#216585=CARTESIAN_POINT('Ctrl Pts',(-17.7068495304908,-61.3772749311671,
-235.350049999996));
#216586=CARTESIAN_POINT('Ctrl Pts',(-17.7124533012131,-61.3775341254997,
-235.350049999996));
#216587=CARTESIAN_POINT('Ctrl Pts',(-17.7180571389861,-61.3777967664626,
-235.350049999996));
#216588=CARTESIAN_POINT('Ctrl Pts',(-17.7236610495722,-61.3780628532939,
-235.350049999996));
#216589=CARTESIAN_POINT('Ctrl Pts',(-17.9268662020405,-61.387711511008,
-235.350049999998));
#216590=CARTESIAN_POINT('Ctrl Pts',(-18.1305704995353,-61.4020849580281,
-235.350049999999));
#216591=CARTESIAN_POINT('Ctrl Pts',(-18.3343978331705,-61.421036350068,
-235.350049999999));
#216592=CARTESIAN_POINT('Ctrl Pts',(-18.5413055198001,-61.4402741461744,
-235.35005));
#216593=CARTESIAN_POINT('Ctrl Pts',(-18.7483412532968,-61.4642294656438,
-235.35005));
#216594=CARTESIAN_POINT('Ctrl Pts',(-18.95511001473,-61.4928010494512,-235.35005));
#216595=CARTESIAN_POINT('Ctrl Pts',(-19.1581684655807,-61.5208599375833,
-235.35005));
#216596=CARTESIAN_POINT('Ctrl Pts',(-19.3609706050519,-61.5533713065191,
-235.35005));
#216597=CARTESIAN_POINT('Ctrl Pts',(-19.5631227327773,-61.5902847141104,
-235.35005));
#216598=CARTESIAN_POINT('Ctrl Pts',(-19.7559941247032,-61.6255034396464,
-235.35005));
#216599=CARTESIAN_POINT('Ctrl Pts',(-19.9482746078014,-61.6647297766438,
-235.35005));
#216600=CARTESIAN_POINT('Ctrl Pts',(-20.1395905386961,-61.7079550103905,
-235.35005));
#216601=CARTESIAN_POINT('Ctrl Pts',(-20.1991813366268,-61.7214187410775,
-235.35005));
#216602=CARTESIAN_POINT('Ctrl Pts',(-20.2586782689426,-61.7352706787151,
-235.35005));
#216603=CARTESIAN_POINT('Ctrl Pts',(-20.3180691938068,-61.7495111937247,
-235.35005));
#216604=CARTESIAN_POINT('',(14.2619189241969,-62.8884528813233,-234.757545437753));
#216605=CARTESIAN_POINT('Ctrl Pts',(14.2619189241969,-62.8884528813233,
-234.757545437753));
#216606=CARTESIAN_POINT('Ctrl Pts',(14.2676221315376,-62.8870512825747,
-234.757599285427));
#216607=CARTESIAN_POINT('Ctrl Pts',(14.27309559464,-62.8857530533057,-234.757590335366));
#216608=CARTESIAN_POINT('Ctrl Pts',(14.2782562309469,-62.8845979535437,
-234.75749584595));
#216609=CARTESIAN_POINT('Ctrl Pts',(14.4728210423908,-62.8410487177465,
-234.753933433427));
#216610=CARTESIAN_POINT('Ctrl Pts',(14.6676054707436,-62.8029521711093,
-234.749855174901));
#216611=CARTESIAN_POINT('Ctrl Pts',(14.862267472532,-62.7701957889222,-234.74525442655));
#216612=CARTESIAN_POINT('Ctrl Pts',(15.0540973159843,-62.7379159828518,
-234.74072061498));
#216613=CARTESIAN_POINT('Ctrl Pts',(15.2458081247477,-62.7108217116278,
-234.735679369408));
#216614=CARTESIAN_POINT('Ctrl Pts',(15.4370736548847,-62.6887561762043,
-234.730130586681));
#216615=CARTESIAN_POINT('Ctrl Pts',(15.5314733326893,-62.6778656648139,
-234.727391968273));
#216616=CARTESIAN_POINT('Ctrl Pts',(15.6257144198455,-62.6682049982271,
-234.72453379674));
#216617=CARTESIAN_POINT('Ctrl Pts',(15.7197562183719,-62.6597512994103,
-234.721556787451));
#216618=CARTESIAN_POINT('Ctrl Pts',(15.9194398772557,-62.6418011374898,
-234.715235554589));
#216619=CARTESIAN_POINT('Ctrl Pts',(16.1183147406937,-62.6293052674362,
-234.708351013767));
#216620=CARTESIAN_POINT('Ctrl Pts',(16.3159941005111,-62.6220209771202,
-234.700911847004));
#216621=CARTESIAN_POINT('Ctrl Pts',(16.3574225292628,-62.6204943801976,
-234.699352792025));
#216622=CARTESIAN_POINT('Ctrl Pts',(16.3987984837776,-62.6191965047478,
-234.69776940586));
#216623=CARTESIAN_POINT('Ctrl Pts',(16.4401184612598,-62.6181248397371,
-234.696161814787));
#216624=CARTESIAN_POINT('Ctrl Pts',(16.5593593875656,-62.615032235715,-234.691522638766));
#216625=CARTESIAN_POINT('Ctrl Pts',(16.6781351876571,-62.6138244557668,
-234.68668086609));
#216626=CARTESIAN_POINT('Ctrl Pts',(16.7963700013562,-62.6144400515916,
-234.681635659345));
#216627=CARTESIAN_POINT('Ctrl Pts',(16.8554874082058,-62.6147478495039,
-234.679113055972));
#216628=CARTESIAN_POINT('Ctrl Pts',(16.9144695680729,-62.6155114373711,
-234.676539558438));
#216629=CARTESIAN_POINT('Ctrl Pts',(16.9733077389818,-62.6167227855682,
-234.673914918543));
#216630=CARTESIAN_POINT('Ctrl Pts',(17.0027268244363,-62.6173284596667,
-234.672602598595));
#216631=CARTESIAN_POINT('Ctrl Pts',(17.0321099129192,-62.6180460709255,
-234.671277491313));
#216632=CARTESIAN_POINT('Ctrl Pts',(17.0614559345793,-62.6188745972855,
-234.669939556944));
#216633=CARTESIAN_POINT('Ctrl Pts',(17.0847044612134,-62.6195309730414,
-234.668879617605));
#216634=CARTESIAN_POINT('Ctrl Pts',(17.1070374630585,-62.6202275257495,
-234.667852866661));
#216635=CARTESIAN_POINT('Ctrl Pts',(17.1305750905829,-62.621033000521,-234.666761357511));
#216636=CARTESIAN_POINT('Ctrl Pts',(17.136748409392,-62.6212442559907,-234.666475082526));
#216637=CARTESIAN_POINT('Ctrl Pts',(17.1430045641319,-62.6214632738738,
-234.666184319474));
#216638=CARTESIAN_POINT('Ctrl Pts',(17.1493817430919,-62.6216918876598,
-234.665887227365));
#216639=CARTESIAN_POINT('Ctrl Pts',(17.3478766374233,-62.6288076781356,
-234.656639993278));
#216640=CARTESIAN_POINT('Ctrl Pts',(17.5455520004757,-62.6410046705095,
-234.646771670025));
#216641=CARTESIAN_POINT('Ctrl Pts',(17.742009985154,-62.6580565731071,-234.636283597108));
#216642=CARTESIAN_POINT('Ctrl Pts',(17.9389575403572,-62.6751509688054,
-234.625769388061));
#216643=CARTESIAN_POINT('Ctrl Pts',(18.1347846733241,-62.6971222883386,
-234.614612391247));
#216644=CARTESIAN_POINT('Ctrl Pts',(18.3292291451991,-62.7237598595182,
-234.602804984691));
#216645=CARTESIAN_POINT('Ctrl Pts',(18.5259098814926,-62.7507037837252,
-234.590861783669));
#216646=CARTESIAN_POINT('Ctrl Pts',(18.7211759890429,-62.7824217829876,
-234.57825304333));
#216647=CARTESIAN_POINT('Ctrl Pts',(18.9147618610651,-62.8186429668106,
-234.56498137667));
#216648=CARTESIAN_POINT('Ctrl Pts',(19.1126402616024,-62.8556673108167,
-234.551415427131));
#216649=CARTESIAN_POINT('Ctrl Pts',(19.3087631000518,-62.8973966834212,
-234.537156722191));
#216650=CARTESIAN_POINT('Ctrl Pts',(19.5028524817591,-62.943488244167,-234.522220426416));
#216651=CARTESIAN_POINT('Ctrl Pts',(19.6704349995014,-62.9832850621511,
-234.509323986488));
#216652=CARTESIAN_POINT('Ctrl Pts',(19.8365016601851,-63.0263329686421,
-234.49592257589));
#216653=CARTESIAN_POINT('Ctrl Pts',(20.0008767707152,-63.0723812833681,
-234.482033933862));
#216654=CARTESIAN_POINT('Ctrl Pts',(8.7858832621216,-63.0089393155471,-234.571897587772));
#216655=CARTESIAN_POINT('Ctrl Pts',(8.79681567493446,-63.0115709797409,
-234.57181396807));
#216656=CARTESIAN_POINT('Ctrl Pts',(8.80985252396294,-63.0142665213595,
-234.572494303784));
#216657=CARTESIAN_POINT('Ctrl Pts',(8.82210928715347,-63.0169068663223,
-234.572891922504));
#216658=CARTESIAN_POINT('Ctrl Pts',(8.85244345145974,-63.0234414347627,
-234.573875985863));
#216659=CARTESIAN_POINT('Ctrl Pts',(8.88278396117814,-63.0298509579082,
-234.574862091849));
#216660=CARTESIAN_POINT('Ctrl Pts',(8.91316422636502,-63.0361424884105,
-234.575851272007));
#216661=CARTESIAN_POINT('Ctrl Pts',(8.99242293231775,-63.0525563861501,
-234.578431932142));
#216662=CARTESIAN_POINT('Ctrl Pts',(9.0719524711103,-63.0681709773559,-234.581033503827));
#216663=CARTESIAN_POINT('Ctrl Pts',(9.15234381497248,-63.0830750262618,
-234.583674547358));
#216664=CARTESIAN_POINT('Ctrl Pts',(9.19361826977972,-63.0907270502666,
-234.585030509663));
#216665=CARTESIAN_POINT('Ctrl Pts',(9.23511984058779,-63.0981909396172,
-234.586396884075));
#216666=CARTESIAN_POINT('Ctrl Pts',(9.27692812757237,-63.1054733788026,
-234.587776220271));
#216667=CARTESIAN_POINT('Ctrl Pts',(9.35723190012809,-63.1194612118898,
-234.590425596942));
#216668=CARTESIAN_POINT('Ctrl Pts',(9.4386674796978,-63.1327830283328,-234.593122828895));
#216669=CARTESIAN_POINT('Ctrl Pts',(9.52179594456459,-63.1454466317045,
-234.595885927164));
#216670=CARTESIAN_POINT('Ctrl Pts',(9.60320028398561,-63.1578475856835,
-234.598591717408));
#216671=CARTESIAN_POINT('Ctrl Pts',(9.68622805619257,-63.1696173756771,
-234.60136068521));
#216672=CARTESIAN_POINT('Ctrl Pts',(9.77140172737696,-63.1807142389001,
-234.604209720771));
#216673=CARTESIAN_POINT('Ctrl Pts',(9.84650123949516,-63.1904985889522,
-234.606721778519));
#216674=CARTESIAN_POINT('Ctrl Pts',(9.92326901592422,-63.1997592047957,
-234.60929609172));
#216675=CARTESIAN_POINT('Ctrl Pts',(10.0020597851061,-63.2084339698903,
-234.611944069746));
#216676=CARTESIAN_POINT('Ctrl Pts',(10.0079176914778,-63.2090789180518,
-234.612140940617));
#216677=CARTESIAN_POINT('Ctrl Pts',(10.0137868348703,-63.2097206627102,
-234.61233823974));
#216678=CARTESIAN_POINT('Ctrl Pts',(10.0196673616597,-63.2103591682456,
-234.61253597217));
#216679=CARTESIAN_POINT('Ctrl Pts',(10.1775217355446,-63.2274989407736,
-234.617843817891));
#216680=CARTESIAN_POINT('Ctrl Pts',(10.3408423339544,-63.2420090474358,
-234.623376571456));
#216681=CARTESIAN_POINT('Ctrl Pts',(10.5096382176533,-63.2531987375938,
-234.629123175597));
#216682=CARTESIAN_POINT('Ctrl Pts',(10.5851067962263,-63.2582016440177,
-234.631692480231));
#216683=CARTESIAN_POINT('Ctrl Pts',(10.6616697717933,-63.2625401196258,
-234.634304495196));
#216684=CARTESIAN_POINT('Ctrl Pts',(10.7393274396082,-63.2661491027286,
-234.636958032241));
#216685=CARTESIAN_POINT('Ctrl Pts',(10.8650023153563,-63.2719895884886,
-234.641252301536));
#216686=CARTESIAN_POINT('Ctrl Pts',(10.9935433905513,-63.2759200262142,
-234.645655597734));
#216687=CARTESIAN_POINT('Ctrl Pts',(11.124943865751,-63.2776525377261,-234.650163351666));
#216688=CARTESIAN_POINT('Ctrl Pts',(11.1906441033508,-63.278518793482,-234.652417228633));
#216689=CARTESIAN_POINT('Ctrl Pts',(11.2570590826227,-63.2788353452046,
-234.654697219748));
#216690=CARTESIAN_POINT('Ctrl Pts',(11.3241872747982,-63.2785648884929,
-234.657002776486));
#216691=CARTESIAN_POINT('Ctrl Pts',(11.3577513708859,-63.278429660137,-234.658155554855));
#216692=CARTESIAN_POINT('Ctrl Pts',(11.3914937693878,-63.2781476704804,
-234.659314718289));
#216693=CARTESIAN_POINT('Ctrl Pts',(11.4254142273421,-63.2777141703294,
-234.660480209155));
#216694=CARTESIAN_POINT('Ctrl Pts',(11.4423744563193,-63.2774974202539,
-234.661062954589));
#216695=CARTESIAN_POINT('Ctrl Pts',(11.4593792001185,-63.2772427919946,
-234.661647281495));
#216696=CARTESIAN_POINT('Ctrl Pts',(11.4764284266816,-63.2769496876593,
-234.662233181745));
#216697=CARTESIAN_POINT('Ctrl Pts',(11.4849530399631,-63.2768031354916,
-234.662526131871));
#216698=CARTESIAN_POINT('Ctrl Pts',(11.4934887739323,-63.2766469642703,
-234.662819475307));
#216699=CARTESIAN_POINT('Ctrl Pts',(11.5020356243932,-63.2764810989383,
-234.663113211071));
#216700=CARTESIAN_POINT('Ctrl Pts',(11.510582474854,-63.2763152336063,-234.663406946834));
#216701=CARTESIAN_POINT('Ctrl Pts',(11.5206164958058,-63.2761077505405,
-234.663751807062));
#216702=CARTESIAN_POINT('Ctrl Pts',(11.5277095211746,-63.2759543445152,
-234.663995595652));
#216703=CARTESIAN_POINT('Ctrl Pts',(11.7959382858705,-63.2701531656785,
-234.673214667765));
#216704=CARTESIAN_POINT('Ctrl Pts',(12.0647257367003,-63.2549839288532,
-234.682485491612));
#216705=CARTESIAN_POINT('Ctrl Pts',(12.3338331099587,-63.2303282374309,
-234.691756583846));
#216706=CARTESIAN_POINT('Ctrl Pts',(12.5122102573677,-63.2139852742112,
-234.697901904081));
#216707=CARTESIAN_POINT('Ctrl Pts',(12.6907279881409,-63.1934753535059,
-234.704047292337));
#216708=CARTESIAN_POINT('Ctrl Pts',(12.8693171326838,-63.1687765962808,
-234.710177274085));
#216709=CARTESIAN_POINT('Ctrl Pts',(13.1051691938716,-63.1361584166303,
-234.718272776385));
#216710=CARTESIAN_POINT('Ctrl Pts',(13.3412824605714,-63.0961134334835,
-234.726378967533));
#216711=CARTESIAN_POINT('Ctrl Pts',(13.5774175745815,-63.0484087566338,
-234.734431297969));
#216712=CARTESIAN_POINT('Ctrl Pts',(13.6949932812573,-63.0246557831895,
-234.738440690835));
#216713=CARTESIAN_POINT('Ctrl Pts',(13.8125727957745,-62.9990048475027,
-234.742436205742));
#216714=CARTESIAN_POINT('Ctrl Pts',(13.9301247417777,-62.9714309612777,
-234.746409185644));
#216715=CARTESIAN_POINT('Ctrl Pts',(13.9887912132901,-62.9576697036745,
-234.748391974702));
#216716=CARTESIAN_POINT('Ctrl Pts',(14.0474508288688,-62.9434295279964,
-234.750369153456));
#216717=CARTESIAN_POINT('Ctrl Pts',(14.1060997648205,-62.9287075009776,
-234.75233966774));
#216718=CARTESIAN_POINT('Ctrl Pts',(14.1112871883718,-62.9274053564725,
-234.752513957214));
#216719=CARTESIAN_POINT('Ctrl Pts',(14.1164745284042,-62.9260994424293,
-234.752688194559));
#216720=CARTESIAN_POINT('Ctrl Pts',(14.1216617823046,-62.9247897568609,
-234.752862379056));
#216721=CARTESIAN_POINT('Ctrl Pts',(14.1456979383595,-62.9187210724837,
-234.753669497011));
#216722=CARTESIAN_POINT('Ctrl Pts',(14.1698178995471,-62.9125255294095,
-234.754509575307));
#216723=CARTESIAN_POINT('Ctrl Pts',(14.1939742871885,-62.9062259828314,
-234.755364712355));
#216724=CARTESIAN_POINT('Ctrl Pts',(14.216952479753,-62.9002336881023,-234.756178141251));
#216725=CARTESIAN_POINT('Ctrl Pts',(14.2409845451924,-62.8936465131962,
-234.757285208748));
#216726=CARTESIAN_POINT('Ctrl Pts',(14.2619189241969,-62.8884528813233,
-234.757545437753));
#216727=CARTESIAN_POINT('Ctrl Pts',(55.6596124147223,-63.9410622767582,
-216.790642532039));
#216728=CARTESIAN_POINT('Ctrl Pts',(56.7746082597229,-64.9675904302956,
-215.348143273993));
#216729=CARTESIAN_POINT('Ctrl Pts',(56.7978769236249,-64.9962486583172,
-213.25615446688));
#216730=CARTESIAN_POINT('Ctrl Pts',(56.5646546671649,-62.9482476744138,
-216.79031846553));
#216731=CARTESIAN_POINT('Ctrl Pts',(57.7003423851772,-63.9568776617924,
-215.347378844935));
#216732=CARTESIAN_POINT('Ctrl Pts',(57.7238224635575,-63.9855135774693,
-213.252837709798));
#216733=CARTESIAN_POINT('Ctrl Pts',(57.4569850684519,-61.9095456344264,
-216.789947870949));
#216734=CARTESIAN_POINT('Ctrl Pts',(58.611700878634,-62.9065844937097,-215.346095403267));
#216735=CARTESIAN_POINT('Ctrl Pts',(58.6299194066537,-62.9418272935278,
-213.246154460278));
#216736=CARTESIAN_POINT('Ctrl Pts',(58.3016167962822,-60.8701016111416,
-216.790073419041));
#216737=CARTESIAN_POINT('Ctrl Pts',(59.4805126951739,-61.8494200250926,
-215.345222444811));
#216738=CARTESIAN_POINT('Ctrl Pts',(59.5017489787801,-61.8814728748856,
-213.239284157696));
#216739=CARTESIAN_POINT('',(59.5017489787801,-61.8814728748856,-213.239284157696));
#216740=CARTESIAN_POINT('Ctrl Pts',(56.8144552684302,-64.9781463796361,
-213.256094898505));
#216741=CARTESIAN_POINT('Ctrl Pts',(56.9294188925119,-64.8525744128834,
-213.255680555424));
#216742=CARTESIAN_POINT('Ctrl Pts',(57.0524106752843,-64.7173956850926,
-213.255183250552));
#216743=CARTESIAN_POINT('Ctrl Pts',(57.1833118747465,-64.5723463396209,
-213.254587821642));
#216744=CARTESIAN_POINT('Ctrl Pts',(57.3081863588042,-64.4339750928097,
-213.254019806389));
#216745=CARTESIAN_POINT('Ctrl Pts',(57.4402589750224,-64.2866205890543,
-213.253362393774));
#216746=CARTESIAN_POINT('Ctrl Pts',(57.5793799148568,-64.1300563307852,
-213.252605702994));
#216747=CARTESIAN_POINT('Ctrl Pts',(57.7142502997413,-63.9782755722807,
-213.251872131349));
#216748=CARTESIAN_POINT('Ctrl Pts',(57.8557452334703,-63.8178386808859,
-213.251045156913));
#216749=CARTESIAN_POINT('Ctrl Pts',(58.0036788274559,-63.6485500668985,
-213.250120374855));
#216750=CARTESIAN_POINT('Ctrl Pts',(58.1403782530185,-63.4921173347321,
-213.249265821317));
#216751=CARTESIAN_POINT('Ctrl Pts',(58.2825754484112,-63.3281259468563,
-213.248327716734));
#216752=CARTESIAN_POINT('Ctrl Pts',(58.4300800100018,-63.1564365856218,
-213.247307421374));
#216753=CARTESIAN_POINT('Ctrl Pts',(58.5727477993223,-62.9903770322558,
-213.246320582175));
#216754=CARTESIAN_POINT('Ctrl Pts',(58.7203807787913,-62.817115737271,-213.245256795861));
#216755=CARTESIAN_POINT('Ctrl Pts',(58.8727631035814,-62.6365458514646,
-213.244122705959));
#216756=CARTESIAN_POINT('Ctrl Pts',(59.0185109355358,-62.4638377016922,
-213.243037992593));
#216757=CARTESIAN_POINT('Ctrl Pts',(59.1686036195926,-62.2844432836784,
-213.241888927712));
#216758=CARTESIAN_POINT('Ctrl Pts',(59.3228101732188,-62.0982909448199,
-213.240687014781));
#216759=CARTESIAN_POINT('Ctrl Pts',(59.381858614956,-62.0270098917333,-213.240226780867));
#216760=CARTESIAN_POINT('Ctrl Pts',(59.4415097985946,-61.9547382044033,
-213.239758862166));
#216761=CARTESIAN_POINT('Ctrl Pts',(59.5017489787801,-61.8814728748856,
-213.239284157696));
#216762=CARTESIAN_POINT('',(58.3016167962821,-60.8701016111416,-216.790073419041));
#216763=CARTESIAN_POINT('Origin',(1.94104476119577,-15.0690951428036,-217.435380395218));
#216764=CARTESIAN_POINT('Origin',(55.6399013441494,-58.7068046741696,-213.15202212551));
#216765=CARTESIAN_POINT('Ctrl Pts',(60.0946517248888,-61.0923008758321,
-213.257460793579));
#216766=CARTESIAN_POINT('Ctrl Pts',(59.9794428890559,-61.1951119486122,
-215.368374394716));
#216767=CARTESIAN_POINT('Ctrl Pts',(58.6463245735781,-60.4071924582901,
-216.811211134516));
#216768=CARTESIAN_POINT('Ctrl Pts',(59.9074639858676,-61.3655831923349,
-213.24427462457));
#216769=CARTESIAN_POINT('Ctrl Pts',(59.8200433378112,-61.4202510270675,
-215.35259069506));
#216770=CARTESIAN_POINT('Ctrl Pts',(58.537453097357,-60.5671124334832,-216.797054630904));
#216771=CARTESIAN_POINT('Ctrl Pts',(59.7097127443643,-61.6285208837114,
-213.238301674021));
#216772=CARTESIAN_POINT('Ctrl Pts',(59.653667582921,-61.6382804704428,-215.344967772288));
#216773=CARTESIAN_POINT('Ctrl Pts',(58.4224878547945,-60.7213519315114,
-216.790091385297));
#216774=CARTESIAN_POINT('Ctrl Pts',(59.5017489787801,-61.8814728748855,
-213.239284157696));
#216775=CARTESIAN_POINT('Ctrl Pts',(59.4805126951738,-61.8494200250926,
-215.345222444811));
#216776=CARTESIAN_POINT('Ctrl Pts',(58.3016167962821,-60.8701016111416,
-216.790073419041));
#216777=CARTESIAN_POINT('',(58.6463245735781,-60.4071924582901,-216.811211134516));
#216778=CARTESIAN_POINT('',(60.094651724889,-61.0923008758319,-213.257460793579));
#216779=CARTESIAN_POINT('Origin',(55.9721510687884,-58.2643380616866,-213.170198761392));
#216780=CARTESIAN_POINT('Origin',(52.480669683245,-56.0916407951787,-217.694018753789));
#216781=CARTESIAN_POINT('Origin',(54.9927878736021,-61.8053486253609,-218.50906240554));
#216782=CARTESIAN_POINT('Ctrl Pts',(58.6074055114448,-60.4543100647495,
-216.811910699149));
#216783=CARTESIAN_POINT('Ctrl Pts',(59.9363259578221,-61.2556965846773,
-215.36842105937));
#216784=CARTESIAN_POINT('Ctrl Pts',(60.0500816328534,-61.1568904110335,
-213.254375849603));
#216785=CARTESIAN_POINT('Ctrl Pts',(58.6843926594325,-60.3569715803453,
-216.813280762464));
#216786=CARTESIAN_POINT('Ctrl Pts',(60.0245567355929,-61.1325327891189,
-215.370731335637));
#216787=CARTESIAN_POINT('Ctrl Pts',(60.1415615520333,-61.0252958819011,
-213.260597914992));
#216788=CARTESIAN_POINT('Ctrl Pts',(58.7617161401563,-60.257380322437,-216.813794119462));
#216789=CARTESIAN_POINT('Ctrl Pts',(60.1108245046652,-61.0067372913192,
-215.372344710318));
#216790=CARTESIAN_POINT('Ctrl Pts',(60.2301284165771,-60.8919475940444,
-213.267282154519));
#216791=CARTESIAN_POINT('Ctrl Pts',(58.8637629875194,-60.118929962275,-216.816300847937));
#216792=CARTESIAN_POINT('Ctrl Pts',(60.2274193821809,-60.8294290656787,
-215.376497710853));
#216793=CARTESIAN_POINT('Ctrl Pts',(60.351618647282,-60.7003634878413,-213.277642216535));
#216794=CARTESIAN_POINT('Ctrl Pts',(58.8929787543517,-60.0784113786681,
-216.817245287021));
#216795=CARTESIAN_POINT('Ctrl Pts',(60.2611173232929,-60.7772510392266,
-215.377939075409));
#216796=CARTESIAN_POINT('Ctrl Pts',(60.3869441313173,-60.6435508076928,
-213.280811345684));
#216797=CARTESIAN_POINT('Ctrl Pts',(58.9495124986678,-59.9981405703258,
-216.819674866848));
#216798=CARTESIAN_POINT('Ctrl Pts',(60.3271235407812,-60.6732372865155,
-215.381384415719));
#216799=CARTESIAN_POINT('Ctrl Pts',(60.4565718022466,-60.5293282073925,
-213.287428511102));
#216800=CARTESIAN_POINT('Ctrl Pts',(58.9761430287399,-59.9590023263254,
-216.821371021085));
#216801=CARTESIAN_POINT('Ctrl Pts',(60.359173711659,-60.6218554219661,-215.383594060466));
#216802=CARTESIAN_POINT('Ctrl Pts',(60.4908728037641,-60.4719198229408,
-213.290891213227));
#216803=CARTESIAN_POINT('Ctrl Pts',(59.0642485460056,-59.8329939373022,
-216.824171668603));
#216804=CARTESIAN_POINT('Ctrl Pts',(60.4575238287991,-60.4610669137915,
-215.388063886973));
#216805=CARTESIAN_POINT('Ctrl Pts',(60.5922460955355,-60.2987937845113,
-213.30164664474));
#216806=CARTESIAN_POINT('Ctrl Pts',(59.1308552045038,-59.7401265656055,
-216.823603457484));
#216807=CARTESIAN_POINT('Ctrl Pts',(60.5247139239745,-60.3469167156672,
-215.388758628301));
#216808=CARTESIAN_POINT('Ctrl Pts',(60.6577989462605,-60.182163619438,-213.309190814847));
#216809=CARTESIAN_POINT('Ctrl Pts',(59.2607825507709,-59.5528560555646,
-216.821806470031));
#216810=CARTESIAN_POINT('Ctrl Pts',(60.6547502248839,-60.1166039110421,
-215.389715911556));
#216811=CARTESIAN_POINT('Ctrl Pts',(60.7848819389693,-59.9464002293942,
-213.324386876106));
#216812=CARTESIAN_POINT('Ctrl Pts',(59.3235037477498,-59.4590534661329,
-216.82085617928));
#216813=CARTESIAN_POINT('Ctrl Pts',(60.7174143058776,-60.0009016819405,
-215.390241225136));
#216814=CARTESIAN_POINT('Ctrl Pts',(60.846408364718,-59.8272707789861,-213.332077521816));
#216815=CARTESIAN_POINT('Ctrl Pts',(59.497535989523,-59.1844462404644,-216.821411068371));
#216816=CARTESIAN_POINT('Ctrl Pts',(60.8959799414287,-59.6576852666735,
-215.395296546354));
#216817=CARTESIAN_POINT('Ctrl Pts',(61.0248485990128,-59.4661777527895,
-213.356063148757));
#216818=CARTESIAN_POINT('Ctrl Pts',(59.6013476331263,-59.0045621852585,
-216.824786693514));
#216819=CARTESIAN_POINT('Ctrl Pts',(61.0052029790378,-59.4294490925104,
-215.401835242901));
#216820=CARTESIAN_POINT('Ctrl Pts',(61.1355702178776,-59.2205125002805,
-213.373562975867));
#216821=CARTESIAN_POINT('Ctrl Pts',(59.7620679015636,-58.7165983993849,
-216.825507837644));
#216822=CARTESIAN_POINT('Ctrl Pts',(61.160929555377,-59.0728872758639,-215.408140407826));
#216823=CARTESIAN_POINT('Ctrl Pts',(61.2879458897801,-58.8475849978508,
-213.401799673797));
#216824=CARTESIAN_POINT('Ctrl Pts',(59.8184700980811,-58.6152752114856,
-216.824157923918));
#216825=CARTESIAN_POINT('Ctrl Pts',(61.2120467193731,-58.9500553531654,
-215.408866560461));
#216826=CARTESIAN_POINT('Ctrl Pts',(61.3365745411598,-58.7222537891958,
-213.411505588844));
#216827=CARTESIAN_POINT('Ctrl Pts',(59.9269424397347,-58.4123215093298,
-216.821223970727));
#216828=CARTESIAN_POINT('Ctrl Pts',(61.3093200563378,-58.7041349241579,
-215.410324805557));
#216829=CARTESIAN_POINT('Ctrl Pts',(61.429120358173,-58.4706258869242,-213.431043252633));
#216830=CARTESIAN_POINT('Ctrl Pts',(59.9776849531454,-58.3122310671642,
-216.820297737876));
#216831=CARTESIAN_POINT('Ctrl Pts',(61.3551328190027,-58.5821325532565,
-215.411652153446));
#216832=CARTESIAN_POINT('Ctrl Pts',(61.4730253186173,-58.3443774821519,
-213.440939227853));
#216833=CARTESIAN_POINT('Ctrl Pts',(60.1230288656398,-58.0127552603068,
-216.818391671956));
#216834=CARTESIAN_POINT('Ctrl Pts',(61.4853151645514,-58.2168872743818,
-215.416733820586));
#216835=CARTESIAN_POINT('Ctrl Pts',(61.5977142939005,-57.9644548465746,
-213.471381381577));
#216836=CARTESIAN_POINT('Ctrl Pts',(60.2105402005316,-57.8145726066615,
-216.818537217051));
#216837=CARTESIAN_POINT('Ctrl Pts',(61.5626251138468,-57.9742502615569,
-215.421806822622));
#216838=CARTESIAN_POINT('Ctrl Pts',(61.6714754954738,-57.7096224301994,
-213.49274435759));
#216839=CARTESIAN_POINT('Ctrl Pts',(60.3806025831265,-57.4045491967827,
-216.81529811369));
#216840=CARTESIAN_POINT('Ctrl Pts',(61.7018225456774,-57.4799411928046,
-215.429818040078));
#216841=CARTESIAN_POINT('Ctrl Pts',(61.8007144046227,-57.1969944641333,
-213.537796166961));
#216842=CARTESIAN_POINT('Ctrl Pts',(60.4634339941568,-57.1919229894312,
-216.811338644603));
#216843=CARTESIAN_POINT('Ctrl Pts',(61.7636221410114,-57.2279080669269,
-215.432277259244));
#216844=CARTESIAN_POINT('Ctrl Pts',(61.8562081200067,-56.9391516851297,
-213.561315895501));
#216845=CARTESIAN_POINT('Ctrl Pts',(60.6152405963767,-56.762184327613,-216.802302824218));
#216846=CARTESIAN_POINT('Ctrl Pts',(61.8694772718262,-56.7213693952703,
-215.43746654745));
#216847=CARTESIAN_POINT('Ctrl Pts',(61.9491342563802,-56.4203496749288,
-213.610036002497));
#216848=CARTESIAN_POINT('Ctrl Pts',(60.6824463640865,-56.5477747378356,
-216.798434344268));
#216849=CARTESIAN_POINT('Ctrl Pts',(61.9133532267272,-56.4685867807556,
-215.441201542271));
#216850=CARTESIAN_POINT('Ctrl Pts',(61.9865582056432,-56.1594017179448,
-213.635279158434));
#216851=CARTESIAN_POINT('Ctrl Pts',(60.8073533359841,-56.0969490021232,
-216.792401635896));
#216852=CARTESIAN_POINT('Ctrl Pts',(61.9872021354889,-55.9382448925313,
-215.452237086731));
#216853=CARTESIAN_POINT('Ctrl Pts',(62.0459484757164,-55.6091885457502,
-213.691499099128));
#216854=CARTESIAN_POINT('Ctrl Pts',(60.8666693908396,-55.8585138307279,
-216.788165726564));
#216855=CARTESIAN_POINT('Ctrl Pts',(62.0158520694785,-55.6592576800417,
-215.457808501477));
#216856=CARTESIAN_POINT('Ctrl Pts',(62.0660566009803,-55.3196727763676,
-213.722940188816));
#216857=CARTESIAN_POINT('Ctrl Pts',(60.9269250208923,-55.5935705192412,
-216.775920823856));
#216858=CARTESIAN_POINT('Ctrl Pts',(62.0343090115749,-55.3647134586715,
-215.458374400723));
#216859=CARTESIAN_POINT('Ctrl Pts',(62.0750191951853,-55.0282471371092,
-213.755373099554));
#216860=CARTESIAN_POINT('',(60.9119170756758,-55.6633990141858,-216.777770284882));
#216861=CARTESIAN_POINT('',(62.0723653519316,-55.1059089910534,-213.746749287634));
#216862=CARTESIAN_POINT('Origin',(57.0770276271036,-54.9084593705222,-213.659487255448));
#216863=CARTESIAN_POINT('Ctrl Pts',(60.0946517248888,-61.0923008758318,
-213.257460793579));
#216864=CARTESIAN_POINT('Ctrl Pts',(60.1688733048961,-60.9839420408379,
-213.262689226369));
#216865=CARTESIAN_POINT('Ctrl Pts',(60.2426760592975,-60.8721561614362,
-213.268476733384));
#216866=CARTESIAN_POINT('Ctrl Pts',(60.3157714398376,-60.7568862808627,
-213.274784382698));
#216867=CARTESIAN_POINT('Ctrl Pts',(60.3512737868304,-60.7008998249785,
-213.277848001124));
#216868=CARTESIAN_POINT('Ctrl Pts',(60.3866089369293,-60.6440917231958,
-213.281039224211));
#216869=CARTESIAN_POINT('Ctrl Pts',(60.4217426652322,-60.5864561384688,
-213.284371063984));
#216870=CARTESIAN_POINT('Ctrl Pts',(60.4435624323821,-60.5506616156829,
-213.286440299775));
#216871=CARTESIAN_POINT('Ctrl Pts',(60.4653040350053,-60.514548553946,-213.288569677611));
#216872=CARTESIAN_POINT('Ctrl Pts',(60.4869604790493,-60.4781138482913,
-213.290748336221));
#216873=CARTESIAN_POINT('Ctrl Pts',(60.4995551781952,-60.4569245821652,
-213.292015374783));
#216874=CARTESIAN_POINT('Ctrl Pts',(60.5121204198581,-60.4356273698192,
-213.293306640679));
#216875=CARTESIAN_POINT('Ctrl Pts',(60.5246547397792,-60.4142217745433,
-213.294620659626));
#216876=CARTESIAN_POINT('Ctrl Pts',(60.591150130146,-60.3006636858019,-213.301591616443));
#216877=CARTESIAN_POINT('Ctrl Pts',(60.6567843084902,-60.1840449613726,
-213.309095887413));
#216878=CARTESIAN_POINT('Ctrl Pts',(60.7213395261845,-60.0642830904757,
-213.316803279816));
#216879=CARTESIAN_POINT('Ctrl Pts',(60.7685965359593,-59.9766125952661,
-213.322445400331));
#216880=CARTESIAN_POINT('Ctrl Pts',(60.8152737419114,-59.8872593538088,
-213.328214013836));
#216881=CARTESIAN_POINT('Ctrl Pts',(60.8612668418636,-59.7962116928738,
-213.334193694335));
#216882=CARTESIAN_POINT('Ctrl Pts',(60.8762151842007,-59.7666200452991,
-213.336137166535));
#216883=CARTESIAN_POINT('Ctrl Pts',(60.8910888831917,-59.7368539552651,
-213.338107798564));
#216884=CARTESIAN_POINT('Ctrl Pts',(60.9058862461468,-59.7069094955419,
-213.340107694982));
#216885=CARTESIAN_POINT('Ctrl Pts',(60.9637435733099,-59.5898273905627,
-213.347927241053));
#216886=CARTESIAN_POINT('Ctrl Pts',(61.0204246813107,-59.4700172291252,
-213.356262962161));
#216887=CARTESIAN_POINT('Ctrl Pts',(61.0757281447404,-59.3474693357667,
-213.365036420254));
#216888=CARTESIAN_POINT('Ctrl Pts',(61.1204542243354,-59.2483600487051,
-213.372131859865));
#216889=CARTESIAN_POINT('Ctrl Pts',(61.1642786072501,-59.1474602983931,
-213.37951365019));
#216890=CARTESIAN_POINT('Ctrl Pts',(61.2070729743782,-59.0447771657053,
-213.387142007677));
#216891=CARTESIAN_POINT('Ctrl Pts',(61.2171558757692,-59.0205837035538,
-213.388939346473));
#216892=CARTESIAN_POINT('Ctrl Pts',(61.2271793702854,-58.996296378915,-213.390750959789));
#216893=CARTESIAN_POINT('Ctrl Pts',(61.2371418312946,-58.9719150325815,
-213.392578681107));
#216894=CARTESIAN_POINT('Ctrl Pts',(61.2783750144538,-58.8710041714885,
-213.400143354916));
#216895=CARTESIAN_POINT('Ctrl Pts',(61.3186449470215,-58.7682927383909,
-213.407960918625));
#216896=CARTESIAN_POINT('Ctrl Pts',(61.3577808239653,-58.6639330018756,
-213.416038726705));
#216897=CARTESIAN_POINT('Ctrl Pts',(61.3604129670204,-58.6569141287302,
-213.416582012));
#216898=CARTESIAN_POINT('Ctrl Pts',(61.3630399688414,-58.649887813559,-213.417126466415));
#216899=CARTESIAN_POINT('Ctrl Pts',(61.3656617724452,-58.642854108928,-213.417672088598));
#216900=CARTESIAN_POINT('Ctrl Pts',(61.3714146872104,-58.6274203429637,
-213.418869324694));
#216901=CARTESIAN_POINT('Ctrl Pts',(61.3771434762636,-58.6119486844701,
-213.420070235415));
#216902=CARTESIAN_POINT('Ctrl Pts',(61.3828474496664,-58.59643983806,-213.421274420738));
#216903=CARTESIAN_POINT('Ctrl Pts',(61.4066350315578,-58.5317624758125,
-213.426296298467));
#216904=CARTESIAN_POINT('Ctrl Pts',(61.4299886141107,-58.4664490159562,
-213.431392104351));
#216905=CARTESIAN_POINT('Ctrl Pts',(61.4528841092791,-58.4004915334073,
-213.436581849268));
#216906=CARTESIAN_POINT('Ctrl Pts',(61.4671034320988,-58.3595284212386,
-213.439804957473));
#216907=CARTESIAN_POINT('Ctrl Pts',(61.48114539916,-58.318318751907,-213.443064189012));
#216908=CARTESIAN_POINT('Ctrl Pts',(61.4950031156842,-58.2768639431237,
-213.446364418246));
#216909=CARTESIAN_POINT('Ctrl Pts',(61.4998241791749,-58.2624419231042,
-213.447512559402));
#216910=CARTESIAN_POINT('Ctrl Pts',(61.5050437465624,-58.2467173872201,
-213.448767386496));
#216911=CARTESIAN_POINT('Ctrl Pts',(61.5096349176404,-58.2327939136108,
-213.449881149215));
#216912=CARTESIAN_POINT('Ctrl Pts',(61.5106925269236,-58.2295865413098,
-213.450137712469));
#216913=CARTESIAN_POINT('Ctrl Pts',(61.5117170122721,-58.2264747787118,
-213.450386767174));
#216914=CARTESIAN_POINT('Ctrl Pts',(61.5126961916284,-58.2234966253952,
-213.450625245251));
#216915=CARTESIAN_POINT('Ctrl Pts',(61.5133274243917,-58.221576744287,-213.450778981311));
#216916=CARTESIAN_POINT('Ctrl Pts',(61.5139581302282,-58.2196567378002,
-213.450932777525));
#216917=CARTESIAN_POINT('Ctrl Pts',(61.5145883090845,-58.2177366063309,
-213.451086634312));
#216918=CARTESIAN_POINT('Ctrl Pts',(61.5754675922918,-58.0322397011969,
-213.465950177932));
#216919=CARTESIAN_POINT('Ctrl Pts',(61.6314260330506,-57.8455859554956,
-213.481413045566));
#216920=CARTESIAN_POINT('Ctrl Pts',(61.6824475740234,-57.6580324650191,
-213.49749706447));
#216921=CARTESIAN_POINT('Ctrl Pts',(61.7009806262513,-57.5899055804081,
-213.503339419615));
#216922=CARTESIAN_POINT('Ctrl Pts',(61.7188627796439,-57.5216600629364,
-213.509263678944));
#216923=CARTESIAN_POINT('Ctrl Pts',(61.736094926277,-57.4533085098064,-213.51527069985));
#216924=CARTESIAN_POINT('Ctrl Pts',(61.7840826055166,-57.2629647019827,
-213.531998911289));
#216925=CARTESIAN_POINT('Ctrl Pts',(61.8270345946187,-57.0717719007629,
-213.549276027728));
#216926=CARTESIAN_POINT('Ctrl Pts',(61.8649529491542,-56.8799677222285,
-213.567015134291));
#216927=CARTESIAN_POINT('Ctrl Pts',(61.8781328721527,-56.8132991039609,
-213.573181015206));
#216928=CARTESIAN_POINT('Ctrl Pts',(61.8907051028513,-56.7465566994706,
-213.579402669573));
#216929=CARTESIAN_POINT('Ctrl Pts',(61.9026711707414,-56.6797507397666,
-213.585676324044));
#216930=CARTESIAN_POINT('Ctrl Pts',(61.9367372826433,-56.4895613375432,
-213.60353674546));
#216931=CARTESIAN_POINT('Ctrl Pts',(61.9658823716952,-56.2988624688379,
-213.621842648317));
#216932=CARTESIAN_POINT('Ctrl Pts',(61.9901097322645,-56.1079785002405,
-213.640827105813));
#216933=CARTESIAN_POINT('Ctrl Pts',(61.9990293863389,-56.0377017995089,
-213.647816509102));
#216934=CARTESIAN_POINT('Ctrl Pts',(62.0072829516351,-55.9674000675249,
-213.654897754168));
#216935=CARTESIAN_POINT('Ctrl Pts',(62.0148722891561,-55.8970896752966,
-213.662081941508));
#216936=CARTESIAN_POINT('Ctrl Pts',(62.0354032478553,-55.7068833819308,
-213.68151687284));
#216937=CARTESIAN_POINT('Ctrl Pts',(62.0510721347403,-55.5166252894532,
-213.701767805664));
#216938=CARTESIAN_POINT('Ctrl Pts',(62.0619255431476,-55.3264908015158,
-213.722497227011));
#216939=CARTESIAN_POINT('Ctrl Pts',(62.0661239505739,-55.2529413674403,
-213.730515957465));
#216940=CARTESIAN_POINT('Ctrl Pts',(62.0696023181198,-55.1794105511713,
-213.738606363368));
#216941=CARTESIAN_POINT('Ctrl Pts',(62.0723653519315,-55.1059089910535,
-213.746749287634));
#216942=CARTESIAN_POINT('Ctrl Pts',(60.9119170756758,-55.6633990141858,
-216.777770284882));
#216943=CARTESIAN_POINT('Ctrl Pts',(60.9073907830727,-55.6830113627593,
-216.778588585298));
#216944=CARTESIAN_POINT('Ctrl Pts',(60.9027344732998,-55.7030660698564,
-216.779382142226));
#216945=CARTESIAN_POINT('Ctrl Pts',(60.8979388924468,-55.7235631928626,
-216.780150955665));
#216946=CARTESIAN_POINT('Ctrl Pts',(60.8855667250161,-55.7764439273244,
-216.782134425215));
#216947=CARTESIAN_POINT('Ctrl Pts',(60.8722672911103,-55.8322729157864,
-216.783953203688));
#216948=CARTESIAN_POINT('Ctrl Pts',(60.8579173895963,-55.8910134972092,
-216.785607291083));
#216949=CARTESIAN_POINT('Ctrl Pts',(60.8525552968731,-55.9129629470987,
-216.786225369888));
#216950=CARTESIAN_POINT('Ctrl Pts',(60.8470465325387,-55.9353184362973,
-216.786820453299));
#216951=CARTESIAN_POINT('Ctrl Pts',(60.8413847105074,-55.9580761274448,
-216.787392541314));
#216952=CARTESIAN_POINT('Ctrl Pts',(60.8280412423979,-56.0117101916013,
-216.788740806617));
#216953=CARTESIAN_POINT('Ctrl Pts',(60.8138474727369,-56.0675809540217,
-216.789961349869));
#216954=CARTESIAN_POINT('Ctrl Pts',(60.7987212695568,-56.1256111309988,
-216.791054171069));
#216955=CARTESIAN_POINT('Ctrl Pts',(60.7911581679667,-56.1546262194874,
-216.791600581669));
#216956=CARTESIAN_POINT('Ctrl Pts',(60.7833619960081,-56.1841805428932,
-216.792115061728));
#216957=CARTESIAN_POINT('Ctrl Pts',(60.7753227949662,-56.2142603888131,
-216.792597612924));
#216958=CARTESIAN_POINT('Ctrl Pts',(60.7713031944453,-56.2293003117731,
-216.792838888522));
#216959=CARTESIAN_POINT('Ctrl Pts',(60.7672228324461,-56.2444716142868,
-216.793072178277));
#216960=CARTESIAN_POINT('Ctrl Pts',(60.7630805012708,-56.2597722389012,
-216.793297487807));
#216961=CARTESIAN_POINT('Ctrl Pts',(60.7595341573754,-56.2728714514941,
-216.793490380419));
#216962=CARTESIAN_POINT('Ctrl Pts',(60.7555793881087,-56.2873946780629,
-216.793695306117));
#216963=CARTESIAN_POINT('Ctrl Pts',(60.7521474474415,-56.2999266198356,
-216.793866332403));
#216964=CARTESIAN_POINT('Ctrl Pts',(60.7515706864043,-56.3020326981266,
-216.793895074536));
#216965=CARTESIAN_POINT('Ctrl Pts',(60.7510088127115,-56.3040825498413,
-216.793922859246));
#216966=CARTESIAN_POINT('Ctrl Pts',(60.7504663829785,-56.3060599824529,
-216.793949468515));
#216967=CARTESIAN_POINT('Ctrl Pts',(60.726744928692,-56.3925367635904,-216.795113141008));
#216968=CARTESIAN_POINT('Ctrl Pts',(60.7021402838857,-56.4777392222418,
-216.796372991844));
#216969=CARTESIAN_POINT('Ctrl Pts',(60.6768135902453,-56.5613350649519,
-216.797729021024));
#216970=CARTESIAN_POINT('Ctrl Pts',(60.6619983636042,-56.610235698157,-216.798522250488));
#216971=CARTESIAN_POINT('Ctrl Pts',(60.6469357952424,-56.6585875450376,
-216.799348390635));
#216972=CARTESIAN_POINT('Ctrl Pts',(60.6316559403284,-56.7063320203518,
-216.800207441465));
#216973=CARTESIAN_POINT('Ctrl Pts',(60.6232394165903,-56.7326308636398,
-216.800680628007));
#216974=CARTESIAN_POINT('Ctrl Pts',(60.6147569210123,-56.7587455902481,
-216.801163799913));
#216975=CARTESIAN_POINT('Ctrl Pts',(60.6062090667045,-56.7846826419487,
-216.801656957185));
#216976=CARTESIAN_POINT('Ctrl Pts',(60.5977766165011,-56.8102695189606,
-216.802143456368));
#216977=CARTESIAN_POINT('Ctrl Pts',(60.5892805607033,-56.8356834853934,
-216.802639673109));
#216978=CARTESIAN_POINT('Ctrl Pts',(60.5807215482445,-56.8609304861147,
-216.803145607486));
#216979=CARTESIAN_POINT('Ctrl Pts',(60.5764420420152,-56.8735539864754,
-216.803398574674));
#216980=CARTESIAN_POINT('Ctrl Pts',(60.5721467964869,-56.8861357453652,
-216.803653971149));
#216981=CARTESIAN_POINT('Ctrl Pts',(60.5678358994622,-56.8986764798207,
-216.803911797061));
#216982=CARTESIAN_POINT('Ctrl Pts',(60.5656804509498,-56.9049468470485,
-216.804040710018));
#216983=CARTESIAN_POINT('Ctrl Pts',(60.5635210895554,-56.9112069581651,
-216.804170230326));
#216984=CARTESIAN_POINT('Ctrl Pts',(60.5613578264237,-56.9174569020256,
-216.804300357988));
#216985=CARTESIAN_POINT('Ctrl Pts',(60.5591945632921,-56.923706845886,-216.80443048565));
#216986=CARTESIAN_POINT('Ctrl Pts',(60.5576872782576,-56.9280531415995,
-216.8045212999));
#216987=CARTESIAN_POINT('Ctrl Pts',(60.5548563430524,-56.9361763202472,
-216.804692563016));
#216988=CARTESIAN_POINT('Ctrl Pts',(60.531775183356,-57.002406159512,-216.806088904177));
#216989=CARTESIAN_POINT('Ctrl Pts',(60.5092923413343,-57.0649063224503,
-216.80735534074));
#216990=CARTESIAN_POINT('Ctrl Pts',(60.4875747703621,-57.1238418980249,
-216.808491872706));
#216991=CARTESIAN_POINT('Ctrl Pts',(60.4666733138366,-57.1805627611569,
-216.809585695468));
#216992=CARTESIAN_POINT('Ctrl Pts',(60.4464808877171,-57.2339808981995,
-216.810559193437));
#216993=CARTESIAN_POINT('Ctrl Pts',(60.4271400166051,-57.2841984344429,
-216.811412366612));
#216994=CARTESIAN_POINT('Ctrl Pts',(60.4074215554359,-57.3353963630518,
-216.812282196209));
#216995=CARTESIAN_POINT('Ctrl Pts',(60.3885884660559,-57.3832669787684,
-216.813026956971));
#216996=CARTESIAN_POINT('Ctrl Pts',(60.3707817467398,-57.4278816294471,
-216.813646648899));
#216997=CARTESIAN_POINT('Ctrl Pts',(60.3618783870818,-57.4501889547864,
-216.813956494863));
#216998=CARTESIAN_POINT('Ctrl Pts',(60.353231441283,-57.4716817687946,-216.814235073607));
#216999=CARTESIAN_POINT('Ctrl Pts',(60.344857338237,-57.4923662297235,-216.814482391391));
#217000=CARTESIAN_POINT('Ctrl Pts',(60.340670286714,-57.502708460188,-216.814606050283));
#217001=CARTESIAN_POINT('Ctrl Pts',(60.3365514347898,-57.5128485980101,
-216.814721883031));
#217002=CARTESIAN_POINT('Ctrl Pts',(60.3325027491553,-57.5227872445278,
-216.814829903421));
#217003=CARTESIAN_POINT('Ctrl Pts',(60.330478406338,-57.5277565677866,-216.814883913616));
#217004=CARTESIAN_POINT('Ctrl Pts',(60.3284716044061,-57.5326755179509,
-216.814935970048));
#217005=CARTESIAN_POINT('Ctrl Pts',(60.3264825839235,-57.5375441656945,
-216.814986072732));
#217006=CARTESIAN_POINT('Ctrl Pts',(60.3244935634409,-57.5424128134381,
-216.815036175415));
#217007=CARTESIAN_POINT('Ctrl Pts',(60.3231512484711,-57.5456958600444,
-216.815069449648));
#217008=CARTESIAN_POINT('Ctrl Pts',(60.3205691041673,-57.5519992691854,
-216.815130518181));
#217009=CARTESIAN_POINT('Ctrl Pts',(60.3057977046936,-57.5880585143369,
-216.815479866468));
#217010=CARTESIAN_POINT('Ctrl Pts',(60.2908264545178,-57.6241214719244,
-216.815797788964));
#217011=CARTESIAN_POINT('Ctrl Pts',(60.2756504796204,-57.6602025647167,
-216.816084285669));
#217012=CARTESIAN_POINT('Ctrl Pts',(60.2483805836785,-57.7250371241154,
-216.816599095121));
#217013=CARTESIAN_POINT('Ctrl Pts',(60.2204496607956,-57.7899302381468,
-216.81701243403));
#217014=CARTESIAN_POINT('Ctrl Pts',(60.1919174451317,-57.854738387928,-216.817324302395));
#217015=CARTESIAN_POINT('Ctrl Pts',(60.1697121029587,-57.9051756606042,
-216.817567015538));
#217016=CARTESIAN_POINT('Ctrl Pts',(60.1471425664518,-57.9555614731162,
-216.817748269903));
#217017=CARTESIAN_POINT('Ctrl Pts',(60.124236944089,-58.0058281702384,-216.817868065669));
#217018=CARTESIAN_POINT('Ctrl Pts',(60.1127841329077,-58.0309615187996,
-216.817927963552));
#217019=CARTESIAN_POINT('Ctrl Pts',(60.1012472999562,-58.0560650883737,
-216.817972496468));
#217020=CARTESIAN_POINT('Ctrl Pts',(60.0896299548045,-58.0811304205851,
-216.818001664822));
#217021=CARTESIAN_POINT('Ctrl Pts',(60.0794647777968,-58.1030625862702,
-216.818027187132));
#217022=CARTESIAN_POINT('Ctrl Pts',(60.0692379586165,-58.1249654764669,
-216.81804094593));
#217023=CARTESIAN_POINT('Ctrl Pts',(60.0589518474159,-58.146833423864,-216.818042941059));
#217024=CARTESIAN_POINT('Ctrl Pts',(60.0574824029587,-58.1499574163493,
-216.818043226077));
#217025=CARTESIAN_POINT('Ctrl Pts',(60.0554334228072,-58.1543076149849,
-216.818043194359));
#217026=CARTESIAN_POINT('Ctrl Pts',(60.0545398907524,-58.156203245427,-216.818043075904));
#217027=CARTESIAN_POINT('Ctrl Pts',(60.0450523572134,-58.1763310710596,
-216.818041818146));
#217028=CARTESIAN_POINT('Ctrl Pts',(60.0333692392358,-58.2007570838859,
-216.818133804124));
#217029=CARTESIAN_POINT('Ctrl Pts',(60.019406065471,-58.2294040937821,-216.818319033837));
#217030=CARTESIAN_POINT('Ctrl Pts',(60.0123285027026,-58.2439245039755,
-216.81841292187));
#217031=CARTESIAN_POINT('Ctrl Pts',(60.0046647473224,-58.2595287307156,
-216.818530766153));
#217032=CARTESIAN_POINT('Ctrl Pts',(59.9964016741368,-58.2762019403733,
-216.818672566686));
#217033=CARTESIAN_POINT('Ctrl Pts',(59.9841191164583,-58.3009856563962,
-216.818883344587));
#217034=CARTESIAN_POINT('Ctrl Pts',(59.9705125067986,-58.32813243013,-216.819147053873));
#217035=CARTESIAN_POINT('Ctrl Pts',(59.955534532171,-58.35757651355,-216.819463694545));
#217036=CARTESIAN_POINT('Ctrl Pts',(59.9480455448571,-58.37229855526,-216.819622014881));
#217037=CARTESIAN_POINT('Ctrl Pts',(59.9402136478829,-58.3875945819531,
-216.819793568053));
#217038=CARTESIAN_POINT('Ctrl Pts',(59.9320326268601,-58.4034540498328,
-216.819978358033));
#217039=CARTESIAN_POINT('Ctrl Pts',(59.9279421163487,-58.4113837837727,
-216.820070753024));
#217040=CARTESIAN_POINT('Ctrl Pts',(59.9237643184495,-58.4194543747942,
-216.82016645031));
#217041=CARTESIAN_POINT('Ctrl Pts',(59.9194984513664,-58.4276643114252,
-216.820265458625));
#217042=CARTESIAN_POINT('Ctrl Pts',(59.9173655178249,-58.4317692797407,
-216.820314962783));
#217043=CARTESIAN_POINT('Ctrl Pts',(59.9152105665835,-58.4359090842562,
-216.820365294261));
#217044=CARTESIAN_POINT('Ctrl Pts',(59.9130334990711,-58.4400835282948,
-216.820416453085));
#217045=CARTESIAN_POINT('Ctrl Pts',(59.9108564315587,-58.4442579723333,
-216.82046761191));
#217046=CARTESIAN_POINT('Ctrl Pts',(59.9093877396424,-58.447071603812,-216.820502230613));
#217047=CARTESIAN_POINT('Ctrl Pts',(59.9064358482483,-58.4527105781537,
-216.820572410718));
#217048=CARTESIAN_POINT('Ctrl Pts',(59.8836567049482,-58.4962253920307,
-216.821113976256));
#217049=CARTESIAN_POINT('Ctrl Pts',(59.863123350219,-58.5347073198221,-216.821591266887));
#217050=CARTESIAN_POINT('Ctrl Pts',(59.8449810090749,-58.5683168623629,
-216.82200428261));
#217051=CARTESIAN_POINT('Ctrl Pts',(59.8406893207328,-58.5762674174075,
-216.822101984155));
#217052=CARTESIAN_POINT('Ctrl Pts',(59.8365311992246,-58.5839453291258,
-216.822196088943));
#217053=CARTESIAN_POINT('Ctrl Pts',(59.8325081565776,-58.5913526920526,
-216.822286596973));
#217054=CARTESIAN_POINT('Ctrl Pts',(59.8182762284612,-58.6175570020629,
-216.822606778461));
#217055=CARTESIAN_POINT('Ctrl Pts',(59.8057378540362,-58.6403753963495,
-216.822881947839));
#217056=CARTESIAN_POINT('Ctrl Pts',(59.7949528527874,-58.6598895003186,
-216.823112105107));
#217057=CARTESIAN_POINT('Ctrl Pts',(59.7823725663588,-58.6826519471338,
-216.82338057465));
#217058=CARTESIAN_POINT('Ctrl Pts',(59.7721774792337,-58.7009207038603,
-216.82358779928));
#217059=CARTESIAN_POINT('Ctrl Pts',(59.764413184972,-58.7148074027386,-216.823733778996));
#217060=CARTESIAN_POINT('Ctrl Pts',(59.7639315295643,-58.715668859477,-216.823742834799));
#217061=CARTESIAN_POINT('Ctrl Pts',(59.7634592167051,-58.7165134410566,
-216.823751654913));
#217062=CARTESIAN_POINT('Ctrl Pts',(59.7629962529251,-58.7173411691037,
-216.823760239338));
#217063=CARTESIAN_POINT('Ctrl Pts',(59.7590332786009,-58.7244265289962,
-216.823833722101));
#217064=CARTESIAN_POINT('Ctrl Pts',(59.7557554978705,-58.7302773052047,
-216.823889935053));
#217065=CARTESIAN_POINT('Ctrl Pts',(59.7531659200656,-58.7349047974698,
-216.82392889424));
#217066=CARTESIAN_POINT('Ctrl Pts',(59.7518711311631,-58.7372185436024,
-216.823948373834));
#217067=CARTESIAN_POINT('Ctrl Pts',(59.7507483680804,-58.739226455036,-216.823963511933));
#217068=CARTESIAN_POINT('Ctrl Pts',(59.7497978555437,-58.7409294698187,
-216.823974344221));
#217069=CARTESIAN_POINT('Ctrl Pts',(59.7493225992753,-58.7417809772101,
-216.823979760365));
#217070=CARTESIAN_POINT('Ctrl Pts',(59.7488904041548,-58.7425562596209,
-216.823984098381));
#217071=CARTESIAN_POINT('Ctrl Pts',(59.7485012918142,-58.7432554149837,
-216.823987357719));
#217072=CARTESIAN_POINT('Ctrl Pts',(59.7483067356439,-58.743604992665,-216.823988987388));
#217073=CARTESIAN_POINT('Ctrl Pts',(59.7481229499662,-58.7439355379926,
-216.823990347285));
#217074=CARTESIAN_POINT('Ctrl Pts',(59.7479553264888,-58.74423756571,-216.823991302489));
#217075=CARTESIAN_POINT('Ctrl Pts',(59.7477877030115,-58.7445395934275,
-216.823992257693));
#217076=CARTESIAN_POINT('Ctrl Pts',(59.7476255091587,-58.7448323222523,
-216.823993077977));
#217077=CARTESIAN_POINT('Ctrl Pts',(59.7467469666766,-58.7464181291695,
-216.823996273977));
#217078=CARTESIAN_POINT('Ctrl Pts',(59.7093801477012,-58.8138668424792,
-216.824132208612));
#217079=CARTESIAN_POINT('Ctrl Pts',(59.671557263908,-58.8808174952574,-216.824072812657));
#217080=CARTESIAN_POINT('Ctrl Pts',(59.6338697911996,-58.9464350884605,
-216.823817390672));
#217081=CARTESIAN_POINT('Ctrl Pts',(59.6148480499456,-58.9795538090835,
-216.823688473274));
#217082=CARTESIAN_POINT('Ctrl Pts',(59.5958613342072,-59.012333442612,-216.823509619128));
#217083=CARTESIAN_POINT('Ctrl Pts',(59.576987047306,-59.0446718084732,-216.823280738817));
#217084=CARTESIAN_POINT('Ctrl Pts',(59.5488522419803,-59.0928767357806,
-216.822939560206));
#217085=CARTESIAN_POINT('Ctrl Pts',(59.520967162405,-59.1401021366816,-216.822487212211));
#217086=CARTESIAN_POINT('Ctrl Pts',(59.4934981529907,-59.1861679523762,
-216.821923708002));
#217087=CARTESIAN_POINT('Ctrl Pts',(59.4797636482836,-59.2092008602235,
-216.821641955898));
#217088=CARTESIAN_POINT('Ctrl Pts',(59.4661331607649,-59.2319438715733,
-216.821332414342));
#217089=CARTESIAN_POINT('Ctrl Pts',(59.4526274993308,-59.2543744490891,
-216.82099508287));
#217090=CARTESIAN_POINT('Ctrl Pts',(59.4458746686138,-59.2655897378471,
-216.820826417134));
#217091=CARTESIAN_POINT('Ctrl Pts',(59.4391530444012,-59.2767269181358,
-216.820650803898));
#217092=CARTESIAN_POINT('Ctrl Pts',(59.4324652288841,-59.2877831705383,
-216.820468243147));
#217093=CARTESIAN_POINT('Ctrl Pts',(59.4266133903066,-59.2974573913905,
-216.820308502491));
#217094=CARTESIAN_POINT('Ctrl Pts',(59.4207874365105,-59.307069651829,-216.820143442642));
#217095=CARTESIAN_POINT('Ctrl Pts',(59.4149891112262,-59.3166180621561,
-216.81997306359));
#217096=CARTESIAN_POINT('Ctrl Pts',(59.4141607790427,-59.3179821207743,
-216.819948723726));
#217097=CARTESIAN_POINT('Ctrl Pts',(59.4127237069262,-59.3203476995733,
-216.819906186974));
#217098=CARTESIAN_POINT('Ctrl Pts',(59.412505811316,-59.3207063232844,-216.819899718332));
#217099=CARTESIAN_POINT('Ctrl Pts',(59.4101950050686,-59.3245095660916,
-216.81983111769));
#217100=CARTESIAN_POINT('Ctrl Pts',(59.4065064701905,-59.3304507048173,
-216.819787891195));
#217101=CARTESIAN_POINT('Ctrl Pts',(59.4014629664427,-59.3384677889279,
-216.819770038848));
#217102=CARTESIAN_POINT('Ctrl Pts',(59.3965571326525,-59.3462660347695,
-216.819752673807));
#217103=CARTESIAN_POINT('Ctrl Pts',(59.390369086223,-59.3560285473249,-216.819759316569));
#217104=CARTESIAN_POINT('Ctrl Pts',(59.3829384292983,-59.3676532194846,
-216.819789967134));
#217105=CARTESIAN_POINT('Ctrl Pts',(59.3755077723737,-59.3792778916444,
-216.819820617699));
#217106=CARTESIAN_POINT('Ctrl Pts',(59.3668340747563,-59.3927651891293,
-216.819875276067));
#217107=CARTESIAN_POINT('Ctrl Pts',(59.3569807137444,-59.4079627143511,
-216.819953942239));
#217108=CARTESIAN_POINT('Ctrl Pts',(59.345244910556,-59.4260636613008,-216.820047637243));
#217109=CARTESIAN_POINT('Ctrl Pts',(59.3318368966217,-59.446588707006,-216.820175389473));
#217110=CARTESIAN_POINT('Ctrl Pts',(59.3168812995138,-59.4692357632739,
-216.820337198929));
#217111=CARTESIAN_POINT('Ctrl Pts',(59.3114313506556,-59.4774885463329,
-216.820396163693));
#217112=CARTESIAN_POINT('Ctrl Pts',(59.3057761218172,-59.486022628311,-216.820459651041));
#217113=CARTESIAN_POINT('Ctrl Pts',(59.299922358357,-59.4948219380608,-216.820527660973));
#217114=CARTESIAN_POINT('Ctrl Pts',(59.2894628196999,-59.5105445959898,
-216.820649181515));
#217115=CARTESIAN_POINT('Ctrl Pts',(59.2783692893878,-59.5271142151468,
-216.820785141153));
#217116=CARTESIAN_POINT('Ctrl Pts',(59.2666825624745,-59.5444352646829,
-216.820935540058));
#217117=CARTESIAN_POINT('Ctrl Pts',(59.2608391990179,-59.553095789451,-216.821010739511));
#217118=CARTESIAN_POINT('Ctrl Pts',(59.2548475363252,-59.561944171757,-216.821089548675));
#217119=CARTESIAN_POINT('Ctrl Pts',(59.248712924834,-59.5709681710487,-216.821171967444));
#217120=CARTESIAN_POINT('Ctrl Pts',(59.2456456190885,-59.5754801706945,
-216.821213176829));
#217121=CARTESIAN_POINT('Ctrl Pts',(59.2425425764809,-59.5800360748127,
-216.821255289034));
#217122=CARTESIAN_POINT('Ctrl Pts',(59.2394044660912,-59.5846343656262,
-216.821298303416));
#217123=CARTESIAN_POINT('Ctrl Pts',(59.2368833700425,-59.5883285418536,
-216.821332860324));
#217124=CARTESIAN_POINT('Ctrl Pts',(59.2338763518166,-59.5927271064996,
-216.821374460242));
#217125=CARTESIAN_POINT('Ctrl Pts',(59.231500599681,-59.5961969430932,-216.821407532326));
#217126=CARTESIAN_POINT('Ctrl Pts',(59.2309191568838,-59.5970461526822,
-216.821415626405));
#217127=CARTESIAN_POINT('Ctrl Pts',(59.2303754231141,-59.5978399769206,
-216.821423209684));
#217128=CARTESIAN_POINT('Ctrl Pts',(59.2298856041354,-59.5985548823212,
-216.821430053904));
#217129=CARTESIAN_POINT('Ctrl Pts',(59.209665444883,-59.6280668074965,-216.821712589333));
#217130=CARTESIAN_POINT('Ctrl Pts',(59.190618034438,-59.6556168075343,-216.821931387029));
#217131=CARTESIAN_POINT('Ctrl Pts',(59.1726374240291,-59.6814738124503,
-216.822086446994));
#217132=CARTESIAN_POINT('Ctrl Pts',(59.1551735707798,-59.7065876950744,
-216.822237050583));
#217133=CARTESIAN_POINT('Ctrl Pts',(59.1387162929886,-59.7301038456633,
-216.822327527399));
#217134=CARTESIAN_POINT('Ctrl Pts',(59.1231840355727,-59.752224284079,-216.822357877443));
#217135=CARTESIAN_POINT('Ctrl Pts',(59.1074219776338,-59.7746719954842,
-216.822388676518));
#217136=CARTESIAN_POINT('Ctrl Pts',(59.0926126061971,-59.7956820867913,
-216.822357556502));
#217137=CARTESIAN_POINT('Ctrl Pts',(59.0786847843651,-59.8154259777699,
-216.822264517394));
#217138=CARTESIAN_POINT('Ctrl Pts',(59.0717208734491,-59.8252979232592,
-216.82221799784));
#217139=CARTESIAN_POINT('Ctrl Pts',(59.0649775596332,-59.8348527320287,
-216.822155998507));
#217140=CARTESIAN_POINT('Ctrl Pts',(59.0584471400814,-59.8441085381158,
-216.82207852147));
#217141=CARTESIAN_POINT('Ctrl Pts',(59.0551819303055,-59.8487364411594,
-216.822039782951));
#217142=CARTESIAN_POINT('Ctrl Pts',(59.0519699404847,-59.8532895909422,
-216.821997170372));
#217143=CARTESIAN_POINT('Ctrl Pts',(59.0488102987358,-59.8577700233926,
-216.821950690937));
#217144=CARTESIAN_POINT('Ctrl Pts',(59.0465865056734,-59.8609234045008,
-216.821917978162));
#217145=CARTESIAN_POINT('Ctrl Pts',(59.0449907155021,-59.8631849981604,
-216.821893998581));
#217146=CARTESIAN_POINT('Ctrl Pts',(59.0427507400838,-59.8663637683885,
-216.82185626504));
#217147=CARTESIAN_POINT('Ctrl Pts',(59.0418080813048,-59.8677015043465,
-216.821840385467));
#217148=CARTESIAN_POINT('Ctrl Pts',(59.0407515417077,-59.8692012370604,
-216.821822070046));
#217149=CARTESIAN_POINT('Ctrl Pts',(59.0394875349051,-59.8709951915532,
-216.821799642799));
#217150=CARTESIAN_POINT('Ctrl Pts',(59.0135515911386,-59.9078050431719,
-216.821339461873));
#217151=CARTESIAN_POINT('Ctrl Pts',(58.9883333235131,-59.9434790847653,
-216.820707237385));
#217152=CARTESIAN_POINT('Ctrl Pts',(58.9637410153438,-59.9783059369304,
-216.819902969334));
#217153=CARTESIAN_POINT('Ctrl Pts',(58.9559613748387,-59.989323218753,-216.81964854359));
#217154=CARTESIAN_POINT('Ctrl Pts',(58.9482443777768,-60.0002557171563,
-216.819376900789));
#217155=CARTESIAN_POINT('Ctrl Pts',(58.9405878012406,-60.0111070272961,
-216.819088040933));
#217156=CARTESIAN_POINT('Ctrl Pts',(58.9246578683285,-60.033683780982,-216.81848705195));
#217157=CARTESIAN_POINT('Ctrl Pts',(58.9089894699818,-60.055909105829,-216.817811535297));
#217158=CARTESIAN_POINT('Ctrl Pts',(58.8935626743483,-60.0778152568291,
-216.817061490999));
#217159=CARTESIAN_POINT('Ctrl Pts',(58.8858492765315,-60.0887683323292,
-216.81668646885));
#217160=CARTESIAN_POINT('Ctrl Pts',(58.8781962793657,-60.099641614347,-216.816292814753));
#217161=CARTESIAN_POINT('Ctrl Pts',(58.8706012070292,-60.110439113199,-216.815880528753));
#217162=CARTESIAN_POINT('Ctrl Pts',(58.866803670861,-60.115837862625,-216.815674385752));
#217163=CARTESIAN_POINT('Ctrl Pts',(58.863020615899,-60.1212176662587,-216.815463584775));
#217164=CARTESIAN_POINT('Ctrl Pts',(58.8592517332946,-60.1265790245349,
-216.815248125819));
#217165=CARTESIAN_POINT('Ctrl Pts',(58.8564250713412,-60.1306000432421,
-216.815086531601));
#217166=CARTESIAN_POINT('Ctrl Pts',(58.8536063813388,-60.1346106864355,
-216.814922317271));
#217167=CARTESIAN_POINT('Ctrl Pts',(58.8507955332033,-60.1386111649472,
-216.814755482828));
#217168=CARTESIAN_POINT('Ctrl Pts',(58.8498585838248,-60.1399446577845,
-216.814699871346));
#217169=CARTESIAN_POINT('Ctrl Pts',(58.8480958402674,-60.1424537514167,
-216.814594297181));
#217170=CARTESIAN_POINT('Ctrl Pts',(58.847987294226,-60.1426082630128,-216.814587775013));
#217171=CARTESIAN_POINT('Ctrl Pts',(58.8468665099384,-60.1442036613052,
-216.81452043084));
#217172=CARTESIAN_POINT('Ctrl Pts',(58.8440935586267,-60.1480106610434,
-216.814434654858));
#217173=CARTESIAN_POINT('Ctrl Pts',(58.8396892604093,-60.1539873399552,
-216.814330447067));
#217174=CARTESIAN_POINT('Ctrl Pts',(58.8351105470343,-60.1602007020666,
-216.814222112531));
#217175=CARTESIAN_POINT('Ctrl Pts',(58.8287688656326,-60.1687588230416,
-216.81409385744));
#217176=CARTESIAN_POINT('Ctrl Pts',(58.8207128959423,-60.1795626343486,
-216.813945681793));
#217177=CARTESIAN_POINT('Ctrl Pts',(58.811869777269,-60.191422086306,-216.813783027901));
#217178=CARTESIAN_POINT('Ctrl Pts',(58.8009614040296,-60.2059870821187,
-216.813596370391));
#217179=CARTESIAN_POINT('Ctrl Pts',(58.7880784139399,-60.2230686165378,
-216.813385709263));
#217180=CARTESIAN_POINT('Ctrl Pts',(58.7710458173898,-60.2456521070313,
-216.813107194263));
#217181=CARTESIAN_POINT('Ctrl Pts',(58.7505644746547,-60.2726315580116,
-216.8127867222));
#217182=CARTESIAN_POINT('Ctrl Pts',(58.7268679369996,-60.3034884132764,
-216.812424293076));
#217183=CARTESIAN_POINT('Ctrl Pts',(58.7099212444828,-60.3255558412619,
-216.812165100149));
#217184=CARTESIAN_POINT('Ctrl Pts',(58.6913314136815,-60.3496032862428,
-216.811884448436));
#217185=CARTESIAN_POINT('Ctrl Pts',(58.6711668129565,-60.3754537841668,
-216.811582337935));
#217186=CARTESIAN_POINT('Ctrl Pts',(58.6631352792496,-60.3857500031817,
-216.811462007723));
#217187=CARTESIAN_POINT('Ctrl Pts',(58.6548536162727,-60.3963326193122,
-216.81133827325));
#217188=CARTESIAN_POINT('Ctrl Pts',(58.6463245735781,-60.4071924582901,
-216.811211134516));
#217189=CARTESIAN_POINT('Ctrl Pts',(62.1098409646983,-54.1012044962367,
-213.84767448904));
#217190=CARTESIAN_POINT('Ctrl Pts',(62.0847752059267,-54.0775469760354,
-215.334866061346));
#217191=CARTESIAN_POINT('Ctrl Pts',(61.2512793605065,-54.0263658558187,
-216.565923216592));
#217192=CARTESIAN_POINT('Ctrl Pts',(62.1058460411768,-54.2039809660857,
-213.849362952052));
#217193=CARTESIAN_POINT('Ctrl Pts',(62.0790252058314,-54.2159363746381,
-215.358533969393));
#217194=CARTESIAN_POINT('Ctrl Pts',(61.2229035024388,-54.1935258578861,
-216.601366064467));
#217195=CARTESIAN_POINT('Ctrl Pts',(62.1019433372586,-54.3058734208768,
-213.846873799599));
#217196=CARTESIAN_POINT('Ctrl Pts',(62.0728759814261,-54.3629917147794,
-215.384322257423));
#217197=CARTESIAN_POINT('Ctrl Pts',(61.1851466716199,-54.3765718104657,
-216.640959213404));
#217198=CARTESIAN_POINT('Ctrl Pts',(62.0951493333585,-54.4857552569347,
-213.835536336055));
#217199=CARTESIAN_POINT('Ctrl Pts',(62.062450771888,-54.6155445114012,-215.41819658183));
#217200=CARTESIAN_POINT('Ctrl Pts',(61.1204223943136,-54.6858014957792,
-216.694930502363));
#217201=CARTESIAN_POINT('Ctrl Pts',(62.0922232746455,-54.5640610712165,
-213.828298048138));
#217202=CARTESIAN_POINT('Ctrl Pts',(62.058075754172,-54.7227158315903,-215.428854453095));
#217203=CARTESIAN_POINT('Ctrl Pts',(61.0933565049856,-54.8149488052244,
-216.712883469383));
#217204=CARTESIAN_POINT('Ctrl Pts',(62.0827290302579,-54.8200529665633,
-213.798945603707));
#217205=CARTESIAN_POINT('Ctrl Pts',(62.0441877755472,-55.0659530526541,
-215.453222968095));
#217206=CARTESIAN_POINT('Ctrl Pts',(61.0091373101189,-55.2224505676427,
-216.757651828807));
#217207=CARTESIAN_POINT('Ctrl Pts',(62.076302448301,-54.9963150897595,-213.769847381886));
#217208=CARTESIAN_POINT('Ctrl Pts',(62.0350662400492,-55.2949984649606,
-215.456884065042));
#217209=CARTESIAN_POINT('Ctrl Pts',(60.9535367563429,-55.4889120684891,
-216.77161448955));
#217210=CARTESIAN_POINT('Ctrl Pts',(62.0700163106713,-55.1711147821028,
-213.733564105162));
#217211=CARTESIAN_POINT('Ctrl Pts',(62.0256791069586,-55.5302233529213,
-215.457837347772));
#217212=CARTESIAN_POINT('Ctrl Pts',(60.8876885241678,-55.7663600659722,
-216.781995879541));
#217213=CARTESIAN_POINT('',(61.2313176176752,-54.1392424392486,-216.589725631893));
#217214=CARTESIAN_POINT('',(62.1072060041622,-54.1692103455281,-213.848185004792));
#217215=CARTESIAN_POINT('Origin',(57.1116967348753,-53.976149530741,-213.760922972606));
#217216=CARTESIAN_POINT('Ctrl Pts',(62.072365351932,-55.1059089910533,-213.746749287634));
#217217=CARTESIAN_POINT('Ctrl Pts',(62.0768793934982,-54.9808272265131,
-213.771366922161));
#217218=CARTESIAN_POINT('Ctrl Pts',(62.0814562559799,-54.8552883750893,
-213.792161075658));
#217219=CARTESIAN_POINT('Ctrl Pts',(62.0861030190974,-54.7293175780445,
-213.808641588953));
#217220=CARTESIAN_POINT('Ctrl Pts',(62.0871755724076,-54.7002413389646,
-213.812445576512));
#217221=CARTESIAN_POINT('Ctrl Pts',(62.088251845208,-54.6711421307964,-213.816019960792));
#217222=CARTESIAN_POINT('Ctrl Pts',(62.0893319159673,-54.6420203440083,
-213.819359111929));
#217223=CARTESIAN_POINT('Ctrl Pts',(62.0922302587967,-54.5638727585909,
-213.828319640368));
#217224=CARTESIAN_POINT('Ctrl Pts',(62.0951568916034,-54.4855551406274,
-213.835548948843));
#217225=CARTESIAN_POINT('Ctrl Pts',(62.0981243813907,-54.4069862261454,
-213.840500934119));
#217226=CARTESIAN_POINT('Ctrl Pts',(62.1011078230656,-54.3279949605924,
-213.845479539036));
#217227=CARTESIAN_POINT('Ctrl Pts',(62.1041343851103,-54.2487398377214,
-213.848073534587));
#217228=CARTESIAN_POINT('Ctrl Pts',(62.1072060041623,-54.1692103455281,
-213.848185004792));
#217229=CARTESIAN_POINT('Ctrl Pts',(61.2313176176752,-54.1392424392486,
-216.589725631893));
#217230=CARTESIAN_POINT('Ctrl Pts',(61.2129639729121,-54.2384590041938,
-216.610734004428));
#217231=CARTESIAN_POINT('Ctrl Pts',(61.1963872015487,-54.3223059115667,
-216.627485554306));
#217232=CARTESIAN_POINT('Ctrl Pts',(61.1768147446742,-54.4186192835125,
-216.64622764514));
#217233=CARTESIAN_POINT('Ctrl Pts',(61.1711748801229,-54.4458286746357,
-216.651410803087));
#217234=CARTESIAN_POINT('Ctrl Pts',(61.1643153908603,-54.4787172038371,
-216.657589231512));
#217235=CARTESIAN_POINT('Ctrl Pts',(61.1612845711754,-54.4931830366251,
-216.660279368601));
#217236=CARTESIAN_POINT('Ctrl Pts',(61.158491861122,-54.5065045129988,-216.662719476904));
#217237=CARTESIAN_POINT('Ctrl Pts',(61.157285649663,-54.51226760884,-216.663764934813));
#217238=CARTESIAN_POINT('Ctrl Pts',(61.1568098734461,-54.5145442864167,
-216.664175574723));
#217239=CARTESIAN_POINT('Ctrl Pts',(61.1565018821742,-54.5160190449251,
-216.664441020556));
#217240=CARTESIAN_POINT('Ctrl Pts',(61.1566637740706,-54.5152420950941,
-216.664302098725));
#217241=CARTESIAN_POINT('Ctrl Pts',(61.1416133774214,-54.5874172342758,
-216.677234683339));
#217242=CARTESIAN_POINT('Ctrl Pts',(61.1274208796436,-54.6546260509771,
-216.68825404635));
#217243=CARTESIAN_POINT('Ctrl Pts',(61.1005609955658,-54.7818940695041,
-216.707250122171));
#217244=CARTESIAN_POINT('Ctrl Pts',(61.0876513362582,-54.8431501608505,
-216.71536360823));
#217245=CARTESIAN_POINT('Ctrl Pts',(61.031332251096,-55.115600279193,-216.746956680543));
#217246=CARTESIAN_POINT('Ctrl Pts',(60.9789434732668,-55.3729747777418,
-216.765652701273));
#217247=CARTESIAN_POINT('Ctrl Pts',(60.9119170756758,-55.6633990141858,
-216.777770284882));
#217248=CARTESIAN_POINT('Ctrl Pts',(61.2313176176758,-54.1392424392492,
-216.589725631893));
#217249=CARTESIAN_POINT('Ctrl Pts',(62.080918261728,-54.1703109655354,-215.35065029375));
#217250=CARTESIAN_POINT('Ctrl Pts',(62.1072060041624,-54.1692103455281,
-213.848185004792));
#217251=CARTESIAN_POINT('Ctrl Pts',(61.3352033242247,-51.5493321211752,
-216.587755286045));
#217252=CARTESIAN_POINT('Ctrl Pts',(62.1810780798069,-51.5788094394057,
-215.35057926127));
#217253=CARTESIAN_POINT('Ctrl Pts',(62.2073146990362,-51.5772242306454,
-213.851818178003));
#217254=CARTESIAN_POINT('Ctrl Pts',(61.4293178843645,-48.9588621990231,
-216.585940879273));
#217255=CARTESIAN_POINT('Ctrl Pts',(62.2718155001796,-48.9862078816508,
-215.350513478332));
#217256=CARTESIAN_POINT('Ctrl Pts',(62.2979780119688,-48.9848138223875,
-213.855140923936));
#217257=CARTESIAN_POINT('Ctrl Pts',(61.5136373793521,-46.3682170785133,
-216.584262774589));
#217258=CARTESIAN_POINT('Ctrl Pts',(62.3531001006731,-46.3930946875274,
-215.350420378609));
#217259=CARTESIAN_POINT('Ctrl Pts',(62.3791894693652,-46.3921971636372,
-213.85810601718));
#217260=CARTESIAN_POINT('',(61.7446212189112,-46.4961938534599,-216.203488006702));
#217261=CARTESIAN_POINT('',(62.3685680449238,-46.7295402395978,-213.85775323375));
#217262=CARTESIAN_POINT('Ctrl Pts',(61.744621222757,-46.4961938535833,-216.203488008845));
#217263=CARTESIAN_POINT('Ctrl Pts',(61.823821619514,-46.5121026275102,-216.060434887725));
#217264=CARTESIAN_POINT('Ctrl Pts',(61.9058788067412,-46.5300994083013,
-215.895819447354));
#217265=CARTESIAN_POINT('Ctrl Pts',(62.0235044292652,-46.5599185298986,
-215.613803489315));
#217266=CARTESIAN_POINT('Ctrl Pts',(62.0617695753442,-46.5703278495255,
-215.513967395468));
#217267=CARTESIAN_POINT('Ctrl Pts',(62.1162526519497,-46.586598946888,-215.355377457539));
#217268=CARTESIAN_POINT('Ctrl Pts',(62.1427627631244,-46.5948986888364,
-215.273876942239));
#217269=CARTESIAN_POINT('Ctrl Pts',(62.1720569338811,-46.6048578961246,
-215.174955056835));
#217270=CARTESIAN_POINT('Ctrl Pts',(62.1862495019753,-46.6099050968833,
-215.124540908492));
#217271=CARTESIAN_POINT('Ctrl Pts',(62.1922296880582,-46.6120825122955,
-215.10273136339));
#217272=CARTESIAN_POINT('Ctrl Pts',(62.1961931824135,-46.6135372894546,
-215.088146545192));
#217273=CARTESIAN_POINT('Ctrl Pts',(62.1984567548069,-46.614375749181,-215.07973190005));
#217274=CARTESIAN_POINT('Ctrl Pts',(62.3066601348565,-46.6547437913238,
-214.674282540586));
#217275=CARTESIAN_POINT('Ctrl Pts',(62.3626521870614,-46.692922721645,-214.26279861847));
#217276=CARTESIAN_POINT('Ctrl Pts',(62.3685682383788,-46.7295544375158,
-213.857742675887));
#217277=CARTESIAN_POINT('Origin',(-1003.27568749664,-12.9672887026865,-175.207747633911));
#217278=CARTESIAN_POINT('',(61.5121276274299,-46.4145707938174,-216.584292818064));
#217279=CARTESIAN_POINT('Origin',(-967.127514096642,-12.8777453687604,-231.930774818293));
#217280=CARTESIAN_POINT('Origin',(59.4886098259839,-41.5000831614117,-215.164704043177));
#217281=CARTESIAN_POINT('Ctrl Pts',(61.6670578759491,-45.7769853366197,
-216.220244871724));
#217282=CARTESIAN_POINT('Ctrl Pts',(61.620109783049,-46.0863015287385,-216.444037055829));
#217283=CARTESIAN_POINT('Ctrl Pts',(61.4891978237332,-46.4033111269098,
-216.618195686949));
#217284=CARTESIAN_POINT('Ctrl Pts',(61.7028325176855,-45.8210961670719,
-216.166526245294));
#217285=CARTESIAN_POINT('Ctrl Pts',(61.6781627682026,-46.1318587895498,
-216.346038562299));
#217286=CARTESIAN_POINT('Ctrl Pts',(61.5806679860909,-46.4492865503325,
-216.484073286616));
#217287=CARTESIAN_POINT('Ctrl Pts',(61.7397430092403,-45.8565257688032,
-216.106843396371));
#217288=CARTESIAN_POINT('Ctrl Pts',(61.7393332826304,-46.1679717108974,
-216.237169913932));
#217289=CARTESIAN_POINT('Ctrl Pts',(61.674934118594,-46.4851009680931,-216.332569263343));
#217290=CARTESIAN_POINT('Ctrl Pts',(61.7761254129207,-45.8740236618143,
-216.040906882924));
#217291=CARTESIAN_POINT('Ctrl Pts',(61.8021587798992,-46.1846331282861,
-216.116674563313));
#217292=CARTESIAN_POINT('Ctrl Pts',(61.7678808137169,-46.5004734283573,
-216.161019659926));
#217293=CARTESIAN_POINT('',(61.7670326019138,-45.86927832895,-216.057267272101));
#217294=CARTESIAN_POINT('',(61.6760242364037,-45.7878268313144,-216.206690793879));
#217295=CARTESIAN_POINT('Ctrl Pts',(61.7670197730419,-45.8692809645528,
-216.057260894207));
#217296=CARTESIAN_POINT('Ctrl Pts',(61.7550845763212,-45.8625955283723,
-216.078505375557));
#217297=CARTESIAN_POINT('Ctrl Pts',(61.7431797213835,-45.854115763207,-216.09895572692));
#217298=CARTESIAN_POINT('Ctrl Pts',(61.7313327680375,-45.8441875378893,
-216.118692871638));
#217299=CARTESIAN_POINT('Ctrl Pts',(61.7181196261084,-45.8331143913684,
-216.140706100425));
#217300=CARTESIAN_POINT('Ctrl Pts',(61.7049782714986,-45.8202388908385,
-216.161832418214));
#217301=CARTESIAN_POINT('Ctrl Pts',(61.691944051632,-45.8059771378073,-216.182163997265));
#217302=CARTESIAN_POINT('Ctrl Pts',(61.6866187535004,-45.8001503152166,
-216.190470725327));
#217303=CARTESIAN_POINT('Ctrl Pts',(61.6813113300833,-45.7940914684588,
-216.198644553705));
#217304=CARTESIAN_POINT('Ctrl Pts',(61.6760242364037,-45.7878268313144,
-216.206690793879));
#217305=CARTESIAN_POINT('Origin',(59.1250215884199,-46.412156871143,-214.743818340268));
#217306=CARTESIAN_POINT('Origin',(59.0334256450291,-46.3348777618666,-214.896191665971));
#217307=CARTESIAN_POINT('Ctrl Pts',(61.7670197730426,-45.8692809645531,
-216.057260894206));
#217308=CARTESIAN_POINT('Ctrl Pts',(61.7864942538559,-46.1800624966811,
-216.146540979352));
#217309=CARTESIAN_POINT('Ctrl Pts',(61.744621222757,-46.4961938535834,-216.203488008845));
#217310=CARTESIAN_POINT('Ctrl Pts',(61.9631621369174,-46.0106807568515,
-215.721163036308));
#217311=CARTESIAN_POINT('Ctrl Pts',(61.9754348687076,-46.2721634433876,
-215.791058678043));
#217312=CARTESIAN_POINT('Ctrl Pts',(61.9444015484922,-46.5363231985591,
-215.842641422359));
#217313=CARTESIAN_POINT('Ctrl Pts',(62.1106980495454,-46.1537572969976,
-215.368567684276));
#217314=CARTESIAN_POINT('Ctrl Pts',(62.1171497321372,-46.3642951884269,
-215.421651993854));
#217315=CARTESIAN_POINT('Ctrl Pts',(62.0956418404433,-46.5759866556878,
-215.465343832486));
#217316=CARTESIAN_POINT('Ctrl Pts',(62.3127271221,-46.4421422876624,-214.631724106531));
#217317=CARTESIAN_POINT('Ctrl Pts',(62.3119048875977,-46.5481874588022,
-214.656051542736));
#217318=CARTESIAN_POINT('Ctrl Pts',(62.3051790602976,-46.6542226656792,
-214.679477777819));
#217319=CARTESIAN_POINT('Ctrl Pts',(62.3662837353377,-46.5885519083916,
-214.24418481767));
#217320=CARTESIAN_POINT('Ctrl Pts',(62.3644265280729,-46.6408054190759,
-214.25579858017));
#217321=CARTESIAN_POINT('Ctrl Pts',(62.3625689806341,-46.6930535773299,
-214.267441525086));
#217322=CARTESIAN_POINT('Ctrl Pts',(62.3685685933127,-46.7295566356152,
-213.857718370431));
#217323=CARTESIAN_POINT('Ctrl Pts',(62.3685685933127,-46.7295566356152,
-213.857718370431));
#217324=CARTESIAN_POINT('Ctrl Pts',(62.3685685933127,-46.7295566356152,
-213.857718370431));
#217325=CARTESIAN_POINT('Ctrl Pts',(61.7670326019138,-45.86927832895,-216.057267272101));
#217326=CARTESIAN_POINT('Ctrl Pts',(61.8196450544845,-45.9072070747506,
-215.96711325074));
#217327=CARTESIAN_POINT('Ctrl Pts',(61.8687216511235,-45.9452722675006,
-215.875738558968));
#217328=CARTESIAN_POINT('Ctrl Pts',(61.9143495212748,-45.9834416652426,
-215.783201258363));
#217329=CARTESIAN_POINT('Ctrl Pts',(61.9604188031332,-46.0219803201725,
-215.689768736313));
#217330=CARTESIAN_POINT('Ctrl Pts',(62.0029730973334,-46.0606255964866,
-215.595150355294));
#217331=CARTESIAN_POINT('Ctrl Pts',(62.0420704302675,-46.099363287737,-215.499366831777));
#217332=CARTESIAN_POINT('Ctrl Pts',(62.081415222604,-46.1383461621038,-215.402977064004));
#217333=CARTESIAN_POINT('Ctrl Pts',(62.1172597709746,-46.177423080767,-215.305406534752));
#217334=CARTESIAN_POINT('Ctrl Pts',(62.1496206711299,-46.2165922631161,
-215.206648172333));
#217335=CARTESIAN_POINT('Ctrl Pts',(62.1719889253612,-46.2436664861635,
-215.138385171383));
#217336=CARTESIAN_POINT('Ctrl Pts',(62.1926918700032,-46.2707850609034,
-215.069554047601));
#217337=CARTESIAN_POINT('Ctrl Pts',(62.2117212103626,-46.2979491248436,
-215.000147998789));
#217338=CARTESIAN_POINT('Ctrl Pts',(62.2374034026224,-46.3346100231978,
-214.906476885869));
#217339=CARTESIAN_POINT('Ctrl Pts',(62.2600776278325,-46.3714179102784,
-214.811587750487));
#217340=CARTESIAN_POINT('Ctrl Pts',(62.2796089098324,-46.4082437749361,
-214.71578939826));
#217341=CARTESIAN_POINT('Ctrl Pts',(62.2991036321638,-46.4450007070266,
-214.620170366368));
#217342=CARTESIAN_POINT('Ctrl Pts',(62.3154669417998,-46.4817752829743,
-214.523646019044));
#217343=CARTESIAN_POINT('Ctrl Pts',(62.3286125540718,-46.5184396641695,
-214.426543203837));
#217344=CARTESIAN_POINT('Ctrl Pts',(62.3417577176969,-46.555102794045,-214.329443702654));
#217345=CARTESIAN_POINT('Ctrl Pts',(62.3516852860051,-46.5916554724708,
-214.231766313919));
#217346=CARTESIAN_POINT('Ctrl Pts',(62.3583595568947,-46.6279743143229,
-214.133849819246));
#217347=CARTESIAN_POINT('Ctrl Pts',(62.3646248451903,-46.6620676285631,
-214.041933401983));
#217348=CARTESIAN_POINT('Ctrl Pts',(62.3680237825966,-46.6959547578441,
-213.949806767614));
#217349=CARTESIAN_POINT('Ctrl Pts',(62.3685680449238,-46.7295402395978,
-213.85775323375));
#217350=CARTESIAN_POINT('Ctrl Pts',(62.3422326083537,21.4655488148376,-214.137178092368));
#217351=CARTESIAN_POINT('Ctrl Pts',(62.3412085237329,20.8691191735829,-215.298600946727));
#217352=CARTESIAN_POINT('Ctrl Pts',(61.7024165239503,20.3282348619418,-216.300609606759));
#217353=CARTESIAN_POINT('Ctrl Pts',(62.3680533687935,20.8390832881022,-213.816997587882));
#217354=CARTESIAN_POINT('Ctrl Pts',(62.3638965167735,20.3074474023936,-215.017927985833));
#217355=CARTESIAN_POINT('Ctrl Pts',(61.7172757020854,19.824196871917,-216.053279622787));
#217356=CARTESIAN_POINT('Ctrl Pts',(62.3936763768326,20.1737977939208,-213.547199312721));
#217357=CARTESIAN_POINT('Ctrl Pts',(62.3866033956745,19.7050928579686,-214.784132304911));
#217358=CARTESIAN_POINT('Ctrl Pts',(61.7283519101567,19.2781211138106,-215.848545883872));
#217359=CARTESIAN_POINT('Ctrl Pts',(62.4421294023084,18.8292102512288,-213.116884807332));
#217360=CARTESIAN_POINT('Ctrl Pts',(62.4297715597234,18.480223357531,-214.418244849069));
#217361=CARTESIAN_POINT('Ctrl Pts',(61.7440121152497,18.1590865773314,-215.532301635935));
#217362=CARTESIAN_POINT('Ctrl Pts',(62.465140608479,18.1462075363528,-212.953486548188));
#217363=CARTESIAN_POINT('Ctrl Pts',(62.4504011796583,17.8540628328224,-214.283557758829));
#217364=CARTESIAN_POINT('Ctrl Pts',(61.7487288909466,17.58324508504,-215.418454515118));
#217365=CARTESIAN_POINT('Ctrl Pts',(62.5088056235126,16.7621631730818,-212.713827714098));
#217366=CARTESIAN_POINT('Ctrl Pts',(62.4897025499552,16.5802648276791,-214.096157268913));
#217367=CARTESIAN_POINT('Ctrl Pts',(61.7533580267159,16.4056510722738,-215.266990172273));
#217368=CARTESIAN_POINT('Ctrl Pts',(62.5294585302,16.0610980086273,-212.637681074457));
#217369=CARTESIAN_POINT('Ctrl Pts',(62.5083765259719,15.9323648740618,-214.043664436094));
#217370=CARTESIAN_POINT('Ctrl Pts',(61.7532369224541,15.8039519787059,-215.229498767323));
#217371=CARTESIAN_POINT('Ctrl Pts',(62.568416048291,14.6428357290655,-212.563275779244));
#217372=CARTESIAN_POINT('Ctrl Pts',(62.5437053983983,14.6184979888445,-214.012589278034));
#217373=CARTESIAN_POINT('Ctrl Pts',(61.7487163900049,14.5792839170071,-215.224013067664));
#217374=CARTESIAN_POINT('Ctrl Pts',(62.5864410346862,13.9358240577698,-212.565541839207));
#217375=CARTESIAN_POINT('Ctrl Pts',(62.5601079803605,13.9617491203001,-214.034345816612));
#217376=CARTESIAN_POINT('Ctrl Pts',(61.7443571097689,13.9650597457188,-215.256029021813));
#217377=CARTESIAN_POINT('Ctrl Pts',(62.6364325628104,11.8237195743705,-212.673714044577));
#217378=CARTESIAN_POINT('Ctrl Pts',(62.6057492551312,11.9950165428146,-214.195845570981));
#217379=CARTESIAN_POINT('Ctrl Pts',(61.7256266748608,12.1232209481819,-215.442654533669));
#217380=CARTESIAN_POINT('Ctrl Pts',(62.6643973443486,10.4250272317226,-212.879944055009));
#217381=CARTESIAN_POINT('Ctrl Pts',(62.6313772356455,10.6897808013045,-214.431496688937));
#217382=CARTESIAN_POINT('Ctrl Pts',(61.7057160584319,10.8942002544619,-215.687059023784));
#217383=CARTESIAN_POINT('Ctrl Pts',(62.6882099634729,8.99324453840434,-213.207737243319));
#217384=CARTESIAN_POINT('Ctrl Pts',(62.6531941668671,9.35784434440792,-214.783414534773));
#217385=CARTESIAN_POINT('Ctrl Pts',(61.6775843047233,9.63385243594079,-216.04393851968));
#217386=CARTESIAN_POINT('Ctrl Pts',(62.6889267575668,8.94986797085776,-213.217780919801));
#217387=CARTESIAN_POINT('Ctrl Pts',(62.6538525956858,9.31739109066463,-214.794211638116));
#217388=CARTESIAN_POINT('Ctrl Pts',(61.676724484433,9.59566774192812,-216.054853410616));
#217389=CARTESIAN_POINT('Ctrl Pts',(62.6899947648924,8.88481924519104,-213.233011700935));
#217390=CARTESIAN_POINT('Ctrl Pts',(62.6548336726685,9.25672938439221,-214.810565067534));
#217391=CARTESIAN_POINT('Ctrl Pts',(61.6754236852739,9.53840185263947,-216.071375999175));
#217392=CARTESIAN_POINT('Ctrl Pts',(62.6903499578519,8.86313707307649,-213.238096257503));
#217393=CARTESIAN_POINT('Ctrl Pts',(62.6552786040791,9.23183909531466,-214.814707920553));
#217394=CARTESIAN_POINT('Ctrl Pts',(61.6776818994437,9.51109461514074,-216.07534089488));
#217395=CARTESIAN_POINT('Ctrl Pts',(62.6910610727136,8.81976237959028,-213.248159965146));
#217396=CARTESIAN_POINT('Ctrl Pts',(62.6561013689098,9.18470089827482,-214.823639829792));
#217397=CARTESIAN_POINT('Ctrl Pts',(61.6806556143609,9.46114018087874,-216.084046497709));
#217398=CARTESIAN_POINT('Ctrl Pts',(62.6914166532021,8.79807157636304,-213.253156652719));
#217399=CARTESIAN_POINT('Ctrl Pts',(62.6565126981162,9.16112631942749,-214.82807085154));
#217400=CARTESIAN_POINT('Ctrl Pts',(61.6821392223453,9.43615432575777,-216.088363130015));
#217401=CARTESIAN_POINT('Ctrl Pts',(62.693194685499,8.68960018849763,-213.277963347887));
#217402=CARTESIAN_POINT('Ctrl Pts',(62.658568741826,9.04324596366052,-214.850046563724));
#217403=CARTESIAN_POINT('Ctrl Pts',(61.6895409461648,9.31118142695972,-216.109764509573));
#217404=CARTESIAN_POINT('Ctrl Pts',(62.6946175261465,8.60276749258736,-213.297243169367));
#217405=CARTESIAN_POINT('Ctrl Pts',(62.6602130641221,8.94883672773494,-214.867068548325));
#217406=CARTESIAN_POINT('Ctrl Pts',(61.6954101007806,9.21106386992964,-216.126303896624));
#217407=CARTESIAN_POINT('Ctrl Pts',(62.6988878681185,8.34209912341666,-213.353350073391));
#217408=CARTESIAN_POINT('Ctrl Pts',(62.665143127837,8.66539857132349,-214.916400103904));
#217409=CARTESIAN_POINT('Ctrl Pts',(61.7128578780018,8.91027943593482,-216.174139388407));
#217410=CARTESIAN_POINT('Ctrl Pts',(62.7017371797686,8.16809322423106,-213.388445162621));
#217411=CARTESIAN_POINT('Ctrl Pts',(62.6684282615003,8.47602746148447,-214.947001892893));
#217412=CARTESIAN_POINT('Ctrl Pts',(61.724276890348,8.70918150967842,-216.203653357584));
#217413=CARTESIAN_POINT('Ctrl Pts',(62.7102973061953,7.64536444866494,-213.486494648388));
#217414=CARTESIAN_POINT('Ctrl Pts',(62.6782774788102,7.90698464843204,-215.031562829203));
#217415=CARTESIAN_POINT('Ctrl Pts',(61.7578672711065,8.10404764104899,-216.284743705441));
#217416=CARTESIAN_POINT('Ctrl Pts',(62.7160201318226,7.29593153216955,-213.542223849032));
#217417=CARTESIAN_POINT('Ctrl Pts',(62.684844443005,7.52585577339385,-215.078390952383));
#217418=CARTESIAN_POINT('Ctrl Pts',(61.7793738539193,7.69817704538221,-216.328880163446));
#217419=CARTESIAN_POINT('Ctrl Pts',(62.7332823333847,6.24451635056923,-213.677692349319));
#217420=CARTESIAN_POINT('Ctrl Pts',(62.7045693598837,6.37797772727193,-215.187097629475));
#217421=CARTESIAN_POINT('Ctrl Pts',(61.8409395976697,6.47220794885748,-216.42854185076));
#217422=CARTESIAN_POINT('Ctrl Pts',(62.7449139403618,5.53942734608012,-213.725811404425));
#217423=CARTESIAN_POINT('Ctrl Pts',(62.7177658905222,5.6055034086315,-215.217916782497));
#217424=CARTESIAN_POINT('Ctrl Pts',(61.8776376267353,5.64552562952192,-216.451762661138));
#217425=CARTESIAN_POINT('Ctrl Pts',(62.7627331655823,4.47441539748971,-213.722866226851));
#217426=CARTESIAN_POINT('Ctrl Pts',(62.7377858408184,4.43512030427846,-215.189372776564));
#217427=CARTESIAN_POINT('Ctrl Pts',(61.9246048946113,4.38883323215275,-216.409638751896));
#217428=CARTESIAN_POINT('Ctrl Pts',(62.7687354860423,4.11817803008359,-213.709326696013));
#217429=CARTESIAN_POINT('Ctrl Pts',(62.7444894112431,4.04343699957454,-215.167470850043));
#217430=CARTESIAN_POINT('Ctrl Pts',(61.9388297011265,3.96768865050412,-216.38283829128));
#217431=CARTESIAN_POINT('Ctrl Pts',(62.7808960763514,3.40303826436503,-213.655109821484));
#217432=CARTESIAN_POINT('Ctrl Pts',(62.7579914493339,3.25632764876865,-215.096816607535));
#217433=CARTESIAN_POINT('Ctrl Pts',(61.9642060846595,3.12029037299094,-216.301632685202));
#217434=CARTESIAN_POINT('Ctrl Pts',(62.7870578417518,3.04396622992889,-213.614329768932));
#217435=CARTESIAN_POINT('Ctrl Pts',(62.764798254127,2.86044742865292,-215.047932027892));
#217436=CARTESIAN_POINT('Ctrl Pts',(61.9753669262453,2.69358808816948,-216.247065417161));
#217437=CARTESIAN_POINT('Ctrl Pts',(62.7994785535875,2.32831168170424,-213.504372226852));
#217438=CARTESIAN_POINT('Ctrl Pts',(62.7784280077131,2.07098012791206,-214.922299288837));
#217439=CARTESIAN_POINT('Ctrl Pts',(61.9941529245256,1.84204963832674,-216.109426235826));
#217440=CARTESIAN_POINT('Ctrl Pts',(62.8057475169848,1.97109323824117,-213.43520790963));
#217441=CARTESIAN_POINT('Ctrl Pts',(62.7852637475919,1.67660733927831,-214.845546681094));
#217442=CARTESIAN_POINT('Ctrl Pts',(62.0018065488482,1.41657236335453,-216.026373118398));
#217443=CARTESIAN_POINT('Ctrl Pts',(62.8136699413683,1.52535840970665,-213.330389729488));
#217444=CARTESIAN_POINT('Ctrl Pts',(62.7938456712648,1.18416909955933,-214.731582640628));
#217445=CARTESIAN_POINT('Ctrl Pts',(62.0091417138508,0.88496462984438,-215.904115945249));
#217446=CARTESIAN_POINT('Ctrl Pts',(62.8152587437295,1.43625087081009,-213.308507593617));
#217447=CARTESIAN_POINT('Ctrl Pts',(62.7955641544421,1.08569455170218,-214.70788534455));
#217448=CARTESIAN_POINT('Ctrl Pts',(62.0104970411636,0.778654812026788,
-215.878741948443));
#217449=CARTESIAN_POINT('Ctrl Pts',(62.81764868783,1.3026492637952,-213.274293620792));
#217450=CARTESIAN_POINT('Ctrl Pts',(62.7981450769487,0.938013811545139,
-214.670972759063));
#217451=CARTESIAN_POINT('Ctrl Pts',(62.0123610115366,0.619204373827452,
-215.839283178847));
#217452=CARTESIAN_POINT('Ctrl Pts',(62.8184464593903,1.25812534522924,-213.262657162745));
#217453=CARTESIAN_POINT('Ctrl Pts',(62.7990059459185,0.888790452628964,
-214.658440360413));
#217454=CARTESIAN_POINT('Ctrl Pts',(62.0129541628601,0.566056612067846,
-215.825897286883));
#217455=CARTESIAN_POINT('Ctrl Pts',(62.8194451065877,1.20248294550228,-213.247820438255));
#217456=CARTESIAN_POINT('Ctrl Pts',(62.8000827277237,0.827267573996727,
-214.642488734758));
#217457=CARTESIAN_POINT('Ctrl Pts',(62.0136602192421,0.499624509372178,
-215.808872193624));
#217458=CARTESIAN_POINT('Ctrl Pts',(62.8196449076661,1.19135509048132,-213.24483853566));
#217459=CARTESIAN_POINT('Ctrl Pts',(62.8002981228947,0.814963083819151,
-214.639284042805));
#217460=CARTESIAN_POINT('Ctrl Pts',(62.0137996613151,0.486338219736283,
-215.805452538661));
#217461=CARTESIAN_POINT('Ctrl Pts',(62.8200446538203,1.16910063183232,-213.238845579474));
#217462=CARTESIAN_POINT('Ctrl Pts',(62.8007289854141,0.790354624727844,
-214.632845981801));
#217463=CARTESIAN_POINT('Ctrl Pts',(62.0140750027388,0.45976589102507,-215.798583917059));
#217464=CARTESIAN_POINT('Ctrl Pts',(62.8202446769491,1.15797422719196,-213.235829903834));
#217465=CARTESIAN_POINT('Ctrl Pts',(62.8009680223541,0.776644373992607,
-214.629327854389));
#217466=CARTESIAN_POINT('Ctrl Pts',(62.0141560873609,0.443889927808329,
-215.794583971007));
#217467=CARTESIAN_POINT('Ctrl Pts',(62.8208444503325,1.12459558460624,-213.226769479739));
#217468=CARTESIAN_POINT('Ctrl Pts',(62.8015104527899,0.745946623824953,
-214.620839027899));
#217469=CARTESIAN_POINT('Ctrl Pts',(62.0148004761842,0.41547430450863,-215.786623443142));
#217470=CARTESIAN_POINT('Ctrl Pts',(62.8212428505405,1.102341230911,-213.22077375003));
#217471=CARTESIAN_POINT('Ctrl Pts',(62.8018707964773,0.725477633258065,
-214.615222311207));
#217472=CARTESIAN_POINT('Ctrl Pts',(62.0152269887982,0.396525463221588,
-215.781356665904));
#217473=CARTESIAN_POINT('Ctrl Pts',(62.8248154365303,0.902034785229426,
-213.167211635172));
#217474=CARTESIAN_POINT('Ctrl Pts',(62.805102284956,0.541229956352993,-214.565055000306));
#217475=CARTESIAN_POINT('Ctrl Pts',(62.0190380353134,0.225940477598872,
-215.734316604759));
#217476=CARTESIAN_POINT('Ctrl Pts',(62.8278985261067,0.72386189685476,-213.122440498364));
#217477=CARTESIAN_POINT('Ctrl Pts',(62.8078932046147,0.377207549051993,
-214.523169982245));
#217478=CARTESIAN_POINT('Ctrl Pts',(62.0222296924439,0.0739868204750567,
-215.695069192559));
#217479=CARTESIAN_POINT('Ctrl Pts',(62.8548240427874,-0.880767445010574,
-212.744334484548));
#217480=CARTESIAN_POINT('Ctrl Pts',(62.8322777445444,-1.10067369440056,
-214.170022992711));
#217481=CARTESIAN_POINT('Ctrl Pts',(62.0492626355665,-1.29628340734911,
-215.364351700278));
#217482=CARTESIAN_POINT('Ctrl Pts',(62.8729565843244,-2.31461725004268,
-212.582049783317));
#217483=CARTESIAN_POINT('Ctrl Pts',(62.8488210432101,-2.42949334313602,
-214.022238296534));
#217484=CARTESIAN_POINT('Ctrl Pts',(62.0615715076119,-2.53314160129442,
-215.228142992244));
#217485=CARTESIAN_POINT('Ctrl Pts',(62.8981414605001,-5.19559191584348,
-212.564399664962));
#217486=CARTESIAN_POINT('Ctrl Pts',(62.8718519000548,-5.1001878562054,-214.022587242802));
#217487=CARTESIAN_POINT('Ctrl Pts',(62.0663646755723,-5.02417617024219,
-215.238634491797));
#217488=CARTESIAN_POINT('Ctrl Pts',(62.9051900334741,-6.64273030664321,
-212.709348944425));
#217489=CARTESIAN_POINT('Ctrl Pts',(62.8783440818401,-6.44396797060244,
-214.171257323535));
#217490=CARTESIAN_POINT('Ctrl Pts',(62.0588087843662,-6.27849882636757,
-215.385574614432));
#217491=CARTESIAN_POINT('Ctrl Pts',(62.9066422728629,-8.27861416050181,
-213.053996708501));
#217492=CARTESIAN_POINT('Ctrl Pts',(62.8797610895578,-7.95625364053062,
-214.512708735063));
#217493=CARTESIAN_POINT('Ctrl Pts',(62.0376955265922,-7.69029576577868,
-215.717956609814));
#217494=CARTESIAN_POINT('Ctrl Pts',(62.9067130375752,-8.46050513615589,
-213.09485254092));
#217495=CARTESIAN_POINT('Ctrl Pts',(62.8798363892243,-8.12450410435317,
-214.553151196536));
#217496=CARTESIAN_POINT('Ctrl Pts',(62.0351702942178,-7.84718504561344,
-215.757241843704));
#217497=CARTESIAN_POINT('Ctrl Pts',(62.9066818269245,-8.7334636680148,-213.160032454394));
#217498=CARTESIAN_POINT('Ctrl Pts',(62.8798247003438,-8.37686367832318,
-214.617556180156));
#217499=CARTESIAN_POINT('Ctrl Pts',(62.0311058209299,-8.08247086921434,
-215.819744443959));
#217500=CARTESIAN_POINT('Ctrl Pts',(62.9066485485958,-8.82432470155739,
-213.182373733743));
#217501=CARTESIAN_POINT('Ctrl Pts',(62.8798000295548,-8.46085638262443,
-214.639616572718));
#217502=CARTESIAN_POINT('Ctrl Pts',(62.0297070531108,-8.16076599954354,
-215.841141115965));
#217503=CARTESIAN_POINT('Ctrl Pts',(62.9065784769814,-8.9377445621295,-213.211068643959));
#217504=CARTESIAN_POINT('Ctrl Pts',(62.879743353183,-8.56567236571989,-214.66792785609));
#217505=CARTESIAN_POINT('Ctrl Pts',(62.0279032485469,-8.25846566363754,
-215.868589453836));
#217506=CARTESIAN_POINT('Ctrl Pts',(62.9065630389366,-8.96042071227823,
-213.21684604351));
#217507=CARTESIAN_POINT('Ctrl Pts',(62.8797307248969,-8.58662834582749,
-214.673627324421));
#217508=CARTESIAN_POINT('Ctrl Pts',(62.0275397202892,-8.27799712775361,
-215.8741142462));
#217509=CARTESIAN_POINT('Ctrl Pts',(62.9065377484219,-8.99442320332278,
-213.225569775073));
#217510=CARTESIAN_POINT('Ctrl Pts',(62.8797098464659,-8.61804933049181,
-214.682231763241));
#217511=CARTESIAN_POINT('Ctrl Pts',(62.0269902683634,-8.3072815813721,-215.882454117388));
#217512=CARTESIAN_POINT('Ctrl Pts',(62.9065289038154,-9.00575475318705,
-213.228490523492));
#217513=CARTESIAN_POINT('Ctrl Pts',(62.8796976742588,-8.62706334820223,
-214.685080386211));
#217514=CARTESIAN_POINT('Ctrl Pts',(62.0264604156775,-8.31439581090885,
-215.885082867452));
#217515=CARTESIAN_POINT('Ctrl Pts',(62.9065107565238,-9.02841676696405,
-213.234337353352));
#217516=CARTESIAN_POINT('Ctrl Pts',(62.879695591268,-8.65191985769815,-214.690932006268));
#217517=CARTESIAN_POINT('Ctrl Pts',(62.0270215450733,-8.3410207670247,-215.89110921259));
#217518=CARTESIAN_POINT('Ctrl Pts',(62.9065017229464,-9.03975023999172,
-213.237248654769));
#217519=CARTESIAN_POINT('Ctrl Pts',(62.8796945523615,-8.66435102539255,
-214.693845992121));
#217520=CARTESIAN_POINT('Ctrl Pts',(62.0273007300244,-8.35433682400823,
-215.894110381235));
#217521=CARTESIAN_POINT('Ctrl Pts',(62.9064567562113,-9.0964299581106,-213.251744484892));
#217522=CARTESIAN_POINT('Ctrl Pts',(62.8796893713575,-8.72651863071803,
-214.708356037324));
#217523=CARTESIAN_POINT('Ctrl Pts',(62.0286897292193,-8.42093498218168,
-215.909056095157));
#217524=CARTESIAN_POINT('Ctrl Pts',(62.906421426558,-9.14181326257087,-213.263146980914));
#217525=CARTESIAN_POINT('Ctrl Pts',(62.8796852689654,-8.77630162451325,
-214.719775098578));
#217526=CARTESIAN_POINT('Ctrl Pts',(62.0297787648922,-8.47427065578853,
-215.920820239223));
#217527=CARTESIAN_POINT('Ctrl Pts',(62.9061093426684,-9.55062130297945,
-213.364009501424));
#217528=CARTESIAN_POINT('Ctrl Pts',(62.8796487835579,-9.22458700993411,
-214.82078775372));
#217529=CARTESIAN_POINT('Ctrl Pts',(62.0393775573417,-8.95480295651162,
-216.024953117001));
#217530=CARTESIAN_POINT('Ctrl Pts',(62.9058739446102,-9.91655549914845,
-213.44114324688));
#217531=CARTESIAN_POINT('Ctrl Pts',(62.8796194018479,-9.62623601331707,
-214.898410179928));
#217532=CARTESIAN_POINT('Ctrl Pts',(62.0464615113934,-9.38552114236539,
-216.105099157688));
#217533=CARTESIAN_POINT('Ctrl Pts',(62.9054945382152,-10.6537874440521,
-213.569065352509));
#217534=CARTESIAN_POINT('Ctrl Pts',(62.8795693127297,-10.435460010221,-215.027900806566));
#217535=CARTESIAN_POINT('Ctrl Pts',(62.0574632007413,-10.2539989076757,
-216.239254263903));
#217536=CARTESIAN_POINT('Ctrl Pts',(62.905350423994,-11.0264379343114,-213.619939162974));
#217537=CARTESIAN_POINT('Ctrl Pts',(62.87954862193,-10.8446388729512,-215.079895997074));
#217538=CARTESIAN_POINT('Ctrl Pts',(62.0613821604612,-10.6933250732436,
-216.293358240871));
#217539=CARTESIAN_POINT('Ctrl Pts',(62.9051593336146,-11.7684901551169,
-213.693446645343));
#217540=CARTESIAN_POINT('Ctrl Pts',(62.8795160056152,-11.6592885823963,
-215.156242176727));
#217541=CARTESIAN_POINT('Ctrl Pts',(62.0658080661948,-11.5683522558103,
-216.37343912484));
#217542=CARTESIAN_POINT('Ctrl Pts',(62.9051117861205,-12.1381923296176,
-213.716251957739));
#217543=CARTESIAN_POINT('Ctrl Pts',(62.8795039952751,-12.0652013454517,
-215.180780877871));
#217544=CARTESIAN_POINT('Ctrl Pts',(62.0663326131717,-12.0043471050542,
-216.399586213771));
#217545=CARTESIAN_POINT('Ctrl Pts',(62.9051036527997,-13.243445563085,-213.744071341037));
#217546=CARTESIAN_POINT('Ctrl Pts',(62.8794748263331,-13.2783114028496,
-215.214676585691));
#217547=CARTESIAN_POINT('Ctrl Pts',(62.0629721988681,-13.3072813139657,
-216.437555879606));
#217548=CARTESIAN_POINT('Ctrl Pts',(62.9052789204624,-13.9751373806058,
-213.708426173576));
#217549=CARTESIAN_POINT('Ctrl Pts',(62.8794655689834,-14.081457450616,-215.184200160213));
#217550=CARTESIAN_POINT('Ctrl Pts',(62.0541257046421,-14.1689833911665,
-216.408834050813));
#217551=CARTESIAN_POINT('Ctrl Pts',(62.9057445940404,-15.0655774299771,
-213.580180828239));
#217552=CARTESIAN_POINT('Ctrl Pts',(62.8794187494639,-15.2755977889231,
-215.065402979219));
#217553=CARTESIAN_POINT('Ctrl Pts',(62.0320573263821,-15.4490848449937,
-216.291038336921));
#217554=CARTESIAN_POINT('Ctrl Pts',(62.9059331942183,-15.4278764578799,
-213.524990067775));
#217555=CARTESIAN_POINT('Ctrl Pts',(62.8793972253274,-15.6723243016018,
-215.013586287052));
#217556=CARTESIAN_POINT('Ctrl Pts',(62.0232381588368,-15.8737432145396,
-216.239343311923));
#217557=CARTESIAN_POINT('Ctrl Pts',(62.9062547760745,-15.9696430762788,
-213.424484058149));
#217558=CARTESIAN_POINT('Ctrl Pts',(62.8793480927401,-16.2648134030746,
-214.918541783998));
#217559=CARTESIAN_POINT('Ctrl Pts',(62.0080259576815,-16.5073872973098,
-216.144071868544));
#217560=CARTESIAN_POINT('Ctrl Pts',(62.9063683773708,-16.1499518187337,
-213.38803074649));
#217561=CARTESIAN_POINT('Ctrl Pts',(62.8793288120533,-16.4619892047426,
-214.883956414301));
#217562=CARTESIAN_POINT('Ctrl Pts',(62.0026218050749,-16.7180652996643,
-216.109363202134));
#217563=CARTESIAN_POINT('Ctrl Pts',(62.9065468872613,-16.4200061599841,
-213.329044171076));
#217564=CARTESIAN_POINT('Ctrl Pts',(62.8792944775105,-16.7571264425052,
-214.827867382111));
#217565=CARTESIAN_POINT('Ctrl Pts',(61.994042677577,-17.0332563013891,-216.052989402922));
#217566=CARTESIAN_POINT('Ctrl Pts',(62.9066077402092,-16.5099561526457,
-213.308664291015));
#217567=CARTESIAN_POINT('Ctrl Pts',(62.8792821285777,-16.8554254196337,
-214.808463837074));
#217568=CARTESIAN_POINT('Ctrl Pts',(61.9911043964934,-17.1381808858366,
-216.033479730101));
#217569=CARTESIAN_POINT('Ctrl Pts',(62.9067008407091,-16.644780457911,-213.277033722408));
#217570=CARTESIAN_POINT('Ctrl Pts',(62.8792621149752,-17.0027153104515,
-214.778320560607));
#217571=CARTESIAN_POINT('Ctrl Pts',(61.9865832503263,-17.2953539198766,
-216.003152916317));
#217572=CARTESIAN_POINT('Ctrl Pts',(62.9067321776173,-16.6897051128861,
-213.266313413053));
#217573=CARTESIAN_POINT('Ctrl Pts',(62.8792551943321,-17.0517917499927,
-214.768098452986));
#217574=CARTESIAN_POINT('Ctrl Pts',(61.985057249836,-17.3477092677032,-215.992866939259));
#217575=CARTESIAN_POINT('Ctrl Pts',(62.9067796117351,-16.7570671165656,
-213.249969786042));
#217576=CARTESIAN_POINT('Ctrl Pts',(62.879244422478,-17.1253666622028,-214.75250769517));
#217577=CARTESIAN_POINT('Ctrl Pts',(61.9827403503223,-17.4261881952898,
-215.977174377362));
#217578=CARTESIAN_POINT('Ctrl Pts',(62.9067954945617,-16.7795169546794,
-213.244478050128));
#217579=CARTESIAN_POINT('Ctrl Pts',(62.8792407664544,-17.1498865664599,
-214.747267502411));
#217580=CARTESIAN_POINT('Ctrl Pts',(61.9819634009862,-17.4523388156653,
-215.971899592409));
#217581=CARTESIAN_POINT('Ctrl Pts',(62.9068194226298,-16.8131854913724,
-213.236174910655));
#217582=CARTESIAN_POINT('Ctrl Pts',(62.8792351823635,-17.1866564730818,
-214.739343052782));
#217583=CARTESIAN_POINT('Ctrl Pts',(61.9807910694282,-17.4915511452329,
-215.963921765975));
#217584=CARTESIAN_POINT('Ctrl Pts',(62.9068274159574,-16.8244073001866,
-213.233396274889));
#217585=CARTESIAN_POINT('Ctrl Pts',(62.8792333042642,-17.1989118397669,
-214.736690790842));
#217586=CARTESIAN_POINT('Ctrl Pts',(61.9803991410476,-17.5046196532664,
-215.961251549351));
#217587=CARTESIAN_POINT('Ctrl Pts',(62.9068434366578,-16.8468488483916,
-213.227817200875));
#217588=CARTESIAN_POINT('Ctrl Pts',(62.8792295142709,-17.223419512581,-214.731364863971));
#217589=CARTESIAN_POINT('Ctrl Pts',(61.9796129930294,-17.5307521218042,
-215.955889275238));
#217590=CARTESIAN_POINT('Ctrl Pts',(62.9068512246001,-16.8580698646293,
-213.225030214802));
#217591=CARTESIAN_POINT('Ctrl Pts',(62.8792447756866,-17.2324410430089,
-214.728381164571));
#217592=CARTESIAN_POINT('Ctrl Pts',(61.980377068186,-17.5380100722587,-215.952980774701));
#217593=CARTESIAN_POINT('Ctrl Pts',(62.9078064251384,-18.3057228153494,
-212.867003491606));
#217594=CARTESIAN_POINT('Ctrl Pts',(62.8802082957154,-18.5725016104741,
-214.363427060571));
#217595=CARTESIAN_POINT('Ctrl Pts',(62.0149243105808,-18.7952395296689,
-215.59183941935));
#217596=CARTESIAN_POINT('Ctrl Pts',(62.9033129898347,-19.7553919607571,
-212.653495577744));
#217597=CARTESIAN_POINT('Ctrl Pts',(62.8762357607657,-19.9205453051955,
-214.136541643927));
#217598=CARTESIAN_POINT('Ctrl Pts',(62.0392411361479,-20.0571576067025,
-215.363703521968));
#217599=CARTESIAN_POINT('Ctrl Pts',(62.8830851680151,-22.6547081034196,
-212.52986856343));
#217600=CARTESIAN_POINT('Ctrl Pts',(62.8581004822445,-22.6112951161231,
-213.975521928866));
#217601=CARTESIAN_POINT('Ctrl Pts',(62.0686653400334,-22.5711272294273,
-215.185493388832));
#217602=CARTESIAN_POINT('Ctrl Pts',(62.8673563795338,-24.1094370634719,
-212.617838162876));
#217603=CARTESIAN_POINT('Ctrl Pts',(62.8439525084138,-23.9605649484755,
-214.038745368151));
#217604=CARTESIAN_POINT('Ctrl Pts',(62.0739679487614,-23.8279590992824,
-215.233708940831));
#217605=CARTESIAN_POINT('Ctrl Pts',(62.8399085993617,-25.9282456355318,
-212.959941102886));
#217606=CARTESIAN_POINT('Ctrl Pts',(62.8193618641866,-25.6370453624972,
-214.33907548895));
#217607=CARTESIAN_POINT('Ctrl Pts',(62.0659506819248,-25.3798830245726,
-215.502362302155));
#217608=CARTESIAN_POINT('Ctrl Pts',(62.8340297350381,-26.2918276350351,
-213.040124650367));
#217609=CARTESIAN_POINT('Ctrl Pts',(62.8141018085935,-25.9715146998356,
-214.410299819559));
#217610=CARTESIAN_POINT('Ctrl Pts',(62.0635946113577,-25.6891136834931,
-215.566638111475));
#217611=CARTESIAN_POINT('Ctrl Pts',(62.8261731592033,-26.7460613321157,
-213.156334850829));
#217612=CARTESIAN_POINT('Ctrl Pts',(62.8070813385858,-26.3885631025506,
-214.514477388603));
#217613=CARTESIAN_POINT('Ctrl Pts',(62.0595992131559,-26.0739174525129,
-215.661200292517));
#217614=CARTESIAN_POINT('Ctrl Pts',(62.8245764208424,-26.8368958608164,
-213.180377302499));
#217615=CARTESIAN_POINT('Ctrl Pts',(62.8056550731544,-26.4719143407304,
-214.536069637883));
#217616=CARTESIAN_POINT('Ctrl Pts',(62.0587474792527,-26.1507912740874,
-215.680824692928));
#217617=CARTESIAN_POINT('Ctrl Pts',(62.8225483225521,-26.950423403808,-213.211454506225));
#217618=CARTESIAN_POINT('Ctrl Pts',(62.8038440965971,-26.5760357433315,
-214.564029548489));
#217619=CARTESIAN_POINT('Ctrl Pts',(62.0576149086873,-26.2467696827909,
-215.706264227521));
#217620=CARTESIAN_POINT('Ctrl Pts',(62.8221410940189,-26.9731281314207,
-213.217721160271));
#217621=CARTESIAN_POINT('Ctrl Pts',(62.8034805008598,-26.5968562497989,
-214.56966990827));
#217622=CARTESIAN_POINT('Ctrl Pts',(62.0573849987646,-26.2659596714963,
-215.71139759155));
#217623=CARTESIAN_POINT('Ctrl Pts',(62.8215278301372,-27.0071840444279,
-213.227198424036));
#217624=CARTESIAN_POINT('Ctrl Pts',(62.8029329912778,-26.6280818473612,
-214.57820358626));
#217625=CARTESIAN_POINT('Ctrl Pts',(62.0570349989822,-26.2947360125198,
-215.719166196104));
#217626=CARTESIAN_POINT('Ctrl Pts',(62.8213230053295,-27.0185358190149,
-213.230370392442));
#217627=CARTESIAN_POINT('Ctrl Pts',(62.8027501360862,-26.6384894816988,
-214.581060324812));
#217628=CARTESIAN_POINT('Ctrl Pts',(62.0569174765794,-26.3043266859831,
-215.721767157448));
#217629=CARTESIAN_POINT('Ctrl Pts',(62.8210151618606,-27.0355631854271,
-213.235147724465));
#217630=CARTESIAN_POINT('Ctrl Pts',(62.8024753235955,-26.6540996350435,
-214.585363770433));
#217631=CARTESIAN_POINT('Ctrl Pts',(62.0567399040033,-26.3187105229747,
-215.725685786475));
#217632=CARTESIAN_POINT('Ctrl Pts',(62.8209124463284,-27.0412389249793,
-213.236743398352));
#217633=CARTESIAN_POINT('Ctrl Pts',(62.8023836313177,-26.659302793678,-214.586801305957));
#217634=CARTESIAN_POINT('Ctrl Pts',(62.0566804983261,-26.3235047731397,
-215.726994860647));
#217635=CARTESIAN_POINT('Ctrl Pts',(62.8207068130133,-27.0525903054424,
-213.239941215787));
#217636=CARTESIAN_POINT('Ctrl Pts',(62.8022000701859,-26.669708670566,-214.589682496766));
#217637=CARTESIAN_POINT('Ctrl Pts',(62.0565612564283,-26.3330925469615,
-215.729618745949));
#217638=CARTESIAN_POINT('Ctrl Pts',(62.8206039569716,-27.0582660000666,
-213.241539781896));
#217639=CARTESIAN_POINT('Ctrl Pts',(62.8020756172633,-26.6766427063805,
-214.591683103012));
#217640=CARTESIAN_POINT('Ctrl Pts',(62.0563759404316,-26.3410999882819,
-215.731950428965));
#217641=CARTESIAN_POINT('Ctrl Pts',(62.8196787974583,-27.1093480735134,
-213.255871682944));
#217642=CARTESIAN_POINT('Ctrl Pts',(62.8010604891949,-26.7335035083587,
-214.607839142305));
#217643=CARTESIAN_POINT('Ctrl Pts',(62.0551041668616,-26.4028713900106,
-215.749611986012));
#217644=CARTESIAN_POINT('Ctrl Pts',(62.8188583609006,-27.1547585116387,
-213.268331481197));
#217645=CARTESIAN_POINT('Ctrl Pts',(62.8001595869042,-26.7840369239728,
-214.621921517333));
#217646=CARTESIAN_POINT('Ctrl Pts',(62.0539403091928,-26.4577601301325,
-215.765023583509));
#217647=CARTESIAN_POINT('Ctrl Pts',(62.8147655328413,-27.3818312159601,
-213.329248041548));
#217648=CARTESIAN_POINT('Ctrl Pts',(62.7956617726082,-27.0366682767733,
-214.690959778013));
#217649=CARTESIAN_POINT('Ctrl Pts',(62.0479560084918,-26.7321109243143,
-215.840660860072));
#217650=CARTESIAN_POINT('Ctrl Pts',(62.811521179222,-27.5635550010564,-213.373559009004));
#217651=CARTESIAN_POINT('Ctrl Pts',(62.792085332894,-27.238636566617,-214.741789248302));
#217652=CARTESIAN_POINT('Ctrl Pts',(62.0426408175475,-26.9512950299888,
-215.89662634158));
#217653=CARTESIAN_POINT('Ctrl Pts',(62.7954319749737,-28.4724876729194,
-213.573958234288));
#217654=CARTESIAN_POINT('Ctrl Pts',(62.7742896842574,-28.2481778367032,
-214.974978243553));
#217655=CARTESIAN_POINT('Ctrl Pts',(62.0135384026934,-28.0458953208882,
-216.15474774953));
#217656=CARTESIAN_POINT('Ctrl Pts',(62.7829855880237,-29.2006385623099,
-213.666528824371));
#217657=CARTESIAN_POINT('Ctrl Pts',(62.7603316101004,-29.0547579215752,
-215.09426369493));
#217658=CARTESIAN_POINT('Ctrl Pts',(61.9820535417445,-28.9180045033719,
-216.291912296996));
#217659=CARTESIAN_POINT('Ctrl Pts',(62.7463293349581,-31.3876040979605,
-213.774365476532));
#217660=CARTESIAN_POINT('Ctrl Pts',(62.7188256094512,-31.4679377673016,
-215.282340428597));
#217661=CARTESIAN_POINT('Ctrl Pts',(61.8687456407067,-31.514819604097,-216.526229178884));
#217662=CARTESIAN_POINT('Ctrl Pts',(62.7227759583408,-32.8489094531929,
-213.621230861582));
#217663=CARTESIAN_POINT('Ctrl Pts',(62.6915950430413,-33.0690705517719,
-215.181307910843));
#217664=CARTESIAN_POINT('Ctrl Pts',(61.7680050000962,-33.2220331134748,
-216.448292898274));
#217665=CARTESIAN_POINT('Ctrl Pts',(62.6973153894392,-34.4039131251247,
-213.297292874274));
#217666=CARTESIAN_POINT('Ctrl Pts',(62.6621683869121,-34.7487344411069,
-214.913581096992));
#217667=CARTESIAN_POINT('Ctrl Pts',(61.6490045697264,-35.0057699870247,
-216.194181682595));
#217668=CARTESIAN_POINT('Ctrl Pts',(62.6958162562235,-34.4953927542909,
-213.277636702595));
#217669=CARTESIAN_POINT('Ctrl Pts',(62.6604275289915,-34.8479236941524,
-214.897160427577));
#217670=CARTESIAN_POINT('Ctrl Pts',(61.6419554736938,-35.1105969222302,
-216.178600343238));
#217671=CARTESIAN_POINT('Ctrl Pts',(62.6939402205335,-34.609753063567,-213.252332432689));
#217672=CARTESIAN_POINT('Ctrl Pts',(62.6582484377325,-34.9718435394741,
-214.875901505568));
#217673=CARTESIAN_POINT('Ctrl Pts',(61.6330839192102,-35.241514474014,-216.158350002109));
#217674=CARTESIAN_POINT('Ctrl Pts',(62.6935649074929,-34.632625664123,-213.247234872736));
#217675=CARTESIAN_POINT('Ctrl Pts',(62.657812349987,-34.9966309075331,-214.871611881384));
#217676=CARTESIAN_POINT('Ctrl Pts',(61.6313066004446,-35.267692149343,-216.15426125142));
#217677=CARTESIAN_POINT('Ctrl Pts',(62.6930017735534,-34.6669353682869,
-213.23953378686));
#217678=CARTESIAN_POINT('Ctrl Pts',(62.6571579734683,-35.0338077059872,
-214.865122644271));
#217679=CARTESIAN_POINT('Ctrl Pts',(61.6286361305327,-35.306950041299,-216.148070435334));
#217680=CARTESIAN_POINT('Ctrl Pts',(62.6928140348451,-34.6783720702322,
-213.23695763384));
#217681=CARTESIAN_POINT('Ctrl Pts',(62.6569397952362,-35.0461999389248,
-214.86295031173));
#217682=CARTESIAN_POINT('Ctrl Pts',(61.6277452254698,-35.3200345655743,
-216.145997215361));
#217683=CARTESIAN_POINT('Ctrl Pts',(62.6924385017241,-34.7012457411244,
-213.231787130787));
#217684=CARTESIAN_POINT('Ctrl Pts',(62.6565033481798,-35.0709834459169,
-214.858587353424));
#217685=CARTESIAN_POINT('Ctrl Pts',(61.6259619219035,-35.3462007537114,
-216.141831601746));
#217686=CARTESIAN_POINT('Ctrl Pts',(62.6922505031027,-34.7126825313609,
-213.229204685838));
#217687=CARTESIAN_POINT('Ctrl Pts',(62.6563676105427,-35.0803506782823,
-214.855199499274));
#217688=CARTESIAN_POINT('Ctrl Pts',(61.6272019533633,-35.3540299418295,
-216.138259961343));
#217689=CARTESIAN_POINT('Ctrl Pts',(62.6913088110138,-34.7698657850159,
-213.216337901175));
#217690=CARTESIAN_POINT('Ctrl Pts',(62.6555047555815,-35.1338645553915,
-214.840975106258));
#217691=CARTESIAN_POINT('Ctrl Pts',(61.6286902735705,-35.4047784879965,
-216.12373712742));
#217692=CARTESIAN_POINT('Ctrl Pts',(62.6905505732427,-34.8156106395255,
-213.206157663252));
#217693=CARTESIAN_POINT('Ctrl Pts',(62.6548100127451,-35.176676489797,-214.829703015251));
#217694=CARTESIAN_POINT('Ctrl Pts',(61.6298739292442,-35.4453709799185,
-216.112221039658));
#217695=CARTESIAN_POINT('Ctrl Pts',(62.6867349314903,-35.0443261388968,
-213.15582449853));
#217696=CARTESIAN_POINT('Ctrl Pts',(62.6513153166306,-35.3906577352144,
-214.773903124995));
#217697=CARTESIAN_POINT('Ctrl Pts',(61.635757391351,-35.6483009438719,-216.05515295758));
#217698=CARTESIAN_POINT('Ctrl Pts',(62.6836041752042,-35.227270469835,-213.117375270577));
#217699=CARTESIAN_POINT('Ctrl Pts',(62.6484482028618,-35.561854520356,-214.730986421537));
#217700=CARTESIAN_POINT('Ctrl Pts',(61.6403527485721,-35.810539975685,-216.011138030016));
#217701=CARTESIAN_POINT('Ctrl Pts',(62.6739757829552,-35.7760179301671,
-213.007568080911));
#217702=CARTESIAN_POINT('Ctrl Pts',(62.6396380425831,-36.0750857329258,
-214.607582586062));
#217703=CARTESIAN_POINT('Ctrl Pts',(61.6538107373805,-36.2969010033139,
-215.884077811248));
#217704=CARTESIAN_POINT('Ctrl Pts',(62.6672458339371,-36.1415480006374,
-212.941772621246));
#217705=CARTESIAN_POINT('Ctrl Pts',(62.6334830510151,-36.4170090776854,
-214.532350962691));
#217706=CARTESIAN_POINT('Ctrl Pts',(61.6623415978292,-36.6205004660809,
-215.806047787868));
#217707=CARTESIAN_POINT('Ctrl Pts',(62.6460655421939,-37.2394079985843,
-212.767180740501));
#217708=CARTESIAN_POINT('Ctrl Pts',(62.6141474585686,-37.4426606009465,
-214.328492936668));
#217709=CARTESIAN_POINT('Ctrl Pts',(61.6866935200193,-37.5909455865243,
-215.592253113864));
#217710=CARTESIAN_POINT('Ctrl Pts',(62.6306238454731,-37.9731020337408,
-212.681065126087));
#217711=CARTESIAN_POINT('Ctrl Pts',(62.6000692240083,-38.1280246284507,
-214.221120830614));
#217712=CARTESIAN_POINT('Ctrl Pts',(61.7012950170652,-38.2375005898279,
-215.476682421731));
#217713=CARTESIAN_POINT('Ctrl Pts',(62.5969132094228,-39.4445711917938,
-212.577895377786));
#217714=CARTESIAN_POINT('Ctrl Pts',(62.5694213181663,-39.4999857528758,
-214.071635186044));
#217715=CARTESIAN_POINT('Ctrl Pts',(61.7271079946506,-39.52809238237,-215.306122006413));
#217716=CARTESIAN_POINT('Ctrl Pts',(62.5786465561153,-40.1823394734562,
-212.56072643116));
#217717=CARTESIAN_POINT('Ctrl Pts',(62.5528572913972,-40.186716811975,-214.029227841839));
#217718=CARTESIAN_POINT('Ctrl Pts',(61.7383115771298,-40.1721899106378,
-215.251065883709));
#217719=CARTESIAN_POINT('Ctrl Pts',(62.5489095967688,-41.2926666211419,
-212.597076537344));
#217720=CARTESIAN_POINT('Ctrl Pts',(62.5259796592712,-41.2177253956526,
-214.023715172298));
#217721=CARTESIAN_POINT('Ctrl Pts',(61.7522529494064,-41.1345693196256,
-215.221901979336));
#217722=CARTESIAN_POINT('Ctrl Pts',(62.5385733023658,-41.6645079426499,
-212.619734584269));
#217723=CARTESIAN_POINT('Ctrl Pts',(62.5166614548086,-41.5622368317271,
-214.031654331973));
#217724=CARTESIAN_POINT('Ctrl Pts',(61.7564322562654,-41.4556717679246,
-215.221175362458));
#217725=CARTESIAN_POINT('Ctrl Pts',(62.5172963966415,-42.4017436060864,
-212.687617475152));
#217726=CARTESIAN_POINT('Ctrl Pts',(62.4975235652628,-42.243965739272,-214.068785079329));
#217727=CARTESIAN_POINT('Ctrl Pts',(61.763623688336,-42.0895206278039,-215.239343116333));
#217728=CARTESIAN_POINT('Ctrl Pts',(62.5063477838447,-42.7675314704579,
-212.732780967694));
#217729=CARTESIAN_POINT('Ctrl Pts',(62.4876965212927,-42.5815841800676,
-214.097879730704));
#217730=CARTESIAN_POINT('Ctrl Pts',(61.7666445972041,-42.4026166823129,
-215.258164485443));
#217731=CARTESIAN_POINT('Ctrl Pts',(62.4725701813139,-43.8557232524475,
-212.904651540613));
#217732=CARTESIAN_POINT('Ctrl Pts',(62.4574785572312,-43.5829084833784,
-214.219091484158));
#217733=CARTESIAN_POINT('Ctrl Pts',(61.773814934178,-43.3290662887116,-215.345785453686));
#217734=CARTESIAN_POINT('Ctrl Pts',(62.4488123543698,-44.5690597591882,
-213.067323574869));
#217735=CARTESIAN_POINT('Ctrl Pts',(62.4363119561656,-44.236699042062,-214.344774294021));
#217736=CARTESIAN_POINT('Ctrl Pts',(61.7761368886402,-43.9296800867984,
-215.445400831427));
#217737=CARTESIAN_POINT('Ctrl Pts',(62.411269138031,-45.6166733720249,-213.400195879719));
#217738=CARTESIAN_POINT('Ctrl Pts',(62.4031003559944,-45.1899483809382,
-214.615484592056));
#217739=CARTESIAN_POINT('Ctrl Pts',(61.7744895314065,-44.7976174234393,
-215.668902106843));
#217740=CARTESIAN_POINT('Ctrl Pts',(62.3984364151383,-45.962125223904,-213.526046844514));
#217741=CARTESIAN_POINT('Ctrl Pts',(62.39179260267,-45.5029471693551,-214.719404394484));
#217742=CARTESIAN_POINT('Ctrl Pts',(61.7730731774584,-45.0814095354759,
-215.755816696107));
#217743=CARTESIAN_POINT('Ctrl Pts',(62.3721154800596,-46.6444314431214,
-213.811880088235));
#217744=CARTESIAN_POINT('Ctrl Pts',(62.3687040669745,-46.1180536806806,
-214.958482420413));
#217745=CARTESIAN_POINT('Ctrl Pts',(61.7680734151979,-45.6360416008198,
-215.957640236994));
#217746=CARTESIAN_POINT('Ctrl Pts',(62.3585615338657,-46.9827912699497,
-213.972791370421));
#217747=CARTESIAN_POINT('Ctrl Pts',(62.3568641610027,-46.4215724898018,
-215.094442901992));
#217748=CARTESIAN_POINT('Ctrl Pts',(61.7644619516127,-45.9080672741359,
-216.073240699382));
#217749=CARTESIAN_POINT('Ctrl Pts',(62.3449264240553,-47.3099624311764,
-214.150201433913));
#217750=CARTESIAN_POINT('Ctrl Pts',(62.3450159671272,-46.7131851982871,
-215.245597852421));
#217751=CARTESIAN_POINT('Ctrl Pts',(61.7595433353131,-46.167485490306,-216.202399824357));
#217752=CARTESIAN_POINT('',(61.7131038227433,20.038950662233,-216.160137831863));
#217753=CARTESIAN_POINT('',(62.3650463286435,20.9007637244406,-213.866522994717));
#217754=CARTESIAN_POINT('Ctrl Pts',(61.7131038227445,20.0389506617929,-216.160137831687));
#217755=CARTESIAN_POINT('Ctrl Pts',(61.7368124258176,20.0546467655865,-216.121235415936));
#217756=CARTESIAN_POINT('Ctrl Pts',(61.761719571167,20.0715966718075,-216.079068639254));
#217757=CARTESIAN_POINT('Ctrl Pts',(61.7875162077924,20.0898264294659,-216.033490938998));
#217758=CARTESIAN_POINT('Ctrl Pts',(61.8136580552382,20.1083001379032,-215.987303317552));
#217759=CARTESIAN_POINT('Ctrl Pts',(61.8407134872745,20.1280882012577,-215.937612918845));
#217760=CARTESIAN_POINT('Ctrl Pts',(61.8683094332131,20.1492190576661,-215.884248757928));
#217761=CARTESIAN_POINT('Ctrl Pts',(61.8959053791516,20.1703499140744,-215.83088459701));
#217762=CARTESIAN_POINT('Ctrl Pts',(61.924041838205,20.1928235921681,-215.773846675231));
#217763=CARTESIAN_POINT('Ctrl Pts',(61.9522938471338,20.2166694774165,-215.712945365588));
#217764=CARTESIAN_POINT('Ctrl Pts',(61.9839298364388,20.2433715846044,-215.644749394626));
#217765=CARTESIAN_POINT('Ctrl Pts',(62.0157021939934,20.2717882751306,-215.571724442015));
#217766=CARTESIAN_POINT('Ctrl Pts',(62.0468955895493,20.3019109118738,-215.493710167469));
#217767=CARTESIAN_POINT('Ctrl Pts',(62.0660815959063,20.3204383305708,-215.445726216356));
#217768=CARTESIAN_POINT('Ctrl Pts',(62.085048844248,20.3396125459156,-215.395850629491));
#217769=CARTESIAN_POINT('Ctrl Pts',(62.1036166227799,20.3594252104984,-215.344058873871));
#217770=CARTESIAN_POINT('Ctrl Pts',(62.1253168115682,20.3825802993589,-215.283529776506));
#217771=CARTESIAN_POINT('Ctrl Pts',(62.1464708764804,20.4066073064949,-215.220383743453));
#217772=CARTESIAN_POINT('Ctrl Pts',(62.1667783859581,20.4314829485095,-215.154604313644));
#217773=CARTESIAN_POINT('Ctrl Pts',(62.1721575938579,20.4380721981753,-215.137180156887));
#217774=CARTESIAN_POINT('Ctrl Pts',(62.1773035625962,20.4445030896074,-215.120148444136));
#217775=CARTESIAN_POINT('Ctrl Pts',(62.1825121872622,20.4511480694473,-215.10252207976));
#217776=CARTESIAN_POINT('Ctrl Pts',(62.1864240742462,20.4561387170388,-215.089283969933));
#217777=CARTESIAN_POINT('Ctrl Pts',(62.1903704548995,20.4612501557837,-215.075710136272));
#217778=CARTESIAN_POINT('Ctrl Pts',(62.1944585031203,20.4666408209093,-215.061375901005));
#217779=CARTESIAN_POINT('Ctrl Pts',(62.1945458745928,20.4667560324539,-215.061069543747));
#217780=CARTESIAN_POINT('Ctrl Pts',(62.1946331997095,20.466871226232,-215.060763226167));
#217781=CARTESIAN_POINT('Ctrl Pts',(62.1947204784964,20.4669864022318,-215.0604569483));
#217782=CARTESIAN_POINT('Ctrl Pts',(62.2137408953005,20.4920863789936,-214.993710687232));
#217783=CARTESIAN_POINT('Ctrl Pts',(62.2305183466783,20.5163680122445,-214.928763782419));
#217784=CARTESIAN_POINT('Ctrl Pts',(62.2453129380165,20.5396752117267,-214.866095687917));
#217785=CARTESIAN_POINT('Ctrl Pts',(62.2602442721621,20.5631978339817,-214.802848367469));
#217786=CARTESIAN_POINT('Ctrl Pts',(62.2731565800729,20.5857280016135,-214.74192226384));
#217787=CARTESIAN_POINT('Ctrl Pts',(62.2843394053267,20.6071284880971,-214.683764654696));
#217788=CARTESIAN_POINT('Ctrl Pts',(62.2959819233376,20.6294086850662,-214.623216358844));
#217789=CARTESIAN_POINT('Ctrl Pts',(62.305750679233,20.6504644959011,-214.565668984582));
#217790=CARTESIAN_POINT('Ctrl Pts',(62.3139850117542,20.6701651459376,-214.511575895126));
#217791=CARTESIAN_POINT('Ctrl Pts',(62.3213517958911,20.6877901854663,-214.463181916342));
#217792=CARTESIAN_POINT('Ctrl Pts',(62.3274911569473,20.7043310817668,-214.417551780352));
#217793=CARTESIAN_POINT('Ctrl Pts',(62.332644851844,20.7197079144591,-214.374977598554));
#217794=CARTESIAN_POINT('Ctrl Pts',(62.3385799996162,20.7374163306779,-214.325947909116));
#217795=CARTESIAN_POINT('Ctrl Pts',(62.343548092569,20.7545910669149,-214.278189339776));
#217796=CARTESIAN_POINT('Ctrl Pts',(62.3476965833135,20.7713604195755,-214.231380372206));
#217797=CARTESIAN_POINT('Ctrl Pts',(62.3519241262657,20.7884493232321,-214.183679429109));
#217798=CARTESIAN_POINT('Ctrl Pts',(62.3553004212001,20.8051173944794,-214.136964144099));
#217799=CARTESIAN_POINT('Ctrl Pts',(62.3579284930835,20.8215000454921,-214.090879110919));
#217800=CARTESIAN_POINT('Ctrl Pts',(62.3605956251293,20.8381261864238,-214.044109131146));
#217801=CARTESIAN_POINT('Ctrl Pts',(62.3624920885415,20.8544585042312,-213.997987834824));
#217802=CARTESIAN_POINT('Ctrl Pts',(62.3636727291745,20.8706359516702,-213.95213530026));
#217803=CARTESIAN_POINT('Ctrl Pts',(62.364409404324,20.8807300676777,-213.923525051031));
#217804=CARTESIAN_POINT('Ctrl Pts',(62.364866354255,20.8907638289918,-213.895019299259));
#217805=CARTESIAN_POINT('Ctrl Pts',(62.3650466932196,20.9007701135701,-213.866525240701));
#217806=CARTESIAN_POINT('Ctrl Pts',(62.3685680730117,-46.7295395343351,
-213.857752904022));
#217807=CARTESIAN_POINT('Ctrl Pts',(62.3741929789703,-46.5883029740106,
-213.791721229881));
#217808=CARTESIAN_POINT('Ctrl Pts',(62.379769730669,-46.4460136161633,-213.728758447291));
#217809=CARTESIAN_POINT('Ctrl Pts',(62.3852759446209,-46.3032780419763,
-213.66896415876));
#217810=CARTESIAN_POINT('Ctrl Pts',(62.3975426120195,-45.9852937010517,
-213.535755268559));
#217811=CARTESIAN_POINT('Ctrl Pts',(62.4095164075117,-45.6637866135429,
-213.417460796858));
#217812=CARTESIAN_POINT('Ctrl Pts',(62.4212099409829,-45.3390922762075,
-213.312250040624));
#217813=CARTESIAN_POINT('Ctrl Pts',(62.4220692467669,-45.3152319329839,
-213.304518569927));
#217814=CARTESIAN_POINT('Ctrl Pts',(62.4229270386808,-45.2913543736635,
-213.296857775458));
#217815=CARTESIAN_POINT('Ctrl Pts',(62.423783321531,-45.2674597292971,-213.289266941104));
#217816=CARTESIAN_POINT('Ctrl Pts',(62.4306555056666,-45.0756908577114,
-213.228345936535));
#217817=CARTESIAN_POINT('Ctrl Pts',(62.4374306715992,-44.882827891531,-213.171905711604));
#217818=CARTESIAN_POINT('Ctrl Pts',(62.4441103360269,-44.688905615938,-213.119707758193));
#217819=CARTESIAN_POINT('Ctrl Pts',(62.4591991199772,-44.2508519754838,
-213.001797098131));
#217820=CARTESIAN_POINT('Ctrl Pts',(62.4737962270731,-43.807586665038,-212.90545317022));
#217821=CARTESIAN_POINT('Ctrl Pts',(62.487910617321,-43.3597345734855,-212.828052812568));
#217822=CARTESIAN_POINT('Ctrl Pts',(62.4903171662194,-43.2833743525594,
-212.814855802838));
#217823=CARTESIAN_POINT('Ctrl Pts',(62.4927096777594,-43.2068808554448,
-212.802209610105));
#217824=CARTESIAN_POINT('Ctrl Pts',(62.4950881915083,-43.1302572609202,
-212.790101352926));
#217825=CARTESIAN_POINT('Ctrl Pts',(62.5008761037459,-42.9438002178856,
-212.760636932155));
#217826=CARTESIAN_POINT('Ctrl Pts',(62.5065809373473,-42.7565658493193,
-212.734385263862));
#217827=CARTESIAN_POINT('Ctrl Pts',(62.5122027551557,-42.5685838171507,
-212.711227872825));
#217828=CARTESIAN_POINT('Ctrl Pts',(62.5175209296256,-42.3907549941012,
-212.68932124938));
#217829=CARTESIAN_POINT('Ctrl Pts',(62.5227648065833,-42.21226341704,-212.670174115219));
#217830=CARTESIAN_POINT('Ctrl Pts',(62.527934793664,-42.0331254267331,-212.653679770052));
#217831=CARTESIAN_POINT('Ctrl Pts',(62.5385750526626,-41.6644446962851,
-212.619733049905));
#217832=CARTESIAN_POINT('Ctrl Pts',(62.5489103696869,-41.2926330468725,
-212.597082683292));
#217833=CARTESIAN_POINT('Ctrl Pts',(62.5588215912844,-40.9225569182794,
-212.584979442347));
#217834=CARTESIAN_POINT('Ctrl Pts',(62.563546913138,-40.7461176367326,-212.579209042767));
#217835=CARTESIAN_POINT('Ctrl Pts',(62.5681836632464,-40.569818240452,-212.575793047685));
#217836=CARTESIAN_POINT('Ctrl Pts',(62.5727340550042,-40.3936434675018,
-212.574637782399));
#217837=CARTESIAN_POINT('Ctrl Pts',(62.5872728250113,-39.830754678735,-212.570946641683));
#217838=CARTESIAN_POINT('Ctrl Pts',(62.6009299850148,-39.2692127837649,
-212.590224636208));
#217839=CARTESIAN_POINT('Ctrl Pts',(62.6137680988129,-38.7088381795347,
-212.62950263278));
#217840=CARTESIAN_POINT('Ctrl Pts',(62.6174709897939,-38.5472096022638,
-212.640831566418));
#217841=CARTESIAN_POINT('Ctrl Pts',(62.621105625632,-38.3856786969335,-212.653829961871));
#217842=CARTESIAN_POINT('Ctrl Pts',(62.624672913913,-38.2242434316524,-212.668455765851));
#217843=CARTESIAN_POINT('Ctrl Pts',(62.6373436782581,-37.6508363946395,
-212.720405622716));
#217844=CARTESIAN_POINT('Ctrl Pts',(62.6491674651189,-37.0786070163394,
-212.792770228162));
#217845=CARTESIAN_POINT('Ctrl Pts',(62.6601855978898,-36.5075023878112,
-212.883581944354));
#217846=CARTESIAN_POINT('Ctrl Pts',(62.6630243100176,-36.3603629705465,
-212.906978678217));
#217847=CARTESIAN_POINT('Ctrl Pts',(62.6658095819956,-36.2132944881765,
-212.93160444825));
#217848=CARTESIAN_POINT('Ctrl Pts',(62.6685426178707,-36.0662511671652,
-212.957447775204));
#217849=CARTESIAN_POINT('Ctrl Pts',(62.6726066835548,-35.8475955247613,
-212.995877193271));
#217850=CARTESIAN_POINT('Ctrl Pts',(62.67655631062,-35.6289441133066,-213.037001059776));
#217851=CARTESIAN_POINT('Ctrl Pts',(62.6803946782102,-35.4101865945502,
-213.080774391982));
#217852=CARTESIAN_POINT('Ctrl Pts',(62.6828563633534,-35.2698894184096,
-213.108847826594));
#217853=CARTESIAN_POINT('Ctrl Pts',(62.6852717293958,-35.1295761809506,
-213.138007694812));
#217854=CARTESIAN_POINT('Ctrl Pts',(62.6876407845124,-34.9892589138444,
-213.16823854491));
#217855=CARTESIAN_POINT('Ctrl Pts',(62.6883605905984,-34.9466253667735,
-213.177423789158));
#217856=CARTESIAN_POINT('Ctrl Pts',(62.6890761418335,-34.9039903123139,
-213.186708083956));
#217857=CARTESIAN_POINT('Ctrl Pts',(62.6897874443054,-34.8613537452904,
-213.196091056993));
#217858=CARTESIAN_POINT('Ctrl Pts',(62.6905505729892,-34.8156106352106,
-213.206157682861));
#217859=CARTESIAN_POINT('Ctrl Pts',(62.6913088108168,-34.7698657837733,
-213.216337913904));
#217860=CARTESIAN_POINT('Ctrl Pts',(62.6920621645108,-34.7241191838738,
-213.2266313368));
#217861=CARTESIAN_POINT('Ctrl Pts',(62.6922505029487,-34.7126825330211,
-213.229204692721));
#217862=CARTESIAN_POINT('Ctrl Pts',(62.6924385015879,-34.701245742664,-213.231787136791));
#217863=CARTESIAN_POINT('Ctrl Pts',(62.692626268168,-34.6898089068763,-213.234372387596));
#217864=CARTESIAN_POINT('Ctrl Pts',(62.6928140347403,-34.678372071559,-213.236957638295));
#217865=CARTESIAN_POINT('Ctrl Pts',(62.6930017734619,-34.6669353695333,
-213.239533790651));
#217866=CARTESIAN_POINT('Ctrl Pts',(62.6931894847934,-34.6554988009795,
-213.242100818803));
#217867=CARTESIAN_POINT('Ctrl Pts',(62.6935649074065,-34.6326256669264,
-213.247234874423));
#217868=CARTESIAN_POINT('Ctrl Pts',(62.6939402204544,-34.6097530667514,
-213.252332433524));
#217869=CARTESIAN_POINT('Ctrl Pts',(62.6943154276501,-34.5868810019283,
-213.257393287646));
#217870=CARTESIAN_POINT('Ctrl Pts',(62.6950609186324,-34.5414369958777,
-213.267448588167));
#217871=CARTESIAN_POINT('Ctrl Pts',(62.6958059915227,-34.4959951029891,
-213.277359001683));
#217872=CARTESIAN_POINT('Ctrl Pts',(62.6965506762906,-34.450555335488,-213.287122844289));
#217873=CARTESIAN_POINT('Ctrl Pts',(62.6973051981913,-34.4045153179871,
-213.297015665251));
#217874=CARTESIAN_POINT('Ctrl Pts',(62.6980593192824,-34.3584776267158,
-213.306757986268));
#217875=CARTESIAN_POINT('Ctrl Pts',(62.6988130699628,-34.3124423208934,
-213.316348049998));
#217876=CARTESIAN_POINT('Ctrl Pts',(62.7009988974642,-34.1789429555056,
-213.344158605375));
#217877=CARTESIAN_POINT('Ctrl Pts',(62.7031812969115,-34.0454633873906,
-213.370706259287));
#217878=CARTESIAN_POINT('Ctrl Pts',(62.7053612372102,-33.9120052530642,
-213.395935334584));
#217879=CARTESIAN_POINT('Ctrl Pts',(62.7241253003464,-32.7632504637629,
-213.613097227511));
#217880=CARTESIAN_POINT('Ctrl Pts',(62.7427109763742,-31.6158487719858,
-213.732605809556));
#217881=CARTESIAN_POINT('Ctrl Pts',(62.7617431549812,-30.470412971391,-213.718959456451));
#217882=CARTESIAN_POINT('Ctrl Pts',(62.7647391511292,-30.2901014412562,
-213.716811282971));
#217883=CARTESIAN_POINT('Ctrl Pts',(62.767746212059,-30.1098386199596,-213.711363604099));
#217884=CARTESIAN_POINT('Ctrl Pts',(62.770766775426,-29.9296268901167,-213.702478069901));
#217885=CARTESIAN_POINT('Ctrl Pts',(62.7725414402335,-29.8237474974408,
-213.697257571961));
#217886=CARTESIAN_POINT('Ctrl Pts',(62.7743209052535,-29.7178858577718,
-213.690842589647));
#217887=CARTESIAN_POINT('Ctrl Pts',(62.7761057740119,-29.6120425444016,
-213.683199054815));
#217888=CARTESIAN_POINT('Ctrl Pts',(62.7866097971823,-28.989150462946,-213.638216550309));
#217889=CARTESIAN_POINT('Ctrl Pts',(62.7973012895257,-28.3668822616731,
-213.550676253015));
#217890=CARTESIAN_POINT('Ctrl Pts',(62.8083033340944,-27.7453414694754,
-213.413639151457));
#217891=CARTESIAN_POINT('Ctrl Pts',(62.8099338015368,-27.6532311331184,
-213.39333069596));
#217892=CARTESIAN_POINT('Ctrl Pts',(62.811571077252,-27.5611367494674,-213.371935988233));
#217893=CARTESIAN_POINT('Ctrl Pts',(62.8132156027367,-27.4690586781095,
-213.349430181196));
#217894=CARTESIAN_POINT('Ctrl Pts',(62.8148166574626,-27.3794145633349,
-213.32751928407));
#217895=CARTESIAN_POINT('Ctrl Pts',(62.8164245864001,-27.2897858690399,
-213.3045551313));
#217896=CARTESIAN_POINT('Ctrl Pts',(62.8180397952865,-27.2001730524583,
-213.280514793433));
#217897=CARTESIAN_POINT('Ctrl Pts',(62.818858360563,-27.1547585301625,-213.268331486382));
#217898=CARTESIAN_POINT('Ctrl Pts',(62.8196787972069,-27.1093480871571,
-213.25587168702));
#217899=CARTESIAN_POINT('Ctrl Pts',(62.8205011614668,-27.063941785938,-213.243132215583));
#217900=CARTESIAN_POINT('Ctrl Pts',(62.820603956966,-27.0582660001277,-213.24153978217));
#217901=CARTESIAN_POINT('Ctrl Pts',(62.8207068130079,-27.0525903054936,
-213.239941216059));
#217902=CARTESIAN_POINT('Ctrl Pts',(62.8208096296676,-27.046914615143,-213.238342307309));
#217903=CARTESIAN_POINT('Ctrl Pts',(62.8209124463233,-27.0412389250115,
-213.23674339862));
#217904=CARTESIAN_POINT('Ctrl Pts',(62.8210151618557,-27.03556318545,-213.23514772473));
#217905=CARTESIAN_POINT('Ctrl Pts',(62.821117776347,-27.0298873965556,-213.233555280696));
#217906=CARTESIAN_POINT('Ctrl Pts',(62.8213230053217,-27.0185358191961,
-213.230370392749));
#217907=CARTESIAN_POINT('Ctrl Pts',(62.8215278301309,-27.0071840445339,
-213.22719842432));
#217908=CARTESIAN_POINT('Ctrl Pts',(62.8217322514279,-26.9958320733607,
-213.224039336346));
#217909=CARTESIAN_POINT('Ctrl Pts',(62.8221023145259,-26.9752816430423,
-213.218320451379));
#217910=CARTESIAN_POINT('Ctrl Pts',(62.8224710552458,-26.9547305687673,
-213.212643777775));
#217911=CARTESIAN_POINT('Ctrl Pts',(62.8228384774045,-26.9341788553177,
-213.207009087125));
#217912=CARTESIAN_POINT('Ctrl Pts',(62.8228769801512,-26.9320252088913,
-213.206418619015));
#217913=CARTESIAN_POINT('Ctrl Pts',(62.8229154684173,-26.9298715555002,
-213.205828611962));
#217914=CARTESIAN_POINT('Ctrl Pts',(62.8229539422071,-26.9277178951481,
-213.205239065704));
#217915=CARTESIAN_POINT('Ctrl Pts',(62.8245764233091,-26.8368957212833,
-213.180377265789));
#217916=CARTESIAN_POINT('Ctrl Pts',(62.8261731614529,-26.7460611681055,
-213.156334842928));
#217917=CARTESIAN_POINT('Ctrl Pts',(62.8277444695764,-26.6552145055668,
-213.133093149396));
#217918=CARTESIAN_POINT('Ctrl Pts',(62.8292202126583,-26.5698930261205,
-213.111264987287));
#217919=CARTESIAN_POINT('Ctrl Pts',(62.8306735455578,-26.4845608838062,
-213.090141906316));
#217920=CARTESIAN_POINT('Ctrl Pts',(62.8321046858337,-26.3992182785356,
-213.069710892685));
#217921=CARTESIAN_POINT('Ctrl Pts',(62.8367688988909,-26.1210791607011,
-213.003124407662));
#217922=CARTESIAN_POINT('Ctrl Pts',(62.8411971255009,-25.8428597458081,
-212.943883039828));
#217923=CARTESIAN_POINT('Ctrl Pts',(62.8453976824702,-25.5644780440299,
-212.891551576529));
#217924=CARTESIAN_POINT('Ctrl Pts',(62.8465846366303,-25.4858155424996,
-212.876764240344));
#217925=CARTESIAN_POINT('Ctrl Pts',(62.8477534065636,-25.407149458358,-212.862521456414));
#217926=CARTESIAN_POINT('Ctrl Pts',(62.8489040944972,-25.3284786414785,
-212.848818315902));
#217927=CARTESIAN_POINT('Ctrl Pts',(62.8589719385763,-24.640155165815,-212.728923878815));
#217928=CARTESIAN_POINT('Ctrl Pts',(62.867653735289,-23.9520875862966,-212.650037662992));
#217929=CARTESIAN_POINT('Ctrl Pts',(62.8750146865603,-23.2647003090921,
-212.608425061389));
#217930=CARTESIAN_POINT('Ctrl Pts',(62.8823756378316,-22.5773130318876,
-212.566812459786));
#217931=CARTESIAN_POINT('Ctrl Pts',(62.8884156923502,-21.8906064258735,
-212.562474309897));
#217932=CARTESIAN_POINT('Ctrl Pts',(62.8931986251439,-21.2050511218171,
-212.591707581156));
#217933=CARTESIAN_POINT('Ctrl Pts',(62.8935577382081,-21.1535781288824,
-212.593902479154));
#217934=CARTESIAN_POINT('Ctrl Pts',(62.8939097569274,-21.1021052395343,
-212.596289051621));
#217935=CARTESIAN_POINT('Ctrl Pts',(62.8942546885952,-21.0506330432678,
-212.598866899388));
#217936=CARTESIAN_POINT('Ctrl Pts',(62.8968212608728,-20.6676380203924,
-212.618048184355));
#217937=CARTESIAN_POINT('Ctrl Pts',(62.898993894224,-20.2848774438081,-212.647828821471));
#217938=CARTESIAN_POINT('Ctrl Pts',(62.900778786722,-19.9023518511915,-212.687972680865));
#217939=CARTESIAN_POINT('Ctrl Pts',(62.9023087147126,-19.5744684565815,
-212.722382156061));
#217940=CARTESIAN_POINT('Ctrl Pts',(62.9035537360166,-19.2467573919566,
-212.764406500889));
#217941=CARTESIAN_POINT('Ctrl Pts',(62.9045166573415,-18.9192122497013,
-212.81392668013));
#217942=CARTESIAN_POINT('Ctrl Pts',(62.9053466520591,-18.6368831218555,
-212.856610839387));
#217943=CARTESIAN_POINT('Ctrl Pts',(62.9059670124065,-18.3545500700666,
-212.904900139622));
#217944=CARTESIAN_POINT('Ctrl Pts',(62.9063776080623,-18.0726457860283,
-212.958691242021));
#217945=CARTESIAN_POINT('Ctrl Pts',(62.9064830589281,-18.0002459678496,
-212.972506094273));
#217946=CARTESIAN_POINT('Ctrl Pts',(62.9065746841136,-17.9278744301198,
-212.986683569855));
#217947=CARTESIAN_POINT('Ctrl Pts',(62.9066525023395,-17.8555384962728,
-213.00122136616));
#217948=CARTESIAN_POINT('Ctrl Pts',(62.9070069220114,-17.5260876814359,
-213.06743311714));
#217949=CARTESIAN_POINT('Ctrl Pts',(62.9070749640207,-17.197340288906,-213.141130341411));
#217950=CARTESIAN_POINT('Ctrl Pts',(62.9068586171446,-16.8692921444043,
-213.222255473336));
#217951=CARTESIAN_POINT('Ctrl Pts',(62.9068512161578,-16.8580699810933,
-213.225030674155));
#217952=CARTESIAN_POINT('Ctrl Pts',(62.9068434310689,-16.8468489287218,
-213.227817504345));
#217953=CARTESIAN_POINT('Ctrl Pts',(62.9068354227292,-16.8356281229708,
-213.230606932774));
#217954=CARTESIAN_POINT('Ctrl Pts',(62.9068274143987,-16.8244073300739,
-213.233396358007));
#217955=CARTESIAN_POINT('Ctrl Pts',(62.9068194222443,-16.81318550769,-213.236174929377));
#217956=CARTESIAN_POINT('Ctrl Pts',(62.9068114465212,-16.8019626469682,
-213.238942628495));
#217957=CARTESIAN_POINT('Ctrl Pts',(62.9068100308831,-16.7999706633578,
-213.239433876798));
#217958=CARTESIAN_POINT('Ctrl Pts',(62.9068086157626,-16.7979786470357,
-213.239924782582));
#217959=CARTESIAN_POINT('Ctrl Pts',(62.9068072011611,-16.7959865979526,
-213.240415345746));
#217960=CARTESIAN_POINT('Ctrl Pts',(62.9067926759976,-16.7755321875305,
-213.245452460734));
#217961=CARTESIAN_POINT('Ctrl Pts',(62.9067782084953,-16.755074364096,-213.250453275771));
#217962=CARTESIAN_POINT('Ctrl Pts',(62.9067638003454,-16.7346131155667,
-213.255417662646));
#217963=CARTESIAN_POINT('Ctrl Pts',(62.9067321774736,-16.6897049597551,
-213.266313452264));
#217964=CARTESIAN_POINT('Ctrl Pts',(62.9067008405294,-16.6447803048274,
-213.277033762557));
#217965=CARTESIAN_POINT('Ctrl Pts',(62.9066698070808,-16.5998390244792,
-213.287577252305));
#217966=CARTESIAN_POINT('Ctrl Pts',(62.9066077395427,-16.5099555355157,
-213.308664449577));
#217967=CARTESIAN_POINT('Ctrl Pts',(62.9065468864317,-16.4200055414544,
-213.329044330242));
#217968=CARTESIAN_POINT('Ctrl Pts',(62.9064873833149,-16.3299880540902,
-213.348706398678));
#217969=CARTESIAN_POINT('Ctrl Pts',(62.9063683745862,-16.14994930492,-213.388031359981));
#217970=CARTESIAN_POINT('Ctrl Pts',(62.9062547727652,-15.9696405404371,
-213.424484631683));
#217971=CARTESIAN_POINT('Ctrl Pts',(62.9061475795573,-15.7890542301196,
-213.457986204279));
#217972=CARTESIAN_POINT('Ctrl Pts',(62.9059331838863,-15.4278660176251,
-213.524992242004));
#217973=CARTESIAN_POINT('Ctrl Pts',(62.9057445834295,-15.0655667619647,
-213.58018242881));
#217974=CARTESIAN_POINT('Ctrl Pts',(62.905589362047,-14.7020974635233,-213.622929699831));
#217975=CARTESIAN_POINT('Ctrl Pts',(62.9052798509934,-13.9773405794218,
-213.708167652755));
#217976=CARTESIAN_POINT('Ctrl Pts',(62.9051047269462,-13.2479237446018,
-213.743849925036));
#217977=CARTESIAN_POINT('Ctrl Pts',(62.9051090261727,-12.5134449350678,
-213.725695782834));
#217978=CARTESIAN_POINT('Ctrl Pts',(62.9051090395082,-12.5111666950214,
-213.725639471484));
#217979=CARTESIAN_POINT('Ctrl Pts',(62.9051090545696,-12.5088884062743,
-213.725582642177));
#217980=CARTESIAN_POINT('Ctrl Pts',(62.9051090713583,-12.5066100688143,
-213.725525294786));
#217981=CARTESIAN_POINT('Ctrl Pts',(62.9051117186635,-12.1473516978959,
-213.716482503419));
#217982=CARTESIAN_POINT('Ctrl Pts',(62.9051569926989,-11.7868835043618,
-213.694572753784));
#217983=CARTESIAN_POINT('Ctrl Pts',(62.9052478305722,-11.4251692471516,
-213.659411822611));
#217984=CARTESIAN_POINT('Ctrl Pts',(62.9052501495695,-11.4159350548302,
-213.658514200263));
#217985=CARTESIAN_POINT('Ctrl Pts',(62.905252498141,-11.4066999814362,-213.657607942971));
#217986=CARTESIAN_POINT('Ctrl Pts',(62.9052548763439,-11.3974640308012,
-213.656693043944));
#217987=CARTESIAN_POINT('Ctrl Pts',(62.9053396597116,-11.0682006948942,
-213.624076725649));
#217988=CARTESIAN_POINT('Ctrl Pts',(62.9054625664031,-10.7375855896784,
-213.580337710379));
#217989=CARTESIAN_POINT('Ctrl Pts',(62.9056218033686,-10.409778663214,-213.526208718247));
#217990=CARTESIAN_POINT('Ctrl Pts',(62.9056341733888,-10.3843136067658,
-213.522003810635));
#217991=CARTESIAN_POINT('Ctrl Pts',(62.905646762572,-10.358865493353,-213.517736228733));
#217992=CARTESIAN_POINT('Ctrl Pts',(62.9056595700396,-10.3334362698611,
-213.513406328741));
#217993=CARTESIAN_POINT('Ctrl Pts',(62.9056676765601,-10.317340775653,-213.510665707099));
#217994=CARTESIAN_POINT('Ctrl Pts',(62.9056758700813,-10.3012520481916,
-213.507900031565));
#217995=CARTESIAN_POINT('Ctrl Pts',(62.9056841503679,-10.2851705845394,
-213.505109387712));
#217996=CARTESIAN_POINT('Ctrl Pts',(62.9058495001971,-9.96403831223543,
-213.449382756036));
#217997=CARTESIAN_POINT('Ctrl Pts',(62.9060495440864,-9.64477667567345,
-213.383630454476));
#217998=CARTESIAN_POINT('Ctrl Pts',(62.9062818494613,-9.32750692224311,
-213.308308849075));
#217999=CARTESIAN_POINT('Ctrl Pts',(62.9062995203884,-9.30337295346862,
-213.302579310558));
#218000=CARTESIAN_POINT('Ctrl Pts',(62.9063173779087,-9.27925050600009,
-213.296794425732));
#218001=CARTESIAN_POINT('Ctrl Pts',(62.9063354209129,-9.25513963110861,
-213.290954407383));
#218002=CARTESIAN_POINT('Ctrl Pts',(62.9063523663721,-9.23249540595939,
-213.28546963377));
#218003=CARTESIAN_POINT('Ctrl Pts',(62.9063694755794,-9.20986097578642,
-213.279936139709));
#218004=CARTESIAN_POINT('Ctrl Pts',(62.9063867476374,-9.18723633851541,
-213.274354087607));
#218005=CARTESIAN_POINT('Ctrl Pts',(62.9064214242477,-9.14181351020547,
-213.263147163439));
#218006=CARTESIAN_POINT('Ctrl Pts',(62.9064567545313,-9.09643013343645,
-213.251744618045));
#218007=CARTESIAN_POINT('Ctrl Pts',(62.9064927284741,-9.05108616789961,
-213.240147881952));
#218008=CARTESIAN_POINT('Ctrl Pts',(62.9065017219161,-9.03975023169194,
-213.23724871204));
#218009=CARTESIAN_POINT('Ctrl Pts',(62.9065107555831,-9.02841675862816,
-213.234337405481));
#218010=CARTESIAN_POINT('Ctrl Pts',(62.9065198293118,-9.01708574800015,
-213.231413985003));
#218011=CARTESIAN_POINT('Ctrl Pts',(62.9065289030347,-9.00575474452809,
-213.228490566372));
#218012=CARTESIAN_POINT('Ctrl Pts',(62.9065377477119,-8.99442319446877,
-213.225569813864));
#218013=CARTESIAN_POINT('Ctrl Pts',(62.9065461779452,-8.98308903056771,
-213.222661899751));
#218014=CARTESIAN_POINT('Ctrl Pts',(62.9065630384181,-8.96042069442155,
-213.216846069384));
#218015=CARTESIAN_POINT('Ctrl Pts',(62.9065784765558,-8.93774453557201,
-213.211068662567));
#218016=CARTESIAN_POINT('Ctrl Pts',(62.9065924909309,-8.91506058486269,
-213.205329682185));
#218017=CARTESIAN_POINT('Ctrl Pts',(62.906632507978,-8.85028818379569,-213.188942433607));
#218018=CARTESIAN_POINT('Ctrl Pts',(62.9066609166417,-8.7854522548987,-213.172868479925));
#218019=CARTESIAN_POINT('Ctrl Pts',(62.9066776826504,-8.72055350098855,
-213.157107960246));
#218020=CARTESIAN_POINT('Ctrl Pts',(62.9066844034019,-8.69453846021989,
-213.1507902648));
#218021=CARTESIAN_POINT('Ctrl Pts',(62.9066892533842,-8.66851311367876,
-213.144522883906));
#218022=CARTESIAN_POINT('Ctrl Pts',(62.9066922303343,-8.64247748890024,
-213.13830582419));
#218023=CARTESIAN_POINT('Ctrl Pts',(62.9067096741274,-8.48991865034706,
-213.101876223688));
#218024=CARTESIAN_POINT('Ctrl Pts',(62.9066627545095,-8.33741593724109,
-213.067272060264));
#218025=CARTESIAN_POINT('Ctrl Pts',(62.906552054195,-8.18500124845787,-213.034473300197));
#218026=CARTESIAN_POINT('Ctrl Pts',(62.9065307100423,-8.15561413774858,
-213.02814936383));
#218027=CARTESIAN_POINT('Ctrl Pts',(62.906506993431,-8.12623007030402,-213.021892565579));
#218028=CARTESIAN_POINT('Ctrl Pts',(62.9064809085264,-8.09684923724608,
-213.015702751583));
#218029=CARTESIAN_POINT('Ctrl Pts',(62.9056899601275,-7.20596145140312,
-212.828014755284));
#218030=CARTESIAN_POINT('Ctrl Pts',(62.9027366747181,-6.31764267914539,
-212.700961335132));
#218031=CARTESIAN_POINT('Ctrl Pts',(62.8976715771841,-5.43185195165195,
-212.632707606633));
#218032=CARTESIAN_POINT('Ctrl Pts',(62.8947900085006,-4.92791953904146,
-212.593877592946));
#218033=CARTESIAN_POINT('Ctrl Pts',(62.8912249487153,-4.42480439538323,
-212.574078170132));
#218034=CARTESIAN_POINT('Ctrl Pts',(62.8869856905768,-3.92249156539548,
-212.572970530223));
#218035=CARTESIAN_POINT('Ctrl Pts',(62.8865147226824,-3.8666862314995,-212.572847475005));
#218036=CARTESIAN_POINT('Ctrl Pts',(62.8860354164368,-3.81089071961118,
-212.572956060008));
#218037=CARTESIAN_POINT('Ctrl Pts',(62.885547785291,-3.75510503118202,-212.573295788909));
#218038=CARTESIAN_POINT('Ctrl Pts',(62.8793243758262,-3.04313824163497,
-212.577631590838));
#218039=CARTESIAN_POINT('Ctrl Pts',(62.8717459291031,-2.332772344863,-212.619539913621));
#218040=CARTESIAN_POINT('Ctrl Pts',(62.862782948286,-1.62412895620658,-212.701365863942));
#218041=CARTESIAN_POINT('Ctrl Pts',(62.8546488502804,-0.981019828565715,
-212.775624675034));
#218042=CARTESIAN_POINT('Ctrl Pts',(62.8453744839341,-0.339328956701179,
-212.882759122652));
#218043=CARTESIAN_POINT('Ctrl Pts',(62.8349373318117,0.300889820690812,
-213.0245235881));
#218044=CARTESIAN_POINT('Ctrl Pts',(62.833607314137,0.382473597531864,-213.0425887885));
#218045=CARTESIAN_POINT('Ctrl Pts',(62.8322582595392,0.464033344884034,
-213.0612252722));
#218046=CARTESIAN_POINT('Ctrl Pts',(62.8308901810048,0.545568613619925,
-213.080433504715));
#218047=CARTESIAN_POINT('Ctrl Pts',(62.8293216865052,0.639048349845703,
-213.102455637427));
#218048=CARTESIAN_POINT('Ctrl Pts',(62.8277279878957,0.732495388150152,
-213.125241286057));
#218049=CARTESIAN_POINT('Ctrl Pts',(62.8261090055383,0.825909081274457,
-213.148796974995));
#218050=CARTESIAN_POINT('Ctrl Pts',(62.8246401331402,0.910661577070946,
-213.170168610789));
#218051=CARTESIAN_POINT('Ctrl Pts',(62.8231504392874,0.995387120789026,
-213.19217425345));
#218052=CARTESIAN_POINT('Ctrl Pts',(62.8216398034464,1.08008493804852,-213.214822482474));
#218053=CARTESIAN_POINT('Ctrl Pts',(62.8212428495944,1.10234121180029,-213.220773818665));
#218054=CARTESIAN_POINT('Ctrl Pts',(62.8208444494793,1.12459557041626,-213.226769539353));
#218055=CARTESIAN_POINT('Ctrl Pts',(62.8204446007168,1.1468479993255,-213.232809812552));
#218056=CARTESIAN_POINT('Ctrl Pts',(62.8202446762942,1.15797421608229,-213.235829949777));
#218057=CARTESIAN_POINT('Ctrl Pts',(62.8200446532189,1.16910062229262,-213.238845621166));
#218058=CARTESIAN_POINT('Ctrl Pts',(62.8198447802284,1.18022785110113,-213.241842094699));
#218059=CARTESIAN_POINT('Ctrl Pts',(62.8196449071674,1.19135508383185,-213.244838569288));
#218060=CARTESIAN_POINT('Ctrl Pts',(62.8194451061373,1.20248294022609,-213.247820468069));
#218061=CARTESIAN_POINT('Ctrl Pts',(62.8192453767934,1.21361141859933,-213.250787808692));
#218062=CARTESIAN_POINT('Ctrl Pts',(62.8184464580711,1.25812540713238,-213.262657191193));
#218063=CARTESIAN_POINT('Ctrl Pts',(62.8176486863074,1.30264934735082,-213.27429364379));
#218064=CARTESIAN_POINT('Ctrl Pts',(62.8168520397832,1.34718313255599,-213.285698279349));
#218065=CARTESIAN_POINT('Ctrl Pts',(62.8168331493297,1.34823913841709,-213.28596871138));
#218066=CARTESIAN_POINT('Ctrl Pts',(62.8168142595089,1.3492951498137,-213.286239013068));
#218067=CARTESIAN_POINT('Ctrl Pts',(62.8167953703204,1.35035116674446,-213.286509184428));
#218068=CARTESIAN_POINT('Ctrl Pts',(62.8152210633643,1.43836420129823,-213.309026438185));
#218069=CARTESIAN_POINT('Ctrl Pts',(62.8136511488776,1.52641572030258,-213.330638365248));
#218070=CARTESIAN_POINT('Ctrl Pts',(62.8120854563785,1.61450537353353,-213.351353373465));
#218071=CARTESIAN_POINT('Ctrl Pts',(62.8074297466584,1.87644688185748,-213.412951078738));
#218072=CARTESIAN_POINT('Ctrl Pts',(62.8028113125304,2.13872544174159,-213.466621196677));
#218073=CARTESIAN_POINT('Ctrl Pts',(62.7982260322374,2.40133274732117,-213.512564584869));
#218074=CARTESIAN_POINT('Ctrl Pts',(62.7965691479007,2.4962255136348,-213.529166161088));
#218075=CARTESIAN_POINT('Ctrl Pts',(62.7949165988104,2.59116092814633,-213.544758707681));
#218076=CARTESIAN_POINT('Ctrl Pts',(62.7932681861794,2.6861388388309,-213.559351754428));
#218077=CARTESIAN_POINT('Ctrl Pts',(62.7870578081227,3.04396716487127,-213.614330911704));
#218078=CARTESIAN_POINT('Ctrl Pts',(62.7808961247407,3.40303459047103,-213.655110348135));
#218079=CARTESIAN_POINT('Ctrl Pts',(62.7748157638915,3.76060806585576,-213.682219323134));
#218080=CARTESIAN_POINT('Ctrl Pts',(62.7705733532611,4.0100954812797,-213.701133891952));
#218081=CARTESIAN_POINT('Ctrl Pts',(62.7663688307482,4.25893819616771,-213.71344333557));
#218082=CARTESIAN_POINT('Ctrl Pts',(62.7621968858992,4.50717455612251,-213.719490676919));
#218083=CARTESIAN_POINT('Ctrl Pts',(62.760389727327,4.61470293486154,-213.722110199743));
#218084=CARTESIAN_POINT('Ctrl Pts',(62.758588694089,4.72211697151828,-213.723554528345));
#218085=CARTESIAN_POINT('Ctrl Pts',(62.756793361705,4.8294193693953,-213.723851522448));
#218086=CARTESIAN_POINT('Ctrl Pts',(62.744914568547,5.53938427675417,-213.725816580036));
#218087=CARTESIAN_POINT('Ctrl Pts',(62.7332829196987,6.24447623948652,-213.677701667471));
#218088=CARTESIAN_POINT('Ctrl Pts',(62.7217741472389,6.94546014142257,-213.587382621443));
#218089=CARTESIAN_POINT('Ctrl Pts',(62.7160202469305,7.29592249555947,-213.542226911865));
#218090=CARTESIAN_POINT('Ctrl Pts',(62.7102974318193,7.64535562408464,-213.486497387274));
#218091=CARTESIAN_POINT('Ctrl Pts',(62.7045905440092,7.99385039894293,-213.421128855621));
#218092=CARTESIAN_POINT('Ctrl Pts',(62.7017372091522,8.16809112729064,-213.388445838864));
#218093=CARTESIAN_POINT('Ctrl Pts',(62.6988879008502,8.34209702777281,-213.353350616144));
#218094=CARTESIAN_POINT('Ctrl Pts',(62.6960409729441,8.51587804140931,-213.31594549485));
#218095=CARTESIAN_POINT('Ctrl Pts',(62.6953306860554,8.55923508435001,-213.306613201199));
#218096=CARTESIAN_POINT('Ctrl Pts',(62.6946205479401,8.6025781254609,-213.297137089371));
#218097=CARTESIAN_POINT('Ctrl Pts',(62.693910534767,8.64590730924635,-213.287518647044));
#218098=CARTESIAN_POINT('Ctrl Pts',(62.6931976571302,8.68941129946275,-213.277861400257));
#218099=CARTESIAN_POINT('Ctrl Pts',(62.6924849069969,8.73290123523708,-213.268060682277));
#218100=CARTESIAN_POINT('Ctrl Pts',(62.6917722569378,8.77637732701844,-213.258118114802));
#218101=CARTESIAN_POINT('Ctrl Pts',(62.6914166494633,8.79807159758174,-213.253156842064));
#218102=CARTESIAN_POINT('Ctrl Pts',(62.6910610669504,8.81976242088063,-213.248160247012));
#218103=CARTESIAN_POINT('Ctrl Pts',(62.6907055060663,8.84144982288392,-213.243128526156));
#218104=CARTESIAN_POINT('Ctrl Pts',(62.69034994597,8.86313717683587,-213.238096816449));
#218105=CARTESIAN_POINT('Ctrl Pts',(62.6899947488889,8.88481939248927,-213.233012444835));
#218106=CARTESIAN_POINT('Ctrl Pts',(62.6896387405559,8.90650238461306,-213.227935756798));
#218107=CARTESIAN_POINT('Ctrl Pts',(62.6889267268058,8.94986819125055,-213.217782422308));
#218108=CARTESIAN_POINT('Ctrl Pts',(62.6882099166076,8.99324491620445,-213.20773948302));
#218109=CARTESIAN_POINT('Ctrl Pts',(62.6874882954834,9.03663265289044,-213.197807426414));
#218110=CARTESIAN_POINT('Ctrl Pts',(62.6868204901171,9.0767846972564,-213.1886160648));
#218111=CARTESIAN_POINT('Ctrl Pts',(62.6861485996542,9.11694554599575,-213.179518348821));
#218112=CARTESIAN_POINT('Ctrl Pts',(62.6854726096978,9.15711522005327,-213.170514913905));
#218113=CARTESIAN_POINT('Ctrl Pts',(62.6826037415343,9.3275933432039,-213.132304778465));
#218114=CARTESIAN_POINT('Ctrl Pts',(62.6796606062759,9.49823764842399,-213.0958088569));
#218115=CARTESIAN_POINT('Ctrl Pts',(62.6766425417446,9.66904980342632,-213.061049681902));
#218116=CARTESIAN_POINT('Ctrl Pts',(62.6706064126818,10.010674113431,-212.991531331906));
#218117=CARTESIAN_POINT('Ctrl Pts',(62.664270812359,10.3529550669585,-212.928960848345));
#218118=CARTESIAN_POINT('Ctrl Pts',(62.6576327768096,10.6957266313347,-212.873621170708));
#218119=CARTESIAN_POINT('Ctrl Pts',(62.6473143570134,11.2285440393083,-212.787599030422));
#218120=CARTESIAN_POINT('Ctrl Pts',(62.6362643202696,11.7626593744765,-212.718966127623));
#218121=CARTESIAN_POINT('Ctrl Pts',(62.6244492722701,12.298183791666,-212.669131165341));
#218122=CARTESIAN_POINT('Ctrl Pts',(62.6210626304398,12.4516854441756,-212.654846570993));
#218123=CARTESIAN_POINT('Ctrl Pts',(62.6176131332116,12.6053025653798,-212.642106558566));
#218124=CARTESIAN_POINT('Ctrl Pts',(62.6140999935327,12.7590370278545,-212.630944584506));
#218125=CARTESIAN_POINT('Ctrl Pts',(62.6105014211192,12.9165100139116,-212.619511172914));
#218126=CARTESIAN_POINT('Ctrl Pts',(62.6068362958068,13.0740938080762,-212.609737755954));
#218127=CARTESIAN_POINT('Ctrl Pts',(62.6031038882692,13.2317919256033,-212.60165208257));
#218128=CARTESIAN_POINT('Ctrl Pts',(62.5920978381641,13.696809040022,-212.577809207562));
#218129=CARTESIAN_POINT('Ctrl Pts',(62.5804979949266,14.1630945001764,-212.568752968163));
#218130=CARTESIAN_POINT('Ctrl Pts',(62.5682752553844,14.6305393352631,-212.5760493123));
#218131=CARTESIAN_POINT('Ctrl Pts',(62.5664789095161,14.699238549155,-212.577121637993));
#218132=CARTESIAN_POINT('Ctrl Pts',(62.564669105666,14.7679628448817,-212.578547253472));
#218133=CARTESIAN_POINT('Ctrl Pts',(62.5628457474452,14.8367119180636,-212.580331218975));
#218134=CARTESIAN_POINT('Ctrl Pts',(62.5582940634694,15.0083315434169,-212.584784566155));
#218135=CARTESIAN_POINT('Ctrl Pts',(62.5536582189233,15.1800866651588,-212.591481763735));
#218136=CARTESIAN_POINT('Ctrl Pts',(62.5489369347187,15.3519656949738,-212.600500512767));
#218137=CARTESIAN_POINT('Ctrl Pts',(62.5345339878629,15.8763070446592,-212.628013485379));
#218138=CARTESIAN_POINT('Ctrl Pts',(62.5194888785073,16.3962308632545,-212.676843393471));
#218139=CARTESIAN_POINT('Ctrl Pts',(62.5037997387388,16.9113773860641,-212.748829194443));
#218140=CARTESIAN_POINT('Ctrl Pts',(62.4982710429057,17.0929098649717,-212.774196270252));
#218141=CARTESIAN_POINT('Ctrl Pts',(62.4926620464245,17.2738497478371,-212.802456316523));
#218142=CARTESIAN_POINT('Ctrl Pts',(62.4869727360513,17.4541800510743,-212.833687547545));
#218143=CARTESIAN_POINT('Ctrl Pts',(62.471224815544,17.953331458564,-212.920135097635));
#218144=CARTESIAN_POINT('Ctrl Pts',(62.4548621630433,18.4478214139081,-213.029285839066));
#218145=CARTESIAN_POINT('Ctrl Pts',(62.4378715929549,18.937051788145,-213.164110067595));
#218146=CARTESIAN_POINT('Ctrl Pts',(62.4313084944047,19.126031153945,-213.216189820905));
#218147=CARTESIAN_POINT('Ctrl Pts',(62.4246524255105,19.3141920754888,-213.27211651907));
#218148=CARTESIAN_POINT('Ctrl Pts',(62.4179027766836,19.5014992838758,-213.332056784808));
#218149=CARTESIAN_POINT('Ctrl Pts',(62.4127593088452,19.6442339100702,-213.377733358058));
#218150=CARTESIAN_POINT('Ctrl Pts',(62.407553332654,19.7866395914419,-213.425870497296));
#218151=CARTESIAN_POINT('Ctrl Pts',(62.4022963811677,19.9284129896787,-213.476422874377));
#218152=CARTESIAN_POINT('Ctrl Pts',(62.3923400029788,20.1969240409302,-213.572166307785));
#218153=CARTESIAN_POINT('Ctrl Pts',(62.3821761384627,20.4638252083206,-213.676819485766));
#218154=CARTESIAN_POINT('Ctrl Pts',(62.3718829557378,20.7269505827977,-213.790195793082));
#218155=CARTESIAN_POINT('Ctrl Pts',(62.3696094190776,20.7850691648823,-213.815238114585));
#218156=CARTESIAN_POINT('Ctrl Pts',(62.3673295818174,20.8430033464101,-213.840705944543));
#218157=CARTESIAN_POINT('Ctrl Pts',(62.3650443003753,20.9007294710424,-213.866597158579));
#218158=CARTESIAN_POINT('',(61.6307906445947,-35.3347454921122,-216.138336328427));
#218159=CARTESIAN_POINT('Ctrl Pts',(61.6307906445947,-35.3347454921122,
-216.138336328427));
#218160=CARTESIAN_POINT('Ctrl Pts',(61.6308040666128,-35.3417600414872,
-216.136573459783));
#218161=CARTESIAN_POINT('Ctrl Pts',(61.6308188619637,-35.3487748507191,
-216.134811634988));
#218162=CARTESIAN_POINT('Ctrl Pts',(61.6310464376898,-35.3557090446008,
-216.132792415564));
#218163=CARTESIAN_POINT('Ctrl Pts',(61.6312601624137,-35.3622212007881,
-216.130896092432));
#218164=CARTESIAN_POINT('Ctrl Pts',(61.6316614890751,-35.3686622440919,
-216.128772703321));
#218165=CARTESIAN_POINT('Ctrl Pts',(61.6319689130928,-35.375140928003,-216.1267658518));
#218166=CARTESIAN_POINT('Ctrl Pts',(61.6326034322233,-35.3885128464071,
-216.122623736647));
#218167=CARTESIAN_POINT('Ctrl Pts',(61.632838216593,-35.4020451702368,-216.118978299824));
#218168=CARTESIAN_POINT('Ctrl Pts',(61.6331431613905,-35.4155525532659,
-216.115257033341));
#218169=CARTESIAN_POINT('Ctrl Pts',(61.633753020954,-35.4425659890872,-216.107814866852));
#218170=CARTESIAN_POINT('Ctrl Pts',(61.6346427632318,-35.4694795358603,
-216.100068857125));
#218171=CARTESIAN_POINT('Ctrl Pts',(61.6354796087042,-35.4964244671033,
-216.092424963586));
#218172=CARTESIAN_POINT('Ctrl Pts',(61.6371531603808,-35.5503098454024,
-216.077138448608));
#218173=CARTESIAN_POINT('Ctrl Pts',(61.6386161988779,-35.6043209298415,
-216.062261116095));
#218174=CARTESIAN_POINT('Ctrl Pts',(61.6401043809673,-35.658364025579,-216.047507238149));
#218175=CARTESIAN_POINT('Ctrl Pts',(61.6430804365425,-35.766439010163,-216.018002541761));
#218176=CARTESIAN_POINT('Ctrl Pts',(61.646155530417,-35.8746417481196,-215.98899042091));
#218177=CARTESIAN_POINT('Ctrl Pts',(61.649162113972,-35.9830350128333,-215.960691861929));
#218178=CARTESIAN_POINT('Ctrl Pts',(61.6551756296919,-36.1998341103363,
-215.904091462781));
#218179=CARTESIAN_POINT('Ctrl Pts',(61.6609168613943,-36.4173956880617,
-215.850346973261));
#218180=CARTESIAN_POINT('Ctrl Pts',(61.6665143671927,-36.6356225549127,
-215.799441647033));
#218181=CARTESIAN_POINT('Ctrl Pts',(61.6721571209959,-36.855613480733,-215.748124822448));
#218182=CARTESIAN_POINT('Ctrl Pts',(61.6776529206739,-37.0762803739165,
-215.699692593711));
#218183=CARTESIAN_POINT('Ctrl Pts',(61.682966870277,-37.2975828727595,-215.654351989951));
#218184=CARTESIAN_POINT('Ctrl Pts',(61.6881722529671,-37.5143640398369,
-215.609937719663));
#218185=CARTESIAN_POINT('Ctrl Pts',(61.6932031661431,-37.7317551162009,
-215.568490060376));
#218186=CARTESIAN_POINT('Ctrl Pts',(61.6980595479273,-37.9497193529901,
-215.530178847675));
#218187=CARTESIAN_POINT('Ctrl Pts',(61.7021486633458,-38.1332471234445,
-215.497920475596));
#218188=CARTESIAN_POINT('Ctrl Pts',(61.7061154994121,-38.3171775092552,
-215.467884589685));
#218189=CARTESIAN_POINT('Ctrl Pts',(61.7099526889049,-38.5014704241579,
-215.440197130652));
#218190=CARTESIAN_POINT('Ctrl Pts',(61.7155196281875,-38.7688399323387,
-215.400028563628));
#218191=CARTESIAN_POINT('Ctrl Pts',(61.7208119697472,-39.0369744580731,
-215.364802915884));
#218192=CARTESIAN_POINT('Ctrl Pts',(61.7258355244156,-39.305719263793,-215.334904757817));
#218193=CARTESIAN_POINT('Ctrl Pts',(61.7303410289492,-39.5467499722198,
-215.30808982385));
#218194=CARTESIAN_POINT('Ctrl Pts',(61.7346309998384,-39.7882688950653,
-215.285559347836));
#218195=CARTESIAN_POINT('Ctrl Pts',(61.7386614013115,-40.0301288296822,
-215.267705907674));
#218196=CARTESIAN_POINT('Ctrl Pts',(61.7418669752936,-40.2224917788592,
-215.253506199865));
#218197=CARTESIAN_POINT('Ctrl Pts',(61.7449089826414,-40.4150698378095,
-215.242265088223));
#218198=CARTESIAN_POINT('Ctrl Pts',(61.7477803186499,-40.6077707354279,
-215.234180086954));
#218199=CARTESIAN_POINT('Ctrl Pts',(61.7510847334047,-40.8295363830086,
-215.224875638639));
#218200=CARTESIAN_POINT('Ctrl Pts',(61.7541605291425,-41.0514720876124,
-215.21975341874));
#218201=CARTESIAN_POINT('Ctrl Pts',(61.7569816337569,-41.2734309002291,
-215.219176498584));
#218202=CARTESIAN_POINT('Ctrl Pts',(61.7577170450897,-41.3312915784105,
-215.219026105855));
#218203=CARTESIAN_POINT('Ctrl Pts',(61.7584352929738,-41.3891536203518,
-215.219184613554));
#218204=CARTESIAN_POINT('Ctrl Pts',(61.7591360681483,-41.4470135072824,
-215.21965872786));
#218205=CARTESIAN_POINT('Ctrl Pts',(61.7610546287376,-41.6054205154189,
-215.220956743338));
#218206=CARTESIAN_POINT('Ctrl Pts',(61.7628416990792,-41.7638121989732,
-215.224620350087));
#218207=CARTESIAN_POINT('Ctrl Pts',(61.7644946995693,-41.9221090036954,
-215.230787163063));
#218208=CARTESIAN_POINT('Ctrl Pts',(61.7666911381223,-42.1324472382017,
-215.238981368601));
#218209=CARTESIAN_POINT('Ctrl Pts',(61.7686498260413,-42.3426193701357,
-215.251595075326));
#218210=CARTESIAN_POINT('Ctrl Pts',(61.7703482765748,-42.5524019980439,
-215.269012080392));
#218211=CARTESIAN_POINT('Ctrl Pts',(61.7719995865043,-42.7563620955974,
-215.28594567536));
#218212=CARTESIAN_POINT('Ctrl Pts',(61.773404874694,-42.959953962892,-215.307419583956));
#218213=CARTESIAN_POINT('Ctrl Pts',(61.7745274697019,-43.1629057175116,
-215.33385125057));
#218214=CARTESIAN_POINT('Ctrl Pts',(61.7756179114226,-43.3600445422469,
-215.359525863247));
#218215=CARTESIAN_POINT('Ctrl Pts',(61.7764416279693,-43.5565795724041,
-215.389878433321));
#218216=CARTESIAN_POINT('Ctrl Pts',(61.776979990947,-43.7522133493642,-215.425304673598));
#218217=CARTESIAN_POINT('Ctrl Pts',(61.7772599446031,-43.8539446967897,
-215.443726641489));
#218218=CARTESIAN_POINT('Ctrl Pts',(61.7774630868531,-43.9554311411284,
-215.463520493776));
#218219=CARTESIAN_POINT('Ctrl Pts',(61.7775694692765,-44.0566083899622,
-215.484773367159));
#218220=CARTESIAN_POINT('Ctrl Pts',(61.7776616631061,-44.1442912770964,
-215.503191670874));
#218221=CARTESIAN_POINT('Ctrl Pts',(61.7776812199491,-44.2317418789998,
-215.522705760019));
#218222=CARTESIAN_POINT('Ctrl Pts',(61.7776158976463,-44.3189153994202,
-215.543372349475));
#218223=CARTESIAN_POINT('Ctrl Pts',(61.7774793872847,-44.5010903732092,
-215.586561329047));
#218224=CARTESIAN_POINT('Ctrl Pts',(61.776971632175,-44.6820611556678,-215.634785515999));
#218225=CARTESIAN_POINT('Ctrl Pts',(61.7762981534219,-44.861601675134,-215.688054278203));
#218226=CARTESIAN_POINT('Ctrl Pts',(61.7758058406997,-44.9928457291807,
-215.726993723886));
#218227=CARTESIAN_POINT('Ctrl Pts',(61.7752246785357,-45.1233178082053,
-215.76862450638));
#218228=CARTESIAN_POINT('Ctrl Pts',(61.7741149286305,-45.2524961979307,
-215.813816197241));
#218229=CARTESIAN_POINT('Ctrl Pts',(61.7737518188742,-45.2947633190072,
-215.828602901684));
#218230=CARTESIAN_POINT('Ctrl Pts',(61.7733322304229,-45.3368915425888,
-215.84377083554));
#218231=CARTESIAN_POINT('Ctrl Pts',(61.7728410789541,-45.3788614114542,
-215.85935045978));
#218232=CARTESIAN_POINT('Ctrl Pts',(61.7716501647156,-45.4806273993207,
-215.897126985992));
#218233=CARTESIAN_POINT('Ctrl Pts',(61.770039058637,-45.5814837181052,-215.937335255004));
#218234=CARTESIAN_POINT('Ctrl Pts',(61.7687805957718,-45.6818729518896,
-215.97872923867));
#218235=CARTESIAN_POINT('Ctrl Pts',(61.7679957127754,-45.7444840982349,
-216.004545998808));
#218236=CARTESIAN_POINT('Ctrl Pts',(61.7673475935058,-45.8069144706641,
-216.030823980101));
#218237=CARTESIAN_POINT('Ctrl Pts',(61.7670197730423,-45.8692809645529,
-216.057260894206));
#218238=CARTESIAN_POINT('',(62.0596235416337,-26.3318125162586,-215.724256795808));
#218239=CARTESIAN_POINT('Ctrl Pts',(62.0596235416336,-26.3318125162586,
-215.724256795808));
#218240=CARTESIAN_POINT('Ctrl Pts',(62.0577555696928,-26.4339470287308,
-215.753206765195));
#218241=CARTESIAN_POINT('Ctrl Pts',(62.0556509594839,-26.5309758697194,
-215.78008917588));
#218242=CARTESIAN_POINT('Ctrl Pts',(62.0535185542792,-26.6228963243231,
-215.804904027864));
#218243=CARTESIAN_POINT('Ctrl Pts',(62.0524523516769,-26.6688565516249,
-215.817311453857));
#218244=CARTESIAN_POINT('Ctrl Pts',(62.0513788550085,-26.7135398071411,
-215.829201990171));
#218245=CARTESIAN_POINT('Ctrl Pts',(62.0503220815731,-26.7569463787902,
-215.840575642485));
#218246=CARTESIAN_POINT('Ctrl Pts',(62.0497936948554,-26.7786496646148,
-215.846262468642));
#218247=CARTESIAN_POINT('Ctrl Pts',(62.0492694727596,-26.8000337816635,
-215.851820063874));
#218248=CARTESIAN_POINT('Ctrl Pts',(62.0487522794443,-26.8210987994165,
-215.857248440741));
#218249=CARTESIAN_POINT('Ctrl Pts',(62.0484936827866,-26.831631308293,-215.859962629175));
#218250=CARTESIAN_POINT('Ctrl Pts',(62.0482368423131,-26.8420840424851,
-215.862644512399));
#218251=CARTESIAN_POINT('Ctrl Pts',(62.0479821086777,-26.8524570116361,
-215.865294090431));
#218252=CARTESIAN_POINT('Ctrl Pts',(62.0477273750424,-26.8628299807872,
-215.867943668463));
#218253=CARTESIAN_POINT('Ctrl Pts',(62.0475055092753,-26.8718673652825,
-215.87024310001));
#218254=CARTESIAN_POINT('Ctrl Pts',(62.0472245741916,-26.8833366343711,
-215.873145907713));
#218255=CARTESIAN_POINT('Ctrl Pts',(62.044686460433,-26.9869559804883,-215.899371383265));
#218256=CARTESIAN_POINT('Ctrl Pts',(62.0420179406569,-27.0914557462519,
-215.92482563192));
#218257=CARTESIAN_POINT('Ctrl Pts',(62.0392255024341,-27.1958803121717,
-215.949297947245));
#218258=CARTESIAN_POINT('Ctrl Pts',(62.037072574512,-27.276390083844,-215.968165734741));
#218259=CARTESIAN_POINT('Ctrl Pts',(62.0348470483848,-27.3568551308637,
-215.986449843552));
#218260=CARTESIAN_POINT('Ctrl Pts',(62.0325730614187,-27.4368380736824,
-216.004053709611));
#218261=CARTESIAN_POINT('Ctrl Pts',(62.0273496175495,-27.6205622632014,
-216.044490531642));
#218262=CARTESIAN_POINT('Ctrl Pts',(62.0217447926267,-27.8051449629816,
-216.082146693372));
#218263=CARTESIAN_POINT('Ctrl Pts',(62.0157615800826,-27.9906023336393,
-216.117022203835));
#218264=CARTESIAN_POINT('Ctrl Pts',(62.0127699738106,-28.0833310189681,
-216.134459959066));
#218265=CARTESIAN_POINT('Ctrl Pts',(62.0096837379248,-28.1762783746767,
-216.151202530794));
#218266=CARTESIAN_POINT('Ctrl Pts',(62.0065029781599,-28.2694468745861,
-216.167249951255));
#218267=CARTESIAN_POINT('Ctrl Pts',(62.0045649202469,-28.326215056352,-216.17702775043));
#218268=CARTESIAN_POINT('Ctrl Pts',(62.0025715818842,-28.3837721485962,
-216.186658104095));
#218269=CARTESIAN_POINT('Ctrl Pts',(62.0005575197782,-28.440826636372,-216.195938775444));
#218270=CARTESIAN_POINT('Ctrl Pts',(61.999266083288,-28.4774105367535,-216.201889633464));
#218271=CARTESIAN_POINT('Ctrl Pts',(61.9979668951508,-28.5137878102374,
-216.207696719568));
#218272=CARTESIAN_POINT('Ctrl Pts',(61.9966772047599,-28.5496182363568,
-216.213306717361));
#218273=CARTESIAN_POINT('Ctrl Pts',(61.9834730873014,-28.916457563364,-216.270743037214));
#218274=CARTESIAN_POINT('Ctrl Pts',(61.9688293280833,-29.2870958911852,
-216.317548125342));
#218275=CARTESIAN_POINT('Ctrl Pts',(61.952786772668,-29.6616689192713,-216.353721981745));
#218276=CARTESIAN_POINT('Ctrl Pts',(61.9447654949604,-29.8489554333143,
-216.371808909947));
#218277=CARTESIAN_POINT('Ctrl Pts',(61.9363936787991,-30.0372261754395,
-216.387238030228));
#218278=CARTESIAN_POINT('Ctrl Pts',(61.927671271276,-30.2265006299287,-216.400009356926));
#218279=CARTESIAN_POINT('Ctrl Pts',(61.9233100675144,-30.3211378571733,
-216.406395020275));
#218280=CARTESIAN_POINT('Ctrl Pts',(61.918861178249,-30.416026012326,-216.412116210088));
#218281=CARTESIAN_POINT('Ctrl Pts',(61.9143242456229,-30.511167646582,-216.417172959074));
#218282=CARTESIAN_POINT('Ctrl Pts',(61.9122918465998,-30.5537880204005,
-216.419438219007));
#218283=CARTESIAN_POINT('Ctrl Pts',(61.9102417779571,-30.5964592611722,
-216.421570140067));
#218284=CARTESIAN_POINT('Ctrl Pts',(61.9081739949697,-30.6391815979838,
-216.423568722218));
#218285=CARTESIAN_POINT('Ctrl Pts',(61.9079338177601,-30.6441438845029,
-216.42380086161));
#218286=CARTESIAN_POINT('Ctrl Pts',(61.907693401551,-30.6491068603752,-216.424031202087));
#218287=CARTESIAN_POINT('Ctrl Pts',(61.9074527465505,-30.6540705259621,
-216.424259743649));
#218288=CARTESIAN_POINT('Ctrl Pts',(61.9062964708086,-30.6779194636387,
-216.425357817919));
#218289=CARTESIAN_POINT('Ctrl Pts',(61.9051346810113,-30.7017843234952,
-216.426414366295));
#218290=CARTESIAN_POINT('Ctrl Pts',(61.9039674023205,-30.7256651457048,
-216.427429384853));
#218291=CARTESIAN_POINT('Ctrl Pts',(61.9028001236297,-30.7495459679144,
-216.42844440341));
#218292=CARTESIAN_POINT('Ctrl Pts',(61.9015664443406,-30.774678958245,-216.429466072831));
#218293=CARTESIAN_POINT('Ctrl Pts',(61.9004491180021,-30.7973555397603,
-216.430349855778));
#218294=CARTESIAN_POINT('Ctrl Pts',(61.8821128244839,-31.1694978945224,
-216.444853499847));
#218295=CARTESIAN_POINT('Ctrl Pts',(61.8624992424722,-31.5454595353348,
-216.449238051427));
#218296=CARTESIAN_POINT('Ctrl Pts',(61.8416722272066,-31.9253979377884,
-216.443503510518));
#218297=CARTESIAN_POINT('Ctrl Pts',(61.8234061296913,-32.2586186043355,
-216.438474096456));
#218298=CARTESIAN_POINT('Ctrl Pts',(61.80420578693,-32.5948987249562,-216.425661108758));
#218299=CARTESIAN_POINT('Ctrl Pts',(61.7840819782534,-32.9343377021117,
-216.405064547423));
#218300=CARTESIAN_POINT('Ctrl Pts',(61.7608750372752,-33.3257815105432,
-216.381312424209));
#218301=CARTESIAN_POINT('Ctrl Pts',(61.736440544479,-33.7214276748005,-216.347209011029));
#218302=CARTESIAN_POINT('Ctrl Pts',(61.710868892887,-34.1214456828077,-216.302754307884));
#218303=CARTESIAN_POINT('Ctrl Pts',(61.6852972412951,-34.5214636908148,
-216.258299604738));
#218304=CARTESIAN_POINT('Ctrl Pts',(61.6585878780578,-34.9258545898999,
-216.203493611628));
#218305=CARTESIAN_POINT('Ctrl Pts',(61.6307906445938,-35.3347454916144,
-216.138336328552));
#218306=CARTESIAN_POINT('',(61.9835319875972,-17.519732572983,-215.952954107728));
#218307=CARTESIAN_POINT('Ctrl Pts',(61.9835319875972,-17.519732572983,-215.952954107728));
#218308=CARTESIAN_POINT('Ctrl Pts',(61.9836423128332,-17.5314237398636,
-215.949884435609));
#218309=CARTESIAN_POINT('Ctrl Pts',(61.9839561888802,-17.5486136892257,
-215.94516693725));
#218310=CARTESIAN_POINT('Ctrl Pts',(61.9846242057265,-17.5694505236489,
-215.939058207716));
#218311=CARTESIAN_POINT('Ctrl Pts',(61.9850106576282,-17.5789972212952,
-215.936149795196));
#218312=CARTESIAN_POINT('Ctrl Pts',(61.9852497232006,-17.5844090820673,
-215.934473721412));
#218313=CARTESIAN_POINT('Ctrl Pts',(61.985366427141,-17.5869458954142,-215.933681710066));
#218314=CARTESIAN_POINT('Ctrl Pts',(61.985432903138,-17.5883703075193,-215.933235701669));
#218315=CARTESIAN_POINT('Ctrl Pts',(61.9856070518024,-17.594619343813,-215.931447708497));
#218316=CARTESIAN_POINT('Ctrl Pts',(61.9860546172725,-17.6114739051512,
-215.92667840684));
#218317=CARTESIAN_POINT('Ctrl Pts',(61.9863253289469,-17.6217716024391,
-215.923771928037));
#218318=CARTESIAN_POINT('Ctrl Pts',(61.9867299233137,-17.6370620065691,
-215.919467837146));
#218319=CARTESIAN_POINT('Ctrl Pts',(61.9869232851332,-17.6443175804049,
-215.917427541273));
#218320=CARTESIAN_POINT('Ctrl Pts',(61.9870567406185,-17.6493108036505,
-215.91602385836));
#218321=CARTESIAN_POINT('Ctrl Pts',(61.9871592737459,-17.6531325304696,
-215.914949912397));
#218322=CARTESIAN_POINT('Ctrl Pts',(61.9884067096461,-17.6995234326739,
-215.901916052651));
#218323=CARTESIAN_POINT('Ctrl Pts',(61.9896013562167,-17.7444613163572,
-215.889465407473));
#218324=CARTESIAN_POINT('Ctrl Pts',(61.9931612274189,-17.8798611362945,
-215.852478094865));
#218325=CARTESIAN_POINT('Ctrl Pts',(61.9954673813378,-17.9696252699092,
-215.828653542303));
#218326=CARTESIAN_POINT('Ctrl Pts',(62.0023087939979,-18.2421350443946,
-215.758452964092));
#218327=CARTESIAN_POINT('Ctrl Pts',(62.0066123618738,-18.4220229695549,
-215.714899340256));
#218328=CARTESIAN_POINT('Ctrl Pts',(62.0149533931261,-18.7884597836193,
-215.631916484355));
#218329=CARTESIAN_POINT('Ctrl Pts',(62.0208820386822,-19.0631041231828,
-215.574032320922));
#218330=CARTESIAN_POINT('Ctrl Pts',(62.0263304049722,-19.337211649177,-215.522677625229));
#218331=CARTESIAN_POINT('Ctrl Pts',(62.0298564228196,-19.5198018772034,
-215.489892154265));
#218332=CARTESIAN_POINT('Ctrl Pts',(62.0315368963012,-19.6094031181495,
-215.474490491189));
#218333=CARTESIAN_POINT('Ctrl Pts',(62.0399691054701,-20.0731650506289,
-215.398453897984));
#218334=CARTESIAN_POINT('Ctrl Pts',(62.0458406539154,-20.4430189247693,
-215.349605146099));
#218335=CARTESIAN_POINT('Ctrl Pts',(62.053384096181,-20.9946381408474,-215.294302802292));
#218336=CARTESIAN_POINT('Ctrl Pts',(62.0568388647613,-21.2696575934642,
-215.271144326393));
#218337=CARTESIAN_POINT('Ctrl Pts',(62.0603145156397,-21.5888204107672,
-215.25198832252));
#218338=CARTESIAN_POINT('Ctrl Pts',(62.0619127847657,-21.7479398050394,
-215.244375875086));
#218339=CARTESIAN_POINT('Ctrl Pts',(62.0625677447133,-21.8160306805066,
-215.241534587864));
#218340=CARTESIAN_POINT('Ctrl Pts',(62.0629977011145,-21.8614012144509,
-215.239733994217));
#218341=CARTESIAN_POINT('Ctrl Pts',(62.0631962788612,-21.8826539937182,
-215.23893107315));
#218342=CARTESIAN_POINT('Ctrl Pts',(62.0775837642522,-23.4480132314265,
-215.183208144136));
#218343=CARTESIAN_POINT('Ctrl Pts',(62.0768822737846,-24.9479678284623,
-215.345269143632));
#218344=CARTESIAN_POINT('Ctrl Pts',(62.0596235416337,-26.3318125162586,
-215.724256795808));
#218345=CARTESIAN_POINT('',(62.0301313496079,-8.32556739006806,-215.882447372551));
#218346=CARTESIAN_POINT('Ctrl Pts',(62.030115892062,-8.32556237289759,-215.882468962491));
#218347=CARTESIAN_POINT('Ctrl Pts',(62.0303011812704,-8.34626436240946,
-215.88753471463));
#218348=CARTESIAN_POINT('Ctrl Pts',(62.030989541129,-8.38035489028408,-215.895278718971));
#218349=CARTESIAN_POINT('Ctrl Pts',(62.0325396354948,-8.45153820976076,
-215.910912103787));
#218350=CARTESIAN_POINT('Ctrl Pts',(62.0334411715356,-8.49214135874183,
-215.919733140771));
#218351=CARTESIAN_POINT('Ctrl Pts',(62.0346319766011,-8.54826989225757,
-215.931781953593));
#218352=CARTESIAN_POINT('Ctrl Pts',(62.035249580053,-8.57852190021065,-215.938245760757));
#218353=CARTESIAN_POINT('Ctrl Pts',(62.035517626716,-8.59195564672906,-215.941110121131));
#218354=CARTESIAN_POINT('Ctrl Pts',(62.035696909637,-8.60101558787812,-215.943040618559));
#218355=CARTESIAN_POINT('Ctrl Pts',(62.0358192267169,-8.60726231337101,
-215.944370592652));
#218356=CARTESIAN_POINT('Ctrl Pts',(62.0377253709339,-8.70525149376917,
-215.965223593057));
#218357=CARTESIAN_POINT('Ctrl Pts',(62.0394990136822,-8.80024742224131,
-215.984787334564));
#218358=CARTESIAN_POINT('Ctrl Pts',(62.0446069194413,-9.08616302923329,
-216.041699399449));
#218359=CARTESIAN_POINT('Ctrl Pts',(62.0477024749532,-9.27634345079324,
-216.076945388547));
#218360=CARTESIAN_POINT('Ctrl Pts',(62.0561197654603,-9.85181203919491,
-216.175621086794));
#218361=CARTESIAN_POINT('Ctrl Pts',(62.0604994716209,-10.2371764573657,
-216.231000261074));
#218362=CARTESIAN_POINT('Ctrl Pts',(62.0666464852748,-11.0056304231739,
-216.320132465571));
#218363=CARTESIAN_POINT('Ctrl Pts',(62.0684180957827,-11.3899288480629,
-216.354110109381));
#218364=CARTESIAN_POINT('Ctrl Pts',(62.0691637284138,-11.9674718683663,
-216.38919388744));
#218365=CARTESIAN_POINT('Ctrl Pts',(62.0690573031364,-12.2565170460506,
-216.402765104555));
#218366=CARTESIAN_POINT('Ctrl Pts',(62.0682218034411,-12.546158239528,-216.410380313799));
#218367=CARTESIAN_POINT('Ctrl Pts',(62.0675010132409,-12.7394054961317,
-216.414133562656));
#218368=CARTESIAN_POINT('Ctrl Pts',(62.0670521567137,-12.8373278964512,
-216.415355334398));
#218369=CARTESIAN_POINT('Ctrl Pts',(62.064459531591,-13.3151375449165,-216.418086040195));
#218370=CARTESIAN_POINT('Ctrl Pts',(62.0611113064883,-13.6974629887201,
-216.409927510236));
#218371=CARTESIAN_POINT('Ctrl Pts',(62.0542476848807,-14.2720292606053,
-216.382175073402));
#218372=CARTESIAN_POINT('Ctrl Pts',(62.0516520094611,-14.4637308422343,
-216.370338487474));
#218373=CARTESIAN_POINT('Ctrl Pts',(62.0458415981264,-14.8476509075169,
-216.341493768322));
#218374=CARTESIAN_POINT('Ctrl Pts',(62.0425860803387,-15.0420961048042,
-216.32425904904));
#218375=CARTESIAN_POINT('Ctrl Pts',(62.0251468210422,-15.9937435603833,
-216.227422444945));
#218376=CARTESIAN_POINT('Ctrl Pts',(62.0064818380416,-16.7545321493873,
-216.110109904781));
#218377=CARTESIAN_POINT('Ctrl Pts',(61.9835319875972,-17.519732572983,-215.952954107728));
#218378=CARTESIAN_POINT('',(62.0174953884411,0.438808195154074,-215.788045995909));
#218379=CARTESIAN_POINT('Ctrl Pts',(62.0174993799523,0.438809887676684,
-215.78803981657));
#218380=CARTESIAN_POINT('Ctrl Pts',(62.0175199857004,0.437737880397535,
-215.787745494507));
#218381=CARTESIAN_POINT('Ctrl Pts',(62.0175417397146,0.436720607586659,
-215.787462636701));
#218382=CARTESIAN_POINT('Ctrl Pts',(62.0175648395666,0.435767459872816,
-215.787193239101));
#218383=CARTESIAN_POINT('Ctrl Pts',(62.0180184663837,0.417049878348607,
-215.781902903222));
#218384=CARTESIAN_POINT('Ctrl Pts',(62.0184685135507,0.398079840556354,
-215.776592465129));
#218385=CARTESIAN_POINT('Ctrl Pts',(62.0189140804213,0.3789318657975,-215.771283693546));
#218386=CARTESIAN_POINT('Ctrl Pts',(62.0200362972047,0.330705258177559,
-215.757912877713));
#218387=CARTESIAN_POINT('Ctrl Pts',(62.0211298298166,0.281349530773877,
-215.744556209106));
#218388=CARTESIAN_POINT('Ctrl Pts',(62.0221829382759,0.232059213442546,
-215.731526094723));
#218389=CARTESIAN_POINT('Ctrl Pts',(62.0232455199048,0.182325508223198,
-215.718378768783));
#218390=CARTESIAN_POINT('Ctrl Pts',(62.0242669515709,0.132658426088991,
-215.705563865472));
#218391=CARTESIAN_POINT('Ctrl Pts',(62.0252391344941,0.0842905961880013,
-215.693349192722));
#218392=CARTESIAN_POINT('Ctrl Pts',(62.0262580962381,0.0335954367315529,
-215.680546782854));
#218393=CARTESIAN_POINT('Ctrl Pts',(62.0272229739792,-0.01567238529281,
-215.668403547226));
#218394=CARTESIAN_POINT('Ctrl Pts',(62.0281286510849,-0.0620880344041088,
-215.657170900034));
#218395=CARTESIAN_POINT('Ctrl Pts',(62.028226837897,-0.0671200757225747,
-215.655953139518));
#218396=CARTESIAN_POINT('Ctrl Pts',(62.0283243325486,-0.0721185899463497,
-215.654746031811));
#218397=CARTESIAN_POINT('Ctrl Pts',(62.0284211310589,-0.0770817583052276,
-215.653549862627));
#218398=CARTESIAN_POINT('Ctrl Pts',(62.0286398303158,-0.088295166749099,
-215.650847328145));
#218399=CARTESIAN_POINT('Ctrl Pts',(62.0288550016787,-0.0993281296954822,
-215.648200444206));
#218400=CARTESIAN_POINT('Ctrl Pts',(62.0290666028553,-0.110159665422851,
-215.64561242937));
#218401=CARTESIAN_POINT('Ctrl Pts',(62.0293620204162,-0.125281631738813,
-215.641999287692));
#218402=CARTESIAN_POINT('Ctrl Pts',(62.0296517907571,-0.140209428581813,
-215.638457495469));
#218403=CARTESIAN_POINT('Ctrl Pts',(62.0299360452298,-0.154942260830281,
-215.634985279954));
#218404=CARTESIAN_POINT('Ctrl Pts',(62.0300059984789,-0.158567918766427,
-215.634130789417));
#218405=CARTESIAN_POINT('Ctrl Pts',(62.0300756176579,-0.162181769268651,
-215.633280512819));
#218406=CARTESIAN_POINT('Ctrl Pts',(62.0301449046902,-0.165783800560488,
-215.632434424177));
#218407=CARTESIAN_POINT('Ctrl Pts',(62.0301647249564,-0.166814198551956,
-215.632192391844));
#218408=CARTESIAN_POINT('Ctrl Pts',(62.0301845180428,-0.167843629372059,
-215.631950702214));
#218409=CARTESIAN_POINT('Ctrl Pts',(62.0302042839942,-0.168872092745587,
-215.631709354683));
#218410=CARTESIAN_POINT('Ctrl Pts',(62.0302210196731,-0.169742884768136,
-215.631505007586));
#218411=CARTESIAN_POINT('Ctrl Pts',(62.0302377586917,-0.170614166281166,
-215.631300627362));
#218412=CARTESIAN_POINT('Ctrl Pts',(62.0302547273007,-0.171497727936975,
-215.631093451879));
#218413=CARTESIAN_POINT('Ctrl Pts',(62.0305332898224,-0.186002579968649,
-215.627692387902));
#218414=CARTESIAN_POINT('Ctrl Pts',(62.030856381188,-0.202924818300808,
-215.623750049934));
#218415=CARTESIAN_POINT('Ctrl Pts',(62.0311751486078,-0.219750316957847,
-215.619863638711));
#218416=CARTESIAN_POINT('Ctrl Pts',(62.0312538679905,-0.223905361629116,
-215.618903892283));
#218417=CARTESIAN_POINT('Ctrl Pts',(62.0313323354895,-0.228054487912501,
-215.617947396967));
#218418=CARTESIAN_POINT('Ctrl Pts',(62.0314098394012,-0.232159795046044,
-215.617002821984));
#218419=CARTESIAN_POINT('Ctrl Pts',(62.031458562176,-0.234740593235482,
-215.616409015643));
#218420=CARTESIAN_POINT('Ctrl Pts',(62.0315067944369,-0.237298224911199,
-215.615821256297));
#218421=CARTESIAN_POINT('Ctrl Pts',(62.0315550744332,-0.239861171708681,
-215.615232983426));
#218422=CARTESIAN_POINT('Ctrl Pts',(62.0323343763903,-0.281230467590438,
-215.605737493905));
#218423=CARTESIAN_POINT('Ctrl Pts',(62.0331009888089,-0.322656164563466,
-215.596414500743));
#218424=CARTESIAN_POINT('Ctrl Pts',(62.0338548909205,-0.364136660223962,
-215.587264567044));
#218425=CARTESIAN_POINT('Ctrl Pts',(62.0340165521309,-0.373031431884385,
-215.585302522723));
#218426=CARTESIAN_POINT('Ctrl Pts',(62.0341776604944,-0.381930442620933,
-215.583348052048));
#218427=CARTESIAN_POINT('Ctrl Pts',(62.0343383387091,-0.390840585373911,
-215.581399672612));
#218428=CARTESIAN_POINT('Ctrl Pts',(62.0354513689017,-0.45256182073756,
-215.567903100327));
#218429=CARTESIAN_POINT('Ctrl Pts',(62.0365412856687,-0.514694904346594,
-215.554729173333));
#218430=CARTESIAN_POINT('Ctrl Pts',(62.0375948581298,-0.576467803200393,
-215.542038436149));
#218431=CARTESIAN_POINT('Ctrl Pts',(62.0378614395503,-0.592097964134217,
-215.538827347335));
#218432=CARTESIAN_POINT('Ctrl Pts',(62.0381257087559,-0.607705042805249,
-215.535646994792));
#218433=CARTESIAN_POINT('Ctrl Pts',(62.0383874809175,-0.623276488100884,
-215.532499578114));
#218434=CARTESIAN_POINT('Ctrl Pts',(62.0385111622365,-0.630633637468982,
-215.531012496203));
#218435=CARTESIAN_POINT('Ctrl Pts',(62.0386342476484,-0.637980515719275,
-215.529533228673));
#218436=CARTESIAN_POINT('Ctrl Pts',(62.038756844207,-0.645323326956518,
-215.528060485936));
#218437=CARTESIAN_POINT('Ctrl Pts',(62.0411798407565,-0.790446538305592,
-215.498953220549));
#218438=CARTESIAN_POINT('Ctrl Pts',(62.0434488356458,-0.936202892943907,
-215.471950926648));
#218439=CARTESIAN_POINT('Ctrl Pts',(62.0455635795042,-1.08252171004957,
-215.4470693343));
#218440=CARTESIAN_POINT('Ctrl Pts',(62.0460443920013,-1.11578905613439,
-215.441412204478));
#218441=CARTESIAN_POINT('Ctrl Pts',(62.0465172330842,-1.14908547288418,
-215.435864670581));
#218442=CARTESIAN_POINT('Ctrl Pts',(62.0469821039688,-1.18241012093648,
-215.430426863699));
#218443=CARTESIAN_POINT('Ctrl Pts',(62.0471750188093,-1.19623937843347,
-215.428170250771));
#218444=CARTESIAN_POINT('Ctrl Pts',(62.0473666820277,-1.2100821617595,-215.425931119288));
#218445=CARTESIAN_POINT('Ctrl Pts',(62.0475571027041,-1.22393946910655,
-215.423709384899));
#218446=CARTESIAN_POINT('Ctrl Pts',(62.0487854491708,-1.31332878778413,
-215.409377645093));
#218447=CARTESIAN_POINT('Ctrl Pts',(62.0499611329979,-1.40327519821237,
-215.395781629928));
#218448=CARTESIAN_POINT('Ctrl Pts',(62.0510753972293,-1.49309213594665,
-215.383025488572));
#218449=CARTESIAN_POINT('Ctrl Pts',(62.0520503784318,-1.57168195646414,
-215.371863864886));
#218450=CARTESIAN_POINT('Ctrl Pts',(62.0529783941484,-1.65017255152723,
-215.361344478395));
#218451=CARTESIAN_POINT('Ctrl Pts',(62.0538558009956,-1.728101006012,-215.351506437208));
#218452=CARTESIAN_POINT('Ctrl Pts',(62.053961526629,-1.73749121676863,-215.350320974456));
#218453=CARTESIAN_POINT('Ctrl Pts',(62.0540665752971,-1.74687815347842,
-215.34914474847));
#218454=CARTESIAN_POINT('Ctrl Pts',(62.0541710336924,-1.75626947748911,
-215.347976789977));
#218455=CARTESIAN_POINT('Ctrl Pts',(62.0568806618616,-1.99987839011803,
-215.317680199397));
#218456=CARTESIAN_POINT('Ctrl Pts',(62.0591750307562,-2.24486471169071,
-215.29315003336));
#218457=CARTESIAN_POINT('Ctrl Pts',(62.0610585920148,-2.49090725646128,
-215.274384720384));
#218458=CARTESIAN_POINT('Ctrl Pts',(62.0629666027971,-2.74014355084581,
-215.255375824693));
#218459=CARTESIAN_POINT('Ctrl Pts',(62.064453075031,-2.99046152215792,-215.242282398062));
#218460=CARTESIAN_POINT('Ctrl Pts',(62.0655265978205,-3.24153013486207,
-215.235049704537));
#218461=CARTESIAN_POINT('Ctrl Pts',(62.06572580812,-3.28812015981675,-215.233707555998));
#218462=CARTESIAN_POINT('Ctrl Pts',(62.0659108088742,-3.33473606268537,
-215.232567081462));
#218463=CARTESIAN_POINT('Ctrl Pts',(62.0660816687505,-3.38137573845494,
-215.231627742877));
#218464=CARTESIAN_POINT('Ctrl Pts',(62.0664200834408,-3.47375290608351,
-215.229767235991));
#218465=CARTESIAN_POINT('Ctrl Pts',(62.0667030200249,-3.56622340514867,
-215.228695834708));
#218466=CARTESIAN_POINT('Ctrl Pts',(62.0669311442066,-3.65877138252441,
-215.228408582734));
#218467=CARTESIAN_POINT('Ctrl Pts',(62.0670291451991,-3.69852952464318,
-215.228285180741));
#218468=CARTESIAN_POINT('Ctrl Pts',(62.0671176862561,-3.73860300807162,
-215.228306525401));
#218469=CARTESIAN_POINT('Ctrl Pts',(62.0671957931192,-3.77860267586971,
-215.228474317159));
#218470=CARTESIAN_POINT('Ctrl Pts',(62.0672995013967,-3.83171320269179,
-215.228697106725));
#218471=CARTESIAN_POINT('Ctrl Pts',(62.0673846537059,-3.8846939386638,-215.229179757501));
#218472=CARTESIAN_POINT('Ctrl Pts',(62.0674508958752,-3.93663220814274,
-215.229897227125));
#218473=CARTESIAN_POINT('Ctrl Pts',(62.0677838568108,-4.19769574163658,
-215.233503530476));
#218474=CARTESIAN_POINT('Ctrl Pts',(62.0676791696996,-4.45960993311365,
-215.243348814244));
#218475=CARTESIAN_POINT('Ctrl Pts',(62.0671218812092,-4.72202625183822,
-215.259534787271));
#218476=CARTESIAN_POINT('Ctrl Pts',(62.0665693752761,-4.98219055725087,
-215.275581854964));
#218477=CARTESIAN_POINT('Ctrl Pts',(62.0655719913671,-5.24284830173915,
-215.297861274943));
#218478=CARTESIAN_POINT('Ctrl Pts',(62.0641187349921,-5.50365673697162,
-215.326421191673));
#218479=CARTESIAN_POINT('Ctrl Pts',(62.06267127947,-5.76342412301369,-215.354867107956));
#218480=CARTESIAN_POINT('Ctrl Pts',(62.0607715710024,-6.02334089753718,
-215.389543527112));
#218481=CARTESIAN_POINT('Ctrl Pts',(62.0584124940865,-6.28306684796035,
-215.430446656303));
#218482=CARTESIAN_POINT('Ctrl Pts',(62.056064416915,-6.54158176576643,-215.471159065147));
#218483=CARTESIAN_POINT('Ctrl Pts',(62.0532612348401,-6.79990753681709,
-215.518040271634));
#218484=CARTESIAN_POINT('Ctrl Pts',(62.0499998217298,-7.0577086353118,-215.571035080249));
#218485=CARTESIAN_POINT('Ctrl Pts',(62.0479865133785,-7.21685226019025,
-215.603749393695));
#218486=CARTESIAN_POINT('Ctrl Pts',(62.0457986624207,-7.37579595113682,
-215.638792426276));
#218487=CARTESIAN_POINT('Ctrl Pts',(62.0434363036247,-7.53446101372002,
-215.676141298899));
#218488=CARTESIAN_POINT('Ctrl Pts',(62.0410955413965,-7.69167556812021,
-215.713148729969));
#218489=CARTESIAN_POINT('Ctrl Pts',(62.0385792907942,-7.8486307341177,-215.752453819732));
#218490=CARTESIAN_POINT('Ctrl Pts',(62.0358856150351,-8.00521067750114,
-215.794042233454));
#218491=CARTESIAN_POINT('Ctrl Pts',(62.0356705839639,-8.01771015998553,
-215.797362158328));
#218492=CARTESIAN_POINT('Ctrl Pts',(62.0354544772225,-8.03020406724771,
-215.800695783931));
#218493=CARTESIAN_POINT('Ctrl Pts',(62.0352372951836,-8.04269236432169,
-215.804043085035));
#218494=CARTESIAN_POINT('Ctrl Pts',(62.0340910376763,-8.10860391184118,
-215.821709688772));
#218495=CARTESIAN_POINT('Ctrl Pts',(62.0329135938924,-8.17442996315404,
-215.839776233286));
#218496=CARTESIAN_POINT('Ctrl Pts',(62.0317048636879,-8.24016300281515,
-215.858240914477));
#218497=CARTESIAN_POINT('Ctrl Pts',(62.0313454521133,-8.25970848550308,
-215.863731320951));
#218498=CARTESIAN_POINT('Ctrl Pts',(62.0309832742987,-8.27924574457128,
-215.869256928137));
#218499=CARTESIAN_POINT('Ctrl Pts',(62.0306183276176,-8.2987745826764,-215.87481768646));
#218500=CARTESIAN_POINT('Ctrl Pts',(62.0304520445045,-8.30767263864652,
-215.877351372209));
#218501=CARTESIAN_POINT('Ctrl Pts',(62.0299989413369,-8.31437631353327,
-215.87976001137));
#218502=CARTESIAN_POINT('Ctrl Pts',(62.0301313496079,-8.32556739006806,
-215.882447372551));
#218503=CARTESIAN_POINT('',(61.6795265634691,9.54487894167559,-216.064116268519));
#218504=CARTESIAN_POINT('Ctrl Pts',(61.6795265634691,9.54487894167559,-216.064116268519));
#218505=CARTESIAN_POINT('Ctrl Pts',(61.6802430723727,9.521532518164,-216.069164370748));
#218506=CARTESIAN_POINT('Ctrl Pts',(61.6858191140444,9.43596373115034,-216.083872747801));
#218507=CARTESIAN_POINT('Ctrl Pts',(61.6957728249672,9.26950019496731,-216.11128748116));
#218508=CARTESIAN_POINT('Ctrl Pts',(61.6969269211031,9.25002898428,-216.114484504439));
#218509=CARTESIAN_POINT('Ctrl Pts',(61.6987217468774,9.21935845937455,-216.119506452048));
#218510=CARTESIAN_POINT('Ctrl Pts',(61.6990332190503,9.21399578439662,-216.120382944374));
#218511=CARTESIAN_POINT('Ctrl Pts',(61.6997227074585,9.20216114842476,-216.122313163012));
#218512=CARTESIAN_POINT('Ctrl Pts',(61.7014452264265,9.17257711291344,-216.127127572639));
#218513=CARTESIAN_POINT('Ctrl Pts',(61.7031617251547,9.1430058402448,-216.131886297433));
#218514=CARTESIAN_POINT('Ctrl Pts',(61.707269685065,9.07205921748622,-216.143200322058));
#218515=CARTESIAN_POINT('Ctrl Pts',(61.7099772069086,9.02506624388822,-216.150558627133));
#218516=CARTESIAN_POINT('Ctrl Pts',(61.7181461990841,8.88255125425903,-216.172456831843));
#218517=CARTESIAN_POINT('Ctrl Pts',(61.7235262896899,8.78772837399376,-216.186468897908));
#218518=CARTESIAN_POINT('Ctrl Pts',(61.7341541864233,8.59845357840604,-216.21331955589));
#218519=CARTESIAN_POINT('Ctrl Pts',(61.7393293185008,8.50532389398001,-216.225986299975));
#218520=CARTESIAN_POINT('Ctrl Pts',(61.7550912725796,8.21855250979642,-216.263257408001));
#218521=CARTESIAN_POINT('Ctrl Pts',(61.7704389797822,7.9330281740466,-216.296891034172));
#218522=CARTESIAN_POINT('Ctrl Pts',(61.7876193646635,7.6020550716402,-216.329764671456));
#218523=CARTESIAN_POINT('Ctrl Pts',(61.7948263815603,7.46066243116414,-216.342489317454));
#218524=CARTESIAN_POINT('Ctrl Pts',(61.7995963088469,7.36650073122957,-216.350669291297));
#218525=CARTESIAN_POINT('Ctrl Pts',(61.8019009783335,7.32072772463824,-216.354506331839));
#218526=CARTESIAN_POINT('Ctrl Pts',(61.8236187514576,6.88657756038332,-216.389500564472));
#218527=CARTESIAN_POINT('Ctrl Pts',(61.841685773179,6.50361036801132,-216.410524462369));
#218528=CARTESIAN_POINT('Ctrl Pts',(61.8669476828372,5.93336384123643,-216.426937179217));
#218529=CARTESIAN_POINT('Ctrl Pts',(61.8791181718381,5.6492911840457,-216.431362755141));
#218530=CARTESIAN_POINT('Ctrl Pts',(61.8925037732819,5.31966138595964,-216.429909557678));
#218531=CARTESIAN_POINT('Ctrl Pts',(61.89806457218,5.17876916430307,-216.427868965328));
#218532=CARTESIAN_POINT('Ctrl Pts',(61.9017324838976,5.08492433768665,-216.42619350522));
#218533=CARTESIAN_POINT('Ctrl Pts',(61.9034768601047,5.03986902103991,-216.425243169568));
#218534=CARTESIAN_POINT('Ctrl Pts',(61.965005265824,3.43392956880248,-216.385718336118));
#218535=CARTESIAN_POINT('Ctrl Pts',(62.0024632855742,1.91945558740173,-216.173720582219));
#218536=CARTESIAN_POINT('Ctrl Pts',(62.0174913965262,0.438806542391791,
-215.788052185604));
#218537=CARTESIAN_POINT('Ctrl Pts',(61.7131038227345,20.0389506617863,-216.160137831703));
#218538=CARTESIAN_POINT('Ctrl Pts',(61.7323346392832,19.2987667715537,-215.83025492416));
#218539=CARTESIAN_POINT('Ctrl Pts',(61.7438969106769,18.4794569854656,-215.58734776891));
#218540=CARTESIAN_POINT('Ctrl Pts',(61.7532854409784,17.1629064376784,-215.353450664475));
#218541=CARTESIAN_POINT('Ctrl Pts',(61.7550394001384,16.7094538020103,-215.29722890107));
#218542=CARTESIAN_POINT('Ctrl Pts',(61.7556514218488,16.011209030212,-215.245512163072));
#218543=CARTESIAN_POINT('Ctrl Pts',(61.7554491649581,15.657569560302,-215.227807770851));
#218544=CARTESIAN_POINT('Ctrl Pts',(61.7542962920732,15.2379182467459,-215.221422105953));
#218545=CARTESIAN_POINT('Ctrl Pts',(61.7534832401325,15.0264285229173,-215.221796638344));
#218546=CARTESIAN_POINT('Ctrl Pts',(61.7529831735412,14.91269863981,-215.22295282485));
#218547=CARTESIAN_POINT('Ctrl Pts',(61.7527320896283,14.8595090355654,-215.223752498906));
#218548=CARTESIAN_POINT('Ctrl Pts',(61.7525842430511,14.8290869986268,-215.224273158453));
#218549=CARTESIAN_POINT('Ctrl Pts',(61.7525410952316,14.8203036414675,-215.224430378052));
#218550=CARTESIAN_POINT('Ctrl Pts',(61.7443507875376,13.1665996145072,-215.255022606964));
#218551=CARTESIAN_POINT('Ctrl Pts',(61.720909381464,11.3762073620345,-215.53487822515));
#218552=CARTESIAN_POINT('Ctrl Pts',(61.6795265634691,9.54487894167559,-216.064116268519));
#218553=CARTESIAN_POINT('Ctrl Pts',(61.6907486315906,20.6657286340102,-216.300532529068));
#218554=CARTESIAN_POINT('Ctrl Pts',(61.7321110912357,20.3496658649069,-216.247078381677));
#218555=CARTESIAN_POINT('Ctrl Pts',(61.713103822739,20.0389506617614,-216.160137831685));
#218556=CARTESIAN_POINT('Ctrl Pts',(61.9064790936528,20.7060595729952,-215.92903923894));
#218557=CARTESIAN_POINT('Ctrl Pts',(61.9373844794568,20.4413798330517,-215.880084558757));
#218558=CARTESIAN_POINT('Ctrl Pts',(61.9252463833055,20.1793980393595,-215.812042320923));
#218559=CARTESIAN_POINT('Ctrl Pts',(62.0699842872639,20.7460043187545,-215.538658319552));
#218560=CARTESIAN_POINT('Ctrl Pts',(62.0914940184093,20.5335632238432,-215.496856996578));
#218561=CARTESIAN_POINT('Ctrl Pts',(62.0850713031281,20.3222903717942,-215.445236972404));
#218562=CARTESIAN_POINT('Ctrl Pts',(62.2967890390184,20.824939865421,-214.721940813782));
#218563=CARTESIAN_POINT('Ctrl Pts',(62.3035607512221,20.7183157084577,-214.699282243487));
#218564=CARTESIAN_POINT('Ctrl Pts',(62.3043696537349,20.611682425576,-214.675676922536));
#218565=CARTESIAN_POINT('Ctrl Pts',(62.3587717320579,20.8641365401031,-214.2924597236));
#218566=CARTESIAN_POINT('Ctrl Pts',(62.36063660277,20.8116268449194,-214.281171503343));
#218567=CARTESIAN_POINT('Ctrl Pts',(62.3625010497726,20.7591101230298,-214.269920324208));
#218568=CARTESIAN_POINT('Ctrl Pts',(62.3650472056256,20.9007985863674,-213.86644416092));
#218569=CARTESIAN_POINT('Ctrl Pts',(62.3650472056256,20.9007985863674,-213.86644416092));
#218570=CARTESIAN_POINT('Ctrl Pts',(62.3650472056256,20.9007985863674,-213.86644416092));
#218571=CARTESIAN_POINT('',(61.6907486315871,20.6657286340098,-216.300532529074));
#218572=CARTESIAN_POINT('Origin',(59.1013738165116,20.5826972454933,-214.78783829177));
#218573=CARTESIAN_POINT('Ctrl Pts',(61.6907486315871,20.66572863401,-216.300532529074));
#218574=CARTESIAN_POINT('Ctrl Pts',(61.9064790936528,20.7060595729952,-215.92903923894));
#218575=CARTESIAN_POINT('Ctrl Pts',(62.0699842872639,20.7460043187545,-215.538658319552));
#218576=CARTESIAN_POINT('Ctrl Pts',(62.296781831605,20.8249373570031,-214.721966767474));
#218577=CARTESIAN_POINT('Ctrl Pts',(62.358763853093,20.864131557726,-214.292514315806));
#218578=CARTESIAN_POINT('Ctrl Pts',(62.3650460084164,20.9007915960462,-213.866525388642));
#218579=CARTESIAN_POINT('Ctrl Pts',(61.4993881814496,20.607119072182,-216.605481304304));
#218580=CARTESIAN_POINT('Ctrl Pts',(61.6055583132372,20.2909606839731,-216.465410556121));
#218581=CARTESIAN_POINT('Ctrl Pts',(61.6377935655235,19.9815886122025,-216.280755810352));
#218582=CARTESIAN_POINT('Ctrl Pts',(61.5691908701343,20.635935030248,-216.502281627828));
#218583=CARTESIAN_POINT('Ctrl Pts',(61.6507949119074,20.3194192931332,-216.390568004056));
#218584=CARTESIAN_POINT('Ctrl Pts',(61.6652027952701,20.0090334790708,-216.239468240025));
#218585=CARTESIAN_POINT('Ctrl Pts',(61.6387815649058,20.6575029215218,-216.391600777272));
#218586=CARTESIAN_POINT('Ctrl Pts',(61.6967727624802,20.3410293418688,-216.311297779665));
#218587=CARTESIAN_POINT('Ctrl Pts',(61.6926044944813,20.0301302514676,-216.195652941674));
#218588=CARTESIAN_POINT('Ctrl Pts',(61.7080768938388,20.6687713493157,-216.270467388273));
#218589=CARTESIAN_POINT('Ctrl Pts',(61.7438559996883,20.3528222220489,-216.225852774312));
#218590=CARTESIAN_POINT('Ctrl Pts',(61.7199387591126,20.0421410735254,-216.14839440092));
#218591=CARTESIAN_POINT('',(61.5168384358791,20.6141575017552,-216.579518431174));
#218592=CARTESIAN_POINT('',(61.6446456814072,19.9883159925442,-216.270380726959));
#218593=CARTESIAN_POINT('Origin',(59.0326817073425,20.5344053061246,-214.899457439615));
#218594=CARTESIAN_POINT('Ctrl Pts',(61.516838435851,20.614157501844,-216.579518431211));
#218595=CARTESIAN_POINT('Ctrl Pts',(61.5771479675576,20.6380049970577,-216.489212055522));
#218596=CARTESIAN_POINT('Ctrl Pts',(61.6351552038294,20.6553354111624,-216.396265812028));
#218597=CARTESIAN_POINT('Ctrl Pts',(61.6907486315871,20.66572863401,-216.300532529074));
#218598=CARTESIAN_POINT('Ctrl Pts',(61.6446456814073,19.9883159925441,-216.270380726959));
#218599=CARTESIAN_POINT('Ctrl Pts',(61.6589899518011,20.0021161053552,-216.248548270214));
#218600=CARTESIAN_POINT('Ctrl Pts',(61.6733754048797,20.0141614257302,-216.225936038732));
#218601=CARTESIAN_POINT('Ctrl Pts',(61.6878163906252,20.0240270541524,-216.202356324519));
#218602=CARTESIAN_POINT('Ctrl Pts',(61.6962258005136,20.0297720991703,-216.188625164793));
#218603=CARTESIAN_POINT('Ctrl Pts',(61.7046540333319,20.034777214613,-216.174565637229));
#218604=CARTESIAN_POINT('Ctrl Pts',(61.7131038227239,20.038950661781,-216.160137831721));
#218605=CARTESIAN_POINT('Ctrl Pts',(62.0998335778874,28.4197995297673,-213.858707258037));
#218606=CARTESIAN_POINT('Ctrl Pts',(62.0737483304577,28.4205138141115,-215.350417820742));
#218607=CARTESIAN_POINT('Ctrl Pts',(61.235107328202,28.3894013135675,-216.583947161644));
#218608=CARTESIAN_POINT('Ctrl Pts',(62.2010617731482,25.8108994796242,-213.861712475947));
#218609=CARTESIAN_POINT('Ctrl Pts',(62.1750190192639,25.812006950141,-215.350359724743));
#218610=CARTESIAN_POINT('Ctrl Pts',(61.3394317178725,25.7825379828778,-216.58230034997));
#218611=CARTESIAN_POINT('Ctrl Pts',(62.2927210668524,23.2015642400677,-213.864398964149));
#218612=CARTESIAN_POINT('Ctrl Pts',(62.2667395005803,23.2024779691081,-215.350312870121));
#218613=CARTESIAN_POINT('Ctrl Pts',(61.4338508567495,23.1751069333097,-216.580828347939));
#218614=CARTESIAN_POINT('Ctrl Pts',(62.3748047396227,20.5920154834281,-213.866720382044));
#218615=CARTESIAN_POINT('Ctrl Pts',(62.3488810204336,20.5925259779214,-215.350234406272));
#218616=CARTESIAN_POINT('Ctrl Pts',(61.5183514407949,20.5675003107738,-216.579494546858));
#218617=CARTESIAN_POINT('',(61.2351073280272,28.3894013125172,-216.583947161963));
#218618=CARTESIAN_POINT('Origin',(-967.060476622167,-12.7722155952905,-232.807288933329));
#218619=CARTESIAN_POINT('',(62.099833577893,28.4197995297552,-213.858707258032));
#218620=CARTESIAN_POINT('Origin',(57.1043579940171,28.2258690560256,-213.771445225846));
#218621=CARTESIAN_POINT('Origin',(-1003.25098428815,-12.9621320438613,-174.780968069139));
#218622=CARTESIAN_POINT('Ctrl Pts',(62.0688011703024,29.2457316556486,-213.781328275569));
#218623=CARTESIAN_POINT('Ctrl Pts',(62.0289469563781,29.5310768106848,-215.415988103393));
#218624=CARTESIAN_POINT('Ctrl Pts',(61.0052807181397,29.7205356651696,-216.708851684624));
#218625=CARTESIAN_POINT('Ctrl Pts',(62.0742729941045,29.0960629819322,-213.807353032748));
#218626=CARTESIAN_POINT('Ctrl Pts',(62.0368058273153,29.3327506759839,-215.417932437979));
#218627=CARTESIAN_POINT('Ctrl Pts',(61.0493770342224,29.4859232929652,-216.703260974786));
#218628=CARTESIAN_POINT('Ctrl Pts',(62.0798211066684,28.9461456833678,-213.82776792667));
#218629=CARTESIAN_POINT('Ctrl Pts',(62.0445308741403,29.1383495067355,-215.415821866988));
#218630=CARTESIAN_POINT('Ctrl Pts',(61.0888241268935,29.2581335927935,-216.69312078545));
#218631=CARTESIAN_POINT('Ctrl Pts',(62.0911177663954,28.645756714799,-213.854728078229));
#218632=CARTESIAN_POINT('Ctrl Pts',(62.0608777530688,28.7334658375517,-215.390288011995));
#218633=CARTESIAN_POINT('Ctrl Pts',(61.1729733940828,28.7720316195816,-216.645653415601));
#218634=CARTESIAN_POINT('Ctrl Pts',(62.0968756241727,28.4952634919339,-213.860788934278));
#218635=CARTESIAN_POINT('Ctrl Pts',(62.0695770660397,28.5216890337278,-215.365176615215));
#218636=CARTESIAN_POINT('Ctrl Pts',(61.2182542009739,28.5113092167426,-216.605776792465));
#218637=CARTESIAN_POINT('Ctrl Pts',(62.1027691607293,28.3443970744867,-213.858075427907));
#218638=CARTESIAN_POINT('Ctrl Pts',(62.0779510070526,28.3183576151588,-215.336592494545));
#218639=CARTESIAN_POINT('Ctrl Pts',(61.2532962738455,28.2653275536711,-216.563073912214));
#218640=CARTESIAN_POINT('',(61.0271214515743,29.6036708476852,-216.705447812142));
#218641=CARTESIAN_POINT('',(62.0715435503803,29.170876467827,-213.793867031503));
#218642=CARTESIAN_POINT('Origin',(57.0762058255522,28.9734268472959,-213.706604999317));
#218643=CARTESIAN_POINT('Ctrl Pts',(62.0998335778932,28.4197995297553,-213.858707258032));
#218644=CARTESIAN_POINT('Ctrl Pts',(62.0949496006365,28.5456716573274,-213.858562269111));
#218645=CARTESIAN_POINT('Ctrl Pts',(62.0901675429832,28.6710240626335,-213.852460313436));
#218646=CARTESIAN_POINT('Ctrl Pts',(62.0854694365319,28.7959511990833,-213.84124800245));
#218647=CARTESIAN_POINT('Ctrl Pts',(62.0807548271212,28.9213171649822,-213.829996306167));
#218648=CARTESIAN_POINT('Ctrl Pts',(62.0761182844882,29.0462698189248,-213.813935251642));
#218649=CARTESIAN_POINT('Ctrl Pts',(62.0715435503805,29.1708764678268,-213.793867031503));
#218650=CARTESIAN_POINT('Ctrl Pts',(61.0271214515743,29.6036708476852,-216.705447812142));
#218651=CARTESIAN_POINT('Ctrl Pts',(61.0473497691228,29.4934302108373,-216.701965843739));
#218652=CARTESIAN_POINT('Ctrl Pts',(61.0662258246735,29.3872447406964,-216.697037564987));
#218653=CARTESIAN_POINT('Ctrl Pts',(61.092939107741,29.234817073613,-216.687475681334));
#218654=CARTESIAN_POINT('Ctrl Pts',(61.1015764034094,29.1851490360971,-216.683926809195));
#218655=CARTESIAN_POINT('Ctrl Pts',(61.1141822136387,29.1124498685452,-216.678061134607));
#218656=CARTESIAN_POINT('Ctrl Pts',(61.1203973405399,29.0765540137621,-216.674992705717));
#218657=CARTESIAN_POINT('Ctrl Pts',(61.1264920221608,29.0413270583538,-216.671720889435));
#218658=CARTESIAN_POINT('Ctrl Pts',(61.1305296762386,29.01798876909,-216.669494481381));
#218659=CARTESIAN_POINT('Ctrl Pts',(61.1328731847041,29.0044428970592,-216.668162653334));
#218660=CARTESIAN_POINT('Ctrl Pts',(61.1610345826342,28.8416940907171,-216.651802264667));
#218661=CARTESIAN_POINT('Ctrl Pts',(61.1982120890333,28.6316301319716,-216.62405122618));
#218662=CARTESIAN_POINT('Ctrl Pts',(61.2351073279234,28.3894013132814,-216.583947162069));
#218663=CARTESIAN_POINT('Ctrl Pts',(61.0265937502316,29.6037608952923,-216.706123999504));
#218664=CARTESIAN_POINT('Ctrl Pts',(62.0328659203364,29.432086372265,-215.416932921719));
#218665=CARTESIAN_POINT('Ctrl Pts',(62.0715435503799,29.1708764678276,-213.793867031504));
#218666=CARTESIAN_POINT('Ctrl Pts',(60.9825645796766,29.8436221509486,-216.713705040631));
#218667=CARTESIAN_POINT('Ctrl Pts',(62.0158262438435,29.7028146280762,-215.414349655834));
#218668=CARTESIAN_POINT('Ctrl Pts',(62.0610597588847,29.4471784511516,-213.768820140554));
#218669=CARTESIAN_POINT('Ctrl Pts',(60.9251255281948,30.093369550312,-216.724290200207));
#218670=CARTESIAN_POINT('Ctrl Pts',(61.9883890041931,29.9794001400379,-215.414675965098));
#218671=CARTESIAN_POINT('Ctrl Pts',(62.0405226886033,29.7223719581141,-213.744683753048));
#218672=CARTESIAN_POINT('Ctrl Pts',(60.8090550311091,30.5582447334237,-216.734083503021));
#218673=CARTESIAN_POINT('Ctrl Pts',(61.9158847636691,30.513005122286,-215.407737544432));
#218674=CARTESIAN_POINT('Ctrl Pts',(61.9794688757528,30.270714507063,-213.698186104728));
#218675=CARTESIAN_POINT('Ctrl Pts',(60.7468471946344,30.7826875211125,-216.737055032757));
#218676=CARTESIAN_POINT('Ctrl Pts',(61.8707136570867,30.7753294640716,-215.403383061571));
#218677=CARTESIAN_POINT('Ctrl Pts',(61.9389263175003,30.5439708219921,-213.676343773128));
#218678=CARTESIAN_POINT('Ctrl Pts',(60.5974728457365,31.2445885019563,-216.748323533354));
#218679=CARTESIAN_POINT('Ctrl Pts',(61.7592263865063,31.3084059968012,-215.399922850299));
#218680=CARTESIAN_POINT('Ctrl Pts',(61.8376360324932,31.0884065479068,-213.634598566576));
#218681=CARTESIAN_POINT('Ctrl Pts',(60.5132484754513,31.4761990764113,-216.754202271862));
#218682=CARTESIAN_POINT('Ctrl Pts',(61.6932218885361,31.5756441252082,-215.398886644252));
#218683=CARTESIAN_POINT('Ctrl Pts',(61.7769096374107,31.3595164244255,-213.614424841559));
#218684=CARTESIAN_POINT('Ctrl Pts',(60.3353787972406,31.9258725276716,-216.761796156373));
#218685=CARTESIAN_POINT('Ctrl Pts',(61.5426514848983,32.1020838962177,-215.394244475031));
#218686=CARTESIAN_POINT('Ctrl Pts',(61.6347983988382,31.8994507060226,-213.575433990375));
#218687=CARTESIAN_POINT('Ctrl Pts',(60.2431411074621,32.1425438899593,-216.763259486997));
#218688=CARTESIAN_POINT('Ctrl Pts',(61.4584458415044,32.3604872290325,-215.390415183932));
#218689=CARTESIAN_POINT('Ctrl Pts',(61.553185886347,32.168827114668,-213.55678698258));
#218690=CARTESIAN_POINT('Ctrl Pts',(60.0922775089899,32.4653895464032,-216.76679570928));
#218691=CARTESIAN_POINT('Ctrl Pts',(61.3177123000692,32.7449914243882,-215.386464661929));
#218692=CARTESIAN_POINT('Ctrl Pts',(61.4159587545684,32.5674954665497,-213.530743809026));
#218693=CARTESIAN_POINT('Ctrl Pts',(60.0397836500009,32.5728382848651,-216.768161995858));
#218694=CARTESIAN_POINT('Ctrl Pts',(61.2682557637607,32.8729588341924,-215.3854110548));
#218695=CARTESIAN_POINT('Ctrl Pts',(61.367676762258,32.699721268844,-213.52234238551));
#218696=CARTESIAN_POINT('Ctrl Pts',(59.9288125178118,32.7888250337031,-216.771641849425));
#218697=CARTESIAN_POINT('Ctrl Pts',(61.1639802174555,33.1287940399443,-215.384139008864));
#218698=CARTESIAN_POINT('Ctrl Pts',(61.2664764446162,32.9616854374291,-213.505934868453));
#218699=CARTESIAN_POINT('Ctrl Pts',(59.8686110761104,32.8993820177949,-216.774231175379));
#218700=CARTESIAN_POINT('Ctrl Pts',(61.1085304672864,33.2580306163176,-215.384328545335));
#218701=CARTESIAN_POINT('Ctrl Pts',(61.2135447672982,33.0914831455605,-213.497857516741));
#218702=CARTESIAN_POINT('Ctrl Pts',(59.6957162986054,33.2125071669439,-216.777043804247));
#218703=CARTESIAN_POINT('Ctrl Pts',(60.9396247822756,33.6325165068372,-215.38088449035));
#218704=CARTESIAN_POINT('Ctrl Pts',(61.0478125873327,33.4773667644598,-213.474082387732));
#218705=CARTESIAN_POINT('Ctrl Pts',(59.5851327557243,33.4043691267079,-216.775410250767));
#218706=CARTESIAN_POINT('Ctrl Pts',(60.8222645138006,33.8692180996893,-215.375922515872));
#218707=CARTESIAN_POINT('Ctrl Pts',(60.928044089869,33.730020614473,-213.459385328775));
#218708=CARTESIAN_POINT('Ctrl Pts',(59.401265962428,33.6968854804001,-216.776684954411));
#218709=CARTESIAN_POINT('Ctrl Pts',(60.6302585737573,34.2248518898603,-215.372298465673));
#218710=CARTESIAN_POINT('Ctrl Pts',(60.7344672841328,34.1022007074189,-213.439632708163));
#218711=CARTESIAN_POINT('Ctrl Pts',(59.3355992902892,33.7965187512738,-216.777959065008));
#218712=CARTESIAN_POINT('Ctrl Pts',(60.5629578125134,34.3444556219022,-215.371922956317));
#218713=CARTESIAN_POINT('Ctrl Pts',(60.6676250274774,34.2251152633889,-213.433348725254));
#218714=CARTESIAN_POINT('Ctrl Pts',(59.1992609912169,33.9957058462152,-216.780349347581));
#218715=CARTESIAN_POINT('Ctrl Pts',(60.4230592905929,34.5826912965888,-215.371180244526));
#218716=CARTESIAN_POINT('Ctrl Pts',(60.5293279501712,34.4685916589618,-213.420959244596));
#218717=CARTESIAN_POINT('Ctrl Pts',(59.1288052942883,34.0949722689346,-216.781320682795));
#218718=CARTESIAN_POINT('Ctrl Pts',(60.3505196458902,34.7011122420226,-215.370684459066));
#218719=CARTESIAN_POINT('Ctrl Pts',(60.45787721928,34.5891494282615,-213.414818675447));
#218720=CARTESIAN_POINT('Ctrl Pts',(59.03102591712,34.2324713614236,-216.780298741043));
#218721=CARTESIAN_POINT('Ctrl Pts',(60.2427003997968,34.8702746739671,-215.367852804425));
#218722=CARTESIAN_POINT('Ctrl Pts',(60.3471832550309,34.7682519438017,-213.406087731129));
#218723=CARTESIAN_POINT('Ctrl Pts',(59.0007435323251,34.2754518704397,-216.779359734745));
#218724=CARTESIAN_POINT('Ctrl Pts',(60.2073665276868,34.9246098826991,-215.366397395166));
#218725=CARTESIAN_POINT('Ctrl Pts',(60.3096963328381,34.8276667087864,-213.40328205755));
#218726=CARTESIAN_POINT('Ctrl Pts',(58.9378339843495,34.3626721170424,-216.778074064536));
#218727=CARTESIAN_POINT('Ctrl Pts',(60.1349754818777,35.0339069140606,-215.36407541824));
#218728=CARTESIAN_POINT('Ctrl Pts',(60.2335269589271,34.945932810391,-213.397980978203));
#218729=CARTESIAN_POINT('Ctrl Pts',(58.9053639383789,34.4067399736955,-216.777661739873));
#218730=CARTESIAN_POINT('Ctrl Pts',(60.0979756928914,35.088748275143,-215.363147491525));
#218731=CARTESIAN_POINT('Ctrl Pts',(60.1948462339725,35.0047819102636,-213.395467604646));
#218732=CARTESIAN_POINT('Ctrl Pts',(58.8053491301352,34.5398396001192,-216.776857332426));
#218733=CARTESIAN_POINT('Ctrl Pts',(59.9846859375433,35.2535081898727,-215.360820730381));
#218734=CARTESIAN_POINT('Ctrl Pts',(60.0770110939915,35.1804605606286,-213.388255279851));
#218735=CARTESIAN_POINT('Ctrl Pts',(58.7349881372357,34.6298757701064,-216.776911998089));
#218736=CARTESIAN_POINT('Ctrl Pts',(59.9060137786903,35.3637066384188,-215.359888334169));
#218737=CARTESIAN_POINT('Ctrl Pts',(59.9960526306669,35.2964118100118,-213.383856689816));
#218738=CARTESIAN_POINT('Ctrl Pts',(58.6659957159662,34.7166003426006,-216.776374027644));
#218739=CARTESIAN_POINT('Ctrl Pts',(59.8268160252816,35.4705884119597,-215.358542412566));
#218740=CARTESIAN_POINT('Ctrl Pts',(59.9134443065885,35.4101621769243,-213.379883144536));
#218741=CARTESIAN_POINT('',(58.6665914736623,34.7169872964315,-216.775646223556));
#218742=CARTESIAN_POINT('',(59.9134443065973,35.4101621769153,-213.379883144535));
#218743=CARTESIAN_POINT('Origin',(55.8698139418538,32.470529749032,-213.292621112349));
#218744=CARTESIAN_POINT('Ctrl Pts',(62.0715435503799,29.1708764678276,-213.793867031504));
#218745=CARTESIAN_POINT('Ctrl Pts',(62.0643014392995,29.3617434510075,-213.776564859235));
#218746=CARTESIAN_POINT('Ctrl Pts',(62.0522600475002,29.5519971941426,-213.759753107678));
#218747=CARTESIAN_POINT('Ctrl Pts',(62.0354890800171,29.7414131526144,-213.743402541702));
#218748=CARTESIAN_POINT('Ctrl Pts',(62.0279429432301,29.8266413145379,-213.736045565575));
#218749=CARTESIAN_POINT('Ctrl Pts',(62.0194399620359,29.9116999236011,-213.728781830163));
#218750=CARTESIAN_POINT('Ctrl Pts',(62.0099898554776,29.9965687797107,-213.721608053805));
#218751=CARTESIAN_POINT('Ctrl Pts',(61.9889706914869,30.1853362177545,-213.705651960531));
#218752=CARTESIAN_POINT('Ctrl Pts',(61.9632502648204,30.373215364858,-213.690387208237));
#218753=CARTESIAN_POINT('Ctrl Pts',(61.9329235309347,30.5599217016399,-213.675635343783));
#218754=CARTESIAN_POINT('Ctrl Pts',(61.9190056872795,30.6456068141406,-213.668865272733));
#218755=CARTESIAN_POINT('Ctrl Pts',(61.904118389167,30.73104504063,-213.66220316716));
#218756=CARTESIAN_POINT('Ctrl Pts',(61.8882744453593,30.8162093827887,-213.655631541451));
#218757=CARTESIAN_POINT('Ctrl Pts',(61.8865583969754,30.8254334833975,-213.654919772474));
#218758=CARTESIAN_POINT('Ctrl Pts',(61.884831153,30.8346542910449,-213.654208753614));
#218759=CARTESIAN_POINT('Ctrl Pts',(61.8830927250357,30.8438717751564,-213.653498479181));
#218760=CARTESIAN_POINT('Ctrl Pts',(61.8486303829777,31.0265978339227,-213.639418102558));
#218761=CARTESIAN_POINT('Ctrl Pts',(61.8097530423276,31.20808602447,-213.625773220073));
#218762=CARTESIAN_POINT('Ctrl Pts',(61.7665678010779,31.3880986014977,-213.612525374102));
#218763=CARTESIAN_POINT('Ctrl Pts',(61.747192030664,31.4688642117661,-213.606581509611));
#218764=CARTESIAN_POINT('Ctrl Pts',(61.7269497583691,31.54933287442,-213.600717484172));
#218765=CARTESIAN_POINT('Ctrl Pts',(61.7058540178194,31.6294835659502,-213.594929422224));
#218766=CARTESIAN_POINT('Ctrl Pts',(61.7034089471228,31.6387733136466,-213.59425856544));
#218767=CARTESIAN_POINT('Ctrl Pts',(61.7009521439872,31.6480594437296,-213.593588930303));
#218768=CARTESIAN_POINT('Ctrl Pts',(61.6984836689592,31.6573418016004,-213.592920528782));
#218769=CARTESIAN_POINT('Ctrl Pts',(61.6606248428338,31.7997046647723,-213.582669302148));
#218770=CARTESIAN_POINT('Ctrl Pts',(61.6200524091205,31.941077973338,-213.572715378021));
#218771=CARTESIAN_POINT('Ctrl Pts',(61.5768449470309,32.0813729523784,-213.563091155333));
#218772=CARTESIAN_POINT('Ctrl Pts',(61.5412940675433,32.1968069457527,-213.555172393981));
#218773=CARTESIAN_POINT('Ctrl Pts',(61.5039582038038,32.3115108548697,-213.547476866768));
#218774=CARTESIAN_POINT('Ctrl Pts',(61.4648558996718,32.4254280494983,-213.540024838124));
#218775=CARTESIAN_POINT('Ctrl Pts',(61.4637643495236,32.4286080751626,-213.539816812967));
#218776=CARTESIAN_POINT('Ctrl Pts',(61.4627391435221,32.4315904138355,-213.539621864181));
#218777=CARTESIAN_POINT('Ctrl Pts',(61.4617011316131,32.4346060163256,-213.539424870969));
#218778=CARTESIAN_POINT('Ctrl Pts',(61.4600818133902,32.4393104132821,-213.539117557831));
#218779=CARTESIAN_POINT('Ctrl Pts',(61.4584315246665,32.4440961213275,-213.538805189393));
#218780=CARTESIAN_POINT('Ctrl Pts',(61.4564456905764,32.4498387425552,-213.538430823349));
#218781=CARTESIAN_POINT('Ctrl Pts',(61.4168161144555,32.5644392755033,-213.530959923492));
#218782=CARTESIAN_POINT('Ctrl Pts',(61.3757353289488,32.6772777468317,-213.52379011113));
#218783=CARTESIAN_POINT('Ctrl Pts',(61.3334684629503,32.7880141235003,-213.516853234189));
#218784=CARTESIAN_POINT('Ctrl Pts',(61.3280232273835,32.8022802783837,-213.515959557117));
#218785=CARTESIAN_POINT('Ctrl Pts',(61.3225582818976,32.8165116104594,-213.515069754931));
#218786=CARTESIAN_POINT('Ctrl Pts',(61.317074171808,32.8307074509615,-213.514183689717));
#218787=CARTESIAN_POINT('Ctrl Pts',(61.2657604929994,32.963534981416,-213.505892961587));
#218788=CARTESIAN_POINT('Ctrl Pts',(61.2127553614539,33.0933166559663,-213.497856596317));
#218789=CARTESIAN_POINT('Ctrl Pts',(61.1582925442941,33.2201235367584,-213.490078204233));
#218790=CARTESIAN_POINT('Ctrl Pts',(61.0707863518123,33.423865977882,-213.477580549678));
#218791=CARTESIAN_POINT('Ctrl Pts',(60.9794973350864,33.6199773638123,-213.466093247516));
#218792=CARTESIAN_POINT('Ctrl Pts',(60.8853140442522,33.8087163473985,-213.455630952108));
#218793=CARTESIAN_POINT('Ctrl Pts',(60.8567940840068,33.8658690361711,-213.452462829116));
#218794=CARTESIAN_POINT('Ctrl Pts',(60.8280087145055,33.9223456729049,-213.449388335299));
#218795=CARTESIAN_POINT('Ctrl Pts',(60.7989825602443,33.9781533043984,-213.446406949198));
#218796=CARTESIAN_POINT('Ctrl Pts',(60.7789255400534,34.0167162770057,-213.444346816784));
#218797=CARTESIAN_POINT('Ctrl Pts',(60.758753934641,34.0549586516216,-213.44232317516));
#218798=CARTESIAN_POINT('Ctrl Pts',(60.7384761670337,34.0928815999144,-213.440328492273));
#218799=CARTESIAN_POINT('Ctrl Pts',(60.6923105839104,34.179219260726,-213.43578727746));
#218800=CARTESIAN_POINT('Ctrl Pts',(60.645609474611,34.2638723253871,-213.431435301927));
#218801=CARTESIAN_POINT('Ctrl Pts',(60.5984740490749,34.3468561605459,-213.427198972163));
#218802=CARTESIAN_POINT('Ctrl Pts',(60.5325838024229,34.4628586216366,-213.421277039564));
#218803=CARTESIAN_POINT('Ctrl Pts',(60.465847821872,34.5755963690338,-213.415555332432));
#218804=CARTESIAN_POINT('Ctrl Pts',(60.3984978653644,34.6851586013184,-213.410238215137));
#218805=CARTESIAN_POINT('Ctrl Pts',(60.3936934720552,34.6929741973935,-213.409858919825));
#218806=CARTESIAN_POINT('Ctrl Pts',(60.3888859574889,34.7007736311751,-213.409481661815));
#218807=CARTESIAN_POINT('Ctrl Pts',(60.3840754072371,34.7085569334586,-213.409106505425));
#218808=CARTESIAN_POINT('Ctrl Pts',(60.366977631822,34.7362205368859,-213.407773115403));
#218809=CARTESIAN_POINT('Ctrl Pts',(60.3498409473359,34.7636809861284,-213.406471589833));
#218810=CARTESIAN_POINT('Ctrl Pts',(60.3326688897114,34.7909397659281,-213.405206193258));
#218811=CARTESIAN_POINT('Ctrl Pts',(60.3123511070016,34.8231920432625,-213.403708990464));
#218812=CARTESIAN_POINT('Ctrl Pts',(60.2919954872675,34.8551439920857,-213.402249242024));
#218813=CARTESIAN_POINT('Ctrl Pts',(60.2716012226596,34.8868093488113,-213.400835331901));
#218814=CARTESIAN_POINT('Ctrl Pts',(60.233057341349,34.9466548874837,-213.398163130427));
#218815=CARTESIAN_POINT('Ctrl Pts',(60.1943775602019,35.0054745948108,-213.395635650738));
#218816=CARTESIAN_POINT('Ctrl Pts',(60.1555597569617,35.0633482773578,-213.393230682939));
#218817=CARTESIAN_POINT('Ctrl Pts',(60.1054112893713,35.1381149115123,-213.390123720679));
#218818=CARTESIAN_POINT('Ctrl Pts',(60.0550310847817,35.2112955200002,-213.387210565911));
#218819=CARTESIAN_POINT('Ctrl Pts',(60.0045837464213,35.2828198922257,-213.384513350095));
#218820=CARTESIAN_POINT('Ctrl Pts',(59.9742196990514,35.3258701203834,-213.382889906887));
#218821=CARTESIAN_POINT('Ctrl Pts',(59.9438303909373,35.3683210152462,-213.381344746419));
#218822=CARTESIAN_POINT('Ctrl Pts',(59.9134443065957,35.4101621769143,-213.379883144536));
#218823=CARTESIAN_POINT('Ctrl Pts',(58.6665914736623,34.7169872964315,-216.775646223557));
#218824=CARTESIAN_POINT('Ctrl Pts',(58.6670681057105,34.7163534317084,-216.775672326265));
#218825=CARTESIAN_POINT('Ctrl Pts',(58.6694802109214,34.7133058321613,-216.775702228632));
#218826=CARTESIAN_POINT('Ctrl Pts',(58.6738398478374,34.7078154007888,-216.77573593066));
#218827=CARTESIAN_POINT('Ctrl Pts',(58.6779611895904,34.7026250731325,-216.775767790554));
#218828=CARTESIAN_POINT('Ctrl Pts',(58.6838228717898,34.6952517669432,-216.775803046086));
#218829=CARTESIAN_POINT('Ctrl Pts',(58.6914531347878,34.6856286956792,-216.775841697255));
#218830=CARTESIAN_POINT('Ctrl Pts',(58.6946762133137,34.6815638404636,-216.77585802379));
#218831=CARTESIAN_POINT('Ctrl Pts',(58.6982150950876,34.6770970184521,-216.775874956201));
#218832=CARTESIAN_POINT('Ctrl Pts',(58.7020730820553,34.6722205751115,-216.775892494489));
#218833=CARTESIAN_POINT('Ctrl Pts',(58.7104004168453,34.6616949365798,-216.775930350291));
#218834=CARTESIAN_POINT('Ctrl Pts',(58.7202130485412,34.6492638479551,-216.775971028858));
#218835=CARTESIAN_POINT('Ctrl Pts',(58.7315582160844,34.6348202407144,-216.776014530189));
#218836=CARTESIAN_POINT('Ctrl Pts',(58.7356441068596,34.6296184663589,-216.776030196919));
#218837=CARTESIAN_POINT('Ctrl Pts',(58.7399289731632,34.624155238461,-216.776046229773));
#218838=CARTESIAN_POINT('Ctrl Pts',(58.7444157618656,34.6184240118923,-216.776062628748));
#218839=CARTESIAN_POINT('Ctrl Pts',(58.752888320475,34.6076015381303,-216.776093595502));
#218840=CARTESIAN_POINT('Ctrl Pts',(58.7599936864881,34.5984905903666,-216.77611896689));
#218841=CARTESIAN_POINT('Ctrl Pts',(58.766363196952,34.5903053720178,-216.776141810194));
#218842=CARTESIAN_POINT('Ctrl Pts',(58.7727327074159,34.582120153669,-216.776164653498));
#218843=CARTESIAN_POINT('Ctrl Pts',(58.7783668410405,34.5748594774657,-216.776184968719));
#218844=CARTESIAN_POINT('Ctrl Pts',(58.7839180023781,34.5676893598984,-216.776205823138));
#218845=CARTESIAN_POINT('Ctrl Pts',(58.7981566088431,34.5492981663918,-216.776259314263));
#218846=CARTESIAN_POINT('Ctrl Pts',(58.8103680803945,34.5334124046094,-216.776308259613));
#218847=CARTESIAN_POINT('Ctrl Pts',(58.8204666936249,34.5202243498463,-216.776352659188));
#218848=CARTESIAN_POINT('Ctrl Pts',(58.8261165404609,34.5128460605926,-216.776377499311));
#218849=CARTESIAN_POINT('Ctrl Pts',(58.831105290415,34.5063115020565,-216.776400916589));
#218850=CARTESIAN_POINT('Ctrl Pts',(58.8354207734538,34.5006474105254,-216.776422911022));
#218851=CARTESIAN_POINT('Ctrl Pts',(58.8430653672725,34.4906138456338,-216.776461872709));
#218852=CARTESIAN_POINT('Ctrl Pts',(58.8509803426121,34.4801753925234,-216.776514330255));
#218853=CARTESIAN_POINT('Ctrl Pts',(58.859576729319,34.4687645990523,-216.77659066946));
#218854=CARTESIAN_POINT('Ctrl Pts',(58.8645070583051,34.4622201091727,-216.776634452669));
#218855=CARTESIAN_POINT('Ctrl Pts',(58.8696618519958,34.4553550877796,-216.776686091569));
#218856=CARTESIAN_POINT('Ctrl Pts',(58.8751220460667,34.4480552757866,-216.776747545545));
#218857=CARTESIAN_POINT('Ctrl Pts',(58.8887140285765,34.4298839588616,-216.776900522043));
#218858=CARTESIAN_POINT('Ctrl Pts',(58.9035417976025,34.4099025757787,-216.777103008302));
#218859=CARTESIAN_POINT('Ctrl Pts',(58.9196893653339,34.3879363985254,-216.777355004323));
#218860=CARTESIAN_POINT('Ctrl Pts',(58.9350478981359,34.3670435768017,-216.777594686807));
#218861=CARTESIAN_POINT('Ctrl Pts',(58.9516002919803,34.344355360868,-216.777879158776));
#218862=CARTESIAN_POINT('Ctrl Pts',(58.9694406023619,34.3196790386863,-216.778208420229));
#218863=CARTESIAN_POINT('Ctrl Pts',(58.9741892585224,34.3131108026612,-216.778296061609));
#218864=CARTESIAN_POINT('Ctrl Pts',(58.9790292925856,34.3064014597548,-216.778386876301));
#218865=CARTESIAN_POINT('Ctrl Pts',(58.9839627723711,34.2995468089717,-216.778480864304));
#218866=CARTESIAN_POINT('Ctrl Pts',(58.9886303649067,34.2930615859201,-216.778569786874));
#218867=CARTESIAN_POINT('Ctrl Pts',(58.9937888639037,34.2858763757545,-216.778670966967));
#218868=CARTESIAN_POINT('Ctrl Pts',(58.9986503973408,34.2790909006063,-216.778766669489));
#218869=CARTESIAN_POINT('Ctrl Pts',(59.0011878457208,34.275549262326,-216.77881662085));
#218870=CARTESIAN_POINT('Ctrl Pts',(59.0036439919825,34.2721173577295,-216.77886507998));
#218871=CARTESIAN_POINT('Ctrl Pts',(59.0059043510499,34.2689566585687,-216.778909525111));
#218872=CARTESIAN_POINT('Ctrl Pts',(59.0092769019573,34.2642407623304,-216.778975839117));
#218873=CARTESIAN_POINT('Ctrl Pts',(59.0122136252413,34.2601285170381,-216.779033217198));
#218874=CARTESIAN_POINT('Ctrl Pts',(59.0143297408352,34.2571655299183,-216.779073283126));
#218875=CARTESIAN_POINT('Ctrl Pts',(59.0205814042945,34.2484119446414,-216.779191650335));
#218876=CARTESIAN_POINT('Ctrl Pts',(59.0269902590843,34.2394421233898,-216.779297323683));
#218877=CARTESIAN_POINT('Ctrl Pts',(59.0335603692097,34.230245789034,-216.779390226452));
#218878=CARTESIAN_POINT('Ctrl Pts',(59.0467005894606,34.2118531203223,-216.779576031989));
#218879=CARTESIAN_POINT('Ctrl Pts',(59.0604859975106,34.1925545204065,-216.779710952715));
#218880=CARTESIAN_POINT('Ctrl Pts',(59.0749542980427,34.1722521293946,-216.779794966433));
#218881=CARTESIAN_POINT('Ctrl Pts',(59.0928834858082,34.1470933085825,-216.779899076638));
#218882=CARTESIAN_POINT('Ctrl Pts',(59.1118608905283,34.1203946818412,-216.779925012753));
#218883=CARTESIAN_POINT('Ctrl Pts',(59.1319699799244,34.0919293325671,-216.779872774776));
#218884=CARTESIAN_POINT('Ctrl Pts',(59.1515521564952,34.0642098528504,-216.779821905577));
#218885=CARTESIAN_POINT('Ctrl Pts',(59.1722074420135,34.034815269011,-216.779696905362));
#218886=CARTESIAN_POINT('Ctrl Pts',(59.1940260470494,34.00348904357,-216.77949777413));
#218887=CARTESIAN_POINT('Ctrl Pts',(59.2150912904043,33.9732444627997,-216.779305518583));
#218888=CARTESIAN_POINT('Ctrl Pts',(59.2372408851721,33.9411994683062,-216.779044162892));
#218889=CARTESIAN_POINT('Ctrl Pts',(59.2605688679621,33.9070761502832,-216.778713707057));
#218890=CARTESIAN_POINT('Ctrl Pts',(59.2683576234456,33.8956830442971,-216.778603374341));
#218891=CARTESIAN_POINT('Ctrl Pts',(59.2762778514711,33.8840578464883,-216.77848533861));
#218892=CARTESIAN_POINT('Ctrl Pts',(59.2843333938043,33.8721889432235,-216.778359599865));
#218893=CARTESIAN_POINT('Ctrl Pts',(59.2946877417116,33.8569330177253,-216.778197979125));
#218894=CARTESIAN_POINT('Ctrl Pts',(59.3052656351694,33.8412745138219,-216.778023631672));
#218895=CARTESIAN_POINT('Ctrl Pts',(59.3160756783319,33.825187105161,-216.777836559618));
#218896=CARTESIAN_POINT('Ctrl Pts',(59.3214806999131,33.8171434008306,-216.777743023591));
#218897=CARTESIAN_POINT('Ctrl Pts',(59.3269437546586,33.8089924675107,-216.777646301599));
#218898=CARTESIAN_POINT('Ctrl Pts',(59.3324659843164,33.8007307931777,-216.777546401141));
#218899=CARTESIAN_POINT('Ctrl Pts',(59.336148956312,33.7952207877831,-216.777479773962));
#218900=CARTESIAN_POINT('Ctrl Pts',(59.3386313887352,33.7914980545715,-216.77743462791));
#218901=CARTESIAN_POINT('Ctrl Pts',(59.3409419466165,33.788029764492,-216.777393081159));
#218902=CARTESIAN_POINT('Ctrl Pts',(59.3420958275834,33.7862977178972,-216.777372332921));
#218903=CARTESIAN_POINT('Ctrl Pts',(59.3432071719571,33.7846282449242,-216.777352482332));
#218904=CARTESIAN_POINT('Ctrl Pts',(59.3444056335457,33.7828262864623,-216.777331302268));
#218905=CARTESIAN_POINT('Ctrl Pts',(59.3587987884887,33.7611853197513,-216.777076936214));
#218906=CARTESIAN_POINT('Ctrl Pts',(59.3733313547227,33.7391229883341,-216.776840546535));
#218907=CARTESIAN_POINT('Ctrl Pts',(59.3880081141125,33.7166181250504,-216.776622133232));
#218908=CARTESIAN_POINT('Ctrl Pts',(59.3968408863624,33.7030742406942,-216.776490687664));
#218909=CARTESIAN_POINT('Ctrl Pts',(59.4057258834763,33.689370076979,-216.776365752919));
#218910=CARTESIAN_POINT('Ctrl Pts',(59.414664146579,33.6755010224523,-216.776247328996));
#218911=CARTESIAN_POINT('Ctrl Pts',(59.4354299748332,33.6432797283332,-216.775972200504));
#218912=CARTESIAN_POINT('Ctrl Pts',(59.4564833090992,33.6101684309622,-216.775732214143));
#218913=CARTESIAN_POINT('Ctrl Pts',(59.4777543001217,33.5762439212329,-216.775527369912));
#218914=CARTESIAN_POINT('Ctrl Pts',(59.5386076841382,33.4791905579952,-216.7749413387));
#218915=CARTESIAN_POINT('Ctrl Pts',(59.6012426021026,33.3754811362627,-216.774642929323));
#218916=CARTESIAN_POINT('Ctrl Pts',(59.6640221266443,33.2669168310396,-216.774632140179));
#218917=CARTESIAN_POINT('Ctrl Pts',(59.6954118889152,33.2126346784281,-216.774626745607));
#218918=CARTESIAN_POINT('Ctrl Pts',(59.7268378070652,33.1571388073496,-216.774693260578));
#218919=CARTESIAN_POINT('Ctrl Pts',(59.7580951362872,33.1006547607048,-216.774831677976));
#218920=CARTESIAN_POINT('Ctrl Pts',(59.7624935951323,33.0927064567148,-216.774851155751));
#218921=CARTESIAN_POINT('Ctrl Pts',(59.7675147142201,33.0835960625502,-216.774877767774));
#218922=CARTESIAN_POINT('Ctrl Pts',(59.771546136366,33.0762626462417,-216.77489833135));
#218923=CARTESIAN_POINT('Ctrl Pts',(59.7746769665955,33.0705674645828,-216.774914301164));
#218924=CARTESIAN_POINT('Ctrl Pts',(59.7772112214269,33.0659462300852,-216.774926623049));
#218925=CARTESIAN_POINT('Ctrl Pts',(59.7783965726506,33.0637901480713,-216.774929122416));
#218926=CARTESIAN_POINT('Ctrl Pts',(59.7811082446338,33.0588577811293,-216.774934840101));
#218927=CARTESIAN_POINT('Ctrl Pts',(59.7843039578434,33.0530748594205,-216.774921261397));
#218928=CARTESIAN_POINT('Ctrl Pts',(59.787982068665,33.0464338395745,-216.774888013666));
#218929=CARTESIAN_POINT('Ctrl Pts',(59.7953382903084,33.0331517998827,-216.774821518205));
#218930=CARTESIAN_POINT('Ctrl Pts',(59.8046250197526,33.016437872032,-216.77467730494));
#218931=CARTESIAN_POINT('Ctrl Pts',(59.8158139222979,32.9962087252168,-216.774455267294));
#218932=CARTESIAN_POINT('Ctrl Pts',(59.8273746215905,32.9753073828081,-216.774225851545));
#218933=CARTESIAN_POINT('Ctrl Pts',(59.8409673874441,32.9506520965263,-216.773913353466));
#218934=CARTESIAN_POINT('Ctrl Pts',(59.8565272281041,32.9221349455562,-216.773517773058));
#218935=CARTESIAN_POINT('Ctrl Pts',(59.8668775326413,32.9031655226989,-216.77325463555));
#218936=CARTESIAN_POINT('Ctrl Pts',(59.8780975533821,32.8824869344996,-216.772954735577));
#218937=CARTESIAN_POINT('Ctrl Pts',(59.890155046688,32.86006864128,-216.772618073137));
#218938=CARTESIAN_POINT('Ctrl Pts',(59.8950579505909,32.8509527550394,-216.772481177056));
#218939=CARTESIAN_POINT('Ctrl Pts',(59.9000991622126,32.8415492682111,-216.772338202461));
#218940=CARTESIAN_POINT('Ctrl Pts',(59.905276601872,32.8318558217261,-216.772189149354));
#218941=CARTESIAN_POINT('Ctrl Pts',(59.923802279304,32.7971711755308,-216.771655814354));
#218942=CARTESIAN_POINT('Ctrl Pts',(59.9440745976445,32.7587734499515,-216.771044655015));
#218943=CARTESIAN_POINT('Ctrl Pts',(59.9659784543963,32.7165579454281,-216.770355671337));
#218944=CARTESIAN_POINT('Ctrl Pts',(59.9785736797882,32.6922830517175,-216.769959489751));
#218945=CARTESIAN_POINT('Ctrl Pts',(59.9897140153398,32.6705908525983,-216.769604001407));
#218946=CARTESIAN_POINT('Ctrl Pts',(60.0001226521558,32.6501730512935,-216.769272192519));
#218947=CARTESIAN_POINT('Ctrl Pts',(60.0078152626543,32.6350830644442,-216.769026965734));
#218948=CARTESIAN_POINT('Ctrl Pts',(60.0151073907883,32.6206878929927,-216.768794672909));
#218949=CARTESIAN_POINT('Ctrl Pts',(60.0222799414978,32.6064454485188,-216.768568445878));
#218950=CARTESIAN_POINT('Ctrl Pts',(60.0440128353844,32.5632907122228,-216.767882975919));
#218951=CARTESIAN_POINT('Ctrl Pts',(60.0636456592396,32.5235387638354,-216.767272561604));
#218952=CARTESIAN_POINT('Ctrl Pts',(60.0812847352957,32.4873272570907,-216.766737202934));
#218953=CARTESIAN_POINT('Ctrl Pts',(60.0910422583728,32.4672959010496,-216.766441055077));
#218954=CARTESIAN_POINT('Ctrl Pts',(60.1001895698892,32.4483469042561,-216.766167874568));
#218955=CARTESIAN_POINT('Ctrl Pts',(60.1087433600541,32.4304970192806,-216.765917661409));
#218956=CARTESIAN_POINT('Ctrl Pts',(60.120751774401,32.4054380909345,-216.765566394517));
#218957=CARTESIAN_POINT('Ctrl Pts',(60.1315907220463,32.3825457742647,-216.765260392976));
#218958=CARTESIAN_POINT('Ctrl Pts',(60.1413019208989,32.3618542151778,-216.764999703275));
#218959=CARTESIAN_POINT('Ctrl Pts',(60.1461575203253,32.3515084356343,-216.764869358425));
#218960=CARTESIAN_POINT('Ctrl Pts',(60.1507310984236,32.34171280714,-216.764750259777));
#218961=CARTESIAN_POINT('Ctrl Pts',(60.1550272753044,32.3324703279183,-216.764642510907));
#218962=CARTESIAN_POINT('Ctrl Pts',(60.1571753637447,32.3278490883075,-216.764588636472));
#218963=CARTESIAN_POINT('Ctrl Pts',(60.1592540966846,32.3233661336264,-216.764537594417));
#218964=CARTESIAN_POINT('Ctrl Pts',(60.1612640098706,32.3190218110534,-216.764489384796));
#218965=CARTESIAN_POINT('Ctrl Pts',(60.1632739230566,32.3146774884804,-216.764441175175));
#218966=CARTESIAN_POINT('Ctrl Pts',(60.1643981239921,32.3122456819017,-216.764414355239));
#218967=CARTESIAN_POINT('Ctrl Pts',(60.1670878018744,32.3064050638589,-216.764353243169));
#218968=CARTESIAN_POINT('Ctrl Pts',(60.2018664146461,32.2308835322313,-216.763563039623));
#218969=CARTESIAN_POINT('Ctrl Pts',(60.2364926227202,32.1536653398071,-216.762652288959));
#218970=CARTESIAN_POINT('Ctrl Pts',(60.2707822025251,32.0749362568614,-216.761620991176));
#218971=CARTESIAN_POINT('Ctrl Pts',(60.2901586062156,32.030447916613,-216.761038223984));
#218972=CARTESIAN_POINT('Ctrl Pts',(60.3094271217391,31.9854779357794,-216.760416964048));
#218973=CARTESIAN_POINT('Ctrl Pts',(60.3285512744986,31.9400665097129,-216.75975721137));
#218974=CARTESIAN_POINT('Ctrl Pts',(60.3668652508642,31.8490877182901,-216.758435440475));
#218975=CARTESIAN_POINT('Ctrl Pts',(60.4045983421644,31.7563428873234,-216.756959169431));
#218976=CARTESIAN_POINT('Ctrl Pts',(60.4416544436433,31.6615857304821,-216.755328398239));
#218977=CARTESIAN_POINT('Ctrl Pts',(60.478078104031,31.5684458058176,-216.753725459621));
#218978=CARTESIAN_POINT('Ctrl Pts',(60.513847627481,31.4733618155951,-216.751973249597));
#218979=CARTESIAN_POINT('Ctrl Pts',(60.5488797035791,31.3760505696478,-216.750071768167));
#218980=CARTESIAN_POINT('Ctrl Pts',(60.5831095211231,31.2809678179308,-216.748213831966));
#218981=CARTESIAN_POINT('Ctrl Pts',(60.6166352373989,31.183758742476,-216.746213382909));
#218982=CARTESIAN_POINT('Ctrl Pts',(60.649387527739,31.0841099747386,-216.744070420997));
#218983=CARTESIAN_POINT('Ctrl Pts',(60.6594381189747,31.0535310741102,-216.743412817086));
#218984=CARTESIAN_POINT('Ctrl Pts',(60.6694159421373,31.0227220726697,-216.742741793132));
#218985=CARTESIAN_POINT('Ctrl Pts',(60.6793191674292,30.9916729347315,-216.742057349136));
#218986=CARTESIAN_POINT('Ctrl Pts',(60.704438687947,30.9129168290677,-216.740321257659));
#218987=CARTESIAN_POINT('Ctrl Pts',(60.7290793248211,30.8326114173318,-216.738498823948));
#218988=CARTESIAN_POINT('Ctrl Pts',(60.7531045634047,30.7510497143758,-216.736590048002));
#218989=CARTESIAN_POINT('Ctrl Pts',(60.7768402186365,30.6704710989022,-216.734704279101));
#218990=CARTESIAN_POINT('Ctrl Pts',(60.7999752420945,30.5886661793071,-216.732734236839));
#218991=CARTESIAN_POINT('Ctrl Pts',(60.8223658568759,30.505966038184,-216.730679921216));
#218992=CARTESIAN_POINT('Ctrl Pts',(60.8443315930004,30.424835194073,-216.728664587767));
#218993=CARTESIAN_POINT('Ctrl Pts',(60.8655809084215,30.3428427332773,-216.726568148913));
#218994=CARTESIAN_POINT('Ctrl Pts',(60.8859661387063,30.2603493499802,-216.724390604653));
#218995=CARTESIAN_POINT('Ctrl Pts',(60.905775148304,30.1801877722767,-216.722274612115));
#218996=CARTESIAN_POINT('Ctrl Pts',(60.924768216205,30.0995532287051,-216.720082034513));
#218997=CARTESIAN_POINT('Ctrl Pts',(60.9427985975151,30.018822490257,-216.717812871847));
#218998=CARTESIAN_POINT('Ctrl Pts',(60.9628078301142,29.929231477415,-216.715294666445));
#218999=CARTESIAN_POINT('Ctrl Pts',(60.981629326843,29.8395226647074,-216.712682142926));
#219000=CARTESIAN_POINT('Ctrl Pts',(60.9992577262092,29.7501026756727,-216.709975301288));
#219001=CARTESIAN_POINT('Ctrl Pts',(61.0089023416902,29.7011804001644,-216.70849437008));
#219002=CARTESIAN_POINT('Ctrl Pts',(61.0181900345037,29.6523454397984,-216.706985207031));
#219003=CARTESIAN_POINT('Ctrl Pts',(61.0271214515743,29.6036708476852,-216.705447812141));
#219004=CARTESIAN_POINT('Ctrl Pts',(59.4999643211654,35.9450057402374,-213.371639708519));
#219005=CARTESIAN_POINT('Ctrl Pts',(59.4820528027665,35.9125166648153,-215.346308247144));
#219006=CARTESIAN_POINT('Ctrl Pts',(58.4265182736836,35.031835198701,-216.764384131257));
#219007=CARTESIAN_POINT('Ctrl Pts',(59.6440986517757,35.7696968033851,-213.370755972398));
#219008=CARTESIAN_POINT('Ctrl Pts',(59.6013542567595,35.7669646494558,-215.346152352702));
#219009=CARTESIAN_POINT('Ctrl Pts',(58.510163538665,34.9284713760201,-216.764533686556));
#219010=CARTESIAN_POINT('Ctrl Pts',(59.7818407313688,35.5913782362947,-213.373552880528));
#219011=CARTESIAN_POINT('Ctrl Pts',(59.7162237024563,35.619624715777,-215.350089533734));
#219012=CARTESIAN_POINT('Ctrl Pts',(58.5901397589686,34.8235003567024,-216.76833687912));
#219013=CARTESIAN_POINT('Ctrl Pts',(59.9134443065991,35.4101621769129,-213.379883144535));
#219014=CARTESIAN_POINT('Ctrl Pts',(59.8268417476681,35.4705704696998,-215.357954892849));
#219015=CARTESIAN_POINT('Ctrl Pts',(58.6665914736623,34.7169872964315,-216.775646223556));
#219016=CARTESIAN_POINT('',(58.4265182736835,35.0318351987012,-216.764384131257));
#219017=CARTESIAN_POINT('',(59.4999643211654,35.9450057402376,-213.371639708519));
#219018=CARTESIAN_POINT('Origin',(55.6381166865346,32.7703375395218,-213.284377676332));
#219019=CARTESIAN_POINT('Origin',(52.7506200812507,30.3721960348575,-218.064222059651));
#219020=CARTESIAN_POINT('Origin',(55.6093041609777,32.7570348813246,-220.18888881869));
#219021=CARTESIAN_POINT('Ctrl Pts',(58.4265182736835,35.0318351987011,-216.764384131257));
#219022=CARTESIAN_POINT('Ctrl Pts',(59.4820528027664,35.9125166648155,-215.346308247144));
#219023=CARTESIAN_POINT('Ctrl Pts',(59.4999643211654,35.9450057402375,-213.371639708519));
#219024=CARTESIAN_POINT('Ctrl Pts',(57.5486529224426,36.1166487545749,-216.76281454263));
#219025=CARTESIAN_POINT('Ctrl Pts',(58.5785030826818,37.0120312881232,-215.346864153326));
#219026=CARTESIAN_POINT('Ctrl Pts',(58.5926451028776,37.0484655333588,-213.380920503252));
#219027=CARTESIAN_POINT('Ctrl Pts',(56.6223825642191,37.1990499756784,-216.761500614409));
#219028=CARTESIAN_POINT('Ctrl Pts',(57.6304520413514,38.1023651317007,-215.347861259707));
#219029=CARTESIAN_POINT('Ctrl Pts',(57.6483853099758,38.1336349814895,-213.391180664313));
#219030=CARTESIAN_POINT('Ctrl Pts',(55.6813080372829,38.2352492592495,-216.760202274403));
#219031=CARTESIAN_POINT('Ctrl Pts',(56.6650296771562,39.1519706625638,-215.348455523392));
#219032=CARTESIAN_POINT('Ctrl Pts',(56.682191157046,39.1835711849515,-213.399142265953));
#219033=CARTESIAN_POINT('Ctrl Pts',(59.4999643211654,35.9450057402376,-213.371639708519));
#219034=CARTESIAN_POINT('Ctrl Pts',(59.3530691590842,36.1236561004343,-213.373142271034));
#219035=CARTESIAN_POINT('Ctrl Pts',(59.2112226056842,36.2945126600292,-213.374608432805));
#219036=CARTESIAN_POINT('Ctrl Pts',(59.0746685317258,36.4576720204601,-213.376021791858));
#219037=CARTESIAN_POINT('Ctrl Pts',(58.9328872802121,36.6270769869141,-213.377489253132));
#219038=CARTESIAN_POINT('Ctrl Pts',(58.796811282469,36.7881845701405,-213.378899850635));
#219039=CARTESIAN_POINT('Ctrl Pts',(58.6666613429046,36.9411232025734,-213.380242059925));
#219040=CARTESIAN_POINT('Ctrl Pts',(58.5286621778041,37.1032854260672,-213.381665216648));
#219041=CARTESIAN_POINT('Ctrl Pts',(58.3973253842116,37.2562640920389,-213.383011540957));
#219042=CARTESIAN_POINT('Ctrl Pts',(58.2728579280455,37.4002283770448,-213.384273976912));
#219043=CARTESIAN_POINT('Ctrl Pts',(58.1439265508173,37.5493558205486,-213.385581689076));
#219044=CARTESIAN_POINT('Ctrl Pts',(58.0223657791532,37.6888112780918,-213.386799480846));
#219045=CARTESIAN_POINT('Ctrl Pts',(57.9083499192908,37.8187915053139,-213.387925278214));
#219046=CARTESIAN_POINT('Ctrl Pts',(57.7890456668349,37.9548005996757,-213.389103293391));
#219047=CARTESIAN_POINT('Ctrl Pts',(57.6780022225769,38.080435763234,-213.390180681546));
#219048=CARTESIAN_POINT('Ctrl Pts',(57.5753634650057,38.1959220404739,-213.391159767909));
#219049=CARTESIAN_POINT('Ctrl Pts',(57.5666424872746,38.205734642223,-213.391242958612));
#219050=CARTESIAN_POINT('Ctrl Pts',(57.5579821567034,38.2154739702272,-213.391325441773));
#219051=CARTESIAN_POINT('Ctrl Pts',(57.54938254494,38.2251401600279,-213.391407219936));
#219052=CARTESIAN_POINT('Ctrl Pts',(57.4434126431882,38.3442531167146,-213.392414942629));
#219053=CARTESIAN_POINT('Ctrl Pts',(57.3467222359999,38.4521993238965,-213.393315003254));
#219054=CARTESIAN_POINT('Ctrl Pts',(57.2595019988215,38.5491319021046,-213.394112818152));
#219055=CARTESIAN_POINT('Ctrl Pts',(57.1707868735558,38.6477258304891,-213.394924306987));
#219056=CARTESIAN_POINT('Ctrl Pts',(57.0918688820637,38.7349261105185,-213.395630140928));
#219057=CARTESIAN_POINT('Ctrl Pts',(57.0229004219518,38.8108710912233,-213.396237430413));
#219058=CARTESIAN_POINT('Ctrl Pts',(56.9539806056297,38.8867625075645,-213.396844291575));
#219059=CARTESIAN_POINT('Ctrl Pts',(56.8949958287087,38.9514150403455,-213.39735285088));
#219060=CARTESIAN_POINT('Ctrl Pts',(56.846057438065,39.0049345300186,-213.397769859768));
#219061=CARTESIAN_POINT('Ctrl Pts',(56.7974487746849,39.0580934268187,-213.398184059017));
#219062=CARTESIAN_POINT('Ctrl Pts',(56.758751223571,39.1002691381783,-213.398508007919));
#219063=CARTESIAN_POINT('Ctrl Pts',(56.7300398301481,39.1315270272855,-213.398746686664));
#219064=CARTESIAN_POINT('Ctrl Pts',(56.718140259053,39.1444820054098,-213.398845608184));
#219065=CARTESIAN_POINT('Ctrl Pts',(56.7079556605156,39.1555611147679,-213.398929857286));
#219066=CARTESIAN_POINT('Ctrl Pts',(56.6994898314762,39.1647668800231,-213.398999668388));
#219067=CARTESIAN_POINT('Origin',(55.9211377566494,34.484843995799,-216.774150960848));
#219068=CARTESIAN_POINT('Ctrl Pts',(-33.195117167568,-74.788972786398,-216.360364163614));
#219069=CARTESIAN_POINT('Ctrl Pts',(-33.5111161912263,-75.4317844535893,
-215.275130706023));
#219070=CARTESIAN_POINT('Ctrl Pts',(-33.8499480590156,-75.4429517542805,
-214.019797229742));
#219071=CARTESIAN_POINT('Ctrl Pts',(-32.6155847805473,-74.7878402293263,
-216.243940775302));
#219072=CARTESIAN_POINT('Ctrl Pts',(-32.8892442190157,-75.4538060704667,
-215.132352055413));
#219073=CARTESIAN_POINT('Ctrl Pts',(-33.1824288617165,-75.4672690607831,
-213.840684379537));
#219074=CARTESIAN_POINT('Ctrl Pts',(-32.0212270237052,-74.7863264493868,
-216.159798603417));
#219075=CARTESIAN_POINT('Ctrl Pts',(-32.2560519535044,-75.4749926756692,
-215.02671038484));
#219076=CARTESIAN_POINT('Ctrl Pts',(-32.5054567082896,-75.490529408973,
-213.70327768978));
#219077=CARTESIAN_POINT('Ctrl Pts',(-30.8096077807694,-74.7834423664695,
-216.044618097811));
#219078=CARTESIAN_POINT('Ctrl Pts',(-30.9708520272369,-75.5157273627552,
-214.874910704589));
#219079=CARTESIAN_POINT('Ctrl Pts',(-31.1363635597063,-75.5350116089517,
-213.495389670921));
#219080=CARTESIAN_POINT('Ctrl Pts',(-30.1906743701442,-74.7820017193782,
-216.013777891697));
#219081=CARTESIAN_POINT('Ctrl Pts',(-30.3169577787275,-75.5353200743763,
-214.829020724472));
#219082=CARTESIAN_POINT('Ctrl Pts',(-30.4420278504982,-75.5562948594353,
-213.424911104697));
#219083=CARTESIAN_POINT('Ctrl Pts',(-28.3231908545672,-74.7775797475947,
-215.993570943196));
#219084=CARTESIAN_POINT('Ctrl Pts',(-28.3468574989069,-75.5911225591905,
-214.770729972352));
#219085=CARTESIAN_POINT('Ctrl Pts',(-28.3564670829161,-75.6166161717328,
-213.301750622476));
#219086=CARTESIAN_POINT('Ctrl Pts',(-27.0679344027315,-74.7746484451523,
-216.074360875667));
#219087=CARTESIAN_POINT('Ctrl Pts',(-27.0307252020175,-75.6241519763574,
-214.8360616272));
#219088=CARTESIAN_POINT('Ctrl Pts',(-26.9668397448124,-75.6520766916683,
-213.334864912836));
#219089=CARTESIAN_POINT('Ctrl Pts',(-25.4972121053677,-74.7680761663345,
-216.277655442628));
#219090=CARTESIAN_POINT('Ctrl Pts',(-25.3875902558758,-75.660467613276,
-215.025917676458));
#219091=CARTESIAN_POINT('Ctrl Pts',(-25.2304946712801,-75.69095341109,-213.493045368148));
#219092=CARTESIAN_POINT('Ctrl Pts',(-25.1829211564315,-74.7666138888157,
-216.323526964491));
#219093=CARTESIAN_POINT('Ctrl Pts',(-25.0584884038483,-75.667492051274,
-215.069507359353));
#219094=CARTESIAN_POINT('Ctrl Pts',(-24.8832331864634,-75.6984545252065,
-213.530658916364));
#219095=CARTESIAN_POINT('Ctrl Pts',(-24.7112938709068,-74.7641811379905,
-216.400031379012));
#219096=CARTESIAN_POINT('Ctrl Pts',(-24.5649041979751,-75.677656913773,
-215.143052185656));
#219097=CARTESIAN_POINT('Ctrl Pts',(-24.3623518852465,-75.7092984574834,
-213.595842802549));
#219098=CARTESIAN_POINT('Ctrl Pts',(-24.5540530570477,-74.7633303755955,
-216.426816063351));
#219099=CARTESIAN_POINT('Ctrl Pts',(-24.4003337914636,-75.6809842523408,
-215.168937491766));
#219100=CARTESIAN_POINT('Ctrl Pts',(-24.1887266067715,-75.7128451348644,
-213.619031941073));
#219101=CARTESIAN_POINT('Ctrl Pts',(-24.3771247109268,-74.7623270196362,
-216.458383475085));
#219102=CARTESIAN_POINT('Ctrl Pts',(-24.2152221662776,-75.6846576265878,
-215.199574868406));
#219103=CARTESIAN_POINT('Ctrl Pts',(-23.993400190719,-75.7167589553957,
-213.646748365346));
#219104=CARTESIAN_POINT('Ctrl Pts',(-24.3524265920656,-74.7640480279028,
-216.460210032117));
#219105=CARTESIAN_POINT('Ctrl Pts',(-24.1918224422937,-75.685150167527,
-215.201759610203));
#219106=CARTESIAN_POINT('Ctrl Pts',(-23.971697273502,-75.7171928640745,
-213.64984499144));
#219107=CARTESIAN_POINT('Ctrl Pts',(-24.3044381111283,-74.7669661611978,
-216.464262972695));
#219108=CARTESIAN_POINT('Ctrl Pts',(-24.145811351019,-75.686111198423,-215.206400261357));
#219109=CARTESIAN_POINT('Ctrl Pts',(-23.9282912658856,-75.7180607732476,
-213.655957300462));
#219110=CARTESIAN_POINT('Ctrl Pts',(-24.2804399390943,-74.768422067462,
-216.466265094574));
#219111=CARTESIAN_POINT('Ctrl Pts',(-24.122804155314,-75.6865914263234,
-215.208696671395));
#219112=CARTESIAN_POINT('Ctrl Pts',(-23.9065882035168,-75.7184945038463,
-213.65898840561));
#219113=CARTESIAN_POINT('Ctrl Pts',(-24.2084335919611,-74.7727802747408,
-216.472197988386));
#219114=CARTESIAN_POINT('Ctrl Pts',(-24.0537812020154,-75.6880311791424,
-215.215513350447));
#219115=CARTESIAN_POINT('Ctrl Pts',(-23.8414788399347,-75.7197950312437,
-213.668006138953));
#219116=CARTESIAN_POINT('Ctrl Pts',(-24.1604135896905,-74.7756730640264,
-216.476055288949));
#219117=CARTESIAN_POINT('Ctrl Pts',(-24.007756858606,-75.6889899241308,
-215.21996181218));
#219118=CARTESIAN_POINT('Ctrl Pts',(-23.7980723622357,-75.7206611636291,
-213.673917185906));
#219119=CARTESIAN_POINT('Ctrl Pts',(-24.0163059872845,-74.7843131366596,
-216.487329869079));
#219120=CARTESIAN_POINT('Ctrl Pts',(-23.8696780681879,-75.6918624958728,
-215.233013550851));
#219121=CARTESIAN_POINT('Ctrl Pts',(-23.6678522169305,-75.7232569640359,
-213.691344507444));
#219122=CARTESIAN_POINT('Ctrl Pts',(-23.9201708060206,-74.790022125549,
-216.494449836486));
#219123=CARTESIAN_POINT('Ctrl Pts',(-23.7775889862671,-75.693773263006,
-215.24132615917));
#219124=CARTESIAN_POINT('Ctrl Pts',(-23.5810378370742,-75.7249840351277,
-213.702554973155));
#219125=CARTESIAN_POINT('Ctrl Pts',(-23.0543761384816,-74.8409373246843,
-216.55487821878));
#219126=CARTESIAN_POINT('Ctrl Pts',(-22.9496972317124,-75.7109072613411,
-215.31244750849));
#219127=CARTESIAN_POINT('Ctrl Pts',(-22.7996997171921,-75.7404979925406,
-213.799694500261));
#219128=CARTESIAN_POINT('Ctrl Pts',(-22.2802129953757,-74.8830149514975,
-216.582469365009));
#219129=CARTESIAN_POINT('Ctrl Pts',(-22.2105077358072,-75.7258946484434,
-215.350200325304));
#219130=CARTESIAN_POINT('Ctrl Pts',(-22.1051150671109,-75.7540771354417,
-213.859339381341));
#219131=CARTESIAN_POINT('Ctrl Pts',(-19.9480374324794,-74.9971174078387,
-216.573710635787));
#219132=CARTESIAN_POINT('Ctrl Pts',(-19.9923615170938,-75.7701462160935,
-215.372355885965));
#219133=CARTESIAN_POINT('Ctrl Pts',(-20.0211481644292,-75.7944435076961,
-213.943127994586));
#219134=CARTESIAN_POINT('Ctrl Pts',(-18.3784534462325,-75.0569932128216,
-216.444004457652));
#219135=CARTESIAN_POINT('Ctrl Pts',(-18.5026050448183,-75.7989293347893,
-215.264664590274));
#219136=CARTESIAN_POINT('Ctrl Pts',(-18.6315506331755,-75.820882116255,
-213.870845873572));
#219137=CARTESIAN_POINT('Ctrl Pts',(-16.4159929405093,-75.1060693071363,
-216.099784138263));
#219138=CARTESIAN_POINT('Ctrl Pts',(-16.6428565698784,-75.8341980922607,
-214.945032036074));
#219139=CARTESIAN_POINT('Ctrl Pts',(-16.8941304191336,-75.8539663905531,
-213.584247821028));
#219140=CARTESIAN_POINT('Ctrl Pts',(-16.0234311669877,-75.1146217816123,
-216.021999801869));
#219141=CARTESIAN_POINT('Ctrl Pts',(-16.2709049660166,-75.8412164523101,
-214.872036381481));
#219142=CARTESIAN_POINT('Ctrl Pts',(-16.5465119853673,-75.8605843548391,
-213.517253116689));
#219143=CARTESIAN_POINT('Ctrl Pts',(-15.5821111183439,-75.1228293554344,
-215.924370829589));
#219144=CARTESIAN_POINT('Ctrl Pts',(-15.8527737534803,-75.8490693606545,
-214.779617569726));
#219145=CARTESIAN_POINT('Ctrl Pts',(-16.1557115150513,-75.8680259655566,
-213.430908966255));
#219146=CARTESIAN_POINT('Ctrl Pts',(-15.5330836643943,-75.1237216024415,
-215.913383521458));
#219147=CARTESIAN_POINT('Ctrl Pts',(-15.80632185682,-75.8499412604403,-214.76920653716));
#219148=CARTESIAN_POINT('Ctrl Pts',(-16.1122963714596,-75.8688526965665,
-213.421163614009));
#219149=CARTESIAN_POINT('Ctrl Pts',(-15.4595543784234,-75.1250304693475,
-215.89669284964));
#219150=CARTESIAN_POINT('Ctrl Pts',(-15.7366548093111,-75.8512481475662,
-214.753376392039));
#219151=CARTESIAN_POINT('Ctrl Pts',(-16.0471843630155,-75.8700926288146,
-213.406318025322));
#219152=CARTESIAN_POINT('Ctrl Pts',(-15.4428346873128,-75.1249802811429,
-215.893460636911));
#219153=CARTESIAN_POINT('Ctrl Pts',(-15.717616990686,-75.8515973969198,
-214.749400339868));
#219154=CARTESIAN_POINT('Ctrl Pts',(-16.0254808327191,-75.8705054473464,
-213.40135933222));
#219155=CARTESIAN_POINT('Ctrl Pts',(-15.4044488780932,-75.1251858633582,
-215.885607154577));
#219156=CARTESIAN_POINT('Ctrl Pts',(-15.6768826779187,-75.8523475797937,
-214.740718555761));
#219157=CARTESIAN_POINT('Ctrl Pts',(-15.9820686541031,-75.8713279510056,
-213.391549918843));
#219158=CARTESIAN_POINT('Ctrl Pts',(-15.3852505461376,-75.125287706196,
-215.881710069587));
#219159=CARTESIAN_POINT('Ctrl Pts',(-15.6565119316422,-75.8527215830931,
-214.736409774352));
#219160=CARTESIAN_POINT('Ctrl Pts',(-15.9603609089925,-75.8717379561663,
-213.386680086228));
#219161=CARTESIAN_POINT('Ctrl Pts',(-15.2892320910633,-75.1257922165004,
-215.862372207289));
#219162=CARTESIAN_POINT('Ctrl Pts',(-15.554636473512,-75.8545862406554,
-214.71502472581));
#219163=CARTESIAN_POINT('Ctrl Pts',(-15.8518139508743,-75.8737817636487,
-213.362504307539));
#219164=CARTESIAN_POINT('Ctrl Pts',(-15.2123315921028,-75.1261807769495,
-215.84737406594));
#219165=CARTESIAN_POINT('Ctrl Pts',(-15.4730825113387,-75.8560605251818,
-214.698428383582));
#219166=CARTESIAN_POINT('Ctrl Pts',(-15.7649500436515,-75.8753969121213,
-213.343718445522));
#219167=CARTESIAN_POINT('Ctrl Pts',(-14.9813854912302,-75.1273026315548,
-215.803769736317));
#219168=CARTESIAN_POINT('Ctrl Pts',(-15.228245061749,-75.8604317832489,
-214.650138423064));
#219169=CARTESIAN_POINT('Ctrl Pts',(-15.5042810069002,-75.8801832140909,
-213.288988999601));
#219170=CARTESIAN_POINT('Ctrl Pts',(-14.8270954714867,-75.1279921494453,
-215.776553069533));
#219171=CARTESIAN_POINT('Ctrl Pts',(-15.0648116368335,-75.8632766913161,
-214.619948856185));
#219172=CARTESIAN_POINT('Ctrl Pts',(-15.3303985992444,-75.8832952367866,
-213.254672773818));
#219173=CARTESIAN_POINT('Ctrl Pts',(-14.0541706789573,-75.1311620007791,
-215.649419407507));
#219174=CARTESIAN_POINT('Ctrl Pts',(-14.246396511414,-75.8771638537659,
-214.478590791259));
#219175=CARTESIAN_POINT('Ctrl Pts',(-14.4604916971159,-75.8984676315696,
-213.093510431314));
#219176=CARTESIAN_POINT('Ctrl Pts',(-13.431184632244,-75.132817249281,-215.576219198929));
#219177=CARTESIAN_POINT('Ctrl Pts',(-13.5887407903827,-75.8871770758808,
-214.396239991641));
#219178=CARTESIAN_POINT('Ctrl Pts',(-13.7629914808672,-75.909367896352,
-212.997732926983));
#219179=CARTESIAN_POINT('Ctrl Pts',(-11.5527066094476,-75.1354056675812,
-215.433716025809));
#219180=CARTESIAN_POINT('Ctrl Pts',(-11.6081515883783,-75.914047646435,
-214.231144849336));
#219181=CARTESIAN_POINT('Ctrl Pts',(-11.6663094461884,-75.9385232689356,
-212.798366319057));
#219182=CARTESIAN_POINT('Ctrl Pts',(-10.2877799376859,-75.1340135603591,
-215.440539106394));
#219183=CARTESIAN_POINT('Ctrl Pts',(-10.2793458601892,-75.927717636071,
-214.229655494057));
#219184=CARTESIAN_POINT('Ctrl Pts',(-10.2630041028497,-75.9532535042689,
-212.78151870618));
#219185=CARTESIAN_POINT('Ctrl Pts',(-8.38347923240153,-75.126649730628,
-215.593193327535));
#219186=CARTESIAN_POINT('Ctrl Pts',(-8.28003450179184,-75.941922781162,
-214.376965965048));
#219187=CARTESIAN_POINT('Ctrl Pts',(-8.15049526818619,-75.9684568916159,
-212.91497169383));
#219188=CARTESIAN_POINT('Ctrl Pts',(-7.74635347447534,-75.1232850699231,
-215.668279738107));
#219189=CARTESIAN_POINT('Ctrl Pts',(-7.61095052122154,-75.9456083422809,
-214.451585639128));
#219190=CARTESIAN_POINT('Ctrl Pts',(-7.44371915288171,-75.9723750977203,
-212.986447448666));
#219191=CARTESIAN_POINT('Ctrl Pts',(-6.7941630494427,-75.1167245643831,
-215.8171218942));
#219192=CARTESIAN_POINT('Ctrl Pts',(-6.61073165231177,-75.949511555175,
-214.601581194446));
#219193=CARTESIAN_POINT('Ctrl Pts',(-6.38618665189478,-75.9764782937961,
-213.134044386266));
#219194=CARTESIAN_POINT('Ctrl Pts',(-6.47794571480321,-75.1142884671426,
-215.872668348987));
#219195=CARTESIAN_POINT('Ctrl Pts',(-6.27842297660572,-75.9505402725157,
-214.657841670266));
#219196=CARTESIAN_POINT('Ctrl Pts',(-6.03476907566787,-75.97754871877,-213.189871250874));
#219197=CARTESIAN_POINT('Ctrl Pts',(-6.00556655574115,-75.1102319614325,
-215.964906904596));
#219198=CARTESIAN_POINT('Ctrl Pts',(-5.78184694432798,-75.9516786620228,
-214.751620845591));
#219199=CARTESIAN_POINT('Ctrl Pts',(-5.50928664215075,-75.978712818264,
-213.283577816478));
#219200=CARTESIAN_POINT('Ctrl Pts',(-5.84843151319126,-75.1088126744791,
-215.997140440631));
#219201=CARTESIAN_POINT('Ctrl Pts',(-5.61661283811424,-75.9519906782163,
-214.784451666501));
#219202=CARTESIAN_POINT('Ctrl Pts',(-5.33440000717681,-75.9790272405617,
-213.316475520459));
#219203=CARTESIAN_POINT('Ctrl Pts',(-5.65243869966684,-75.1069512163146,
-216.039300200532));
#219204=CARTESIAN_POINT('Ctrl Pts',(-5.4104807172672,-75.9522966621249,
-214.827456690397));
#219205=CARTESIAN_POINT('Ctrl Pts',(-5.1161362621178,-75.9793285596488,
-213.359686451246));
#219206=CARTESIAN_POINT('Ctrl Pts',(-5.61326165750729,-75.1065745592821,
-216.04782548518));
#219207=CARTESIAN_POINT('Ctrl Pts',(-5.36927136766082,-75.9523536622172,
-214.836156753581));
#219208=CARTESIAN_POINT('Ctrl Pts',(-5.07250098499984,-75.9793842386791,
-213.368433019225));
#219209=CARTESIAN_POINT('Ctrl Pts',(-5.55450205387992,-75.1060026905412,
-216.060759634097));
#219210=CARTESIAN_POINT('Ctrl Pts',(-5.30746024813262,-75.9524328958794,
-214.849360730742));
#219211=CARTESIAN_POINT('Ctrl Pts',(-5.00704455769206,-75.979460913428,
-213.381715900943));
#219212=CARTESIAN_POINT('Ctrl Pts',(-5.53491761156424,-75.1058109307596,
-216.065095153168));
#219213=CARTESIAN_POINT('Ctrl Pts',(-5.28685781194929,-75.9524582612829,
-214.85378754548));
#219214=CARTESIAN_POINT('Ctrl Pts',(-4.9852263867816,-75.9794853292611,
-213.386170460015));
#219215=CARTESIAN_POINT('Ctrl Pts',(-5.50554413451951,-75.1055215751752,
-216.071634702396));
#219216=CARTESIAN_POINT('Ctrl Pts',(-5.2559566454412,-75.952494739044,-214.860465953734));
#219217=CARTESIAN_POINT('Ctrl Pts',(-4.95250008958594,-75.9795202381749,
-213.392892775367));
#219218=CARTESIAN_POINT('Ctrl Pts',(-5.49575350661914,-75.1054248373341,
-216.073820597239));
#219219=CARTESIAN_POINT('Ctrl Pts',(-5.24565657882127,-75.9525066366783,
-214.862698474386));
#219220=CARTESIAN_POINT('Ctrl Pts',(-4.94159148370997,-75.9795315886736,
-213.395140293282));
#219221=CARTESIAN_POINT('Ctrl Pts',(-5.47617332109849,-75.1052307878912,
-216.078204488416));
#219222=CARTESIAN_POINT('Ctrl Pts',(-5.22505721795924,-75.9525299083859,
-214.867176270342));
#219223=CARTESIAN_POINT('Ctrl Pts',(-4.91977459201134,-75.9795537178522,
-213.399648834811));
#219224=CARTESIAN_POINT('Ctrl Pts',(-5.46775998763707,-75.1049040600624,
-216.080458414741));
#219225=CARTESIAN_POINT('Ctrl Pts',(-5.21551613357834,-75.9525365950561,
-214.869490968336));
#219226=CARTESIAN_POINT('Ctrl Pts',(-4.90886637668479,-75.979564444277,
-213.401912833547));
#219227=CARTESIAN_POINT('Ctrl Pts',(-5.35883349107929,-75.1074979249758,
-216.099458947456));
#219228=CARTESIAN_POINT('Ctrl Pts',(-5.11136656618359,-75.9527073582981,
-214.888713509689));
#219229=CARTESIAN_POINT('Ctrl Pts',(-4.81069244996574,-75.9796594680882,
-213.422289301941));
#219230=CARTESIAN_POINT('Ctrl Pts',(-5.26196254924258,-75.109746081089,
-216.115929091618));
#219231=CARTESIAN_POINT('Ctrl Pts',(-5.01875445567398,-75.9528546760428,
-214.905377832462));
#219232=CARTESIAN_POINT('Ctrl Pts',(-4.72341604058447,-75.9797411532712,
-213.43995044954));
#219233=CARTESIAN_POINT('Ctrl Pts',(-4.38966212112596,-75.129464412617,
-216.260333501036));
#219234=CARTESIAN_POINT('Ctrl Pts',(-4.1856409578542,-75.9541400040838,
-215.05137059809));
#219235=CARTESIAN_POINT('Ctrl Pts',(-3.93783085851934,-75.9804521342285,
-213.594787559664));
#219236=CARTESIAN_POINT('Ctrl Pts',(-3.61066071653182,-75.143382837027,
-216.361345807815));
#219237=CARTESIAN_POINT('Ctrl Pts',(-3.44231755118432,-75.9550058719466,
-215.153647449945));
#219238=CARTESIAN_POINT('Ctrl Pts',(-3.2388370683562,-75.9809140489,-213.703064133886));
#219239=CARTESIAN_POINT('Ctrl Pts',(-2.43793380877736,-75.158324347106,
-216.467698922128));
#219240=CARTESIAN_POINT('Ctrl Pts',(-2.32497867688892,-75.9559405053742,
-215.261362555356));
#219241=CARTESIAN_POINT('Ctrl Pts',(-2.18920489796754,-75.9814176712845,
-213.817320721562));
#219242=CARTESIAN_POINT('Ctrl Pts',(-2.04653708635396,-75.1623004098586,
-216.495634771282));
#219243=CARTESIAN_POINT('Ctrl Pts',(-1.95228850104495,-75.956191020554,
-215.289675834488));
#219244=CARTESIAN_POINT('Ctrl Pts',(-1.83913744423942,-75.9815538586382,
-213.847387631165));
#219245=CARTESIAN_POINT('Ctrl Pts',(-1.26261892289813,-75.1682023804309,
-216.536118946838));
#219246=CARTESIAN_POINT('Ctrl Pts',(-1.20625878776482,-75.956574549768,
-215.330747400307));
#219247=CARTESIAN_POINT('Ctrl Pts',(-1.13861344723909,-75.9817683431745,
-213.891105902662));
#219248=CARTESIAN_POINT('Ctrl Pts',(-0.870690610263053,-75.1700713359302,
-216.548458769496));
#219249=CARTESIAN_POINT('Ctrl Pts',(-0.8331611987563,-75.9567099274067,
-215.34331728403));
#219250=CARTESIAN_POINT('Ctrl Pts',(-0.788152053854913,-75.9818502107287,
-213.904552602819));
#219251=CARTESIAN_POINT('Ctrl Pts',(-0.0946346290956796,-75.1716828999797,
-216.55940101613));
#219252=CARTESIAN_POINT('Ctrl Pts',(-0.0911222846775505,-75.9568355718726,
-215.354479378076));
#219253=CARTESIAN_POINT('Ctrl Pts',(-0.0868749634279395,-75.9819292803481,
-213.916498075924));
#219254=CARTESIAN_POINT('Ctrl Pts',(0.289821995872756,-75.1715354727665,
-216.558387830722));
#219255=CARTESIAN_POINT('Ctrl Pts',(0.278068638204925,-75.956821763788,
-215.353439573327));
#219256=CARTESIAN_POINT('Ctrl Pts',(0.263931643533207,-75.9819197939239,
-213.91538037431));
#219257=CARTESIAN_POINT('Ctrl Pts',(1.06864077654397,-75.1692292709605,
-216.542760365914));
#219258=CARTESIAN_POINT('Ctrl Pts',(1.0219251337563,-75.9566479467771,-215.337513737709));
#219259=CARTESIAN_POINT('Ctrl Pts',(0.965895527519129,-75.9818124764925,
-213.898350217505));
#219260=CARTESIAN_POINT('Ctrl Pts',(1.46241230485478,-75.1669596440325,
-216.527770436365));
#219261=CARTESIAN_POINT('Ctrl Pts',(1.39635237112926,-75.9564918800891,
-215.322268188682));
#219262=CARTESIAN_POINT('Ctrl Pts',(1.31706165436456,-75.9817211615821,
-213.882064332672));
#219263=CARTESIAN_POINT('Ctrl Pts',(2.64158476672795,-75.157028128614,-216.458935843592));
#219264=CARTESIAN_POINT('Ctrl Pts',(2.518920939202,-75.9558541077429,-215.25245869547));
#219265=CARTESIAN_POINT('Ctrl Pts',(2.37116135636138,-75.9813684091457,
-213.807836336228));
#219266=CARTESIAN_POINT('Ctrl Pts',(3.42746352318773,-75.1462601427746,
-216.381942172347));
#219267=CARTESIAN_POINT('Ctrl Pts',(3.26785428161275,-75.9551914419494,
-215.174452709293));
#219268=CARTESIAN_POINT('Ctrl Pts',(3.07468059463055,-75.9810166072727,
-213.725184571819));
#219269=CARTESIAN_POINT('Ctrl Pts',(4.60404126994595,-75.1242840669289,
-216.222415136132));
#219270=CARTESIAN_POINT('Ctrl Pts',(4.39015023062561,-75.9537982622651,
-215.013097647576));
#219271=CARTESIAN_POINT('Ctrl Pts',(4.13107556051587,-75.9802608955334,
-213.554116576666));
#219272=CARTESIAN_POINT('Ctrl Pts',(4.99546403484811,-75.1160271457934,
-216.161939532443));
#219273=CARTESIAN_POINT('Ctrl Pts',(4.76410117541733,-75.9532672027339,
-214.951901043922));
#219274=CARTESIAN_POINT('Ctrl Pts',(4.48326091718761,-75.9799705283094,
-213.489291039963));
#219275=CARTESIAN_POINT('Ctrl Pts',(5.41027241482983,-75.1062699534614,
-216.09046397724));
#219276=CARTESIAN_POINT('Ctrl Pts',(5.16054567878141,-75.9526264884405,
-214.879614360294));
#219277=CARTESIAN_POINT('Ctrl Pts',(4.85705526974492,-75.9796144475554,
-213.412642866388));
#219278=CARTESIAN_POINT('Ctrl Pts',(5.4346695038882,-75.1056923633818,-216.086232887577));
#219279=CARTESIAN_POINT('Ctrl Pts',(5.18387402798683,-75.952588500194,-214.875333406559));
#219280=CARTESIAN_POINT('Ctrl Pts',(4.87904219608802,-75.9795933268261,
-213.408105477469));
#219281=CARTESIAN_POINT('Ctrl Pts',(5.4712601362539,-75.1048205145248,-216.079846427648));
#219282=CARTESIAN_POINT('Ctrl Pts',(5.21886319527768,-75.9525310919893,
-214.868871767276));
#219283=CARTESIAN_POINT('Ctrl Pts',(4.91202112514165,-75.9795613813585,
-213.40125652354));
#219284=CARTESIAN_POINT('Ctrl Pts',(5.4790807817468,-75.1052596530533,-216.077552452273));
#219285=CARTESIAN_POINT('Ctrl Pts',(5.22811604565769,-75.9525264981582,
-214.866510233269));
#219286=CARTESIAN_POINT('Ctrl Pts',(4.92301425681121,-75.9795504814768,
-213.398978166736));
#219287=CARTESIAN_POINT('Ctrl Pts',(5.49881361376608,-75.1054550956631,
-216.073136911307));
#219288=CARTESIAN_POINT('Ctrl Pts',(5.24887592608961,-75.9525029380811,
-214.862000190262));
#219289=CARTESIAN_POINT('Ctrl Pts',(4.94500105373396,-75.9795280629415,
-213.394437292551));
#219290=CARTESIAN_POINT('Ctrl Pts',(5.5086806337521,-75.1055525263003,-216.070935271933));
#219291=CARTESIAN_POINT('Ctrl Pts',(5.25925632234409,-75.9524908921101,
-214.859751631201));
#219292=CARTESIAN_POINT('Ctrl Pts',(4.95599468254889,-75.9795165632374,
-213.392173699146));
#219293=CARTESIAN_POINT('Ctrl Pts',(5.55801873311596,-75.1060382306792,
-216.05995770291));
#219294=CARTESIAN_POINT('Ctrl Pts',(5.31115963401093,-75.9524293340583,
-214.848541320831));
#219295=CARTESIAN_POINT('Ctrl Pts',(5.01096397729203,-75.9794576130073,
-213.380889917595));
#219296=CARTESIAN_POINT('Ctrl Pts',(5.59749880870147,-75.1064221580628,
-216.051273655991));
#219297=CARTESIAN_POINT('Ctrl Pts',(5.35269029216777,-75.9523758332619,
-214.839676206352));
#219298=CARTESIAN_POINT('Ctrl Pts',(5.05494309510992,-75.9794058073811,
-213.371972284299));
#219299=CARTESIAN_POINT('Ctrl Pts',(5.7159670297233,-75.1075602019096,-216.025514511917));
#219300=CARTESIAN_POINT('Ctrl Pts',(5.47730056979923,-75.9522025875599,
-214.813390278519));
#219301=CARTESIAN_POINT('Ctrl Pts',(5.18689145327219,-75.9792364716388,
-213.345546335821));
#219302=CARTESIAN_POINT('Ctrl Pts',(5.79498316352783,-75.1083005814153,
-216.008732396227));
#219303=CARTESIAN_POINT('Ctrl Pts',(5.56040450116008,-75.9520700938053,
-214.796277534812));
#219304=CARTESIAN_POINT('Ctrl Pts',(5.27487169751627,-75.9791050230153,
-213.328364951587));
#219305=CARTESIAN_POINT('Ctrl Pts',(6.03213727287012,-75.1104680783436,
-215.959550347728));
#219306=CARTESIAN_POINT('Ctrl Pts',(5.80978587963131,-75.9516217475982,
-214.746168419211));
#219307=CARTESIAN_POINT('Ctrl Pts',(5.53885614015153,-75.9786551294951,
-213.278119496813));
#219308=CARTESIAN_POINT('Ctrl Pts',(6.1903809047475,-75.1118415742934,-215.928314470138));
#219309=CARTESIAN_POINT('Ctrl Pts',(5.97615687411766,-75.9512550103054,
-214.71439558984));
#219310=CARTESIAN_POINT('Ctrl Pts',(5.71490403776887,-75.9782811424582,
-213.246353807529));
#219311=CARTESIAN_POINT('Ctrl Pts',(6.98222284448457,-75.1183676778219,
-215.779809027149));
#219312=CARTESIAN_POINT('Ctrl Pts',(6.80827192600329,-75.9490838436669,
-214.563656651227));
#219313=CARTESIAN_POINT('Ctrl Pts',(6.59543144166356,-75.9760422697398,
-213.096080563456));
#219314=CARTESIAN_POINT('Ctrl Pts',(7.61766362532376,-75.1225044545407,
-215.685484989009));
#219315=CARTESIAN_POINT('Ctrl Pts',(7.47572460167024,-75.9462668204644,
-214.468784151763));
#219316=CARTESIAN_POINT('Ctrl Pts',(7.30077147419061,-75.9730722423746,
-213.003143500855));
#219317=CARTESIAN_POINT('Ctrl Pts',(9.52720981831856,-75.1321158303546,
-215.474464687372));
#219318=CARTESIAN_POINT('Ctrl Pts',(9.48054159649718,-75.9345906696201,
-214.260062974152));
#219319=CARTESIAN_POINT('Ctrl Pts',(9.4194934943534,-75.960636334928,-212.804632346833));
#219320=CARTESIAN_POINT('Ctrl Pts',(10.8047815872151,-75.1348247966243,
-215.428648443105));
#219321=CARTESIAN_POINT('Ctrl Pts',(10.8218971913187,-75.9225254849928,
-214.220488336749));
#219322=CARTESIAN_POINT('Ctrl Pts',(10.8355301758809,-75.9476698821379,
-212.777963649677));
#219323=CARTESIAN_POINT('Ctrl Pts',(12.7172077249894,-75.1340707842268,
-215.513470836751));
#219324=CARTESIAN_POINT('Ctrl Pts',(12.8359348263178,-75.8977553183569,
-214.324390406467));
#219325=CARTESIAN_POINT('Ctrl Pts',(12.9654496957873,-75.9208595381148,
-212.912174558945));
#219326=CARTESIAN_POINT('Ctrl Pts',(13.3539693845637,-75.1330093149386,
-215.567557023935));
#219327=CARTESIAN_POINT('Ctrl Pts',(13.5071520281508,-75.8883911745511,
-214.386405940268));
#219328=CARTESIAN_POINT('Ctrl Pts',(13.6764103124011,-75.9106906578871,
-212.986243267424));
#219329=CARTESIAN_POINT('Ctrl Pts',(14.3064153442316,-75.1300979705268,
-215.691855458681));
#219330=CARTESIAN_POINT('Ctrl Pts',(14.5136752922168,-75.8725932457468,
-214.525772201742));
#219331=CARTESIAN_POINT('Ctrl Pts',(14.7445314576483,-75.8934744325803,
-213.147223427492));
#219332=CARTESIAN_POINT('Ctrl Pts',(14.623689531781,-75.1289051437049,-215.740556702165));
#219333=CARTESIAN_POINT('Ctrl Pts',(14.8492851726867,-75.8670321534769,
-214.580010009994));
#219334=CARTESIAN_POINT('Ctrl Pts',(15.1011378555104,-75.8874026004125,
-213.209291022116));
#219335=CARTESIAN_POINT('Ctrl Pts',(15.0973358826677,-75.1267587770309,
-215.825039956629));
#219336=CARTESIAN_POINT('Ctrl Pts',(15.3511219071714,-75.8582618484975,
-214.673710136175));
#219337=CARTESIAN_POINT('Ctrl Pts',(15.6350705546162,-75.8778081087278,
-213.315738009231));
#219338=CARTESIAN_POINT('Ctrl Pts',(15.2548567752318,-75.125983673237,-215.855107341301));
#219339=CARTESIAN_POINT('Ctrl Pts',(15.5181282247503,-75.8552673104085,
-214.706995901577));
#219340=CARTESIAN_POINT('Ctrl Pts',(15.8129038281666,-75.8745286185941,
-213.353446581077));
#219341=CARTESIAN_POINT('Ctrl Pts',(15.4218002487273,-75.1250930170855,
-215.889154542325));
#219342=CARTESIAN_POINT('Ctrl Pts',(15.6952956461322,-75.8520085747563,
-214.744640182935));
#219343=CARTESIAN_POINT('Ctrl Pts',(16.0016916963461,-75.8709562729166,
-213.395980975865));
#219344=CARTESIAN_POINT('Ctrl Pts',(15.4316188990632,-75.1250403784937,
-215.891165045285));
#219345=CARTESIAN_POINT('Ctrl Pts',(15.7057151340514,-75.8518166215729,
-214.746862695126));
#219346=CARTESIAN_POINT('Ctrl Pts',(16.0127962765676,-75.8707458117443,
-213.398492081262));
#219347=CARTESIAN_POINT('Ctrl Pts',(15.4512530718343,-75.1249346051803,
-215.895201541308));
#219348=CARTESIAN_POINT('Ctrl Pts',(15.7265519313712,-75.8514321507501,
-214.75132449253));
#219349=CARTESIAN_POINT('Ctrl Pts',(16.0350042567052,-75.8703242422743,
-213.403532508095));
#219350=CARTESIAN_POINT('Ctrl Pts',(15.459740253059,-75.1249637297094,-215.896828454245));
#219351=CARTESIAN_POINT('Ctrl Pts',(15.7362557047496,-75.8512542699721,
-214.753340594192));
#219352=CARTESIAN_POINT('Ctrl Pts',(16.0461076394828,-75.8701131295941,
-213.406062095362));
#219353=CARTESIAN_POINT('Ctrl Pts',(15.4820248334799,-75.1246924436737,
-215.901694128387));
#219354=CARTESIAN_POINT('Ctrl Pts',(15.7585152623914,-75.8508393951058,
-214.758282360298));
#219355=CARTESIAN_POINT('Ctrl Pts',(16.0683132899191,-75.8696902738925,
-213.411138474507));
#219356=CARTESIAN_POINT('Ctrl Pts',(15.4959535248115,-75.1243825850165,
-215.904955531531));
#219357=CARTESIAN_POINT('Ctrl Pts',(15.7711420877953,-75.8506012003567,
-214.761213105418));
#219358=CARTESIAN_POINT('Ctrl Pts',(16.0794167111148,-75.86947882605,-213.413667362903));
#219359=CARTESIAN_POINT('Ctrl Pts',(15.521032584694,-75.123932842705,-215.910624249774));
#219360=CARTESIAN_POINT('Ctrl Pts',(15.7949037776395,-75.8501553676149,
-214.766587894379));
#219361=CARTESIAN_POINT('Ctrl Pts',(16.101624858776,-75.8690559192528,-213.418704779072));
#219362=CARTESIAN_POINT('Ctrl Pts',(15.5335728237211,-75.1237066808223,
-215.913449505672));
#219363=CARTESIAN_POINT('Ctrl Pts',(15.8067852660439,-75.8499324059612,
-214.769266012297));
#219364=CARTESIAN_POINT('Ctrl Pts',(16.1127295663156,-75.8688444554581,
-213.421213600409));
#219365=CARTESIAN_POINT('Ctrl Pts',(15.596277579428,-75.1225694141948,-215.927530278499));
#219366=CARTESIAN_POINT('Ctrl Pts',(15.866195871248,-75.8488173718676,-214.78261021411));
#219367=CARTESIAN_POINT('Ctrl Pts',(16.1682562721183,-75.8677870840726,
-213.433708281287));
#219368=CARTESIAN_POINT('Ctrl Pts',(15.6464527782837,-75.1216389380232,
-215.93864927566));
#219369=CARTESIAN_POINT('Ctrl Pts',(15.9137348084119,-75.8479246157398,
-214.793137208678));
#219370=CARTESIAN_POINT('Ctrl Pts',(16.2126877745262,-75.8669410192569,
-213.443545863115));
#219371=CARTESIAN_POINT('Ctrl Pts',(15.7970131172075,-75.1187853774811,
-215.971569760114));
#219372=CARTESIAN_POINT('Ctrl Pts',(16.0563828683782,-75.8452441451922,
-214.824273352458));
#219373=CARTESIAN_POINT('Ctrl Pts',(16.3460126749685,-75.8644023051579,
-213.472584430655));
#219374=CARTESIAN_POINT('Ctrl Pts',(15.8974330079295,-75.1168001636331,
-215.992934742601));
#219375=CARTESIAN_POINT('Ctrl Pts',(16.1515241770282,-75.8434542111259,
-214.844437852363));
#219376=CARTESIAN_POINT('Ctrl Pts',(16.4349364663841,-75.8627091362929,
-213.491311234129));
#219377=CARTESIAN_POINT('Ctrl Pts',(17.6053820959646,-75.0816362045942,
-216.346260837099));
#219378=CARTESIAN_POINT('Ctrl Pts',(17.7698966769832,-75.8129696618018,
-215.177219033293));
#219379=CARTESIAN_POINT('Ctrl Pts',(17.9473288709126,-75.8339127266394,
-213.798933624518));
#219380=CARTESIAN_POINT('Ctrl Pts',(19.2277908337019,-75.0263499924907,
-216.527622591312));
#219381=CARTESIAN_POINT('Ctrl Pts',(19.3086934863095,-75.7834585100956,
-215.336116175665));
#219382=CARTESIAN_POINT('Ctrl Pts',(19.3813247221325,-75.8066729690042,
-213.923601542428));
#219383=CARTESIAN_POINT('Ctrl Pts',(21.6558359806902,-74.9150494601847,
-216.590897359445));
#219384=CARTESIAN_POINT('Ctrl Pts',(21.6153500443125,-75.7378479315545,
-215.366882072238));
#219385=CARTESIAN_POINT('Ctrl Pts',(21.5462509158658,-75.7649417071187,
-213.893044878855));
#219386=CARTESIAN_POINT('Ctrl Pts',(22.4648784248499,-74.8731903210939,
-216.578042999207));
#219387=CARTESIAN_POINT('Ctrl Pts',(22.3867384863216,-75.7223537446655,
-215.343224536461));
#219388=CARTESIAN_POINT('Ctrl Pts',(22.2701738627727,-75.7508758505917,
-213.84723891686));
#219389=CARTESIAN_POINT('Ctrl Pts',(23.4728708240175,-74.816161830225,-216.524453677946));
#219390=CARTESIAN_POINT('Ctrl Pts',(23.3494355632829,-75.7026196357405,
-215.276919328278));
#219391=CARTESIAN_POINT('Ctrl Pts',(23.177540032039,-75.732985743614,-213.751482920168));
#219392=CARTESIAN_POINT('Ctrl Pts',(23.6743655621636,-74.8045134968797,
-216.511872971906));
#219393=CARTESIAN_POINT('Ctrl Pts',(23.5422576362207,-75.6986468679756,
-215.261803887036));
#219394=CARTESIAN_POINT('Ctrl Pts',(23.3591731636709,-75.7293914716431,
-213.730409932309));
#219395=CARTESIAN_POINT('Ctrl Pts',(23.9762017683036,-74.7867010048439,
-216.490346610853));
#219396=CARTESIAN_POINT('Ctrl Pts',(23.8312594277273,-75.6926601948462,
-215.236527096512));
#219397=CARTESIAN_POINT('Ctrl Pts',(23.6316298755007,-75.7239779322202,
-213.696069266785));
#219398=CARTESIAN_POINT('Ctrl Pts',(24.0767465863703,-74.7807068465897,
-216.48272879554));
#219399=CARTESIAN_POINT('Ctrl Pts',(23.9275870343842,-75.690659379697,-215.227664419223));
#219400=CARTESIAN_POINT('Ctrl Pts',(23.7224502835782,-75.7221697265246,
-213.684167363404));
#219401=CARTESIAN_POINT('Ctrl Pts',(24.2274640600537,-74.7716317815129,
-216.470654320984));
#219402=CARTESIAN_POINT('Ctrl Pts',(24.0720224749929,-75.687650992375,-215.213735619942));
#219403=CARTESIAN_POINT('Ctrl Pts',(23.858683087999,-75.7194515985814,-213.665648035631));
#219404=CARTESIAN_POINT('Ctrl Pts',(24.2776865884637,-74.7685927882663,
-216.466521534823));
#219405=CARTESIAN_POINT('Ctrl Pts',(24.1201662478945,-75.6866468359805,
-215.208986051363));
#219406=CARTESIAN_POINT('Ctrl Pts',(23.9040943881952,-75.7185445860867,
-213.659363844575));
#219407=CARTESIAN_POINT('Ctrl Pts',(24.3529955852829,-74.7640134807405,
-216.460162360007));
#219408=CARTESIAN_POINT('Ctrl Pts',(24.1923680699484,-75.6851387760389,
-215.201704952376));
#219409=CARTESIAN_POINT('Ctrl Pts',(23.9722118786887,-75.7171825779668,
-213.649772915152));
#219410=CARTESIAN_POINT('Ctrl Pts',(24.3784994717427,-74.7623348648064,
-216.458136672852));
#219411=CARTESIAN_POINT('Ctrl Pts',(24.2166607054916,-75.6846291537297,
-215.199335161605));
#219412=CARTESIAN_POINT('Ctrl Pts',(23.9949178673861,-75.7167286261278,
-213.64653127887));
#219413=CARTESIAN_POINT('Ctrl Pts',(24.4196337599662,-74.7625680326348,
-216.450800742114));
#219414=CARTESIAN_POINT('Ctrl Pts',(24.259705887401,-75.6837748047058,-215.192214283183));
#219415=CARTESIAN_POINT('Ctrl Pts',(24.0403296350762,-75.7158185240332,
-213.640091106598));
#219416=CARTESIAN_POINT('Ctrl Pts',(24.4402002771278,-74.762683912951,-216.447154613061));
#219417=CARTESIAN_POINT('Ctrl Pts',(24.2812282571141,-75.6833465808423,
-215.188677021339));
#219418=CARTESIAN_POINT('Ctrl Pts',(24.0630354011898,-75.715362317608,-213.636895804635));
#219419=CARTESIAN_POINT('Ctrl Pts',(24.7898203708446,-74.764641964529,-216.385541888145));
#219420=CARTESIAN_POINT('Ctrl Pts',(24.6469467821791,-75.6760520799882,
-215.128963778829));
#219421=CARTESIAN_POINT('Ctrl Pts',(24.4490314221452,-75.7075871592492,
-213.582997463384));
#219422=CARTESIAN_POINT('Ctrl Pts',(25.1187116623081,-74.7663052298968,
-216.333145267762));
#219423=CARTESIAN_POINT('Ctrl Pts',(24.9912410172876,-75.6689153385714,
-215.078669907208));
#219424=CARTESIAN_POINT('Ctrl Pts',(24.812291644422,-75.6999735317664,-213.538617767255));
#219425=CARTESIAN_POINT('Ctrl Pts',(26.7622290318585,-74.7737857064687,
-216.099514369437));
#219426=CARTESIAN_POINT('Ctrl Pts',(26.7099624617689,-75.6319318195073,
-214.857743429527));
#219427=CARTESIAN_POINT('Ctrl Pts',(26.6284393652984,-75.6604150064864,
-213.3491278222));
#219428=CARTESIAN_POINT('Ctrl Pts',(28.075080877613,-74.7769924622541,-216.001871476478));
#219429=CARTESIAN_POINT('Ctrl Pts',(28.0859463587902,-75.5980221249252,
-214.775154563847));
#219430=CARTESIAN_POINT('Ctrl Pts',(28.0808759169087,-75.6240391544431,
-213.29892337729));
#219431=CARTESIAN_POINT('Ctrl Pts',(30.0270254090569,-74.7816141294705,
-216.00764859601));
#219432=CARTESIAN_POINT('Ctrl Pts',(30.1441281348009,-75.5404095409703,
-214.819104347431));
#219433=CARTESIAN_POINT('Ctrl Pts',(30.2586772078354,-75.5618154664653,
-213.408748577776));
#219434=CARTESIAN_POINT('Ctrl Pts',(30.6746003481513,-74.783131073334,-216.03519912743));
#219435=CARTESIAN_POINT('Ctrl Pts',(30.8278988046784,-75.5201201036592,
-214.861853605089));
#219436=CARTESIAN_POINT('Ctrl Pts',(30.9844671541994,-75.5397907755024,
-213.476605004965));
#219437=CARTESIAN_POINT('Ctrl Pts',(31.9599958800107,-74.7861720113306,
-216.151048029206));
#219438=CARTESIAN_POINT('Ctrl Pts',(32.1907307647438,-75.477181336842,-215.015719242188));
#219439=CARTESIAN_POINT('Ctrl Pts',(32.435703007658,-75.4929295570714,-213.689014761762));
#219440=CARTESIAN_POINT('Ctrl Pts',(32.6006286165977,-74.7878210783825,
-216.24000664944));
#219441=CARTESIAN_POINT('Ctrl Pts',(32.872988366941,-75.4544140916729,-215.127572191219));
#219442=CARTESIAN_POINT('Ctrl Pts',(33.1649378192402,-75.46794300932,-213.834823319187));
#219443=CARTESIAN_POINT('Ctrl Pts',(33.2168085208362,-74.7890149970872,
-216.36473842254));
#219444=CARTESIAN_POINT('Ctrl Pts',(33.5343686210915,-75.4309604638016,
-215.280488076331));
#219445=CARTESIAN_POINT('Ctrl Pts',(33.8749380667978,-75.4420407256794,
-214.026523605855));
#219446=CARTESIAN_POINT('',(24.3802580872756,-74.7628322230906,-216.457148834596));
#219447=CARTESIAN_POINT('',(15.4710515403103,-75.1252154310809,-215.898655568186));
#219448=CARTESIAN_POINT('Ctrl Pts',(24.3802580872756,-74.7628322230906,
-216.457148834596));
#219449=CARTESIAN_POINT('Ctrl Pts',(23.6057867097546,-74.8100705737294,
-216.52370992462));
#219450=CARTESIAN_POINT('Ctrl Pts',(22.8447074397333,-74.8532777187265,
-216.562969013006));
#219451=CARTESIAN_POINT('Ctrl Pts',(21.7246656382609,-74.9110314666933,
-216.58090464313));
#219452=CARTESIAN_POINT('Ctrl Pts',(21.3548976004719,-74.9291197144322,
-216.580057686095));
#219453=CARTESIAN_POINT('Ctrl Pts',(20.805828082717,-74.9545797369581,-216.568548999929));
#219454=CARTESIAN_POINT('Ctrl Pts',(20.5326875016302,-74.9668922756974,
-216.560235094192));
#219455=CARTESIAN_POINT('Ctrl Pts',(20.2164959770152,-74.9805477557225,
-216.546056302856));
#219456=CARTESIAN_POINT('Ctrl Pts',(20.0815178427006,-74.9862507373229,
-216.539019842002));
#219457=CARTESIAN_POINT('Ctrl Pts',(19.9916510399144,-74.9900198259762,
-216.534115571212));
#219458=CARTESIAN_POINT('Ctrl Pts',(19.9487412234712,-74.9918067539723,
-216.531673616063));
#219459=CARTESIAN_POINT('Ctrl Pts',(18.4050368468729,-75.0555944587559,
-216.439859003958));
#219460=CARTESIAN_POINT('Ctrl Pts',(16.9264817129947,-75.0994115785442,
-216.229780408324));
#219461=CARTESIAN_POINT('Ctrl Pts',(15.4710515403103,-75.1252154310809,
-215.898655568186));
#219462=CARTESIAN_POINT('',(32.8638454863375,-74.7886392304488,-216.296979356602));
#219463=CARTESIAN_POINT('Ctrl Pts',(32.863845486296,-74.788639230448,-216.296979356596));
#219464=CARTESIAN_POINT('Ctrl Pts',(32.2178333387358,-74.7872541619425,
-216.181772728121));
#219465=CARTESIAN_POINT('Ctrl Pts',(31.5389214686617,-74.7860747654139,
-216.100629599085));
#219466=CARTESIAN_POINT('Ctrl Pts',(30.4747208094706,-74.7835574505676,
-216.030010154687));
#219467=CARTESIAN_POINT('Ctrl Pts',(30.1123332242519,-74.7826192987842,
-216.014986214748));
#219468=CARTESIAN_POINT('Ctrl Pts',(29.5576378729449,-74.7811432549687,
-216.005224117128));
#219469=CARTESIAN_POINT('Ctrl Pts',(29.2775116904412,-74.7803894360587,
-216.00353652139));
#219470=CARTESIAN_POINT('Ctrl Pts',(28.9459188512441,-74.7795141404412,
-216.007156202572));
#219471=CARTESIAN_POINT('Ctrl Pts',(28.7789380649846,-74.7790835460274,
-216.010363178883));
#219472=CARTESIAN_POINT('Ctrl Pts',(28.6951526914092,-74.7788711619761,
-216.012315950968));
#219473=CARTESIAN_POINT('Ctrl Pts',(28.6591815979652,-74.7787808680542,
-216.013227699846));
#219474=CARTESIAN_POINT('Ctrl Pts',(28.6351868666064,-74.7787208463327,
-216.013852165));
#219475=CARTESIAN_POINT('Ctrl Pts',(28.6219205756486,-74.7786877885733,
-216.014207264721));
#219476=CARTESIAN_POINT('Ctrl Pts',(27.2352432404576,-74.7752439591572,
-216.052173807495));
#219477=CARTESIAN_POINT('Ctrl Pts',(25.8185917312215,-74.7709950882897,
-216.199722892692));
#219478=CARTESIAN_POINT('Ctrl Pts',(24.3802580872756,-74.7628322230906,
-216.457148834596));
#219479=CARTESIAN_POINT('',(33.3513892243221,-75.4608554610386,-213.894117162909));
#219480=CARTESIAN_POINT('Ctrl Pts',(32.863845486296,-74.788639230448,-216.296979356596));
#219481=CARTESIAN_POINT('Ctrl Pts',(32.9410850039213,-74.999970347199,-215.939487466059));
#219482=CARTESIAN_POINT('Ctrl Pts',(33.0236138935975,-75.1681413467096,
-215.548509757113));
#219483=CARTESIAN_POINT('Ctrl Pts',(33.1895226861483,-75.3962354831127,
-214.734437839155));
#219484=CARTESIAN_POINT('Ctrl Pts',(33.2727909348202,-75.4560174753842,
-214.311772816012));
#219485=CARTESIAN_POINT('Ctrl Pts',(33.3513899426336,-75.4608558287546,
-213.894117302352));
#219486=CARTESIAN_POINT('Ctrl Pts',(-33.3513928247577,-75.4608558931301,
-213.894101966659));
#219487=CARTESIAN_POINT('Ctrl Pts',(-32.8873496662889,-75.4772841921233,
-213.784425468418));
#219488=CARTESIAN_POINT('Ctrl Pts',(-32.4201892950423,-75.4931733089948,
-213.693836888586));
#219489=CARTESIAN_POINT('Ctrl Pts',(-31.9507721192534,-75.5085355661565,
-213.619497087055));
#219490=CARTESIAN_POINT('Ctrl Pts',(-31.9075027906416,-75.5099516084055,
-213.612644689088));
#219491=CARTESIAN_POINT('Ctrl Pts',(-31.8642143022296,-75.5113631741533,
-213.605930383152));
#219492=CARTESIAN_POINT('Ctrl Pts',(-31.8209073365556,-75.5127702730643,
-213.599351966943));
#219493=CARTESIAN_POINT('Ctrl Pts',(-31.657104814835,-75.51809242728,-213.574470030579));
#219494=CARTESIAN_POINT('Ctrl Pts',(-31.4929112225694,-75.5233541895962,
-213.551532319841));
#219495=CARTESIAN_POINT('Ctrl Pts',(-31.3284605632087,-75.5285525767555,
-213.530477412274));
#219496=CARTESIAN_POINT('Ctrl Pts',(-30.9340514163604,-75.5410200940794,
-213.479980514525));
#219497=CARTESIAN_POINT('Ctrl Pts',(-30.5375718139143,-75.5531426206814,
-213.440194218096));
#219498=CARTESIAN_POINT('Ctrl Pts',(-30.1405091673275,-75.5648865535421,
-213.410317899452));
#219499=CARTESIAN_POINT('Ctrl Pts',(-30.0093310829785,-75.5687664113645,
-213.400447622606));
#219500=CARTESIAN_POINT('Ctrl Pts',(-29.8780892162955,-75.5726049379618,
-213.391659383122));
#219501=CARTESIAN_POINT('Ctrl Pts',(-29.7468368704954,-75.5764008912256,
-213.383925473857));
#219502=CARTESIAN_POINT('Ctrl Pts',(-29.5908035364721,-75.5809135362373,
-213.37473137039));
#219503=CARTESIAN_POINT('Ctrl Pts',(-29.4348076545751,-75.5853653973002,
-213.366996066073));
#219504=CARTESIAN_POINT('Ctrl Pts',(-29.2788373795595,-75.5897573793404,
-213.360688865401));
#219505=CARTESIAN_POINT('Ctrl Pts',(-28.587495913932,-75.6092249304514,
-213.332732068141));
#219506=CARTESIAN_POINT('Ctrl Pts',(-27.8963404060334,-75.6275309381467,
-213.332477866803));
#219507=CARTESIAN_POINT('Ctrl Pts',(-27.2053257342637,-75.6447219136339,
-213.35739210847));
#219508=CARTESIAN_POINT('Ctrl Pts',(-26.6627179145517,-75.6582208422514,
-213.376955603868));
#219509=CARTESIAN_POINT('Ctrl Pts',(-26.120198033493,-75.6710321930194,
-213.412038537932));
#219510=CARTESIAN_POINT('Ctrl Pts',(-25.5777648626619,-75.683177813424,
-213.461422194978));
#219511=CARTESIAN_POINT('Ctrl Pts',(-25.4434846238148,-75.6861844820729,
-213.473647201891));
#219512=CARTESIAN_POINT('Ctrl Pts',(-25.3092057560598,-75.689150084866,
-213.48676925098));
#219513=CARTESIAN_POINT('Ctrl Pts',(-25.1749285663624,-75.692074732042,
-213.50078176889));
#219514=CARTESIAN_POINT('Ctrl Pts',(-24.9619426474422,-75.6967137080862,
-213.523007949004));
#219515=CARTESIAN_POINT('Ctrl Pts',(-24.7489594890241,-75.7012498838473,
-213.547462664372));
#219516=CARTESIAN_POINT('Ctrl Pts',(-24.5359790241656,-75.7056838071389,
-213.574115147839));
#219517=CARTESIAN_POINT('Ctrl Pts',(-24.4070995903422,-75.7083668772684,
-213.590243185599));
#219518=CARTESIAN_POINT('Ctrl Pts',(-24.2782211440055,-75.7110124995285,
-213.607176310471));
#219519=CARTESIAN_POINT('Ctrl Pts',(-24.1493436789706,-75.713620770764,
-213.62490909452));
#219520=CARTESIAN_POINT('Ctrl Pts',(-24.1045967081316,-75.714526377007,
-213.631066015519));
#219521=CARTESIAN_POINT('Ctrl Pts',(-24.0598498586817,-75.7154274806628,
-213.637319324643));
#219522=CARTESIAN_POINT('Ctrl Pts',(-24.0151031302881,-75.7163240858007,
-213.643668793969));
#219523=CARTESIAN_POINT('Ctrl Pts',(-23.9934001948624,-75.7167589547645,
-213.646748396159));
#219524=CARTESIAN_POINT('Ctrl Pts',(-23.9716972776745,-75.7171928634372,
-213.649845022571));
#219525=CARTESIAN_POINT('Ctrl Pts',(-23.9499942742991,-75.7176268179877,
-213.652901178597));
#219526=CARTESIAN_POINT('Ctrl Pts',(-23.9282912704726,-75.7180607725472,
-213.655957334687));
#219527=CARTESIAN_POINT('Ctrl Pts',(-23.9065882084806,-75.7184945030891,
-213.658988442607));
#219528=CARTESIAN_POINT('Ctrl Pts',(-23.8848850880541,-75.7189280121292,
-213.661994358033));
#219529=CARTESIAN_POINT('Ctrl Pts',(-23.8414788461836,-75.7197950302298,
-213.668006189026));
#219530=CARTESIAN_POINT('Ctrl Pts',(-23.7980723705685,-75.7206611623083,
-213.673917250899));
#219531=CARTESIAN_POINT('Ctrl Pts',(-23.7546656590397,-75.7215264286156,
-213.679726381899));
#219532=CARTESIAN_POINT('Ctrl Pts',(-23.6678522342647,-75.7232569612644,
-213.691344644129));
#219533=CARTESIAN_POINT('Ctrl Pts',(-23.581037865851,-75.7249840306461,
-213.702555193327));
#219534=CARTESIAN_POINT('Ctrl Pts',(-23.4942225353474,-75.7267078008841,
-213.713348614776));
#219535=CARTESIAN_POINT('Ctrl Pts',(-23.3707348340602,-75.7291597229468,
-213.72870137328));
#219536=CARTESIAN_POINT('Ctrl Pts',(-23.2472451863123,-75.7316049709933,
-213.743210120025));
#219537=CARTESIAN_POINT('Ctrl Pts',(-23.1237535338497,-75.7340440351597,
-213.75684673174));
#219538=CARTESIAN_POINT('Ctrl Pts',(-22.5526996859888,-75.7453228297144,
-213.819905565566));
#219539=CARTESIAN_POINT('Ctrl Pts',(-21.9816053178851,-75.7564694844777,
-213.864306970363));
#219540=CARTESIAN_POINT('Ctrl Pts',(-21.4104614756218,-75.7675316609456,
-213.88731993422));
#219541=CARTESIAN_POINT('Ctrl Pts',(-21.2977418163553,-75.7697148671187,
-213.891861720812));
#219542=CARTESIAN_POINT('Ctrl Pts',(-21.1850201592615,-75.7718949319907,
-213.895561976977));
#219543=CARTESIAN_POINT('Ctrl Pts',(-21.0722963627658,-75.7740721183519,
-213.898405686423));
#219544=CARTESIAN_POINT('Ctrl Pts',(-20.3101280724893,-75.7887929001041,
-213.917633083245));
#219545=CARTESIAN_POINT('Ctrl Pts',(-19.5478296370527,-75.8033869760415,
-213.897455950411));
#219546=CARTESIAN_POINT('Ctrl Pts',(-18.7854746599048,-75.8179333033253,
-213.833237968256));
#219547=CARTESIAN_POINT('Ctrl Pts',(-18.2708779812001,-75.8277522091264,
-213.789890234823));
#219548=CARTESIAN_POINT('Ctrl Pts',(-17.7562545676338,-75.8375493971014,
-213.72647578556));
#219549=CARTESIAN_POINT('Ctrl Pts',(-17.241613757919,-75.8473494730384,
-213.641571672275));
#219550=CARTESIAN_POINT('Ctrl Pts',(-17.1504453664671,-75.8490855521491,
-213.626530946219));
#219551=CARTESIAN_POINT('Ctrl Pts',(-17.059268607012,-75.8508216747552,
-213.610825285784));
#219552=CARTESIAN_POINT('Ctrl Pts',(-16.96809027621,-75.8525577589421,-213.594453482362));
#219553=CARTESIAN_POINT('Ctrl Pts',(-16.7970429357528,-75.8558145917923,
-213.563740555186));
#219554=CARTESIAN_POINT('Ctrl Pts',(-16.6259904766021,-75.8590713549408,
-213.530679591711));
#219555=CARTESIAN_POINT('Ctrl Pts',(-16.4549329472469,-75.8623283920597,
-213.495250367538));
#219556=CARTESIAN_POINT('Ctrl Pts',(-16.3696536621392,-75.8639521603797,
-213.477587427353));
#219557=CARTESIAN_POINT('Ctrl Pts',(-16.2843852368415,-75.865575760016,
-213.459338620813));
#219558=CARTESIAN_POINT('Ctrl Pts',(-16.1991337604474,-75.8671991180785,
-213.440502891606));
#219559=CARTESIAN_POINT('Ctrl Pts',(-16.1557108260507,-75.8680259773147,
-213.430908891968));
#219560=CARTESIAN_POINT('Ctrl Pts',(-16.1122956661453,-75.868852709237,
-213.421163496792));
#219561=CARTESIAN_POINT('Ctrl Pts',(-16.0688883605895,-75.8696793177453,
-213.411266577736));
#219562=CARTESIAN_POINT('Ctrl Pts',(-16.0471841769452,-75.8700926321087,
-213.40631799717));
#219563=CARTESIAN_POINT('Ctrl Pts',(-16.0254806449976,-75.8705054507595,
-213.401359298027));
#219564=CARTESIAN_POINT('Ctrl Pts',(-16.0037747424049,-75.8709166991138,
-213.396454629959));
#219565=CARTESIAN_POINT('Ctrl Pts',(-15.9831651900046,-75.871307175597,
-213.391797693296));
#219566=CARTESIAN_POINT('Ctrl Pts',(-15.9625543147019,-75.8716965249299,
-213.387172236819));
#219567=CARTESIAN_POINT('Ctrl Pts',(-15.9419421324393,-75.8720847496106,
-213.382578090849));
#219568=CARTESIAN_POINT('Ctrl Pts',(-15.9408452649187,-75.8721054088032,
-213.382333615547));
#219569=CARTESIAN_POINT('Ctrl Pts',(-15.9397483932213,-75.87212606482,-213.382089228799));
#219570=CARTESIAN_POINT('Ctrl Pts',(-15.9386515173484,-75.8721467176615,
-213.381844930582));
#219571=CARTESIAN_POINT('Ctrl Pts',(-15.851813756867,-75.8737817672998,
-213.362504264434));
#219572=CARTESIAN_POINT('Ctrl Pts',(-15.7649498283845,-75.8753969160326,
-213.343718402895));
#219573=CARTESIAN_POINT('Ctrl Pts',(-15.6780603215635,-75.8769923431775,
-213.325475501279));
#219574=CARTESIAN_POINT('Ctrl Pts',(-15.5042797865617,-75.8801832254017,
-213.288989378631));
#219575=CARTESIAN_POINT('Ctrl Pts',(-15.3303969644586,-75.883295232643,
-213.25467435116));
#219576=CARTESIAN_POINT('Ctrl Pts',(-15.1564162069293,-75.8863296353476,
-213.222445734065));
#219577=CARTESIAN_POINT('Ctrl Pts',(-15.0759336740236,-75.8877333331991,
-213.207536954653));
#219578=CARTESIAN_POINT('Ctrl Pts',(-14.9954303042051,-75.8891204649254,
-213.193072142904));
#219579=CARTESIAN_POINT('Ctrl Pts',(-14.9149064146963,-75.8904911137141,
-213.179045535909));
#219580=CARTESIAN_POINT('Ctrl Pts',(-14.2991321754372,-75.9009726021306,
-213.071782668898));
#219581=CARTESIAN_POINT('Ctrl Pts',(-13.6821528490865,-75.9104918796616,
-212.990053078907));
#219582=CARTESIAN_POINT('Ctrl Pts',(-13.0640933699476,-75.9190856566173,
-212.931320199254));
#219583=CARTESIAN_POINT('Ctrl Pts',(-12.9941535614473,-75.9200581311684,
-212.924673967792));
#219584=CARTESIAN_POINT('Ctrl Pts',(-12.9242001019972,-75.9210188053301,
-212.918319156356));
#219585=CARTESIAN_POINT('Ctrl Pts',(-12.8542330789119,-75.9219676899831,
-212.912254648701));
#219586=CARTESIAN_POINT('Ctrl Pts',(-12.103744918449,-75.932145723381,-212.847204843899));
#219587=CARTESIAN_POINT('Ctrl Pts',(-11.3516069380129,-75.9409718595207,
-212.815352430239));
#219588=CARTESIAN_POINT('Ctrl Pts',(-10.5980291929577,-75.9484605685429,
-212.815191307246));
#219589=CARTESIAN_POINT('Ctrl Pts',(-10.0177252773204,-75.9542273619457,
-212.815067232053));
#219590=CARTESIAN_POINT('Ctrl Pts',(-9.43656819308798,-75.9592010864688,
-212.833735208245));
#219591=CARTESIAN_POINT('Ctrl Pts',(-8.85466502499123,-75.9633890545989,
-212.870489657771));
#219592=CARTESIAN_POINT('Ctrl Pts',(-8.80621265809307,-75.9637377672018,
-212.873550029619));
#219593=CARTESIAN_POINT('Ctrl Pts',(-8.7577487416815,-75.9640810280511,
-212.876738332401));
#219594=CARTESIAN_POINT('Ctrl Pts',(-8.70927474202254,-75.9644188262203,
-212.880054548429));
#219595=CARTESIAN_POINT('Ctrl Pts',(-8.16802284443195,-75.9681906193745,
-212.917082815758));
#219596=CARTESIAN_POINT('Ctrl Pts',(-7.62521966310781,-75.9712836556175,
-212.970057781598));
#219597=CARTESIAN_POINT('Ctrl Pts',(-7.08306476118715,-75.9736810365594,
-213.038940050712));
#219598=CARTESIAN_POINT('Ctrl Pts',(-6.96823963948708,-75.9741887873101,
-213.053528897748));
#219599=CARTESIAN_POINT('Ctrl Pts',(-6.85344360943193,-75.9746653412367,
-213.06883110778));
#219600=CARTESIAN_POINT('Ctrl Pts',(-6.73869756970069,-75.9751105507597,
-213.084846007434));
#219601=CARTESIAN_POINT('Ctrl Pts',(-6.70123227716741,-75.9752559144258,
-213.090074971343));
#219602=CARTESIAN_POINT('Ctrl Pts',(-6.66377970851828,-75.9753979183016,
-213.095378751942));
#219603=CARTESIAN_POINT('Ctrl Pts',(-6.62633993925021,-75.9755365658722,
-213.10075735341));
#219604=CARTESIAN_POINT('Ctrl Pts',(-6.31150977816634,-75.9767024501139,
-213.145985889793));
#219605=CARTESIAN_POINT('Ctrl Pts',(-5.99754483591358,-75.9776311781919,
-213.196509446686));
#219606=CARTESIAN_POINT('Ctrl Pts',(-5.68444746635923,-75.9783247837595,
-213.252342367387));
#219607=CARTESIAN_POINT('Ctrl Pts',(-5.65269333611006,-75.9783951287822,
-213.258004905653));
#219608=CARTESIAN_POINT('Ctrl Pts',(-5.62094813600815,-75.9784630546653,
-213.263722092798));
#219609=CARTESIAN_POINT('Ctrl Pts',(-5.5892118753693,-75.9785285627877,
-213.269493984429));
#219610=CARTESIAN_POINT('Ctrl Pts',(-5.4458894272464,-75.9788244005545,
-213.295560118943));
#219611=CARTESIAN_POINT('Ctrl Pts',(-5.30273879712366,-75.9790709489129,
-213.322743719392));
#219612=CARTESIAN_POINT('Ctrl Pts',(-5.15978901555836,-75.9792682954213,
-213.351044287356));
#219613=CARTESIAN_POINT('Ctrl Pts',(-5.13085816823248,-75.9793082353333,
-213.35677188905));
#219614=CARTESIAN_POINT('Ctrl Pts',(-5.1019356538566,-75.9793461604998,
-213.362545209928));
#219615=CARTESIAN_POINT('Ctrl Pts',(-5.07301593827139,-75.9793820774016,
-213.368365449668));
#219616=CARTESIAN_POINT('Ctrl Pts',(-5.05829718990994,-75.9794003573822,
-213.37132767258));
#219617=CARTESIAN_POINT('Ctrl Pts',(-5.04358000194555,-75.9794181161351,
-213.374301880288));
#219618=CARTESIAN_POINT('Ctrl Pts',(-5.02886336884999,-75.9794353549927,
-213.377288283786));
#219619=CARTESIAN_POINT('Ctrl Pts',(-5.00704302178793,-75.9794609150413,
-213.381716223271));
#219620=CARTESIAN_POINT('Ctrl Pts',(-4.98522511827338,-75.9794853303841,
-213.386170733756));
#219621=CARTESIAN_POINT('Ctrl Pts',(-4.96340885953034,-75.9795086014944,
-213.390652023996));
#219622=CARTESIAN_POINT('Ctrl Pts',(-4.9524998768548,-75.9795202379597,
-213.392892844394));
#219623=CARTESIAN_POINT('Ctrl Pts',(-4.94159130543411,-75.979531588317,
-213.39514036091));
#219624=CARTESIAN_POINT('Ctrl Pts',(-4.93068304543216,-75.9795426525913,
-213.397394600517));
#219625=CARTESIAN_POINT('Ctrl Pts',(-4.91977448336048,-75.9795537171721,
-213.399648902548));
#219626=CARTESIAN_POINT('Ctrl Pts',(-4.9088663032563,-75.9795644433992,
-213.401912903139));
#219627=CARTESIAN_POINT('Ctrl Pts',(-4.89795817571377,-75.9795750013207,
-213.404176948458));
#219628=CARTESIAN_POINT('Ctrl Pts',(-4.8107062930038,-75.9796594519766,
-213.422286584224));
#219629=CARTESIAN_POINT('Ctrl Pts',(-4.72344700942351,-75.9797411185036,
-213.439944730912));
#219630=CARTESIAN_POINT('Ctrl Pts',(-4.63612898071532,-75.9798201342666,
-213.457155494977));
#219631=CARTESIAN_POINT('Ctrl Pts',(-4.60996385918782,-75.9798438115881,
-213.462312754481));
#219632=CARTESIAN_POINT('Ctrl Pts',(-4.5837934588528,-75.9798672535015,
-213.467429677896));
#219633=CARTESIAN_POINT('Ctrl Pts',(-4.5576163974065,-75.9798904631868,
-213.472506347965));
#219634=CARTESIAN_POINT('Ctrl Pts',(-4.07663947765109,-75.9803169175844,
-213.565785004833));
#219635=CARTESIAN_POINT('Ctrl Pts',(-3.59417252100192,-75.9806646032663,
-213.645311443452));
#219636=CARTESIAN_POINT('Ctrl Pts',(-3.11009598855904,-75.9809468066053,
-213.709986409894));
#219637=CARTESIAN_POINT('Ctrl Pts',(-2.92000878015336,-75.9810576222332,
-213.735382980479));
#219638=CARTESIAN_POINT('Ctrl Pts',(-2.72967334665686,-75.9811583442642,
-213.758488932177));
#219639=CARTESIAN_POINT('Ctrl Pts',(-2.53908232066754,-75.9812497918801,
-213.77923549017));
#219640=CARTESIAN_POINT('Ctrl Pts',(-2.52097369221552,-75.981258480594,
-213.781206683244));
#219641=CARTESIAN_POINT('Ctrl Pts',(-2.50286275684531,-75.9812670852011,
-213.783156596776));
#219642=CARTESIAN_POINT('Ctrl Pts',(-2.4847495087102,-75.9812756060268,
-213.785085192613));
#219643=CARTESIAN_POINT('Ctrl Pts',(-2.15358059177547,-75.9814313943545,
-213.820346178928));
#219644=CARTESIAN_POINT('Ctrl Pts',(-1.82162137854988,-75.9815590179761,
-213.848492418773));
#219645=CARTESIAN_POINT('Ctrl Pts',(-1.48887673016169,-75.9816607414808,
-213.86926725327));
#219646=CARTESIAN_POINT('Ctrl Pts',(-1.13928261377975,-75.9817676160432,
-213.891094080371));
#219647=CARTESIAN_POINT('Ctrl Pts',(-0.788816617423684,-75.9818494936408,
-213.90457805642));
#219648=CARTESIAN_POINT('Ctrl Pts',(-0.437513953977255,-75.9818892910274,
-213.91055136394));
#219649=CARTESIAN_POINT('Ctrl Pts',(-0.422238919642044,-75.9818910214625,
-213.910811090059));
#219650=CARTESIAN_POINT('Ctrl Pts',(-0.406962321199802,-75.9818926595883,
-213.911057348003));
#219651=CARTESIAN_POINT('Ctrl Pts',(-0.391684159219294,-75.9818942057822,
-213.911290104531));
#219652=CARTESIAN_POINT('Ctrl Pts',(-0.106400275277922,-75.9819230773301,
-213.915636287441));
#219653=CARTESIAN_POINT('Ctrl Pts',(0.179082832830468,-75.9819195513841,
-213.915281542));
#219654=CARTESIAN_POINT('Ctrl Pts',(0.464388804013359,-75.98188633428,-213.910069992462));
#219655=CARTESIAN_POINT('Ctrl Pts',(0.514569929607294,-75.9818804918797,
-213.909153357522));
#219656=CARTESIAN_POINT('Ctrl Pts',(0.564745571523509,-75.9818737317438,
-213.908086604403));
#219657=CARTESIAN_POINT('Ctrl Pts',(0.614913677116972,-75.9818660695581,
-213.906869053894));
#219658=CARTESIAN_POINT('Ctrl Pts',(0.883836747769246,-75.981824996879,
-213.90034244864));
#219659=CARTESIAN_POINT('Ctrl Pts',(1.15254856945707,-75.9817618231612,
-213.889259482589));
#219660=CARTESIAN_POINT('Ctrl Pts',(1.42073621839167,-75.9816819480231,
-213.873375461236));
#219661=CARTESIAN_POINT('Ctrl Pts',(1.50335308767494,-75.9816573419912,
-213.868482289903));
#219662=CARTESIAN_POINT('Ctrl Pts',(1.58592020389488,-75.9816311515161,
-213.86313387284));
#219663=CARTESIAN_POINT('Ctrl Pts',(1.66842839174222,-75.9816035352139,
-213.857324070858));
#219664=CARTESIAN_POINT('Ctrl Pts',(1.68217044445011,-75.9815989356136,
-213.856356426227));
#219665=CARTESIAN_POINT('Ctrl Pts',(1.69591085645726,-75.9815942920412,
-213.855376236483));
#219666=CARTESIAN_POINT('Ctrl Pts',(1.70964958405473,-75.9815896042878,
-213.854383528651));
#219667=CARTESIAN_POINT('Ctrl Pts',(2.19610545981022,-75.98142362202,-213.819234090393));
#219668=CARTESIAN_POINT('Ctrl Pts',(2.68121874436983,-75.9812020443835,
-213.76833459995));
#219669=CARTESIAN_POINT('Ctrl Pts',(3.16507275796152,-75.9809144082949,
-213.702579531751));
#219670=CARTESIAN_POINT('Ctrl Pts',(3.36992000515139,-75.9807926330087,
-213.674741083932));
#219671=CARTESIAN_POINT('Ctrl Pts',(3.57454157170993,-75.980659021922,-213.644239294627));
#219672=CARTESIAN_POINT('Ctrl Pts',(3.77894390642551,-75.980512799313,-213.611139249122));
#219673=CARTESIAN_POINT('Ctrl Pts',(3.78445653335865,-75.9805088557636,
-213.610246557742));
#219674=CARTESIAN_POINT('Ctrl Pts',(3.78996896840898,-75.9805049029287,
-213.609351987569));
#219675=CARTESIAN_POINT('Ctrl Pts',(3.79548121007169,-75.9805009407858,
-213.608455540887));
#219676=CARTESIAN_POINT('Ctrl Pts',(4.06858712343268,-75.9803046350508,
-213.56404078103));
#219677=CARTESIAN_POINT('Ctrl Pts',(4.34137765120749,-75.9800854014844,
-213.514997391923));
#219678=CARTESIAN_POINT('Ctrl Pts',(4.61403589949818,-75.9798400767937,
-213.461499221038));
#219679=CARTESIAN_POINT('Ctrl Pts',(4.68714478617817,-75.9797742969571,
-213.447154554271));
#219680=CARTESIAN_POINT('Ctrl Pts',(4.76024416353237,-75.979706639818,-213.432489315292));
#219681=CARTESIAN_POINT('Ctrl Pts',(4.83333754839952,-75.9796370409594,
-213.417506229945));
#219682=CARTESIAN_POINT('Ctrl Pts',(4.83391415551471,-75.9796364919194,
-213.417388033837));
#219683=CARTESIAN_POINT('Ctrl Pts',(4.8344907616134,-75.9796359427591,-213.41726981808));
#219684=CARTESIAN_POINT('Ctrl Pts',(4.83506736669369,-75.9796353934785,
-213.417151582676));
#219685=CARTESIAN_POINT('Ctrl Pts',(4.85705527089062,-75.9796144475508,
-213.412642866356));
#219686=CARTESIAN_POINT('Ctrl Pts',(4.87904219752034,-75.979593326817,-213.408105477613));
#219687=CARTESIAN_POINT('Ctrl Pts',(4.90102814896698,-75.9795720298321,
-213.40353950903));
#219688=CARTESIAN_POINT('Ctrl Pts',(4.91202112578867,-75.9795613813386,
-213.40125652451));
#219689=CARTESIAN_POINT('Ctrl Pts',(4.92301425754122,-75.9795504814521,
-213.398978167959));
#219690=CARTESIAN_POINT('Ctrl Pts',(4.93400765560909,-75.9795392721793,
-213.396707731265));
#219691=CARTESIAN_POINT('Ctrl Pts',(4.94500105464879,-75.9795280629055,
-213.39443729437));
#219692=CARTESIAN_POINT('Ctrl Pts',(4.95599468356498,-75.9795165631949,
-213.392173701309));
#219693=CARTESIAN_POINT('Ctrl Pts',(4.96698854204686,-75.9795047731424,
-213.3899169455));
#219694=CARTESIAN_POINT('Ctrl Pts',(5.01096398928681,-75.9794576129176,
-213.38088991953));
#219695=CARTESIAN_POINT('Ctrl Pts',(5.05494310946406,-75.9794058072462,
-213.371972288104));
#219696=CARTESIAN_POINT('Ctrl Pts',(5.09892588297217,-75.9793493619682,
-213.363163643794));
#219697=CARTESIAN_POINT('Ctrl Pts',(5.18689153127894,-75.9792364712821,
-213.345546334888));
#219698=CARTESIAN_POINT('Ctrl Pts',(5.27487179213221,-75.9791050224788,
-213.328364955098));
#219699=CARTESIAN_POINT('Ctrl Pts',(5.36286651682885,-75.9789550580173,
-213.31161649334));
#219700=CARTESIAN_POINT('Ctrl Pts',(5.53216176684228,-75.9786665376417,
-213.279393709186));
#219701=CARTESIAN_POINT('Ctrl Pts',(5.70151054468751,-75.9783094868255,
-213.248773074071));
#219702=CARTESIAN_POINT('Ctrl Pts',(5.8709119085587,-75.9778841486961,-213.219736583428));
#219703=CARTESIAN_POINT('Ctrl Pts',(5.87761103143291,-75.9778673283334,
-213.218588310391));
#219704=CARTESIAN_POINT('Ctrl Pts',(5.88431023694467,-75.9778504011683,
-213.217442515181));
#219705=CARTESIAN_POINT('Ctrl Pts',(5.89100952505437,-75.977833367216,-213.216299196671));
#219706=CARTESIAN_POINT('Ctrl Pts',(6.57648381222072,-75.9760904452671,
-213.099314313008));
#219707=CARTESIAN_POINT('Ctrl Pts',(7.26281953055674,-75.9732311015326,
-213.008169089905));
#219708=CARTESIAN_POINT('Ctrl Pts',(7.95000030915388,-75.9692589748972,
-212.942376327843));
#219709=CARTESIAN_POINT('Ctrl Pts',(7.96900370297949,-75.969149129149,-212.940556885554));
#219710=CARTESIAN_POINT('Ctrl Pts',(7.98800774705063,-75.96903843191,-212.938756857887));
#219711=CARTESIAN_POINT('Ctrl Pts',(8.00701244074232,-75.9689268832679,
-212.936976234005));
#219712=CARTESIAN_POINT('Ctrl Pts',(9.01669616134442,-75.9630005131925,
-212.842375027793));
#219713=CARTESIAN_POINT('Ctrl Pts',(10.0281851201039,-75.954683893227,-212.80183031115));
#219714=CARTESIAN_POINT('Ctrl Pts',(11.0415920643372,-75.9438949943452,
-212.819044947185));
#219715=CARTESIAN_POINT('Ctrl Pts',(11.4021166221425,-75.9400567899391,
-212.825169139525));
#219716=CARTESIAN_POINT('Ctrl Pts',(11.7628843913312,-75.9359056873238,
-212.838603457441));
#219717=CARTESIAN_POINT('Ctrl Pts',(12.1239020500588,-75.9314379745397,
-212.859514796659));
#219718=CARTESIAN_POINT('Ctrl Pts',(12.1677558321591,-75.9308952694997,
-212.862054953051));
#219719=CARTESIAN_POINT('Ctrl Pts',(12.2116133487246,-75.9303478845685,
-212.864705871123));
#219720=CARTESIAN_POINT('Ctrl Pts',(12.2554746014879,-75.9297958135096,
-212.86746783182));
#219721=CARTESIAN_POINT('Ctrl Pts',(12.9091879304763,-75.9215676807724,
-212.90863242261));
#219722=CARTESIAN_POINT('Ctrl Pts',(13.5637374768946,-75.9122941099966,
-212.974714278678));
#219723=CARTESIAN_POINT('Ctrl Pts',(14.2192120561195,-75.9019172187269,
-213.068681012528));
#219724=CARTESIAN_POINT('Ctrl Pts',(14.2756314127241,-75.9010240375913,
-213.076769110578));
#219725=CARTESIAN_POINT('Ctrl Pts',(14.3320574272743,-75.9001226764094,
-213.085064287729));
#219726=CARTESIAN_POINT('Ctrl Pts',(14.3884903026081,-75.8992130957741,
-213.093568472595));
#219727=CARTESIAN_POINT('Ctrl Pts',(14.6818682279193,-75.894484453505,-213.137779229139));
#219728=CARTESIAN_POINT('Ctrl Pts',(14.9756256940205,-75.8895296456064,
-213.187702769479));
#219729=CARTESIAN_POINT('Ctrl Pts',(15.2691013315942,-75.8843532160818,
-213.243611744504));
#219730=CARTESIAN_POINT('Ctrl Pts',(15.3317819141186,-75.8832476332788,
-213.25555279403));
#219731=CARTESIAN_POINT('Ctrl Pts',(15.3944477533609,-75.882131973196,-213.267766562248));
#219732=CARTESIAN_POINT('Ctrl Pts',(15.4570929624156,-75.8810062707486,
-213.280255808989));
#219733=CARTESIAN_POINT('Ctrl Pts',(15.56931266771,-75.8789897398949,-213.302628463016));
#219734=CARTESIAN_POINT('Ctrl Pts',(15.6814735367602,-75.87694090377,-213.325885882819));
#219735=CARTESIAN_POINT('Ctrl Pts',(15.7935782943546,-75.8748593371064,
-213.350053261412));
#219736=CARTESIAN_POINT('Ctrl Pts',(15.8592678329298,-75.8736396105169,
-213.364214515426));
#219737=CARTESIAN_POINT('Ctrl Pts',(15.9249374177143,-75.8724086568486,
-213.378688144354));
#219738=CARTESIAN_POINT('Ctrl Pts',(15.9905865115854,-75.8711664099023,
-213.393479023437));
#219739=CARTESIAN_POINT('Ctrl Pts',(16.0016916798719,-75.8709562720226,
-213.395981041236));
#219740=CARTESIAN_POINT('Ctrl Pts',(16.0127962614987,-75.8707458109113,
-213.39849214194));
#219741=CARTESIAN_POINT('Ctrl Pts',(16.0239002537432,-75.8705350262171,
-213.401012351154));
#219742=CARTESIAN_POINT('Ctrl Pts',(16.0350042443252,-75.8703242415545,
-213.403532559989));
#219743=CARTESIAN_POINT('Ctrl Pts',(16.0461076283636,-75.870113128927,-213.406062143155));
#219744=CARTESIAN_POINT('Ctrl Pts',(16.0572104545953,-75.8699017011283,
-213.408600328877));
#219745=CARTESIAN_POINT('Ctrl Pts',(16.068313281294,-75.8696902733207,-213.411138514705));
#219746=CARTESIAN_POINT('Ctrl Pts',(16.0794167037132,-75.8694788255209,
-213.413667399603));
#219747=CARTESIAN_POINT('Ctrl Pts',(16.0905207773752,-75.8692673721864,
-213.416186104166));
#219748=CARTESIAN_POINT('Ctrl Pts',(16.1016248536337,-75.8690559188024,
-213.418704809319));
#219749=CARTESIAN_POINT('Ctrl Pts',(16.1127295622337,-75.8688444550433,
-213.421213627703));
#219750=CARTESIAN_POINT('Ctrl Pts',(16.1238349020251,-75.868632980843,-213.423712560667));
#219751=CARTESIAN_POINT('Ctrl Pts',(16.1682563297534,-75.8677870827362,
-213.43370830795));
#219752=CARTESIAN_POINT('Ctrl Pts',(16.2126878564162,-75.8669410175819,
-213.44354588758));
#219753=CARTESIAN_POINT('Ctrl Pts',(16.2571294072557,-75.8660947811755,
-213.453225389057));
#219754=CARTESIAN_POINT('Ctrl Pts',(16.2772265474938,-75.8657121002966,
-213.45760260576));
#219755=CARTESIAN_POINT('Ctrl Pts',(16.2973257376673,-75.8653293844006,
-213.461947495525));
#219756=CARTESIAN_POINT('Ctrl Pts',(16.3174269708162,-75.8649466330907,
-213.466260067273));
#219757=CARTESIAN_POINT('Ctrl Pts',(16.3862275772071,-75.8636365879792,
-213.481020731416));
#219758=CARTESIAN_POINT('Ctrl Pts',(16.4550519918267,-75.8623261155969,
-213.495403612882));
#219759=CARTESIAN_POINT('Ctrl Pts',(16.5239002432807,-75.8610151961749,
-213.509409025261));
#219760=CARTESIAN_POINT('Ctrl Pts',(17.2221321564218,-75.8477203665076,
-213.651446414345));
#219761=CARTESIAN_POINT('Ctrl Pts',(17.9228698040644,-75.8343918984152,
-213.753884770493));
#219762=CARTESIAN_POINT('Ctrl Pts',(18.6259929002108,-75.8209788271971,
-213.818960489682));
#219763=CARTESIAN_POINT('Ctrl Pts',(19.2618685562882,-75.8088485963633,
-213.877812297936));
#219764=CARTESIAN_POINT('Ctrl Pts',(19.8996944331453,-75.7966491630361,
-213.906106594897));
#219765=CARTESIAN_POINT('Ctrl Pts',(20.5393478070102,-75.7843436373544,
-213.905482499602));
#219766=CARTESIAN_POINT('Ctrl Pts',(20.6343955077762,-75.7825151283986,
-213.905389763715));
#219767=CARTESIAN_POINT('Ctrl Pts',(20.7294829484021,-75.780684194172,-213.904663931103));
#219768=CARTESIAN_POINT('Ctrl Pts',(20.8246099557498,-75.7788507122291,
-213.903310241351));
#219769=CARTESIAN_POINT('Ctrl Pts',(21.4384220517384,-75.7670200720597,
-213.894575485918));
#219770=CARTESIAN_POINT('Ctrl Pts',(22.0538553854744,-75.7550759076376,
-213.860164387392));
#219771=CARTESIAN_POINT('Ctrl Pts',(22.6707441337976,-75.742964226742,-213.802911549687));
#219772=CARTESIAN_POINT('Ctrl Pts',(22.7791427338394,-75.7408359835915,
-213.792851182282));
#219773=CARTESIAN_POINT('Ctrl Pts',(22.8875828374366,-75.738702595359,-213.782088145393));
#219774=CARTESIAN_POINT('Ctrl Pts',(22.9960671998898,-75.7365636899579,
-213.770637922095));
#219775=CARTESIAN_POINT('Ctrl Pts',(23.1775336789479,-75.7329858505033,
-213.751484638991));
#219776=CARTESIAN_POINT('Ctrl Pts',(23.3591607784853,-75.729391712817,-213.730411774765));
#219777=CARTESIAN_POINT('Ctrl Pts',(23.5408109811078,-75.7257824438295,
-213.707516230951));
#219778=CARTESIAN_POINT('Ctrl Pts',(23.6074556822628,-75.7244582578413,
-213.699116203572));
#219779=CARTESIAN_POINT('Ctrl Pts',(23.6741036716134,-75.7231320329098,
-213.690470919469));
#219780=CARTESIAN_POINT('Ctrl Pts',(23.7407558015218,-75.7218036786003,
-213.681584355796));
#219781=CARTESIAN_POINT('Ctrl Pts',(23.7649272860614,-75.7213219491238,
-213.67836163153));
#219782=CARTESIAN_POINT('Ctrl Pts',(23.7890994558372,-75.7208399367944,
-213.675107155865));
#219783=CARTESIAN_POINT('Ctrl Pts',(23.8132721536629,-75.7203576411583,
-213.671821148346));
#219784=CARTESIAN_POINT('Ctrl Pts',(23.8586819366496,-75.719451621469,-213.665648196968));
#219785=CARTESIAN_POINT('Ctrl Pts',(23.9040935831152,-75.7185446020397,
-213.659363966219));
#219786=CARTESIAN_POINT('Ctrl Pts',(23.9495060511029,-75.7176365802963,
-213.652969909908));
#219787=CARTESIAN_POINT('Ctrl Pts',(23.9722118101336,-75.7171825789216,
-213.649772948628));
#219788=CARTESIAN_POINT('Ctrl Pts',(23.9949178430555,-75.7167286260788,
-213.646531313061));
#219789=CARTESIAN_POINT('Ctrl Pts',(24.0176237567913,-75.716273574272,-213.64331123187));
#219790=CARTESIAN_POINT('Ctrl Pts',(24.040329699698,-75.7158185218806,-213.640091146543));
#219791=CARTESIAN_POINT('Ctrl Pts',(24.0630355105879,-75.715362314347,-213.636895849934));
#219792=CARTESIAN_POINT('Ctrl Pts',(24.0857410597618,-75.7149049538362,
-213.63372538747));
#219793=CARTESIAN_POINT('Ctrl Pts',(24.149226200756,-75.7136261652772,-213.624860715005));
#219794=CARTESIAN_POINT('Ctrl Pts',(24.2127092960951,-75.7123383647039,
-213.616190085964));
#219795=CARTESIAN_POINT('Ctrl Pts',(24.2761875099214,-75.7110415995584,
-213.60771456582));
#219796=CARTESIAN_POINT('Ctrl Pts',(24.4546501076116,-75.707395875104,-213.583886495517));
#219797=CARTESIAN_POINT('Ctrl Pts',(24.6330855092358,-75.7036790698468,
-213.561598684543));
#219798=CARTESIAN_POINT('Ctrl Pts',(24.811493481113,-75.6998909745234,-213.540865649074));
#219799=CARTESIAN_POINT('Ctrl Pts',(24.9328485812406,-75.6973142696687,
-213.526762806198));
#219800=CARTESIAN_POINT('Ctrl Pts',(25.0541916184914,-75.694704503639,-213.51338286188));
#219801=CARTESIAN_POINT('Ctrl Pts',(25.1755222227724,-75.6920616293237,
-213.500729684749));
#219802=CARTESIAN_POINT('Ctrl Pts',(25.9054256855671,-75.6761625647317,
-213.42461040835));
#219803=CARTESIAN_POINT('Ctrl Pts',(26.6348775042369,-75.6590755014285,
-213.374208344441));
#219804=CARTESIAN_POINT('Ctrl Pts',(27.3638191453224,-75.6407602143513,
-213.352071040965));
#219805=CARTESIAN_POINT('Ctrl Pts',(27.9388020795704,-75.6263132724952,
-213.334609325251));
#219806=CARTESIAN_POINT('Ctrl Pts',(28.5134684250624,-75.6111021500901,
-213.334733221256));
#219807=CARTESIAN_POINT('Ctrl Pts',(29.0878122600391,-75.5951066404747,
-213.353691247444));
#219808=CARTESIAN_POINT('Ctrl Pts',(29.2361430259429,-75.5909756199121,
-213.358587371287));
#219809=CARTESIAN_POINT('Ctrl Pts',(29.3844524585103,-75.5867919458944,
-213.364758607598));
#219810=CARTESIAN_POINT('Ctrl Pts',(29.5327391727653,-75.5825553544812,
-213.372223725378));
#219811=CARTESIAN_POINT('Ctrl Pts',(30.095996724499,-75.5664629343402,-213.400579495384));
#219812=CARTESIAN_POINT('Ctrl Pts',(30.6589214000291,-75.5496030053619,
-213.447840466442));
#219813=CARTESIAN_POINT('Ctrl Pts',(31.2214620547992,-75.5319252870199,
-213.517061341304));
#219814=CARTESIAN_POINT('Ctrl Pts',(31.3845113472357,-75.5268014982891,
-213.537124628415));
#219815=CARTESIAN_POINT('Ctrl Pts',(31.5473250535973,-75.5216152683976,
-213.559016745048));
#219816=CARTESIAN_POINT('Ctrl Pts',(31.7100818423904,-75.5163598790567,
-213.582831843075));
#219817=CARTESIAN_POINT('Ctrl Pts',(31.9201729023719,-75.5095760740589,
-213.613573044256));
#219818=CARTESIAN_POINT('Ctrl Pts',(32.1304868253325,-75.5026645193156,
-213.647621648096));
#219819=CARTESIAN_POINT('Ctrl Pts',(32.3408536996831,-75.4956277389932,
-213.685202481806));
#219820=CARTESIAN_POINT('Ctrl Pts',(32.5391806661271,-75.4889936940697,
-213.720632455128));
#219821=CARTESIAN_POINT('Ctrl Pts',(32.7375557017912,-75.4822483051993,
-213.759202024971));
#219822=CARTESIAN_POINT('Ctrl Pts',(32.9358259199764,-75.4753925207355,
-213.801143310705));
#219823=CARTESIAN_POINT('Ctrl Pts',(33.0744170048196,-75.470600320399,-213.830460312233));
#219824=CARTESIAN_POINT('Ctrl Pts',(33.2129566775175,-75.4657541566474,
-213.861425618706));
#219825=CARTESIAN_POINT('Ctrl Pts',(33.3513856130173,-75.4608541370173,
-213.894132075576));
#219826=CARTESIAN_POINT('',(-24.3802580872756,-74.7628322230906,-216.457148834596));
#219827=CARTESIAN_POINT('Ctrl Pts',(-32.863845486296,-74.788639230448,-216.296979356596));
#219828=CARTESIAN_POINT('Ctrl Pts',(-32.3897890127524,-74.7876292350666,
-216.21237071581));
#219829=CARTESIAN_POINT('Ctrl Pts',(-31.9064151032494,-74.7864231071773,
-216.148265135018));
#219830=CARTESIAN_POINT('Ctrl Pts',(-30.8096937949103,-74.783832940506,
-216.043994115321));
#219831=CARTESIAN_POINT('Ctrl Pts',(-30.1907416630467,-74.7824030861366,
-216.013146550001));
#219832=CARTESIAN_POINT('Ctrl Pts',(-28.3232034263091,-74.7780118788819,
-215.992921294503));
#219833=CARTESIAN_POINT('Ctrl Pts',(-27.0679146701128,-74.7750988404896,
-216.073704234167));
#219834=CARTESIAN_POINT('Ctrl Pts',(-25.4971541039145,-74.7685482393304,
-216.276993162089));
#219835=CARTESIAN_POINT('Ctrl Pts',(-25.1828553480248,-74.7670902389161,
-216.322863772022));
#219836=CARTESIAN_POINT('Ctrl Pts',(-24.7112165018673,-74.7646638286032,
-216.399367062212));
#219837=CARTESIAN_POINT('Ctrl Pts',(-24.5539718322166,-74.7638151669929,
-216.426151417743));
#219838=CARTESIAN_POINT('Ctrl Pts',(-24.3915131858716,-74.7628960486129,
-216.455136152234));
#219839=CARTESIAN_POINT('Ctrl Pts',(-24.3859775141005,-74.7629941311872,
-216.455944332801));
#219840=CARTESIAN_POINT('Ctrl Pts',(-24.3802580872756,-74.7628322230906,
-216.457148834596));
#219841=CARTESIAN_POINT('',(-15.4710514507746,-75.1252161784242,-215.898656021024));
#219842=CARTESIAN_POINT('Ctrl Pts',(-24.3802580872756,-74.7628322230906,
-216.457148834596));
#219843=CARTESIAN_POINT('Ctrl Pts',(-24.3593193041524,-74.7638570105243,
-216.459291035607));
#219844=CARTESIAN_POINT('Ctrl Pts',(-24.3356346771204,-74.7655513238598,
-216.460962733904));
#219845=CARTESIAN_POINT('Ctrl Pts',(-24.2899211502609,-74.7683276680052,
-216.464803183085));
#219846=CARTESIAN_POINT('Ctrl Pts',(-24.2213401559703,-74.7724835783518,
-216.470497497242));
#219847=CARTESIAN_POINT('Ctrl Pts',(-24.0612427007151,-74.7821202755749,
-216.483317127563));
#219848=CARTESIAN_POINT('Ctrl Pts',(-23.9238868015989,-74.7902760704183,
-216.493495745774));
#219849=CARTESIAN_POINT('Ctrl Pts',(-23.6490005011524,-74.8064468993936,
-216.512749384951));
#219850=CARTESIAN_POINT('Ctrl Pts',(-23.0984533463628,-74.8382473041046,
-216.546816326886));
#219851=CARTESIAN_POINT('Ctrl Pts',(-22.5457350571009,-74.8683220564567,
-216.56702542312));
#219852=CARTESIAN_POINT('Ctrl Pts',(-21.4378390571114,-74.9258908205721,
-216.587544672568));
#219853=CARTESIAN_POINT('Ctrl Pts',(-20.6958771255011,-74.9607892729635,
-216.574455021372));
#219854=CARTESIAN_POINT('Ctrl Pts',(-19.207074977151,-75.0225411715837,
-216.488342549631));
#219855=CARTESIAN_POINT('Ctrl Pts',(-18.4604021561735,-75.0494131998981,
-216.415548765925));
#219856=CARTESIAN_POINT('Ctrl Pts',(-17.3393212995558,-75.0829993251798,
-216.258218186126));
#219857=CARTESIAN_POINT('Ctrl Pts',(-16.965457286696,-75.0930660264359,
-216.197703030854));
#219858=CARTESIAN_POINT('Ctrl Pts',(-16.3111878076399,-75.1086524189823,
-216.077446851186));
#219859=CARTESIAN_POINT('Ctrl Pts',(-16.0307837607371,-75.1146887137984,
-216.021340208994));
#219860=CARTESIAN_POINT('Ctrl Pts',(-15.7037899646612,-75.1209827194714,
-215.950528672311));
#219861=CARTESIAN_POINT('Ctrl Pts',(-15.6570792202537,-75.1218640593031,
-215.940285071964));
#219862=CARTESIAN_POINT('Ctrl Pts',(-15.5870218132984,-75.123159310396,
-215.924728992095));
#219863=CARTESIAN_POINT('Ctrl Pts',(-15.5636711778655,-75.1235865944026,
-215.91951195042));
#219864=CARTESIAN_POINT('Ctrl Pts',(-15.5169735358771,-75.124432237608,
-215.90901446866));
#219865=CARTESIAN_POINT('Ctrl Pts',(-15.4919351428462,-75.1249550271076,
-215.903217577102));
#219866=CARTESIAN_POINT('Ctrl Pts',(-15.4710515403103,-75.1252154310809,
-215.898655568186));
#219867=CARTESIAN_POINT('',(-5.46041973257396,-75.1055542085046,-216.081029782323));
#219868=CARTESIAN_POINT('Ctrl Pts',(-15.4710513612508,-75.1252169257673,
-215.898656473865));
#219869=CARTESIAN_POINT('Ctrl Pts',(-15.4532848117673,-75.1254395973537,
-215.894776408977));
#219870=CARTESIAN_POINT('Ctrl Pts',(-15.4393547346688,-75.1254225509925,
-215.892050193159));
#219871=CARTESIAN_POINT('Ctrl Pts',(-15.4238009726903,-75.1255059168102,
-215.888868014377));
#219872=CARTESIAN_POINT('Ctrl Pts',(-15.4139021823397,-75.125558972833,
-215.886842798828));
#219873=CARTESIAN_POINT('Ctrl Pts',(-15.4040019487999,-75.1256117765925,
-215.884825471668));
#219874=CARTESIAN_POINT('Ctrl Pts',(-15.3941002813744,-75.1256643291047,
-215.882816013199));
#219875=CARTESIAN_POINT('Ctrl Pts',(-15.3848027542714,-75.125713675178,
-215.880929159826));
#219876=CARTESIAN_POINT('Ctrl Pts',(-15.3755039630117,-75.1257627998731,
-215.879049244014));
#219877=CARTESIAN_POINT('Ctrl Pts',(-15.3662039151108,-75.1258117037368,
-215.877176249902));
#219878=CARTESIAN_POINT('Ctrl Pts',(-15.3500371100749,-75.1258967161193,
-215.87392031714));
#219879=CARTESIAN_POINT('Ctrl Pts',(-15.3338665084111,-75.1259810613781,
-215.870685298734));
#219880=CARTESIAN_POINT('Ctrl Pts',(-15.3176921482388,-75.1260647420003,
-215.867471115233));
#219881=CARTESIAN_POINT('Ctrl Pts',(-15.2667346398205,-75.1263283787665,
-215.857344793014));
#219882=CARTESIAN_POINT('Ctrl Pts',(-15.2157398292535,-75.126585424701,
-215.84742526286));
#219883=CARTESIAN_POINT('Ctrl Pts',(-15.1647089702132,-75.1268360572174,
-215.837709888246));
#219884=CARTESIAN_POINT('Ctrl Pts',(-15.1549733482384,-75.1268838726663,
-215.835856397704));
#219885=CARTESIAN_POINT('Ctrl Pts',(-15.1452364133038,-75.1269314532125,
-215.834010339996));
#219886=CARTESIAN_POINT('Ctrl Pts',(-15.1354981739144,-75.1269787997638,
-215.832171697309));
#219887=CARTESIAN_POINT('Ctrl Pts',(-15.0431472560069,-75.1274278026377,
-215.814735245702));
#219888=CARTESIAN_POINT('Ctrl Pts',(-14.9506790955974,-75.1278557796285,
-215.797965447865));
#219889=CARTESIAN_POINT('Ctrl Pts',(-14.8581003871648,-75.1282633600128,
-215.781848690665));
#219890=CARTESIAN_POINT('Ctrl Pts',(-14.7963296830584,-75.1285353072859,
-215.771095209039));
#219891=CARTESIAN_POINT('Ctrl Pts',(-14.7345097643979,-75.1287981742431,
-215.760632452894));
#219892=CARTESIAN_POINT('Ctrl Pts',(-14.6726426166134,-75.1290521427022,
-215.750456386401));
#219893=CARTESIAN_POINT('Ctrl Pts',(-14.0542810189402,-75.1315905552163,
-215.648746691346));
#219894=CARTESIAN_POINT('Ctrl Pts',(-13.4312745436638,-75.133248132206,
-215.575545102645));
#219895=CARTESIAN_POINT('Ctrl Pts',(-12.8050954815233,-75.1341130418415,
-215.528043650926));
#219896=CARTESIAN_POINT('Ctrl Pts',(-11.5527373572422,-75.1358428611124,
-215.433040747489));
#219897=CARTESIAN_POINT('Ctrl Pts',(-10.2877748918477,-75.1344540393816,
-215.439867099146));
#219898=CARTESIAN_POINT('Ctrl Pts',(-9.0182067883447,-75.1295474748707,
-215.541642492796));
#219899=CARTESIAN_POINT('Ctrl Pts',(-8.38342273659319,-75.1270941926152,
-215.592530189621));
#219900=CARTESIAN_POINT('Ctrl Pts',(-7.74627999058338,-75.123730716052,
-215.66762028791));
#219901=CARTESIAN_POINT('Ctrl Pts',(-7.11146965938098,-75.119358125502,
-215.766852735003));
#219902=CARTESIAN_POINT('Ctrl Pts',(-6.79406449377977,-75.117171830227,
-215.81646895855));
#219903=CARTESIAN_POINT('Ctrl Pts',(-6.47783883753869,-75.1147362439731,
-215.87201775923));
#219904=CARTESIAN_POINT('Ctrl Pts',(-6.1629111324363,-75.1120324006556,
-215.933512637504));
#219905=CARTESIAN_POINT('Ctrl Pts',(-6.03250386903793,-75.1109127760498,
-215.95897682709));
#219906=CARTESIAN_POINT('Ctrl Pts',(-5.90231929343371,-75.1097471139405,
-215.985461175739));
#219907=CARTESIAN_POINT('Ctrl Pts',(-5.77236656503421,-75.108533846862,
-216.012969613053));
#219908=CARTESIAN_POINT('Ctrl Pts',(-5.74540428172294,-75.1082821210914,
-216.018676998265));
#219909=CARTESIAN_POINT('Ctrl Pts',(-5.71845197873014,-75.1080283460713,
-216.024428467385));
#219910=CARTESIAN_POINT('Ctrl Pts',(-5.69150973786122,-75.1077725078021,
-216.03022405551));
#219911=CARTESIAN_POINT('Ctrl Pts',(-5.66646960728471,-75.1075347316017,
-216.035610477676));
#219912=CARTESIAN_POINT('Ctrl Pts',(-5.64143825767027,-75.1072951740359,
-216.041034985145));
#219913=CARTESIAN_POINT('Ctrl Pts',(-5.61641111550247,-75.1070537769128,
-216.046498659192));
#219914=CARTESIAN_POINT('Ctrl Pts',(-5.60225899656066,-75.1069172738804,
-216.049588207509));
#219915=CARTESIAN_POINT('Ctrl Pts',(-5.5881082229804,-75.1067801826414,
-216.052690279619));
#219916=CARTESIAN_POINT('Ctrl Pts',(-5.57395797348773,-75.1066424926987,
-216.055805069817));
#219917=CARTESIAN_POINT('Ctrl Pts',(-5.56213395055293,-75.106527438258,
-216.058407804897));
#219918=CARTESIAN_POINT('Ctrl Pts',(-5.5503106939716,-75.1064119695425,
-216.061019334865));
#219919=CARTESIAN_POINT('Ctrl Pts',(-5.5384882141471,-75.1062960850126,
-216.06363966873));
#219920=CARTESIAN_POINT('Ctrl Pts',(-5.53072620436407,-75.1062200014103,
-216.065360040209));
#219921=CARTESIAN_POINT('Ctrl Pts',(-5.52296450117121,-75.1061437384122,
-216.067084212726));
#219922=CARTESIAN_POINT('Ctrl Pts',(-5.51520313283029,-75.1060672957268,
-216.068812183402));
#219923=CARTESIAN_POINT('Ctrl Pts',(-5.50998013296097,-75.1060158537493,
-216.069975018384));
#219924=CARTESIAN_POINT('Ctrl Pts',(-5.50475728473136,-75.1059643304001,
-216.071139573398));
#219925=CARTESIAN_POINT('Ctrl Pts',(-5.49953459675603,-75.1059127255892,
-216.072305847558));
#219926=CARTESIAN_POINT('Ctrl Pts',(-5.4949664419899,-75.1058675881496,
-216.073325958444));
#219927=CARTESIAN_POINT('Ctrl Pts',(-5.49039840272466,-75.1058223886675,
-216.074347385634));
#219928=CARTESIAN_POINT('Ctrl Pts',(-5.48583047998682,-75.1057771267157,
-216.075370130076));
#219929=CARTESIAN_POINT('Ctrl Pts',(-5.47741546935228,-75.1056937453129,
-216.077254226161));
#219930=CARTESIAN_POINT('Ctrl Pts',(-5.47001733418767,-75.1054407487899,
-216.079184123322));
#219931=CARTESIAN_POINT('Ctrl Pts',(-5.46041973163172,-75.1055542085157,
-216.081029782504));
#219932=CARTESIAN_POINT('',(-2.08228321273563E-9,-75.1718294574641,-216.556685219365));
#219933=CARTESIAN_POINT('Ctrl Pts',(-5.46041973163172,-75.1055542085157,
-216.081029782504));
#219934=CARTESIAN_POINT('Ctrl Pts',(-5.45885110379661,-75.1055727671836,
-216.081331414038));
#219935=CARTESIAN_POINT('Ctrl Pts',(-5.45722372289247,-75.1056011148421,
-216.08163079528));
#219936=CARTESIAN_POINT('Ctrl Pts',(-5.45552354686627,-75.1056415918994,
-216.081927358492));
#219937=CARTESIAN_POINT('Ctrl Pts',(-5.42896346001207,-75.1062739229874,
-216.086560258006));
#219938=CARTESIAN_POINT('Ctrl Pts',(-5.4023997922979,-75.1069019363042,
-216.091161602676));
#219939=CARTESIAN_POINT('Ctrl Pts',(-5.37583248801623,-75.1075256256449,
-216.095731281078));
#219940=CARTESIAN_POINT('Ctrl Pts',(-5.34756454570321,-75.1081892388635,
-216.100593475754));
#219941=CARTESIAN_POINT('Ctrl Pts',(-5.31929239183766,-75.1088479905342,
-216.105419789335));
#219942=CARTESIAN_POINT('Ctrl Pts',(-5.29101614121995,-75.109501813166,
-216.110210140245));
#219943=CARTESIAN_POINT('Ctrl Pts',(-5.24899125576366,-75.1104735410511,
-216.117329682048));
#219944=CARTESIAN_POINT('Ctrl Pts',(-5.2069570409512,-75.1114344776116,
-216.124369701056));
#219945=CARTESIAN_POINT('Ctrl Pts',(-5.16491312624508,-75.1123846717332,
-216.131329677671));
#219946=CARTESIAN_POINT('Ctrl Pts',(-5.15037893222956,-75.1127131450881,
-216.133735677474));
#219947=CARTESIAN_POINT('Ctrl Pts',(-5.13584345917987,-75.1130403536024,
-216.136132065221));
#219948=CARTESIAN_POINT('Ctrl Pts',(-5.12130671024801,-75.1133662960798,
-216.138518821461));
#219949=CARTESIAN_POINT('Ctrl Pts',(-5.00813060145967,-75.1159039268427,
-216.157100953211));
#219950=CARTESIAN_POINT('Ctrl Pts',(-4.89487775170335,-75.1183645441208,
-216.17509957011));
#219951=CARTESIAN_POINT('Ctrl Pts',(-4.7815505844652,-75.1207471055566,
-216.192506042143));
#219952=CARTESIAN_POINT('Ctrl Pts',(-4.13290185680472,-75.1343841308309,
-216.292135162081));
#219953=CARTESIAN_POINT('Ctrl Pts',(-3.48181844620929,-75.1454639977537,
-216.372365290844));
#219954=CARTESIAN_POINT('Ctrl Pts',(-2.82877069498839,-75.1537838320299,
-216.431585941174));
#219955=CARTESIAN_POINT('Ctrl Pts',(-2.4378715048134,-75.1587638912597,
-216.467034044643));
#219956=CARTESIAN_POINT('Ctrl Pts',(-2.04648484597347,-75.1627399695325,
-216.49496695171));
#219957=CARTESIAN_POINT('Ctrl Pts',(-1.6545361090901,-75.1656914643869,
-216.51520608631));
#219958=CARTESIAN_POINT('Ctrl Pts',(-1.55726525698595,-75.1664239438987,
-216.520228880576));
#219959=CARTESIAN_POINT('Ctrl Pts',(-1.45999630524016,-75.1670898141191,
-216.524764978152));
#219960=CARTESIAN_POINT('Ctrl Pts',(-1.36278838454174,-75.1676893633231,
-216.528830176404));
#219961=CARTESIAN_POINT('Ctrl Pts',(-1.0683010862481,-75.1695056723644,
-216.541145523156));
#219962=CARTESIAN_POINT('Ctrl Pts',(-0.774374080750881,-75.1707133120289,
-216.549139133372));
#219963=CARTESIAN_POINT('Ctrl Pts',(-0.482651045412875,-75.1713202986035,
-216.553250233342));
#219964=CARTESIAN_POINT('Ctrl Pts',(-0.32135449366988,-75.1716559074844,
-216.55552330118));
#219965=CARTESIAN_POINT('Ctrl Pts',(-0.160674879972797,-75.1718268822641,
-216.556675869296));
#219966=CARTESIAN_POINT('Ctrl Pts',(-2.08390146224025E-9,-75.1718294574641,
-216.556685219365));
#219967=CARTESIAN_POINT('',(5.46042745654276,-75.1055279660516,-216.081066924971));
#219968=CARTESIAN_POINT('Ctrl Pts',(5.46042745578382,-75.1055279660664,
-216.081066925108));
#219969=CARTESIAN_POINT('Ctrl Pts',(5.45993480282964,-75.1055396823069,
-216.08115292583));
#219970=CARTESIAN_POINT('Ctrl Pts',(5.45943508011546,-75.105552577858,-216.081238659116));
#219971=CARTESIAN_POINT('Ctrl Pts',(5.45892782922234,-75.1055667291498,
-216.081324107006));
#219972=CARTESIAN_POINT('Ctrl Pts',(5.43445808519729,-75.106249386377,-216.08544610666));
#219973=CARTESIAN_POINT('Ctrl Pts',(5.41003401191501,-75.1069218819067,
-216.089540658102));
#219974=CARTESIAN_POINT('Ctrl Pts',(5.38565413548417,-75.1075845285616,
-216.093607913568));
#219975=CARTESIAN_POINT('Ctrl Pts',(5.18349069268347,-75.1130793443166,
-216.127334514682));
#219976=CARTESIAN_POINT('Ctrl Pts',(4.98432744151869,-75.1178998244099,
-216.159195131404));
#219977=CARTESIAN_POINT('Ctrl Pts',(4.7873988108972,-75.1222097067706,-216.189233242711));
#219978=CARTESIAN_POINT('Ctrl Pts',(4.59346686514457,-75.1264540051721,
-216.218814260739));
#219979=CARTESIAN_POINT('Ctrl Pts',(4.40170187503902,-75.1302028561389,
-216.246627797542));
#219980=CARTESIAN_POINT('Ctrl Pts',(4.2113748109516,-75.133596771578,-216.272668667851));
#219981=CARTESIAN_POINT('Ctrl Pts',(4.02263252030788,-75.1369624273102,
-216.29849270678));
#219982=CARTESIAN_POINT('Ctrl Pts',(3.83539560876742,-75.1399698220657,
-216.322564617354));
#219983=CARTESIAN_POINT('Ctrl Pts',(3.64894511433005,-75.1427408218472,
-216.344863570406));
#219984=CARTESIAN_POINT('Ctrl Pts',(3.46350264848808,-75.1454968404561,
-216.367041966081));
#219985=CARTESIAN_POINT('Ctrl Pts',(3.27883802569263,-75.1480189080841,
-216.387466521769));
#219986=CARTESIAN_POINT('Ctrl Pts',(3.0942537415948,-75.1504164842619,-216.406067479382));
#219987=CARTESIAN_POINT('Ctrl Pts',(2.97606961646031,-75.1519515848497,
-216.417977149335));
#219988=CARTESIAN_POINT('Ctrl Pts',(2.8579186272538,-75.1534354475146,-216.429138253026));
#219989=CARTESIAN_POINT('Ctrl Pts',(2.73962012210223,-75.1548947920788,
-216.439521688862));
#219990=CARTESIAN_POINT('Ctrl Pts',(2.47563199262865,-75.1581513813423,
-216.462692766133));
#219991=CARTESIAN_POINT('Ctrl Pts',(2.20960587740754,-75.1609796487111,
-216.482597308869));
#219992=CARTESIAN_POINT('Ctrl Pts',(1.94119260980385,-75.1633477206973,
-216.499030144061));
#219993=CARTESIAN_POINT('Ctrl Pts',(1.91262982784451,-75.1635997154083,
-216.500778818755));
#219994=CARTESIAN_POINT('Ctrl Pts',(1.88404001758171,-75.16384649255,-216.502488132198));
#219995=CARTESIAN_POINT('Ctrl Pts',(1.85542276083298,-75.1640880090813,
-216.504157802307));
#219996=CARTESIAN_POINT('Ctrl Pts',(1.6615865500581,-75.1657238978628,-216.515467150717));
#219997=CARTESIAN_POINT('Ctrl Pts',(1.46632769852334,-75.167117630478,-216.524914581302));
#219998=CARTESIAN_POINT('Ctrl Pts',(1.27012448174892,-75.1682493321424,
-216.532526663344));
#219999=CARTESIAN_POINT('Ctrl Pts',(1.0739212649745,-75.1693810338068,-216.540138745386));
#220000=CARTESIAN_POINT('Ctrl Pts',(0.876772908783234,-75.1702507211618,
-216.545915388321));
#220001=CARTESIAN_POINT('Ctrl Pts',(0.679214520499131,-75.1708359333832,
-216.549878882062));
#220002=CARTESIAN_POINT('Ctrl Pts',(0.514175265018196,-75.1713248166453,
-216.553189964228));
#220003=CARTESIAN_POINT('Ctrl Pts',(0.348963760683292,-75.1716349551876,
-216.555303266427));
#220004=CARTESIAN_POINT('Ctrl Pts',(0.182855563317092,-75.1717627023986,
-216.556196336037));
#220005=CARTESIAN_POINT('Ctrl Pts',(0.122036851785086,-75.1718094756518,
-216.556523323771));
#220006=CARTESIAN_POINT('Ctrl Pts',(0.0610974427796169,-75.17183179282,
-216.556686693538));
#220007=CARTESIAN_POINT('Ctrl Pts',(-2.08228314334659E-9,-75.1718294574641,
-216.556685219365));
#220008=CARTESIAN_POINT('Ctrl Pts',(15.4710515403117,-75.1252154310692,
-215.898655568178));
#220009=CARTESIAN_POINT('Ctrl Pts',(15.4710444072622,-75.1252155180421,
-215.898654010539));
#220010=CARTESIAN_POINT('Ctrl Pts',(15.4710372753328,-75.1252156049439,
-215.898652453234));
#220011=CARTESIAN_POINT('Ctrl Pts',(15.4710301445247,-75.1252156917747,
-215.898650896265));
#220012=CARTESIAN_POINT('Ctrl Pts',(15.4632205313114,-75.1253107882393,
-215.89694571343));
#220013=CARTESIAN_POINT('Ctrl Pts',(15.4566954720675,-75.1253250136118,
-215.895632435197));
#220014=CARTESIAN_POINT('Ctrl Pts',(15.4500821771012,-75.1253433777805,
-215.894298660203));
#220015=CARTESIAN_POINT('Ctrl Pts',(15.4473001599164,-75.1253511030419,
-215.893737580594));
#220016=CARTESIAN_POINT('Ctrl Pts',(15.4445019222413,-75.1253595982398,
-215.89317269173));
#220017=CARTESIAN_POINT('Ctrl Pts',(15.4415826360871,-75.1253753548161,
-215.892572501974));
#220018=CARTESIAN_POINT('Ctrl Pts',(15.431805521493,-75.1254281258855,-215.890562379049));
#220019=CARTESIAN_POINT('Ctrl Pts',(15.4219863172516,-75.125480885207,-215.888551578341));
#220020=CARTESIAN_POINT('Ctrl Pts',(15.4121257804215,-75.1255336230737,
-215.886540432606));
#220021=CARTESIAN_POINT('Ctrl Pts',(15.3125359516136,-75.1260662670059,
-215.866228185619));
#220022=CARTESIAN_POINT('Ctrl Pts',(15.2087290430498,-75.1265966180202,
-215.845884352904));
#220023=CARTESIAN_POINT('Ctrl Pts',(15.1014911451759,-75.1271154275382,
-215.825827329062));
#220024=CARTESIAN_POINT('Ctrl Pts',(15.0483340175637,-75.1273725980377,
-215.815885192961));
#220025=CARTESIAN_POINT('Ctrl Pts',(14.994334045534,-75.1276269586628,-215.806012782418));
#220026=CARTESIAN_POINT('Ctrl Pts',(14.9395881264798,-75.1278775432677,
-215.796244204861));
#220027=CARTESIAN_POINT('Ctrl Pts',(14.8328496966638,-75.1283661094974,
-215.777198353628));
#220028=CARTESIAN_POINT('Ctrl Pts',(14.7232666795004,-75.1288402890429,
-215.758549615031));
#220029=CARTESIAN_POINT('Ctrl Pts',(14.6116090761272,-75.1292936107873,
-215.740523436667));
#220030=CARTESIAN_POINT('Ctrl Pts',(14.4998196734473,-75.1297474676273,
-215.722475980418));
#220031=CARTESIAN_POINT('Ctrl Pts',(14.3859511729408,-75.1301804134914,
-215.705052733827));
#220032=CARTESIAN_POINT('Ctrl Pts',(14.2707946954948,-75.1305875112326,
-215.688430822599));
#220033=CARTESIAN_POINT('Ctrl Pts',(14.1775809961871,-75.1309170375196,
-215.674976174892));
#220034=CARTESIAN_POINT('Ctrl Pts',(14.08352386201,-75.1312296577405,-215.662045641129));
#220035=CARTESIAN_POINT('Ctrl Pts',(13.9890487123067,-75.131523511689,-215.649708842601));
#220036=CARTESIAN_POINT('Ctrl Pts',(13.8706173590175,-75.1318918786183,
-215.634243783804));
#220037=CARTESIAN_POINT('Ctrl Pts',(13.7514956746712,-75.1322310618388,
-215.619703035971));
#220038=CARTESIAN_POINT('Ctrl Pts',(13.6324649705354,-75.1325385051961,
-215.606174570825));
#220039=CARTESIAN_POINT('Ctrl Pts',(13.5110600892106,-75.1328520807948,
-215.592376267964));
#220040=CARTESIAN_POINT('Ctrl Pts',(13.3897499113001,-75.1331326371434,
-215.579631007093));
#220041=CARTESIAN_POINT('Ctrl Pts',(13.269366485729,-75.1333791353553,-215.567977329651));
#220042=CARTESIAN_POINT('Ctrl Pts',(13.1857541228561,-75.1335503408002,
-215.559883262694));
#220043=CARTESIAN_POINT('Ctrl Pts',(13.1025888908574,-75.1337051523037,
-215.552314606038));
#220044=CARTESIAN_POINT('Ctrl Pts',(13.0201501679703,-75.1338436762563,
-215.545269564757));
#220045=CARTESIAN_POINT('Ctrl Pts',(12.74793949394,-75.1343010790058,-215.522007008418));
#220046=CARTESIAN_POINT('Ctrl Pts',(12.4736131226656,-75.1346118390224,
-215.503567904302));
#220047=CARTESIAN_POINT('Ctrl Pts',(12.1974965686788,-75.1347541683181,
-215.489955494028));
#220048=CARTESIAN_POINT('Ctrl Pts',(12.158295281145,-75.1347743753341,-215.488022889838));
#220049=CARTESIAN_POINT('Ctrl Pts',(12.1190579304802,-75.1347911879743,
-215.486187491866));
#220050=CARTESIAN_POINT('Ctrl Pts',(12.079785468434,-75.134804544487,-215.484449227347));
#220051=CARTESIAN_POINT('Ctrl Pts',(11.9686573435008,-75.1348423390162,
-215.479530511623));
#220052=CARTESIAN_POINT('Ctrl Pts',(11.8572498437104,-75.1348526804321,
-215.475382902043));
#220053=CARTESIAN_POINT('Ctrl Pts',(11.745583751326,-75.1348334804312,-215.472014693408));
#220054=CARTESIAN_POINT('Ctrl Pts',(11.531040929044,-75.1347965916827,-215.465543391591));
#220055=CARTESIAN_POINT('Ctrl Pts',(11.3155447321185,-75.134682579359,-215.461900568881));
#220056=CARTESIAN_POINT('Ctrl Pts',(11.0992457878686,-75.1344846717163,
-215.461123426466));
#220057=CARTESIAN_POINT('Ctrl Pts',(10.9910963157436,-75.134385717895,-215.460734855258));
#220058=CARTESIAN_POINT('Ctrl Pts',(10.8827460955464,-75.1342626066487,
-215.46106738632));
#220059=CARTESIAN_POINT('Ctrl Pts',(10.7742145999442,-75.1341148057718,
-215.462123878904));
#220060=CARTESIAN_POINT('Ctrl Pts',(10.719948852143,-75.1340409053334,-215.462652125196));
#220061=CARTESIAN_POINT('Ctrl Pts',(10.665637788193,-75.1339608327989,-215.463361348184));
#220062=CARTESIAN_POINT('Ctrl Pts',(10.6112838593016,-75.1338745235653,
-215.464251823122));
#220063=CARTESIAN_POINT('Ctrl Pts',(10.5841068948558,-75.1338313689484,
-215.464697060592));
#220064=CARTESIAN_POINT('Ctrl Pts',(10.5569192142964,-75.1337866551771,
-215.465187610195));
#220065=CARTESIAN_POINT('Ctrl Pts',(10.5297211268796,-75.1337403743035,
-215.465723501161));
#220066=CARTESIAN_POINT('Ctrl Pts',(10.5025230394628,-75.1336940934299,
-215.466259392128));
#220067=CARTESIAN_POINT('Ctrl Pts',(10.4739383472588,-75.1336437465829,
-215.466872305924));
#220068=CARTESIAN_POINT('Ctrl Pts',(10.448095954022,-75.1335968225131,-215.467467223928));
#220069=CARTESIAN_POINT('Ctrl Pts',(10.1462333405878,-75.1330487067788,
-215.474416406298));
#220070=CARTESIAN_POINT('Ctrl Pts',(9.84329653499747,-75.1323073858502,
-215.486945485866));
#220071=CARTESIAN_POINT('Ctrl Pts',(9.53971836891024,-75.1313633897806,
-215.505042608647));
#220072=CARTESIAN_POINT('Ctrl Pts',(9.2333624588946,-75.1304107561355,-215.523305320322));
#220073=CARTESIAN_POINT('Ctrl Pts',(8.9263535402191,-75.1292517076195,-215.54723840805));
#220074=CARTESIAN_POINT('Ctrl Pts',(8.61913837793364,-75.1278781119617,
-215.576776604102));
#220075=CARTESIAN_POINT('Ctrl Pts',(8.49748869591185,-75.1273342017141,
-215.588473006488));
#220076=CARTESIAN_POINT('Ctrl Pts',(8.37580668504316,-75.1267566698495,
-215.601047692491));
#220077=CARTESIAN_POINT('Ctrl Pts',(8.25412008964395,-75.1261450871463,
-215.614494361863));
#220078=CARTESIAN_POINT('Ctrl Pts',(7.93597421378264,-75.1245461229043,
-215.649650267003));
#220079=CARTESIAN_POINT('Ctrl Pts',(7.6177819932054,-75.1227121680132,-215.690837597706));
#220080=CARTESIAN_POINT('Ctrl Pts',(7.30003766104192,-75.1206257462514,
-215.738083374911));
#220081=CARTESIAN_POINT('Ctrl Pts',(6.98229332887844,-75.1185393244897,
-215.785329152116));
#220082=CARTESIAN_POINT('Ctrl Pts',(6.66499706338629,-75.1162004058076,
-215.838633471389));
#220083=CARTESIAN_POINT('Ctrl Pts',(6.34863921534703,-75.1135939732195,
-215.897965001334));
#220084=CARTESIAN_POINT('Ctrl Pts',(6.19013846044381,-75.1122881054013,
-215.92769112428));
#220085=CARTESIAN_POINT('Ctrl Pts',(6.03187496724258,-75.110914607648,-215.95893405755));
#220086=CARTESIAN_POINT('Ctrl Pts',(5.87391202237455,-75.1094709993413,
-215.99169380274));
#220087=CARTESIAN_POINT('Ctrl Pts',(5.85986277650748,-75.1093426046216,
-215.994607458946));
#220088=CARTESIAN_POINT('Ctrl Pts',(5.84581590807222,-75.1092136552757,
-215.997533113053));
#220089=CARTESIAN_POINT('Ctrl Pts',(5.83177146177245,-75.1090841494548,
-216.000470765675));
#220090=CARTESIAN_POINT('Ctrl Pts',(5.76675282097511,-75.1084846033941,
-216.014070602686));
#220091=CARTESIAN_POINT('Ctrl Pts',(5.70178675789727,-75.1078733517838,
-216.027927095996));
#220092=CARTESIAN_POINT('Ctrl Pts',(5.63685944095259,-75.1072499409931,
-216.042044479373));
#220093=CARTESIAN_POINT('Ctrl Pts',(5.59736507119977,-75.1068707290152,
-216.050631884263));
#220094=CARTESIAN_POINT('Ctrl Pts',(5.55788503954139,-75.1064870172208,
-216.059315834801));
#220095=CARTESIAN_POINT('Ctrl Pts',(5.51841624616035,-75.1060986971487,
-216.068097395342));
#220096=CARTESIAN_POINT('Ctrl Pts',(5.50854826989078,-75.106001609477,-216.07029295856));
#220097=CARTESIAN_POINT('Ctrl Pts',(5.49868099617033,-75.1059042337217,
-216.072494623766));
#220098=CARTESIAN_POINT('Ctrl Pts',(5.48881437665547,-75.1058065681362,
-216.074702408412));
#220099=CARTESIAN_POINT('Ctrl Pts',(5.47935752456062,-75.1057129586689,
-216.07681850226));
#220100=CARTESIAN_POINT('Ctrl Pts',(5.47177960667182,-75.105305864689,-216.079013797392));
#220101=CARTESIAN_POINT('Ctrl Pts',(5.46042745654277,-75.1055279660516,
-216.081066924971));
#220102=CARTESIAN_POINT('Ctrl Pts',(33.2001189077142,-74.6413232806246,
-216.55743652807));
#220103=CARTESIAN_POINT('Ctrl Pts',(33.006978144415,-74.6583015829289,-216.5409993187));
#220104=CARTESIAN_POINT('Ctrl Pts',(32.8147762212939,-74.654089681431,-216.510956849065));
#220105=CARTESIAN_POINT('Ctrl Pts',(33.2543277379907,-75.1597676010536,
-215.769699247187));
#220106=CARTESIAN_POINT('Ctrl Pts',(33.1208674957723,-75.1687053141157,
-215.755692348251));
#220107=CARTESIAN_POINT('Ctrl Pts',(32.9875388545361,-75.1686237089069,
-215.738022261266));
#220108=CARTESIAN_POINT('Ctrl Pts',(33.3072722515331,-75.4457401389311,
-214.838681123811));
#220109=CARTESIAN_POINT('Ctrl Pts',(33.2414347818499,-75.4479382330087,
-214.830721324794));
#220110=CARTESIAN_POINT('Ctrl Pts',(33.1755313708028,-75.45012854121,-214.823325453787));
#220111=CARTESIAN_POINT('Ctrl Pts',(33.3513928282978,-75.4608560063641,
-213.894101968638));
#220112=CARTESIAN_POINT('Ctrl Pts',(33.3513928282978,-75.4608560063641,
-213.894101968638));
#220113=CARTESIAN_POINT('Ctrl Pts',(33.3513928282978,-75.4608560063641,
-213.894101968638));
#220114=CARTESIAN_POINT('',(33.2148661077881,-74.776924583375,-216.339144130369));
#220115=CARTESIAN_POINT('Origin',(33.132841491033,-72.1913959359691,-214.819830610287));
#220116=CARTESIAN_POINT('Origin',(33.2007176148554,-71.2835629216187,-214.037774394011));
#220117=CARTESIAN_POINT('Ctrl Pts',(33.1752262860966,-74.6372704537069,
-216.564961398279));
#220118=CARTESIAN_POINT('Ctrl Pts',(32.9990492150883,-74.6974990623407,
-216.482388336084));
#220119=CARTESIAN_POINT('Ctrl Pts',(32.8237598256931,-74.7342241033955,
-216.385388039321));
#220120=CARTESIAN_POINT('Ctrl Pts',(33.1949631872882,-74.6820694401112,
-216.496303691397));
#220121=CARTESIAN_POINT('Ctrl Pts',(33.0186275335319,-74.7272821064536,
-216.433478854616));
#220122=CARTESIAN_POINT('Ctrl Pts',(32.8430811295252,-74.7517232841479,
-216.358132577342));
#220123=CARTESIAN_POINT('Ctrl Pts',(33.2094670740371,-74.7292736488378,
-216.420526748278));
#220124=CARTESIAN_POINT('Ctrl Pts',(33.0332084422046,-74.7590740423288,
-216.380020841619));
#220125=CARTESIAN_POINT('Ctrl Pts',(32.8576392292869,-74.7701076430367,
-216.328432913941));
#220126=CARTESIAN_POINT('Ctrl Pts',(33.214866107803,-74.776924583857,-216.339144130663));
#220127=CARTESIAN_POINT('Ctrl Pts',(33.039029721468,-74.791820591591,-216.32328753345));
#220128=CARTESIAN_POINT('Ctrl Pts',(32.8638454862961,-74.788639230448,-216.296979356596));
#220129=CARTESIAN_POINT('',(33.1752262860962,-74.6372704537073,-216.564961398278));
#220130=CARTESIAN_POINT('',(32.8237598256931,-74.7342241033955,-216.385388039321));
#220131=CARTESIAN_POINT('Origin',(33.095784450501,-72.1361943004091,-214.910178309726));
#220132=CARTESIAN_POINT('Origin',(32.1378319467103,-74.4550490573172,-216.331724193165));
#220133=CARTESIAN_POINT('Origin',(31.688241471423,-74.6383695133239,-216.347659411481));
#220134=CARTESIAN_POINT('Ctrl Pts',(40.9503927122327,-75.196232348644,-213.885776709122));
#220135=CARTESIAN_POINT('Ctrl Pts',(40.9511754288092,-75.170618016806,-215.350418326104));
#220136=CARTESIAN_POINT('Ctrl Pts',(40.9214983009156,-74.3592730501824,
-216.569709261874));
#220137=CARTESIAN_POINT('Ctrl Pts',(38.3512480421664,-75.2960131239162,
-213.888896036206));
#220138=CARTESIAN_POINT('Ctrl Pts',(38.3524464105013,-75.2704427058848,
-215.35035620914));
#220139=CARTESIAN_POINT('Ctrl Pts',(38.3243446255555,-74.4622360886798,
-216.567950322327));
#220140=CARTESIAN_POINT('Ctrl Pts',(35.7515873189136,-75.386298205372,-213.891764703899));
#220141=CARTESIAN_POINT('Ctrl Pts',(35.7526446696784,-75.3607900951698,
-215.350336416166));
#220142=CARTESIAN_POINT('Ctrl Pts',(35.7265937516153,-74.5554064323997,
-216.566381833318));
#220143=CARTESIAN_POINT('Ctrl Pts',(33.1518661790638,-75.4670741746135,
-213.89429696046));
#220144=CARTESIAN_POINT('Ctrl Pts',(33.1525004164731,-75.4416278685769,
-215.350281850594));
#220145=CARTESIAN_POINT('Ctrl Pts',(33.1287433582894,-74.6387629869627,
-216.564935505388));
#220146=CARTESIAN_POINT('',(40.9214982998565,-74.3592730496089,-216.569709262804));
#220147=CARTESIAN_POINT('Origin',(-0.00331736233953883,957.648657693644,
-233.042565174374));
#220148=CARTESIAN_POINT('',(40.9503927122327,-75.1962323486441,-213.885776709122));
#220149=CARTESIAN_POINT('Origin',(40.758509388043,-70.2006777120066,-213.798514676938));
#220150=CARTESIAN_POINT('Origin',(-0.00137743448293204,990.512730862347,
-181.064274177303));
#220151=CARTESIAN_POINT('Ctrl Pts',(41.9926628230245,-75.1580153204876,
-213.752528187964));
#220152=CARTESIAN_POINT('Ctrl Pts',(42.3889675192146,-75.111938779609,-215.496580546143));
#220153=CARTESIAN_POINT('Ctrl Pts',(42.6506409244545,-73.9423397713714,
-216.824911934325));
#220154=CARTESIAN_POINT('Ctrl Pts',(41.9066793323699,-75.1610610934851,
-213.772054913982));
#220155=CARTESIAN_POINT('Ctrl Pts',(42.2773680112949,-75.116350496584,-215.497499167852));
#220156=CARTESIAN_POINT('Ctrl Pts',(42.5223146433776,-73.9743057102176,
-216.821387777151));
#220157=CARTESIAN_POINT('Ctrl Pts',(41.8205323433655,-75.1641318505835,
-213.789924116914));
#220158=CARTESIAN_POINT('Ctrl Pts',(42.1584887885637,-75.1211304958163,
-215.492781710638));
#220159=CARTESIAN_POINT('Ctrl Pts',(42.3813794284652,-74.0123061097281,
-216.810485774879));
#220160=CARTESIAN_POINT('Ctrl Pts',(41.6477999581399,-75.1703415381605,
-213.821539718001));
#220161=CARTESIAN_POINT('Ctrl Pts',(41.9257553840235,-75.1304773990168,
-215.482136500692));
#220162=CARTESIAN_POINT('Ctrl Pts',(42.1071714177053,-74.0810920561211,
-216.786773384908));
#220163=CARTESIAN_POINT('Ctrl Pts',(41.5612314342482,-75.1734777382289,
-213.835404439881));
#220164=CARTESIAN_POINT('Ctrl Pts',(41.8102296619885,-75.1351214208437,
-215.47561143684));
#220165=CARTESIAN_POINT('Ctrl Pts',(41.9710574680702,-74.1134796538391,
-216.773245626094));
#220166=CARTESIAN_POINT('Ctrl Pts',(41.3876518834424,-75.1798203744341,
-213.858883738274));
#220167=CARTESIAN_POINT('Ctrl Pts',(41.5763451014607,-75.1445888151757,
-215.456563678652));
#220168=CARTESIAN_POINT('Ctrl Pts',(41.6930958560081,-74.1786675398504,
-216.738185296849));
#220169=CARTESIAN_POINT('Ctrl Pts',(41.3006463902351,-75.1830256709096,
-213.868551556963));
#220170=CARTESIAN_POINT('Ctrl Pts',(41.457783462217,-75.1494218955781,-215.443955718151));
#220171=CARTESIAN_POINT('Ctrl Pts',(41.5508831144746,-74.211785746889,-216.716530930378));
#220172=CARTESIAN_POINT('Ctrl Pts',(41.1260290982083,-75.1895400074134,
-213.882061105842));
#220173=CARTESIAN_POINT('Ctrl Pts',(41.2077086857337,-75.1598056161679,
-215.404074252971));
#220174=CARTESIAN_POINT('Ctrl Pts',(41.2425985226721,-74.2859889767733,
-216.652644382816));
#220175=CARTESIAN_POINT('Ctrl Pts',(41.0384011165223,-75.1928537189715,
-213.885671097949));
#220176=CARTESIAN_POINT('Ctrl Pts',(41.0764186050639,-75.1653524051027,
-215.376453037444));
#220177=CARTESIAN_POINT('Ctrl Pts',(41.0767448130875,-74.3265280313286,
-216.609717214812));
#220178=CARTESIAN_POINT('Ctrl Pts',(40.9503927097337,-75.1962323487394,
-213.885776709126));
#220179=CARTESIAN_POINT('Ctrl Pts',(40.9511754272533,-75.1706180168537,
-215.350418326773));
#220180=CARTESIAN_POINT('Ctrl Pts',(40.9214983001298,-74.3592730495305,
-216.569709262898));
#220181=CARTESIAN_POINT('',(42.6506409244548,-73.9423397713703,-216.824911934326));
#220182=CARTESIAN_POINT('',(41.992662823025,-75.1580153204871,-213.752528187964));
#220183=CARTESIAN_POINT('Origin',(41.7958961124187,-70.1626506491805,-213.665266155779));
#220184=CARTESIAN_POINT('Ctrl Pts',(40.9503927122327,-75.1962323486435,
-213.885776709123));
#220185=CARTESIAN_POINT('Ctrl Pts',(41.0384742514642,-75.1928509113328,
-213.885671010119));
#220186=CARTESIAN_POINT('Ctrl Pts',(41.1260976159393,-75.1895374500536,
-213.882055874302));
#220187=CARTESIAN_POINT('Ctrl Pts',(41.2133377538246,-75.1862828366109,
-213.875306456167));
#220188=CARTESIAN_POINT('Ctrl Pts',(41.3007070197978,-75.183023405867,-213.868547047912));
#220189=CARTESIAN_POINT('Ctrl Pts',(41.3877081322076,-75.1798183151621,
-213.858876354802));
#220190=CARTESIAN_POINT('Ctrl Pts',(41.474441679009,-75.1766490529394,-213.847144238358));
#220191=CARTESIAN_POINT('Ctrl Pts',(41.5612776272786,-75.1734760489453,
-213.835398270459));
#220192=CARTESIAN_POINT('Ctrl Pts',(41.6478454293564,-75.1703399027889,
-213.821531434952));
#220193=CARTESIAN_POINT('Ctrl Pts',(41.7341661542895,-75.167236693896,-213.805731936783));
#220194=CARTESIAN_POINT('Ctrl Pts',(41.8205769752921,-75.1641302460715,
-213.789915948105));
#220195=CARTESIAN_POINT('Ctrl Pts',(41.9067233040927,-75.1610595358851,
-213.772044928068));
#220196=CARTESIAN_POINT('Ctrl Pts',(41.9926628230246,-75.1580153204876,
-213.752528187964));
#220197=CARTESIAN_POINT('Ctrl Pts',(42.6506409244545,-73.9423397713714,
-216.824911934325));
#220198=CARTESIAN_POINT('Ctrl Pts',(42.6307622877728,-73.9472915225057,
-216.824366012901));
#220199=CARTESIAN_POINT('Ctrl Pts',(42.6093064459885,-73.9527355471689,
-216.823572622786));
#220200=CARTESIAN_POINT('Ctrl Pts',(42.5862580487576,-73.9586516704412,
-216.822521533163));
#220201=CARTESIAN_POINT('Ctrl Pts',(42.5651297238504,-73.9640749444952,
-216.821558005729));
#220202=CARTESIAN_POINT('Ctrl Pts',(42.5426629131741,-73.9698950400132,
-216.820377807274));
#220203=CARTESIAN_POINT('Ctrl Pts',(42.5188810740907,-73.9760752302692,
-216.818985181213));
#220204=CARTESIAN_POINT('Ctrl Pts',(42.5012061616511,-73.9806684125396,
-216.817950166907));
#220205=CARTESIAN_POINT('Ctrl Pts',(42.4828055171911,-73.9854601121619,
-216.816798032545));
#220206=CARTESIAN_POINT('Ctrl Pts',(42.4637042950621,-73.9904260452816,
-216.815536054635));
#220207=CARTESIAN_POINT('Ctrl Pts',(42.4404178110658,-73.9964800622099,
-216.813997565203));
#220208=CARTESIAN_POINT('Ctrl Pts',(42.4160776169921,-74.0027995026238,
-216.812291477255));
#220209=CARTESIAN_POINT('Ctrl Pts',(42.3906990643268,-74.0093570496853,
-216.810412585741));
#220210=CARTESIAN_POINT('Ctrl Pts',(42.3763863042646,-74.0130553140792,
-216.809352945983));
#220211=CARTESIAN_POINT('Ctrl Pts',(42.3617439418181,-74.0168288938945,
-216.808238554472));
#220212=CARTESIAN_POINT('Ctrl Pts',(42.3467808471404,-74.0206690551345,
-216.807070477435));
#220213=CARTESIAN_POINT('Ctrl Pts',(42.3260334557344,-74.0259937108977,
-216.805450855826));
#220214=CARTESIAN_POINT('Ctrl Pts',(42.3046653349005,-74.0314489113354,
-216.803726144206));
#220215=CARTESIAN_POINT('Ctrl Pts',(42.282693951358,-74.0370140073013,-216.801893254208));
#220216=CARTESIAN_POINT('Ctrl Pts',(42.2717082595868,-74.0397965552843,
-216.80097680921));
#220217=CARTESIAN_POINT('Ctrl Pts',(42.2605717445896,-74.0426065375714,
-216.80003328781));
#220218=CARTESIAN_POINT('Ctrl Pts',(42.2492868609298,-74.0454417000548,
-216.799061210825));
#220219=CARTESIAN_POINT('Ctrl Pts',(42.2476466472937,-74.0458537798162,
-216.798919923243));
#220220=CARTESIAN_POINT('Ctrl Pts',(42.2459714240578,-74.0462743143251,
-216.79877538963));
#220221=CARTESIAN_POINT('Ctrl Pts',(42.2442753061012,-74.0466997068187,
-216.798628821829));
#220222=CARTESIAN_POINT('Ctrl Pts',(42.2343019113844,-74.0492010701416,
-216.797766984048));
#220223=CARTESIAN_POINT('Ctrl Pts',(42.2235917525255,-74.0518770861086,
-216.796829303334));
#220224=CARTESIAN_POINT('Ctrl Pts',(42.2149915568324,-74.0540196533554,
-216.796068609183));
#220225=CARTESIAN_POINT('Ctrl Pts',(42.1706803715226,-74.0650589014953,
-216.79214924959));
#220226=CARTESIAN_POINT('Ctrl Pts',(42.1275668081456,-74.0756321880183,
-216.788126946768));
#220227=CARTESIAN_POINT('Ctrl Pts',(42.0856601792248,-74.0857924220622,
-216.783988160757));
#220228=CARTESIAN_POINT('Ctrl Pts',(42.0514330282735,-74.0940907718287,
-216.780607815995));
#220229=CARTESIAN_POINT('Ctrl Pts',(42.0180116994635,-74.1021132445813,
-216.777150281193));
#220230=CARTESIAN_POINT('Ctrl Pts',(41.9854208969419,-74.1098785765232,
-216.773621645226));
#220231=CARTESIAN_POINT('Ctrl Pts',(41.9491739275612,-74.1185150545277,
-216.769697152734));
#220232=CARTESIAN_POINT('Ctrl Pts',(41.9139454439493,-74.1268379755528,
-216.765680926037));
#220233=CARTESIAN_POINT('Ctrl Pts',(41.8797446980124,-74.1348830668482,
-216.76157559263));
#220234=CARTESIAN_POINT('Ctrl Pts',(41.8636268779551,-74.1386744851431,
-216.759640868012));
#220235=CARTESIAN_POINT('Ctrl Pts',(41.8477367980506,-74.1424044857841,
-216.757686077121));
#220236=CARTESIAN_POINT('Ctrl Pts',(41.8320763341616,-74.1460759416482,
-216.755712418611));
#220237=CARTESIAN_POINT('Ctrl Pts',(41.8311216619832,-74.1462997560124,
-216.75559210309));
#220238=CARTESIAN_POINT('Ctrl Pts',(41.8301678262242,-74.1465233676039,
-216.755471711903));
#220239=CARTESIAN_POINT('Ctrl Pts',(41.8292148259921,-74.146746777301,-216.755351244198));
#220240=CARTESIAN_POINT('Ctrl Pts',(41.8209218072531,-74.1486908909979,
-216.754302932876));
#220241=CARTESIAN_POINT('Ctrl Pts',(41.8126931811236,-74.150619097667,-216.753249433925));
#220242=CARTESIAN_POINT('Ctrl Pts',(41.8045289047161,-74.1525319178485,
-216.752190218595));
#220243=CARTESIAN_POINT('Ctrl Pts',(41.7971876354883,-74.154251914482,-216.751237778412));
#220244=CARTESIAN_POINT('Ctrl Pts',(41.7908759595339,-74.155730666367,-216.750410022281));
#220245=CARTESIAN_POINT('Ctrl Pts',(41.7829568743593,-74.1575858560275,
-216.749357771845));
#220246=CARTESIAN_POINT('Ctrl Pts',(41.7820690900058,-74.157793835651,-216.749239807276));
#220247=CARTESIAN_POINT('Ctrl Pts',(41.7811610687575,-74.1580065539296,
-216.749118981173));
#220248=CARTESIAN_POINT('Ctrl Pts',(41.780229065532,-74.158224887783,-216.748994768089));
#220249=CARTESIAN_POINT('Ctrl Pts',(41.7432469728695,-74.166888423037,-216.74406596565));
#220250=CARTESIAN_POINT('Ctrl Pts',(41.7064247994052,-74.1755267166944,
-216.738833576768));
#220251=CARTESIAN_POINT('Ctrl Pts',(41.6698363362772,-74.1841324671723,
-216.733270467841));
#220252=CARTESIAN_POINT('Ctrl Pts',(41.6357861761109,-74.1921411988071,
-216.728093296301));
#220253=CARTESIAN_POINT('Ctrl Pts',(41.6019383182243,-74.2001218266649,
-216.722629698114));
#220254=CARTESIAN_POINT('Ctrl Pts',(41.5683888997643,-74.2080560005233,
-216.716887710817));
#220255=CARTESIAN_POINT('Ctrl Pts',(41.5658879250897,-74.208647461383,-216.716459668678));
#220256=CARTESIAN_POINT('Ctrl Pts',(41.5633886271414,-74.2092386577173,
-216.716030094091));
#220257=CARTESIAN_POINT('Ctrl Pts',(41.5608910547313,-74.209829578775,-216.715598997537));
#220258=CARTESIAN_POINT('Ctrl Pts',(41.5248897036665,-74.218347432497,-216.709384940102));
#220259=CARTESIAN_POINT('Ctrl Pts',(41.4892213917955,-74.2268154997241,
-216.702847269723));
#220260=CARTESIAN_POINT('Ctrl Pts',(41.4539047110238,-74.2352388213443,
-216.695991911182));
#220261=CARTESIAN_POINT('Ctrl Pts',(41.436246370638,-74.2394504821544,-216.692564231912));
#220262=CARTESIAN_POINT('Ctrl Pts',(41.4186759422659,-74.2436510576244,
-216.689057198583));
#220263=CARTESIAN_POINT('Ctrl Pts',(41.4011954472694,-74.2478417983752,
-216.685471738462));
#220264=CARTESIAN_POINT('Ctrl Pts',(41.3997093795187,-74.2481980654421,
-216.685166928062));
#220265=CARTESIAN_POINT('Ctrl Pts',(41.3982239689329,-74.248554247276,-216.684861570055));
#220266=CARTESIAN_POINT('Ctrl Pts',(41.3967391882741,-74.2489103603681,
-216.684555646867));
#220267=CARTESIAN_POINT('Ctrl Pts',(41.3894912914141,-74.2506487120545,
-216.683062295171));
#220268=CARTESIAN_POINT('Ctrl Pts',(41.3822589060392,-74.2523842115382,
-216.681553953867));
#220269=CARTESIAN_POINT('Ctrl Pts',(41.3750419560604,-74.2541173315647,
-216.680030625044));
#220270=CARTESIAN_POINT('Ctrl Pts',(41.3706942605806,-74.2551614122536,
-216.679112928531));
#220271=CARTESIAN_POINT('Ctrl Pts',(41.3663519670483,-74.2562081204571,
-216.678184906664));
#220272=CARTESIAN_POINT('Ctrl Pts',(41.3620153797659,-74.2572535870782,
-216.677252080092));
#220273=CARTESIAN_POINT('Ctrl Pts',(41.3597115677721,-74.2578089912207,
-216.676756515976));
#220274=CARTESIAN_POINT('Ctrl Pts',(41.357083273891,-74.2584426661523,-216.67618918604));
#220275=CARTESIAN_POINT('Ctrl Pts',(41.3546498070752,-74.2590293918546,
-216.675661945151));
#220276=CARTESIAN_POINT('Ctrl Pts',(41.3534710965864,-74.2593135871167,
-216.675406562845));
#220277=CARTESIAN_POINT('Ctrl Pts',(41.3523381619096,-74.2595867503155,
-216.675160651369));
#220278=CARTESIAN_POINT('Ctrl Pts',(41.3513103446013,-74.2598345701721,
-216.674937249552));
#220279=CARTESIAN_POINT('Ctrl Pts',(41.3507823355832,-74.2599618798779,
-216.674822483851));
#220280=CARTESIAN_POINT('Ctrl Pts',(41.3502820707845,-74.2600825005792,
-216.67471366168));
#220281=CARTESIAN_POINT('Ctrl Pts',(41.3498176099809,-74.260194488636,-216.674612565794));
#220282=CARTESIAN_POINT('Ctrl Pts',(41.3495507065253,-74.2602588428271,
-216.674554470813));
#220283=CARTESIAN_POINT('Ctrl Pts',(41.349295626601,-74.2603203462675,-216.6744989274));
#220284=CARTESIAN_POINT('Ctrl Pts',(41.3490539004976,-74.2603786299418,
-216.674446274729));
#220285=CARTESIAN_POINT('Ctrl Pts',(41.3488409954975,-74.2604299644295,
-216.674399899858));
#220286=CARTESIAN_POINT('Ctrl Pts',(41.3486297325562,-74.26048090302,-216.674353868862));
#220287=CARTESIAN_POINT('Ctrl Pts',(41.3484171089924,-74.260532169689,-216.674307527587));
#220288=CARTESIAN_POINT('Ctrl Pts',(41.332256670365,-74.2644286891677,-216.670785362304));
#220289=CARTESIAN_POINT('Ctrl Pts',(41.313866979032,-74.2688638131955,-216.666696381376));
#220290=CARTESIAN_POINT('Ctrl Pts',(41.2933719087617,-74.2737953734653,
-216.662018990123));
#220291=CARTESIAN_POINT('Ctrl Pts',(41.2715055234229,-74.2790569020066,
-216.657028636922));
#220292=CARTESIAN_POINT('Ctrl Pts',(41.2472462603474,-74.2848832608977,
-216.651368281838));
#220293=CARTESIAN_POINT('Ctrl Pts',(41.2207831869297,-74.2911945272362,
-216.645041682585));
#220294=CARTESIAN_POINT('Ctrl Pts',(41.2075516502209,-74.2943501604055,
-216.641878382958));
#220295=CARTESIAN_POINT('Ctrl Pts',(41.193769728485,-74.2976265312604,-216.638549076509));
#220296=CARTESIAN_POINT('Ctrl Pts',(41.1794634363018,-74.3010106466872,
-216.635057733616));
#220297=CARTESIAN_POINT('Ctrl Pts',(41.175886863256,-74.3018566755439,-216.634184897892));
#220298=CARTESIAN_POINT('Ctrl Pts',(41.1722775197716,-74.3027094288298,
-216.633301946298));
#220299=CARTESIAN_POINT('Ctrl Pts',(41.1686358540257,-74.303568675218,-216.632408973159));
#220300=CARTESIAN_POINT('Ctrl Pts',(41.1678188235789,-74.3037614525099,
-216.63220862906));
#220301=CARTESIAN_POINT('Ctrl Pts',(41.1670023237384,-74.3039540472148,
-216.632008309053));
#220302=CARTESIAN_POINT('Ctrl Pts',(41.166193024558,-74.3041448868624,-216.631809653647));
#220303=CARTESIAN_POINT('Ctrl Pts',(41.1561807058362,-74.3065058769922,
-216.629351970152));
#220304=CARTESIAN_POINT('Ctrl Pts',(41.146902295185,-74.3086873866522,-216.627062103609));
#220305=CARTESIAN_POINT('Ctrl Pts',(41.1349991103359,-74.3114709450446,
-216.624104235142));
#220306=CARTESIAN_POINT('Ctrl Pts',(41.1124558837132,-74.316742675968,-216.618502381518));
#220307=CARTESIAN_POINT('Ctrl Pts',(41.0914762557644,-74.3215964004882,
-216.61322223478));
#220308=CARTESIAN_POINT('Ctrl Pts',(41.0720298933579,-74.3260478784422,
-216.608296677193));
#220309=CARTESIAN_POINT('Ctrl Pts',(41.0490622752251,-74.3313054090608,
-216.602479222835));
#220310=CARTESIAN_POINT('Ctrl Pts',(41.0282329838513,-74.3360021895108,
-216.597156269549));
#220311=CARTESIAN_POINT('Ctrl Pts',(41.009435971611,-74.3401861457994,-216.59233766627));
#220312=CARTESIAN_POINT('Ctrl Pts',(40.9866694566912,-74.3452536587665,
-216.586501483263));
#220313=CARTESIAN_POINT('Ctrl Pts',(40.9668825400494,-74.3495699488692,
-216.581404474632));
#220314=CARTESIAN_POINT('Ctrl Pts',(40.9498286058995,-74.3532377994501,
-216.577010383348));
#220315=CARTESIAN_POINT('Ctrl Pts',(40.9393802972515,-74.355484954541,-216.574318287696));
#220316=CARTESIAN_POINT('Ctrl Pts',(40.9299569023606,-74.357488938127,-216.571889095025));
#220317=CARTESIAN_POINT('Ctrl Pts',(40.9214983001327,-74.359273049609,-216.56970926278));
#220318=CARTESIAN_POINT('Ctrl Pts',(42.378985830374,-74.0076928996301,-216.816073769133));
#220319=CARTESIAN_POINT('Ctrl Pts',(42.0789070994075,-75.1309710808869,
-215.501557062395));
#220320=CARTESIAN_POINT('Ctrl Pts',(41.6783348544084,-75.1653401212506,
-213.793428390226));
#220321=CARTESIAN_POINT('Ctrl Pts',(42.695627452923,-73.9307974382047,-216.831927633052));
#220322=CARTESIAN_POINT('Ctrl Pts',(42.436365014004,-75.113727280111,-215.499981515909));
#220323=CARTESIAN_POINT('Ctrl Pts',(42.0353813628522,-75.1619567754401,
-213.74615836671));
#220324=CARTESIAN_POINT('Ctrl Pts',(42.9815174465389,-73.8601470375395,
-216.832053666316));
#220325=CARTESIAN_POINT('Ctrl Pts',(42.7754409185831,-75.0814850954717,
-215.487452688235));
#220326=CARTESIAN_POINT('Ctrl Pts',(42.390949946975,-75.141795992121,-213.701832784708));
#220327=CARTESIAN_POINT('Ctrl Pts',(43.472508493266,-73.7123523458651,-216.83864882647));
#220328=CARTESIAN_POINT('Ctrl Pts',(43.3576044403188,-74.9997256985912,
-215.473802374509));
#220329=CARTESIAN_POINT('Ctrl Pts',(42.9950456425551,-75.0789259129395,
-213.631395393593));
#220330=CARTESIAN_POINT('Ctrl Pts',(43.6784848417686,-73.6416002218129,
-216.843674394851));
#220331=CARTESIAN_POINT('Ctrl Pts',(43.6010750190848,-74.9575939227159,
-215.470830714392));
#220332=CARTESIAN_POINT('Ctrl Pts',(43.2442829554274,-75.0445859118627,
-213.603599246343));
#220333=CARTESIAN_POINT('Ctrl Pts',(44.0840990697417,-73.4894561004303,
-216.851382274181));
#220334=CARTESIAN_POINT('Ctrl Pts',(44.0850213450697,-74.8573500503074,
-215.464209987895));
#220335=CARTESIAN_POINT('Ctrl Pts',(43.7407999450918,-74.95923489871,-213.549700262593));
#220336=CARTESIAN_POINT('Ctrl Pts',(44.2823423460514,-73.4093259654149,
-216.853445535287));
#220337=CARTESIAN_POINT('Ctrl Pts',(44.3244805372772,-74.7994341803878,
-215.459998179187));
#220338=CARTESIAN_POINT('Ctrl Pts',(43.9880896419911,-74.9082283395985,
-213.523624316504));
#220339=CARTESIAN_POINT('Ctrl Pts',(44.6663395277273,-73.2455758099323,
-216.853514051937));
#220340=CARTESIAN_POINT('Ctrl Pts',(44.7957647856255,-74.6691872475075,
-215.448954698364));
#220341=CARTESIAN_POINT('Ctrl Pts',(44.4808857844433,-74.7891870797359,
-213.473791302964));
#220342=CARTESIAN_POINT('Ctrl Pts',(44.8545941767413,-73.160040525945,-216.852689496172));
#220343=CARTESIAN_POINT('Ctrl Pts',(45.0293409228867,-74.5964823667737,
-215.443148236746));
#220344=CARTESIAN_POINT('Ctrl Pts',(44.7267891898549,-74.721020944827,-213.450088190065));
#220345=CARTESIAN_POINT('Ctrl Pts',(45.1403300017806,-73.0164913703724,
-216.854408324069));
#220346=CARTESIAN_POINT('Ctrl Pts',(45.3818326897387,-74.4739715465294,
-215.437873869065));
#220347=CARTESIAN_POINT('Ctrl Pts',(45.0928291473828,-74.6060271525094,
-213.416036405783));
#220348=CARTESIAN_POINT('Ctrl Pts',(45.2374002351368,-72.9646875296883,
-216.856056355454));
#220349=CARTESIAN_POINT('Ctrl Pts',(45.5006825021446,-74.4305046217021,
-215.437245699608));
#220350=CARTESIAN_POINT('Ctrl Pts',(45.214226071449,-74.5656241151966,-213.404928397068));
#220351=CARTESIAN_POINT('Ctrl Pts',(45.4284787286636,-72.8598153097967,
-216.858166103866));
#220352=CARTESIAN_POINT('Ctrl Pts',(45.7360618860342,-74.3398903326153,
-215.435132674419));
#220353=CARTESIAN_POINT('Ctrl Pts',(45.4557176198574,-74.4806914809447,
-213.382939645023));
#220354=CARTESIAN_POINT('Ctrl Pts',(45.5194683717665,-72.8099576191881,
-216.85739628503));
#220355=CARTESIAN_POINT('Ctrl Pts',(45.8503038319864,-74.2936199432179,
-215.432466908975));
#220356=CARTESIAN_POINT('Ctrl Pts',(45.5757446359314,-74.4361813329111,
-213.372122623236));
#220357=CARTESIAN_POINT('Ctrl Pts',(45.7858192096191,-72.661331939478,-216.853747605829));
#220358=CARTESIAN_POINT('Ctrl Pts',(46.1875371987659,-74.1507296656985,
-215.423451267174));
#220359=CARTESIAN_POINT('Ctrl Pts',(45.9328087573252,-74.2968675255568,
-213.340776903284));
#220360=CARTESIAN_POINT('Ctrl Pts',(45.9533357768491,-72.5652157418087,
-216.849067911601));
#220361=CARTESIAN_POINT('Ctrl Pts',(46.4038103241023,-74.0507287717429,
-215.415634323609));
#220362=CARTESIAN_POINT('Ctrl Pts',(46.1672258662471,-74.1961452862636,
-213.321432015392));
#220363=CARTESIAN_POINT('Ctrl Pts',(46.2126944376478,-72.3997852941367,
-216.847762456798));
#220364=CARTESIAN_POINT('Ctrl Pts',(46.7326853185615,-73.8858310589856,
-215.40996726368));
#220365=CARTESIAN_POINT('Ctrl Pts',(46.5133864112302,-74.0333951638931,
-213.294382252724));
#220366=CARTESIAN_POINT('Ctrl Pts',(46.3017762942777,-72.3394642981084,
-216.848685723507));
#220367=CARTESIAN_POINT('Ctrl Pts',(46.8441430626577,-73.827734396332,-215.409501019432));
#220368=CARTESIAN_POINT('Ctrl Pts',(46.6278478339237,-73.9772067981799,
-213.285618874283));
#220369=CARTESIAN_POINT('Ctrl Pts',(46.4779428408734,-72.2168840934957,
-216.849684972937));
#220370=CARTESIAN_POINT('Ctrl Pts',(47.0649879674724,-73.7078522436265,
-215.407953880452));
#220371=CARTESIAN_POINT('Ctrl Pts',(46.854860842577,-73.860987309113,-213.268274976754));
#220372=CARTESIAN_POINT('Ctrl Pts',(46.563987673213,-72.1558719051303,-216.84929201614));
#220373=CARTESIAN_POINT('Ctrl Pts',(47.1735256569728,-73.6464646449198,
-215.406402005381));
#220374=CARTESIAN_POINT('Ctrl Pts',(46.9674078998239,-73.8009605735783,
-213.259666405972));
#220375=CARTESIAN_POINT('Ctrl Pts',(46.6792210572178,-72.0788709964896,
-216.844067134084));
#220376=CARTESIAN_POINT('Ctrl Pts',(47.3251236075319,-73.5574882456331,
-215.399499935695));
#220377=CARTESIAN_POINT('Ctrl Pts',(47.1348908421815,-73.7079618268763,
-213.247450860241));
#220378=CARTESIAN_POINT('Ctrl Pts',(46.7161187190905,-72.054648443314,-216.841899297837));
#220379=CARTESIAN_POINT('Ctrl Pts',(47.3744063047614,-73.5280295183312,
-215.39678689924));
#220380=CARTESIAN_POINT('Ctrl Pts',(47.1904997834325,-73.6764658823414,
-213.243519901449));
#220381=CARTESIAN_POINT('Ctrl Pts',(46.7914227504076,-72.0034439643619,
-216.838436648525));
#220382=CARTESIAN_POINT('Ctrl Pts',(47.4739959337873,-73.4674961130268,
-215.392271721982));
#220383=CARTESIAN_POINT('Ctrl Pts',(47.3012779793222,-73.6124762223558,
-213.23594003108));
#220384=CARTESIAN_POINT('Ctrl Pts',(46.8291605334885,-71.9772975723057,
-216.836877529182));
#220385=CARTESIAN_POINT('Ctrl Pts',(47.5237795851717,-73.4367153932032,
-215.390203908609));
#220386=CARTESIAN_POINT('Ctrl Pts',(47.3564465383167,-73.5799829806061,
-213.232287185903));
#220387=CARTESIAN_POINT('Ctrl Pts',(47.0047959981998,-71.8539654157978,
-216.829930772006));
#220388=CARTESIAN_POINT('Ctrl Pts',(47.7552986345005,-73.2910829611759,
-215.380974273969));
#220389=CARTESIAN_POINT('Ctrl Pts',(47.6127233872645,-73.4260937179139,
-213.215858918559));
#220390=CARTESIAN_POINT('Ctrl Pts',(47.1416754793996,-71.7530639275421,
-216.825332946412));
#220391=CARTESIAN_POINT('Ctrl Pts',(47.9349954979552,-73.1707886047709,
-215.374842476235));
#220392=CARTESIAN_POINT('Ctrl Pts',(47.8110561400091,-73.2984848189965,
-213.204657242929));
#220393=CARTESIAN_POINT('Ctrl Pts',(47.2645314954405,-71.6680428481242,
-216.815412755198));
#220394=CARTESIAN_POINT('Ctrl Pts',(48.1016743030229,-73.0519933533766,
-215.363909661586));
#220395=CARTESIAN_POINT('Ctrl Pts',(48.0063773132287,-73.1639317249219,
-213.195676583529));
#220396=CARTESIAN_POINT('',(47.0905557676078,-71.7934728593479,-216.824560386716));
#220397=CARTESIAN_POINT('',(47.738383176916,-73.3429891884109,-213.20923907124));
#220398=CARTESIAN_POINT('Origin',(45.0170666017296,-69.1493247484068,-213.121977039054));
#220399=CARTESIAN_POINT('Ctrl Pts',(41.9926628230251,-75.158015320487,-213.752528187964));
#220400=CARTESIAN_POINT('Ctrl Pts',(42.2254656098299,-75.1493651193979,
-213.722768055243));
#220401=CARTESIAN_POINT('Ctrl Pts',(42.4681215167616,-75.1331685973929,
-213.693142558933));
#220402=CARTESIAN_POINT('Ctrl Pts',(42.7199965340293,-75.1075199128603,
-213.663651669654));
#220403=CARTESIAN_POINT('Ctrl Pts',(42.7283364387217,-75.1066706520372,
-213.662675188507));
#220404=CARTESIAN_POINT('Ctrl Pts',(42.7366864637874,-75.105811021856,-213.661698964705));
#220405=CARTESIAN_POINT('Ctrl Pts',(42.7450465875749,-75.1049409518136,
-213.660723025752));
#220406=CARTESIAN_POINT('Ctrl Pts',(42.8629292927521,-75.092672448034,-213.646961707528));
#220407=CARTESIAN_POINT('Ctrl Pts',(42.9828102619913,-75.0783292984929,
-213.633222439322));
#220408=CARTESIAN_POINT('Ctrl Pts',(43.1046068311246,-75.061707483384,-213.619516336771));
#220409=CARTESIAN_POINT('Ctrl Pts',(43.1698239612476,-75.0528071745612,
-213.61217727394));
#220410=CARTESIAN_POINT('Ctrl Pts',(43.2355897416449,-75.0432535660333,
-213.60484662163));
#220411=CARTESIAN_POINT('Ctrl Pts',(43.3018892782285,-75.0330153825397,
-213.597524382064));
#220412=CARTESIAN_POINT('Ctrl Pts',(43.3350390465203,-75.0278962907928,
-213.593863262281));
#220413=CARTESIAN_POINT('Ctrl Pts',(43.3683222534951,-75.0226060529535,
-213.590204245643));
#220414=CARTESIAN_POINT('Ctrl Pts',(43.4017369013796,-75.0171407709502,
-213.586547333187));
#220415=CARTESIAN_POINT('Ctrl Pts',(43.4257091389091,-75.0132198845532,
-213.583923801904));
#220416=CARTESIAN_POINT('Ctrl Pts',(43.4506713130679,-75.0090536411257,
-213.581201064996));
#220417=CARTESIAN_POINT('Ctrl Pts',(43.4746375299073,-75.0049733307183,
-213.578595150767));
#220418=CARTESIAN_POINT('Ctrl Pts',(43.4806793653705,-75.003944692603,-213.577938204988));
#220419=CARTESIAN_POINT('Ctrl Pts',(43.4866579344334,-75.0029217746917,
-213.577288656496));
#220420=CARTESIAN_POINT('Ctrl Pts',(43.492541479833,-75.0019103973164,-213.576649914173));
#220421=CARTESIAN_POINT('Ctrl Pts',(43.4958506536986,-75.001341552623,-213.576290656402));
#220422=CARTESIAN_POINT('Ctrl Pts',(43.4991297695187,-75.0007763630848,
-213.575934821562));
#220423=CARTESIAN_POINT('Ctrl Pts',(43.5023731804519,-75.0002158902631,
-213.575583015162));
#220424=CARTESIAN_POINT('Ctrl Pts',(43.6789624549774,-74.9697006422707,
-213.556428724122));
#220425=CARTESIAN_POINT('Ctrl Pts',(43.8536594409741,-74.9352051779825,
-213.537945346085));
#220426=CARTESIAN_POINT('Ctrl Pts',(44.0262846068755,-74.8969298990303,
-213.5201354507));
#220427=CARTESIAN_POINT('Ctrl Pts',(44.0960369712285,-74.8814640705733,
-213.512939035824));
#220428=CARTESIAN_POINT('Ctrl Pts',(44.1654511141014,-74.8653816412826,
-213.505852312176));
#220429=CARTESIAN_POINT('Ctrl Pts',(44.2345154218962,-74.8486979706476,
-213.498874379054));
#220430=CARTESIAN_POINT('Ctrl Pts',(44.2414195724209,-74.8470301544189,
-213.498176816127));
#220431=CARTESIAN_POINT('Ctrl Pts',(44.2483205387897,-74.8453562275326,
-213.497480382308));
#220432=CARTESIAN_POINT('Ctrl Pts',(44.2552182767284,-74.8436762135253,
-213.496785065357));
#220433=CARTESIAN_POINT('Ctrl Pts',(44.3785490214338,-74.8136377602704,
-213.484352879892));
#220434=CARTESIAN_POINT('Ctrl Pts',(44.5007688078792,-74.7816740241074,
-213.472271040558));
#220435=CARTESIAN_POINT('Ctrl Pts',(44.6218268047523,-74.7478698888918,
-213.460539666428));
#220436=CARTESIAN_POINT('Ctrl Pts',(44.6823558031889,-74.730967821284,-213.454673979364));
#220437=CARTESIAN_POINT('Ctrl Pts',(44.7425943156762,-74.7136054349217,
-213.448895904716));
#220438=CARTESIAN_POINT('Ctrl Pts',(44.8025361239107,-74.6957920070001,
-213.443205432122));
#220439=CARTESIAN_POINT('Ctrl Pts',(44.832507028028,-74.6868852930393,-213.440360195825));
#220440=CARTESIAN_POINT('Ctrl Pts',(44.862403752144,-74.6778658069359,-213.437536859826));
#220441=CARTESIAN_POINT('Ctrl Pts',(44.8922255056854,-74.6687346377144,
-213.434735421505));
#220442=CARTESIAN_POINT('Ctrl Pts',(44.9071363824561,-74.6641690531036,
-213.433334702345));
#220443=CARTESIAN_POINT('Ctrl Pts',(44.9220285163037,-74.659575547045,-213.431939457592));
#220444=CARTESIAN_POINT('Ctrl Pts',(44.9369018081516,-74.6549542512991,
-213.430549686832));
#220445=CARTESIAN_POINT('Ctrl Pts',(44.9443384540756,-74.6526436034261,
-213.429854801452));
#220446=CARTESIAN_POINT('Ctrl Pts',(44.951770389481,-74.6503260080913,-213.42916128457));
#220447=CARTESIAN_POINT('Ctrl Pts',(44.9591976019665,-74.648001481498,-213.428469136128));
#220448=CARTESIAN_POINT('Ctrl Pts',(44.9632239542959,-74.6467413367153,
-213.428093916826));
#220449=CARTESIAN_POINT('Ctrl Pts',(44.9669164143748,-74.6455834371407,
-213.42775004086));
#220450=CARTESIAN_POINT('Ctrl Pts',(44.9708158520873,-74.6443584060741,
-213.427387164341));
#220451=CARTESIAN_POINT('Ctrl Pts',(44.9741095137599,-74.6433236830783,
-213.427080660539));
#220452=CARTESIAN_POINT('Ctrl Pts',(44.9775507366128,-74.6422410785831,
-213.426760598811));
#220453=CARTESIAN_POINT('Ctrl Pts',(44.9814650631701,-74.6410071371356,
-213.426396801056));
#220454=CARTESIAN_POINT('Ctrl Pts',(45.1029661757967,-74.6027054633773,
-213.415104480054));
#220455=CARTESIAN_POINT('Ctrl Pts',(45.2207505984801,-74.5633287619067,
-213.404380114071));
#220456=CARTESIAN_POINT('Ctrl Pts',(45.3349856468011,-74.5231510781069,
-213.394033506047));
#220457=CARTESIAN_POINT('Ctrl Pts',(45.4338636380008,-74.4883746349437,
-213.385077832353));
#220458=CARTESIAN_POINT('Ctrl Pts',(45.5300341549536,-74.4530118326486,
-213.376452280864));
#220459=CARTESIAN_POINT('Ctrl Pts',(45.6234911871441,-74.4172713854539,
-213.368201767278));
#220460=CARTESIAN_POINT('Ctrl Pts',(45.647438567939,-74.4081132720548,-213.366087660015));
#220461=CARTESIAN_POINT('Ctrl Pts',(45.6712079590872,-74.3989302024541,
-213.363998049609));
#220462=CARTESIAN_POINT('Ctrl Pts',(45.6947996061161,-74.3897253635627,
-213.361933438076));
#220463=CARTESIAN_POINT('Ctrl Pts',(45.7122545962654,-74.3829148864485,
-213.36040587309));
#220464=CARTESIAN_POINT('Ctrl Pts',(45.7296144252457,-74.3760917616531,
-213.358892409563));
#220465=CARTESIAN_POINT('Ctrl Pts',(45.7468800576082,-74.3692569240176,
-213.35739252679));
#220466=CARTESIAN_POINT('Ctrl Pts',(45.8653228670678,-74.3223697116205,
-213.347103281331));
#220467=CARTESIAN_POINT('Ctrl Pts',(45.9792491168717,-74.2749665555787,
-213.337419776965));
#220468=CARTESIAN_POINT('Ctrl Pts',(46.0887466065047,-74.227432345403,-213.328341976054));
#220469=CARTESIAN_POINT('Ctrl Pts',(46.1434953513212,-74.2036652403152,
-213.323803075599));
#220470=CARTESIAN_POINT('Ctrl Pts',(46.1971371799208,-74.1798649863958,
-213.319415602941));
#220471=CARTESIAN_POINT('Ctrl Pts',(46.2496845193491,-74.1560772358378,
-213.315179562423));
#220472=CARTESIAN_POINT('Ctrl Pts',(46.2759581890632,-74.1441833605588,
-213.313061542164));
#220473=CARTESIAN_POINT('Ctrl Pts',(46.3019582288627,-74.1322925940271,
-213.310981379613));
#220474=CARTESIAN_POINT('Ctrl Pts',(46.3276862909874,-74.1204104680073,
-213.308939076144));
#220475=CARTESIAN_POINT('Ctrl Pts',(46.3405503220498,-74.1144694049973,
-213.307917924409));
#220476=CARTESIAN_POINT('Ctrl Pts',(46.3533463581902,-74.1085305009325,
-213.306906237422));
#220477=CARTESIAN_POINT('Ctrl Pts',(46.3660746062855,-74.1025944385409,
-213.305904015303));
#220478=CARTESIAN_POINT('Ctrl Pts',(46.3724387303331,-74.0996264073452,
-213.305402904244));
#220479=CARTESIAN_POINT('Ctrl Pts',(46.3787859073362,-74.0966590864933,
-213.3049041594));
#220480=CARTESIAN_POINT('Ctrl Pts',(46.3851161634271,-74.0936925606538,
-213.304407780787));
#220481=CARTESIAN_POINT('Ctrl Pts',(46.3882812914726,-74.0922092977341,
-213.304159591481));
#220482=CARTESIAN_POINT('Ctrl Pts',(46.3914421892879,-74.0907262335627,
-213.303911993733));
#220483=CARTESIAN_POINT('Ctrl Pts',(46.3945988601571,-74.0892433786806,
-213.303664987544));
#220484=CARTESIAN_POINT('Ctrl Pts',(46.3958585478266,-74.0886516369096,
-213.303566418304));
#220485=CARTESIAN_POINT('Ctrl Pts',(46.3969087996539,-74.0881580320819,
-213.303484260743));
#220486=CARTESIAN_POINT('Ctrl Pts',(46.3979995769197,-74.0876451955363,
-213.303398971659));
#220487=CARTESIAN_POINT('Ctrl Pts',(46.3996421953226,-74.0868729070281,
-213.303270533503));
#220488=CARTESIAN_POINT('Ctrl Pts',(46.401376773792,-74.0860571311396,-213.303134964987));
#220489=CARTESIAN_POINT('Ctrl Pts',(46.4040561947953,-74.0847954504982,
-213.30292574716));
#220490=CARTESIAN_POINT('Ctrl Pts',(46.5066049547341,-74.0365074864015,
-213.294918409471));
#220491=CARTESIAN_POINT('Ctrl Pts',(46.6048557467194,-73.9883693144774,
-213.28738335352));
#220492=CARTESIAN_POINT('Ctrl Pts',(46.6989248687914,-73.9407068034154,
-213.280190704557));
#220493=CARTESIAN_POINT('Ctrl Pts',(46.7131637398907,-73.9334923175529,
-213.27910198172));
#220494=CARTESIAN_POINT('Ctrl Pts',(46.7273067980788,-73.9262886830176,
-213.278021188919));
#220495=CARTESIAN_POINT('Ctrl Pts',(46.7413544421108,-73.9190969799375,
-213.276947964261));
#220496=CARTESIAN_POINT('Ctrl Pts',(46.8219064532499,-73.877858310642,-213.270793878609));
#220497=CARTESIAN_POINT('Ctrl Pts',(46.8993200983177,-73.8370145004555,
-213.264878976843));
#220498=CARTESIAN_POINT('Ctrl Pts',(46.9736981082125,-73.7967395376575,
-213.259314339676));
#220499=CARTESIAN_POINT('Ctrl Pts',(47.0095207926616,-73.7773419054064,
-213.256634243213));
#220500=CARTESIAN_POINT('Ctrl Pts',(47.0446390884701,-73.7580761615461,
-213.254034615544));
#220501=CARTESIAN_POINT('Ctrl Pts',(47.0790632952255,-73.7389613310804,
-213.25152381406));
#220502=CARTESIAN_POINT('Ctrl Pts',(47.1365946196497,-73.7070157434696,
-213.247327646642));
#220503=CARTESIAN_POINT('Ctrl Pts',(47.1921917917575,-73.6754884956987,
-213.243405092136));
#220504=CARTESIAN_POINT('Ctrl Pts',(47.2458889523972,-73.6444709939159,
-213.239730824515));
#220505=CARTESIAN_POINT('Ctrl Pts',(47.3032098578872,-73.6113602806669,
-213.235808599493));
#220506=CARTESIAN_POINT('Ctrl Pts',(47.3583648958864,-73.5788310316487,
-213.232164844058));
#220507=CARTESIAN_POINT('Ctrl Pts',(47.4113921142577,-73.546989220601,-213.228765490142));
#220508=CARTESIAN_POINT('Ctrl Pts',(47.5006757254644,-73.4933761523499,
-213.223041890023));
#220509=CARTESIAN_POINT('Ctrl Pts',(47.5839277861292,-73.4417153369978,
-213.218003707915));
#220510=CARTESIAN_POINT('Ctrl Pts',(47.6613227244206,-73.3924652818581,
-213.213567309774));
#220511=CARTESIAN_POINT('Ctrl Pts',(47.6876873451025,-73.3756882283325,
-213.212056048744));
#220512=CARTESIAN_POINT('Ctrl Pts',(47.7133720810526,-73.3591905530428,
-213.210614503331));
#220513=CARTESIAN_POINT('Ctrl Pts',(47.7383831769159,-73.3429891884108,
-213.20923907124));
#220514=CARTESIAN_POINT('Ctrl Pts',(47.0905557676078,-71.7934728593479,
-216.824560386716));
#220515=CARTESIAN_POINT('Ctrl Pts',(47.0153154861726,-71.8474340839192,
-216.828160153995));
#220516=CARTESIAN_POINT('Ctrl Pts',(46.9368040133168,-71.9030117484293,
-216.831773097603));
#220517=CARTESIAN_POINT('Ctrl Pts',(46.8105116370282,-71.9908582593833,
-216.837212277512));
#220518=CARTESIAN_POINT('Ctrl Pts',(46.7669927040833,-72.020887478965,-216.839028631564));
#220519=CARTESIAN_POINT('Ctrl Pts',(46.6991242326024,-72.0673122522426,
-216.841758103766));
#220520=CARTESIAN_POINT('Ctrl Pts',(46.6760717227842,-72.0830169115032,
-216.842668751354));
#220521=CARTESIAN_POINT('Ctrl Pts',(46.6407809462547,-72.106953442936,-216.844035958017));
#220522=CARTESIAN_POINT('Ctrl Pts',(46.6199834046119,-72.121027909888,-216.844833855528));
#220523=CARTESIAN_POINT('Ctrl Pts',(46.5987769248733,-72.1353112488642,
-216.845632383546));
#220524=CARTESIAN_POINT('Ctrl Pts',(46.5865515833884,-72.1435268361654,
-216.846088839681));
#220525=CARTESIAN_POINT('Ctrl Pts',(46.5819665060498,-72.1466049757675,
-216.846259389817));
#220526=CARTESIAN_POINT('Ctrl Pts',(46.555537766819,-72.1643384243489,-216.847240570889));
#220527=CARTESIAN_POINT('Ctrl Pts',(46.5231938316714,-72.1867724289952,
-216.847819543089));
#220528=CARTESIAN_POINT('Ctrl Pts',(46.4606822267319,-72.2303448318372,
-216.848171262885));
#220529=CARTESIAN_POINT('Ctrl Pts',(46.4374915718699,-72.246531469105,-216.848202379732));
#220530=CARTESIAN_POINT('Ctrl Pts',(46.3856103030984,-72.2825820153409,
-216.848092367259));
#220531=CARTESIAN_POINT('Ctrl Pts',(46.3558503353891,-72.3031801798479,
-216.847943622513));
#220532=CARTESIAN_POINT('Ctrl Pts',(46.2631145147534,-72.3667848726466,
-216.847284711573));
#220533=CARTESIAN_POINT('Ctrl Pts',(46.208151407488,-72.4033115039303,-216.847007932495));
#220534=CARTESIAN_POINT('Ctrl Pts',(46.1416458441078,-72.4467401169996,
-216.846836506201));
#220535=CARTESIAN_POINT('Ctrl Pts',(46.1221295340369,-72.4593269700902,
-216.846819987823));
#220536=CARTESIAN_POINT('Ctrl Pts',(46.0974082219484,-72.4751244180359,
-216.846856145838));
#220537=CARTESIAN_POINT('Ctrl Pts',(46.0861848140159,-72.4822527182994,
-216.84688945874));
#220538=CARTESIAN_POINT('Ctrl Pts',(46.0751835275252,-72.4891763075989,
-216.846954983109));
#220539=CARTESIAN_POINT('Ctrl Pts',(46.0709255770755,-72.4918415808474,
-216.846988777692));
#220540=CARTESIAN_POINT('Ctrl Pts',(46.0681893543815,-72.4935509553511,
-216.847012576906));
#220541=CARTESIAN_POINT('Ctrl Pts',(46.0680823775556,-72.4936192985686,
-216.847012518365));
#220542=CARTESIAN_POINT('Ctrl Pts',(45.986400536202,-72.544427560482,-216.847862664063));
#220543=CARTESIAN_POINT('Ctrl Pts',(45.8584635249158,-72.6215820396233,
-216.849534490042));
#220544=CARTESIAN_POINT('Ctrl Pts',(45.6967296702545,-72.714040109495,-216.852246641916));
#220545=CARTESIAN_POINT('Ctrl Pts',(45.6042304529531,-72.7654497464509,
-216.853958836125));
#220546=CARTESIAN_POINT('Ctrl Pts',(45.5586484610098,-72.7903262952877,
-216.85485107458));
#220547=CARTESIAN_POINT('Ctrl Pts',(45.5341488619496,-72.8035792364326,
-216.855342803594));
#220548=CARTESIAN_POINT('Ctrl Pts',(45.5294717188307,-72.8061050271169,
-216.855437120383));
#220549=CARTESIAN_POINT('Ctrl Pts',(45.5046882376694,-72.8194776935945,
-216.855938034955));
#220550=CARTESIAN_POINT('Ctrl Pts',(45.470715692922,-72.8383454154814,-216.856101554138));
#220551=CARTESIAN_POINT('Ctrl Pts',(45.4028375426769,-72.8758731489928,
-216.855884938175));
#220552=CARTESIAN_POINT('Ctrl Pts',(45.3773872318471,-72.8899169068841,
-216.855735750397));
#220553=CARTESIAN_POINT('Ctrl Pts',(45.3348444051485,-72.9132059925027,
-216.855396495046));
#220554=CARTESIAN_POINT('Ctrl Pts',(45.3124812465956,-72.9254056289433,
-216.855197998949));
#220555=CARTESIAN_POINT('Ctrl Pts',(45.2884584929797,-72.9384146386768,
-216.854956200221));
#220556=CARTESIAN_POINT('Ctrl Pts',(45.2720721122027,-72.9472642953749,
-216.854785378261));
#220557=CARTESIAN_POINT('Ctrl Pts',(45.2647205457611,-72.951225960519,-216.85470655318));
#220558=CARTESIAN_POINT('Ctrl Pts',(45.1783811276406,-72.9976001084211,
-216.853748673381));
#220559=CARTESIAN_POINT('Ctrl Pts',(45.1162386053219,-73.0296995672728,
-216.853096086082));
#220560=CARTESIAN_POINT('Ctrl Pts',(45.0467315615012,-73.0651255515261,
-216.852415497251));
#220561=CARTESIAN_POINT('Ctrl Pts',(45.0274969846771,-73.074811491286,-216.85223834966));
#220562=CARTESIAN_POINT('Ctrl Pts',(45.0046549590261,-73.0862425626378,
-216.852047201304));
#220563=CARTESIAN_POINT('Ctrl Pts',(44.9947354495031,-73.0911831765483,
-216.851970270382));
#220564=CARTESIAN_POINT('Ctrl Pts',(44.985805048694,-73.0956046027232,-216.851913143341));
#220565=CARTESIAN_POINT('Ctrl Pts',(44.9825450402972,-73.0972128634217,
-216.851895651545));
#220566=CARTESIAN_POINT('Ctrl Pts',(44.9804978794133,-73.0982214477538,
-216.851885543953));
#220567=CARTESIAN_POINT('Ctrl Pts',(44.9815296466787,-73.0977154089663,
-216.851889037914));
#220568=CARTESIAN_POINT('Ctrl Pts',(44.7937050256253,-73.1899692383285,
-216.851156413369));
#220569=CARTESIAN_POINT('Ctrl Pts',(44.6038221421328,-73.276007932375,-216.850981194006));
#220570=CARTESIAN_POINT('Ctrl Pts',(44.3891332656768,-73.3655067295875,
-216.851398473015));
#220571=CARTESIAN_POINT('Ctrl Pts',(44.3652648622609,-73.3753494207078,
-216.851453370693));
#220572=CARTESIAN_POINT('Ctrl Pts',(44.3354181459926,-73.3875229791999,
-216.851532659472));
#220573=CARTESIAN_POINT('Ctrl Pts',(44.3303128275422,-73.3895972284648,
-216.851547718566));
#220574=CARTESIAN_POINT('Ctrl Pts',(44.3241159589436,-73.3921189971362,
-216.851559824846));
#220575=CARTESIAN_POINT('Ctrl Pts',(44.3145787175221,-73.3960037439674,
-216.851569925362));
#220576=CARTESIAN_POINT('Ctrl Pts',(44.2769462497412,-73.4113612035586,
-216.851518312626));
#220577=CARTESIAN_POINT('Ctrl Pts',(44.2346656261212,-73.428647567988,-216.851202761778));
#220578=CARTESIAN_POINT('Ctrl Pts',(44.1176065965149,-73.4759833562347,
-216.849929669799));
#220579=CARTESIAN_POINT('Ctrl Pts',(44.0188557871459,-73.5153738373685,
-216.848393248556));
#220580=CARTESIAN_POINT('Ctrl Pts',(43.8384285616185,-73.5832970739191,
-216.845057076804));
#220581=CARTESIAN_POINT('Ctrl Pts',(43.7728881056669,-73.6074012984833,
-216.843773096239));
#220582=CARTESIAN_POINT('Ctrl Pts',(43.6928204059483,-73.6358421539148,
-216.842135204374));
#220583=CARTESIAN_POINT('Ctrl Pts',(43.6838358636326,-73.6390206080686,
-216.841950530088));
#220584=CARTESIAN_POINT('Ctrl Pts',(43.6656893389447,-73.6454130775643,
-216.841575808911));
#220585=CARTESIAN_POINT('Ctrl Pts',(43.6613867719329,-73.6469205732218,
-216.841486892913));
#220586=CARTESIAN_POINT('Ctrl Pts',(43.6432709423947,-73.6532597550245,
-216.841114816226));
#220587=CARTESIAN_POINT('Ctrl Pts',(43.6069988100621,-73.6658712095105,
-216.840375657652));
#220588=CARTESIAN_POINT('Ctrl Pts',(43.5706001821117,-73.6782836949642,
-216.839651483473));
#220589=CARTESIAN_POINT('Ctrl Pts',(43.4489677593928,-73.7192243136924,
-216.837270868198));
#220590=CARTESIAN_POINT('Ctrl Pts',(43.3505740698763,-73.7506204343719,
-216.835472931678));
#220591=CARTESIAN_POINT('Ctrl Pts',(43.052725368472,-73.8406182541426,-216.830398789216));
#220592=CARTESIAN_POINT('Ctrl Pts',(42.850988648335,-73.8949175961045,-216.827442250372));
#220593=CARTESIAN_POINT('Ctrl Pts',(42.6506409244548,-73.9423397713703,
-216.824911934326));
#220594=CARTESIAN_POINT('Ctrl Pts',(48.7454044931546,-72.6086641314349,
-213.184229057458));
#220595=CARTESIAN_POINT('Ctrl Pts',(48.7033558856732,-72.5944415704724,
-215.339600005589));
#220596=CARTESIAN_POINT('Ctrl Pts',(47.6826029798323,-71.3710801272352,
-216.791855002172));
#220597=CARTESIAN_POINT('Ctrl Pts',(48.4201758660447,-72.8745352082672,
-213.18165597563));
#220598=CARTESIAN_POINT('Ctrl Pts',(48.4312469413185,-72.8157272237703,
-215.339098369127));
#220599=CARTESIAN_POINT('Ctrl Pts',(47.4907935026806,-71.5238447201971,
-216.792044585111));
#220600=CARTESIAN_POINT('Ctrl Pts',(48.0843074405258,-73.1189108367609,
-213.190215709195));
#220601=CARTESIAN_POINT('Ctrl Pts',(48.1524733410718,-73.0220158932171,
-215.351128153903));
#220602=CARTESIAN_POINT('Ctrl Pts',(47.2933342139034,-71.6644126162231,
-216.803168697192));
#220603=CARTESIAN_POINT('Ctrl Pts',(47.7383831769152,-73.3429891884114,
-213.20923907124));
#220604=CARTESIAN_POINT('Ctrl Pts',(47.8674267413582,-73.2141877251378,
-215.374920075632));
#220605=CARTESIAN_POINT('Ctrl Pts',(47.0905557676078,-71.7934728593478,
-216.824560386716));
#220606=CARTESIAN_POINT('',(47.6826029798323,-71.3710801272351,-216.791855002172));
#220607=CARTESIAN_POINT('',(48.7454044931547,-72.6086641314348,-213.184229057458));
#220608=CARTESIAN_POINT('Origin',(45.5817163713881,-68.7378163165586,-213.096967025272));
#220609=CARTESIAN_POINT('Origin',(42.8925236218019,-65.4916988456017,-217.549100737884));
#220610=CARTESIAN_POINT('Ctrl Pts',(47.6826029798323,-71.3710801272352,
-216.791855002172));
#220611=CARTESIAN_POINT('Ctrl Pts',(47.5930241849003,-71.4424241948411,
-216.791943540537));
#220612=CARTESIAN_POINT('Ctrl Pts',(47.501770357419,-71.5114565096234,-216.794420184531));
#220613=CARTESIAN_POINT('Ctrl Pts',(47.4089903151591,-71.5780732065795,
-216.799270679234));
#220614=CARTESIAN_POINT('Ctrl Pts',(47.315016754119,-71.6455468580804,-216.804183570508));
#220615=CARTESIAN_POINT('Ctrl Pts',(47.2194774794399,-71.7105423809681,
-216.81153173483));
#220616=CARTESIAN_POINT('Ctrl Pts',(47.1225445112692,-71.7729893080334,
-216.821266633682));
#220617=CARTESIAN_POINT('Ctrl Pts',(47.1118983115526,-71.7798478874183,
-216.822335822828));
#220618=CARTESIAN_POINT('Ctrl Pts',(47.1012353169086,-71.7866757600782,
-216.823433769923));
#220619=CARTESIAN_POINT('Ctrl Pts',(47.0905557676078,-71.7934728593478,
-216.824560386716));
#220620=CARTESIAN_POINT('Ctrl Pts',(47.6826029798322,-71.3710801272353,
-216.791855002172));
#220621=CARTESIAN_POINT('Ctrl Pts',(48.7033558856732,-72.5944415704724,
-215.339600005589));
#220622=CARTESIAN_POINT('Ctrl Pts',(48.7454044931547,-72.6086641314348,
-213.184229057458));
#220623=CARTESIAN_POINT('Ctrl Pts',(48.7278636855945,-70.5385934818759,
-216.790821882089));
#220624=CARTESIAN_POINT('Ctrl Pts',(49.761732857596,-71.7299417527765,-215.340395531872));
#220625=CARTESIAN_POINT('Ctrl Pts',(49.8084038141043,-71.7395463911349,
-213.198257848046));
#220626=CARTESIAN_POINT('Ctrl Pts',(49.7727562910368,-69.6608348552492,
-216.790293600173));
#220627=CARTESIAN_POINT('Ctrl Pts',(50.8130965389874,-70.8232845236527,
-215.341943634334));
#220628=CARTESIAN_POINT('Ctrl Pts',(50.8549407258148,-70.835967150169,-213.213888016011));
#220629=CARTESIAN_POINT('Ctrl Pts',(50.7746555306532,-68.7687177611616,
-216.79041881877));
#220630=CARTESIAN_POINT('Ctrl Pts',(51.8269633350129,-69.9002951910831,
-215.34395680141));
#220631=CARTESIAN_POINT('Ctrl Pts',(51.8687937432179,-69.9121576054873,
-213.227785479717));
#220632=CARTESIAN_POINT('Origin',(46.9399934642734,-69.2345705942718,-216.824055271245));
#220633=CARTESIAN_POINT('Ctrl Pts',(48.7454044931547,-72.6086641314348,
-213.184229057458));
#220634=CARTESIAN_POINT('Ctrl Pts',(49.0966483416997,-72.3214805470352,
-213.189018754026));
#220635=CARTESIAN_POINT('Ctrl Pts',(49.445331300399,-72.0311663472331,-213.193869847133));
#220636=CARTESIAN_POINT('Ctrl Pts',(49.7914306652966,-71.7378094434948,
-213.198721048627));
#220637=CARTESIAN_POINT('Ctrl Pts',(50.1399413000144,-71.4424087259844,
-213.20360604838));
#220638=CARTESIAN_POINT('Ctrl Pts',(50.4858333869782,-71.1439217890174,
-213.208491419808));
#220639=CARTESIAN_POINT('Ctrl Pts',(50.8290574947046,-70.8423935581624,
-213.213315112328));
#220640=CARTESIAN_POINT('Ctrl Pts',(51.172281602431,-70.5408653273073,-213.218138804848));
#220641=CARTESIAN_POINT('Ctrl Pts',(51.5128390059467,-70.2362947052039,
-213.222901065645));
#220642=CARTESIAN_POINT('Ctrl Pts',(51.8506357777519,-69.9286975574418,
-213.227536544435));
#220643=CARTESIAN_POINT('Origin',(-7.03224757818595E-6,47.3239895493301,
-196.659261305123));
#220644=CARTESIAN_POINT('',(0.0473571427401393,53.3225154460666,-213.879539002147));
#220645=CARTESIAN_POINT('Origin',(0.46976145343121,53.0041184688829,-208.56971754274));
#220646=CARTESIAN_POINT('',(0.0544835933803345,52.4792219709059,-216.57221503382));
#220647=CARTESIAN_POINT('Origin',(0.0463362411570871,48.3232770745245,-213.79227696996));
#220648=CARTESIAN_POINT('Origin',(0.0318052213360498,52.469100728301,-216.511513110739));
#220649=CARTESIAN_POINT('Ctrl Pts',(0.0473571427401181,53.3225154460666,
-213.879539002147));
#220650=CARTESIAN_POINT('Ctrl Pts',(0.0513181061457815,53.2968418492561,
-215.350332007314));
#220651=CARTESIAN_POINT('Ctrl Pts',(0.0544853477938667,52.4787689033323,
-216.572892235108));
#220652=CARTESIAN_POINT('Ctrl Pts',(1.50078629177953,53.3222855571144,-213.875705279281));
#220653=CARTESIAN_POINT('Ctrl Pts',(1.62614544992748,53.2965621608307,-215.346507035678));
#220654=CARTESIAN_POINT('Ctrl Pts',(1.72636223391502,52.4781147405702,-216.56897010493));
#220655=CARTESIAN_POINT('Ctrl Pts',(2.92702243085717,53.3114912412646,-213.695947807356));
#220656=CARTESIAN_POINT('Ctrl Pts',(3.17360837162122,53.2833921337829,-215.166683249136));
#220657=CARTESIAN_POINT('Ctrl Pts',(3.36628637758863,52.4472954145725,-216.38513789576));
#220658=CARTESIAN_POINT('Ctrl Pts',(4.37281940663811,53.2905575229658,-213.348880503444));
#220659=CARTESIAN_POINT('Ctrl Pts',(4.73714801109632,53.2579878078057,-214.82094618417));
#220660=CARTESIAN_POINT('Ctrl Pts',(5.02417785496923,52.3884400051989,-216.030189424361));
#220661=CARTESIAN_POINT('Ctrl Pts',(4.4166077184939,53.289913868413,-213.338209943704));
#220662=CARTESIAN_POINT('Ctrl Pts',(4.78457700700934,53.2572054630635,-214.810300111701));
#220663=CARTESIAN_POINT('Ctrl Pts',(5.07438936223524,52.38663030623,-216.019276413929));
#220664=CARTESIAN_POINT('Ctrl Pts',(4.47131352346949,53.2890977177666,-213.324680435774));
#220665=CARTESIAN_POINT('Ctrl Pts',(4.84383217904547,53.2562134344238,-214.796802126739));
#220666=CARTESIAN_POINT('Ctrl Pts',(5.13712105476995,52.3843352406963,-216.005439190793));
#220667=CARTESIAN_POINT('Ctrl Pts',(4.48225430767143,53.2889337622212,-213.321972140265));
#220668=CARTESIAN_POINT('Ctrl Pts',(4.8530836264365,53.2560652079218,-214.794050223811));
#220669=CARTESIAN_POINT('Ctrl Pts',(5.14497267313242,52.3846620371662,-216.002795752475));
#220670=CARTESIAN_POINT('Ctrl Pts',(4.50414007083002,53.2886037420393,-213.316582951083));
#220671=CARTESIAN_POINT('Ctrl Pts',(4.87325651228538,53.2557343778721,-214.788605124326));
#220672=CARTESIAN_POINT('Ctrl Pts',(5.16368704978722,52.384808931647,-215.997453930094));
#220673=CARTESIAN_POINT('Ctrl Pts',(4.51508431353993,53.2884377751688,-213.313897267951));
#220674=CARTESIAN_POINT('Ctrl Pts',(4.88334426763236,53.2555681292117,-214.785891301654));
#220675=CARTESIAN_POINT('Ctrl Pts',(5.17304536586829,52.3848811302304,-215.994791426239));
#220676=CARTESIAN_POINT('Ctrl Pts',(4.54792112758205,53.2879370021236,-213.30586696962));
#220677=CARTESIAN_POINT('Ctrl Pts',(4.91361107625039,53.2550668868734,-214.777776140093));
#220678=CARTESIAN_POINT('Ctrl Pts',(5.20112370349652,52.3850939761974,-215.986829153085));
#220679=CARTESIAN_POINT('Ctrl Pts',(4.56981778483334,53.2875993235168,-213.300549105442));
#220680=CARTESIAN_POINT('Ctrl Pts',(4.93379446859988,53.2547293838989,-214.77240089122));
#220681=CARTESIAN_POINT('Ctrl Pts',(5.21984711401021,52.3852308738026,-215.981554622283));
#220682=CARTESIAN_POINT('Ctrl Pts',(4.67932834463653,53.2858917529309,-213.274138348232));
#220683=CARTESIAN_POINT('Ctrl Pts',(5.03472988581075,53.2530252892833,-214.745701624089));
#220684=CARTESIAN_POINT('Ctrl Pts',(5.31348684546282,52.3858903127237,-215.955350443654));
#220685=CARTESIAN_POINT('Ctrl Pts',(4.76702406700707,53.2844643286532,-213.253581139957));
#220686=CARTESIAN_POINT('Ctrl Pts',(5.11556895614656,53.2516084370936,-214.724900005178));
#220687=CARTESIAN_POINT('Ctrl Pts',(5.38847118038393,52.3863377057957,-215.934926221979));
#220688=CARTESIAN_POINT('Ctrl Pts',(5.03037439102468,53.2799968687426,-213.193632432861));
#220689=CARTESIAN_POINT('Ctrl Pts',(5.35831561743065,53.247196875607,-214.664189566484));
#220690=CARTESIAN_POINT('Ctrl Pts',(5.61364510061675,52.3874374899134,-215.875279476601));
#220691=CARTESIAN_POINT('Ctrl Pts',(5.20629213894649,53.2767716505112,-213.155963782957));
#220692=CARTESIAN_POINT('Ctrl Pts',(5.52050447418381,53.2440403454911,-214.625960795307));
#220693=CARTESIAN_POINT('Ctrl Pts',(5.76405550081911,52.3878474698,-215.837682829783));
#220694=CARTESIAN_POINT('Ctrl Pts',(5.7351090490271,53.2663464299268,-213.049921731156));
#220695=CARTESIAN_POINT('Ctrl Pts',(6.00800931507342,53.2339186236173,-214.518122615114));
#220696=CARTESIAN_POINT('Ctrl Pts',(6.21619890377965,52.3880929077652,-215.731466854287));
#220697=CARTESIAN_POINT('Ctrl Pts',(6.08932836962055,53.2583903798102,-212.988474563998));
#220698=CARTESIAN_POINT('Ctrl Pts',(6.33470802101544,53.2262917188763,-214.455267165325));
#220699=CARTESIAN_POINT('Ctrl Pts',(6.51906256367254,52.3869415830987,-215.669383233572));
#220700=CARTESIAN_POINT('Ctrl Pts',(7.15467547994453,53.2314932970166,-212.832839779496));
#220701=CARTESIAN_POINT('Ctrl Pts',(7.31721137313374,53.2007743525897,-214.294930171996));
#220702=CARTESIAN_POINT('Ctrl Pts',(7.4301490293476,52.3794528536415,-215.510259917988));
#220703=CARTESIAN_POINT('Ctrl Pts',(7.86408306340235,53.2096427750673,-212.767811172676));
#220704=CARTESIAN_POINT('Ctrl Pts',(7.9719989895612,53.1803473395072,-214.22594561548));
#220705=CARTESIAN_POINT('Ctrl Pts',(8.03673212095718,52.3691912963031,-215.440813554609));
#220706=CARTESIAN_POINT('Ctrl Pts',(9.98981135051243,53.1323666949439,-212.690409355922));
#220707=CARTESIAN_POINT('Ctrl Pts',(9.93185501850042,53.1089544676763,-214.134581778742));
#220708=CARTESIAN_POINT('Ctrl Pts',(9.85169968539593,52.3227594953376,-215.343739708831));
#220709=CARTESIAN_POINT('Ctrl Pts',(11.4039030907724,53.0652276040225,-212.794256396978));
#220710=CARTESIAN_POINT('Ctrl Pts',(11.2367879874246,53.0477230606374,-214.22619279686));
#220711=CARTESIAN_POINT('Ctrl Pts',(11.0567236931827,52.271013981524,-215.426125580955));
#220712=CARTESIAN_POINT('Ctrl Pts',(13.1664443333411,52.9616798229974,-213.138287858329));
#220713=CARTESIAN_POINT('Ctrl Pts',(12.8547213220072,52.9546856753362,-214.549698418581));
#220714=CARTESIAN_POINT('Ctrl Pts',(12.54724214411,52.1791590921482,-215.730009700032));
#220715=CARTESIAN_POINT('Ctrl Pts',(13.5182905195363,52.9400113359771,-213.217839110357));
#220716=CARTESIAN_POINT('Ctrl Pts',(13.1775056939578,52.9352623790446,-214.624917702853));
#220717=CARTESIAN_POINT('Ctrl Pts',(12.8442482944742,52.1594335681189,-215.800867210821));
#220718=CARTESIAN_POINT('Ctrl Pts',(13.8914034372555,52.9159732378538,-213.314153161469));
#220719=CARTESIAN_POINT('Ctrl Pts',(13.519416343042,52.91377595379,-214.716322291134));
#220720=CARTESIAN_POINT('Ctrl Pts',(13.1586925435442,52.137008372533,-215.887205379916));
#220721=CARTESIAN_POINT('Ctrl Pts',(13.9133485948345,52.9145554991731,-213.319862053585));
#220722=CARTESIAN_POINT('Ctrl Pts',(13.5395282183867,52.9125087139671,-214.721742162107));
#220723=CARTESIAN_POINT('Ctrl Pts',(13.1771851227051,52.1356838534725,-215.892324735676));
#220724=CARTESIAN_POINT('Ctrl Pts',(13.9572335779744,52.9117125575511,-213.331366738556));
#220725=CARTESIAN_POINT('Ctrl Pts',(13.5797448109807,52.9099679570789,-214.732666696408));
#220726=CARTESIAN_POINT('Ctrl Pts',(13.2141620165421,52.1330240247262,-215.90264489138));
#220727=CARTESIAN_POINT('Ctrl Pts',(13.9791751707466,52.910287801062,-213.337130942172));
#220728=CARTESIAN_POINT('Ctrl Pts',(13.6053354404193,52.9083470662355,-214.739112678143));
#220729=CARTESIAN_POINT('Ctrl Pts',(13.2427576996845,52.1315237651408,-215.909751051737));
#220730=CARTESIAN_POINT('Ctrl Pts',(14.0450114907337,52.906007261992,-213.354204614102));
#220731=CARTESIAN_POINT('Ctrl Pts',(13.67719453886,52.9037874808928,-214.757359487488));
#220732=CARTESIAN_POINT('Ctrl Pts',(13.3194789666303,52.1271448577845,-215.929109421424));
#220733=CARTESIAN_POINT('Ctrl Pts',(14.0889121696723,52.9031437987804,-213.36539506595));
#220734=CARTESIAN_POINT('Ctrl Pts',(13.7251035033336,52.9007361441998,-214.769331200397));
#220735=CARTESIAN_POINT('Ctrl Pts',(13.3706237530771,52.1241944637679,-215.941816004742));
#220736=CARTESIAN_POINT('Ctrl Pts',(14.2206434120527,52.8945239974864,-213.398393774553));
#220737=CARTESIAN_POINT('Ctrl Pts',(13.8688369510683,52.8915473464146,-214.804670640288));
#220738=CARTESIAN_POINT('Ctrl Pts',(13.5240519748989,52.1152502744402,-215.979342795789));
#220739=CARTESIAN_POINT('Ctrl Pts',(14.3085031783526,52.8887382469479,-213.419629432868));
#220740=CARTESIAN_POINT('Ctrl Pts',(13.9646727465828,52.8853747963935,-214.827463939186));
#220741=CARTESIAN_POINT('Ctrl Pts',(13.6263292941939,52.1091634838073,-216.003570107382));
#220742=CARTESIAN_POINT('Ctrl Pts',(14.5721978639792,52.8712625751263,-213.481070862543));
#220743=CARTESIAN_POINT('Ctrl Pts',(14.252217261359,52.8667166406394,-214.893568804806));
#220744=CARTESIAN_POINT('Ctrl Pts',(13.9331521185388,52.0905335590214,-216.073910240701));
#220745=CARTESIAN_POINT('Ctrl Pts',(14.7481481313963,52.8594542225811,-213.519011772404));
#220746=CARTESIAN_POINT('Ctrl Pts',(14.4439820930866,52.8540893087314,-214.934610621538));
#220747=CARTESIAN_POINT('Ctrl Pts',(14.1376887958124,52.0776210286607,-216.117682146349));
#220748=CARTESIAN_POINT('Ctrl Pts',(15.6286519779478,52.799613377426,-213.693903709884));
#220749=CARTESIAN_POINT('Ctrl Pts',(15.4031772187442,52.7899993081263,-215.12497225672));
#220750=CARTESIAN_POINT('Ctrl Pts',(15.1604959234659,52.0106176596974,-216.321274261672));
#220751=CARTESIAN_POINT('Ctrl Pts',(16.3354684203193,52.7491845407321,-213.786320807185));
#220752=CARTESIAN_POINT('Ctrl Pts',(16.1726687571268,52.7356086885058,-215.229790369045));
#220753=CARTESIAN_POINT('Ctrl Pts',(15.9799531666696,51.9491102505506,-216.435321014709));
#220754=CARTESIAN_POINT('Ctrl Pts',(18.4626009435542,52.5898921039226,-213.93074044221));
#220755=CARTESIAN_POINT('Ctrl Pts',(18.4831256320861,52.5630943102473,-215.41083522379));
#220756=CARTESIAN_POINT('Ctrl Pts',(18.4346796935493,51.7426456517123,-216.639808829428));
#220757=CARTESIAN_POINT('Ctrl Pts',(19.889576854664,52.4730122776555,-213.850322288953));
#220758=CARTESIAN_POINT('Ctrl Pts',(20.0303223005475,52.4352353701873,-215.353938852772));
#220759=CARTESIAN_POINT('Ctrl Pts',(20.0708290034904,51.5750773518433,-216.593838971602));
#220760=CARTESIAN_POINT('Ctrl Pts',(21.6827252055215,52.3125514421363,-213.558099210805));
#220761=CARTESIAN_POINT('Ctrl Pts',(21.9611240710592,52.2595696821476,-215.091433587878));
#220762=CARTESIAN_POINT('Ctrl Pts',(22.10701332157,51.3339336809999,-216.337638892853));
#220763=CARTESIAN_POINT('Ctrl Pts',(22.0420804380365,52.2797161015951,-213.490009648216));
#220764=CARTESIAN_POINT('Ctrl Pts',(22.3484158142329,52.2235225648504,-215.02913808195));
#220765=CARTESIAN_POINT('Ctrl Pts',(22.5140828494934,51.2840959663516,-216.276412274292));
#220766=CARTESIAN_POINT('Ctrl Pts',(22.489685929986,52.237965427953,-213.393843363054));
#220767=CARTESIAN_POINT('Ctrl Pts',(22.830297685778,52.1776606940211,-214.940224931789));
#220768=CARTESIAN_POINT('Ctrl Pts',(23.0202154747916,51.2201134032129,-216.188409850374));
#220769=CARTESIAN_POINT('Ctrl Pts',(22.5791527085523,52.2295777954778,-213.374053497722));
#220770=CARTESIAN_POINT('Ctrl Pts',(22.9266518936637,52.1684397634174,-214.92187419643));
#220771=CARTESIAN_POINT('Ctrl Pts',(23.1213352805328,51.2072292399456,-216.170232433021));
#220772=CARTESIAN_POINT('Ctrl Pts',(22.6909190277613,52.2190463850868,-213.348628685159));
#220773=CARTESIAN_POINT('Ctrl Pts',(23.0469943568649,52.156860007596,-214.898249234479));
#220774=CARTESIAN_POINT('Ctrl Pts',(23.2476077584572,51.1910139587644,-216.146798480699));
#220775=CARTESIAN_POINT('Ctrl Pts',(22.7132689336663,52.2169377595729,-213.343509345961));
#220776=CARTESIAN_POINT('Ctrl Pts',(23.0710617306981,52.1545410005613,-214.893489132397));
#220777=CARTESIAN_POINT('Ctrl Pts',(23.2728558874527,51.1877653983752,-216.142076078541));
#220778=CARTESIAN_POINT('Ctrl Pts',(22.7467887689231,52.2137713063516,-213.335778919634));
#220779=CARTESIAN_POINT('Ctrl Pts',(23.1071557559864,52.1510584252376,-214.886297549121));
#220780=CARTESIAN_POINT('Ctrl Pts',(23.3107186471497,51.1828842897498,-216.134939216676));
#220781=CARTESIAN_POINT('Ctrl Pts',(22.7579612100689,52.2127152361209,-213.333193541222));
#220782=CARTESIAN_POINT('Ctrl Pts',(23.1191863165467,52.1498968514716,-214.883891703835));
#220783=CARTESIAN_POINT('Ctrl Pts',(23.3233379945114,51.1812558755664,-216.132551386277));
#220784=CARTESIAN_POINT('Ctrl Pts',(22.7803044200105,52.2106019240513,-213.328005669353));
#220785=CARTESIAN_POINT('Ctrl Pts',(23.1432453661066,52.147572322968,-214.879062842723));
#220786=CARTESIAN_POINT('Ctrl Pts',(23.3485735632596,51.1779962891938,-216.127757998687));
#220787=CARTESIAN_POINT('Ctrl Pts',(22.7914750239802,52.2095447316332,-213.325401286812));
#220788=CARTESIAN_POINT('Ctrl Pts',(23.1566284527116,52.1462704833645,-214.87692670199));
#220789=CARTESIAN_POINT('Ctrl Pts',(23.3635425140041,51.1754974311187,-216.125669225138));
#220790=CARTESIAN_POINT('Ctrl Pts',(22.8473256024037,52.2042553206975,-213.312356521225));
#220791=CARTESIAN_POINT('Ctrl Pts',(23.2084106565659,52.1413088528524,-214.863000994536));
#220792=CARTESIAN_POINT('Ctrl Pts',(23.4121150904848,51.1726824854318,-216.111643547468));
#220793=CARTESIAN_POINT('Ctrl Pts',(22.8920158443536,52.2000074805641,-213.302049206934));
#220794=CARTESIAN_POINT('Ctrl Pts',(23.2498473184699,52.1373250721395,-214.851985232895));
#220795=CARTESIAN_POINT('Ctrl Pts',(23.450976928624,51.1704115507272,-216.100543254307));
#220796=CARTESIAN_POINT('Ctrl Pts',(23.1155161868957,52.1786865508133,-213.251157958149));
#220797=CARTESIAN_POINT('Ctrl Pts',(23.4570203439368,52.117339881761,-214.797550367366));
#220798=CARTESIAN_POINT('Ctrl Pts',(23.6453045375155,51.1589619023911,-216.045645542894));
#220799=CARTESIAN_POINT('Ctrl Pts',(23.2944736580684,52.1613682854172,-213.212509671947));
#220800=CARTESIAN_POINT('Ctrl Pts',(23.6229334914969,52.1011197585585,-214.756006577968));
#220801=CARTESIAN_POINT('Ctrl Pts',(23.8008254618619,51.1494982987292,-216.003659147808));
#220802=CARTESIAN_POINT('Ctrl Pts',(24.1900632291311,52.0734578840137,-213.02978559012));
#220803=CARTESIAN_POINT('Ctrl Pts',(24.4523439445286,52.0189511941718,-214.558750653319));
#220804=CARTESIAN_POINT('Ctrl Pts',(24.5786925763469,51.1006544733309,-215.803557774365));
#220805=CARTESIAN_POINT('Ctrl Pts',(24.9090934498498,51.9989121398747,-212.917162893799));
#220806=CARTESIAN_POINT('Ctrl Pts',(25.1186944050463,51.9494811141712,-214.433449924263));
#220807=CARTESIAN_POINT('Ctrl Pts',(25.2018288175531,51.0567050281331,-215.674851310126));
#220808=CARTESIAN_POINT('Ctrl Pts',(26.3528137916526,51.8410386164222,-212.765468959133));
#220809=CARTESIAN_POINT('Ctrl Pts',(26.4549358636402,51.803024530226,-214.254620439179));
#220810=CARTESIAN_POINT('Ctrl Pts',(26.4489097601866,50.9587713152296,-215.485839368666));
#220811=CARTESIAN_POINT('Ctrl Pts',(27.0774998386423,51.757712611848,-212.726350374933));
#220812=CARTESIAN_POINT('Ctrl Pts',(27.1250938204043,51.7260245846545,-214.200855802869));
#220813=CARTESIAN_POINT('Ctrl Pts',(27.0728462116736,50.9047968613094,-215.425489070919));
#220814=CARTESIAN_POINT('Ctrl Pts',(28.1693846366643,51.6257897144361,-212.730030329923));
#220815=CARTESIAN_POINT('Ctrl Pts',(28.133153944658,51.6046668429049,-214.180734173614));
#220816=CARTESIAN_POINT('Ctrl Pts',(28.0085132019179,50.8158988470028,-215.392519511646));
#220817=CARTESIAN_POINT('Ctrl Pts',(28.5341580010441,51.5806587005877,-212.741678726248));
#220818=CARTESIAN_POINT('Ctrl Pts',(28.4694894459954,51.5632588178081,-214.184116855442));
#220819=CARTESIAN_POINT('Ctrl Pts',(28.320362539182,50.7849405015155,-215.391147109929));
#220820=CARTESIAN_POINT('Ctrl Pts',(29.2654690940375,51.4880085266914,-212.787471470535));
#220821=CARTESIAN_POINT('Ctrl Pts',(29.1429594857087,51.4784684902285,-214.212632134674));
#220822=CARTESIAN_POINT('Ctrl Pts',(28.9438185512427,50.7202631028992,-215.409064536584));
#220823=CARTESIAN_POINT('Ctrl Pts',(29.6331976033025,51.4403305324129,-212.821772692263));
#220824=CARTESIAN_POINT('Ctrl Pts',(29.4812293665496,51.4349376880746,-214.237876571198));
#220825=CARTESIAN_POINT('Ctrl Pts',(29.2564302637446,50.6864303950653,-215.42845818016));
#220826=CARTESIAN_POINT('Ctrl Pts',(31.462411304102,51.1976497020186,-213.05276291922));
#220827=CARTESIAN_POINT('Ctrl Pts',(31.1598855435033,51.2141722963552,-214.421574027106));
#220828=CARTESIAN_POINT('Ctrl Pts',(30.8062875514217,50.5113774631636,-215.58023710365));
#220829=CARTESIAN_POINT('Ctrl Pts',(32.8718379544085,50.9930622692497,-213.421070504589));
#220830=CARTESIAN_POINT('Ctrl Pts',(32.4486765378635,51.0294768386726,-214.747355725967));
#220831=CARTESIAN_POINT('Ctrl Pts',(31.9841321905945,50.3552367741408,-215.87179911295));
#220832=CARTESIAN_POINT('Ctrl Pts',(34.2185104850841,50.7818638678805,-214.004031647198));
#220833=CARTESIAN_POINT('Ctrl Pts',(33.6642034707759,50.8420733856997,-215.278241777324));
#220834=CARTESIAN_POINT('Ctrl Pts',(33.0835570625902,50.1833829144682,-216.356884220228));
#220835=CARTESIAN_POINT('',(5.13104565674618,52.3850329666526,-216.006074884366));
#220836=CARTESIAN_POINT('',(13.2064798588263,52.1340212825562,-215.899800104744));
#220837=CARTESIAN_POINT('Ctrl Pts',(5.13104565674618,52.3850329666526,-216.006074884366));
#220838=CARTESIAN_POINT('Ctrl Pts',(5.1522723863429,52.3849119363674,-216.000415561109));
#220839=CARTESIAN_POINT('Ctrl Pts',(5.18369007136552,52.3849388776591,-215.991787544618));
#220840=CARTESIAN_POINT('Ctrl Pts',(5.2221706225626,52.3853576829994,-215.98074183974));
#220841=CARTESIAN_POINT('Ctrl Pts',(5.23991278899162,52.3856572015947,-215.975516213414));
#220842=CARTESIAN_POINT('Ctrl Pts',(5.24999842259676,52.3858537036521,-215.972512762277));
#220843=CARTESIAN_POINT('Ctrl Pts',(5.25431824827715,52.3859432179003,-215.971219626002));
#220844=CARTESIAN_POINT('Ctrl Pts',(5.26070648918049,52.3860788494767,-215.96930321972));
#220845=CARTESIAN_POINT('Ctrl Pts',(5.27389209107745,52.3861808482352,-215.965609200379));
#220846=CARTESIAN_POINT('Ctrl Pts',(5.30493951670919,52.3863517352301,-215.957082350732));
#220847=CARTESIAN_POINT('Ctrl Pts',(5.32328062740663,52.3864424667375,-215.95207247075));
#220848=CARTESIAN_POINT('Ctrl Pts',(5.34961236428572,52.3865761864417,-215.944921314242));
#220849=CARTESIAN_POINT('Ctrl Pts',(5.36195508675722,52.3866420092958,-215.941576612198));
#220850=CARTESIAN_POINT('Ctrl Pts',(5.37041866445846,52.3866880806414,-215.939284606238));
#220851=CARTESIAN_POINT('Ctrl Pts',(5.3766407570771,52.3867228499403,-215.937600959149));
#220852=CARTESIAN_POINT('Ctrl Pts',(5.46224792408119,52.387209238623,-215.914445988889));
#220853=CARTESIAN_POINT('Ctrl Pts',(5.54481645278234,52.3875795430898,-215.892793204776));
#220854=CARTESIAN_POINT('Ctrl Pts',(5.79534687511541,52.3884036177798,-215.829175878375));
#220855=CARTESIAN_POINT('Ctrl Pts',(5.96055636587489,52.3885516848245,-215.789947269247));
#220856=CARTESIAN_POINT('Ctrl Pts',(6.2979554273082,52.3880338386774,-215.715495695431));
#220857=CARTESIAN_POINT('Ctrl Pts',(6.4666575859569,52.3873610716747,-215.681107141238));
#220858=CARTESIAN_POINT('Ctrl Pts',(6.80397794650947,52.3851945176741,-215.618004498281));
#220859=CARTESIAN_POINT('Ctrl Pts',(6.97119969975367,52.3837164893957,-215.589504826742));
#220860=CARTESIAN_POINT('Ctrl Pts',(7.48099337258852,52.3779565382077,-215.511231006924));
#220861=CARTESIAN_POINT('Ctrl Pts',(7.82010832743786,52.3724788185414,-215.470605457691));
#220862=CARTESIAN_POINT('Ctrl Pts',(8.32716511723021,52.3618554631322,-215.427002629812));
#220863=CARTESIAN_POINT('Ctrl Pts',(8.58029034720757,52.3559412520016,-215.409535089865));
#220864=CARTESIAN_POINT('Ctrl Pts',(8.8747949213488,52.347988683421,-215.396740572747));
#220865=CARTESIAN_POINT('Ctrl Pts',(9.00082715023796,52.3443544942176,-215.392882411015));
#220866=CARTESIAN_POINT('Ctrl Pts',(9.08480653626051,52.3418814354433,-215.390671459359));
#220867=CARTESIAN_POINT('Ctrl Pts',(9.12559907967593,52.3406558542846,-215.389767430667));
#220868=CARTESIAN_POINT('Ctrl Pts',(10.5486606647616,52.2969998804139,-215.364516209537));
#220869=CARTESIAN_POINT('Ctrl Pts',(11.9026484148537,52.2279542766091,-215.534782163801));
#220870=CARTESIAN_POINT('Ctrl Pts',(13.2064798588263,52.1340212825562,-215.899800104744));
#220871=CARTESIAN_POINT('Ctrl Pts',(0.0544835933803345,52.4792219709059,
-216.57221503382));
#220872=CARTESIAN_POINT('Ctrl Pts',(0.911160817479643,52.4788868661666,
-216.570205286074));
#220873=CARTESIAN_POINT('Ctrl Pts',(1.76241895715707,52.4706614931604,-216.520914925994));
#220874=CARTESIAN_POINT('Ctrl Pts',(3.03147279341818,52.4469055640949,-216.37863656052));
#220875=CARTESIAN_POINT('Ctrl Pts',(3.45317987983679,52.437124954073,-216.319765648019));
#220876=CARTESIAN_POINT('Ctrl Pts',(4.08382026129649,52.4196309296523,-216.214709957797));
#220877=CARTESIAN_POINT('Ctrl Pts',(4.29371035972386,52.4133485556671,-216.176866822026));
#220878=CARTESIAN_POINT('Ctrl Pts',(4.71285393159547,52.3998755739423,-216.095622991724));
#220879=CARTESIAN_POINT('Ctrl Pts',(4.92331707557612,52.3926407185815,-216.051954867598));
#220880=CARTESIAN_POINT('Ctrl Pts',(5.13104565674618,52.3850329666526,-216.006074884366));
#220881=CARTESIAN_POINT('',(33.8288256031492,50.8425198063061,-213.842075047864));
#220882=CARTESIAN_POINT('Ctrl Pts',(33.8288255478891,50.842519431512,-213.842075041244));
#220883=CARTESIAN_POINT('Ctrl Pts',(33.4284854188798,50.9043645576862,-213.682497552222));
#220884=CARTESIAN_POINT('Ctrl Pts',(33.0234151108197,50.9655031314903,-213.541601722254));
#220885=CARTESIAN_POINT('Ctrl Pts',(32.6138910800848,51.0258461372266,-213.418284882882));
#220886=CARTESIAN_POINT('Ctrl Pts',(32.331432047247,51.0674662272815,-213.333230154545));
#220887=CARTESIAN_POINT('Ctrl Pts',(32.0468531911046,51.1087080507273,-213.256538359194));
#220888=CARTESIAN_POINT('Ctrl Pts',(31.760231540292,51.1495445945205,-213.187851585035));
#220889=CARTESIAN_POINT('Ctrl Pts',(31.409874876356,51.1994618119026,-213.103891182943));
#220890=CARTESIAN_POINT('Ctrl Pts',(31.0565047178319,51.2487669147299,-213.031971634751));
#220891=CARTESIAN_POINT('Ctrl Pts',(30.7001071569706,51.2974289024419,-212.971577841718));
#220892=CARTESIAN_POINT('Ctrl Pts',(30.4677048343532,51.3291607665437,-212.932195816379));
#220893=CARTESIAN_POINT('Ctrl Pts',(30.2340152891889,51.3606190839795,-212.897715883105));
#220894=CARTESIAN_POINT('Ctrl Pts',(29.9990356615501,51.3917943388598,-212.868006986073));
#220895=CARTESIAN_POINT('Ctrl Pts',(29.8721559397073,51.4086277456846,-212.851965354593));
#220896=CARTESIAN_POINT('Ctrl Pts',(29.7450788398527,51.425353889665,-212.837366281459));
#220897=CARTESIAN_POINT('Ctrl Pts',(29.6179629924412,51.4419530974048,-212.824189892595));
#220898=CARTESIAN_POINT('Ctrl Pts',(29.3784059472776,51.4732352486014,-212.799358238269));
#220899=CARTESIAN_POINT('Ctrl Pts',(29.1386589563805,51.5040741022767,-212.779534675732));
#220900=CARTESIAN_POINT('Ctrl Pts',(28.8998133411101,51.5343335838555,-212.76457826505));
#220901=CARTESIAN_POINT('Ctrl Pts',(28.5341328392157,51.5806618465631,-212.7416795078));
#220902=CARTESIAN_POINT('Ctrl Pts',(28.1693740007316,51.6257909648341,-212.73003226545));
#220903=CARTESIAN_POINT('Ctrl Pts',(27.8054230251458,51.6697639760348,-212.728805896947));
#220904=CARTESIAN_POINT('Ctrl Pts',(27.2316173468697,51.7390918943822,-212.726872402443));
#220905=CARTESIAN_POINT('Ctrl Pts',(26.6598134037606,51.8055490660031,-212.750767890064));
#220906=CARTESIAN_POINT('Ctrl Pts',(26.0896436282477,51.8692665869875,-212.798150768092));
#220907=CARTESIAN_POINT('Ctrl Pts',(25.9366320432575,51.8863659130062,-212.810866505719));
#220908=CARTESIAN_POINT('Ctrl Pts',(25.7837381711085,51.9032678997162,-212.825274048008));
#220909=CARTESIAN_POINT('Ctrl Pts',(25.6309549566012,51.9199750044334,-212.8413287466));
#220910=CARTESIAN_POINT('Ctrl Pts',(25.5252626824047,51.9315326346253,-212.8524350557));
#220911=CARTESIAN_POINT('Ctrl Pts',(25.4196234520893,51.9429969636597,-212.864330645356));
#220912=CARTESIAN_POINT('Ctrl Pts',(25.3140353742927,51.9543686087815,-212.877005898441));
#220913=CARTESIAN_POINT('Ctrl Pts',(24.6986753884516,52.0206417669555,-212.950876393313));
#220914=CARTESIAN_POINT('Ctrl Pts',(24.085246551812,52.0837464971781,-213.05117739929));
#220915=CARTESIAN_POINT('Ctrl Pts',(23.4735918363912,52.1437861556349,-213.17596614546));
#220916=CARTESIAN_POINT('Ctrl Pts',(23.3778558249152,52.1531835448581,-213.195498042353));
#220917=CARTESIAN_POINT('Ctrl Pts',(23.2821634538006,52.1625057785251,-213.215631611061));
#220918=CARTESIAN_POINT('Ctrl Pts',(23.186514300368,52.1717531873607,-213.236361158368));
#220919=CARTESIAN_POINT('Ctrl Pts',(23.1032160300043,52.1798065065351,-213.254413962539));
#220920=CARTESIAN_POINT('Ctrl Pts',(23.0199493662686,52.187803195851,-213.27291866346));
#220921=CARTESIAN_POINT('Ctrl Pts',(22.9367159200592,52.195743293347,-213.291870988623));
#220922=CARTESIAN_POINT('Ctrl Pts',(22.8920159948606,52.2000074657477,-213.302049198894));
#220923=CARTESIAN_POINT('Ctrl Pts',(22.8473256517277,52.2042553156829,-213.312356529244));
#220924=CARTESIAN_POINT('Ctrl Pts',(22.8026451428263,52.2084868488976,-213.322792347156));
#220925=CARTESIAN_POINT('Ctrl Pts',(22.7914750218758,52.209544731607,-213.325401300168));
#220926=CARTESIAN_POINT('Ctrl Pts',(22.780304416052,52.2106019242221,-213.328005681876));
#220927=CARTESIAN_POINT('Ctrl Pts',(22.769132817356,52.2116585796836,-213.330599615209));
#220928=CARTESIAN_POINT('Ctrl Pts',(22.7579612024781,52.2127152366756,-213.333193552299));
#220929=CARTESIAN_POINT('Ctrl Pts',(22.7467887595399,52.2137713070928,-213.335778930073));
#220930=CARTESIAN_POINT('Ctrl Pts',(22.7356154921252,52.2148267904764,-213.3383557354));
#220931=CARTESIAN_POINT('Ctrl Pts',(22.7132688713518,52.2169377653624,-213.343509365876));
#220932=CARTESIAN_POINT('Ctrl Pts',(22.6909189526696,52.2190463920882,-213.348628706468));
#220933=CARTESIAN_POINT('Ctrl Pts',(22.6685657646965,52.2211526670291,-213.353713651068));
#220934=CARTESIAN_POINT('Ctrl Pts',(22.6646488913269,52.2215217424485,-213.354604668677));
#220935=CARTESIAN_POINT('Ctrl Pts',(22.6607319175832,52.2218907456562,-213.35549463026));
#220936=CARTESIAN_POINT('Ctrl Pts',(22.656814843617,52.2222596766334,-213.356383535222));
#220937=CARTESIAN_POINT('Ctrl Pts',(22.571309563035,52.2303130212968,-213.37578732203));
#220938=CARTESIAN_POINT('Ctrl Pts',(22.4857590592471,52.2383317076776,-213.394687120906));
#220939=CARTESIAN_POINT('Ctrl Pts',(22.400164917909,52.2463155472972,-213.413077019702));
#220940=CARTESIAN_POINT('Ctrl Pts',(22.3089921278352,52.2548197383814,-213.432665491017));
#220941=CARTESIAN_POINT('Ctrl Pts',(22.2177437865542,52.2632866458112,-213.451679464809));
#220942=CARTESIAN_POINT('Ctrl Pts',(22.1264553921399,52.2717131158806,-213.470105691494));
#220943=CARTESIAN_POINT('Ctrl Pts',(21.8592067817213,52.2963817764615,-213.524048840656));
#220944=CARTESIAN_POINT('Ctrl Pts',(21.5914443578931,52.320719710873,-213.572977568712));
#220945=CARTESIAN_POINT('Ctrl Pts',(21.3240957724509,52.3446435619465,-213.616545275377));
#220946=CARTESIAN_POINT('Ctrl Pts',(21.2373298036592,52.3524078675335,-213.63068484627));
#220947=CARTESIAN_POINT('Ctrl Pts',(21.1505925461993,52.3601300382443,-213.644263375919));
#220948=CARTESIAN_POINT('Ctrl Pts',(21.0638877077022,52.367809951321,-213.657275547301));
#220949=CARTESIAN_POINT('Ctrl Pts',(19.9403638201412,52.4673264944071,-213.825887652807));
#220950=CARTESIAN_POINT('Ctrl Pts',(18.8213013409432,52.5598362291047,-213.899469470177));
#220951=CARTESIAN_POINT('Ctrl Pts',(17.707326389879,52.6457198325126,-213.866672048325));
#220952=CARTESIAN_POINT('Ctrl Pts',(17.4861860769682,52.6627689833156,-213.860161280624));
#220953=CARTESIAN_POINT('Ctrl Pts',(17.2652462240557,52.6795570130793,-213.849458152787));
#220954=CARTESIAN_POINT('Ctrl Pts',(17.0445116841478,52.6960869022234,-213.834473635931));
#220955=CARTESIAN_POINT('Ctrl Pts',(16.9763221692139,52.7011933306197,-213.829844605348));
#220956=CARTESIAN_POINT('Ctrl Pts',(16.9081523016037,52.7062751479288,-213.824806041847));
#220957=CARTESIAN_POINT('Ctrl Pts',(16.840002239673,52.711332452689,-213.819355050373));
#220958=CARTESIAN_POINT('Ctrl Pts',(16.1996233055684,52.7588539272113,-213.768134258916));
#220959=CARTESIAN_POINT('Ctrl Pts',(15.5609952943595,52.8042113945009,-213.68046926394));
#220960=CARTESIAN_POINT('Ctrl Pts',(14.924248781074,52.8474860509722,-213.553990748347));
#220961=CARTESIAN_POINT('Ctrl Pts',(14.8649438022416,52.8515165443199,-213.542210855511));
#220962=CARTESIAN_POINT('Ctrl Pts',(14.805655093962,52.8555289645469,-213.530094945451));
#220963=CARTESIAN_POINT('Ctrl Pts',(14.7463827693231,52.8595233836131,-213.517640823919));
#220964=CARTESIAN_POINT('Ctrl Pts',(14.6296583420206,52.8673895552329,-213.49311504039));
#220965=CARTESIAN_POINT('Ctrl Pts',(14.5129975854129,52.8751859177491,-213.467277078932));
#220966=CARTESIAN_POINT('Ctrl Pts',(14.3964014059857,52.8829130229972,-213.440109913241));
#220967=CARTESIAN_POINT('Ctrl Pts',(14.3392716131961,52.8866991498142,-213.426798546143));
#220968=CARTESIAN_POINT('Ctrl Pts',(14.2821573282399,52.8904686504836,-213.413167990813));
#220969=CARTESIAN_POINT('Ctrl Pts',(14.2250586750738,52.8942215948612,-213.399215938865));
#220970=CARTESIAN_POINT('Ctrl Pts',(14.194308849405,52.8962427000706,-213.391702221092));
#220971=CARTESIAN_POINT('Ctrl Pts',(14.1635634419795,52.8982590111407,-213.384095232764));
#220972=CARTESIAN_POINT('Ctrl Pts',(14.1328225823492,52.9002705316719,-213.376394641145));
#220973=CARTESIAN_POINT('Ctrl Pts',(14.0889125166806,52.9031437759365,-213.365395160722));
#220974=CARTESIAN_POINT('Ctrl Pts',(14.04501173063,52.9060072461916,-213.354204687974));
#220975=CARTESIAN_POINT('Ctrl Pts',(14.0011206054638,52.9088609546765,-213.342822186056));
#220976=CARTESIAN_POINT('Ctrl Pts',(13.9791751851707,52.9102877996675,-213.337130971998));
#220977=CARTESIAN_POINT('Ctrl Pts',(13.9572335774877,52.9117125570174,-213.331366770806));
#220978=CARTESIAN_POINT('Ctrl Pts',(13.9352910762429,52.9131340283108,-213.325614433984));
#220979=CARTESIAN_POINT('Ctrl Pts',(13.9133485638354,52.9145555003274,-213.319862094235));
#220980=CARTESIAN_POINT('Ctrl Pts',(13.8914033905367,52.9159732398363,-213.314153208262));
#220981=CARTESIAN_POINT('Ctrl Pts',(13.8694556009263,52.9173872435139,-213.308487695886));
#220982=CARTESIAN_POINT('Ctrl Pts',(13.8144534891343,52.9209307980008,-213.294289676376));
#220983=CARTESIAN_POINT('Ctrl Pts',(13.7594349499713,52.9244508908472,-213.280363986675));
#220984=CARTESIAN_POINT('Ctrl Pts',(13.7044006823105,52.9279474706966,-213.266709421035));
#220985=CARTESIAN_POINT('Ctrl Pts',(13.4080399531756,52.9467766292863,-213.193179287882));
#220986=CARTESIAN_POINT('Ctrl Pts',(13.111238199284,52.9649231366537,-213.127512319222));
#220987=CARTESIAN_POINT('Ctrl Pts',(12.8139330465279,52.9823892815607,-213.069496767474));
#220988=CARTESIAN_POINT('Ctrl Pts',(12.7628798586912,52.9853885648508,-213.059534347269));
#220989=CARTESIAN_POINT('Ctrl Pts',(12.7118203984046,52.9883673151377,-213.049796876756));
#220990=CARTESIAN_POINT('Ctrl Pts',(12.6607543476393,52.9913255531845,-213.040283642667));
#220991=CARTESIAN_POINT('Ctrl Pts',(11.9341251305787,53.033418923704,-212.904917900964));
#220992=CARTESIAN_POINT('Ctrl Pts',(11.2065836165116,53.0713381586144,-212.814853696238));
#220993=CARTESIAN_POINT('Ctrl Pts',(10.4781609695859,53.1051019822928,-212.767914897224));
#220994=CARTESIAN_POINT('Ctrl Pts',(9.84365029734438,53.1345128010667,-212.727027688346));
#220995=CARTESIAN_POINT('Ctrl Pts',(9.20847145458215,53.1607704757915,-212.71886382913));
#220996=CARTESIAN_POINT('Ctrl Pts',(8.57265926894805,53.1838840251076,-212.742013573981));
#220997=CARTESIAN_POINT('Ctrl Pts',(8.53829774072219,53.1851331626599,-212.743264667667));
#220998=CARTESIAN_POINT('Ctrl Pts',(8.50393420974303,53.186373110042,-212.744608085481));
#220999=CARTESIAN_POINT('Ctrl Pts',(8.46956866922752,53.1876038661027,-212.746043776936));
#221000=CARTESIAN_POINT('Ctrl Pts',(8.05134105999121,53.2025821308736,-212.76351609939));
#221001=CARTESIAN_POINT('Ctrl Pts',(7.63294373529608,53.2161951626094,-212.794632608455));
#221002=CARTESIAN_POINT('Ctrl Pts',(7.21417793555096,53.2284476001673,-212.839302228769));
#221003=CARTESIAN_POINT('Ctrl Pts',(6.95775348625815,53.2359501816942,-212.866654946675));
#221004=CARTESIAN_POINT('Ctrl Pts',(6.7011908579688,53.2429425029055,-212.899090463672));
#221005=CARTESIAN_POINT('Ctrl Pts',(6.44444424425754,53.2494246606916,-212.936597453296));
#221006=CARTESIAN_POINT('Ctrl Pts',(6.41857408693467,53.2500778122144,-212.940376711407));
#221007=CARTESIAN_POINT('Ctrl Pts',(6.39270791173976,53.2507256250243,-212.944206865458));
#221008=CARTESIAN_POINT('Ctrl Pts',(6.36684597343843,53.2513681007524,-212.948087807708));
#221009=CARTESIAN_POINT('Ctrl Pts',(6.07745447788328,53.2585573148641,-212.991515012155));
#221010=CARTESIAN_POINT('Ctrl Pts',(5.78889207385616,53.2650712745851,-213.041253048807));
#221011=CARTESIAN_POINT('Ctrl Pts',(5.50128323027576,53.270919363331,-213.097172229243));
#221012=CARTESIAN_POINT('Ctrl Pts',(5.46169210968322,53.2717243886004,-213.10486984726));
#221013=CARTESIAN_POINT('Ctrl Pts',(5.42211906881833,53.272516787632,-213.112684672594));
#221014=CARTESIAN_POINT('Ctrl Pts',(5.38256444434729,53.2732965767615,-213.120616442334));
#221015=CARTESIAN_POINT('Ctrl Pts',(5.3611025543334,53.273719681487,-213.124920130514));
#221016=CARTESIAN_POINT('Ctrl Pts',(5.3396451356634,53.2741390978143,-213.129258387298));
#221017=CARTESIAN_POINT('Ctrl Pts',(5.31819206008386,53.2745548325864,-213.133631201848));
#221018=CARTESIAN_POINT('Ctrl Pts',(5.16346960690728,53.2775531674208,-213.165168525801));
#221019=CARTESIAN_POINT('Ctrl Pts',(5.00900884763755,53.2803593125375,-213.198496059741));
#221020=CARTESIAN_POINT('Ctrl Pts',(4.8548075087274,53.282975175313,-213.233598239233));
#221021=CARTESIAN_POINT('Ctrl Pts',(4.83548667519224,53.2833029328383,-213.237996407053));
#221022=CARTESIAN_POINT('Ctrl Pts',(4.81616991445747,53.2836277030468,-213.242422436058));
#221023=CARTESIAN_POINT('Ctrl Pts',(4.79685722222972,53.2839494896213,-213.246876296775));
#221024=CARTESIAN_POINT('Ctrl Pts',(4.72842778016165,53.2850896556584,-213.262657380027));
#221025=CARTESIAN_POINT('Ctrl Pts',(4.66004791848346,53.2861923861431,-213.278788317342));
#221026=CARTESIAN_POINT('Ctrl Pts',(4.59171994251606,53.2872578052511,-213.295267139758));
#221027=CARTESIAN_POINT('Ctrl Pts',(4.5698179350381,53.2875993171566,-213.300549299616));
#221028=CARTESIAN_POINT('Ctrl Pts',(4.54792125858747,53.2879369954791,-213.305867203353));
#221029=CARTESIAN_POINT('Ctrl Pts',(4.5260299888062,53.2882708445054,-213.311220784634));
#221030=CARTESIAN_POINT('Ctrl Pts',(4.51508439514893,53.2884377683898,-213.313897565191));
#221031=CARTESIAN_POINT('Ctrl Pts',(4.50414015314406,53.2886037349587,-213.316583265061));
#221032=CARTESIAN_POINT('Ctrl Pts',(4.49319727224048,53.2887687447573,-213.319277875874));
#221033=CARTESIAN_POINT('Ctrl Pts',(4.48225439119639,53.288933754558,-213.321972486721));
#221034=CARTESIAN_POINT('Ctrl Pts',(4.47131360771932,53.2890977098182,-213.324680797967));
#221035=CARTESIAN_POINT('Ctrl Pts',(4.46037245702231,53.2892609395381,-213.327386711909));
#221036=CARTESIAN_POINT('Ctrl Pts',(4.41660743854964,53.2899138646194,-213.338210470483));
#221037=CARTESIAN_POINT('Ctrl Pts',(4.37281891468805,53.2905575212915,-213.348881124149));
#221038=CARTESIAN_POINT('Ctrl Pts',(4.32900749630779,53.2911918673437,-213.359398181113));
#221039=CARTESIAN_POINT('Ctrl Pts',(4.3117489870416,53.2914417535064,-213.36354113589));
#221040=CARTESIAN_POINT('Ctrl Pts',(4.29448693048927,53.2916901975378,-213.367660294877));
#221041=CARTESIAN_POINT('Ctrl Pts',(4.27722136169741,53.2919371969757,-213.371755612804));
#221042=CARTESIAN_POINT('Ctrl Pts',(3.34936233526414,53.3052110520531,-213.591839743872));
#221043=CARTESIAN_POINT('Ctrl Pts',(2.41131193878792,53.31431299312,-213.743095767745));
#221044=CARTESIAN_POINT('Ctrl Pts',(1.46228217016154,53.3189491272516,-213.820197476168));
#221045=CARTESIAN_POINT('Ctrl Pts',(0.993352427694286,53.3212399101715,
-213.858294578567));
#221046=CARTESIAN_POINT('Ctrl Pts',(0.521742197153976,53.3224404125564,
-213.878287712818));
#221047=CARTESIAN_POINT('Ctrl Pts',(0.0473571427401393,53.3225154460666,
-213.879539002147));
#221048=CARTESIAN_POINT('',(32.9259571996587,50.2082406705958,-216.288179546259));
#221049=CARTESIAN_POINT('Ctrl Pts',(33.8288256585371,50.8425201819751,-213.84207505449));
#221050=CARTESIAN_POINT('Ctrl Pts',(33.8195965630401,50.8433616845868,-213.871510133232));
#221051=CARTESIAN_POINT('Ctrl Pts',(33.8091847500211,50.8440238380756,-213.904584950093));
#221052=CARTESIAN_POINT('Ctrl Pts',(33.7975369080429,50.8442737231641,-213.941293234272));
#221053=CARTESIAN_POINT('Ctrl Pts',(33.7860605485555,50.8445199293808,-213.977461089759));
#221054=CARTESIAN_POINT('Ctrl Pts',(33.7733837057459,50.8443657685501,-214.017156701474));
#221055=CARTESIAN_POINT('Ctrl Pts',(33.7594592797241,50.8435407324466,-214.060358070837));
#221056=CARTESIAN_POINT('Ctrl Pts',(33.7574531295846,50.8434218660538,-214.066582272325));
#221057=CARTESIAN_POINT('Ctrl Pts',(33.7554210983262,50.8432889943485,-214.072879209069));
#221058=CARTESIAN_POINT('Ctrl Pts',(33.7533630630681,50.8431412280489,-214.079248777559));
#221059=CARTESIAN_POINT('Ctrl Pts',(33.743082867682,50.8424031131771,-214.111065729359));
#221060=CARTESIAN_POINT('Ctrl Pts',(33.7321506472359,50.8412946106023,-214.144698787172));
#221061=CARTESIAN_POINT('Ctrl Pts',(33.7205438950311,50.839697062375,-214.180141701911));
#221062=CARTESIAN_POINT('Ctrl Pts',(33.7050682254247,50.8375669980719,-214.227398921562));
#221063=CARTESIAN_POINT('Ctrl Pts',(33.6883933898817,50.8345693205334,-214.277874335582));
#221064=CARTESIAN_POINT('Ctrl Pts',(33.6704630953645,50.8303840566376,-214.3315457339));
#221065=CARTESIAN_POINT('Ctrl Pts',(33.6535595541392,50.8264384560377,-214.382143714498));
#221066=CARTESIAN_POINT('Ctrl Pts',(33.6355453144694,50.8214386172029,-214.435562374112));
#221067=CARTESIAN_POINT('Ctrl Pts',(33.616381403873,50.8150836718686,-214.491738971497));
#221068=CARTESIAN_POINT('Ctrl Pts',(33.5979822127623,50.8089823152004,-214.54567388974));
#221069=CARTESIAN_POINT('Ctrl Pts',(33.5785230926711,50.8016316349254,-214.60215137588));
#221070=CARTESIAN_POINT('Ctrl Pts',(33.5579782849136,50.7927360421654,-214.661078169069));
#221071=CARTESIAN_POINT('Ctrl Pts',(33.5545247916949,50.7912407315431,-214.670983507833));
#221072=CARTESIAN_POINT('Ctrl Pts',(33.5510406454633,50.7897017020583,-214.68095795797));
#221073=CARTESIAN_POINT('Ctrl Pts',(33.5475257550617,50.7881174703285,-214.691000955107));
#221074=CARTESIAN_POINT('Ctrl Pts',(33.5276567606859,50.7791621153292,-214.747772071938));
#221075=CARTESIAN_POINT('Ctrl Pts',(33.5068038044279,50.7687640806476,-214.806738808839));
#221076=CARTESIAN_POINT('Ctrl Pts',(33.4849539835288,50.7566390582463,-214.867785259312));
#221077=CARTESIAN_POINT('Ctrl Pts',(33.4813986178706,50.7546660952435,-214.877718633804));
#221078=CARTESIAN_POINT('Ctrl Pts',(33.4778168848558,50.752647352948,-214.887706978624));
#221079=CARTESIAN_POINT('Ctrl Pts',(33.474208761572,50.7505815441923,-214.897749680414));
#221080=CARTESIAN_POINT('Ctrl Pts',(33.4613176761033,50.7432008326319,-214.93363019694));
#221081=CARTESIAN_POINT('Ctrl Pts',(33.4480895339613,50.7352195121941,-214.970205208588));
#221082=CARTESIAN_POINT('Ctrl Pts',(33.4345241362373,50.7265767845305,-215.007444068341));
#221083=CARTESIAN_POINT('Ctrl Pts',(33.4277414373753,50.7222554206986,-215.026063498218));
#221084=CARTESIAN_POINT('Ctrl Pts',(33.420874423949,50.7177686428876,-215.044848868558));
#221085=CARTESIAN_POINT('Ctrl Pts',(33.4139232666345,50.7131085754662,-215.063795757132));
#221086=CARTESIAN_POINT('Ctrl Pts',(33.4104476879772,50.7107785417556,-215.073269201418));
#221087=CARTESIAN_POINT('Ctrl Pts',(33.4069510734007,50.7084051816795,-215.082783023661));
#221088=CARTESIAN_POINT('Ctrl Pts',(33.4034334518911,50.7059874903625,-215.092336644895));
#221089=CARTESIAN_POINT('Ctrl Pts',(33.4006142359874,50.7040498191854,-215.099993443913));
#221090=CARTESIAN_POINT('Ctrl Pts',(33.3974201203686,50.7018312093553,-215.108655100518));
#221091=CARTESIAN_POINT('Ctrl Pts',(33.3947200356436,50.6999375550647,-215.115966490004));
#221092=CARTESIAN_POINT('Ctrl Pts',(33.3941967810423,50.6995705801652,-215.117383378206));
#221093=CARTESIAN_POINT('Ctrl Pts',(33.3936920899953,50.6992159596698,-215.118749616727));
#221094=CARTESIAN_POINT('Ctrl Pts',(33.3932122995932,50.6988783027811,-215.120048145458));
#221095=CARTESIAN_POINT('Ctrl Pts',(33.3930787584929,50.698784322009,-215.120409567768));
#221096=CARTESIAN_POINT('Ctrl Pts',(33.3929471464134,50.6986916573888,-215.120765745917));
#221097=CARTESIAN_POINT('Ctrl Pts',(33.3928176000307,50.6986004087735,-215.121116312229));
#221098=CARTESIAN_POINT('Ctrl Pts',(33.3296193541769,50.6540854458574,-215.292137497787));
#221099=CARTESIAN_POINT('Ctrl Pts',(33.269750414294,50.6027332408916,-215.448578025303));
#221100=CARTESIAN_POINT('Ctrl Pts',(33.213875240217,50.5483631417154,-215.590759975443));
#221101=CARTESIAN_POINT('Ctrl Pts',(33.1849670106321,50.520233595177,-215.664320881971));
#221102=CARTESIAN_POINT('Ctrl Pts',(33.157127397143,50.4912973997056,-215.734065604051));
#221103=CARTESIAN_POINT('Ctrl Pts',(33.130445480466,50.4620814546802,-215.800037964159));
#221104=CARTESIAN_POINT('Ctrl Pts',(33.1027008264358,50.4317018422744,-215.868637994993));
#221105=CARTESIAN_POINT('Ctrl Pts',(33.076200305561,50.4010143910844,-215.933180065315));
#221106=CARTESIAN_POINT('Ctrl Pts',(33.0509711670511,50.3705041612344,-215.993871545003));
#221107=CARTESIAN_POINT('Ctrl Pts',(33.0258539400521,50.340129268781,-216.054293809189));
#221108=CARTESIAN_POINT('Ctrl Pts',(33.0019968128992,50.3099300470371,-216.110899575011));
#221109=CARTESIAN_POINT('Ctrl Pts',(32.9794222099075,50.2803372957559,-216.163874712886));
#221110=CARTESIAN_POINT('Ctrl Pts',(32.9607164963076,50.2558162208868,-216.207770845074));
#221111=CARTESIAN_POINT('Ctrl Pts',(32.9428912873839,50.2317107069135,-216.249173830476));
#221112=CARTESIAN_POINT('Ctrl Pts',(32.9259571994407,50.208240670622,-216.288179546181));
#221113=CARTESIAN_POINT('',(23.3713075575292,51.175583428683,-216.122695209519));
#221114=CARTESIAN_POINT('Ctrl Pts',(23.3713098772595,51.175574422021,-216.122706729219));
#221115=CARTESIAN_POINT('Ctrl Pts',(23.3842461965447,51.1745227766932,-216.1193823466));
#221116=CARTESIAN_POINT('Ctrl Pts',(23.4031827800646,51.173197367639,-216.114240118892));
#221117=CARTESIAN_POINT('Ctrl Pts',(23.4259755039501,51.172009386705,-216.10752048342));
#221118=CARTESIAN_POINT('Ctrl Pts',(23.4363729991939,51.171582118472,-216.104305205249));
#221119=CARTESIAN_POINT('Ctrl Pts',(23.4422558498776,51.1713690087708,-216.102448446714));
#221120=CARTESIAN_POINT('Ctrl Pts',(23.4450357599012,51.1712750486653,-216.10156219481));
#221121=CARTESIAN_POINT('Ctrl Pts',(23.4463575991215,51.1712315234358,-216.101139270919));
#221122=CARTESIAN_POINT('Ctrl Pts',(23.4531000314565,51.1708420894904,-216.099209074551));
#221123=CARTESIAN_POINT('Ctrl Pts',(23.4715714957454,51.1697457853851,-216.093982383968));
#221124=CARTESIAN_POINT('Ctrl Pts',(23.4828968517328,51.1690699569358,-216.090786189668));
#221125=CARTESIAN_POINT('Ctrl Pts',(23.4997698432704,51.1680649377872,-216.086037310555));
#221126=CARTESIAN_POINT('Ctrl Pts',(23.5077858872702,51.1675887931229,-216.083783508271));
#221127=CARTESIAN_POINT('Ctrl Pts',(23.5133043622529,51.1672613852725,-216.082232402665));
#221128=CARTESIAN_POINT('Ctrl Pts',(23.5175432944616,51.1670102829937,-216.081041398148));
#221129=CARTESIAN_POINT('Ctrl Pts',(23.5684041867088,51.1640002556831,-216.066753810042));
#221130=CARTESIAN_POINT('Ctrl Pts',(23.617522122373,51.1610630770063,-216.053151092884));
#221131=CARTESIAN_POINT('Ctrl Pts',(23.765876757628,51.1521012881781,-216.012658976564));
#221132=CARTESIAN_POINT('Ctrl Pts',(23.8636871351588,51.1460726566935,-215.986741705726));
#221133=CARTESIAN_POINT('Ctrl Pts',(24.0625051787286,51.1335736717109,-215.935672011281));
#221134=CARTESIAN_POINT('Ctrl Pts',(24.1616902419922,51.127214610338,-215.911003826816));
#221135=CARTESIAN_POINT('Ctrl Pts',(24.3595824477507,51.1142829433766,-215.863400783403));
#221136=CARTESIAN_POINT('Ctrl Pts',(24.4562741336651,51.1078470209333,-215.84091768686));
#221137=CARTESIAN_POINT('Ctrl Pts',(24.757680353937,51.0874063464124,-215.773357811072));
#221138=CARTESIAN_POINT('Ctrl Pts',(25.0576479162834,51.0662997370015,-215.711186730808));
#221139=CARTESIAN_POINT('Ctrl Pts',(25.4047677167914,51.0405701572308,-215.648084196));
#221140=CARTESIAN_POINT('Ctrl Pts',(25.5775768522701,51.0274352005315,-215.618890526638));
#221141=CARTESIAN_POINT('Ctrl Pts',(25.6514727371838,51.0217486675082,-215.606884153634));
#221142=CARTESIAN_POINT('Ctrl Pts',(25.7006994792023,51.0179449857611,-215.598992171539));
#221143=CARTESIAN_POINT('Ctrl Pts',(25.7241069658211,51.0161293054655,-215.595287525604));
#221144=CARTESIAN_POINT('Ctrl Pts',(26.1620821414063,50.9820110096248,-215.526965608493));
#221145=CARTESIAN_POINT('Ctrl Pts',(26.5699068021216,50.9480387215192,-215.478347477118));
#221146=CARTESIAN_POINT('Ctrl Pts',(27.173438244869,50.8946136997262,-215.428947554207));
#221147=CARTESIAN_POINT('Ctrl Pts',(27.4731530412198,50.8672827350125,-215.41012941129));
#221148=CARTESIAN_POINT('Ctrl Pts',(27.8188791896975,50.834366423916,-215.398468093662));
#221149=CARTESIAN_POINT('Ctrl Pts',(27.9907131851713,50.8176558576065,-215.395210730458));
#221150=CARTESIAN_POINT('Ctrl Pts',(28.0763674429529,50.809238077671,-215.394225372759));
#221151=CARTESIAN_POINT('Ctrl Pts',(28.1130195236067,50.805617126528,-215.393940931724));
#221152=CARTESIAN_POINT('Ctrl Pts',(28.137441537465,50.8032002031682,-215.393781938839));
#221153=CARTESIAN_POINT('Ctrl Pts',(28.1484568678156,50.8021083756591,-215.393722523643));
#221154=CARTESIAN_POINT('Ctrl Pts',(29.8754561237135,50.6305994564353,-215.386804771997));
#221155=CARTESIAN_POINT('Ctrl Pts',(31.4945003627672,50.4284988051297,-215.684974988241));
#221156=CARTESIAN_POINT('Ctrl Pts',(32.9259571993476,50.2082406704928,-216.288179546395));
#221157=CARTESIAN_POINT('Ctrl Pts',(13.206503688621,52.1340678863284,-215.899726709711));
#221158=CARTESIAN_POINT('Ctrl Pts',(13.21434555531,52.1335848677323,-215.90178674226));
#221159=CARTESIAN_POINT('Ctrl Pts',(13.2231507448613,52.1330862366278,-215.904029229699));
#221160=CARTESIAN_POINT('Ctrl Pts',(13.2322895587349,52.1325819238806,-215.906330078911));
#221161=CARTESIAN_POINT('Ctrl Pts',(13.2421441100756,52.1320381141556,-215.908811126998));
#221162=CARTESIAN_POINT('Ctrl Pts',(13.2523869533356,52.1314876923625,-215.911360109152));
#221163=CARTESIAN_POINT('Ctrl Pts',(13.2622878817901,52.1309421505403,-215.913833109968));
#221164=CARTESIAN_POINT('Ctrl Pts',(13.2644020884909,52.1308256576092,-215.914361185181));
#221165=CARTESIAN_POINT('Ctrl Pts',(13.2665008919367,52.1307093841564,-215.914885832636));
#221166=CARTESIAN_POINT('Ctrl Pts',(13.268577468265,52.1305934374337,-215.915405707262));
#221167=CARTESIAN_POINT('Ctrl Pts',(13.3206494413752,52.1276859716487,-215.92844201957));
#221168=CARTESIAN_POINT('Ctrl Pts',(13.3712586349829,52.1247839437585,-215.940981499432));
#221169=CARTESIAN_POINT('Ctrl Pts',(13.4220397900242,52.1218170785976,-215.953412057766));
#221170=CARTESIAN_POINT('Ctrl Pts',(13.4721084324292,52.1188918416532,-215.965668202386));
#221171=CARTESIAN_POINT('Ctrl Pts',(13.5223442093494,52.1159035600009,-215.977818360123));
#221172=CARTESIAN_POINT('Ctrl Pts',(13.5743125134382,52.1127772956712,-215.990186103883));
#221173=CARTESIAN_POINT('Ctrl Pts',(13.6237866881243,52.1098010710228,-216.001960279046));
#221174=CARTESIAN_POINT('Ctrl Pts',(13.6748310589708,52.106699798131,-216.01393169343));
#221175=CARTESIAN_POINT('Ctrl Pts',(13.7287953846035,52.1034020067022,-216.026336308893));
#221176=CARTESIAN_POINT('Ctrl Pts',(13.7581476789267,52.1016082708685,-216.033083431548));
#221177=CARTESIAN_POINT('Ctrl Pts',(13.7883638330608,52.0997562789374,-216.039957977688));
#221178=CARTESIAN_POINT('Ctrl Pts',(13.8196609440104,52.0978335624414,-216.046991805997));
#221179=CARTESIAN_POINT('Ctrl Pts',(13.8490469338718,52.0960282543556,-216.053596121894));
#221180=CARTESIAN_POINT('Ctrl Pts',(13.8789171341203,52.0941830434785,-216.060245085436));
#221181=CARTESIAN_POINT('Ctrl Pts',(13.9092735522173,52.0922980630924,-216.066930897808));
#221182=CARTESIAN_POINT('Ctrl Pts',(13.9325325762528,52.0908537950643,-216.072053553259));
#221183=CARTESIAN_POINT('Ctrl Pts',(13.9518947805123,52.0896438292969,-216.076285734692));
#221184=CARTESIAN_POINT('Ctrl Pts',(13.9714301061238,52.0884198382981,-216.080530595315));
#221185=CARTESIAN_POINT('Ctrl Pts',(13.9773912291603,52.0880463425559,-216.081825896809));
#221186=CARTESIAN_POINT('Ctrl Pts',(13.9833684716841,52.0876714833885,-216.083122015781));
#221187=CARTESIAN_POINT('Ctrl Pts',(13.9894774736147,52.0872880602886,-216.08444370039));
#221188=CARTESIAN_POINT('Ctrl Pts',(14.0417353629624,52.0840081657732,-216.095749712219));
#221189=CARTESIAN_POINT('Ctrl Pts',(14.0940361976639,52.080693570248,-216.10686308862));
#221190=CARTESIAN_POINT('Ctrl Pts',(14.1463794799969,52.0773442814346,-216.117783727481));
#221191=CARTESIAN_POINT('Ctrl Pts',(14.2116086830721,52.0731704614059,-216.131392819961));
#221192=CARTESIAN_POINT('Ctrl Pts',(14.2770368470204,52.0689342305803,-216.144729384953));
#221193=CARTESIAN_POINT('Ctrl Pts',(14.3424131370686,52.0646515126906,-216.157742539444));
#221194=CARTESIAN_POINT('Ctrl Pts',(14.3819594720578,52.0620608824145,-216.165614239817));
#221195=CARTESIAN_POINT('Ctrl Pts',(14.4214887322589,52.0594530513133,-216.173367856955));
#221196=CARTESIAN_POINT('Ctrl Pts',(14.4609448354491,52.0568318528244,-216.180993676633));
#221197=CARTESIAN_POINT('Ctrl Pts',(14.6703112873129,52.0429229519732,-216.221458666319));
#221198=CARTESIAN_POINT('Ctrl Pts',(14.8802278373797,52.0284671787079,-216.258828965844));
#221199=CARTESIAN_POINT('Ctrl Pts',(15.0906678685067,52.0134661474936,-216.29311301509));
#221200=CARTESIAN_POINT('Ctrl Pts',(15.2048442057614,52.0053271884281,-216.311714167866));
#221201=CARTESIAN_POINT('Ctrl Pts',(15.3196612788897,51.9969923389717,-216.329481780615));
#221202=CARTESIAN_POINT('Ctrl Pts',(15.4343240930968,51.9885185807898,-216.346290289808));
#221203=CARTESIAN_POINT('Ctrl Pts',(15.4912716221164,51.9843100708792,-216.354638271424));
#221204=CARTESIAN_POINT('Ctrl Pts',(15.5481810921433,51.9800674264624,-216.362750478828));
#221205=CARTESIAN_POINT('Ctrl Pts',(15.6049550958312,51.9757983834695,-216.37061622704));
#221206=CARTESIAN_POINT('Ctrl Pts',(15.6432593674605,51.972918146534,-216.375923088218));
#221207=CARTESIAN_POINT('Ctrl Pts',(15.6815019757728,51.9700259035013,-216.381117827339));
#221208=CARTESIAN_POINT('Ctrl Pts',(15.7196530119027,51.9671241561828,-216.386197949282));
#221209=CARTESIAN_POINT('Ctrl Pts',(15.7321491591731,51.9661737059327,-216.387861913316));
#221210=CARTESIAN_POINT('Ctrl Pts',(15.7446430517792,51.9652216618178,-216.38951459821));
#221211=CARTESIAN_POINT('Ctrl Pts',(15.757141562356,51.964267500545,-216.391156918244));
#221212=CARTESIAN_POINT('Ctrl Pts',(16.1023878232211,51.9379107110961,-216.436522711827));
#221213=CARTESIAN_POINT('Ctrl Pts',(16.4495094479191,51.9100635699139,-216.473758372625));
#221214=CARTESIAN_POINT('Ctrl Pts',(16.7982755207299,51.8807308388097,-216.502811102886));
#221215=CARTESIAN_POINT('Ctrl Pts',(16.9356744178246,51.8691749989024,-216.514256634452));
#221216=CARTESIAN_POINT('Ctrl Pts',(17.0733636198955,51.8573836148247,-216.524441248057));
#221217=CARTESIAN_POINT('Ctrl Pts',(17.2113121006742,51.8453591541769,-216.533361219666));
#221218=CARTESIAN_POINT('Ctrl Pts',(17.3873312366818,51.8300162148257,-216.544742901341));
#221219=CARTESIAN_POINT('Ctrl Pts',(17.563780758969,51.8142931202842,-216.554066374654));
#221220=CARTESIAN_POINT('Ctrl Pts',(17.740651385583,51.798190546547,-216.561329640317));
#221221=CARTESIAN_POINT('Ctrl Pts',(17.82908669889,51.7901392596783,-216.564961273148));
#221222=CARTESIAN_POINT('Ctrl Pts',(17.9176273123319,51.7819931029086,-216.568077867492));
#221223=CARTESIAN_POINT('Ctrl Pts',(18.0062721385295,51.7737521657921,-216.57067924594));
#221224=CARTESIAN_POINT('Ctrl Pts',(18.0284333450789,51.771691931513,-216.571329590552));
#221225=CARTESIAN_POINT('Ctrl Pts',(18.0506010648767,51.7696257735029,-216.571947734384));
#221226=CARTESIAN_POINT('Ctrl Pts',(18.0727752807906,51.767553693247,-216.572533675092));
#221227=CARTESIAN_POINT('Ctrl Pts',(18.0826472293756,51.7666312042702,-216.572794535568));
#221228=CARTESIAN_POINT('Ctrl Pts',(18.0925204655065,51.7657075414897,-216.573049013306));
#221229=CARTESIAN_POINT('Ctrl Pts',(18.1023949876674,51.7647827050386,-216.573297108109));
#221230=CARTESIAN_POINT('Ctrl Pts',(18.1081226892839,51.7642462550566,-216.573441015123));
#221231=CARTESIAN_POINT('Ctrl Pts',(18.1138457806533,51.7637098836875,-216.573582655078));
#221232=CARTESIAN_POINT('Ctrl Pts',(18.1195929857986,51.763170895431,-216.573722717714));
#221233=CARTESIAN_POINT('Ctrl Pts',(18.1603576817877,51.7593478733078,-216.574716176378));
#221234=CARTESIAN_POINT('Ctrl Pts',(18.2020533295113,51.7554188871131,-216.575618681072));
#221235=CARTESIAN_POINT('Ctrl Pts',(18.2422451882278,51.7516141613284,-216.576382388678));
#221236=CARTESIAN_POINT('Ctrl Pts',(18.2524463154636,51.750648480888,-216.576576225905));
#221237=CARTESIAN_POINT('Ctrl Pts',(18.2625505722048,51.7496908479096,-216.576761383499));
#221238=CARTESIAN_POINT('Ctrl Pts',(18.2725181564702,51.748745111455,-216.576937599951));
#221239=CARTESIAN_POINT('Ctrl Pts',(18.7428983089622,51.7041148734871,-216.585253428466));
#221240=CARTESIAN_POINT('Ctrl Pts',(19.216369753222,51.6568224052065,-216.57911957981));
#221241=CARTESIAN_POINT('Ctrl Pts',(19.6931266362225,51.6068304012012,-216.55847565067));
#221242=CARTESIAN_POINT('Ctrl Pts',(20.1859350419897,51.555155258852,-216.537136678604));
#221243=CARTESIAN_POINT('Ctrl Pts',(20.6822542104159,51.5005957234902,-216.500293855085));
#221244=CARTESIAN_POINT('Ctrl Pts',(21.182281606225,51.4431025697233,-216.447827972626));
#221245=CARTESIAN_POINT('Ctrl Pts',(21.3543133005346,51.4233223642053,-216.429777372342));
#221246=CARTESIAN_POINT('Ctrl Pts',(21.5267837552778,51.4031948498831,-216.409877098555));
#221247=CARTESIAN_POINT('Ctrl Pts',(21.6997004409249,51.38271782281,-216.388121030837));
#221248=CARTESIAN_POINT('Ctrl Pts',(21.9953744771053,51.3477037047621,-216.350919853117));
#221249=CARTESIAN_POINT('Ctrl Pts',(22.2925066862195,51.3116541950269,-216.308265698683));
#221250=CARTESIAN_POINT('Ctrl Pts',(22.5903904274446,51.2746319829009,-216.260299999768));
#221251=CARTESIAN_POINT('Ctrl Pts',(22.6888701076597,51.2623925246612,-216.244442649947));
#221252=CARTESIAN_POINT('Ctrl Pts',(22.7874315150287,51.2500467878896,-216.228004830549));
#221253=CARTESIAN_POINT('Ctrl Pts',(22.8860478603066,51.2375971391525,-216.21099182717));
#221254=CARTESIAN_POINT('Ctrl Pts',(22.8969925217376,51.2362154494338,-216.209103686199));
#221255=CARTESIAN_POINT('Ctrl Pts',(22.9079381323242,51.2348324777314,-216.207208369015));
#221256=CARTESIAN_POINT('Ctrl Pts',(22.9188844817569,51.233448249318,-216.205305911946));
#221257=CARTESIAN_POINT('Ctrl Pts',(23.0199556227651,51.2206672262,-216.187739918103));
#221258=CARTESIAN_POINT('Ctrl Pts',(23.1211180993683,51.2077756142702,-216.169561242903));
#221259=CARTESIAN_POINT('Ctrl Pts',(23.2222432186999,51.1947893198607,-216.150796397354));
#221260=CARTESIAN_POINT('Ctrl Pts',(23.2474937923346,51.1915466894895,-216.14611088383));
#221261=CARTESIAN_POINT('Ctrl Pts',(23.2727420420805,51.1882981597227,-216.141388850273));
#221262=CARTESIAN_POINT('Ctrl Pts',(23.2979859748199,51.1850439859153,-216.136630762429));
#221263=CARTESIAN_POINT('Ctrl Pts',(23.310606184657,51.1834171254447,-216.134252049585));
#221264=CARTESIAN_POINT('Ctrl Pts',(23.3232253155973,51.1817888544157,-216.131864325995));
#221265=CARTESIAN_POINT('Ctrl Pts',(23.3358431189853,51.180159205015,-216.129467651824));
#221266=CARTESIAN_POINT('Ctrl Pts',(23.3476893197676,51.1786292117656,-216.127217538822));
#221267=CARTESIAN_POINT('Ctrl Pts',(23.3616078199705,51.1763334684996,-216.125238790202));
#221268=CARTESIAN_POINT('Ctrl Pts',(23.3713052124462,51.1755924372823,-216.1226836965));
#221269=CARTESIAN_POINT('Ctrl Pts',(32.9259571993474,50.2082406704929,-216.288179546395));
#221270=CARTESIAN_POINT('Ctrl Pts',(33.2211981697202,50.1902923385546,-216.363964513646));
#221271=CARTESIAN_POINT('Ctrl Pts',(33.5148860377456,50.119298258903,-216.408010072973));
#221272=CARTESIAN_POINT('Ctrl Pts',(33.085259856697,50.4290321519905,-215.921237668862));
#221273=CARTESIAN_POINT('Ctrl Pts',(33.3343836373402,50.4107015464113,-215.980471424072));
#221274=CARTESIAN_POINT('Ctrl Pts',(33.5814103734301,50.3541144443598,-216.021456775784));
#221275=CARTESIAN_POINT('Ctrl Pts',(33.241157299543,50.5918672086098,-215.531581018364));
#221276=CARTESIAN_POINT('Ctrl Pts',(33.4420534427606,50.5741543933337,-215.576409379719));
#221277=CARTESIAN_POINT('Ctrl Pts',(33.6410713756206,50.5314895370126,-215.611814434793));
#221278=CARTESIAN_POINT('Ctrl Pts',(33.5452672954357,50.8058893973708,-214.708515271655));
#221279=CARTESIAN_POINT('Ctrl Pts',(33.6463864491617,50.7933600420917,-214.728899815191));
#221280=CARTESIAN_POINT('Ctrl Pts',(33.74687298472,50.7754606859937,-214.748374319679));
#221281=CARTESIAN_POINT('Ctrl Pts',(33.6935058134431,50.8548585528471,-214.273661258903));
#221282=CARTESIAN_POINT('Ctrl Pts',(33.7431496001434,50.8473673908384,-214.28335774542));
#221283=CARTESIAN_POINT('Ctrl Pts',(33.7927859204527,50.839876592974,-214.293095991117));
#221284=CARTESIAN_POINT('Ctrl Pts',(33.8288256585371,50.8425201819751,-213.84207505449));
#221285=CARTESIAN_POINT('Ctrl Pts',(33.8288256585371,50.8425201819751,-213.84207505449));
#221286=CARTESIAN_POINT('Ctrl Pts',(33.8288256585371,50.8425201819751,-213.84207505449));
#221287=CARTESIAN_POINT('',(33.5148860365099,50.1192982504877,-216.408010067648));
#221288=CARTESIAN_POINT('Ctrl Pts',(33.828825603085,50.8425198058687,-213.84207504786));
#221289=CARTESIAN_POINT('Ctrl Pts',(33.8203599637206,50.8418988523823,-213.948018702658));
#221290=CARTESIAN_POINT('Ctrl Pts',(33.8113602728046,50.8379426869151,-214.054203876756));
#221291=CARTESIAN_POINT('Ctrl Pts',(33.801851649264,50.8306220685841,-214.160265521188));
#221292=CARTESIAN_POINT('Ctrl Pts',(33.7923627726763,50.8233166532847,-214.266106903004));
#221293=CARTESIAN_POINT('Ctrl Pts',(33.782367072251,50.8126607033274,-214.371824659818));
#221294=CARTESIAN_POINT('Ctrl Pts',(33.7718970641518,50.7986764690415,-214.477053509786));
#221295=CARTESIAN_POINT('Ctrl Pts',(33.7614327641875,50.7846998588086,-214.582224990125));
#221296=CARTESIAN_POINT('Ctrl Pts',(33.7504946875091,50.7673986651718,-214.686907490459));
#221297=CARTESIAN_POINT('Ctrl Pts',(33.739122769926,50.7468461932371,-214.790742945814));
#221298=CARTESIAN_POINT('Ctrl Pts',(33.7277363195123,50.726267456111,-214.894711098498));
#221299=CARTESIAN_POINT('Ctrl Pts',(33.7159149485736,50.7024293080928,-214.997829456524));
#221300=CARTESIAN_POINT('Ctrl Pts',(33.7037059133141,50.6754546714005,-215.099754179867));
#221301=CARTESIAN_POINT('Ctrl Pts',(33.7004879085736,50.6683448132581,-215.126619057879));
#221302=CARTESIAN_POINT('Ctrl Pts',(33.6972430090231,50.6610173127084,-215.153401121628));
#221303=CARTESIAN_POINT('Ctrl Pts',(33.6939721578997,50.6534749601291,-215.180094331735));
#221304=CARTESIAN_POINT('Ctrl Pts',(33.680746959044,50.6229785819881,-215.288024347028));
#221305=CARTESIAN_POINT('Ctrl Pts',(33.6670909984717,50.5889646595794,-215.394538656221));
#221306=CARTESIAN_POINT('Ctrl Pts',(33.6530129144354,50.5514703365522,-215.499660268446));
#221307=CARTESIAN_POINT('Ctrl Pts',(33.6390782603778,50.5143580122358,-215.603710883327));
#221308=CARTESIAN_POINT('Ctrl Pts',(33.62472996409,50.4738353334169,-215.706398080906));
#221309=CARTESIAN_POINT('Ctrl Pts',(33.6099691795183,50.4298895667813,-215.807726784846));
#221310=CARTESIAN_POINT('Ctrl Pts',(33.5949804948845,50.3852652967167,-215.910619959686));
#221311=CARTESIAN_POINT('Ctrl Pts',(33.5795664055371,50.337110875308,-216.012113461442));
#221312=CARTESIAN_POINT('Ctrl Pts',(33.5637217734253,50.2853700999101,-216.112178111571));
#221313=CARTESIAN_POINT('Ctrl Pts',(33.5478771413135,50.2336293245122,-216.2122427617));
#221314=CARTESIAN_POINT('Ctrl Pts',(33.5316018373211,50.1783013178955,-216.310879445869));
#221315=CARTESIAN_POINT('Ctrl Pts',(33.5148860340386,50.1192982336575,-216.408010056999));
#221316=CARTESIAN_POINT('Origin',(33.1454591002416,47.6034469977721,-214.816150729402));
#221317=CARTESIAN_POINT('Ctrl Pts',(42.4267736782988,48.5085693923201,-216.591605848694));
#221318=CARTESIAN_POINT('Ctrl Pts',(42.583706717545,49.3531444934432,-215.348104479787));
#221319=CARTESIAN_POINT('Ctrl Pts',(42.5875626890161,49.379257463449,-213.836967828456));
#221320=CARTESIAN_POINT('Ctrl Pts',(39.4353118162483,49.0695244129458,-216.590608342213));
#221321=CARTESIAN_POINT('Ctrl Pts',(39.5811128234,49.9141052314507,-215.348112574353));
#221322=CARTESIAN_POINT('Ctrl Pts',(39.5843350108959,49.9402879854258,-213.83895548199));
#221323=CARTESIAN_POINT('Ctrl Pts',(36.428830517738,49.5716582570521,-216.58986415622));
#221324=CARTESIAN_POINT('Ctrl Pts',(36.5632179392288,50.4163761404316,-215.34823479602));
#221325=CARTESIAN_POINT('Ctrl Pts',(36.5662930978424,50.4425286599252,-213.840777099111));
#221326=CARTESIAN_POINT('Ctrl Pts',(33.4195851394632,50.0130984955555,-216.589106829638));
#221327=CARTESIAN_POINT('Ctrl Pts',(33.542491458609,50.8579889698439,-215.348218150781));
#221328=CARTESIAN_POINT('Ctrl Pts',(33.5455787101075,50.8841045229765,-213.842210502424));
#221329=CARTESIAN_POINT('',(33.4734406969954,50.0051916611406,-216.589120383859));
#221330=CARTESIAN_POINT('',(42.426773677794,48.5085693922785,-216.591605848887));
#221331=CARTESIAN_POINT('Ctrl Pts',(33.4734406957278,50.0051916525032,-216.589120377853));
#221332=CARTESIAN_POINT('Ctrl Pts',(34.6872050562177,49.8268448619461,-216.589425787482));
#221333=CARTESIAN_POINT('Ctrl Pts',(35.900785979965,49.6385891008449,-216.589729376108));
#221334=CARTESIAN_POINT('Ctrl Pts',(37.1141764064761,49.4403902132283,-216.590048882378));
#221335=CARTESIAN_POINT('Ctrl Pts',(38.3138694840402,49.2444286923036,-216.590364781903));
#221336=CARTESIAN_POINT('Ctrl Pts',(39.5133769998352,49.038747081503,-216.590696227305));
#221337=CARTESIAN_POINT('Ctrl Pts',(40.7126774431349,48.8232639614083,-216.591060621883));
#221338=CARTESIAN_POINT('Ctrl Pts',(41.2840915331536,48.720595700364,-216.591234239927));
#221339=CARTESIAN_POINT('Ctrl Pts',(41.8554583384076,48.6157016985461,-216.591415342921));
#221340=CARTESIAN_POINT('Ctrl Pts',(42.4267736778188,48.5085693924101,-216.591605848693));
#221341=CARTESIAN_POINT('Origin',(31.3861213810748,49.6296476280943,-215.743606971984));
#221342=CARTESIAN_POINT('',(42.5875626890161,49.379257463449,-213.836967828456));
#221343=CARTESIAN_POINT('Origin',(32.5120060875395,16.8401705115765,-213.68691157036));
#221344=CARTESIAN_POINT('Origin',(41.6694842675319,44.465041620637,-213.749705796269));
#221345=CARTESIAN_POINT('Ctrl Pts',(32.8943360433596,50.1648136138274,-216.360311415042));
#221346=CARTESIAN_POINT('Ctrl Pts',(33.1846932575851,50.1143213461432,-216.493132115846));
#221347=CARTESIAN_POINT('Ctrl Pts',(33.4734406974176,50.0051916640201,-216.589120385861));
#221348=CARTESIAN_POINT('Ctrl Pts',(32.9074380702227,50.1790964451624,-216.336991557183));
#221349=CARTESIAN_POINT('Ctrl Pts',(33.1995861132115,50.1392297940232,-216.451282693355));
#221350=CARTESIAN_POINT('Ctrl Pts',(33.4901672823063,50.0432442151984,-216.530872105694));
#221351=CARTESIAN_POINT('Ctrl Pts',(32.9180956124805,50.1935640066324,-216.312978006505));
#221352=CARTESIAN_POINT('Ctrl Pts',(33.2118808797868,50.1645315900617,-216.408280615883));
#221353=CARTESIAN_POINT('Ctrl Pts',(33.5041153010624,50.0812800820291,-216.470595425695));
#221354=CARTESIAN_POINT('Ctrl Pts',(32.9259571993478,50.2082406704929,-216.288179546395));
#221355=CARTESIAN_POINT('Ctrl Pts',(33.2211981697207,50.1902923385545,-216.363964513646));
#221356=CARTESIAN_POINT('Ctrl Pts',(33.514886037746,50.1192982589029,-216.408010072973));
#221357=CARTESIAN_POINT('',(32.8943360433598,50.1648136138275,-216.360311415042));
#221358=CARTESIAN_POINT('Origin',(33.114566694526,47.5599010752717,-214.888601821826));
#221359=CARTESIAN_POINT('Ctrl Pts',(32.9259571993478,50.2082406704928,-216.288179546395));
#221360=CARTESIAN_POINT('Ctrl Pts',(32.9213942089986,50.1997220625292,-216.302573035724));
#221361=CARTESIAN_POINT('Ctrl Pts',(32.9158742467131,50.1912547814121,-216.316733684137));
#221362=CARTESIAN_POINT('Ctrl Pts',(32.9095161990492,50.1828980465912,-216.330573580559));
#221363=CARTESIAN_POINT('Ctrl Pts',(32.9048796509347,50.1768039741453,-216.340666198458));
#221364=CARTESIAN_POINT('Ctrl Pts',(32.8997987066436,50.1707685930943,-216.350588604011));
#221365=CARTESIAN_POINT('Ctrl Pts',(32.8943360433598,50.1648136138274,-216.360311415041));
#221366=CARTESIAN_POINT('Ctrl Pts',(43.8236246153786,48.0167834579706,-216.751202893194));
#221367=CARTESIAN_POINT('Ctrl Pts',(43.7824688833554,49.1245550970912,-215.437118008003));
#221368=CARTESIAN_POINT('Ctrl Pts',(43.4788788509402,49.2125323561774,-213.747150416911));
#221369=CARTESIAN_POINT('Ctrl Pts',(43.7070375561973,48.0584796180488,-216.749598999916));
#221370=CARTESIAN_POINT('Ctrl Pts',(43.6780057882132,49.1445743904358,-215.439141898609));
#221371=CARTESIAN_POINT('Ctrl Pts',(43.3960890720396,49.2280611496102,-213.762531770702));
#221372=CARTESIAN_POINT('Ctrl Pts',(43.5769822704868,48.1075829537179,-216.741403895083));
#221373=CARTESIAN_POINT('Ctrl Pts',(43.5654977323301,49.1661436865509,-215.436130708587));
#221374=CARTESIAN_POINT('Ctrl Pts',(43.3131689559366,49.2435966472704,-213.776308010994));
#221375=CARTESIAN_POINT('Ctrl Pts',(43.3411495534845,48.1931491450329,-216.723561139181));
#221376=CARTESIAN_POINT('Ctrl Pts',(43.360551859855,49.2053294166112,-215.42835185675));
#221377=CARTESIAN_POINT('Ctrl Pts',(43.1590773754414,49.2724456764506,-213.798159517638));
#221378=CARTESIAN_POINT('Ctrl Pts',(43.2329881782316,48.2313298419848,-216.7140760013));
#221379=CARTESIAN_POINT('Ctrl Pts',(43.2666405269032,49.2232479005123,-215.423740216265));
#221380=CARTESIAN_POINT('Ctrl Pts',(43.0879593352497,49.2857509575947,-213.806842606535));
#221381=CARTESIAN_POINT('Ctrl Pts',(43.0131869934634,48.3080252308524,-216.690346042172));
#221382=CARTESIAN_POINT('Ctrl Pts',(43.0771008479443,49.25936156653,-215.41076207127));
#221383=CARTESIAN_POINT('Ctrl Pts',(42.9454754544989,49.3123914274194,-213.82126574075));
#221384=CARTESIAN_POINT('Ctrl Pts',(42.9009214691654,48.3469469661758,-216.675816338558));
#221385=CARTESIAN_POINT('Ctrl Pts',(42.9810968950835,49.2776314124782,-215.402200104636));
#221386=CARTESIAN_POINT('Ctrl Pts',(42.8741106150282,49.325726212528,-213.827018288817));
#221387=CARTESIAN_POINT('Ctrl Pts',(42.6462982590026,48.4352161716465,-216.634760492906));
#221388=CARTESIAN_POINT('Ctrl Pts',(42.7667553785484,49.3184005119929,-215.376486525154));
#221389=CARTESIAN_POINT('Ctrl Pts',(42.7188997255464,49.3547228975728,-213.835548827928));
#221390=CARTESIAN_POINT('Ctrl Pts',(42.5029768685179,48.4845286599184,-216.606768911376));
#221391=CARTESIAN_POINT('Ctrl Pts',(42.6479264611755,49.3409861001092,-215.358258220572));
#221392=CARTESIAN_POINT('Ctrl Pts',(42.6349927775592,49.3703969686686,-213.837560447468));
#221393=CARTESIAN_POINT('Ctrl Pts',(42.3669756126708,48.5277324522344,-216.579923496877));
#221394=CARTESIAN_POINT('Ctrl Pts',(42.5335765527017,49.3626423449188,-215.340343539781));
#221395=CARTESIAN_POINT('Ctrl Pts',(42.5508500423968,49.3861157519262,-213.836818243375));
#221396=CARTESIAN_POINT('',(43.4427334535923,49.2193110042465,-213.753761106585));
#221397=CARTESIAN_POINT('',(43.7719279964152,48.0354975596111,-216.750009718968));
#221398=CARTESIAN_POINT('Origin',(42.506225613034,44.3085739513886,-213.666499074398));
#221399=CARTESIAN_POINT('Ctrl Pts',(42.4267736781731,48.508569392226,-216.591605848995));
#221400=CARTESIAN_POINT('Ctrl Pts',(42.5057689245607,48.4828880590072,-216.607095809672));
#221401=CARTESIAN_POINT('Ctrl Pts',(42.575038200036,48.4597022300457,-216.619925307791));
#221402=CARTESIAN_POINT('Ctrl Pts',(42.6601019032662,48.4307995702034,-216.635178861068));
#221403=CARTESIAN_POINT('Ctrl Pts',(42.6853248155618,48.4221459310976,-216.639598263176));
#221404=CARTESIAN_POINT('Ctrl Pts',(42.7180424554192,48.4108740731269,-216.645229692863));
#221405=CARTESIAN_POINT('Ctrl Pts',(42.733123554025,48.4056646763262,-216.647795989338));
#221406=CARTESIAN_POINT('Ctrl Pts',(42.7484073760464,48.4003773583356,-216.650353519746));
#221407=CARTESIAN_POINT('Ctrl Pts',(42.754455589884,48.3982847882281,-216.651356072319));
#221408=CARTESIAN_POINT('Ctrl Pts',(42.75837545544,48.396928711148,-216.652003655836));
#221409=CARTESIAN_POINT('Ctrl Pts',(42.758272534821,48.396964146891,-216.651987901739));
#221410=CARTESIAN_POINT('Ctrl Pts',(42.8237908566439,48.3743057303187,-216.662734627152));
#221411=CARTESIAN_POINT('Ctrl Pts',(42.883124963599,48.3536052295174,-216.671690111223));
#221412=CARTESIAN_POINT('Ctrl Pts',(42.9675591338409,48.324082926417,-216.683384715795));
#221413=CARTESIAN_POINT('Ctrl Pts',(42.9949458054802,48.3144969358278,-216.686993147063));
#221414=CARTESIAN_POINT('Ctrl Pts',(43.0479583477075,48.2959547366843,-216.693630469087));
#221415=CARTESIAN_POINT('Ctrl Pts',(43.0723486758755,48.2874289836569,-216.69652208628));
#221416=CARTESIAN_POINT('Ctrl Pts',(43.1499857554147,48.2603817225497,-216.705151268472));
#221417=CARTESIAN_POINT('Ctrl Pts',(43.2040029954931,48.2414864744923,-216.710625663544));
#221418=CARTESIAN_POINT('Ctrl Pts',(43.2882855452362,48.211708547662,-216.718419666566));
#221419=CARTESIAN_POINT('Ctrl Pts',(43.3312401528149,48.1964607001404,-216.722212270681));
#221420=CARTESIAN_POINT('Ctrl Pts',(43.3753820418788,48.1806472701165,-216.725848278702));
#221421=CARTESIAN_POINT('Ctrl Pts',(43.4050695940576,48.169976191394,-216.728237484917));
#221422=CARTESIAN_POINT('Ctrl Pts',(43.4180564137545,48.1652953793453,-216.729262098874));
#221423=CARTESIAN_POINT('Ctrl Pts',(43.5718487752363,48.10963028015,-216.741073640917));
#221424=CARTESIAN_POINT('Ctrl Pts',(43.6853875967172,48.0669209671252,-216.747552049762));
#221425=CARTESIAN_POINT('Ctrl Pts',(43.7719279964152,48.0354975596111,-216.750009718968));
#221426=CARTESIAN_POINT('Ctrl Pts',(43.4427334535923,49.2193110042462,-213.753761106585));
#221427=CARTESIAN_POINT('Ctrl Pts',(43.3719706400381,49.2325796186167,-213.766495780037));
#221428=CARTESIAN_POINT('Ctrl Pts',(43.3010945110738,49.2458572251103,-213.778020270751));
#221429=CARTESIAN_POINT('Ctrl Pts',(43.2300784559227,49.2591528525595,-213.788090955962));
#221430=CARTESIAN_POINT('Ctrl Pts',(43.1590933274703,49.2724426899114,-213.798157255503));
#221431=CARTESIAN_POINT('Ctrl Pts',(43.0879758381644,49.2857478720148,-213.806840936004));
#221432=CARTESIAN_POINT('Ctrl Pts',(43.0167173948743,49.2990711925071,-213.814054173643));
#221433=CARTESIAN_POINT('Ctrl Pts',(42.9454929340351,49.3123881592388,-213.821263971359));
#221434=CARTESIAN_POINT('Ctrl Pts',(42.8741286599837,49.3257228413477,-213.827017297049));
#221435=CARTESIAN_POINT('Ctrl Pts',(42.8025937883447,49.3390870721022,-213.830948922094));
#221436=CARTESIAN_POINT('Ctrl Pts',(42.731095982805,49.3524443781234,-213.83487850995));
#221437=CARTESIAN_POINT('Ctrl Pts',(42.6594242987748,49.3658330544367,-213.836920272795));
#221438=CARTESIAN_POINT('Ctrl Pts',(42.5875626890161,49.3792574634491,-213.836967828456));
#221439=CARTESIAN_POINT('Ctrl Pts',(47.064076521496,46.1934774086348,-216.786882195125));
#221440=CARTESIAN_POINT('Ctrl Pts',(47.7234387387225,47.4080545337851,-215.373546262479));
#221441=CARTESIAN_POINT('Ctrl Pts',(47.6028228022501,47.5293656571523,-213.40423171224));
#221442=CARTESIAN_POINT('Ctrl Pts',(46.9484052815617,46.2805028601163,-216.790124036479));
#221443=CARTESIAN_POINT('Ctrl Pts',(47.5766388725972,47.508813370891,-215.37845116732));
#221444=CARTESIAN_POINT('Ctrl Pts',(47.4422878419382,47.6357207591759,-213.413415509028));
#221445=CARTESIAN_POINT('Ctrl Pts',(46.8302467814474,46.3687247217733,-216.791504353852));
#221446=CARTESIAN_POINT('Ctrl Pts',(47.4263946384086,47.6067406666075,-215.382015347526));
#221447=CARTESIAN_POINT('Ctrl Pts',(47.2794655898102,47.7377048300804,-213.423678997697));
#221448=CARTESIAN_POINT('Ctrl Pts',(46.5987178641575,46.5304722851862,-216.79905959227));
#221449=CARTESIAN_POINT('Ctrl Pts',(47.129483939867,47.7906773992089,-215.393854083401));
#221450=CARTESIAN_POINT('Ctrl Pts',(46.9524663169082,47.931159795535,-213.446422385028));
#221451=CARTESIAN_POINT('Ctrl Pts',(46.4620556574027,46.6321591428633,-216.795250645318));
#221452=CARTESIAN_POINT('Ctrl Pts',(46.9655757003049,47.8868672070918,-215.393231131327));
#221453=CARTESIAN_POINT('Ctrl Pts',(46.7883227793212,48.0228296206497,-213.458567219471));
#221454=CARTESIAN_POINT('Ctrl Pts',(46.2017839218346,46.8104888208194,-216.792669267422));
#221455=CARTESIAN_POINT('Ctrl Pts',(46.6457795593283,48.0640235510291,-215.396870081809));
#221456=CARTESIAN_POINT('Ctrl Pts',(46.4554564500058,48.1980381642128,-213.483257157301));
#221457=CARTESIAN_POINT('Ctrl Pts',(46.0766700563314,46.8895585675527,-216.794042256812));
#221458=CARTESIAN_POINT('Ctrl Pts',(46.4887913192792,48.1462000233379,-215.401238442915));
#221459=CARTESIAN_POINT('Ctrl Pts',(46.2867982818209,48.281531361307,-213.496222696252));
#221460=CARTESIAN_POINT('Ctrl Pts',(45.87994004771,47.0109902272891,-216.794160241211));
#221461=CARTESIAN_POINT('Ctrl Pts',(46.2457858413235,48.2661200717717,-215.40646574203));
#221462=CARTESIAN_POINT('Ctrl Pts',(46.0305084677243,48.4005429744946,-213.516940454076));
#221463=CARTESIAN_POINT('Ctrl Pts',(45.8130083614259,47.0517196539655,-216.793924557511));
#221464=CARTESIAN_POINT('Ctrl Pts',(46.1636642989778,48.3054420800928,-215.408029222597));
#221465=CARTESIAN_POINT('Ctrl Pts',(45.9444636232077,48.4392026490444,-213.524043423009));
#221466=CARTESIAN_POINT('Ctrl Pts',(45.6738275139891,47.1362504084184,-216.791429029715));
#221467=CARTESIAN_POINT('Ctrl Pts',(45.9955390217945,48.3833415744636,-215.409524793596));
#221468=CARTESIAN_POINT('Ctrl Pts',(45.7716909901163,48.5142583186283,-213.538427044985));
#221469=CARTESIAN_POINT('Ctrl Pts',(45.6014941600616,47.1800522287631,-216.789086099185));
#221470=CARTESIAN_POINT('Ctrl Pts',(45.909487227893,48.4219032984012,-215.409390457658));
#221471=CARTESIAN_POINT('Ctrl Pts',(45.6849221753667,48.5506755813471,-213.545667919355));
#221472=CARTESIAN_POINT('Ctrl Pts',(45.3906864148211,47.3015955364168,-216.784924808343));
#221473=CARTESIAN_POINT('Ctrl Pts',(45.6556189845464,48.5320404250428,-215.41161214138));
#221474=CARTESIAN_POINT('Ctrl Pts',(45.4234990388784,48.656600479725,-213.567641621079));
#221475=CARTESIAN_POINT('Ctrl Pts',(45.2524205018182,47.3757252143881,-216.78361659133));
#221476=CARTESIAN_POINT('Ctrl Pts',(45.4876266651675,48.6001390907726,-215.414568111945));
#221477=CARTESIAN_POINT('Ctrl Pts',(45.2477531990456,48.72277066996,-213.582727977839));
#221478=CARTESIAN_POINT('Ctrl Pts',(44.9704029731687,47.5202017602144,-216.780193800645));
#221479=CARTESIAN_POINT('Ctrl Pts',(45.1474130999697,48.7286782833904,-215.420341153695));
#221480=CARTESIAN_POINT('Ctrl Pts',(44.8934628220207,48.8462330088366,-213.614222279602));
#221481=CARTESIAN_POINT('Ctrl Pts',(44.8252346194533,47.5917409614306,-216.777410227236));
#221482=CARTESIAN_POINT('Ctrl Pts',(44.9742728080524,48.7893969151401,-215.42260502614));
#221483=CARTESIAN_POINT('Ctrl Pts',(44.7149101065309,48.9035307364313,-213.630594481039));
#221484=CARTESIAN_POINT('Ctrl Pts',(44.5266344343995,47.7322552775795,-216.769106033588));
#221485=CARTESIAN_POINT('Ctrl Pts',(44.6220976077485,48.9031595903168,-215.425477584854));
#221486=CARTESIAN_POINT('Ctrl Pts',(44.3548749879417,49.0092996064572,-213.664137638348));
#221487=CARTESIAN_POINT('Ctrl Pts',(44.3737726429906,47.8005581457219,-216.763841197291));
#221488=CARTESIAN_POINT('Ctrl Pts',(44.4434408439288,48.9560287134227,-215.426312574315));
#221489=CARTESIAN_POINT('Ctrl Pts',(44.1732412416258,49.0577948170598,-213.681295718708));
#221490=CARTESIAN_POINT('Ctrl Pts',(44.0708469448104,47.925010686338,-216.756464337538));
#221491=CARTESIAN_POINT('Ctrl Pts',(44.0869468343345,49.052302299606,-215.431212914185));
#221492=CARTESIAN_POINT('Ctrl Pts',(43.8055081380661,49.1462823788298,-213.716921533579));
#221493=CARTESIAN_POINT('Ctrl Pts',(43.9199928553144,47.9817986673754,-216.754308697682));
#221494=CARTESIAN_POINT('Ctrl Pts',(43.9084710831663,49.0958794298658,-215.435250774665));
#221495=CARTESIAN_POINT('Ctrl Pts',(43.6192098223546,49.1861560840058,-213.735550650933));
#221496=CARTESIAN_POINT('Ctrl Pts',(43.7631348840936,48.0386758038654,-216.749772686363));
#221497=CARTESIAN_POINT('Ctrl Pts',(43.7261216974267,49.135628774228,-215.437783134142));
#221498=CARTESIAN_POINT('Ctrl Pts',(43.4322454110891,49.2212868218137,-213.754842699038));
#221499=CARTESIAN_POINT('',(47.5938143592265,47.5353276146283,-213.404748058676));
#221500=CARTESIAN_POINT('',(47.0575921287078,46.1983743823903,-216.787046295788));
#221501=CARTESIAN_POINT('Origin',(44.8332438581234,43.3673981711062,-213.31748602649));
#221502=CARTESIAN_POINT('Ctrl Pts',(43.7719279964153,48.0354975596113,-216.750009718968));
#221503=CARTESIAN_POINT('Ctrl Pts',(43.7999682355946,48.025315958121,-216.750806036441));
#221504=CARTESIAN_POINT('Ctrl Pts',(43.8324552729532,48.0134635334545,-216.75163878995));
#221505=CARTESIAN_POINT('Ctrl Pts',(43.869389236841,47.9997974421566,-216.752507979496));
#221506=CARTESIAN_POINT('Ctrl Pts',(43.887856218785,47.9929643965077,-216.752942574269));
#221507=CARTESIAN_POINT('Ctrl Pts',(43.907434250537,47.9856775685499,-216.753386278009));
#221508=CARTESIAN_POINT('Ctrl Pts',(43.9281174324963,47.9779175176578,-216.753839100978));
#221509=CARTESIAN_POINT('Ctrl Pts',(43.9384590234759,47.9740374922117,-216.754065512463));
#221510=CARTESIAN_POINT('Ctrl Pts',(43.9490768944605,47.9700391399423,-216.75429418598));
#221511=CARTESIAN_POINT('Ctrl Pts',(43.9599697070893,47.9659199939512,-216.754525143987));
#221512=CARTESIAN_POINT('Ctrl Pts',(43.9654161134037,47.9638604209556,-216.75464062299));
#221513=CARTESIAN_POINT('Ctrl Pts',(43.970931254658,47.9617706482002,-216.754756671998));
#221514=CARTESIAN_POINT('Ctrl Pts',(43.9765149348169,47.9596503652226,-216.754873291075));
#221515=CARTESIAN_POINT('Ctrl Pts',(43.9820986149759,47.957530082245,-216.754989910151));
#221516=CARTESIAN_POINT('Ctrl Pts',(43.986323611751,47.95592358258,-216.755077719017));
#221517=CARTESIAN_POINT('Ctrl Pts',(43.9934713819637,47.9531976722309,-216.755224856242));
#221518=CARTESIAN_POINT('Ctrl Pts',(44.0285940305662,47.9398031186203,-216.755947857807));
#221519=CARTESIAN_POINT('Ctrl Pts',(44.0598368421922,47.9276795028024,-216.756596414032));
#221520=CARTESIAN_POINT('Ctrl Pts',(44.0871926282956,47.916949837956,-216.757170524919));
#221521=CARTESIAN_POINT('Ctrl Pts',(44.1043740011675,47.9102108478271,-216.757531107254));
#221522=CARTESIAN_POINT('Ctrl Pts',(44.1200230264987,47.9040208116318,-216.757862322909));
#221523=CARTESIAN_POINT('Ctrl Pts',(44.1341440632014,47.8984021424213,-216.758164171885));
#221524=CARTESIAN_POINT('Ctrl Pts',(44.1524461762284,47.8911198499724,-216.758555394866));
#221525=CARTESIAN_POINT('Ctrl Pts',(44.1681816696013,47.8847977496136,-216.758897286368));
#221526=CARTESIAN_POINT('Ctrl Pts',(44.1813646140109,47.8794715426646,-216.75918984639));
#221527=CARTESIAN_POINT('Ctrl Pts',(44.1879560862157,47.8768084391901,-216.759336126401));
#221528=CARTESIAN_POINT('Ctrl Pts',(44.1939094622523,47.8743940914731,-216.759470073542));
#221529=CARTESIAN_POINT('Ctrl Pts',(44.1992265052247,47.8722317355578,-216.759591691156));
#221530=CARTESIAN_POINT('Ctrl Pts',(44.2018850267109,47.8711505576002,-216.759652499962));
#221531=CARTESIAN_POINT('Ctrl Pts',(44.204384462322,47.8701323708537,-216.759710220538));
#221532=CARTESIAN_POINT('Ctrl Pts',(44.2067250158902,47.8691775029316,-216.759764860289));
#221533=CARTESIAN_POINT('Ctrl Pts',(44.2078952926744,47.8687000689706,-216.759792180164));
#221534=CARTESIAN_POINT('Ctrl Pts',(44.2090258474261,47.8682384623275,-216.759818729464));
#221535=CARTESIAN_POINT('Ctrl Pts',(44.2100969163324,47.8678007420343,-216.759844122804));
#221536=CARTESIAN_POINT('Ctrl Pts',(44.2111679852387,47.8673630217411,-216.759869516143));
#221537=CARTESIAN_POINT('Ctrl Pts',(44.2122192840712,47.8669333446112,-216.75989452408));
#221538=CARTESIAN_POINT('Ctrl Pts',(44.2144806688504,47.8660075143691,-216.759948709947));
#221539=CARTESIAN_POINT('Ctrl Pts',(44.2449761228487,47.8535224150545,-216.760679422656));
#221540=CARTESIAN_POINT('Ctrl Pts',(44.2755711243667,47.8408061684401,-216.761443377949));
#221541=CARTESIAN_POINT('Ctrl Pts',(44.3061404540436,47.8279027716419,-216.762238392159));
#221542=CARTESIAN_POINT('Ctrl Pts',(44.3481107408968,47.8101869999606,-216.763329910186));
#221543=CARTESIAN_POINT('Ctrl Pts',(44.3900317972361,47.7921181966764,-216.764479974366));
#221544=CARTESIAN_POINT('Ctrl Pts',(44.4317077200863,47.7737754898824,-216.765682933317));
#221545=CARTESIAN_POINT('Ctrl Pts',(44.4677231453878,47.7579241219657,-216.766722504256));
#221546=CARTESIAN_POINT('Ctrl Pts',(44.5035561515456,47.7418688288015,-216.767801577222));
#221547=CARTESIAN_POINT('Ctrl Pts',(44.5392322306382,47.7255991325106,-216.768920152147));
#221548=CARTESIAN_POINT('Ctrl Pts',(44.5570702701845,47.7174642843651,-216.76947943961));
#221549=CARTESIAN_POINT('Ctrl Pts',(44.5748690780222,47.7092758355722,-216.770048602683));
#221550=CARTESIAN_POINT('Ctrl Pts',(44.5926318406004,47.7010324781867,-216.770627641213));
#221551=CARTESIAN_POINT('Ctrl Pts',(44.605953912534,47.6948499601476,-216.77106192011));
#221552=CARTESIAN_POINT('Ctrl Pts',(44.6192557090139,47.6886365560366,-216.771501753962));
#221553=CARTESIAN_POINT('Ctrl Pts',(44.6325385743512,47.6823917143765,-216.771947142795));
#221554=CARTESIAN_POINT('Ctrl Pts',(44.6369661961303,47.6803101004898,-216.772095605739));
#221555=CARTESIAN_POINT('Ctrl Pts',(44.6432770207651,47.6773348113996,-216.772308487795));
#221556=CARTESIAN_POINT('Ctrl Pts',(44.6458151790926,47.6761363731342,-216.772394383283));
#221557=CARTESIAN_POINT('Ctrl Pts',(44.667735113507,47.6657864718322,-216.773136190224));
#221558=CARTESIAN_POINT('Ctrl Pts',(44.6940783900531,47.6533905421585,-216.773881695209));
#221559=CARTESIAN_POINT('Ctrl Pts',(44.7248101335922,47.6388298667565,-216.774630898238));
#221560=CARTESIAN_POINT('Ctrl Pts',(44.7510143492991,47.6264143304045,-216.775269725571));
#221561=CARTESIAN_POINT('Ctrl Pts',(44.7804087087902,47.6124243901338,-216.775911241589));
#221562=CARTESIAN_POINT('Ctrl Pts',(44.8129802196091,47.5967576098995,-216.776555446292));
#221563=CARTESIAN_POINT('Ctrl Pts',(44.8483655605272,47.5797373874492,-216.777255303391));
#221564=CARTESIAN_POINT('Ctrl Pts',(44.8874993594066,47.5607390605947,-216.777958333788));
#221565=CARTESIAN_POINT('Ctrl Pts',(44.9303902108242,47.5395897055685,-216.778664537483));
#221566=CARTESIAN_POINT('Ctrl Pts',(44.951835636533,47.5290150280554,-216.77901763933));
#221567=CARTESIAN_POINT('Ctrl Pts',(44.9742208346179,47.517901876086,-216.779371534503));
#221568=CARTESIAN_POINT('Ctrl Pts',(44.9975507822766,47.5062239777693,-216.779726222999));
#221569=CARTESIAN_POINT('Ctrl Pts',(44.9983644784359,47.5058166789126,-216.779738593737));
#221570=CARTESIAN_POINT('Ctrl Pts',(44.9991793241654,47.5054086927271,-216.77975096544));
#221571=CARTESIAN_POINT('Ctrl Pts',(44.9999953197465,47.5050000180245,-216.779763338108));
#221572=CARTESIAN_POINT('Ctrl Pts',(45.0108772620136,47.4995500197372,-216.77992833736));
#221573=CARTESIAN_POINT('Ctrl Pts',(45.0219637216991,47.4939775693251,-216.78009350826));
#221574=CARTESIAN_POINT('Ctrl Pts',(45.0332532520402,47.4882807840264,-216.780258851139));
#221575=CARTESIAN_POINT('Ctrl Pts',(45.0393212967433,47.4852188012147,-216.780347721796));
#221576=CARTESIAN_POINT('Ctrl Pts',(45.0454480117016,47.4821208957931,-216.780436641231));
#221577=CARTESIAN_POINT('Ctrl Pts',(45.0516331238869,47.4789867866292,-216.780525610852));
#221578=CARTESIAN_POINT('Ctrl Pts',(45.0578182360722,47.4758526774653,-216.780614580473));
#221579=CARTESIAN_POINT('Ctrl Pts',(45.062340348357,47.4735583574169,-216.780679268952));
#221580=CARTESIAN_POINT('Ctrl Pts',(45.0703633822198,47.469475560477,-216.780792668464));
#221581=CARTESIAN_POINT('Ctrl Pts',(45.1106116695992,47.4489938340672,-216.781361547544));
#221582=CARTESIAN_POINT('Ctrl Pts',(45.1479437072911,47.4296838782679,-216.781890800055));
#221583=CARTESIAN_POINT('Ctrl Pts',(45.1823388278365,47.4116798480988,-216.782380425997));
#221584=CARTESIAN_POINT('Ctrl Pts',(45.2210852171756,47.391398158384,-216.782931993692));
#221585=CARTESIAN_POINT('Ctrl Pts',(45.2561053197537,47.3727738991893,-216.783433274439));
#221586=CARTESIAN_POINT('Ctrl Pts',(45.2874192254577,47.3559454252637,-216.783884268239));
#221587=CARTESIAN_POINT('Ctrl Pts',(45.3169652113322,47.3400670529649,-216.78430979984));
#221588=CARTESIAN_POINT('Ctrl Pts',(45.3432132151396,47.3257864069596,-216.784690562402));
#221589=CARTESIAN_POINT('Ctrl Pts',(45.3662022526885,47.3131837743999,-216.785026555925));
#221590=CARTESIAN_POINT('Ctrl Pts',(45.3945609497833,47.297637484626,-216.785441029064));
#221591=CARTESIAN_POINT('Ctrl Pts',(45.4179621298102,47.284645416901,-216.785787376854));
#221592=CARTESIAN_POINT('Ctrl Pts',(45.4364877857767,47.2743030919902,-216.786065599295));
#221593=CARTESIAN_POINT('Ctrl Pts',(45.4404938146909,47.2720666447244,-216.786125762733));
#221594=CARTESIAN_POINT('Ctrl Pts',(45.4442718252743,47.2699539101085,-216.786182740581));
#221595=CARTESIAN_POINT('Ctrl Pts',(45.4478225530286,47.2679655548132,-216.786236532841));
#221596=CARTESIAN_POINT('Ctrl Pts',(45.4578079875536,47.2623738584096,-216.786387808615));
#221597=CARTESIAN_POINT('Ctrl Pts',(45.4659962721697,47.2577662199214,-216.786513890861));
#221598=CARTESIAN_POINT('Ctrl Pts',(45.4724009492202,47.2541536209048,-216.786614810403));
#221599=CARTESIAN_POINT('Ctrl Pts',(45.4756032877455,47.2523473213965,-216.786665270174));
#221600=CARTESIAN_POINT('Ctrl Pts',(45.4783596950982,47.2507897283842,-216.786709385351));
#221601=CARTESIAN_POINT('Ctrl Pts',(45.4806713295795,47.2494816957264,-216.786747224623));
#221602=CARTESIAN_POINT('Ctrl Pts',(45.4818271468202,47.2488276793975,-216.78676614426));
#221603=CARTESIAN_POINT('Ctrl Pts',(45.482871769002,47.2482360497932,-216.786783491525));
#221604=CARTESIAN_POINT('Ctrl Pts',(45.4838053126926,47.2477068917666,-216.786799265584));
#221605=CARTESIAN_POINT('Ctrl Pts',(45.4842720845379,47.2474423127533,-216.786807152614));
#221606=CARTESIAN_POINT('Ctrl Pts',(45.4847110860037,47.2471933509791,-216.786814646129));
#221607=CARTESIAN_POINT('Ctrl Pts',(45.4851084672805,47.2469678398215,-216.786821549312));
#221608=CARTESIAN_POINT('Ctrl Pts',(45.4855058485574,47.2467423286638,-216.786828452496));
#221609=CARTESIAN_POINT('Ctrl Pts',(45.4858895864854,47.2465247922921,-216.786835158855));
#221610=CARTESIAN_POINT('Ctrl Pts',(45.4879940552358,47.2453288536159,-216.78687250758));
#221611=CARTESIAN_POINT('Ctrl Pts',(45.5247478018735,47.2244422393148,-216.787524788859));
#221612=CARTESIAN_POINT('Ctrl Pts',(45.5620119202703,47.2028903192636,-216.788266723893));
#221613=CARTESIAN_POINT('Ctrl Pts',(45.5989423960054,47.1811378446028,-216.789080931354));
#221614=CARTESIAN_POINT('Ctrl Pts',(45.6258353862223,47.165297564276,-216.789673842029));
#221615=CARTESIAN_POINT('Ctrl Pts',(45.6525518901226,47.1493516911605,-216.790305077603));
#221616=CARTESIAN_POINT('Ctrl Pts',(45.6787817315062,47.1334878263734,-216.790967926176));
#221617=CARTESIAN_POINT('Ctrl Pts',(45.6825303096061,47.1312206782328,-216.791062655672));
#221618=CARTESIAN_POINT('Ctrl Pts',(45.6862689755748,47.1289552138267,-216.791158030833));
#221619=CARTESIAN_POINT('Ctrl Pts',(45.6899967965639,47.1266920637689,-216.791254032068));
#221620=CARTESIAN_POINT('Ctrl Pts',(45.7228131866165,47.1067693219689,-216.792099140777));
#221621=CARTESIAN_POINT('Ctrl Pts',(45.7561216578679,47.0864990412011,-216.792755263244));
#221622=CARTESIAN_POINT('Ctrl Pts',(45.7898044813981,47.065949222955,-216.793222399469));
#221623=CARTESIAN_POINT('Ctrl Pts',(45.8066458931633,47.0556743138319,-216.793455967582));
#221624=CARTESIAN_POINT('Ctrl Pts',(45.8235805995987,47.0453297617529,-216.793642289121));
#221625=CARTESIAN_POINT('Ctrl Pts',(45.8405920420434,47.0349255859399,-216.793781363054));
#221626=CARTESIAN_POINT('Ctrl Pts',(45.8490977632657,47.0297234980334,-216.79385090002));
#221627=CARTESIAN_POINT('Ctrl Pts',(45.8576226695517,47.0245065059502,-216.793908626949));
#221628=CARTESIAN_POINT('Ctrl Pts',(45.8661645460346,47.0192759789475,-216.793954541448));
#221629=CARTESIAN_POINT('Ctrl Pts',(45.870435484276,47.0166607154462,-216.793977498697));
#221630=CARTESIAN_POINT('Ctrl Pts',(45.8747106651369,47.0140420683319,-216.793997502963));
#221631=CARTESIAN_POINT('Ctrl Pts',(45.8789898076483,47.0114202126398,-216.79401455427));
#221632=CARTESIAN_POINT('Ctrl Pts',(45.8811293789039,47.0101092847938,-216.794023079923));
#221633=CARTESIAN_POINT('Ctrl Pts',(45.8832699405766,47.0087975548103,-216.794030867345));
#221634=CARTESIAN_POINT('Ctrl Pts',(45.8854114570194,47.0074850449998,-216.794037916534));
#221635=CARTESIAN_POINT('Ctrl Pts',(45.8875529734622,47.0061725351893,-216.794044965722));
#221636=CARTESIAN_POINT('Ctrl Pts',(45.8907066610453,47.0042392997017,-216.794053905808));
#221637=CARTESIAN_POINT('Ctrl Pts',(45.8918388348603,47.0035451985448,-216.794056849418));
#221638=CARTESIAN_POINT('Ctrl Pts',(45.9017349656741,46.9974781832549,-216.794082578986));
#221639=CARTESIAN_POINT('Ctrl Pts',(45.9140558641918,46.9899297596758,-216.794091079011));
#221640=CARTESIAN_POINT('Ctrl Pts',(45.9287146500497,46.9809163219443,-216.794082349493));
#221641=CARTESIAN_POINT('Ctrl Pts',(45.9408886437017,46.9734307406152,-216.794075099704));
#221642=CARTESIAN_POINT('Ctrl Pts',(45.9546746901182,46.9649346626169,-216.794055966429));
#221643=CARTESIAN_POINT('Ctrl Pts',(45.9699974444731,46.9554476628383,-216.794024949666));
#221644=CARTESIAN_POINT('Ctrl Pts',(45.9868839363196,46.9449924835213,-216.793990767541));
#221645=CARTESIAN_POINT('Ctrl Pts',(46.0056380469337,46.9333329342966,-216.793942152665));
#221646=CARTESIAN_POINT('Ctrl Pts',(46.026117443191,46.9205161485541,-216.793879105039));
#221647=CARTESIAN_POINT('Ctrl Pts',(46.0363571413196,46.9141077556829,-216.793847581226));
#221648=CARTESIAN_POINT('Ctrl Pts',(46.0470274212995,46.9074104503921,-216.793812449226));
#221649=CARTESIAN_POINT('Ctrl Pts',(46.0581055216702,46.9004329827126,-216.793773709038));
#221650=CARTESIAN_POINT('Ctrl Pts',(46.0655876516163,46.8957204130368,-216.793747543982));
#221651=CARTESIAN_POINT('Ctrl Pts',(46.0738521325161,46.890503370826,-216.793717443146));
#221652=CARTESIAN_POINT('Ctrl Pts',(46.0816805652799,46.8855491135382,-216.79368804623));
#221653=CARTESIAN_POINT('Ctrl Pts',(46.0854429715589,46.8831680585699,-216.793673917841));
#221654=CARTESIAN_POINT('Ctrl Pts',(46.0891054119841,46.8808474685615,-216.793659952046));
#221655=CARTESIAN_POINT('Ctrl Pts',(46.0925367545552,46.8786711564055,-216.793646663912));
#221656=CARTESIAN_POINT('Ctrl Pts',(46.1249973118812,46.8580832075096,-216.79352095794));
#221657=CARTESIAN_POINT('Ctrl Pts',(46.1545286634281,46.8390961398004,-216.79344153441));
#221658=CARTESIAN_POINT('Ctrl Pts',(46.1813384366676,46.8216767497614,-216.793408393323));
#221659=CARTESIAN_POINT('Ctrl Pts',(46.1894515732713,46.8164053179713,-216.793398364213));
#221660=CARTESIAN_POINT('Ctrl Pts',(46.1973156706764,46.8112771226396,-216.793392573558));
#221661=CARTESIAN_POINT('Ctrl Pts',(46.2049368905182,46.8062904844855,-216.793391021358));
#221662=CARTESIAN_POINT('Ctrl Pts',(46.2213396202164,46.7955580191531,-216.793387680643));
#221663=CARTESIAN_POINT('Ctrl Pts',(46.2366172731346,46.7854815518693,-216.793403973138));
#221664=CARTESIAN_POINT('Ctrl Pts',(46.2508323842425,46.7760404634134,-216.793439914088));
#221665=CARTESIAN_POINT('Ctrl Pts',(46.2579399397965,46.7713199191855,-216.793457884563));
#221666=CARTESIAN_POINT('Ctrl Pts',(46.2647818439802,46.7667581956347,-216.793480740381));
#221667=CARTESIAN_POINT('Ctrl Pts',(46.2713659264824,46.7623523087817,-216.793508515375));
#221668=CARTESIAN_POINT('Ctrl Pts',(46.2746579677335,46.7601493653551,-216.793522402872));
#221669=CARTESIAN_POINT('Ctrl Pts',(46.2778855526769,46.7579853797555,-216.793537518667));
#221670=CARTESIAN_POINT('Ctrl Pts',(46.2810496433213,46.7558599741858,-216.793553862528));
#221671=CARTESIAN_POINT('Ctrl Pts',(46.2815161385684,46.755546616666,-216.793556272173));
#221672=CARTESIAN_POINT('Ctrl Pts',(46.2819516748022,46.7552540000806,-216.79355852675));
#221673=CARTESIAN_POINT('Ctrl Pts',(46.2823694031142,46.7549732901716,-216.793560706644));
#221674=CARTESIAN_POINT('Ctrl Pts',(46.2845577700535,46.7535027260118,-216.793572126526));
#221675=CARTESIAN_POINT('Ctrl Pts',(46.2862606393729,46.7523574370574,-216.793581496779));
#221676=CARTESIAN_POINT('Ctrl Pts',(46.2893451131554,46.75027822677,-216.793600374501));
#221677=CARTESIAN_POINT('Ctrl Pts',(46.2896653831733,46.7500623362282,-216.793602334631));
#221678=CARTESIAN_POINT('Ctrl Pts',(46.2900005062908,46.7498363964486,-216.793604397263));
#221679=CARTESIAN_POINT('Ctrl Pts',(46.2903525372648,46.7495990142202,-216.793606575336));
#221680=CARTESIAN_POINT('Ctrl Pts',(46.3125906116356,46.7346033915579,-216.793744165901));
#221681=CARTESIAN_POINT('Ctrl Pts',(46.3339221814183,46.7199958452874,-216.793972420847));
#221682=CARTESIAN_POINT('Ctrl Pts',(46.3546813907234,46.7056150358813,-216.794248529204));
#221683=CARTESIAN_POINT('Ctrl Pts',(46.3762392929501,46.6906809370646,-216.794535260595));
#221684=CARTESIAN_POINT('Ctrl Pts',(46.3971796363455,46.6759914456177,-216.794873598471));
#221685=CARTESIAN_POINT('Ctrl Pts',(46.4178247858721,46.6613900474904,-216.795215597964));
#221686=CARTESIAN_POINT('Ctrl Pts',(46.4397055789028,46.6459147335447,-216.795578066646));
#221687=CARTESIAN_POINT('Ctrl Pts',(46.4612546635803,46.630538341508,-216.795944648367));
#221688=CARTESIAN_POINT('Ctrl Pts',(46.4828018122461,46.6151008458368,-216.796258264017));
#221689=CARTESIAN_POINT('Ctrl Pts',(46.5052220656438,46.5990378126186,-216.796584587581));
#221690=CARTESIAN_POINT('Ctrl Pts',(46.5276398302866,46.5829086656922,-216.796853565667));
#221691=CARTESIAN_POINT('Ctrl Pts',(46.5503739020283,46.566560657057,-216.797000895555));
#221692=CARTESIAN_POINT('Ctrl Pts',(46.5760029895584,46.5481308505086,-216.797166986814));
#221693=CARTESIAN_POINT('Ctrl Pts',(46.602033725843,46.529422623157,-216.797178475217));
#221694=CARTESIAN_POINT('Ctrl Pts',(46.628861222937,46.5102540599383,-216.79694323161));
#221695=CARTESIAN_POINT('Ctrl Pts',(46.6442602233249,46.4992512924642,-216.796808201629));
#221696=CARTESIAN_POINT('Ctrl Pts',(46.6599206127002,46.4880975557103,-216.796591879193));
#221697=CARTESIAN_POINT('Ctrl Pts',(46.6759114459435,46.4767631089541,-216.796276840848));
#221698=CARTESIAN_POINT('Ctrl Pts',(46.6906059672228,46.4663474998038,-216.795987341383));
#221699=CARTESIAN_POINT('Ctrl Pts',(46.7050820297943,46.4560666092541,-216.795679810554));
#221700=CARTESIAN_POINT('Ctrl Pts',(46.7193659094848,46.4459104620005,-216.795354248359));
#221701=CARTESIAN_POINT('Ctrl Pts',(46.7382039925211,46.4325161777138,-216.794924885483));
#221702=CARTESIAN_POINT('Ctrl Pts',(46.7567078125574,46.4193388589338,-216.794464160181));
#221703=CARTESIAN_POINT('Ctrl Pts',(46.7749052518499,46.4063621036006,-216.793972072453));
#221704=CARTESIAN_POINT('Ctrl Pts',(46.7909030289276,46.3949539468994,-216.793539467093));
#221705=CARTESIAN_POINT('Ctrl Pts',(46.8066640171603,46.3837007972895,-216.793082623085));
#221706=CARTESIAN_POINT('Ctrl Pts',(46.8222071071304,46.3725915476252,-216.792601540443));
#221707=CARTESIAN_POINT('Ctrl Pts',(46.8299786521155,46.367036922793,-216.792360999121));
#221708=CARTESIAN_POINT('Ctrl Pts',(46.8376957225221,46.3615182729302,-216.792114398121));
#221709=CARTESIAN_POINT('Ctrl Pts',(46.8453606733607,46.3560342140465,-216.791861737467));
#221710=CARTESIAN_POINT('Ctrl Pts',(46.8511093864896,46.3519211698836,-216.791672241976));
#221711=CARTESIAN_POINT('Ctrl Pts',(46.8568287823605,46.3478275831453,-216.791479337929));
#221712=CARTESIAN_POINT('Ctrl Pts',(46.8625198537008,46.3437528704933,-216.79128302532));
#221713=CARTESIAN_POINT('Ctrl Pts',(46.8641769268255,46.3425664336306,-216.791225864844));
#221714=CARTESIAN_POINT('Ctrl Pts',(46.8672064496826,46.3403971424021,-216.791120311155));
#221715=CARTESIAN_POINT('Ctrl Pts',(46.8680054423642,46.3398248670299,-216.791092423137));
#221716=CARTESIAN_POINT('Ctrl Pts',(46.8681211396226,46.3397419993226,-216.791088384843));
#221717=CARTESIAN_POINT('Ctrl Pts',(46.8681901367227,46.3396925799012,-216.791085975056));
#221718=CARTESIAN_POINT('Ctrl Pts',(46.868201520183,46.3396844276801,-216.791085576526));
#221719=CARTESIAN_POINT('Ctrl Pts',(46.8685685936507,46.3394215494343,-216.791072725425));
#221720=CARTESIAN_POINT('Ctrl Pts',(46.8709671673915,46.3376639117433,-216.791022665875));
#221721=CARTESIAN_POINT('Ctrl Pts',(46.875368288887,46.334427330707,-216.790935397876));
#221722=CARTESIAN_POINT('Ctrl Pts',(46.8795994466559,46.331315740852,-216.790851500016));
#221723=CARTESIAN_POINT('Ctrl Pts',(46.8856808427705,46.326837585854,-216.790733212068));
#221724=CARTESIAN_POINT('Ctrl Pts',(46.8935467207944,46.3210286787986,-216.790580534032));
#221725=CARTESIAN_POINT('Ctrl Pts',(46.90157058323,46.3151031011362,-216.790424789491));
#221726=CARTESIAN_POINT('Ctrl Pts',(46.9114507502922,46.3077931236649,-216.790233259554));
#221727=CARTESIAN_POINT('Ctrl Pts',(46.9230833813073,46.2991549282109,-216.790005944221));
#221728=CARTESIAN_POINT('Ctrl Pts',(46.9288996968149,46.2948358304839,-216.789892286554));
#221729=CARTESIAN_POINT('Ctrl Pts',(46.9351536534424,46.2901849284473,-216.789769682536));
#221730=CARTESIAN_POINT('Ctrl Pts',(46.9418300414805,46.285210383585,-216.789638133061));
#221731=CARTESIAN_POINT('Ctrl Pts',(46.9451682354996,46.2827231111539,-216.789572358324));
#221732=CARTESIAN_POINT('Ctrl Pts',(46.9486120361007,46.2801549263655,-216.789504345222));
#221733=CARTESIAN_POINT('Ctrl Pts',(46.9521594324836,46.2775069041238,-216.789434096866));
#221734=CARTESIAN_POINT('Ctrl Pts',(46.9550814801921,46.2753256854247,-216.789376232159));
#221735=CARTESIAN_POINT('Ctrl Pts',(46.9589745467844,46.2724170025407,-216.789298950658));
#221736=CARTESIAN_POINT('Ctrl Pts',(46.9616112445893,46.2704454910704,-216.789246484071));
#221737=CARTESIAN_POINT('Ctrl Pts',(46.9621755254093,46.2700235670612,-216.789235255674));
#221738=CARTESIAN_POINT('Ctrl Pts',(46.9626824488577,46.2696444664173,-216.789225163812));
#221739=CARTESIAN_POINT('Ctrl Pts',(46.9631104211035,46.2693243772486,-216.789216642034));
#221740=CARTESIAN_POINT('Ctrl Pts',(46.980514184376,46.2563077478473,-216.788870098506));
#221741=CARTESIAN_POINT('Ctrl Pts',(46.9963445219175,46.2444288905238,-216.788533594325));
#221742=CARTESIAN_POINT('Ctrl Pts',(47.0107402837605,46.2336120791181,-216.788207129489));
#221743=CARTESIAN_POINT('Ctrl Pts',(47.0261770769916,46.2220130485903,-216.787857056307));
#221744=CARTESIAN_POINT('Ctrl Pts',(47.0399639945659,46.2116354196435,-216.787518526964));
#221745=CARTESIAN_POINT('Ctrl Pts',(47.0522206527176,46.2024148717456,-216.787191541462));
#221746=CARTESIAN_POINT('Ctrl Pts',(47.0540450260366,46.2010424159454,-216.787142870477));
#221747=CARTESIAN_POINT('Ctrl Pts',(47.0558354138571,46.19969564163,-216.787094455252));
#221748=CARTESIAN_POINT('Ctrl Pts',(47.0575921287077,46.1983743823902,-216.787046295788));
#221749=CARTESIAN_POINT('Ctrl Pts',(47.5938143592254,47.5353276146289,-213.404748058676));
#221750=CARTESIAN_POINT('Ctrl Pts',(47.4864021701981,47.6063414465537,-213.410916600681));
#221751=CARTESIAN_POINT('Ctrl Pts',(47.3727955180169,47.6788238138538,-213.41786320449));
#221752=CARTESIAN_POINT('Ctrl Pts',(47.2527927928078,47.7521475639727,-213.425781542233));
#221753=CARTESIAN_POINT('Ctrl Pts',(47.2075811278853,47.7797726767813,-213.428764818089));
#221754=CARTESIAN_POINT('Ctrl Pts',(47.161461484639,47.8075168510272,-213.431886395367));
#221755=CARTESIAN_POINT('Ctrl Pts',(47.1144227976596,47.8353452540809,-213.435158020616));
#221756=CARTESIAN_POINT('Ctrl Pts',(47.0214662420634,47.8903389765197,-213.441623316181));
#221757=CARTESIAN_POINT('Ctrl Pts',(46.9249056173264,47.945674409168,-213.448583307771));
#221758=CARTESIAN_POINT('Ctrl Pts',(46.8246139149985,48.0010896024748,-213.455937351587));
#221759=CARTESIAN_POINT('Ctrl Pts',(46.7880174307094,48.0213106297797,-213.458620845263));
#221760=CARTESIAN_POINT('Ctrl Pts',(46.7509240118438,48.0415422237553,-213.461356338266));
#221761=CARTESIAN_POINT('Ctrl Pts',(46.7133270224978,48.0617714853602,-213.464137256222));
#221762=CARTESIAN_POINT('Ctrl Pts',(46.6831717520134,48.0779966902505,-213.466367736232));
#221763=CARTESIAN_POINT('Ctrl Pts',(46.6526943629849,48.0942192315053,-213.468635888902));
#221764=CARTESIAN_POINT('Ctrl Pts',(46.6218917752265,48.110432305252,-213.470934821448));
#221765=CARTESIAN_POINT('Ctrl Pts',(46.4984211243293,48.1754216101847,-213.480149978956));
#221766=CARTESIAN_POINT('Ctrl Pts',(46.3697617304992,48.2402352763643,-213.490086744041));
#221767=CARTESIAN_POINT('Ctrl Pts',(46.2357652584914,48.304370847364,-213.500726997951));
#221768=CARTESIAN_POINT('Ctrl Pts',(46.219639872116,48.3120890420842,-213.502007466032));
#221769=CARTESIAN_POINT('Ctrl Pts',(46.2034371774102,48.3197973951656,-213.503298178144));
#221770=CARTESIAN_POINT('Ctrl Pts',(46.1871569030505,48.327495013277,-213.504599149635));
#221771=CARTESIAN_POINT('Ctrl Pts',(46.1635870781003,48.3386392672011,-213.506482635727));
#221772=CARTESIAN_POINT('Ctrl Pts',(46.1398591423213,48.3497589583645,-213.508384553586));
#221773=CARTESIAN_POINT('Ctrl Pts',(46.1159688146372,48.3608529964996,-213.510307882609));
#221774=CARTESIAN_POINT('Ctrl Pts',(46.0459424972984,48.393371371521,-213.515945463234));
#221775=CARTESIAN_POINT('Ctrl Pts',(45.9744755547282,48.4256892487927,-213.521758156206));
#221776=CARTESIAN_POINT('Ctrl Pts',(45.9016170264935,48.4577050961598,-213.527740501239));
#221777=CARTESIAN_POINT('Ctrl Pts',(45.8871630536565,48.4640565309117,-213.528927303315));
#221778=CARTESIAN_POINT('Ctrl Pts',(45.8726527968879,48.470396704033,-213.530121292051));
#221779=CARTESIAN_POINT('Ctrl Pts',(45.8580875854649,48.4767243421701,-213.531322368788));
#221780=CARTESIAN_POINT('Ctrl Pts',(45.8234192369333,48.4917854873846,-213.534181190795));
#221781=CARTESIAN_POINT('Ctrl Pts',(45.7884329611125,48.5067790279182,-213.537073745386));
#221782=CARTESIAN_POINT('Ctrl Pts',(45.7531297470218,48.5216957329351,-213.540007556183));
#221783=CARTESIAN_POINT('Ctrl Pts',(45.7280621712483,48.5322875626859,-213.542090752468));
#221784=CARTESIAN_POINT('Ctrl Pts',(45.7028344378474,48.5428408361259,-213.544193292514));
#221785=CARTESIAN_POINT('Ctrl Pts',(45.6774461022642,48.553352630891,-213.546315176312));
#221786=CARTESIAN_POINT('Ctrl Pts',(45.6647519344726,48.5586085282736,-213.547376118211));
#221787=CARTESIAN_POINT('Ctrl Pts',(45.6520176160559,48.5638540557922,-213.548441896045));
#221788=CARTESIAN_POINT('Ctrl Pts',(45.6392430948086,48.5690888454429,-213.549512509832));
#221789=CARTESIAN_POINT('Ctrl Pts',(45.6276157176962,48.5738535542092,-213.55048698316));
#221790=CARTESIAN_POINT('Ctrl Pts',(45.6145896480273,48.5791640088112,-213.55158016601));
#221791=CARTESIAN_POINT('Ctrl Pts',(45.6038931400742,48.5835053146679,-213.552478890456));
#221792=CARTESIAN_POINT('Ctrl Pts',(45.6028378344585,48.5839336230905,-213.552567557613));
#221793=CARTESIAN_POINT('Ctrl Pts',(45.6018052171491,48.5843525379327,-213.552654329039));
#221794=CARTESIAN_POINT('Ctrl Pts',(45.6007988765239,48.584760628636,-213.552738902164));
#221795=CARTESIAN_POINT('Ctrl Pts',(45.5997929733645,48.5851685419385,-213.552823438524));
#221796=CARTESIAN_POINT('Ctrl Pts',(45.5987870597672,48.5855762915489,-213.552907982691));
#221797=CARTESIAN_POINT('Ctrl Pts',(45.5977811357529,48.5859838775069,-213.552992534718));
#221798=CARTESIAN_POINT('Ctrl Pts',(45.4223180751081,48.6570789887088,-213.567740922417));
#221799=CARTESIAN_POINT('Ctrl Pts',(45.2465642771724,48.723184982287,-213.582833694045));
#221800=CARTESIAN_POINT('Ctrl Pts',(45.0706080135195,48.7845018379456,-213.598475150732));
#221801=CARTESIAN_POINT('Ctrl Pts',(44.8922650990797,48.8466503884742,-213.614328766362));
#221802=CARTESIAN_POINT('Ctrl Pts',(44.7137050712026,48.9038847439255,-213.630706762686));
#221803=CARTESIAN_POINT('Ctrl Pts',(44.5348925487863,48.9564151707958,-213.64736607016));
#221804=CARTESIAN_POINT('Ctrl Pts',(44.3782619231994,49.0024291384522,-213.661958771589));
#221805=CARTESIAN_POINT('Ctrl Pts',(44.2213274321021,49.0448507637341,-213.676759131991));
#221806=CARTESIAN_POINT('Ctrl Pts',(44.0648182073631,49.0836230166911,-213.691823145796));
#221807=CARTESIAN_POINT('Ctrl Pts',(44.0402375397782,49.0897124204502,-213.694189035196));
#221808=CARTESIAN_POINT('Ctrl Pts',(44.0156672588303,49.0957118208884,-213.696561420079));
#221809=CARTESIAN_POINT('Ctrl Pts',(43.9911100751508,49.1016210123337,-213.698940508622));
#221810=CARTESIAN_POINT('Ctrl Pts',(43.8077580917296,49.1457409727519,-213.716703563573));
#221811=CARTESIAN_POINT('Ctrl Pts',(43.6249609203382,49.1848928448817,-213.734979503089));
#221812=CARTESIAN_POINT('Ctrl Pts',(43.4427334535923,49.2193110042465,-213.753761106585));
#221813=CARTESIAN_POINT('Ctrl Pts',(47.5746165801345,45.8238283676803,-216.758537654376));
#221814=CARTESIAN_POINT('Ctrl Pts',(48.4386236174112,46.8746099006705,-215.343430354514));
#221815=CARTESIAN_POINT('Ctrl Pts',(48.4710160211071,46.8924605148108,-213.380827300298));
#221816=CARTESIAN_POINT('Ctrl Pts',(47.406334611411,45.9580463783691,-216.758691640524));
#221817=CARTESIAN_POINT('Ctrl Pts',(48.202043344371,47.0656079993358,-215.343093772686));
#221818=CARTESIAN_POINT('Ctrl Pts',(48.1862070583782,47.1231145402161,-213.379368669215));
#221819=CARTESIAN_POINT('Ctrl Pts',(47.2339088845731,46.082710612235,-216.768384423925));
#221820=CARTESIAN_POINT('Ctrl Pts',(47.960805927557,47.2450787050191,-215.353433308566));
#221821=CARTESIAN_POINT('Ctrl Pts',(47.8936638370752,47.3370869807142,-213.387528102992));
#221822=CARTESIAN_POINT('Ctrl Pts',(47.0575921287078,46.1983743823903,-216.787046295788));
#221823=CARTESIAN_POINT('Ctrl Pts',(47.7151968771192,47.4137062867165,-215.373807350724));
#221824=CARTESIAN_POINT('Ctrl Pts',(47.5938143592261,47.5353276146285,-213.404748058676));
#221825=CARTESIAN_POINT('',(48.4710160211073,46.8924605148106,-213.380827300298));
#221826=CARTESIAN_POINT('',(47.5746165801346,45.8238283676801,-216.758537654376));
#221827=CARTESIAN_POINT('Origin',(45.3249961798233,43.0072392217583,-213.293565268111));
#221828=CARTESIAN_POINT('Ctrl Pts',(47.0575921287078,46.1983743823903,-216.787046295788));
#221829=CARTESIAN_POINT('Ctrl Pts',(47.1206620655918,46.1575511266546,-216.779921519949));
#221830=CARTESIAN_POINT('Ctrl Pts',(47.1845910131245,46.1142804480577,-216.774132275845));
#221831=CARTESIAN_POINT('Ctrl Pts',(47.2492989402458,46.068604399768,-216.769677997844));
#221832=CARTESIAN_POINT('Ctrl Pts',(47.2701598994296,46.0538790605176,-216.768241998953));
#221833=CARTESIAN_POINT('Ctrl Pts',(47.2911021053937,46.0389034482834,-216.766944780022));
#221834=CARTESIAN_POINT('Ctrl Pts',(47.3121237178813,46.0236781569863,-216.765786424972));
#221835=CARTESIAN_POINT('Ctrl Pts',(47.3752706746417,45.9779428066763,-216.7623068348));
#221836=CARTESIAN_POINT('Ctrl Pts',(47.4391323549421,45.9299570309712,-216.760079358312));
#221837=CARTESIAN_POINT('Ctrl Pts',(47.5036335622899,45.8797589197311,-216.759104615009));
#221838=CARTESIAN_POINT('Ctrl Pts',(47.5272094638708,45.861410957285,-216.758748335598));
#221839=CARTESIAN_POINT('Ctrl Pts',(47.5508712124359,45.8427671528649,-216.758559382341));
#221840=CARTESIAN_POINT('Ctrl Pts',(47.5746165801345,45.8238283676803,-216.758537654376));
#221841=CARTESIAN_POINT('Origin',(42.9552659882971,40.1115177027145,-218.083290145329));
#221842=CARTESIAN_POINT('Ctrl Pts',(50.7984099663005,43.0953291376929,-216.756961257354));
#221843=CARTESIAN_POINT('Ctrl Pts',(51.7004178351441,44.0801543735299,-215.34722316631));
#221844=CARTESIAN_POINT('Ctrl Pts',(51.7300796834961,44.0990078745203,-213.405670914582));
#221845=CARTESIAN_POINT('Ctrl Pts',(49.7561440689262,44.0321489495818,-216.756606633388));
#221846=CARTESIAN_POINT('Ctrl Pts',(50.6433589272998,45.038170309669,-215.345619228189));
#221847=CARTESIAN_POINT('Ctrl Pts',(50.6732101690724,45.0571976655732,-213.399273427567));
#221848=CARTESIAN_POINT('Ctrl Pts',(48.6689534025382,44.9510092870779,-216.757536292366));
#221849=CARTESIAN_POINT('Ctrl Pts',(49.5465852939469,45.977756673802,-215.344527068798));
#221850=CARTESIAN_POINT('Ctrl Pts',(49.5810652140745,45.9933960278872,-213.390312554365));
#221851=CARTESIAN_POINT('Ctrl Pts',(47.5746165801346,45.82382836768,-216.758537654376));
#221852=CARTESIAN_POINT('Ctrl Pts',(48.4386236174113,46.8746099006704,-215.343430354514));
#221853=CARTESIAN_POINT('Ctrl Pts',(48.4710160211072,46.8924605148107,-213.380827300298));
#221854=CARTESIAN_POINT('Ctrl Pts',(47.5746165801346,45.82382836768,-216.758537654376));
#221855=CARTESIAN_POINT('Ctrl Pts',(47.7452087461311,45.6877677925128,-216.758381555714));
#221856=CARTESIAN_POINT('Ctrl Pts',(47.9124683327338,45.5531103788107,-216.758230158611));
#221857=CARTESIAN_POINT('Ctrl Pts',(48.0767469921133,45.4196924030786,-216.758087000702));
#221858=CARTESIAN_POINT('Ctrl Pts',(48.2545046554837,45.2753275311754,-216.757932096738));
#221859=CARTESIAN_POINT('Ctrl Pts',(48.4287726329384,45.1324137879986,-216.757786825112));
#221860=CARTESIAN_POINT('Ctrl Pts',(48.6000196954607,44.990687035835,-216.757654799907));
#221861=CARTESIAN_POINT('Ctrl Pts',(48.786492574132,44.8363591596576,-216.757511036156));
#221862=CARTESIAN_POINT('Ctrl Pts',(48.9693842428768,44.6834386251299,-216.757382955664));
#221863=CARTESIAN_POINT('Ctrl Pts',(49.1493163534013,44.5315208113952,-216.757274540693));
#221864=CARTESIAN_POINT('Ctrl Pts',(49.3151698180586,44.3914896870029,-216.757174608567));
#221865=CARTESIAN_POINT('Ctrl Pts',(49.4785095089783,44.2523092521545,-216.757091358214));
#221866=CARTESIAN_POINT('Ctrl Pts',(49.6398237993626,44.113623656301,-216.757027743289));
#221867=CARTESIAN_POINT('Ctrl Pts',(51.7111509599702,44.1161634567458,-213.405556126747));
#221868=CARTESIAN_POINT('Ctrl Pts',(51.5538775663418,44.2586564036198,-213.404600680556));
#221869=CARTESIAN_POINT('Ctrl Pts',(51.3882561727022,44.4075223032268,-213.403542288886));
#221870=CARTESIAN_POINT('Ctrl Pts',(51.2140278838009,44.5626338811098,-213.40237201694));
#221871=CARTESIAN_POINT('Ctrl Pts',(51.0473579435284,44.7110164289977,-213.401252513577));
#221872=CARTESIAN_POINT('Ctrl Pts',(50.872811270086,44.8651146889509,-213.400030584105));
#221873=CARTESIAN_POINT('Ctrl Pts',(50.6901748034305,45.0247715567893,-213.398701013203));
#221874=CARTESIAN_POINT('Ctrl Pts',(50.5184166713263,45.1749188187229,-213.397450635232));
#221875=CARTESIAN_POINT('Ctrl Pts',(50.339503487995,45.3299822316343,-213.396105033313));
#221876=CARTESIAN_POINT('Ctrl Pts',(50.1532748754427,45.489788841628,-213.394662671329));
#221877=CARTESIAN_POINT('Ctrl Pts',(49.9727593666554,45.6446929195525,-213.393264557989));
#221878=CARTESIAN_POINT('Ctrl Pts',(49.7853700957918,45.8040538101684,-213.391775498415));
#221879=CARTESIAN_POINT('Ctrl Pts',(49.5909813482879,45.9676714965567,-213.390197223026));
#221880=CARTESIAN_POINT('Ctrl Pts',(49.4054192875547,46.1238597299213,-213.388690613012));
#221881=CARTESIAN_POINT('Ctrl Pts',(49.2134787906277,46.2839269881764,-213.387102687596));
#221882=CARTESIAN_POINT('Ctrl Pts',(49.0150726319924,46.4476586616144,-213.385438187813));
#221883=CARTESIAN_POINT('Ctrl Pts',(48.8388362262783,46.5930950826748,-213.383959677967));
#221884=CARTESIAN_POINT('Ctrl Pts',(48.6574984947564,46.7414223711376,-213.382420773499));
#221885=CARTESIAN_POINT('Ctrl Pts',(48.4710160211073,46.8924605148106,-213.380827300298));
#221886=CARTESIAN_POINT('Ctrl Pts',(32.8237598256933,-74.7342241033955,
-216.385388039321));
#221887=CARTESIAN_POINT('Ctrl Pts',(32.9990492150882,-74.6974990623407,
-216.482388336084));
#221888=CARTESIAN_POINT('Ctrl Pts',(33.1752262860961,-74.6372704537072,
-216.564961398279));
#221889=CARTESIAN_POINT('Ctrl Pts',(30.6715671894371,-72.7849850406464,
-219.42138468029));
#221890=CARTESIAN_POINT('Ctrl Pts',(30.8686320743566,-72.7455847913414,
-219.534693600851));
#221891=CARTESIAN_POINT('Ctrl Pts',(31.0696428925502,-72.6787836312099,
-219.626145751152));
#221892=CARTESIAN_POINT('Ctrl Pts',(28.5222070452525,-70.8331480683141,
-222.457793536072));
#221893=CARTESIAN_POINT('Ctrl Pts',(28.74408228947,-70.7922628748654,-222.589726795606));
#221894=CARTESIAN_POINT('Ctrl Pts',(28.9728528878395,-70.717730574095,-222.691719005855));
#221895=CARTESIAN_POINT('Ctrl Pts',(24.22299709402,-66.9233834882713,-228.527077755974));
#221896=CARTESIAN_POINT('Ctrl Pts',(24.5031890807173,-66.8863601198576,
-228.700118508997));
#221897=CARTESIAN_POINT('Ctrl Pts',(24.7931301396491,-66.7918626783751,
-228.829883596514));
#221898=CARTESIAN_POINT('Ctrl Pts',(22.0732081844572,-64.9654158172774,
-231.5599598492));
#221899=CARTESIAN_POINT('Ctrl Pts',(22.3840010183804,-64.9310042721652,
-231.75981083814));
#221900=CARTESIAN_POINT('Ctrl Pts',(22.7103354655404,-64.8270019993908,
-231.902532738117));
#221901=CARTESIAN_POINT('Ctrl Pts',(19.9239651248057,-63.0021267267442,
-234.590483038352));
#221902=CARTESIAN_POINT('Ctrl Pts',(20.2743464925947,-62.9804444339628,
-234.812766684068));
#221903=CARTESIAN_POINT('Ctrl Pts',(20.6355201207023,-62.8599765985421,
-234.979164865714));
#221904=CARTESIAN_POINT('Ctrl Pts',(20.0008767612649,-63.072381322781,-234.482033952692));
#221905=CARTESIAN_POINT('Ctrl Pts',(20.8043363234604,-63.8062709127761,
-233.349112874569));
#221906=CARTESIAN_POINT('Ctrl Pts',(21.6389257523856,-64.5677853736611,
-232.172066819715));
#221907=CARTESIAN_POINT('Ctrl Pts',(22.5046052525514,-65.3568774568241,
-230.950881057122));
#221908=CARTESIAN_POINT('Ctrl Pts',(22.6909951274677,-65.5267772576743,
-230.687946955649));
#221909=CARTESIAN_POINT('Ctrl Pts',(22.8788262188055,-65.6979556905867,
-230.422966630293));
#221910=CARTESIAN_POINT('Ctrl Pts',(23.0680980001634,-65.8704125801202,
-230.15593998937));
#221911=CARTESIAN_POINT('Ctrl Pts',(23.892776251857,-66.6218264735841,-228.992475146313));
#221912=CARTESIAN_POINT('Ctrl Pts',(24.7448045778254,-67.3975073430028,
-227.790160920506));
#221913=CARTESIAN_POINT('Ctrl Pts',(25.6241174401257,-68.1974604163476,
-226.549006038147));
#221914=CARTESIAN_POINT('Ctrl Pts',(25.871454308192,-68.4224746248779,-226.199888705114));
#221915=CARTESIAN_POINT('Ctrl Pts',(26.1209497924506,-68.6494095067943,
-225.847698406426));
#221916=CARTESIAN_POINT('Ctrl Pts',(26.3726020696362,-68.8782657782927,
-225.492435646023));
#221917=CARTESIAN_POINT('Ctrl Pts',(26.3807555168343,-68.8856806427496,
-225.480925254817));
#221918=CARTESIAN_POINT('Ctrl Pts',(26.388911227222,-68.8930975247752,-225.469411638228));
#221919=CARTESIAN_POINT('Ctrl Pts',(26.3970692009449,-68.9005164243056,
-225.457894796357));
#221920=CARTESIAN_POINT('Ctrl Pts',(26.4015990100156,-68.9046358539004,
-225.451499936978));
#221921=CARTESIAN_POINT('Ctrl Pts',(26.4072298854293,-68.9097565796957,
-225.443550657396));
#221922=CARTESIAN_POINT('Ctrl Pts',(26.4106607344689,-68.9128765773254,
-225.438707242511));
#221923=CARTESIAN_POINT('Ctrl Pts',(26.9376257303311,-69.3920960122429,
-224.694777656712));
#221924=CARTESIAN_POINT('Ctrl Pts',(27.4987696124221,-69.9022318817608,
-223.902462772249));
#221925=CARTESIAN_POINT('Ctrl Pts',(28.0941798074988,-70.4432427576873,
-223.06172624895));
#221926=CARTESIAN_POINT('Ctrl Pts',(28.6593592576155,-70.9567849037433,
-222.263676417321));
#221927=CARTESIAN_POINT('Ctrl Pts',(29.2554133760404,-71.4981462944317,
-221.42199684022));
#221928=CARTESIAN_POINT('Ctrl Pts',(29.8824557852991,-72.0672894473805,
-220.536679862955));
#221929=CARTESIAN_POINT('Ctrl Pts',(30.4700178601725,-72.6005977641848,
-219.707104905343));
#221930=CARTESIAN_POINT('Ctrl Pts',(31.0847886949289,-73.1582994545215,
-218.839214470805));
#221931=CARTESIAN_POINT('Ctrl Pts',(31.7269003069944,-73.7403633058953,
-217.933026378428));
#221932=CARTESIAN_POINT('Ctrl Pts',(32.0840513618251,-74.0641149942168,
-217.428992458178));
#221933=CARTESIAN_POINT('Ctrl Pts',(32.449661634212,-74.3954036850947,-216.913110714144));
#221934=CARTESIAN_POINT('Ctrl Pts',(32.8237598256933,-74.7342241033955,
-216.385388039321));
#221935=CARTESIAN_POINT('Ctrl Pts',(33.175226286096,-74.6372704537073,-216.564961398278));
#221936=CARTESIAN_POINT('Ctrl Pts',(31.0696461168607,-72.6787866302694,
-219.626141063516));
#221937=CARTESIAN_POINT('Ctrl Pts',(28.9728566674875,-70.7177341241867,
-222.691713455223));
#221938=CARTESIAN_POINT('Ctrl Pts',(26.8829915137443,-68.7547966262351,
-225.760801301184));
#221939=CARTESIAN_POINT('Ctrl Pts',(24.8618782440303,-66.8564353766477,
-228.728923029172));
#221940=CARTESIAN_POINT('Ctrl Pts',(22.8473703065303,-64.9562682465909,
-231.700386777838));
#221941=CARTESIAN_POINT('Ctrl Pts',(20.8402917354589,-63.0540784607098,
-234.675571320208));
#221942=CARTESIAN_POINT('Ctrl Pts',(49.585934372064,-31.4593264371528,-234.588572160238));
#221943=CARTESIAN_POINT('Ctrl Pts',(49.5518743118955,-31.8037460359236,
-234.831813626471));
#221944=CARTESIAN_POINT('Ctrl Pts',(49.4157810444631,-32.1591416363978,
-235.016540311968));
#221945=CARTESIAN_POINT('Ctrl Pts',(53.6191877437562,-36.2386826179501,
-228.465030977459));
#221946=CARTESIAN_POINT('Ctrl Pts',(53.577029434305,-36.5620211523723,-228.699571716257));
#221947=CARTESIAN_POINT('Ctrl Pts',(53.4511949264874,-36.9037628342018,
-228.868965623418));
#221948=CARTESIAN_POINT('Ctrl Pts',(57.647776611751,-41.0147938695427,-222.337140791317));
#221949=CARTESIAN_POINT('Ctrl Pts',(57.6060482975282,-41.3304581550816,
-222.559407848575));
#221950=CARTESIAN_POINT('Ctrl Pts',(57.4820653937753,-41.6584214713118,
-222.726315285231));
#221951=CARTESIAN_POINT('Ctrl Pts',(61.6760242364039,-45.7878268313144,
-216.206690793878));
#221952=CARTESIAN_POINT('Ctrl Pts',(61.634703071674,-46.0974912749688,-216.419279621934));
#221953=CARTESIAN_POINT('Ctrl Pts',(61.5121276273783,-46.4145707939142,
-216.584292819143));
#221954=CARTESIAN_POINT('Ctrl Pts',(49.628292885354,-32.4090157027691,-234.692796608792));
#221955=CARTESIAN_POINT('Ctrl Pts',(50.3968964627269,-33.3128002682304,
-233.521887849703));
#221956=CARTESIAN_POINT('Ctrl Pts',(51.2000586009216,-34.2576769533107,
-232.298264219454));
#221957=CARTESIAN_POINT('Ctrl Pts',(52.0377754118614,-35.2438971802995,
-231.021914190803));
#221958=CARTESIAN_POINT('Ctrl Pts',(52.1772574460439,-35.4081054206212,
-230.809398581709));
#221959=CARTESIAN_POINT('Ctrl Pts',(52.3176974834605,-35.5734597351558,
-230.595421181564));
#221960=CARTESIAN_POINT('Ctrl Pts',(52.4590955550812,-35.7399611653641,
-230.379981875082));
#221961=CARTESIAN_POINT('Ctrl Pts',(52.9544067724006,-36.3232083421935,
-229.625307473028));
#221962=CARTESIAN_POINT('Ctrl Pts',(53.4614885013061,-36.9204792537099,
-228.852675067089));
#221963=CARTESIAN_POINT('Ctrl Pts',(53.9803314191105,-37.5317625649504,
-228.062098198908));
#221964=CARTESIAN_POINT('Ctrl Pts',(54.3046082427385,-37.9138146344759,
-227.567987656295));
#221965=CARTESIAN_POINT('Ctrl Pts',(54.6334770682644,-38.3013448755334,
-227.066870608985));
#221966=CARTESIAN_POINT('Ctrl Pts',(54.9669330063277,-38.694346084446,-226.558754472118));
#221967=CARTESIAN_POINT('Ctrl Pts',(55.1128199792304,-38.8662841133452,
-226.336453662239));
#221968=CARTESIAN_POINT('Ctrl Pts',(55.2595849207926,-39.0392692670975,
-226.112813235058));
#221969=CARTESIAN_POINT('Ctrl Pts',(55.4072272930583,-39.2133007270977,
-225.887834013941));
#221970=CARTESIAN_POINT('Ctrl Pts',(55.4418309740581,-39.2540893505352,
-225.835104508991));
#221971=CARTESIAN_POINT('Ctrl Pts',(55.4764828535101,-39.294935448816,-225.782301462303));
#221972=CARTESIAN_POINT('Ctrl Pts',(55.5111829239329,-39.3358390104245,
-225.729424885354));
#221973=CARTESIAN_POINT('Ctrl Pts',(55.5197223943885,-39.3459051212891,
-225.716412290246));
#221974=CARTESIAN_POINT('Ctrl Pts',(55.5282647833905,-39.3559747122528,
-225.703395241991));
#221975=CARTESIAN_POINT('Ctrl Pts',(55.5368100908256,-39.3660477831409,
-225.690373740763));
#221976=CARTESIAN_POINT('Ctrl Pts',(55.5410660544895,-39.3710646446184,
-225.683888422768));
#221977=CARTESIAN_POINT('Ctrl Pts',(55.5453227420728,-39.3760823692935,
-225.677402000211));
#221978=CARTESIAN_POINT('Ctrl Pts',(55.5495801535614,-39.3811009571446,
-225.670914473112));
#221979=CARTESIAN_POINT('Ctrl Pts',(55.5517047016773,-39.3836053501054,
-225.667677045038));
#221980=CARTESIAN_POINT('Ctrl Pts',(55.5538294300633,-39.3861099580181,
-225.664439341906));
#221981=CARTESIAN_POINT('Ctrl Pts',(55.5559543387177,-39.38861478088,-225.66120136372));
#221982=CARTESIAN_POINT('Ctrl Pts',(55.5570799677375,-39.3899416620601,
-225.65948610777));
#221983=CARTESIAN_POINT('Ctrl Pts',(55.5582056473433,-39.3912686035581,
-225.657770774635));
#221984=CARTESIAN_POINT('Ctrl Pts',(55.5593313775347,-39.3925956053735,
-225.656055364317));
#221985=CARTESIAN_POINT('Ctrl Pts',(55.5596938325846,-39.3930228645097,
-225.655503048018));
#221986=CARTESIAN_POINT('Ctrl Pts',(55.5600602415825,-39.3934547845997,
-225.654944706604));
#221987=CARTESIAN_POINT('Ctrl Pts',(55.5604310504557,-39.3938918913041,
-225.654379660559));
#221988=CARTESIAN_POINT('Ctrl Pts',(55.56260151923,-39.3964504235328,-225.651072256439));
#221989=CARTESIAN_POINT('Ctrl Pts',(55.5649034761736,-39.3991639557866,
-225.647564487588));
#221990=CARTESIAN_POINT('Ctrl Pts',(55.567076907099,-39.4017259849979,-225.644252568918));
#221991=CARTESIAN_POINT('Ctrl Pts',(55.5681625613162,-39.4030057486127,
-225.64259822673));
#221992=CARTESIAN_POINT('Ctrl Pts',(55.5692161467671,-39.4042477103806,
-225.640992751492));
#221993=CARTESIAN_POINT('Ctrl Pts',(55.5702052568722,-39.4054136694099,
-225.639485525041));
#221994=CARTESIAN_POINT('Ctrl Pts',(55.5707995144804,-39.4061141778977,
-225.638579982998));
#221995=CARTESIAN_POINT('Ctrl Pts',(55.5713704990073,-39.4067872523628,
-225.637709904929));
#221996=CARTESIAN_POINT('Ctrl Pts',(55.5719111825918,-39.4074246083393,
-225.636886000043));
#221997=CARTESIAN_POINT('Ctrl Pts',(55.5721274114958,-39.4076794982383,
-225.636556505944));
#221998=CARTESIAN_POINT('Ctrl Pts',(55.5723390474855,-39.4079289740502,
-225.63623401062));
#221999=CARTESIAN_POINT('Ctrl Pts',(55.5725523044745,-39.4081803607153,
-225.63590904518));
#222000=CARTESIAN_POINT('Ctrl Pts',(56.480606911226,-40.4785922629171,-224.252196527753));
#222001=CARTESIAN_POINT('Ctrl Pts',(57.4295918931899,-41.5977057670165,
-222.806047408064));
#222002=CARTESIAN_POINT('Ctrl Pts',(58.41951461835,-42.7654653352818,-221.297452480847));
#222003=CARTESIAN_POINT('Ctrl Pts',(59.3138922525458,-43.8205154047766,
-219.9344637064));
#222004=CARTESIAN_POINT('Ctrl Pts',(60.2416866050878,-44.9152741778433,
-218.520501594197));
#222005=CARTESIAN_POINT('Ctrl Pts',(61.2029208033956,-46.0496598975624,
-217.055538740336));
#222006=CARTESIAN_POINT('Ctrl Pts',(61.305608086042,-46.1708447110407,-216.899038841658));
#222007=CARTESIAN_POINT('Ctrl Pts',(61.4086770135913,-46.292481719804,-216.741956884158));
#222008=CARTESIAN_POINT('Ctrl Pts',(61.512127627378,-46.4145707939139,-216.584292819143));
#222009=CARTESIAN_POINT('Ctrl Pts',(61.6760242364037,-45.7878268313144,
-216.206690793879));
#222010=CARTESIAN_POINT('Ctrl Pts',(60.5637265567327,-44.4698757063932,
-217.899457957883));
#222011=CARTESIAN_POINT('Ctrl Pts',(59.5069823263366,-43.2175506185294,
-219.507438028199));
#222012=CARTESIAN_POINT('Ctrl Pts',(58.5057724458651,-42.0309753379664,
-221.030605568401));
#222013=CARTESIAN_POINT('Ctrl Pts',(58.0051675056294,-41.4376876976849,
-221.792189338502));
#222014=CARTESIAN_POINT('Ctrl Pts',(57.5184463076789,-40.8608379362804,
-222.532571676405));
#222015=CARTESIAN_POINT('Ctrl Pts',(57.0456083644949,-40.3004320974512,
-223.251750990183));
#222016=CARTESIAN_POINT('Ctrl Pts',(56.8091893929029,-40.0202291780366,
-223.611340647071));
#222017=CARTESIAN_POINT('Ctrl Pts',(56.5762412683301,-39.7441372317215,
-223.965629563901));
#222018=CARTESIAN_POINT('Ctrl Pts',(56.3467639682679,-39.4721564367441,
-224.314617689053));
#222019=CARTESIAN_POINT('Ctrl Pts',(56.2320253182368,-39.3361660392554,
-224.489111751629));
#222020=CARTESIAN_POINT('Ctrl Pts',(56.118154376098,-39.2012034292329,-224.662280617158));
#222021=CARTESIAN_POINT('Ctrl Pts',(56.0051511455154,-39.0672686087644,
-224.834124283574));
#222022=CARTESIAN_POINT('Ctrl Pts',(55.948649530224,-39.0003011985301,-224.920046116782));
#222023=CARTESIAN_POINT('Ctrl Pts',(55.8923648429232,-38.9335907356627,
-225.005636650262));
#222024=CARTESIAN_POINT('Ctrl Pts',(55.8362970842186,-38.8671372180928,
-225.090895883975));
#222025=CARTESIAN_POINT('Ctrl Pts',(55.783733560433,-38.804837045371,-225.170826415581));
#222026=CARTESIAN_POINT('Ctrl Pts',(55.7313606965502,-38.7427627034764,
-225.250465765753));
#222027=CARTESIAN_POINT('Ctrl Pts',(55.6791784931789,-38.6809141896789,
-225.329813934577));
#222028=CARTESIAN_POINT('Ctrl Pts',(55.6756996796209,-38.6767909554257,
-225.335103812498));
#222029=CARTESIAN_POINT('Ctrl Pts',(55.6731827947325,-38.6738078386652,
-225.338930980825));
#222030=CARTESIAN_POINT('Ctrl Pts',(55.6687445946432,-38.6685474979491,
-225.345679685923));
#222031=CARTESIAN_POINT('Ctrl Pts',(54.483867468869,-37.2641814795681,-227.147397981386));
#222032=CARTESIAN_POINT('Ctrl Pts',(53.3720416758563,-35.9463663620178,
-228.837390453384));
#222033=CARTESIAN_POINT('Ctrl Pts',(52.3333167239498,-34.7152710364236,
-230.415667378188));
#222034=CARTESIAN_POINT('Ctrl Pts',(51.3799740041157,-33.5853706100183,
-231.864211396874));
#222035=CARTESIAN_POINT('Ctrl Pts',(50.4882100328808,-32.5285192791855,
-233.21865145119));
#222036=CARTESIAN_POINT('Ctrl Pts',(49.6580997553206,-31.5448418376796,
-234.479004906517));
#222037=CARTESIAN_POINT('Ctrl Pts',(61.6446456814074,19.9883159925443,-216.270380726959));
#222038=CARTESIAN_POINT('Ctrl Pts',(61.616890721367,20.2979288461104,-216.446591335266));
#222039=CARTESIAN_POINT('Ctrl Pts',(61.5168384358512,20.6141575018442,-216.579518431211));
#222040=CARTESIAN_POINT('Ctrl Pts',(57.6234673266503,16.1196899878155,-222.390750665928));
#222041=CARTESIAN_POINT('Ctrl Pts',(57.5955705123416,16.4361291341491,-222.575565676854));
#222042=CARTESIAN_POINT('Ctrl Pts',(57.494494092276,16.762978594578,-222.709815956689));
#222043=CARTESIAN_POINT('Ctrl Pts',(53.6019508938474,12.2476417326856,-228.50878407383));
#222044=CARTESIAN_POINT('Ctrl Pts',(53.5738347736258,12.5726920250932,-228.704663275299));
#222045=CARTESIAN_POINT('Ctrl Pts',(53.4715033219665,12.9130963103019,-228.840508302186));
#222046=CARTESIAN_POINT('Ctrl Pts',(49.5760442618401,8.3708766333566,-234.622127004475));
#222047=CARTESIAN_POINT('Ctrl Pts',(49.5561728047784,8.71705005588278,-234.825566445945));
#222048=CARTESIAN_POINT('Ctrl Pts',(49.444665056238,9.07318219289785,-234.975080467413));
#222049=CARTESIAN_POINT('Ctrl Pts',(49.6480781836462,8.44024209637808,-234.512742074857));
#222050=CARTESIAN_POINT('Ctrl Pts',(50.5108389786845,9.27104318303506,-233.202606649067));
#222051=CARTESIAN_POINT('Ctrl Pts',(51.4422122349174,10.1678939238171,-231.787674256305));
#222052=CARTESIAN_POINT('Ctrl Pts',(52.942166373959,11.6122001294847,-229.508080216706));
#222053=CARTESIAN_POINT('Ctrl Pts',(53.4592996669872,12.1101370188218,-228.722016295096));
#222054=CARTESIAN_POINT('Ctrl Pts',(54.2607151734181,12.8817572829805,-227.503621550068));
#222055=CARTESIAN_POINT('Ctrl Pts',(54.6678517734159,13.273745816856,-226.8845994619));
#222056=CARTESIAN_POINT('Ctrl Pts',(55.1540928798677,13.7418663231132,-226.14521377331));
#222057=CARTESIAN_POINT('Ctrl Pts',(55.4307667843284,14.0082198307574,-225.724473721243));
#222058=CARTESIAN_POINT('Ctrl Pts',(55.5679131202823,14.1402470759619,-225.515906191076));
#222059=CARTESIAN_POINT('Ctrl Pts',(55.6389493534834,14.2086309446081,-225.407874655615));
#222060=CARTESIAN_POINT('Ctrl Pts',(55.6443683020085,14.2138475540897,-225.399633534663));
#222061=CARTESIAN_POINT('Ctrl Pts',(57.4212558731114,15.9243864082124,-222.697345395563));
#222062=CARTESIAN_POINT('Ctrl Pts',(59.4202299305932,17.8482884045604,-219.656016999063));
#222063=CARTESIAN_POINT('Ctrl Pts',(61.6446456814072,19.9883159925442,-216.270380726959));
#222064=CARTESIAN_POINT('Ctrl Pts',(61.5168384358511,20.614157501844,-216.579518431211));
#222065=CARTESIAN_POINT('Ctrl Pts',(60.509204282799,19.6494018606037,-218.115214191548));
#222066=CARTESIAN_POINT('Ctrl Pts',(59.5377925343497,18.7194149348883,-219.595668877975));
#222067=CARTESIAN_POINT('Ctrl Pts',(58.6026020527902,17.8244138442871,-221.020869980282));
#222068=CARTESIAN_POINT('Ctrl Pts',(58.5427562442271,17.7671398824708,-221.112073124469));
#222069=CARTESIAN_POINT('Ctrl Pts',(58.4830587721403,17.710009176867,-221.203049992023));
#222070=CARTESIAN_POINT('Ctrl Pts',(58.4235096385423,17.6530217783262,-221.293800577196));
#222071=CARTESIAN_POINT('Ctrl Pts',(57.9284578513069,17.1792665480993,-222.048240426577));
#222072=CARTESIAN_POINT('Ctrl Pts',(57.4436640563974,16.715388786722,-222.787033765522));
#222073=CARTESIAN_POINT('Ctrl Pts',(56.9691198749181,16.2614050505997,-223.510192149142));
#222074=CARTESIAN_POINT('Ctrl Pts',(56.6725297614939,15.9776652155236,-223.962166138905));
#222075=CARTESIAN_POINT('Ctrl Pts',(56.3799432813792,15.6977900414939,-224.408032920716));
#222076=CARTESIAN_POINT('Ctrl Pts',(56.091358153519,15.4217789157186,-224.847795942265));
#222077=CARTESIAN_POINT('Ctrl Pts',(55.9651021600802,15.3010240481919,-225.040192264193));
#222078=CARTESIAN_POINT('Ctrl Pts',(55.8396120364535,15.1810087617059,-225.231420310576));
#222079=CARTESIAN_POINT('Ctrl Pts',(55.7148875380785,15.0617329150462,-225.421480456045));
#222080=CARTESIAN_POINT('Ctrl Pts',(55.6856552337718,15.0337776384854,-225.466025802639));
#222081=CARTESIAN_POINT('Ctrl Pts',(55.6564649864125,15.0058629803695,-225.510506994689));
#222082=CARTESIAN_POINT('Ctrl Pts',(55.6273167926219,14.9779889384813,-225.554924037388));
#222083=CARTESIAN_POINT('Ctrl Pts',(55.6201436043062,14.9711293109853,-225.56585479399));
#222084=CARTESIAN_POINT('Ctrl Pts',(55.6129729628437,14.9642721432938,-225.576781665572));
#222085=CARTESIAN_POINT('Ctrl Pts',(55.6058048681833,14.9574174353723,-225.587704652211));
#222086=CARTESIAN_POINT('Ctrl Pts',(55.6022348210379,14.954003469513,-225.593144811573));
#222087=CARTESIAN_POINT('Ctrl Pts',(55.5986654056286,14.9505901138013,-225.598584007272));
#222088=CARTESIAN_POINT('Ctrl Pts',(55.595096621949,14.947177368233,-225.604022239318));
#222089=CARTESIAN_POINT('Ctrl Pts',(55.5933157152495,14.9454743282082,-225.606736044567));
#222090=CARTESIAN_POINT('Ctrl Pts',(55.5915349658661,14.943771440124,-225.609449609844));
#222091=CARTESIAN_POINT('Ctrl Pts',(55.589754373798,14.9420687039798,-225.612162935149));
#222092=CARTESIAN_POINT('Ctrl Pts',(55.5887986781916,14.9411547959146,-225.613619255841));
#222093=CARTESIAN_POINT('Ctrl Pts',(55.5878430279043,14.94024093162,-225.615075507402));
#222094=CARTESIAN_POINT('Ctrl Pts',(55.586887422936,14.9393271110959,-225.616531689833));
#222095=CARTESIAN_POINT('Ctrl Pts',(55.5865850402481,14.9390379502863,-225.616992470565));
#222096=CARTESIAN_POINT('Ctrl Pts',(55.5862873065917,14.9387532352696,-225.617446166943));
#222097=CARTESIAN_POINT('Ctrl Pts',(55.5859935256647,14.9384723001864,-225.617893840014));
#222098=CARTESIAN_POINT('Ctrl Pts',(55.584266632255,14.9368209167942,-225.62052533718));
#222099=CARTESIAN_POINT('Ctrl Pts',(55.5826696508247,14.9352937661347,-225.622958869973));
#222100=CARTESIAN_POINT('Ctrl Pts',(55.5809424055013,14.9336420489766,-225.625590902938));
#222101=CARTESIAN_POINT('Ctrl Pts',(55.5800796262211,14.9328169969,-225.626905634248));
#222102=CARTESIAN_POINT('Ctrl Pts',(55.5791843445349,14.9319608640104,-225.628269893732));
#222103=CARTESIAN_POINT('Ctrl Pts',(55.578224133597,14.9310426415477,-225.629733094454));
#222104=CARTESIAN_POINT('Ctrl Pts',(55.5776368070909,14.9304809978822,-225.630628081727));
#222105=CARTESIAN_POINT('Ctrl Pts',(55.5770251884148,14.929896124466,-225.631560086172));
#222106=CARTESIAN_POINT('Ctrl Pts',(55.5763818568836,14.92928092516,-225.632540415665));
#222107=CARTESIAN_POINT('Ctrl Pts',(55.5761254152632,14.9290356974675,-225.632931189739));
#222108=CARTESIAN_POINT('Ctrl Pts',(55.5758654862487,14.9287871349127,-225.633327278013));
#222109=CARTESIAN_POINT('Ctrl Pts',(55.5756069918427,14.9285399442642,-225.633721180178));
#222110=CARTESIAN_POINT('Ctrl Pts',(54.6009073193254,13.9964631235507,-227.119000174852));
#222111=CARTESIAN_POINT('Ctrl Pts',(53.6642063037329,13.101179913745,-228.546300112712));
#222112=CARTESIAN_POINT('Ctrl Pts',(52.7655077853552,12.2427220677471,-229.915616611674));
#222113=CARTESIAN_POINT('Ctrl Pts',(51.8033650152148,11.323660788456,-231.381600968574));
#222114=CARTESIAN_POINT('Ctrl Pts',(50.8847798806897,10.4468075147946,-232.781126025169));
#222115=CARTESIAN_POINT('Ctrl Pts',(50.0097760330178,9.61214928592863,-234.114165364083));
#222116=CARTESIAN_POINT('Ctrl Pts',(49.8830780335951,9.49129321417494,-234.307185563756));
#222117=CARTESIAN_POINT('Ctrl Pts',(49.7572937961925,9.37132173405822,-234.498811779421));
#222118=CARTESIAN_POINT('Ctrl Pts',(49.6324234200406,9.25223473081225,-234.689043900262));
#222119=CARTESIAN_POINT('Ctrl Pts',(23.3435674340446,39.0028315981393,-234.685329588431));
#222120=CARTESIAN_POINT('Ctrl Pts',(23.6220011219804,38.9711607503308,-234.795474514856));
#222121=CARTESIAN_POINT('Ctrl Pts',(23.9003793742244,38.8880062428325,-234.874538682189));
#222122=CARTESIAN_POINT('Ctrl Pts',(24.8211107939746,40.877797860099,-231.583566767888));
#222123=CARTESIAN_POINT('Ctrl Pts',(25.0911477353951,40.8413970872541,-231.693486415051));
#222124=CARTESIAN_POINT('Ctrl Pts',(25.3613763065334,40.7570726336726,-231.772074584151));
#222125=CARTESIAN_POINT('Ctrl Pts',(26.3601379756881,42.7472614109061,-228.507926237645));
#222126=CARTESIAN_POINT('Ctrl Pts',(26.6294910045101,42.7083687308544,-228.618918190678));
#222127=CARTESIAN_POINT('Ctrl Pts',(26.8976008468902,42.6201313634466,-228.700804952979));
#222128=CARTESIAN_POINT('Ctrl Pts',(29.5673202653105,46.4871525231188,-222.371256086851));
#222129=CARTESIAN_POINT('Ctrl Pts',(29.8423301360257,46.4421792512365,-222.490600959002));
#222130=CARTESIAN_POINT('Ctrl Pts',(30.1156268744464,46.3449292397562,-222.578666771697));
#222131=CARTESIAN_POINT('Ctrl Pts',(31.2349886649714,48.357017195617,-219.311797960276));
#222132=CARTESIAN_POINT('Ctrl Pts',(31.5173957493039,48.3097394640464,-219.436505895139));
#222133=CARTESIAN_POINT('Ctrl Pts',(31.7969999993534,48.2062302604519,-219.529408809912));
#222134=CARTESIAN_POINT('Ctrl Pts',(32.9442943454133,50.2193438073887,-216.27126917285));
#222135=CARTESIAN_POINT('Ctrl Pts',(33.2349457782287,50.1687782395761,-216.404317351376));
#222136=CARTESIAN_POINT('Ctrl Pts',(33.5239821027453,50.0594436315753,-216.500446897106));
#222137=CARTESIAN_POINT('Ctrl Pts',(23.9972286658434,39.0117605909834,-234.669151698811));
#222138=CARTESIAN_POINT('Ctrl Pts',(24.3327345456529,39.4399669118617,-233.958598804035));
#222139=CARTESIAN_POINT('Ctrl Pts',(24.6854969464168,39.8847826332992,-233.221626122003));
#222140=CARTESIAN_POINT('Ctrl Pts',(25.2417823256465,40.576961386451,-232.076537418069));
#222141=CARTESIAN_POINT('Ctrl Pts',(25.4317384457601,40.8118462958157,-231.688236236611));
#222142=CARTESIAN_POINT('Ctrl Pts',(25.723657541265,41.1704115471192,-231.095877044201));
#222143=CARTESIAN_POINT('Ctrl Pts',(25.8713636961786,41.3512535867699,-230.797220592941));
#222144=CARTESIAN_POINT('Ctrl Pts',(26.0467904156662,41.564964282497,-230.444453570124));
#222145=CARTESIAN_POINT('Ctrl Pts',(26.1416066636588,41.6801828126252,-230.254310210665));
#222146=CARTESIAN_POINT('Ctrl Pts',(26.1860831699019,41.7341503401857,-230.165260585893));
#222147=CARTESIAN_POINT('Ctrl Pts',(26.2115545459155,41.7650376285435,-230.114297684302));
#222148=CARTESIAN_POINT('Ctrl Pts',(26.2187586061939,41.7737714214641,-230.099887554133));
#222149=CARTESIAN_POINT('Ctrl Pts',(26.5792284479624,42.210703138559,-229.378993935433));
#222150=CARTESIAN_POINT('Ctrl Pts',(26.9502784517109,42.6554480634503,-228.645975349437));
#222151=CARTESIAN_POINT('Ctrl Pts',(27.5320846287234,43.3443938192852,-227.511624012913));
#222152=CARTESIAN_POINT('Ctrl Pts',(27.8292992959109,43.6943231798319,-226.935742480268));
#222153=CARTESIAN_POINT('Ctrl Pts',(28.187363035252,44.1121215812652,-226.248645429514));
#222154=CARTESIAN_POINT('Ctrl Pts',(28.3692597182274,44.3234069165231,-225.90128808847));
#222155=CARTESIAN_POINT('Ctrl Pts',(28.4674767065592,44.4372345141931,-225.714183580142));
#222156=CARTESIAN_POINT('Ctrl Pts',(28.5135222374433,44.4905279982249,-225.626590416781));
#222157=CARTESIAN_POINT('Ctrl Pts',(28.5398857549393,44.5210240112345,-225.576469166008));
#222158=CARTESIAN_POINT('Ctrl Pts',(28.5472959748104,44.5295939877615,-225.562384320267));
#222159=CARTESIAN_POINT('Ctrl Pts',(28.9232877526146,44.9643580741901,-224.847853406652));
#222160=CARTESIAN_POINT('Ctrl Pts',(29.3098036855485,45.4068161964465,-224.121210421383));
#222161=CARTESIAN_POINT('Ctrl Pts',(29.9147542901699,46.0921360058483,-222.996588661072));
#222162=CARTESIAN_POINT('Ctrl Pts',(30.223526374801,46.4402036354049,-222.425613460314));
#222163=CARTESIAN_POINT('Ctrl Pts',(30.594963504495,46.8557539570813,-221.744313165042));
#222164=CARTESIAN_POINT('Ctrl Pts',(30.7835078386655,47.0658975627284,-221.399872377143));
#222165=CARTESIAN_POINT('Ctrl Pts',(30.8852740454166,47.1791089645397,-221.214335176413));
#222166=CARTESIAN_POINT('Ctrl Pts',(30.9329723885077,47.2321136761852,-221.127474748553));
#222167=CARTESIAN_POINT('Ctrl Pts',(30.9602794753431,47.2624443837978,-221.077772528342));
#222168=CARTESIAN_POINT('Ctrl Pts',(30.9679432262936,47.2709552412231,-221.063826154286));
#222169=CARTESIAN_POINT('Ctrl Pts',(31.7422680026501,48.1307494830713,-219.654932201219));
#222170=CARTESIAN_POINT('Ctrl Pts',(32.5743824792101,49.0398372611993,-218.167004164594));
#222171=CARTESIAN_POINT('Ctrl Pts',(33.473440697418,50.0051916640197,-216.589120385862));
#222172=CARTESIAN_POINT('Ctrl Pts',(32.8943360433598,50.1648136138275,-216.360311415042));
#222173=CARTESIAN_POINT('Ctrl Pts',(31.9457996056765,49.1307894599697,-218.048583135007));
#222174=CARTESIAN_POINT('Ctrl Pts',(31.0649583664921,48.1537646198439,-219.645964150516));
#222175=CARTESIAN_POINT('Ctrl Pts',(29.839374049799,46.7731472080332,-221.905699617094));
#222176=CARTESIAN_POINT('Ctrl Pts',(29.4468033566793,46.3270986719498,-222.636222096506));
#222177=CARTESIAN_POINT('Ctrl Pts',(28.8812510347518,45.6792205773753,-223.697921801452));
#222178=CARTESIAN_POINT('Ctrl Pts',(28.6043018556398,45.3605804968602,-224.220250650383));
#222179=CARTESIAN_POINT('Ctrl Pts',(28.2912644925847,44.998100764893,-224.814722551268));
#222180=CARTESIAN_POINT('Ctrl Pts',(28.1372482450597,44.8191770801532,-225.108230562661));
#222181=CARTESIAN_POINT('Ctrl Pts',(28.0526798290621,44.7207710516647,-225.269676371552));
#222182=CARTESIAN_POINT('Ctrl Pts',(28.0119681642909,44.6733490752071,-225.347483262868));
#222183=CARTESIAN_POINT('Ctrl Pts',(27.990307112259,44.6481055978128,-225.388902606174));
#222184=CARTESIAN_POINT('Ctrl Pts',(27.9883067709655,44.6457743250737,-225.39272775696));
#222185=CARTESIAN_POINT('Ctrl Pts',(26.2378764098086,42.6055670942602,-228.740321770674));
#222186=CARTESIAN_POINT('Ctrl Pts',(24.7202894771203,40.7480003447697,-231.798693741316));
#222187=CARTESIAN_POINT('Ctrl Pts',(23.3965311730097,39.0699180251917,-234.574369193282));
#222188=CARTESIAN_POINT('Origin',(7.99493453126772,-4.92182388367686,-192.281986444803));
#222189=CARTESIAN_POINT('',(7.45184924284871,-4.40456343718705,-229.35005));
#222190=CARTESIAN_POINT('',(8.57396770167424,-4.44514727677342,-229.35005));
#222191=CARTESIAN_POINT('Origin',(7.99493453126772,-4.92182388367686,-229.35005));
#222192=CARTESIAN_POINT('',(7.45184924284871,-4.40456343718705,-192.281986444803));
#222193=CARTESIAN_POINT('',(8.57396770167424,-4.44514727677342,-192.281986444803));
#222194=CARTESIAN_POINT('Origin',(1.25,-20.2703558849778,-192.281986444803));
#222195=CARTESIAN_POINT('',(0.5,-20.2703558849778,-229.35005));
#222196=CARTESIAN_POINT('',(0.5,-20.2703558849778,-235.35005));
#222197=CARTESIAN_POINT('',(1.14413406213993,-19.5278652094801,-229.35005));
#222198=CARTESIAN_POINT('',(1.14413406213993,-19.5278652094801,-192.281986444803));
#222199=CARTESIAN_POINT('Origin',(1.25,-20.2703558849778,-229.35005));
#222200=CARTESIAN_POINT('Origin',(10.2798200094577,-12.7534818258363,-192.281986444803));
#222201=CARTESIAN_POINT('',(10.2798200094577,-12.0034818258363,-229.35005));
#222202=CARTESIAN_POINT('',(10.2798200094577,-12.0034818258363,-229.35005));
#222203=CARTESIAN_POINT('',(11.0243360211906,-12.844013081618,-229.35005));
#222204=CARTESIAN_POINT('',(11.0243360211906,-12.844013081618,-192.281986444803));
#222205=CARTESIAN_POINT('Origin',(10.2798200094577,-12.7534818258363,-229.35005));
#222206=CARTESIAN_POINT('Origin',(8.76687405914144,-12.7534818258363,-192.281986444803));
#222207=CARTESIAN_POINT('',(8.02438338364376,-12.6476158879763,-229.35005));
#222208=CARTESIAN_POINT('',(8.02438338364376,-12.6476158879763,-192.281986444803));
#222209=CARTESIAN_POINT('',(8.76687405914144,-12.0034818258363,-229.35005));
#222210=CARTESIAN_POINT('',(8.76687405914144,-12.0034818258363,-235.35005));
#222211=CARTESIAN_POINT('Origin',(8.76687405914144,-12.7534818258363,-229.35005));
#222212=CARTESIAN_POINT('Origin',(8.76687405914145,-10.2534818258363,-192.281986444803));
#222213=CARTESIAN_POINT('',(8.76687405914145,-11.0034818258363,-229.35005));
#222214=CARTESIAN_POINT('',(8.76687405914145,-11.0034818258363,-229.35005));
#222215=CARTESIAN_POINT('',(8.02438338364376,-10.3593477636964,-229.35005));
#222216=CARTESIAN_POINT('',(8.02438338364376,-10.3593477636964,-192.281986444803));
#222217=CARTESIAN_POINT('Origin',(8.76687405914145,-10.2534818258363,-229.35005));
#222218=CARTESIAN_POINT('Origin',(10.2798200094577,-10.2534818258363,-192.281986444803));
#222219=CARTESIAN_POINT('',(11.0243360211906,-10.1629505700546,-229.35005));
#222220=CARTESIAN_POINT('',(11.0243360211906,-10.1629505700546,-192.281986444803));
#222221=CARTESIAN_POINT('',(10.2798200094577,-11.0034818258363,-229.35005));
#222222=CARTESIAN_POINT('',(10.2798200094577,-11.0034818258363,-229.35005));
#222223=CARTESIAN_POINT('Origin',(10.2798200094577,-10.2534818258363,-229.35005));
#222224=CARTESIAN_POINT('Origin',(6.95148506756697,-6.01736880073006,-192.281986444803));
#222225=CARTESIAN_POINT('',(6.36274467860838,-6.48200280121742,-229.35005));
#222226=CARTESIAN_POINT('',(6.36274467860838,-6.48200280121742,-192.281986444803));
#222227=CARTESIAN_POINT('',(6.40839977914796,-5.50010835424024,-229.35005));
#222228=CARTESIAN_POINT('',(6.40839977914796,-5.50010835424024,-235.35005));
#222229=CARTESIAN_POINT('Origin',(6.95148506756697,-6.01736880073006,-229.35005));
#222230=CARTESIAN_POINT('Origin',(5.14120077283694,-4.29316731243069,-192.281986444803));
#222231=CARTESIAN_POINT('',(5.68428606125595,-4.81042775892049,-229.35005));
#222232=CARTESIAN_POINT('',(5.68428606125595,-4.81042775892049,-229.35005));
#222233=CARTESIAN_POINT('',(4.70577833960231,-4.90382867901287,-229.35005));
#222234=CARTESIAN_POINT('',(4.70577833960231,-4.90382867901288,-192.281986444803));
#222235=CARTESIAN_POINT('Origin',(5.14120077283694,-4.29316731243068,-229.35005));
#222236=CARTESIAN_POINT('Origin',(1.25,-2.73660776669488,-192.281986444803));
#222237=CARTESIAN_POINT('',(1.14413406213993,-3.47909844219256,-229.35005));
#222238=CARTESIAN_POINT('',(1.14413406213993,-3.47909844219257,-192.281986444803));
#222239=CARTESIAN_POINT('',(0.5,-2.73660776669487,-229.35005));
#222240=CARTESIAN_POINT('',(0.5,-2.73660776669487,-235.35005));
#222241=CARTESIAN_POINT('Origin',(1.25,-2.73660776669487,-229.35005));
#222242=CARTESIAN_POINT('Origin',(8.87499999999985,-23.3741205625531,-192.281986444803));
#222243=CARTESIAN_POINT('',(8.83216440217218,-22.6253448207192,-229.35005));
#222244=CARTESIAN_POINT('',(9.62499999999985,-23.3741205625531,-229.35005));
#222245=CARTESIAN_POINT('Origin',(8.87499999999985,-23.3741205625531,-229.35005));
#222246=CARTESIAN_POINT('',(8.83216440217218,-22.6253448207192,-192.281986444803));
#222247=CARTESIAN_POINT('',(9.62499999999985,-23.3741205625531,-235.35005));
#222248=CARTESIAN_POINT('Origin',(12.7946237611812,-12.7534818258363,-192.281986444803));
#222249=CARTESIAN_POINT('',(12.0481776255232,-12.6805560652209,-229.35005));
#222250=CARTESIAN_POINT('',(12.0481776255232,-12.6805560652209,-192.281986444803));
#222251=CARTESIAN_POINT('',(12.7946237611812,-12.0034818258363,-229.35005));
#222252=CARTESIAN_POINT('',(12.7946237611812,-12.0034818258363,-235.35005));
#222253=CARTESIAN_POINT('Origin',(12.7946237611812,-12.7534818258363,-229.35005));
#222254=CARTESIAN_POINT('Origin',(11.3749999999999,-20.8590213785032,-229.35005));
#222255=CARTESIAN_POINT('',(11.3749999999999,-21.6090213785032,-229.35005));
#222256=CARTESIAN_POINT('',(11.3749999999999,-21.6090213785032,-229.35005));
#222257=CARTESIAN_POINT('',(10.6249999999999,-20.8590213785032,-229.35005));
#222258=CARTESIAN_POINT('',(10.6249999999999,-20.8590213785032,-235.35005));
#222259=CARTESIAN_POINT('Origin',(11.3749999999999,-20.8590213785032,-229.35005));
#222260=CARTESIAN_POINT('Origin',(19.,-20.8590213785032,-229.35005));
#222261=CARTESIAN_POINT('',(19.75,-20.8590213785032,-229.35005));
#222262=CARTESIAN_POINT('',(19.75,-20.8590213785032,-235.35005));
#222263=CARTESIAN_POINT('',(19.,-21.6090213785031,-229.35005));
#222264=CARTESIAN_POINT('',(19.,-21.6090213785031,-229.35005));
#222265=CARTESIAN_POINT('Origin',(19.,-20.8590213785032,-229.35005));
#222266=CARTESIAN_POINT('Origin',(19.,-12.7534818258363,-229.35005));
#222267=CARTESIAN_POINT('',(19.,-12.0034818258363,-229.35005));
#222268=CARTESIAN_POINT('',(19.,-12.0034818258363,-229.35005));
#222269=CARTESIAN_POINT('',(19.75,-12.7534818258363,-229.35005));
#222270=CARTESIAN_POINT('',(19.75,-12.7534818258363,-235.35005));
#222271=CARTESIAN_POINT('Origin',(19.,-12.7534818258363,-229.35005));
#222272=CARTESIAN_POINT('Origin',(12.7946237611812,-10.2534818258363,-192.281986444803));
#222273=CARTESIAN_POINT('',(12.7946237611812,-11.0034818258363,-229.35005));
#222274=CARTESIAN_POINT('',(12.7946237611812,-11.0034818258363,-229.35005));
#222275=CARTESIAN_POINT('',(12.0481776255232,-10.3264075864518,-229.35005));
#222276=CARTESIAN_POINT('',(12.0481776255232,-10.3264075864518,-192.281986444803));
#222277=CARTESIAN_POINT('Origin',(12.7946237611812,-10.2534818258363,-229.35005));
#222278=CARTESIAN_POINT('Origin',(19.,-10.2534818258363,-229.35005));
#222279=CARTESIAN_POINT('',(19.75,-10.2534818258363,-229.35005));
#222280=CARTESIAN_POINT('',(19.75,-10.2534818258363,-235.35005));
#222281=CARTESIAN_POINT('',(19.,-11.0034818258363,-229.35005));
#222282=CARTESIAN_POINT('',(19.,-11.0034818258363,-229.35005));
#222283=CARTESIAN_POINT('Origin',(19.,-10.2534818258363,-229.35005));
#222284=CARTESIAN_POINT('Origin',(19.,-2.14794227316951,-229.35005));
#222285=CARTESIAN_POINT('',(19.,-1.39794227316951,-229.35005));
#222286=CARTESIAN_POINT('',(19.,-1.39794227316951,-229.35005));
#222287=CARTESIAN_POINT('',(19.75,-2.14794227316951,-229.35005));
#222288=CARTESIAN_POINT('',(19.75,-2.14794227316951,-235.35005));
#222289=CARTESIAN_POINT('Origin',(19.,-2.14794227316951,-229.35005));
#222290=CARTESIAN_POINT('Origin',(11.3749999999999,-2.14794227316951,-229.35005));
#222291=CARTESIAN_POINT('',(10.6249999999999,-2.14794227316951,-229.35005));
#222292=CARTESIAN_POINT('',(10.6249999999999,-2.14794227316951,-235.35005));
#222293=CARTESIAN_POINT('',(11.3749999999999,-1.3979422731695,-229.35005));
#222294=CARTESIAN_POINT('',(11.3749999999999,-1.3979422731695,-229.35005));
#222295=CARTESIAN_POINT('Origin',(11.3749999999999,-2.14794227316951,-229.35005));
#222296=CARTESIAN_POINT('Origin',(8.87499999999985,0.367156910880378,-192.281986444803));
#222297=CARTESIAN_POINT('',(9.62499999999985,0.367156910880385,-229.35005));
#222298=CARTESIAN_POINT('',(9.62499999999985,0.367156910880383,-229.35005));
#222299=CARTESIAN_POINT('',(8.83216440217218,-0.38161883095341,-229.35005));
#222300=CARTESIAN_POINT('',(8.83216440217218,-0.381618830953416,-192.281986444803));
#222301=CARTESIAN_POINT('Origin',(8.87499999999985,0.367156910880383,-229.35005));
#222302=CARTESIAN_POINT('Origin',(8.87499999999986,8.45759727949731,-229.35005));
#222303=CARTESIAN_POINT('',(8.87499999999986,9.20759727949731,-229.35005));
#222304=CARTESIAN_POINT('',(8.87499999999986,9.20759727949731,-229.35005));
#222305=CARTESIAN_POINT('',(9.62499999999986,8.45759727949731,-229.35005));
#222306=CARTESIAN_POINT('',(9.62499999999986,8.45759727949731,-235.35005));
#222307=CARTESIAN_POINT('Origin',(8.87499999999986,8.45759727949731,-229.35005));
#222308=CARTESIAN_POINT('Origin',(1.25,8.45759727949731,-229.35005));
#222309=CARTESIAN_POINT('',(0.5,8.45759727949731,-229.35005));
#222310=CARTESIAN_POINT('',(0.5,8.45759727949731,-235.35005));
#222311=CARTESIAN_POINT('',(1.25,9.20759727949731,-229.35005));
#222312=CARTESIAN_POINT('',(1.25,9.20759727949731,-229.35005));
#222313=CARTESIAN_POINT('Origin',(1.25,8.45759727949731,-229.35005));
#222314=CARTESIAN_POINT('Origin',(1.25,2.29555713691451,-192.281986444803));
#222315=CARTESIAN_POINT('',(1.18233753211584,1.54861551239502,-229.35005));
#222316=CARTESIAN_POINT('',(1.18233753211584,1.54861551239501,-192.281986444803));
#222317=CARTESIAN_POINT('',(0.5,2.29555713691451,-229.35005));
#222318=CARTESIAN_POINT('',(0.5,2.29555713691451,-235.35005));
#222319=CARTESIAN_POINT('Origin',(1.25,2.29555713691451,-229.35005));
#222320=CARTESIAN_POINT('Origin',(1.25,-25.3025207885872,-192.281986444803));
#222321=CARTESIAN_POINT('',(0.5,-25.3025207885872,-229.35005));
#222322=CARTESIAN_POINT('',(0.5,-25.3025207885872,-235.35005));
#222323=CARTESIAN_POINT('',(1.18233753211584,-24.5555791640676,-229.35005));
#222324=CARTESIAN_POINT('',(1.18233753211584,-24.5555791640676,-192.281986444803));
#222325=CARTESIAN_POINT('Origin',(1.25,-25.3025207885872,-229.35005));
#222326=CARTESIAN_POINT('Origin',(1.25,-31.46456093117,-229.35005));
#222327=CARTESIAN_POINT('',(1.25,-32.21456093117,-229.35005));
#222328=CARTESIAN_POINT('',(1.25,-32.21456093117,-229.35005));
#222329=CARTESIAN_POINT('',(0.5,-31.46456093117,-229.35005));
#222330=CARTESIAN_POINT('',(0.5,-31.46456093117,-235.35005));
#222331=CARTESIAN_POINT('Origin',(1.25,-31.46456093117,-229.35005));
#222332=CARTESIAN_POINT('Origin',(8.87499999999984,-31.46456093117,-229.35005));
#222333=CARTESIAN_POINT('',(9.62499999999984,-31.46456093117,-229.35005));
#222334=CARTESIAN_POINT('',(9.62499999999984,-31.46456093117,-235.35005));
#222335=CARTESIAN_POINT('',(8.87499999999984,-32.21456093117,-229.35005));
#222336=CARTESIAN_POINT('',(8.87499999999984,-32.21456093117,-229.35005));
#222337=CARTESIAN_POINT('Origin',(8.87499999999984,-31.46456093117,-229.35005));
#222338=CARTESIAN_POINT('Origin',(31.625,21.5631368321642,-229.35005));
#222339=CARTESIAN_POINT('',(31.625,20.8131368321642,-229.35005));
#222340=CARTESIAN_POINT('',(31.625,20.8131368321642,-229.35005));
#222341=CARTESIAN_POINT('',(30.875,21.5631368321642,-229.35005));
#222342=CARTESIAN_POINT('',(30.875,21.5631368321642,-235.35005));
#222343=CARTESIAN_POINT('Origin',(31.625,21.5631368321642,-229.35005));
#222344=CARTESIAN_POINT('Origin',(33.751462642771,21.5631368321642,-229.35005));
#222345=CARTESIAN_POINT('',(34.2872001450371,22.0880037949896,-229.35005));
#222346=CARTESIAN_POINT('',(34.2872001450371,22.0880037949896,-229.35005));
#222347=CARTESIAN_POINT('',(33.751462642771,20.8131368321642,-229.35005));
#222348=CARTESIAN_POINT('',(33.751462642771,20.8131368321642,-229.35005));
#222349=CARTESIAN_POINT('Origin',(33.751462642771,21.5631368321642,-229.35005));
#222350=CARTESIAN_POINT('Origin',(31.625,23.6023848491226,-229.35005));
#222351=CARTESIAN_POINT('',(30.875,23.6023848491226,-229.35005));
#222352=CARTESIAN_POINT('',(32.1269841269841,24.1596208280901,-229.35005));
#222353=CARTESIAN_POINT('Origin',(31.625,23.6023848491226,-229.35005));
#222354=CARTESIAN_POINT('',(30.875,23.6023848491226,-229.35005));
#222355=CARTESIAN_POINT('',(32.1269841269841,24.1596208280901,-229.35005));
#222356=CARTESIAN_POINT('Origin',(29.125,19.0631368321642,-229.35005));
#222357=CARTESIAN_POINT('',(29.125,19.8131368321642,-229.35005));
#222358=CARTESIAN_POINT('',(29.125,19.8131368321642,-229.35005));
#222359=CARTESIAN_POINT('',(29.875,19.0631368321642,-229.35005));
#222360=CARTESIAN_POINT('',(29.875,19.0631368321642,-235.35005));
#222361=CARTESIAN_POINT('Origin',(29.125,19.0631368321642,-229.35005));
#222362=CARTESIAN_POINT('Origin',(21.5,19.0631368321642,-229.35005));
#222363=CARTESIAN_POINT('',(20.75,19.0631368321642,-229.35005));
#222364=CARTESIAN_POINT('',(20.75,19.0631368321642,-235.35005));
#222365=CARTESIAN_POINT('',(21.5,19.8131368321642,-229.35005));
#222366=CARTESIAN_POINT('',(21.5,19.8131368321642,-229.35005));
#222367=CARTESIAN_POINT('Origin',(21.5,19.0631368321642,-229.35005));
#222368=CARTESIAN_POINT('Origin',(21.5,10.9575972794973,-229.35005));
#222369=CARTESIAN_POINT('',(21.5,10.2075972794973,-229.35005));
#222370=CARTESIAN_POINT('',(21.5,10.2075972794973,-229.35005));
#222371=CARTESIAN_POINT('',(20.75,10.9575972794973,-229.35005));
#222372=CARTESIAN_POINT('',(20.75,10.9575972794973,-235.35005));
#222373=CARTESIAN_POINT('Origin',(21.5,10.9575972794973,-229.35005));
#222374=CARTESIAN_POINT('Origin',(29.125,10.9575972794973,-229.35005));
#222375=CARTESIAN_POINT('',(29.875,10.9575972794973,-229.35005));
#222376=CARTESIAN_POINT('',(29.875,10.9575972794973,-235.35005));
#222377=CARTESIAN_POINT('',(29.125,10.2075972794973,-229.35005));
#222378=CARTESIAN_POINT('',(29.125,10.2075972794973,-229.35005));
#222379=CARTESIAN_POINT('Origin',(29.125,10.9575972794973,-229.35005));
#222380=CARTESIAN_POINT('Origin',(29.125,8.45759727949731,-229.35005));
#222381=CARTESIAN_POINT('',(29.125,9.20759727949731,-229.35005));
#222382=CARTESIAN_POINT('',(29.125,9.20759727949731,-229.35005));
#222383=CARTESIAN_POINT('',(29.875,8.45759727949731,-229.35005));
#222384=CARTESIAN_POINT('',(29.875,8.45759727949731,-235.35005));
#222385=CARTESIAN_POINT('Origin',(29.125,8.45759727949731,-229.35005));
#222386=CARTESIAN_POINT('Origin',(21.5,8.45759727949731,-229.35005));
#222387=CARTESIAN_POINT('',(20.75,8.45759727949731,-229.35005));
#222388=CARTESIAN_POINT('',(20.75,8.45759727949731,-235.35005));
#222389=CARTESIAN_POINT('',(21.5,9.20759727949731,-229.35005));
#222390=CARTESIAN_POINT('',(21.5,9.20759727949731,-229.35005));
#222391=CARTESIAN_POINT('Origin',(21.5,8.45759727949731,-229.35005));
#222392=CARTESIAN_POINT('Origin',(21.5,0.35205772683049,-229.35005));
#222393=CARTESIAN_POINT('',(21.5,-0.39794227316951,-229.35005));
#222394=CARTESIAN_POINT('',(21.5,-0.39794227316951,-229.35005));
#222395=CARTESIAN_POINT('',(20.75,0.352057726830487,-229.35005));
#222396=CARTESIAN_POINT('',(20.75,0.352057726830487,-235.35005));
#222397=CARTESIAN_POINT('Origin',(21.5,0.35205772683049,-229.35005));
#222398=CARTESIAN_POINT('Origin',(29.125,0.352057726830493,-229.35005));
#222399=CARTESIAN_POINT('',(29.875,0.352057726830494,-229.35005));
#222400=CARTESIAN_POINT('',(29.875,0.352057726830494,-235.35005));
#222401=CARTESIAN_POINT('',(29.125,-0.397942273169507,-229.35005));
#222402=CARTESIAN_POINT('',(29.125,-0.397942273169507,-229.35005));
#222403=CARTESIAN_POINT('Origin',(29.125,0.352057726830493,-229.35005));
#222404=CARTESIAN_POINT('Origin',(29.125,-44.5701004838368,-229.35005));
#222405=CARTESIAN_POINT('',(29.125,-43.8201004838368,-229.35005));
#222406=CARTESIAN_POINT('',(29.125,-43.8201004838368,-229.35005));
#222407=CARTESIAN_POINT('',(29.875,-44.5701004838368,-229.35005));
#222408=CARTESIAN_POINT('',(29.875,-44.5701004838368,-235.35005));
#222409=CARTESIAN_POINT('Origin',(29.125,-44.5701004838368,-229.35005));
#222410=CARTESIAN_POINT('Origin',(21.5,-44.5701004838368,-229.35005));
#222411=CARTESIAN_POINT('',(20.75,-44.5701004838368,-229.35005));
#222412=CARTESIAN_POINT('',(20.75,-44.5701004838368,-235.35005));
#222413=CARTESIAN_POINT('',(21.5,-43.8201004838368,-229.35005));
#222414=CARTESIAN_POINT('',(21.5,-43.8201004838368,-229.35005));
#222415=CARTESIAN_POINT('Origin',(21.5,-44.5701004838368,-229.35005));
#222416=CARTESIAN_POINT('Origin',(21.5,-52.8339989151841,-229.35005));
#222417=CARTESIAN_POINT('',(21.5238294101153,-53.5836202590728,-229.35005));
#222418=CARTESIAN_POINT('',(21.5238294101154,-53.5836202590729,-229.35005));
#222419=CARTESIAN_POINT('',(20.75,-52.8339989151841,-229.35005));
#222420=CARTESIAN_POINT('',(20.75,-52.8339989151841,-235.35005));
#222421=CARTESIAN_POINT('Origin',(21.5,-52.8339989151841,-229.35005));
#222422=CARTESIAN_POINT('Origin',(29.125,-48.7096221120845,-229.35005));
#222423=CARTESIAN_POINT('',(29.875,-48.7096221120845,-229.35005));
#222424=CARTESIAN_POINT('',(29.875,-48.7096221120845,-229.35005));
#222425=CARTESIAN_POINT('',(29.5873015873016,-49.3001957674217,-229.35005));
#222426=CARTESIAN_POINT('',(29.5873015873016,-49.3001957674217,-229.35005));
#222427=CARTESIAN_POINT('Origin',(29.125,-48.7096221120845,-229.35005));
#222428=CARTESIAN_POINT('Origin',(31.625,-42.0701004838368,-229.35005));
#222429=CARTESIAN_POINT('',(31.625,-42.8201004838368,-229.35005));
#222430=CARTESIAN_POINT('',(31.625,-42.8201004838368,-229.35005));
#222431=CARTESIAN_POINT('',(30.875,-42.0701004838368,-229.35005));
#222432=CARTESIAN_POINT('',(30.875,-42.0701004838368,-235.35005));
#222433=CARTESIAN_POINT('Origin',(31.625,-42.0701004838368,-229.35005));
#222434=CARTESIAN_POINT('Origin',(36.0311576807678,-42.0701004838368,-229.35005));
#222435=CARTESIAN_POINT('',(36.6030808185578,-42.5552849069797,-229.35005));
#222436=CARTESIAN_POINT('',(36.6030808185578,-42.5552849069797,-229.35005));
#222437=CARTESIAN_POINT('',(36.0311576807678,-42.8201004838368,-229.35005));
#222438=CARTESIAN_POINT('',(36.0311576807678,-42.8201004838368,-229.35005));
#222439=CARTESIAN_POINT('Origin',(36.0311576807678,-42.0701004838368,-229.35005));
#222440=CARTESIAN_POINT('Origin',(39.3771239584772,-33.96456093117,-229.35005));
#222441=CARTESIAN_POINT('',(39.3771239584772,-33.21456093117,-229.35005));
#222442=CARTESIAN_POINT('',(39.3771239584772,-33.21456093117,-229.35005));
#222443=CARTESIAN_POINT('',(40.1267106833091,-33.9894555481763,-229.35005));
#222444=CARTESIAN_POINT('',(40.1267106833092,-33.9894555481763,-229.35005));
#222445=CARTESIAN_POINT('Origin',(39.3771239584772,-33.96456093117,-229.35005));
#222446=CARTESIAN_POINT('Origin',(31.625,-33.96456093117,-229.35005));
#222447=CARTESIAN_POINT('',(30.875,-33.96456093117,-229.35005));
#222448=CARTESIAN_POINT('',(30.875,-33.96456093117,-235.35005));
#222449=CARTESIAN_POINT('',(31.625,-33.21456093117,-229.35005));
#222450=CARTESIAN_POINT('',(31.625,-33.21456093117,-229.35005));
#222451=CARTESIAN_POINT('Origin',(31.625,-33.96456093117,-229.35005));
#222452=CARTESIAN_POINT('Origin',(29.125,-2.14794227316952,-229.35005));
#222453=CARTESIAN_POINT('',(29.125,-1.39794227316951,-229.35005));
#222454=CARTESIAN_POINT('',(29.125,-1.39794227316951,-229.35005));
#222455=CARTESIAN_POINT('',(29.875,-2.14794227316951,-229.35005));
#222456=CARTESIAN_POINT('',(29.875,-2.14794227316951,-235.35005));
#222457=CARTESIAN_POINT('Origin',(29.125,-2.14794227316952,-229.35005));
#222458=CARTESIAN_POINT('Origin',(21.5,-2.14794227316951,-229.35005));
#222459=CARTESIAN_POINT('',(20.75,-2.14794227316951,-229.35005));
#222460=CARTESIAN_POINT('',(20.75,-2.14794227316951,-235.35005));
#222461=CARTESIAN_POINT('',(21.5,-1.39794227316951,-229.35005));
#222462=CARTESIAN_POINT('',(21.5,-1.39794227316951,-229.35005));
#222463=CARTESIAN_POINT('Origin',(21.5,-2.14794227316951,-229.35005));
#222464=CARTESIAN_POINT('Origin',(21.5,-10.2534818258363,-229.35005));
#222465=CARTESIAN_POINT('',(21.5,-11.0034818258363,-229.35005));
#222466=CARTESIAN_POINT('',(21.5,-11.0034818258363,-229.35005));
#222467=CARTESIAN_POINT('',(20.75,-10.2534818258363,-229.35005));
#222468=CARTESIAN_POINT('',(20.75,-10.2534818258363,-235.35005));
#222469=CARTESIAN_POINT('Origin',(21.5,-10.2534818258363,-229.35005));
#222470=CARTESIAN_POINT('Origin',(29.125,-10.2534818258363,-229.35005));
#222471=CARTESIAN_POINT('',(29.875,-10.2534818258363,-229.35005));
#222472=CARTESIAN_POINT('',(29.875,-10.2534818258363,-235.35005));
#222473=CARTESIAN_POINT('',(29.125,-11.0034818258363,-229.35005));
#222474=CARTESIAN_POINT('',(29.125,-11.0034818258363,-229.35005));
#222475=CARTESIAN_POINT('Origin',(29.125,-10.2534818258363,-229.35005));
#222476=CARTESIAN_POINT('Origin',(29.125,-12.7534818258363,-229.35005));
#222477=CARTESIAN_POINT('',(29.125,-12.0034818258363,-229.35005));
#222478=CARTESIAN_POINT('',(29.125,-12.0034818258363,-229.35005));
#222479=CARTESIAN_POINT('',(29.875,-12.7534818258363,-229.35005));
#222480=CARTESIAN_POINT('',(29.875,-12.7534818258363,-235.35005));
#222481=CARTESIAN_POINT('Origin',(29.125,-12.7534818258363,-229.35005));
#222482=CARTESIAN_POINT('Origin',(21.5,-12.7534818258363,-229.35005));
#222483=CARTESIAN_POINT('',(20.75,-12.7534818258363,-229.35005));
#222484=CARTESIAN_POINT('',(20.75,-12.7534818258363,-235.35005));
#222485=CARTESIAN_POINT('',(21.5,-12.0034818258363,-229.35005));
#222486=CARTESIAN_POINT('',(21.5,-12.0034818258363,-229.35005));
#222487=CARTESIAN_POINT('Origin',(21.5,-12.7534818258363,-229.35005));
#222488=CARTESIAN_POINT('Origin',(21.5,-20.8590213785032,-229.35005));
#222489=CARTESIAN_POINT('',(21.5,-21.6090213785031,-229.35005));
#222490=CARTESIAN_POINT('',(21.5,-21.6090213785031,-229.35005));
#222491=CARTESIAN_POINT('',(20.75,-20.8590213785032,-229.35005));
#222492=CARTESIAN_POINT('',(20.75,-20.8590213785032,-235.35005));
#222493=CARTESIAN_POINT('Origin',(21.5,-20.8590213785032,-229.35005));
#222494=CARTESIAN_POINT('Origin',(29.125,-20.8590213785032,-229.35005));
#222495=CARTESIAN_POINT('',(29.875,-20.8590213785032,-229.35005));
#222496=CARTESIAN_POINT('',(29.875,-20.8590213785032,-235.35005));
#222497=CARTESIAN_POINT('',(29.125,-21.6090213785031,-229.35005));
#222498=CARTESIAN_POINT('',(29.125,-21.6090213785031,-229.35005));
#222499=CARTESIAN_POINT('Origin',(29.125,-20.8590213785032,-229.35005));
#222500=CARTESIAN_POINT('Origin',(29.125,-23.3590213785032,-229.35005));
#222501=CARTESIAN_POINT('',(29.125,-22.6090213785032,-229.35005));
#222502=CARTESIAN_POINT('',(29.125,-22.6090213785032,-229.35005));
#222503=CARTESIAN_POINT('',(29.875,-23.3590213785032,-229.35005));
#222504=CARTESIAN_POINT('',(29.875,-23.3590213785032,-235.35005));
#222505=CARTESIAN_POINT('Origin',(29.125,-23.3590213785032,-229.35005));
#222506=CARTESIAN_POINT('Origin',(21.5,-23.3590213785032,-229.35005));
#222507=CARTESIAN_POINT('',(20.75,-23.3590213785032,-229.35005));
#222508=CARTESIAN_POINT('',(20.75,-23.3590213785032,-235.35005));
#222509=CARTESIAN_POINT('',(21.5,-22.6090213785032,-229.35005));
#222510=CARTESIAN_POINT('',(21.5,-22.6090213785032,-229.35005));
#222511=CARTESIAN_POINT('Origin',(21.5,-23.3590213785032,-229.35005));
#222512=CARTESIAN_POINT('Origin',(21.5,-31.46456093117,-229.35005));
#222513=CARTESIAN_POINT('',(21.5,-32.21456093117,-229.35005));
#222514=CARTESIAN_POINT('',(21.5,-32.21456093117,-229.35005));
#222515=CARTESIAN_POINT('',(20.75,-31.46456093117,-229.35005));
#222516=CARTESIAN_POINT('',(20.75,-31.46456093117,-235.35005));
#222517=CARTESIAN_POINT('Origin',(21.5,-31.46456093117,-229.35005));
#222518=CARTESIAN_POINT('Origin',(29.125,-31.46456093117,-229.35005));
#222519=CARTESIAN_POINT('',(29.875,-31.46456093117,-229.35005));
#222520=CARTESIAN_POINT('',(29.875,-31.46456093117,-235.35005));
#222521=CARTESIAN_POINT('',(29.125,-32.21456093117,-229.35005));
#222522=CARTESIAN_POINT('',(29.125,-32.21456093117,-229.35005));
#222523=CARTESIAN_POINT('Origin',(29.125,-31.46456093117,-229.35005));
#222524=CARTESIAN_POINT('Origin',(31.625,-44.5701004838368,-229.35005));
#222525=CARTESIAN_POINT('',(30.875,-44.5701004838368,-229.35005));
#222526=CARTESIAN_POINT('',(30.875,-44.5701004838368,-235.35005));
#222527=CARTESIAN_POINT('',(31.625,-43.8201004838368,-229.35005));
#222528=CARTESIAN_POINT('',(31.625,-43.8201004838368,-229.35005));
#222529=CARTESIAN_POINT('Origin',(31.625,-44.5701004838368,-229.35005));
#222530=CARTESIAN_POINT('Origin',(31.625,-46.609348500795,-229.35005));
#222531=CARTESIAN_POINT('',(32.1269841269841,-47.1665844797626,-229.35005));
#222532=CARTESIAN_POINT('',(32.1269841269841,-47.1665844797626,-229.35005));
#222533=CARTESIAN_POINT('',(30.875,-46.609348500795,-229.35005));
#222534=CARTESIAN_POINT('',(30.875,-46.609348500795,-235.35005));
#222535=CARTESIAN_POINT('Origin',(31.625,-46.609348500795,-229.35005));
#222536=CARTESIAN_POINT('Origin',(33.7514626427707,-44.5701004838368,-229.35005));
#222537=CARTESIAN_POINT('',(33.7514626427707,-43.8201004838368,-229.35005));
#222538=CARTESIAN_POINT('',(33.7514626427707,-43.8201004838368,-229.35005));
#222539=CARTESIAN_POINT('',(34.2872001450369,-45.0949674466622,-229.35005));
#222540=CARTESIAN_POINT('',(34.2872001450369,-45.0949674466622,-229.35005));
#222541=CARTESIAN_POINT('Origin',(33.7514626427707,-44.5701004838368,-229.35005));
#222542=CARTESIAN_POINT('Origin',(29.125,-42.0701004838368,-229.35005));
#222543=CARTESIAN_POINT('',(29.875,-42.0701004838368,-229.35005));
#222544=CARTESIAN_POINT('',(29.875,-42.0701004838368,-235.35005));
#222545=CARTESIAN_POINT('',(29.125,-42.8201004838368,-229.35005));
#222546=CARTESIAN_POINT('',(29.125,-42.8201004838368,-229.35005));
#222547=CARTESIAN_POINT('Origin',(29.125,-42.0701004838368,-229.35005));
#222548=CARTESIAN_POINT('Origin',(29.125,-33.96456093117,-229.35005));
#222549=CARTESIAN_POINT('',(29.125,-33.21456093117,-229.35005));
#222550=CARTESIAN_POINT('',(29.125,-33.21456093117,-229.35005));
#222551=CARTESIAN_POINT('',(29.875,-33.96456093117,-229.35005));
#222552=CARTESIAN_POINT('',(29.875,-33.96456093117,-235.35005));
#222553=CARTESIAN_POINT('Origin',(29.125,-33.96456093117,-229.35005));
#222554=CARTESIAN_POINT('Origin',(21.5,-33.96456093117,-229.35005));
#222555=CARTESIAN_POINT('',(20.75,-33.96456093117,-229.35005));
#222556=CARTESIAN_POINT('',(20.75,-33.96456093117,-235.35005));
#222557=CARTESIAN_POINT('',(21.5,-33.21456093117,-229.35005));
#222558=CARTESIAN_POINT('',(21.5,-33.21456093117,-229.35005));
#222559=CARTESIAN_POINT('Origin',(21.5,-33.96456093117,-229.35005));
#222560=CARTESIAN_POINT('Origin',(21.5,-42.0701004838368,-229.35005));
#222561=CARTESIAN_POINT('',(21.5,-42.8201004838368,-229.35005));
#222562=CARTESIAN_POINT('',(21.5,-42.8201004838368,-229.35005));
#222563=CARTESIAN_POINT('',(20.75,-42.0701004838368,-229.35005));
#222564=CARTESIAN_POINT('',(20.75,-42.0701004838368,-235.35005));
#222565=CARTESIAN_POINT('Origin',(21.5,-42.0701004838368,-229.35005));
#222566=CARTESIAN_POINT('Origin',(31.625,-23.3590213785032,-229.35005));
#222567=CARTESIAN_POINT('',(30.875,-23.3590213785032,-229.35005));
#222568=CARTESIAN_POINT('',(30.875,-23.3590213785032,-235.35005));
#222569=CARTESIAN_POINT('',(31.625,-22.6090213785032,-229.35005));
#222570=CARTESIAN_POINT('',(31.625,-22.6090213785032,-229.35005));
#222571=CARTESIAN_POINT('Origin',(31.625,-23.3590213785032,-229.35005));
#222572=CARTESIAN_POINT('Origin',(31.625,-31.46456093117,-229.35005));
#222573=CARTESIAN_POINT('',(31.625,-32.21456093117,-229.35005));
#222574=CARTESIAN_POINT('',(31.625,-32.21456093117,-229.35005));
#222575=CARTESIAN_POINT('',(30.875,-31.46456093117,-229.35005));
#222576=CARTESIAN_POINT('',(30.875,-31.46456093117,-235.35005));
#222577=CARTESIAN_POINT('Origin',(31.625,-31.46456093117,-229.35005));
#222578=CARTESIAN_POINT('Origin',(39.4555265729267,-31.46456093117,-229.35005));
#222579=CARTESIAN_POINT('',(40.2052001948773,-31.486684686535,-229.35005));
#222580=CARTESIAN_POINT('',(40.2052001948774,-31.486684686535,-229.35005));
#222581=CARTESIAN_POINT('',(39.4555265729267,-32.21456093117,-229.35005));
#222582=CARTESIAN_POINT('',(39.4555265729267,-32.21456093117,-229.35005));
#222583=CARTESIAN_POINT('Origin',(39.4555265729267,-31.46456093117,-229.35005));
#222584=CARTESIAN_POINT('Origin',(39.6461373136998,-23.3590213785032,-229.35005));
#222585=CARTESIAN_POINT('',(39.6461373136998,-22.6090213785032,-229.35005));
#222586=CARTESIAN_POINT('',(39.6461373136998,-22.6090213785032,-229.35005));
#222587=CARTESIAN_POINT('',(40.3960221980464,-23.3721614024167,-229.35005));
#222588=CARTESIAN_POINT('',(40.3960221980465,-23.3721614024167,-229.35005));
#222589=CARTESIAN_POINT('Origin',(39.6461373136998,-23.3590213785032,-229.35005));
#222590=CARTESIAN_POINT('Origin',(31.625,-12.7534818258363,-229.35005));
#222591=CARTESIAN_POINT('',(30.875,-12.7534818258363,-229.35005));
#222592=CARTESIAN_POINT('',(30.875,-12.7534818258363,-235.35005));
#222593=CARTESIAN_POINT('',(31.625,-12.0034818258363,-229.35005));
#222594=CARTESIAN_POINT('',(31.625,-12.0034818258363,-229.35005));
#222595=CARTESIAN_POINT('Origin',(31.625,-12.7534818258363,-229.35005));
#222596=CARTESIAN_POINT('Origin',(31.625,-20.8590213785032,-229.35005));
#222597=CARTESIAN_POINT('',(31.625,-21.6090213785031,-229.35005));
#222598=CARTESIAN_POINT('',(31.625,-21.6090213785031,-229.35005));
#222599=CARTESIAN_POINT('',(30.875,-20.8590213785032,-229.35005));
#222600=CARTESIAN_POINT('',(30.875,-20.8590213785032,-235.35005));
#222601=CARTESIAN_POINT('Origin',(31.625,-20.8590213785032,-229.35005));
#222602=CARTESIAN_POINT('Origin',(39.6853241707135,-20.8590213785032,-229.35005));
#222603=CARTESIAN_POINT('',(40.4352524876037,-20.8693905407753,-229.35005));
#222604=CARTESIAN_POINT('',(40.4352524876037,-20.8693905407753,-229.35005));
#222605=CARTESIAN_POINT('',(39.6853241707135,-21.6090213785031,-229.35005));
#222606=CARTESIAN_POINT('',(39.6853241707135,-21.6090213785031,-229.35005));
#222607=CARTESIAN_POINT('Origin',(39.6853241707135,-20.8590213785032,-229.35005));
#222608=CARTESIAN_POINT('Origin',(39.7488454733312,-12.7534818258363,-229.35005));
#222609=CARTESIAN_POINT('',(39.7488454733312,-12.0034818258363,-229.35005));
#222610=CARTESIAN_POINT('',(39.7488454733312,-12.0034818258363,-229.35005));
#222611=CARTESIAN_POINT('',(40.4988441937178,-12.754867256657,-229.35005));
#222612=CARTESIAN_POINT('',(40.4988441937178,-12.754867256657,-229.35005));
#222613=CARTESIAN_POINT('Origin',(39.7488454733312,-12.7534818258363,-229.35005));
#222614=CARTESIAN_POINT('Origin',(31.625,-2.14794227316952,-229.35005));
#222615=CARTESIAN_POINT('',(30.875,-2.14794227316951,-229.35005));
#222616=CARTESIAN_POINT('',(30.875,-2.14794227316951,-235.35005));
#222617=CARTESIAN_POINT('',(31.625,-1.39794227316951,-229.35005));
#222618=CARTESIAN_POINT('',(31.625,-1.39794227316951,-229.35005));
#222619=CARTESIAN_POINT('Origin',(31.625,-2.14794227316952,-229.35005));
#222620=CARTESIAN_POINT('Origin',(31.625,-10.2534818258363,-229.35005));
#222621=CARTESIAN_POINT('',(31.625,-11.0034818258363,-229.35005));
#222622=CARTESIAN_POINT('',(31.625,-11.0034818258363,-229.35005));
#222623=CARTESIAN_POINT('',(30.875,-10.2534818258363,-229.35005));
#222624=CARTESIAN_POINT('',(30.875,-10.2534818258363,-235.35005));
#222625=CARTESIAN_POINT('Origin',(31.625,-10.2534818258363,-229.35005));
#222626=CARTESIAN_POINT('Origin',(39.7488454733312,-10.2534818258363,-229.35005));
#222627=CARTESIAN_POINT('',(40.4988441937178,-10.2520963950157,-229.35005));
#222628=CARTESIAN_POINT('',(40.4988441937178,-10.2520963950157,-229.35005));
#222629=CARTESIAN_POINT('',(39.7488454733312,-11.0034818258363,-229.35005));
#222630=CARTESIAN_POINT('',(39.7488454733312,-11.0034818258363,-229.35005));
#222631=CARTESIAN_POINT('Origin',(39.7488454733312,-10.2534818258363,-229.35005));
#222632=CARTESIAN_POINT('Origin',(39.6853241707135,-2.14794227316952,-229.35005));
#222633=CARTESIAN_POINT('',(39.6853241707135,-1.39794227316952,-229.35005));
#222634=CARTESIAN_POINT('',(39.6853241707135,-1.39794227316952,-229.35005));
#222635=CARTESIAN_POINT('',(40.4352524876037,-2.13757311089736,-229.35005));
#222636=CARTESIAN_POINT('',(40.4352524876037,-2.13757311089736,-229.35005));
#222637=CARTESIAN_POINT('Origin',(39.6853241707135,-2.14794227316952,-229.35005));
#222638=CARTESIAN_POINT('Origin',(31.625,8.45759727949731,-229.35005));
#222639=CARTESIAN_POINT('',(30.875,8.45759727949731,-229.35005));
#222640=CARTESIAN_POINT('',(30.875,8.45759727949731,-235.35005));
#222641=CARTESIAN_POINT('',(31.625,9.20759727949731,-229.35005));
#222642=CARTESIAN_POINT('',(31.625,9.20759727949731,-229.35005));
#222643=CARTESIAN_POINT('Origin',(31.625,8.45759727949731,-229.35005));
#222644=CARTESIAN_POINT('Origin',(31.625,0.352057726830494,-229.35005));
#222645=CARTESIAN_POINT('',(31.625,-0.397942273169506,-229.35005));
#222646=CARTESIAN_POINT('',(31.625,-0.397942273169506,-229.35005));
#222647=CARTESIAN_POINT('',(30.875,0.352057726830494,-229.35005));
#222648=CARTESIAN_POINT('',(30.875,0.352057726830494,-235.35005));
#222649=CARTESIAN_POINT('Origin',(31.625,0.352057726830494,-229.35005));
#222650=CARTESIAN_POINT('Origin',(39.6461373136998,0.352057726830498,-229.35005));
#222651=CARTESIAN_POINT('',(40.3960221980465,0.365197750743975,-229.35005));
#222652=CARTESIAN_POINT('',(40.3960221980464,0.365197750743973,-229.35005));
#222653=CARTESIAN_POINT('',(39.6461373136998,-0.397942273169503,-229.35005));
#222654=CARTESIAN_POINT('',(39.6461373136998,-0.397942273169503,-229.35005));
#222655=CARTESIAN_POINT('Origin',(39.6461373136998,0.352057726830498,-229.35005));
#222656=CARTESIAN_POINT('Origin',(39.4555265729267,8.45759727949731,-229.35005));
#222657=CARTESIAN_POINT('',(39.4555265729267,9.20759727949731,-229.35005));
#222658=CARTESIAN_POINT('',(39.4555265729267,9.20759727949731,-229.35005));
#222659=CARTESIAN_POINT('',(40.2052001948774,8.47972103486228,-229.35005));
#222660=CARTESIAN_POINT('',(40.2052001948774,8.47972103486227,-229.35005));
#222661=CARTESIAN_POINT('Origin',(39.4555265729267,8.45759727949731,-229.35005));
#222662=CARTESIAN_POINT('Origin',(31.625,19.0631368321642,-229.35005));
#222663=CARTESIAN_POINT('',(30.875,19.0631368321642,-229.35005));
#222664=CARTESIAN_POINT('',(30.875,19.0631368321642,-235.35005));
#222665=CARTESIAN_POINT('',(31.625,19.8131368321642,-229.35005));
#222666=CARTESIAN_POINT('',(31.625,19.8131368321642,-229.35005));
#222667=CARTESIAN_POINT('Origin',(31.625,19.0631368321642,-229.35005));
#222668=CARTESIAN_POINT('Origin',(31.625,10.9575972794973,-229.35005));
#222669=CARTESIAN_POINT('',(31.625,10.2075972794973,-229.35005));
#222670=CARTESIAN_POINT('',(31.625,10.2075972794973,-229.35005));
#222671=CARTESIAN_POINT('',(30.875,10.9575972794973,-229.35005));
#222672=CARTESIAN_POINT('',(30.875,10.9575972794973,-235.35005));
#222673=CARTESIAN_POINT('Origin',(31.625,10.9575972794973,-229.35005));
#222674=CARTESIAN_POINT('Origin',(39.3771239584772,10.9575972794973,-229.35005));
#222675=CARTESIAN_POINT('',(40.1267106833092,10.9824918965036,-229.35005));
#222676=CARTESIAN_POINT('',(40.1267106833092,10.9824918965036,-229.35005));
#222677=CARTESIAN_POINT('',(39.3771239584772,10.2075972794973,-229.35005));
#222678=CARTESIAN_POINT('',(39.3771239584772,10.2075972794973,-229.35005));
#222679=CARTESIAN_POINT('Origin',(39.3771239584772,10.9575972794973,-229.35005));
#222680=CARTESIAN_POINT('Origin',(36.0311576807679,19.0631368321642,-229.35005));
#222681=CARTESIAN_POINT('',(36.0311576807679,19.8131368321642,-229.35005));
#222682=CARTESIAN_POINT('',(36.0311576807679,19.8131368321642,-229.35005));
#222683=CARTESIAN_POINT('',(36.6030808185579,19.548321255307,-229.35005));
#222684=CARTESIAN_POINT('',(36.6030808185579,19.548321255307,-229.35005));
#222685=CARTESIAN_POINT('Origin',(36.0311576807679,19.0631368321642,-229.35005));
#222686=CARTESIAN_POINT('Origin',(29.125,21.5631368321642,-229.35005));
#222687=CARTESIAN_POINT('',(29.875,21.5631368321642,-229.35005));
#222688=CARTESIAN_POINT('',(29.875,21.5631368321642,-235.35005));
#222689=CARTESIAN_POINT('',(29.125,20.8131368321642,-229.35005));
#222690=CARTESIAN_POINT('',(29.125,20.8131368321642,-229.35005));
#222691=CARTESIAN_POINT('Origin',(29.125,21.5631368321642,-229.35005));
#222692=CARTESIAN_POINT('Origin',(29.125,25.702658460412,-229.35005));
#222693=CARTESIAN_POINT('',(29.5873015873016,26.2932321157492,-229.35005));
#222694=CARTESIAN_POINT('',(29.5873015873016,26.2932321157492,-229.35005));
#222695=CARTESIAN_POINT('',(29.875,25.702658460412,-229.35005));
#222696=CARTESIAN_POINT('',(29.875,25.702658460412,-235.35005));
#222697=CARTESIAN_POINT('Origin',(29.125,25.702658460412,-229.35005));
#222698=CARTESIAN_POINT('Origin',(21.5,29.0311209585238,-229.35005));
#222699=CARTESIAN_POINT('',(20.75,29.0311209585238,-229.35005));
#222700=CARTESIAN_POINT('',(21.5791427781145,29.776933549375,-229.35005));
#222701=CARTESIAN_POINT('Origin',(21.5,29.0311209585238,-229.35005));
#222702=CARTESIAN_POINT('',(20.75,29.0311209585238,-229.35005));
#222703=CARTESIAN_POINT('',(21.5791427781145,29.7769335493751,-229.35005));
#222704=CARTESIAN_POINT('Origin',(21.5,21.5631368321642,-229.35005));
#222705=CARTESIAN_POINT('',(21.5,20.8131368321642,-229.35005));
#222706=CARTESIAN_POINT('',(21.5,20.8131368321642,-229.35005));
#222707=CARTESIAN_POINT('',(20.75,21.5631368321642,-229.35005));
#222708=CARTESIAN_POINT('',(20.75,21.5631368321642,-235.35005));
#222709=CARTESIAN_POINT('Origin',(21.5,21.5631368321642,-229.35005));
#222710=CARTESIAN_POINT('Origin',(19.,-52.9088458284789,-229.35005));
#222711=CARTESIAN_POINT('',(19.75,-52.9088458284789,-229.35005));
#222712=CARTESIAN_POINT('',(19.75,-52.9088458284789,-229.35005));
#222713=CARTESIAN_POINT('',(19.021058548474,-53.658550128544,-229.35005));
#222714=CARTESIAN_POINT('',(19.021058548474,-53.6585501285442,-229.35005));
#222715=CARTESIAN_POINT('Origin',(19.,-52.9088458284789,-229.35005));
#222716=CARTESIAN_POINT('Origin',(19.,-44.5701004838368,-229.35005));
#222717=CARTESIAN_POINT('',(19.,-43.8201004838368,-229.35005));
#222718=CARTESIAN_POINT('',(19.,-43.8201004838368,-229.35005));
#222719=CARTESIAN_POINT('',(19.75,-44.5701004838368,-229.35005));
#222720=CARTESIAN_POINT('',(19.75,-44.5701004838368,-235.35005));
#222721=CARTESIAN_POINT('Origin',(19.,-44.5701004838368,-229.35005));
#222722=CARTESIAN_POINT('Origin',(11.3749999999999,-44.5701004838369,-229.35005));
#222723=CARTESIAN_POINT('',(10.6249999999999,-44.5701004838369,-229.35005));
#222724=CARTESIAN_POINT('',(10.6249999999999,-44.5701004838369,-235.35005));
#222725=CARTESIAN_POINT('',(11.3749999999999,-43.8201004838368,-229.35005));
#222726=CARTESIAN_POINT('',(11.3749999999999,-43.8201004838368,-229.35005));
#222727=CARTESIAN_POINT('Origin',(11.3749999999999,-44.5701004838369,-229.35005));
#222728=CARTESIAN_POINT('Origin',(11.3749999999999,-53.08002700974,-229.35005));
#222729=CARTESIAN_POINT('',(11.3876074204679,-53.8299210375528,-229.35005));
#222730=CARTESIAN_POINT('',(11.3876074204679,-53.8299210375529,-229.35005));
#222731=CARTESIAN_POINT('',(10.6249999999999,-53.08002700974,-229.35005));
#222732=CARTESIAN_POINT('',(10.6249999999999,-53.08002700974,-235.35005));
#222733=CARTESIAN_POINT('Origin',(11.3749999999999,-53.08002700974,-229.35005));
#222734=CARTESIAN_POINT('Origin',(19.,19.0631368321642,-229.35005));
#222735=CARTESIAN_POINT('',(19.,19.8131368321642,-229.35005));
#222736=CARTESIAN_POINT('',(19.,19.8131368321642,-229.35005));
#222737=CARTESIAN_POINT('',(19.75,19.0631368321642,-229.35005));
#222738=CARTESIAN_POINT('',(19.75,19.0631368321642,-235.35005));
#222739=CARTESIAN_POINT('Origin',(19.,19.0631368321642,-229.35005));
#222740=CARTESIAN_POINT('Origin',(11.3749999999999,19.0631368321642,-229.35005));
#222741=CARTESIAN_POINT('',(10.6249999999999,19.0631368321642,-229.35005));
#222742=CARTESIAN_POINT('',(10.6249999999999,19.0631368321642,-235.35005));
#222743=CARTESIAN_POINT('',(11.3749999999999,19.8131368321642,-229.35005));
#222744=CARTESIAN_POINT('',(11.3749999999999,19.8131368321642,-229.35005));
#222745=CARTESIAN_POINT('Origin',(11.3749999999999,19.0631368321642,-229.35005));
#222746=CARTESIAN_POINT('Origin',(11.3749999999999,10.9575972794973,-229.35005));
#222747=CARTESIAN_POINT('',(11.3749999999999,10.2075972794973,-229.35005));
#222748=CARTESIAN_POINT('',(11.3749999999999,10.2075972794973,-229.35005));
#222749=CARTESIAN_POINT('',(10.6249999999999,10.9575972794973,-229.35005));
#222750=CARTESIAN_POINT('',(10.6249999999999,10.9575972794973,-235.35005));
#222751=CARTESIAN_POINT('Origin',(11.3749999999999,10.9575972794973,-229.35005));
#222752=CARTESIAN_POINT('Origin',(19.,10.9575972794973,-229.35005));
#222753=CARTESIAN_POINT('',(19.75,10.9575972794973,-229.35005));
#222754=CARTESIAN_POINT('',(19.75,10.9575972794973,-235.35005));
#222755=CARTESIAN_POINT('',(19.,10.2075972794973,-229.35005));
#222756=CARTESIAN_POINT('',(19.,10.2075972794973,-229.35005));
#222757=CARTESIAN_POINT('Origin',(19.,10.9575972794973,-229.35005));
#222758=CARTESIAN_POINT('Origin',(19.,8.45759727949731,-229.35005));
#222759=CARTESIAN_POINT('',(19.,9.20759727949731,-229.35005));
#222760=CARTESIAN_POINT('',(19.,9.20759727949731,-229.35005));
#222761=CARTESIAN_POINT('',(19.75,8.45759727949731,-229.35005));
#222762=CARTESIAN_POINT('',(19.75,8.45759727949731,-235.35005));
#222763=CARTESIAN_POINT('Origin',(19.,8.45759727949731,-229.35005));
#222764=CARTESIAN_POINT('Origin',(11.3749999999999,8.45759727949731,-229.35005));
#222765=CARTESIAN_POINT('',(10.6249999999999,8.45759727949731,-229.35005));
#222766=CARTESIAN_POINT('',(10.6249999999999,8.45759727949731,-235.35005));
#222767=CARTESIAN_POINT('',(11.3749999999999,9.20759727949731,-229.35005));
#222768=CARTESIAN_POINT('',(11.3749999999999,9.20759727949731,-229.35005));
#222769=CARTESIAN_POINT('Origin',(11.3749999999999,8.45759727949731,-229.35005));
#222770=CARTESIAN_POINT('Origin',(11.3749999999999,0.352057726830486,-229.35005));
#222771=CARTESIAN_POINT('',(11.3749999999999,-0.397942273169514,-229.35005));
#222772=CARTESIAN_POINT('',(11.3749999999999,-0.397942273169514,-229.35005));
#222773=CARTESIAN_POINT('',(10.6249999999999,0.352057726830487,-229.35005));
#222774=CARTESIAN_POINT('',(10.6249999999999,0.352057726830487,-235.35005));
#222775=CARTESIAN_POINT('Origin',(11.3749999999999,0.352057726830486,-229.35005));
#222776=CARTESIAN_POINT('Origin',(19.,0.352057726830489,-229.35005));
#222777=CARTESIAN_POINT('',(19.75,0.352057726830487,-229.35005));
#222778=CARTESIAN_POINT('',(19.75,0.352057726830487,-235.35005));
#222779=CARTESIAN_POINT('',(19.,-0.397942273169511,-229.35005));
#222780=CARTESIAN_POINT('',(19.,-0.397942273169511,-229.35005));
#222781=CARTESIAN_POINT('Origin',(19.,0.352057726830489,-229.35005));
#222782=CARTESIAN_POINT('Origin',(19.,-23.3590213785032,-229.35005));
#222783=CARTESIAN_POINT('',(19.,-22.6090213785032,-229.35005));
#222784=CARTESIAN_POINT('',(19.,-22.6090213785032,-229.35005));
#222785=CARTESIAN_POINT('',(19.75,-23.3590213785032,-229.35005));
#222786=CARTESIAN_POINT('',(19.75,-23.3590213785032,-235.35005));
#222787=CARTESIAN_POINT('Origin',(19.,-23.3590213785032,-229.35005));
#222788=CARTESIAN_POINT('Origin',(11.3749999999999,-23.3590213785032,-229.35005));
#222789=CARTESIAN_POINT('',(10.6249999999999,-23.3590213785032,-229.35005));
#222790=CARTESIAN_POINT('',(10.6249999999999,-23.3590213785032,-235.35005));
#222791=CARTESIAN_POINT('',(11.3749999999999,-22.6090213785032,-229.35005));
#222792=CARTESIAN_POINT('',(11.3749999999999,-22.6090213785032,-229.35005));
#222793=CARTESIAN_POINT('Origin',(11.3749999999999,-23.3590213785032,-229.35005));
#222794=CARTESIAN_POINT('Origin',(11.3749999999999,-31.46456093117,-229.35005));
#222795=CARTESIAN_POINT('',(11.3749999999999,-32.21456093117,-229.35005));
#222796=CARTESIAN_POINT('',(11.3749999999999,-32.21456093117,-229.35005));
#222797=CARTESIAN_POINT('',(10.6249999999999,-31.46456093117,-229.35005));
#222798=CARTESIAN_POINT('',(10.6249999999999,-31.46456093117,-235.35005));
#222799=CARTESIAN_POINT('Origin',(11.3749999999999,-31.46456093117,-229.35005));
#222800=CARTESIAN_POINT('Origin',(19.,-31.46456093117,-229.35005));
#222801=CARTESIAN_POINT('',(19.75,-31.46456093117,-229.35005));
#222802=CARTESIAN_POINT('',(19.75,-31.46456093117,-235.35005));
#222803=CARTESIAN_POINT('',(19.,-32.21456093117,-229.35005));
#222804=CARTESIAN_POINT('',(19.,-32.21456093117,-229.35005));
#222805=CARTESIAN_POINT('Origin',(19.,-31.46456093117,-229.35005));
#222806=CARTESIAN_POINT('Origin',(19.,-42.0701004838368,-229.35005));
#222807=CARTESIAN_POINT('',(19.75,-42.0701004838368,-229.35005));
#222808=CARTESIAN_POINT('',(19.75,-42.0701004838368,-235.35005));
#222809=CARTESIAN_POINT('',(19.,-42.8201004838368,-229.35005));
#222810=CARTESIAN_POINT('',(19.,-42.8201004838368,-229.35005));
#222811=CARTESIAN_POINT('Origin',(19.,-42.0701004838368,-229.35005));
#222812=CARTESIAN_POINT('Origin',(19.,-33.96456093117,-229.35005));
#222813=CARTESIAN_POINT('',(19.,-33.21456093117,-229.35005));
#222814=CARTESIAN_POINT('',(19.,-33.21456093117,-229.35005));
#222815=CARTESIAN_POINT('',(19.75,-33.96456093117,-229.35005));
#222816=CARTESIAN_POINT('',(19.75,-33.96456093117,-235.35005));
#222817=CARTESIAN_POINT('Origin',(19.,-33.96456093117,-229.35005));
#222818=CARTESIAN_POINT('Origin',(11.3749999999999,-33.96456093117,-229.35005));
#222819=CARTESIAN_POINT('',(10.6249999999999,-33.96456093117,-229.35005));
#222820=CARTESIAN_POINT('',(10.6249999999999,-33.96456093117,-235.35005));
#222821=CARTESIAN_POINT('',(11.3749999999999,-33.21456093117,-229.35005));
#222822=CARTESIAN_POINT('',(11.3749999999999,-33.21456093117,-229.35005));
#222823=CARTESIAN_POINT('Origin',(11.3749999999999,-33.96456093117,-229.35005));
#222824=CARTESIAN_POINT('Origin',(11.3749999999999,-42.0701004838369,-229.35005));
#222825=CARTESIAN_POINT('',(11.3749999999999,-42.8201004838369,-229.35005));
#222826=CARTESIAN_POINT('',(11.3749999999999,-42.8201004838369,-229.35005));
#222827=CARTESIAN_POINT('',(10.6249999999999,-42.0701004838368,-229.35005));
#222828=CARTESIAN_POINT('',(10.6249999999999,-42.0701004838368,-235.35005));
#222829=CARTESIAN_POINT('Origin',(11.3749999999999,-42.0701004838369,-229.35005));
#222830=CARTESIAN_POINT('Origin',(19.,21.5631368321642,-229.35005));
#222831=CARTESIAN_POINT('',(19.75,21.5631368321642,-229.35005));
#222832=CARTESIAN_POINT('',(19.75,21.5631368321642,-235.35005));
#222833=CARTESIAN_POINT('',(19.,20.8131368321642,-229.35005));
#222834=CARTESIAN_POINT('',(19.,20.8131368321642,-229.35005));
#222835=CARTESIAN_POINT('Origin',(19.,21.5631368321642,-229.35005));
#222836=CARTESIAN_POINT('Origin',(19.,29.2808336449858,-229.35005));
#222837=CARTESIAN_POINT('',(19.0699401294965,30.0275654430807,-229.35005));
#222838=CARTESIAN_POINT('',(19.0699401294965,30.0275654430807,-229.35005));
#222839=CARTESIAN_POINT('',(19.75,29.2808336449858,-229.35005));
#222840=CARTESIAN_POINT('',(19.75,29.2808336449858,-235.35005));
#222841=CARTESIAN_POINT('Origin',(19.,29.2808336449858,-229.35005));
#222842=CARTESIAN_POINT('Origin',(11.3749999999999,29.8508988479304,-229.35005));
#222843=CARTESIAN_POINT('',(10.6249999999999,29.8508988479304,-229.35005));
#222844=CARTESIAN_POINT('',(11.4168720512116,30.5997290899261,-229.35005));
#222845=CARTESIAN_POINT('Origin',(11.3749999999999,29.8508988479304,-229.35005));
#222846=CARTESIAN_POINT('',(10.6249999999999,29.8508988479304,-229.35005));
#222847=CARTESIAN_POINT('',(11.4168720512116,30.5997290899261,-229.35005));
#222848=CARTESIAN_POINT('Origin',(11.3749999999999,21.5631368321642,-229.35005));
#222849=CARTESIAN_POINT('',(11.3749999999999,20.8131368321642,-229.35005));
#222850=CARTESIAN_POINT('',(11.3749999999999,20.8131368321642,-229.35005));
#222851=CARTESIAN_POINT('',(10.6249999999999,21.5631368321642,-229.35005));
#222852=CARTESIAN_POINT('',(10.6249999999999,21.5631368321642,-235.35005));
#222853=CARTESIAN_POINT('Origin',(11.3749999999999,21.5631368321642,-229.35005));
#222854=CARTESIAN_POINT('Origin',(8.87499999999984,-53.1174378937751,-229.35005));
#222855=CARTESIAN_POINT('',(9.62499999999984,-53.1174378937751,-229.35005));
#222856=CARTESIAN_POINT('',(9.62499999999984,-53.1174378937751,-229.35005));
#222857=CARTESIAN_POINT('',(8.88483655882654,-53.8673733857413,-229.35005));
#222858=CARTESIAN_POINT('',(8.88483655882654,-53.8673733857413,-229.35005));
#222859=CARTESIAN_POINT('Origin',(8.87499999999984,-53.1174378937751,-229.35005));
#222860=CARTESIAN_POINT('Origin',(8.87499999999984,-44.5701004838369,-229.35005));
#222861=CARTESIAN_POINT('',(8.87499999999984,-43.8201004838368,-229.35005));
#222862=CARTESIAN_POINT('',(8.87499999999984,-43.8201004838368,-229.35005));
#222863=CARTESIAN_POINT('',(9.62499999999984,-44.5701004838369,-229.35005));
#222864=CARTESIAN_POINT('',(9.62499999999984,-44.5701004838369,-235.35005));
#222865=CARTESIAN_POINT('Origin',(8.87499999999984,-44.5701004838369,-229.35005));
#222866=CARTESIAN_POINT('Origin',(1.25,-44.5701004838369,-229.35005));
#222867=CARTESIAN_POINT('',(0.5,-44.5701004838369,-229.35005));
#222868=CARTESIAN_POINT('',(0.5,-44.5701004838369,-235.35005));
#222869=CARTESIAN_POINT('',(1.25,-43.8201004838368,-229.35005));
#222870=CARTESIAN_POINT('',(1.25,-43.8201004838368,-229.35005));
#222871=CARTESIAN_POINT('Origin',(1.25,-44.5701004838369,-229.35005));
#222872=CARTESIAN_POINT('Origin',(1.25,-53.1744855098348,-229.35005));
#222873=CARTESIAN_POINT('',(1.25138543082066,-53.9244842302215,-229.35005));
#222874=CARTESIAN_POINT('',(1.25138543082066,-53.9244842302215,-229.35005));
#222875=CARTESIAN_POINT('',(0.5,-53.1744855098348,-229.35005));
#222876=CARTESIAN_POINT('',(0.5,-53.1744855098348,-235.35005));
#222877=CARTESIAN_POINT('Origin',(1.25,-53.1744855098348,-229.35005));
#222878=CARTESIAN_POINT('Origin',(8.87499999999986,19.0631368321642,-229.35005));
#222879=CARTESIAN_POINT('',(8.87499999999986,19.8131368321642,-229.35005));
#222880=CARTESIAN_POINT('',(8.87499999999986,19.8131368321642,-229.35005));
#222881=CARTESIAN_POINT('',(9.62499999999986,19.0631368321642,-229.35005));
#222882=CARTESIAN_POINT('',(9.62499999999986,19.0631368321642,-235.35005));
#222883=CARTESIAN_POINT('Origin',(8.87499999999986,19.0631368321642,-229.35005));
#222884=CARTESIAN_POINT('Origin',(1.25,19.0631368321642,-229.35005));
#222885=CARTESIAN_POINT('',(0.5,19.0631368321642,-229.35005));
#222886=CARTESIAN_POINT('',(0.5,19.0631368321642,-235.35005));
#222887=CARTESIAN_POINT('',(1.25,19.8131368321642,-229.35005));
#222888=CARTESIAN_POINT('',(1.25,19.8131368321642,-229.35005));
#222889=CARTESIAN_POINT('Origin',(1.25,19.0631368321642,-229.35005));
#222890=CARTESIAN_POINT('Origin',(1.25,10.9575972794973,-229.35005));
#222891=CARTESIAN_POINT('',(1.25,10.2075972794973,-229.35005));
#222892=CARTESIAN_POINT('',(1.25,10.2075972794973,-229.35005));
#222893=CARTESIAN_POINT('',(0.5,10.9575972794973,-229.35005));
#222894=CARTESIAN_POINT('',(0.5,10.9575972794973,-235.35005));
#222895=CARTESIAN_POINT('Origin',(1.25,10.9575972794973,-229.35005));
#222896=CARTESIAN_POINT('Origin',(8.87499999999986,10.9575972794973,-229.35005));
#222897=CARTESIAN_POINT('',(9.62499999999986,10.9575972794973,-229.35005));
#222898=CARTESIAN_POINT('',(9.62499999999986,10.9575972794973,-235.35005));
#222899=CARTESIAN_POINT('',(8.87499999999986,10.2075972794973,-229.35005));
#222900=CARTESIAN_POINT('',(8.87499999999986,10.2075972794973,-229.35005));
#222901=CARTESIAN_POINT('Origin',(8.87499999999986,10.9575972794973,-229.35005));
#222902=CARTESIAN_POINT('Origin',(8.87499999999984,-42.0701004838369,-229.35005));
#222903=CARTESIAN_POINT('',(9.62499999999984,-42.0701004838368,-229.35005));
#222904=CARTESIAN_POINT('',(9.62499999999984,-42.0701004838368,-235.35005));
#222905=CARTESIAN_POINT('',(8.87499999999984,-42.8201004838369,-229.35005));
#222906=CARTESIAN_POINT('',(8.87499999999984,-42.8201004838369,-229.35005));
#222907=CARTESIAN_POINT('Origin',(8.87499999999984,-42.0701004838369,-229.35005));
#222908=CARTESIAN_POINT('Origin',(8.87499999999984,-33.96456093117,-229.35005));
#222909=CARTESIAN_POINT('',(8.87499999999984,-33.21456093117,-229.35005));
#222910=CARTESIAN_POINT('',(8.87499999999984,-33.21456093117,-229.35005));
#222911=CARTESIAN_POINT('',(9.62499999999984,-33.96456093117,-229.35005));
#222912=CARTESIAN_POINT('',(9.62499999999984,-33.96456093117,-235.35005));
#222913=CARTESIAN_POINT('Origin',(8.87499999999984,-33.96456093117,-229.35005));
#222914=CARTESIAN_POINT('Origin',(1.25,-33.96456093117,-229.35005));
#222915=CARTESIAN_POINT('',(0.5,-33.96456093117,-229.35005));
#222916=CARTESIAN_POINT('',(0.5,-33.96456093117,-235.35005));
#222917=CARTESIAN_POINT('',(1.25,-33.21456093117,-229.35005));
#222918=CARTESIAN_POINT('',(1.25,-33.21456093117,-229.35005));
#222919=CARTESIAN_POINT('Origin',(1.25,-33.96456093117,-229.35005));
#222920=CARTESIAN_POINT('Origin',(1.25,-42.0701004838369,-229.35005));
#222921=CARTESIAN_POINT('',(1.25,-42.8201004838369,-229.35005));
#222922=CARTESIAN_POINT('',(1.25,-42.8201004838369,-229.35005));
#222923=CARTESIAN_POINT('',(0.5,-42.0701004838369,-229.35005));
#222924=CARTESIAN_POINT('',(0.5,-42.0701004838369,-235.35005));
#222925=CARTESIAN_POINT('Origin',(1.25,-42.0701004838369,-229.35005));
#222926=CARTESIAN_POINT('Origin',(8.87499999999986,21.5631368321642,-229.35005));
#222927=CARTESIAN_POINT('',(9.62499999999986,21.5631368321642,-229.35005));
#222928=CARTESIAN_POINT('',(9.62499999999986,21.5631368321642,-235.35005));
#222929=CARTESIAN_POINT('',(8.87499999999986,20.8131368321642,-229.35005));
#222930=CARTESIAN_POINT('',(8.87499999999986,20.8131368321642,-229.35005));
#222931=CARTESIAN_POINT('Origin',(8.87499999999986,21.5631368321642,-229.35005));
#222932=CARTESIAN_POINT('Origin',(8.87499999999986,29.9752906431998,-229.35005));
#222933=CARTESIAN_POINT('',(8.90766940259363,30.7245787787886,-229.35005));
#222934=CARTESIAN_POINT('',(8.90766940259363,30.7245787787886,-229.35005));
#222935=CARTESIAN_POINT('',(9.62499999999986,29.9752906431998,-229.35005));
#222936=CARTESIAN_POINT('',(9.62499999999986,29.9752906431998,-235.35005));
#222937=CARTESIAN_POINT('Origin',(8.87499999999986,29.9752906431998,-229.35005));
#222938=CARTESIAN_POINT('Origin',(1.25,30.1648419118246,-229.35005));
#222939=CARTESIAN_POINT('',(0.5,30.1648419118246,-229.35005));
#222940=CARTESIAN_POINT('',(1.25460132430898,30.9148277969016,-229.35005));
#222941=CARTESIAN_POINT('Origin',(1.25,30.1648419118246,-229.35005));
#222942=CARTESIAN_POINT('',(0.5,30.1648419118246,-229.35005));
#222943=CARTESIAN_POINT('',(1.25460132430898,30.9148277969016,-229.35005));
#222944=CARTESIAN_POINT('Origin',(1.25,21.5631368321642,-229.35005));
#222945=CARTESIAN_POINT('',(1.25,20.8131368321642,-229.35005));
#222946=CARTESIAN_POINT('',(1.25,20.8131368321642,-229.35005));
#222947=CARTESIAN_POINT('',(0.5,21.5631368321642,-229.35005));
#222948=CARTESIAN_POINT('',(0.5,21.5631368321642,-235.35005));
#222949=CARTESIAN_POINT('Origin',(1.25,21.5631368321642,-229.35005));
#222950=CARTESIAN_POINT('Origin',(7.99493453126771,-18.0851397679958,-192.281986444803));
#222951=CARTESIAN_POINT('',(8.57396770167423,-18.5618163748993,-229.35005));
#222952=CARTESIAN_POINT('',(8.57396770167423,-18.5618163748993,-192.281986444803));
#222953=CARTESIAN_POINT('',(7.4518492428487,-18.6024002144856,-229.35005));
#222954=CARTESIAN_POINT('',(7.4518492428487,-18.6024002144856,-235.35005));
#222955=CARTESIAN_POINT('Origin',(7.99493453126771,-18.0851397679958,-229.35005));
#222956=CARTESIAN_POINT('Origin',(6.18465023653768,-19.8093412562951,-192.281986444803));
#222957=CARTESIAN_POINT('',(6.72773552495669,-19.2920808098054,-229.35005));
#222958=CARTESIAN_POINT('',(6.72773552495669,-19.2920808098054,-229.35005));
#222959=CARTESIAN_POINT('',(6.63257355852516,-20.4108931639637,-229.35005));
#222960=CARTESIAN_POINT('',(6.63257355852516,-20.4108931639637,-192.281986444803));
#222961=CARTESIAN_POINT('Origin',(6.18465023653768,-19.8093412562951,-229.35005));
#222962=CARTESIAN_POINT('Origin',(6.18465023653769,-3.19762239537749,-192.281986444803));
#222963=CARTESIAN_POINT('',(6.63257355852517,-2.59607048770891,-229.35005));
#222964=CARTESIAN_POINT('',(6.63257355852517,-2.59607048770891,-192.281986444803));
#222965=CARTESIAN_POINT('',(6.7277355249567,-3.7148828418673,-229.35005));
#222966=CARTESIAN_POINT('',(6.7277355249567,-3.7148828418673,-192.281986444803));
#222967=CARTESIAN_POINT('Origin',(6.18465023653769,-3.19762239537748,-229.35005));
#222968=CARTESIAN_POINT('Origin',(1.25,-1.22366181637858,-192.281986444803));
#222969=CARTESIAN_POINT('',(0.5,-1.22366181637858,-229.35005));
#222970=CARTESIAN_POINT('',(1.3405312557817,-0.479145804645729,-229.35005));
#222971=CARTESIAN_POINT('Origin',(1.25,-1.22366181637858,-229.35005));
#222972=CARTESIAN_POINT('',(0.5,-1.22366181637858,-229.35005));
#222973=CARTESIAN_POINT('',(1.3405312557817,-0.479145804645732,-192.281986444803));
#222974=CARTESIAN_POINT('Origin',(1.25,-21.7833018352941,-192.281986444803));
#222975=CARTESIAN_POINT('',(1.3405312557817,-22.5278178470269,-229.35005));
#222976=CARTESIAN_POINT('',(1.3405312557817,-22.5278178470269,-192.281986444803));
#222977=CARTESIAN_POINT('',(0.5,-21.7833018352941,-229.35005));
#222978=CARTESIAN_POINT('',(0.5,-21.7833018352941,-235.35005));
#222979=CARTESIAN_POINT('Origin',(1.25,-21.7833018352941,-229.35005));
#222980=CARTESIAN_POINT('Origin',(5.14120077283693,-18.713796339242,-192.281986444803));
#222981=CARTESIAN_POINT('',(4.7057783396023,-18.1031349726598,-229.35005));
#222982=CARTESIAN_POINT('',(5.68428606125594,-18.1965358927522,-229.35005));
#222983=CARTESIAN_POINT('Origin',(5.14120077283693,-18.713796339242,-229.35005));
#222984=CARTESIAN_POINT('',(4.7057783396023,-18.1031349726598,-192.281986444803));
#222985=CARTESIAN_POINT('',(5.68428606125594,-18.1965358927522,-192.281986444803));
#222986=CARTESIAN_POINT('Origin',(6.95148506756696,-16.9895948509426,-192.281986444803));
#222987=CARTESIAN_POINT('',(6.40839977914796,-17.5068552974324,-229.35005));
#222988=CARTESIAN_POINT('',(6.40839977914795,-17.5068552974324,-192.281986444803));
#222989=CARTESIAN_POINT('',(6.36274467860837,-16.5249608504553,-229.35005));
#222990=CARTESIAN_POINT('',(6.36274467860837,-16.5249608504553,-192.281986444803));
#222991=CARTESIAN_POINT('Origin',(6.95148506756696,-16.9895948509426,-229.35005));
#222992=CARTESIAN_POINT('Origin',(20.625,-3.54959888009691,-192.281986444803));
#222993=CARTESIAN_POINT('',(11.294759518486,-7.14773903260897,-229.35005));
#222994=CARTESIAN_POINT('',(11.294759518486,-7.14773903260897,-192.281986444803));
#222995=CARTESIAN_POINT('',(10.6249999999999,-3.54959888009691,-229.35005));
#222996=CARTESIAN_POINT('',(10.6249999999999,-3.54959888009691,-235.35005));
#222997=CARTESIAN_POINT('Origin',(20.625,-3.54959888009691,-229.35005));
#222998=CARTESIAN_POINT('Origin',(20.625,-19.4573647715757,-192.281986444803));
#222999=CARTESIAN_POINT('',(10.6249999999999,-19.4573647715757,-229.35005));
#223000=CARTESIAN_POINT('',(10.6249999999999,-19.4573647715757,-235.35005));
#223001=CARTESIAN_POINT('',(11.294759518486,-15.8592246190636,-229.35005));
#223002=CARTESIAN_POINT('',(11.294759518486,-15.8592246190636,-192.281986444803));
#223003=CARTESIAN_POINT('Origin',(20.625,-19.4573647715757,-229.35005));
#223004=CARTESIAN_POINT('Origin',(9.40330570654103,-32.6090213785032,-192.281986444803));
#223005=CARTESIAN_POINT('',(5.33358654455951,-23.474614668563,-229.35005));
#223006=CARTESIAN_POINT('',(5.33358654455951,-23.474614668563,-192.281986444803));
#223007=CARTESIAN_POINT('Origin',(9.40330570654103,-32.6090213785032,-229.35005));
#223008=CARTESIAN_POINT('Origin',(9.40330570654115,9.60205772683048,-192.281986444803));
#223009=CARTESIAN_POINT('',(5.33358654455957,0.46765101689032,-229.35005));
#223010=CARTESIAN_POINT('',(5.33358654455957,0.467651016890315,-192.281986444803));
#223011=CARTESIAN_POINT('Origin',(9.40330570654115,9.60205772683049,-229.35005));
#223012=CARTESIAN_POINT('Origin',(0.,-11.5034818258363,-235.35005));
#223013=CARTESIAN_POINT('',(-5.66442007243621E-16,-16.1288318258363,-235.35005));
#223014=CARTESIAN_POINT('Origin',(0.,-11.5034818258363,-235.35005));
#223015=CARTESIAN_POINT('Origin',(0.,-11.5034818258363,-235.35005));
#223016=CARTESIAN_POINT('',(-5.66442007243621E-16,-16.1288318258363,-235.35005));
#223017=CARTESIAN_POINT('Origin',(0.,-11.5034818258363,-236.10005));
#223018=CARTESIAN_POINT('Origin',(0.,-11.5034818258363,-192.281986444803));
#223019=CARTESIAN_POINT('Origin',(0.,-11.5034818258363,-229.35005));
#223020=CARTESIAN_POINT('Origin',(0.,-11.5034818258363,-192.281986444803));
#223021=CARTESIAN_POINT('Origin',(0.,-11.5034818258363,-229.35005));
#223022=CARTESIAN_POINT('Origin',(0.,-11.5034818258363,-192.281986444803));
#223023=CARTESIAN_POINT('',(-9.92642306853573E-16,-19.6090213785032,-235.35005));
#223024=CARTESIAN_POINT('',(-9.92642306853574E-16,-19.6090213785032,-192.281986444803));
#223025=CARTESIAN_POINT('Origin',(0.,-11.5034818258363,-235.35005));
#223026=CARTESIAN_POINT('Origin',(0.,-11.5034818258363,-229.35005));
#223027=CARTESIAN_POINT('Origin',(0.,-11.5034818258363,-235.35005));
#223028=CARTESIAN_POINT('Origin',(0.,-11.5034818258363,-229.35005));
#223029=CARTESIAN_POINT('Origin',(0.,-11.5034818258363,-235.35005));
#223030=CARTESIAN_POINT('Origin',(0.,-11.5034818258363,-229.35005));
#223031=CARTESIAN_POINT('Origin',(0.,-11.5034818258363,-235.35005));
#223032=CARTESIAN_POINT('Origin',(0.,-11.5034818258363,-229.35005));
#223033=CARTESIAN_POINT('Origin',(0.,-11.5034818258363,-235.35005));
#223034=CARTESIAN_POINT('Origin',(0.,-11.5034818258363,-229.35005));
#223035=CARTESIAN_POINT('Origin',(0.,-11.5034818258363,-235.35005));
#223036=CARTESIAN_POINT('Origin',(0.,-11.5034818258363,-229.35005));
#223037=CARTESIAN_POINT('Origin',(0.,-11.5034818258363,-235.35005));
#223038=CARTESIAN_POINT('Origin',(0.,-11.5034818258363,-229.35005));
#223039=CARTESIAN_POINT('Origin',(0.,-11.5034818258363,-235.35005));
#223040=CARTESIAN_POINT('Origin',(0.,-11.5034818258363,-229.35005));
#223041=CARTESIAN_POINT('Origin',(0.,-11.5034818258363,-235.35005));
#223042=CARTESIAN_POINT('Origin',(0.,-11.5034818258363,-192.281986444803));
#223043=CARTESIAN_POINT('Origin',(0.,-11.5034818258363,-229.35005));
#223044=CARTESIAN_POINT('Origin',(-6.10697827817036,-5.81657868152891,-192.281986444803));
#223045=CARTESIAN_POINT('',(-6.10697827817036,-5.81657868152891,-229.35005));
#223046=CARTESIAN_POINT('Origin',(-5.38286456027835,-5.12689808620917,-192.281986444803));
#223047=CARTESIAN_POINT('',(-5.38286456027835,-5.12689808620916,-229.35005));
#223048=CARTESIAN_POINT('Origin',(0.,-11.5034818258363,-192.281986444803));
#223049=CARTESIAN_POINT('Origin',(0.,-11.5034818258363,-229.35005));
#223050=CARTESIAN_POINT('Origin',(0.,-11.5034818258363,-192.281986444803));
#223051=CARTESIAN_POINT('Origin',(0.,-11.5034818258363,-229.35005));
#223052=CARTESIAN_POINT('Origin',(0.,-11.5034818258363,-192.281986444803));
#223053=CARTESIAN_POINT('Origin',(0.,-11.5034818258363,-229.35005));
#223054=CARTESIAN_POINT('Origin',(5.38286456027834,-5.12689808620917,-192.281986444803));
#223055=CARTESIAN_POINT('',(5.38286456027834,-5.12689808620916,-229.35005));
#223056=CARTESIAN_POINT('Origin',(6.10697827817035,-5.81657868152891,-192.281986444803));
#223057=CARTESIAN_POINT('',(6.10697827817035,-5.81657868152891,-229.35005));
#223058=CARTESIAN_POINT('Origin',(0.,-11.5034818258363,-192.281986444803));
#223059=CARTESIAN_POINT('Origin',(0.,-11.5034818258363,-229.35005));
#223060=CARTESIAN_POINT('Origin',(0.,-11.5034818258363,-192.281986444803));
#223061=CARTESIAN_POINT('Origin',(0.,-11.5034818258363,-229.35005));
#223062=CARTESIAN_POINT('Origin',(29.875,26.0662450163965,-235.35005));
#223063=CARTESIAN_POINT('',(29.875,26.0662450163965,-229.35005));
#223064=CARTESIAN_POINT('Origin',(30.875,26.0662450163965,-235.35005));
#223065=CARTESIAN_POINT('',(30.875,26.0662450163965,-229.35005));
#223066=CARTESIAN_POINT('Origin',(30.875,26.0662450163965,-235.35005));
#223067=CARTESIAN_POINT('',(30.875,26.0662450163965,-229.35005));
#223068=CARTESIAN_POINT('Origin',(29.875,26.0662450163965,-235.35005));
#223069=CARTESIAN_POINT('',(29.875,26.0662450163965,-229.35005));
#223070=CARTESIAN_POINT('Origin',(30.875,26.0662450163965,-235.35005));
#223071=CARTESIAN_POINT('',(30.875,26.0662450163965,-229.35005));
#223072=CARTESIAN_POINT('Origin',(29.875,26.0662450163965,-235.35005));
#223073=CARTESIAN_POINT('',(29.875,26.0662450163965,-229.35005));
#223074=CARTESIAN_POINT('Origin',(30.875,26.0662450163965,-235.35005));
#223075=CARTESIAN_POINT('',(30.875,26.0662450163965,-229.35005));
#223076=CARTESIAN_POINT('Origin',(29.875,26.0662450163965,-235.35005));
#223077=CARTESIAN_POINT('',(29.875,26.0662450163965,-229.35005));
#223078=CARTESIAN_POINT('Origin',(30.875,26.0662450163965,-235.35005));
#223079=CARTESIAN_POINT('',(30.875,26.0662450163965,-229.35005));
#223080=CARTESIAN_POINT('Origin',(29.875,26.0662450163965,-235.35005));
#223081=CARTESIAN_POINT('',(29.875,26.0662450163965,-229.35005));
#223082=CARTESIAN_POINT('Origin',(30.875,26.0662450163965,-235.35005));
#223083=CARTESIAN_POINT('',(30.875,26.0662450163965,-229.35005));
#223084=CARTESIAN_POINT('Origin',(29.875,26.0662450163965,-235.35005));
#223085=CARTESIAN_POINT('',(29.875,26.0662450163965,-229.35005));
#223086=CARTESIAN_POINT('Origin',(30.875,26.0662450163965,-235.35005));
#223087=CARTESIAN_POINT('',(30.875,26.0662450163965,-229.35005));
#223088=CARTESIAN_POINT('Origin',(29.875,26.0662450163965,-235.35005));
#223089=CARTESIAN_POINT('',(29.875,26.0662450163965,-229.35005));
#223090=CARTESIAN_POINT('Origin',(30.875,26.0662450163965,-235.35005));
#223091=CARTESIAN_POINT('',(30.875,26.0662450163965,-229.35005));
#223092=CARTESIAN_POINT('Origin',(29.875,26.0662450163965,-235.35005));
#223093=CARTESIAN_POINT('',(29.875,26.0662450163965,-229.35005));
#223094=CARTESIAN_POINT('Origin',(19.75,32.818676384831,-235.35005));
#223095=CARTESIAN_POINT('',(19.75,32.818676384831,-229.35005));
#223096=CARTESIAN_POINT('Origin',(20.75,32.818676384831,-235.35005));
#223097=CARTESIAN_POINT('',(20.75,32.818676384831,-229.35005));
#223098=CARTESIAN_POINT('Origin',(20.75,32.818676384831,-235.35005));
#223099=CARTESIAN_POINT('',(20.75,32.818676384831,-229.35005));
#223100=CARTESIAN_POINT('Origin',(19.75,32.818676384831,-235.35005));
#223101=CARTESIAN_POINT('',(19.75,32.818676384831,-229.35005));
#223102=CARTESIAN_POINT('Origin',(20.75,32.818676384831,-235.35005));
#223103=CARTESIAN_POINT('',(20.75,32.818676384831,-229.35005));
#223104=CARTESIAN_POINT('Origin',(19.75,32.818676384831,-235.35005));
#223105=CARTESIAN_POINT('',(19.75,32.818676384831,-229.35005));
#223106=CARTESIAN_POINT('Origin',(20.75,32.818676384831,-235.35005));
#223107=CARTESIAN_POINT('',(20.75,32.818676384831,-229.35005));
#223108=CARTESIAN_POINT('Origin',(19.75,32.818676384831,-235.35005));
#223109=CARTESIAN_POINT('',(19.75,32.818676384831,-229.35005));
#223110=CARTESIAN_POINT('Origin',(20.75,32.818676384831,-235.35005));
#223111=CARTESIAN_POINT('',(20.75,32.818676384831,-229.35005));
#223112=CARTESIAN_POINT('Origin',(19.75,32.818676384831,-235.35005));
#223113=CARTESIAN_POINT('',(19.75,32.818676384831,-229.35005));
#223114=CARTESIAN_POINT('Origin',(20.75,32.818676384831,-235.35005));
#223115=CARTESIAN_POINT('',(20.75,32.818676384831,-229.35005));
#223116=CARTESIAN_POINT('Origin',(19.75,32.818676384831,-235.35005));
#223117=CARTESIAN_POINT('',(19.75,32.818676384831,-229.35005));
#223118=CARTESIAN_POINT('Origin',(20.75,32.818676384831,-235.35005));
#223119=CARTESIAN_POINT('',(20.75,32.818676384831,-229.35005));
#223120=CARTESIAN_POINT('Origin',(19.75,32.818676384831,-235.35005));
#223121=CARTESIAN_POINT('',(19.75,32.818676384831,-229.35005));
#223122=CARTESIAN_POINT('Origin',(20.75,32.818676384831,-235.35005));
#223123=CARTESIAN_POINT('',(20.75,32.818676384831,-229.35005));
#223124=CARTESIAN_POINT('Origin',(19.75,32.818676384831,-235.35005));
#223125=CARTESIAN_POINT('',(19.75,32.818676384831,-229.35005));
#223126=CARTESIAN_POINT('Origin',(20.75,32.818676384831,-235.35005));
#223127=CARTESIAN_POINT('',(20.75,32.818676384831,-232.25005));
#223128=CARTESIAN_POINT('',(20.75,32.818676384831,-229.35005));
#223129=CARTESIAN_POINT('',(20.75,32.818676384831,-235.35005));
#223130=CARTESIAN_POINT('',(19.75,32.818676384831,-232.25005));
#223131=CARTESIAN_POINT('',(11.4589044897296,32.818676384831,-232.25005));
#223132=CARTESIAN_POINT('',(19.75,32.818676384831,-229.35005));
#223133=CARTESIAN_POINT('',(19.75,32.818676384831,-235.35005));
#223134=CARTESIAN_POINT('',(20.75,32.818676384831,-229.35005));
#223135=CARTESIAN_POINT('Origin',(20.75,32.818676384831,-235.35005));
#223136=CARTESIAN_POINT('',(20.75,32.3760227311709,-232.25005));
#223137=CARTESIAN_POINT('',(20.75,32.3760227311709,-229.35005));
#223138=CARTESIAN_POINT('',(20.75,32.3760227311709,-229.35005));
#223139=CARTESIAN_POINT('',(20.75,-32.0203896799758,-232.25005));
#223140=CARTESIAN_POINT('',(20.75,32.818676384831,-229.35005));
#223141=CARTESIAN_POINT('Origin',(19.75,32.818676384831,-235.35005));
#223142=CARTESIAN_POINT('',(19.75,32.4743226583831,-232.25005));
#223143=CARTESIAN_POINT('',(19.75,-32.0203896799758,-232.25005));
#223144=CARTESIAN_POINT('',(19.75,32.4743226583832,-229.35005));
#223145=CARTESIAN_POINT('',(19.75,32.4743226583832,-229.35005));
#223146=CARTESIAN_POINT('',(19.75,32.818676384831,-229.35005));
#223147=CARTESIAN_POINT('Origin',(9.62499999999986,32.818676384831,-235.35005));
#223148=CARTESIAN_POINT('',(9.62499999999986,32.818676384831,-229.35005));
#223149=CARTESIAN_POINT('Origin',(10.6249999999999,32.818676384831,-235.35005));
#223150=CARTESIAN_POINT('',(10.6249999999999,32.818676384831,-229.35005));
#223151=CARTESIAN_POINT('Origin',(10.6249999999999,32.818676384831,-235.35005));
#223152=CARTESIAN_POINT('',(10.6249999999999,32.818676384831,-229.35005));
#223153=CARTESIAN_POINT('Origin',(9.62499999999986,32.818676384831,-235.35005));
#223154=CARTESIAN_POINT('',(9.62499999999986,32.818676384831,-229.35005));
#223155=CARTESIAN_POINT('Origin',(10.6249999999999,32.818676384831,-235.35005));
#223156=CARTESIAN_POINT('',(10.6249999999999,32.818676384831,-229.35005));
#223157=CARTESIAN_POINT('Origin',(9.62499999999986,32.818676384831,-235.35005));
#223158=CARTESIAN_POINT('',(9.62499999999986,32.818676384831,-229.35005));
#223159=CARTESIAN_POINT('Origin',(10.6249999999999,32.818676384831,-235.35005));
#223160=CARTESIAN_POINT('',(10.6249999999999,32.818676384831,-229.35005));
#223161=CARTESIAN_POINT('Origin',(9.62499999999986,32.818676384831,-235.35005));
#223162=CARTESIAN_POINT('',(9.62499999999986,32.818676384831,-229.35005));
#223163=CARTESIAN_POINT('Origin',(10.6249999999999,32.818676384831,-235.35005));
#223164=CARTESIAN_POINT('',(10.6249999999999,32.818676384831,-229.35005));
#223165=CARTESIAN_POINT('Origin',(10.6249999999999,32.818676384831,-235.35005));
#223166=CARTESIAN_POINT('',(10.6249999999999,32.818676384831,-229.35005));
#223167=CARTESIAN_POINT('Origin',(10.6249999999999,32.818676384831,-235.35005));
#223168=CARTESIAN_POINT('',(10.6249999999999,32.818676384831,-229.35005));
#223169=CARTESIAN_POINT('Origin',(9.62499999999986,32.818676384831,-235.35005));
#223170=CARTESIAN_POINT('',(9.62499999999986,32.818676384831,-229.35005));
#223171=CARTESIAN_POINT('Origin',(10.6249999999999,32.818676384831,-235.35005));
#223172=CARTESIAN_POINT('',(10.6249999999999,32.818676384831,-229.35005));
#223173=CARTESIAN_POINT('Origin',(9.62499999999986,32.818676384831,-235.35005));
#223174=CARTESIAN_POINT('',(9.62499999999986,32.818676384831,-229.35005));
#223175=CARTESIAN_POINT('Origin',(0.5,32.818676384831,-235.35005));
#223176=CARTESIAN_POINT('',(0.5,32.818676384831,-229.35005));
#223177=CARTESIAN_POINT('Origin',(0.5,32.818676384831,-235.35005));
#223178=CARTESIAN_POINT('',(0.5,32.818676384831,-229.35005));
#223179=CARTESIAN_POINT('Origin',(0.5,32.818676384831,-235.35005));
#223180=CARTESIAN_POINT('',(0.5,32.818676384831,-229.35005));
#223181=CARTESIAN_POINT('Origin',(0.5,32.818676384831,-235.35005));
#223182=CARTESIAN_POINT('',(0.5,32.818676384831,-229.35005));
#223183=CARTESIAN_POINT('Origin',(0.5,32.818676384831,-235.35005));
#223184=CARTESIAN_POINT('',(0.5,32.818676384831,-229.35005));
#223185=CARTESIAN_POINT('Origin',(0.5,32.818676384831,-235.35005));
#223186=CARTESIAN_POINT('',(0.5,32.818676384831,-229.35005));
#223187=CARTESIAN_POINT('Origin',(0.5,32.818676384831,-235.35005));
#223188=CARTESIAN_POINT('',(0.5,32.818676384831,-229.35005));
#223189=CARTESIAN_POINT('Origin',(0.5,32.818676384831,-235.35005));
#223190=CARTESIAN_POINT('',(0.5,32.818676384831,-229.35005));
#223191=CARTESIAN_POINT('Origin',(7.14692237356698E-14,623.509175991979,
-229.35005));
#223192=CARTESIAN_POINT('Origin',(-2.61456814389029E-14,-173.57701443073,
-229.35005));
#223193=CARTESIAN_POINT('',(23.0363900009079,-56.0352881775207,-229.35005));
#223194=CARTESIAN_POINT('Origin',(7.14692237356698E-14,623.509175991979,
-229.35005));
#223195=CARTESIAN_POINT('',(24.6244543289934,-55.593007214519,-229.35005));
#223196=CARTESIAN_POINT('Origin',(22.9178089794592,-52.5372975341153,-229.35005));
#223197=CARTESIAN_POINT('',(41.8942895912772,-39.701327481882,-229.35005));
#223198=CARTESIAN_POINT('Origin',(-6.29739814579425E-15,-11.5034818258363,
-229.35005));
#223199=CARTESIAN_POINT('',(42.4880898820538,-37.8828103193512,-229.35005));
#223200=CARTESIAN_POINT('Origin',(38.9907249661392,-37.7470213473046,-229.35005));
#223201=CARTESIAN_POINT('',(42.4880898820539,14.8758466676788,-229.35005));
#223202=CARTESIAN_POINT('Origin',(-636.934816028482,-11.5034818258361,-229.35005));
#223203=CARTESIAN_POINT('',(41.8942895912773,16.6943638302095,-229.35005));
#223204=CARTESIAN_POINT('Origin',(38.9907249661392,14.740057695632,-229.35005));
#223205=CARTESIAN_POINT('',(26.6879613405455,31.3684521110126,-229.35005));
#223206=CARTESIAN_POINT('Origin',(-6.29739814579425E-15,-11.5034818258363,
-229.35005));
#223207=CARTESIAN_POINT('',(25.2655040598954,31.8709602996399,-229.35005));
#223208=CARTESIAN_POINT('Origin',(24.838300653577,28.3971299569735,-229.35005));
#223209=CARTESIAN_POINT('Origin',(-2.61456814389029E-14,-173.57701443073,
-229.35005));
#223210=CARTESIAN_POINT('Origin',(7.14692237356698E-14,623.509175991979,
-229.35005));
#223211=CARTESIAN_POINT('',(-1.23757166668304E-15,-43.8201004838368,-229.35005));
#223212=CARTESIAN_POINT('',(-1.54373336646988E-15,19.8131368321642,-229.35005));
#223213=CARTESIAN_POINT('',(-2.53637567332344E-15,10.2075972794973,-229.35005));
#223214=CARTESIAN_POINT('',(-2.8425373731103E-15,9.20759727949731,-229.35005));
#223215=CARTESIAN_POINT('',(-1.11087130309497E-13,-0.397942273169518,-229.35005));
#223216=CARTESIAN_POINT('',(-3.33261390928491E-13,-22.6090213785032,-229.35005));
#223217=CARTESIAN_POINT('',(0.,-32.21456093117,-229.35005));
#223218=CARTESIAN_POINT('',(-1.54373336646987E-15,-42.8201004838369,-229.35005));
#223219=CARTESIAN_POINT('',(0.,-33.21456093117,-229.35005));
#223220=CARTESIAN_POINT('Origin',(-2.61456814389029E-14,-173.57701443073,
-229.35005));
#223221=CARTESIAN_POINT('',(-1.23757166668304E-15,20.8131368321642,-229.35005));
#223222=CARTESIAN_POINT('Origin',(-2.61456814389029E-14,-173.57701443073,
-229.35005));
#223223=CARTESIAN_POINT('',(-1.23757166668304E-15,20.8131368321642,-229.35005));
#223224=CARTESIAN_POINT('',(-1.54373336646987E-15,-42.8201004838369,-229.35005));
#223225=CARTESIAN_POINT('',(0.,-33.21456093117,-229.35005));
#223226=CARTESIAN_POINT('',(-1.54373336646988E-15,19.8131368321642,-229.35005));
#223227=CARTESIAN_POINT('',(-2.53637567332344E-15,10.2075972794973,-229.35005));
#223228=CARTESIAN_POINT('Origin',(7.14692237356698E-14,623.509175991979,
-229.35005));
#223229=CARTESIAN_POINT('',(-1.23757166668304E-15,-43.8201004838368,-229.35005));
#223230=CARTESIAN_POINT('',(-1.23757166668304E-15,20.8131368321642,-229.35005));
#223231=CARTESIAN_POINT('',(24.960358769668,29.3896529120211,-229.35005));
#223232=CARTESIAN_POINT('Origin',(-2.61456814389029E-14,-173.57701443073,
-229.35005));
#223233=CARTESIAN_POINT('',(25.366775135568,29.2460791438418,-229.35005));
#223234=CARTESIAN_POINT('Origin',(24.838300653577,28.3971299569735,-229.35005));
#223235=CARTESIAN_POINT('Origin',(-6.29739814579425E-15,-11.5034818258363,
-229.35005));
#223236=CARTESIAN_POINT('',(-2.53637567332344E-15,10.2075972794973,-229.35005));
#223237=CARTESIAN_POINT('',(-1.54373336646988E-15,19.8131368321642,-229.35005));
#223238=CARTESIAN_POINT('',(39.8203148590359,15.2984308769399,-229.35005));
#223239=CARTESIAN_POINT('Origin',(-6.29739814579425E-15,-11.5034818258363,
-229.35005));
#223240=CARTESIAN_POINT('',(39.989972084972,14.7788545447883,-229.35005));
#223241=CARTESIAN_POINT('Origin',(38.9907249661392,14.740057695632,-229.35005));
#223242=CARTESIAN_POINT('Origin',(-636.934816028482,-11.5034818258361,-229.35005));
#223243=CARTESIAN_POINT('',(-1.11087130309497E-13,-0.397942273169518,-229.35005));
#223244=CARTESIAN_POINT('',(-2.8425373731103E-15,9.20759727949731,-229.35005));
#223245=CARTESIAN_POINT('Origin',(-636.934816028482,-11.5034818258361,-229.35005));
#223246=CARTESIAN_POINT('',(-2.22174260618994E-13,-11.0034818258363,-229.35005));
#223247=CARTESIAN_POINT('',(-1.11087130309497E-13,-1.3979422731695,-229.35005));
#223248=CARTESIAN_POINT('Origin',(-636.934816028482,-11.5034818258361,-229.35005));
#223249=CARTESIAN_POINT('',(-3.33261390928491E-13,-21.6090213785032,-229.35005));
#223250=CARTESIAN_POINT('',(-2.22174260618994E-13,-12.0034818258363,-229.35005));
#223251=CARTESIAN_POINT('Origin',(-636.934816028482,-11.5034818258361,-229.35005));
#223252=CARTESIAN_POINT('',(0.,-32.21456093117,-229.35005));
#223253=CARTESIAN_POINT('',(-3.33261390928491E-13,-22.6090213785032,-229.35005));
#223254=CARTESIAN_POINT('Origin',(-636.934816028482,-11.5034818258361,-229.35005));
#223255=CARTESIAN_POINT('',(-1.54373336646987E-15,-42.8201004838369,-229.35005));
#223256=CARTESIAN_POINT('',(0.,-33.21456093117,-229.35005));
#223257=CARTESIAN_POINT('',(-1.23757166668304E-15,-43.8201004838368,-229.35005));
#223258=CARTESIAN_POINT('Origin',(-6.29739814579425E-15,-11.5034818258363,
-229.35005));
#223259=CARTESIAN_POINT('',(-3.33261390928491E-13,-22.6090213785032,-229.35005));
#223260=CARTESIAN_POINT('',(0.,-32.21456093117,-229.35005));
#223261=CARTESIAN_POINT('',(-2.22174260618994E-13,-12.0034818258363,-229.35005));
#223262=CARTESIAN_POINT('',(-3.33261390928491E-13,-21.6090213785032,-229.35005));
#223263=CARTESIAN_POINT('',(-1.11087130309497E-13,-1.3979422731695,-229.35005));
#223264=CARTESIAN_POINT('',(-2.22174260618994E-13,-11.0034818258363,-229.35005));
#223265=CARTESIAN_POINT('',(-1.54373336646987E-15,-42.8201004838369,-229.35005));
#223266=CARTESIAN_POINT('',(0.,-33.21456093117,-229.35005));
#223267=CARTESIAN_POINT('',(39.989972084972,-37.7858181964606,-229.35005));
#223268=CARTESIAN_POINT('Origin',(-636.934816028482,-11.5034818258361,-229.35005));
#223269=CARTESIAN_POINT('',(39.8203148590358,-38.3053945286125,-229.35005));
#223270=CARTESIAN_POINT('Origin',(38.9907249661392,-37.7470213473046,-229.35005));
#223271=CARTESIAN_POINT('Origin',(-6.29739814579425E-15,-11.5034818258363,
-229.35005));
#223272=CARTESIAN_POINT('',(-1.23757166668304E-15,-43.8201004838368,-229.35005));
#223273=CARTESIAN_POINT('',(23.4054219364689,-53.410357442802,-229.35005));
#223274=CARTESIAN_POINT('Origin',(-6.29739814579425E-15,-11.5034818258363,
-229.35005));
#223275=CARTESIAN_POINT('',(22.9516892713016,-53.5367234322311,-229.35005));
#223276=CARTESIAN_POINT('Origin',(22.9178089794592,-52.5372975341153,-229.35005));
#223277=CARTESIAN_POINT('Origin',(7.14692237356698E-14,623.509175991979,
-229.35005));
#223278=CARTESIAN_POINT('',(-2.8425373731103E-15,9.20759727949731,-229.35005));
#223279=CARTESIAN_POINT('',(-1.11087130309497E-13,-0.397942273169518,-229.35005));
#223280=CARTESIAN_POINT('',(-1.54373336646988E-15,19.8131368321642,-229.35005));
#223281=CARTESIAN_POINT('',(-2.53637567332344E-15,10.2075972794973,-229.35005));
#223282=CARTESIAN_POINT('',(-1.23757166668304E-15,20.8131368321642,-229.35005));
#223283=CARTESIAN_POINT('Origin',(-6.29739814579425E-15,-11.5034818258363,
-229.35005));
#223284=CARTESIAN_POINT('',(-2.22174260618994E-13,-11.0034818258363,-229.35005));
#223285=CARTESIAN_POINT('',(-1.11087130309497E-13,-1.3979422731695,-229.35005));
#223286=CARTESIAN_POINT('',(0.,-32.21456093117,-229.35005));
#223287=CARTESIAN_POINT('',(-2.22174260618994E-13,-12.0034818258363,-229.35005));
#223288=CARTESIAN_POINT('',(-2.8425373731103E-15,9.20759727949731,-229.35005));
#223289=CARTESIAN_POINT('',(-2.22174260618994E-13,-11.0034818258363,-229.35005));
#223290=CARTESIAN_POINT('',(-2.22174260618994E-13,-12.0034818258363,-229.35005));
#223291=CARTESIAN_POINT('',(-3.33261390928491E-13,-21.6090213785032,-229.35005));
#223292=CARTESIAN_POINT('Origin',(24.838300653577,28.3971299569735,-229.35005));
#223293=CARTESIAN_POINT('',(25.2655040598954,31.8709602996399,-232.25005));
#223294=CARTESIAN_POINT('',(25.2655040598954,31.8709602996399,-229.35005));
#223295=CARTESIAN_POINT('',(26.6879613405455,31.3684521110126,-232.25005));
#223296=CARTESIAN_POINT('',(26.6879613405455,31.3684521110126,-229.35005));
#223297=CARTESIAN_POINT('Origin',(24.838300653577,28.3971299569735,-232.25005));
#223298=CARTESIAN_POINT('Origin',(-6.29739814579425E-15,-11.5034818258363,
-229.35005));
#223299=CARTESIAN_POINT('',(41.8942895912773,16.6943638302095,-232.25005));
#223300=CARTESIAN_POINT('Origin',(-6.29739814579425E-15,-11.5034818258363,
-232.25005));
#223301=CARTESIAN_POINT('',(41.8942895912773,16.6943638302095,-229.35005));
#223302=CARTESIAN_POINT('Origin',(38.9907249661392,14.740057695632,-229.35005));
#223303=CARTESIAN_POINT('',(42.4880898820539,14.8758466676788,-232.25005));
#223304=CARTESIAN_POINT('',(42.4880898820538,14.8758466676788,-229.35005));
#223305=CARTESIAN_POINT('Origin',(38.9907249661392,14.740057695632,-232.25005));
#223306=CARTESIAN_POINT('Origin',(-636.934816028482,-11.5034818258361,-229.35005));
#223307=CARTESIAN_POINT('',(42.4880898820539,-37.8828103193509,-232.25005));
#223308=CARTESIAN_POINT('',(42.4880898820539,-37.8828103193507,-229.35005));
#223309=CARTESIAN_POINT('Origin',(-636.934816028482,-11.5034818258361,-232.25005));
#223310=CARTESIAN_POINT('Origin',(38.9907249661392,-37.7470213473046,-229.35005));
#223311=CARTESIAN_POINT('',(41.8942895912772,-39.701327481882,-232.25005));
#223312=CARTESIAN_POINT('',(41.8942895912772,-39.701327481882,-229.35005));
#223313=CARTESIAN_POINT('Origin',(38.9907249661392,-37.7470213473046,-232.25005));
#223314=CARTESIAN_POINT('Origin',(-6.29739814579425E-15,-11.5034818258363,
-229.35005));
#223315=CARTESIAN_POINT('',(24.6244543289934,-55.593007214519,-232.25005));
#223316=CARTESIAN_POINT('Origin',(-6.29739814579425E-15,-11.5034818258363,
-232.25005));
#223317=CARTESIAN_POINT('',(24.6244543289934,-55.593007214519,-229.35005));
#223318=CARTESIAN_POINT('Origin',(22.9178089794592,-52.5372975341153,-229.35005));
#223319=CARTESIAN_POINT('',(23.036390000908,-56.0352881775208,-232.25005));
#223320=CARTESIAN_POINT('',(23.036390000908,-56.0352881775208,-229.35005));
#223321=CARTESIAN_POINT('Origin',(22.9178089794592,-52.5372975341153,-232.25005));
#223322=CARTESIAN_POINT('Origin',(7.14692237356698E-14,623.509175991979,
-229.35005));
#223323=CARTESIAN_POINT('Origin',(7.14692237356698E-14,623.509175991979,
-232.25005));
#223324=CARTESIAN_POINT('Origin',(0.127542579976414,-12.8706479699377,-225.85005));
#223325=CARTESIAN_POINT('',(45.4582830719504,-55.6286991261908,-225.850049994059));
#223326=CARTESIAN_POINT('',(46.0196463796681,-56.2008156187296,-225.85005));
#223327=CARTESIAN_POINT('',(1.84775995058105,-11.1827640290625,-225.85005));
#223328=CARTESIAN_POINT('',(41.9650064389658,-58.9506113934371,-225.850044661983));
#223329=CARTESIAN_POINT('Ctrl Pts',(45.4582830570449,-55.6286991119449,
-225.85005));
#223330=CARTESIAN_POINT('Ctrl Pts',(44.9026972694785,-56.2100079876823,
-225.85005));
#223331=CARTESIAN_POINT('Ctrl Pts',(44.3324112171386,-56.7795949075102,
-225.85005));
#223332=CARTESIAN_POINT('Ctrl Pts',(43.1653582851246,-57.8895859697625,
-225.85005));
#223333=CARTESIAN_POINT('Ctrl Pts',(42.5695992766628,-58.4285233279616,
-225.85005));
#223334=CARTESIAN_POINT('Ctrl Pts',(41.9650009328216,-58.9506050170295,
-225.85005));
#223335=CARTESIAN_POINT('',(42.5792116384512,-59.576583500476,-225.85005));
#223336=CARTESIAN_POINT('',(-1.59267479062803,-14.5585319108126,-225.85005));
#223337=CARTESIAN_POINT('Origin',(48.1334350484927,-61.7961505568785,-225.85005));
#223338=CARTESIAN_POINT('Origin',(53.4203077633109,-63.7432454966418,-228.35005));
#223339=CARTESIAN_POINT('',(46.0300274667465,-56.2113955881677,-225.0730275154));
#223340=CARTESIAN_POINT('',(46.0300165430729,-56.2113851125247,-225.073041905978));
#223341=CARTESIAN_POINT('',(46.0300271011815,-56.2113951953429,-225.073057235855));
#223342=CARTESIAN_POINT('Origin',(0.128459562639233,-12.6359082483571,-225.85005));
#223343=CARTESIAN_POINT('',(43.3207863665692,34.1152634411122,-225.85005));
#223344=CARTESIAN_POINT('',(43.7661191575918,33.2092653454987,-225.850049986033));
#223345=CARTESIAN_POINT('Origin',(48.892180948596,36.2913696007177,-225.85005));
#223346=CARTESIAN_POINT('',(43.0713417429912,33.8649821651551,-225.850049999629));
#223347=CARTESIAN_POINT('',(50.4030915963197,41.2213231498315,-225.85005));
#223348=CARTESIAN_POINT('Ctrl Pts',(43.7661189696348,33.2092654883827,-225.85005));
#223349=CARTESIAN_POINT('Ctrl Pts',(43.6513378376322,33.3196167396708,-225.85005));
#223350=CARTESIAN_POINT('Ctrl Pts',(43.5360342857599,33.4294426438742,-225.85005));
#223351=CARTESIAN_POINT('Ctrl Pts',(43.3044413458354,33.6480087532319,-225.85005));
#223352=CARTESIAN_POINT('Ctrl Pts',(43.188133833512,33.7567661029554,-225.85005));
#223353=CARTESIAN_POINT('Ctrl Pts',(43.0713417424048,33.8649821645222,-225.85005));
#223354=CARTESIAN_POINT('Origin',(50.4030915963197,41.2213231498315,-228.35005));
#223355=CARTESIAN_POINT('',(43.3259173910555,34.120411675359,-225.468974352258));
#223356=CARTESIAN_POINT('Ctrl Pts',(43.325917391056,34.1204116753647,-225.468974352262));
#223357=CARTESIAN_POINT('Ctrl Pts',(43.2834889555987,34.0778409323755,-225.532489880709));
#223358=CARTESIAN_POINT('Ctrl Pts',(43.2410614099671,34.0352710821964,-225.596002003533));
#223359=CARTESIAN_POINT('Ctrl Pts',(43.1562018216867,33.9501268697379,-225.72302878886));
#223360=CARTESIAN_POINT('Ctrl Pts',(43.1137729118023,33.9075556507304,-225.786538761927));
#223361=CARTESIAN_POINT('Ctrl Pts',(43.0713417427678,33.8649821649953,-225.850049999372));
#223362=CARTESIAN_POINT('',(43.3259171707406,34.1204114543102,-225.468990713749));
#223363=CARTESIAN_POINT('Origin',(48.982196043432,-44.3222432618617,-167.906149834141));
#223364=CARTESIAN_POINT('',(54.2707699605536,-64.1721709500326,-208.192630912054));
#223365=CARTESIAN_POINT('',(54.238698329297,-64.0517945379221,-214.260116171494));
#223366=CARTESIAN_POINT('Ctrl Pts',(54.2707699605539,-64.1721709500341,
-208.192630912048));
#223367=CARTESIAN_POINT('Ctrl Pts',(54.2547227572974,-64.1119400013452,
-211.229354398965));
#223368=CARTESIAN_POINT('Ctrl Pts',(54.2386983294438,-64.051794536968,-214.260116171476));
#223369=CARTESIAN_POINT('',(53.7300151844417,-62.1425230012532,-215.85005));
#223370=CARTESIAN_POINT('Ctrl Pts',(53.7300151844416,-62.1425230012532,
-215.85005));
#223371=CARTESIAN_POINT('Ctrl Pts',(53.8150179700951,-62.4615691514925,
-215.58578405635));
#223372=CARTESIAN_POINT('Ctrl Pts',(53.8997787313547,-62.7797068967878,
-215.321544427173));
#223373=CARTESIAN_POINT('Ctrl Pts',(54.0694761933685,-63.4166427518271,
-214.791113982271));
#223374=CARTESIAN_POINT('Ctrl Pts',(54.153975481613,-63.7337990944663,-214.526290576087));
#223375=CARTESIAN_POINT('Ctrl Pts',(54.238698329735,-64.0517945380611,-214.260116171799));
#223376=CARTESIAN_POINT('',(54.2707699605536,-64.1721709500326,-215.85005));
#223377=CARTESIAN_POINT('',(53.272912245153,-60.426850603907,-215.85005));
#223378=CARTESIAN_POINT('',(54.2707699605536,-64.1721709500326,-208.192630912054));
#223379=CARTESIAN_POINT('Origin',(52.3809255634408,-67.7420224291304,-167.906149834141));
#223380=CARTESIAN_POINT('',(50.9302694872204,-67.3511117063321,-214.24934096818));
#223381=CARTESIAN_POINT('',(51.0503406624406,-67.3834674874005,-208.192630912054));
#223382=CARTESIAN_POINT('Ctrl Pts',(50.9302694862954,-67.35111170647,-214.249340968162));
#223383=CARTESIAN_POINT('Ctrl Pts',(50.9902625163406,-67.3672781287523,
-211.223956213722));
#223384=CARTESIAN_POINT('Ctrl Pts',(51.0503406624421,-67.3834674874009,
-208.192630912048));
#223385=CARTESIAN_POINT('',(51.0503406624406,-67.3834674874005,-215.85005));
#223386=CARTESIAN_POINT('',(51.0503406624406,-67.3834674874005,-208.192630912054));
#223387=CARTESIAN_POINT('',(48.9715866554311,-66.8233021636441,-215.85005));
#223388=CARTESIAN_POINT('',(52.3809255634408,-67.7420224291304,-215.85005));
#223389=CARTESIAN_POINT('Ctrl Pts',(50.930269487352,-67.3511117067547,-214.249340968478));
#223390=CARTESIAN_POINT('Ctrl Pts',(50.6138859321166,-67.2658553002478,
-214.510066201586));
#223391=CARTESIAN_POINT('Ctrl Pts',(50.2970498578574,-67.1804769526797,
-214.770075985769));
#223392=CARTESIAN_POINT('Ctrl Pts',(49.6441919995299,-67.0045502521929,
-215.303702766343));
#223393=CARTESIAN_POINT('Ctrl Pts',(49.308126257683,-66.9139900538979,-215.577233713243));
#223394=CARTESIAN_POINT('Ctrl Pts',(48.9715866554311,-66.8233021636442,
-215.85005));
#223395=CARTESIAN_POINT('Origin',(0.,-12.9675000200281,-167.906149834141));
#223396=CARTESIAN_POINT('Origin',(0.,-12.9675000200281,-208.192630912054));
#223397=CARTESIAN_POINT('Origin',(0.,-12.9675000200281,-215.85005));
#223398=CARTESIAN_POINT('Origin',(48.9106432152246,18.4987427374335,-167.906149834141));
#223399=CARTESIAN_POINT('',(54.1218033366501,38.2387592929899,-214.33352989342));
#223400=CARTESIAN_POINT('',(54.1539855075907,38.3606662320892,-208.192630912062));
#223401=CARTESIAN_POINT('Ctrl Pts',(54.1218033367874,38.2387592920601,-214.333529893402));
#223402=CARTESIAN_POINT('Ctrl Pts',(54.1378828568779,38.299668952361,-211.26613387672));
#223403=CARTESIAN_POINT('Ctrl Pts',(54.1539855075911,38.3606662320908,-208.192630912056));
#223404=CARTESIAN_POINT('',(54.1539855075907,38.3606662320892,-215.85005));
#223405=CARTESIAN_POINT('',(54.1539855075907,38.3606662320892,-208.192630912062));
#223406=CARTESIAN_POINT('',(53.6858060762413,36.5871897873468,-215.85005));
#223407=CARTESIAN_POINT('',(53.3004948454233,35.1276203445352,-215.85005));
#223408=CARTESIAN_POINT('Ctrl Pts',(54.1218033370754,38.2387592931511,-214.333529893716));
#223409=CARTESIAN_POINT('Ctrl Pts',(54.0493242413282,37.9642065032659,-214.587336490182));
#223410=CARTESIAN_POINT('Ctrl Pts',(53.9768175206474,37.6895490693776,-214.840391892315));
#223411=CARTESIAN_POINT('Ctrl Pts',(53.8314491180682,37.1388895988389,-215.346026703309));
#223412=CARTESIAN_POINT('Ctrl Pts',(53.7586988751255,36.8633096959893,-215.598218415187));
#223413=CARTESIAN_POINT('Ctrl Pts',(53.6858060762413,36.5871897873468,-215.85005));
#223414=CARTESIAN_POINT('Origin',(52.2560139340206,41.9262034053684,-167.906149834141));
#223415=CARTESIAN_POINT('',(50.9262492693411,41.5646183371225,-208.192630912063));
#223416=CARTESIAN_POINT('',(50.8045364442235,41.5315226009329,-214.335913275013));
#223417=CARTESIAN_POINT('Ctrl Pts',(50.9262492693426,41.5646183371229,-208.192630912057));
#223418=CARTESIAN_POINT('Ctrl Pts',(50.8653490995025,41.5480585708328,-211.267327940101));
#223419=CARTESIAN_POINT('Ctrl Pts',(50.8045364435665,41.5315226010249,-214.335913275001));
#223420=CARTESIAN_POINT('',(49.1680521502591,41.086535378401,-215.85005));
#223421=CARTESIAN_POINT('Ctrl Pts',(49.1680521502591,41.086535378401,-215.85005));
#223422=CARTESIAN_POINT('Ctrl Pts',(49.4414268426973,41.1608704915587,-215.598356099773));
#223423=CARTESIAN_POINT('Ctrl Pts',(49.7144017835735,41.2350969056362,-215.34641310643));
#223424=CARTESIAN_POINT('Ctrl Pts',(50.2599964077802,41.3834531333722,-214.841609804263));
#223425=CARTESIAN_POINT('Ctrl Pts',(50.5323141821189,41.4575008529682,-214.589028866932));
#223426=CARTESIAN_POINT('Ctrl Pts',(50.8045364443354,41.5315226012339,-214.335913275222));
#223427=CARTESIAN_POINT('',(50.9262492693411,41.5646183371225,-215.85005));
#223428=CARTESIAN_POINT('',(47.6970590536189,40.6865479570431,-215.85005));
#223429=CARTESIAN_POINT('',(50.9262492693411,41.5646183371225,-208.192630912063));
#223430=CARTESIAN_POINT('Origin',(0.,-12.9675000200281,-167.906149834141));
#223431=CARTESIAN_POINT('Origin',(0.,-12.9675000200281,-208.192630912063));
#223432=CARTESIAN_POINT('Origin',(0.,-12.9675000200281,-215.85005));
#223433=CARTESIAN_POINT('Ctrl Pts',(-34.6658396818824,-73.7171632516135,
-213.428100838228));
#223434=CARTESIAN_POINT('Ctrl Pts',(-32.4073514514297,-71.6005216742484,
-216.754800866966));
#223435=CARTESIAN_POINT('Ctrl Pts',(-30.1566827897054,-69.4835812050616,
-220.086775418501));
#223436=CARTESIAN_POINT('Ctrl Pts',(-27.9187794471678,-67.3680563271156,
-223.428575651002));
#223437=CARTESIAN_POINT('Ctrl Pts',(-25.6808761046303,-65.2525314491696,
-226.770375883505));
#223438=CARTESIAN_POINT('Ctrl Pts',(-23.4556914905361,-63.138057119071,
-230.121736209584));
#223439=CARTESIAN_POINT('Ctrl Pts',(-21.2513677279815,-61.0308575536349,
-233.492320591244));
#223440=CARTESIAN_POINT('Ctrl Pts',(-33.2915597883734,-73.6042889215327,
-213.3745249105));
#223441=CARTESIAN_POINT('Ctrl Pts',(-31.0883634812044,-71.468152600341,
-216.692012555656));
#223442=CARTESIAN_POINT('Ctrl Pts',(-28.8904868213221,-69.3312704464811,
-220.012578308794));
#223443=CARTESIAN_POINT('Ctrl Pts',(-26.7014864455845,-67.1937325026276,
-223.338673968425));
#223444=CARTESIAN_POINT('Ctrl Pts',(-24.5124860698469,-65.056194558774,
-226.664769628057));
#223445=CARTESIAN_POINT('Ctrl Pts',(-22.3321348006857,-62.9178895928583,
-229.996164050332));
#223446=CARTESIAN_POINT('Ctrl Pts',(-20.1678151009491,-60.7799059276903,
-233.338582766127));
#223447=CARTESIAN_POINT('Ctrl Pts',(-31.9147855165948,-73.552107297594,
-213.332282575322));
#223448=CARTESIAN_POINT('Ctrl Pts',(-29.762790671335,-71.4048671987398,
-216.642517917955));
#223449=CARTESIAN_POINT('Ctrl Pts',(-27.614141519417,-69.2569201923722,
-219.954463723004));
#223450=CARTESIAN_POINT('Ctrl Pts',(-25.4710721309401,-67.1080216677693,
-223.269410149594));
#223451=CARTESIAN_POINT('Ctrl Pts',(-23.3280027424632,-64.9591231431663,
-226.584356576184));
#223452=CARTESIAN_POINT('Ctrl Pts',(-21.1903744149072,-62.8092567666832,
-229.902202966067));
#223453=CARTESIAN_POINT('Ctrl Pts',(-19.0627867609462,-60.6582241972154,
-233.225804571524));
#223454=CARTESIAN_POINT('Ctrl Pts',(-30.5241947376933,-73.5610723424068,
-213.298768106724));
#223455=CARTESIAN_POINT('Ctrl Pts',(-28.4276303246862,-71.4106207619995,
-216.603490576449));
#223456=CARTESIAN_POINT('Ctrl Pts',(-26.3326980553541,-69.2597735546543,
-219.908997954485));
#223457=CARTESIAN_POINT('Ctrl Pts',(-24.2404948075278,-67.1083375120315,
-223.215865028164));
#223458=CARTESIAN_POINT('Ctrl Pts',(-22.1482915597014,-64.9569014694087,
-226.522732101843));
#223459=CARTESIAN_POINT('Ctrl Pts',(-20.0587460707107,-62.8048792414949,
-229.830915083866));
#223460=CARTESIAN_POINT('Ctrl Pts',(-17.9741423861937,-60.651964437303,
-233.141673289924));
#223461=CARTESIAN_POINT('Ctrl Pts',(-29.1336039587916,-73.5700373872195,
-213.265253638125));
#223462=CARTESIAN_POINT('Ctrl Pts',(-27.0924699780375,-71.4163743252592,
-216.564463234942));
#223463=CARTESIAN_POINT('Ctrl Pts',(-25.0512545912912,-69.2626269169363,
-219.863532185965));
#223464=CARTESIAN_POINT('Ctrl Pts',(-23.0099174841155,-67.1086533562937,
-223.162319906734));
#223465=CARTESIAN_POINT('Ctrl Pts',(-20.9685803769398,-64.9546797956511,
-226.461107627501));
#223466=CARTESIAN_POINT('Ctrl Pts',(-18.9271177265143,-62.8005017163066,
-229.759627201665));
#223467=CARTESIAN_POINT('Ctrl Pts',(-16.8854980114412,-60.6457046773906,
-233.057542008323));
#223468=CARTESIAN_POINT('Ctrl Pts',(-27.7294536429032,-73.6399428041704,
-213.240474674736));
#223469=CARTESIAN_POINT('Ctrl Pts',(-25.7480542838189,-71.4909831817195,
-216.535913459003));
#223470=CARTESIAN_POINT('Ctrl Pts',(-23.7650962505812,-69.3425324796987,
-219.83072032752));
#223471=CARTESIAN_POINT('Ctrl Pts',(-21.7795474514592,-67.1949306447615,
-223.124474795611));
#223472=CARTESIAN_POINT('Ctrl Pts',(-19.7939986523371,-65.0473288098244,
-226.418229263703));
#223473=CARTESIAN_POINT('Ctrl Pts',(-17.8059306828216,-62.9005566886187,
-229.710963422664));
#223474=CARTESIAN_POINT('Ctrl Pts',(-15.8131699469721,-60.7552971507389,
-233.001768361203));
#223475=CARTESIAN_POINT('Ctrl Pts',(-26.2966554094194,-73.7792956476785,
-213.222281607897));
#223476=CARTESIAN_POINT('Ctrl Pts',(-24.3872303655785,-71.6390760412356,
-216.515494177504));
#223477=CARTESIAN_POINT('Ctrl Pts',(-22.4748413392017,-69.5000413221554,
-219.807779103235));
#223478=CARTESIAN_POINT('Ctrl Pts',(-20.557339302015,-67.3632863153304,
-223.098617135674));
#223479=CARTESIAN_POINT('Ctrl Pts',(-18.6398372648283,-65.2265313085053,
-226.389455168113));
#223480=CARTESIAN_POINT('Ctrl Pts',(-16.7173760151126,-63.0919383281561,
-229.678857882383));
#223481=CARTESIAN_POINT('Ctrl Pts',(-14.7853232876922,-60.962226893778,
-232.965939947977));
#223482=CARTESIAN_POINT('Ctrl Pts',(-25.9384558510484,-73.8141338585555,
-213.217733341187));
#223483=CARTESIAN_POINT('Ctrl Pts',(-24.0470243860184,-71.6760992561146,
-216.510389357129));
#223484=CARTESIAN_POINT('Ctrl Pts',(-22.1522776113568,-69.5394185327696,
-219.802043797164));
#223485=CARTESIAN_POINT('Ctrl Pts',(-20.251787264654,-67.4053752329726,
-223.09215272069));
#223486=CARTESIAN_POINT('Ctrl Pts',(-18.3512969179511,-65.2713319331756,
-226.382261644216));
#223487=CARTESIAN_POINT('Ctrl Pts',(-16.4452373481854,-63.1397837380405,
-229.670831497314));
#223488=CARTESIAN_POINT('Ctrl Pts',(-14.5283616228722,-61.0139593295377,
-232.95698284467));
#223489=CARTESIAN_POINT('Ctrl Pts',(-25.5784605350385,-73.8533601027436,
-213.213609922838));
#223490=CARTESIAN_POINT('Ctrl Pts',(-23.7057733627891,-71.7177470584876,
-216.50580220452));
#223491=CARTESIAN_POINT('Ctrl Pts',(-21.829424123399,-69.5836623243557,
-219.796931745576));
#223492=CARTESIAN_POINT('Ctrl Pts',(-19.9466959826127,-67.4525975067612,
-223.08644224016));
#223493=CARTESIAN_POINT('Ctrl Pts',(-18.0639678418265,-65.3215326891668,
-226.375952734745));
#223494=CARTESIAN_POINT('Ctrl Pts',(-16.1750566993381,-63.193316429139,
-229.663842850422));
#223495=CARTESIAN_POINT('Ctrl Pts',(-14.2740735233503,-61.0717557132381,
-232.949279321911));
#223496=CARTESIAN_POINT('Ctrl Pts',(-25.2164735434195,-73.8971500307606,
-213.209914643405));
#223497=CARTESIAN_POINT('Ctrl Pts',(-23.3633710413988,-71.7641197332807,
-216.501723891369));
#223498=CARTESIAN_POINT('Ctrl Pts',(-21.5062602068635,-69.6327963210957,
-219.792419393228));
#223499=CARTESIAN_POINT('Ctrl Pts',(-19.6421180325743,-67.5049019292708,
-223.081443379649));
#223500=CARTESIAN_POINT('Ctrl Pts',(-17.7779758582852,-65.3770075374459,
-226.370467366069));
#223501=CARTESIAN_POINT('Ctrl Pts',(-15.9070218020806,-63.2523352409497,
-229.657807174511));
#223502=CARTESIAN_POINT('Ctrl Pts',(-14.0226731406951,-61.135361514269,
-232.942719688923));
#223503=CARTESIAN_POINT('Ctrl Pts',(-25.1938493564434,-73.8998869012617,
-213.20968368844));
#223504=CARTESIAN_POINT('Ctrl Pts',(-23.341970896312,-71.7670180254552,
-216.501468996797));
#223505=CARTESIAN_POINT('Ctrl Pts',(-21.48606246208,-69.635867195892,-219.792137371206));
#223506=CARTESIAN_POINT('Ctrl Pts',(-19.6230819106969,-67.5081709556776,
-223.081130950866));
#223507=CARTESIAN_POINT('Ctrl Pts',(-17.7601013593138,-65.3804747154633,
-226.370124530527));
#223508=CARTESIAN_POINT('Ctrl Pts',(-15.8902696210019,-63.2560239166879,
-229.657429944766));
#223509=CARTESIAN_POINT('Ctrl Pts',(-14.0069606167792,-61.1393368768334,
-232.942309711862));
#223510=CARTESIAN_POINT('Ctrl Pts',(-25.1712173883496,-73.9026415976708,
-213.209454406389));
#223511=CARTESIAN_POINT('Ctrl Pts',(-23.3205662528727,-71.7699347734086,
-216.501216091021));
#223512=CARTESIAN_POINT('Ctrl Pts',(-21.4658635039096,-69.6389571726479,
-219.791857693934));
#223513=CARTESIAN_POINT('Ctrl Pts',(-19.6040477936697,-67.5114598348967,
-223.080821306009));
#223514=CARTESIAN_POINT('Ctrl Pts',(-17.7422320834297,-65.3839624971454,
-226.369784918083));
#223515=CARTESIAN_POINT('Ctrl Pts',(-15.8735258224357,-63.2597340257226,
-229.657056446399));
#223516=CARTESIAN_POINT('Ctrl Pts',(-13.9912593731559,-61.1433349412254,
-232.941904217913));
#223517=CARTESIAN_POINT('Ctrl Pts',(-25.1485775908401,-73.9054141624873,
-213.20922679825));
#223518=CARTESIAN_POINT('Ctrl Pts',(-23.2991570846963,-71.7728700013293,
-216.500965172342));
#223519=CARTESIAN_POINT('Ctrl Pts',(-21.4456633269945,-69.64206625697,-219.791580356527));
#223520=CARTESIAN_POINT('Ctrl Pts',(-19.585015694187,-67.5147685546799,
-223.080514436398));
#223521=CARTESIAN_POINT('Ctrl Pts',(-17.7243680613796,-65.3874708523898,
-226.369448516269));
#223522=CARTESIAN_POINT('Ctrl Pts',(-15.8567904524812,-63.2634655201407,
-229.656686662215));
#223523=CARTESIAN_POINT('Ctrl Pts',(-13.9755694621469,-61.1473556487506,
-232.94150318618));
#223524=CARTESIAN_POINT('Ctrl Pts',(-25.1372576920853,-73.9068004448956,
-213.209112994182));
#223525=CARTESIAN_POINT('Ctrl Pts',(-23.2884525006082,-71.7743376152897,
-216.500839713002));
#223526=CARTESIAN_POINT('Ctrl Pts',(-21.435563238537,-69.6436207991311,
-219.791441687824));
#223527=CARTESIAN_POINT('Ctrl Pts',(-19.5754996444458,-67.5164229145716,
-223.080361001593));
#223528=CARTESIAN_POINT('Ctrl Pts',(-17.7154360503545,-65.3892250300121,
-226.369280315361));
#223529=CARTESIAN_POINT('Ctrl Pts',(-15.848422767504,-63.2653312673498,
-229.656501770123));
#223530=CARTESIAN_POINT('Ctrl Pts',(-13.9677245066424,-61.1493660025132,
-232.941302670313));
#223531=CARTESIAN_POINT('Ctrl Pts',(-25.1275380438543,-73.9076291783905,
-213.20952316564));
#223532=CARTESIAN_POINT('Ctrl Pts',(-23.2795399985599,-71.7751646462399,
-216.501290127757));
#223533=CARTESIAN_POINT('Ctrl Pts',(-21.4274775737994,-69.6444332830956,
-219.791935697107));
#223534=CARTESIAN_POINT('Ctrl Pts',(-19.5682702013894,-67.5171959518095,
-223.080900090889));
#223535=CARTESIAN_POINT('Ctrl Pts',(-17.7090628289793,-65.3899586205233,
-226.369864484671));
#223536=CARTESIAN_POINT('Ctrl Pts',(-15.8429357037125,-63.2660013665179,
-229.657133322639));
#223537=CARTESIAN_POINT('Ctrl Pts',(-13.9631639616011,-61.1499215051536,
-232.941973404526));
#223538=CARTESIAN_POINT('Ctrl Pts',(-25.1172506902082,-73.9086491431425,
-213.209748447694));
#223539=CARTESIAN_POINT('Ctrl Pts',(-23.2699927375599,-71.7762117787703,
-216.501537340245));
#223540=CARTESIAN_POINT('Ctrl Pts',(-21.4186793651933,-69.6455012585658,
-219.79220648111));
#223541=CARTESIAN_POINT('Ctrl Pts',(-19.5602329485478,-67.5182732019455,
-223.081194907277));
#223542=CARTESIAN_POINT('Ctrl Pts',(-17.7017865319023,-65.3910451453252,
-226.370183333444));
#223543=CARTESIAN_POINT('Ctrl Pts',(-15.836432876535,-63.267085758858,-229.657477064394));
#223544=CARTESIAN_POINT('Ctrl Pts',(-13.9574463443376,-61.150982255238,
-232.942337206168));
#223545=CARTESIAN_POINT('Ctrl Pts',(-25.106963336562,-73.9096691078946,
-213.209973729747));
#223546=CARTESIAN_POINT('Ctrl Pts',(-23.2604454765599,-71.7772589113006,
-216.501784552733));
#223547=CARTESIAN_POINT('Ctrl Pts',(-21.4098811565871,-69.6465692340359,
-219.792477265113));
#223548=CARTESIAN_POINT('Ctrl Pts',(-19.5521956957062,-67.5193504520815,
-223.081489723665));
#223549=CARTESIAN_POINT('Ctrl Pts',(-17.6945102348253,-65.392131670127,
-226.370502182217));
#223550=CARTESIAN_POINT('Ctrl Pts',(-15.8299300493574,-63.2681701511981,
-229.657820806149));
#223551=CARTESIAN_POINT('Ctrl Pts',(-13.9517287270741,-61.1520430053224,
-232.94270100781));
#223552=CARTESIAN_POINT('Ctrl Pts',(-25.0966732952022,-73.9106854314293,
-213.210198877687));
#223553=CARTESIAN_POINT('Ctrl Pts',(-23.250895955041,-71.7783021244353,
-216.502031618963));
#223554=CARTESIAN_POINT('Ctrl Pts',(-21.4010811306241,-69.6476330262175,
-219.792747904445));
#223555=CARTESIAN_POINT('Ctrl Pts',(-19.5441571297629,-67.5204232646219,
-223.081784431703));
#223556=CARTESIAN_POINT('Ctrl Pts',(-17.6872331289017,-65.3932135030263,
-226.370820958961));
#223557=CARTESIAN_POINT('Ctrl Pts',(-15.8234269724959,-63.2692496127142,
-229.658164546835));
#223558=CARTESIAN_POINT('Ctrl Pts',(-13.9460116075155,-61.1530985453856,
-232.943064954014));
#223559=CARTESIAN_POINT('Ctrl Pts',(-25.0863805784975,-73.9116981070231,
-213.210423891692));
#223560=CARTESIAN_POINT('Ctrl Pts',(-23.2413441840141,-71.7793414134067,
-216.502278538958));
#223561=CARTESIAN_POINT('Ctrl Pts',(-21.3922792967099,-69.6486926323558,
-219.793018398825));
#223562=CARTESIAN_POINT('Ctrl Pts',(-19.5361172580706,-67.5214916392076,
-223.082079030658));
#223563=CARTESIAN_POINT('Ctrl Pts',(-17.6799552194313,-65.3942906460594,
-226.371139662492));
#223564=CARTESIAN_POINT('Ctrl Pts',(-15.8169236486442,-63.2703241481874,
-229.658508284608));
#223565=CARTESIAN_POINT('Ctrl Pts',(-13.9402949855656,-61.1541488842789,
-232.943429042643));
#223566=CARTESIAN_POINT('Ctrl Pts',(-25.045209711679,-73.9157488093984,
-213.211323947711));
#223567=CARTESIAN_POINT('Ctrl Pts',(-23.2031370999064,-71.7834985692924,
-216.503266218939));
#223568=CARTESIAN_POINT('Ctrl Pts',(-21.3570719610534,-69.6529310569089,
-219.794100376343));
#223569=CARTESIAN_POINT('Ctrl Pts',(-19.5039577713016,-67.5257651375503,
-223.083257426481));
#223570=CARTESIAN_POINT('Ctrl Pts',(-17.6508435815496,-65.3985992181917,
-226.372414476619));
#223571=CARTESIAN_POINT('Ctrl Pts',(-15.790910353237,-63.2746222900799,
-229.659883235697));
#223572=CARTESIAN_POINT('Ctrl Pts',(-13.917428497766,-61.1583502398519,
-232.944885397156));
#223573=CARTESIAN_POINT('Ctrl Pts',(-25.0039960393562,-73.9197411446691,
-213.212221860696));
#223574=CARTESIAN_POINT('Ctrl Pts',(-23.1648940236841,-71.7875929385222,
-216.504251559075));
#223575=CARTESIAN_POINT('Ctrl Pts',(-21.3218356981714,-69.6571025047546,
-219.795180034489));
#223576=CARTESIAN_POINT('Ctrl Pts',(-19.4717773925363,-67.5299676286889,
-223.084434076858));
#223577=CARTESIAN_POINT('Ctrl Pts',(-17.621719086901,-65.4028327526231,
-226.373688119226));
#223578=CARTESIAN_POINT('Ctrl Pts',(-15.764893105952,-63.2788416156206,
-229.661258140053));
#223579=CARTESIAN_POINT('Ctrl Pts',(-13.8945699719964,-61.1624683771664,
-232.946344030549));
#223580=CARTESIAN_POINT('Ctrl Pts',(-24.9627403530703,-73.923674682942,
-213.213117642504));
#223581=CARTESIAN_POINT('Ctrl Pts',(-23.1266156599325,-71.7916242163186,
-216.505234561518));
#223582=CARTESIAN_POINT('Ctrl Pts',(-21.2865711101685,-69.6612067996797,
-219.796257356156));
#223583=CARTESIAN_POINT('Ctrl Pts',(-19.4395765925336,-67.534099089021,
-223.085608935934));
#223584=CARTESIAN_POINT('Ctrl Pts',(-17.5925820748987,-65.4069913783622,
-226.374960515711));
#223585=CARTESIAN_POINT('Ctrl Pts',(-15.7388720794572,-63.2829824280842,
-229.662632880376));
#223586=CARTESIAN_POINT('Ctrl Pts',(-13.8717193997808,-61.1665038590062,
-232.947804805375));
#223587=CARTESIAN_POINT('Ctrl Pts',(-24.8802289804986,-73.9315417594878,
-213.214909206118));
#223588=CARTESIAN_POINT('Ctrl Pts',(-23.050058932429,-71.7996867719115,
-216.507200566404));
#223589=CARTESIAN_POINT('Ctrl Pts',(-21.2160419341625,-69.6694153895299,
-219.79841199949));
#223590=CARTESIAN_POINT('Ctrl Pts',(-19.3751749925283,-67.5423620096852,
-223.087958654085));
#223591=CARTESIAN_POINT('Ctrl Pts',(-17.534308050894,-65.4153086298405,
-226.37750530868));
#223592=CARTESIAN_POINT('Ctrl Pts',(-15.6868300264676,-63.2912640530112,
-229.665382361023));
#223593=CARTESIAN_POINT('Ctrl Pts',(-13.8260182553497,-61.1745748226858,
-232.950726355029));
#223594=CARTESIAN_POINT('Ctrl Pts',(-24.7975495521845,-73.9391736473788,
-213.216692244198));
#223595=CARTESIAN_POINT('Ctrl Pts',(-22.9733610549633,-71.8074969612026,
-216.509157219437));
#223596=CARTESIAN_POINT('Ctrl Pts',(-21.1453994575107,-69.6773553674969,
-219.800557295378));
#223597=CARTESIAN_POINT('Ctrl Pts',(-19.3106917073121,-67.5503408080304,
-223.090301205408));
#223598=CARTESIAN_POINT('Ctrl Pts',(-17.4759839571134,-65.4233262485639,
-226.380045115437));
#223599=CARTESIAN_POINT('Ctrl Pts',(-15.6347728560193,-63.2992316298716,
-229.668131184037));
#223600=CARTESIAN_POINT('Ctrl Pts',(-13.7803489284904,-61.1823151706218,
-232.953656471305));
#223601=CARTESIAN_POINT('Ctrl Pts',(-24.7147083990042,-73.9465669153705,
-213.218466861474));
#223602=CARTESIAN_POINT('Ctrl Pts',(-22.8965276622237,-71.8150523527114,
-216.511104550879));
#223603=CARTESIAN_POINT('Ctrl Pts',(-21.0746484989569,-69.6850253260783,
-219.802693125391));
#223604=CARTESIAN_POINT('Ctrl Pts',(-19.2461305058836,-67.5580352841057,
-223.092636242468));
#223605=CARTESIAN_POINT('Ctrl Pts',(-17.4176125128103,-65.431045242133,
-226.382579359545));
#223606=CARTESIAN_POINT('Ctrl Pts',(-15.5827019558309,-63.3068875335073,
-229.67087842819));
#223607=CARTESIAN_POINT('Ctrl Pts',(-13.7347113090203,-61.1897293326622,
-232.956594042948));
#223608=CARTESIAN_POINT('Ctrl Pts',(-24.5490260926436,-73.9613534513537,
-213.222016096024));
#223609=CARTESIAN_POINT('Ctrl Pts',(-22.7428608767445,-71.8301631357291,
-216.51499921376));
#223610=CARTESIAN_POINT('Ctrl Pts',(-20.9331465818493,-69.7003652432411,
-219.806964785417));
#223611=CARTESIAN_POINT('Ctrl Pts',(-19.1170081030267,-67.5734242362562,
-223.097306316589));
#223612=CARTESIAN_POINT('Ctrl Pts',(-17.3008696242042,-65.4464832292714,
-226.387647847762));
#223613=CARTESIAN_POINT('Ctrl Pts',(-15.478560155454,-63.3221993407787,
-229.676372916496));
#223614=CARTESIAN_POINT('Ctrl Pts',(-13.64343607008,-61.2045576567429,-232.962469186234));
#223615=CARTESIAN_POINT('Ctrl Pts',(-24.382696887998,-73.9751854967928,
-213.225531634411));
#223616=CARTESIAN_POINT('Ctrl Pts',(-22.5886520321449,-71.8442547181521,
-216.518856573352));
#223617=CARTESIAN_POINT('Ctrl Pts',(-20.79121073452,-69.7146250786933,-219.811198558066));
#223618=CARTESIAN_POINT('Ctrl Pts',(-18.987574030311,-67.5876759125815,
-223.101946307423));
#223619=CARTESIAN_POINT('Ctrl Pts',(-17.183937326102,-65.4607267464698,
-226.39269405678));
#223620=CARTESIAN_POINT('Ctrl Pts',(-15.3743634215613,-63.3362645204375,
-229.681861061496));
#223621=CARTESIAN_POINT('Ctrl Pts',(-13.5522877040622,-61.2180813417051,
-232.968374159806));
#223622=CARTESIAN_POINT('Ctrl Pts',(-24.2157714140078,-73.9880357308615,
-213.229014471039));
#223623=CARTESIAN_POINT('Ctrl Pts',(-22.4339461787348,-71.8573077591623,
-216.522677077293));
#223624=CARTESIAN_POINT('Ctrl Pts',(-20.6488795380216,-69.7277936159865,
-219.815393786219));
#223625=CARTESIAN_POINT('Ctrl Pts',(-18.8578584941732,-67.6007885459744,
-223.106553748693));
#223626=CARTESIAN_POINT('Ctrl Pts',(-17.0668374503248,-65.4737834759622,
-226.397713711166));
#223627=CARTESIAN_POINT('Ctrl Pts',(-15.2701229993362,-63.3491012702364,
-229.687335801966));
#223628=CARTESIAN_POINT('Ctrl Pts',(-13.4612647392615,-61.230334612939,
-232.974299931676));
#223629=CARTESIAN_POINT('Ctrl Pts',(-23.5480695180473,-74.0394366671362,
-213.24294581755));
#223630=CARTESIAN_POINT('Ctrl Pts',(-21.8151227650944,-71.9095199232031,
-216.537959093058));
#223631=CARTESIAN_POINT('Ctrl Pts',(-20.0795547520278,-69.7804677651596,
-219.832174698832));
#223632=CARTESIAN_POINT('Ctrl Pts',(-18.3389963496219,-67.6532390795458,
-223.124983513772));
#223633=CARTESIAN_POINT('Ctrl Pts',(-16.598437947216,-65.526010393932,-226.417792328712));
#223634=CARTESIAN_POINT('Ctrl Pts',(-14.8531613104359,-63.4004482694319,
-229.709234763845));
#223635=CARTESIAN_POINT('Ctrl Pts',(-13.0971728800584,-61.279347697875,
-232.998003019155));
#223636=CARTESIAN_POINT('Ctrl Pts',(-22.8709481805904,-74.0750232880782,
-213.256420242625));
#223637=CARTESIAN_POINT('Ctrl Pts',(-21.1884296153893,-71.9450395755471,
-216.552700075075));
#223638=CARTESIAN_POINT('Ctrl Pts',(-19.5039372878188,-69.8156379211665,
-219.84836591417));
#223639=CARTESIAN_POINT('Ctrl Pts',(-17.815594292309,-67.6874631000348,
-223.142892403823));
#223640=CARTESIAN_POINT('Ctrl Pts',(-16.1272512967992,-65.5592882789031,
-226.437418893476));
#223641=CARTESIAN_POINT('Ctrl Pts',(-14.4353045594034,-63.4322301175141,
-229.730858925088));
#223642=CARTESIAN_POINT('Ctrl Pts',(-12.7347707201458,-61.3081954246526,
-233.021942401312));
#223643=CARTESIAN_POINT('Ctrl Pts',(-22.1870742035844,-74.0934804397452,
-213.269235878432));
#223644=CARTESIAN_POINT('Ctrl Pts',(-20.5563486581325,-71.9629449474399,
-216.566743885946));
#223645=CARTESIAN_POINT('Ctrl Pts',(-18.9243205135762,-69.8327666793282,
-219.863841772444));
#223646=CARTESIAN_POINT('Ctrl Pts',(-17.2897176470888,-67.7033388994737,
-223.160157702189));
#223647=CARTESIAN_POINT('Ctrl Pts',(-15.6551147806014,-65.5739111196192,
-226.456473631933));
#223648=CARTESIAN_POINT('Ctrl Pts',(-14.0181153557779,-63.4451661048354,
-229.752051509661));
#223649=CARTESIAN_POINT('Ctrl Pts',(-12.3752611396659,-61.3182690712574,
-233.045942634108));
#223650=CARTESIAN_POINT('Ctrl Pts',(-20.8193262495723,-74.1303947430791,
-213.294867150045));
#223651=CARTESIAN_POINT('Ctrl Pts',(-19.292186743619,-71.9987556912256,
-216.594831507688));
#223652=CARTESIAN_POINT('Ctrl Pts',(-17.765086965091,-69.8670241956515,
-219.894793488995));
#223653=CARTESIAN_POINT('Ctrl Pts',(-16.2379643566484,-67.7350904983513,
-223.194688298921));
#223654=CARTESIAN_POINT('Ctrl Pts',(-14.7108417482059,-65.6031568010512,
-226.494583108848));
#223655=CARTESIAN_POINT('Ctrl Pts',(-13.183736948527,-63.471038079478,-229.794436678806));
#223656=CARTESIAN_POINT('Ctrl Pts',(-11.656241978706,-61.3384163644669,
-233.0939430997));
#223657=CARTESIAN_POINT('Ctrl Pts',(-19.42533001526,-74.0979893885821,-213.31813023739));
#223658=CARTESIAN_POINT('Ctrl Pts',(-18.0070778075469,-71.9634650061569,
-216.620336307912));
#223659=CARTESIAN_POINT('Ctrl Pts',(-16.5902654999009,-69.828635705168,
-219.92301297597));
#223660=CARTESIAN_POINT('Ctrl Pts',(-15.1764619582282,-67.6931640554203,
-223.226671478159));
#223661=CARTESIAN_POINT('Ctrl Pts',(-13.7626584165554,-65.5576924056727,
-226.53032998035));
#223662=CARTESIAN_POINT('Ctrl Pts',(-12.3515772232236,-63.4216427758456,
-229.834879431719));
#223663=CARTESIAN_POINT('Ctrl Pts',(-10.9479532026315,-61.283976471277,
-233.141846820839));
#223664=CARTESIAN_POINT('Ctrl Pts',(-18.0356123358475,-73.9925802279181,
-213.337833927419));
#223665=CARTESIAN_POINT('Ctrl Pts',(-16.7281499098072,-71.8547048439425,
-216.642247555954));
#223666=CARTESIAN_POINT('Ctrl Pts',(-15.4235797449757,-69.7165429992464,
-219.947634512311));
#223667=CARTESIAN_POINT('Ctrl Pts',(-14.1251185099843,-67.5779955815407,
-223.255219367307));
#223668=CARTESIAN_POINT('Ctrl Pts',(-12.8266572749929,-65.4394481638349,
-226.562804222303));
#223669=CARTESIAN_POINT('Ctrl Pts',(-11.5337362244292,-63.3004500825909,
-229.872316979927));
#223670=CARTESIAN_POINT('Ctrl Pts',(-10.2559925260515,-61.1612854472115,
-233.187802584486));
#223671=CARTESIAN_POINT('Ctrl Pts',(-17.6881829159944,-73.9662279377521,
-213.342759849927));
#223672=CARTESIAN_POINT('Ctrl Pts',(-16.4084179353722,-71.8275148033889,
-216.647725367964));
#223673=CARTESIAN_POINT('Ctrl Pts',(-15.1319083062445,-69.688519822766,
-219.953789896397));
#223674=CARTESIAN_POINT('Ctrl Pts',(-13.8622826479234,-67.5492034630707,
-223.262356339594));
#223675=CARTESIAN_POINT('Ctrl Pts',(-12.5926569896023,-65.4098871033754,
-226.570922782791));
#223676=CARTESIAN_POINT('Ctrl Pts',(-11.3292759747306,-63.2701519092773,
-229.881676366978));
#223677=CARTESIAN_POINT('Ctrl Pts',(-10.0830023569065,-61.1306126911951,
-233.199291525398));
#223678=CARTESIAN_POINT('Ctrl Pts',(-17.3409698674155,-73.935384443929,
-213.34743873701));
#223679=CARTESIAN_POINT('Ctrl Pts',(-16.0890297520637,-71.7957877789297,
-216.65295762787));
#223680=CARTESIAN_POINT('Ctrl Pts',(-14.8407142907582,-69.6559284272906,
-219.959704440269));
#223681=CARTESIAN_POINT('Ctrl Pts',(-13.6000677993871,-67.5158548561218,
-223.269270451958));
#223682=CARTESIAN_POINT('Ctrl Pts',(-12.3594213080159,-65.375781284953,
-226.578836463649));
#223683=CARTESIAN_POINT('Ctrl Pts',(-11.1257374792571,-63.2353536891053,
-229.890858807334));
#223684=CARTESIAN_POINT('Ctrl Pts',(-9.91109018312546,-61.0956375485126,
-233.210683839047));
#223685=CARTESIAN_POINT('Ctrl Pts',(-16.9945696080803,-73.9001081635259,
-213.351879630837));
#223686=CARTESIAN_POINT('Ctrl Pts',(-15.7705099053272,-71.7595755214746,
-216.657951790479));
#223687=CARTESIAN_POINT('Ctrl Pts',(-14.5504477647407,-69.6188149294866,
-219.965383361714));
#223688=CARTESIAN_POINT('Ctrl Pts',(-13.3388364480016,-67.4779925971457,
-223.275961013327));
#223689=CARTESIAN_POINT('Ctrl Pts',(-12.1272251312625,-65.3371702648048,
-226.586538664941));
#223690=CARTESIAN_POINT('Ctrl Pts',(-10.9233008549777,-63.1960951941825,
-229.899850654492));
#223691=CARTESIAN_POINT('Ctrl Pts',(-9.74027549479166,-61.0564003174778,
-233.221936356199));
#223692=CARTESIAN_POINT('Ctrl Pts',(-16.8213694784127,-73.8824700233243,
-213.35410007775));
#223693=CARTESIAN_POINT('Ctrl Pts',(-15.611249981959,-71.7414693927469,
-216.660448871784));
#223694=CARTESIAN_POINT('Ctrl Pts',(-14.4053145017319,-69.6002581805847,
-219.968222822436));
#223695=CARTESIAN_POINT('Ctrl Pts',(-13.2082207723089,-67.4590614676576,
-223.279306294012));
#223696=CARTESIAN_POINT('Ctrl Pts',(-12.0111270428858,-65.3178647547306,
-226.590389765587));
#223697=CARTESIAN_POINT('Ctrl Pts',(-10.822082542838,-63.1764659467212,
-229.904346578071));
#223698=CARTESIAN_POINT('Ctrl Pts',(-9.65486815062476,-61.0367817019604,
-233.227562614775));
#223699=CARTESIAN_POINT('Ctrl Pts',(-16.6483725774174,-73.8637237686103,
-213.356261096586));
#223700=CARTESIAN_POINT('Ctrl Pts',(-15.4522071799355,-71.7222420367263,
-216.662886513868));
#223701=CARTESIAN_POINT('Ctrl Pts',(-14.2604131527873,-69.5805709842817,
-219.971003481449));
#223702=CARTESIAN_POINT('Ctrl Pts',(-13.0778510032714,-67.4390019693148,
-223.282595807161));
#223703=CARTESIAN_POINT('Ctrl Pts',(-11.8952888537556,-65.297432954348,
-226.594188132872));
#223704=CARTESIAN_POINT('Ctrl Pts',(-10.7211396966759,-63.1557216095298,
-229.908795015727));
#223705=CARTESIAN_POINT('Ctrl Pts',(-9.5697351055252,-61.0160972517994,
-233.233154034774));
#223706=CARTESIAN_POINT('Ctrl Pts',(-16.475653681056,-73.8438772043605,
-213.358364250325));
#223707=CARTESIAN_POINT('Ctrl Pts',(-15.293447315483,-71.7019004243738,
-216.665266171061));
#223708=CARTESIAN_POINT('Ctrl Pts',(-14.1158002338706,-69.5597595986402,
-219.973726626617));
#223709=CARTESIAN_POINT('Ctrl Pts',(-12.9477726440157,-67.4178197482303,
-223.28583020421));
#223710=CARTESIAN_POINT('Ctrl Pts',(-11.7797450541607,-65.2758798978204,
-226.597933781803));
#223711=CARTESIAN_POINT('Ctrl Pts',(-10.6204947589615,-63.133867051308,
-229.913195248457));
#223712=CARTESIAN_POINT('Ctrl Pts',(-9.48487851766271,-60.9943501153288,
-233.238705966824));
#223713=CARTESIAN_POINT('Ctrl Pts',(-16.3892942328753,-73.8339539222356,
-213.359415827195));
#223714=CARTESIAN_POINT('Ctrl Pts',(-15.2140673832569,-71.6917296181976,
-216.666455999658));
#223715=CARTESIAN_POINT('Ctrl Pts',(-14.0434937744123,-69.5493539058194,
-219.9750881992));
#223716=CARTESIAN_POINT('Ctrl Pts',(-12.8827334643878,-67.407228637688,
-223.287447402734));
#223717=CARTESIAN_POINT('Ctrl Pts',(-11.7219731543633,-65.2651033695566,
-226.599806606268));
#223718=CARTESIAN_POINT('Ctrl Pts',(-10.5701722901042,-63.1229397721972,
-229.915395364823));
#223719=CARTESIAN_POINT('Ctrl Pts',(-9.44245022373146,-60.9834765470935,
-233.241481932849));
#223720=CARTESIAN_POINT('Ctrl Pts',(-16.3030042884726,-73.8237555680483,
-213.360452942392));
#223721=CARTESIAN_POINT('Ctrl Pts',(-15.1347581882095,-71.6812802533029,
-216.667631337573));
#223722=CARTESIAN_POINT('Ctrl Pts',(-13.9712594252062,-69.5386671710029,
-219.976435400044));
#223723=CARTESIAN_POINT('Ctrl Pts',(-12.8177671391991,-67.3963568497133,
-223.289050830054));
#223724=CARTESIAN_POINT('Ctrl Pts',(-11.664274853192,-65.2540465284237,
-226.601666260063));
#223725=CARTESIAN_POINT('Ctrl Pts',(-10.5199242971055,-63.1117349369396,
-229.917583440331));
#223726=CARTESIAN_POINT('Ctrl Pts',(-9.40009104247648,-60.9723372875069,
-233.244248035339));
#223727=CARTESIAN_POINT('Ctrl Pts',(-16.2167932117529,-73.8132831498086,
-213.361475819387));
#223728=CARTESIAN_POINT('Ctrl Pts',(-15.0555279749204,-71.6705532338771,
-216.66879240035));
#223729=CARTESIAN_POINT('Ctrl Pts',(-13.8991042674645,-69.5277002093067,
-219.977768430969));
#223730=CARTESIAN_POINT('Ctrl Pts',(-12.7528793682143,-67.3852051104264,
-223.290640615083));
#223731=CARTESIAN_POINT('Ctrl Pts',(-11.6066544689641,-65.242710011546,
-226.603512799196));
#223732=CARTESIAN_POINT('Ctrl Pts',(-10.4697535757229,-63.1002531490252,
-229.919759447508));
#223733=CARTESIAN_POINT('Ctrl Pts',(-9.35780123872676,-60.9609326117215,
-233.247003746217));
#223734=CARTESIAN_POINT('Ctrl Pts',(-16.1952404425729,-73.8106650452487,
-213.361731538637));
#223735=CARTESIAN_POINT('Ctrl Pts',(-15.0357204215981,-71.6678714790206,
-216.669082666044));
#223736=CARTESIAN_POINT('Ctrl Pts',(-13.8810654780291,-69.5249584688827,
-219.9781016887));
#223737=CARTESIAN_POINT('Ctrl Pts',(-12.7366574254681,-67.3824171756047,
-223.29103806134));
#223738=CARTESIAN_POINT('Ctrl Pts',(-11.5922493729072,-65.2398758823266,
-226.60397443398));
#223739=CARTESIAN_POINT('Ctrl Pts',(-10.4572108953772,-63.0973827020465,
-229.920303449302));
#223740=CARTESIAN_POINT('Ctrl Pts',(-9.34722878778933,-60.9580814427752,
-233.247692673936));
#223741=CARTESIAN_POINT('Ctrl Pts',(-16.1749279659312,-73.8079309222085,
-213.362368684823));
#223742=CARTESIAN_POINT('Ctrl Pts',(-15.0172739344155,-71.6650756920887,
-216.669799089985));
#223743=CARTESIAN_POINT('Ctrl Pts',(-13.8645330142372,-69.5221076454515,
-219.978916472587));
#223744=CARTESIAN_POINT('Ctrl Pts',(-12.7221372554057,-67.3795379414851,
-223.291998591574));
#223745=CARTESIAN_POINT('Ctrl Pts',(-11.5797414965742,-65.2369682375188,
-226.605080710561));
#223746=CARTESIAN_POINT('Ctrl Pts',(-10.4468084359715,-63.0944652668042,
-229.921596248607));
#223747=CARTESIAN_POINT('Ctrl Pts',(-9.33915242519547,-60.9552650705159,
-233.249310581749));
#223748=CARTESIAN_POINT('Ctrl Pts',(-16.1509595327512,-73.8054672009616,
-213.361871023763));
#223749=CARTESIAN_POINT('Ctrl Pts',(-14.9948134280635,-71.6625434043229,
-216.669248038006));
#223750=CARTESIAN_POINT('Ctrl Pts',(-13.8435558938145,-69.5195048912895,
-219.978299602301));
#223751=CARTESIAN_POINT('Ctrl Pts',(-12.702592770651,-67.376854004913,-223.291285721626));
#223752=CARTESIAN_POINT('Ctrl Pts',(-11.5616296474874,-65.2342031185365,
-226.60427184095));
#223753=CARTESIAN_POINT('Ctrl Pts',(-10.4300813444879,-63.0916122772293,
-229.920665266036));
#223754=CARTESIAN_POINT('Ctrl Pts',(-9.32369428622946,-60.9522734066326,
-233.248170744692));
#223755=CARTESIAN_POINT('Ctrl Pts',(-16.1269910995712,-73.8030034797147,
-213.361373362703));
#223756=CARTESIAN_POINT('Ctrl Pts',(-14.9723529217116,-71.660011116557,
-216.668696986026));
#223757=CARTESIAN_POINT('Ctrl Pts',(-13.8225787733917,-69.5169021371276,
-219.977682732017));
#223758=CARTESIAN_POINT('Ctrl Pts',(-12.6830482858962,-67.3741700683409,
-223.290572851677));
#223759=CARTESIAN_POINT('Ctrl Pts',(-11.5435177984007,-65.2314379995542,
-226.603462971339));
#223760=CARTESIAN_POINT('Ctrl Pts',(-10.4133542530044,-63.0887592876544,
-229.919734283464));
#223761=CARTESIAN_POINT('Ctrl Pts',(-9.30823614726345,-60.9492817427492,
-233.247030907634));
#223762=CARTESIAN_POINT('Ctrl Pts',(-16.103019054535,-73.8005584760351,
-213.360877925168));
#223763=CARTESIAN_POINT('Ctrl Pts',(-14.9498889438717,-71.6574980953291,
-216.668148455574));
#223764=CARTESIAN_POINT('Ctrl Pts',(-13.80159836519,-69.5143192404771,-219.977068760275));
#223765=CARTESIAN_POINT('Ctrl Pts',(-12.6635007640913,-67.3715067403955,
-223.289863459617));
#223766=CARTESIAN_POINT('Ctrl Pts',(-11.5254031629927,-65.2286942403139,
-226.602658158959));
#223767=CARTESIAN_POINT('Ctrl Pts',(-10.3966247242771,-63.0859285253037,
-229.918808118652));
#223768=CARTESIAN_POINT('Ctrl Pts',(-9.29277587349895,-60.9463138180459,
-233.245897218204));
#223769=CARTESIAN_POINT('Ctrl Pts',(-16.0790434247684,-73.7981321994186,
-213.360384703604));
#223770=CARTESIAN_POINT('Ctrl Pts',(-14.9274215266728,-71.6550043474074,
-216.66760243706));
#223771=CARTESIAN_POINT('Ctrl Pts',(-13.7806147058298,-69.5117562048794,
-219.976457674749));
#223772=CARTESIAN_POINT('Ctrl Pts',(-12.643950246094,-67.3688640192604,
-223.28915752863));
#223773=CARTESIAN_POINT('Ctrl Pts',(-11.5072857863581,-65.2259718336413,
-226.601857382511));
#223774=CARTESIAN_POINT('Ctrl Pts',(-10.379892806367,-63.0831199759327,
-229.917886743822));
#223775=CARTESIAN_POINT('Ctrl Pts',(-9.27731352151551,-60.9433696029743,
-233.244769639116));
#223776=CARTESIAN_POINT('Ctrl Pts',(-16.0310921652353,-73.7932796461856,
-213.359398260476));
#223777=CARTESIAN_POINT('Ctrl Pts',(-14.8824866922748,-71.6500168515638,
-216.666510400032));
#223778=CARTESIAN_POINT('Ctrl Pts',(-13.7386473871094,-69.5066301336839,
-219.975235503696));
#223779=CARTESIAN_POINT('Ctrl Pts',(-12.6048492100992,-67.36357857699,-223.287745666656));
#223780=CARTESIAN_POINT('Ctrl Pts',(-11.471051033089,-65.220527020296,-226.600255829615));
#223781=CARTESIAN_POINT('Ctrl Pts',(-10.3464289705466,-63.0775028771908,
-229.916043994163));
#223782=CARTESIAN_POINT('Ctrl Pts',(-9.24638881754862,-60.9374811728312,
-233.242514480938));
#223783=CARTESIAN_POINT('Ctrl Pts',(-15.9831265667899,-73.7885020011607,
-213.358420681147));
#223784=CARTESIAN_POINT('Ctrl Pts',(-14.8375381004534,-71.6451064488818,
-216.665428410643));
#223785=CARTESIAN_POINT('Ctrl Pts',(-13.6966670637724,-69.5015835066084,
-219.974024877362));
#223786=CARTESIAN_POINT('Ctrl Pts',(-12.565736189382,-67.3583755618043,
-223.286347648786));
#223787=CARTESIAN_POINT('Ctrl Pts',(-11.4348053149916,-65.2151676170003,
-226.598670420209));
#223788=CARTESIAN_POINT('Ctrl Pts',(-10.3129555781029,-63.0719746300436,
-229.914220404117));
#223789=CARTESIAN_POINT('Ctrl Pts',(-9.21545580106647,-60.9316875806773,
-233.24028376377));
#223790=CARTESIAN_POINT('Ctrl Pts',(-15.9351468463194,-73.7837993408402,
-213.357451906235));
#223791=CARTESIAN_POINT('Ctrl Pts',(-14.7925760080749,-71.6402731942684,
-216.664356393475));
#223792=CARTESIAN_POINT('Ctrl Pts',(-13.6546740285727,-69.496616353084,
-219.972825698813));
#223793=CARTESIAN_POINT('Ctrl Pts',(-12.5266115102174,-67.3532549610625,
-223.284963342766));
#223794=CARTESIAN_POINT('Ctrl Pts',(-11.3985489918621,-65.209893569041,
-226.597100986719));
#223795=CARTESIAN_POINT('Ctrl Pts',(-10.2794730121742,-63.066535124477,
-229.912415755275));
#223796=CARTESIAN_POINT('Ctrl Pts',(-9.18451492026534,-60.9259885966326,
-233.238077193559));
#223797=CARTESIAN_POINT('Ctrl Pts',(-15.1674713187905,-73.7085567757124,
-213.341951507641));
#223798=CARTESIAN_POINT('Ctrl Pts',(-14.0731825300186,-71.5629411204543,
-216.64720411878));
#223799=CARTESIAN_POINT('Ctrl Pts',(-12.9827854653765,-69.4171418966931,
-219.953638842029));
#223800=CARTESIAN_POINT('Ctrl Pts',(-11.9006166435836,-67.2713253491929,
-223.262814446454));
#223801=CARTESIAN_POINT('Ctrl Pts',(-10.8184478217907,-65.1255088016927,
-226.571990050878));
#223802=CARTESIAN_POINT('Ctrl Pts',(-9.74375195731604,-62.9795030354101,
-229.88354137378));
#223803=CARTESIAN_POINT('Ctrl Pts',(-8.68946082744711,-60.8348048519179,
-233.202772070185));
#223804=CARTESIAN_POINT('Ctrl Pts',(-14.3961811415349,-73.6525070500062,
-213.328697733291));
#223805=CARTESIAN_POINT('Ctrl Pts',(-13.3503336845521,-71.5053542835831,
-216.632595555745));
#223806=CARTESIAN_POINT('Ctrl Pts',(-12.3076436285635,-69.3580059281157,
-219.937370861218));
#223807=CARTESIAN_POINT('Ctrl Pts',(-11.2716399932958,-67.2104822157957,
-223.24415985318));
#223808=CARTESIAN_POINT('Ctrl Pts',(-10.2356363580282,-65.0629585034757,
-226.550948845142));
#223809=CARTESIAN_POINT('Ctrl Pts',(-9.20568876581819,-62.9151648957076,
-229.859489304317));
#223810=CARTESIAN_POINT('Ctrl Pts',(-8.19241564950965,-60.7677996422107,
-233.173615252749));
#223811=CARTESIAN_POINT('Ctrl Pts',(-13.6221605046832,-73.6159852550019,
-213.31749452838));
#223812=CARTESIAN_POINT('Ctrl Pts',(-12.6250760081642,-71.4677688674574,
-216.620281085237));
#223813=CARTESIAN_POINT('Ctrl Pts',(-11.6304405856088,-69.3193741723362,
-219.923700795082));
#223814=CARTESIAN_POINT('Ctrl Pts',(-10.640997887323,-67.1707515656038,
-223.228560662602));
#223815=CARTESIAN_POINT('Ctrl Pts',(-9.65155518903714,-65.0221289588714,
-226.533420530121));
#223816=CARTESIAN_POINT('Ctrl Pts',(-8.66680721407077,-62.8732305917486,
-229.839537084505));
#223817=CARTESIAN_POINT('Ctrl Pts',(-7.69505740665787,-60.7243047821025,
-233.149611908546));
#223818=CARTESIAN_POINT('Ctrl Pts',(-12.07411923098,-73.5429416649933,-213.295088118557));
#223819=CARTESIAN_POINT('Ctrl Pts',(-11.1745606553882,-71.392598035206,
-216.595652144222));
#223820=CARTESIAN_POINT('Ctrl Pts',(-10.2760344996993,-69.2421106607772,
-219.89636066281));
#223821=CARTESIAN_POINT('Ctrl Pts',(-9.37971367537722,-67.09129026522,-223.197362281445));
#223822=CARTESIAN_POINT('Ctrl Pts',(-8.48339285105508,-64.9404698696628,
-226.498363900081));
#223823=CARTESIAN_POINT('Ctrl Pts',(-7.58904411057593,-62.7893619838305,
-229.79963264488));
#223824=CARTESIAN_POINT('Ctrl Pts',(-6.70034092095431,-60.6373150618862,
-233.101605220139));
#223825=CARTESIAN_POINT('Ctrl Pts',(-10.5152913094354,-73.5480397670874,
-213.280876146804));
#223826=CARTESIAN_POINT('Ctrl Pts',(-9.71465477633019,-71.3974778260467,
-216.58020457724));
#223827=CARTESIAN_POINT('Ctrl Pts',(-8.91375512880964,-69.2469206315281,
-219.879431150906));
#223828=CARTESIAN_POINT('Ctrl Pts',(-8.11230379659613,-67.0963349552283,
-223.178417000718));
#223829=CARTESIAN_POINT('Ctrl Pts',(-7.31085246438261,-64.9457492789285,
-226.47740285053));
#223830=CARTESIAN_POINT('Ctrl Pts',(-6.50890496550992,-62.7951562480888,
-229.776184191023));
#223831=CARTESIAN_POINT('Ctrl Pts',(-5.70557348161402,-60.6443501137825,
-233.074265786289));
#223832=CARTESIAN_POINT('Ctrl Pts',(-8.95359233126488,-73.6335280557816,
-213.274065021079));
#223833=CARTESIAN_POINT('Ctrl Pts',(-8.25459642710867,-71.4837698867061,
-216.57292704644));
#223834=CARTESIAN_POINT('Ctrl Pts',(-7.5540771905589,-69.3342366336724,
-219.871616502806));
#223835=CARTESIAN_POINT('Ctrl Pts',(-6.8502996103062,-67.185240788125,-223.169973551181));
#223836=CARTESIAN_POINT('Ctrl Pts',(-6.1465220300535,-65.0362449425776,
-226.468330599556));
#223837=CARTESIAN_POINT('Ctrl Pts',(-5.43981664545391,-62.8877051452245,
-229.766371465045));
#223838=CARTESIAN_POINT('Ctrl Pts',(-4.72482964674679,-60.740737267561,
-233.063701736715));
#223839=CARTESIAN_POINT('Ctrl Pts',(-8.1727428421796,-73.6762722001287,
-213.270659458216));
#223840=CARTESIAN_POINT('Ctrl Pts',(-7.52456725249791,-71.5269159170358,
-216.569288281039));
#223841=CARTESIAN_POINT('Ctrl Pts',(-6.87423822143353,-69.3778946347445,
-219.867709178756));
#223842=CARTESIAN_POINT('Ctrl Pts',(-6.21929751716124,-67.2296937045733,
-223.165751826413));
#223843=CARTESIAN_POINT('Ctrl Pts',(-5.56435681288895,-65.0814927744022,
-226.463794474069));
#223844=CARTESIAN_POINT('Ctrl Pts',(-4.90527248542591,-62.9339795937923,
-229.761465102056));
#223845=CARTESIAN_POINT('Ctrl Pts',(-4.23445772931318,-60.7889308444503,
-233.058419711927));
#223846=CARTESIAN_POINT('Ctrl Pts',(-7.39116334463378,-73.7391136679641,
-213.269118043698));
#223847=CARTESIAN_POINT('Ctrl Pts',(-6.79447747105095,-71.5904135964271,
-216.567708642569));
#223848=CARTESIAN_POINT('Ctrl Pts',(-6.19501537235948,-69.4421777820088,
-219.866101050477));
#223849=CARTESIAN_POINT('Ctrl Pts',(-5.5895961783157,-67.2951158690107,
-223.164183697639));
#223850=CARTESIAN_POINT('Ctrl Pts',(-4.98417698427192,-65.1480539560125,
-226.462266344801));
#223851=CARTESIAN_POINT('Ctrl Pts',(-4.37340476876875,-63.0019608814007,
-229.760014474659));
#223852=CARTESIAN_POINT('Ctrl Pts',(-3.74746533531928,-60.8595124428614,
-233.057401329873));
#223853=CARTESIAN_POINT('Ctrl Pts',(-6.60994240840707,-73.8222558927847,
-213.269427912899));
#223854=CARTESIAN_POINT('Ctrl Pts',(-6.06557267238966,-71.6743247983103,
-216.568167153263));
#223855=CARTESIAN_POINT('Ctrl Pts',(-5.51780600976748,-69.5270045782123,
-219.866761419183));
#223856=CARTESIAN_POINT('Ctrl Pts',(-4.96273068554881,-67.3812822930865,
-223.165228588343));
#223857=CARTESIAN_POINT('Ctrl Pts',(-4.40765536133015,-65.2355600079607,
-226.463695757503));
#223858=CARTESIAN_POINT('Ctrl Pts',(-3.84600674946129,-63.0911343879048,
-229.761957061969));
#223859=CARTESIAN_POINT('Ctrl Pts',(-3.2657468262204,-60.9518397874746,
-233.060586757597));
#223860=CARTESIAN_POINT('Ctrl Pts',(-6.21933194029372,-73.863827005195,
-213.2695828475));
#223861=CARTESIAN_POINT('Ctrl Pts',(-5.70112027305902,-71.7162803992519,
-216.568396408611));
#223862=CARTESIAN_POINT('Ctrl Pts',(-5.17920132847148,-69.569417976314,
-219.867091603535));
#223863=CARTESIAN_POINT('Ctrl Pts',(-4.64929793916537,-67.4243655051244,
-223.165751033694));
#223864=CARTESIAN_POINT('Ctrl Pts',(-4.11939454985925,-65.2793130339348,
-226.464410463854));
#223865=CARTESIAN_POINT('Ctrl Pts',(-3.58230773980756,-63.1357211411568,
-229.762928355624));
#223866=CARTESIAN_POINT('Ctrl Pts',(-3.02488757167096,-60.9980034597812,
-233.062179471459));
#223867=CARTESIAN_POINT('Ctrl Pts',(-5.82880537803933,-73.9104727623473,
-213.27020061172));
#223868=CARTESIAN_POINT('Ctrl Pts',(-5.33695524072191,-71.7633387196078,
-216.56913509822));
#223869=CARTESIAN_POINT('Ctrl Pts',(-4.84108747043389,-69.6169666428243,
-219.86798871271));
#223870=CARTESIAN_POINT('Ctrl Pts',(-4.33655677660738,-67.4726345985374,
-223.16692657622));
#223871=CARTESIAN_POINT('Ctrl Pts',(-3.83202608278088,-65.3283025542505,
-226.465864439729));
#223872=CARTESIAN_POINT('Ctrl Pts',(-3.31969806921586,-63.1856069990699,
-229.764747958359));
#223873=CARTESIAN_POINT('Ctrl Pts',(-2.78530983748405,-61.0496071561033,
-233.064823984859));
#223874=CARTESIAN_POINT('Ctrl Pts',(-5.43848674342394,-73.9622193313154,
-213.27128471988));
#223875=CARTESIAN_POINT('Ctrl Pts',(-4.97321480130516,-71.8155087180245,
-216.570386574246));
#223876=CARTESIAN_POINT('Ctrl Pts',(-4.50361309768486,-69.6696426023929,
-219.869456114948));
#223877=CARTESIAN_POINT('Ctrl Pts',(-4.02466312854686,-67.526066627963,
-223.168760046202));
#223878=CARTESIAN_POINT('Ctrl Pts',(-3.54571315940887,-65.3824906535331,
-226.468063977456));
#223879=CARTESIAN_POINT('Ctrl Pts',(-3.05834355347626,-63.2407400353646,
-229.767424405843));
#223880=CARTESIAN_POINT('Ctrl Pts',(-2.54717478765636,-61.1065960304884,
-233.06853892423));
#223881=CARTESIAN_POINT('Ctrl Pts',(-5.4262892860922,-73.9638364115957,
-213.27131859826));
#223882=CARTESIAN_POINT('Ctrl Pts',(-4.96184791257339,-71.817139030475,
-216.570425682871));
#223883=CARTESIAN_POINT('Ctrl Pts',(-4.49306702353645,-69.6712887261295,
-219.869501971269));
#223884=CARTESIAN_POINT('Ctrl Pts',(-4.01491645204497,-67.5277363788826,
-223.168817342139));
#223885=CARTESIAN_POINT('Ctrl Pts',(-3.53676588055349,-65.3841840316357,
-226.468132713009));
#223886=CARTESIAN_POINT('Ctrl Pts',(-3.0501762248594,-63.2424629427488,
-229.767508044828));
#223887=CARTESIAN_POINT('Ctrl Pts',(-2.53973306734924,-61.1083769328129,
-233.068655016085));
#223888=CARTESIAN_POINT('Ctrl Pts',(-5.41409203184723,-73.9654584732471,
-213.271352932467));
#223889=CARTESIAN_POINT('Ctrl Pts',(-4.95048143852496,-71.8187743349515,
-216.570465292767));
#223890=CARTESIAN_POINT('Ctrl Pts',(-4.48252157393744,-69.6729398572013,
-219.869548385134));
#223891=CARTESIAN_POINT('Ctrl Pts',(-4.00517060326625,-67.5294111720907,
-223.168875281415));
#223892=CARTESIAN_POINT('Ctrl Pts',(-3.52781963259506,-65.3858824869801,
-226.468202177696));
#223893=CARTESIAN_POINT('Ctrl Pts',(-3.04201012206819,-63.2441909750325,
-229.767592521906));
#223894=CARTESIAN_POINT('Ctrl Pts',(-2.53229275617624,-61.1101630954175,
-233.068772155269));
#223895=CARTESIAN_POINT('Ctrl Pts',(-5.40189498448029,-73.9670855170893,
-213.27138772269));
#223896=CARTESIAN_POINT('Ctrl Pts',(-4.93911538335592,-71.8204146317568,
-216.570505404131));
#223897=CARTESIAN_POINT('Ctrl Pts',(-4.47197675343487,-69.6745959954063,
-219.869595356765));
#223898=CARTESIAN_POINT('Ctrl Pts',(-3.99542558698367,-67.5310910069568,
-223.168933864337));
#223899=CARTESIAN_POINT('Ctrl Pts',(-3.51887442053248,-65.3875860185073,
-226.468272371909));
#223900=CARTESIAN_POINT('Ctrl Pts',(-3.03384525018033,-63.2459241307671,
-229.767677837598));
#223901=CARTESIAN_POINT('Ctrl Pts',(-2.52485385910942,-61.1119545168846,
-233.068890342738));
#223902=CARTESIAN_POINT('Ctrl Pts',(-5.38969793711334,-73.9687125609316,
-213.271422512912));
#223903=CARTESIAN_POINT('Ctrl Pts',(-4.92774932818688,-71.8220549285621,
-216.570545515496));
#223904=CARTESIAN_POINT('Ctrl Pts',(-4.4614319329323,-69.6762521336113,
-219.869642328397));
#223905=CARTESIAN_POINT('Ctrl Pts',(-3.9856805707011,-67.5327708418229,
-223.16899244726));
#223906=CARTESIAN_POINT('Ctrl Pts',(-3.5099292084699,-65.3892895500345,
-226.468342566123));
#223907=CARTESIAN_POINT('Ctrl Pts',(-3.02568037829247,-63.2476572865017,
-229.767763153291));
#223908=CARTESIAN_POINT('Ctrl Pts',(-2.51741496204259,-61.1137459383516,
-233.069008530206));
#223909=CARTESIAN_POINT('Ctrl Pts',(-5.37672637028157,-73.9704678685259,
-213.271433929509));
#223910=CARTESIAN_POINT('Ctrl Pts',(-4.9155433526131,-71.8238395746452,
-216.570564049875));
#223911=CARTESIAN_POINT('Ctrl Pts',(-4.44996909929499,-69.6780729754426,
-219.869670623327));
#223912=CARTESIAN_POINT('Ctrl Pts',(-3.97491462260742,-67.5346472458208,
-223.169039474058));
#223913=CARTESIAN_POINT('Ctrl Pts',(-3.49986014591986,-65.3912215161989,
-226.468408324789));
#223914=CARTESIAN_POINT('Ctrl Pts',(-3.01626470944041,-63.2496602746465,
-229.767854189359));
#223915=CARTESIAN_POINT('Ctrl Pts',(-2.50854660210467,-61.1158851609529,
-233.069159596983));
#223916=CARTESIAN_POINT('Ctrl Pts',(-5.36570279694763,-73.9719187759859,
-213.271505747073));
#223917=CARTESIAN_POINT('Ctrl Pts',(-4.90545050752033,-71.8252794240533,
-216.570638631499));
#223918=CARTESIAN_POINT('Ctrl Pts',(-4.44081643235981,-69.6794979085229,
-219.869747875903));
#223919=CARTESIAN_POINT('Ctrl Pts',(-3.96671825976106,-67.536047760413,
-223.169117864674));
#223920=CARTESIAN_POINT('Ctrl Pts',(-3.49262008716231,-65.3925976123031,
-226.468487853445));
#223921=CARTESIAN_POINT('Ctrl Pts',(-3.00999783445047,-63.2510034927325,
-229.767933853275));
#223922=CARTESIAN_POINT('Ctrl Pts',(-2.50327678459181,-61.1171690939225,
-233.069231764379));
#223923=CARTESIAN_POINT('Ctrl Pts',(-5.34365565027976,-73.9748205909058,
-213.271649382202));
#223924=CARTESIAN_POINT('Ctrl Pts',(-4.88526481733479,-71.8281591228697,
-216.570787794748));
#223925=CARTESIAN_POINT('Ctrl Pts',(-4.42251109848946,-69.6823477746836,
-219.869902381056));
#223926=CARTESIAN_POINT('Ctrl Pts',(-3.95032553406833,-67.5388487895975,
-223.169274645906));
#223927=CARTESIAN_POINT('Ctrl Pts',(-3.4781399696472,-65.3953498045114,
-226.468646910757));
#223928=CARTESIAN_POINT('Ctrl Pts',(-2.99746408447056,-63.2536899289045,
-229.768093181107));
#223929=CARTESIAN_POINT('Ctrl Pts',(-2.4927371495661,-61.1197369598615,
-233.069376099171));
#223930=CARTESIAN_POINT('Ctrl Pts',(-5.32159500200748,-73.9777056883786,
-213.271792108186));
#223931=CARTESIAN_POINT('Ctrl Pts',(-4.86506777599914,-71.8310217620559,
-216.570936017706));
#223932=CARTESIAN_POINT('Ctrl Pts',(-4.40419656758946,-69.6851802994998,
-219.870055928012));
#223933=CARTESIAN_POINT('Ctrl Pts',(-3.93392595850568,-67.5416322892271,
-223.16943049385));
#223934=CARTESIAN_POINT('Ctrl Pts',(-3.4636553494219,-65.3980842789543,
-226.468805059689));
#223935=CARTESIAN_POINT('Ctrl Pts',(-2.98492828270904,-63.2563585875261,
-229.76825167595));
#223936=CARTESIAN_POINT('Ctrl Pts',(-2.48219900959581,-61.1222869643936,
-233.069519750154));
#223937=CARTESIAN_POINT('Ctrl Pts',(-5.29952110564376,-73.9805739848368,
-213.271933926145));
#223938=CARTESIAN_POINT('Ctrl Pts',(-4.84485958837554,-71.833867280769,
-216.571083300788));
#223939=CARTESIAN_POINT('Ctrl Pts',(-4.38587299316779,-69.6879954448049,
-219.870208515872));
#223940=CARTESIAN_POINT('Ctrl Pts',(-3.91751962681961,-67.5443982464756,
-223.169585405614));
#223941=CARTESIAN_POINT('Ctrl Pts',(-3.44916626047143,-65.4008010481464,
-226.468962295357));
#223942=CARTESIAN_POINT('Ctrl Pts',(-2.97239039461706,-63.2590095074215,
-229.768409329534));
#223943=CARTESIAN_POINT('Ctrl Pts',(-2.47166224167208,-61.1248191908138,
-233.069662708859));
#223944=CARTESIAN_POINT('Ctrl Pts',(-5.25537331291633,-73.9863105777533,
-213.272217562064));
#223945=CARTESIAN_POINT('Ctrl Pts',(-4.80444321312832,-71.8395583181952,
-216.571377866951));
#223946=CARTESIAN_POINT('Ctrl Pts',(-4.34922584432445,-69.693625735415,
-219.870513691592));
#223947=CARTESIAN_POINT('Ctrl Pts',(-3.88470696344747,-67.5499301609728,
-223.169895229143));
#223948=CARTESIAN_POINT('Ctrl Pts',(-3.42018808257049,-65.4062345865307,
-226.469276766693));
#223949=CARTESIAN_POINT('Ctrl Pts',(-2.9473146184331,-63.2643113472122,
-229.768724636701));
#223950=CARTESIAN_POINT('Ctrl Pts',(-2.45058870582462,-61.1298836436543,
-233.069948626269));
#223951=CARTESIAN_POINT('Ctrl Pts',(-5.21117252788928,-73.9919799664689,
-213.272497565759));
#223952=CARTESIAN_POINT('Ctrl Pts',(-4.7639822528083,-71.8451808736014,
-216.57166867345));
#223953=CARTESIAN_POINT('Ctrl Pts',(-4.3125425214412,-69.699186507887,-219.870815030722));
#223954=CARTESIAN_POINT('Ctrl Pts',(-3.85186727558167,-67.5553919059884,
-223.170201307704));
#223955=CARTESIAN_POINT('Ctrl Pts',(-3.39119202972214,-65.4115973040898,
-226.469587584685));
#223956=CARTESIAN_POINT('Ctrl Pts',(-2.92223049669452,-63.2695422325334,
-229.769036578502));
#223957=CARTESIAN_POINT('Ctrl Pts',(-2.42952065843729,-61.1348769849848,
-233.070231774323));
#223958=CARTESIAN_POINT('Ctrl Pts',(-5.16692077781557,-73.9975814841632,
-213.272773947677));
#223959=CARTESIAN_POINT('Ctrl Pts',(-4.72347834531912,-71.8507344617868,
-216.57195572551));
#223960=CARTESIAN_POINT('Ctrl Pts',(-4.27582425199423,-69.7046774580107,
-219.871112528569));
#223961=CARTESIAN_POINT('Ctrl Pts',(-3.81900131317034,-67.5607833783998,
-223.170503621156));
#223962=CARTESIAN_POINT('Ctrl Pts',(-3.36217837434646,-65.4168892987889,
-226.469894713743));
#223963=CARTESIAN_POINT('Ctrl Pts',(-2.89713775575502,-63.2747024686849,
-229.769345092714));
#223964=CARTESIAN_POINT('Ctrl Pts',(-2.40845711188386,-61.1397998699931,
-233.070512088159));
#223965=CARTESIAN_POINT('Ctrl Pts',(-5.07841727766817,-74.0087845195517,
-213.273326711516));
#223966=CARTESIAN_POINT('Ctrl Pts',(-4.64247053034076,-71.8618416381575,
-216.572529829629));
#223967=CARTESIAN_POINT('Ctrl Pts',(-4.2023877131003,-69.715659358258,-219.871707524263));
#223968=CARTESIAN_POINT('Ctrl Pts',(-3.7532693883477,-67.5715663232226,
-223.171108248061));
#223969=CARTESIAN_POINT('Ctrl Pts',(-3.30415106359509,-65.4274732881873,
-226.470508971858));
#223970=CARTESIAN_POINT('Ctrl Pts',(-2.84695227387601,-63.285022940988,
-229.769962121139));
#223971=CARTESIAN_POINT('Ctrl Pts',(-2.366330018777,-61.1496456400098,-233.07107271583));
#223972=CARTESIAN_POINT('Ctrl Pts',(-4.98970991817215,-74.0197160685976,
-213.273864986293));
#223973=CARTESIAN_POINT('Ctrl Pts',(-4.56129092778213,-71.8726729436333,
-216.573088913503));
#223974=CARTESIAN_POINT('Ctrl Pts',(-4.12881138864584,-69.7263619676298,
-219.872287151588));
#223975=CARTESIAN_POINT('Ctrl Pts',(-3.68743236529496,-67.5820681782785,
-223.171697810615));
#223976=CARTESIAN_POINT('Ctrl Pts',(-3.24605334194409,-65.4377743889271,
-226.471108469642));
#223977=CARTESIAN_POINT('Ctrl Pts',(-2.79673231139314,-63.2950608232797,
-229.770565433851));
#223978=CARTESIAN_POINT('Ctrl Pts',(-2.32422093228867,-61.1592096000228,
-233.071622002575));
#223979=CARTESIAN_POINT('Ctrl Pts',(-4.90081490576138,-74.0303708240067,
-213.274388879266));
#223980=CARTESIAN_POINT('Ctrl Pts',(-4.47995262653692,-71.8832245209659,
-216.573633049045));
#223981=CARTESIAN_POINT('Ctrl Pts',(-4.05510508965952,-69.7367828703165,
-219.872851412303));
#223982=CARTESIAN_POINT('Ctrl Pts',(-3.62149624377294,-67.5922881106059,
-223.172272195036));
#223983=CARTESIAN_POINT('Ctrl Pts',(-3.18788739788636,-65.4477933508953,
-226.471692977771));
#223984=CARTESIAN_POINT('Ctrl Pts',(-2.74647572406062,-63.3048184758955,
-229.77115459683));
#223985=CARTESIAN_POINT('Ctrl Pts',(-2.28212190434125,-61.1684968100619,
-233.072159477025));
#223986=CARTESIAN_POINT('Ctrl Pts',(-4.72302488093985,-74.051680334825,
-213.275436665212));
#223987=CARTESIAN_POINT('Ctrl Pts',(-4.3172760240465,-71.904327675631,-216.574721320128));
#223988=CARTESIAN_POINT('Ctrl Pts',(-3.90769249168688,-69.7576246756899,
-219.873979933731));
#223989=CARTESIAN_POINT('Ctrl Pts',(-3.48962400072889,-67.6127279752608,
-223.17342096388));
#223990=CARTESIAN_POINT('Ctrl Pts',(-3.0715555097709,-65.4678312748317,
-226.472861994029));
#223991=CARTESIAN_POINT('Ctrl Pts',(-2.64596254939558,-63.3243337811273,
-229.772332922788));
#223992=CARTESIAN_POINT('Ctrl Pts',(-2.19792384844641,-61.18707123014,-233.073234425924));
#223993=CARTESIAN_POINT('Ctrl Pts',(-4.54448425091446,-74.071882635413,
-213.276426893072));
#223994=CARTESIAN_POINT('Ctrl Pts',(-4.15396463899018,-71.9243118863183,
-216.57574975929));
#223995=CARTESIAN_POINT('Ctrl Pts',(-3.75976000462968,-69.7773396309741,
-219.87504693894));
#223996=CARTESIAN_POINT('Ctrl Pts',(-3.35735536122353,-67.6320401585041,
-223.174508959174));
#223997=CARTESIAN_POINT('Ctrl Pts',(-2.95495071781737,-65.486740686034,
-226.47397097941));
#223998=CARTESIAN_POINT('Ctrl Pts',(-2.54530281321105,-63.3427282647259,
-229.773454562434));
#223999=CARTESIAN_POINT('Ctrl Pts',(-2.11376604236526,-61.2045389007808,
-233.074262056417));
#224000=CARTESIAN_POINT('Ctrl Pts',(-4.36532254289751,-74.090935698542,
-213.277360794546));
#224001=CARTESIAN_POINT('Ctrl Pts',(-3.99012300028631,-71.9431466770906,
-216.576719412775));
#224002=CARTESIAN_POINT('Ctrl Pts',(-3.61138599425699,-69.7959086923527,
-219.876053052738));
#224003=CARTESIAN_POINT('Ctrl Pts',(-3.22473834211198,-67.6502178766122,
-223.175536013948));
#224004=CARTESIAN_POINT('Ctrl Pts',(-2.83809068996697,-65.5045270608717,
-226.475018975158));
#224005=CARTESIAN_POINT('Ctrl Pts',(-2.44448009833563,-63.3600195797742,
-229.774517081184));
#224006=CARTESIAN_POINT('Ctrl Pts',(-2.02958446470485,-61.2209373357876,
-233.075239398162));
#224007=CARTESIAN_POINT('Ctrl Pts',(-3.64867571082973,-74.1671479510582,
-213.281096400445));
#224008=CARTESIAN_POINT('Ctrl Pts',(-3.33475644547083,-72.0184858401796,
-216.580598026715));
#224009=CARTESIAN_POINT('Ctrl Pts',(-3.01788995276623,-69.8701849378668,
-219.880077507931));
#224010=CARTESIAN_POINT('Ctrl Pts',(-2.69427026566578,-67.7229287490447,
-223.179644233041));
#224011=CARTESIAN_POINT('Ctrl Pts',(-2.37065057856533,-65.5756725602225,
-226.479210958151));
#224012=CARTESIAN_POINT('Ctrl Pts',(-2.04118923883392,-63.4291848399676,
-229.778767156183));
#224013=CARTESIAN_POINT('Ctrl Pts',(-1.69285815406323,-61.2865310758151,
-233.079148765145));
#224014=CARTESIAN_POINT('Ctrl Pts',(-2.92179171700349,-74.2248568155794,
-213.283931439761));
#224015=CARTESIAN_POINT('Ctrl Pts',(-2.67067383150201,-72.0753567042848,
-216.583539105332));
#224016=CARTESIAN_POINT('Ctrl Pts',(-2.4171737530214,-69.9260843575689,
-219.883132378737));
#224017=CARTESIAN_POINT('Ctrl Pts',(-2.15816590409808,-67.7774746840945,
-223.182780825433));
#224018=CARTESIAN_POINT('Ctrl Pts',(-1.89915805517477,-65.6288650106202,
-226.48242927213));
#224019=CARTESIAN_POINT('Ctrl Pts',(-1.6354272504708,-63.4807382255424,
-229.782069599427));
#224020=CARTESIAN_POINT('Ctrl Pts',(-1.35605364503039,-61.3350668114237,
-233.08223904777));
#224021=CARTESIAN_POINT('Ctrl Pts',(-2.19241710279808,-74.2625655408562,
-213.285868033891));
#224022=CARTESIAN_POINT('Ctrl Pts',(-2.00425439386506,-72.1126446956918,
-216.585548495067));
#224023=CARTESIAN_POINT('Ctrl Pts',(-1.81427677031869,-69.9628615488284,
-219.885219900497));
#224024=CARTESIAN_POINT('Ctrl Pts',(-1.62009069259905,-67.8134811173994,
-223.184924670423));
#224025=CARTESIAN_POINT('Ctrl Pts',(-1.4259046148794,-65.6641006859703,
-226.484629440349));
#224026=CARTESIAN_POINT('Ctrl Pts',(-1.22812047595596,-63.5150120219902,
-229.784328496798));
#224027=CARTESIAN_POINT('Ctrl Pts',(-1.01831914241026,-61.36742518831,-233.084352143351));
#224028=CARTESIAN_POINT('Ctrl Pts',(-1.46304248859267,-74.3002742661329,
-213.287804628021));
#224029=CARTESIAN_POINT('Ctrl Pts',(-1.3378349562281,-72.1499326870988,
-216.587557884803));
#224030=CARTESIAN_POINT('Ctrl Pts',(-1.21137978761598,-69.999638740088,
-219.887307422256));
#224031=CARTESIAN_POINT('Ctrl Pts',(-1.08201548110001,-67.8494875507042,
-223.187068515412));
#224032=CARTESIAN_POINT('Ctrl Pts',(-0.952651174584045,-65.6993363613204,
-226.486829608568));
#224033=CARTESIAN_POINT('Ctrl Pts',(-0.820813701441127,-63.5492858184379,
-229.786587394169));
#224034=CARTESIAN_POINT('Ctrl Pts',(-0.680584639790125,-61.3997835651962,
-233.086465238933));
#224035=CARTESIAN_POINT('Ctrl Pts',(-0.731897203934337,-74.3172201941713,
-213.288876053933));
#224036=CARTESIAN_POINT('Ctrl Pts',(-0.669711243166844,-72.1670055479396,
-216.588673926417));
#224037=CARTESIAN_POINT('Ctrl Pts',(-0.606834169240839,-70.016790901708,
-219.888471798901));
#224038=CARTESIAN_POINT('Ctrl Pts',(-0.542375109003111,-67.8665762554763,
-223.188269671383));
#224039=CARTESIAN_POINT('Ctrl Pts',(-0.477916048765383,-65.7163616092447,
-226.488067543867));
#224040=CARTESIAN_POINT('Ctrl Pts',(-0.412094305693277,-63.566146963013,
-229.787865416351));
#224041=CARTESIAN_POINT('Ctrl Pts',(-0.341829933578211,-61.4159323167813,
-233.087663288834));
#224042=CARTESIAN_POINT('Ctrl Pts',(-6.84354621607228E-13,-74.3172201941715,
-213.288876053933));
#224043=CARTESIAN_POINT('Ctrl Pts',(-1.42776780017916E-12,-72.1670055479398,
-216.588673926417));
#224044=CARTESIAN_POINT('Ctrl Pts',(-2.08399076963921E-12,-70.0167909017082,
-219.8884717989));
#224045=CARTESIAN_POINT('Ctrl Pts',(-2.80926784707921E-12,-67.8665762554765,
-223.188269671383));
#224046=CARTESIAN_POINT('Ctrl Pts',(-3.53454492451921E-12,-65.7163616092449,
-226.488067543867));
#224047=CARTESIAN_POINT('Ctrl Pts',(-4.11012448022973E-12,-63.5661469630132,
-229.787865416351));
#224048=CARTESIAN_POINT('Ctrl Pts',(-4.66308425881617E-12,-61.4159323167815,
-233.087663288834));
#224049=CARTESIAN_POINT('Ctrl Pts',(0.731897203932968,-74.3172201941717,
-213.288876053933));
#224050=CARTESIAN_POINT('Ctrl Pts',(0.669711243163988,-72.16700554794,-216.588673926417));
#224051=CARTESIAN_POINT('Ctrl Pts',(0.606834169236671,-70.0167909017083,
-219.8884717989));
#224052=CARTESIAN_POINT('Ctrl Pts',(0.542375108997492,-67.8665762554767,
-223.188269671383));
#224053=CARTESIAN_POINT('Ctrl Pts',(0.477916048758314,-65.716361609245,
-226.488067543867));
#224054=CARTESIAN_POINT('Ctrl Pts',(0.412094305685056,-63.5661469630133,
-229.787865416351));
#224055=CARTESIAN_POINT('Ctrl Pts',(0.341829933568885,-61.4159323167817,
-233.087663288834));
#224056=CARTESIAN_POINT('Ctrl Pts',(1.4630412071525,-74.3002743777528,-213.287804633297));
#224057=CARTESIAN_POINT('Ctrl Pts',(1.33783407544282,-72.1499327874783,
-216.587557889776));
#224058=CARTESIAN_POINT('Ctrl Pts',(1.2113792856225,-69.9996388304174,-219.887307427019));
#224059=CARTESIAN_POINT('Ctrl Pts',(1.08201528753655,-67.8494876362415,
-223.187068521293));
#224060=CARTESIAN_POINT('Ctrl Pts',(0.952651289450599,-65.6993364420655,
-226.486829615567));
#224061=CARTESIAN_POINT('Ctrl Pts',(0.820814077178737,-63.5492858967185,
-229.786587402353));
#224062=CARTESIAN_POINT('Ctrl Pts',(0.680584991670135,-61.3997836690735,
-233.086465258331));
#224063=CARTESIAN_POINT('Ctrl Pts',(2.19241535457815,-74.2625656556727,
-213.285868034929));
#224064=CARTESIAN_POINT('Ctrl Pts',(2.00425272002901,-72.1126448113594,
-216.585548496058));
#224065=CARTESIAN_POINT('Ctrl Pts',(1.81427515642486,-69.96286166618,-219.885219901252));
#224066=CARTESIAN_POINT('Ctrl Pts',(1.62008907510343,-67.813481242547,-223.184924671597));
#224067=CARTESIAN_POINT('Ctrl Pts',(1.425902993782,-65.6641008189139,-226.484629441941));
#224068=CARTESIAN_POINT('Ctrl Pts',(1.2281188155361,-63.5150121637255,-229.784328497621));
#224069=CARTESIAN_POINT('Ctrl Pts',(1.01831713572084,-61.3674253807579,
-233.084352154385));
#224070=CARTESIAN_POINT('Ctrl Pts',(2.92178950200379,-74.2248569335925,
-213.28393143656));
#224071=CARTESIAN_POINT('Ctrl Pts',(2.6706713646152,-72.0753568352406,-216.583539102341));
#224072=CARTESIAN_POINT('Ctrl Pts',(2.41717102722723,-69.9260845019427,
-219.883132375486));
#224073=CARTESIAN_POINT('Ctrl Pts',(2.15816286267031,-67.7774748488525,
-223.182780821899));
#224074=CARTESIAN_POINT('Ctrl Pts',(1.8991546981134,-65.6288651957623,-226.482429268314));
#224075=CARTESIAN_POINT('Ctrl Pts',(1.63542355389346,-63.4807384307325,
-229.782069592889));
#224076=CARTESIAN_POINT('Ctrl Pts',(1.35604927977155,-61.3350670924422,
-233.082239050439));
#224077=CARTESIAN_POINT('Ctrl Pts',(3.64867763480066,-74.1671476563362,
-213.281096434137));
#224078=CARTESIAN_POINT('Ctrl Pts',(3.33475783198323,-72.0184856638598,
-216.580598059648));
#224079=CARTESIAN_POINT('Ctrl Pts',(3.01789082047128,-69.8701848769235,
-219.880077539642));
#224080=CARTESIAN_POINT('Ctrl Pts',(2.6942706773542,-67.7229287903462,-223.179644260014));
#224081=CARTESIAN_POINT('Ctrl Pts',(2.37065053423712,-65.5756727037689,
-226.479210980387));
#224082=CARTESIAN_POINT('Ctrl Pts',(2.04118878099155,-63.4291850796541,
-229.778767173092));
#224083=CARTESIAN_POINT('Ctrl Pts',(1.69285753982065,-61.2865313428857,
-233.079148752624));
#224084=CARTESIAN_POINT('Ctrl Pts',(4.36532376578682,-74.0909355242495,
-213.27736081295));
#224085=CARTESIAN_POINT('Ctrl Pts',(3.99012383085994,-71.9431465837745,
-216.576719427696));
#224086=CARTESIAN_POINT('Ctrl Pts',(3.61138642781057,-69.7959086820964,
-219.876053064671));
#224087=CARTESIAN_POINT('Ctrl Pts',(3.2247384017838,-67.6502179485229,-223.175536024031));
#224088=CARTESIAN_POINT('Ctrl Pts',(2.83809037575702,-65.5045272149494,
-226.47501898339));
#224089=CARTESIAN_POINT('Ctrl Pts',(2.44447941230847,-63.3600198215615,
-229.774517090706));
#224090=CARTESIAN_POINT('Ctrl Pts',(2.02958360100885,-61.2209376265333,
-233.07523940264));
#224091=CARTESIAN_POINT('Ctrl Pts',(4.54448529853335,-74.0718824912277,
-213.276426907653));
#224092=CARTESIAN_POINT('Ctrl Pts',(4.15396533057911,-71.9243118137532,
-216.575749769707));
#224093=CARTESIAN_POINT('Ctrl Pts',(3.75976032964539,-69.7773396333896,
-219.875046945928));
#224094=CARTESIAN_POINT('Ctrl Pts',(3.35735533289119,-67.632040238067,-223.174508965034));
#224095=CARTESIAN_POINT('Ctrl Pts',(2.95495033613699,-65.4867408427445,
-226.47397098414));
#224096=CARTESIAN_POINT('Ctrl Pts',(2.5453020701377,-63.3427285070384,-229.773454570109));
#224097=CARTESIAN_POINT('Ctrl Pts',(2.1137651163059,-61.2045391974451,-233.074262065144));
#224098=CARTESIAN_POINT('Ctrl Pts',(4.72302558275178,-74.0516802394771,
-213.275436674357));
#224099=CARTESIAN_POINT('Ctrl Pts',(4.31727644647028,-71.9043276347028,
-216.574721325169));
#224100=CARTESIAN_POINT('Ctrl Pts',(3.90769262251043,-69.7576246931073,
-219.873979935587));
#224101=CARTESIAN_POINT('Ctrl Pts',(3.48962384895622,-67.6127280546252,
-223.173420965523));
#224102=CARTESIAN_POINT('Ctrl Pts',(3.07155507540201,-65.4678314161431,
-226.472861995458));
#224103=CARTESIAN_POINT('Ctrl Pts',(2.64596182151007,-63.3243339939848,
-229.77233292858));
#224104=CARTESIAN_POINT('Ctrl Pts',(2.19792298970101,-61.1870714878141,
-233.073234436702));
#224105=CARTESIAN_POINT('Ctrl Pts',(4.90081532807169,-74.0303707671596,
-213.27438888447));
#224106=CARTESIAN_POINT('Ctrl Pts',(4.47995285021341,-71.8832245017814,
-216.573633050881));
#224107=CARTESIAN_POINT('Ctrl Pts',(4.05510510402121,-69.7367828923109,
-219.87285141164));
#224108=CARTESIAN_POINT('Ctrl Pts',(3.62149605519719,-67.5922881772786,
-223.172272194658));
#224109=CARTESIAN_POINT('Ctrl Pts',(3.18788700637317,-65.4477934622463,
-226.471692977676));
#224110=CARTESIAN_POINT('Ctrl Pts',(2.7464751198719,-63.3048186403858,-229.771154601106));
#224111=CARTESIAN_POINT('Ctrl Pts',(2.28212121845882,-61.1684970065069,
-233.072159487081));
#224112=CARTESIAN_POINT('Ctrl Pts',(4.98971020073165,-74.0197160310009,
-213.273864989526));
#224113=CARTESIAN_POINT('Ctrl Pts',(4.56129105208498,-71.8726729353207,
-216.573088913737));
#224114=CARTESIAN_POINT('Ctrl Pts',(4.1288113447766,-69.7263619919127,-219.872287149666));
#224115=CARTESIAN_POINT('Ctrl Pts',(3.68743215831767,-67.5820682386053,
-223.171697809226));
#224116=CARTESIAN_POINT('Ctrl Pts',(3.24605297185875,-65.4377744852979,
-226.471108468786));
#224117=CARTESIAN_POINT('Ctrl Pts',(2.79673176905281,-63.2950609635863,
-229.770565437369));
#224118=CARTESIAN_POINT('Ctrl Pts',(2.32422033283773,-61.1592097658532,
-233.071622012271));
#224119=CARTESIAN_POINT('Ctrl Pts',(5.07841743705022,-74.0087844985998,
-213.273326713143));
#224120=CARTESIAN_POINT('Ctrl Pts',(4.64247057287694,-71.8618416382213,
-216.572529828792));
#224121=CARTESIAN_POINT('Ctrl Pts',(4.20238763043668,-69.7156593822006,
-219.871707521718));
#224122=CARTESIAN_POINT('Ctrl Pts',(3.7532691846266,-67.5715663740637,-223.171108246189));
#224123=CARTESIAN_POINT('Ctrl Pts',(3.30415073881651,-65.4274733659267,
-226.47050897066));
#224124=CARTESIAN_POINT('Ctrl Pts',(2.84695182048441,-63.2850230523818,
-229.76996212396));
#224125=CARTESIAN_POINT('Ctrl Pts',(2.3663295321107,-61.149645769708,-233.071072724443));
#224126=CARTESIAN_POINT('Ctrl Pts',(5.1669208602018,-73.9975814734869,-213.272773948399));
#224127=CARTESIAN_POINT('Ctrl Pts',(4.72347834880175,-71.8507344649978,
-216.571955724444));
#224128=CARTESIAN_POINT('Ctrl Pts',(4.27582417043258,-69.704677477251,-219.871112526297));
#224129=CARTESIAN_POINT('Ctrl Pts',(3.81900114961728,-67.5607834159342,
-223.170503619482));
#224130=CARTESIAN_POINT('Ctrl Pts',(3.36217812880197,-65.4168893546174,
-226.469894712669));
#224131=CARTESIAN_POINT('Ctrl Pts',(2.89713742276365,-63.2747025478298,
-229.769345094758));
#224132=CARTESIAN_POINT('Ctrl Pts',(2.40845676115674,-61.1397999611404,
-233.070512094721));
#224133=CARTESIAN_POINT('Ctrl Pts',(5.21117257177759,-73.9919799609304,
-213.272497566026));
#224134=CARTESIAN_POINT('Ctrl Pts',(4.76398223676415,-71.8451808783859,
-216.571668672269));
#224135=CARTESIAN_POINT('Ctrl Pts',(4.31254244043052,-69.6991865247762,
-219.870815028586));
#224136=CARTESIAN_POINT('Ctrl Pts',(3.85186713211261,-67.5553919368695,
-223.17020130613));
#224137=CARTESIAN_POINT('Ctrl Pts',(3.3911918237947,-65.4115973489628,-226.469587583673));
#224138=CARTESIAN_POINT('Ctrl Pts',(2.92223022390326,-63.2695422955538,
-229.769036580157));
#224139=CARTESIAN_POINT('Ctrl Pts',(2.42952037567976,-61.1348770568567,
-233.070231779859));
#224140=CARTESIAN_POINT('Ctrl Pts',(5.25537332985224,-73.9863105757591,
-213.272217562053));
#224141=CARTESIAN_POINT('Ctrl Pts',(4.804443188236,-71.8395583232445,-216.571377865865));
#224142=CARTESIAN_POINT('Ctrl Pts',(4.34922577383909,-69.693625748861,-219.870513689814));
#224143=CARTESIAN_POINT('Ctrl Pts',(3.8847068492901,-67.5499301842444,-223.169895227836));
#224144=CARTESIAN_POINT('Ctrl Pts',(3.42018792474111,-65.4062346196278,
-226.469276765858));
#224145=CARTESIAN_POINT('Ctrl Pts',(2.94731441370204,-63.2643113932744,
-229.768724637945));
#224146=CARTESIAN_POINT('Ctrl Pts',(2.45058849682277,-61.1298836956491,
-233.069948630535));
#224147=CARTESIAN_POINT('Ctrl Pts',(5.29952111087686,-73.9805739843142,
-213.271933926068));
#224148=CARTESIAN_POINT('Ctrl Pts',(4.8448595684564,-71.8338672844239,-216.571083300041));
#224149=CARTESIAN_POINT('Ctrl Pts',(4.38587294574325,-69.6879954534902,
-219.870208514701));
#224150=CARTESIAN_POINT('Ctrl Pts',(3.91751955310888,-67.5443982610901,
-223.169585404755));
#224151=CARTESIAN_POINT('Ctrl Pts',(3.44916616047452,-65.4008010686901,
-226.46896229481));
#224152=CARTESIAN_POINT('Ctrl Pts',(2.97239026633894,-63.2590095358678,
-229.768409330315));
#224153=CARTESIAN_POINT('Ctrl Pts',(2.47166211180462,-61.1248192227346,
-233.069662711569));
#224154=CARTESIAN_POINT('Ctrl Pts',(5.32159500138917,-73.9777056885918,
-213.271792108075));
#224155=CARTESIAN_POINT('Ctrl Pts',(4.8650677585666,-71.8310217650135,-216.570936017129));
#224156=CARTESIAN_POINT('Ctrl Pts',(4.40419653169533,-69.6851803058048,
-219.870055927144));
#224157=CARTESIAN_POINT('Ctrl Pts',(3.93392590501828,-67.541632299513,-223.169430493215));
#224158=CARTESIAN_POINT('Ctrl Pts',(3.46365527834122,-65.3980842932212,
-226.468805059286));
#224159=CARTESIAN_POINT('Ctrl Pts',(2.98492819265739,-63.2563586071644,
-229.7682516765));
#224160=CARTESIAN_POINT('Ctrl Pts',(2.48219891929555,-61.1222869862773,
-233.069519752087));
#224161=CARTESIAN_POINT('Ctrl Pts',(5.34365564762243,-73.9748205913366,
-213.271649382111));
#224162=CARTESIAN_POINT('Ctrl Pts',(4.8852648058442,-71.8281591247152,-216.570787794402));
#224163=CARTESIAN_POINT('Ctrl Pts',(4.42251107725984,-69.6823477782787,
-219.869902380553));
#224164=CARTESIAN_POINT('Ctrl Pts',(3.95032550358819,-67.5388487952928,
-223.169274645539));
#224165=CARTESIAN_POINT('Ctrl Pts',(3.47813992991653,-65.395349812307,-226.468646910525));
#224166=CARTESIAN_POINT('Ctrl Pts',(2.99746403474337,-63.2536899395703,
-229.768093181413));
#224167=CARTESIAN_POINT('Ctrl Pts',(2.49273710017753,-61.119736971659,-233.069376100254));
#224168=CARTESIAN_POINT('Ctrl Pts',(5.36570279652679,-73.9719187760556,
-213.27150574706));
#224169=CARTESIAN_POINT('Ctrl Pts',(4.90545050582003,-71.8252794243274,
-216.570638631449));
#224170=CARTESIAN_POINT('Ctrl Pts',(4.44081642924868,-69.6794979090499,
-219.86974787583));
#224171=CARTESIAN_POINT('Ctrl Pts',(3.96671825530998,-67.5360477612441,
-223.16911786462));
#224172=CARTESIAN_POINT('Ctrl Pts',(3.49262008137128,-65.3925976134382,
-226.468487853411));
#224173=CARTESIAN_POINT('Ctrl Pts',(3.00999782721103,-63.2510034942836,
-229.76793385332));
#224174=CARTESIAN_POINT('Ctrl Pts',(2.50327677740755,-61.1171690956365,
-233.069231764537));
#224175=CARTESIAN_POINT('Ctrl Pts',(5.37672637097897,-73.9704678684151,
-213.271433929534));
#224176=CARTESIAN_POINT('Ctrl Pts',(4.91554335580794,-71.8238395741335,
-216.570564049972));
#224177=CARTESIAN_POINT('Ctrl Pts',(4.44996910524309,-69.6780729744356,
-219.869670623468));
#224178=CARTESIAN_POINT('Ctrl Pts',(3.97491463117087,-67.5346472442197,
-223.169039474161));
#224179=CARTESIAN_POINT('Ctrl Pts',(3.49986015709865,-65.3912215140038,
-226.468408324854));
#224180=CARTESIAN_POINT('Ctrl Pts',(3.01626472344486,-63.2496602716403,
-229.767854189273));
#224181=CARTESIAN_POINT('Ctrl Pts',(2.50854661602256,-61.1158851576253,
-233.069159596678));
#224182=CARTESIAN_POINT('Ctrl Pts',(5.38969793711063,-73.9687125609349,
-213.271422512912));
#224183=CARTESIAN_POINT('Ctrl Pts',(4.92774932818247,-71.8220549285655,
-216.570545515496));
#224184=CARTESIAN_POINT('Ctrl Pts',(4.46143193292641,-69.6762521336146,
-219.869642328397));
#224185=CARTESIAN_POINT('Ctrl Pts',(3.98568057069344,-67.5327708418263,
-223.16899244726));
#224186=CARTESIAN_POINT('Ctrl Pts',(3.50992920846046,-65.389289550038,-226.468342566122));
#224187=CARTESIAN_POINT('Ctrl Pts',(3.02568037828113,-63.2476572865054,
-229.767763153291));
#224188=CARTESIAN_POINT('Ctrl Pts',(2.51741496202948,-61.1137459383554,
-233.069008530206));
#224189=CARTESIAN_POINT('Ctrl Pts',(5.40189498447758,-73.9670855170926,
-213.27138772269));
#224190=CARTESIAN_POINT('Ctrl Pts',(4.93911538335151,-71.8204146317601,
-216.570505404131));
#224191=CARTESIAN_POINT('Ctrl Pts',(4.47197675342897,-69.6745959954096,
-219.869595356765));
#224192=CARTESIAN_POINT('Ctrl Pts',(3.995425586976,-67.5310910069602,-223.168933864337));
#224193=CARTESIAN_POINT('Ctrl Pts',(3.51887442052304,-65.3875860185108,
-226.468272371909));
#224194=CARTESIAN_POINT('Ctrl Pts',(3.03384525016898,-63.2459241307708,
-229.767677837598));
#224195=CARTESIAN_POINT('Ctrl Pts',(2.5248538590963,-61.1119545168883,-233.068890342738));
#224196=CARTESIAN_POINT('Ctrl Pts',(5.41409203184453,-73.9654584732504,
-213.271352932467));
#224197=CARTESIAN_POINT('Ctrl Pts',(4.95048143852055,-71.8187743349548,
-216.570465292767));
#224198=CARTESIAN_POINT('Ctrl Pts',(4.48252157393154,-69.6729398572046,
-219.869548385134));
#224199=CARTESIAN_POINT('Ctrl Pts',(4.00517060325858,-67.5294111720941,
-223.168875281415));
#224200=CARTESIAN_POINT('Ctrl Pts',(3.52781963258561,-65.3858824869837,
-226.468202177696));
#224201=CARTESIAN_POINT('Ctrl Pts',(3.04201012205683,-63.2441909750361,
-229.767592521906));
#224202=CARTESIAN_POINT('Ctrl Pts',(2.53229275616311,-61.1101630954213,
-233.068772155269));
#224203=CARTESIAN_POINT('Ctrl Pts',(5.42628928608951,-73.963836411599,-213.27131859826));
#224204=CARTESIAN_POINT('Ctrl Pts',(4.96184791256897,-71.8171390304783,
-216.570425682871));
#224205=CARTESIAN_POINT('Ctrl Pts',(4.49306702353044,-69.6712887261328,
-219.869501971269));
#224206=CARTESIAN_POINT('Ctrl Pts',(4.01491645203717,-67.527736378886,-223.168817342139));
#224207=CARTESIAN_POINT('Ctrl Pts',(3.5367658805439,-65.3841840316392,-226.468132713009));
#224208=CARTESIAN_POINT('Ctrl Pts',(3.05017622484798,-63.2424629427525,
-229.767508044828));
#224209=CARTESIAN_POINT('Ctrl Pts',(2.53973306733594,-61.1083769328167,
-233.068655016085));
#224210=CARTESIAN_POINT('Ctrl Pts',(5.43848674342124,-73.9622193313187,
-213.27128471988));
#224211=CARTESIAN_POINT('Ctrl Pts',(4.97321480130074,-71.8155087180278,
-216.570386574246));
#224212=CARTESIAN_POINT('Ctrl Pts',(4.50361309767885,-69.6696426023963,
-219.869456114948));
#224213=CARTESIAN_POINT('Ctrl Pts',(4.02466312853905,-67.5260666279664,
-223.168760046202));
#224214=CARTESIAN_POINT('Ctrl Pts',(3.54571315939927,-65.3824906535366,
-226.468063977456));
#224215=CARTESIAN_POINT('Ctrl Pts',(3.05834355346484,-63.2407400353682,
-229.767424405843));
#224216=CARTESIAN_POINT('Ctrl Pts',(2.54717478764305,-61.1065960304922,
-233.06853892423));
#224217=CARTESIAN_POINT('Ctrl Pts',(5.82880537803666,-73.9104727623503,
-213.27020061172));
#224218=CARTESIAN_POINT('Ctrl Pts',(5.33695524071748,-71.7633387196109,
-216.56913509822));
#224219=CARTESIAN_POINT('Ctrl Pts',(4.84108747042776,-69.6169666428275,
-219.86798871271));
#224220=CARTESIAN_POINT('Ctrl Pts',(4.33655677659942,-67.4726345985407,
-223.16692657622));
#224221=CARTESIAN_POINT('Ctrl Pts',(3.83202608277108,-65.3283025542538,
-226.465864439729));
#224222=CARTESIAN_POINT('Ctrl Pts',(3.31969806920419,-63.1856069990734,
-229.764747958359));
#224223=CARTESIAN_POINT('Ctrl Pts',(2.78530983747041,-61.049607156107,-233.064823984859));
#224224=CARTESIAN_POINT('Ctrl Pts',(6.2193319402912,-73.8638270051978,-213.2695828475));
#224225=CARTESIAN_POINT('Ctrl Pts',(5.70112027305471,-71.7162803992548,
-216.56839640861));
#224226=CARTESIAN_POINT('Ctrl Pts',(5.17920132846573,-69.5694179763168,
-219.867091603535));
#224227=CARTESIAN_POINT('Ctrl Pts',(4.64929793915769,-67.4243655051274,
-223.165751033694));
#224228=CARTESIAN_POINT('Ctrl Pts',(4.11939454984966,-65.2793130339379,
-226.464410463854));
#224229=CARTESIAN_POINT('Ctrl Pts',(3.58230773979595,-63.13572114116,-229.762928355624));
#224230=CARTESIAN_POINT('Ctrl Pts',(3.02488757165734,-60.9980034597846,
-233.062179471459));
#224231=CARTESIAN_POINT('Ctrl Pts',(6.60994240840454,-73.8222558927873,
-213.269427912899));
#224232=CARTESIAN_POINT('Ctrl Pts',(6.06557267238532,-71.6743247983129,
-216.568167153263));
#224233=CARTESIAN_POINT('Ctrl Pts',(5.51780600976152,-69.5270045782149,
-219.866761419183));
#224234=CARTESIAN_POINT('Ctrl Pts',(4.96273068554095,-67.3812822930893,
-223.165228588343));
#224235=CARTESIAN_POINT('Ctrl Pts',(4.40765536132037,-65.2355600079636,
-226.463695757503));
#224236=CARTESIAN_POINT('Ctrl Pts',(3.84600674944955,-63.0911343879077,
-229.761957061969));
#224237=CARTESIAN_POINT('Ctrl Pts',(3.26574682620663,-60.9518397874778,
-233.060586757597));
#224238=CARTESIAN_POINT('Ctrl Pts',(7.39116334463119,-73.7391136679663,
-213.269118043698));
#224239=CARTESIAN_POINT('Ctrl Pts',(6.79447747104655,-71.5904135964293,
-216.567708642569));
#224240=CARTESIAN_POINT('Ctrl Pts',(6.19501537235311,-69.4421777820111,
-219.866101050477));
#224241=CARTESIAN_POINT('Ctrl Pts',(5.58959617830746,-67.2951158690131,
-223.164183697639));
#224242=CARTESIAN_POINT('Ctrl Pts',(4.9841769842618,-65.148053956015,-226.462266344801));
#224243=CARTESIAN_POINT('Ctrl Pts',(4.37340476875675,-63.0019608814033,
-229.760014474658));
#224244=CARTESIAN_POINT('Ctrl Pts',(3.7474653353052,-60.8595124428641,-233.057401329873));
#224245=CARTESIAN_POINT('Ctrl Pts',(8.17274284217698,-73.6762722001305,
-213.270659458216));
#224246=CARTESIAN_POINT('Ctrl Pts',(7.52456725249353,-71.5269159170376,
-216.569288281038));
#224247=CARTESIAN_POINT('Ctrl Pts',(6.87423822142749,-69.3778946347463,
-219.867709178756));
#224248=CARTESIAN_POINT('Ctrl Pts',(6.2192975171534,-67.2296937045752,-223.165751826412));
#224249=CARTESIAN_POINT('Ctrl Pts',(5.56435681287931,-65.0814927744041,
-226.463794474068));
#224250=CARTESIAN_POINT('Ctrl Pts',(4.90527248541439,-62.9339795937943,
-229.761465102056));
#224251=CARTESIAN_POINT('Ctrl Pts',(4.23445772929978,-60.7889308444523,
-233.058419711927));
#224252=CARTESIAN_POINT('Ctrl Pts',(8.95359233126237,-73.6335280557829,
-213.274065021078));
#224253=CARTESIAN_POINT('Ctrl Pts',(8.25459642710441,-71.4837698867074,
-216.572927046439));
#224254=CARTESIAN_POINT('Ctrl Pts',(7.55407719055292,-69.3342366336737,
-219.871616502806));
#224255=CARTESIAN_POINT('Ctrl Pts',(6.85029961029843,-67.1852407881264,
-223.16997355118));
#224256=CARTESIAN_POINT('Ctrl Pts',(6.14652203004394,-65.036244942579,-226.468330599556));
#224257=CARTESIAN_POINT('Ctrl Pts',(5.43981664544253,-62.8877051452259,
-229.766371465045));
#224258=CARTESIAN_POINT('Ctrl Pts',(4.72482964673358,-60.7407372675625,
-233.063701736715));
#224259=CARTESIAN_POINT('Ctrl Pts',(10.5152913094331,-73.5480397670876,
-213.280876146803));
#224260=CARTESIAN_POINT('Ctrl Pts',(9.71465477632616,-71.397477826047,-216.58020457724));
#224261=CARTESIAN_POINT('Ctrl Pts',(8.91375512880376,-69.2469206315284,
-219.879431150906));
#224262=CARTESIAN_POINT('Ctrl Pts',(8.11230379658849,-67.0963349552287,
-223.178417000718));
#224263=CARTESIAN_POINT('Ctrl Pts',(7.31085246437322,-64.945749278929,-226.47740285053));
#224264=CARTESIAN_POINT('Ctrl Pts',(6.50890496549881,-62.7951562480893,
-229.776184191023));
#224265=CARTESIAN_POINT('Ctrl Pts',(5.70557348160117,-60.6443501137831,
-233.074265786289));
#224266=CARTESIAN_POINT('Ctrl Pts',(12.0741192309778,-73.5429416649928,
-213.295088118557));
#224267=CARTESIAN_POINT('Ctrl Pts',(11.174560655384,-71.3925980352056,-216.595652144222));
#224268=CARTESIAN_POINT('Ctrl Pts',(10.276034499693,-69.2421106607767,-219.89636066281));
#224269=CARTESIAN_POINT('Ctrl Pts',(9.37971367536872,-67.0912902652196,
-223.197362281445));
#224270=CARTESIAN_POINT('Ctrl Pts',(8.48339285104444,-64.9404698696625,
-226.498363900081));
#224271=CARTESIAN_POINT('Ctrl Pts',(7.58904411056311,-62.7893619838303,
-229.799632644879));
#224272=CARTESIAN_POINT('Ctrl Pts',(6.70034092093902,-60.637315061886,-233.101605220138));
#224273=CARTESIAN_POINT('Ctrl Pts',(13.6221605046809,-73.6159852550006,
-213.31749452838));
#224274=CARTESIAN_POINT('Ctrl Pts',(12.62507600816,-71.4677688674561,-216.620281085237));
#224275=CARTESIAN_POINT('Ctrl Pts',(11.6304405856027,-69.3193741723348,
-219.923700795081));
#224276=CARTESIAN_POINT('Ctrl Pts',(10.6409978873149,-67.1707515656024,
-223.228560662601));
#224277=CARTESIAN_POINT('Ctrl Pts',(9.65155518902709,-65.0221289588701,
-226.533420530121));
#224278=CARTESIAN_POINT('Ctrl Pts',(8.66680721405871,-62.8732305917473,
-229.839537084504));
#224279=CARTESIAN_POINT('Ctrl Pts',(7.69505740664371,-60.7243047821012,
-233.149611908545));
#224280=CARTESIAN_POINT('Ctrl Pts',(14.3961811415325,-73.6525070500044,
-213.32869773329));
#224281=CARTESIAN_POINT('Ctrl Pts',(13.3503336845479,-71.5053542835814,
-216.632595555744));
#224282=CARTESIAN_POINT('Ctrl Pts',(12.3076436285575,-69.3580059281139,
-219.937370861218));
#224283=CARTESIAN_POINT('Ctrl Pts',(11.271639993288,-67.2104822157939,-223.244159853179));
#224284=CARTESIAN_POINT('Ctrl Pts',(10.2356363580184,-65.0629585034738,
-226.550948845141));
#224285=CARTESIAN_POINT('Ctrl Pts',(9.20568876580652,-62.9151648957058,
-229.859489304316));
#224286=CARTESIAN_POINT('Ctrl Pts',(8.19241564949605,-60.7677996422088,
-233.173615252749));
#224287=CARTESIAN_POINT('Ctrl Pts',(15.1674713187882,-73.7085567757101,
-213.341951507641));
#224288=CARTESIAN_POINT('Ctrl Pts',(14.0731825300145,-71.562941120452,-216.647204118779));
#224289=CARTESIAN_POINT('Ctrl Pts',(12.9827854653705,-69.4171418966908,
-219.953638842029));
#224290=CARTESIAN_POINT('Ctrl Pts',(11.9006166435758,-67.2713253491906,
-223.262814446454));
#224291=CARTESIAN_POINT('Ctrl Pts',(10.818447821781,-65.1255088016904,-226.571990050878));
#224292=CARTESIAN_POINT('Ctrl Pts',(9.74375195730441,-62.9795030354078,
-229.883541373779));
#224293=CARTESIAN_POINT('Ctrl Pts',(8.68946082743354,-60.8348048519155,
-233.202772070184));
#224294=CARTESIAN_POINT('Ctrl Pts',(15.9351468463176,-73.7837993408375,
-213.357451906234));
#224295=CARTESIAN_POINT('Ctrl Pts',(14.7925760080712,-71.6402731942657,
-216.664356393474));
#224296=CARTESIAN_POINT('Ctrl Pts',(13.6546740285671,-69.4966163530812,
-219.972825698813));
#224297=CARTESIAN_POINT('Ctrl Pts',(12.5266115102098,-67.3532549610597,
-223.284963342766));
#224298=CARTESIAN_POINT('Ctrl Pts',(11.3985489918526,-65.2098935690382,
-226.597100986718));
#224299=CARTESIAN_POINT('Ctrl Pts',(10.2794730121625,-63.0665351244741,
-229.912415755274));
#224300=CARTESIAN_POINT('Ctrl Pts',(9.1845149202515,-60.9259885966297,-233.238077193558));
#224301=CARTESIAN_POINT('Ctrl Pts',(15.9831265667882,-73.788502001158,-213.358420681146));
#224302=CARTESIAN_POINT('Ctrl Pts',(14.8375381004497,-71.645106448879,-216.665428410643));
#224303=CARTESIAN_POINT('Ctrl Pts',(13.6966670637669,-69.5015835066056,
-219.974024877362));
#224304=CARTESIAN_POINT('Ctrl Pts',(12.5657361893745,-67.3583755618015,
-223.286347648785));
#224305=CARTESIAN_POINT('Ctrl Pts',(11.434805314982,-65.2151676169974,-226.598670420208));
#224306=CARTESIAN_POINT('Ctrl Pts',(10.3129555780911,-63.0719746300408,
-229.914220404117));
#224307=CARTESIAN_POINT('Ctrl Pts',(9.21545580105263,-60.9316875806744,
-233.240283763769));
#224308=CARTESIAN_POINT('Ctrl Pts',(16.0310921652337,-73.7932796461828,
-213.359398260476));
#224309=CARTESIAN_POINT('Ctrl Pts',(14.8824866922713,-71.6500168515611,
-216.666510400031));
#224310=CARTESIAN_POINT('Ctrl Pts',(13.7386473871037,-69.5066301336811,
-219.975235503695));
#224311=CARTESIAN_POINT('Ctrl Pts',(12.6048492100916,-67.3635785769872,
-223.287745666655));
#224312=CARTESIAN_POINT('Ctrl Pts',(11.4710510330794,-65.2205270202932,
-226.600255829615));
#224313=CARTESIAN_POINT('Ctrl Pts',(10.3464289705351,-63.077502877188,-229.916043994162));
#224314=CARTESIAN_POINT('Ctrl Pts',(9.24638881753499,-60.9374811728283,
-233.242514480938));
#224315=CARTESIAN_POINT('Ctrl Pts',(16.0790434247669,-73.7981321994158,
-213.360384703604));
#224316=CARTESIAN_POINT('Ctrl Pts',(14.9274215266693,-71.6550043474046,
-216.66760243706));
#224317=CARTESIAN_POINT('Ctrl Pts',(13.7806147058241,-69.5117562048766,
-219.976457674748));
#224318=CARTESIAN_POINT('Ctrl Pts',(12.6439502460863,-67.3688640192575,
-223.28915752863));
#224319=CARTESIAN_POINT('Ctrl Pts',(11.5072857863485,-65.2259718336384,
-226.60185738251));
#224320=CARTESIAN_POINT('Ctrl Pts',(10.3798928063555,-63.0831199759298,
-229.917886743821));
#224321=CARTESIAN_POINT('Ctrl Pts',(9.27731352150188,-60.9433696029714,
-233.244769639115));
#224322=CARTESIAN_POINT('Ctrl Pts',(16.1030190545335,-73.8005584760323,
-213.360877925168));
#224323=CARTESIAN_POINT('Ctrl Pts',(14.9498889438683,-71.6574980953263,
-216.668148455574));
#224324=CARTESIAN_POINT('Ctrl Pts',(13.8015983651843,-69.5143192404743,
-219.977068760275));
#224325=CARTESIAN_POINT('Ctrl Pts',(12.6635007640837,-67.3715067403927,
-223.289863459617));
#224326=CARTESIAN_POINT('Ctrl Pts',(11.5254031629831,-65.228694240311,-226.602658158959));
#224327=CARTESIAN_POINT('Ctrl Pts',(10.3966247242656,-63.0859285253007,
-229.918808118651));
#224328=CARTESIAN_POINT('Ctrl Pts',(9.29277587348532,-60.9463138180429,
-233.245897218204));
#224329=CARTESIAN_POINT('Ctrl Pts',(16.1269910995696,-73.8030034797118,
-213.361373362703));
#224330=CARTESIAN_POINT('Ctrl Pts',(14.972352921708,-71.6600111165541,-216.668696986025));
#224331=CARTESIAN_POINT('Ctrl Pts',(13.8225787733862,-69.5169021371247,
-219.977682732017));
#224332=CARTESIAN_POINT('Ctrl Pts',(12.6830482858887,-67.374170068338,-223.290572851677));
#224333=CARTESIAN_POINT('Ctrl Pts',(11.5435177983912,-65.2314379995513,
-226.603462971338));
#224334=CARTESIAN_POINT('Ctrl Pts',(10.4133542529928,-63.0887592876515,
-229.919734283464));
#224335=CARTESIAN_POINT('Ctrl Pts',(9.30823614724962,-60.9492817427462,
-233.247030907634));
#224336=CARTESIAN_POINT('Ctrl Pts',(16.1509595327496,-73.8054672009588,
-213.361871023762));
#224337=CARTESIAN_POINT('Ctrl Pts',(14.99481342806,-71.66254340432,-216.669248038005));
#224338=CARTESIAN_POINT('Ctrl Pts',(13.8435558938089,-69.5195048912867,
-219.978299602301));
#224339=CARTESIAN_POINT('Ctrl Pts',(12.7025927706434,-67.3768540049101,
-223.291285721626));
#224340=CARTESIAN_POINT('Ctrl Pts',(11.5616296474779,-65.2342031185336,
-226.60427184095));
#224341=CARTESIAN_POINT('Ctrl Pts',(10.4300813444763,-63.0916122772264,
-229.920665266035));
#224342=CARTESIAN_POINT('Ctrl Pts',(9.32369428621562,-60.9522734066295,
-233.248170744691));
#224343=CARTESIAN_POINT('Ctrl Pts',(16.1749279659296,-73.8079309222057,
-213.362368684823));
#224344=CARTESIAN_POINT('Ctrl Pts',(15.0172739344119,-71.6650756920859,
-216.669799089985));
#224345=CARTESIAN_POINT('Ctrl Pts',(13.8645330142317,-69.5221076454487,
-219.978916472587));
#224346=CARTESIAN_POINT('Ctrl Pts',(12.7221372553981,-67.3795379414822,
-223.291998591574));
#224347=CARTESIAN_POINT('Ctrl Pts',(11.5797414965646,-65.2369682375158,
-226.605080710561));
#224348=CARTESIAN_POINT('Ctrl Pts',(10.4468084359598,-63.0944652668013,
-229.921596248607));
#224349=CARTESIAN_POINT('Ctrl Pts',(9.33915242518163,-60.9552650705129,
-233.249310581748));
#224350=CARTESIAN_POINT('Ctrl Pts',(16.1952404425737,-73.8106650452457,
-213.361731538637));
#224351=CARTESIAN_POINT('Ctrl Pts',(15.0357204215971,-71.6678714790176,
-216.669082666045));
#224352=CARTESIAN_POINT('Ctrl Pts',(13.8810654780263,-69.5249584688797,
-219.978101688701));
#224353=CARTESIAN_POINT('Ctrl Pts',(12.7366574254637,-67.3824171756017,
-223.29103806134));
#224354=CARTESIAN_POINT('Ctrl Pts',(11.5922493729011,-65.2398758823236,
-226.60397443398));
#224355=CARTESIAN_POINT('Ctrl Pts',(10.4572108953697,-63.0973827020436,
-229.920303449303));
#224356=CARTESIAN_POINT('Ctrl Pts',(9.34722878778031,-60.9580814427723,
-233.247692673937));
#224357=CARTESIAN_POINT('Ctrl Pts',(16.2167932117536,-73.8132831498057,
-213.361475819388));
#224358=CARTESIAN_POINT('Ctrl Pts',(15.0555279749194,-71.6705532338741,
-216.66879240035));
#224359=CARTESIAN_POINT('Ctrl Pts',(13.8991042674617,-69.5277002093038,
-219.977768430969));
#224360=CARTESIAN_POINT('Ctrl Pts',(12.7528793682099,-67.3852051104234,
-223.290640615083));
#224361=CARTESIAN_POINT('Ctrl Pts',(11.606654468958,-65.2427100115431,-226.603512799197));
#224362=CARTESIAN_POINT('Ctrl Pts',(10.4697535757153,-63.1002531490222,
-229.919759447509));
#224363=CARTESIAN_POINT('Ctrl Pts',(9.35780123871772,-60.9609326117186,
-233.247003746218));
#224364=CARTESIAN_POINT('Ctrl Pts',(16.3030042884734,-73.8237555680453,
-213.360452942392));
#224365=CARTESIAN_POINT('Ctrl Pts',(15.1347581882085,-71.6812802533,-216.667631337573));
#224366=CARTESIAN_POINT('Ctrl Pts',(13.9712594252033,-69.538667171,-219.976435400044));
#224367=CARTESIAN_POINT('Ctrl Pts',(12.8177671391946,-67.3963568497104,
-223.289050830054));
#224368=CARTESIAN_POINT('Ctrl Pts',(11.6642748531859,-65.2540465284208,
-226.601666260063));
#224369=CARTESIAN_POINT('Ctrl Pts',(10.5199242970979,-63.1117349369367,
-229.917583440332));
#224370=CARTESIAN_POINT('Ctrl Pts',(9.40009104246739,-60.972337287504,-233.24424803534));
#224371=CARTESIAN_POINT('Ctrl Pts',(16.3892942328758,-73.8339539222327,
-213.359415827195));
#224372=CARTESIAN_POINT('Ctrl Pts',(15.2140673832556,-71.6917296181947,
-216.666455999658));
#224373=CARTESIAN_POINT('Ctrl Pts',(14.0434937744094,-69.5493539058165,
-219.975088199201));
#224374=CARTESIAN_POINT('Ctrl Pts',(12.8827334643832,-67.4072286376852,
-223.287447402735));
#224375=CARTESIAN_POINT('Ctrl Pts',(11.7219731543571,-65.2651033695538,
-226.599806606268));
#224376=CARTESIAN_POINT('Ctrl Pts',(10.5701722900963,-63.1229397721944,
-229.915395364823));
#224377=CARTESIAN_POINT('Ctrl Pts',(9.44245022372204,-60.9834765470907,
-233.24148193285));
#224378=CARTESIAN_POINT('Ctrl Pts',(16.4756536810565,-73.8438772043577,
-213.358364250326));
#224379=CARTESIAN_POINT('Ctrl Pts',(15.2934473154818,-71.701900424371,-216.665266171061));
#224380=CARTESIAN_POINT('Ctrl Pts',(14.1158002338677,-69.5597595986373,
-219.973726626617));
#224381=CARTESIAN_POINT('Ctrl Pts',(12.9477726440111,-67.4178197482275,
-223.28583020421));
#224382=CARTESIAN_POINT('Ctrl Pts',(11.7797450541545,-65.2758798978176,
-226.597933781804));
#224383=CARTESIAN_POINT('Ctrl Pts',(10.6204947589536,-63.1338670513053,
-229.913195248458));
#224384=CARTESIAN_POINT('Ctrl Pts',(9.48487851765326,-60.9943501153261,
-233.238705966825));
#224385=CARTESIAN_POINT('Ctrl Pts',(16.6483725774179,-73.8637237686076,
-213.356261096586));
#224386=CARTESIAN_POINT('Ctrl Pts',(15.4522071799342,-71.7222420367236,
-216.662886513868));
#224387=CARTESIAN_POINT('Ctrl Pts',(14.2604131527844,-69.5805709842789,
-219.97100348145));
#224388=CARTESIAN_POINT('Ctrl Pts',(13.0778510032668,-67.4390019693121,
-223.282595807161));
#224389=CARTESIAN_POINT('Ctrl Pts',(11.8952888537493,-65.2974329543453,
-226.594188132872));
#224390=CARTESIAN_POINT('Ctrl Pts',(10.721139696668,-63.1557216095271,-229.908795015729));
#224391=CARTESIAN_POINT('Ctrl Pts',(9.5697351055157,-61.0160972517968,-233.233154034775));
#224392=CARTESIAN_POINT('Ctrl Pts',(16.8213694784135,-73.8824700233217,
-213.354100077751));
#224393=CARTESIAN_POINT('Ctrl Pts',(15.6112499819579,-71.7414693927443,
-216.660448871784));
#224394=CARTESIAN_POINT('Ctrl Pts',(14.4053145017287,-69.6002581805821,
-219.968222822437));
#224395=CARTESIAN_POINT('Ctrl Pts',(13.2082207723041,-67.459061467655,-223.279306294012));
#224396=CARTESIAN_POINT('Ctrl Pts',(12.0111270428794,-65.317864754728,-226.590389765588));
#224397=CARTESIAN_POINT('Ctrl Pts',(10.8220825428301,-63.1764659467185,
-229.904346578072));
#224398=CARTESIAN_POINT('Ctrl Pts',(9.65486815061528,-61.0367817019578,
-233.227562614776));
#224399=CARTESIAN_POINT('Ctrl Pts',(16.994569608081,-73.9001081635233,-213.351879630837));
#224400=CARTESIAN_POINT('Ctrl Pts',(15.7705099053261,-71.759575521472,-216.657951790479));
#224401=CARTESIAN_POINT('Ctrl Pts',(14.5504477647375,-69.6188149294841,
-219.965383361714));
#224402=CARTESIAN_POINT('Ctrl Pts',(13.3388364479968,-67.4779925971432,
-223.275961013328));
#224403=CARTESIAN_POINT('Ctrl Pts',(12.1272251312561,-65.3371702648023,
-226.586538664941));
#224404=CARTESIAN_POINT('Ctrl Pts',(10.9233008549698,-63.19609519418,-229.899850654492));
#224405=CARTESIAN_POINT('Ctrl Pts',(9.74027549478214,-61.0564003174753,
-233.2219363562));
#224406=CARTESIAN_POINT('Ctrl Pts',(17.340969867416,-73.9353844439267,-213.347438737011));
#224407=CARTESIAN_POINT('Ctrl Pts',(16.0890297520624,-71.7957877789274,
-216.652957627871));
#224408=CARTESIAN_POINT('Ctrl Pts',(14.8407142907551,-69.6559284272883,
-219.959704440269));
#224409=CARTESIAN_POINT('Ctrl Pts',(13.6000677993823,-67.5158548561195,
-223.269270451959));
#224410=CARTESIAN_POINT('Ctrl Pts',(12.3594213080095,-65.3757812849507,
-226.578836463649));
#224411=CARTESIAN_POINT('Ctrl Pts',(11.125737479249,-63.235353689103,-229.890858807335));
#224412=CARTESIAN_POINT('Ctrl Pts',(9.91109018311586,-61.0956375485103,
-233.210683839047));
#224413=CARTESIAN_POINT('Ctrl Pts',(17.6881829159947,-73.96622793775,-213.342759849927));
#224414=CARTESIAN_POINT('Ctrl Pts',(16.4084179353708,-71.8275148033868,
-216.647725367964));
#224415=CARTESIAN_POINT('Ctrl Pts',(15.1319083062413,-69.6885198227639,
-219.953789896397));
#224416=CARTESIAN_POINT('Ctrl Pts',(13.8622826479186,-67.5492034630686,
-223.262356339594));
#224417=CARTESIAN_POINT('Ctrl Pts',(12.5926569895958,-65.4098871033733,
-226.570922782791));
#224418=CARTESIAN_POINT('Ctrl Pts',(11.3292759747224,-63.2701519092751,
-229.881676366979));
#224419=CARTESIAN_POINT('Ctrl Pts',(10.0830023568968,-61.130612691193,-233.199291525399));
#224420=CARTESIAN_POINT('Ctrl Pts',(18.0356123358478,-73.9925802279162,
-213.337833927419));
#224421=CARTESIAN_POINT('Ctrl Pts',(16.7281499098057,-71.8547048439406,
-216.642247555954));
#224422=CARTESIAN_POINT('Ctrl Pts',(15.4235797449726,-69.7165429992444,
-219.947634512312));
#224423=CARTESIAN_POINT('Ctrl Pts',(14.1251185099795,-67.5779955815387,
-223.255219367308));
#224424=CARTESIAN_POINT('Ctrl Pts',(12.8266572749865,-65.4394481638329,
-226.562804222303));
#224425=CARTESIAN_POINT('Ctrl Pts',(11.533736224421,-63.300450082589,-229.872316979927));
#224426=CARTESIAN_POINT('Ctrl Pts',(10.2559925260419,-61.1612854472096,
-233.187802584487));
#224427=CARTESIAN_POINT('Ctrl Pts',(19.4253300152602,-74.0979893885809,
-213.31813023739));
#224428=CARTESIAN_POINT('Ctrl Pts',(18.0070778075454,-71.9634650061557,
-216.620336307913));
#224429=CARTESIAN_POINT('Ctrl Pts',(16.5902654998976,-69.8286357051668,
-219.923012975971));
#224430=CARTESIAN_POINT('Ctrl Pts',(15.1764619582234,-67.6931640554191,
-223.22667147816));
#224431=CARTESIAN_POINT('Ctrl Pts',(13.7626584165491,-65.5576924056715,
-226.53032998035));
#224432=CARTESIAN_POINT('Ctrl Pts',(12.3515772232155,-63.4216427758444,
-229.83487943172));
#224433=CARTESIAN_POINT('Ctrl Pts',(10.9479532026221,-61.2839764712757,
-233.14184682084));
#224434=CARTESIAN_POINT('Ctrl Pts',(20.8193262495726,-74.1303947430786,
-213.294867150046));
#224435=CARTESIAN_POINT('Ctrl Pts',(19.2921867436174,-71.9987556912252,
-216.594831507688));
#224436=CARTESIAN_POINT('Ctrl Pts',(17.7650869650877,-69.8670241956512,
-219.894793488995));
#224437=CARTESIAN_POINT('Ctrl Pts',(16.2379643566434,-67.735090498351,-223.194688298922));
#224438=CARTESIAN_POINT('Ctrl Pts',(14.7108417481991,-65.6031568010509,
-226.494583108848));
#224439=CARTESIAN_POINT('Ctrl Pts',(13.1837369485187,-63.4710380794777,
-229.794436678806));
#224440=CARTESIAN_POINT('Ctrl Pts',(11.6562419786961,-61.3384163644667,
-233.0939430997));
#224441=CARTESIAN_POINT('Ctrl Pts',(22.1870742035852,-74.0934804397454,
-213.269235878432));
#224442=CARTESIAN_POINT('Ctrl Pts',(20.5563486581314,-71.9629449474402,
-216.566743885946));
#224443=CARTESIAN_POINT('Ctrl Pts',(18.9243205135732,-69.8327666793285,
-219.863841772445));
#224444=CARTESIAN_POINT('Ctrl Pts',(17.289717647084,-67.703338899474,-223.16015770219));
#224445=CARTESIAN_POINT('Ctrl Pts',(15.6551147805949,-65.5739111196196,
-226.456473631934));
#224446=CARTESIAN_POINT('Ctrl Pts',(14.0181153557698,-63.4451661048359,
-229.752051509661));
#224447=CARTESIAN_POINT('Ctrl Pts',(12.3752611396561,-61.3182690712579,
-233.045942634108));
#224448=CARTESIAN_POINT('Ctrl Pts',(22.8709481805915,-74.0750232880787,
-213.256420242625));
#224449=CARTESIAN_POINT('Ctrl Pts',(21.1884296153885,-71.9450395755477,
-216.552700075075));
#224450=CARTESIAN_POINT('Ctrl Pts',(19.5039372878161,-69.8156379211672,
-219.848365914171));
#224451=CARTESIAN_POINT('Ctrl Pts',(17.8155942923044,-67.6874631000356,
-223.142892403823));
#224452=CARTESIAN_POINT('Ctrl Pts',(16.1272512967927,-65.559288278904,-226.437418893476));
#224453=CARTESIAN_POINT('Ctrl Pts',(14.4353045593953,-63.432230117515,-229.730858925089));
#224454=CARTESIAN_POINT('Ctrl Pts',(12.7347707201362,-61.3081954246535,
-233.021942401313));
#224455=CARTESIAN_POINT('Ctrl Pts',(23.5480695180481,-74.0394366671371,
-213.24294581755));
#224456=CARTESIAN_POINT('Ctrl Pts',(21.8151227650933,-71.9095199232041,
-216.537959093058));
#224457=CARTESIAN_POINT('Ctrl Pts',(20.0795547520248,-69.7804677651607,
-219.832174698833));
#224458=CARTESIAN_POINT('Ctrl Pts',(18.3389963496171,-67.653239079547,-223.124983513773));
#224459=CARTESIAN_POINT('Ctrl Pts',(16.5984379472094,-65.5260103939333,
-226.417792328712));
#224460=CARTESIAN_POINT('Ctrl Pts',(14.8531613104273,-63.4004482694333,
-229.709234763845));
#224461=CARTESIAN_POINT('Ctrl Pts',(13.0971728800481,-61.2793476978764,
-232.998003019156));
#224462=CARTESIAN_POINT('Ctrl Pts',(24.2157714140089,-73.9880357308627,
-213.229014471039));
#224463=CARTESIAN_POINT('Ctrl Pts',(22.4339461787341,-71.8573077591636,
-216.522677077293));
#224464=CARTESIAN_POINT('Ctrl Pts',(20.6488795380189,-69.727793615988,-219.815393786219));
#224465=CARTESIAN_POINT('Ctrl Pts',(18.8578584941687,-67.6007885459759,
-223.106553748693));
#224466=CARTESIAN_POINT('Ctrl Pts',(17.0668374503185,-65.4737834759639,
-226.397713711167));
#224467=CARTESIAN_POINT('Ctrl Pts',(15.2701229993281,-63.3491012702381,
-229.687335801967));
#224468=CARTESIAN_POINT('Ctrl Pts',(13.4612647392516,-61.2303346129408,
-232.974299931676));
#224469=CARTESIAN_POINT('Ctrl Pts',(24.3826968879991,-73.9751854967941,
-213.225531634411));
#224470=CARTESIAN_POINT('Ctrl Pts',(22.5886520321442,-71.8442547181535,
-216.518856573352));
#224471=CARTESIAN_POINT('Ctrl Pts',(20.7912107345175,-69.7146250786948,
-219.811198558066));
#224472=CARTESIAN_POINT('Ctrl Pts',(18.9875740303066,-67.5876759125832,
-223.101946307423));
#224473=CARTESIAN_POINT('Ctrl Pts',(17.1839373260957,-65.4607267464716,
-226.39269405678));
#224474=CARTESIAN_POINT('Ctrl Pts',(15.3743634215533,-63.3362645204393,
-229.681861061497));
#224475=CARTESIAN_POINT('Ctrl Pts',(13.5522877040525,-61.2180813417068,
-232.968374159806));
#224476=CARTESIAN_POINT('Ctrl Pts',(24.5490260926448,-73.9613534513551,
-213.222016096025));
#224477=CARTESIAN_POINT('Ctrl Pts',(22.7428608767437,-71.8301631357306,
-216.514999213761));
#224478=CARTESIAN_POINT('Ctrl Pts',(20.9331465818466,-69.7003652432428,
-219.806964785417));
#224479=CARTESIAN_POINT('Ctrl Pts',(19.1170081030222,-67.573424236258,-223.09730631659));
#224480=CARTESIAN_POINT('Ctrl Pts',(17.3008696241978,-65.4464832292733,
-226.387647847762));
#224481=CARTESIAN_POINT('Ctrl Pts',(15.4785601554459,-63.3221993407807,
-229.676372916497));
#224482=CARTESIAN_POINT('Ctrl Pts',(13.6434360700701,-61.2045576567449,
-232.962469186235));
#224483=CARTESIAN_POINT('Ctrl Pts',(24.7147083990055,-73.9465669153719,
-213.218466861474));
#224484=CARTESIAN_POINT('Ctrl Pts',(22.896527662223,-71.8150523527131,-216.511104550879));
#224485=CARTESIAN_POINT('Ctrl Pts',(21.0746484989543,-69.6850253260801,
-219.802693125391));
#224486=CARTESIAN_POINT('Ctrl Pts',(19.2461305058791,-67.5580352841076,
-223.092636242469));
#224487=CARTESIAN_POINT('Ctrl Pts',(17.417612512804,-65.431045242135,-226.382579359546));
#224488=CARTESIAN_POINT('Ctrl Pts',(15.5827019558228,-63.3068875335093,
-229.670878428191));
#224489=CARTESIAN_POINT('Ctrl Pts',(13.7347113090105,-61.1897293326642,
-232.956594042948));
#224490=CARTESIAN_POINT('Ctrl Pts',(24.7975495521858,-73.9391736473804,
-213.216692244198));
#224491=CARTESIAN_POINT('Ctrl Pts',(22.9733610549627,-71.8074969612043,
-216.509157219438));
#224492=CARTESIAN_POINT('Ctrl Pts',(21.1453994575082,-69.6773553674987,
-219.800557295379));
#224493=CARTESIAN_POINT('Ctrl Pts',(19.3106917073076,-67.5503408080323,
-223.090301205408));
#224494=CARTESIAN_POINT('Ctrl Pts',(17.4759839571071,-65.4233262485659,
-226.380045115437));
#224495=CARTESIAN_POINT('Ctrl Pts',(15.6347728560114,-63.2992316298737,
-229.668131184037));
#224496=CARTESIAN_POINT('Ctrl Pts',(13.7803489284807,-61.1823151706239,
-232.953656471305));
#224497=CARTESIAN_POINT('Ctrl Pts',(24.8802289805,-73.9315417594893,-213.214909206118));
#224498=CARTESIAN_POINT('Ctrl Pts',(23.0500589324285,-71.7996867719131,
-216.507200566405));
#224499=CARTESIAN_POINT('Ctrl Pts',(21.2160419341602,-69.6694153895317,
-219.79841199949));
#224500=CARTESIAN_POINT('Ctrl Pts',(19.3751749925241,-67.5423620096871,
-223.087958654086));
#224501=CARTESIAN_POINT('Ctrl Pts',(17.5343080508878,-65.4153086298425,
-226.37750530868));
#224502=CARTESIAN_POINT('Ctrl Pts',(15.6868300264596,-63.2912640530134,
-229.665382361024));
#224503=CARTESIAN_POINT('Ctrl Pts',(13.8260182553397,-61.174574822688,-232.950726355029));
#224504=CARTESIAN_POINT('Ctrl Pts',(24.9627403530718,-73.9236746829435,
-213.213117642504));
#224505=CARTESIAN_POINT('Ctrl Pts',(23.126615659932,-71.7916242163204,-216.505234561518));
#224506=CARTESIAN_POINT('Ctrl Pts',(21.2865711101662,-69.6612067996815,
-219.796257356157));
#224507=CARTESIAN_POINT('Ctrl Pts',(19.4395765925294,-67.5340990890229,
-223.085608935934));
#224508=CARTESIAN_POINT('Ctrl Pts',(17.5925820748926,-65.4069913783643,
-226.374960515711));
#224509=CARTESIAN_POINT('Ctrl Pts',(15.7388720794492,-63.2829824280864,
-229.662632880377));
#224510=CARTESIAN_POINT('Ctrl Pts',(13.8717193997709,-61.1665038590085,
-232.947804805376));
#224511=CARTESIAN_POINT('Ctrl Pts',(25.0039960393577,-73.9197411446707,
-213.212221860697));
#224512=CARTESIAN_POINT('Ctrl Pts',(23.1648940236837,-71.787592938524,-216.504251559075));
#224513=CARTESIAN_POINT('Ctrl Pts',(21.3218356981692,-69.6571025047564,
-219.79518003449));
#224514=CARTESIAN_POINT('Ctrl Pts',(19.4717773925321,-67.5299676286908,
-223.084434076858));
#224515=CARTESIAN_POINT('Ctrl Pts',(17.621719086895,-65.4028327526252,-226.373688119227));
#224516=CARTESIAN_POINT('Ctrl Pts',(15.764893105944,-63.2788416156229,-229.661258140053));
#224517=CARTESIAN_POINT('Ctrl Pts',(13.8945699719865,-61.1624683771687,
-232.946344030549));
#224518=CARTESIAN_POINT('Ctrl Pts',(25.0452097116804,-73.9157488094,-213.211323947711));
#224519=CARTESIAN_POINT('Ctrl Pts',(23.2031370999057,-71.7834985692942,
-216.503266218939));
#224520=CARTESIAN_POINT('Ctrl Pts',(21.357071961051,-69.6529310569108,-219.794100376343));
#224521=CARTESIAN_POINT('Ctrl Pts',(19.5039577712971,-67.5257651375524,
-223.083257426481));
#224522=CARTESIAN_POINT('Ctrl Pts',(17.6508435815433,-65.3985992181939,
-226.372414476619));
#224523=CARTESIAN_POINT('Ctrl Pts',(15.7909103532289,-63.2746222900822,
-229.659883235697));
#224524=CARTESIAN_POINT('Ctrl Pts',(13.9174284977559,-61.1583502398543,
-232.944885397156));
#224525=CARTESIAN_POINT('Ctrl Pts',(25.0863805784989,-73.9116981070247,
-213.210423891692));
#224526=CARTESIAN_POINT('Ctrl Pts',(23.2413441840135,-71.7793414134085,
-216.502278538958));
#224527=CARTESIAN_POINT('Ctrl Pts',(21.3922792967075,-69.6486926323577,
-219.793018398826));
#224528=CARTESIAN_POINT('Ctrl Pts',(19.5361172580662,-67.5214916392097,
-223.082079030659));
#224529=CARTESIAN_POINT('Ctrl Pts',(17.679955219425,-65.3942906460616,-226.371139662493));
#224530=CARTESIAN_POINT('Ctrl Pts',(15.8169236486359,-63.2703241481897,
-229.658508284608));
#224531=CARTESIAN_POINT('Ctrl Pts',(13.9402949855555,-61.1541488842813,
-232.943429042643));
#224532=CARTESIAN_POINT('Ctrl Pts',(25.0966732952035,-73.9106854314309,
-213.210198877688));
#224533=CARTESIAN_POINT('Ctrl Pts',(23.2508959550404,-71.7783021244371,
-216.502031618964));
#224534=CARTESIAN_POINT('Ctrl Pts',(21.4010811306217,-69.6476330262194,
-219.792747904446));
#224535=CARTESIAN_POINT('Ctrl Pts',(19.5441571297585,-67.520423264624,-223.081784431704));
#224536=CARTESIAN_POINT('Ctrl Pts',(17.6872331288954,-65.3932135030285,
-226.370820958961));
#224537=CARTESIAN_POINT('Ctrl Pts',(15.8234269724877,-63.2692496127166,
-229.658164546835));
#224538=CARTESIAN_POINT('Ctrl Pts',(13.9460116075054,-61.1530985453881,
-232.943064954015));
#224539=CARTESIAN_POINT('Ctrl Pts',(25.1069633365636,-73.9096691078962,
-213.209973729747));
#224540=CARTESIAN_POINT('Ctrl Pts',(23.2604454765595,-71.7772589113024,
-216.501784552734));
#224541=CARTESIAN_POINT('Ctrl Pts',(21.409881156585,-69.6465692340378,-219.792477265113));
#224542=CARTESIAN_POINT('Ctrl Pts',(19.5521956957022,-67.5193504520834,
-223.081489723665));
#224543=CARTESIAN_POINT('Ctrl Pts',(17.6945102348195,-65.392131670129,-226.370502182217));
#224544=CARTESIAN_POINT('Ctrl Pts',(15.8299300493494,-63.2681701512003,
-229.657820806149));
#224545=CARTESIAN_POINT('Ctrl Pts',(13.9517287270644,-61.1520430053247,
-232.942701007811));
#224546=CARTESIAN_POINT('Ctrl Pts',(25.1172506902097,-73.9086491431441,
-213.209748447694));
#224547=CARTESIAN_POINT('Ctrl Pts',(23.2699927375595,-71.776211778772,-216.501537340246));
#224548=CARTESIAN_POINT('Ctrl Pts',(21.4186793651912,-69.6455012585676,
-219.792206481111));
#224549=CARTESIAN_POINT('Ctrl Pts',(19.5602329485438,-67.5182732019474,
-223.081194907278));
#224550=CARTESIAN_POINT('Ctrl Pts',(17.7017865318965,-65.3910451453272,
-226.370183333445));
#224551=CARTESIAN_POINT('Ctrl Pts',(15.836432876527,-63.2670857588602,-229.657477064395));
#224552=CARTESIAN_POINT('Ctrl Pts',(13.9574463443279,-61.1509822552403,
-232.942337206169));
#224553=CARTESIAN_POINT('Ctrl Pts',(25.1275380438559,-73.9076291783921,
-213.209523165641));
#224554=CARTESIAN_POINT('Ctrl Pts',(23.2795399985595,-71.7751646462416,
-216.501290127757));
#224555=CARTESIAN_POINT('Ctrl Pts',(21.4274775737974,-69.6444332830974,
-219.791935697108));
#224556=CARTESIAN_POINT('Ctrl Pts',(19.5682702013855,-67.5171959518114,
-223.080900090889));
#224557=CARTESIAN_POINT('Ctrl Pts',(17.7090628289735,-65.3899586205254,
-226.369864484671));
#224558=CARTESIAN_POINT('Ctrl Pts',(15.8429357037046,-63.2660013665201,
-229.65713332264));
#224559=CARTESIAN_POINT('Ctrl Pts',(13.9631639615914,-61.149921505156,-232.941973404527));
#224560=CARTESIAN_POINT('Ctrl Pts',(25.1372576920846,-73.906800444898,-213.209112994181));
#224561=CARTESIAN_POINT('Ctrl Pts',(23.2884525006053,-71.7743376152923,
-216.500839713002));
#224562=CARTESIAN_POINT('Ctrl Pts',(21.435563238532,-69.643620799134,-219.791441687824));
#224563=CARTESIAN_POINT('Ctrl Pts',(19.5754996444385,-67.5164229145748,
-223.080361001592));
#224564=CARTESIAN_POINT('Ctrl Pts',(17.7154360503449,-65.3892250300156,
-226.369280315361));
#224565=CARTESIAN_POINT('Ctrl Pts',(15.8484227674922,-63.2653312673536,
-229.656501770123));
#224566=CARTESIAN_POINT('Ctrl Pts',(13.9677245066283,-61.1493660025175,
-232.941302670312));
#224567=CARTESIAN_POINT('Ctrl Pts',(25.1485775908394,-73.9054141624897,
-213.20922679825));
#224568=CARTESIAN_POINT('Ctrl Pts',(23.2991570846935,-71.7728700013319,
-216.500965172341));
#224569=CARTESIAN_POINT('Ctrl Pts',(21.4456633269895,-69.642066256973,-219.791580356526));
#224570=CARTESIAN_POINT('Ctrl Pts',(19.5850156941798,-67.5147685546832,
-223.080514436398));
#224571=CARTESIAN_POINT('Ctrl Pts',(17.72436806137,-65.3874708523934,-226.369448516268));
#224572=CARTESIAN_POINT('Ctrl Pts',(15.8567904524694,-63.2634655201446,
-229.656686662214));
#224573=CARTESIAN_POINT('Ctrl Pts',(13.9755694621328,-61.1473556487549,
-232.941503186179));
#224574=CARTESIAN_POINT('Ctrl Pts',(25.171217388349,-73.9026415976731,-213.209454406389));
#224575=CARTESIAN_POINT('Ctrl Pts',(23.3205662528698,-71.7699347734113,
-216.501216091021));
#224576=CARTESIAN_POINT('Ctrl Pts',(21.4658635039045,-69.6389571726509,
-219.791857693933));
#224577=CARTESIAN_POINT('Ctrl Pts',(19.6040477936623,-67.5114598348999,
-223.080821306008));
#224578=CARTESIAN_POINT('Ctrl Pts',(17.7422320834202,-65.383962497149,-226.369784918083));
#224579=CARTESIAN_POINT('Ctrl Pts',(15.8735258224239,-63.2597340257264,
-229.657056446399));
#224580=CARTESIAN_POINT('Ctrl Pts',(13.9912593731417,-61.1433349412296,
-232.941904217913));
#224581=CARTESIAN_POINT('Ctrl Pts',(25.193849356443,-73.8998869012639,-213.209683688439));
#224582=CARTESIAN_POINT('Ctrl Pts',(23.3419708963093,-71.7670180254577,
-216.501468996797));
#224583=CARTESIAN_POINT('Ctrl Pts',(21.4860624620753,-69.6358671958947,
-219.792137371206));
#224584=CARTESIAN_POINT('Ctrl Pts',(19.62308191069,-67.5081709556807,-223.081130950866));
#224585=CARTESIAN_POINT('Ctrl Pts',(17.7601013593046,-65.3804747154667,
-226.370124530527));
#224586=CARTESIAN_POINT('Ctrl Pts',(15.8902696209903,-63.2560239166916,
-229.657429944766));
#224587=CARTESIAN_POINT('Ctrl Pts',(14.0069606167652,-61.1393368768376,
-232.942309711861));
#224588=CARTESIAN_POINT('Ctrl Pts',(25.2164735434192,-73.8971500307629,
-213.209914643404));
#224589=CARTESIAN_POINT('Ctrl Pts',(23.3633710413963,-71.7641197332832,
-216.501723891369));
#224590=CARTESIAN_POINT('Ctrl Pts',(21.5062602068588,-69.6327963210985,
-219.792419393227));
#224591=CARTESIAN_POINT('Ctrl Pts',(19.6421180325673,-67.5049019292739,
-223.081443379648));
#224592=CARTESIAN_POINT('Ctrl Pts',(17.7779758582759,-65.3770075374493,
-226.370467366069));
#224593=CARTESIAN_POINT('Ctrl Pts',(15.9070218020689,-63.2523352409534,
-229.65780717451));
#224594=CARTESIAN_POINT('Ctrl Pts',(14.0226731406812,-61.1353615142731,
-232.942719688923));
#224595=CARTESIAN_POINT('Ctrl Pts',(25.5784605350381,-73.8533601027457,
-213.213609922837));
#224596=CARTESIAN_POINT('Ctrl Pts',(23.7057733627864,-71.7177470584899,
-216.505802204519));
#224597=CARTESIAN_POINT('Ctrl Pts',(21.8294241233942,-69.5836623243583,
-219.796931745576));
#224598=CARTESIAN_POINT('Ctrl Pts',(19.9466959826056,-67.4525975067642,
-223.08644224016));
#224599=CARTESIAN_POINT('Ctrl Pts',(18.063967841817,-65.32153268917,-226.375952734744));
#224600=CARTESIAN_POINT('Ctrl Pts',(16.1750566993262,-63.1933164291426,
-229.663842850422));
#224601=CARTESIAN_POINT('Ctrl Pts',(14.274073523336,-61.0717557132421,-232.94927932191));
#224602=CARTESIAN_POINT('Ctrl Pts',(25.9384558510478,-73.8141338585575,
-213.217733341187));
#224603=CARTESIAN_POINT('Ctrl Pts',(24.0470243860156,-71.6760992561169,
-216.510389357129));
#224604=CARTESIAN_POINT('Ctrl Pts',(22.1522776113516,-69.5394185327721,
-219.802043797164));
#224605=CARTESIAN_POINT('Ctrl Pts',(20.2517872646464,-67.4053752329754,
-223.09215272069));
#224606=CARTESIAN_POINT('Ctrl Pts',(18.3512969179412,-65.2713319331787,
-226.382261644215));
#224607=CARTESIAN_POINT('Ctrl Pts',(16.4452373481732,-63.1397837380439,
-229.670831497313));
#224608=CARTESIAN_POINT('Ctrl Pts',(14.5283616228576,-61.0139593295415,
-232.956982844669));
#224609=CARTESIAN_POINT('Ctrl Pts',(26.2966554094189,-73.7792956476803,
-213.222281607897));
#224610=CARTESIAN_POINT('Ctrl Pts',(24.3872303655758,-71.6390760412376,
-216.515494177504));
#224611=CARTESIAN_POINT('Ctrl Pts',(22.4748413391966,-69.5000413221577,
-219.807779103235));
#224612=CARTESIAN_POINT('Ctrl Pts',(20.5573393020075,-67.3632863153329,
-223.098617135674));
#224613=CARTESIAN_POINT('Ctrl Pts',(18.6398372648184,-65.2265313085082,
-226.389455168112));
#224614=CARTESIAN_POINT('Ctrl Pts',(16.7173760151004,-63.0919383281592,
-229.678857882383));
#224615=CARTESIAN_POINT('Ctrl Pts',(14.7853232876775,-60.9622268937814,
-232.965939947976));
#224616=CARTESIAN_POINT('Ctrl Pts',(27.7294536429034,-73.6399428041712,
-213.240474674736));
#224617=CARTESIAN_POINT('Ctrl Pts',(25.7480542838167,-71.4909831817206,
-216.535913459003));
#224618=CARTESIAN_POINT('Ctrl Pts',(23.7650962505765,-69.3425324796999,
-219.830720327519));
#224619=CARTESIAN_POINT('Ctrl Pts',(21.779547451452,-67.194930644763,-223.124474795611));
#224620=CARTESIAN_POINT('Ctrl Pts',(19.7939986523274,-65.047328809826,-226.418229263702));
#224621=CARTESIAN_POINT('Ctrl Pts',(17.8059306828092,-62.9005566886207,
-229.710963422663));
#224622=CARTESIAN_POINT('Ctrl Pts',(15.8131699469571,-60.7552971507412,
-233.001768361203));
#224623=CARTESIAN_POINT('Ctrl Pts',(29.1336039587918,-73.5700373872199,
-213.265253638125));
#224624=CARTESIAN_POINT('Ctrl Pts',(27.0924699780351,-71.4163743252597,
-216.564463234942));
#224625=CARTESIAN_POINT('Ctrl Pts',(25.0512545912863,-69.2626269169371,
-219.863532185965));
#224626=CARTESIAN_POINT('Ctrl Pts',(23.009917484108,-67.1086533562946,-223.162319906733));
#224627=CARTESIAN_POINT('Ctrl Pts',(20.9685803769297,-64.9546797956521,
-226.461107627501));
#224628=CARTESIAN_POINT('Ctrl Pts',(18.9271177265018,-62.8005017163077,
-229.759627201665));
#224629=CARTESIAN_POINT('Ctrl Pts',(16.8854980114262,-60.6457046773919,
-233.057542008322));
#224630=CARTESIAN_POINT('Ctrl Pts',(30.5241947376933,-73.5610723424065,
-213.298768106723));
#224631=CARTESIAN_POINT('Ctrl Pts',(28.4276303246838,-71.4106207619993,
-216.603490576448));
#224632=CARTESIAN_POINT('Ctrl Pts',(26.3326980553491,-69.2597735546542,
-219.908997954484));
#224633=CARTESIAN_POINT('Ctrl Pts',(24.2404948075201,-67.1083375120314,
-223.215865028163));
#224634=CARTESIAN_POINT('Ctrl Pts',(22.1482915596912,-64.9569014694087,
-226.522732101842));
#224635=CARTESIAN_POINT('Ctrl Pts',(20.0587460706978,-62.804879241495,-229.830915083865));
#224636=CARTESIAN_POINT('Ctrl Pts',(17.9741423861781,-60.6519644373032,
-233.141673289922));
#224637=CARTESIAN_POINT('Ctrl Pts',(31.9147855165948,-73.552107297593,-213.332282575321));
#224638=CARTESIAN_POINT('Ctrl Pts',(29.7627906713323,-71.4048671987388,
-216.642517917954));
#224639=CARTESIAN_POINT('Ctrl Pts',(27.6141415194118,-69.2569201923712,
-219.954463723003));
#224640=CARTESIAN_POINT('Ctrl Pts',(25.4710721309322,-67.1080216677683,
-223.269410149593));
#224641=CARTESIAN_POINT('Ctrl Pts',(23.3280027424525,-64.9591231431653,
-226.584356576183));
#224642=CARTESIAN_POINT('Ctrl Pts',(21.1903744148938,-62.8092567666822,
-229.902202966066));
#224643=CARTESIAN_POINT('Ctrl Pts',(19.0627867609299,-60.6582241972144,
-233.225804571522));
#224644=CARTESIAN_POINT('Ctrl Pts',(33.2915597883743,-73.6042889215309,
-213.3745249105));
#224645=CARTESIAN_POINT('Ctrl Pts',(31.0883634812026,-71.4681526003391,
-216.692012555656));
#224646=CARTESIAN_POINT('Ctrl Pts',(28.8904868213177,-69.3312704464791,
-220.012578308793));
#224647=CARTESIAN_POINT('Ctrl Pts',(26.7014864455774,-67.1937325026255,
-223.338673968425));
#224648=CARTESIAN_POINT('Ctrl Pts',(24.5124860698371,-65.0561945587718,
-226.664769628056));
#224649=CARTESIAN_POINT('Ctrl Pts',(22.3321348006731,-62.917889592856,-229.996164050331));
#224650=CARTESIAN_POINT('Ctrl Pts',(20.1678151009338,-60.7799059276878,
-233.338582766125));
#224651=CARTESIAN_POINT('Ctrl Pts',(34.6658396818832,-73.7171632516111,
-213.428100838228));
#224652=CARTESIAN_POINT('Ctrl Pts',(32.4073514514279,-71.6005216742458,
-216.754800866965));
#224653=CARTESIAN_POINT('Ctrl Pts',(30.156682789701,-69.4835812050588,-220.0867754185));
#224654=CARTESIAN_POINT('Ctrl Pts',(27.9187794471608,-67.3680563271126,
-223.428575651002));
#224655=CARTESIAN_POINT('Ctrl Pts',(25.6808761046207,-65.2525314491663,
-226.770375883503));
#224656=CARTESIAN_POINT('Ctrl Pts',(23.4556914905238,-63.1380571190676,
-230.121736209584));
#224657=CARTESIAN_POINT('Ctrl Pts',(21.2513677279665,-61.0308575536311,
-233.492320591243));
#224658=CARTESIAN_POINT('',(1.75269631448936,-61.4233992294301,-232.850052402311));
#224659=CARTESIAN_POINT('',(3.75861995924126,-61.4153261928714,-232.250048639703));
#224660=CARTESIAN_POINT('Ctrl Pts',(1.75269750311554,-61.4233975212337,
-232.850057162107));
#224661=CARTESIAN_POINT('Ctrl Pts',(1.92316075991213,-61.4229613169472,
-232.80733217942));
#224662=CARTESIAN_POINT('Ctrl Pts',(2.09239735025022,-61.4224645393753,
-232.759040177349));
#224663=CARTESIAN_POINT('Ctrl Pts',(2.40516232917589,-61.4214325003053,
-232.659804474909));
#224664=CARTESIAN_POINT('Ctrl Pts',(2.54699173612178,-61.4209053575993,
-232.609626264845));
#224665=CARTESIAN_POINT('Ctrl Pts',(2.58749755058152,-61.4207526026485,
-232.595189827728));
#224666=CARTESIAN_POINT('Ctrl Pts',(2.59231693841156,-61.4207343791064,
-232.593474272114));
#224667=CARTESIAN_POINT('Ctrl Pts',(2.5994697764427,-61.420707260306,-232.590934719885));
#224668=CARTESIAN_POINT('Ctrl Pts',(2.60233972176209,-61.4206963617489,
-232.589917449231));
#224669=CARTESIAN_POINT('Ctrl Pts',(2.65446877101508,-61.4204981063414,
-232.571459343799));
#224670=CARTESIAN_POINT('Ctrl Pts',(2.70416777645081,-61.420303711325,-232.554260849743));
#224671=CARTESIAN_POINT('Ctrl Pts',(3.08402302180499,-61.4187763761994,
-232.425844903788));
#224672=CARTESIAN_POINT('Ctrl Pts',(3.41955797258862,-61.4171877854095,
-232.329833606325));
#224673=CARTESIAN_POINT('Ctrl Pts',(3.75861934084146,-61.4153271385636,
-232.25004598973));
#224674=CARTESIAN_POINT('',(-1.75269627833716,-61.4233992207715,-232.850052391314));
#224675=CARTESIAN_POINT('Ctrl Pts',(-1.75269547230688,-61.4234026156414,
-232.85005));
#224676=CARTESIAN_POINT('Ctrl Pts',(-1.17332845865336,-61.5217870874547,
-232.85005));
#224677=CARTESIAN_POINT('Ctrl Pts',(-0.588369382046338,-61.5708786969769,
-232.850050000284));
#224678=CARTESIAN_POINT('Ctrl Pts',(0.591121623461373,-61.5706529925896,
-232.850050000284));
#224679=CARTESIAN_POINT('Ctrl Pts',(1.17468362875101,-61.5215566961185,
-232.85005));
#224680=CARTESIAN_POINT('Ctrl Pts',(1.7526954934496,-61.4234026418405,-232.85005));
#224681=CARTESIAN_POINT('',(-3.75861995924035,-61.4153261928713,-232.250048639703));
#224682=CARTESIAN_POINT('Ctrl Pts',(-1.75269746119008,-61.4233975213411,
-232.850057127972));
#224683=CARTESIAN_POINT('Ctrl Pts',(-1.92316007055054,-61.4229613187217,
-232.80733218066));
#224684=CARTESIAN_POINT('Ctrl Pts',(-2.09239806687771,-61.422464537097,
-232.759039771134));
#224685=CARTESIAN_POINT('Ctrl Pts',(-2.40516295459882,-61.4214324981669,
-232.659804234222));
#224686=CARTESIAN_POINT('Ctrl Pts',(-2.54699180261749,-61.4209053573394,
-232.609626241571));
#224687=CARTESIAN_POINT('Ctrl Pts',(-2.58749737645083,-61.4207526033062,
-232.595189889748));
#224688=CARTESIAN_POINT('Ctrl Pts',(-2.59231675754469,-61.420734379791,
-232.593474336454));
#224689=CARTESIAN_POINT('Ctrl Pts',(-2.59946962941021,-61.4207072608641,
-232.590934772013));
#224690=CARTESIAN_POINT('Ctrl Pts',(-2.60233959172383,-61.4206963622429,
-232.589917495322));
#224691=CARTESIAN_POINT('Ctrl Pts',(-2.65446865657193,-61.420498106789,
-232.571459383405));
#224692=CARTESIAN_POINT('Ctrl Pts',(-2.70416771898085,-61.420303711556,
-232.554260869169));
#224693=CARTESIAN_POINT('Ctrl Pts',(-3.08402302193468,-61.4187763761988,
-232.42584490375));
#224694=CARTESIAN_POINT('Ctrl Pts',(-3.41955797265308,-61.4171877854092,
-232.329833606309));
#224695=CARTESIAN_POINT('Ctrl Pts',(-3.75861934084049,-61.4153271385636,
-232.250045989729));
#224696=CARTESIAN_POINT('Ctrl Pts',(-3.75861965563748,-61.4153243588594,
-232.25005));
#224697=CARTESIAN_POINT('Ctrl Pts',(-4.5339585652984,-61.2869745330173,
-232.25005));
#224698=CARTESIAN_POINT('Ctrl Pts',(-5.31753185133202,-61.2192652887292,
-232.250049999975));
#224699=CARTESIAN_POINT('Ctrl Pts',(-6.89308966243379,-61.2051366152526,
-232.250049999975));
#224700=CARTESIAN_POINT('Ctrl Pts',(-7.68211271552188,-61.2596464565366,
-232.25005));
#224701=CARTESIAN_POINT('Ctrl Pts',(-8.46313927246256,-61.3733404249057,
-232.25005));
#224702=CARTESIAN_POINT('',(33.4888861408047,-72.9429671618309,-214.578382767941));
#224703=CARTESIAN_POINT('Ctrl Pts',(-33.4888960070708,-72.9429805807943,
-214.578360966077));
#224704=CARTESIAN_POINT('Ctrl Pts',(-32.3582303407525,-72.9833613098026,
-214.304136356274));
#224705=CARTESIAN_POINT('Ctrl Pts',(-31.1954383806093,-73.0208514112019,
-214.148157206533));
#224706=CARTESIAN_POINT('Ctrl Pts',(-30.0308162541928,-73.0549738991022,
-214.07652205636));
#224707=CARTESIAN_POINT('Ctrl Pts',(-28.8424164729157,-73.08979305309,-214.003424358087));
#224708=CARTESIAN_POINT('Ctrl Pts',(-27.6841438207362,-73.1198927243157,
-214.026849366582));
#224709=CARTESIAN_POINT('Ctrl Pts',(-26.7546989061683,-73.1422369981543,
-214.085588387952));
#224710=CARTESIAN_POINT('Ctrl Pts',(-26.3846816526908,-73.1511323793728,
-214.108972723073));
#224711=CARTESIAN_POINT('Ctrl Pts',(-26.0470604925031,-73.1589301782192,
-214.137473495031));
#224712=CARTESIAN_POINT('Ctrl Pts',(-25.7490556660394,-73.1656334354033,
-214.1665654633));
#224713=CARTESIAN_POINT('Ctrl Pts',(-25.2381704858424,-73.1771251779869,
-214.216439338256));
#224714=CARTESIAN_POINT('Ctrl Pts',(-24.843656759113,-73.1854170412888,
-214.267796851654));
#224715=CARTESIAN_POINT('Ctrl Pts',(-24.6022876971483,-73.1904242292317,
-214.300631104614));
#224716=CARTESIAN_POINT('Ctrl Pts',(-24.5762615999557,-73.1909641391895,
-214.304171522975));
#224717=CARTESIAN_POINT('Ctrl Pts',(-24.5520172332706,-73.191465550504,
-214.307503072173));
#224718=CARTESIAN_POINT('Ctrl Pts',(-24.5296015630572,-73.1919280895696,
-214.310606246882));
#224719=CARTESIAN_POINT('Ctrl Pts',(-24.5181753315148,-73.192163865632,
-214.312188068545));
#224720=CARTESIAN_POINT('Ctrl Pts',(-24.5072235105972,-73.1923896531126,
-214.313705098403));
#224721=CARTESIAN_POINT('Ctrl Pts',(-24.4967513448984,-73.1926055432137,
-214.315147724587));
#224722=CARTESIAN_POINT('Ctrl Pts',(-24.4856096015616,-73.1928352370674,
-214.31668259055));
#224723=CARTESIAN_POINT('Ctrl Pts',(-24.475145401741,-73.1930508945055,
-214.318118499124));
#224724=CARTESIAN_POINT('Ctrl Pts',(-24.4645402940566,-73.193269393582,
-214.31956858846));
#224725=CARTESIAN_POINT('Ctrl Pts',(-24.4216369917593,-73.1941533385836,
-214.325434971244));
#224726=CARTESIAN_POINT('Ctrl Pts',(-24.3787176016695,-73.1950365526006,
-214.331215731291));
#224727=CARTESIAN_POINT('Ctrl Pts',(-24.3357827357383,-73.1959190376299,
-214.336909622653));
#224728=CARTESIAN_POINT('Ctrl Pts',(-24.2501463703594,-73.1976792110641,
-214.348266457021));
#224729=CARTESIAN_POINT('Ctrl Pts',(-24.1644484378959,-73.1994364840595,
-214.359277703943));
#224730=CARTESIAN_POINT('Ctrl Pts',(-24.0786937902358,-73.2011908763299,
-214.369933459421));
#224731=CARTESIAN_POINT('Ctrl Pts',(-23.9081084143817,-73.2046807590709,
-214.391130165404));
#224732=CARTESIAN_POINT('Ctrl Pts',(-23.73729861722,-73.2081592380516,-214.410920190191));
#224733=CARTESIAN_POINT('Ctrl Pts',(-23.5663025513546,-73.2116265266727,
-214.42922541616));
#224734=CARTESIAN_POINT('Ctrl Pts',(-22.8928093732761,-73.2252829533333,
-214.501323243384));
#224735=CARTESIAN_POINT('Ctrl Pts',(-22.2169419775558,-73.2387551891486,
-214.550192391158));
#224736=CARTESIAN_POINT('Ctrl Pts',(-21.5429340824075,-73.2520260634925,
-214.571593675925));
#224737=CARTESIAN_POINT('Ctrl Pts',(-20.2344232034334,-73.2777899804694,
-214.613141874609));
#224738=CARTESIAN_POINT('Ctrl Pts',(-18.9179325307332,-73.3030987781156,
-214.549221422764));
#224739=CARTESIAN_POINT('Ctrl Pts',(-17.6290654905074,-73.3276542359699,
-214.365597122485));
#224740=CARTESIAN_POINT('Ctrl Pts',(-17.3112709393207,-73.333708848637,
-214.320321077499));
#224741=CARTESIAN_POINT('Ctrl Pts',(-16.9943207454879,-73.3397323820754,
-214.267877114593));
#224742=CARTESIAN_POINT('Ctrl Pts',(-16.6776489964845,-73.3457377633419,
-214.208133599092));
#224743=CARTESIAN_POINT('Ctrl Pts',(-16.5202984040686,-73.348721769029,
-214.178447725354));
#224744=CARTESIAN_POINT('Ctrl Pts',(-16.3630167155269,-73.3517012823133,
-214.14695825813));
#224745=CARTESIAN_POINT('Ctrl Pts',(-16.2057362493982,-73.3546778160574,
-214.113641116658));
#224746=CARTESIAN_POINT('Ctrl Pts',(-16.1285703446302,-73.3561381812577,
-214.097294856825));
#224747=CARTESIAN_POINT('Ctrl Pts',(-16.0540481310187,-73.3575478723989,
-214.081112834302));
#224748=CARTESIAN_POINT('Ctrl Pts',(-15.9707337467274,-73.3591230654466,
-214.062497710563));
#224749=CARTESIAN_POINT('Ctrl Pts',(-15.9510424824022,-73.3594953606143,
-214.058098046266));
#224750=CARTESIAN_POINT('Ctrl Pts',(-15.9307720996078,-73.3598788385264,
-214.053523320411));
#224751=CARTESIAN_POINT('Ctrl Pts',(-15.9108326277847,-73.360255350698,
-214.049031142856));
#224752=CARTESIAN_POINT('Ctrl Pts',(-15.8886047025696,-73.3606750751755,
-214.044023398034));
#224753=CARTESIAN_POINT('Ctrl Pts',(-15.866490646101,-73.3610912795177,
-214.039079884622));
#224754=CARTESIAN_POINT('Ctrl Pts',(-15.8444879208456,-73.3615040573541,
-214.034198614662));
#224755=CARTESIAN_POINT('Ctrl Pts',(-15.7996818915998,-73.3623446321283,
-214.02425846761));
#224756=CARTESIAN_POINT('Ctrl Pts',(-15.7553375620968,-73.363170999314,
-214.014576371314));
#224757=CARTESIAN_POINT('Ctrl Pts',(-15.7114332100267,-73.363983929539,
-214.005136319819));
#224758=CARTESIAN_POINT('Ctrl Pts',(-14.8755074705471,-73.3794618780206,
-213.825400561189));
#224759=CARTESIAN_POINT('Ctrl Pts',(-14.200932295193,-73.3903009570716,
-213.725936317316));
#224760=CARTESIAN_POINT('Ctrl Pts',(-13.5220442722281,-73.4002664906795,
-213.649153708601));
#224761=CARTESIAN_POINT('Ctrl Pts',(-12.0023561450994,-73.4225742978466,
-213.477276145754));
#224762=CARTESIAN_POINT('Ctrl Pts',(-10.4375864502759,-73.4395813172516,
-213.449904713926));
#224763=CARTESIAN_POINT('Ctrl Pts',(-8.89412533715207,-73.4506496059436,
-213.554697369729));
#224764=CARTESIAN_POINT('Ctrl Pts',(-8.27388677673257,-73.455097388519,
-213.596808211022));
#224765=CARTESIAN_POINT('Ctrl Pts',(-7.65474848612153,-73.4586193936194,
-213.660275636283));
#224766=CARTESIAN_POINT('Ctrl Pts',(-7.03950648809697,-73.4612182559598,
-213.744499693054));
#224767=CARTESIAN_POINT('Ctrl Pts',(-6.8607698195727,-73.4619732629297,
-213.768967995552));
#224768=CARTESIAN_POINT('Ctrl Pts',(-6.68268475627248,-73.4626454086591,
-213.795231774059));
#224769=CARTESIAN_POINT('Ctrl Pts',(-6.51891006801078,-73.4632010570914,
-213.820863067777));
#224770=CARTESIAN_POINT('Ctrl Pts',(-6.06764672989509,-73.4647320859033,
-213.89148730945));
#224771=CARTESIAN_POINT('Ctrl Pts',(-5.69298242973501,-73.4655622034381,
-213.960560234722));
#224772=CARTESIAN_POINT('Ctrl Pts',(-5.3308760600164,-73.4660981256226,
-214.03375600607));
#224773=CARTESIAN_POINT('Ctrl Pts',(-5.31850955169774,-73.4661164282173,
-214.036255758051));
#224774=CARTESIAN_POINT('Ctrl Pts',(-5.30615791932013,-73.4661343368019,
-214.038761469138));
#224775=CARTESIAN_POINT('Ctrl Pts',(-5.29381864882765,-73.4661518572792,
-214.041273601485));
#224776=CARTESIAN_POINT('Ctrl Pts',(-5.2815968807776,-73.4661692109154,
-214.043761811699));
#224777=CARTESIAN_POINT('Ctrl Pts',(-5.26938778610787,-73.466186132111,
-214.046259128319));
#224778=CARTESIAN_POINT('Ctrl Pts',(-5.25718718520783,-73.4662027904425,
-214.04875708583));
#224779=CARTESIAN_POINT('Ctrl Pts',(-5.23494474483045,-73.4662331595979,
-214.053311014891));
#224780=CARTESIAN_POINT('Ctrl Pts',(-5.2127240106781,-73.466263272517,-214.05783355763));
#224781=CARTESIAN_POINT('Ctrl Pts',(-5.19051019778499,-73.4662931515064,
-214.062327747256));
#224782=CARTESIAN_POINT('Ctrl Pts',(-5.1460600974665,-73.4663529397149,
-214.071320673444));
#224783=CARTESIAN_POINT('Ctrl Pts',(-5.10163770420206,-73.4664117924303,
-214.080200219155));
#224784=CARTESIAN_POINT('Ctrl Pts',(-5.05712471353571,-73.4664698739798,
-214.088988919222));
#224785=CARTESIAN_POINT('Ctrl Pts',(-4.96883161704773,-73.4665850807942,
-214.106421617664));
#224786=CARTESIAN_POINT('Ctrl Pts',(-4.88018237053404,-73.4666972705213,
-214.123499182983));
#224787=CARTESIAN_POINT('Ctrl Pts',(-4.79025277101939,-73.4668075128244,
-214.140369998645));
#224788=CARTESIAN_POINT('Ctrl Pts',(-4.61905021585963,-73.4670173854812,
-214.172487641383));
#224789=CARTESIAN_POINT('Ctrl Pts',(-4.44321791793865,-73.4672204138825,
-214.203890324126));
#224790=CARTESIAN_POINT('Ctrl Pts',(-4.25629393769659,-73.4674212578825,
-214.235206565164));
#224791=CARTESIAN_POINT('Ctrl Pts',(-3.64983483109652,-73.4680728793205,
-214.336809470994));
#224792=CARTESIAN_POINT('Ctrl Pts',(-2.86106847301697,-73.4687282647771,
-214.442238213622));
#224793=CARTESIAN_POINT('Ctrl Pts',(-2.12288746980912,-73.4691288002137,
-214.503638101334));
#224794=CARTESIAN_POINT('Ctrl Pts',(-1.42250617613227,-73.4695088256087,
-214.561893912038));
#224795=CARTESIAN_POINT('Ctrl Pts',(-0.720121136870457,-73.4697481762702,
-214.589437542788));
#224796=CARTESIAN_POINT('Ctrl Pts',(-9.73630898126743E-13,-73.4697481762702,
-214.589437542788));
#224797=CARTESIAN_POINT('Ctrl Pts',(0.702421357999057,-73.4697481762702,
-214.589437542788));
#224798=CARTESIAN_POINT('Ctrl Pts',(1.40882352807894,-73.4695162472501,
-214.563032076116));
#224799=CARTESIAN_POINT('Ctrl Pts',(2.12288573821906,-73.4691288005736,
-214.503638278573));
#224800=CARTESIAN_POINT('Ctrl Pts',(2.75005748515334,-73.4687885002392,
-214.451471798912));
#224801=CARTESIAN_POINT('Ctrl Pts',(3.40090625139601,-73.4682792287222,
-214.369727571729));
#224802=CARTESIAN_POINT('Ctrl Pts',(3.92541310539679,-73.4677620863878,
-214.288535941429));
#224803=CARTESIAN_POINT('Ctrl Pts',(4.03901420267087,-73.467650080346,-214.270950931393));
#224804=CARTESIAN_POINT('Ctrl Pts',(4.14897936068259,-73.4675365646685,
-214.253185445256));
#224805=CARTESIAN_POINT('Ctrl Pts',(4.2562950728238,-73.4674212570593,-214.23520635228));
#224806=CARTESIAN_POINT('Ctrl Pts',(4.44044509701261,-73.467223393218,-214.204354854951));
#224807=CARTESIAN_POINT('Ctrl Pts',(4.61680175851431,-73.4670201417657,
-214.172909458352));
#224808=CARTESIAN_POINT('Ctrl Pts',(4.79025315005858,-73.4668075122857,
-214.140369931774));
#224809=CARTESIAN_POINT('Ctrl Pts',(4.87976449140688,-73.4666977826965,
-214.123577580643));
#224810=CARTESIAN_POINT('Ctrl Pts',(4.96850006460584,-73.4665855133531,
-214.106487083431));
#224811=CARTESIAN_POINT('Ctrl Pts',(5.05712477774532,-73.4664698738595,
-214.088988908638));
#224812=CARTESIAN_POINT('Ctrl Pts',(5.10158648516536,-73.4664118592364,
-214.080210333221));
#224813=CARTESIAN_POINT('Ctrl Pts',(5.14602026857021,-73.4663529932743,
-214.07132873217));
#224814=CARTESIAN_POINT('Ctrl Pts',(5.19051019684309,-73.4662931515016,
-214.06232774779));
#224815=CARTESIAN_POINT('Ctrl Pts',(5.2127183722053,-73.4662632800985,-214.057834698525));
#224816=CARTESIAN_POINT('Ctrl Pts',(5.23494054055089,-73.4662331653379,
-214.053311875695));
#224817=CARTESIAN_POINT('Ctrl Pts',(5.25718718445785,-73.4662027904434,
-214.048757085989));
#224818=CARTESIAN_POINT('Ctrl Pts',(5.26938721880819,-73.4661861328855,
-214.046259244468));
#224819=CARTESIAN_POINT('Ctrl Pts',(5.28159655675219,-73.4661692113754,
-214.043761877671));
#224820=CARTESIAN_POINT('Ctrl Pts',(5.2938186488238,-73.4661518572791,-214.04127360149));
#224821=CARTESIAN_POINT('Ctrl Pts',(5.30615807585072,-73.4661343365795,
-214.038761437274));
#224822=CARTESIAN_POINT('Ctrl Pts',(5.31850995238531,-73.4661164276243,
-214.036255677061));
#224823=CARTESIAN_POINT('Ctrl Pts',(5.33087606001262,-73.4660981256225,
-214.033756006075));
#224824=CARTESIAN_POINT('Ctrl Pts',(5.69862312937633,-73.4655538551284,
-213.959420030091));
#224825=CARTESIAN_POINT('Ctrl Pts',(6.07882234604323,-73.4646941697047,
-213.889738287654));
#224826=CARTESIAN_POINT('Ctrl Pts',(6.51891006800735,-73.4632010570914,
-213.820863067781));
#224827=CARTESIAN_POINT('Ctrl Pts',(7.07951671635194,-73.4612990525228,
-213.733126227511));
#224828=CARTESIAN_POINT('Ctrl Pts',(7.74704151965693,-73.4581513210782,
-213.649508682059));
#224829=CARTESIAN_POINT('Ctrl Pts',(8.38225235563468,-73.4541123126368,
-213.594313827671));
#224830=CARTESIAN_POINT('Ctrl Pts',(8.55274426588832,-73.4530282343659,
-213.579499413892));
#224831=CARTESIAN_POINT('Ctrl Pts',(8.72338814746169,-73.4518739766063,
-213.566289500818));
#224832=CARTESIAN_POINT('Ctrl Pts',(8.89412533714898,-73.4506496059436,
-213.55469736973));
#224833=CARTESIAN_POINT('Ctrl Pts',(10.4367821614907,-73.4395870848738,
-213.449959320781));
#224834=CARTESIAN_POINT('Ctrl Pts',(11.9885581120666,-73.4227768419441,
-213.47571558063));
#224835=CARTESIAN_POINT('Ctrl Pts',(13.5220442722263,-73.4002664906795,
-213.649153708599));
#224836=CARTESIAN_POINT('Ctrl Pts',(14.3005224069512,-73.3888390538237,
-213.737200013717));
#224837=CARTESIAN_POINT('Ctrl Pts',(15.1211380770204,-73.374913797141,-213.878214586776));
#224838=CARTESIAN_POINT('Ctrl Pts',(15.711433210026,-73.3639839295391,-214.005136319814));
#224839=CARTESIAN_POINT('Ctrl Pts',(15.7565784132858,-73.3631480237914,
-214.014843171719));
#224840=CARTESIAN_POINT('Ctrl Pts',(15.8008882476979,-73.3623220005201,
-214.024526095807));
#224841=CARTESIAN_POINT('Ctrl Pts',(15.8444879208452,-73.3615040573542,
-214.034198614657));
#224842=CARTESIAN_POINT('Ctrl Pts',(15.8667829643265,-73.3610857955387,
-214.039144734955));
#224843=CARTESIAN_POINT('Ctrl Pts',(15.8888923011116,-73.3606696445225,
-214.044088191306));
#224844=CARTESIAN_POINT('Ctrl Pts',(15.9108326277843,-73.360255350698,-214.049031142851));
#224845=CARTESIAN_POINT('Ctrl Pts',(15.9309288957193,-73.3598758777838,
-214.053558645112));
#224846=CARTESIAN_POINT('Ctrl Pts',(15.95088806449,-73.3594982801345,-214.058063544314));
#224847=CARTESIAN_POINT('Ctrl Pts',(15.9707337467294,-73.3591230654467,
-214.062497710559));
#224848=CARTESIAN_POINT('Ctrl Pts',(16.0506907171643,-73.3576113497325,
-214.080362679629));
#224849=CARTESIAN_POINT('Ctrl Pts',(16.1287529786783,-73.3561347249074,
-214.097333544679));
#224850=CARTESIAN_POINT('Ctrl Pts',(16.2057362493999,-73.3546778160574,
-214.113641116654));
#224851=CARTESIAN_POINT('Ctrl Pts',(16.3652674515949,-73.3516586871201,
-214.147435037562));
#224852=CARTESIAN_POINT('Ctrl Pts',(16.5201573269693,-73.3487244444233,
-214.178421109645));
#224853=CARTESIAN_POINT('Ctrl Pts',(16.6776489964862,-73.3457377633419,
-214.208133599088));
#224854=CARTESIAN_POINT('Ctrl Pts',(16.9698848482653,-73.3401957858362,
-214.263267020986));
#224855=CARTESIAN_POINT('Ctrl Pts',(17.2708194530509,-73.3344795291924,
-214.314557972668));
#224856=CARTESIAN_POINT('Ctrl Pts',(17.6290654905084,-73.3276542359699,
-214.365597122482));
#224857=CARTESIAN_POINT('Ctrl Pts',(18.0016463094319,-73.3205558369025,
-214.418678542084));
#224858=CARTESIAN_POINT('Ctrl Pts',(18.4365382335761,-73.3122584971473,
-214.472002564731));
#224859=CARTESIAN_POINT('Ctrl Pts',(18.9898749871452,-73.3016297273226,
-214.515254103018));
#224860=CARTESIAN_POINT('Ctrl Pts',(19.5172859611096,-73.2914989528728,
-214.556479154104));
#224861=CARTESIAN_POINT('Ctrl Pts',(20.0662563549184,-73.280892719631,-214.579525909555));
#224862=CARTESIAN_POINT('Ctrl Pts',(20.6050328168092,-73.2703945802866,
-214.583321183555));
#224863=CARTESIAN_POINT('Ctrl Pts',(20.9172357412455,-73.2643112599556,
-214.585520417792));
#224864=CARTESIAN_POINT('Ctrl Pts',(21.2297201296423,-73.2581930877065,
-214.581538931826));
#224865=CARTESIAN_POINT('Ctrl Pts',(21.5429340824073,-73.2520260634924,
-214.571593675926));
#224866=CARTESIAN_POINT('Ctrl Pts',(22.2161471553522,-73.2387708387955,
-214.550217628573));
#224867=CARTESIAN_POINT('Ctrl Pts',(22.8929026451804,-73.2252810620581,
-214.501313258575));
#224868=CARTESIAN_POINT('Ctrl Pts',(23.566302551354,-73.2116265266727,-214.429225416162));
#224869=CARTESIAN_POINT('Ctrl Pts',(23.7340873546836,-73.2082243528482,
-214.411263957672));
#224870=CARTESIAN_POINT('Ctrl Pts',(23.9005400109352,-73.2048355955593,
-214.392070604889));
#224871=CARTESIAN_POINT('Ctrl Pts',(24.0786937902351,-73.2011908763299,
-214.369933459424));
#224872=CARTESIAN_POINT('Ctrl Pts',(24.1624301494928,-73.1994777747612,
-214.359528493708));
#224873=CARTESIAN_POINT('Ctrl Pts',(24.2481278545952,-73.1977206997215,
-214.348534146447));
#224874=CARTESIAN_POINT('Ctrl Pts',(24.3357827357377,-73.1959190376298,
-214.336909622655));
#224875=CARTESIAN_POINT('Ctrl Pts',(24.3782426834008,-73.1950463140904,
-214.331278713511));
#224876=CARTESIAN_POINT('Ctrl Pts',(24.4211619094295,-73.1941631267963,
-214.325499931626));
#224877=CARTESIAN_POINT('Ctrl Pts',(24.4645402940559,-73.1932693935819,
-214.319568588463));
#224878=CARTESIAN_POINT('Ctrl Pts',(24.4752493247181,-73.1930487533603,
-214.318104289219));
#224879=CARTESIAN_POINT('Ctrl Pts',(24.4859863412596,-73.1928274703479,
-214.316630691588));
#224880=CARTESIAN_POINT('Ctrl Pts',(24.4967513448978,-73.1926055432136,
-214.315147724591));
#224881=CARTESIAN_POINT('Ctrl Pts',(24.5076725708397,-73.1923803954608,
-214.313643236697));
#224882=CARTESIAN_POINT('Ctrl Pts',(24.5186222445091,-73.1921546437477,
-214.312126198923));
#224883=CARTESIAN_POINT('Ctrl Pts',(24.5296015630537,-73.1919280895696,
-214.310606246885));
#224884=CARTESIAN_POINT('Ctrl Pts',(24.5536847868459,-73.1914311411526,
-214.307272219828));
#224885=CARTESIAN_POINT('Ctrl Pts',(24.5779134331013,-73.1909298720015,
-214.303946818507));
#224886=CARTESIAN_POINT('Ctrl Pts',(24.6022876971452,-73.1904242292317,
-214.300631104617));
#224887=CARTESIAN_POINT('Ctrl Pts',(24.954073049667,-73.1831264614014,-214.252776548783));
#224888=CARTESIAN_POINT('Ctrl Pts',(25.3362127923774,-73.1749198351962,
-214.206868205789));
#224889=CARTESIAN_POINT('Ctrl Pts',(25.7490556660367,-73.1656334354033,
-214.166565463302));
#224890=CARTESIAN_POINT('Ctrl Pts',(26.6546937674681,-73.1452622045691,
-214.07815483176));
#224891=CARTESIAN_POINT('Ctrl Pts',(27.7073087536273,-73.1198009845544,
-214.013625094252));
#224892=CARTESIAN_POINT('Ctrl Pts',(28.9155236124462,-73.0866210775832,
-214.033403996694));
#224893=CARTESIAN_POINT('Ctrl Pts',(29.2736562011569,-73.0767860669558,
-214.039266753208));
#224894=CARTESIAN_POINT('Ctrl Pts',(29.6479283148488,-73.0661922065524,
-214.052970868027));
#224895=CARTESIAN_POINT('Ctrl Pts',(30.0308162541926,-73.0549738991023,
-214.076522056359));
#224896=CARTESIAN_POINT('Ctrl Pts',(31.1936395115523,-73.0209041166128,
-214.148046559264));
#224897=CARTESIAN_POINT('Ctrl Pts',(32.3571796024045,-72.9833988359979,
-214.303881516735));
#224898=CARTESIAN_POINT('Ctrl Pts',(33.4888960070749,-72.9429805807943,
-214.578360966074));
#224899=CARTESIAN_POINT('',(21.0035817852092,-61.2574554370328,-232.850037376712));
#224900=CARTESIAN_POINT('Ctrl Pts',(21.0035817852092,-61.2574554370328,
-232.850037376712));
#224901=CARTESIAN_POINT('Ctrl Pts',(21.507201965559,-61.7327572754185,-232.106553581838));
#224902=CARTESIAN_POINT('Ctrl Pts',(22.0340605092179,-62.2294925524995,
-231.329524302083));
#224903=CARTESIAN_POINT('Ctrl Pts',(22.584297728091,-62.7476944804053,-230.518968394386));
#224904=CARTESIAN_POINT('Ctrl Pts',(23.0070557094251,-63.1458391232079,
-229.896202489894));
#224905=CARTESIAN_POINT('Ctrl Pts',(23.4436140473167,-63.556655839147,-229.253645314622));
#224906=CARTESIAN_POINT('Ctrl Pts',(23.8940180431183,-63.9801538708211,
-228.59129617684));
#224907=CARTESIAN_POINT('Ctrl Pts',(24.4123301828051,-64.4675033903552,
-227.829083580983));
#224908=CARTESIAN_POINT('Ctrl Pts',(24.9489959478791,-64.9716496124015,
-227.040665559205));
#224909=CARTESIAN_POINT('Ctrl Pts',(25.5041662984108,-65.4925976086513,
-226.226043613375));
#224910=CARTESIAN_POINT('Ctrl Pts',(25.7817514736766,-65.7530716067762,
-225.81873264046));
#224911=CARTESIAN_POINT('Ctrl Pts',(26.0639634999476,-66.0177457474341,
-225.404870543246));
#224912=CARTESIAN_POINT('Ctrl Pts',(26.3508255150318,-66.2866181925986,
-224.984456238475));
#224913=CARTESIAN_POINT('Ctrl Pts',(26.4942565225739,-66.4210544151808,
-224.774249086089));
#224914=CARTESIAN_POINT('Ctrl Pts',(26.6388500325804,-66.5565401775674,
-224.562403862182));
#224915=CARTESIAN_POINT('Ctrl Pts',(26.7846092496479,-66.693075046961,-224.348920320831));
#224916=CARTESIAN_POINT('Ctrl Pts',(26.8574888581816,-66.7613424816577,
-224.242178550156));
#224917=CARTESIAN_POINT('Ctrl Pts',(26.9306598938017,-66.8298721904186,
-224.135027198621));
#224918=CARTESIAN_POINT('Ctrl Pts',(27.0041227667667,-66.8986641033831,
-224.027466226649));
#224919=CARTESIAN_POINT('Ctrl Pts',(27.0408542032493,-66.9330600598653,
-223.973685740662));
#224920=CARTESIAN_POINT('Ctrl Pts',(27.0776585990868,-66.9675215672189,
-223.919802849465));
#224921=CARTESIAN_POINT('Ctrl Pts',(27.1145360066284,-67.0020486157321,
-223.865817547554));
#224922=CARTESIAN_POINT('Ctrl Pts',(27.1468037382272,-67.0322597831812,
-223.818580408381));
#224923=CARTESIAN_POINT('Ctrl Pts',(27.1791273694131,-67.0625211305701,
-223.771264861001));
#224924=CARTESIAN_POINT('Ctrl Pts',(27.2115069356365,-67.0928326509612,
-223.723870901481));
#224925=CARTESIAN_POINT('Ctrl Pts',(27.2161325879541,-67.09716286816,-223.717100335835));
#224926=CARTESIAN_POINT('Ctrl Pts',(27.221744269903,-67.1024160746729,-223.708886619672));
#224927=CARTESIAN_POINT('Ctrl Pts',(27.2253873172964,-67.1058263743519,
-223.703554403788));
#224928=CARTESIAN_POINT('Ctrl Pts',(27.2955613340804,-67.1715171000192,
-223.600842864093));
#224929=CARTESIAN_POINT('Ctrl Pts',(27.3660468581061,-67.2374900781918,
-223.497689857422));
#224930=CARTESIAN_POINT('Ctrl Pts',(27.4368442106614,-67.3037452399979,
-223.394095310731));
#224931=CARTESIAN_POINT('Ctrl Pts',(28.1054064990158,-67.9294141526563,
-222.415818515097));
#224932=CARTESIAN_POINT('Ctrl Pts',(28.8017874464413,-68.5802721850816,
-221.398191038935));
#224933=CARTESIAN_POINT('Ctrl Pts',(29.526328713446,-69.2563390389742,-220.341246127668));
#224934=CARTESIAN_POINT('Ctrl Pts',(30.1857768193341,-69.8716676980254,
-219.379257692358));
#224935=CARTESIAN_POINT('Ctrl Pts',(30.868552817987,-70.5078791976191,-218.384699241817));
#224936=CARTESIAN_POINT('Ctrl Pts',(31.5748931285518,-71.1649718599665,
-217.357564074703));
#224937=CARTESIAN_POINT('Ctrl Pts',(32.1946991469904,-71.7415635972682,
-216.456264023148));
#224938=CARTESIAN_POINT('Ctrl Pts',(32.8326493021217,-72.3342334965497,
-215.529880154047));
#224939=CARTESIAN_POINT('Ctrl Pts',(33.4888861408047,-72.9429671618309,
-214.578382767941));
#224940=CARTESIAN_POINT('',(20.3871357022548,-61.1221564407624,-232.850041788804));
#224941=CARTESIAN_POINT('Ctrl Pts',(20.3871899404023,-61.1221588841747,
-232.85005));
#224942=CARTESIAN_POINT('Ctrl Pts',(20.4903351182918,-61.1426979252128,
-232.85005));
#224943=CARTESIAN_POINT('Ctrl Pts',(20.5932743876311,-61.1642481051802,
-232.850050000001));
#224944=CARTESIAN_POINT('Ctrl Pts',(20.7987564077365,-61.2093548950276,
-232.850050000001));
#224945=CARTESIAN_POINT('Ctrl Pts',(20.9012901690195,-61.2329102063449,
-232.85005));
#224946=CARTESIAN_POINT('Ctrl Pts',(21.0035920114962,-61.2574518715881,
-232.85005));
#224947=CARTESIAN_POINT('',(13.6391777675809,-61.2898273935358,-232.85005));
#224948=CARTESIAN_POINT('Ctrl Pts',(13.6391777675808,-61.2898273935357,
-232.85005));
#224949=CARTESIAN_POINT('Ctrl Pts',(13.7679778534055,-61.2872620754521,
-232.820255967491));
#224950=CARTESIAN_POINT('Ctrl Pts',(13.8962943901741,-61.2846700045695,
-232.788034396798));
#224951=CARTESIAN_POINT('Ctrl Pts',(14.0579979554195,-61.2813584495603,
-232.744562636335));
#224952=CARTESIAN_POINT('Ctrl Pts',(14.0841407462284,-61.2808208278271,
-232.737348171446));
#224953=CARTESIAN_POINT('Ctrl Pts',(14.1136793541503,-61.2802122861796,
-232.729268530917));
#224954=CARTESIAN_POINT('Ctrl Pts',(14.1196218852399,-61.2800897833605,
-232.727647117922));
#224955=CARTESIAN_POINT('Ctrl Pts',(14.1382345388739,-61.2797058487444,
-232.72258133054));
#224956=CARTESIAN_POINT('Ctrl Pts',(14.1509054406719,-61.2794441266197,
-232.719151061028));
#224957=CARTESIAN_POINT('Ctrl Pts',(14.3680771090753,-61.2749523319826,
-232.660673210438));
#224958=CARTESIAN_POINT('Ctrl Pts',(14.5738916280709,-61.2706036847836,
-232.610036215021));
#224959=CARTESIAN_POINT('Ctrl Pts',(15.5130869595282,-61.2503314810904,
-232.401689231487));
#224960=CARTESIAN_POINT('Ctrl Pts',(16.2652400909217,-61.2328950900081,
-232.297341076677));
#224961=CARTESIAN_POINT('Ctrl Pts',(17.5574155716905,-61.2007887070003,
-232.254652621959));
#224962=CARTESIAN_POINT('Ctrl Pts',(18.1075672352859,-61.1864563064502,
-232.278708928573));
#224963=CARTESIAN_POINT('Ctrl Pts',(18.9473592855207,-61.1635855249077,
-232.402122405498));
#224964=CARTESIAN_POINT('Ctrl Pts',(19.2463100800112,-61.1552436964812,
-232.463744244733));
#224965=CARTESIAN_POINT('Ctrl Pts',(19.8287142286265,-61.1386226678887,
-232.626250777395));
#224966=CARTESIAN_POINT('Ctrl Pts',(20.1129420847393,-61.1303255101922,
-232.726867615163));
#224967=CARTESIAN_POINT('Ctrl Pts',(20.3871350980681,-61.1221605172865,
-232.850025366413));
#224968=CARTESIAN_POINT('',(10.1856061283693,-61.3499012171702,-232.85005));
#224969=CARTESIAN_POINT('Ctrl Pts',(10.1856061283695,-61.3499012171691,
-232.85005));
#224970=CARTESIAN_POINT('Ctrl Pts',(10.7540331802441,-61.4387873154263,
-232.85005));
#224971=CARTESIAN_POINT('Ctrl Pts',(11.3321672515837,-61.4795692676092,
-232.85005));
#224972=CARTESIAN_POINT('Ctrl Pts',(12.4893568167562,-61.4603506902607,
-232.85005));
#224973=CARTESIAN_POINT('Ctrl Pts',(13.0690230887892,-61.4003891841391,
-232.85005));
#224974=CARTESIAN_POINT('Ctrl Pts',(13.6391777675808,-61.2898273935355,
-232.85005));
#224975=CARTESIAN_POINT('',(8.46314246804488,-61.3733482641976,-232.250044026166));
#224976=CARTESIAN_POINT('Ctrl Pts',(10.1856061283698,-61.3499012171704,
-232.850049999998));
#224977=CARTESIAN_POINT('Ctrl Pts',(9.82032687378921,-61.3553338539534,
-232.743373739325));
#224978=CARTESIAN_POINT('Ctrl Pts',(9.60751931165371,-61.3583117635075,
-232.640308531512));
#224979=CARTESIAN_POINT('Ctrl Pts',(9.04581817610225,-61.3659623843548,
-232.420098274378));
#224980=CARTESIAN_POINT('Ctrl Pts',(8.75670787170129,-61.3697245641445,
-232.326864869009));
#224981=CARTESIAN_POINT('Ctrl Pts',(8.46321410432618,-61.3733513183578,
-232.25005));
#224982=CARTESIAN_POINT('Ctrl Pts',(3.75861965563843,-61.4153243588596,
-232.25005));
#224983=CARTESIAN_POINT('Ctrl Pts',(4.5340023135914,-61.2869672909125,-232.25005));
#224984=CARTESIAN_POINT('Ctrl Pts',(5.31762015306685,-61.2192576556064,
-232.250049999968));
#224985=CARTESIAN_POINT('Ctrl Pts',(6.89317806954359,-61.2051427085062,
-232.250049999968));
#224986=CARTESIAN_POINT('Ctrl Pts',(7.68215656537121,-61.2596528397479,
-232.25005));
#224987=CARTESIAN_POINT('Ctrl Pts',(8.463139272608,-61.3733404249266,-232.25005));
#224988=CARTESIAN_POINT('Ctrl Pts',(24.1738391241342,37.0431280107547,-233.208100039793));
#224989=CARTESIAN_POINT('Ctrl Pts',(27.6162083218107,41.0700375551415,-226.588760311268));
#224990=CARTESIAN_POINT('Ctrl Pts',(31.0681786417009,45.0961310980358,-219.973963300133));
#224991=CARTESIAN_POINT('Ctrl Pts',(34.5233304970369,49.1218089274639,-213.360583123942));
#224992=CARTESIAN_POINT('Ctrl Pts',(21.9374099124571,36.8211293809628,-233.1017016503));
#224993=CARTESIAN_POINT('Ctrl Pts',(25.111743736431,40.8399102882666,-226.485020448574));
#224994=CARTESIAN_POINT('Ctrl Pts',(28.2953870757527,44.857120760978,-219.871880044709));
#224995=CARTESIAN_POINT('Ctrl Pts',(31.4821075812935,48.8736850008129,-213.259832488631));
#224996=CARTESIAN_POINT('Ctrl Pts',(19.6791533800966,36.9243838380731,-233.031259797898));
#224997=CARTESIAN_POINT('Ctrl Pts',(22.5835629262214,40.9731440158751,-226.416479441913));
#224998=CARTESIAN_POINT('Ctrl Pts',(25.4972748241131,45.0198316409588,-219.804613185821));
#224999=CARTESIAN_POINT('Ctrl Pts',(28.4139919192639,49.0657183803849,-213.193598354232));
#225000=CARTESIAN_POINT('Ctrl Pts',(17.5054530978035,37.329644059109,-232.985683121183));
#225001=CARTESIAN_POINT('Ctrl Pts',(20.1305665853578,41.4552389705233,-226.372636955178));
#225002=CARTESIAN_POINT('Ctrl Pts',(22.7661343835796,45.5778704773325,-219.761939447884));
#225003=CARTESIAN_POINT('Ctrl Pts',(25.4048641344257,49.6994667549787,-213.151865731098));
#225004=CARTESIAN_POINT('Ctrl Pts',(17.2337405625169,37.3803015867384,-232.979986036594));
#225005=CARTESIAN_POINT('Ctrl Pts',(19.8239420427498,41.5155008398544,-226.367156644337));
#225006=CARTESIAN_POINT('Ctrl Pts',(22.4247418285129,45.6476253318793,-219.756605230642));
#225007=CARTESIAN_POINT('Ctrl Pts',(25.0287231613209,49.7786853018029,-213.146649153206));
#225008=CARTESIAN_POINT('Ctrl Pts',(16.9633432334929,37.4356224487032,-232.97468748568));
#225009=CARTESIAN_POINT('Ctrl Pts',(19.518484591489,41.5811860530679,-226.362072247411));
#225010=CARTESIAN_POINT('Ctrl Pts',(22.0843912488166,45.7235559153002,-219.751665537454));
#225011=CARTESIAN_POINT('Ctrl Pts',(24.6535036963345,49.8648302271687,-213.141825886988));
#225012=CARTESIAN_POINT('Ctrl Pts',(16.6944159673799,37.4955299722126,-232.969765709419));
#225013=CARTESIAN_POINT('Ctrl Pts',(19.2143590590312,41.6522508528778,-226.357368433448));
#225014=CARTESIAN_POINT('Ctrl Pts',(21.7452541089279,45.8056509057175,-219.747108569133));
#225015=CARTESIAN_POINT('Ctrl Pts',(24.2793821656715,49.9579228935011,-213.137386917182));
#225016=CARTESIAN_POINT('Ctrl Pts',(16.5599523343234,37.5254837339673,-232.967304821289));
#225017=CARTESIAN_POINT('Ctrl Pts',(19.0622962928022,41.6877832527827,-226.355016526466));
#225018=CARTESIAN_POINT('Ctrl Pts',(21.5756855389835,45.8466984009262,-219.744830084973));
#225019=CARTESIAN_POINT('Ctrl Pts',(24.09232140034,50.0044692266673,-213.135167432279));
#225020=CARTESIAN_POINT('Ctrl Pts',(16.4258562209343,37.5565842202126,-232.964938221388));
#225021=CARTESIAN_POINT('Ctrl Pts',(18.9105665123802,41.7246605912085,-226.352759839903));
#225022=CARTESIAN_POINT('Ctrl Pts',(21.4064203345213,45.8892870285343,-219.742647341783));
#225023=CARTESIAN_POINT('Ctrl Pts',(23.9055351228988,50.0527525170248,-213.133044069172));
#225024=CARTESIAN_POINT('Ctrl Pts',(16.2921470072812,37.5888221841555,-232.962663752566));
#225025=CARTESIAN_POINT('Ctrl Pts',(18.7591903623818,41.7628776356138,-226.35059690245));
#225026=CARTESIAN_POINT('Ctrl Pts',(21.2374799657885,45.9334155456487,-219.740559220295));
#225027=CARTESIAN_POINT('Ctrl Pts',(23.7190454157132,50.1027755574024,-213.131015984566));
#225028=CARTESIAN_POINT('Ctrl Pts',(16.2252924004546,37.6049411661268,-232.961526518156));
#225029=CARTESIAN_POINT('Ctrl Pts',(18.6835022873825,41.7819861578165,-226.349515433724));
#225030=CARTESIAN_POINT('Ctrl Pts',(21.1530097814222,45.9554798042059,-219.739515159551));
#225031=CARTESIAN_POINT('Ctrl Pts',(23.6258005621204,50.1277870775912,-213.130001942264));
#225032=CARTESIAN_POINT('Ctrl Pts',(16.1585345187945,37.6213445208979,-232.96041232234));
#225033=CARTESIAN_POINT('Ctrl Pts',(18.607902620454,41.8014296088707,-226.348457406886));
#225034=CARTESIAN_POINT('Ctrl Pts',(21.0686208064075,45.9779290368421,-219.738494757914));
#225035=CARTESIAN_POINT('Ctrl Pts',(23.53262985142,50.1532335364878,-213.12901172252));
#225036=CARTESIAN_POINT('Ctrl Pts',(16.0918757861226,37.6380311124284,-232.959320930339));
#225037=CARTESIAN_POINT('Ctrl Pts',(18.5323939450749,41.8212073484617,-226.347422665632));
#225038=CARTESIAN_POINT('Ctrl Pts',(20.9843157271392,46.0007630980888,-219.737497897487));
#225039=CARTESIAN_POINT('Ctrl Pts',(23.4395360459604,50.1791152901554,-213.128045237458));
#225040=CARTESIAN_POINT('Ctrl Pts',(16.0585464197866,37.6463744081936,-232.958775234339));
#225041=CARTESIAN_POINT('Ctrl Pts',(18.4946396073852,41.8310962182573,-226.346905295004));
#225042=CARTESIAN_POINT('Ctrl Pts',(20.942163187505,46.0121801287122,-219.736999467274));
#225043=CARTESIAN_POINT('Ctrl Pts',(23.3929891432306,50.1920561669893,-213.127561994927));
#225044=CARTESIAN_POINT('Ctrl Pts',(16.0340227552118,37.651660998028,-232.959574803646));
#225045=CARTESIAN_POINT('Ctrl Pts',(18.4657919650916,41.8377973386214,-226.347688324445));
#225046=CARTESIAN_POINT('Ctrl Pts',(20.9089874042012,46.0203250376801,-219.737774455135));
#225047=CARTESIAN_POINT('Ctrl Pts',(23.3554742352741,50.2016574692251,-213.128330340674));
#225048=CARTESIAN_POINT('Ctrl Pts',(16.0065882955589,37.6578607887702,-232.959932115556));
#225049=CARTESIAN_POINT('Ctrl Pts',(18.433980532035,41.8454422045226,-226.348044075791));
#225050=CARTESIAN_POINT('Ctrl Pts',(20.8728043396308,46.0294291007631,-219.738131122272));
#225051=CARTESIAN_POINT('Ctrl Pts',(23.3149134039151,50.2122277347419,-213.128687613044));
#225052=CARTESIAN_POINT('Ctrl Pts',(15.9791538359061,37.6640605795124,-232.960289427464));
#225053=CARTESIAN_POINT('Ctrl Pts',(18.4021690989782,41.8530870704238,-226.348399827135));
#225054=CARTESIAN_POINT('Ctrl Pts',(20.8366212750604,46.0385331638461,-219.738487789409));
#225055=CARTESIAN_POINT('Ctrl Pts',(23.2743525725561,50.2227980002586,-213.129044885415));
#225056=CARTESIAN_POINT('Ctrl Pts',(15.9517175466003,37.6701942678452,-232.960648289437));
#225057=CARTESIAN_POINT('Ctrl Pts',(18.3703417060476,41.8606571366407,-226.348757259569));
#225058=CARTESIAN_POINT('Ctrl Pts',(20.8004076106497,46.0475539212133,-219.738846178464));
#225059=CARTESIAN_POINT('Ctrl Pts',(23.2337464674417,50.2332764439494,-213.129403912862));
#225060=CARTESIAN_POINT('Ctrl Pts',(15.9242793293033,37.6762620249318,-232.961008682583));
#225061=CARTESIAN_POINT('Ctrl Pts',(18.3384986904741,41.8681523497137,-226.349116370535));
#225062=CARTESIAN_POINT('Ctrl Pts',(20.7641640754571,46.0564910996168,-219.739206294065));
#225063=CARTESIAN_POINT('Ctrl Pts',(23.1930961992297,50.2436625758447,-213.129764705805));
#225064=CARTESIAN_POINT('Ctrl Pts',(15.4852678525495,37.7733461383171,-232.966774972931));
#225065=CARTESIAN_POINT('Ctrl Pts',(17.8290104412988,41.9880757588812,-226.354862145998));
#225066=CARTESIAN_POINT('Ctrl Pts',(20.1842675123756,46.1994859540735,-219.744968143682));
#225067=CARTESIAN_POINT('Ctrl Pts',(22.542691907838,50.4098406861693,-213.135537392885));
#225068=CARTESIAN_POINT('Ctrl Pts',(15.0457657134741,37.8535630790418,-232.972927812655));
#225069=CARTESIAN_POINT('Ctrl Pts',(17.3155230681897,42.0888383893238,-226.361030538136));
#225070=CARTESIAN_POINT('Ctrl Pts',(19.5967238562187,46.3210799188354,-219.751163746593));
#225071=CARTESIAN_POINT('Ctrl Pts',(21.8809817406798,50.5523768769246,-213.141752862445));
#225072=CARTESIAN_POINT('Ctrl Pts',(14.6053482723449,37.9175430616014,-232.979423896539));
#225073=CARTESIAN_POINT('Ctrl Pts',(16.7994169624042,42.1702102018592,-226.367656683047));
#225074=CARTESIAN_POINT('Ctrl Pts',(19.0045202167024,46.4201832439773,-219.757864926228));
#225075=CARTESIAN_POINT('Ctrl Pts',(21.2125144100672,50.6693289807885,-213.14851265933));
#225076=CARTESIAN_POINT('Ctrl Pts',(13.7245133900865,38.0455030267203,-232.992416064308));
#225077=CARTESIAN_POINT('Ctrl Pts',(15.7672047508334,42.3329538269303,-226.380908972868));
#225078=CARTESIAN_POINT('Ctrl Pts',(17.8201129376698,46.6183898942611,-219.771267285497));
#225079=CARTESIAN_POINT('Ctrl Pts',(19.8755797488418,50.9032331885162,-213.162032253098));
#225080=CARTESIAN_POINT('Ctrl Pts',(12.8410916883673,38.1084776461205,-233.006963660748));
#225081=CARTESIAN_POINT('Ctrl Pts',(14.724086953151,42.4181211429224,-226.395942520899));
#225082=CARTESIAN_POINT('Ctrl Pts',(16.6157332633671,46.7264684524801,-219.786529994355));
#225083=CARTESIAN_POINT('Ctrl Pts',(18.5095511653412,51.0344230260212,-213.177478362809));
#225084=CARTESIAN_POINT('Ctrl Pts',(11.955172894378,38.1072504572934,-233.023244257721));
#225085=CARTESIAN_POINT('Ctrl Pts',(13.6810225510899,42.425138848756,-226.412704198706));
#225086=CARTESIAN_POINT('Ctrl Pts',(15.4140075684236,46.7422144596123,-219.803514561937));
#225087=CARTESIAN_POINT('Ctrl Pts',(17.1488260183707,51.0590344085956,-213.194641337275));
#225088=CARTESIAN_POINT('Ctrl Pts',(11.5122134973833,38.1066368628798,-233.031384556208));
#225089=CARTESIAN_POINT('Ctrl Pts',(13.1594903500593,42.4286477016728,-226.42108503761));
#225090=CARTESIAN_POINT('Ctrl Pts',(14.8131447209518,46.7500874631785,-219.812006845727));
#225091=CARTESIAN_POINT('Ctrl Pts',(16.4684634448856,51.0713400998828,-213.203222824509));
#225092=CARTESIAN_POINT('Ctrl Pts',(11.068442842925,38.0899454377874,-233.039926782418));
#225093=CARTESIAN_POINT('Ctrl Pts',(12.638087651299,42.4126385857459,-226.429918907221));
#225094=CARTESIAN_POINT('Ctrl Pts',(14.2132461865494,46.7349565804957,-219.820978804832));
#225095=CARTESIAN_POINT('Ctrl Pts',(15.7898789431435,51.0571445898823,-213.212305200586));
#225096=CARTESIAN_POINT('Ctrl Pts',(10.6242185846299,38.0568674493847,-233.048972600031));
#225097=CARTESIAN_POINT('Ctrl Pts',(12.1179517821572,42.3771929832929,-226.439171170324));
#225098=CARTESIAN_POINT('Ctrl Pts',(13.616560960907,46.6972819912565,-219.83032594524));
#225099=CARTESIAN_POINT('Ctrl Pts',(15.1165093571175,51.0172823841975,-213.221727885471));
#225100=CARTESIAN_POINT('Ctrl Pts',(10.4021064554823,38.0403284551833,-233.053495508837));
#225101=CARTESIAN_POINT('Ctrl Pts',(11.8578838475863,42.3594701820664,-226.443797301875));
#225102=CARTESIAN_POINT('Ctrl Pts',(13.3182183480858,46.6784446966368,-219.834999515444));
#225103=CARTESIAN_POINT('Ctrl Pts',(14.7798245641045,50.9973512813551,-213.226439227913));
#225104=CARTESIAN_POINT('Ctrl Pts',(10.1798442304524,38.0196877247783,-233.058136253378));
#225105=CARTESIAN_POINT('Ctrl Pts',(11.5981402637213,42.3368907999987,-226.448528404105));
#225106=CARTESIAN_POINT('Ctrl Pts',(13.0207092672998,46.6539843758851,-219.839771381179));
#225107=CARTESIAN_POINT('Ctrl Pts',(14.4444911339896,50.971027695944,-213.231243449257));
#225108=CARTESIAN_POINT('Ctrl Pts',(9.95736629516326,37.9948908576778,-233.062889218446));
#225109=CARTESIAN_POINT('Ctrl Pts',(11.3388927023683,42.3094675608905,-226.453369189966));
#225110=CARTESIAN_POINT('Ctrl Pts',(12.72441998614,46.6239835088188,-219.844651948282));
#225111=CARTESIAN_POINT('Ctrl Pts',(14.1111031532653,50.9384648126854,-213.236155478191));
#225112=CARTESIAN_POINT('Ctrl Pts',(9.90174681134099,37.9886916409027,-233.064077459713));
#225113=CARTESIAN_POINT('Ctrl Pts',(11.2740808120301,42.3026117511134,-226.454579386432));
#225114=CARTESIAN_POINT('Ctrl Pts',(12.65034766585,46.6164832920523,-219.845872090057));
#225115=CARTESIAN_POINT('Ctrl Pts',(14.0277561580842,50.9303240918707,-213.237383485424));
#225116=CARTESIAN_POINT('Ctrl Pts',(9.84611383502457,37.9822326217319,-233.065272735655));
#225117=CARTESIAN_POINT('Ctrl Pts',(11.2092999192987,42.2954531938643,-226.45579646572));
#225118=CARTESIAN_POINT('Ctrl Pts',(12.5763515947833,46.6086368083103,-219.847099060522));
#225119=CARTESIAN_POINT('Ctrl Pts',(13.9445307783566,50.9217934508064,-213.238618271349));
#225120=CARTESIAN_POINT('Ctrl Pts',(9.79046632326175,37.9755128618122,-233.066475001199));
#225121=CARTESIAN_POINT('Ctrl Pts',(11.1445526978925,42.2879920750123,-226.457020557358));
#225122=CARTESIAN_POINT('Ctrl Pts',(12.5024378319264,46.6004453814869,-219.84833309334));
#225123=CARTESIAN_POINT('Ctrl Pts',(13.8614363478657,50.9128753563308,-213.23986015266));
#225124=CARTESIAN_POINT('Ctrl Pts',(9.76264256738034,37.9721529818524,-233.067076133971));
#225125=CARTESIAN_POINT('Ctrl Pts',(11.1121790871894,42.2842615155863,-226.457632603177));
#225126=CARTESIAN_POINT('Ctrl Pts',(12.465480950498,46.5963496680752,-219.848950109749));
#225127=CARTESIAN_POINT('Ctrl Pts',(13.8198891326202,50.908416309093,-213.240481093316));
#225128=CARTESIAN_POINT('Ctrl Pts',(9.73481517756063,37.9687279161475,-233.067679014418));
#225129=CARTESIAN_POINT('Ctrl Pts',(11.0798138942533,42.2804553156771,-226.458246402439));
#225130=CARTESIAN_POINT('Ctrl Pts',(12.4285446462698,46.5921677191209,-219.849568892204));
#225131=CARTESIAN_POINT('Ctrl Pts',(13.7783746550183,50.9038603989768,-213.241103808359));
#225132=CARTESIAN_POINT('Ctrl Pts',(9.70698402304477,37.96523754405,-233.068283638575));
#225133=CARTESIAN_POINT('Ctrl Pts',(11.0474574528907,42.2765734980184,-226.458861973485));
#225134=CARTESIAN_POINT('Ctrl Pts',(12.3916296775021,46.5878997014944,-219.850189472689));
#225135=CARTESIAN_POINT('Ctrl Pts',(13.7368940838208,50.899207937222,-213.241728340674));
#225136=CARTESIAN_POINT('Ctrl Pts',(9.70002623441581,37.9643649510258,-233.068434794615));
#225137=CARTESIAN_POINT('Ctrl Pts',(11.0393683425501,42.2756030436037,-226.459015866247));
#225138=CARTESIAN_POINT('Ctrl Pts',(12.3824009353102,46.5868326970878,-219.850344617811));
#225139=CARTESIAN_POINT('Ctrl Pts',(13.7265239410214,50.8980448217833,-213.241884473752));
#225140=CARTESIAN_POINT('Ctrl Pts',(9.69306821049259,37.9634882763409,-233.068586059642));
#225141=CARTESIAN_POINT('Ctrl Pts',(11.0312797791815,42.274627863078,-226.459169869752));
#225142=CARTESIAN_POINT('Ctrl Pts',(12.3731735265874,46.5857603133937,-219.850499875318));
#225143=CARTESIAN_POINT('Ctrl Pts',(13.7161559173791,50.8968756718767,-213.242040720421));
#225144=CARTESIAN_POINT('Ctrl Pts',(9.68610994922948,37.9626075180887,-233.068737433605));
#225145=CARTESIAN_POINT('Ctrl Pts',(11.0231917679977,42.2736479567932,-226.4593239843));
#225146=CARTESIAN_POINT('Ctrl Pts',(12.3639474631874,46.5846825530287,-219.850655245729));
#225147=CARTESIAN_POINT('Ctrl Pts',(13.7057900311691,50.8957004923844,-213.242197081372));
#225148=CARTESIAN_POINT('Ctrl Pts',(9.67915168796636,37.9617267598364,-233.068888807568));
#225149=CARTESIAN_POINT('Ctrl Pts',(11.0151037568139,42.2726680505084,-226.45947809885));
#225150=CARTESIAN_POINT('Ctrl Pts',(12.3547213997873,46.5836047926636,-219.850810616141));
#225151=CARTESIAN_POINT('Ctrl Pts',(13.6954241449592,50.8945253128921,-213.242353442324));
#225152=CARTESIAN_POINT('Ctrl Pts',(9.67042752180553,37.9608610921302,-233.068693023327));
#225153=CARTESIAN_POINT('Ctrl Pts',(11.0052222966165,42.2717086326066,-226.459283167064));
#225154=CARTESIAN_POINT('Ctrl Pts',(12.3436850388287,46.5825507404394,-219.850615812936));
#225155=CARTESIAN_POINT('Ctrl Pts',(13.6832345689085,50.893376327398,-213.242158728148));
#225156=CARTESIAN_POINT('Ctrl Pts',(9.66184542602245,37.9600013369658,-233.068526032011));
#225157=CARTESIAN_POINT('Ctrl Pts',(10.9954862692264,42.2707559642258,-226.459117194178));
#225158=CARTESIAN_POINT('Ctrl Pts',(12.3327965955135,46.5815044535368,-219.850450070761));
#225159=CARTESIAN_POINT('Ctrl Pts',(13.6711951099458,50.8922361823624,-213.241993156658));
#225160=CARTESIAN_POINT('Ctrl Pts',(9.64468123445628,37.9582818266369,-233.068192049379));
#225161=CARTESIAN_POINT('Ctrl Pts',(10.9760142144462,42.2688506274643,-226.458785248407));
#225162=CARTESIAN_POINT('Ctrl Pts',(12.3110197088832,46.5794118797315,-219.850118586413));
#225163=CARTESIAN_POINT('Ctrl Pts',(13.6471161920205,50.8899558922912,-213.241662013679));
#225164=CARTESIAN_POINT('Ctrl Pts',(9.62751103593916,37.9565806023487,-233.067859586963));
#225165=CARTESIAN_POINT('Ctrl Pts',(10.9565400925601,42.2669669096503,-226.45845486089));
#225166=CARTESIAN_POINT('Ctrl Pts',(12.2892446808081,46.5773442546879,-219.84978869258));
#225167=CARTESIAN_POINT('Ctrl Pts',(13.6230430466713,50.8877038777316,-213.241332486873));
#225168=CARTESIAN_POINT('Ctrl Pts',(9.61033490623753,37.9548976948076,-233.067528635586));
#225169=CARTESIAN_POINT('Ctrl Pts',(10.9370639460897,42.2651048145231,-226.458126026541));
#225170=CARTESIAN_POINT('Ctrl Pts',(12.2674715123898,46.5753015551307,-219.849460386617));
#225171=CARTESIAN_POINT('Ctrl Pts',(13.5989756308849,50.8854800884845,-213.241004575592));
#225172=CARTESIAN_POINT('Ctrl Pts',(9.47292586862441,37.9414344344784,-233.064881024575));
#225173=CARTESIAN_POINT('Ctrl Pts',(10.781254774326,42.2502080535059,-226.455495351754));
#225174=CARTESIAN_POINT('Ctrl Pts',(12.0932861650433,46.5589599586724,-219.846833938909));
#225175=CARTESIAN_POINT('Ctrl Pts',(13.4064363045935,50.8676897745073,-213.238381285338));
#225176=CARTESIAN_POINT('Ctrl Pts',(9.33513720062877,37.9291434250167,-233.062330002944));
#225177=CARTESIAN_POINT('Ctrl Pts',(10.6253160438035,42.2366951589798,-226.452964024174));
#225178=CARTESIAN_POINT('Ctrl Pts',(11.9192198479895,46.5442136325115,-219.844309093483));
#225179=CARTESIAN_POINT('Ctrl Pts',(13.2142636771733,50.8517059403811,-213.235861394914));
#225180=CARTESIAN_POINT('Ctrl Pts',(9.19700793929405,37.9180405342928,-233.059871683743));
#225181=CARTESIAN_POINT('Ctrl Pts',(10.4692694200224,42.2245679458519,-226.450529821256));
#225182=CARTESIAN_POINT('Ctrl Pts',(11.7452730443862,46.5310503906422,-219.841884642173));
#225183=CARTESIAN_POINT('Ctrl Pts',(13.0224356883732,50.837502473063,-213.233444529244));
#225184=CARTESIAN_POINT('Ctrl Pts',(8.09197384861627,37.8292174085014,-233.040205130141));
#225185=CARTESIAN_POINT('Ctrl Pts',(9.22089642977294,42.127550240828,-226.431056197904));
#225186=CARTESIAN_POINT('Ctrl Pts',(10.3536986155595,46.4257444556877,-219.822489031695));
#225187=CARTESIAN_POINT('Ctrl Pts',(11.4878117779725,50.7238747345189,-213.214109603883));
#225188=CARTESIAN_POINT('Ctrl Pts',(6.96366628211354,37.817478743917,-233.026371514464));
#225189=CARTESIAN_POINT('Ctrl Pts',(7.96513083913426,42.1193492727609,-226.417759570225));
#225190=CARTESIAN_POINT('Ctrl Pts',(8.96999102861579,46.4210021903668,-219.809524838153));
#225191=CARTESIAN_POINT('Ctrl Pts',(9.97605097124068,50.7225615951693,-213.201412296365));
#225192=CARTESIAN_POINT('Ctrl Pts',(5.84306516179973,37.8861012056782,-233.018416954225));
#225193=CARTESIAN_POINT('Ctrl Pts',(6.71532812355339,42.200163598718,-226.410167180765));
#225194=CARTESIAN_POINT('Ctrl Pts',(7.59093984899072,46.5139246326119,-219.802167559906));
#225195=CARTESIAN_POINT('Ctrl Pts',(8.46772145573762,50.8275648303208,-213.194245174231));
#225196=CARTESIAN_POINT('Ctrl Pts',(5.28276460164283,37.9204124365589,-233.014439674105));
#225197=CARTESIAN_POINT('Ctrl Pts',(6.09042676576295,42.2405707616966,-226.406370986035));
#225198=CARTESIAN_POINT('Ctrl Pts',(6.90141425917819,46.5603858537345,-219.798488920782));
#225199=CARTESIAN_POINT('Ctrl Pts',(7.71355669798609,50.8800664478965,-213.190661613164));
#225200=CARTESIAN_POINT('Ctrl Pts',(4.72420359085666,37.9746163354193,-233.011901696954));
#225201=CARTESIAN_POINT('Ctrl Pts',(5.46710405454763,42.3031873848396,-226.404003962692));
#225202=CARTESIAN_POINT('Ctrl Pts',(6.21329977779021,46.631377304189,-219.796233811454));
#225203=CARTESIAN_POINT('Ctrl Pts',(6.96062066828757,50.9594220750768,-213.188496987808));
#225204=CARTESIAN_POINT('Ctrl Pts',(4.17154639348007,38.0479355872538,-233.010781243767));
#225205=CARTESIAN_POINT('Ctrl Pts',(4.84705870160623,42.3878146595778,-226.403055663777));
#225206=CARTESIAN_POINT('Ctrl Pts',(5.52606587862577,46.7272431542647,-219.795396517945));
#225207=CARTESIAN_POINT('Ctrl Pts',(6.20622728545421,51.0665072531629,-213.187749079048));
#225208=CARTESIAN_POINT('Ctrl Pts',(3.89521779479178,38.084595213171,-233.010221017175));
#225209=CARTESIAN_POINT('Ctrl Pts',(4.53703602513553,42.430128296947,-226.40258151432));
#225210=CARTESIAN_POINT('Ctrl Pts',(5.18244892904355,46.7751760793026,-219.79497787119));
#225211=CARTESIAN_POINT('Ctrl Pts',(5.82903059403753,51.120049842206,-213.187375124668));
#225212=CARTESIAN_POINT('Ctrl Pts',(3.62033230763568,38.1260099641606,-233.010008856396));
#225213=CARTESIAN_POINT('Ctrl Pts',(4.22782250111806,42.4779423112143,-226.402459711852));
#225214=CARTESIAN_POINT('Ctrl Pts',(4.83905947521474,46.8293464189,-219.794913824891));
#225215=CARTESIAN_POINT('Ctrl Pts',(5.45149186218708,51.1805647729974,-213.187357480979));
#225216=CARTESIAN_POINT('Ctrl Pts',(3.3472053680105,38.1720472809816,-233.010141828064));
#225217=CARTESIAN_POINT('Ctrl Pts',(3.91959777386105,42.5312252846951,-226.402693706711));
#225218=CARTESIAN_POINT('Ctrl Pts',(4.49591409333425,46.8898251581957,-219.79521026164));
#225219=CARTESIAN_POINT('Ctrl Pts',(5.07345273996658,51.2482268355656,-213.187703873502));
#225220=CARTESIAN_POINT('Ctrl Pts',(3.31306450055735,38.1778019455842,-233.010158449522));
#225221=CARTESIAN_POINT('Ctrl Pts',(3.88106968295392,42.5378856563802,-226.402722956068));
#225222=CARTESIAN_POINT('Ctrl Pts',(4.4530209205992,46.8973850006076,-219.795247316233));
#225223=CARTESIAN_POINT('Ctrl Pts',(5.02619784968901,51.2566845933866,-213.187747172567));
#225224=CARTESIAN_POINT('Ctrl Pts',(3.27895110668782,38.1836288427124,-233.010180490037));
#225225=CARTESIAN_POINT('Ctrl Pts',(3.84255704326453,42.5446314764555,-226.40275777909));
#225226=CARTESIAN_POINT('Ctrl Pts',(4.41013156071601,46.9050434021283,-219.795290009254));
#225227=CARTESIAN_POINT('Ctrl Pts',(4.97893513726685,51.2652540112937,-213.187796158858));
#225228=CARTESIAN_POINT('Ctrl Pts',(3.24486579879784,38.189527717747,-233.010207966644));
#225229=CARTESIAN_POINT('Ctrl Pts',(3.80406020697863,42.5514626799883,-226.402798194813));
#225230=CARTESIAN_POINT('Ctrl Pts',(4.36724604523574,46.9128004931692,-219.795338357216));
#225231=CARTESIAN_POINT('Ctrl Pts',(4.93166428986477,51.2739354189312,-213.187850846732));
#225232=CARTESIAN_POINT('Ctrl Pts',(3.22782314485287,38.1924771552642,-233.010221704948));
#225233=CARTESIAN_POINT('Ctrl Pts',(3.78481178883567,42.5548782817547,-226.402818402674));
#225234=CARTESIAN_POINT('Ctrl Pts',(4.34580328749561,46.9166790386897,-219.795362531197));
#225235=CARTESIAN_POINT('Ctrl Pts',(4.90802886616373,51.27827612275,-213.187878190669));
#225236=CARTESIAN_POINT('Ctrl Pts',(3.2091142548194,38.1957230397313,-233.010272450532));
#225237=CARTESIAN_POINT('Ctrl Pts',(3.76387619377607,42.5586038688915,-226.402879998958));
#225238=CARTESIAN_POINT('Ctrl Pts',(4.32265861601423,46.9208779346775,-219.795430892831));
#225239=CARTESIAN_POINT('Ctrl Pts',(4.8826791576102,51.2829464276728,-213.187951984205));
#225240=CARTESIAN_POINT('Ctrl Pts',(3.19521896463729,38.1981918611683,-233.010222308172));
#225241=CARTESIAN_POINT('Ctrl Pts',(3.74780277505935,42.5615272078309,-226.402828279549));
#225242=CARTESIAN_POINT('Ctrl Pts',(4.30440722078206,46.924258408687,-219.795377959448));
#225243=CARTESIAN_POINT('Ctrl Pts',(4.86224701055348,51.286785332518,-213.187898031142));
#225244=CARTESIAN_POINT('Ctrl Pts',(3.18132367445518,38.2006606826052,-233.010172165812));
#225245=CARTESIAN_POINT('Ctrl Pts',(3.73172935634261,42.5644505467704,-226.40277656014));
#225246=CARTESIAN_POINT('Ctrl Pts',(4.2861558255499,46.9276388826966,-219.795325026065));
#225247=CARTESIAN_POINT('Ctrl Pts',(4.84181486349676,51.2906242373631,-213.18784407808));
#225248=CARTESIAN_POINT('Ctrl Pts',(3.16743147142012,38.2031124001538,-233.010122353862));
#225249=CARTESIAN_POINT('Ctrl Pts',(3.71565332942976,42.5673549891757,-226.402725177996));
#225250=CARTESIAN_POINT('Ctrl Pts',(4.26789592397522,46.9309986996984,-219.795272437686));
#225251=CARTESIAN_POINT('Ctrl Pts',(4.82136828241006,51.2944407248906,-213.187790477329));
#225252=CARTESIAN_POINT('Ctrl Pts',(3.15354223077676,38.2055470668879,-233.010072871279));
#225253=CARTESIAN_POINT('Ctrl Pts',(3.69957471452757,42.5702405351138,-226.402674131436));
#225254=CARTESIAN_POINT('Ctrl Pts',(4.24962766557925,46.9343378075759,-219.795220191932));
#225255=CARTESIAN_POINT('Ctrl Pts',(4.80090754229887,51.2982346912123,-213.187737225894));
#225256=CARTESIAN_POINT('Ctrl Pts',(3.0979852682033,38.2152857338245,-233.009874940946));
#225257=CARTESIAN_POINT('Ctrl Pts',(3.63526025491884,42.5817827188659,-226.402469945196));
#225258=CARTESIAN_POINT('Ctrl Pts',(4.17655463199535,46.9476942390858,-219.795011208915));
#225259=CARTESIAN_POINT('Ctrl Pts',(4.71906458185412,51.3134105564988,-213.187524220153));
#225260=CARTESIAN_POINT('Ctrl Pts',(3.04247570622088,38.2247515964697,-233.009682277023));
#225261=CARTESIAN_POINT('Ctrl Pts',(3.57090438655314,42.5930225619112,-226.402271124004));
#225262=CARTESIAN_POINT('Ctrl Pts',(4.10334789020144,46.9607193231595,-219.794807702832));
#225263=CARTESIAN_POINT('Ctrl Pts',(4.63699508002042,51.3282260774085,-213.187316797717));
#225264=CARTESIAN_POINT('Ctrl Pts',(2.98700554062687,38.2339479819771,-233.00949483998));
#225265=CARTESIAN_POINT('Ctrl Pts',(3.50650841057442,42.603960046196,-226.402077594881));
#225266=CARTESIAN_POINT('Ctrl Pts',(4.03001700195513,46.9734097359153,-219.79460956207));
#225267=CARTESIAN_POINT('Ctrl Pts',(4.55471661214503,51.3426746460284,-213.187114813067));
#225268=CARTESIAN_POINT('Ctrl Pts',(2.87606520943884,38.2523407529919,-233.009119965892));
#225269=CARTESIAN_POINT('Ctrl Pts',(3.377716458617,42.6258350147655,-226.401690536636));
#225270=CARTESIAN_POINT('Ctrl Pts',(3.88335522546252,46.9987905614268,-219.794213280545));
#225271=CARTESIAN_POINT('Ctrl Pts',(4.39015967639427,51.371571783268,-213.186710843768));
#225272=CARTESIAN_POINT('Ctrl Pts',(2.76528247646328,38.2696557306506,-233.008765954417));
#225273=CARTESIAN_POINT('Ctrl Pts',(3.24876407214238,42.6465005820265,-226.401324592275));
#225274=CARTESIAN_POINT('Ctrl Pts',(3.73619687364432,47.022832683185,-219.793838397139));
#225275=CARTESIAN_POINT('Ctrl Pts',(4.22476690304323,51.399001049048,-213.186328554894));
#225276=CARTESIAN_POINT('Ctrl Pts',(2.65459305129999,38.2859181692768,-233.008433022771));
#225277=CARTESIAN_POINT('Ctrl Pts',(3.11966175705484,42.6659561887148,-226.400979835546));
#225278=CARTESIAN_POINT('Ctrl Pts',(3.58861830572296,47.0455097321839,-219.793484786749));
#225279=CARTESIAN_POINT('Ctrl Pts',(4.05867850381481,51.4249103438683,-213.185967647486));
#225280=CARTESIAN_POINT('Ctrl Pts',(1.76907764999372,38.4160176782863,-233.005769569593));
#225281=CARTESIAN_POINT('Ctrl Pts',(2.08684323635451,42.8216010422206,-226.398221781712));
#225282=CARTESIAN_POINT('Ctrl Pts',(2.40798976235202,47.2269261241753,-219.790655903623));
#225283=CARTESIAN_POINT('Ctrl Pts',(2.72997130998742,51.6321847024301,-213.183080388226));
#225284=CARTESIAN_POINT('Ctrl Pts',(0.890062972301118,38.479927604964,-233.004448903383));
#225285=CARTESIAN_POINT('Ctrl Pts',(1.04391929270151,42.8997957436814,-226.396837718844));
#225286=CARTESIAN_POINT('Ctrl Pts',(1.19912105624254,47.3196638824289,-219.789226534345));
#225287=CARTESIAN_POINT('Ctrl Pts',(1.35468411325127,51.7395320211862,-213.181615349858));
#225288=CARTESIAN_POINT('Ctrl Pts',(-3.8650254009658E-7,38.4799275828018,
-233.004448906301));
#225289=CARTESIAN_POINT('Ctrl Pts',(-2.20334945258451E-7,42.8997957173221,
-226.396837721859));
#225290=CARTESIAN_POINT('Ctrl Pts',(-5.48039408136561E-8,47.3196638518424,
-219.789226537417));
#225291=CARTESIAN_POINT('Ctrl Pts',(1.10556392490902E-7,51.7395319863627,
-213.181615352975));
#225292=CARTESIAN_POINT('Ctrl Pts',(-0.890063745306199,38.4799275606396,
-233.00444890922));
#225293=CARTESIAN_POINT('Ctrl Pts',(-1.0439197333714,42.8997956909628,-226.396837724873));
#225294=CARTESIAN_POINT('Ctrl Pts',(-1.19912116585042,47.3196638212559,
-219.789226540489));
#225295=CARTESIAN_POINT('Ctrl Pts',(-1.35468389213849,51.7395319515393,
-213.181615356092));
#225296=CARTESIAN_POINT('Ctrl Pts',(-1.76907793008316,38.4160177700962,
-233.00576958377));
#225297=CARTESIAN_POINT('Ctrl Pts',(-2.08684470470783,42.8216008459315,
-226.39822179569));
#225298=CARTESIAN_POINT('Ctrl Pts',(-2.40799248287211,47.2269256299894,
-219.790655917783));
#225299=CARTESIAN_POINT('Ctrl Pts',(-2.72997529686207,51.6321839080993,
-213.183080402463));
#225300=CARTESIAN_POINT('Ctrl Pts',(-2.65459339500538,38.2859181503802,
-233.008433046465));
#225301=CARTESIAN_POINT('Ctrl Pts',(-3.11966241780403,42.6659560328282,
-226.400979857926));
#225302=CARTESIAN_POINT('Ctrl Pts',(-3.58861921803428,47.0455094471256,
-219.793484808433));
#225303=CARTESIAN_POINT('Ctrl Pts',(-4.05867966122096,51.4249099306337,
-213.185967668711));
#225304=CARTESIAN_POINT('Ctrl Pts',(-2.76528282812066,38.2696556979156,
-233.008765979303));
#225305=CARTESIAN_POINT('Ctrl Pts',(-3.24876463194106,42.6465004311903,
-226.401324615705));
#225306=CARTESIAN_POINT('Ctrl Pts',(-3.73619755992955,47.0228324242676,
-219.793838419764));
#225307=CARTESIAN_POINT('Ctrl Pts',(-4.22476770676582,51.3990006834506,
-213.186328576992));
#225308=CARTESIAN_POINT('Ctrl Pts',(-2.87606561582561,38.252340690496,-233.00911999099));
#225309=CARTESIAN_POINT('Ctrl Pts',(-3.37771687383254,42.6258348673936,
-226.401690560757));
#225310=CARTESIAN_POINT('Ctrl Pts',(-3.88335557699796,46.9987903386579,
-219.794213304243));
#225311=CARTESIAN_POINT('Ctrl Pts',(-4.39015995698515,51.3715714863033,
-213.186710867252));
#225312=CARTESIAN_POINT('Ctrl Pts',(-2.98700605032629,38.2339478860131,
-233.009494864304));
#225313=CARTESIAN_POINT('Ctrl Pts',(-3.50650877598108,42.6039598904826,
-226.402077618808));
#225314=CARTESIAN_POINT('Ctrl Pts',(-4.0300171714589,46.9734095274016,-219.794609585932));
#225315=CARTESIAN_POINT('Ctrl Pts',(-4.55471658101984,51.342674385518,-213.18711483698));
#225316=CARTESIAN_POINT('Ctrl Pts',(-3.04247626757663,38.2247514837717,
-233.00968230096));
#225317=CARTESIAN_POINT('Ctrl Pts',(-3.57090472705535,42.5930224020271,
-226.402271147832));
#225318=CARTESIAN_POINT('Ctrl Pts',(-4.10334796868937,46.9607191217734,
-219.794807726776));
#225319=CARTESIAN_POINT('Ctrl Pts',(-4.63699489303719,51.3282258351254,
-213.187316821844));
#225320=CARTESIAN_POINT('Ctrl Pts',(-3.09798589335121,38.2152856034861,
-233.009874964222));
#225321=CARTESIAN_POINT('Ctrl Pts',(-3.63526059420306,42.5817825518452,
-226.402469968673));
#225322=CARTESIAN_POINT('Ctrl Pts',(-4.17655465764593,46.9476940393167,
-219.795011232678));
#225323=CARTESIAN_POINT('Ctrl Pts',(-4.71906429187351,51.3134103243417,
-213.187524244216));
#225324=CARTESIAN_POINT('Ctrl Pts',(-3.15354293202228,38.2055469196549,
-233.010072893454));
#225325=CARTESIAN_POINT('Ctrl Pts',(-3.69957509350717,42.5702403566339,
-226.402674154044));
#225326=CARTESIAN_POINT('Ctrl Pts',(-4.24962770925554,46.9343375997015,
-219.795220214898));
#225327=CARTESIAN_POINT('Ctrl Pts',(-4.8009072498816,51.2982344540852,-213.187737249183));
#225328=CARTESIAN_POINT('Ctrl Pts',(-3.16743219169004,38.2031122486971,
-233.010122375761));
#225329=CARTESIAN_POINT('Ctrl Pts',(-3.7156537183332,42.5673548078311,-226.402725200387));
#225330=CARTESIAN_POINT('Ctrl Pts',(-4.26789597215794,46.9309984897978,
-219.795272460453));
#225331=CARTESIAN_POINT('Ctrl Pts',(-4.82136798938362,51.2944404865211,
-213.187790500425));
#225332=CARTESIAN_POINT('Ctrl Pts',(-3.18132441451801,38.200660526972,-233.010172187407));
#225333=CARTESIAN_POINT('Ctrl Pts',(-3.73172975772618,42.5644503622906,
-226.402776582281));
#225334=CARTESIAN_POINT('Ctrl Pts',(-4.28615588266773,46.9276386701613,
-219.795325048593));
#225335=CARTESIAN_POINT('Ctrl Pts',(-4.84181457614597,51.2906239968065,
-213.187844100936));
#225336=CARTESIAN_POINT('Ctrl Pts',(-3.19521972526473,38.1981917014322,
-233.010222329432));
#225337=CARTESIAN_POINT('Ctrl Pts',(-3.74780319174879,42.5615270199239,
-226.402828301403));
#225338=CARTESIAN_POINT('Ctrl Pts',(-4.30440729177531,46.9242581928414,
-219.795377981691));
#225339=CARTESIAN_POINT('Ctrl Pts',(-4.86224673591111,51.2867850887177,
-213.187898053706));
#225340=CARTESIAN_POINT('Ctrl Pts',(-3.20911503601145,38.1957228758924,
-233.010272471457));
#225341=CARTESIAN_POINT('Ctrl Pts',(-3.76387662577141,42.5586036775571,
-226.402880020524));
#225342=CARTESIAN_POINT('Ctrl Pts',(-4.32265870088289,46.9208777155215,
-219.79543091479));
#225343=CARTESIAN_POINT('Ctrl Pts',(-4.88267889567624,51.282946180629,-213.187952006476));
#225344=CARTESIAN_POINT('Ctrl Pts',(-3.22782410538323,38.1924769641916,
-233.010221721999));
#225345=CARTESIAN_POINT('Ctrl Pts',(-3.78481240503387,42.5548780619928,
-226.40281841985));
#225346=CARTESIAN_POINT('Ctrl Pts',(-4.34580355870831,46.9166787905631,
-219.795362548448));
#225347=CARTESIAN_POINT('Ctrl Pts',(-4.90802879230411,51.2782758463453,
-213.187878207983));
#225348=CARTESIAN_POINT('Ctrl Pts',(-3.24486675962954,38.1895275274507,
-233.010207983672));
#225349=CARTESIAN_POINT('Ctrl Pts',(-3.8040608233549,42.5514624611386,-226.402798211965));
#225350=CARTESIAN_POINT('Ctrl Pts',(-4.36724631650623,46.912800246089,-219.795338374444));
#225351=CARTESIAN_POINT('Ctrl Pts',(-4.93166421594236,51.2739351437073,
-213.187850864022));
#225352=CARTESIAN_POINT('Ctrl Pts',(-3.27895206812217,38.1836286539689,
-233.010180507016));
#225353=CARTESIAN_POINT('Ctrl Pts',(-3.84255765999695,42.5446312594299,
-226.402757796196));
#225354=CARTESIAN_POINT('Ctrl Pts',(-4.41013183210206,46.905043157141,-219.795290026436));
#225355=CARTESIAN_POINT('Ctrl Pts',(-4.97893506321885,51.2652537384313,
-213.187796176101));
#225356=CARTESIAN_POINT('Ctrl Pts',(-3.31306546258716,38.1778017583963,
-233.010158466454));
#225357=CARTESIAN_POINT('Ctrl Pts',(-3.8810703000381,42.5378854411796,-226.402722973126));
#225358=CARTESIAN_POINT('Ctrl Pts',(-4.45302119209974,46.8973847577122,
-219.795247333368));
#225359=CARTESIAN_POINT('Ctrl Pts',(-5.0261977755178,51.2566843228826,-213.187747189765));
#225360=CARTESIAN_POINT('Ctrl Pts',(-3.34720633062972,38.1720470953519,
-233.010141844947));
#225361=CARTESIAN_POINT('Ctrl Pts',(-3.91959839129335,42.5312250713203,
-226.402693723722));
#225362=CARTESIAN_POINT('Ctrl Pts',(-4.4959143649488,46.8898249173908,-219.795210278728));
#225363=CARTESIAN_POINT('Ctrl Pts',(-5.07345266567515,51.2482265674168,
-213.187703890653));
#225364=CARTESIAN_POINT('Ctrl Pts',(-3.62033327497023,38.1260097909964,
-233.010008872892));
#225365=CARTESIAN_POINT('Ctrl Pts',(-4.22782312133536,42.4779421124458,
-226.402459728486));
#225366=CARTESIAN_POINT('Ctrl Pts',(-4.83905974774131,46.8293461948202,
-219.794913841607));
#225367=CARTESIAN_POINT('Ctrl Pts',(-5.45149178693396,51.1805645236904,
-213.187357497761));
#225368=CARTESIAN_POINT('Ctrl Pts',(-3.89521876641643,38.0845950526478,
-233.010221033278));
#225369=CARTESIAN_POINT('Ctrl Pts',(-4.53703664788045,42.4301281128367,
-226.402581530569));
#225370=CARTESIAN_POINT('Ctrl Pts',(-5.18244920243109,46.7751758718739,
-219.794977887527));
#225371=CARTESIAN_POINT('Ctrl Pts',(-5.82903051799349,51.1200496115382,
-213.187375141075));
#225372=CARTESIAN_POINT('Ctrl Pts',(-4.17154736896545,38.0479354395528,
-233.010781259488));
#225373=CARTESIAN_POINT('Ctrl Pts',(-4.84705932662186,42.3878144901718,
-226.403055679645));
#225374=CARTESIAN_POINT('Ctrl Pts',(-5.52606615282163,46.7272429633994,
-219.795396533901));
#225375=CARTESIAN_POINT('Ctrl Pts',(-6.20622720878553,51.0665070409123,
-213.187749095075));
#225376=CARTESIAN_POINT('Ctrl Pts',(-4.72420457406351,37.9746162133627,
-233.011901711911));
#225377=CARTESIAN_POINT('Ctrl Pts',(-5.46710468410469,42.3031872448421,
-226.404003977796));
#225378=CARTESIAN_POINT('Ctrl Pts',(-6.21330005360272,46.6313771464505,
-219.79623382665));
#225379=CARTESIAN_POINT('Ctrl Pts',(-6.96062059036963,50.9594218996606,
-213.188497003076));
#225380=CARTESIAN_POINT('Ctrl Pts',(-5.28276558977247,37.9204123410526,
-233.014439688315));
#225381=CARTESIAN_POINT('Ctrl Pts',(-6.0904273987647,42.2405706513073,-226.406371000396));
#225382=CARTESIAN_POINT('Ctrl Pts',(-6.90141453697469,46.5603857286617,
-219.798488935235));
#225383=CARTESIAN_POINT('Ctrl Pts',(-7.71355662058354,50.8800663082066,
-213.19066162769));
#225384=CARTESIAN_POINT('Ctrl Pts',(-5.84306615270387,37.8861011368416,
-233.018416967692));
#225385=CARTESIAN_POINT('Ctrl Pts',(-6.71532875876053,42.2001635180319,
-226.410167194365));
#225386=CARTESIAN_POINT('Ctrl Pts',(-7.59094012855401,46.513924540267,-219.80216757359));
#225387=CARTESIAN_POINT('Ctrl Pts',(-8.46772137968994,50.8275647263818,
-213.194245187983));
#225388=CARTESIAN_POINT('Ctrl Pts',(-6.96366727856668,37.8174787284193,
-233.026371526446));
#225389=CARTESIAN_POINT('Ctrl Pts',(-7.96513147875218,42.1193492514812,
-226.417759582303));
#225390=CARTESIAN_POINT('Ctrl Pts',(-8.96999131171265,46.4210021634777,
-219.8095248503));
#225391=CARTESIAN_POINT('Ctrl Pts',(-9.97605089790276,50.7225615627321,
-213.201412308567));
#225392=CARTESIAN_POINT('Ctrl Pts',(-8.09197483879552,37.8292174475599,
-233.040205140506));
#225393=CARTESIAN_POINT('Ctrl Pts',(-9.22089706830802,42.1275502793173,
-226.431056208459));
#225394=CARTESIAN_POINT('Ctrl Pts',(-10.3536989025166,46.4257444938288,
-219.822489042393));
#225395=CARTESIAN_POINT('Ctrl Pts',(-11.4878117132961,50.7238747723913,
-213.214109614699));
#225396=CARTESIAN_POINT('Ctrl Pts',(-9.19700891511567,37.9180406246053,
-233.059871692371));
#225397=CARTESIAN_POINT('Ctrl Pts',(-10.4692700536151,42.2245680436116,
-226.45052983021));
#225398=CARTESIAN_POINT('Ctrl Pts',(-11.7452733355946,46.5310504960556,
-219.841884651363));
#225399=CARTESIAN_POINT('Ctrl Pts',(-13.0224356370472,50.8375025861988,
-213.233444538625));
#225400=CARTESIAN_POINT('Ctrl Pts',(-9.33513817465568,37.929143521736,-233.062330011354));
#225401=CARTESIAN_POINT('Ctrl Pts',(-10.6253166767785,42.2366952641485,
-226.452964032928));
#225402=CARTESIAN_POINT('Ctrl Pts',(-11.9192201397294,46.544213746334,-219.844309102484));
#225403=CARTESIAN_POINT('Ctrl Pts',(-13.2142636275161,50.8517060629247,
-213.235861404116));
#225404=CARTESIAN_POINT('Ctrl Pts',(-9.47292684075068,37.9414345375616,
-233.064881032772));
#225405=CARTESIAN_POINT('Ctrl Pts',(-10.7812554066213,42.250208166077,-226.455495360308));
#225406=CARTESIAN_POINT('Ctrl Pts',(-12.0932864573056,46.5589600809337,
-219.84683394772));
#225407=CARTESIAN_POINT('Ctrl Pts',(-13.4064362566527,50.8676899065243,
-213.238381294356));
#225408=CARTESIAN_POINT('Ctrl Pts',(-9.61033587635758,37.9548978042124,
-233.067528643578));
#225409=CARTESIAN_POINT('Ctrl Pts',(-10.9370645776426,42.2651049344897,
-226.458126034897));
#225410=CARTESIAN_POINT('Ctrl Pts',(-12.2674718051654,46.5753016858586,
-219.849460395235));
#225411=CARTESIAN_POINT('Ctrl Pts',(-13.5989755847082,50.8854802300378,
-213.241004584421));
#225412=CARTESIAN_POINT('Ctrl Pts',(-9.62751200580844,37.9565807125437,
-233.067859594929));
#225413=CARTESIAN_POINT('Ctrl Pts',(-10.9565407240203,42.2669670305412,
-226.458454869221));
#225414=CARTESIAN_POINT('Ctrl Pts',(-12.2892449736479,46.5773443864743,
-219.849788701174));
#225415=CARTESIAN_POINT('Ctrl Pts',(-13.6230430007151,50.8877040204769,
-213.24133249568));
#225416=CARTESIAN_POINT('Ctrl Pts',(-9.64468220407303,37.9582819376215,
-233.068192057319));
#225417=CARTESIAN_POINT('Ctrl Pts',(-10.9760148458125,42.2688507492795,
-226.458785256713));
#225418=CARTESIAN_POINT('Ctrl Pts',(-12.3110200017871,46.5794120125766,
-219.850118594983));
#225419=CARTESIAN_POINT('Ctrl Pts',(-13.6471161462857,50.8899560362295,
-213.241662022461));
#225420=CARTESIAN_POINT('Ctrl Pts',(-9.66184639538513,37.9600014487392,
-233.068526039926));
#225421=CARTESIAN_POINT('Ctrl Pts',(-10.9954869004979,42.2707560869652,
-226.459117202459));
#225422=CARTESIAN_POINT('Ctrl Pts',(-12.3327968884813,46.5815045874411,
-219.850450079307));
#225423=CARTESIAN_POINT('Ctrl Pts',(-13.671195064433,50.8922363274947,-213.241993165417));
#225424=CARTESIAN_POINT('Ctrl Pts',(-9.67042849104117,37.9608612042982,
-233.068693031229));
#225425=CARTESIAN_POINT('Ctrl Pts',(-11.0052229278407,42.2717087558081,
-226.459283175332));
#225426=CARTESIAN_POINT('Ctrl Pts',(-12.3436853318284,46.5825508748733,
-219.850615821469));
#225427=CARTESIAN_POINT('Ctrl Pts',(-13.6832345235066,50.8933764731273,
-213.242158736895));
#225428=CARTESIAN_POINT('Ctrl Pts',(-9.67915246067952,37.9617268745383,
-233.068888776823));
#225429=CARTESIAN_POINT('Ctrl Pts',(-11.0151041884445,42.272668176984,-226.459478068261));
#225430=CARTESIAN_POINT('Ctrl Pts',(-12.3547214913109,46.5836049308703,
-219.850810585692));
#225431=CARTESIAN_POINT('Ctrl Pts',(-13.6954238965826,50.8945254628113,
-213.242353411989));
#225432=CARTESIAN_POINT('Ctrl Pts',(-9.68611072192926,37.9626076324355,
-233.068737402912));
#225433=CARTESIAN_POINT('Ctrl Pts',(-11.0231921996786,42.2736480828614,
-226.459323953766));
#225434=CARTESIAN_POINT('Ctrl Pts',(-12.3639475548251,46.584682690775,-219.850655215335));
#225435=CARTESIAN_POINT('Ctrl Pts',(-13.7057897829706,50.8957006417903,
-213.242197051092));
#225436=CARTESIAN_POINT('Ctrl Pts',(-9.69306898317901,37.9634883903329,
-233.068586029));
#225437=CARTESIAN_POINT('Ctrl Pts',(-11.0312802109126,42.2746279887388,
-226.459169839269));
#225438=CARTESIAN_POINT('Ctrl Pts',(-12.3731736183394,46.5857604506798,
-219.850499844976));
#225439=CARTESIAN_POINT('Ctrl Pts',(-13.7161556693587,50.8968758207694,
-213.242040690194));
#225440=CARTESIAN_POINT('Ctrl Pts',(-9.70002700708928,37.9643650646628,
-233.068434764026));
#225441=CARTESIAN_POINT('Ctrl Pts',(-11.039368774331,42.275603168857,-226.459015835818));
#225442=CARTESIAN_POINT('Ctrl Pts',(-12.3824010271756,46.5868328339135,
-219.850344587522));
#225443=CARTESIAN_POINT('Ctrl Pts',(-13.7265236931781,50.8980449701626,
-213.241884443579));
#225444=CARTESIAN_POINT('Ctrl Pts',(-9.70698479570498,37.9652376573323,
-233.068283608038));
#225445=CARTESIAN_POINT('Ctrl Pts',(-11.0474578847215,42.2765736228642,
-226.458861943109));
#225446=CARTESIAN_POINT('Ctrl Pts',(-12.3916297694808,46.5878998378596,
-219.850189442454));
#225447=CARTESIAN_POINT('Ctrl Pts',(-13.7368938361541,50.8992080850876,
-213.241728310554));
#225448=CARTESIAN_POINT('Ctrl Pts',(-9.73481595016779,37.9687280280104,
-233.067678984089));
#225449=CARTESIAN_POINT('Ctrl Pts',(-11.0798143262832,42.2804554388931,
-226.458246372274));
#225450=CARTESIAN_POINT('Ctrl Pts',(-12.4285447387014,46.5921678536441,
-219.849568862182));
#225451=CARTESIAN_POINT('Ctrl Pts',(-13.7783744080581,50.9038605447878,
-213.241103778454));
#225452=CARTESIAN_POINT('Ctrl Pts',(-9.76264333993521,37.9721530922971,
-233.067076103849));
#225453=CARTESIAN_POINT('Ctrl Pts',(-11.112179519415,42.2842616371721,-226.457632573223));
#225454=CARTESIAN_POINT('Ctrl Pts',(-12.4654810433745,46.5963498007545,
-219.848950079941));
#225455=CARTESIAN_POINT('Ctrl Pts',(-13.8198888863544,50.908416452846,-213.240481063626));
#225456=CARTESIAN_POINT('Ctrl Pts',(-9.79046709576529,37.9755129708399,
-233.066474971284));
#225457=CARTESIAN_POINT('Ctrl Pts',(-11.1445531303096,42.2879921949675,
-226.457020527615));
#225458=CARTESIAN_POINT('Ctrl Pts',(-12.5024379252396,46.6004455123205,
-219.848333063744));
#225459=CARTESIAN_POINT('Ctrl Pts',(-13.8614361022817,50.9128754980226,
-213.239860123184));
#225460=CARTESIAN_POINT('Ctrl Pts',(-9.84611460742545,37.9822327279253,
-233.065272706155));
#225461=CARTESIAN_POINT('Ctrl Pts',(-11.2093003520988,42.2954533105585,
-226.455796436398));
#225462=CARTESIAN_POINT('Ctrl Pts',(-12.5763516889697,46.6086369354524,
-219.847099031351));
#225463=CARTESIAN_POINT('Ctrl Pts',(-13.9445305341362,50.9217935883757,
-213.238618242301));
#225464=CARTESIAN_POINT('Ctrl Pts',(-9.90174758364278,37.9886917442662,
-233.064077430627));
#225465=CARTESIAN_POINT('Ctrl Pts',(-11.2740812451978,42.302611864545,-226.454579357529));
#225466=CARTESIAN_POINT('Ctrl Pts',(-12.6503477608772,46.6164834154958,
-219.845872061308));
#225467=CARTESIAN_POINT('Ctrl Pts',(-14.0277559151782,50.9303242253047,
-213.2373834568));
#225468=CARTESIAN_POINT('Ctrl Pts',(-9.95736706736925,37.9948909582156,
-233.062889189772));
#225469=CARTESIAN_POINT('Ctrl Pts',(-11.3388931358883,42.309467671058,-226.453369161482));
#225470=CARTESIAN_POINT('Ctrl Pts',(-12.7244200819753,46.6239836285565,
-219.844651919953));
#225471=CARTESIAN_POINT('Ctrl Pts',(-14.1111029116247,50.9384649419709,
-213.236155449989));
#225472=CARTESIAN_POINT('Ctrl Pts',(-10.1798450022751,38.0196878140133,
-233.058136226355));
#225473=CARTESIAN_POINT('Ctrl Pts',(-11.5981406986501,42.3368908971099,
-226.44852837729));
#225474=CARTESIAN_POINT('Ctrl Pts',(-13.0207093663679,46.6539844807995,
-219.839771354532));
#225475=CARTESIAN_POINT('Ctrl Pts',(-14.4444908974109,50.9710278086359,
-213.231243422746));
#225476=CARTESIAN_POINT('Ctrl Pts',(-10.4021072269767,38.0403285331826,
-233.053495483453));
#225477=CARTESIAN_POINT('Ctrl Pts',(-11.8578842836773,42.3594702660982,
-226.443797276706));
#225478=CARTESIAN_POINT('Ctrl Pts',(-13.3182184498665,46.6784447866133,
-219.834999490445));
#225479=CARTESIAN_POINT('Ctrl Pts',(-14.779824331803,50.9973513772468,-213.226439203051));
#225480=CARTESIAN_POINT('Ctrl Pts',(-10.624219355847,38.0568675162082,-233.048972576276));
#225481=CARTESIAN_POINT('Ctrl Pts',(-12.1179522191619,42.3771930542225,
-226.439171146782));
#225482=CARTESIAN_POINT('Ctrl Pts',(-13.6165610648823,46.6972820661859,
-219.830325921867));
#225483=CARTESIAN_POINT('Ctrl Pts',(-15.1165091283142,51.0172824630919,
-213.221727862234));
#225484=CARTESIAN_POINT('Ctrl Pts',(-11.0684436135876,38.0899454822592,
-233.039926761921));
#225485=CARTESIAN_POINT('Ctrl Pts',(-12.6380880901309,42.4126386304711,
-226.429918886935));
#225486=CARTESIAN_POINT('Ctrl Pts',(-14.213246294914,46.734956625331,-219.820978784711));
#225487=CARTESIAN_POINT('Ctrl Pts',(-15.7898787213367,51.0571446347821,
-213.212305180598));
#225488=CARTESIAN_POINT('Ctrl Pts',(-11.5122142673659,38.1066368853063,
-233.031384538877));
#225489=CARTESIAN_POINT('Ctrl Pts',(-13.1594907899084,42.4286477200682,
-226.421085020555));
#225490=CARTESIAN_POINT('Ctrl Pts',(-14.8131448321181,46.7500874773532,
-219.812006828876));
#225491=CARTESIAN_POINT('Ctrl Pts',(-16.4684632276865,51.0713401097786,
-213.203222807822));
#225492=CARTESIAN_POINT('Ctrl Pts',(-11.955173663454,38.1072504577147,-233.023244243446));
#225493=CARTESIAN_POINT('Ctrl Pts',(-13.6810229909314,42.4251388408351,
-226.412704184797));
#225494=CARTESIAN_POINT('Ctrl Pts',(-15.4140076804602,46.7422144431276,
-219.803514548276));
#225495=CARTESIAN_POINT('Ctrl Pts',(-17.1488258029255,51.0590343834786,
-213.194641323813));
#225496=CARTESIAN_POINT('Ctrl Pts',(-12.84109245563,38.1084776025314,-233.006963652583));
#225497=CARTESIAN_POINT('Ctrl Pts',(-14.7240873929774,42.4181210823689,
-226.39594251328));
#225498=CARTESIAN_POINT('Ctrl Pts',(-16.6157333771444,46.7264683746764,
-219.786529987073));
#225499=CARTESIAN_POINT('Ctrl Pts',(-18.5095509534035,51.0344229308787,
-213.177478355796));
#225500=CARTESIAN_POINT('Ctrl Pts',(-13.7245141560456,38.045502939269,-232.992416062106));
#225501=CARTESIAN_POINT('Ctrl Pts',(-15.7672051862484,42.332953713727,-226.380908971242));
#225502=CARTESIAN_POINT('Ctrl Pts',(-17.8201130442209,46.6183897548803,
-219.77126728422));
#225503=CARTESIAN_POINT('Ctrl Pts',(-19.8755795270071,50.9032330228086,
-213.162032252099));
#225504=CARTESIAN_POINT('Ctrl Pts',(-14.6053490349759,37.9175429299717,
-232.979423899816));
#225505=CARTESIAN_POINT('Ctrl Pts',(-16.7994173900859,42.1702100364746,
-226.367656687286));
#225506=CARTESIAN_POINT('Ctrl Pts',(-19.0045203102992,46.4201830445647,
-219.757864931005));
#225507=CARTESIAN_POINT('Ctrl Pts',(-21.2125141699292,50.6693287472216,
-213.14851266454));
#225508=CARTESIAN_POINT('Ctrl Pts',(-15.0457664744411,37.8535629253232,
-232.97292781867));
#225509=CARTESIAN_POINT('Ctrl Pts',(-17.3155234920046,42.0888381978483,
-226.361030545308));
#225510=CARTESIAN_POINT('Ctrl Pts',(-19.5967239433384,46.3210796894069,
-219.751163754398));
#225511=CARTESIAN_POINT('Ctrl Pts',(-21.8809814913902,50.552376609428,-213.14175287076));
#225512=CARTESIAN_POINT('Ctrl Pts',(-15.48526861201,37.7733459621789,-232.966774981656));
#225513=CARTESIAN_POINT('Ctrl Pts',(-17.8290108602587,41.988075541514,-226.354862155988));
#225514=CARTESIAN_POINT('Ctrl Pts',(-20.1842675910139,46.1994856953577,
-219.744968154358));
#225515=CARTESIAN_POINT('Ctrl Pts',(-22.5426916464067,50.4098403859979,
-213.135537404114));
#225516=CARTESIAN_POINT('Ctrl Pts',(-15.9242800874034,37.6762618259859,
-232.961008694015));
#225517=CARTESIAN_POINT('Ctrl Pts',(-18.3384991035959,41.8681521066547,
-226.349116383292));
#225518=CARTESIAN_POINT('Ctrl Pts',(-20.764164143618,46.056490812383,-219.739206307543));
#225519=CARTESIAN_POINT('Ctrl Pts',(-23.1930959226737,50.2436622443285,
-213.129764719864));
#225520=CARTESIAN_POINT('Ctrl Pts',(-15.9517183046155,37.6701940674739,
-232.960648301037));
#225521=CARTESIAN_POINT('Ctrl Pts',(-18.3703421188045,41.860656891976,-226.348757272499));
#225522=CARTESIAN_POINT('Ctrl Pts',(-20.8004076781558,46.0475536321971,
-219.738846192116));
#225523=CARTESIAN_POINT('Ctrl Pts',(-23.2337461899404,50.2332761104742,
-213.129403927098));
#225524=CARTESIAN_POINT('Ctrl Pts',(-15.9791545938371,37.6640603777139,
-232.960289439234));
#225525=CARTESIAN_POINT('Ctrl Pts',(-18.4021695113665,41.8530868241542,
-226.348399840238));
#225526=CARTESIAN_POINT('Ctrl Pts',(-20.8366213419039,46.0385328730506,
-219.738487803237));
#225527=CARTESIAN_POINT('Ctrl Pts',(-23.2743522940981,50.2227976648295,
-213.129044899828));
#225528=CARTESIAN_POINT('Ctrl Pts',(-16.0065890534061,37.6578605855432,
-232.959932127495));
#225529=CARTESIAN_POINT('Ctrl Pts',(-18.4339809440506,41.8454419566488,
-226.348044089065));
#225530=CARTESIAN_POINT('Ctrl Pts',(-20.8728044058038,46.0294288081912,
-219.738131136274));
#225531=CARTESIAN_POINT('Ctrl Pts',(-23.3149131244886,50.2122273973641,
-213.128687627634));
#225532=CARTESIAN_POINT('Ctrl Pts',(-16.0340235129751,37.6516607933725,
-232.959574815754));
#225533=CARTESIAN_POINT('Ctrl Pts',(-18.4657923767348,41.8377970891434,
-226.347688337893));
#225534=CARTESIAN_POINT('Ctrl Pts',(-20.9089874697038,46.0203247433318,
-219.737774469313));
#225535=CARTESIAN_POINT('Ctrl Pts',(-23.3554739548789,50.2016571298987,
-213.128330355439));
#225536=CARTESIAN_POINT('Ctrl Pts',(-16.0585473554683,37.6463741383586,
-232.958775273912));
#225537=CARTESIAN_POINT('Ctrl Pts',(-18.4946401987194,41.8310959004748,
-226.346905335007));
#225538=CARTESIAN_POINT('Ctrl Pts',(-20.9421634338297,46.0121797638875,
-219.736999507462));
#225539=CARTESIAN_POINT('Ctrl Pts',(-23.3929890444876,50.192055755358,-213.127562035262));
#225540=CARTESIAN_POINT('Ctrl Pts',(-16.0918767223523,37.6380308441171,
-232.959320969893));
#225541=CARTESIAN_POINT('Ctrl Pts',(-18.5323945369195,41.821207032461,-226.347422705618));
#225542=CARTESIAN_POINT('Ctrl Pts',(-20.9843159739407,46.0007627353008,
-219.737497937658));
#225543=CARTESIAN_POINT('Ctrl Pts',(-23.4395359476608,50.1791148808152,
-213.128045277776));
#225544=CARTESIAN_POINT('Ctrl Pts',(-16.1585354561205,37.6213442556341,
-232.960412361857));
#225545=CARTESIAN_POINT('Ctrl Pts',(-18.6079032133198,41.8014292964334,
-226.348457446837));
#225546=CARTESIAN_POINT('Ctrl Pts',(-21.0686210541628,45.9779286781272,
-219.73849479805));
#225547=CARTESIAN_POINT('Ctrl Pts',(-23.532629754007,50.1532331317297,-213.129011762805));
#225548=CARTESIAN_POINT('Ctrl Pts',(-16.2252933388625,37.6049409039171,
-232.961526557635));
#225549=CARTESIAN_POINT('Ctrl Pts',(-18.6835028812545,41.7819858489469,
-226.349515473638));
#225550=CARTESIAN_POINT('Ctrl Pts',(-21.1530100301158,45.955479449566,-219.739515199653));
#225551=CARTESIAN_POINT('Ctrl Pts',(-23.6258004655779,50.1277866774147,
-213.130001982515));
#225552=CARTESIAN_POINT('Ctrl Pts',(-16.2921479467574,37.5888219250063,
-232.962663792009));
#225553=CARTESIAN_POINT('Ctrl Pts',(-18.7591909572452,41.7628773303161,
-226.350596942329));
#225554=CARTESIAN_POINT('Ctrl Pts',(-21.2374802154051,45.9334151950853,
-219.740559260363));
#225555=CARTESIAN_POINT('Ctrl Pts',(-23.7190453200257,50.1027751618064,
-213.131016024784));
#225556=CARTESIAN_POINT('Ctrl Pts',(-16.425857162547,37.5565839671848,-232.964938260758));
#225557=CARTESIAN_POINT('Ctrl Pts',(-18.9105671092267,41.7246602930543,
-226.352759879711));
#225558=CARTESIAN_POINT('Ctrl Pts',(-21.4064205859838,45.889286686124,-219.742647381781));
#225559=CARTESIAN_POINT('Ctrl Pts',(-23.9055350289214,50.0527521305898,
-213.133044109322));
#225560=CARTESIAN_POINT('Ctrl Pts',(-16.5599532780166,37.5254834870874,
-232.967304860586));
#225561=CARTESIAN_POINT('Ctrl Pts',(-19.0622968915723,41.6877829617887,
-226.355016566202));
#225562=CARTESIAN_POINT('Ctrl Pts',(-21.5756857922305,45.8466980666759,
-219.744830124902));
#225563=CARTESIAN_POINT('Ctrl Pts',(-24.0923213080095,50.0044688493901,
-213.135167472361));
#225564=CARTESIAN_POINT('Ctrl Pts',(-16.6944169130979,37.4955297315077,
-232.969765748647));
#225565=CARTESIAN_POINT('Ctrl Pts',(-19.2143596596656,41.6522505690609,
-226.357368473114));
#225566=CARTESIAN_POINT('Ctrl Pts',(-21.7452543638979,45.8056505796339,
-219.747108608993));
#225567=CARTESIAN_POINT('Ctrl Pts',(-24.2793820749247,49.9579225253783,
-213.137386957196));
#225568=CARTESIAN_POINT('Ctrl Pts',(-16.9633441832605,37.4356222203481,
-232.974687524767));
#225569=CARTESIAN_POINT('Ctrl Pts',(-19.5184851958523,41.5811857836052,
-226.362072286937));
#225570=CARTESIAN_POINT('Ctrl Pts',(-22.0843915072326,45.72355560555,-219.751665577176));
#225571=CARTESIAN_POINT('Ctrl Pts',(-24.6535036087552,49.8648298773548,
-213.141825926864));
#225572=CARTESIAN_POINT('Ctrl Pts',(-17.2337415161106,37.3803013708413,
-232.97998607555));
#225573=CARTESIAN_POINT('Ctrl Pts',(-19.8239426506046,41.5155005848133,
-226.367156683727));
#225574=CARTESIAN_POINT('Ctrl Pts',(-22.424742090129,45.6476250384896,-219.756605270226));
#225575=CARTESIAN_POINT('Ctrl Pts',(-25.0287230766563,49.7786849702844,
-213.146649192944));
#225576=CARTESIAN_POINT('Ctrl Pts',(-17.5054540549992,37.3296438557812,
-232.985683160017));
#225577=CARTESIAN_POINT('Ctrl Pts',(-20.1305671964664,41.4552387299725,
-226.372636994436));
#225578=CARTESIAN_POINT('Ctrl Pts',(-22.7661346481492,45.5778702003308,
-219.761939487332));
#225579=CARTESIAN_POINT('Ctrl Pts',(-25.4048640524227,49.6994664417413,
-213.151865770696));
#225580=CARTESIAN_POINT('Ctrl Pts',(-19.6791543661082,36.9243837353004,
-233.031259835762));
#225581=CARTESIAN_POINT('Ctrl Pts',(-22.5835635633614,40.9731438912471,
-226.416479480112));
#225582=CARTESIAN_POINT('Ctrl Pts',(-25.4972751123102,45.0198314950608,
-219.804613224178));
#225583=CARTESIAN_POINT('Ctrl Pts',(-28.4139918585542,49.0657182133968,
-213.193598392712));
#225584=CARTESIAN_POINT('Ctrl Pts',(-21.9374109084496,36.8211293864807,
-233.101701686809));
#225585=CARTESIAN_POINT('Ctrl Pts',(-25.111744382231,40.8399102842966,-226.485020485526));
#225586=CARTESIAN_POINT('Ctrl Pts',(-28.2953873712226,44.8571207481071,
-219.871880081892));
#225587=CARTESIAN_POINT('Ctrl Pts',(-31.4821075264257,48.8736849792366,
-213.259832525996));
#225588=CARTESIAN_POINT('Ctrl Pts',(-24.1738401119771,37.0431281239647,
-233.208100074818));
#225589=CARTESIAN_POINT('Ctrl Pts',(-27.6162089587335,41.0700376714878,
-226.588760346578));
#225590=CARTESIAN_POINT('Ctrl Pts',(-31.0681789277548,45.0961312181189,
-219.973963335611));
#225591=CARTESIAN_POINT('Ctrl Pts',(-34.5233304322506,49.1218090514821,
-213.360583159555));
#225592=CARTESIAN_POINT('',(23.1986390639935,37.1456077148496,-232.850148134873));
#225593=CARTESIAN_POINT('',(23.9219400150789,37.2105701781699,-232.850048861683));
#225594=CARTESIAN_POINT('Ctrl Pts',(23.1986878229135,37.1456673944601,-232.85005));
#225595=CARTESIAN_POINT('Ctrl Pts',(23.3194048257383,37.1546203352643,-232.85005));
#225596=CARTESIAN_POINT('Ctrl Pts',(23.4400515103151,37.1645093048432,-232.85005));
#225597=CARTESIAN_POINT('Ctrl Pts',(23.6811421252914,37.1861530761466,-232.85005));
#225598=CARTESIAN_POINT('Ctrl Pts',(23.8015841730299,37.1979071335885,-232.85005));
#225599=CARTESIAN_POINT('Ctrl Pts',(23.9219289933242,37.2105934913504,-232.85005));
#225600=CARTESIAN_POINT('',(33.4675954689601,48.355842190426,-214.55199127893));
#225601=CARTESIAN_POINT('Ctrl Pts',(23.9219400150789,37.2105701781699,-232.850048861683));
#225602=CARTESIAN_POINT('Ctrl Pts',(24.4418606617069,37.878778891458,-231.743275247233));
#225603=CARTESIAN_POINT('Ctrl Pts',(24.9947791463521,38.5760331124526,-230.591022418697));
#225604=CARTESIAN_POINT('Ctrl Pts',(25.5827531876322,39.3022826557374,-229.39331304588));
#225605=CARTESIAN_POINT('Ctrl Pts',(25.7351746609535,39.4905495138209,-229.082828884338));
#225606=CARTESIAN_POINT('Ctrl Pts',(25.8899517028263,39.6807648773527,-228.769290034352));
#225607=CARTESIAN_POINT('Ctrl Pts',(26.0471192761083,39.8729278713654,-228.45269696414));
#225608=CARTESIAN_POINT('Ctrl Pts',(26.4288443515238,40.3396490394141,-227.683762819018));
#225609=CARTESIAN_POINT('Ctrl Pts',(26.8246878338526,40.8178589630018,-226.896809721117));
#225610=CARTESIAN_POINT('Ctrl Pts',(27.2352389947482,41.3075425018447,-226.091828317012));
#225611=CARTESIAN_POINT('Ctrl Pts',(27.440514575196,41.5523842712661,-225.689337614959));
#225612=CARTESIAN_POINT('Ctrl Pts',(27.6494678664072,41.8000944125765,-225.282339642736));
#225613=CARTESIAN_POINT('Ctrl Pts',(27.8621772375357,42.0506708295902,-224.870831918007));
#225614=CARTESIAN_POINT('Ctrl Pts',(27.9685319231,42.1759590380971,-224.665078055643));
#225615=CARTESIAN_POINT('Ctrl Pts',(28.0758256277802,42.3019638116919,-224.458196752125));
#225616=CARTESIAN_POINT('Ctrl Pts',(28.1840684939521,42.4286848767254,-224.250187589526));
#225617=CARTESIAN_POINT('Ctrl Pts',(28.238189927038,42.4920454092422,-224.146183008227));
#225618=CARTESIAN_POINT('Ctrl Pts',(28.292548650422,42.5555850143397,-224.041896461924));
#225619=CARTESIAN_POINT('Ctrl Pts',(28.3471459410457,42.6193036567116,-223.937327894143));
#225620=CARTESIAN_POINT('Ctrl Pts',(28.3744445863575,42.6511629778975,-223.885043610253));
#225621=CARTESIAN_POINT('Ctrl Pts',(28.4018028734742,42.6830670583836,-223.832688820977));
#225622=CARTESIAN_POINT('Ctrl Pts',(28.4292209631686,42.7150158936996,-223.78026351885));
#225623=CARTESIAN_POINT('Ctrl Pts',(28.4532117916512,42.742971124601,-223.734391379489));
#225624=CARTESIAN_POINT('Ctrl Pts',(28.477248406482,42.770960620918,-223.688465253726));
#225625=CARTESIAN_POINT('Ctrl Pts',(28.5013309157674,42.7989843796288,-223.642485136405));
#225626=CARTESIAN_POINT('Ctrl Pts',(28.5047712742368,42.8029877737304,-223.635916548216));
#225627=CARTESIAN_POINT('Ctrl Pts',(28.5087290203377,42.8075927211393,-223.628361017554));
#225628=CARTESIAN_POINT('Ctrl Pts',(28.5116548013666,42.8109966596226,-223.622776066215));
#225629=CARTESIAN_POINT('Ctrl Pts',(28.8371805675898,43.1897227748008,-223.001387949309));
#225630=CARTESIAN_POINT('Ctrl Pts',(29.1745459726135,43.5788145813041,-222.363412782327));
#225631=CARTESIAN_POINT('Ctrl Pts',(29.5240447341431,43.9782923394872,-221.70885488244));
#225632=CARTESIAN_POINT('Ctrl Pts',(29.5766255923689,44.0383923618034,-221.610378950841));
#225633=CARTESIAN_POINT('Ctrl Pts',(29.6294811733118,44.0987274444299,-221.511527682382));
#225634=CARTESIAN_POINT('Ctrl Pts',(29.6826125773133,44.1592976381529,-221.412301090776));
#225635=CARTESIAN_POINT('Ctrl Pts',(29.8857573664897,44.390884201043,-221.03291407078));
#225636=CARTESIAN_POINT('Ctrl Pts',(30.0929331856782,44.6259080707781,-220.648040158275));
#225637=CARTESIAN_POINT('Ctrl Pts',(30.3042007923876,44.864372719193,-220.257679030983));
#225638=CARTESIAN_POINT('Ctrl Pts',(30.4098345957423,44.9836050434004,-220.062498467337));
#225639=CARTESIAN_POINT('Ctrl Pts',(30.5164913454516,45.1036975586825,-219.865946097492));
#225640=CARTESIAN_POINT('Ctrl Pts',(30.6241789389476,45.2246506847414,-219.668021790972));
#225641=CARTESIAN_POINT('Ctrl Pts',(30.6780227356957,45.2851272477709,-219.569059637713));
#225642=CARTESIAN_POINT('Ctrl Pts',(30.7321242433433,45.3458189632478,-219.4697545001));
#225643=CARTESIAN_POINT('Ctrl Pts',(30.7864844571222,45.4067258825371,-219.370106358403));
#225644=CARTESIAN_POINT('Ctrl Pts',(30.8136645640117,45.4371793421818,-219.320282287555));
#225645=CARTESIAN_POINT('Ctrl Pts',(30.8409093474307,45.4676866027635,-219.270372465674));
#225646=CARTESIAN_POINT('Ctrl Pts',(30.8682189327952,45.4982476706417,-219.220376889958));
#225647=CARTESIAN_POINT('Ctrl Pts',(30.8887011218186,45.5211684715504,-219.182880208172));
#225648=CARTESIAN_POINT('Ctrl Pts',(30.9092197619361,45.5441195390619,-219.145335289853));
#225649=CARTESIAN_POINT('Ctrl Pts',(30.9297749062752,45.5671008758434,-219.107742133744));
#225650=CARTESIAN_POINT('Ctrl Pts',(30.9366266210549,45.5747613214372,-219.095211081708));
#225651=CARTESIAN_POINT('Ctrl Pts',(30.9443340309044,45.5833769999799,-219.081117624891));
#225652=CARTESIAN_POINT('Ctrl Pts',(30.9503422206756,45.5900923024801,-219.070132898319));
#225653=CARTESIAN_POINT('Ctrl Pts',(31.2808092427288,45.9594524764969,-218.465942615328));
#225654=CARTESIAN_POINT('Ctrl Pts',(31.6240078517053,46.3403008201657,-217.843285810584));
#225655=CARTESIAN_POINT('Ctrl Pts',(31.9801868039357,46.7326727266222,-217.202164072734));
#225656=CARTESIAN_POINT('Ctrl Pts',(32.3336946073896,47.1221020567942,-216.565850399861));
#225657=CARTESIAN_POINT('Ctrl Pts',(32.6999887764574,47.5228828432546,-215.911347715658));
#225658=CARTESIAN_POINT('Ctrl Pts',(33.0793631737681,47.935041240388,-215.23865685648));
#225659=CARTESIAN_POINT('Ctrl Pts',(33.2072821834606,48.0740144931206,-215.011836203464));
#225660=CARTESIAN_POINT('Ctrl Pts',(33.3366887540973,48.2142812245276,-214.782947673812));
#225661=CARTESIAN_POINT('Ctrl Pts',(33.4675954689601,48.355842190426,-214.55199127893));
#225662=CARTESIAN_POINT('Ctrl Pts',(33.4676028656973,48.3558414173478,-214.551973774401));
#225663=CARTESIAN_POINT('Ctrl Pts',(30.901862658951,48.7536658275797,-213.450221490923));
#225664=CARTESIAN_POINT('Ctrl Pts',(28.0171449119245,49.1337591199062,-213.211816166462));
#225665=CARTESIAN_POINT('Ctrl Pts',(25.2356859051905,49.4352084301762,-213.575672669215));
#225666=CARTESIAN_POINT('Ctrl Pts',(24.8032357476663,49.482076567149,-213.632243627676));
#225667=CARTESIAN_POINT('Ctrl Pts',(24.3877560644765,49.5255154092148,-213.701836863213));
#225668=CARTESIAN_POINT('Ctrl Pts',(24.03731337216,49.561263296092,-213.768798684283));
#225669=CARTESIAN_POINT('Ctrl Pts',(23.8252559380841,49.5828948076944,-213.80931815371));
#225670=CARTESIAN_POINT('Ctrl Pts',(23.6273316981886,49.6027398562885,-213.850344519519));
#225671=CARTESIAN_POINT('Ctrl Pts',(23.4328829972625,49.6219541201266,-213.893239486649));
#225672=CARTESIAN_POINT('Ctrl Pts',(23.3313424796551,49.6319877500057,-213.915639107446));
#225673=CARTESIAN_POINT('Ctrl Pts',(23.230757278012,49.6418462076065,-213.938569475617));
#225674=CARTESIAN_POINT('Ctrl Pts',(23.1296327664199,49.6516771209836,-213.96235621794));
#225675=CARTESIAN_POINT('Ctrl Pts',(23.085029569752,49.6560132622008,-213.972847885383));
#225676=CARTESIAN_POINT('Ctrl Pts',(23.0403017126433,49.6603474871157,-213.983418653291));
#225677=CARTESIAN_POINT('Ctrl Pts',(22.9952661957579,49.6647017043639,-213.993851883475));
#225678=CARTESIAN_POINT('Ctrl Pts',(22.9520128737166,49.6688836117539,-214.003872238435));
#225679=CARTESIAN_POINT('Ctrl Pts',(22.908490275569,49.6730813341779,-214.013831433549));
#225680=CARTESIAN_POINT('Ctrl Pts',(22.8645836069524,49.6773054855748,-214.02374962579));
#225681=CARTESIAN_POINT('Ctrl Pts',(22.7494415108754,49.6883830202935,-214.049759375103));
#225682=CARTESIAN_POINT('Ctrl Pts',(22.6316603245303,49.6996429322849,-214.075496523236));
#225683=CARTESIAN_POINT('Ctrl Pts',(22.5091539919612,49.7112704713707,-214.101231806193));
#225684=CARTESIAN_POINT('Ctrl Pts',(22.0167441198786,49.75800695359,-214.204673866071));
#225685=CARTESIAN_POINT('Ctrl Pts',(21.3972641828706,49.8152106337258,-214.315369623735));
#225686=CARTESIAN_POINT('Ctrl Pts',(20.796432808198,49.8685261402426,-214.394114559153));
#225687=CARTESIAN_POINT('Ctrl Pts',(19.4772558081119,49.9855849239708,-214.567005842891));
#225688=CARTESIAN_POINT('Ctrl Pts',(18.1397819123848,50.0948434821514,-214.617115230396));
#225689=CARTESIAN_POINT('Ctrl Pts',(16.8015661238258,50.1948649177512,-214.517648223079));
#225690=CARTESIAN_POINT('Ctrl Pts',(16.0733214987344,50.2492956556727,-214.463519199889));
#225691=CARTESIAN_POINT('Ctrl Pts',(15.4167055758679,50.2955918304614,-214.369161556618));
#225692=CARTESIAN_POINT('Ctrl Pts',(14.8786895652353,50.3323031651629,-214.269588134207));
#225693=CARTESIAN_POINT('Ctrl Pts',(14.5167312569262,50.3570012639959,-214.2025986268));
#225694=CARTESIAN_POINT('Ctrl Pts',(14.202155330086,50.3778195415913,-214.1327896286));
#225695=CARTESIAN_POINT('Ctrl Pts',(13.9364760833966,50.3951159243116,-214.068404584443));
#225696=CARTESIAN_POINT('Ctrl Pts',(13.8539190573513,50.4004905929638,-214.048397610493));
#225697=CARTESIAN_POINT('Ctrl Pts',(13.7760879080755,50.405523949103,-214.028903353814));
#225698=CARTESIAN_POINT('Ctrl Pts',(13.7030382763995,50.4102234769291,-214.010137001906));
#225699=CARTESIAN_POINT('Ctrl Pts',(13.6627871480097,50.4128129670273,-213.99979654128));
#225700=CARTESIAN_POINT('Ctrl Pts',(13.623987818724,50.4153010762635,-213.98967678931));
#225701=CARTESIAN_POINT('Ctrl Pts',(13.5866496246302,50.4176888915325,-213.979811340452));
#225702=CARTESIAN_POINT('Ctrl Pts',(13.5768617283821,50.4183148373951,-213.977225195294));
#225703=CARTESIAN_POINT('Ctrl Pts',(13.5671742371175,50.4189338907117,-213.974656515408));
#225704=CARTESIAN_POINT('Ctrl Pts',(13.5575873139323,50.4195460700437,-213.972105883982));
#225705=CARTESIAN_POINT('Ctrl Pts',(13.5466235875268,50.4202461660575,-213.969188949678));
#225706=CARTESIAN_POINT('Ctrl Pts',(13.5357905517574,50.4209372643919,-213.966298904327));
#225707=CARTESIAN_POINT('Ctrl Pts',(13.5250821831194,50.421619333823,-213.963461027108));
#225708=CARTESIAN_POINT('Ctrl Pts',(13.501794131956,50.4231026660043,-213.957289346613));
#225709=CARTESIAN_POINT('Ctrl Pts',(13.4791042282484,50.4245433767524,-213.951330941414));
#225710=CARTESIAN_POINT('Ctrl Pts',(13.4570189352174,50.4259417414909,-213.945579087136));
#225711=CARTESIAN_POINT('Ctrl Pts',(13.2532048418568,50.4388465483666,-213.892498108615));
#225712=CARTESIAN_POINT('Ctrl Pts',(13.0902503949803,50.4488803522574,-213.853486772554));
#225713=CARTESIAN_POINT('Ctrl Pts',(12.9104008459301,50.4597229754217,-213.813164200894));
#225714=CARTESIAN_POINT('Ctrl Pts',(11.4496555026504,50.5477872012135,-213.485662635884));
#225715=CARTESIAN_POINT('Ctrl Pts',(9.93840942401383,50.6207736864612,-213.359232839684));
#225716=CARTESIAN_POINT('Ctrl Pts',(8.43667805237259,50.6748332488454,-213.428209574319));
#225717=CARTESIAN_POINT('Ctrl Pts',(8.23238827711037,50.6821873043435,-213.437592904709));
#225718=CARTESIAN_POINT('Ctrl Pts',(8.02834204153374,50.6891969690078,-213.450528247198));
#225719=CARTESIAN_POINT('Ctrl Pts',(7.824503888911,50.6958660191919,-213.466980375523));
#225720=CARTESIAN_POINT('Ctrl Pts',(7.25602553293655,50.7144651412688,-213.512863242603));
#225721=CARTESIAN_POINT('Ctrl Pts',(6.6538362810014,50.7311625041638,-213.593251906418));
#225722=CARTESIAN_POINT('Ctrl Pts',(6.15552385199797,50.7430175186589,-213.680345086889));
#225723=CARTESIAN_POINT('Ctrl Pts',(5.72610318100236,50.7532335758609,-213.755397623852));
#225724=CARTESIAN_POINT('Ctrl Pts',(5.36706219916213,50.7604549681015,-213.832054599617));
#225725=CARTESIAN_POINT('Ctrl Pts',(5.00965909049245,50.7667680020115,-213.917612838338));
#225726=CARTESIAN_POINT('Ctrl Pts',(4.96190685115584,50.7676114795832,-213.929044181249));
#225727=CARTESIAN_POINT('Ctrl Pts',(4.91419131129741,50.7684360583204,-213.940659514235));
#225728=CARTESIAN_POINT('Ctrl Pts',(4.86635293877012,50.7692443949469,-213.952498814775));
#225729=CARTESIAN_POINT('Ctrl Pts',(4.8430126288082,50.7696387818463,-213.958275201591));
#225730=CARTESIAN_POINT('Ctrl Pts',(4.81964739249074,50.7700288847056,-213.964123321728));
#225731=CARTESIAN_POINT('Ctrl Pts',(4.7962245577203,50.7704163078938,-213.969988537243));
#225732=CARTESIAN_POINT('Ctrl Pts',(4.77566091609363,50.7707564388677,-213.975137793988));
#225733=CARTESIAN_POINT('Ctrl Pts',(4.75504506642069,50.7710952449316,-213.980267091875));
#225734=CARTESIAN_POINT('Ctrl Pts',(4.73436429387878,50.7714328972265,-213.985379046521));
#225735=CARTESIAN_POINT('Ctrl Pts',(4.65303700461145,50.7727607173458,-214.005481845554));
#225736=CARTESIAN_POINT('Ctrl Pts',(4.57070598326991,50.7740709043372,-214.025319649038));
#225737=CARTESIAN_POINT('Ctrl Pts',(4.48659701201007,50.7753721870468,-214.045025781685));
#225738=CARTESIAN_POINT('Ctrl Pts',(4.32894533783954,50.7778112776057,-214.081962445595));
#225739=CARTESIAN_POINT('Ctrl Pts',(4.16505838170397,50.7802213764123,-214.118471962292));
#225740=CARTESIAN_POINT('Ctrl Pts',(3.98974842067771,50.7826329069094,-214.155016004706));
#225741=CARTESIAN_POINT('Ctrl Pts',(3.57148470877949,50.7883864630175,-214.242204700306));
#225742=CARTESIAN_POINT('Ctrl Pts',(3.10286408217604,50.7938341521992,-214.324313596318));
#225743=CARTESIAN_POINT('Ctrl Pts',(2.65136385212586,50.7979637376852,-214.386713900287));
#225744=CARTESIAN_POINT('Ctrl Pts',(1.77493142783601,50.8059799077288,-214.507842630781));
#225745=CARTESIAN_POINT('Ctrl Pts',(0.886906888442037,50.8100674225229,
-214.57114562896));
#225746=CARTESIAN_POINT('Ctrl Pts',(7.57796986272652E-8,50.8100674233964,
-214.571145595706));
#225747=CARTESIAN_POINT('Ctrl Pts',(-0.689331197484988,50.8100674240753,
-214.57114556986));
#225748=CARTESIAN_POINT('Ctrl Pts',(-1.38062861972754,50.807607880196,-214.532824696008));
#225749=CARTESIAN_POINT('Ctrl Pts',(-2.06681665421521,50.8027193023931,
-214.458682419818));
#225750=CARTESIAN_POINT('Ctrl Pts',(-2.71339489002495,50.7981129148542,
-214.388819962695));
#225751=CARTESIAN_POINT('Ctrl Pts',(-3.37138077803095,50.7911390626746,
-214.283916861856));
#225752=CARTESIAN_POINT('Ctrl Pts',(-3.98974958328583,50.7826328964271,
-214.155015446714));
#225753=CARTESIAN_POINT('Ctrl Pts',(-4.1637062425794,50.7802399809838,-214.118753495326));
#225754=CARTESIAN_POINT('Ctrl Pts',(-4.3278016707857,50.777828977619,-214.08223006206));
#225755=CARTESIAN_POINT('Ctrl Pts',(-4.48659703808242,50.7753721929754,
-214.045025412884));
#225756=CARTESIAN_POINT('Ctrl Pts',(-4.5704464158805,50.7740749267689,-214.025380087345));
#225757=CARTESIAN_POINT('Ctrl Pts',(-4.65281520992318,50.77276434532,-214.005536277871));
#225758=CARTESIAN_POINT('Ctrl Pts',(-4.73436407287352,50.7714329078382,
-213.985378700013));
#225759=CARTESIAN_POINT('Ctrl Pts',(-4.75503326394108,50.7710954446939,
-213.980269605746));
#225760=CARTESIAN_POINT('Ctrl Pts',(-4.77564977279552,50.7707566302578,
-213.97514017803));
#225761=CARTESIAN_POINT('Ctrl Pts',(-4.79622435607242,50.7704163183534,
-213.96998817968));
#225762=CARTESIAN_POINT('Ctrl Pts',(-4.8196348408496,50.7700290994945,-213.964126054683));
#225763=CARTESIAN_POINT('Ctrl Pts',(-4.84300112848971,50.7696389832667,
-213.958277641287));
#225764=CARTESIAN_POINT('Ctrl Pts',(-4.86635294089622,50.7692444019801,
-213.952498409351));
#225765=CARTESIAN_POINT('Ctrl Pts',(-4.91415558624414,50.768436668988,-213.940667953976));
#225766=CARTESIAN_POINT('Ctrl Pts',(-4.96187958607181,50.7676119681406,
-213.929050309711));
#225767=CARTESIAN_POINT('Ctrl Pts',(-5.00965909045278,50.7667680089134,
-213.917612443077));
#225768=CARTESIAN_POINT('Ctrl Pts',(-5.36927133290557,50.7604159532737,
-213.831525387076));
#225769=CARTESIAN_POINT('Ctrl Pts',(-5.73167895489853,50.753100932397,-213.754422765144));
#225770=CARTESIAN_POINT('Ctrl Pts',(-6.15552383543092,50.7430175245826,
-213.680344773112));
#225771=CARTESIAN_POINT('Ctrl Pts',(-6.31572994732526,50.7392061689787,
-213.652344559767));
#225772=CARTESIAN_POINT('Ctrl Pts',(-6.48476935122518,50.7349828986066,
-213.624915677394));
#225773=CARTESIAN_POINT('Ctrl Pts',(-6.66599545505587,50.7301771498111,
-213.598432925724));
#225774=CARTESIAN_POINT('Ctrl Pts',(-7.23349350002257,50.715128252393,-213.515503869255));
#225775=CARTESIAN_POINT('Ctrl Pts',(-7.84439075174546,50.6961545036633,
-213.45541400729));
#225776=CARTESIAN_POINT('Ctrl Pts',(-8.436678010806,50.6748332530167,-213.428209423087));
#225777=CARTESIAN_POINT('Ctrl Pts',(-9.31368610829759,50.6432625764916,
-213.387927211592));
#225778=CARTESIAN_POINT('Ctrl Pts',(-10.1922509633074,50.6054259689156,
-213.412946620486));
#225779=CARTESIAN_POINT('Ctrl Pts',(-11.0647191696714,50.5616460640852,
-213.507390029984));
#225780=CARTESIAN_POINT('Ctrl Pts',(-11.6857669687375,50.5304822768665,
-213.574617547477));
#225781=CARTESIAN_POINT('Ctrl Pts',(-12.3036600542713,50.4963016674955,
-213.677132040931));
#225782=CARTESIAN_POINT('Ctrl Pts',(-12.9104007912719,50.4597229753191,
-213.81316438299));
#225783=CARTESIAN_POINT('Ctrl Pts',(-13.1010995860117,50.44822628145,-213.855919388702));
#225784=CARTESIAN_POINT('Ctrl Pts',(-13.2813016781285,50.4370675494195,
-213.899815823864));
#225785=CARTESIAN_POINT('Ctrl Pts',(-13.4570188815656,50.4259417407046,
-213.945579312412));
#225786=CARTESIAN_POINT('Ctrl Pts',(-13.4797777977165,50.4245007244427,
-213.951506605689));
#225787=CARTESIAN_POINT('Ctrl Pts',(-13.5024612388415,50.4230601703824,
-213.957466382958));
#225788=CARTESIAN_POINT('Ctrl Pts',(-13.5250821296103,50.4216193329497,
-213.963461257796));
#225789=CARTESIAN_POINT('Ctrl Pts',(-13.5359306197904,50.4209283384658,
-213.966336270167));
#225790=CARTESIAN_POINT('Ctrl Pts',(-13.54676299098,50.4202372600292,-213.969226285269));
#225791=CARTESIAN_POINT('Ctrl Pts',(-13.5575870608609,50.4195460819038,
-213.972106062562));
#225792=CARTESIAN_POINT('Ctrl Pts',(-13.5672802347205,50.4189271178902,
-213.974684961469));
#225793=CARTESIAN_POINT('Ctrl Pts',(-13.5769673322604,50.4183080796475,
-213.977253341563));
#225794=CARTESIAN_POINT('Ctrl Pts',(-13.5866493728619,50.417688903386,-213.979811516833));
#225795=CARTESIAN_POINT('Ctrl Pts',(-13.6255051838502,50.4152040350842,
-213.990077945045));
#225796=CARTESIAN_POINT('Ctrl Pts',(-13.6642796078801,50.412716947939,-214.000180186509));
#225797=CARTESIAN_POINT('Ctrl Pts',(-13.7030380297945,50.4102234887559,
-214.010137169485));
#225798=CARTESIAN_POINT('Ctrl Pts',(-13.7807410638259,50.40522459215,-214.030098967433));
#225799=CARTESIAN_POINT('Ctrl Pts',(-13.8583799763604,50.4002001721689,
-214.049478889196));
#225800=CARTESIAN_POINT('Ctrl Pts',(-13.9364758468782,50.3951159360852,
-214.068404734377));
#225801=CARTESIAN_POINT('Ctrl Pts',(-14.2341686709201,50.3757353902535,
-214.140547963741));
#225802=CARTESIAN_POINT('Ctrl Pts',(-14.5382696861838,50.3555315939824,
-214.206584999646));
#225803=CARTESIAN_POINT('Ctrl Pts',(-14.8786893660444,50.3323031767319,
-214.269588212978));
#225804=CARTESIAN_POINT('Ctrl Pts',(-15.3967781923265,50.2969515676985,
-214.365473565024));
#225805=CARTESIAN_POINT('Ctrl Pts',(-15.9993479121824,50.2548246171532,
-214.458020891098));
#225806=CARTESIAN_POINT('Ctrl Pts',(-16.8015659878209,50.1948649289014,
-214.517648156697));
#225807=CARTESIAN_POINT('Ctrl Pts',(-17.2395658580743,50.1621277761592,
-214.550203811312));
#225808=CARTESIAN_POINT('Ctrl Pts',(-17.7082120160163,50.1260503285933,
-214.567856665254));
#225809=CARTESIAN_POINT('Ctrl Pts',(-18.1637878991495,50.0898577036051,
-214.568151042825));
#225810=CARTESIAN_POINT('Ctrl Pts',(-19.0450457944776,50.0198473327658,
-214.568720481568));
#225811=CARTESIAN_POINT('Ctrl Pts',(-19.9260477691704,49.9457608258918,
-214.508186877708));
#225812=CARTESIAN_POINT('Ctrl Pts',(-20.7964327548152,49.8685261515117,
-214.394114193465));
#225813=CARTESIAN_POINT('Ctrl Pts',(-21.5053808339726,49.8056167781319,
-214.301199435384));
#225814=CARTESIAN_POINT('Ctrl Pts',(-22.2396557444683,49.7374282494541,
-214.16491573399));
#225815=CARTESIAN_POINT('Ctrl Pts',(-22.8645835730838,49.6773054980824,
-214.023749106193));
#225816=CARTESIAN_POINT('Ctrl Pts',(-22.9084582558125,49.6730844240313,
-214.013838136121));
#225817=CARTESIAN_POINT('Ctrl Pts',(-22.9519885580468,49.6688859720506,
-214.003877337734));
#225818=CARTESIAN_POINT('Ctrl Pts',(-22.9952661624728,49.6647017170029,
-213.993851354185));
#225819=CARTESIAN_POINT('Ctrl Pts',(-23.0402921169331,49.6603484243535,
-213.983420336001));
#225820=CARTESIAN_POINT('Ctrl Pts',(-23.0850289057069,49.6560133363786,
-213.972847495132));
#225821=CARTESIAN_POINT('Ctrl Pts',(-23.1296329441772,49.6516771132442,
-213.962355632284));
#225822=CARTESIAN_POINT('Ctrl Pts',(-23.2309014126094,49.6418322047861,
-213.938535034013));
#225823=CARTESIAN_POINT('Ctrl Pts',(-23.3315871269299,49.6319635848738,
-213.915584604225));
#225824=CARTESIAN_POINT('Ctrl Pts',(-23.4328831691411,49.6219541124168,
-213.893238920191));
#225825=CARTESIAN_POINT('Ctrl Pts',(-23.6291639753803,49.602558810478,-213.849939806204));
#225826=CARTESIAN_POINT('Ctrl Pts',(-23.8277143103713,49.5826440436499,
-213.808847903502));
#225827=CARTESIAN_POINT('Ctrl Pts',(-24.0373135320024,49.5612632885096,
-213.768798156763));
#225828=CARTESIAN_POINT('Ctrl Pts',(-24.3911283485615,49.525171418039,-213.701192019271));
#225829=CARTESIAN_POINT('Ctrl Pts',(-24.786966358124,49.4838398214064,-213.634371448189));
#225830=CARTESIAN_POINT('Ctrl Pts',(-25.2356860399355,49.4352084231262,
-213.57567222148));
#225831=CARTESIAN_POINT('Ctrl Pts',(-28.0133620326269,49.1341691039938,
-213.212310774616));
#225832=CARTESIAN_POINT('Ctrl Pts',(-30.9016860171707,48.7536932160381,
-213.450145604589));
#225833=CARTESIAN_POINT('Ctrl Pts',(-33.4676027871724,48.3558414255462,
-214.55197396609));
#225834=CARTESIAN_POINT('Ctrl Pts',(-23.1985904601668,37.1455480181648,
-232.850246331936));
#225835=CARTESIAN_POINT('Ctrl Pts',(-22.1564545595563,37.2602774694449,
-232.514130204924));
#225836=CARTESIAN_POINT('Ctrl Pts',(-21.0641804092463,37.3724708937409,
-232.345177904713));
#225837=CARTESIAN_POINT('Ctrl Pts',(-19.9681071327435,37.4761722827196,
-232.313659235738));
#225838=CARTESIAN_POINT('Ctrl Pts',(-19.2991366874209,37.5394647339204,
-232.294422330258));
#225839=CARTESIAN_POINT('Ctrl Pts',(-18.6376856229304,37.5985673286038,
-232.329772980603));
#225840=CARTESIAN_POINT('Ctrl Pts',(-18.0769455458819,37.64655661213,-232.388919611448));
#225841=CARTESIAN_POINT('Ctrl Pts',(-17.9570080780068,37.6568211061209,
-232.401570565833));
#225842=CARTESIAN_POINT('Ctrl Pts',(-17.8401560569646,37.6667188889414,
-232.41533436964));
#225843=CARTESIAN_POINT('Ctrl Pts',(-17.72605548882,37.6762929544425,-232.430022763024));
#225844=CARTESIAN_POINT('Ctrl Pts',(-17.4149087979919,37.7024009646557,
-232.470077296226));
#225845=CARTESIAN_POINT('Ctrl Pts',(-17.1241467866706,37.7261173291054,
-232.516791489072));
#225846=CARTESIAN_POINT('Ctrl Pts',(-16.8475890215201,37.7481654899999,
-232.567875869631));
#225847=CARTESIAN_POINT('Ctrl Pts',(-16.6967373793616,37.7601919152052,
-232.595740437786));
#225848=CARTESIAN_POINT('Ctrl Pts',(-16.5501315589411,37.7717180670409,
-232.624939985054));
#225849=CARTESIAN_POINT('Ctrl Pts',(-16.4068314221588,37.7828417554715,
-232.655316959781));
#225850=CARTESIAN_POINT('Ctrl Pts',(-16.3324722176574,37.7886138966669,
-232.67107973382));
#225851=CARTESIAN_POINT('Ctrl Pts',(-16.259003222542,37.7942775108324,-232.687161754288));
#225852=CARTESIAN_POINT('Ctrl Pts',(-16.1862882705909,37.7998456944697,
-232.70355571365));
#225853=CARTESIAN_POINT('Ctrl Pts',(-16.1550881440824,37.802234859686,-232.710589942407));
#225854=CARTESIAN_POINT('Ctrl Pts',(-16.1240153770202,37.8046073304442,
-232.717626099841));
#225855=CARTESIAN_POINT('Ctrl Pts',(-16.0930261937342,37.8069665902894,
-232.724502972898));
#225856=CARTESIAN_POINT('Ctrl Pts',(-16.063092214273,37.8092455156518,-232.731145683515));
#225857=CARTESIAN_POINT('Ctrl Pts',(-16.0332453620651,37.8115114139419,
-232.737684631239));
#225858=CARTESIAN_POINT('Ctrl Pts',(-16.003476624031,37.8137650756407,-232.744122743264));
#225859=CARTESIAN_POINT('Ctrl Pts',(-15.824134731135,37.827342270433,-232.782909177407));
#225860=CARTESIAN_POINT('Ctrl Pts',(-15.6476298224866,37.8404768185726,
-232.818057012347));
#225861=CARTESIAN_POINT('Ctrl Pts',(-15.4720288026693,37.853326932794,-232.850049999999));
#225862=CARTESIAN_POINT('',(-2.58126937689227,38.4029617620279,-232.850050996336));
#225863=CARTESIAN_POINT('Ctrl Pts',(-10.3603804086809,38.1653654608598,
-232.850050113495));
#225864=CARTESIAN_POINT('Ctrl Pts',(-9.71419790368592,38.196982639096,-232.721004312897));
#225865=CARTESIAN_POINT('Ctrl Pts',(-9.35549486807857,38.2135078924852,
-232.595584405869));
#225866=CARTESIAN_POINT('Ctrl Pts',(-7.88550439629379,38.2731624675052,
-232.364954948601));
#225867=CARTESIAN_POINT('Ctrl Pts',(-7.16548125236048,38.2987680162378,
-232.312392715194));
#225868=CARTESIAN_POINT('Ctrl Pts',(-5.68487376001899,38.3438073799782,
-232.321825074893));
#225869=CARTESIAN_POINT('Ctrl Pts',(-4.92650521021758,38.3627520068666,
-232.390644239872));
#225870=CARTESIAN_POINT('Ctrl Pts',(-3.50691587437607,38.3907272609826,
-232.631934382068));
#225871=CARTESIAN_POINT('Ctrl Pts',(-3.19597628779658,38.3954757183434,
-232.732911385662));
#225872=CARTESIAN_POINT('Ctrl Pts',(-2.58126982511239,38.4029609689687,
-232.850053829461));
#225873=CARTESIAN_POINT('',(2.58126928063572,38.4029617514691,-232.850050981496));
#225874=CARTESIAN_POINT('Ctrl Pts',(-2.58126959429465,38.4029635779833,
-232.85005));
#225875=CARTESIAN_POINT('Ctrl Pts',(-1.72249329171046,38.5235335172581,
-232.85005));
#225876=CARTESIAN_POINT('Ctrl Pts',(-0.867273575857391,38.583205095121,
-232.85005));
#225877=CARTESIAN_POINT('Ctrl Pts',(0.867251683657016,38.583206657092,-232.85005));
#225878=CARTESIAN_POINT('Ctrl Pts',(1.72248215657025,38.5235349591089,-232.85005));
#225879=CARTESIAN_POINT('Ctrl Pts',(2.58126949479989,38.4029635403769,-232.85005));
#225880=CARTESIAN_POINT('',(10.3603804821857,38.1653654824018,-232.850050038668));
#225881=CARTESIAN_POINT('Ctrl Pts',(10.3603804658313,38.1653654580635,-232.850050114597));
#225882=CARTESIAN_POINT('Ctrl Pts',(9.71419795896007,38.1969826365663,-232.721004310544));
#225883=CARTESIAN_POINT('Ctrl Pts',(9.35549489011901,38.2135078916454,-232.595584392477));
#225884=CARTESIAN_POINT('Ctrl Pts',(7.88550438721803,38.2731624678223,-232.364954942449));
#225885=CARTESIAN_POINT('Ctrl Pts',(7.16548124909485,38.2987680163253,-232.312392716592));
#225886=CARTESIAN_POINT('Ctrl Pts',(5.68487373797052,38.3438073806628,-232.321825087222));
#225887=CARTESIAN_POINT('Ctrl Pts',(4.9265051676737,38.3627520079171,-232.390644261604));
#225888=CARTESIAN_POINT('Ctrl Pts',(3.50691613666394,38.3907272556243,-232.631934364075));
#225889=CARTESIAN_POINT('Ctrl Pts',(3.19597714514061,38.3954757082021,-232.732911221419));
#225890=CARTESIAN_POINT('Ctrl Pts',(2.58126972217957,38.4029609702222,-232.850053772423));
#225891=CARTESIAN_POINT('',(15.4720289242324,37.8533269238987,-232.85005));
#225892=CARTESIAN_POINT('Ctrl Pts',(10.3603804783137,38.1653655319544,-232.85005));
#225893=CARTESIAN_POINT('Ctrl Pts',(11.193556676016,38.2304686654651,-232.85005));
#225894=CARTESIAN_POINT('Ctrl Pts',(12.0312562221273,38.2388535343039,-232.85005));
#225895=CARTESIAN_POINT('Ctrl Pts',(13.7409536714611,38.140257937513,-232.85005));
#225896=CARTESIAN_POINT('Ctrl Pts',(14.613269214461,38.0271219437723,-232.85005));
#225897=CARTESIAN_POINT('Ctrl Pts',(15.4720289242322,37.8533269238976,-232.85005));
#225898=CARTESIAN_POINT('Ctrl Pts',(23.1985903050735,37.1455480352391,-232.850246269746));
#225899=CARTESIAN_POINT('Ctrl Pts',(22.0455775581368,37.2724839932101,-232.478369482393));
#225900=CARTESIAN_POINT('Ctrl Pts',(20.8316287206699,37.3962101542244,-232.311280498896));
#225901=CARTESIAN_POINT('Ctrl Pts',(19.6181202835508,37.5089924027573,-232.30820532281));
#225902=CARTESIAN_POINT('Ctrl Pts',(18.9222079202927,37.5736697949445,-232.306441797323));
#225903=CARTESIAN_POINT('Ctrl Pts',(18.2806146166533,37.6297604507304,-232.358633251125));
#225904=CARTESIAN_POINT('Ctrl Pts',(17.7260544830199,37.6762930388382,-232.430022919809));
#225905=CARTESIAN_POINT('Ctrl Pts',(17.4149077894093,37.7024010477931,-232.470077474801));
#225906=CARTESIAN_POINT('Ctrl Pts',(17.1241457734926,37.7261174112266,-232.516791687499));
#225907=CARTESIAN_POINT('Ctrl Pts',(16.8475879986799,37.7481655715443,-232.567876087736));
#225908=CARTESIAN_POINT('Ctrl Pts',(16.6967363558847,37.7601919960656,-232.59574066577));
#225909=CARTESIAN_POINT('Ctrl Pts',(16.5501305330696,37.7717181473772,-232.624940222784));
#225910=CARTESIAN_POINT('Ctrl Pts',(16.4068303915331,37.7828418354739,-232.655317207503));
#225911=CARTESIAN_POINT('Ctrl Pts',(16.3324711865191,37.7886139763443,-232.671079986313));
#225912=CARTESIAN_POINT('Ctrl Pts',(16.2590021902051,37.794277590242,-232.687162011602));
#225913=CARTESIAN_POINT('Ctrl Pts',(16.1862872362639,37.7998457736738,-232.7035559759));
#225914=CARTESIAN_POINT('Ctrl Pts',(16.1550871799105,37.8022349333644,-232.710590190766));
#225915=CARTESIAN_POINT('Ctrl Pts',(16.1240144811553,37.80460739877,-232.71762632881));
#225916=CARTESIAN_POINT('Ctrl Pts',(16.0930253659941,37.8069666533067,-232.724503184806));
#225917=CARTESIAN_POINT('Ctrl Pts',(16.0630913871853,37.8092455785015,-232.7311458934));
#225918=CARTESIAN_POINT('Ctrl Pts',(16.0332445354967,37.8115114766347,-232.73768483914));
#225919=CARTESIAN_POINT('Ctrl Pts',(16.0034757978481,37.8137651381874,-232.744122949218));
#225920=CARTESIAN_POINT('Ctrl Pts',(15.8241342326628,37.8273423074652,-232.782909301255));
#225921=CARTESIAN_POINT('Ctrl Pts',(15.6476296366115,37.840476832073,-232.818057068527));
#225922=CARTESIAN_POINT('Ctrl Pts',(15.4720289242322,37.8533269238983,-232.850049999999));
#225923=CARTESIAN_POINT('Origin',(22.9178089794592,-52.5372975341153,-234.75005));
#225924=CARTESIAN_POINT('',(27.0625191140422,-59.958306757953,-232.85005));
#225925=CARTESIAN_POINT('',(23.2057914601203,-61.0324176680998,-232.85005));
#225926=CARTESIAN_POINT('Origin',(22.9178089794592,-52.5372975341153,-232.85005));
#225927=CARTESIAN_POINT('',(27.0625191140422,-59.958306757953,-232.25005));
#225928=CARTESIAN_POINT('',(27.0625191140422,-59.958306757953,-234.75005));
#225929=CARTESIAN_POINT('',(23.2057914601203,-61.0324176680998,-232.25005));
#225930=CARTESIAN_POINT('Origin',(22.9178089794592,-52.5372975341153,-232.25005));
#225931=CARTESIAN_POINT('',(23.2057914601203,-61.0324176680998,-234.75005));
#225932=CARTESIAN_POINT('Origin',(7.14692237356698E-14,623.509175991979,
-234.75005));
#225933=CARTESIAN_POINT('Origin',(7.14692237356698E-14,623.509175991979,
-232.25005));
#225934=CARTESIAN_POINT('Origin',(7.14692237356698E-14,623.509175991979,
-232.85005));
#225935=CARTESIAN_POINT('Origin',(-2.61456814389029E-14,-173.57701443073,
-234.75005));
#225936=CARTESIAN_POINT('',(25.8757946403502,36.8335750748777,-232.25005));
#225937=CARTESIAN_POINT('Origin',(-2.61456814389029E-14,-173.57701443073,
-232.25005));
#225938=CARTESIAN_POINT('',(25.8757946403502,36.8335750748777,-232.85005));
#225939=CARTESIAN_POINT('',(25.8757946403502,36.8335750748777,-234.75005));
#225940=CARTESIAN_POINT('Origin',(-2.61456814389029E-14,-173.57701443073,
-232.85005));
#225941=CARTESIAN_POINT('Origin',(-2.61456814389029E-14,-173.57701443073,
-232.85005));
#225942=CARTESIAN_POINT('Origin',(-2.61456814389029E-14,-173.57701443073,
-232.85005));
#225943=CARTESIAN_POINT('Origin',(24.838300653577,28.3971299569735,-234.75005));
#225944=CARTESIAN_POINT('',(29.3303337505005,35.613198045354,-232.85005));
#225945=CARTESIAN_POINT('Origin',(24.838300653577,28.3971299569735,-232.85005));
#225946=CARTESIAN_POINT('',(29.3303337505005,35.613198045354,-232.25005));
#225947=CARTESIAN_POINT('Origin',(24.838300653577,28.3971299569735,-232.25005));
#225948=CARTESIAN_POINT('',(29.3303337505005,35.613198045354,-234.75005));
#225949=CARTESIAN_POINT('Origin',(-6.29739814579425E-15,-11.5034818258363,
-234.75005));
#225950=CARTESIAN_POINT('',(46.0422390557602,19.4862297367486,-232.85005));
#225951=CARTESIAN_POINT('Origin',(-6.29739814579425E-15,-11.5034818258363,
-232.85005));
#225952=CARTESIAN_POINT('',(46.0422390557602,19.4862297367486,-232.25005));
#225953=CARTESIAN_POINT('Origin',(-6.29739814579425E-15,-11.5034818258363,
-232.25005));
#225954=CARTESIAN_POINT('',(46.0422390557602,19.4862297367486,-234.75005));
#225955=CARTESIAN_POINT('Origin',(38.9907249661392,14.740057695632,-234.75005));
#225956=CARTESIAN_POINT('',(47.4843254762175,15.0698309134599,-232.85005));
#225957=CARTESIAN_POINT('Origin',(38.9907249661392,14.740057695632,-232.85005));
#225958=CARTESIAN_POINT('',(47.4843254762175,15.0698309134599,-232.25005));
#225959=CARTESIAN_POINT('Origin',(38.9907249661392,14.740057695632,-232.25005));
#225960=CARTESIAN_POINT('',(47.4843254762175,15.0698309134599,-234.75005));
#225961=CARTESIAN_POINT('Origin',(-636.934816028482,-11.5034818258361,-234.75005));
#225962=CARTESIAN_POINT('',(47.7644117008771,6.45952891261178,-232.25005));
#225963=CARTESIAN_POINT('Origin',(-636.934816028482,-11.5034818258361,-232.25005));
#225964=CARTESIAN_POINT('',(47.7015217244055,8.71393886986192,-232.849988375574));
#225965=CARTESIAN_POINT('Ctrl Pts',(47.764411700877,6.45952891261171,-232.250050000001));
#225966=CARTESIAN_POINT('Ctrl Pts',(47.7539918567994,6.85670393504417,-232.299135434164));
#225967=CARTESIAN_POINT('Ctrl Pts',(47.7432936090854,7.25119812638128,-232.373336512398));
#225968=CARTESIAN_POINT('Ctrl Pts',(47.7222110876844,8.00529930166126,-232.573920981311));
#225969=CARTESIAN_POINT('Ctrl Pts',(47.7118378495729,8.36566358596881,-232.697530953773));
#225970=CARTESIAN_POINT('Ctrl Pts',(47.70155338045,8.71393369956125,-232.849926751148));
#225971=CARTESIAN_POINT('Origin',(-636.934816028482,-11.5034818258361,-232.85005));
#225972=CARTESIAN_POINT('Origin',(38.9907249661392,-37.7470213473046,-234.75005));
#225973=CARTESIAN_POINT('',(47.4843254762176,-38.0767945651323,-232.85005));
#225974=CARTESIAN_POINT('',(46.0422390557601,-42.4931933884212,-232.85005));
#225975=CARTESIAN_POINT('Origin',(38.9907249661392,-37.7470213473046,-232.85005));
#225976=CARTESIAN_POINT('',(47.4843254762176,-38.0767945651323,-232.25005));
#225977=CARTESIAN_POINT('',(47.4843254762176,-38.0767945651323,-234.75005));
#225978=CARTESIAN_POINT('',(46.0422390557601,-42.4931933884212,-232.25005));
#225979=CARTESIAN_POINT('Origin',(38.9907249661392,-37.7470213473046,-232.25005));
#225980=CARTESIAN_POINT('',(46.0422390557601,-42.4931933884212,-234.75005));
#225981=CARTESIAN_POINT('Origin',(-6.29739814579425E-15,-11.5034818258363,
-234.75005));
#225982=CARTESIAN_POINT('Origin',(-6.29739814579425E-15,-11.5034818258363,
-232.85005));
#225983=CARTESIAN_POINT('Origin',(-6.29739814579425E-15,-11.5034818258363,
-232.25005));
#225984=CARTESIAN_POINT('Ctrl Pts',(47.0185565395742,-41.6609971057424,
-232.962224970815));
#225985=CARTESIAN_POINT('Ctrl Pts',(47.4683098495203,-42.4379579278734,
-232.173885913265));
#225986=CARTESIAN_POINT('Ctrl Pts',(47.9182404464189,-43.214781541947,-231.385510833981));
#225987=CARTESIAN_POINT('Ctrl Pts',(48.3683681238743,-43.9914549619569,
-230.597098052473));
#225988=CARTESIAN_POINT('Ctrl Pts',(48.8184958013296,-44.7681283819668,
-229.808685270963));
#225989=CARTESIAN_POINT('Ctrl Pts',(49.2688205234849,-45.5446516231764,
-229.020234782073));
#225990=CARTESIAN_POINT('Ctrl Pts',(49.7193651569502,-46.321010055599,-228.231745013587));
#225991=CARTESIAN_POINT('Ctrl Pts',(50.6204544238808,-47.8737269204442,
-226.654765476616));
#225992=CARTESIAN_POINT('Ctrl Pts',(51.5224188067103,-49.4257867780962,
-225.077628467932));
#225993=CARTESIAN_POINT('Ctrl Pts',(52.4254879069396,-50.9770488729761,
-223.500324296104));
#225994=CARTESIAN_POINT('Ctrl Pts',(54.2316261073984,-54.079573062736,-220.345715952448));
#225995=CARTESIAN_POINT('Ctrl Pts',(56.0420505223762,-57.178961519516,-217.190418744692));
#225996=CARTESIAN_POINT('Ctrl Pts',(57.8597736100785,-60.2735586547801,
-214.03449525351));
#225997=CARTESIAN_POINT('Ctrl Pts',(47.0588574073719,-41.5858000428048,
-232.968566523408));
#225998=CARTESIAN_POINT('Ctrl Pts',(47.5093207248854,-42.363022265842,-232.17977481419));
#225999=CARTESIAN_POINT('Ctrl Pts',(47.9599297574655,-43.1401459593037,
-231.39096724535));
#226000=CARTESIAN_POINT('Ctrl Pts',(48.4106907142535,-43.9171701566874,
-230.602146349555));
#226001=CARTESIAN_POINT('Ctrl Pts',(48.8614516710415,-44.6941943540713,
-229.813325453759));
#226002=CARTESIAN_POINT('Ctrl Pts',(49.3123645814213,-45.4711190318301,
-229.024491224305));
#226003=CARTESIAN_POINT('Ctrl Pts',(49.7634348829592,-46.2479443404272,
-228.235646862402));
#226004=CARTESIAN_POINT('Ctrl Pts',(50.6655754860351,-47.8015949576215,
-226.657958138597));
#226005=CARTESIAN_POINT('Ctrl Pts',(51.5683478186111,-49.3548459662596,
-225.080227999184));
#226006=CARTESIAN_POINT('Ctrl Pts',(52.4717770943224,-50.9077187028313,
-223.502491635481));
#226007=CARTESIAN_POINT('Ctrl Pts',(54.2786356457449,-54.0134641759745,
-220.347018908076));
#226008=CARTESIAN_POINT('Ctrl Pts',(56.0882389522679,-57.1176157229696,
-217.191507400736));
#226009=CARTESIAN_POINT('Ctrl Pts',(57.8999640673718,-60.2209901065118,
-214.036411889894));
#226010=CARTESIAN_POINT('Ctrl Pts',(47.0788820514615,-41.5349619911827,
-232.977219483294));
#226011=CARTESIAN_POINT('Ctrl Pts',(47.5313585913162,-42.310877567243,-232.187698020531));
#226012=CARTESIAN_POINT('Ctrl Pts',(47.9838932303251,-43.0867923470826,
-231.398208761274));
#226013=CARTESIAN_POINT('Ctrl Pts',(48.4364687519895,-43.8627275668274,
-230.608763067264));
#226014=CARTESIAN_POINT('Ctrl Pts',(48.889044273654,-44.6386627865722,-229.819317373254));
#226015=CARTESIAN_POINT('Ctrl Pts',(49.3416606701069,-45.4146183959999,
-229.029915190037));
#226016=CARTESIAN_POINT('Ctrl Pts',(49.7943023545749,-46.1906112611962,
-228.240564453713));
#226017=CARTESIAN_POINT('Ctrl Pts',(50.6995857235109,-47.7425969915886,
-226.661862981063));
#226018=CARTESIAN_POINT('Ctrl Pts',(51.6049685652275,-49.2947346592046,
-225.083369244233));
#226019=CARTESIAN_POINT('Ctrl Pts',(52.5103464401617,-50.8471174431018,
-223.505116662391));
#226020=CARTESIAN_POINT('Ctrl Pts',(54.3211021900301,-53.951883010896,-220.348611498707));
#226021=CARTESIAN_POINT('Ctrl Pts',(56.1318167680608,-57.0576530539869,
-217.193082767306));
#226022=CARTESIAN_POINT('Ctrl Pts',(57.9419471071077,-60.1647335356702,
-214.038526270145));
#226023=CARTESIAN_POINT('Ctrl Pts',(47.0912031843055,-41.4946844018168,
-232.986503298756));
#226024=CARTESIAN_POINT('Ctrl Pts',(47.5465884139282,-42.2680813083878,
-232.195931935019));
#226025=CARTESIAN_POINT('Ctrl Pts',(48.0017768129395,-43.0417829154583,
-231.40555195953));
#226026=CARTESIAN_POINT('Ctrl Pts',(48.4567760318361,-43.8157641577748,
-230.615342754576));
#226027=CARTESIAN_POINT('Ctrl Pts',(48.9117752507326,-44.5897454000911,
-229.825133549621));
#226028=CARTESIAN_POINT('Ctrl Pts',(49.366585304478,-45.364006290321,-229.035095136287));
#226029=CARTESIAN_POINT('Ctrl Pts',(49.8212141883276,-46.1385240104118,
-228.245209329223));
#226030=CARTESIAN_POINT('Ctrl Pts',(50.7304719560267,-47.6875594505935,
-226.665437715093));
#226031=CARTESIAN_POINT('Ctrl Pts',(51.6390050797513,-49.2376203690394,
-225.086274713309));
#226032=CARTESIAN_POINT('Ctrl Pts',(52.5468787652607,-50.7885482821615,
-223.507599498114));
#226033=CARTESIAN_POINT('Ctrl Pts',(54.3626261362793,-53.8904041084056,
-220.350249067725));
#226034=CARTESIAN_POINT('Ctrl Pts',(56.1757402684043,-56.9957065400334,
-217.194831063113));
#226035=CARTESIAN_POINT('Ctrl Pts',(57.9867151256432,-60.1034983677464,
-214.040672462087));
#226036=CARTESIAN_POINT('Ctrl Pts',(47.1035243171495,-41.4544068124509,
-232.995787114217));
#226037=CARTESIAN_POINT('Ctrl Pts',(47.5618182365402,-42.2252850495327,
-232.204165849507));
#226038=CARTESIAN_POINT('Ctrl Pts',(48.0196603955539,-42.9967734838342,
-231.412895157786));
#226039=CARTESIAN_POINT('Ctrl Pts',(48.4770833116826,-43.7688007487221,
-230.621922441887));
#226040=CARTESIAN_POINT('Ctrl Pts',(48.9345062278113,-44.54082801361,-229.830949725988));
#226041=CARTESIAN_POINT('Ctrl Pts',(49.391509938849,-45.313394184642,-229.040275082537));
#226042=CARTESIAN_POINT('Ctrl Pts',(49.8481260220802,-46.0864367596275,
-228.249854204732));
#226043=CARTESIAN_POINT('Ctrl Pts',(50.7613581885425,-47.6325219095984,
-226.669012449123));
#226044=CARTESIAN_POINT('Ctrl Pts',(51.6730415942752,-49.1805060788742,
-225.089180182384));
#226045=CARTESIAN_POINT('Ctrl Pts',(52.5834110903597,-50.7299791212212,
-223.510082333838));
#226046=CARTESIAN_POINT('Ctrl Pts',(54.4041500825286,-53.8289252059152,
-220.351886636744));
#226047=CARTESIAN_POINT('Ctrl Pts',(56.2196637687479,-56.9337600260798,
-217.196579358919));
#226048=CARTESIAN_POINT('Ctrl Pts',(58.0314831441787,-60.0422631998226,
-214.04281865403));
#226049=CARTESIAN_POINT('Ctrl Pts',(47.1094181844823,-41.4235916164857,
-233.005271954373));
#226050=CARTESIAN_POINT('Ctrl Pts',(47.5714574466843,-42.1907462838401,
-232.21226382723));
#226051=CARTESIAN_POINT('Ctrl Pts',(48.0325802899557,-42.9590937957815,
-231.419919822014));
#226052=CARTESIAN_POINT('Ctrl Pts',(48.4929276099559,-43.7283935879396,
-230.628080779981));
#226053=CARTESIAN_POINT('Ctrl Pts',(48.9532749299561,-44.4976933800977,
-229.836241737948));
#226054=CARTESIAN_POINT('Ctrl Pts',(49.4128465653679,-45.2679465967797,
-229.044908707219));
#226055=CARTESIAN_POINT('Ctrl Pts',(49.8717607150419,-46.0389694518266,
-228.253966129662));
#226056=CARTESIAN_POINT('Ctrl Pts',(50.7895890143898,-47.5810151619205,
-226.672080974546));
#226057=CARTESIAN_POINT('Ctrl Pts',(51.7048034669659,-49.1261109180323,
-225.091738429241));
#226058=CARTESIAN_POINT('Ctrl Pts',(52.6181227187143,-50.6732510827466,
-223.512347273439));
#226059=CARTESIAN_POINT('Ctrl Pts',(54.4447612222111,-53.7675314121752,
-220.353564961834));
#226060=CARTESIAN_POINT('Ctrl Pts',(56.2639490448981,-56.8698182307502,
-217.198492064106));
#226061=CARTESIAN_POINT('Ctrl Pts',(58.0790346309092,-59.9760499787848,
-214.044995596012));
#226062=CARTESIAN_POINT('Ctrl Pts',(47.1301259245572,-41.3776365805516,
-233.007883276788));
#226063=CARTESIAN_POINT('Ctrl Pts',(47.5942000936469,-42.1428559602882,
-232.214484939109));
#226064=CARTESIAN_POINT('Ctrl Pts',(48.0571442886842,-42.9095264965149,
-231.42188110874));
#226065=CARTESIAN_POINT('Ctrl Pts',(48.5191679953314,-43.677310151957,-230.629855880101));
#226066=CARTESIAN_POINT('Ctrl Pts',(48.9811917019786,-44.445093807399,-229.837830651463));
#226067=CARTESIAN_POINT('Ctrl Pts',(49.4422942329435,-45.2139930242057,
-229.046386055781));
#226068=CARTESIAN_POINT('Ctrl Pts',(49.9026408989544,-45.9837637819335,
-228.255374275861));
#226069=CARTESIAN_POINT('Ctrl Pts',(50.8233342309762,-47.5233052973892,
-226.673350716021));
#226070=CARTESIAN_POINT('Ctrl Pts',(51.7410289944696,-49.0662933806299,
-225.093033330561));
#226071=CARTESIAN_POINT('Ctrl Pts',(52.6566611088264,-50.611475717687,-223.51371347964));
#226072=CARTESIAN_POINT('Ctrl Pts',(54.4879253375398,-53.7018403918012,
-220.355073777797));
#226073=CARTESIAN_POINT('Ctrl Pts',(56.3111024468989,-56.8007837303405,
-217.200320668143));
#226074=CARTESIAN_POINT('Ctrl Pts',(58.1301468566089,-59.9036654708269,
-214.047106057761));
#226075=CARTESIAN_POINT('Ctrl Pts',(47.171541404707,-41.2857265086834,-233.01310592162));
#226076=CARTESIAN_POINT('Ctrl Pts',(47.639685387572,-42.0470753131842,-232.218927162867));
#226077=CARTESIAN_POINT('Ctrl Pts',(48.1062722861412,-42.8103918979816,
-231.425803682192));
#226078=CARTESIAN_POINT('Ctrl Pts',(48.5716487660823,-43.5751432799917,
-230.633406080342));
#226079=CARTESIAN_POINT('Ctrl Pts',(49.0370252460235,-44.3398946620018,
-229.841008478492));
#226080=CARTESIAN_POINT('Ctrl Pts',(49.5011895680945,-45.1060858790577,
-229.049340752905));
#226081=CARTESIAN_POINT('Ctrl Pts',(49.9644012667793,-45.8733524421474,
-228.25819056826));
#226082=CARTESIAN_POINT('Ctrl Pts',(50.8908246641489,-47.4078855683268,
-226.675890198969));
#226083=CARTESIAN_POINT('Ctrl Pts',(51.8134800494771,-48.9466583058251,
-225.095623133202));
#226084=CARTESIAN_POINT('Ctrl Pts',(52.7337378890505,-50.4879249875678,
-223.516445892042));
#226085=CARTESIAN_POINT('Ctrl Pts',(54.5742535681973,-53.5704583510531,
-220.358091409721));
#226086=CARTESIAN_POINT('Ctrl Pts',(56.4054092509004,-56.6627147295212,
-217.203977876217));
#226087=CARTESIAN_POINT('Ctrl Pts',(58.2323713080084,-59.7588964549113,
-214.051326981263));
#226088=CARTESIAN_POINT('Ctrl Pts',(47.2037604911033,-41.2022757926265,
-233.020733994064));
#226089=CARTESIAN_POINT('Ctrl Pts',(47.6765307304169,-41.9587290407164,
-232.2257873802));
#226090=CARTESIAN_POINT('Ctrl Pts',(48.1471647665248,-42.7177804449826,
-231.432193257086));
#226091=CARTESIAN_POINT('Ctrl Pts',(48.6161649822748,-43.4787209967311,
-230.639525123807));
#226092=CARTESIAN_POINT('Ctrl Pts',(49.0851651980248,-44.2396615484797,
-229.846856990528));
#226093=CARTESIAN_POINT('Ctrl Pts',(49.5525384413198,-45.0024830404561,
-229.055111557421));
#226094=CARTESIAN_POINT('Ctrl Pts',(50.0187056640015,-45.76663525977,-228.263983251877));
#226095=CARTESIAN_POINT('Ctrl Pts',(50.9510401093651,-47.2949396983977,
-226.68172664079));
#226096=CARTESIAN_POINT('Ctrl Pts',(51.8786366079818,-48.8284550182444,
-225.101877330191));
#226097=CARTESIAN_POINT('Ctrl Pts',(52.8035983099936,-50.3646700206687,
-223.523161428396));
#226098=CARTESIAN_POINT('Ctrl Pts',(54.6535217140174,-53.4371000255173,
-220.365729624806));
#226099=CARTESIAN_POINT('Ctrl Pts',(56.4932286367666,-56.5200179818056,
-217.212714221123));
#226100=CARTESIAN_POINT('Ctrl Pts',(58.3292814169375,-59.6063766654718,
-214.060952327901));
#226101=CARTESIAN_POINT('Ctrl Pts',(47.2184619313714,-41.1386068777002,
-233.034226791445));
#226102=CARTESIAN_POINT('Ctrl Pts',(47.6994633038231,-41.8843414973674,
-232.236899734718));
#226103=CARTESIAN_POINT('Ctrl Pts',(48.1764662990288,-42.6351364657344,
-231.442184400327));
#226104=CARTESIAN_POINT('Ctrl Pts',(48.6511105129755,-43.3886793381388,
-230.648777192266));
#226105=CARTESIAN_POINT('Ctrl Pts',(49.1257547269221,-44.1422222105431,
-229.855369984204));
#226106=CARTESIAN_POINT('Ctrl Pts',(49.5980020098404,-44.8985826028918,
-229.063316695606));
#226107=CARTESIAN_POINT('Ctrl Pts',(50.0687290729088,-45.6566352866088,
-228.272029084797));
#226108=CARTESIAN_POINT('Ctrl Pts',(51.0101831990457,-47.1727406540429,
-226.689453863181));
#226109=CARTESIAN_POINT('Ctrl Pts',(51.9456932760972,-48.695455984225,-225.109865596097));
#226110=CARTESIAN_POINT('Ctrl Pts',(52.8784745199465,-50.2209883221406,
-223.531433290935));
#226111=CARTESIAN_POINT('Ctrl Pts',(54.7440370076451,-53.2720529979718,
-220.374568680612));
#226112=CARTESIAN_POINT('Ctrl Pts',(56.5988680832651,-56.3342829748578,
-217.222334895439));
#226113=CARTESIAN_POINT('Ctrl Pts',(58.4505854057776,-59.3994904876393,
-214.071174978969));
#226114=CARTESIAN_POINT('Ctrl Pts',(47.2331633716395,-41.074937962774,-233.047719588827));
#226115=CARTESIAN_POINT('Ctrl Pts',(47.7223958772293,-41.8099539540185,
-232.248012089236));
#226116=CARTESIAN_POINT('Ctrl Pts',(48.2057678315329,-42.5524924864862,
-231.452175543568));
#226117=CARTESIAN_POINT('Ctrl Pts',(48.6860560436761,-43.2986376795464,
-230.658029260724));
#226118=CARTESIAN_POINT('Ctrl Pts',(49.1663442558194,-44.0447828726065,
-229.86388297788));
#226119=CARTESIAN_POINT('Ctrl Pts',(49.6434655783611,-44.7946821653274,
-229.071521833792));
#226120=CARTESIAN_POINT('Ctrl Pts',(50.1187524818162,-45.5466353134476,
-228.280074917719));
#226121=CARTESIAN_POINT('Ctrl Pts',(51.0693262887264,-47.0505416096881,
-226.697181085572));
#226122=CARTESIAN_POINT('Ctrl Pts',(52.0127499442126,-48.5624569502057,
-225.117853862002));
#226123=CARTESIAN_POINT('Ctrl Pts',(52.9533507298994,-50.0773066236126,
-223.539705153474));
#226124=CARTESIAN_POINT('Ctrl Pts',(54.8345523012729,-53.1070059704263,
-220.383407736418));
#226125=CARTESIAN_POINT('Ctrl Pts',(56.7045075297636,-56.1485479679101,
-217.231955569755));
#226126=CARTESIAN_POINT('Ctrl Pts',(58.5718893946176,-59.1926043098068,
-214.081397630038));
#226127=CARTESIAN_POINT('Ctrl Pts',(47.2442225930031,-41.0165984906687,
-233.060484538427));
#226128=CARTESIAN_POINT('Ctrl Pts',(47.7410879851243,-41.7396655945174,
-232.258993064984));
#226129=CARTESIAN_POINT('Ctrl Pts',(48.2304947549091,-42.4727467259007,
-231.46264144105));
#226130=CARTESIAN_POINT('Ctrl Pts',(48.7165337536793,-43.2098774487494,
-230.66815609265));
#226131=CARTESIAN_POINT('Ctrl Pts',(49.2025727524494,-43.9470081715982,
-229.873670744249));
#226132=CARTESIAN_POINT('Ctrl Pts',(49.6850684896479,-44.6884971892255,
-229.081242904766));
#226133=CARTESIAN_POINT('Ctrl Pts',(50.1656830825472,-45.4321663014423,
-228.289778191998));
#226134=CARTESIAN_POINT('Ctrl Pts',(51.1269122683457,-46.9195045258758,
-226.706848766463));
#226135=CARTESIAN_POINT('Ctrl Pts',(52.0807938880043,-48.415379750843,-225.127702010668));
#226136=CARTESIAN_POINT('Ctrl Pts',(53.0320528840148,-49.9140824163154,
-223.549690567007));
#226137=CARTESIAN_POINT('Ctrl Pts',(54.9345708760356,-52.9114877472602,
-220.393667679684));
#226138=CARTESIAN_POINT('Ctrl Pts',(56.8264228500083,-55.9205802770675,
-217.24244325845));
#226139=CARTESIAN_POINT('Ctrl Pts',(58.7160309997225,-58.9319583435186,
-214.092043625716));
#226140=CARTESIAN_POINT('Ctrl Pts',(47.2640162261029,-40.9447914059068,
-233.067937997558));
#226141=CARTESIAN_POINT('Ctrl Pts',(47.7628369926546,-41.6622203630557,
-232.268067857029));
#226142=CARTESIAN_POINT('Ctrl Pts',(48.2549965369399,-42.3887167282325,
-231.472771264582));
#226143=CARTESIAN_POINT('Ctrl Pts',(48.7442220365055,-43.1188281595447,
-230.679129004258));
#226144=CARTESIAN_POINT('Ctrl Pts',(49.2334475360712,-43.8489395908569,
-229.885486743933));
#226145=CARTESIAN_POINT('Ctrl Pts',(49.7195709178301,-44.5829547593942,
-229.093671052645));
#226146=CARTESIAN_POINT('Ctrl Pts',(50.2040684510243,-45.3189094985237,
-228.302711021656));
#226147=CARTESIAN_POINT('Ctrl Pts',(51.1730635174128,-46.7908189767828,
-226.720790959677));
#226148=CARTESIAN_POINT('Ctrl Pts',(52.1357048103052,-48.2703270275798,
-225.142232468079));
#226149=CARTESIAN_POINT('Ctrl Pts',(53.0961142063379,-49.7523323833611,
-223.564687821978));
#226150=CARTESIAN_POINT('Ctrl Pts',(55.0169329984032,-52.7163430949238,
-220.409598529776));
#226151=CARTESIAN_POINT('Ctrl Pts',(56.9286455988057,-55.6906960308185,
-217.258791511269));
#226152=CARTESIAN_POINT('Ctrl Pts',(58.8384812385968,-58.6670561134909,
-214.108729566325));
#226153=CARTESIAN_POINT('Ctrl Pts',(47.2838098592026,-40.8729843211449,
-233.075391456688));
#226154=CARTESIAN_POINT('Ctrl Pts',(47.7845860001848,-41.584775131594,-232.277142649072));
#226155=CARTESIAN_POINT('Ctrl Pts',(48.2794983189707,-42.3046867305642,
-231.482901088115));
#226156=CARTESIAN_POINT('Ctrl Pts',(48.7719103193318,-43.02777887034,-230.690101915866));
#226157=CARTESIAN_POINT('Ctrl Pts',(49.2643223196929,-43.7508710101157,
-229.897302743617));
#226158=CARTESIAN_POINT('Ctrl Pts',(49.7540733460123,-44.4774123295628,
-229.106099200524));
#226159=CARTESIAN_POINT('Ctrl Pts',(50.2424538195015,-45.2056526956051,
-228.315643851313));
#226160=CARTESIAN_POINT('Ctrl Pts',(51.2192147664799,-46.6621334276898,
-226.734733152891));
#226161=CARTESIAN_POINT('Ctrl Pts',(52.1906157326061,-48.1252743043166,
-225.156762925491));
#226162=CARTESIAN_POINT('Ctrl Pts',(53.160175528661,-49.5905823504069,-223.57968507695));
#226163=CARTESIAN_POINT('Ctrl Pts',(55.0992951207707,-52.5211984425875,
-220.425529379868));
#226164=CARTESIAN_POINT('Ctrl Pts',(57.0308683476032,-55.4608117845694,
-217.275139764089));
#226165=CARTESIAN_POINT('Ctrl Pts',(58.960931477471,-58.4021538834631,-214.125415506933));
#226166=CARTESIAN_POINT('Ctrl Pts',(47.2969979727536,-40.8060289412791,
-233.085985533281));
#226167=CARTESIAN_POINT('Ctrl Pts',(47.8004278329226,-41.5103244226814,
-232.28875968809));
#226168=CARTESIAN_POINT('Ctrl Pts',(48.2986559156506,-42.2220372798219,
-231.495168009573));
#226169=CARTESIAN_POINT('Ctrl Pts',(48.7946878038133,-42.9366432257674,
-230.702889499098));
#226170=CARTESIAN_POINT('Ctrl Pts',(49.2907196919761,-43.6512491717128,
-229.910610988623));
#226171=CARTESIAN_POINT('Ctrl Pts',(49.7844091161609,-44.3689959246396,
-229.119784028342));
#226172=CARTESIAN_POINT('Ctrl Pts',(50.2768976831464,-45.088287213268,-228.329639845834));
#226173=CARTESIAN_POINT('Ctrl Pts',(51.2618748171174,-46.5268697905249,
-226.749351480816));
#226174=CARTESIAN_POINT('Ctrl Pts',(52.2421543662867,-47.9715077333147,
-225.171746235109));
#226175=CARTESIAN_POINT('Ctrl Pts',(53.2208294063969,-49.4181128068083,
-223.594959717073));
#226176=CARTESIAN_POINT('Ctrl Pts',(55.1781794866173,-52.3113229537955,
-220.441386681001));
#226177=CARTESIAN_POINT('Ctrl Pts',(57.1289452771368,-55.2127036344464,
-217.291264707778));
#226178=CARTESIAN_POINT('Ctrl Pts',(59.078404570546,-58.1156526803525,-214.141757511623));
#226179=CARTESIAN_POINT('Ctrl Pts',(47.3009006987844,-40.7491010613005,
-233.101301752625));
#226180=CARTESIAN_POINT('Ctrl Pts',(47.8070153253589,-41.445066041129,-232.304686649286));
#226181=CARTESIAN_POINT('Ctrl Pts',(48.3084583519731,-42.1479407187119,
-231.511460238167));
#226182=CARTESIAN_POINT('Ctrl Pts',(48.8079303323174,-42.8535202192507,
-230.719470612188));
#226183=CARTESIAN_POINT('Ctrl Pts',(49.3074023126618,-43.5590997197895,
-229.92748098621));
#226184=CARTESIAN_POINT('Ctrl Pts',(49.8047715089351,-44.2676134042324,
-229.136855227393));
#226185=CARTESIAN_POINT('Ctrl Pts',(50.3010627023117,-44.9775733943649,
-228.346875024182));
#226186=CARTESIAN_POINT('Ctrl Pts',(51.293645089065,-46.3974933746299,-226.766914617761));
#226187=CARTESIAN_POINT('Ctrl Pts',(52.2820103247895,-47.8230831255928,
-225.189490258971));
#226188=CARTESIAN_POINT('Ctrl Pts',(53.2689347752898,-49.2505213363517,
-223.612847133253));
#226189=CARTESIAN_POINT('Ctrl Pts',(55.2427836762905,-52.1053977578695,
-220.459560881818));
#226190=CARTESIAN_POINT('Ctrl Pts',(57.2107204090195,-54.9679461288674,
-217.309560330918));
#226191=CARTESIAN_POINT('Ctrl Pts',(59.1774846171821,-57.8319751776559,
-214.160152831317));
#226192=CARTESIAN_POINT('Ctrl Pts',(47.3048034248152,-40.692173181322,-233.11661797197));
#226193=CARTESIAN_POINT('Ctrl Pts',(47.8136028177951,-41.3798076595766,
-232.320613610482));
#226194=CARTESIAN_POINT('Ctrl Pts',(48.3182607882955,-42.0738441576018,
-231.527752466761));
#226195=CARTESIAN_POINT('Ctrl Pts',(48.8211728608215,-42.770397212734,-230.736051725279));
#226196=CARTESIAN_POINT('Ctrl Pts',(49.3240849333475,-43.4669502678662,
-229.944350983796));
#226197=CARTESIAN_POINT('Ctrl Pts',(49.8251339017092,-44.1662308838252,
-229.153926426443));
#226198=CARTESIAN_POINT('Ctrl Pts',(50.325227721477,-44.8668595754618,-228.364110202531));
#226199=CARTESIAN_POINT('Ctrl Pts',(51.3254153610126,-46.2681169587348,
-226.784477754705));
#226200=CARTESIAN_POINT('Ctrl Pts',(52.3218662832923,-47.674658517871,-225.207234282834));
#226201=CARTESIAN_POINT('Ctrl Pts',(53.3170401441828,-49.0829298658951,
-223.630734549434));
#226202=CARTESIAN_POINT('Ctrl Pts',(55.3073878659637,-51.8994725619434,
-220.477735082634));
#226203=CARTESIAN_POINT('Ctrl Pts',(57.2924955409022,-54.7231886232885,
-217.327855954057));
#226204=CARTESIAN_POINT('Ctrl Pts',(59.2765646638181,-57.5482976749593,
-214.178548151011));
#226205=CARTESIAN_POINT('Ctrl Pts',(47.3080516727752,-40.6337213157799,
-233.131438257577));
#226206=CARTESIAN_POINT('Ctrl Pts',(47.8183168860115,-41.3141454117954,
-232.336628860671));
#226207=CARTESIAN_POINT('Ctrl Pts',(48.3251567152684,-42.0000633572803,
-231.544500449812));
#226208=CARTESIAN_POINT('Ctrl Pts',(48.8305551087238,-42.688161659062,-230.753383167905));
#226209=CARTESIAN_POINT('Ctrl Pts',(49.3359535021791,-43.3762599608436,
-229.962265885999));
#226210=CARTESIAN_POINT('Ctrl Pts',(49.8398128115685,-44.0667165790755,
-229.172255055445));
#226211=CARTESIAN_POINT('Ctrl Pts',(50.3428831683021,-44.7583456287819,
-228.382778415603));
#226212=CARTESIAN_POINT('Ctrl Pts',(51.3490238817693,-46.1416037281948,
-226.803825135918));
#226213=CARTESIAN_POINT('Ctrl Pts',(52.3520777883286,-47.5294564292592,
-225.226968306426));
#226214=CARTESIAN_POINT('Ctrl Pts',(53.3540764188403,-48.9188259619783,
-223.65077630667));
#226215=CARTESIAN_POINT('Ctrl Pts',(55.3580736798637,-51.6975650274167,
-220.498392307158));
#226216=CARTESIAN_POINT('Ctrl Pts',(57.35774124088,-54.4825830356932,-217.348785724916));
#226217=CARTESIAN_POINT('Ctrl Pts',(59.3565528325338,-57.2688342364512,
-214.199700145503));
#226218=CARTESIAN_POINT('Ctrl Pts',(47.3143897740156,-40.5659557077008,
-233.143618951735));
#226219=CARTESIAN_POINT('Ctrl Pts',(47.8252832097387,-41.239862847313,-232.350527479362));
#226220=CARTESIAN_POINT('Ctrl Pts',(48.3335556171132,-41.9180591247534,
-231.559510554001));
#226221=CARTESIAN_POINT('Ctrl Pts',(48.84072766068,-42.5979714018469,-230.769289654088));
#226222=CARTESIAN_POINT('Ctrl Pts',(49.3478997042467,-43.2778836789405,
-229.979068754174));
#226223=CARTESIAN_POINT('Ctrl Pts',(49.853896141919,-43.9596488205701,-229.189715484531));
#226224=CARTESIAN_POINT('Ctrl Pts',(50.3592905012865,-44.6423395873253,
-228.400785431186));
#226225=CARTESIAN_POINT('Ctrl Pts',(51.3700792200214,-46.0077211208357,
-226.822925324494));
#226226=CARTESIAN_POINT('Ctrl Pts',(52.3785121216331,-47.3767293468831,
-225.246725326938));
#226227=CARTESIAN_POINT('Ctrl Pts',(53.3861409718259,-48.7469431347296,
-223.67105962423));
#226228=CARTESIAN_POINT('Ctrl Pts',(55.4013986722116,-51.4873707104227,
-220.519728218813));
#226229=CARTESIAN_POINT('Ctrl Pts',(57.4133569116451,-54.2327814391975,
-217.37062149599));
#226230=CARTESIAN_POINT('Ctrl Pts',(59.4246687676614,-56.9791795051587,
-214.221940194738));
#226231=CARTESIAN_POINT('Ctrl Pts',(47.320727875256,-40.4981900996217,-233.155799645893));
#226232=CARTESIAN_POINT('Ctrl Pts',(47.8322495334659,-41.1655802828307,
-232.364426098052));
#226233=CARTESIAN_POINT('Ctrl Pts',(48.3419545189581,-41.8360548922265,
-231.574520658189));
#226234=CARTESIAN_POINT('Ctrl Pts',(48.8509002126362,-42.507781144632,-230.785196140269));
#226235=CARTESIAN_POINT('Ctrl Pts',(49.3598459063144,-43.1795073970375,
-229.995871622349));
#226236=CARTESIAN_POINT('Ctrl Pts',(49.8679794722695,-43.8525810620647,
-229.207175913618));
#226237=CARTESIAN_POINT('Ctrl Pts',(50.3756978342709,-44.5263335458687,
-228.418792446769));
#226238=CARTESIAN_POINT('Ctrl Pts',(51.3911345582736,-45.8738385134766,
-226.842025513071));
#226239=CARTESIAN_POINT('Ctrl Pts',(52.4049464549377,-47.224002264507,-225.266482347449));
#226240=CARTESIAN_POINT('Ctrl Pts',(53.4182055248116,-48.5750603074809,
-223.691342941789));
#226241=CARTESIAN_POINT('Ctrl Pts',(55.4447236645594,-51.2771763934287,
-220.541064130469));
#226242=CARTESIAN_POINT('Ctrl Pts',(57.4689725824102,-53.9829798427017,
-217.392457267063));
#226243=CARTESIAN_POINT('Ctrl Pts',(59.492784702789,-56.6895247738662,-214.244180243974));
#226244=CARTESIAN_POINT('Ctrl Pts',(47.3211789031199,-40.4350426000942,
-233.171747992562));
#226245=CARTESIAN_POINT('Ctrl Pts',(47.8337422070404,-41.0944281592508,
-232.381526838764));
#226246=CARTESIAN_POINT('Ctrl Pts',(48.3450895420457,-41.7559741023036,
-231.59233795934));
#226247=CARTESIAN_POINT('Ctrl Pts',(48.8559011403763,-42.4184505962563,
-230.803585490448));
#226248=CARTESIAN_POINT('Ctrl Pts',(49.3667127387069,-43.080927090209,-230.014833021558));
#226249=CARTESIAN_POINT('Ctrl Pts',(49.87695729968,-43.7443929697667,-229.226546244883));
#226250=CARTESIAN_POINT('Ctrl Pts',(50.3869032026916,-44.4083742082442,
-228.43849935464));
#226251=CARTESIAN_POINT('Ctrl Pts',(51.4067950087149,-45.7363366851993,
-226.862405574156));
#226252=CARTESIAN_POINT('Ctrl Pts',(52.4255193465988,-47.0663149534946,
-225.287250420734));
#226253=CARTESIAN_POINT('Ctrl Pts',(53.4438309990515,-48.3970017219875,
-223.712420269846));
#226254=CARTESIAN_POINT('Ctrl Pts',(55.4804543039569,-51.0583752589733,
-220.562759968072));
#226255=CARTESIAN_POINT('Ctrl Pts',(57.5153972302706,-53.7226435757235,
-217.414431597513));
#226256=CARTESIAN_POINT('Ctrl Pts',(59.5500043535892,-56.3875253353041,
-214.266381372884));
#226257=CARTESIAN_POINT('Ctrl Pts',(47.3174213500927,-40.3725566206431,
-233.190758458866));
#226258=CARTESIAN_POINT('Ctrl Pts',(47.8304331865629,-41.0247379875799,
-232.40178755381));
#226259=CARTESIAN_POINT('Ctrl Pts',(48.3427237376172,-41.6782347797706,
-231.613445913152));
#226260=CARTESIAN_POINT('Ctrl Pts',(48.8546863035239,-42.3323210585191,
-230.825382497106));
#226261=CARTESIAN_POINT('Ctrl Pts',(49.3666488694307,-42.9864073372676,
-230.037319081059));
#226262=CARTESIAN_POINT('Ctrl Pts',(49.8782662454544,-43.6411158354054,
-229.249550061497));
#226263=CARTESIAN_POINT('Ctrl Pts',(50.3896983451462,-44.2961564367811,
-228.461936921534));
#226264=CARTESIAN_POINT('Ctrl Pts',(51.4125625445298,-45.6062376395327,
-226.886710641608));
#226265=CARTESIAN_POINT('Ctrl Pts',(52.4347028263001,-46.9176171020422,
-225.312093851176));
#226266=CARTESIAN_POINT('Ctrl Pts',(53.4565811414505,-48.229468784563,-223.737696459652));
#226267=CARTESIAN_POINT('Ctrl Pts',(55.5003377717513,-50.8531721496045,
-220.588901676603));
#226268=CARTESIAN_POINT('Ctrl Pts',(57.5430330553295,-53.4787928890259,
-217.440999537853));
#226269=CARTESIAN_POINT('Ctrl Pts',(59.5855147104668,-56.1048379574655,
-214.293293254791));
#226270=CARTESIAN_POINT('Ctrl Pts',(47.3136637970655,-40.310070641192,-233.20976892517));
#226271=CARTESIAN_POINT('Ctrl Pts',(47.8271241660854,-40.955047815909,-232.422048268856));
#226272=CARTESIAN_POINT('Ctrl Pts',(48.3403579331886,-41.6004954572377,
-231.634553866964));
#226273=CARTESIAN_POINT('Ctrl Pts',(48.8534714666716,-42.246191520782,-230.847179503763));
#226274=CARTESIAN_POINT('Ctrl Pts',(49.3665850001545,-42.8918875843263,
-230.059805140562));
#226275=CARTESIAN_POINT('Ctrl Pts',(49.8795751912289,-43.537838701044,-229.272553878112));
#226276=CARTESIAN_POINT('Ctrl Pts',(50.3924934876008,-44.183938665318,-228.485374488428));
#226277=CARTESIAN_POINT('Ctrl Pts',(51.4183300803446,-45.476138593866,-226.911015709061));
#226278=CARTESIAN_POINT('Ctrl Pts',(52.4438863060015,-46.7689192505898,
-225.336937281619));
#226279=CARTESIAN_POINT('Ctrl Pts',(53.4693312838495,-48.0619358471384,
-223.762972649457));
#226280=CARTESIAN_POINT('Ctrl Pts',(55.5202212395457,-50.6479690402357,
-220.615043385133));
#226281=CARTESIAN_POINT('Ctrl Pts',(57.5706688803884,-53.2349422023283,
-217.467567478191));
#226282=CARTESIAN_POINT('Ctrl Pts',(59.6210250673444,-55.8221505796269,
-214.320205136697));
#226283=CARTESIAN_POINT('Ctrl Pts',(47.3091454883712,-40.242131557965,-233.229003132042));
#226284=CARTESIAN_POINT('Ctrl Pts',(47.8231540168911,-40.8795018283497,
-232.442071186825));
#226285=CARTESIAN_POINT('Ctrl Pts',(48.337145706421,-41.5169166318385,-231.655160989632));
#226286=CARTESIAN_POINT('Ctrl Pts',(48.8511232816408,-42.1543682290027,
-230.868268963674));
#226287=CARTESIAN_POINT('Ctrl Pts',(49.3651008568606,-42.7918198261669,
-230.081376937717));
#226288=CARTESIAN_POINT('Ctrl Pts',(49.8790645191143,-43.4293078274282,
-229.294502880311));
#226289=CARTESIAN_POINT('Ctrl Pts',(50.3930177372337,-44.066823718135,-228.507642672989));
#226290=CARTESIAN_POINT('Ctrl Pts',(51.4209241734724,-45.3418554995486,
-226.933922258343));
#226291=CARTESIAN_POINT('Ctrl Pts',(52.4487896446279,-46.616996929731,-225.36025631034));
#226292=CARTESIAN_POINT('Ctrl Pts',(53.4766337325378,-47.8922016232008,
-223.786622036391));
#226293=CARTESIAN_POINT('Ctrl Pts',(55.5323219083575,-50.4426110101405,
-220.639353488495));
#226294=CARTESIAN_POINT('Ctrl Pts',(57.5879280964248,-52.9932654200165,
-217.492207602051));
#226295=CARTESIAN_POINT('Ctrl Pts',(59.6435178458378,-55.5440119530488,
-214.345108432027));
#226296=CARTESIAN_POINT('Ctrl Pts',(47.3051413523369,-40.1629192793609,
-233.246904846954));
#226297=CARTESIAN_POINT('Ctrl Pts',(47.819327369804,-40.7940757964512,-232.460673323282));
#226298=CARTESIAN_POINT('Ctrl Pts',(48.3336083951406,-41.4250391409392,
-231.674348554294));
#226299=CARTESIAN_POINT('Ctrl Pts',(48.8479443642697,-42.0558912348621,
-230.88796994392));
#226300=CARTESIAN_POINT('Ctrl Pts',(49.3622803333988,-42.6867433287849,
-230.101591333545));
#226301=CARTESIAN_POINT('Ctrl Pts',(49.8766723259409,-43.3174819888763,
-229.315157839431));
#226302=CARTESIAN_POINT('Ctrl Pts',(50.3910998220442,-43.9481493585103,
-228.52868979147));
#226303=CARTESIAN_POINT('Ctrl Pts',(51.4199548142509,-45.2094840977783,
-226.955753695549));
#226304=CARTESIAN_POINT('Ctrl Pts',(52.4489487693187,-46.4705399682764,
-225.382682428314));
#226305=CARTESIAN_POINT('Ctrl Pts',(53.4780084556675,-47.7314680211233,
-223.809549063998));
#226306=CARTESIAN_POINT('Ctrl Pts',(55.536127828365,-50.253324126817,-220.663282335366));
#226307=CARTESIAN_POINT('Ctrl Pts',(57.5945065616385,-52.7746765489683,
-217.516770963173));
#226308=CARTESIAN_POINT('Ctrl Pts',(59.6529740461698,-55.2958790062696,
-214.370186647608));
#226309=CARTESIAN_POINT('Ctrl Pts',(47.3011370887008,-40.083704476459,-233.264807132349));
#226310=CARTESIAN_POINT('Ctrl Pts',(47.8155006007713,-40.7086470422379,
-232.479276052542));
#226311=CARTESIAN_POINT('Ctrl Pts',(48.330070971135,-41.3331587221332,-231.693536730416));
#226312=CARTESIAN_POINT('Ctrl Pts',(48.8447653455944,-41.957411102505,-230.907671551986));
#226313=CARTESIAN_POINT('Ctrl Pts',(49.3594597200539,-42.5816634828768,
-230.121806373556));
#226314=CARTESIAN_POINT('Ctrl Pts',(49.8742800565343,-43.2056525867135,
-229.335813456774));
#226315=CARTESIAN_POINT('Ctrl Pts',(50.3891818457356,-43.8294712170295,
-228.549737580672));
#226316=CARTESIAN_POINT('Ctrl Pts',(51.4189854241382,-45.0771084776612,
-226.977585828468));
#226317=CARTESIAN_POINT('Ctrl Pts',(52.4491078990803,-46.3240783396034,
-225.405109260954));
#226318=CARTESIAN_POINT('Ctrl Pts',(53.4793832226061,-47.5707292968664,
-223.832476822232));
#226319=CARTESIAN_POINT('Ctrl Pts',(55.5399338696578,-50.0640312113922,
-220.68721194479));
#226320=CARTESIAN_POINT('Ctrl Pts',(57.6010852364915,-52.5560807120374,
-217.541335107067));
#226321=CARTESIAN_POINT('Ctrl Pts',(59.6624305478473,-55.0477381521116,
-214.39526566237));
#226322=CARTESIAN_POINT('Ctrl Pts',(47.2844095710387,-40.0223529985484,
-233.29571384424));
#226323=CARTESIAN_POINT('Ctrl Pts',(47.799865767177,-40.6397128949599,-232.509454608122));
#226324=CARTESIAN_POINT('Ctrl Pts',(48.3153486991529,-41.2570069665437,
-231.72316146998));
#226325=CARTESIAN_POINT('Ctrl Pts',(48.8308531059458,-41.8742482184852,
-230.936841114977));
#226326=CARTESIAN_POINT('Ctrl Pts',(49.3463575127388,-42.4914894704268,
-230.150520759975));
#226327=CARTESIAN_POINT('Ctrl Pts',(49.8618834246415,-43.1086778283034,
-229.364173149988));
#226328=CARTESIAN_POINT('Ctrl Pts',(50.3774268752988,-43.7258231065776,
-228.577803332719));
#226329=CARTESIAN_POINT('Ctrl Pts',(51.4085137766134,-44.9601136631259,
-227.005063698182));
#226330=CARTESIAN_POINT('Ctrl Pts',(52.4396702308542,-46.1942333889078,
-225.432235999036));
#226331=CARTESIAN_POINT('Ctrl Pts',(53.4708746321289,-47.4282358136099,
-223.859347784982));
#226332=CARTESIAN_POINT('Ctrl Pts',(55.5332834346784,-49.8962406630142,
-220.713571356874));
#226333=CARTESIAN_POINT('Ctrl Pts',(57.5958804822797,-52.3637850919073,
-217.567557391373));
#226334=CARTESIAN_POINT('Ctrl Pts',(59.658577156368,-54.831089092749,-214.42141923076));
#226335=CARTESIAN_POINT('Ctrl Pts',(47.269359813636,-39.9199414144257,-233.323677937652));
#226336=CARTESIAN_POINT('Ctrl Pts',(47.7852688958474,-40.5328114906027,
-232.537018038148));
#226337=CARTESIAN_POINT('Ctrl Pts',(48.3011810934468,-41.1456737613432,
-231.750354102807));
#226338=CARTESIAN_POINT('Ctrl Pts',(48.8170958227919,-41.7585296857987,
-230.963686885275));
#226339=CARTESIAN_POINT('Ctrl Pts',(49.3330105521369,-42.3713856102541,
-230.177019667743));
#226340=CARTESIAN_POINT('Ctrl Pts',(49.8489278162636,-42.9842351808713,
-229.390349164127));
#226341=CARTESIAN_POINT('Ctrl Pts',(50.3648471682373,-43.5970795157942,
-228.603675952145));
#226342=CARTESIAN_POINT('Ctrl Pts',(51.3966858721847,-44.8227681856401,
-227.03032952818));
#226343=CARTESIAN_POINT('Ctrl Pts',(52.4285328613266,-46.0484360781329,
-225.456972356173));
#226344=CARTESIAN_POINT('Ctrl Pts',(53.4603856521184,-47.2740894119757,
-223.883607650579));
#226345=CARTESIAN_POINT('Ctrl Pts',(55.5240912337022,-49.7253960796616,
-220.736878239389));
#226346=CARTESIAN_POINT('Ctrl Pts',(57.5878196113417,-52.1766455410871,
-217.590119225487));
#226347=CARTESIAN_POINT('Ctrl Pts',(59.6515602724445,-54.6278641542596,
-214.443344242486));
#226348=CARTESIAN_POINT('',(47.5799752941295,-40.2889415902933,-232.85005));
#226349=CARTESIAN_POINT('',(47.0825542278859,-41.7715518798765,-232.850050000968));
#226350=CARTESIAN_POINT('Ctrl Pts',(47.5799752940314,-40.2889415926919,
-232.85005));
#226351=CARTESIAN_POINT('Ctrl Pts',(47.5775945735868,-40.3473480101173,
-232.85005));
#226352=CARTESIAN_POINT('Ctrl Pts',(47.5746791399166,-40.3934055204136,
-232.85005));
#226353=CARTESIAN_POINT('Ctrl Pts',(47.5660677926235,-40.4699741879599,
-232.85005));
#226354=CARTESIAN_POINT('Ctrl Pts',(47.5635310903242,-40.4915421250293,
-232.850049999998));
#226355=CARTESIAN_POINT('Ctrl Pts',(47.5531956971805,-40.5727355789934,
-232.850049999998));
#226356=CARTESIAN_POINT('Ctrl Pts',(47.5435314537204,-40.6342224874872,
-232.85005));
#226357=CARTESIAN_POINT('Ctrl Pts',(47.498863464585,-40.8512217208458,-232.85005));
#226358=CARTESIAN_POINT('Ctrl Pts',(47.4667238050309,-40.9561283613665,
-232.850050000008));
#226359=CARTESIAN_POINT('Ctrl Pts',(47.4103530292664,-41.1136517562587,
-232.850050000008));
#226360=CARTESIAN_POINT('Ctrl Pts',(47.3884688969554,-41.1712462220726,
-232.850050000436));
#226361=CARTESIAN_POINT('Ctrl Pts',(47.3415687154481,-41.2863061130767,
-232.850050000436));
#226362=CARTESIAN_POINT('Ctrl Pts',(47.3098061178227,-41.3563636655023,
-232.850049999917));
#226363=CARTESIAN_POINT('Ctrl Pts',(47.238535493308,-41.4987551852984,-232.850049999917));
#226364=CARTESIAN_POINT('Ctrl Pts',(47.2078203687848,-41.5594829940685,
-232.850050000009));
#226365=CARTESIAN_POINT('Ctrl Pts',(47.1722887237613,-41.6240970447738,
-232.850050000009));
#226366=CARTESIAN_POINT('Ctrl Pts',(47.1600291820282,-41.6454764695154,
-232.85005));
#226367=CARTESIAN_POINT('Ctrl Pts',(47.1263867106497,-41.7020987847656,
-232.85005));
#226368=CARTESIAN_POINT('Ctrl Pts',(47.1037445726029,-41.7383217640954,
-232.85005));
#226369=CARTESIAN_POINT('Ctrl Pts',(47.0825542565969,-41.7715518684049,
-232.85005));
#226370=CARTESIAN_POINT('',(57.733985310444,-60.0593815363208,-214.252907888001));
#226371=CARTESIAN_POINT('Ctrl Pts',(47.0825542096955,-41.7715519112001,
-232.850049982949));
#226372=CARTESIAN_POINT('Ctrl Pts',(47.9607606644449,-43.2885970115993,
-231.310756440341));
#226373=CARTESIAN_POINT('Ctrl Pts',(48.8396331722643,-44.8051274616754,
-229.771321514311));
#226374=CARTESIAN_POINT('Ctrl Pts',(49.7193526002943,-46.3210209808882,
-228.231740696015));
#226375=CARTESIAN_POINT('Ctrl Pts',(50.6068212501588,-47.8502676156323,
-226.67859810687));
#226376=CARTESIAN_POINT('Ctrl Pts',(51.4951510340416,-49.3788667920708,
-225.125307245091));
#226377=CARTESIAN_POINT('Ctrl Pts',(52.3845369850665,-50.9067042966212,
-223.571849770436));
#226378=CARTESIAN_POINT('Ctrl Pts',(52.3981868919341,-50.9301528788952,
-223.548007984058));
#226379=CARTESIAN_POINT('Ctrl Pts',(52.4118370435254,-50.9536012831489,
-223.524166157505));
#226380=CARTESIAN_POINT('Ctrl Pts',(52.4254874411528,-50.9770495086906,
-223.500324290775));
#226381=CARTESIAN_POINT('Ctrl Pts',(54.1899580063524,-54.008001785955,-220.418489371959));
#226382=CARTESIAN_POINT('Ctrl Pts',(55.9585237261342,-57.035959927734,-217.335999861453));
#226383=CARTESIAN_POINT('Ctrl Pts',(57.7339853077823,-60.0593815358969,
-214.252907939395));
#226384=CARTESIAN_POINT('',(59.5601545409129,-55.0066093843694,-214.536876504828));
#226385=CARTESIAN_POINT('Ctrl Pts',(59.5601545409136,-55.0066093843693,
-214.536876504827));
#226386=CARTESIAN_POINT('Ctrl Pts',(59.5534103769403,-55.183285281497,-214.523179687364));
#226387=CARTESIAN_POINT('Ctrl Pts',(59.5413857023832,-55.3595267001454,
-214.509940774492));
#226388=CARTESIAN_POINT('Ctrl Pts',(59.5048392787739,-55.7306111662553,
-214.483592249558));
#226389=CARTESIAN_POINT('Ctrl Pts',(59.4790426192872,-55.9255750687639,
-214.470456744663));
#226390=CARTESIAN_POINT('Ctrl Pts',(59.4374186268297,-56.1761840233205,
-214.453298735629));
#226391=CARTESIAN_POINT('Ctrl Pts',(59.4271923857434,-56.2341662641521,
-214.449364106042));
#226392=CARTESIAN_POINT('Ctrl Pts',(59.3290041047216,-56.7600810968204,
-214.414327664314));
#226393=CARTESIAN_POINT('Ctrl Pts',(59.2036000752591,-57.2212958998854,
-214.387817887177));
#226394=CARTESIAN_POINT('Ctrl Pts',(58.9920439420324,-57.8080590467771,
-214.35489987404));
#226395=CARTESIAN_POINT('Ctrl Pts',(58.9383051097013,-57.9461281140662,
-214.347431324614));
#226396=CARTESIAN_POINT('Ctrl Pts',(58.7834285639215,-58.3162123489988,
-214.328364513275));
#226397=CARTESIAN_POINT('Ctrl Pts',(58.6754718372346,-58.5458967426914,
-214.316667298022));
#226398=CARTESIAN_POINT('Ctrl Pts',(58.4793456692785,-58.920803329709,-214.298260215069));
#226399=CARTESIAN_POINT('Ctrl Pts',(58.3955443144802,-59.0701807393243,
-214.291807992095));
#226400=CARTESIAN_POINT('Ctrl Pts',(58.2554398199234,-59.3038767790683,
-214.282137443959));
#226401=CARTESIAN_POINT('Ctrl Pts',(58.2014468386641,-59.3905132232272,
-214.278624601648));
#226402=CARTESIAN_POINT('Ctrl Pts',(58.0758641218467,-59.5844450019102,
-214.270199768697));
#226403=CARTESIAN_POINT('Ctrl Pts',(58.0026577731459,-59.6923453371106,
-214.265296898901));
#226404=CARTESIAN_POINT('Ctrl Pts',(57.8636814802851,-59.8874642716893,
-214.258285826271));
#226405=CARTESIAN_POINT('Ctrl Pts',(57.799587863237,-59.9740538268332,-214.255565510063));
#226406=CARTESIAN_POINT('Ctrl Pts',(57.7339853360531,-60.0593815526408,
-214.252907779836));
#226407=CARTESIAN_POINT('',(59.5781472511572,-54.5406860123134,-214.555282751782));
#226408=CARTESIAN_POINT('Ctrl Pts',(59.5601545409116,-55.0066093843694,
-214.53687650483));
#226409=CARTESIAN_POINT('Ctrl Pts',(59.5631405773446,-54.9283846158517,
-214.542940888217));
#226410=CARTESIAN_POINT('Ctrl Pts',(59.5661299872555,-54.8504833727614,
-214.547589274133));
#226411=CARTESIAN_POINT('Ctrl Pts',(59.572151316647,-54.6945566512149,-214.553743244933));
#226412=CARTESIAN_POINT('Ctrl Pts',(59.5751126784951,-54.6183446757107,
-214.555228232806));
#226413=CARTESIAN_POINT('Ctrl Pts',(59.5781472511111,-54.540686012984,-214.55528275182));
#226414=CARTESIAN_POINT('Ctrl Pts',(47.5799752942349,-40.2889415880665,
-232.85005));
#226415=CARTESIAN_POINT('Ctrl Pts',(51.5792492625364,-45.0398156733569,
-226.7519456074));
#226416=CARTESIAN_POINT('Ctrl Pts',(55.5786810873963,-49.7902940354523,
-220.653636556059));
#226417=CARTESIAN_POINT('Ctrl Pts',(59.5781472511525,-54.540686011977,-214.555282751822));
#226418=CARTESIAN_POINT('Ctrl Pts',(24.9017054131522,-60.8052918727755,
-233.340945144186));
#226419=CARTESIAN_POINT('Ctrl Pts',(25.5906443745351,-61.3025059726095,
-232.554279700873));
#226420=CARTESIAN_POINT('Ctrl Pts',(26.2795988326832,-61.7997136258234,
-231.767623645885));
#226421=CARTESIAN_POINT('Ctrl Pts',(26.9685652314336,-62.2969163567666,
-230.980974825615));
#226422=CARTESIAN_POINT('Ctrl Pts',(27.6575316301841,-62.7941190877098,
-230.194326005343));
#226423=CARTESIAN_POINT('Ctrl Pts',(28.346509997394,-63.2913168845119,-229.407684436704));
#226424=CARTESIAN_POINT('Ctrl Pts',(29.0354977836505,-63.7885108411498,
-228.621048576497));
#226425=CARTESIAN_POINT('Ctrl Pts',(30.4134733561636,-64.7828987544258,
-227.047776856082));
#226426=CARTESIAN_POINT('Ctrl Pts',(31.7914861973683,-65.7772714817533,
-225.474527722644));
#226427=CARTESIAN_POINT('Ctrl Pts',(33.1695232342839,-66.7716346400439,
-223.90129326724));
#226428=CARTESIAN_POINT('Ctrl Pts',(35.925597308115,-68.7603609566252,-220.754824356431));
#226429=CARTESIAN_POINT('Ctrl Pts',(38.6817661332381,-70.749049871159,-217.608412929565));
#226430=CARTESIAN_POINT('Ctrl Pts',(41.437980641355,-72.7377225056729,-214.462029323759));
#226431=CARTESIAN_POINT('Ctrl Pts',(24.9106027465158,-60.8049715273879,
-233.340948124015));
#226432=CARTESIAN_POINT('Ctrl Pts',(25.5998098315156,-61.3021744082037,
-232.554282687331));
#226433=CARTESIAN_POINT('Ctrl Pts',(26.2890324103538,-61.7993707608737,
-231.767626642701));
#226434=CARTESIAN_POINT('Ctrl Pts',(26.9782669268481,-62.2965621103122,
-230.980977835653));
#226435=CARTESIAN_POINT('Ctrl Pts',(27.6675014433422,-62.7937534597507,
-230.194329028605));
#226436=CARTESIAN_POINT('Ctrl Pts',(28.3567479253494,-63.2909397940828,
-229.407687476061));
#226437=CARTESIAN_POINT('Ctrl Pts',(29.0460038234333,-63.7881222076912,
-228.621051634203));
#226438=CARTESIAN_POINT('Ctrl Pts',(30.424515619601,-64.7824870349079,-227.047779950486));
#226439=CARTESIAN_POINT('Ctrl Pts',(31.8030646725822,-65.776836354002,-225.474530862664));
#226440=CARTESIAN_POINT('Ctrl Pts',(33.1816379091815,-66.771175783969,-223.901296458627));
#226441=CARTESIAN_POINT('Ctrl Pts',(35.9387843823801,-68.759854643903,-220.754827650554));
#226442=CARTESIAN_POINT('Ctrl Pts',(38.6960255585086,-70.7484948217514,
-217.608416348934));
#226443=CARTESIAN_POINT('Ctrl Pts',(41.4533123673286,-72.737117447414,-214.462032879015));
#226444=CARTESIAN_POINT('Ctrl Pts',(24.9204263182847,-60.8042678820624,
-233.341483208271));
#226445=CARTESIAN_POINT('Ctrl Pts',(25.6098926659838,-61.3014622348707,
-232.554814099759));
#226446=CARTESIAN_POINT('Ctrl Pts',(26.2993748034754,-61.7986498568027,
-231.768154572902));
#226447=CARTESIAN_POINT('Ctrl Pts',(26.9888691299455,-62.2958322905427,
-230.981502444082));
#226448=CARTESIAN_POINT('Ctrl Pts',(27.6783634564157,-62.7930147242826,
-230.194850315263));
#226449=CARTESIAN_POINT('Ctrl Pts',(28.3678699996353,-63.2901919580089,
-229.408205601368));
#226450=CARTESIAN_POINT('Ctrl Pts',(29.0573861713395,-63.7873651018695,
-228.621566733601));
#226451=CARTESIAN_POINT('Ctrl Pts',(30.4364185147476,-64.7817113895908,
-227.048288998068));
#226452=CARTESIAN_POINT('Ctrl Pts',(31.8154889591027,-65.776041494825,-225.475034396628));
#226453=CARTESIAN_POINT('Ctrl Pts',(33.1945841923364,-66.7703611350645,
-223.901794865388));
#226454=CARTESIAN_POINT('Ctrl Pts',(35.9527746588037,-68.7590004155436,
-220.755315802909));
#226455=CARTESIAN_POINT('Ctrl Pts',(38.7110622045295,-70.7475987291489,
-217.608895764391));
#226456=CARTESIAN_POINT('Ctrl Pts',(41.4693966584753,-72.7361776662597,
-214.462504384327));
#226457=CARTESIAN_POINT('Ctrl Pts',(24.9262307371789,-60.8052629613404,
-233.339663481057));
#226458=CARTESIAN_POINT('Ctrl Pts',(25.6159901042832,-61.3024373924278,
-232.553007006783));
#226459=CARTESIAN_POINT('Ctrl Pts',(26.3057643351287,-61.7996053791141,
-231.766359540212));
#226460=CARTESIAN_POINT('Ctrl Pts',(26.9955499476215,-62.2967684208872,
-230.979718973407));
#226461=CARTESIAN_POINT('Ctrl Pts',(27.6853355601145,-62.7939314626603,
-230.193078406603));
#226462=CARTESIAN_POINT('Ctrl Pts',(28.3751325826488,-63.2910895473583,
-229.406444756795));
#226463=CARTESIAN_POINT('Ctrl Pts',(29.0649385371855,-63.7882437431482,
-228.619816524538));
#226464=CARTESIAN_POINT('Ctrl Pts',(30.4445504462589,-64.7825521347279,
-227.046560060024));
#226465=CARTESIAN_POINT('Ctrl Pts',(31.8241976850135,-65.7768451422546,
-225.473325024605));
#226466=CARTESIAN_POINT('Ctrl Pts',(33.2038676569546,-66.7711282018108,
-223.90010380027));
#226467=CARTESIAN_POINT('Ctrl Pts',(35.9632076008367,-68.7596943209232,
-220.753661351601));
#226468=CARTESIAN_POINT('Ctrl Pts',(38.7226365397166,-70.7482214856064,
-217.607272976111));
#226469=CARTESIAN_POINT('Ctrl Pts',(41.4821077889028,-72.7367298763208,
-214.460910461991));
#226470=CARTESIAN_POINT('Ctrl Pts',(24.9320351560731,-60.8062580406183,
-233.337843753845));
#226471=CARTESIAN_POINT('Ctrl Pts',(25.6220875425827,-61.3034125499849,
-232.551199913808));
#226472=CARTESIAN_POINT('Ctrl Pts',(26.312153866782,-61.8005609014255,-231.764564507522));
#226473=CARTESIAN_POINT('Ctrl Pts',(27.0022307652976,-62.2977045512317,
-230.977935502733));
#226474=CARTESIAN_POINT('Ctrl Pts',(27.6923076638132,-62.794848201038,-230.191306497943));
#226475=CARTESIAN_POINT('Ctrl Pts',(28.3823951656622,-63.2919871367077,
-229.404683912223));
#226476=CARTESIAN_POINT('Ctrl Pts',(29.0724909030316,-63.7891223844269,
-228.618066315475));
#226477=CARTESIAN_POINT('Ctrl Pts',(30.4526823777702,-64.7833928798651,
-227.044831121978));
#226478=CARTESIAN_POINT('Ctrl Pts',(31.8329064109243,-65.7776487896842,
-225.471615652582));
#226479=CARTESIAN_POINT('Ctrl Pts',(33.2131511215727,-66.7718952685571,
-223.898412735151));
#226480=CARTESIAN_POINT('Ctrl Pts',(35.9736405428697,-68.7603882263028,
-220.752006900292));
#226481=CARTESIAN_POINT('Ctrl Pts',(38.7342108749039,-70.7488442420639,
-217.605650187832));
#226482=CARTESIAN_POINT('Ctrl Pts',(41.4948189193303,-72.737282086382,-214.459316539654));
#226483=CARTESIAN_POINT('Ctrl Pts',(24.9376768366503,-60.8072592698702,
-233.336009748324));
#226484=CARTESIAN_POINT('Ctrl Pts',(25.6280319185531,-61.3043928842789,
-232.549378593582));
#226485=CARTESIAN_POINT('Ctrl Pts',(26.318399828189,-61.8015207131228,-231.762755190619));
#226486=CARTESIAN_POINT('Ctrl Pts',(27.0087773823957,-62.2986441421295,
-230.976137619604));
#226487=CARTESIAN_POINT('Ctrl Pts',(27.6991549366024,-62.7957675711362,
-230.189520048589));
#226488=CARTESIAN_POINT('Ctrl Pts',(28.3895421644288,-63.2928865877122,
-229.402908327074));
#226489=CARTESIAN_POINT('Ctrl Pts',(29.0799368492491,-63.7900021575995,
-228.616301118674));
#226490=CARTESIAN_POINT('Ctrl Pts',(30.4607262188897,-64.7842332973742,
-227.043086701871));
#226491=CARTESIAN_POINT('Ctrl Pts',(31.8415450550293,-65.778450807822,-225.469890119541));
#226492=CARTESIAN_POINT('Ctrl Pts',(33.2223823764397,-66.772659477679,-223.89670475417));
#226493=CARTESIAN_POINT('Ctrl Pts',(35.9840570192604,-68.7610768173931,
-220.750334023428));
#226494=CARTESIAN_POINT('Ctrl Pts',(38.7458039689211,-70.7494595084382,
-217.604007176241));
#226495=CARTESIAN_POINT('Ctrl Pts',(41.5075840172059,-72.7378246702262,
-214.457700600944));
#226496=CARTESIAN_POINT('Ctrl Pts',(24.9431675857188,-60.8082654676189,
-233.334164524199));
#226497=CARTESIAN_POINT('Ctrl Pts',(25.6338346604351,-61.3053771897629,
-232.547545996672));
#226498=CARTESIAN_POINT('Ctrl Pts',(26.3245132764945,-61.8024835845448,
-231.760934436748));
#226499=CARTESIAN_POINT('Ctrl Pts',(27.0152005013104,-62.2995859346266,
-230.97432807854));
#226500=CARTESIAN_POINT('Ctrl Pts',(27.7058877261263,-62.7966882847084,
-230.187721720333));
#226501=CARTESIAN_POINT('Ctrl Pts',(28.3965835877948,-63.2937865778419,
-229.401120580787));
#226502=CARTESIAN_POINT('Ctrl Pts',(29.0872860637793,-63.7908816992324,
-228.614523442413));
#226503=CARTESIAN_POINT('Ctrl Pts',(30.4686910157482,-64.7850719420134,
-227.041329165664));
#226504=CARTESIAN_POINT('Ctrl Pts',(31.8501220936262,-65.7792496428099,
-225.468150694098));
#226505=CARTESIAN_POINT('Ctrl Pts',(33.231569388313,-66.7734191417836,-223.894982065188));
#226506=CARTESIAN_POINT('Ctrl Pts',(35.9944639776866,-68.7617581397308,
-220.748644807367));
#226507=CARTESIAN_POINT('Ctrl Pts',(38.7574219835962,-70.7500649666192,
-217.602346047653));
#226508=CARTESIAN_POINT('Ctrl Pts',(41.5204085705364,-72.7383548951067,
-214.45606483788));
#226509=CARTESIAN_POINT('Ctrl Pts',(24.9541490838557,-60.8102778631162,
-233.330474075949));
#226510=CARTESIAN_POINT('Ctrl Pts',(25.6454401441992,-61.307345800731,-232.543880802852));
#226511=CARTESIAN_POINT('Ctrl Pts',(26.3367401731056,-61.8044093273887,
-231.757292929005));
#226512=CARTESIAN_POINT('Ctrl Pts',(27.0280467391398,-62.3014695196208,
-230.970708996412));
#226513=CARTESIAN_POINT('Ctrl Pts',(27.719353305174,-62.7985297118529,-230.18412506382));
#226514=CARTESIAN_POINT('Ctrl Pts',(28.4106664345268,-63.2955865581015,
-229.397545088212));
#226515=CARTESIAN_POINT('Ctrl Pts',(29.1019844928396,-63.7926407824983,
-228.610968089891));
#226516=CARTESIAN_POINT('Ctrl Pts',(30.4846206094652,-64.7867492312918,
-227.037814093248));
#226517=CARTESIAN_POINT('Ctrl Pts',(31.8672761708201,-65.7808473127859,
-225.464671843211));
#226518=CARTESIAN_POINT('Ctrl Pts',(33.2499434120597,-66.7749384699927,
-223.891536687223));
#226519=CARTESIAN_POINT('Ctrl Pts',(36.0152778945389,-68.7631207844063,
-220.745266375246));
#226520=CARTESIAN_POINT('Ctrl Pts',(38.7806580129467,-70.7512758829813,
-217.599023790475));
#226521=CARTESIAN_POINT('Ctrl Pts',(41.5460576771974,-72.7394153448676,
-214.45279331175));
#226522=CARTESIAN_POINT('Ctrl Pts',(24.96452603429,-60.8123106330865,-233.326738316813));
#226523=CARTESIAN_POINT('Ctrl Pts',(25.6564783942742,-61.3093307323952,
-232.540170136386));
#226524=CARTESIAN_POINT('Ctrl Pts',(26.3484364151579,-61.8063476946002,
-231.753605361133));
#226525=CARTESIAN_POINT('Ctrl Pts',(27.0403984599708,-62.3033622546844,
-230.967043014045));
#226526=CARTESIAN_POINT('Ctrl Pts',(27.7323605047837,-62.8003768147686,
-230.180480666957));
#226527=CARTESIAN_POINT('Ctrl Pts',(28.4243265937515,-63.2973889636564,
-229.393920760111));
#226528=CARTESIAN_POINT('Ctrl Pts',(29.1162956595838,-63.794399180595,-228.607362656609));
#226529=CARTESIAN_POINT('Ctrl Pts',(30.5002337912484,-64.7884196144722,
-227.034246449605));
#226530=CARTESIAN_POINT('Ctrl Pts',(31.8841836526759,-65.7824324003622,
-225.461137349913));
#226531=CARTESIAN_POINT('Ctrl Pts',(33.2681403403832,-66.7764397401221,
-223.888032432174));
#226532=CARTESIAN_POINT('Ctrl Pts',(36.0360537157978,-68.7644544196418,
-220.741822596696));
#226533=CARTESIAN_POINT('Ctrl Pts',(38.8039937558954,-70.7524476024647,
-217.595629106873));
#226534=CARTESIAN_POINT('Ctrl Pts',(41.5719446953938,-72.740426365189,-214.449442564061));
#226535=CARTESIAN_POINT('Ctrl Pts',(24.9744025307133,-60.8143487212353,
-233.322986925177));
#226536=CARTESIAN_POINT('Ctrl Pts',(25.6670491804662,-61.3113173869818,
-232.536442059561));
#226537=CARTESIAN_POINT('Ctrl Pts',(26.3596977749792,-61.8082844221729,
-231.749898382092));
#226538=CARTESIAN_POINT('Ctrl Pts',(27.0523477402915,-62.3052500852752,
-230.96335555072));
#226539=CARTESIAN_POINT('Ctrl Pts',(27.7449977056038,-62.8022157483775,
-230.176812719347));
#226540=CARTESIAN_POINT('Ctrl Pts',(28.4376490490292,-63.2991800360968,
-229.390270738434));
#226541=CARTESIAN_POINT('Ctrl Pts',(29.1303013990492,-63.7961431156999,
-228.603729386647));
#226542=CARTESIAN_POINT('Ctrl Pts',(30.5156060990893,-64.7900692749063,
-227.030646683075));
#226543=CARTESIAN_POINT('Ctrl Pts',(31.9009147636639,-65.7839906295158,
-225.45756645914));
#226544=CARTESIAN_POINT('Ctrl Pts',(33.2862256991509,-66.777907941617,-223.884487706564));
#226545=CARTESIAN_POINT('Ctrl Pts',(36.0568475701252,-68.7657425658195,
-220.738330201412));
#226546=CARTESIAN_POINT('Ctrl Pts',(38.827478307619,-70.7535611178629,-217.592178452254));
#226547=CARTESIAN_POINT('Ctrl Pts',(41.5981125175426,-72.7413660196969,
-214.446029255158));
#226548=CARTESIAN_POINT('Ctrl Pts',(24.9941555235601,-60.8184248975328,
-233.315484141906));
#226549=CARTESIAN_POINT('Ctrl Pts',(25.6881907528502,-61.3152906961552,
-232.528985905911));
#226550=CARTESIAN_POINT('Ctrl Pts',(26.3822204946216,-61.8121578773183,
-231.74248442401));
#226551=CARTESIAN_POINT('Ctrl Pts',(27.0762463009327,-62.3090257464567,
-230.955980624069));
#226552=CARTESIAN_POINT('Ctrl Pts',(27.7702721072438,-62.8058936155951,
-230.169476824128));
#226553=CARTESIAN_POINT('Ctrl Pts',(28.4642939595846,-63.3027621809775,
-229.382970695078));
#226554=CARTESIAN_POINT('Ctrl Pts',(29.1583128779801,-63.7996309859099,
-228.596462846723));
#226555=CARTESIAN_POINT('Ctrl Pts',(30.5463507147712,-64.7933685957745,
-227.023447150014));
#226556=CARTESIAN_POINT('Ctrl Pts',(31.9343769856396,-65.7871070878229,
-225.450424677593));
#226557=CARTESIAN_POINT('Ctrl Pts',(33.3223964166864,-66.7808443446069,
-223.877398255344));
#226558=CARTESIAN_POINT('Ctrl Pts',(36.0984352787801,-68.768318858175,-220.731345410844));
#226559=CARTESIAN_POINT('Ctrl Pts',(38.8744474110663,-70.7557881486592,
-217.585277143015));
#226560=CARTESIAN_POINT('Ctrl Pts',(41.6504481618404,-72.7432453287128,
-214.439202637353));
#226561=CARTESIAN_POINT('Ctrl Pts',(25.0118948272389,-60.8225311816015,
-233.307912950748));
#226562=CARTESIAN_POINT('Ctrl Pts',(25.7074533125622,-61.319278145358,-232.521455721897));
#226563=CARTESIAN_POINT('Ctrl Pts',(26.4029963020791,-61.8160309424671,
-231.734989391403));
#226564=CARTESIAN_POINT('Ctrl Pts',(27.0985290755007,-62.3127871125508,
-230.948517073201));
#226565=CARTESIAN_POINT('Ctrl Pts',(27.7940618489222,-62.8095432826346,
-230.162044755));
#226566=CARTESIAN_POINT('Ctrl Pts',(28.489584316755,-63.3063028673177,-229.375566396309));
#226567=CARTESIAN_POINT('Ctrl Pts',(29.1850996372909,-63.8030643940992,
-228.589083860001));
#226568=CARTESIAN_POINT('Ctrl Pts',(30.5761302783625,-64.7965874476622,
-227.016118787385));
#226569=CARTESIAN_POINT('Ctrl Pts',(31.9671328527444,-65.7901180259831,
-225.443137312419));
#226570=CARTESIAN_POINT('Ctrl Pts',(33.3581205213136,-66.7836499900577,
-223.870147199431));
#226571=CARTESIAN_POINT('Ctrl Pts',(36.140095858452,-68.7707139182068,-220.724166973453));
#226572=CARTESIAN_POINT('Ctrl Pts',(38.9220129137361,-70.7577827632511,
-217.578152986549));
#226573=CARTESIAN_POINT('Ctrl Pts',(41.7039086779697,-72.7448392550568,
-214.432127077688));
#226574=CARTESIAN_POINT('Ctrl Pts',(25.028605078732,-60.8264461849104,-233.300589177504));
#226575=CARTESIAN_POINT('Ctrl Pts',(25.7257590504183,-61.3230773961178,
-232.514138876127));
#226576=CARTESIAN_POINT('Ctrl Pts',(26.4228956738429,-61.8197151427821,
-231.727678440368));
#226577=CARTESIAN_POINT('Ctrl Pts',(27.1200213189657,-62.3163563966737,
-230.941211605428));
#226578=CARTESIAN_POINT('Ctrl Pts',(27.8171469640885,-62.8129976505652,
-230.154744770487));
#226579=CARTESIAN_POINT('Ctrl Pts',(28.514261502952,-63.3096424726104,-229.368271461406));
#226580=CARTESIAN_POINT('Ctrl Pts',(29.2113685617452,-63.8062891397564,
-228.581793805278));
#226581=CARTESIAN_POINT('Ctrl Pts',(30.6055826793317,-64.7995824740485,
-227.008838493021));
#226582=CARTESIAN_POINT('Ctrl Pts',(31.9997674609787,-65.7928829112188,
-225.435866135329));
#226583=CARTESIAN_POINT('Ctrl Pts',(33.393937296167,-66.786183616434,-223.862885177104));
#226584=CARTESIAN_POINT('Ctrl Pts',(36.1822769665438,-68.7727850268643,
-220.716923260653));
#226585=CARTESIAN_POINT('Ctrl Pts',(38.9705580867346,-70.7593869240872,
-217.570927667784));
#226586=CARTESIAN_POINT('Ctrl Pts',(41.7588188049893,-72.745971187409,-214.424920813073));
#226587=CARTESIAN_POINT('Ctrl Pts',(25.0620255817184,-60.8342761915281,
-233.285941631018));
#226588=CARTESIAN_POINT('Ctrl Pts',(25.7623705261304,-61.3306758976375,
-232.499505184585));
#226589=CARTESIAN_POINT('Ctrl Pts',(26.4626944173704,-61.8270835434123,
-231.713056538299));
#226590=CARTESIAN_POINT('Ctrl Pts',(27.1630058058958,-62.3234949649194,
-230.926600669881));
#226591=CARTESIAN_POINT('Ctrl Pts',(27.8633171944211,-62.8199063864266,
-230.140144801462));
#226592=CARTESIAN_POINT('Ctrl Pts',(28.5636158753459,-63.3163216831959,
-229.353681591601));
#226593=CARTESIAN_POINT('Ctrl Pts',(29.2639064106539,-63.8127386310709,
-228.567213695831));
#226594=CARTESIAN_POINT('Ctrl Pts',(30.6644874812699,-64.8055725268209,
-226.994277904292));
#226595=CARTESIAN_POINT('Ctrl Pts',(32.0650366774472,-65.7984126816902,
-225.421323781149));
#226596=CARTESIAN_POINT('Ctrl Pts',(33.4655708458739,-66.7912508691866,
-223.848361132451));
#226597=CARTESIAN_POINT('Ctrl Pts',(36.2666391827274,-68.7769272441794,
-220.702435835054));
#226598=CARTESIAN_POINT('Ctrl Pts',(39.0676484327315,-70.7625952457594,
-217.556477030254));
#226599=CARTESIAN_POINT('Ctrl Pts',(41.8686390590285,-72.7482350521135,
-214.410508283843));
#226600=CARTESIAN_POINT('Ctrl Pts',(25.0913820158672,-60.8413726539041,
-233.272320165694));
#226601=CARTESIAN_POINT('Ctrl Pts',(25.7952223871138,-61.337539263733,-232.485770621816));
#226602=CARTESIAN_POINT('Ctrl Pts',(26.4990562522867,-61.8337088794851,
-231.699217348229));
#226603=CARTESIAN_POINT('Ctrl Pts',(27.2028964362607,-62.3298740344814,
-230.912668010765));
#226604=CARTESIAN_POINT('Ctrl Pts',(27.9067366202345,-62.8260391894777,
-230.126118673301));
#226605=CARTESIAN_POINT('Ctrl Pts',(28.6105819801057,-63.3222004675808,
-229.339572581631));
#226606=CARTESIAN_POINT('Ctrl Pts',(29.314434077262,-63.8183564731875,-228.553030636562));
#226607=CARTESIAN_POINT('Ctrl Pts',(30.7221382715748,-64.8106684844009,
-226.97994674642));
#226608=CARTESIAN_POINT('Ctrl Pts',(32.1298688397377,-65.8029595883788,
-225.406879087961));
#226609=CARTESIAN_POINT('Ctrl Pts',(33.5376184032793,-66.7952312053955,
-223.833823110276));
#226610=CARTESIAN_POINT('Ctrl Pts',(36.3531175303626,-68.7797744394288,
-220.687711154908));
#226611=CARTESIAN_POINT('Ctrl Pts',(39.1686880217984,-70.7642419152226,
-217.541643153526));
#226612=CARTESIAN_POINT('Ctrl Pts',(41.9842864659859,-72.7486501639975,
-214.39559293419));
#226613=CARTESIAN_POINT('Ctrl Pts',(25.1256029177818,-60.8447964462213,
-233.262708527412));
#226614=CARTESIAN_POINT('Ctrl Pts',(25.8323432559684,-61.3411439778804,
-232.475469715128));
#226615=CARTESIAN_POINT('Ctrl Pts',(26.5393879179131,-61.8373317659467,
-231.688406549544));
#226616=CARTESIAN_POINT('Ctrl Pts',(27.2465878469089,-62.3334358738351,
-230.90143275512));
#226617=CARTESIAN_POINT('Ctrl Pts',(27.9537877759048,-62.8295399817235,
-230.114458960696));
#226618=CARTESIAN_POINT('Ctrl Pts',(28.6611482655484,-63.3255577393973,
-229.327577621181));
#226619=CARTESIAN_POINT('Ctrl Pts',(29.3686016850915,-63.8215238522036,
-228.540749713863));
#226620=CARTESIAN_POINT('Ctrl Pts',(30.7835085241778,-64.8134560778162,
-226.967093899227));
#226621=CARTESIAN_POINT('Ctrl Pts',(32.198778370749,-65.8051862301184,-225.3936468087));
#226622=CARTESIAN_POINT('Ctrl Pts',(33.6141958867398,-66.7968253706499,
-223.820284551445));
#226623=CARTESIAN_POINT('Ctrl Pts',(36.4450309187215,-68.7801036517128,
-220.673560036935));
#226624=CARTESIAN_POINT('Ctrl Pts',(39.2764551401188,-70.7630188613062,
-217.527174130311));
#226625=CARTESIAN_POINT('Ctrl Pts',(42.1080287367154,-72.7457990899024,
-214.3808746454));
#226626=CARTESIAN_POINT('Ctrl Pts',(25.1598238196964,-60.8482202385386,
-233.25309688913));
#226627=CARTESIAN_POINT('Ctrl Pts',(25.8694641248229,-61.3447486920278,
-232.465168808441));
#226628=CARTESIAN_POINT('Ctrl Pts',(26.5797195835393,-61.8409546524082,
-231.677595750858));
#226629=CARTESIAN_POINT('Ctrl Pts',(27.2902792575572,-62.3369977131888,
-230.890197499475));
#226630=CARTESIAN_POINT('Ctrl Pts',(28.000838931575,-62.8330407739693,-230.102799248092));
#226631=CARTESIAN_POINT('Ctrl Pts',(28.711714550991,-63.3289150112138,-229.315582660731));
#226632=CARTESIAN_POINT('Ctrl Pts',(29.4227692929209,-63.8246912312197,
-228.528468791165));
#226633=CARTESIAN_POINT('Ctrl Pts',(30.8448787767808,-64.8162436712314,
-226.954241052034));
#226634=CARTESIAN_POINT('Ctrl Pts',(32.2676879017602,-65.8074128718581,
-225.380414529439));
#226635=CARTESIAN_POINT('Ctrl Pts',(33.6907733702002,-66.7984195359043,
-223.806745992614));
#226636=CARTESIAN_POINT('Ctrl Pts',(36.5369443070804,-68.7804328639968,
-220.659408918962));
#226637=CARTESIAN_POINT('Ctrl Pts',(39.3842222584393,-70.7617958073898,
-217.512705107097));
#226638=CARTESIAN_POINT('Ctrl Pts',(42.2317710074449,-72.7429480158072,
-214.366156356611));
#226639=CARTESIAN_POINT('Ctrl Pts',(25.1936739556362,-60.8507158919519,
-233.244352036751));
#226640=CARTESIAN_POINT('Ctrl Pts',(25.9062554175954,-61.3475191565963,
-232.455522106742));
#226641=CARTESIAN_POINT('Ctrl Pts',(26.6199310089813,-61.8437435167674,
-231.667324698448));
#226642=CARTESIAN_POINT('Ctrl Pts',(27.3341145564557,-62.3396921598031,
-230.879418569252));
#226643=CARTESIAN_POINT('Ctrl Pts',(28.0482981039303,-62.8356408028389,
-230.091512440055));
#226644=CARTESIAN_POINT('Ctrl Pts',(28.7630142200764,-63.3313013469077,
-229.303912100956));
#226645=CARTESIAN_POINT('Ctrl Pts',(29.4780199079502,-63.8268014559396,
-228.516477155575));
#226646=CARTESIAN_POINT('Ctrl Pts',(30.9080312836978,-64.8178016740036,
-226.941607264814));
#226647=CARTESIAN_POINT('Ctrl Pts',(32.3391739164292,-65.8081747617964,
-225.367383553375));
#226648=CARTESIAN_POINT('Ctrl Pts',(33.7707373952718,-66.7982992813128,
-223.793398542109));
#226649=CARTESIAN_POINT('Ctrl Pts',(36.6338643529568,-68.7785483203456,
-220.645428519576));
#226650=CARTESIAN_POINT('Ctrl Pts',(39.498692720429,-70.7577954999793,-217.498424772054));
#226651=CARTESIAN_POINT('Ctrl Pts',(42.363907023339,-72.7367527914189,-214.351639090142));
#226652=CARTESIAN_POINT('Ctrl Pts',(25.2239774050683,-60.8541676049626,
-233.234470884236));
#226653=CARTESIAN_POINT('Ctrl Pts',(25.9398083842247,-61.3511430455559,
-232.444758300872));
#226654=CARTESIAN_POINT('Ctrl Pts',(26.6572825734193,-61.8472255929447,
-231.655996189968));
#226655=CARTESIAN_POINT('Ctrl Pts',(27.3754647705453,-62.3429113806012,
-230.867638000096));
#226656=CARTESIAN_POINT('Ctrl Pts',(28.0936469676712,-62.8385971682577,
-230.079279810225));
#226657=CARTESIAN_POINT('Ctrl Pts',(28.8125820204444,-63.3338632665416,
-229.291352292986));
#226658=CARTESIAN_POINT('Ctrl Pts',(29.5319096752348,-63.8289050323554,
-228.503647571677));
#226659=CARTESIAN_POINT('Ctrl Pts',(30.9705649848157,-64.8189885639829,
-226.928238129057));
#226660=CARTESIAN_POINT('Ctrl Pts',(32.4107560406701,-65.8081944618785,
-225.353700434162));
#226661=CARTESIAN_POINT('Ctrl Pts',(33.8514884032197,-66.7970717553631,
-223.779466811102));
#226662=CARTESIAN_POINT('Ctrl Pts',(36.732953128319,-68.7748263423323,-220.630999564983));
#226663=CARTESIAN_POINT('Ctrl Pts',(39.6166287632978,-70.7512448922044,
-217.483776946995));
#226664=CARTESIAN_POINT('Ctrl Pts',(42.5007756355285,-72.7273057434785,
-214.336817183699));
#226665=CARTESIAN_POINT('Ctrl Pts',(25.2542808545004,-60.8576193179734,
-233.224589731722));
#226666=CARTESIAN_POINT('Ctrl Pts',(25.9733613508541,-61.3547669345154,
-232.433994495002));
#226667=CARTESIAN_POINT('Ctrl Pts',(26.6946341378572,-61.850707669122,-231.644667681488));
#226668=CARTESIAN_POINT('Ctrl Pts',(27.4168149846347,-62.3461306013993,
-230.855857430941));
#226669=CARTESIAN_POINT('Ctrl Pts',(28.1389958314122,-62.8415535336766,
-230.067047180394));
#226670=CARTESIAN_POINT('Ctrl Pts',(28.8621498208122,-63.3364251861756,
-229.278792485017));
#226671=CARTESIAN_POINT('Ctrl Pts',(29.5857994425194,-63.8310086087711,
-228.490817987778));
#226672=CARTESIAN_POINT('Ctrl Pts',(31.0330986859336,-64.8201754539622,
-226.914868993301));
#226673=CARTESIAN_POINT('Ctrl Pts',(32.482338164911,-65.8082141619607,-225.340017314949));
#226674=CARTESIAN_POINT('Ctrl Pts',(33.9322394111677,-66.7958442294134,
-223.765535080096));
#226675=CARTESIAN_POINT('Ctrl Pts',(36.8320419036812,-68.771104364319,-220.61657061039));
#226676=CARTESIAN_POINT('Ctrl Pts',(39.7345648061665,-70.7446942844296,
-217.469129121935));
#226677=CARTESIAN_POINT('Ctrl Pts',(42.637644247718,-72.7178586955381,-214.321995277256));
#226678=CARTESIAN_POINT('Ctrl Pts',(25.2821906319223,-60.8614218083708,
-233.214245961014));
#226679=CARTESIAN_POINT('Ctrl Pts',(26.0046873376329,-61.35871072973,-232.422705498826));
#226680=CARTESIAN_POINT('Ctrl Pts',(26.7300272921764,-61.854405153137,-231.632810266957));
#226681=CARTESIAN_POINT('Ctrl Pts',(27.4564885610292,-62.3494441225829,
-230.843550233226));
#226682=CARTESIAN_POINT('Ctrl Pts',(28.182949829882,-62.8444830920289,-230.054290199494));
#226683=CARTESIAN_POINT('Ctrl Pts',(28.9106256129361,-63.3388181928255,
-229.265721482054));
#226684=CARTESIAN_POINT('Ctrl Pts',(29.6389030120051,-63.8327945119493,
-228.477491114052));
#226685=CARTESIAN_POINT('Ctrl Pts',(31.0954578101431,-64.8207471501967,
-226.901030378049));
#226686=CARTESIAN_POINT('Ctrl Pts',(32.5543706785782,-65.8072943179338,
-225.32589662341));
#226687=CARTESIAN_POINT('Ctrl Pts',(34.0140584320924,-66.7933503332008,
-223.751191978427));
#226688=CARTESIAN_POINT('Ctrl Pts',(36.933433939121,-68.7654623637348,-220.60178268846));
#226689=CARTESIAN_POINT('Ctrl Pts',(39.8560206222034,-70.7355537328838,
-217.454158252827));
#226690=CARTESIAN_POINT('Ctrl Pts',(42.7792356116896,-72.705154549818,-214.306877306875));
#226691=CARTESIAN_POINT('Ctrl Pts',(25.3082796911041,-60.8654535469475,
-233.203637421846));
#226692=CARTESIAN_POINT('Ctrl Pts',(26.0341343285133,-61.3629238744168,
-232.411039848471));
#226693=CARTESIAN_POINT('Ctrl Pts',(26.7636013838676,-61.8583152760603,
-231.620533187723));
#226694=CARTESIAN_POINT('Ctrl Pts',(27.4944243031966,-62.3528874641244,
-230.830789824077));
#226695=CARTESIAN_POINT('Ctrl Pts',(28.2252472225255,-62.8474596521885,
-230.041046460431));
#226696=CARTESIAN_POINT('Ctrl Pts',(28.9575562895767,-63.3411438699236,
-229.252145525666));
#226697=CARTESIAN_POINT('Ctrl Pts',(29.6905827327532,-63.8343860369735,
-228.463645185323));
#226698=CARTESIAN_POINT('Ctrl Pts',(31.1566356191065,-64.8208703710732,
-226.886644504638));
#226699=CARTESIAN_POINT('Ctrl Pts',(32.6255046561051,-65.8056211821729,
-225.311217867621));
#226700=CARTESIAN_POINT('Ctrl Pts',(34.0952688014063,-66.7897856212239,
-223.736281731367));
#226701=CARTESIAN_POINT('Ctrl Pts',(37.034797092009,-68.7581144993257,-220.58640945886));
#226702=CARTESIAN_POINT('Ctrl Pts',(39.9780639773415,-70.7240153450236,
-217.438595831035));
#226703=CARTESIAN_POINT('Ctrl Pts',(42.922034708619,-72.6893523415957,-214.291161723059));
#226704=CARTESIAN_POINT('Ctrl Pts',(25.3604578094675,-60.8735170241007,
-233.18242034351));
#226705=CARTESIAN_POINT('Ctrl Pts',(26.0930283102741,-61.3713501637903,
-232.387708547763));
#226706=CARTESIAN_POINT('Ctrl Pts',(26.8307495672501,-61.866135521907,-231.595979029253));
#226707=CARTESIAN_POINT('Ctrl Pts',(27.5702957875313,-62.3597741472074,
-230.805269005779));
#226708=CARTESIAN_POINT('Ctrl Pts',(28.3098420078126,-62.8534127725078,
-230.014558982304));
#226709=CARTESIAN_POINT('Ctrl Pts',(29.0514176428578,-63.3457952241198,
-229.224993612889));
#226710=CARTESIAN_POINT('Ctrl Pts',(29.7939421742496,-63.8375690870219,
-228.435953327864));
#226711=CARTESIAN_POINT('Ctrl Pts',(31.2789912370331,-64.8211168128261,
-226.857872757815));
#226712=CARTESIAN_POINT('Ctrl Pts',(32.767772611159,-65.8022749106513,-225.281860356042));
#226713=CARTESIAN_POINT('Ctrl Pts',(34.2576895400343,-66.7826561972701,
-223.706461237247));
#226714=CARTESIAN_POINT('Ctrl Pts',(37.237523397785,-68.7434187705077,-220.555662999657));
#226715=CARTESIAN_POINT('Ctrl Pts',(40.2221506876178,-70.7009385693032,
-217.407470987453));
#226716=CARTESIAN_POINT('Ctrl Pts',(43.2076329024777,-72.657747925151,-214.259730555427));
#226717=CARTESIAN_POINT('Ctrl Pts',(25.4136698948603,-60.8775733111457,
-233.1647909109));
#226718=CARTESIAN_POINT('Ctrl Pts',(26.1536009721352,-61.3753309304317,
-232.367988911507));
#226719=CARTESIAN_POINT('Ctrl Pts',(26.9003944903513,-61.8688530492783,
-231.575160164634));
#226720=CARTESIAN_POINT('Ctrl Pts',(27.6494543016586,-62.3608735835334,
-230.783584826932));
#226721=CARTESIAN_POINT('Ctrl Pts',(28.3985141129659,-62.8528941177885,
-229.992009489228));
#226722=CARTESIAN_POINT('Ctrl Pts',(29.1501449587015,-63.3432443646947,
-229.201875553329));
#226723=CARTESIAN_POINT('Ctrl Pts',(29.902937659956,-63.8328099372364,-228.412377972218));
#226724=CARTESIAN_POINT('Ctrl Pts',(31.4085230624649,-64.8119410823196,
-226.833382809995));
#226725=CARTESIAN_POINT('Ctrl Pts',(32.9186915675153,-65.7879847694566,
-225.256902902535));
#226726=CARTESIAN_POINT('Ctrl Pts',(34.4301958247084,-66.7630648301267,
-223.681133553689));
#226727=CARTESIAN_POINT('Ctrl Pts',(37.4532043390948,-68.7132249514667,
-220.529594855996));
#226728=CARTESIAN_POINT('Ctrl Pts',(40.4819176467888,-70.6593236327973,
-217.381117488375));
#226729=CARTESIAN_POINT('Ctrl Pts',(43.5116000921785,-72.6045769412523,
-214.233142011455));
#226730=CARTESIAN_POINT('Ctrl Pts',(25.4734681104549,-60.8745649395491,
-233.152705479171));
#226731=CARTESIAN_POINT('Ctrl Pts',(26.2191301593905,-61.3728030581697,
-232.352982827705));
#226732=CARTESIAN_POINT('Ctrl Pts',(26.9737314089713,-61.8653651155087,
-231.558531400184));
#226733=CARTESIAN_POINT('Ctrl Pts',(27.7312103498245,-62.3559170177131,
-230.765669056017));
#226734=CARTESIAN_POINT('Ctrl Pts',(28.4886892906776,-62.8464689199175,
-229.972806711851));
#226735=CARTESIAN_POINT('Ctrl Pts',(29.2494572009032,-63.3347856810085,
-229.181797847991));
#226736=CARTESIAN_POINT('Ctrl Pts',(30.0116917876015,-63.8220563583486,
-228.391588810695));
#226737=CARTESIAN_POINT('Ctrl Pts',(31.5361609609982,-64.7965977130286,
-226.811170736103));
#226738=CARTESIAN_POINT('Ctrl Pts',(33.0664220838837,-65.7670232712464,
-225.233920858118));
#226739=CARTESIAN_POINT('Ctrl Pts',(34.5983413220466,-66.7361768147042,
-223.657538786233));
#226740=CARTESIAN_POINT('Ctrl Pts',(37.6621797983723,-68.6744839016197,
-220.504774642461));
#226741=CARTESIAN_POINT('Ctrl Pts',(40.7331349268486,-70.6074216926982,
-217.355782960055));
#226742=CARTESIAN_POINT('Ctrl Pts',(43.8052734509942,-72.5392749729601,
-214.207386766717));
#226743=CARTESIAN_POINT('Ctrl Pts',(25.5332663260497,-60.8715565679525,
-233.140620047442));
#226744=CARTESIAN_POINT('Ctrl Pts',(26.2846593466459,-61.3702751859077,
-232.337976743902));
#226745=CARTESIAN_POINT('Ctrl Pts',(27.0470683275914,-61.861877181739,-231.541902635733));
#226746=CARTESIAN_POINT('Ctrl Pts',(27.8129663979903,-62.3509604518928,
-230.747753285103));
#226747=CARTESIAN_POINT('Ctrl Pts',(28.5788644683892,-62.8400437220466,
-229.953603934473));
#226748=CARTESIAN_POINT('Ctrl Pts',(29.3487694431048,-63.3263269973223,
-229.161720142653));
#226749=CARTESIAN_POINT('Ctrl Pts',(30.120445915247,-63.8113027794608,-228.370799649172));
#226750=CARTESIAN_POINT('Ctrl Pts',(31.6637988595316,-64.7812543437376,
-226.788958662211));
#226751=CARTESIAN_POINT('Ctrl Pts',(33.2141526002521,-65.7460617730361,
-225.210938813702));
#226752=CARTESIAN_POINT('Ctrl Pts',(34.7664868193848,-66.7092887992816,
-223.633944018777));
#226753=CARTESIAN_POINT('Ctrl Pts',(37.8711552576499,-68.6357428517727,
-220.479954428925));
#226754=CARTESIAN_POINT('Ctrl Pts',(40.9843522069086,-70.555519752599,-217.330448431736));
#226755=CARTESIAN_POINT('Ctrl Pts',(44.0989468098099,-72.4739730046678,
-214.18163152198));
#226756=CARTESIAN_POINT('Ctrl Pts',(25.5832151954094,-60.8726283032168,
-233.124939038994));
#226757=CARTESIAN_POINT('Ctrl Pts',(26.3412812962705,-61.3709102534954,
-232.320159632019));
#226758=CARTESIAN_POINT('Ctrl Pts',(27.1119488435164,-61.8607811001136,
-231.522967655684));
#226759=CARTESIAN_POINT('Ctrl Pts',(27.8865579092606,-62.347663656611,-230.727938128436));
#226760=CARTESIAN_POINT('Ctrl Pts',(28.6611669750047,-62.8345462131084,
-229.932908601188));
#226761=CARTESIAN_POINT('Ctrl Pts',(29.4403191496334,-63.3181119795184,
-229.140447526113));
#226762=CARTESIAN_POINT('Ctrl Pts',(30.2214658612003,-63.8001296619401,
-228.349062770292));
#226763=CARTESIAN_POINT('Ctrl Pts',(31.783759284334,-64.7641650267834,-226.766293258651));
#226764=CARTESIAN_POINT('Ctrl Pts',(33.353939516948,-65.7221108760403,-225.187799366854));
#226765=CARTESIAN_POINT('Ctrl Pts',(34.9263287803327,-66.6781922113775,
-223.610428795026));
#226766=CARTESIAN_POINT('Ctrl Pts',(38.071107307102,-68.590354882052,-220.455687651369));
#226767=CARTESIAN_POINT('Ctrl Pts',(41.2254251684497,-70.494636879644,-217.305890990877));
#226768=CARTESIAN_POINT('Ctrl Pts',(44.381286951629,-72.3973753477236,-214.156833956015));
#226769=CARTESIAN_POINT('Ctrl Pts',(25.6298304748707,-60.8753734341798,
-233.107177069033));
#226770=CARTESIAN_POINT('Ctrl Pts',(26.3965314717851,-61.3714239166506,
-232.301492490062));
#226771=CARTESIAN_POINT('Ctrl Pts',(27.1765365083298,-61.8582017525339,
-231.503828898795));
#226772=CARTESIAN_POINT('Ctrl Pts',(27.960699151696,-62.3416685933693,-230.708430592375));
#226773=CARTESIAN_POINT('Ctrl Pts',(28.7448617950622,-62.8251354342047,
-229.913032285956));
#226774=CARTESIAN_POINT('Ctrl Pts',(29.5338172036037,-63.3049330183218,
-229.120332249855));
#226775=CARTESIAN_POINT('Ctrl Pts',(30.3248744392529,-63.7830152939694,
-228.328756578445));
#226776=CARTESIAN_POINT('Ctrl Pts',(31.9069889105511,-64.7391798452646,
-226.745605235623));
#226777=CARTESIAN_POINT('Ctrl Pts',(33.4974147722857,-65.6885985452027,
-225.166922566632));
#226778=CARTESIAN_POINT('Ctrl Pts',(35.0901638016772,-66.6359498673557,
-223.589403428947));
#226779=CARTESIAN_POINT('Ctrl Pts',(38.2756618604604,-68.5306525116616,
-220.434365153576));
#226780=CARTESIAN_POINT('Ctrl Pts',(41.4711974327502,-70.4166207416591,
-217.284462017333));
#226781=CARTESIAN_POINT('Ctrl Pts',(44.6683526580257,-72.3008817462311,
-214.135317230106));
#226782=CARTESIAN_POINT('Ctrl Pts',(25.6764457543321,-60.8781185651427,
-233.089415099072));
#226783=CARTESIAN_POINT('Ctrl Pts',(26.4517816472997,-61.3719375798059,
-232.282825348105));
#226784=CARTESIAN_POINT('Ctrl Pts',(27.2411241731431,-61.8556224049542,
-231.484690141905));
#226785=CARTESIAN_POINT('Ctrl Pts',(28.0348403941315,-62.3356735301276,
-230.688923056315));
#226786=CARTESIAN_POINT('Ctrl Pts',(28.8285566151198,-62.8157246553009,
-229.893155970723));
#226787=CARTESIAN_POINT('Ctrl Pts',(29.6273152575741,-63.2917540571251,
-229.100216973599));
#226788=CARTESIAN_POINT('Ctrl Pts',(30.4282830173054,-63.7659009259987,
-228.308450386598));
#226789=CARTESIAN_POINT('Ctrl Pts',(32.0302185367682,-64.7141946637459,
-226.724917212596));
#226790=CARTESIAN_POINT('Ctrl Pts',(33.6408900276233,-65.6550862143651,
-225.14604576641));
#226791=CARTESIAN_POINT('Ctrl Pts',(35.2539988230218,-66.5937075233338,
-223.568378062868));
#226792=CARTESIAN_POINT('Ctrl Pts',(38.4802164138187,-68.4709501412712,
-220.413042655783));
#226793=CARTESIAN_POINT('Ctrl Pts',(41.7169696970508,-70.3386046036742,
-217.263033043788));
#226794=CARTESIAN_POINT('Ctrl Pts',(44.9554183644225,-72.2043881447385,
-214.113800504198));
#226795=CARTESIAN_POINT('Ctrl Pts',(25.7357162038904,-60.870117557065,-233.078364689706));
#226796=CARTESIAN_POINT('Ctrl Pts',(26.5183910989635,-61.3620069392732,
-232.270042402379));
#226797=CARTESIAN_POINT('Ctrl Pts',(27.3162411879881,-61.842621457398,-231.470961385261));
#226798=CARTESIAN_POINT('Ctrl Pts',(28.1188352251337,-62.3191557444292,
-230.674449007438));
#226799=CARTESIAN_POINT('Ctrl Pts',(28.9214292622792,-62.7956900314603,
-229.877936629616));
#226800=CARTESIAN_POINT('Ctrl Pts',(29.7294897040872,-63.2677206749556,
-229.084499084141));
#226801=CARTESIAN_POINT('Ctrl Pts',(30.5399444913362,-63.7376360518426,
-228.292329686201));
#226802=CARTESIAN_POINT('Ctrl Pts',(32.1608540658341,-64.6774668056166,
-226.707990890321));
#226803=CARTESIAN_POINT('Ctrl Pts',(33.7912315861003,-65.6089833988707,
-225.128696643096));
#226804=CARTESIAN_POINT('Ctrl Pts',(35.4242480247001,-66.5379429467924,
-223.550693656299));
#226805=CARTESIAN_POINT('Ctrl Pts',(38.6902809018998,-68.3958620426357,
-220.394687682705));
#226806=CARTESIAN_POINT('Ctrl Pts',(41.9677233302676,-70.2429924486788,
-217.244409494466));
#226807=CARTESIAN_POINT('Ctrl Pts',(45.2469984405841,-72.088022285615,-214.09495601129));
#226808=CARTESIAN_POINT('Ctrl Pts',(25.8011224073928,-60.8541224995348,
-233.072388186401));
#226809=CARTESIAN_POINT('Ctrl Pts',(26.5882772139689,-61.345584476566,-232.260902563554));
#226810=CARTESIAN_POINT('Ctrl Pts',(27.3926111430279,-61.824140301072,-231.460141397784));
#226811=CARTESIAN_POINT('Ctrl Pts',(28.2023317845711,-62.2979002023416,
-230.662317129508));
#226812=CARTESIAN_POINT('Ctrl Pts',(29.0120524261143,-62.7716601036112,
-229.864492861231));
#226813=CARTESIAN_POINT('Ctrl Pts',(29.8279705672755,-63.2401673093096,
-229.070199114559));
#226814=CARTESIAN_POINT('Ctrl Pts',(30.6466000725898,-63.7061844369386,
-228.277344321055));
#226815=CARTESIAN_POINT('Ctrl Pts',(32.2838590832184,-64.6382186921966,
-226.691634734048));
#226816=CARTESIAN_POINT('Ctrl Pts',(33.9318380253269,-65.5604762032412,
-225.111654172302));
#226817=CARTESIAN_POINT('Ctrl Pts',(35.582792800409,-66.4797047104531,-223.533108945327));
#226818=CARTESIAN_POINT('Ctrl Pts',(38.884702350573,-68.3181617248767,-220.376018491376));
#226819=CARTESIAN_POINT('Ctrl Pts',(42.1994895547755,-70.143871943617,-217.225335489343));
#226820=CARTESIAN_POINT('Ctrl Pts',(45.5163300351324,-71.9671084389128,
-214.075544244624));
#226821=CARTESIAN_POINT('Ctrl Pts',(25.8665286108953,-60.8381274420046,
-233.066411683095));
#226822=CARTESIAN_POINT('Ctrl Pts',(26.6581633289744,-61.3291620138588,
-232.251762724729));
#226823=CARTESIAN_POINT('Ctrl Pts',(27.4689810980677,-61.805659144746,-231.449321410308));
#226824=CARTESIAN_POINT('Ctrl Pts',(28.2858283440085,-62.276644660254,-230.650185251577));
#226825=CARTESIAN_POINT('Ctrl Pts',(29.1026755899493,-62.747630175762,-229.851049092846));
#226826=CARTESIAN_POINT('Ctrl Pts',(29.9264514304638,-63.2126139436637,
-229.055899144978));
#226827=CARTESIAN_POINT('Ctrl Pts',(30.7532556538434,-63.6747328220346,
-228.26235895591));
#226828=CARTESIAN_POINT('Ctrl Pts',(32.4068641006027,-64.5989705787766,
-226.675278577774));
#226829=CARTESIAN_POINT('Ctrl Pts',(34.0724444645535,-65.5119690076117,
-225.094611701508));
#226830=CARTESIAN_POINT('Ctrl Pts',(35.7413375761177,-66.4214664741137,
-223.515524234354));
#226831=CARTESIAN_POINT('Ctrl Pts',(39.0791237992462,-68.2404614071178,
-220.357349300048));
#226832=CARTESIAN_POINT('Ctrl Pts',(42.4312557792835,-70.0447514385552,
-217.206261484219));
#226833=CARTESIAN_POINT('Ctrl Pts',(45.7856616296808,-71.8461945922107,
-214.056132477959));
#226834=CARTESIAN_POINT('Ctrl Pts',(25.9160424850282,-60.8332597800929,
-233.053095414693));
#226835=CARTESIAN_POINT('Ctrl Pts',(26.7216988487821,-61.3154617178527,
-232.241381282086));
#226836=CARTESIAN_POINT('Ctrl Pts',(27.5420567082342,-61.7860906307777,
-231.439128672818));
#226837=CARTESIAN_POINT('Ctrl Pts',(28.3681860245984,-62.2513966239306,
-230.64015111493));
#226838=CARTESIAN_POINT('Ctrl Pts',(29.1943153409628,-62.7167026170834,
-229.841173557043));
#226839=CARTESIAN_POINT('Ctrl Pts',(30.0266724628494,-63.1764484440297,
-229.045833737559));
#226840=CARTESIAN_POINT('Ctrl Pts',(30.8620259206422,-63.633275037949,-228.252108649693));
#226841=CARTESIAN_POINT('Ctrl Pts',(32.5327328362278,-64.5469282257876,
-226.664658473961));
#226842=CARTESIAN_POINT('Ctrl Pts',(34.215164199298,-65.4492058327905,-225.083554042117));
#226843=CARTESIAN_POINT('Ctrl Pts',(35.9011649485234,-66.3475812818863,
-223.504153956677));
#226844=CARTESIAN_POINT('Ctrl Pts',(39.273166446974,-68.1443321800779,-220.345353785796));
#226845=CARTESIAN_POINT('Ctrl Pts',(42.6601436512792,-69.9251393601785,
-217.193943963384));
#226846=CARTESIAN_POINT('Ctrl Pts',(46.0496409219808,-71.7026940143502,
-214.043578157589));
#226847=CARTESIAN_POINT('Ctrl Pts',(25.9715990783732,-60.8263824397187,
-233.038076562284));
#226848=CARTESIAN_POINT('Ctrl Pts',(26.7915895883623,-61.2972176688764,
-232.2311442104));
#226849=CARTESIAN_POINT('Ctrl Pts',(27.6213469993979,-61.7602848222496,
-231.430540367037));
#226850=CARTESIAN_POINT('Ctrl Pts',(28.4556335624375,-62.2192160084591,
-230.63258019833));
#226851=CARTESIAN_POINT('Ctrl Pts',(29.289920125477,-62.6781471946685,-229.834620029623));
#226852=CARTESIAN_POINT('Ctrl Pts',(30.1289511322075,-63.1328363273331,
-229.039478997096));
#226853=CARTESIAN_POINT('Ctrl Pts',(30.9705439434446,-63.5850360083551,
-228.245754373682));
#226854=CARTESIAN_POINT('Ctrl Pts',(32.6537295659188,-64.4894353703992,
-226.658305126855));
#226855=CARTESIAN_POINT('Ctrl Pts',(34.3469173915073,-65.3841225672083,
-225.076391213479));
#226856=CARTESIAN_POINT('Ctrl Pts',(36.0437616605612,-66.2748188763012,
-223.496282027351));
#226857=CARTESIAN_POINT('Ctrl Pts',(39.4374501986691,-68.0562114944868,
-220.336063655097));
#226858=CARTESIAN_POINT('Ctrl Pts',(42.8459482063409,-69.8217123813687,
-217.183304075329));
#226859=CARTESIAN_POINT('Ctrl Pts',(46.2577049582974,-71.5830236206181,
-214.031928620936));
#226860=CARTESIAN_POINT('Ctrl Pts',(26.0271556717183,-60.8195050993445,
-233.023057709875));
#226861=CARTESIAN_POINT('Ctrl Pts',(26.8614803279425,-61.2789736199002,
-232.220907138713));
#226862=CARTESIAN_POINT('Ctrl Pts',(27.7006372905616,-61.7344790137215,
-231.421952061255));
#226863=CARTESIAN_POINT('Ctrl Pts',(28.5430811002764,-62.1870353929875,
-230.62500928173));
#226864=CARTESIAN_POINT('Ctrl Pts',(29.3855249099912,-62.6395917722535,
-229.828066502204));
#226865=CARTESIAN_POINT('Ctrl Pts',(30.2312298015655,-63.0892242106365,
-229.033124256632));
#226866=CARTESIAN_POINT('Ctrl Pts',(31.0790619662469,-63.5367969787612,
-228.239400097671));
#226867=CARTESIAN_POINT('Ctrl Pts',(32.7747262956096,-64.4319425150107,
-226.651951779748));
#226868=CARTESIAN_POINT('Ctrl Pts',(34.4786705837165,-65.3190393016261,
-225.069228384841));
#226869=CARTESIAN_POINT('Ctrl Pts',(36.1863583725991,-66.202056470716,-223.488410098027));
#226870=CARTESIAN_POINT('Ctrl Pts',(39.6017339503642,-67.9680908088958,
-220.326773524398));
#226871=CARTESIAN_POINT('Ctrl Pts',(43.0317527614028,-69.7182854025588,
-217.172664187274));
#226872=CARTESIAN_POINT('Ctrl Pts',(46.4657689946141,-71.4633532268859,
-214.020279084284));
#226873=CARTESIAN_POINT('Ctrl Pts',(26.1079086334631,-60.7917651170397,
-233.017180488577));
#226874=CARTESIAN_POINT('Ctrl Pts',(26.9477933569846,-61.2457491809832,
-232.216198008803));
#226875=CARTESIAN_POINT('Ctrl Pts',(27.791602857653,-61.6966607926582,-231.417878001952));
#226876=CARTESIAN_POINT('Ctrl Pts',(28.6380092466183,-62.1453058875298,
-230.62119554679));
#226877=CARTESIAN_POINT('Ctrl Pts',(29.4844156355837,-62.5939509824013,
-229.824513091628));
#226878=CARTESIAN_POINT('Ctrl Pts',(30.3334386001484,-63.0403250798734,
-229.029487457053));
#226879=CARTESIAN_POINT('Ctrl Pts',(31.1842647171309,-63.485002448237,-228.23553480923));
#226880=CARTESIAN_POINT('Ctrl Pts',(32.8859169510958,-64.3743571849642,
-226.647629513582));
#226881=CARTESIAN_POINT('Ctrl Pts',(34.5946426558381,-65.2570271773188,
-225.063918430622));
#226882=CARTESIAN_POINT('Ctrl Pts',(36.3070242103916,-66.1357954693092,
-223.482151043919));
#226883=CARTESIAN_POINT('Ctrl Pts',(39.7317873194987,-67.8933320532899,
-220.318616270514));
#226884=CARTESIAN_POINT('Ctrl Pts',(43.1708142706306,-69.6356764040323,
-217.162686067389));
#226885=CARTESIAN_POINT('Ctrl Pts',(46.6146568592818,-71.3718952390485,
-214.008891200286));
#226886=CARTESIAN_POINT('Ctrl Pts',(26.1949495995768,-60.7559954632254,
-233.015310708939));
#226887=CARTESIAN_POINT('Ctrl Pts',(27.0387644538443,-61.2057327308231,
-232.215070168042));
#226888=CARTESIAN_POINT('Ctrl Pts',(27.8858336675415,-61.6529664487026,
-231.417079914153));
#226889=CARTESIAN_POINT('Ctrl Pts',(28.7351647823697,-62.0982646553384,
-230.620551354198));
#226890=CARTESIAN_POINT('Ctrl Pts',(29.5844958971979,-62.5435628619743,
-229.824022794242));
#226891=CARTESIAN_POINT('Ctrl Pts',(30.4361008904608,-62.9869237960558,
-229.028968199982));
#226892=CARTESIAN_POINT('Ctrl Pts',(31.2893382107612,-63.4287766497893,
-228.234911333144));
#226893=CARTESIAN_POINT('Ctrl Pts',(32.9958128513619,-64.3124823572563,
-226.646797599469));
#226894=CARTESIAN_POINT('Ctrl Pts',(34.7087066827471,-65.190229522585,-225.062593091688));
#226895=CARTESIAN_POINT('Ctrl Pts',(36.425148099657,-66.0642498543572,-223.480334162157));
#226896=CARTESIAN_POINT('Ctrl Pts',(39.8580309334768,-67.8122905179015,
-220.315816303095));
#226897=CARTESIAN_POINT('Ctrl Pts',(43.304744476869,-69.545794357118,-217.158884043615));
#226898=CARTESIAN_POINT('Ctrl Pts',(46.7566079538913,-71.2728084364657,
-214.004305067604));
#226899=CARTESIAN_POINT('Ctrl Pts',(26.2384700826335,-60.7381106363183,
-233.014375819121));
#226900=CARTESIAN_POINT('Ctrl Pts',(27.0842500022742,-61.1857245057431,
-232.21450624766));
#226901=CARTESIAN_POINT('Ctrl Pts',(27.9329490724857,-61.6311192767247,
-231.416680870253));
#226902=CARTESIAN_POINT('Ctrl Pts',(28.7837425502454,-62.0747440392428,
-230.620229257902));
#226903=CARTESIAN_POINT('Ctrl Pts',(29.634536028005,-62.5183688017608,-229.82377764555));
#226904=CARTESIAN_POINT('Ctrl Pts',(30.487432035617,-62.960223154147,-229.028708571446));
#226905=CARTESIAN_POINT('Ctrl Pts',(31.3418749575762,-63.4006637505655,
-228.234599595102));
#226906=CARTESIAN_POINT('Ctrl Pts',(33.0507608014949,-64.2815449434024,
-226.646381642412));
#226907=CARTESIAN_POINT('Ctrl Pts',(34.7657386962016,-65.1568306952181,
-225.061930422221));
#226908=CARTESIAN_POINT('Ctrl Pts',(36.4842100442897,-66.0284770468812,
-223.479425721276));
#226909=CARTESIAN_POINT('Ctrl Pts',(39.9211527404658,-67.7717697502073,
-220.314416319386));
#226910=CARTESIAN_POINT('Ctrl Pts',(43.3717095799881,-69.5008533336608,
-217.156983031728));
#226911=CARTESIAN_POINT('Ctrl Pts',(46.827583501196,-71.2232650351743,-214.002012001263));
#226912=CARTESIAN_POINT('Ctrl Pts',(26.2629114467516,-60.7391039700744,
-233.002893197821));
#226913=CARTESIAN_POINT('Ctrl Pts',(27.114397963117,-61.1810939660079,-232.20584360482));
#226914=CARTESIAN_POINT('Ctrl Pts',(27.9674707129322,-61.6219011639104,
-231.409926775993));
#226915=CARTESIAN_POINT('Ctrl Pts',(28.8218440521233,-62.0616481295084,
-230.614892210633));
#226916=CARTESIAN_POINT('Ctrl Pts',(29.6762173913143,-62.5013950951064,
-229.819857645272));
#226917=CARTESIAN_POINT('Ctrl Pts',(30.5318920874236,-62.9400822869671,
-229.025706439153));
#226918=CARTESIAN_POINT('Ctrl Pts',(31.3886377598337,-63.3778284552318,
-228.232247232636));
#226919=CARTESIAN_POINT('Ctrl Pts',(33.102129104654,-64.2533207917612,-226.645328819602));
#226920=CARTESIAN_POINT('Ctrl Pts',(34.8198706879942,-65.1250606034272,
-225.061147334889));
#226921=CARTESIAN_POINT('Ctrl Pts',(36.5405225399701,-65.9938853198046,
-223.478668525429));
#226922=CARTESIAN_POINT('Ctrl Pts',(39.981826243922,-67.7315347525594,-220.313710906511));
#226923=CARTESIAN_POINT('Ctrl Pts',(43.4345244003096,-69.457683375828,-217.155376526334));
#226924=CARTESIAN_POINT('Ctrl Pts',(46.8928095579913,-71.1769737453648,
-213.999726959588));
#226925=CARTESIAN_POINT('Ctrl Pts',(26.2982843226441,-60.7344827742712,
-232.991392546795));
#226926=CARTESIAN_POINT('Ctrl Pts',(27.1539710903761,-61.1717772412952,
-232.196575481186));
#226927=CARTESIAN_POINT('Ctrl Pts',(28.0105205110111,-61.6084763232924,
-231.402405653547));
#226928=CARTESIAN_POINT('Ctrl Pts',(28.8678178196021,-62.0446142255719,
-230.608774353877));
#226929=CARTESIAN_POINT('Ctrl Pts',(29.725115128193,-62.4807521278514,-229.815143054206));
#226930=CARTESIAN_POINT('Ctrl Pts',(30.5831604852668,-62.9163290490967,
-229.022050566726));
#226931=CARTESIAN_POINT('Ctrl Pts',(31.441855894783,-63.3513820288522,-228.22940826535));
#226932=CARTESIAN_POINT('Ctrl Pts',(33.1592467138153,-64.2214879883631,
-226.644123662598));
#226933=CARTESIAN_POINT('Ctrl Pts',(34.879225924468,-65.0894996057218,-225.060627483752));
#226934=CARTESIAN_POINT('Ctrl Pts',(36.6011749254936,-65.955713208232,-223.478393801851));
#226935=CARTESIAN_POINT('Ctrl Pts',(40.045072927545,-67.6881404132524,-220.313926438049));
#226936=CARTESIAN_POINT('Ctrl Pts',(43.4967433028155,-69.4134193510673,
-217.154414312055));
#226937=CARTESIAN_POINT('Ctrl Pts',(46.9530675926807,-71.1335421841428,
-213.997473502442));
#226938=CARTESIAN_POINT('Ctrl Pts',(26.3336571985367,-60.7298615784681,
-232.97989189577));
#226939=CARTESIAN_POINT('Ctrl Pts',(27.1935442176352,-61.1624605165825,
-232.187307357553));
#226940=CARTESIAN_POINT('Ctrl Pts',(28.0535703090899,-61.5950514826745,
-231.3948845311));
#226941=CARTESIAN_POINT('Ctrl Pts',(28.9137915870808,-62.0275803216354,
-230.60265649712));
#226942=CARTESIAN_POINT('Ctrl Pts',(29.7740128650717,-62.4601091605963,
-229.810428463141));
#226943=CARTESIAN_POINT('Ctrl Pts',(30.6344288831099,-62.8925758112263,
-229.018394694299));
#226944=CARTESIAN_POINT('Ctrl Pts',(31.4950740297321,-63.3249356024725,
-228.226569298064));
#226945=CARTESIAN_POINT('Ctrl Pts',(33.2163643229766,-64.189655184965,-226.642918505594));
#226946=CARTESIAN_POINT('Ctrl Pts',(34.9385811609418,-65.0539386080163,
-225.060107632614));
#226947=CARTESIAN_POINT('Ctrl Pts',(36.6618273110172,-65.9175410966594,
-223.478119078272));
#226948=CARTESIAN_POINT('Ctrl Pts',(40.108319611168,-67.6447460739454,-220.314141969587));
#226949=CARTESIAN_POINT('Ctrl Pts',(43.5589622053215,-69.3691553263065,
-217.153452097777));
#226950=CARTESIAN_POINT('Ctrl Pts',(47.01332562737,-71.0901106229208,-213.995220045295));
#226951=CARTESIAN_POINT('Ctrl Pts',(26.3821787340349,-60.7171127522114,
-232.969564324364));
#226952=CARTESIAN_POINT('Ctrl Pts',(27.2445605117317,-61.1462290233331,
-232.178536730278));
#226953=CARTESIAN_POINT('Ctrl Pts',(28.1068458309989,-61.5755390840377,
-231.387516472179));
#226954=CARTESIAN_POINT('Ctrl Pts',(28.9690444318655,-62.0050437616364,
-230.596514709636));
#226955=CARTESIAN_POINT('Ctrl Pts',(29.8312430327322,-62.4345484392352,
-229.805512947091));
#226956=CARTESIAN_POINT('Ctrl Pts',(30.6933548791156,-62.8642478097168,
-229.014529680654));
#226957=CARTESIAN_POINT('Ctrl Pts',(31.5553928365677,-63.294139004949,-228.223577554036));
#226958=CARTESIAN_POINT('Ctrl Pts',(33.279468751472,-64.1539213954133,-226.641673300801));
#226959=CARTESIAN_POINT('Ctrl Pts',(35.0032446885496,-65.0144779934189,
-225.059892398919));
#226960=CARTESIAN_POINT('Ctrl Pts',(36.7268700953622,-65.8757200976626,
-223.47835238333));
#226961=CARTESIAN_POINT('Ctrl Pts',(40.1741209089872,-67.59820430615,-220.315272352152));
#226962=CARTESIAN_POINT('Ctrl Pts',(43.6206707171006,-69.3236781200416,
-217.153178316448));
#226963=CARTESIAN_POINT('Ctrl Pts',(47.0687185474759,-71.0494058698413,
-213.993041121244));
#226964=CARTESIAN_POINT('Ctrl Pts',(26.4599578544128,-60.6835996873818,
-232.962469394759));
#226965=CARTESIAN_POINT('Ctrl Pts',(27.3226882880111,-61.1109358874724,
-232.172413742166));
#226966=CARTESIAN_POINT('Ctrl Pts',(28.1852243300615,-61.5385403473352,
-231.38229745923));
#226967=CARTESIAN_POINT('Ctrl Pts',(29.0475520792886,-61.9664437404056,
-230.59212149004));
#226968=CARTESIAN_POINT('Ctrl Pts',(29.9098798285159,-62.3943471334761,
-229.801945520851));
#226969=CARTESIAN_POINT('Ctrl Pts',(30.7719992834121,-62.8225494254431,
-229.011709845514));
#226970=CARTESIAN_POINT('Ctrl Pts',(31.6338956495273,-63.2510852212965,
-228.221416509758));
#226971=CARTESIAN_POINT('Ctrl Pts',(33.3576883817577,-64.1081568130033,
-226.640829838246));
#226972=CARTESIAN_POINT('Ctrl Pts',(35.0805895076854,-64.966557214572,-225.060010587067));
#226973=CARTESIAN_POINT('Ctrl Pts',(36.8024707859496,-65.826619215018,-223.47899392047));
#226974=CARTESIAN_POINT('Ctrl Pts',(40.2462333424779,-67.54674321591,-220.316960587274));
#226975=CARTESIAN_POINT('Ctrl Pts',(43.6859139831841,-69.2733920499482,
-217.154070226751));
#226976=CARTESIAN_POINT('Ctrl Pts',(47.1204141132129,-71.0104275193633,
-213.991161055977));
#226977=CARTESIAN_POINT('',(26.5827141673278,-60.7444095340058,-232.85005));
#226978=CARTESIAN_POINT('',(25.3523897646956,-61.114818041723,-232.850050017304));
#226979=CARTESIAN_POINT('Ctrl Pts',(26.5827141673278,-60.7444095340058,
-232.85005));
#226980=CARTESIAN_POINT('Ctrl Pts',(26.5498602974857,-60.7619654664071,
-232.85005));
#226981=CARTESIAN_POINT('Ctrl Pts',(26.5113303465769,-60.7822271546458,
-232.85005));
#226982=CARTESIAN_POINT('Ctrl Pts',(26.4606301262639,-60.8074293646313,
-232.85005));
#226983=CARTESIAN_POINT('Ctrl Pts',(26.4425447461125,-60.8161729408406,
-232.850050000068));
#226984=CARTESIAN_POINT('Ctrl Pts',(26.387379862291,-60.8413638763713,-232.850050000068));
#226985=CARTESIAN_POINT('Ctrl Pts',(26.3144842454907,-60.8727542686262,
-232.85005));
#226986=CARTESIAN_POINT('Ctrl Pts',(26.1773907479988,-60.9311707559402,
-232.85005));
#226987=CARTESIAN_POINT('Ctrl Pts',(26.1245297076587,-60.9517310532191,
-232.850050000385));
#226988=CARTESIAN_POINT('Ctrl Pts',(26.0341733047922,-60.9830151315338,
-232.850050000385));
#226989=CARTESIAN_POINT('Ctrl Pts',(26.0105117414057,-60.991031970563,-232.850050000013));
#226990=CARTESIAN_POINT('Ctrl Pts',(25.9127285916415,-61.0232844425691,
-232.850050000013));
#226991=CARTESIAN_POINT('Ctrl Pts',(25.8684101044803,-61.0357482370295,
-232.85005));
#226992=CARTESIAN_POINT('Ctrl Pts',(25.7993139457216,-61.0535328833358,
-232.85005));
#226993=CARTESIAN_POINT('Ctrl Pts',(25.7541116741092,-61.0637255831382,
-232.850049999959));
#226994=CARTESIAN_POINT('Ctrl Pts',(25.6627893930028,-61.0828302915598,
-232.850049999959));
#226995=CARTESIAN_POINT('Ctrl Pts',(25.615699312088,-61.0907535096604,-232.850050000018));
#226996=CARTESIAN_POINT('Ctrl Pts',(25.526867967465,-61.1018068046011,-232.850050000018));
#226997=CARTESIAN_POINT('Ctrl Pts',(25.4884409885479,-61.1060188193343,
-232.85005));
#226998=CARTESIAN_POINT('Ctrl Pts',(25.4120097345976,-61.1125648908878,
-232.85005));
#226999=CARTESIAN_POINT('Ctrl Pts',(25.3780718523939,-61.1138880467002,
-232.85005));
#227000=CARTESIAN_POINT('Ctrl Pts',(25.3523897698351,-61.1148181836303,
-232.85005));
#227001=CARTESIAN_POINT('',(41.3748964727292,-72.6655519634609,-214.574036901741));
#227002=CARTESIAN_POINT('Ctrl Pts',(25.3523897720293,-61.114817956777,-232.850049970045));
#227003=CARTESIAN_POINT('Ctrl Pts',(30.6926995480076,-64.965287483333,-226.757725855014));
#227004=CARTESIAN_POINT('Ctrl Pts',(36.0337490039693,-68.8154400690564,
-220.665850944208));
#227005=CARTESIAN_POINT('Ctrl Pts',(41.3748962564069,-72.665551761209,-214.574036584249));
#227006=CARTESIAN_POINT('',(41.8937014876592,-72.6456596144325,-214.55018589167));
#227007=CARTESIAN_POINT('Ctrl Pts',(41.8937014876741,-72.6456596144277,
-214.55018589184));
#227008=CARTESIAN_POINT('Ctrl Pts',(41.8056994101465,-72.6489893684936,
-214.558007661286));
#227009=CARTESIAN_POINT('Ctrl Pts',(41.718477292423,-72.6523092351335,-214.564017375719));
#227010=CARTESIAN_POINT('Ctrl Pts',(41.5868861587709,-72.6573541922645,
-214.570073878361));
#227011=CARTESIAN_POINT('Ctrl Pts',(41.5433370473638,-72.659029772319,-214.571581799465));
#227012=CARTESIAN_POINT('Ctrl Pts',(41.4786634332878,-72.6615274743735,
-214.573057636199));
#227013=CARTESIAN_POINT('Ctrl Pts',(41.457775058709,-72.6623356153501,-214.573417187359));
#227014=CARTESIAN_POINT('Ctrl Pts',(41.4163541860228,-72.6639409738462,
-214.573897183768));
#227015=CARTESIAN_POINT('Ctrl Pts',(41.4039880684433,-72.6644207369686,
-214.574006351066));
#227016=CARTESIAN_POINT('Ctrl Pts',(41.3748964708024,-72.6655518905448,
-214.574037743505));
#227017=CARTESIAN_POINT('',(46.8664918907845,-70.8820281261857,-214.224994454969));
#227018=CARTESIAN_POINT('Ctrl Pts',(46.8664918907845,-70.8820281261857,
-214.224994454969));
#227019=CARTESIAN_POINT('Ctrl Pts',(46.7744407826316,-70.9511131613396,
-214.228242207602));
#227020=CARTESIAN_POINT('Ctrl Pts',(46.6807272794255,-71.0186224422586,
-214.231828155423));
#227021=CARTESIAN_POINT('Ctrl Pts',(46.5495229903282,-71.1092838966295,
-214.237663532242));
#227022=CARTESIAN_POINT('Ctrl Pts',(46.5126373770964,-71.1343646693495,
-214.239393263803));
#227023=CARTESIAN_POINT('Ctrl Pts',(46.3057923038342,-71.2726997130295,
-214.249757794807));
#227024=CARTESIAN_POINT('Ctrl Pts',(46.1254151596486,-71.3847351188338,
-214.258939730929));
#227025=CARTESIAN_POINT('Ctrl Pts',(45.7687595219198,-71.5880113823786,
-214.276898214196));
#227026=CARTESIAN_POINT('Ctrl Pts',(45.5977961988715,-71.6781131952535,
-214.286477772542));
#227027=CARTESIAN_POINT('Ctrl Pts',(45.3185014974946,-71.8138089269496,
-214.303180438964));
#227028=CARTESIAN_POINT('Ctrl Pts',(45.2120152038829,-71.8629654498041,
-214.309490070268));
#227029=CARTESIAN_POINT('Ctrl Pts',(45.046199456443,-71.9355486918505,-214.319240105013));
#227030=CARTESIAN_POINT('Ctrl Pts',(44.9874097484588,-71.9605279865678,
-214.322717043278));
#227031=CARTESIAN_POINT('Ctrl Pts',(44.7920434632078,-72.0410490486407,
-214.334469550239));
#227032=CARTESIAN_POINT('Ctrl Pts',(44.654581930388,-72.0937224739647,-214.343103618599));
#227033=CARTESIAN_POINT('Ctrl Pts',(44.0770061030001,-72.2986437300476,
-214.380774049815));
#227034=CARTESIAN_POINT('Ctrl Pts',(43.6246516203705,-72.4199541120767,
-214.411162580918));
#227035=CARTESIAN_POINT('Ctrl Pts',(43.0535644970527,-72.5255358981687,
-214.454758498744));
#227036=CARTESIAN_POINT('Ctrl Pts',(42.9403769886009,-72.5441841201559,
-214.463730404259));
#227037=CARTESIAN_POINT('Ctrl Pts',(42.745348495263,-72.5724398999531,-214.479262989101));
#227038=CARTESIAN_POINT('Ctrl Pts',(42.6635003407055,-72.5831344326108,
-214.485726488452));
#227039=CARTESIAN_POINT('Ctrl Pts',(42.3528138940059,-72.6193128180452,
-214.510537926902));
#227040=CARTESIAN_POINT('Ctrl Pts',(42.1239061674215,-72.6369493090089,
-214.529724921202));
#227041=CARTESIAN_POINT('Ctrl Pts',(41.8937014876739,-72.6456596144296,
-214.550185891837));
#227042=CARTESIAN_POINT('Ctrl Pts',(26.5827166017585,-60.7444082341964,
-232.850049999054));
#227043=CARTESIAN_POINT('Ctrl Pts',(27.4045078646348,-61.1514990596195,
-232.097463289075));
#227044=CARTESIAN_POINT('Ctrl Pts',(28.2261236616022,-61.5588353729273,
-231.344820212495));
#227045=CARTESIAN_POINT('Ctrl Pts',(29.0475520765728,-61.9664437417409,
-230.592121490192));
#227046=CARTESIAN_POINT('Ctrl Pts',(29.9098779960546,-62.3943462284576,
-229.801947196275));
#227047=CARTESIAN_POINT('Ctrl Pts',(30.7719974086774,-62.8225485010969,
-229.011711557785));
#227048=CARTESIAN_POINT('Ctrl Pts',(31.6338956347565,-63.2510852293973,
-228.221416510165));
#227049=CARTESIAN_POINT('Ctrl Pts',(33.3576804074389,-64.1081528789503,
-226.640837124115));
#227050=CARTESIAN_POINT('Ctrl Pts',(35.0805811947291,-64.9665531261144,
-225.060018166533));
#227051=CARTESIAN_POINT('Ctrl Pts',(36.8024706731575,-65.8266192882738,
-223.478993919512));
#227052=CARTESIAN_POINT('Ctrl Pts',(40.1613324575101,-67.5043363544868,
-220.394915649693));
#227053=CARTESIAN_POINT('Ctrl Pts',(43.5163436116641,-69.1882768775022,
-217.309992116266));
#227054=CARTESIAN_POINT('Ctrl Pts',(46.8664917825725,-70.8820279699867,
-214.22499462617));
#227055=CARTESIAN_POINT('Ctrl Pts',(28.811481324712,36.2672238003158,-232.961663720964));
#227056=CARTESIAN_POINT('Ctrl Pts',(29.5645263655861,36.6399226415611,-232.177270818232));
#227057=CARTESIAN_POINT('Ctrl Pts',(30.3173414199567,37.0126142771829,-231.392803581211));
#227058=CARTESIAN_POINT('Ctrl Pts',(31.069911071871,37.385324556228,-230.608260371606));
#227059=CARTESIAN_POINT('Ctrl Pts',(31.8224807237854,37.7580348352731,-229.823717162));
#227060=CARTESIAN_POINT('Ctrl Pts',(32.5748049718356,38.1307637318441,-229.039097966911));
#227061=CARTESIAN_POINT('Ctrl Pts',(33.326867581659,38.5035402264522,-228.254401763819));
#227062=CARTESIAN_POINT('Ctrl Pts',(34.8309928013059,39.2490932156681,-226.685009357635));
#227063=CARTESIAN_POINT('Ctrl Pts',(36.3340721635766,39.9948325139069,-225.115307761803));
#227064=CARTESIAN_POINT('Ctrl Pts',(37.8359666905481,40.7410341111373,-223.545299801334));
#227065=CARTESIAN_POINT('Ctrl Pts',(40.8397557444911,42.233437305598,-220.405283880397));
#227066=CARTESIAN_POINT('Ctrl Pts',(43.8388051696003,43.7275965705222,-217.264000696622));
#227067=CARTESIAN_POINT('Ctrl Pts',(46.8319258491792,45.2266492383781,-214.121813627025));
#227068=CARTESIAN_POINT('Ctrl Pts',(28.7546828535794,36.2946048538794,-232.967923270373));
#227069=CARTESIAN_POINT('Ctrl Pts',(29.5075354964661,36.6682851435785,-232.18296040294));
#227070=CARTESIAN_POINT('Ctrl Pts',(30.260203356218,37.041928546648,-231.397949783602));
#227071=CARTESIAN_POINT('Ctrl Pts',(31.012687072449,37.4155430678739,-230.612897000714));
#227072=CARTESIAN_POINT('Ctrl Pts',(31.7651707886799,37.7891575890997,-229.827844217825));
#227073=CARTESIAN_POINT('Ctrl Pts',(32.5174703341753,38.1627432696007,-229.042749264024));
#227074=CARTESIAN_POINT('Ctrl Pts',(33.2695884278607,38.5363065970483,-228.257619016064));
#227075=CARTESIAN_POINT('Ctrl Pts',(34.7738246152316,39.2834332519434,-226.687358520144));
#227076=CARTESIAN_POINT('Ctrl Pts',(36.2773319082997,40.0304737792722,-225.116955396868));
#227077=CARTESIAN_POINT('Ctrl Pts',(37.7801639596043,40.7774501421753,-223.546481445834));
#227078=CARTESIAN_POINT('Ctrl Pts',(40.7858280622135,42.2714028679817,-220.405533543764));
#227079=CARTESIAN_POINT('Ctrl Pts',(43.788714991937,43.7652295475826,-217.264288793245));
#227080=CARTESIAN_POINT('Ctrl Pts',(46.7899896154941,45.2580776239732,-214.123556902107));
#227081=CARTESIAN_POINT('Ctrl Pts',(28.7154411546286,36.3084021057357,-232.976115945722));
#227082=CARTESIAN_POINT('Ctrl Pts',(29.4668698155753,36.6840531650027,-232.190299004213));
#227083=CARTESIAN_POINT('Ctrl Pts',(30.2182278401491,37.0595754047064,-231.404498974189));
#227084=CARTESIAN_POINT('Ctrl Pts',(30.9695388460574,37.4349506564828,-230.618731646667));
#227085=CARTESIAN_POINT('Ctrl Pts',(31.7208498519656,37.8103259082591,-229.832964319146));
#227086=CARTESIAN_POINT('Ctrl Pts',(32.4721138113312,38.1855541511188,-229.047229657302));
#227087=CARTESIAN_POINT('Ctrl Pts',(33.2233504871597,38.560617867947,-228.261540054661));
#227088=CARTESIAN_POINT('Ctrl Pts',(34.7258238388169,39.3107453016035,-226.690160849379));
#227089=CARTESIAN_POINT('Ctrl Pts',(36.2281910213353,40.0602134993234,-225.11896419415));
#227090=CARTESIAN_POINT('Ctrl Pts',(37.7305702572955,40.808893913642,-223.548016395278));
#227091=CARTESIAN_POINT('Ctrl Pts',(40.7353287292159,42.3062547422792,-220.406120797533));
#227092=CARTESIAN_POINT('Ctrl Pts',(43.7401655452353,43.8004441673505,-217.265239990539));
#227093=CARTESIAN_POINT('Ctrl Pts',(46.7455490797692,45.2906625887397,-214.1255539434));
#227094=CARTESIAN_POINT('Ctrl Pts',(28.6836693563314,36.3172916302978,-232.984586371767));
#227095=CARTESIAN_POINT('Ctrl Pts',(29.4328038186657,36.6955273714839,-232.197666951892));
#227096=CARTESIAN_POINT('Ctrl Pts',(30.1821597301324,37.0733995616469,-231.410933917807));
#227097=CARTESIAN_POINT('Ctrl Pts',(30.9317206554361,37.4509071831741,-230.624372601034));
#227098=CARTESIAN_POINT('Ctrl Pts',(31.6812815807397,37.8284148047014,-229.83781128426));
#227099=CARTESIAN_POINT('Ctrl Pts',(32.4310475185464,38.2055578694789,-229.051421689267));
#227100=CARTESIAN_POINT('Ctrl Pts',(33.1810027512314,38.5823363130566,-228.265190292231));
#227101=CARTESIAN_POINT('Ctrl Pts',(34.6809132166015,39.3358932002121,-226.69272749816));
#227102=CARTESIAN_POINT('Ctrl Pts',(36.1815801312299,40.0879909915779,-225.120896504533));
#227103=CARTESIAN_POINT('Ctrl Pts',(37.6828865095192,40.8386380933409,-223.549601777981));
#227104=CARTESIAN_POINT('Ctrl Pts',(40.6854992660978,42.3399322968669,-220.407012324875));
#227105=CARTESIAN_POINT('Ctrl Pts',(43.6906591856765,43.835419294533,-217.266555597716));
#227106=CARTESIAN_POINT('Ctrl Pts',(46.6975653758367,45.3252553963054,-214.127639057046));
#227107=CARTESIAN_POINT('Ctrl Pts',(28.6518975580342,36.3261811548597,-232.993056797812));
#227108=CARTESIAN_POINT('Ctrl Pts',(29.398737821756,36.7070015779651,-232.205034899571));
#227109=CARTESIAN_POINT('Ctrl Pts',(30.1460916201158,37.0872237185874,-231.417368861425));
#227110=CARTESIAN_POINT('Ctrl Pts',(30.8939024648147,37.4668637098655,-230.6300135554));
#227111=CARTESIAN_POINT('Ctrl Pts',(31.6417133095137,37.8465037011437,-229.842658249374));
#227112=CARTESIAN_POINT('Ctrl Pts',(32.3899812257617,38.225561587839,-229.055613721231));
#227113=CARTESIAN_POINT('Ctrl Pts',(33.1386550153031,38.6040547581662,-228.268840529801));
#227114=CARTESIAN_POINT('Ctrl Pts',(34.6360025943859,39.3610410988206,-226.69529414694));
#227115=CARTESIAN_POINT('Ctrl Pts',(36.1349692411245,40.1157684838324,-225.122828814917));
#227116=CARTESIAN_POINT('Ctrl Pts',(37.6352027617429,40.8683822730397,-223.551187160683));
#227117=CARTESIAN_POINT('Ctrl Pts',(40.6356698029797,42.3736098514546,-220.407903852216));
#227118=CARTESIAN_POINT('Ctrl Pts',(43.6411528261178,43.8703944217154,-217.267871204892));
#227119=CARTESIAN_POINT('Ctrl Pts',(46.6495816719042,45.3598482038711,-214.129724170691));
#227120=CARTESIAN_POINT('Ctrl Pts',(28.6268841990247,36.3309725707821,-233.001464510274));
#227121=CARTESIAN_POINT('Ctrl Pts',(29.3705829350163,36.7149391799052,-232.212094488675));
#227122=CARTESIAN_POINT('Ctrl Pts',(30.1153093882969,37.097903168935,-231.423383830337));
#227123=CARTESIAN_POINT('Ctrl Pts',(30.8608649961116,37.4799665704452,-230.635190635126));
#227124=CARTESIAN_POINT('Ctrl Pts',(31.6064206039263,37.8620299719552,-229.846997439915));
#227125=CARTESIAN_POINT('Ctrl Pts',(32.3528061165871,38.2431927923484,-229.059322438005));
#227126=CARTESIAN_POINT('Ctrl Pts',(33.0998655521803,38.6235441089799,-228.272058763276));
#227127=CARTESIAN_POINT('Ctrl Pts',(34.5939844233666,39.3842467422428,-226.697531413816));
#227128=CARTESIAN_POINT('Ctrl Pts',(36.0907758686695,40.1417143786457,-225.124632267967));
#227129=CARTESIAN_POINT('Ctrl Pts',(37.5893556701601,40.8965147834728,-223.552789136373));
#227130=CARTESIAN_POINT('Ctrl Pts',(40.5865152731412,42.4061155931272,-220.409102873187));
#227131=CARTESIAN_POINT('Ctrl Pts',(43.5906769196312,43.9051501453593,-217.269543315155));
#227132=CARTESIAN_POINT('Ctrl Pts',(46.598054657578,45.3964490821564,-214.13189626583));
#227133=CARTESIAN_POINT('Ctrl Pts',(28.5917373044541,36.3459190971896,-233.004412799005));
#227134=CARTESIAN_POINT('Ctrl Pts',(29.3336456870839,36.7317236596899,-232.214541575288));
#227135=CARTESIAN_POINT('Ctrl Pts',(30.0768533355596,37.1163079376712,-231.425484075423));
#227136=CARTESIAN_POINT('Ctrl Pts',(30.8210649438641,37.4998384795814,-230.63703601277));
#227137=CARTESIAN_POINT('Ctrl Pts',(31.5652765521686,37.8833690214916,-229.848587950118));
#227138=CARTESIAN_POINT('Ctrl Pts',(32.3104940183536,38.2658454573702,-229.060750983011));
#227139=CARTESIAN_POINT('Ctrl Pts',(33.056499757863,38.6474031071304,-228.273381017246));
#227140=CARTESIAN_POINT('Ctrl Pts',(34.5485112368819,39.4105184066505,-226.698641085717));
#227141=CARTESIAN_POINT('Ctrl Pts',(36.0436413480666,40.1699780267802,-225.125745165631));
#227142=CARTESIAN_POINT('Ctrl Pts',(37.5407436150405,40.9265749496157,-223.553976309726));
#227143=CARTESIAN_POINT('Ctrl Pts',(40.5349481489884,42.439768795287,-220.410438597917));
#227144=CARTESIAN_POINT('Ctrl Pts',(43.536857304037,43.9416524034681,-217.271298591679));
#227145=CARTESIAN_POINT('Ctrl Pts',(46.5420263558244,45.4357480033572,-214.134039310084));
#227146=CARTESIAN_POINT('Ctrl Pts',(28.5214435153128,36.3758121500046,-233.010309376466));
#227147=CARTESIAN_POINT('Ctrl Pts',(29.2597711912192,36.7652926192596,-232.219435748514));
#227148=CARTESIAN_POINT('Ctrl Pts',(29.9999412300851,37.1531174751436,-231.429684565593));
#227149=CARTESIAN_POINT('Ctrl Pts',(30.741464839369,37.539582297854,-230.640726768058));
#227150=CARTESIAN_POINT('Ctrl Pts',(31.482988448653,37.9260471205643,-229.851768970523));
#227151=CARTESIAN_POINT('Ctrl Pts',(32.2258698218865,38.3111507874138,-229.063608073021));
#227152=CARTESIAN_POINT('Ctrl Pts',(32.9697681692284,38.6951211034311,-228.276025525187));
#227153=CARTESIAN_POINT('Ctrl Pts',(34.4575648639124,39.4630617354659,-226.700860429518));
#227154=CARTESIAN_POINT('Ctrl Pts',(35.9493723068607,40.2265053230493,-225.12797096096));
#227155=CARTESIAN_POINT('Ctrl Pts',(37.4435195048015,40.9866952819017,-223.556350656432));
#227156=CARTESIAN_POINT('Ctrl Pts',(40.4318139006829,42.5070751996064,-220.413110047378));
#227157=CARTESIAN_POINT('Ctrl Pts',(43.4292180728484,44.0146569196856,-217.274809144726));
#227158=CARTESIAN_POINT('Ctrl Pts',(46.4299697523172,45.5143458457586,-214.138325398592));
#227159=CARTESIAN_POINT('Ctrl Pts',(28.4570930103932,36.3999229344231,-233.01764278364));
#227160=CARTESIAN_POINT('Ctrl Pts',(29.1907924187055,36.7937286595564,-232.225654625907));
#227161=CARTESIAN_POINT('Ctrl Pts',(29.9270887829037,37.1852362696201,-231.435207732835));
#227162=CARTESIAN_POINT('Ctrl Pts',(30.6652441216594,37.5749249395508,-230.645813317621));
#227163=CARTESIAN_POINT('Ctrl Pts',(31.403399460415,37.9646136094813,-229.856418902407));
#227164=CARTESIAN_POINT('Ctrl Pts',(32.1434103450723,38.3524880305972,-229.06807638164));
#227165=CARTESIAN_POINT('Ctrl Pts',(32.884729259185,38.7389448417248,-228.280447107729));
#227166=CARTESIAN_POINT('Ctrl Pts',(34.3673670874105,39.5118584639798,-226.705188559907));
#227167=CARTESIAN_POINT('Ctrl Pts',(35.8551295881073,40.2791804937992,-225.132717154794));
#227168=CARTESIAN_POINT('Ctrl Pts',(37.3455152808298,41.0429334678829,-223.561600885392));
#227169=CARTESIAN_POINT('Ctrl Pts',(40.3262866662749,42.5704394160502,-220.419368346588));
#227170=CARTESIAN_POINT('Ctrl Pts',(43.3172378956761,44.0839938761798,-217.282413069526));
#227171=CARTESIAN_POINT('Ctrl Pts',(46.3111674951612,45.590157065165,-214.147042344173));
#227172=CARTESIAN_POINT('Ctrl Pts',(28.404523824249,36.4142111160726,-233.028222391732));
#227173=CARTESIAN_POINT('Ctrl Pts',(29.1296788023777,36.8148442685854,-232.23397055258));
#227174=CARTESIAN_POINT('Ctrl Pts',(29.8595774687733,37.2115210846296,-231.442464211111));
#227175=CARTESIAN_POINT('Ctrl Pts',(30.5921210784794,37.6056911614944,-230.652400010517));
#227176=CARTESIAN_POINT('Ctrl Pts',(31.3246646881855,37.9998612383593,-229.862335809922));
#227177=CARTESIAN_POINT('Ctrl Pts',(32.0599114204536,38.3914951944436,-229.073755169551));
#227178=CARTESIAN_POINT('Ctrl Pts',(32.7968044445028,38.7814033859296,-228.286041512615));
#227179=CARTESIAN_POINT('Ctrl Pts',(34.2705904926014,39.5612197689016,-226.710614198745));
#227180=CARTESIAN_POINT('Ctrl Pts',(35.7508066075144,40.334264217189,-225.138570075993));
#227181=CARTESIAN_POINT('Ctrl Pts',(37.2337704007868,41.1036371719424,-223.567901121106));
#227182=CARTESIAN_POINT('Ctrl Pts',(40.1996979873318,42.6423830814493,-220.426563211331));
#227183=CARTESIAN_POINT('Ctrl Pts',(43.1764747241572,44.166666266985,-217.290698996916));
#227184=CARTESIAN_POINT('Ctrl Pts',(46.1558000266483,45.6842043061087,-214.156194672008));
#227185=CARTESIAN_POINT('Ctrl Pts',(28.3519546381049,36.428499297722,-233.038801999823));
#227186=CARTESIAN_POINT('Ctrl Pts',(29.0685651860499,36.8359598776144,-232.242286479252));
#227187=CARTESIAN_POINT('Ctrl Pts',(29.7920661546429,37.237805899639,-231.449720689388));
#227188=CARTESIAN_POINT('Ctrl Pts',(30.5189980352994,37.6364573834381,-230.658986703413));
#227189=CARTESIAN_POINT('Ctrl Pts',(31.2459299159559,38.0351088672372,-229.868252717438));
#227190=CARTESIAN_POINT('Ctrl Pts',(31.9764124958348,38.4305023582899,-229.079433957463));
#227191=CARTESIAN_POINT('Ctrl Pts',(32.7088796298207,38.8238619301343,-228.291635917502));
#227192=CARTESIAN_POINT('Ctrl Pts',(34.1738138977924,39.6105810738233,-226.716039837583));
#227193=CARTESIAN_POINT('Ctrl Pts',(35.6464836269217,40.3893479405787,-225.144422997191));
#227194=CARTESIAN_POINT('Ctrl Pts',(37.122025520744,41.1643408760019,-223.574201356819));
#227195=CARTESIAN_POINT('Ctrl Pts',(40.0731093083885,42.7143267468484,-220.433758076075));
#227196=CARTESIAN_POINT('Ctrl Pts',(43.0357115526382,44.2493386577901,-217.298984924306));
#227197=CARTESIAN_POINT('Ctrl Pts',(46.0004325581354,45.7782515470524,-214.165346999843));
#227198=CARTESIAN_POINT('Ctrl Pts',(28.3059764599357,36.4381392896391,-233.049914691876));
#227199=CARTESIAN_POINT('Ctrl Pts',(29.0134341565471,36.8517973543695,-232.2517252646));
#227200=CARTESIAN_POINT('Ctrl Pts',(29.7298662406445,37.2584322913983,-231.458644991706));
#227201=CARTESIAN_POINT('Ctrl Pts',(30.4501559342506,37.6615657444315,-230.667588797462));
#227202=CARTESIAN_POINT('Ctrl Pts',(31.1704456278568,38.0646991974648,-229.876532603218));
#227203=CARTESIAN_POINT('Ctrl Pts',(31.8948332263391,38.464199380249,-229.087662159456));
#227204=CARTESIAN_POINT('Ctrl Pts',(32.6213338477217,38.8616012616129,-228.299865510382));
#227205=CARTESIAN_POINT('Ctrl Pts',(34.0743350904866,39.6564050243409,-226.724272212234));
#227206=CARTESIAN_POINT('Ctrl Pts',(35.5355956082815,40.4430010719712,-225.152884082953));
#227207=CARTESIAN_POINT('Ctrl Pts',(36.9996482985433,41.2260174336112,-223.582843540199));
#227208=CARTESIAN_POINT('Ctrl Pts',(39.9277536790671,42.792050156891,-220.442762454692));
#227209=CARTESIAN_POINT('Ctrl Pts',(42.8672926273489,44.3436915722972,-217.308286098109));
#227210=CARTESIAN_POINT('Ctrl Pts',(45.8087507912112,45.889714665516,-214.174855839415));
#227211=CARTESIAN_POINT('Ctrl Pts',(28.2536248719719,36.45164456484,-233.058476234802));
#227212=CARTESIAN_POINT('Ctrl Pts',(28.956246064681,36.8674691193729,-232.261151946464));
#227213=CARTESIAN_POINT('Ctrl Pts',(29.6674872789167,37.2766580792002,-231.468687139439));
#227214=CARTESIAN_POINT('Ctrl Pts',(30.3823793991597,37.6826022896234,-230.678128469586));
#227215=CARTESIAN_POINT('Ctrl Pts',(31.0972715194027,38.0885465000466,-229.887569799732));
#227216=CARTESIAN_POINT('Ctrl Pts',(31.8160539135098,38.4911129154006,-229.099074756418));
#227217=CARTESIAN_POINT('Ctrl Pts',(32.5368266733684,38.8917474183737,-228.311589632248));
#227218=CARTESIAN_POINT('Ctrl Pts',(33.9783721930855,39.6930164243198,-226.736619383908));
#227219=CARTESIAN_POINT('Ctrl Pts',(35.4277003933768,40.4867262619234,-225.16560579597));
#227220=CARTESIAN_POINT('Ctrl Pts',(36.8796336124663,41.2771645198602,-223.595856775541));
#227221=CARTESIAN_POINT('Ctrl Pts',(39.7835000506455,42.8580410357338,-220.456358734683));
#227222=CARTESIAN_POINT('Ctrl Pts',(42.6980566108585,44.4257389283559,-217.322125580858));
#227223=CARTESIAN_POINT('Ctrl Pts',(45.6143789670139,45.9882588716253,-214.18887606046));
#227224=CARTESIAN_POINT('Ctrl Pts',(28.2012732840083,36.4651498400409,-233.067037777728));
#227225=CARTESIAN_POINT('Ctrl Pts',(28.8990579728149,36.8831408843765,-232.270578628329));
#227226=CARTESIAN_POINT('Ctrl Pts',(29.6051083171889,37.2948838670021,-231.478729287174));
#227227=CARTESIAN_POINT('Ctrl Pts',(30.3146028640688,37.7036388348153,-230.688668141709));
#227228=CARTESIAN_POINT('Ctrl Pts',(31.0240974109487,38.1123938026283,-229.898606996244));
#227229=CARTESIAN_POINT('Ctrl Pts',(31.7372746006804,38.5180264505524,-229.110487353379));
#227230=CARTESIAN_POINT('Ctrl Pts',(32.4523194990151,38.9218935751344,-228.323313754114));
#227231=CARTESIAN_POINT('Ctrl Pts',(33.8824092956843,39.7296278242987,-226.748966555583));
#227232=CARTESIAN_POINT('Ctrl Pts',(35.3198051784721,40.5304514518755,-225.178327508987));
#227233=CARTESIAN_POINT('Ctrl Pts',(36.7596189263893,41.3283116061093,-223.608870010882));
#227234=CARTESIAN_POINT('Ctrl Pts',(39.6392464222237,42.9240319145765,-220.469955014674));
#227235=CARTESIAN_POINT('Ctrl Pts',(42.5288205943682,44.5077862844145,-217.335965063606));
#227236=CARTESIAN_POINT('Ctrl Pts',(45.4200071428167,46.0868030777345,-214.202896281505));
#227237=CARTESIAN_POINT('Ctrl Pts',(28.1478839352704,36.477738188472,-233.075828397652));
#227238=CARTESIAN_POINT('Ctrl Pts',(28.8401821644882,36.8980247568529,-232.280146620628));
#227239=CARTESIAN_POINT('Ctrl Pts',(29.5403735836712,37.3124695266811,-231.488827353208));
#227240=CARTESIAN_POINT('Ctrl Pts',(30.2438219273577,37.724159990219,-230.69919181366));
#227241=CARTESIAN_POINT('Ctrl Pts',(30.9472702710442,38.1358504537568,-229.909556274112));
#227242=CARTESIAN_POINT('Ctrl Pts',(31.6542085880957,38.5446552966966,-229.121751411976));
#227243=CARTESIAN_POINT('Ctrl Pts',(32.3629082299762,38.9518393215846,-228.334837279587));
#227244=CARTESIAN_POINT('Ctrl Pts',(33.7803075137374,39.7662073713606,-226.761009014808));
#227245=CARTESIAN_POINT('Ctrl Pts',(35.204598643849,40.5742293326632,-225.190672920757));
#227246=CARTESIAN_POINT('Ctrl Pts',(36.6311571182707,41.3795423287398,-223.621449299399));
#227247=CARTESIAN_POINT('Ctrl Pts',(39.4842740671139,42.9901683208929,-220.483002056683));
#227248=CARTESIAN_POINT('Ctrl Pts',(42.3467314369201,44.5898405345135,-217.349193442931));
#227249=CARTESIAN_POINT('Ctrl Pts',(45.2106913777692,46.1851488860278,-214.216254607896));
#227250=CARTESIAN_POINT('Ctrl Pts',(28.0986638608654,36.4864396316355,-233.086219707902));
#227251=CARTESIAN_POINT('Ctrl Pts',(28.7855090882708,36.908671912885,-232.291339757935));
#227252=CARTESIAN_POINT('Ctrl Pts',(29.4797969634702,37.3255148395588,-231.50054713919));
#227253=CARTESIAN_POINT('Ctrl Pts',(30.1771392417705,37.7398414336408,-230.711331015122));
#227254=CARTESIAN_POINT('Ctrl Pts',(30.8744815200707,38.1541680277229,-229.922114891055));
#227255=CARTESIAN_POINT('Ctrl Pts',(31.5751008302705,38.565853402466,-229.134613456395));
#227256=CARTESIAN_POINT('Ctrl Pts',(32.2773697651967,38.9760615626091,-228.347946926293));
#227257=CARTESIAN_POINT('Ctrl Pts',(33.6819076350491,39.7964778828953,-226.77461386609));
#227258=CARTESIAN_POINT('Ctrl Pts',(35.092901360331,40.6111090059392,-225.204554400508));
#227259=CARTESIAN_POINT('Ctrl Pts',(36.506013012055,41.4232755079927,-223.635540355772));
#227260=CARTESIAN_POINT('Ctrl Pts',(39.3322363155031,43.0476085120996,-220.4975122663));
#227261=CARTESIAN_POINT('Ctrl Pts',(42.1671908002668,44.6619661512638,-217.363841724096));
#227262=CARTESIAN_POINT('Ctrl Pts',(45.0035463653253,46.2723209746968,-214.23099286058));
#227263=CARTESIAN_POINT('Ctrl Pts',(28.0494437864605,36.495141074799,-233.096611018152));
#227264=CARTESIAN_POINT('Ctrl Pts',(28.7308360120535,36.9193190689171,-232.302532895241));
#227265=CARTESIAN_POINT('Ctrl Pts',(29.4192203432693,37.3385601524366,-231.512266925172));
#227266=CARTESIAN_POINT('Ctrl Pts',(30.1104565561833,37.7555228770627,-230.723470216585));
#227267=CARTESIAN_POINT('Ctrl Pts',(30.8016927690973,38.1724856016888,-229.934673507997));
#227268=CARTESIAN_POINT('Ctrl Pts',(31.4959930724453,38.5870515082353,-229.147475500813));
#227269=CARTESIAN_POINT('Ctrl Pts',(32.1918313004172,39.0002838036336,-228.361056572999));
#227270=CARTESIAN_POINT('Ctrl Pts',(33.5835077563608,39.82674839443,-226.788218717371));
#227271=CARTESIAN_POINT('Ctrl Pts',(34.981204076813,40.6479886792153,-225.218435880259));
#227272=CARTESIAN_POINT('Ctrl Pts',(36.3808689058395,41.4670086872456,-223.649631412145));
#227273=CARTESIAN_POINT('Ctrl Pts',(39.1801985638925,43.1050487033063,-220.512022475916));
#227274=CARTESIAN_POINT('Ctrl Pts',(41.9876501636135,44.7340917680141,-217.378490005261));
#227275=CARTESIAN_POINT('Ctrl Pts',(44.7964013528814,46.3594930633657,-214.245731113265));
#227276=CARTESIAN_POINT('Ctrl Pts',(28.0080391125216,36.4973005693799,-233.110468735653));
#227277=CARTESIAN_POINT('Ctrl Pts',(28.6837630172434,36.9232178045066,-232.317064221622));
#227278=CARTESIAN_POINT('Ctrl Pts',(29.3659479014001,37.344725328937,-231.527181895889));
#227279=CARTESIAN_POINT('Ctrl Pts',(30.0508000045693,37.7641807455897,-230.73868064955));
#227280=CARTESIAN_POINT('Ctrl Pts',(30.7356521077386,38.1836361622425,-229.950179403211));
#227281=CARTESIAN_POINT('Ctrl Pts',(31.423362687773,38.6009356192233,-229.163175043223));
#227282=CARTESIAN_POINT('Ctrl Pts',(32.1125182041085,39.0170287271978,-228.376907373423));
#227283=CARTESIAN_POINT('Ctrl Pts',(33.4908292367796,39.849214943147,-226.804372033824));
#227284=CARTESIAN_POINT('Ctrl Pts',(34.8747945827483,40.6766756124477,-225.234724065505));
#227285=CARTESIAN_POINT('Ctrl Pts',(36.2606283272941,41.5021120342519,-223.666013493501));
#227286=CARTESIAN_POINT('Ctrl Pts',(39.0322958163857,43.1529848778602,-220.528592349493));
#227287=CARTESIAN_POINT('Ctrl Pts',(41.8116561460013,44.7956635400236,-217.395064921228));
#227288=CARTESIAN_POINT('Ctrl Pts',(44.5922760617361,46.4350000670329,-214.262289445508));
#227289=CARTESIAN_POINT('Ctrl Pts',(27.9635611001738,36.4990952898012,-233.124907406577));
#227290=CARTESIAN_POINT('Ctrl Pts',(28.6335193341731,36.9265762879192,-232.332215621801));
#227291=CARTESIAN_POINT('Ctrl Pts',(29.3093382993415,37.3501779403658,-231.542719800075));
#227292=CARTESIAN_POINT('Ctrl Pts',(29.9876295989316,37.7719445682467,-230.754510440041));
#227293=CARTESIAN_POINT('Ctrl Pts',(30.6659208985218,38.1937111961276,-229.966301080007));
#227294=CARTESIAN_POINT('Ctrl Pts',(31.346850346985,38.6135550182896,-229.179478141202));
#227295=CARTESIAN_POINT('Ctrl Pts',(32.0291309789057,39.032311940978,-228.393348201459));
#227296=CARTESIAN_POINT('Ctrl Pts',(33.3936922427472,39.869825786355,-226.821088321973));
#227297=CARTESIAN_POINT('Ctrl Pts',(34.7635386549114,40.7030825753783,-225.251542754464));
#227298=CARTESIAN_POINT('Ctrl Pts',(36.1351659076718,41.5344930728638,-223.682897927105));
#227299=CARTESIAN_POINT('Ctrl Pts',(38.8784204131928,43.1973140678347,-220.545608272386));
#227300=CARTESIAN_POINT('Ctrl Pts',(41.6289795635766,44.8526757118206,-217.412042386738));
#227301=CARTESIAN_POINT('Ctrl Pts',(44.3807833059246,46.5049749771785,-214.279216302521));
#227302=CARTESIAN_POINT('Ctrl Pts',(27.9190830878262,36.5008900102226,-233.139346077501));
#227303=CARTESIAN_POINT('Ctrl Pts',(28.5832756511028,36.9299347713319,-232.34736702198));
#227304=CARTESIAN_POINT('Ctrl Pts',(29.2527286972829,37.3556305517945,-231.558257704261));
#227305=CARTESIAN_POINT('Ctrl Pts',(29.9244591932939,37.7797083909036,-230.770340230532));
#227306=CARTESIAN_POINT('Ctrl Pts',(30.5961896893049,38.2037862300127,-229.982422756802));
#227307=CARTESIAN_POINT('Ctrl Pts',(31.270338006197,38.626174417356,-229.195781239181));
#227308=CARTESIAN_POINT('Ctrl Pts',(31.945743753703,39.0475951547582,-228.409789029494));
#227309=CARTESIAN_POINT('Ctrl Pts',(33.2965552487149,39.8904366295628,-226.837804610121));
#227310=CARTESIAN_POINT('Ctrl Pts',(34.6522827270746,40.7294895383089,-225.268361443424));
#227311=CARTESIAN_POINT('Ctrl Pts',(36.0097034880497,41.5668741114757,-223.699782360708));
#227312=CARTESIAN_POINT('Ctrl Pts',(38.7245450099999,43.2416432578092,-220.56262419528));
#227313=CARTESIAN_POINT('Ctrl Pts',(41.4463029811519,44.9096878836177,-217.429019852247));
#227314=CARTESIAN_POINT('Ctrl Pts',(44.169290550113,46.5749498873242,-214.296143159535));
#227315=CARTESIAN_POINT('Ctrl Pts',(27.864102341306,36.5072827075644,-233.150523220819));
#227316=CARTESIAN_POINT('Ctrl Pts',(28.523209294369,36.9372652461925,-232.359742014691));
#227317=CARTESIAN_POINT('Ctrl Pts',(29.1867208754184,37.3645078673026,-231.571344200798));
#227318=CARTESIAN_POINT('Ctrl Pts',(29.8522042860804,37.7903963835451,-230.783978402477));
#227319=CARTESIAN_POINT('Ctrl Pts',(30.5176876967423,38.2162848997876,-229.996612604157));
#227320=CARTESIAN_POINT('Ctrl Pts',(31.1852516294648,38.6407638308456,-229.210342644892));
#227321=CARTESIAN_POINT('Ctrl Pts',(31.8539198779964,39.0644229189197,-228.424644456938));
#227322=CARTESIAN_POINT('Ctrl Pts',(33.1912563750597,39.9117410950679,-226.853248081031));
#227323=CARTESIAN_POINT('Ctrl Pts',(34.532908053201,40.7558486265409,-225.284087692051));
#227324=CARTESIAN_POINT('Ctrl Pts',(35.8760898321597,41.5985105380543,-223.715714506644));
#227325=CARTESIAN_POINT('Ctrl Pts',(38.5624533900771,43.2838343610812,-220.578968135829));
#227326=CARTESIAN_POINT('Ctrl Pts',(41.2550333439266,44.9633461404957,-217.4454372649));
#227327=CARTESIAN_POINT('Ctrl Pts',(43.9487716799902,46.6404014421116,-214.312594508648));
#227328=CARTESIAN_POINT('Ctrl Pts',(27.8054264163448,36.5146074937637,-233.160277704479));
#227329=CARTESIAN_POINT('Ctrl Pts',(28.4608655062395,36.9445884335815,-232.371247983632));
#227330=CARTESIAN_POINT('Ctrl Pts',(29.1196314139931,37.372514313029,-231.584005383938));
#227331=CARTESIAN_POINT('Ctrl Pts',(29.7799261927146,37.7994041715398,-230.797562749801));
#227332=CARTESIAN_POINT('Ctrl Pts',(30.4402209714361,38.2262940300507,-230.011120115663));
#227333=CARTESIAN_POINT('Ctrl Pts',(31.1021216515676,38.6521081108545,-229.225521863909));
#227334=CARTESIAN_POINT('Ctrl Pts',(31.7648888134181,39.0772864601489,-228.440373573626));
#227335=CARTESIAN_POINT('Ctrl Pts',(33.090423137119,39.9276431587379,-226.87007699306));
#227336=CARTESIAN_POINT('Ctrl Pts',(34.4193423302246,40.7755094860917,-225.301539303434));
#227337=CARTESIAN_POINT('Ctrl Pts',(35.7494892631586,41.6222215800908,-223.73364023664));
#227338=CARTESIAN_POINT('Ctrl Pts',(38.4097831290267,43.3156457680889,-220.597842103052));
#227339=CARTESIAN_POINT('Ctrl Pts',(41.0750442414306,45.0044380406571,-217.464638507897));
#227340=CARTESIAN_POINT('Ctrl Pts',(43.7412542098013,46.69118281627,-214.332014574282));
#227341=CARTESIAN_POINT('Ctrl Pts',(27.7467504913837,36.5219322799631,-233.170032188139));
#227342=CARTESIAN_POINT('Ctrl Pts',(28.3985217181101,36.9519116209705,-232.382753952573));
#227343=CARTESIAN_POINT('Ctrl Pts',(29.0525419525678,37.3805207587552,-231.59666656708));
#227344=CARTESIAN_POINT('Ctrl Pts',(29.707648099349,37.8084119595345,-230.811147097123));
#227345=CARTESIAN_POINT('Ctrl Pts',(30.3627542461301,38.2363031603138,-230.025627627167));
#227346=CARTESIAN_POINT('Ctrl Pts',(31.0189916736704,38.6634523908632,-229.240701082927));
#227347=CARTESIAN_POINT('Ctrl Pts',(31.6758577488396,39.0901500013781,-228.456102690314));
#227348=CARTESIAN_POINT('Ctrl Pts',(32.9895898991783,39.9435452224079,-226.886905905089));
#227349=CARTESIAN_POINT('Ctrl Pts',(34.305776607248,40.7951703456425,-225.318990914817));
#227350=CARTESIAN_POINT('Ctrl Pts',(35.6228886941575,41.6459326221272,-223.751565966636));
#227351=CARTESIAN_POINT('Ctrl Pts',(38.2571128679763,43.3474571750966,-220.616716070273));
#227352=CARTESIAN_POINT('Ctrl Pts',(40.8950551389346,45.0455299408185,-217.483839750893));
#227353=CARTESIAN_POINT('Ctrl Pts',(43.5337367396124,46.7419641904284,-214.351434639915));
#227354=CARTESIAN_POINT('Ctrl Pts',(27.7033987843753,36.5184180776487,-233.188057587778));
#227355=CARTESIAN_POINT('Ctrl Pts',(28.3494461390117,36.9495031672888,-232.401244113014));
#227356=CARTESIAN_POINT('Ctrl Pts',(28.9972196129455,37.3795877937595,-231.615362013826));
#227357=CARTESIAN_POINT('Ctrl Pts',(29.6459149724228,37.8090935762025,-230.829970164246));
#227358=CARTESIAN_POINT('Ctrl Pts',(30.2946103319002,38.2385993586454,-230.044578314665));
#227359=CARTESIAN_POINT('Ctrl Pts',(30.944252415395,38.6675143670179,-229.259690921114));
#227360=CARTESIAN_POINT('Ctrl Pts',(31.5944542499059,39.0960490201859,-228.475099818776));
#227361=CARTESIAN_POINT('Ctrl Pts',(32.8948579189276,39.9531183265218,-226.905917614101));
#227362=CARTESIAN_POINT('Ctrl Pts',(34.1974465074261,40.8086969168544,-225.337892124046));
#227363=CARTESIAN_POINT('Ctrl Pts',(35.5009303646614,41.6635101961778,-223.770343407667));
#227364=CARTESIAN_POINT('Ctrl Pts',(38.1078980791321,43.3731367548243,-220.635245974907));
#227365=CARTESIAN_POINT('Ctrl Pts',(40.7184182146441,45.0797275518329,-217.502045328114));
#227366=CARTESIAN_POINT('Ctrl Pts',(43.329743245898,46.7848839191427,-214.369334331916));
#227367=CARTESIAN_POINT('Ctrl Pts',(27.6544884050101,36.5134544997187,-233.208489782041));
#227368=CARTESIAN_POINT('Ctrl Pts',(28.2958883125488,36.9453045586868,-232.422071262426));
#227369=CARTESIAN_POINT('Ctrl Pts',(28.9385402233851,37.3764580517972,-231.636337934604));
#227370=CARTESIAN_POINT('Ctrl Pts',(29.5819207190053,37.8071775310161,-230.850998973988));
#227371=CARTESIAN_POINT('Ctrl Pts',(30.2253012146256,38.2378970102351,-230.065660013372));
#227372=CARTESIAN_POINT('Ctrl Pts',(30.8694237090864,38.6681763110842,-229.280723186985));
#227373=CARTESIAN_POINT('Ctrl Pts',(31.5140148312165,39.0981569518477,-228.496039104459));
#227374=CARTESIAN_POINT('Ctrl Pts',(32.8031970754766,39.9581182333748,-226.926670939409));
#227375=CARTESIAN_POINT('Ctrl Pts',(34.094212486763,40.8169068877022,-225.358291458816));
#227376=CARTESIAN_POINT('Ctrl Pts',(35.3860663228485,41.675053386644,-223.79036645522));
#227377=CARTESIAN_POINT('Ctrl Pts',(37.9697739950195,43.3913463845276,-220.654516448028));
#227378=CARTESIAN_POINT('Ctrl Pts',(40.5567806505099,45.1051056979372,-217.520458021817));
#227379=CARTESIAN_POINT('Ctrl Pts',(43.1447063347815,46.8176414904025,-214.386944837765));
#227380=CARTESIAN_POINT('Ctrl Pts',(27.6055780256448,36.5084909217888,-233.228921976304));
#227381=CARTESIAN_POINT('Ctrl Pts',(28.2423304860859,36.9411059500847,-232.442898411838));
#227382=CARTESIAN_POINT('Ctrl Pts',(28.8798608338247,37.3733283098348,-231.657313855381));
#227383=CARTESIAN_POINT('Ctrl Pts',(29.5179264655878,37.8052614858298,-230.87202778373));
#227384=CARTESIAN_POINT('Ctrl Pts',(30.1559920973509,38.2371946618249,-230.08674171208));
#227385=CARTESIAN_POINT('Ctrl Pts',(30.7945950027779,38.6688382551504,-229.301755452856));
#227386=CARTESIAN_POINT('Ctrl Pts',(31.433575412527,39.1002648835096,-228.516978390142));
#227387=CARTESIAN_POINT('Ctrl Pts',(32.7115362320255,39.9631181402278,-226.947424264716));
#227388=CARTESIAN_POINT('Ctrl Pts',(33.9909784660999,40.82511685855,-225.378690793586));
#227389=CARTESIAN_POINT('Ctrl Pts',(35.2712022810355,41.6865965771103,-223.810389502773));
#227390=CARTESIAN_POINT('Ctrl Pts',(37.8316499109069,43.4095560142309,-220.673786921149));
#227391=CARTESIAN_POINT('Ctrl Pts',(40.3951430863757,45.1304838440415,-217.53887071552));
#227392=CARTESIAN_POINT('Ctrl Pts',(42.9596694236649,46.8503990616624,-214.404555343614));
#227393=CARTESIAN_POINT('Ctrl Pts',(27.5495579756445,36.5028921654741,-233.251051919951));
#227394=CARTESIAN_POINT('Ctrl Pts',(28.1827688115622,36.9359521258547,-232.465366213753));
#227395=CARTESIAN_POINT('Ctrl Pts',(28.8164085091962,37.3688162618127,-231.679931708896));
#227396=CARTESIAN_POINT('Ctrl Pts',(29.45037829501,37.8015234896747,-230.894689344989));
#227397=CARTESIAN_POINT('Ctrl Pts',(30.0843480808238,38.2342307175367,-230.109446981082));
#227398=CARTESIAN_POINT('Ctrl Pts',(30.7186486771531,38.6667807943463,-229.324397213218));
#227399=CARTESIAN_POINT('Ctrl Pts',(31.3532086585038,39.0992026045944,-228.539497756859));
#227400=CARTESIAN_POINT('Ctrl Pts',(32.6223286212052,39.9640462250905,-226.96969884414));
#227401=CARTESIAN_POINT('Ctrl Pts',(33.8924746608402,40.828381296436,-225.400494315711));
#227402=CARTESIAN_POINT('Ctrl Pts',(35.1632781294504,41.6923616886714,-223.831668727949));
#227403=CARTESIAN_POINT('Ctrl Pts',(37.7048850666709,43.4203224731419,-220.694017552425));
#227404=CARTESIAN_POINT('Ctrl Pts',(40.2490633538194,45.1468896454712,-217.55784834607));
#227405=CARTESIAN_POINT('Ctrl Pts',(42.7944274621604,46.8726693939935,-214.42236887553));
#227406=CARTESIAN_POINT('Ctrl Pts',(27.4675166955088,36.501209334595,-233.2699618027));
#227407=CARTESIAN_POINT('Ctrl Pts',(28.0986597880893,36.9344896240505,-232.484645254214));
#227408=CARTESIAN_POINT('Ctrl Pts',(28.7300030462673,37.3676977230337,-231.69945191414));
#227409=CARTESIAN_POINT('Ctrl Pts',(29.3615087464634,37.8008474937043,-230.914358703846));
#227410=CARTESIAN_POINT('Ctrl Pts',(29.9930144466596,38.2339972643749,-230.129265493552));
#227411=CARTESIAN_POINT('Ctrl Pts',(30.624682800611,38.6670886387032,-229.344272547955));
#227412=CARTESIAN_POINT('Ctrl Pts',(31.2564852375126,39.1001323034766,-228.559362491382));
#227413=CARTESIAN_POINT('Ctrl Pts',(32.5200901113159,39.9662196330235,-226.989542378236));
#227414=CARTESIAN_POINT('Ctrl Pts',(33.7842270188127,40.8321176985828,-225.420051188828));
#227415=CARTESIAN_POINT('Ctrl Pts',(35.0487393284727,41.6978863030865,-223.850794334856));
#227416=CARTESIAN_POINT('Ctrl Pts',(37.5777639477929,43.429423512094,-220.712280626913));
#227417=CARTESIAN_POINT('Ctrl Pts',(40.1082645173074,45.1604528702306,-217.574688874121));
#227418=CARTESIAN_POINT('Ctrl Pts',(42.6395909737856,46.8912293280373,-214.437630225606));
#227419=CARTESIAN_POINT('',(27.8050196335447,36.7328855798153,-232.850049995496));
#227420=CARTESIAN_POINT('',(28.9186324328831,36.3202559616763,-232.850049990517));
#227421=CARTESIAN_POINT('Ctrl Pts',(27.8050196334018,36.7328855787358,-232.85005));
#227422=CARTESIAN_POINT('Ctrl Pts',(27.8957217939294,36.7208730140292,-232.85005));
#227423=CARTESIAN_POINT('Ctrl Pts',(27.9536434306237,36.7103454425016,-232.850049999997));
#227424=CARTESIAN_POINT('Ctrl Pts',(28.0509870287882,36.6868458484317,-232.850049999997));
#227425=CARTESIAN_POINT('Ctrl Pts',(28.0803209311281,36.6793979170128,-232.850049999947));
#227426=CARTESIAN_POINT('Ctrl Pts',(28.1944269137096,36.649053901996,-232.850049999947));
#227427=CARTESIAN_POINT('Ctrl Pts',(28.2694640302114,36.6259313942996,-232.850050000001));
#227428=CARTESIAN_POINT('Ctrl Pts',(28.4201368589766,36.5675330811538,-232.850050000001));
#227429=CARTESIAN_POINT('Ctrl Pts',(28.4595308694401,36.5515483381828,-232.850050000008));
#227430=CARTESIAN_POINT('Ctrl Pts',(28.5248449659433,36.5234632061754,-232.850050000008));
#227431=CARTESIAN_POINT('Ctrl Pts',(28.5526105252556,36.5109406727164,-232.85005));
#227432=CARTESIAN_POINT('Ctrl Pts',(28.6047252501233,36.4866036083131,-232.85005));
#227433=CARTESIAN_POINT('Ctrl Pts',(28.6308279330002,36.4740323136216,-232.85005));
#227434=CARTESIAN_POINT('Ctrl Pts',(28.6952211500754,36.442440071217,-232.85005));
#227435=CARTESIAN_POINT('Ctrl Pts',(28.7462884613452,36.4168028902437,-232.850050000002));
#227436=CARTESIAN_POINT('Ctrl Pts',(28.7999670577683,36.3884950980527,-232.850050000002));
#227437=CARTESIAN_POINT('Ctrl Pts',(28.8178719483369,36.3786725027028,-232.85005));
#227438=CARTESIAN_POINT('Ctrl Pts',(28.8625139388136,36.353549720413,-232.85005));
#227439=CARTESIAN_POINT('Ctrl Pts',(28.8919158089781,36.3362438515589,-232.85005));
#227440=CARTESIAN_POINT('Ctrl Pts',(28.9186324246664,36.3202560005055,-232.85005));
#227441=CARTESIAN_POINT('',(46.6391379812522,45.1301057287331,-214.324193081127));
#227442=CARTESIAN_POINT('Ctrl Pts',(28.9186324530669,36.3202559475719,-232.850049971551));
#227443=CARTESIAN_POINT('Ctrl Pts',(30.3889628274848,37.0479740123936,-231.318454284006));
#227444=CARTESIAN_POINT('Ctrl Pts',(31.8584196044282,37.7756558134426,-229.786568839607));
#227445=CARTESIAN_POINT('Ctrl Pts',(33.3268737332982,38.5035276796851,-228.254395210835));
#227446=CARTESIAN_POINT('Ctrl Pts',(34.8098341713358,39.2385899198853,-226.707085811785));
#227447=CARTESIAN_POINT('Ctrl Pts',(36.2917724634469,39.9738456977312,-225.159482536368));
#227448=CARTESIAN_POINT('Ctrl Pts',(37.7725665108881,40.7095346352291,-223.61157467501));
#227449=CARTESIAN_POINT('Ctrl Pts',(37.793700233912,40.7200343034737,-223.589483111322));
#227450=CARTESIAN_POINT('Ctrl Pts',(37.8148337232645,40.7305340582079,-223.567391484236));
#227451=CARTESIAN_POINT('Ctrl Pts',(37.8359669785468,40.7410339005308,-223.54529979386));
#227452=CARTESIAN_POINT('Ctrl Pts',(40.7752670935121,42.2013951811095,-220.472696581748));
#227453=CARTESIAN_POINT('Ctrl Pts',(43.710029434473,43.6634416063072,-217.398883050629));
#227454=CARTESIAN_POINT('Ctrl Pts',(46.6391379662423,45.1301057056288,-214.324193130075));
#227455=CARTESIAN_POINT('',(42.9717852817483,46.7498147039571,-214.534096350323));
#227456=CARTESIAN_POINT('Ctrl Pts',(42.9717852817571,46.749814703953,-214.534096350459));
#227457=CARTESIAN_POINT('Ctrl Pts',(43.0986721931634,46.725774799666,-214.525192835447));
#227458=CARTESIAN_POINT('Ctrl Pts',(43.2250603487411,46.6989506892725,-214.516517597904));
#227459=CARTESIAN_POINT('Ctrl Pts',(43.4873979542363,46.637223499967,-214.499052367716));
#227460=CARTESIAN_POINT('Ctrl Pts',(43.623673328713,46.6017076161697,-214.490110644586));
#227461=CARTESIAN_POINT('Ctrl Pts',(43.8528808070891,46.5361367088664,-214.475014174639));
#227462=CARTESIAN_POINT('Ctrl Pts',(43.9471502952977,46.5074540597886,-214.468951067943));
#227463=CARTESIAN_POINT('Ctrl Pts',(44.1657362377398,46.4369225436547,-214.455376470192));
#227464=CARTESIAN_POINT('Ctrl Pts',(44.289571969337,46.3939046796098,-214.447959352174));
#227465=CARTESIAN_POINT('Ctrl Pts',(44.5758870687418,46.2872516657367,-214.430838622362));
#227466=CARTESIAN_POINT('Ctrl Pts',(44.7376694321899,46.2214844640658,-214.421105848154));
#227467=CARTESIAN_POINT('Ctrl Pts',(44.9968192003615,46.1070741799036,-214.406088225855));
#227468=CARTESIAN_POINT('Ctrl Pts',(45.0953309344668,46.0613945558291,-214.400545485095));
#227469=CARTESIAN_POINT('Ctrl Pts',(45.358658729469,45.9333375459576,-214.386175771069));
#227470=CARTESIAN_POINT('Ctrl Pts',(45.5225973319306,45.8471698157457,-214.377106636997));
#227471=CARTESIAN_POINT('Ctrl Pts',(45.7910067954592,45.6952312414373,-214.362880563453));
#227472=CARTESIAN_POINT('Ctrl Pts',(45.8980961664271,45.6315653232451,-214.357676228462));
#227473=CARTESIAN_POINT('Ctrl Pts',(46.0677903918145,45.5257929939876,-214.349632079145));
#227474=CARTESIAN_POINT('Ctrl Pts',(46.1316130052832,45.4848666362459,-214.346627166679));
#227475=CARTESIAN_POINT('Ctrl Pts',(46.2762133611491,45.3894937682619,-214.339569954194));
#227476=CARTESIAN_POINT('Ctrl Pts',(46.3575523973275,45.3339263995932,-214.335548815045));
#227477=CARTESIAN_POINT('Ctrl Pts',(46.5062346419673,45.2285595755895,-214.329247262279));
#227478=CARTESIAN_POINT('Ctrl Pts',(46.5731746847777,45.1796922524229,-214.326639483788));
#227479=CARTESIAN_POINT('Ctrl Pts',(46.6391379874981,45.1301057436029,-214.324192948146));
#227480=CARTESIAN_POINT('',(42.5495440915934,46.8296601108864,-214.549225395662));
#227481=CARTESIAN_POINT('Ctrl Pts',(42.9717852817571,46.7498147039531,-214.534096350459));
#227482=CARTESIAN_POINT('Ctrl Pts',(42.9007618486797,46.7632707532202,-214.539079986663));
#227483=CARTESIAN_POINT('Ctrl Pts',(42.8299856383427,46.7766655446186,-214.542913387513));
#227484=CARTESIAN_POINT('Ctrl Pts',(42.6887342414797,46.8033747711886,-214.547975651047));
#227485=CARTESIAN_POINT('Ctrl Pts',(42.6197623734487,46.8164057424326,-214.549201731095));
#227486=CARTESIAN_POINT('Ctrl Pts',(42.5495441334904,46.8296600955011,-214.549225427215));
#227487=CARTESIAN_POINT('Ctrl Pts',(27.805019639331,36.7328855899921,-232.85005));
#227488=CARTESIAN_POINT('Ctrl Pts',(32.7122624052548,40.1011588208396,-226.745065671994));
#227489=CARTESIAN_POINT('Ctrl Pts',(37.6297308332976,43.4657453232396,-220.646376054327));
#227490=CARTESIAN_POINT('Ctrl Pts',(42.5495441536942,46.8296600915864,-214.549225432877));
#227491=CARTESIAN_POINT('Ctrl Pts',(47.3114554705886,16.8460380888807,-233.260539515782));
#227492=CARTESIAN_POINT('Ctrl Pts',(48.3395590816568,17.8367146054412,-231.692947455239));
#227493=CARTESIAN_POINT('Ctrl Pts',(49.3676726219367,18.8273604593628,-230.125342611939));
#227494=CARTESIAN_POINT('Ctrl Pts',(50.3957927612346,19.8179857984423,-228.557729212486));
#227495=CARTESIAN_POINT('Ctrl Pts',(51.4239129005325,20.8086111375217,-226.990115813032));
#227496=CARTESIAN_POINT('Ctrl Pts',(52.4520396931497,21.7992157970736,-225.422493789));
#227497=CARTESIAN_POINT('Ctrl Pts',(53.480171119088,22.7898059407486,-223.854865709355));
#227498=CARTESIAN_POINT('Ctrl Pts',(55.5364339709647,24.7709862280985,-220.719609550066));
#227499=CARTESIAN_POINT('Ctrl Pts',(57.5927150219887,26.7521094718628,-217.584329593504));
#227500=CARTESIAN_POINT('Ctrl Pts',(59.6490056999632,28.7332018665566,-214.449036765473));
#227501=CARTESIAN_POINT('Ctrl Pts',(47.3110520982437,16.8559465263517,-233.26053824229));
#227502=CARTESIAN_POINT('Ctrl Pts',(48.3391380137511,17.8470909658639,-231.692946212383));
#227503=CARTESIAN_POINT('Ctrl Pts',(49.3672339116285,18.8382047449221,-230.125341393407));
#227504=CARTESIAN_POINT('Ctrl Pts',(50.3953364602535,19.82929801124,-228.55772801405));
#227505=CARTESIAN_POINT('Ctrl Pts',(51.4234390088786,20.8203912775578,-226.990114634692));
#227506=CARTESIAN_POINT('Ctrl Pts',(52.4515482625761,21.8114638664511,-225.422492626496));
#227507=CARTESIAN_POINT('Ctrl Pts',(53.4796622004807,22.8025219415151,-223.854864559695));
#227508=CARTESIAN_POINT('Ctrl Pts',(55.5358900762899,24.7846380916432,-220.719608426093));
#227509=CARTESIAN_POINT('Ctrl Pts',(57.5921363546469,26.7666972063695,-217.58432848346));
#227510=CARTESIAN_POINT('Ctrl Pts',(59.6483924596735,28.7487254799229,-214.449035662994));
#227511=CARTESIAN_POINT('Ctrl Pts',(47.3103397682614,16.8668521773429,-233.260936805424));
#227512=CARTESIAN_POINT('Ctrl Pts',(48.3384173520821,17.8584323054149,-231.693333771247));
#227513=CARTESIAN_POINT('Ctrl Pts',(49.3665034987094,18.8499861389194,-230.125719739421));
#227514=CARTESIAN_POINT('Ctrl Pts',(50.3945954284579,19.8415221922535,-228.558098269208));
#227515=CARTESIAN_POINT('Ctrl Pts',(51.4226873582065,20.8330582455877,-226.990476798996));
#227516=CARTESIAN_POINT('Ctrl Pts',(52.4507851140727,21.8245763873091,-225.422847835511));
#227517=CARTESIAN_POINT('Ctrl Pts',(53.4788869862349,22.8160818579234,-223.855213570177));
#227518=CARTESIAN_POINT('Ctrl Pts',(55.5350907305594,24.7990927991518,-220.719945039509));
#227519=CARTESIAN_POINT('Ctrl Pts',(57.5913106558967,26.7820539269176,-217.584655665656));
#227520=CARTESIAN_POINT('Ctrl Pts',(59.6475394024948,28.7649878151953,-214.449354892196));
#227521=CARTESIAN_POINT('Ctrl Pts',(47.3110535174895,16.873256830116,-233.259496526039));
#227522=CARTESIAN_POINT('Ctrl Pts',(48.3390812029547,17.8654084135782,-231.691932847844));
#227523=CARTESIAN_POINT('Ctrl Pts',(49.3671224159146,18.8575190179354,-230.124352092621));
#227524=CARTESIAN_POINT('Ctrl Pts',(50.3951725945636,19.8496024611769,-228.556760010403));
#227525=CARTESIAN_POINT('Ctrl Pts',(51.4232227732125,20.8416859044184,-226.989167928185));
#227526=CARTESIAN_POINT('Ctrl Pts',(52.4512819949066,21.8337419536198,-225.421564422348));
#227527=CARTESIAN_POINT('Ctrl Pts',(53.4793475235956,22.8257789108232,-223.853952950714));
#227528=CARTESIAN_POINT('Ctrl Pts',(55.5354785809735,24.8098528252302,-220.718730007446));
#227529=CARTESIAN_POINT('Ctrl Pts',(57.5916344152767,26.7938517410564,-217.583475771517));
#227530=CARTESIAN_POINT('Ctrl Pts',(59.6478035550371,28.7778105309341,-214.448204781494));
#227531=CARTESIAN_POINT('Ctrl Pts',(47.3117672667176,16.8796614828891,-233.258056246654));
#227532=CARTESIAN_POINT('Ctrl Pts',(48.3397450538273,17.8723845217414,-231.690531924442));
#227533=CARTESIAN_POINT('Ctrl Pts',(49.3677413331199,18.8650518969515,-230.122984445821));
#227534=CARTESIAN_POINT('Ctrl Pts',(50.3957497606693,19.8576827301003,-228.555421751598));
#227535=CARTESIAN_POINT('Ctrl Pts',(51.4237581882186,20.8503135632492,-226.987859057374));
#227536=CARTESIAN_POINT('Ctrl Pts',(52.4517788757404,21.8429075199303,-225.420281009185));
#227537=CARTESIAN_POINT('Ctrl Pts',(53.4798080609562,22.835475963723,-223.852692331251));
#227538=CARTESIAN_POINT('Ctrl Pts',(55.5358664313876,24.8206128513086,-220.717514975384));
#227539=CARTESIAN_POINT('Ctrl Pts',(57.5919581746568,26.8056495551953,-217.582295877378));
#227540=CARTESIAN_POINT('Ctrl Pts',(59.6480677075794,28.790633246673,-214.447054670791));
#227541=CARTESIAN_POINT('Ctrl Pts',(47.3124780096108,16.8859145617117,-233.256609308214));
#227542=CARTESIAN_POINT('Ctrl Pts',(48.3404033416989,17.879229404878,-231.689125142628));
#227543=CARTESIAN_POINT('Ctrl Pts',(49.3683527798054,18.8724721952687,-230.121611075758));
#227544=CARTESIAN_POINT('Ctrl Pts',(50.3963178475467,19.8656683126149,-228.554077618338));
#227545=CARTESIAN_POINT('Ctrl Pts',(51.424282915288,20.8588644299609,-226.986544160919));
#227546=CARTESIAN_POINT('Ctrl Pts',(52.4522637695665,21.8520134082152,-225.418991120778));
#227547=CARTESIAN_POINT('Ctrl Pts',(53.480255460339,22.8451301056268,-223.851424659566));
#227548=CARTESIAN_POINT('Ctrl Pts',(55.5362388418842,24.83136350045,-220.716291737142));
#227549=CARTESIAN_POINT('Ctrl Pts',(57.5922647611927,26.8174702004918,-217.581106138124));
#227550=CARTESIAN_POINT('Ctrl Pts',(59.6483130536229,28.8035108935828,-214.4458930656));
#227551=CARTESIAN_POINT('Ctrl Pts',(47.3131850756779,16.8920273532507,-233.255157881008));
#227552=CARTESIAN_POINT('Ctrl Pts',(48.3410552958596,17.8859535740668,-231.68771449894));
#227553=CARTESIAN_POINT('Ctrl Pts',(49.3689559345468,18.8797895866585,-230.120233792132));
#227554=CARTESIAN_POINT('Ctrl Pts',(50.3968759670817,19.8735681235901,-228.552729269786));
#227555=CARTESIAN_POINT('Ctrl Pts',(51.4247959996165,20.8673466605217,-226.98522474744));
#227556=CARTESIAN_POINT('Ctrl Pts',(52.4527356437508,21.8610670819393,-225.417696146955));
#227557=CARTESIAN_POINT('Ctrl Pts',(53.4806885888443,22.8547481865589,-223.850151240679));
#227558=CARTESIAN_POINT('Ctrl Pts',(55.5365944790313,24.8421103957982,-220.715061428126));
#227559=CARTESIAN_POINT('Ctrl Pts',(57.5925525533974,26.8293183807281,-217.579907651647));
#227560=CARTESIAN_POINT('Ctrl Pts',(59.6485376230928,28.8164474339779,-214.444721098757));
#227561=CARTESIAN_POINT('Ctrl Pts',(47.3145992078122,16.9042529363287,-233.252255026597));
#227562=CARTESIAN_POINT('Ctrl Pts',(48.342359204181,17.8994019124442,-231.684893211564));
#227563=CARTESIAN_POINT('Ctrl Pts',(49.3701622440295,18.8944243694381,-230.117479224879));
#227564=CARTESIAN_POINT('Ctrl Pts',(50.3979922061516,19.8893677455407,-228.55003257268));
#227565=CARTESIAN_POINT('Ctrl Pts',(51.4258221682736,20.8843111216433,-226.982585920481));
#227566=CARTESIAN_POINT('Ctrl Pts',(52.4536793921196,21.8791744293876,-225.41510619931));
#227567=CARTESIAN_POINT('Ctrl Pts',(53.4815548458549,22.8739843484231,-223.847604402904));
#227568=CARTESIAN_POINT('Ctrl Pts',(55.5373057533255,24.8636041864943,-220.712600810094));
#227569=CARTESIAN_POINT('Ctrl Pts',(57.5931281378066,26.8530147412008,-217.577510678694));
#227570=CARTESIAN_POINT('Ctrl Pts',(59.6489867620326,28.8423205147682,-214.442377165073));
#227571=CARTESIAN_POINT('Ctrl Pts',(47.3159989701972,16.9159167325326,-233.249334003942));
#227572=CARTESIAN_POINT('Ctrl Pts',(48.3436380292726,17.9123669615539,-231.682056339452));
#227573=CARTESIAN_POINT('Ctrl Pts',(49.3713355823747,18.9086472103352,-230.114708908922));
#227574=CARTESIAN_POINT('Ctrl Pts',(50.3990687332636,19.9048240492912,-228.547318949062));
#227575=CARTESIAN_POINT('Ctrl Pts',(51.4268018841524,20.9010008882471,-226.979928989203));
#227576=CARTESIAN_POINT('Ctrl Pts',(52.45457115623,21.8970728138782,-225.412495889199));
#227577=CARTESIAN_POINT('Ctrl Pts',(53.4823640955953,22.8930761954416,-223.84503456711));
#227578=CARTESIAN_POINT('Ctrl Pts',(55.537949974326,24.8850829585685,-220.710111922933));
#227579=CARTESIAN_POINT('Ctrl Pts',(57.5936285702719,26.8768212639349,-217.575078740198));
#227580=CARTESIAN_POINT('Ctrl Pts',(59.6493528038196,28.8684292299185,-214.439991823286));
#227581=CARTESIAN_POINT('Ctrl Pts',(47.317375174873,16.9271166732568,-233.246414795271));
#227582=CARTESIAN_POINT('Ctrl Pts',(48.3448826696721,17.9249382396269,-231.679221637881));
#227583=CARTESIAN_POINT('Ctrl Pts',(49.3724670545446,18.9225395323645,-230.111938592781));
#227584=CARTESIAN_POINT('Ctrl Pts',(50.4000965635423,19.9200114073275,-228.544602587596));
#227585=CARTESIAN_POINT('Ctrl Pts',(51.42772607254,20.9174832822903,-226.977266582412));
#227586=CARTESIAN_POINT('Ctrl Pts',(52.4554015221151,21.9148234426101,-225.409876692422));
#227587=CARTESIAN_POINT('Ctrl Pts',(53.4831063385788,22.9120795922463,-223.842452376097));
#227588=CARTESIAN_POINT('Ctrl Pts',(55.5385159715063,24.9065918915186,-220.707603743446));
#227589=CARTESIAN_POINT('Ctrl Pts',(57.5940405653775,26.9007754041514,-217.572620374409));
#227590=CARTESIAN_POINT('Ctrl Pts',(59.6496198849772,28.8948045789125,-214.437573677779));
#227591=CARTESIAN_POINT('Ctrl Pts',(47.3201275842246,16.9495165547055,-233.240576377928));
#227592=CARTESIAN_POINT('Ctrl Pts',(48.3473719504709,17.9500807957729,-231.67355223474));
#227593=CARTESIAN_POINT('Ctrl Pts',(49.3747299988842,18.9503241764231,-230.106397960498));
#227594=CARTESIAN_POINT('Ctrl Pts',(50.4021522240997,19.9503861234,-228.539169864665));
#227595=CARTESIAN_POINT('Ctrl Pts',(51.4295744493152,20.9504480703769,-226.97194176883));
#227596=CARTESIAN_POINT('Ctrl Pts',(52.4570622538851,21.9503247000739,-225.40463829887));
#227597=CARTESIAN_POINT('Ctrl Pts',(53.4845908245458,22.9500863858554,-223.837287994071));
#227598=CARTESIAN_POINT('Ctrl Pts',(55.539647965867,24.9496097574185,-220.702587384473));
#227599=CARTESIAN_POINT('Ctrl Pts',(57.5948645555888,26.9486836845843,-217.56770364283));
#227600=CARTESIAN_POINT('Ctrl Pts',(59.6501540472924,28.9475552769007,-214.432737386764));
#227601=CARTESIAN_POINT('Ctrl Pts',(47.3227915814476,16.9700523845408,-233.234742668299));
#227602=CARTESIAN_POINT('Ctrl Pts',(48.3497283291618,17.9736436661242,-231.667890368169));
#227603=CARTESIAN_POINT('Ctrl Pts',(49.3768283745781,18.9767837847294,-230.100856716523));
#227604=CARTESIAN_POINT('Ctrl Pts',(50.4040153385433,19.9796831826563,-228.533725925203));
#227605=CARTESIAN_POINT('Ctrl Pts',(51.4312023025085,20.9825825805833,-226.966595133883));
#227606=CARTESIAN_POINT('Ctrl Pts',(52.4584786467041,21.9852345805636,-225.399364559241));
#227607=CARTESIAN_POINT('Ctrl Pts',(53.4858082893199,22.9877393389703,-223.832074478405));
#227608=CARTESIAN_POINT('Ctrl Pts',(55.5404675745514,24.9927488557837,-220.697494316732));
#227609=CARTESIAN_POINT('Ctrl Pts',(57.5953351427,26.9971831704407,-217.562681699479));
#227610=CARTESIAN_POINT('Ctrl Pts',(59.6502925248986,29.0013735664462,-214.427770494967));
#227611=CARTESIAN_POINT('Ctrl Pts',(47.3252263828413,16.9896223025012,-233.229110072315));
#227612=CARTESIAN_POINT('Ctrl Pts',(48.3518314896857,17.9964142568803,-231.662398987523));
#227613=CARTESIAN_POINT('Ctrl Pts',(49.3786544580299,19.0026193721543,-230.095454289591));
#227614=CARTESIAN_POINT('Ctrl Pts',(50.4055851760868,20.0085325545711,-228.528392739382));
#227615=CARTESIAN_POINT('Ctrl Pts',(51.4325158941438,21.0144457369877,-226.961331189173));
#227616=CARTESIAN_POINT('Ctrl Pts',(52.459558588544,22.0200559113108,-225.394148461867));
#227617=CARTESIAN_POINT('Ctrl Pts',(53.4866652007083,23.0254932317529,-223.826896445521));
#227618=CARTESIAN_POINT('Ctrl Pts',(55.5408784250369,25.0363678726369,-220.692392412828));
#227619=CARTESIAN_POINT('Ctrl Pts',(57.5953414810798,27.046567195329,-217.557617709049));
#227620=CARTESIAN_POINT('Ctrl Pts',(59.6499065909155,29.0564953668167,-214.422734451764));
#227621=CARTESIAN_POINT('Ctrl Pts',(47.3300959856285,17.0287621384219,-233.217844880347));
#227622=CARTESIAN_POINT('Ctrl Pts',(48.3560378107335,18.0419554383925,-231.651416226232));
#227623=CARTESIAN_POINT('Ctrl Pts',(49.3823066249335,19.0542905470043,-230.08464943573));
#227624=CARTESIAN_POINT('Ctrl Pts',(50.4087248511739,20.0662312984004,-228.517726367742));
#227625=CARTESIAN_POINT('Ctrl Pts',(51.4351430774143,21.0781720497965,-226.950803299753));
#227626=CARTESIAN_POINT('Ctrl Pts',(52.4617184722238,22.0896985728052,-225.383716267118));
#227627=CARTESIAN_POINT('Ctrl Pts',(53.4883790234851,23.1010010173179,-223.816540379752));
#227628=CARTESIAN_POINT('Ctrl Pts',(55.5417001260078,25.1236059063434,-220.68218860502));
#227629=CARTESIAN_POINT('Ctrl Pts',(57.5953541578395,27.1453352451054,-217.54748972819));
#227630=CARTESIAN_POINT('Ctrl Pts',(59.6491347229493,29.1667389675576,-214.412662365356));
#227631=CARTESIAN_POINT('Ctrl Pts',(47.3340807471002,17.0640763095221,-233.207405072206));
#227632=CARTESIAN_POINT('Ctrl Pts',(48.3592415226016,18.084391760883,-231.641145159187));
#227633=CARTESIAN_POINT('Ctrl Pts',(49.3848779968831,19.1035202524442,-230.074425303614));
#227634=CARTESIAN_POINT('Ctrl Pts',(50.4106976289339,20.1221883131755,-228.507525821657));
#227635=CARTESIAN_POINT('Ctrl Pts',(51.4365172609848,21.1408563739068,-226.9406263397));
#227636=CARTESIAN_POINT('Ctrl Pts',(52.4625365580142,22.1590237254166,-225.373531896091));
#227637=CARTESIAN_POINT('Ctrl Pts',(53.4886544050993,23.1769445199182,-223.806341423117));
#227638=CARTESIAN_POINT('Ctrl Pts',(55.5408900992694,25.2127861089213,-220.671960477169));
#227639=CARTESIAN_POINT('Ctrl Pts',(57.593512687643,27.2476605248632,-217.537203022514));
#227640=CARTESIAN_POINT('Ctrl Pts',(59.6462671267447,29.2822144774089,-214.402322487616));
#227641=CARTESIAN_POINT('Ctrl Pts',(47.3352334252266,17.1035049830549,-233.199529035477));
#227642=CARTESIAN_POINT('Ctrl Pts',(48.3600042849483,18.1301783396072,-231.632852310436));
#227643=CARTESIAN_POINT('Ctrl Pts',(49.3851454200133,19.1559450105208,-230.065825712809));
#227644=CARTESIAN_POINT('Ctrl Pts',(50.4104205557466,20.1813828669923,-228.498672133956));
#227645=CARTESIAN_POINT('Ctrl Pts',(51.4356956914798,21.2068207234638,-226.931518555102));
#227646=CARTESIAN_POINT('Ctrl Pts',(52.4611193627566,22.2318946684557,-225.364224580397));
#227647=CARTESIAN_POINT('Ctrl Pts',(53.4866146769212,23.2567945291104,-223.79686392097));
#227648=CARTESIAN_POINT('Ctrl Pts',(55.5376053052503,25.3065942504197,-220.662142602115));
#227649=CARTESIAN_POINT('Ctrl Pts',(57.5888779614229,27.3557092766758,-217.527159175984));
#227650=CARTESIAN_POINT('Ctrl Pts',(59.6402468289299,29.4046011172088,-214.392093753442));
#227651=CARTESIAN_POINT('Ctrl Pts',(47.3375387814793,17.1823623301207,-233.18377696202));
#227652=CARTESIAN_POINT('Ctrl Pts',(48.3615298096416,18.2217514970558,-231.616266612933));
#227653=CARTESIAN_POINT('Ctrl Pts',(49.3856802662736,19.2607945266738,-230.048626531198));
#227654=CARTESIAN_POINT('Ctrl Pts',(50.4098664093718,20.299771974626,-228.480964758552));
#227655=CARTESIAN_POINT('Ctrl Pts',(51.43405255247,21.3387494225781,-226.913302985906));
#227656=CARTESIAN_POINT('Ctrl Pts',(52.4582849722416,22.377636554534,-225.34560994901));
#227657=CARTESIAN_POINT('Ctrl Pts',(53.4825352205651,23.4164945474948,-223.777908916675));
#227658=CARTESIAN_POINT('Ctrl Pts',(55.5310357172121,25.4942105334166,-220.642506852006));
#227659=CARTESIAN_POINT('Ctrl Pts',(57.5796085089827,27.5718067803009,-217.507071482923));
#227660=CARTESIAN_POINT('Ctrl Pts',(59.6282062333003,29.6493743968087,-214.371636285096));
#227661=CARTESIAN_POINT('Ctrl Pts',(47.3383263868385,17.2535337845356,-233.16852831652));
#227662=CARTESIAN_POINT('Ctrl Pts',(48.3611580995056,18.3073838091979,-231.599694154632));
#227663=CARTESIAN_POINT('Ctrl Pts',(49.3835577975687,19.3623427162029,-230.031292497904));
#227664=CARTESIAN_POINT('Ctrl Pts',(50.4058155742669,20.4176535575179,-228.463032821567));
#227665=CARTESIAN_POINT('Ctrl Pts',(51.4280733509651,21.4729643988329,-226.894773145231));
#227666=CARTESIAN_POINT('Ctrl Pts',(52.4501722979439,22.5286737057843,-225.326672671531));
#227667=CARTESIAN_POINT('Ctrl Pts',(53.472204800048,23.5845483661524,-223.75864059823));
#227668=CARTESIAN_POINT('Ctrl Pts',(55.5162698042562,25.6962976868884,-220.622576451631));
#227669=CARTESIAN_POINT('Ctrl Pts',(57.5600729846415,27.8087001526143,-217.486782588132));
#227670=CARTESIAN_POINT('Ctrl Pts',(59.6038198261226,29.9212462142014,-214.351060388696));
#227671=CARTESIAN_POINT('Ctrl Pts',(47.3388947489722,17.3172597414177,-233.15277350217));
#227672=CARTESIAN_POINT('Ctrl Pts',(48.3602977670814,18.3855423142397,-231.582083581833));
#227673=CARTESIAN_POINT('Ctrl Pts',(49.3799313248768,19.4576103826212,-230.012850342708));
#227674=CARTESIAN_POINT('Ctrl Pts',(50.3991818891466,20.5304657339301,-228.443915670914));
#227675=CARTESIAN_POINT('Ctrl Pts',(51.4184324534164,21.6033210852391,-226.874980999121));
#227676=CARTESIAN_POINT('Ctrl Pts',(52.4371748506907,22.6772399564986,-225.306453273624));
#227677=CARTESIAN_POINT('Ctrl Pts',(53.4557277384216,23.7515480681017,-223.738076580824));
#227678=CARTESIAN_POINT('Ctrl Pts',(55.4928335138835,25.9001642913079,-220.601323195224));
#227679=CARTESIAN_POINT('Ctrl Pts',(57.529175347697,28.050353188994,-217.465180895102));
#227680=CARTESIAN_POINT('Ctrl Pts',(59.5653551090103,30.2008561303528,-214.329177297802));
#227681=CARTESIAN_POINT('Ctrl Pts',(47.3394631111059,17.3809856982998,-233.13701868782));
#227682=CARTESIAN_POINT('Ctrl Pts',(48.3594374346572,18.4637008192816,-231.564473009033));
#227683=CARTESIAN_POINT('Ctrl Pts',(49.3763048521849,19.5528780490395,-229.994408187512));
#227684=CARTESIAN_POINT('Ctrl Pts',(50.3925482040264,20.6432779103424,-228.424798520261));
#227685=CARTESIAN_POINT('Ctrl Pts',(51.4087915558678,21.7336777716453,-226.85518885301));
#227686=CARTESIAN_POINT('Ctrl Pts',(52.4241774034375,22.8258062072129,-225.286233875719));
#227687=CARTESIAN_POINT('Ctrl Pts',(53.4392506767952,23.9185477700511,-223.717512563418));
#227688=CARTESIAN_POINT('Ctrl Pts',(55.4693972235108,26.1040308957274,-220.580069938817));
#227689=CARTESIAN_POINT('Ctrl Pts',(57.4982777107523,28.2920062253737,-217.443579202073));
#227690=CARTESIAN_POINT('Ctrl Pts',(59.526890391898,30.4804660465043,-214.307294206909));
#227691=CARTESIAN_POINT('Ctrl Pts',(47.3366602074855,17.444170151716,-233.123362358707));
#227692=CARTESIAN_POINT('Ctrl Pts',(48.3540763070954,18.5429695999985,-231.549048499502));
#227693=CARTESIAN_POINT('Ctrl Pts',(49.3667036858826,19.6512330207133,-229.97834790794));
#227694=CARTESIAN_POINT('Ctrl Pts',(50.378495909681,20.7610182295588,-228.40819979349));
#227695=CARTESIAN_POINT('Ctrl Pts',(51.3902881334795,21.8708034384043,-226.83805167904));
#227696=CARTESIAN_POINT('Ctrl Pts',(52.4008473220208,22.9829339492799,-225.268781019355));
#227697=CARTESIAN_POINT('Ctrl Pts',(53.4109754339125,24.0958567445521,-223.699807621397));
#227698=CARTESIAN_POINT('Ctrl Pts',(55.4312316576958,26.3217023350964,-220.561860825481));
#227699=CARTESIAN_POINT('Ctrl Pts',(57.4497270949821,28.5507997267972,-217.425137866697));
#227700=CARTESIAN_POINT('Ctrl Pts',(59.4678639415957,30.7804881980906,-214.288663699106));
#227701=CARTESIAN_POINT('Ctrl Pts',(47.3285982419782,17.5118110061916,-233.112766042078));
#227702=CARTESIAN_POINT('Ctrl Pts',(48.3441007183216,18.6236888893903,-231.535741196264));
#227703=CARTESIAN_POINT('Ctrl Pts',(49.3524346981868,19.7490902161012,-229.963964803722));
#227704=CARTESIAN_POINT('Ctrl Pts',(50.3595015772335,20.8765891331594,-228.392921090687));
#227705=CARTESIAN_POINT('Ctrl Pts',(51.3665684562802,22.0040880502176,-226.821877377652));
#227706=CARTESIAN_POINT('Ctrl Pts',(52.3717783622527,23.1348854144855,-225.252060380076));
#227707=CARTESIAN_POINT('Ctrl Pts',(53.3763360684624,24.2667864286898,-223.682648344784));
#227708=CARTESIAN_POINT('Ctrl Pts',(55.3854514808819,26.5305884570984,-220.5438242742));
#227709=CARTESIAN_POINT('Ctrl Pts',(57.3919042457265,28.7989304812669,-217.40667659104));
#227710=CARTESIAN_POINT('Ctrl Pts',(59.397804330835,31.0680944254412,-214.269858953779));
#227711=CARTESIAN_POINT('Ctrl Pts',(47.3205362764709,17.5794518606674,-233.102169725448));
#227712=CARTESIAN_POINT('Ctrl Pts',(48.3341251295478,18.7044081787822,-231.522433893026));
#227713=CARTESIAN_POINT('Ctrl Pts',(49.338165710491,19.8469474114891,-229.949581699504));
#227714=CARTESIAN_POINT('Ctrl Pts',(50.3405072447859,20.99216003676,-228.377642387885));
#227715=CARTESIAN_POINT('Ctrl Pts',(51.3428487790808,22.1373726620309,-226.805703076266));
#227716=CARTESIAN_POINT('Ctrl Pts',(52.3427094024845,23.2868368796911,-225.235339740797));
#227717=CARTESIAN_POINT('Ctrl Pts',(53.3416967030123,24.4377161128276,-223.665489068171));
#227718=CARTESIAN_POINT('Ctrl Pts',(55.3396713040681,26.7394745791004,-220.525787722919));
#227719=CARTESIAN_POINT('Ctrl Pts',(57.334081396471,29.0470612357366,-217.388215315384));
#227720=CARTESIAN_POINT('Ctrl Pts',(59.3277447200742,31.3557006527919,-214.251054208451));
#227721=CARTESIAN_POINT('Ctrl Pts',(47.3141359442706,17.638980093523,-233.090010378228));
#227722=CARTESIAN_POINT('Ctrl Pts',(48.32443367589,18.7780728965381,-231.50825504547));
#227723=CARTESIAN_POINT('Ctrl Pts',(49.3229723535216,19.9379411976756,-229.93469251917));
#227724=CARTESIAN_POINT('Ctrl Pts',(50.3194004745391,21.1008963306773,-228.36214789025));
#227725=CARTESIAN_POINT('Ctrl Pts',(51.3158285955566,22.2638514636789,-226.78960326133));
#227726=CARTESIAN_POINT('Ctrl Pts',(52.3091900605982,23.4317796609776,-225.218887494463));
#227727=CARTESIAN_POINT('Ctrl Pts',(53.3014701549735,24.6013499668753,-223.648755791418));
#227728=CARTESIAN_POINT('Ctrl Pts',(55.2860303437241,26.9404905786706,-220.508492385326));
#227729=CARTESIAN_POINT('Ctrl Pts',(57.2661781231904,29.2864048695037,-217.370664238171));
#227730=CARTESIAN_POINT('Ctrl Pts',(59.2453960697349,31.6335238048983,-214.233295308244));
#227731=CARTESIAN_POINT('Ctrl Pts',(47.3068095033878,17.6967086574683,-233.077497779098));
#227732=CARTESIAN_POINT('Ctrl Pts',(48.3116549954781,18.8520796703188,-231.494638672248));
#227733=CARTESIAN_POINT('Ctrl Pts',(49.3030451918381,20.0301039514678,-229.920713549775));
#227734=CARTESIAN_POINT('Ctrl Pts',(50.2920112564435,21.2114530404761,-228.347855989514));
#227735=CARTESIAN_POINT('Ctrl Pts',(51.280977321049,22.3928021294844,-226.774998429254));
#227736=CARTESIAN_POINT('Ctrl Pts',(52.2664287923936,23.5795439345552,-225.204106117501));
#227737=CARTESIAN_POINT('Ctrl Pts',(53.2506399867227,24.7680561731562,-223.633834433041));
#227738=CARTESIAN_POINT('Ctrl Pts',(55.2190623753812,27.1450806503585,-220.493291064124));
#227739=CARTESIAN_POINT('Ctrl Pts',(57.1824244494106,29.5294142243635,-217.355341819955));
#227740=CARTESIAN_POINT('Ctrl Pts',(59.1447159484551,31.9150218118753,-214.217874373197));
#227741=CARTESIAN_POINT('Ctrl Pts',(47.2994830625051,17.7544372214138,-233.064985179967));
#227742=CARTESIAN_POINT('Ctrl Pts',(48.2988763150662,18.9260864440995,-231.481022299027));
#227743=CARTESIAN_POINT('Ctrl Pts',(49.2831180301545,20.12226670526,-229.90673458038));
#227744=CARTESIAN_POINT('Ctrl Pts',(50.264622038348,21.3220097502749,-228.333564088779));
#227745=CARTESIAN_POINT('Ctrl Pts',(51.2461260465415,22.5217527952899,-226.760393597177));
#227746=CARTESIAN_POINT('Ctrl Pts',(52.2236675241889,23.7273082081328,-225.189324740538));
#227747=CARTESIAN_POINT('Ctrl Pts',(53.199809818472,24.9347623794372,-223.618913074665));
#227748=CARTESIAN_POINT('Ctrl Pts',(55.1520944070382,27.3496707220463,-220.478089742921));
#227749=CARTESIAN_POINT('Ctrl Pts',(57.0986707756308,29.7724235792233,-217.34001940174));
#227750=CARTESIAN_POINT('Ctrl Pts',(59.0440358271753,32.1965198188522,-214.20245343815));
#227751=CARTESIAN_POINT('Ctrl Pts',(47.2842338109509,17.8211612809678,-233.056043673691));
#227752=CARTESIAN_POINT('Ctrl Pts',(48.2782304069827,19.0073087386684,-231.47028620506));
#227753=CARTESIAN_POINT('Ctrl Pts',(49.2548742655618,20.2206444917306,-229.89534347711));
#227754=CARTESIAN_POINT('Ctrl Pts',(50.2283116608323,21.437958506772,-228.321621606276));
#227755=CARTESIAN_POINT('Ctrl Pts',(51.2017490561027,22.6552725218134,-226.747899735443));
#227756=CARTESIAN_POINT('Ctrl Pts',(52.1706012443748,23.8790456722595,-225.176507139922));
#227757=CARTESIAN_POINT('Ctrl Pts',(53.1378257718042,25.1049289791612,-223.60583742058));
#227758=CARTESIAN_POINT('Ctrl Pts',(55.072274826663,27.5566955929646,-220.464497981896));
#227759=CARTESIAN_POINT('Ctrl Pts',(57.0000906545182,30.0171778123751,-217.326191699464));
#227760=CARTESIAN_POINT('Ctrl Pts',(58.9264876034895,32.47914368792,-214.188435032943));
#227761=CARTESIAN_POINT('Ctrl Pts',(47.2636279462708,17.8918194961353,-233.049292072559));
#227762=CARTESIAN_POINT('Ctrl Pts',(48.2527927601426,19.0896993463335,-231.461117845357));
#227763=CARTESIAN_POINT('Ctrl Pts',(49.2222701184903,20.3177090530585,-229.885189443365));
#227764=CARTESIAN_POINT('Ctrl Pts',(50.1877928495361,21.5503879875109,-228.310673435979));
#227765=CARTESIAN_POINT('Ctrl Pts',(51.1533155805818,22.7830669219633,-226.736157428594));
#227766=CARTESIAN_POINT('Ctrl Pts',(52.1134152350247,24.0230769225979,-225.164293315049));
#227767=CARTESIAN_POINT('Ctrl Pts',(53.0715402305708,25.265515738592,-223.593249605752));
#227768=CARTESIAN_POINT('Ctrl Pts',(54.9877902216631,27.75039337058,-220.451162187155));
#227769=CARTESIAN_POINT('Ctrl Pts',(56.8960314270369,30.2452705785478,-217.312517061756));
#227770=CARTESIAN_POINT('Ctrl Pts',(58.8025041724956,32.7418818204746,-214.174488273677));
#227771=CARTESIAN_POINT('Ctrl Pts',(47.2430220815907,17.9624777113029,-233.042540471425));
#227772=CARTESIAN_POINT('Ctrl Pts',(48.2273551133025,19.1720899539984,-231.451949485653));
#227773=CARTESIAN_POINT('Ctrl Pts',(49.1896659714189,20.4147736143863,-229.87503540962));
#227774=CARTESIAN_POINT('Ctrl Pts',(50.1472740382399,21.6628174682499,-228.299725265682));
#227775=CARTESIAN_POINT('Ctrl Pts',(51.1048821050609,22.9108613221134,-226.724415121745));
#227776=CARTESIAN_POINT('Ctrl Pts',(52.0562292256746,24.1671081729364,-225.152079490178));
#227777=CARTESIAN_POINT('Ctrl Pts',(53.0052546893374,25.4261024980228,-223.580661790924));
#227778=CARTESIAN_POINT('Ctrl Pts',(54.9033056166631,27.9440911481955,-220.437826392414));
#227779=CARTESIAN_POINT('Ctrl Pts',(56.7919721995556,30.4733633447205,-217.298842424047));
#227780=CARTESIAN_POINT('Ctrl Pts',(58.6785207415017,33.0046199530293,-214.16054151441));
#227781=CARTESIAN_POINT('Ctrl Pts',(47.2289637142144,18.0209926675766,-233.031939311332));
#227782=CARTESIAN_POINT('Ctrl Pts',(48.1993754505405,19.2535954323428,-231.443888976038));
#227783=CARTESIAN_POINT('Ctrl Pts',(49.1516972038829,20.512132417265,-229.866635744028));
#227784=CARTESIAN_POINT('Ctrl Pts',(50.0988311928047,21.7766727071225,-228.291351005029));
#227785=CARTESIAN_POINT('Ctrl Pts',(51.0459651817265,23.0412129969801,-226.716066266029));
#227786=CARTESIAN_POINT('Ctrl Pts',(51.9869923629565,24.3134260425889,-225.14358686793));
#227787=CARTESIAN_POINT('Ctrl Pts',(52.9255304548883,25.5884625672894,-223.572054708453));
#227788=CARTESIAN_POINT('Ctrl Pts',(54.802606638752,28.1385356166903,-220.4289903895));
#227789=CARTESIAN_POINT('Ctrl Pts',(56.6697948095651,30.6999604033981,-217.289804946001));
#227790=CARTESIAN_POINT('Ctrl Pts',(58.5345519359632,33.2635581737269,-214.151359869686));
#227791=CARTESIAN_POINT('Ctrl Pts',(47.2098674957262,18.0858618424364,-233.021306146667));
#227792=CARTESIAN_POINT('Ctrl Pts',(48.1660577345037,19.3384804806313,-231.436445859109));
#227793=CARTESIAN_POINT('Ctrl Pts',(49.1090703108757,20.6096704873925,-229.859386110464));
#227794=CARTESIAN_POINT('Ctrl Pts',(50.0473336065433,21.8864233995054,-228.284270940977));
#227795=CARTESIAN_POINT('Ctrl Pts',(50.9855969022109,23.1631763116183,-226.709155771488));
#227796=CARTESIAN_POINT('Ctrl Pts',(51.9186177626333,24.4464108695765,-225.136458640789));
#227797=CARTESIAN_POINT('Ctrl Pts',(52.8491949026841,25.7323667348012,-223.564699625624));
#227798=CARTESIAN_POINT('Ctrl Pts',(54.7103491827856,28.3042784652506,-220.421181595292));
#227799=CARTESIAN_POINT('Ctrl Pts',(56.5618994916621,30.8869590362523,-217.281419567094));
#227800=CARTESIAN_POINT('Ctrl Pts',(58.4105543383496,33.4721882778783,-214.142529225918));
#227801=CARTESIAN_POINT('Ctrl Pts',(47.2003193864821,18.1182964298664,-233.015989564334));
#227802=CARTESIAN_POINT('Ctrl Pts',(48.1493988764852,19.3809230047756,-231.432724300644));
#227803=CARTESIAN_POINT('Ctrl Pts',(49.0877568643722,20.6584395224563,-229.855761293683));
#227804=CARTESIAN_POINT('Ctrl Pts',(50.0215848134126,21.9412987456968,-228.28073090895));
#227805=CARTESIAN_POINT('Ctrl Pts',(50.9554127624531,23.2241579689375,-226.705700524218));
#227806=CARTESIAN_POINT('Ctrl Pts',(51.8844304624717,24.5129032830703,-225.132894527219));
#227807=CARTESIAN_POINT('Ctrl Pts',(52.811027126582,25.8043188185571,-223.561022084209));
#227808=CARTESIAN_POINT('Ctrl Pts',(54.6642204548024,28.3871498895308,-220.417277198188));
#227809=CARTESIAN_POINT('Ctrl Pts',(56.5079518327106,30.9804583526794,-217.27722687764));
#227810=CARTESIAN_POINT('Ctrl Pts',(58.3485555395427,33.5765033299539,-214.138113904034));
#227811=CARTESIAN_POINT('Ctrl Pts',(47.1871564758985,18.1551125368272,-233.011717209266));
#227812=CARTESIAN_POINT('Ctrl Pts',(48.1304013675538,19.4253209084676,-231.429532035792));
#227813=CARTESIAN_POINT('Ctrl Pts',(49.0646491667038,20.7079796621986,-229.852677272917));
#227814=CARTESIAN_POINT('Ctrl Pts',(49.9946730832209,21.9956338703083,-228.277678228496));
#227815=CARTESIAN_POINT('Ctrl Pts',(50.924696999738,23.283288078418,-226.702679184075));
#227816=CARTESIAN_POINT('Ctrl Pts',(51.8503135061499,24.5763104484158,-225.129741714031));
#227817=CARTESIAN_POINT('Ctrl Pts',(52.7735535901599,25.8719374112347,-223.557730749151));
#227818=CARTESIAN_POINT('Ctrl Pts',(54.62003375818,28.4631913368726,-220.413708819391));
#227819=CARTESIAN_POINT('Ctrl Pts',(56.4572435867786,31.0646235309543,-217.273328544292));
#227820=CARTESIAN_POINT('Ctrl Pts',(58.2910871452732,33.6689870195509,-214.133955876969));
#227821=CARTESIAN_POINT('Ctrl Pts',(47.1711020320382,18.1951169691784,-233.008152197064));
#227822=CARTESIAN_POINT('Ctrl Pts',(48.1091754301695,19.471620881615,-231.426873602798));
#227823=CARTESIAN_POINT('Ctrl Pts',(49.0396359981975,20.7586423084589,-229.850155627119));
#227824=CARTESIAN_POINT('Ctrl Pts',(49.9662083070876,22.0502814645383,-228.275198729438));
#227825=CARTESIAN_POINT('Ctrl Pts',(50.8927806159777,23.3419206206176,-226.700241831756));
#227826=CARTESIAN_POINT('Ctrl Pts',(51.8153427493086,24.6384368291909,-225.12719326289));
#227827=CARTESIAN_POINT('Ctrl Pts',(52.7356127602431,25.9374582798656,-223.555055698046));
#227828=CARTESIAN_POINT('Ctrl Pts',(54.5761527821122,28.535501181215,-220.410780568357));
#227829=CARTESIAN_POINT('Ctrl Pts',(56.4077512436301,31.1433164616566,-217.270071905955));
#227830=CARTESIAN_POINT('Ctrl Pts',(58.2358086912436,33.7542064961608,-214.130435725157));
#227831=CARTESIAN_POINT('Ctrl Pts',(47.1550475881779,18.2351214015296,-233.004587184861));
#227832=CARTESIAN_POINT('Ctrl Pts',(48.0879494927851,19.5179208547626,-231.424215169804));
#227833=CARTESIAN_POINT('Ctrl Pts',(49.0146228296911,20.8093049547191,-229.847633981322));
#227834=CARTESIAN_POINT('Ctrl Pts',(49.9377435309543,22.1049290587682,-228.272719230379));
#227835=CARTESIAN_POINT('Ctrl Pts',(50.8608642322175,23.4005531628173,-226.697804479436));
#227836=CARTESIAN_POINT('Ctrl Pts',(51.7803719924673,24.7005632099661,-225.124644811749));
#227837=CARTESIAN_POINT('Ctrl Pts',(52.6976719303263,26.0029791484965,-223.55238064694));
#227838=CARTESIAN_POINT('Ctrl Pts',(54.5322718060444,28.6078110255573,-220.407852317323));
#227839=CARTESIAN_POINT('Ctrl Pts',(56.3582589004816,31.2220093923588,-217.266815267618));
#227840=CARTESIAN_POINT('Ctrl Pts',(58.1805302372139,33.8394259727705,-214.126915573344));
#227841=CARTESIAN_POINT('Ctrl Pts',(47.1344245348341,18.280247344257,-233.002416451326));
#227842=CARTESIAN_POINT('Ctrl Pts',(48.0632007737606,19.5675523920502,-231.422572450694));
#227843=CARTESIAN_POINT('Ctrl Pts',(48.9866364942849,20.8622514679632,-229.846057608697));
#227844=CARTESIAN_POINT('Ctrl Pts',(49.906818406825,22.1608591102461,-228.271124311316));
#227845=CARTESIAN_POINT('Ctrl Pts',(50.8270003193651,23.459466752529,-226.696191013934));
#227846=CARTESIAN_POINT('Ctrl Pts',(51.7438894778481,24.7620852261766,-225.12290336813));
#227847=CARTESIAN_POINT('Ctrl Pts',(52.6586605054972,26.0670146466549,-223.550499793187));
#227848=CARTESIAN_POINT('Ctrl Pts',(54.4882025607956,28.6768734876113,-220.405692643303));
#227849=CARTESIAN_POINT('Ctrl Pts',(56.3094666870994,31.2957331374271,-217.264328106627));
#227850=CARTESIAN_POINT('Ctrl Pts',(58.1268789337879,33.9179256653815,-214.124164876537));
#227851=CARTESIAN_POINT('Ctrl Pts',(47.1150642483994,18.3236858273299,-232.999295710587));
#227852=CARTESIAN_POINT('Ctrl Pts',(48.0392206238659,19.6158965079908,-231.420362484156));
#227853=CARTESIAN_POINT('Ctrl Pts',(48.9590100671071,20.9141580894346,-229.844205156969));
#227854=CARTESIAN_POINT('Ctrl Pts',(49.8759725739142,22.2158319633755,-228.269472472139));
#227855=CARTESIAN_POINT('Ctrl Pts',(50.7929350807213,23.5175058373164,-226.694739787308));
#227856=CARTESIAN_POINT('Ctrl Pts',(51.7070476323962,24.8226580511233,-225.12147447558));
#227857=CARTESIAN_POINT('Ctrl Pts',(52.6192352667853,26.1299128826243,-223.549042364026));
#227858=CARTESIAN_POINT('Ctrl Pts',(54.4436105355637,28.7444225456263,-220.404178140919));
#227859=CARTESIAN_POINT('Ctrl Pts',(56.2604448907417,31.367132192526,-217.262559371757));
#227860=CARTESIAN_POINT('Ctrl Pts',(58.0734857403641,33.9931206393803,-214.122173015364));
#227861=CARTESIAN_POINT('Ctrl Pts',(47.0957039619647,18.3671243104028,-232.996174969848));
#227862=CARTESIAN_POINT('Ctrl Pts',(48.0152404739711,19.6642406239314,-231.41815251762));
#227863=CARTESIAN_POINT('Ctrl Pts',(48.9313836399292,20.966064710906,-229.842352705242));
#227864=CARTESIAN_POINT('Ctrl Pts',(49.8451267410034,22.2708048165049,-228.267820632962));
#227865=CARTESIAN_POINT('Ctrl Pts',(50.7588698420775,23.575544922104,-226.693288560683));
#227866=CARTESIAN_POINT('Ctrl Pts',(51.6702057869443,24.8832308760699,-225.12004558303));
#227867=CARTESIAN_POINT('Ctrl Pts',(52.5798100280734,26.1928111185938,-223.547584934865));
#227868=CARTESIAN_POINT('Ctrl Pts',(54.3990185103318,28.8119716036413,-220.402663638535));
#227869=CARTESIAN_POINT('Ctrl Pts',(56.2114230943841,31.438531247625,-217.260790636888));
#227870=CARTESIAN_POINT('Ctrl Pts',(58.0200925469402,34.0683156133792,-214.120181154191));
#227871=CARTESIAN_POINT('Ctrl Pts',(47.0872924863604,18.3980576618883,-232.988186791018));
#227872=CARTESIAN_POINT('Ctrl Pts',(47.999710015843,19.7029483255535,-231.41245041461));
#227873=CARTESIAN_POINT('Ctrl Pts',(48.9104078061524,21.0102083195229,-229.837920310538));
#227874=CARTESIAN_POINT('Ctrl Pts',(49.819663384006,22.3192314144748,-228.264239293901));
#227875=CARTESIAN_POINT('Ctrl Pts',(50.7289189618596,23.6282545094267,-226.690558277265));
#227876=CARTESIAN_POINT('Ctrl Pts',(51.636732524911,24.9390441962169,-225.117729434238));
#227877=CARTESIAN_POINT('Ctrl Pts',(52.5433419461414,26.2511531262214,-223.545508348952));
#227878=CARTESIAN_POINT('Ctrl Pts',(54.3565607886023,28.8753709862302,-220.401066178378));
#227879=CARTESIAN_POINT('Ctrl Pts',(56.1649975877485,31.5047913007538,-217.259011215537));
#227880=CARTESIAN_POINT('Ctrl Pts',(57.9700993556152,34.1370914402818,-214.118198613889));
#227881=CARTESIAN_POINT('Ctrl Pts',(47.07151283755,18.4392609475024,-232.980675631547));
#227882=CARTESIAN_POINT('Ctrl Pts',(47.9784669049768,19.7494077885448,-231.40663525448));
#227883=CARTESIAN_POINT('Ctrl Pts',(48.8846403863511,21.0606622046162,-229.833271513153));
#227884=CARTESIAN_POINT('Ctrl Pts',(49.7901160730939,22.3727913382652,-228.260434083043));
#227885=CARTESIAN_POINT('Ctrl Pts',(50.6955917598367,23.6849204719142,-226.687596652933));
#227886=CARTESIAN_POINT('Ctrl Pts',(51.6003698589295,24.9979251551198,-225.115286361312));
#227887=CARTESIAN_POINT('Ctrl Pts',(52.5045272731894,26.3116209606581,-223.543390841591));
#227888=CARTESIAN_POINT('Ctrl Pts',(54.3128421017092,28.939012571735,-220.399599802148));
#227889=CARTESIAN_POINT('Ctrl Pts',(56.1186826713171,31.569141738417,-217.257449700108));
#227890=CARTESIAN_POINT('Ctrl Pts',(57.9225686339535,34.2009514305169,-214.116344107367));
#227891=CARTESIAN_POINT('Ctrl Pts',(47.0636230131447,18.4598625903094,-232.976920051811));
#227892=CARTESIAN_POINT('Ctrl Pts',(47.9678453495437,19.7726375200406,-231.403727674415));
#227893=CARTESIAN_POINT('Ctrl Pts',(48.8717566764505,21.0858891471629,-229.830947114461));
#227894=CARTESIAN_POINT('Ctrl Pts',(49.7753424176378,22.3995713001604,-228.258531477614));
#227895=CARTESIAN_POINT('Ctrl Pts',(50.6789281588252,23.713253453158,-226.686115840768));
#227896=CARTESIAN_POINT('Ctrl Pts',(51.5821885259387,25.0273656345712,-225.114064824849));
#227897=CARTESIAN_POINT('Ctrl Pts',(52.4851199367133,26.3418548778766,-223.54233208791));
#227898=CARTESIAN_POINT('Ctrl Pts',(54.2909827582626,28.9708333644873,-220.398866614033));
#227899=CARTESIAN_POINT('Ctrl Pts',(56.0955252131014,31.6013169572485,-217.256668942392));
#227900=CARTESIAN_POINT('Ctrl Pts',(57.8988032731226,34.2328814256343,-214.115416854107));
#227901=CARTESIAN_POINT('Ctrl Pts',(47.0538541139573,18.4830182871128,-232.973265811648));
#227902=CARTESIAN_POINT('Ctrl Pts',(47.955722927223,19.7978606128634,-231.400808363276));
#227903=CARTESIAN_POINT('Ctrl Pts',(48.8576105358869,21.1127453662178,-229.828584127488));
#227904=CARTESIAN_POINT('Ctrl Pts',(49.7594936036301,22.4276796074738,-228.256586850871));
#227905=CARTESIAN_POINT('Ctrl Pts',(50.6613766713732,23.7426138487298,-226.684589574255));
#227906=CARTESIAN_POINT('Ctrl Pts',(51.5632551884987,25.0575975968797,-225.112819267293));
#227907=CARTESIAN_POINT('Ctrl Pts',(52.4651047016009,26.3726371360198,-223.541268381319));
#227908=CARTESIAN_POINT('Ctrl Pts',(54.2688037278052,29.0027162143,-220.398166609371));
#227909=CARTESIAN_POINT('Ctrl Pts',(56.0723874025208,31.6330198944631,-217.255944116137));
#227910=CARTESIAN_POINT('Ctrl Pts',(57.875649653532,34.2635844996751,-214.114522751136));
#227911=CARTESIAN_POINT('Ctrl Pts',(47.0405353763693,18.5106352292473,-232.969983979348));
#227912=CARTESIAN_POINT('Ctrl Pts',(47.9405971515569,19.8268187140002,-231.398125716493));
#227913=CARTESIAN_POINT('Ctrl Pts',(48.8408986391317,21.1427526567519,-229.826381496195));
#227914=CARTESIAN_POINT('Ctrl Pts',(49.7414431123329,22.4584427038901,-228.254759191353));
#227915=CARTESIAN_POINT('Ctrl Pts',(50.6419875855342,23.7741327510283,-226.683136886512));
#227916=CARTESIAN_POINT('Ctrl Pts',(51.5427750540585,25.0895788993504,-225.111636500013));
#227917=CARTESIAN_POINT('Ctrl Pts',(52.443808131774,26.4047878990792,-223.540266455142));
#227918=CARTESIAN_POINT('Ctrl Pts',(54.2458742872048,29.0352058985368,-220.397526365399));
#227919=CARTESIAN_POINT('Ctrl Pts',(56.0489238784563,31.6646741163143,-217.255307216989));
#227920=CARTESIAN_POINT('Ctrl Pts',(57.852967529916,34.2932604357928,-214.113682169595));
#227921=CARTESIAN_POINT('Ctrl Pts',(47.0338760075754,18.5244437003147,-232.968343063198));
#227922=CARTESIAN_POINT('Ctrl Pts',(47.9330342637239,19.8412977645685,-231.396784393101));
#227923=CARTESIAN_POINT('Ctrl Pts',(48.8325426907541,21.1577563020188,-229.825280180548));
#227924=CARTESIAN_POINT('Ctrl Pts',(49.7324178666844,22.4738242520981,-228.253845361594));
#227925=CARTESIAN_POINT('Ctrl Pts',(50.6322930426146,23.7898922021775,-226.682410542641));
#227926=CARTESIAN_POINT('Ctrl Pts',(51.5325349868385,25.1055695505858,-225.111045116373));
#227927=CARTESIAN_POINT('Ctrl Pts',(52.4331598468605,26.4208632806089,-223.539765492053));
#227928=CARTESIAN_POINT('Ctrl Pts',(54.2344095669047,29.0514507406552,-220.397206243413));
#227929=CARTESIAN_POINT('Ctrl Pts',(56.0371921164241,31.6805012272399,-217.254988767415));
#227930=CARTESIAN_POINT('Ctrl Pts',(57.8416264681079,34.3080984038517,-214.113261878824));
#227931=CARTESIAN_POINT('Ctrl Pts',(47.0263410003839,18.5393529178172,-232.966789761807));
#227932=CARTESIAN_POINT('Ctrl Pts',(47.9247284510372,19.856700801254,-231.395498625619));
#227933=CARTESIAN_POINT('Ctrl Pts',(48.8235505406218,21.1735412519938,-229.824216617793));
#227934=CARTESIAN_POINT('Ctrl Pts',(49.7228457883083,22.4898650532266,-228.252959195293));
#227935=CARTESIAN_POINT('Ctrl Pts',(50.6221410359948,23.8061888544594,-226.681701772792));
#227936=CARTESIAN_POINT('Ctrl Pts',(51.5219094725163,25.1219959484843,-225.110468904466));
#227937=CARTESIAN_POINT('Ctrl Pts',(52.4221921058014,26.4372796694717,-223.539279612374));
#227938=CARTESIAN_POINT('Ctrl Pts',(54.2227573723716,29.0678471114466,-220.396901028191));
#227939=CARTESIAN_POINT('Ctrl Pts',(56.0253786795592,31.6963162745203,-217.254692290257));
#227940=CARTESIAN_POINT('Ctrl Pts',(57.8304030425693,34.3226797077107,-214.112855014843));
#227941=CARTESIAN_POINT('Ctrl Pts',(47.0177828560111,18.5555300817996,-232.96533252157));
#227942=CARTESIAN_POINT('Ctrl Pts',(47.9155370349421,19.8731929180949,-231.394280823516));
#227943=CARTESIAN_POINT('Ctrl Pts',(48.8137913023007,21.1902606020353,-229.823202807664));
#227944=CARTESIAN_POINT('Ctrl Pts',(49.7126093236726,22.5067040125525,-228.252111396185));
#227945=CARTESIAN_POINT('Ctrl Pts',(50.6114273450444,23.8231474230696,-226.681019984706));
#227946=CARTESIAN_POINT('Ctrl Pts',(51.5108090328418,25.1389665178458,-225.109915092335));
#227947=CARTESIAN_POINT('Ctrl Pts',(52.4108279627846,26.4541313607334,-223.538814574431));
#227948=CARTESIAN_POINT('Ctrl Pts',(54.2108658226704,29.0844610465087,-220.396613538622));
#227949=CARTESIAN_POINT('Ctrl Pts',(56.0134397408495,31.7121723231175,-217.254421501589));
#227950=CARTESIAN_POINT('Ctrl Pts',(57.8192783928772,34.3370299914758,-214.112464332901));
#227951=CARTESIAN_POINT('Ctrl Pts',(47.0135037838248,18.5636186637907,-232.964603901451));
#227952=CARTESIAN_POINT('Ctrl Pts',(47.9109413268945,19.8814389765153,-231.393671922464));
#227953=CARTESIAN_POINT('Ctrl Pts',(48.8089116831402,21.1986202770561,-229.822695902599));
#227954=CARTESIAN_POINT('Ctrl Pts',(49.7074910913547,22.5151234922153,-228.251687496631));
#227955=CARTESIAN_POINT('Ctrl Pts',(50.6060704995693,23.8316267073747,-226.680679090663));
#227956=CARTESIAN_POINT('Ctrl Pts',(51.5052588130045,25.1474518025266,-225.109638186271));
#227957=CARTESIAN_POINT('Ctrl Pts',(52.4051458912763,26.4625572063643,-223.538582055459));
#227958=CARTESIAN_POINT('Ctrl Pts',(54.2049200478198,29.0927680140397,-220.396469793837));
#227959=CARTESIAN_POINT('Ctrl Pts',(56.0074702714946,31.7201003474161,-217.254286107255));
#227960=CARTESIAN_POINT('Ctrl Pts',(57.8137160680311,34.3442051333583,-214.11226899193));
#227961=CARTESIAN_POINT('Ctrl Pts',(47.0089694792463,18.5720236309689,-232.963899094952));
#227962=CARTESIAN_POINT('Ctrl Pts',(47.9061246605823,19.8899568147843,-231.393079846389));
#227963=CARTESIAN_POINT('Ctrl Pts',(48.8038406245385,21.2072131852528,-229.822201313241));
#227964=CARTESIAN_POINT('Ctrl Pts',(49.7022070147003,22.523742233991,-228.251273097427));
#227965=CARTESIAN_POINT('Ctrl Pts',(50.6005734048621,23.8402712827293,-226.680344881612));
#227966=CARTESIAN_POINT('Ctrl Pts',(51.4995899823701,25.1560729994673,-225.109366839153));
#227967=CARTESIAN_POINT('Ctrl Pts',(52.3993648097282,26.4710917806424,-223.538354716999));
#227968=CARTESIAN_POINT('Ctrl Pts',(54.1989144644443,29.1011293429925,-220.39633047269));
#227969=CARTESIAN_POINT('Ctrl Pts',(56.0014694266273,31.7280386185765,-217.25415713023));
#227970=CARTESIAN_POINT('Ctrl Pts',(57.8081784241041,34.3513225267891,-214.112077698071));
#227971=CARTESIAN_POINT('Ctrl Pts',(47.0041643855294,18.580762838696,-232.963218170749));
#227972=CARTESIAN_POINT('Ctrl Pts',(47.9010716022698,19.8987644772325,-231.392505287657));
#227973=CARTESIAN_POINT('Ctrl Pts',(48.7985636253896,21.2160564611115,-229.821719884836));
#227974=CARTESIAN_POINT('Ctrl Pts',(49.6967438426135,22.5325760511435,-228.250869035074));
#227975=CARTESIAN_POINT('Ctrl Pts',(50.5949240598375,23.8490956411754,-226.680018185312));
#227976=CARTESIAN_POINT('Ctrl Pts',(51.4937920916948,25.1648428846195,-225.10910171349));
#227977=CARTESIAN_POINT('Ctrl Pts',(52.3934756614324,26.4797462844595,-223.53813309987));
#227978=CARTESIAN_POINT('Ctrl Pts',(54.1928428009075,29.1095530841393,-220.396195872632));
#227979=CARTESIAN_POINT('Ctrl Pts',(55.9954317595172,31.7359937276413,-217.254034998605));
#227980=CARTESIAN_POINT('Ctrl Pts',(57.8026630300816,34.3583854144121,-214.111890802731));
#227981=CARTESIAN_POINT('Ctrl Pts',(46.9993592918125,18.5895020464233,-232.962537246545));
#227982=CARTESIAN_POINT('Ctrl Pts',(47.8960185439573,19.9075721396807,-231.391930728925));
#227983=CARTESIAN_POINT('Ctrl Pts',(48.7932866262407,21.2248997369702,-229.821238456431));
#227984=CARTESIAN_POINT('Ctrl Pts',(49.6912806705268,22.5414098682959,-228.250464972721));
#227985=CARTESIAN_POINT('Ctrl Pts',(50.5892747148128,23.8579199996217,-226.679691489012));
#227986=CARTESIAN_POINT('Ctrl Pts',(51.4879942010195,25.1736127697718,-225.108836587826));
#227987=CARTESIAN_POINT('Ctrl Pts',(52.3875865131366,26.4884007882765,-223.537911482743));
#227988=CARTESIAN_POINT('Ctrl Pts',(54.1867711373708,29.117976825286,-220.396061272575));
#227989=CARTESIAN_POINT('Ctrl Pts',(55.9893940924071,31.7439488367061,-217.25391286698));
#227990=CARTESIAN_POINT('Ctrl Pts',(57.7971476360592,34.365448302035,-214.11170390739));
#227991=CARTESIAN_POINT('Ctrl Pts',(46.9913120403997,18.6016320696042,-232.962809737275));
#227992=CARTESIAN_POINT('Ctrl Pts',(47.8881017068652,19.919347208754,-231.392174086571));
#227993=CARTESIAN_POINT('Ctrl Pts',(48.7854927208081,21.2363283107576,-229.821456748291));
#227994=CARTESIAN_POINT('Ctrl Pts',(49.6835984491062,22.5525036430274,-228.250662893886));
#227995=CARTESIAN_POINT('Ctrl Pts',(50.5817041774044,23.8686789752972,-226.679869039482));
#227996=CARTESIAN_POINT('Ctrl Pts',(51.480524130202,25.1840486327538,-225.108998471456));
#227997=CARTESIAN_POINT('Ctrl Pts',(52.3802004849816,26.4985292873713,-223.538062914284));
#227998=CARTESIAN_POINT('Ctrl Pts',(54.1795531945409,29.1274905966065,-220.396191799938));
#227999=CARTESIAN_POINT('Ctrl Pts',(55.9822813208348,31.7529097593695,-217.254043978496));
#228000=CARTESIAN_POINT('Ctrl Pts',(57.7900093367969,34.3739628192697,-214.111856605281));
#228001=CARTESIAN_POINT('Ctrl Pts',(46.9840049393815,18.6129810161854,-232.962872244472));
#228002=CARTESIAN_POINT('Ctrl Pts',(47.8808382771992,19.9304390734321,-231.392237704844));
#228003=CARTESIAN_POINT('Ctrl Pts',(48.7782728428765,21.247161929372,-229.821521522905));
#228004=CARTESIAN_POINT('Ctrl Pts',(49.6764219919997,22.5630778387597,-228.250728876356));
#228005=CARTESIAN_POINT('Ctrl Pts',(50.5745711411229,23.8789937481474,-226.679936229808));
#228006=CARTESIAN_POINT('Ctrl Pts',(51.4734343837544,25.1941028059552,-225.109066921118));
#228007=CARTESIAN_POINT('Ctrl Pts',(52.3731538889575,26.508321667889,-223.538132682591));
#228008=CARTESIAN_POINT('Ctrl Pts',(54.1725928993637,29.1367593917566,-220.396264205537));
#228009=CARTESIAN_POINT('Ctrl Pts',(55.9754067618462,31.7616502024816,-217.254119255235));
#228010=CARTESIAN_POINT('Ctrl Pts',(57.7832199428974,34.3821699572177,-214.111935079921));
#228011=CARTESIAN_POINT('',(47.0649767742812,18.6816981840219,-232.850050031414));
#228012=CARTESIAN_POINT('',(47.5797438888055,17.1282946860168,-232.850050025775));
#228013=CARTESIAN_POINT('Ctrl Pts',(47.0649772746806,18.681698503234,-232.85005));
#228014=CARTESIAN_POINT('Ctrl Pts',(47.0894454875514,18.6433419440303,-232.85005));
#228015=CARTESIAN_POINT('Ctrl Pts',(47.1308648548305,18.5779811902918,-232.850050000004));
#228016=CARTESIAN_POINT('Ctrl Pts',(47.1945089631974,18.4622232724225,-232.850050000004));
#228017=CARTESIAN_POINT('Ctrl Pts',(47.228457737075,18.3956815601865,-232.850049999972));
#228018=CARTESIAN_POINT('Ctrl Pts',(47.2942811083109,18.2644664453497,-232.850049999972));
#228019=CARTESIAN_POINT('Ctrl Pts',(47.3292660641502,18.1888432668772,-232.850050000077));
#228020=CARTESIAN_POINT('Ctrl Pts',(47.3838144288267,18.0534939114453,-232.850050000077));
#228021=CARTESIAN_POINT('Ctrl Pts',(47.4061285795857,17.9946070609481,-232.850050000004));
#228022=CARTESIAN_POINT('Ctrl Pts',(47.4807135149771,17.7819049672691,-232.850050000004));
#228023=CARTESIAN_POINT('Ctrl Pts',(47.5062786117714,17.6714141232655,-232.850050000232));
#228024=CARTESIAN_POINT('Ctrl Pts',(47.5414163429777,17.4969266356066,-232.850050000232));
#228025=CARTESIAN_POINT('Ctrl Pts',(47.5518232649238,17.4292236058328,-232.85005));
#228026=CARTESIAN_POINT('Ctrl Pts',(47.5744421319946,17.2492890927419,-232.85005));
#228027=CARTESIAN_POINT('Ctrl Pts',(47.5778246725068,17.1749507868806,-232.85005));
#228028=CARTESIAN_POINT('Ctrl Pts',(47.5797441362696,17.1282946961977,-232.85005));
#228029=CARTESIAN_POINT('',(59.5744430571196,28.6979747816085,-214.56059856522));
#228030=CARTESIAN_POINT('Ctrl Pts',(59.574442786197,28.6979745676233,-214.560598252186));
#228031=CARTESIAN_POINT('Ctrl Pts',(55.5761465166848,24.8416079159137,-220.657162906121));
#228032=CARTESIAN_POINT('Ctrl Pts',(51.5778799971752,20.9851500975526,-226.753689417593));
#228033=CARTESIAN_POINT('Ctrl Pts',(47.5797437329671,17.1282947147807,-232.85004994177));
#228034=CARTESIAN_POINT('',(59.5599473199192,29.0716011550534,-214.548757454512));
#228035=CARTESIAN_POINT('Ctrl Pts',(59.5599473199158,29.0716011550592,-214.548757454608));
#228036=CARTESIAN_POINT('Ctrl Pts',(59.562335847696,29.0094631058834,-214.552626620787));
#228037=CARTESIAN_POINT('Ctrl Pts',(59.5647394386419,28.9472090864927,-214.555583575921));
#228038=CARTESIAN_POINT('Ctrl Pts',(59.5683821822733,28.8533107884066,-214.558574296067));
#228039=CARTESIAN_POINT('Ctrl Pts',(59.5696089211159,28.8217653832972,-214.559329741406));
#228040=CARTESIAN_POINT('Ctrl Pts',(59.5720174159227,28.7599810676142,-214.560318279807));
#228041=CARTESIAN_POINT('Ctrl Pts',(59.5727190081475,28.7420025676916,-214.5605526967));
#228042=CARTESIAN_POINT('Ctrl Pts',(59.5744429767042,28.6979747794677,-214.560599513176));
#228043=CARTESIAN_POINT('',(57.6802384108496,34.1916869461204,-214.317651786459));
#228044=CARTESIAN_POINT('Ctrl Pts',(57.6802384405887,34.1916869762635,-214.317652096406));
#228045=CARTESIAN_POINT('Ctrl Pts',(57.7110766561566,34.1523839012924,-214.318515520258));
#228046=CARTESIAN_POINT('Ctrl Pts',(57.7444787489014,34.1091244865649,-214.319516304846));
#228047=CARTESIAN_POINT('Ctrl Pts',(57.8155385849077,34.0150346366398,-214.321768181642));
#228048=CARTESIAN_POINT('Ctrl Pts',(57.8508234071893,33.9673227106139,-214.32296093355));
#228049=CARTESIAN_POINT('Ctrl Pts',(57.9661234018469,33.8080831440916,-214.32727701056));
#228050=CARTESIAN_POINT('Ctrl Pts',(58.0434074298077,33.6958767305193,-214.331195699283));
#228051=CARTESIAN_POINT('Ctrl Pts',(58.1756532244486,33.4942246550505,-214.338033936497));
#228052=CARTESIAN_POINT('Ctrl Pts',(58.2321817369315,33.4045586829631,-214.340952245207));
#228053=CARTESIAN_POINT('Ctrl Pts',(58.3756461183976,33.1676840614643,-214.348689659444));
#228054=CARTESIAN_POINT('Ctrl Pts',(58.4602479257748,33.018425566341,-214.353756590895));
#228055=CARTESIAN_POINT('Ctrl Pts',(58.6568844792401,32.6464976653534,-214.368544945655));
#228056=CARTESIAN_POINT('Ctrl Pts',(58.7646217839372,32.420153660951,-214.377793138464));
#228057=CARTESIAN_POINT('Ctrl Pts',(58.9195386090982,32.0554702584067,-214.392846705455));
#228058=CARTESIAN_POINT('Ctrl Pts',(58.9732785720272,31.919705788645,-214.398754579606));
#228059=CARTESIAN_POINT('Ctrl Pts',(59.1078149579066,31.553570829642,-214.415391307452));
#228060=CARTESIAN_POINT('Ctrl Pts',(59.1824588553372,31.3211191066135,-214.426591762045));
#228061=CARTESIAN_POINT('Ctrl Pts',(59.2717173594831,30.9979484732622,-214.442018247785));
#228062=CARTESIAN_POINT('Ctrl Pts',(59.2947355260367,30.9092561462818,-214.446284061645));
#228063=CARTESIAN_POINT('Ctrl Pts',(59.3544699104682,30.6634680434043,-214.458293748763));
#228064=CARTESIAN_POINT('Ctrl Pts',(59.388219665549,30.5059342511955,-214.466398394895));
#228065=CARTESIAN_POINT('Ctrl Pts',(59.459087253972,30.1244208307842,-214.487274531045));
#228066=CARTESIAN_POINT('Ctrl Pts',(59.4920723938872,29.8990070152647,-214.499666866016));
#228067=CARTESIAN_POINT('Ctrl Pts',(59.5376880887883,29.4727426573021,-214.524039704182));
#228068=CARTESIAN_POINT('Ctrl Pts',(59.552234017423,29.272264329899,-214.536262708201));
#228069=CARTESIAN_POINT('Ctrl Pts',(59.559947319918,29.0716011550591,-214.548757454604));
#228070=CARTESIAN_POINT('Ctrl Pts',(47.064976549062,18.6816980304454,-232.850049773951));
#228071=CARTESIAN_POINT('Ctrl Pts',(48.8271464669406,21.2716316239801,-229.763684175805));
#228072=CARTESIAN_POINT('Ctrl Pts',(50.5916241034348,23.8587402441049,-226.676997721226));
#228073=CARTESIAN_POINT('Ctrl Pts',(54.1292220261611,29.0291984552365,-220.499446390719));
#228074=CARTESIAN_POINT('Ctrl Pts',(55.9023301608819,31.6125420406575,-217.408571384037));
#228075=CARTESIAN_POINT('Ctrl Pts',(57.680238354192,34.1916868896098,-214.317651706715));
#228076=CARTESIAN_POINT('Origin',(41.5452362233251,-63.7990866568863,-205.306318983907));
#228077=CARTESIAN_POINT('',(47.2772325636527,-70.8123207858077,-202.84995));
#228078=CARTESIAN_POINT('',(41.9017397792002,-72.8497297394107,-202.84995));
#228079=CARTESIAN_POINT('Origin',(41.5452362233251,-63.7990866568863,-202.84995));
#228080=CARTESIAN_POINT('',(47.1516276096017,-70.6586401308144,-214.220867040027));
#228081=CARTESIAN_POINT('',(47.250099122033,-70.7791223733342,-205.306318983907));
#228082=CARTESIAN_POINT('Ctrl Pts',(47.1516276096073,-70.658640130818,-214.220867039664));
#228083=CARTESIAN_POINT('Ctrl Pts',(47.1049465298329,-70.6968004924595,
-214.220539579083));
#228084=CARTESIAN_POINT('Ctrl Pts',(47.0581254645249,-70.7342797725841,
-214.220714572147));
#228085=CARTESIAN_POINT('Ctrl Pts',(46.9626662222936,-70.8090665014228,
-214.222095580797));
#228086=CARTESIAN_POINT('Ctrl Pts',(46.9147757072848,-70.845791160474,-214.22327290135));
#228087=CARTESIAN_POINT('Ctrl Pts',(46.8664918175106,-70.8820283127247,
-214.224988432219));
#228088=CARTESIAN_POINT('',(41.9000522051254,-72.8068868830794,-205.306318983907));
#228089=CARTESIAN_POINT('Origin',(0.,-12.9675000200281,-205.306318983907));
#228090=CARTESIAN_POINT('Ctrl Pts',(50.9302694868398,-67.3511117059353,
-214.24934096937));
#228091=CARTESIAN_POINT('Ctrl Pts',(50.6301450874053,-67.6322327827628,
-214.247062743179));
#228092=CARTESIAN_POINT('Ctrl Pts',(50.3277270489376,-67.9108411525983,
-214.244646208668));
#228093=CARTESIAN_POINT('Ctrl Pts',(49.7080810417752,-68.4722815055611,
-214.240153263142));
#228094=CARTESIAN_POINT('Ctrl Pts',(49.3907687171516,-68.7548784336109,
-214.238095007482));
#228095=CARTESIAN_POINT('Ctrl Pts',(48.439158745486,-69.5878975442323,-214.231198509906));
#228096=CARTESIAN_POINT('Ctrl Pts',(47.7996962354047,-70.1288637578719,
-214.225413141189));
#228097=CARTESIAN_POINT('Ctrl Pts',(47.1516276096073,-70.658640130818,-214.220867039664));
#228098=CARTESIAN_POINT('',(57.7103246972002,-60.4088156810276,-202.84995));
#228099=CARTESIAN_POINT('Origin',(0.,-12.9675000200281,-202.84995));
#228100=CARTESIAN_POINT('',(57.55661147574,-60.2824542804282,-214.249782619794));
#228101=CARTESIAN_POINT('',(57.677203474973,-60.3815880685163,-205.306318983907));
#228102=CARTESIAN_POINT('Ctrl Pts',(57.5566114760922,-60.2824542808246,
-214.249782589791));
#228103=CARTESIAN_POINT('Ctrl Pts',(57.0250153199809,-60.9290548756098,
-214.252086125667));
#228104=CARTESIAN_POINT('Ctrl Pts',(56.4825490095513,-61.5666907428382,
-214.255305282268));
#228105=CARTESIAN_POINT('Ctrl Pts',(55.3753515253954,-62.8244435216547,
-214.258374348072));
#228106=CARTESIAN_POINT('Ctrl Pts',(54.8117226674573,-63.4434099518073,
-214.259195881146));
#228107=CARTESIAN_POINT('Ctrl Pts',(54.2386983288856,-64.0517945375328,
-214.260116172733));
#228108=CARTESIAN_POINT('Origin',(50.7133971693864,-54.6569255427236,-205.306318983907));
#228109=CARTESIAN_POINT('',(59.7639914300581,-55.014666400457,-202.84995));
#228110=CARTESIAN_POINT('Origin',(50.7133971693864,-54.6569255427236,-202.84995));
#228111=CARTESIAN_POINT('',(59.7211488048338,-55.0129729693901,-205.306318983907));
#228112=CARTESIAN_POINT('Origin',(53.6115278221397,-57.0237333927552,-218.549922256745));
#228113=CARTESIAN_POINT('Origin',(50.7133971693864,28.7219255026674,-205.306318983907));
#228114=CARTESIAN_POINT('',(57.7103246972002,34.4738156409714,-202.84995));
#228115=CARTESIAN_POINT('',(59.7639914300583,29.0796663604006,-202.84995));
#228116=CARTESIAN_POINT('Origin',(50.7133971693864,28.7219255026674,-202.84995));
#228117=CARTESIAN_POINT('',(57.555715349607,34.3467175710979,-214.316254908503));
#228118=CARTESIAN_POINT('',(57.677203474973,34.44658802846,-205.306318983907));
#228119=CARTESIAN_POINT('Origin',(53.9184245358859,31.3368194791132,-218.66087791612));
#228120=CARTESIAN_POINT('',(59.7211488048339,29.0779729293336,-205.306318983907));
#228121=CARTESIAN_POINT('Origin',(0.,-12.9675000200281,-205.306318983907));
#228122=CARTESIAN_POINT('Ctrl Pts',(54.1218033362461,38.2387592926022,-214.333529894748));
#228123=CARTESIAN_POINT('Ctrl Pts',(54.7165719869227,37.6101910901286,-214.330972785209));
#228124=CARTESIAN_POINT('Ctrl Pts',(55.3004791816396,36.9711411157046,-214.328783039069));
#228125=CARTESIAN_POINT('Ctrl Pts',(56.4462564532789,35.6724908998646,-214.323424691429));
#228126=CARTESIAN_POINT('Ctrl Pts',(57.006890673464,35.0142562800167,-214.319260128838));
#228127=CARTESIAN_POINT('Ctrl Pts',(57.5557151719484,34.346717423436,-214.316255263493));
#228128=CARTESIAN_POINT('',(47.0132029332902,45.0921138114136,-202.84995));
#228129=CARTESIAN_POINT('Origin',(0.,-12.9675000200281,-202.84995));
#228130=CARTESIAN_POINT('',(46.8872094279775,44.936516366183,-214.320099730218));
#228131=CARTESIAN_POINT('',(46.9862210240714,45.0587921244845,-205.306318983907));
#228132=CARTESIAN_POINT('Ctrl Pts',(46.8872094285464,44.9365163666477,-214.32009968902));
#228133=CARTESIAN_POINT('Ctrl Pts',(47.5590386445095,44.3924387483626,-214.323238559856));
#228134=CARTESIAN_POINT('Ctrl Pts',(48.2215138694951,43.8365850803835,-214.326981002858));
#228135=CARTESIAN_POINT('Ctrl Pts',(49.2064774018634,42.9804492021061,-214.330624876612));
#228136=CARTESIAN_POINT('Ctrl Pts',(49.534775993172,42.6899700282977,-214.331589339685));
#228137=CARTESIAN_POINT('Ctrl Pts',(50.1777464098916,42.1108600896211,-214.333796679539));
#228138=CARTESIAN_POINT('Ctrl Pts',(50.4923590575389,41.8225600986686,-214.334966128449));
#228139=CARTESIAN_POINT('Ctrl Pts',(50.804536443953,41.5315226006458,-214.335913275952));
#228140=CARTESIAN_POINT('Origin',(41.3132181298675,38.0528376956935,-205.306318983907));
#228141=CARTESIAN_POINT('',(43.0099907914441,46.9501517582364,-202.84995));
#228142=CARTESIAN_POINT('Origin',(41.3132181298675,38.0528376956935,-202.84995));
#228143=CARTESIAN_POINT('',(43.001958811097,46.9080347125589,-205.306318983907));
#228144=CARTESIAN_POINT('Origin',(43.9075665164217,41.2822320849722,-218.664372653694));
#228145=CARTESIAN_POINT('Origin',(0.,990.91999998,-205.306318983907));
#228146=CARTESIAN_POINT('Origin',(0.,990.91999998,-202.84995));
#228147=CARTESIAN_POINT('Ctrl Pts',(41.3748964705092,-72.6655519150593,
-214.574036340781));
#228148=CARTESIAN_POINT('Ctrl Pts',(40.060737297785,-72.7166606458032,-214.574827132799));
#228149=CARTESIAN_POINT('Ctrl Pts',(38.7464886157294,-72.7653339442147,
-214.575594614694));
#228150=CARTESIAN_POINT('Ctrl Pts',(36.1178116825572,-72.8578102048044,
-214.577053530196));
#228151=CARTESIAN_POINT('Ctrl Pts',(34.8033909849928,-72.9016129087915,
-214.577744931393));
#228152=CARTESIAN_POINT('Ctrl Pts',(33.4888918292045,-72.9429801998252,
-214.57839031164));
#228153=CARTESIAN_POINT('Origin',(-476.643301415307,-33.8122127813758,-202.84995));
#228154=CARTESIAN_POINT('',(43.478316039927,49.4058943061501,-202.84995));
#228155=CARTESIAN_POINT('Origin',(0.,-178.58000002,-202.84995));
#228156=CARTESIAN_POINT('',(42.0001381210477,-75.3477925421285,-202.84995));
#228157=CARTESIAN_POINT('Origin',(0.,990.91999998,-202.84995));
#228158=CARTESIAN_POINT('',(48.8593175837476,-72.7480395125837,-202.84995));
#228159=CARTESIAN_POINT('Origin',(41.5452362233251,-63.7990866568863,-202.84995));
#228160=CARTESIAN_POINT('',(59.6415426483635,-61.9963915768841,-202.84995));
#228161=CARTESIAN_POINT('Origin',(0.,-12.9675000200281,-202.84995));
#228162=CARTESIAN_POINT('',(62.2620407574844,-55.1134062492798,-202.84995));
#228163=CARTESIAN_POINT('Origin',(50.7133971693864,-54.6569255427236,-202.84995));
#228164=CARTESIAN_POINT('',(62.2620407574844,29.1784062092233,-202.84995));
#228165=CARTESIAN_POINT('Origin',(-1004.,-12.967500020028,-202.84995));
#228166=CARTESIAN_POINT('',(59.6415426483635,36.0613915368278,-202.84995));
#228167=CARTESIAN_POINT('Origin',(50.7133971693864,28.7219255026674,-202.84995));
#228168=CARTESIAN_POINT('',(48.5864524674565,47.0350203720195,-202.84995));
#228169=CARTESIAN_POINT('Origin',(0.,-12.9675000200281,-202.84995));
#228170=CARTESIAN_POINT('Origin',(41.3132181298675,38.0528376956935,-202.84995));
#228171=CARTESIAN_POINT('Origin',(0.,-178.58000002,-202.84995));
#228172=CARTESIAN_POINT('Origin',(-1004.,-12.967500020028,-202.84995));
#228173=CARTESIAN_POINT('Origin',(-1004.,-12.967500020028,-179.606318983907));
#228174=CARTESIAN_POINT('',(62.6666822880186,29.1944003864053,-179.64995));
#228175=CARTESIAN_POINT('',(62.6666822880186,-55.1294004264619,-179.64995));
#228176=CARTESIAN_POINT('Origin',(-1004.,-12.967500020028,-179.64995));
#228177=CARTESIAN_POINT('',(62.6674432759984,29.1944304658105,-179.606318983907));
#228178=CARTESIAN_POINT('',(62.6674432759983,-55.1294305058671,-179.606318983907));
#228179=CARTESIAN_POINT('Origin',(50.7133971693864,28.7219255026673,-179.606318983907));
#228180=CARTESIAN_POINT('',(59.9543671306402,36.3185518471891,-179.64995));
#228181=CARTESIAN_POINT('Origin',(50.7133971693864,28.7219255026673,-179.64995));
#228182=CARTESIAN_POINT('',(59.9549554431411,36.3190354750184,-179.606318983907));
#228183=CARTESIAN_POINT('Origin',(0.,-12.9675000200281,-179.606318983907));
#228184=CARTESIAN_POINT('',(48.8412921507357,47.3497382103492,-179.64995));
#228185=CARTESIAN_POINT('Origin',(0.,-12.9675000200281,-179.64995));
#228186=CARTESIAN_POINT('',(48.8417714142841,47.3503300835849,-179.606318983907));
#228187=CARTESIAN_POINT('Origin',(41.3132181298675,38.0528376956935,-179.606318983907));
#228188=CARTESIAN_POINT('',(43.5541767698386,49.8036828575113,-179.64995));
#228189=CARTESIAN_POINT('Origin',(41.3132181298675,38.0528376956935,-179.64995));
#228190=CARTESIAN_POINT('',(43.5543194371113,49.8044309574546,-179.606318983907));
#228191=CARTESIAN_POINT('Origin',(0.,-178.58000002,-179.606318983907));
#228192=CARTESIAN_POINT('Origin',(0.,-178.58000002,-179.64995));
#228193=CARTESIAN_POINT('Origin',(0.,990.91999998,-179.606318983907));
#228194=CARTESIAN_POINT('',(42.0160769799045,-75.7524362554308,-179.64995));
#228195=CARTESIAN_POINT('Origin',(0.,990.91999998,-179.64995));
#228196=CARTESIAN_POINT('',(42.0161069552755,-75.7531972475156,-179.606318983907));
#228197=CARTESIAN_POINT('Origin',(41.5452362233251,-63.7990866568863,-179.606318983907));
#228198=CARTESIAN_POINT('',(49.1155884655664,-73.0615930440079,-179.64995));
#228199=CARTESIAN_POINT('Origin',(41.5452362233251,-63.7990866568863,-179.64995));
#228200=CARTESIAN_POINT('',(49.1160704206943,-73.0621827275931,-179.606318983907));
#228201=CARTESIAN_POINT('Origin',(0.,-12.9675000200281,-179.606318983907));
#228202=CARTESIAN_POINT('',(59.9543671306402,-62.2535518872453,-179.64995));
#228203=CARTESIAN_POINT('Origin',(0.,-12.9675000200281,-179.64995));
#228204=CARTESIAN_POINT('',(59.9549554431411,-62.2540355150746,-179.606318983907));
#228205=CARTESIAN_POINT('Origin',(50.7133971693864,-54.6569255427236,-179.606318983907));
#228206=CARTESIAN_POINT('Origin',(50.7133971693864,-54.6569255427236,-179.64995));
#228207=CARTESIAN_POINT('Ctrl Pts',(47.5079779560868,-40.2034134198457,
-232.959831751742));
#228208=CARTESIAN_POINT('Ctrl Pts',(51.5558271984379,-45.0119998619165,
-226.787659137649));
#228209=CARTESIAN_POINT('Ctrl Pts',(55.603839292235,-49.8201780781628,-220.615275392699));
#228210=CARTESIAN_POINT('Ctrl Pts',(59.6518858770376,-54.6282695245469,
-214.442846690034));
#228211=CARTESIAN_POINT('Ctrl Pts',(47.6083941910801,-37.6707809958978,
-232.96396511673));
#228212=CARTESIAN_POINT('Ctrl Pts',(51.6738491177805,-42.0114382175837,
-226.791891649754));
#228213=CARTESIAN_POINT('Ctrl Pts',(55.7393519427245,-46.3514436774691,
-220.61950573142));
#228214=CARTESIAN_POINT('Ctrl Pts',(59.8047170999058,-50.6912943906935,
-214.447047813144));
#228215=CARTESIAN_POINT('Ctrl Pts',(47.6970999179399,-35.0937046824551,
-232.967721023846));
#228216=CARTESIAN_POINT('Ctrl Pts',(51.7757137841176,-39.0045377390498,
-226.795568831742));
#228217=CARTESIAN_POINT('Ctrl Pts',(55.8544675412487,-42.9147019697459,
-220.623140932772));
#228218=CARTESIAN_POINT('Ctrl Pts',(59.9332050840609,-46.8246892042479,
-214.450640245293));
#228219=CARTESIAN_POINT('Ctrl Pts',(47.7724784290048,-32.4865586987341,
-232.970973990925));
#228220=CARTESIAN_POINT('Ctrl Pts',(51.8616631458841,-35.9897429718971,
-226.798709657862));
#228221=CARTESIAN_POINT('Ctrl Pts',(55.9509791745034,-39.4923578424338,
-220.626231304292));
#228222=CARTESIAN_POINT('Ctrl Pts',(60.0403077603802,-42.9948148700989,
-214.453693714461));
#228223=CARTESIAN_POINT('',(47.8511644984997,-32.6020541825672,-232.850071652983));
#228224=CARTESIAN_POINT('Ctrl Pts',(47.8511937435036,-32.6021335774055,
-232.85005));
#228225=CARTESIAN_POINT('Ctrl Pts',(47.8129987256184,-33.8832172184,-232.85005));
#228226=CARTESIAN_POINT('Ctrl Pts',(47.7712743196191,-35.1649732916759,
-232.850050000001));
#228227=CARTESIAN_POINT('Ctrl Pts',(47.6808913011582,-37.7267114902632,
-232.850050000001));
#228228=CARTESIAN_POINT('Ctrl Pts',(47.632174582744,-39.0083318774292,-232.85005));
#228229=CARTESIAN_POINT('Ctrl Pts',(47.5799752941153,-40.2889415902927,
-232.85005));
#228230=CARTESIAN_POINT('',(59.8539589593084,-46.7516609733785,-214.560268061993));
#228231=CARTESIAN_POINT('Ctrl Pts',(59.8539609358748,-46.7516610380391,
-214.560271423235));
#228232=CARTESIAN_POINT('Ctrl Pts',(59.8127437126661,-48.0499861503362,
-214.559533037022));
#228233=CARTESIAN_POINT('Ctrl Pts',(59.7691506214273,-49.3482347291554,
-214.558748583908));
#228234=CARTESIAN_POINT('Ctrl Pts',(59.6772124392584,-51.9445894630818,
-214.557078958964));
#228235=CARTESIAN_POINT('Ctrl Pts',(59.6288676637839,-53.2426846405684,
-214.556193992093));
#228236=CARTESIAN_POINT('Ctrl Pts',(59.5781472511379,-54.5406860123126,
-214.555282751789));
#228237=CARTESIAN_POINT('Ctrl Pts',(47.8511937435036,-32.6021335774055,
-232.85005));
#228238=CARTESIAN_POINT('Ctrl Pts',(49.7758731984242,-34.86623842913,-229.917938358392));
#228239=CARTESIAN_POINT('Ctrl Pts',(52.0064725897652,-37.4944438140806,
-226.519199308918));
#228240=CARTESIAN_POINT('Ctrl Pts',(55.7540093783891,-41.9130969187513,
-220.808621196108));
#228241=CARTESIAN_POINT('Ctrl Pts',(57.9042257787852,-44.4502782671364,
-217.531776078052));
#228242=CARTESIAN_POINT('Ctrl Pts',(59.8539550780058,-46.7516786353963,
-214.56027919439));
#228243=CARTESIAN_POINT('Ctrl Pts',(47.7752156818158,9.29411691894321,-232.968782926844));
#228244=CARTESIAN_POINT('Ctrl Pts',(51.8633248967382,11.8855265874929,-226.79842796189));
#228245=CARTESIAN_POINT('Ctrl Pts',(55.9515262957967,14.4763668580276,-220.627916411389));
#228246=CARTESIAN_POINT('Ctrl Pts',(60.0397300597283,17.0670490879089,-214.457361414306));
#228247=CARTESIAN_POINT('Ctrl Pts',(47.6990097155228,11.9175493678758,-232.966275794525));
#228248=CARTESIAN_POINT('Ctrl Pts',(51.7765308861555,14.9186157818217,-226.796020622489));
#228249=CARTESIAN_POINT('Ctrl Pts',(55.8541462985605,17.9190127102163,-220.625556640966));
#228250=CARTESIAN_POINT('Ctrl Pts',(59.9317344440901,20.9192322601435,-214.455037317351));
#228251=CARTESIAN_POINT('Ctrl Pts',(47.6093150514154,14.5106669763354,-232.963237198889));
#228252=CARTESIAN_POINT('Ctrl Pts',(51.673625611954,17.943733161272,-226.793068881834));
#228253=CARTESIAN_POINT('Ctrl Pts',(55.7379386239558,21.3761434795959,-220.622650915033));
#228254=CARTESIAN_POINT('Ctrl Pts',(59.8021028749556,24.8083979649139,-214.45217527183));
#228255=CARTESIAN_POINT('Ctrl Pts',(47.5077687575999,17.0588630313157,-232.959797430566));
#228256=CARTESIAN_POINT('Ctrl Pts',(51.5543587613359,20.962467251341,-226.789554159174));
#228257=CARTESIAN_POINT('Ctrl Pts',(55.6010831372117,24.8656613676635,-220.619139657106));
#228258=CARTESIAN_POINT('Ctrl Pts',(59.6478359854379,28.7687682426261,-214.448688656128));
#228259=CARTESIAN_POINT('',(59.8522817881067,20.867066521038,-214.564623195848));
#228260=CARTESIAN_POINT('Ctrl Pts',(59.5744430045609,28.6979747791773,-214.56059791914));
#228261=CARTESIAN_POINT('Ctrl Pts',(59.6255523742396,27.3929948773228,-214.561350802779));
#228262=CARTESIAN_POINT('Ctrl Pts',(59.6742602842766,26.0879255239846,-214.562076913704));
#228263=CARTESIAN_POINT('Ctrl Pts',(59.7668739927674,23.4776073684025,-214.563426526322));
#228264=CARTESIAN_POINT('Ctrl Pts',(59.8107792367937,22.1723757799868,-214.564049821487));
#228265=CARTESIAN_POINT('Ctrl Pts',(59.8522829924889,20.8670665606092,-214.564626087295));
#228266=CARTESIAN_POINT('',(47.852464780151,9.39110652846466,-232.850060330938));
#228267=CARTESIAN_POINT('Ctrl Pts',(47.5797436947461,17.1282946781069,-232.85005));
#228268=CARTESIAN_POINT('Ctrl Pts',(47.6322830986107,15.8393171716267,-232.85005));
#228269=CARTESIAN_POINT('Ctrl Pts',(47.6812964150144,14.5493107491212,-232.850050000002));
#228270=CARTESIAN_POINT('Ctrl Pts',(47.7721850391674,11.9708027192356,-232.850050000002));
#228271=CARTESIAN_POINT('Ctrl Pts',(47.814119381983,10.6806307165504,-232.85005));
#228272=CARTESIAN_POINT('Ctrl Pts',(47.8524795676142,9.39114590592673,-232.85005));
#228273=CARTESIAN_POINT('Ctrl Pts',(59.8522793526707,20.8670811307954,-214.564630777766));
#228274=CARTESIAN_POINT('Ctrl Pts',(57.9231697045554,19.0197027185266,-217.504721750272));
#228275=CARTESIAN_POINT('Ctrl Pts',(55.7588763923175,16.9478031006038,-220.803046854349));
#228276=CARTESIAN_POINT('Ctrl Pts',(52.0105370813373,13.3623506098877,-226.514897692767));
#228277=CARTESIAN_POINT('Ctrl Pts',(49.77648563263,11.2269580610392,-229.918931538715));
#228278=CARTESIAN_POINT('Ctrl Pts',(47.8524795676142,9.39114590592673,-232.85005));
#228279=CARTESIAN_POINT('Origin',(-1004.,-12.967500020028,-205.306318983907));
#228280=CARTESIAN_POINT('Ctrl Pts',(59.8522836403995,20.8670540894923,-214.564611698659));
#228281=CARTESIAN_POINT('Ctrl Pts',(59.8645512089436,20.5617173212634,-214.418212675891));
#228282=CARTESIAN_POINT('Ctrl Pts',(59.8766484531353,20.2499789990107,-214.285665596515));
#228283=CARTESIAN_POINT('Ctrl Pts',(59.8885301586884,19.9332173750779,-214.16622369325));
#228284=CARTESIAN_POINT('Ctrl Pts',(59.9748434130117,17.6321397659663,-213.298552017052));
#228285=CARTESIAN_POINT('Ctrl Pts',(60.0479352384608,15.1082501424152,-213.117891206253));
#228286=CARTESIAN_POINT('Ctrl Pts',(60.1030981576493,12.6512459219475,-213.346442200715));
#228287=CARTESIAN_POINT('Ctrl Pts',(60.111409107162,12.2810690290415,-213.38087612488));
#228288=CARTESIAN_POINT('Ctrl Pts',(60.119458031761,11.9059152175497,-213.425731330273));
#228289=CARTESIAN_POINT('Ctrl Pts',(60.1268679612506,11.5449119912611,-213.477614509765));
#228290=CARTESIAN_POINT('Ctrl Pts',(60.1377410433281,11.0151879614781,-213.553746147705));
#228291=CARTESIAN_POINT('Ctrl Pts',(60.1459757707366,10.5818923445005,-213.633116799817));
#228292=CARTESIAN_POINT('Ctrl Pts',(60.1532641850396,10.1814317298332,-213.714618736487));
#228293=CARTESIAN_POINT('Ctrl Pts',(60.1571763074449,9.96648086700407,-213.758365639347));
#228294=CARTESIAN_POINT('Ctrl Pts',(60.1608006466485,9.76108925215223,-213.803062347839));
#228295=CARTESIAN_POINT('Ctrl Pts',(60.1643187438617,9.5558923299876,-213.850313921784));
#228296=CARTESIAN_POINT('Ctrl Pts',(60.1647663228057,9.52978679163128,-213.856325355888));
#228297=CARTESIAN_POINT('Ctrl Pts',(60.1652121278246,9.50368446580734,-213.862379491625));
#228298=CARTESIAN_POINT('Ctrl Pts',(60.1656564875316,9.47756602057091,-213.868480820893));
#228299=CARTESIAN_POINT('Ctrl Pts',(60.1660491443594,9.45448655208617,-213.873872238157));
#228300=CARTESIAN_POINT('Ctrl Pts',(60.1664410470053,9.43139075002552,-213.879283604594));
#228301=CARTESIAN_POINT('Ctrl Pts',(60.1668339732078,9.40824978917476,-213.884647521255));
#228302=CARTESIAN_POINT('Ctrl Pts',(60.1675888932483,9.36378959540017,-213.894953090485));
#228303=CARTESIAN_POINT('Ctrl Pts',(60.1683459618837,9.3191789651953,-213.905157368098));
#228304=CARTESIAN_POINT('Ctrl Pts',(60.1691067978077,9.27432300489259,-213.91527730166));
#228305=CARTESIAN_POINT('Ctrl Pts',(60.1705954940518,9.18655519908565,-213.935078557895));
#228306=CARTESIAN_POINT('Ctrl Pts',(60.1720986097153,9.09784859398319,-213.95455921771));
#228307=CARTESIAN_POINT('Ctrl Pts',(60.1736282672258,9.00748926176066,-213.973818634937));
#228308=CARTESIAN_POINT('Ctrl Pts',(60.179215127641,8.67746442098616,-214.044160966466));
#228309=CARTESIAN_POINT('Ctrl Pts',(60.1853553620167,8.313505199782,-214.113465883361));
#228310=CARTESIAN_POINT('Ctrl Pts',(60.1914134093591,7.95361934628413,-214.171719071268));
#228311=CARTESIAN_POINT('Ctrl Pts',(60.2137472534459,6.62684950002414,-214.386477646556));
#228312=CARTESIAN_POINT('Ctrl Pts',(60.236418104203,5.27038456544939,-214.469588956065));
#228313=CARTESIAN_POINT('Ctrl Pts',(60.2591685013589,3.93463693001196,-214.381568911362));
#228314=CARTESIAN_POINT('Ctrl Pts',(60.2705679513422,3.26533923572927,-214.337465061647));
#228315=CARTESIAN_POINT('Ctrl Pts',(60.2826202444479,2.56566381509912,-214.241040503754));
#228316=CARTESIAN_POINT('Ctrl Pts',(60.292057365503,2.02427812018547,-214.137294054647));
#228317=CARTESIAN_POINT('Ctrl Pts',(60.2979421316388,1.68668276825177,-214.07260021562));
#228318=CARTESIAN_POINT('Ctrl Pts',(60.303185101195,1.38822157872398,-214.004609259439));
#228319=CARTESIAN_POINT('Ctrl Pts',(60.3084747241415,1.08920916466885,-213.927821213477));
#228320=CARTESIAN_POINT('Ctrl Pts',(60.3091581982912,1.05057365935606,-213.917899401477));
#228321=CARTESIAN_POINT('Ctrl Pts',(60.3098424352801,1.01193290476613,-213.907817486517));
#228322=CARTESIAN_POINT('Ctrl Pts',(60.3105289330055,0.97320334128505,-213.897551739282));
#228323=CARTESIAN_POINT('Ctrl Pts',(60.3112345718811,0.933393907674637,
-213.886999759185));
#228324=CARTESIAN_POINT('Ctrl Pts',(60.3119438877353,0.893513565114629,
-213.87616273221));
#228325=CARTESIAN_POINT('Ctrl Pts',(60.3126540303502,0.853391001986721,
-213.865328893283));
#228326=CARTESIAN_POINT('Ctrl Pts',(60.3142387111129,0.763857642626977,
-213.841153219592));
#228327=CARTESIAN_POINT('Ctrl Pts',(60.3158218668931,0.67301495760972,-213.817396808284));
#228328=CARTESIAN_POINT('Ctrl Pts',(60.3174186631855,0.579830242826636,
-213.793870865919));
#228329=CARTESIAN_POINT('Ctrl Pts',(60.3203923825933,0.406292017442597,
-213.750058419876));
#228330=CARTESIAN_POINT('Ctrl Pts',(60.3234151563689,0.224650876038405,
-213.706988287316));
#228331=CARTESIAN_POINT('Ctrl Pts',(60.3265631280972,0.028098083539605,
-213.664136837394));
#228332=CARTESIAN_POINT('Ctrl Pts',(60.3270570609419,-0.00274205363575723,
-213.657413226007));
#228333=CARTESIAN_POINT('Ctrl Pts',(60.3275540187065,-0.0339498222745532,
-213.650696726108));
#228334=CARTESIAN_POINT('Ctrl Pts',(60.3280542241711,-0.0655521844311571,
-213.643987602863));
#228335=CARTESIAN_POINT('Ctrl Pts',(60.3362065460935,-0.58060579349666,
-213.534642670864));
#228336=CARTESIAN_POINT('Ctrl Pts',(60.3443922093042,-1.15323528491378,
-213.43974077698));
#228337=CARTESIAN_POINT('Ctrl Pts',(60.3513604009398,-1.70571517675348,
-213.375438538189));
#228338=CARTESIAN_POINT('Ctrl Pts',(60.3631824450793,-2.64303751361287,
-213.266345111226));
#228339=CARTESIAN_POINT('Ctrl Pts',(60.3725736741095,-3.58991685287568,
-213.230688335639));
#228340=CARTESIAN_POINT('Ctrl Pts',(60.3794425164094,-4.53314772643593,
-213.26537659776));
#228341=CARTESIAN_POINT('Ctrl Pts',(60.3850857563185,-5.30807862114289,
-213.293875459232));
#228342=CARTESIAN_POINT('Ctrl Pts',(60.389031621255,-6.08056089768238,-213.369825212478));
#228343=CARTESIAN_POINT('Ctrl Pts',(60.3913108160445,-6.84593414020724,
-213.491429597462));
#228344=CARTESIAN_POINT('Ctrl Pts',(60.3924832204613,-7.23963764207369,
-213.553982179065));
#228345=CARTESIAN_POINT('Ctrl Pts',(60.393210861424,-7.65045599546225,-213.633390155684));
#228346=CARTESIAN_POINT('Ctrl Pts',(60.3934920217241,-7.992850845975,-213.708959851915));
#228347=CARTESIAN_POINT('Ctrl Pts',(60.3936603081493,-8.19778875984038,
-213.754191536544));
#228348=CARTESIAN_POINT('Ctrl Pts',(60.3936984229566,-8.38332920162743,
-213.798440546674));
#228349=CARTESIAN_POINT('Ctrl Pts',(60.393651903161,-8.56176805395002,-213.843419246263));
#228350=CARTESIAN_POINT('Ctrl Pts',(60.393645715246,-8.58550342183546,-213.849402169644));
#228351=CARTESIAN_POINT('Ctrl Pts',(60.3936379471922,-8.60911262131737,
-213.855400254366));
#228352=CARTESIAN_POINT('Ctrl Pts',(60.3936286330974,-8.63262423355807,
-213.86141955001));
#228353=CARTESIAN_POINT('Ctrl Pts',(60.3936240106306,-8.6442927477634,-213.864406849902));
#228354=CARTESIAN_POINT('Ctrl Pts',(60.3936189488047,-8.6559364513167,-213.867402543179));
#228355=CARTESIAN_POINT('Ctrl Pts',(60.3936136334464,-8.66756126923334,
-213.870397484014));
#228356=CARTESIAN_POINT('Ctrl Pts',(60.3936089954616,-8.67770465498889,
-213.873010758511));
#228357=CARTESIAN_POINT('Ctrl Pts',(60.3936043793879,-8.68783651798294,
-213.875611805623));
#228358=CARTESIAN_POINT('Ctrl Pts',(60.3935997841399,-8.69795915571535,
-213.878201268307));
#228359=CARTESIAN_POINT('Ctrl Pts',(60.3935813536366,-8.73855877228198,
-213.888587019024));
#228360=CARTESIAN_POINT('Ctrl Pts',(60.3935632575531,-8.77901001068321,
-213.898786760882));
#228361=CARTESIAN_POINT('Ctrl Pts',(60.3935454305537,-8.81946085570324,
-213.9088392194));
#228362=CARTESIAN_POINT('Ctrl Pts',(60.3935099629075,-8.89993969675756,
-213.928839054034));
#228363=CARTESIAN_POINT('Ctrl Pts',(60.3934755529649,-8.98041627708718,
-213.948259982409));
#228364=CARTESIAN_POINT('Ctrl Pts',(60.3934417749187,-9.06205842258955,
-213.967356720238));
#228365=CARTESIAN_POINT('Ctrl Pts',(60.3932951820256,-9.41637608343349,
-214.05023439862));
#228366=CARTESIAN_POINT('Ctrl Pts',(60.3931504054315,-9.80790367131028,
-214.132035127045));
#228367=CARTESIAN_POINT('Ctrl Pts',(60.3930198925774,-10.2869497542045,
-214.208627827912));
#228368=CARTESIAN_POINT('Ctrl Pts',(60.3927828642322,-11.1569598468437,
-214.34773015054));
#228369=CARTESIAN_POINT('Ctrl Pts',(60.3926877370732,-12.0336216853539,
-214.418420118334));
#228370=CARTESIAN_POINT('Ctrl Pts',(60.3927142613205,-12.9140676164264,
-214.419432663803));
#228371=CARTESIAN_POINT('Ctrl Pts',(60.3927287431374,-13.3947770850747,
-214.419985497517));
#228372=CARTESIAN_POINT('Ctrl Pts',(60.3927779546511,-13.8744234185498,
-214.399911341721));
#228373=CARTESIAN_POINT('Ctrl Pts',(60.3928549418663,-14.3538708453102,
-214.359724352712));
#228374=CARTESIAN_POINT('Ctrl Pts',(60.3929949672705,-15.2258964087699,
-214.286631705262));
#228375=CARTESIAN_POINT('Ctrl Pts',(60.393246335082,-16.1546220845523,-214.127978078364));
#228376=CARTESIAN_POINT('Ctrl Pts',(60.393432985145,-16.8311197866803,-213.976604381314));
#228377=CARTESIAN_POINT('Ctrl Pts',(60.3934565432232,-16.9165040912767,
-213.95749871722));
#228378=CARTESIAN_POINT('Ctrl Pts',(60.3934796365261,-16.9997898733473,
-213.938272995079));
#228379=CARTESIAN_POINT('Ctrl Pts',(60.3935024947112,-17.0821483260314,
-213.918723916564));
#228380=CARTESIAN_POINT('Ctrl Pts',(60.3935141968303,-17.1243112718209,
-213.908715875971));
#228381=CARTESIAN_POINT('Ctrl Pts',(60.3935258376588,-17.1662309100972,
-213.898622064381));
#228382=CARTESIAN_POINT('Ctrl Pts',(60.3935374491214,-17.2080633558844,
-213.888408909728));
#228383=CARTESIAN_POINT('Ctrl Pts',(60.393543288067,-17.2290992392794,-213.883273117969));
#228384=CARTESIAN_POINT('Ctrl Pts',(60.393549119591,-17.2501130687725,-213.878107082029));
#228385=CARTESIAN_POINT('Ctrl Pts',(60.393554947749,-17.2711246845471,-213.872906131118));
#228386=CARTESIAN_POINT('Ctrl Pts',(60.3935615224738,-17.2948278156789,
-213.867038956371));
#228387=CARTESIAN_POINT('Ctrl Pts',(60.3935675567513,-17.3185350501925,
-213.861156493035));
#228388=CARTESIAN_POINT('Ctrl Pts',(60.3935716543076,-17.3422928483403,
-213.855327567938));
#228389=CARTESIAN_POINT('Ctrl Pts',(60.3936041243251,-17.5305553343437,
-213.80913776858));
#228390=CARTESIAN_POINT('Ctrl Pts',(60.3935458845432,-17.7216373314267,
-213.76477468205));
#228391=CARTESIAN_POINT('Ctrl Pts',(60.3933602461435,-17.9298338823286,
-213.719802565618));
#228392=CARTESIAN_POINT('Ctrl Pts',(60.39306103192,-18.26540760757,-213.64731596304));
#228393=CARTESIAN_POINT('Ctrl Pts',(60.3923553391731,-18.6775129550453,
-213.567607646044));
#228394=CARTESIAN_POINT('Ctrl Pts',(60.3910564967462,-19.1075296034981,
-213.499906653704));
#228395=CARTESIAN_POINT('Ctrl Pts',(60.3887092138914,-19.8846605974914,
-213.377556647813));
#228396=CARTESIAN_POINT('Ctrl Pts',(60.3846983903845,-20.6691345815781,
-213.299096394904));
#228397=CARTESIAN_POINT('Ctrl Pts',(60.3789612071656,-21.4554845530463,
-213.268525469849));
#228398=CARTESIAN_POINT('Ctrl Pts',(60.3679012957514,-22.9713784495681,
-213.209592068205));
#228399=CARTESIAN_POINT('Ctrl Pts',(60.3502984944823,-24.5000103406799,
-213.329130293887));
#228400=CARTESIAN_POINT('Ctrl Pts',(60.3264857554362,-25.9796130521886,
-213.6570101885));
#228401=CARTESIAN_POINT('Ctrl Pts',(60.3234504544022,-26.1682112487886,
-213.698803540421));
#228402=CARTESIAN_POINT('Ctrl Pts',(60.3204565330099,-26.3472746066277,
-213.742037759624));
#228403=CARTESIAN_POINT('Ctrl Pts',(60.3175367315417,-26.516649532719,-213.78578065973));
#228404=CARTESIAN_POINT('Ctrl Pts',(60.3159762978469,-26.6071688178879,
-213.8091582407));
#228405=CARTESIAN_POINT('Ctrl Pts',(60.3144291687252,-26.6953838659096,
-213.832796220738));
#228406=CARTESIAN_POINT('Ctrl Pts',(60.3128853379364,-26.7820351410228,
-213.856805411057));
#228407=CARTESIAN_POINT('Ctrl Pts',(60.3124915944157,-26.8041349581722,
-213.862928791414));
#228408=CARTESIAN_POINT('Ctrl Pts',(60.3120980566698,-26.8261330430226,
-213.86907659917));
#228409=CARTESIAN_POINT('Ctrl Pts',(60.311704540284,-26.8480416873385,-213.875251256029));
#228410=CARTESIAN_POINT('Ctrl Pts',(60.3115355397114,-26.8574506308241,
-213.877903040255));
#228411=CARTESIAN_POINT('Ctrl Pts',(60.3113666893836,-26.8668457943141,
-213.880549365385));
#228412=CARTESIAN_POINT('Ctrl Pts',(60.311198146228,-26.8762313719384,-213.883178158384));
#228413=CARTESIAN_POINT('Ctrl Pts',(60.3110325273771,-26.8854541052786,
-213.88576134056));
#228414=CARTESIAN_POINT('Ctrl Pts',(60.3108671528631,-26.8946666125183,
-213.888331312463));
#228415=CARTESIAN_POINT('Ctrl Pts',(60.3107020058,-26.9038697912027,-213.890888412478));
#228416=CARTESIAN_POINT('Ctrl Pts',(60.3100371478399,-26.9409204446891,
-213.901182923738));
#228417=CARTESIAN_POINT('Ctrl Pts',(60.3093759742381,-26.9778199604901,
-213.911268999765));
#228418=CARTESIAN_POINT('Ctrl Pts',(60.308717400326,-27.0146264313552,-213.921167211129));
#228419=CARTESIAN_POINT('Ctrl Pts',(60.3034328975206,-27.3099674628848,
-214.000592048285));
#228420=CARTESIAN_POINT('Ctrl Pts',(60.2983146403093,-27.5991766863688,
-214.068573069905));
#228421=CARTESIAN_POINT('Ctrl Pts',(60.2928256973098,-27.9124538529063,
-214.131004935625));
#228422=CARTESIAN_POINT('Ctrl Pts',(60.2839179962428,-28.420853985854,-214.23232214678));
#228423=CARTESIAN_POINT('Ctrl Pts',(60.2740350908593,-28.9922802878306,
-214.323849549145));
#228424=CARTESIAN_POINT('Ctrl Pts',(60.2607587673069,-29.7735994708971,
-214.377595134823));
#228425=CARTESIAN_POINT('Ctrl Pts',(60.2541200133809,-30.1642939107765,
-214.404470324819));
#228426=CARTESIAN_POINT('Ctrl Pts',(60.2465848770941,-30.6109031181337,
-214.418187345506));
#228427=CARTESIAN_POINT('Ctrl Pts',(60.2393799757732,-31.0395548240251,
-214.41394184185));
#228428=CARTESIAN_POINT('Ctrl Pts',(60.2238711390327,-31.9622446748815,
-214.404803226323));
#228429=CARTESIAN_POINT('Ctrl Pts',(60.2084782565981,-32.8840406813232,
-214.32066535048));
#228430=CARTESIAN_POINT('Ctrl Pts',(60.1931159963307,-33.7953694742733,
-214.178967256063));
#228431=CARTESIAN_POINT('Ctrl Pts',(60.1870407676876,-34.1557676637223,
-214.122930689379));
#228432=CARTESIAN_POINT('Ctrl Pts',(60.1809699443647,-34.5145264949527,
-214.05797839233));
#228433=CARTESIAN_POINT('Ctrl Pts',(60.1749016871999,-34.8710225250701,
-213.985271624848));
#228434=CARTESIAN_POINT('Ctrl Pts',(60.1733510559208,-34.962118515264,-213.96669275042));
#228435=CARTESIAN_POINT('Ctrl Pts',(60.1718496862809,-35.0501934642886,
-213.948229706883));
#228436=CARTESIAN_POINT('Ctrl Pts',(60.1702373704645,-35.144617230878,-213.927869919498));
#228437=CARTESIAN_POINT('Ctrl Pts',(60.1694999096097,-35.1878059355439,
-213.918557509327));
#228438=CARTESIAN_POINT('Ctrl Pts',(60.1687161169395,-35.2336749127147,
-213.908549231463));
#228439=CARTESIAN_POINT('Ctrl Pts',(60.1678875012017,-35.2821213266032,
-213.897823414987));
#228440=CARTESIAN_POINT('Ctrl Pts',(60.1675039091746,-35.3045486801578,
-213.892858100551));
#228441=CARTESIAN_POINT('Ctrl Pts',(60.1671107108273,-35.3275283964064,
-213.887738985336));
#228442=CARTESIAN_POINT('Ctrl Pts',(60.1667080521215,-35.3510503623432,
-213.882463780837));
#228443=CARTESIAN_POINT('Ctrl Pts',(60.1665110501776,-35.36255855265,-213.879882871679));
#228444=CARTESIAN_POINT('Ctrl Pts',(60.1663118308306,-35.3741960784182,
-213.877262456815));
#228445=CARTESIAN_POINT('Ctrl Pts',(60.1661102633079,-35.385963215018,-213.874608964427));
#228446=CARTESIAN_POINT('Ctrl Pts',(60.1658814425207,-35.3993213464457,
-213.871596702288));
#228447=CARTESIAN_POINT('Ctrl Pts',(60.1656492765433,-35.4128496429707,
-213.868556305922));
#228448=CARTESIAN_POINT('Ctrl Pts',(60.1654137561779,-35.4265466933703,
-213.865488895693));
#228449=CARTESIAN_POINT('Ctrl Pts',(60.1622181589696,-35.6123915817958,
-213.823869532767));
#228450=CARTESIAN_POINT('Ctrl Pts',(60.1584061287036,-35.8293021918035,
-213.77724655845));
#228451=CARTESIAN_POINT('Ctrl Pts',(60.1539472537289,-36.0737459393782,
-213.728630617293));
#228452=CARTESIAN_POINT('Ctrl Pts',(60.1418239904513,-36.7383655856395,
-213.596448428404));
#228453=CARTESIAN_POINT('Ctrl Pts',(60.1249235460784,-37.60627443831,-213.44889762005));
#228454=CARTESIAN_POINT('Ctrl Pts',(60.1024025775608,-38.6088068260868,
-213.355157950907));
#228455=CARTESIAN_POINT('Ctrl Pts',(60.0855450330225,-39.3592290099679,
-213.284991312808));
#228456=CARTESIAN_POINT('Ctrl Pts',(60.0650589990151,-40.201475398557,-213.246373506945));
#228457=CARTESIAN_POINT('Ctrl Pts',(60.0426804011851,-41.0361098556587,
-213.267082162192));
#228458=CARTESIAN_POINT('Ctrl Pts',(59.9898111721685,-43.0079259896632,
-213.316006167403));
#228459=CARTESIAN_POINT('Ctrl Pts',(59.9251807248048,-44.9966985869325,
-213.673380572917));
#228460=CARTESIAN_POINT('Ctrl Pts',(59.8539617334964,-46.7516465273356,
-214.56025213689));
#228461=CARTESIAN_POINT('Ctrl Pts',(27.7161624394018,36.671894066742,-232.960596901862));
#228462=CARTESIAN_POINT('Ctrl Pts',(32.6826602701726,40.0809702013776,-226.781662197074));
#228463=CARTESIAN_POINT('Ctrl Pts',(37.6596812128995,43.4862512150987,-220.609204852275));
#228464=CARTESIAN_POINT('Ctrl Pts',(42.6390550299281,46.8908628802244,-214.438294417841));
#228465=CARTESIAN_POINT('Ctrl Pts',(25.7658626658342,36.9296719371149,-232.9601933409));
#228466=CARTESIAN_POINT('Ctrl Pts',(30.3639150200345,40.4303260414807,-226.78272680046));
#228467=CARTESIAN_POINT('Ctrl Pts',(34.9732667504195,43.9421267939794,-220.610591760459));
#228468=CARTESIAN_POINT('Ctrl Pts',(39.587510189865,47.4674439422847,-214.439830103812));
#228469=CARTESIAN_POINT('Ctrl Pts',(23.8044899907809,37.1610589494743,-232.959868581815));
#228470=CARTESIAN_POINT('Ctrl Pts',(28.0381839166385,40.7424490125755,-226.783608200302));
#228471=CARTESIAN_POINT('Ctrl Pts',(32.283433258083,44.3482400615009,-220.611766381486));
#228472=CARTESIAN_POINT('Ctrl Pts',(36.5352279127207,47.9802021638173,-214.441141334719));
#228473=CARTESIAN_POINT('Ctrl Pts',(21.8343359993853,37.3653585113446,-232.959639066595));
#228474=CARTESIAN_POINT('Ctrl Pts',(25.7068670980457,41.0171742382378,-226.784363424386));
#228475=CARTESIAN_POINT('Ctrl Pts',(29.5908265861273,44.7050007481411,-220.612769983421));
#228476=CARTESIAN_POINT('Ctrl Pts',(33.4823003440903,48.4301227180298,-214.442258946369));
#228477=CARTESIAN_POINT('Origin',(0.081845539031451,-172.6064917085,-232.850229531936));
#228478=CARTESIAN_POINT('Ctrl Pts',(33.4676030960081,48.3558410747994,-214.551991263944));
#228479=CARTESIAN_POINT('Ctrl Pts',(34.9861734114818,48.1318948267819,-214.55162202599));
#228480=CARTESIAN_POINT('Ctrl Pts',(36.5024600851346,47.8927123421817,-214.551192124635));
#228481=CARTESIAN_POINT('Ctrl Pts',(39.5300010313928,47.3839475975032,-214.550248247582));
#228482=CARTESIAN_POINT('Ctrl Pts',(41.0411838620008,47.1143772812309,-214.549734342172));
#228483=CARTESIAN_POINT('Ctrl Pts',(42.5495440258949,46.8296601163999,-214.549225394084));
#228484=CARTESIAN_POINT('Origin',(0.,-178.58000002,-205.306318983907));
#228485=CARTESIAN_POINT('Origin',(-296.501483394397,-25.4138432731711,-232.85005));
#228486=CARTESIAN_POINT('',(47.6963129678558,-31.8956500568736,-232.849931336942));
#228487=CARTESIAN_POINT('Origin',(-636.934816028482,-11.5034818258361,-232.85005));
#228488=CARTESIAN_POINT('Origin',(7.14692237356698E-14,623.509175991979,
-232.85005));
#228489=CARTESIAN_POINT('Origin',(0.0517782016034563,643.799970559412,-232.855108208931));
#228490=CARTESIAN_POINT('Ctrl Pts',(47.0825541999675,-41.7715518943956,
-232.85005));
#228491=CARTESIAN_POINT('Ctrl Pts',(46.9318448322354,-42.007890420054,-232.85005));
#228492=CARTESIAN_POINT('Ctrl Pts',(46.7904073409416,-42.2260229336685,
-232.85005));
#228493=CARTESIAN_POINT('Ctrl Pts',(46.4935676457423,-42.6770301148581,
-232.85005));
#228494=CARTESIAN_POINT('Ctrl Pts',(46.3418104287774,-42.9039683373476,
-232.85005));
#228495=CARTESIAN_POINT('Ctrl Pts',(45.8752836487346,-43.5906554858084,
-232.85005));
#228496=CARTESIAN_POINT('Ctrl Pts',(45.5551891811445,-44.0469551838861,
-232.85005));
#228497=CARTESIAN_POINT('Ctrl Pts',(44.5502158895002,-45.4345413296961,
-232.85005));
#228498=CARTESIAN_POINT('Ctrl Pts',(43.8423500925479,-46.3501756007396,
-232.85005));
#228499=CARTESIAN_POINT('Ctrl Pts',(41.5657247068443,-49.1071648985416,
-232.85005));
#228500=CARTESIAN_POINT('Ctrl Pts',(39.8686235209266,-50.9065939957913,
-232.85005));
#228501=CARTESIAN_POINT('Ctrl Pts',(36.3067467195521,-54.2094198597324,
-232.85005));
#228502=CARTESIAN_POINT('Ctrl Pts',(34.3620921324372,-55.7799933590787,
-232.85005));
#228503=CARTESIAN_POINT('Ctrl Pts',(29.6879676367398,-59.0721262304426,
-232.85005));
#228504=CARTESIAN_POINT('Ctrl Pts',(27.4993652273042,-60.2539775291619,
-232.85005));
#228505=CARTESIAN_POINT('Ctrl Pts',(26.5827048610814,-60.7443921296953,
-232.85005));
#228506=CARTESIAN_POINT('Ctrl Pts',(47.6963552853062,-31.896163686755,-232.85005));
#228507=CARTESIAN_POINT('Ctrl Pts',(47.7198209970693,-32.0141643773227,
-232.85005));
#228508=CARTESIAN_POINT('Ctrl Pts',(47.7444480612295,-32.1319277281135,
-232.850050000009));
#228509=CARTESIAN_POINT('Ctrl Pts',(47.7960571707317,-32.3672278207787,
-232.850050000009));
#228510=CARTESIAN_POINT('Ctrl Pts',(47.8230417127431,-32.4847512555908,
-232.85005));
#228511=CARTESIAN_POINT('Ctrl Pts',(47.8511636801433,-32.6020082275363,
-232.85005));
#228512=CARTESIAN_POINT('Ctrl Pts',(20.5341645416114,-61.1949426407512,
-232.965861592748));
#228513=CARTESIAN_POINT('Ctrl Pts',(24.8619705593691,-65.1326290782542,
-226.800008788317));
#228514=CARTESIAN_POINT('Ctrl Pts',(29.1902811104598,-69.0724625871147,
-220.634368994467));
#228515=CARTESIAN_POINT('Ctrl Pts',(33.5187281767876,-73.0145710177392,
-214.468761046583));
#228516=CARTESIAN_POINT('Ctrl Pts',(22.115564575717,-61.1500631726904,-232.964012351071));
#228517=CARTESIAN_POINT('Ctrl Pts',(26.7965523266534,-65.0759017171342,
-226.798067164761));
#228518=CARTESIAN_POINT('Ctrl Pts',(31.4781225651976,-69.0031581792391,
-220.632397171727));
#228519=CARTESIAN_POINT('Ctrl Pts',(36.1598241774431,-72.9319991467586,
-214.466766784373));
#228520=CARTESIAN_POINT('Ctrl Pts',(23.6900699183709,-61.1001919234539,
-232.961968408598));
#228521=CARTESIAN_POINT('Ctrl Pts',(28.7297131786069,-65.012574288375,-226.795902612053));
#228522=CARTESIAN_POINT('Ctrl Pts',(33.7700272351411,-68.9255509631158,
-220.630194103463));
#228523=CARTESIAN_POINT('Ctrl Pts',(38.8104606792061,-72.8393402290212,
-214.464534772546));
#228524=CARTESIAN_POINT('Ctrl Pts',(25.2562521239792,-61.0455007230049,
-232.959725695103));
#228525=CARTESIAN_POINT('Ctrl Pts',(30.6613188291079,-64.9426708583199,
-226.793511106062));
#228526=CARTESIAN_POINT('Ctrl Pts',(36.0671479350067,-68.8395145916166,
-220.627759071707));
#228527=CARTESIAN_POINT('Ctrl Pts',(41.4730739204624,-72.736318130574,-214.462066626483));
#228528=CARTESIAN_POINT('Origin',(0.,-12.9675000200281,-215.85005));
#228529=CARTESIAN_POINT('',(48.0827620446561,42.0414223951255,-215.85005));
#228530=CARTESIAN_POINT('Ctrl Pts',(49.1680521502591,41.0865353784011,-215.85005));
#228531=CARTESIAN_POINT('Ctrl Pts',(48.9895221708308,41.2470622045083,-215.85005));
#228532=CARTESIAN_POINT('Ctrl Pts',(48.810181579503,41.4065414287308,-215.850050000001));
#228533=CARTESIAN_POINT('Ctrl Pts',(48.4494381147294,41.7239310827547,-215.850050000001));
#228534=CARTESIAN_POINT('Ctrl Pts',(48.2659997961092,41.883627806787,-215.85005));
#228535=CARTESIAN_POINT('Ctrl Pts',(48.0827620446562,42.0414223951256,-215.85005));
#228536=CARTESIAN_POINT('',(54.6458252041307,35.5078877047659,-215.85005));
#228537=CARTESIAN_POINT('Origin',(48.892180948596,36.2913696007177,-215.85005));
#228538=CARTESIAN_POINT('Ctrl Pts',(54.6458252041307,35.5078877047659,-215.85005));
#228539=CARTESIAN_POINT('Ctrl Pts',(54.4879844434674,35.6891073117587,-215.85005));
#228540=CARTESIAN_POINT('Ctrl Pts',(54.3295470137666,35.869077059399,-215.85005));
#228541=CARTESIAN_POINT('Ctrl Pts',(54.0105884027086,36.2276517825792,-215.85005));
#228542=CARTESIAN_POINT('Ctrl Pts',(53.8480676261596,36.4085164872071,-215.85005));
#228543=CARTESIAN_POINT('Ctrl Pts',(53.6858060762413,36.5871897873468,-215.85005));
#228544=CARTESIAN_POINT('Ctrl Pts',(46.9910749481346,18.573078208412,-232.979487417878));
#228545=CARTESIAN_POINT('Ctrl Pts',(48.777813963045,21.1992978212187,-229.849984990042));
#228546=CARTESIAN_POINT('Ctrl Pts',(50.5669117785144,23.8226213730258,-226.720151765023));
#228547=CARTESIAN_POINT('Ctrl Pts',(52.3593746083135,26.4424369538029,-223.59005292932));
#228548=CARTESIAN_POINT('Ctrl Pts',(54.1518374381127,29.06225253458,-220.459954093617));
#228549=CARTESIAN_POINT('Ctrl Pts',(55.9476448491922,31.678562291835,-217.329579884935));
#228550=CARTESIAN_POINT('Ctrl Pts',(57.7483973817176,34.2905533170906,-214.199162765268));
#228551=CARTESIAN_POINT('Ctrl Pts',(45.9478671932277,20.2170814818308,-232.97487795833));
#228552=CARTESIAN_POINT('Ctrl Pts',(47.742137018698,22.773387445697,-229.848036259254));
#228553=CARTESIAN_POINT('Ctrl Pts',(49.5390933433176,25.3254669009981,-226.72056760043));
#228554=CARTESIAN_POINT('Ctrl Pts',(51.3405748716693,27.8719256903179,-223.592376908212));
#228555=CARTESIAN_POINT('Ctrl Pts',(53.1420564000211,30.4183844796377,-220.464186215995));
#228556=CARTESIAN_POINT('Ctrl Pts',(54.9479893176734,32.9592452374763,-217.335250628456));
#228557=CARTESIAN_POINT('Ctrl Pts',(56.7618317615675,35.4923074576668,-214.205720218898));
#228558=CARTESIAN_POINT('Ctrl Pts',(44.7615745302087,21.8990643607635,-232.969037860444));
#228559=CARTESIAN_POINT('Ctrl Pts',(46.6097944788647,24.3412907086997,-229.843779326009));
#228560=CARTESIAN_POINT('Ctrl Pts',(48.4600741151173,26.7788374139345,-226.718163107495));
#228561=CARTESIAN_POINT('Ctrl Pts',(50.314645520879,29.2097033728254,-223.592001377317));
#228562=CARTESIAN_POINT('Ctrl Pts',(52.1692169266407,31.6405693317163,-220.465839647138));
#228563=CARTESIAN_POINT('Ctrl Pts',(54.0277552893424,34.0649668687443,-217.339108786108));
#228564=CARTESIAN_POINT('Ctrl Pts',(55.8965060194204,36.4779337667532,-214.211679223185));
#228565=CARTESIAN_POINT('Ctrl Pts',(43.422273991912,23.5661942096002,-232.965337149737));
#228566=CARTESIAN_POINT('Ctrl Pts',(45.3530981989507,25.8862379834418,-229.841157038659));
#228567=CARTESIAN_POINT('Ctrl Pts',(47.2852714213136,28.2012404581192,-226.716776130434));
#228568=CARTESIAN_POINT('Ctrl Pts',(49.2205702668173,30.5094898312471,-223.59207508571));
#228569=CARTESIAN_POINT('Ctrl Pts',(51.155869112321,32.817739204375,-220.467374040986));
#228570=CARTESIAN_POINT('Ctrl Pts',(53.0939569308302,35.1194950308581,-217.342336617277));
#228571=CARTESIAN_POINT('Ctrl Pts',(55.0403804700997,37.4099350168284,-214.216875626567));
#228572=CARTESIAN_POINT('Ctrl Pts',(42.0829734536151,25.2333240584369,-232.96163643903));
#228573=CARTESIAN_POINT('Ctrl Pts',(44.0964019190368,27.4311852581839,-229.838534751308));
#228574=CARTESIAN_POINT('Ctrl Pts',(46.1104687275099,29.6236435023039,-226.715389153373));
#228575=CARTESIAN_POINT('Ctrl Pts',(48.1264950127556,31.8092762896688,-223.592148794104));
#228576=CARTESIAN_POINT('Ctrl Pts',(50.1425212980013,33.9949090770337,-220.468908434835));
#228577=CARTESIAN_POINT('Ctrl Pts',(52.1601585723181,36.1740231929721,-217.345564448446));
#228578=CARTESIAN_POINT('Ctrl Pts',(54.1842549207791,38.3419362669036,-214.22207202995));
#228579=CARTESIAN_POINT('Ctrl Pts',(40.5861557408476,26.890319992193,-232.960340269022));
#228580=CARTESIAN_POINT('Ctrl Pts',(42.7119476104226,28.9566971003925,-229.837640649106));
#228581=CARTESIAN_POINT('Ctrl Pts',(44.8377162696882,31.0173031877438,-226.714988934497));
#228582=CARTESIAN_POINT('Ctrl Pts',(46.9640447743127,33.0713690029734,-223.592432090741));
#228583=CARTESIAN_POINT('Ctrl Pts',(49.0903732789372,35.1254348182031,-220.469875246985));
#228584=CARTESIAN_POINT('Ctrl Pts',(51.2170775857911,37.1731632837144,-217.347402715892));
#228585=CARTESIAN_POINT('Ctrl Pts',(53.3465595646389,39.2117870653358,-214.225170223039));
#228586=CARTESIAN_POINT('Ctrl Pts',(38.9866932910313,28.4456556381462,-232.962790912271));
#228587=CARTESIAN_POINT('Ctrl Pts',(41.2391357104746,30.3925039299732,-229.839958591048));
#228588=CARTESIAN_POINT('Ctrl Pts',(43.490849558744,32.3336071411576,-226.717133201801));
#228589=CARTESIAN_POINT('Ctrl Pts',(45.7416073381742,34.2690638917383,-223.59431099442));
#228590=CARTESIAN_POINT('Ctrl Pts',(47.9923651176044,36.2045206423189,-220.471488787039));
#228591=CARTESIAN_POINT('Ctrl Pts',(50.2421837638693,38.1343124474224,-217.348670714219));
#228592=CARTESIAN_POINT('Ctrl Pts',(52.490668536736,40.0587201499459,-214.225843430884));
#228593=CARTESIAN_POINT('Ctrl Pts',(37.3872308412151,30.0009912840992,-232.96524155552));
#228594=CARTESIAN_POINT('Ctrl Pts',(39.7663238105267,31.8283107595538,-229.842276532991));
#228595=CARTESIAN_POINT('Ctrl Pts',(42.1439828477997,33.6499110945716,-226.719277469106));
#228596=CARTESIAN_POINT('Ctrl Pts',(44.5191699020356,35.4667587805032,-223.596189898099));
#228597=CARTESIAN_POINT('Ctrl Pts',(46.8943569562715,37.2836064664347,-220.473102327093));
#228598=CARTESIAN_POINT('Ctrl Pts',(49.2672899419476,39.0954616111304,-217.349938712546));
#228599=CARTESIAN_POINT('Ctrl Pts',(51.6347775088331,40.905653234556,-214.226516638731));
#228600=CARTESIAN_POINT('Ctrl Pts',(35.6766644639054,31.4635880480613,-232.97088766827));
#228601=CARTESIAN_POINT('Ctrl Pts',(38.1975797295179,33.1824169992017,-229.847322479379));
#228602=CARTESIAN_POINT('Ctrl Pts',(40.7164614543727,34.8957848961753,-226.723562794745));
#228603=CARTESIAN_POINT('Ctrl Pts',(43.231587976361,36.605521367383,-223.599359264791));
#228604=CARTESIAN_POINT('Ctrl Pts',(45.7467144983492,38.3152578385909,-220.475155734837));
#228605=CARTESIAN_POINT('Ctrl Pts',(48.2584201480868,40.0209091135152,-217.350539684011));
#228606=CARTESIAN_POINT('Ctrl Pts',(50.7614553754203,41.7288322173994,-214.224825362635));
#228607=CARTESIAN_POINT('Ctrl Pts',(33.949434877602,32.770352829909,-232.980025784665));
#228608=CARTESIAN_POINT('Ctrl Pts',(36.6048862944054,34.4080943544835,-229.854970428563));
#228609=CARTESIAN_POINT('Ctrl Pts',(39.2576627597897,36.0413528393508,-226.72942775857));
#228610=CARTESIAN_POINT('Ctrl Pts',(41.9056884039802,37.6725825561817,-223.603007266837));
#228611=CARTESIAN_POINT('Ctrl Pts',(44.5537140481708,39.3038122730124,-220.476586775106));
#228612=CARTESIAN_POINT('Ctrl Pts',(47.1972705274053,40.9325619164058,-217.349301164816));
#228613=CARTESIAN_POINT('Ctrl Pts',(49.8308862116777,42.5662844245855,-214.220385090245));
#228614=CARTESIAN_POINT('Ctrl Pts',(33.0858200844503,33.4237352208328,-232.984594842862));
#228615=CARTESIAN_POINT('Ctrl Pts',(35.8085395768491,35.0209330321244,-229.858794403155));
#228616=CARTESIAN_POINT('Ctrl Pts',(38.5282634124981,36.6141368109387,-226.732360240482));
#228617=CARTESIAN_POINT('Ctrl Pts',(41.2427386177898,38.2061131505809,-223.604831267861));
#228618=CARTESIAN_POINT('Ctrl Pts',(43.9572138230815,39.7980894902232,-220.47730229524));
#228619=CARTESIAN_POINT('Ctrl Pts',(46.6666957170646,41.3883883178512,-217.348681905218));
#228620=CARTESIAN_POINT('Ctrl Pts',(49.3656016298064,42.9850105281785,-214.21816495405));
#228621=CARTESIAN_POINT('Ctrl Pts',(32.216695486199,34.0396911750287,-232.98970214378));
#228622=CARTESIAN_POINT('Ctrl Pts',(35.0051317985077,35.6029084387718,-229.862997039215));
#228623=CARTESIAN_POINT('Ctrl Pts',(37.7903020546954,37.1627315739784,-226.7354929936));
#228624=CARTESIAN_POINT('Ctrl Pts',(40.5699478215597,38.7220617966288,-223.60669458574));
#228625=CARTESIAN_POINT('Ctrl Pts',(43.3495935884239,40.2813920192791,-220.477896177879));
#228626=CARTESIAN_POINT('Ctrl Pts',(46.1238945065879,41.8398602062025,-217.347790101788));
#228627=CARTESIAN_POINT('Ctrl Pts',(48.8878519146755,43.4051188865968,-214.215677456544));
#228628=CARTESIAN_POINT('Ctrl Pts',(31.3497500510356,34.6184286458191,-232.99511552399));
#228629=CARTESIAN_POINT('Ctrl Pts',(34.1981927402684,36.1561028618858,-229.86725871849));
#228630=CARTESIAN_POINT('Ctrl Pts',(37.0431800113206,37.6911082882257,-226.738459395528));
#228631=CARTESIAN_POINT('Ctrl Pts',(39.8826292444588,39.2262665988641,-223.608273410873));
#228632=CARTESIAN_POINT('Ctrl Pts',(42.722078477597,40.7614249095024,-220.47808742622));
#228633=CARTESIAN_POINT('Ctrl Pts',(45.5561045113048,42.2964603802716,-217.34649079771));
#228634=CARTESIAN_POINT('Ctrl Pts',(48.3805813576904,43.8381246360801,-214.213011833879));
#228635=CARTESIAN_POINT('Ctrl Pts',(30.916277333454,34.9077973812142,-232.997822214095));
#228636=CARTESIAN_POINT('Ctrl Pts',(33.7947232111487,36.4327000734428,-229.869389558127));
#228637=CARTESIAN_POINT('Ctrl Pts',(36.6696189896331,37.9552966453494,-226.739942596491));
#228638=CARTESIAN_POINT('Ctrl Pts',(39.5389699559083,39.4783689999817,-223.60906282344));
#228639=CARTESIAN_POINT('Ctrl Pts',(42.4083209221835,41.001441354614,-220.47818305039));
#228640=CARTESIAN_POINT('Ctrl Pts',(45.2722095136632,42.5247604673061,-217.345841145671));
#228641=CARTESIAN_POINT('Ctrl Pts',(48.1269460791978,44.0546275108218,-214.211679022545));
#228642=CARTESIAN_POINT('Ctrl Pts',(30.4833514870981,35.1878641409515,-233.000603030011));
#228643=CARTESIAN_POINT('Ctrl Pts',(33.3903722647552,36.7021050405422,-229.871531357437));
#228644=CARTESIAN_POINT('Ctrl Pts',(36.2937694734405,38.2144329802205,-226.741379545545));
#228645=CARTESIAN_POINT('Ctrl Pts',(39.1916813033838,39.727537057445,-223.60977593002));
#228646=CARTESIAN_POINT('Ctrl Pts',(42.089593133327,41.2406411346694,-220.478172314495));
#228647=CARTESIAN_POINT('Ctrl Pts',(44.9820725042275,42.7543411128055,-217.345083947855));
#228648=CARTESIAN_POINT('Ctrl Pts',(47.8659336123358,44.2743593115718,-214.210293173543));
#228649=CARTESIAN_POINT('Ctrl Pts',(30.0519450660363,35.4586704870703,-233.00341455534));
#228650=CARTESIAN_POINT('Ctrl Pts',(32.9855855312196,36.9645966036217,-229.87362179639));
#228651=CARTESIAN_POINT('Ctrl Pts',(35.9155640960709,38.4690265434296,-226.742700788357));
#228652=CARTESIAN_POINT('Ctrl Pts',(38.8401926838925,39.9745043257835,-223.610348870589));
#228653=CARTESIAN_POINT('Ctrl Pts',(41.7648212717142,41.4799821081373,-220.477996952821));
#228654=CARTESIAN_POINT('Ctrl Pts',(44.6841307999907,42.986369790773,-217.344180493823));
#228655=CARTESIAN_POINT('Ctrl Pts',(47.5954455649975,44.4987574479709,-214.208828131933));
#228656=CARTESIAN_POINT('Ctrl Pts',(29.8362418555055,35.5940736601297,-233.004820318005));
#228657=CARTESIAN_POINT('Ctrl Pts',(32.7831921644516,37.0958423851614,-229.874667015866));
#228658=CARTESIAN_POINT('Ctrl Pts',(35.7264614073862,38.5963233250342,-226.743361409764));
#228659=CARTESIAN_POINT('Ctrl Pts',(38.664448374147,40.0979879599528,-223.610635340874));
#228660=CARTESIAN_POINT('Ctrl Pts',(41.6024353409078,41.5996525948713,-220.477909271983));
#228661=CARTESIAN_POINT('Ctrl Pts',(44.5351599478724,43.1023841297568,-217.343728766806));
#228662=CARTESIAN_POINT('Ctrl Pts',(47.4602015413284,44.6109565161706,-214.208095611128));
#228663=CARTESIAN_POINT('Ctrl Pts',(29.6209186123181,35.727161889339,-233.006233607583));
#228664=CARTESIAN_POINT('Ctrl Pts',(32.5806898644201,37.2253600131119,-229.875699165609));
#228665=CARTESIAN_POINT('Ctrl Pts',(35.5367698105028,38.7224845297496,-226.743992894479));
#228666=CARTESIAN_POINT('Ctrl Pts',(38.4876542293243,40.2209213875052,-223.610886590344));
#228667=CARTESIAN_POINT('Ctrl Pts',(41.4385386481458,41.7193582452608,-220.477780286209));
#228668=CARTESIAN_POINT('Ctrl Pts',(44.3842382725856,43.2190102201042,-217.343240349689));
#228669=CARTESIAN_POINT('Ctrl Pts',(47.3225890909698,44.7243219112958,-214.207343022243));
#228670=CARTESIAN_POINT('Ctrl Pts',(29.4060975644904,35.8579413159883,-233.007648088092));
#228671=CARTESIAN_POINT('Ctrl Pts',(32.3781342806196,37.3531855340767,-229.87670909491));
#228672=CARTESIAN_POINT('Ctrl Pts',(35.3464811752108,38.8475743913038,-226.744585492565));
#228673=CARTESIAN_POINT('Ctrl Pts',(38.3097398506307,40.3433960477796,-223.611093856846));
#228674=CARTESIAN_POINT('Ctrl Pts',(41.2729985260507,41.8392177042554,-220.477602221127));
#228675=CARTESIAN_POINT('Ctrl Pts',(44.231172512421,43.3363922589179,-217.342710032053));
#228676=CARTESIAN_POINT('Ctrl Pts',(47.182348866173,44.8390312087872,-214.206565980874));
#228677=CARTESIAN_POINT('Ctrl Pts',(29.2986870405764,35.9233310293129,-233.008355328346));
#228678=CARTESIAN_POINT('Ctrl Pts',(32.2768564887194,37.4170982945592,-229.877214059559));
#228679=CARTESIAN_POINT('Ctrl Pts',(35.2513368575648,38.9101193220809,-226.744881791608));
#228680=CARTESIAN_POINT('Ctrl Pts',(38.220782661284,40.4046333779168,-223.611197490097));
#228681=CARTESIAN_POINT('Ctrl Pts',(41.1902284650032,41.8991474337527,-220.477513188586));
#228682=CARTESIAN_POINT('Ctrl Pts',(44.1546396323386,43.3950832783248,-217.342444873235));
#228683=CARTESIAN_POINT('Ctrl Pts',(47.1122287537746,44.8963858575329,-214.206177460189));
#228684=CARTESIAN_POINT('Ctrl Pts',(29.1914020723121,35.98814355176,-233.009062856813));
#228685=CARTESIAN_POINT('Ctrl Pts',(32.1755653742122,37.4805880407614,-229.877713455064));
#228686=CARTESIAN_POINT('Ctrl Pts',(35.1560432829324,38.9723964221036,-226.745168359446));
#228687=CARTESIAN_POINT('Ctrl Pts',(38.1315454230114,40.4657560119625,-223.611290121901));
#228688=CARTESIAN_POINT('Ctrl Pts',(41.1070475630904,41.9591156018214,-220.477411884356));
#228689=CARTESIAN_POINT('Ctrl Pts',(44.0775707523758,43.4539632651818,-217.342169238531));
#228690=CARTESIAN_POINT('Ctrl Pts',(47.0414517295384,44.9540764555871,-214.205782818867));
#228691=CARTESIAN_POINT('Ctrl Pts',(29.0842579792521,36.0523797092374,-233.009769824147));
#228692=CARTESIAN_POINT('Ctrl Pts',(32.0742678787604,37.5436593534111,-229.878206054095));
#228693=CARTESIAN_POINT('Ctrl Pts',(35.0605994496261,39.0344137463011,-226.745443927067));
#228694=CARTESIAN_POINT('Ctrl Pts',(38.0420193927072,40.5267753480634,-223.611370632498));
#228695=CARTESIAN_POINT('Ctrl Pts',(41.0234393357883,42.0191369498257,-220.477297337928));
#228696=CARTESIAN_POINT('Ctrl Pts',(43.9999418407127,43.5130501216253,-217.341882483075));
#228697=CARTESIAN_POINT('Ctrl Pts',(46.9699855652835,45.0121250312964,-214.205381478311));
#228698=CARTESIAN_POINT('Ctrl Pts',(29.030685932722,36.0844977879761,-233.010123307814));
#228699=CARTESIAN_POINT('Ctrl Pts',(32.0236191310345,37.5751950097359,-229.878452353611));
#228700=CARTESIAN_POINT('Ctrl Pts',(35.012877532973,39.0654224083999,-226.745581710878));
#228701=CARTESIAN_POINT('Ctrl Pts',(37.997256377555,40.5572850161139,-223.611410887796));
#228702=CARTESIAN_POINT('Ctrl Pts',(40.9816352221372,42.0491476238279,-220.477240064714));
#228703=CARTESIAN_POINT('Ctrl Pts',(43.9611273848811,43.5425935498471,-217.341739105347));
#228704=CARTESIAN_POINT('Ctrl Pts',(46.934252483156,45.041149319151,-214.205180808032));
#228705=CARTESIAN_POINT('Ctrl Pts',(28.9771491054224,36.1164717760765,-233.010476650599));
#228706=CARTESIAN_POINT('Ctrl Pts',(31.9729687878842,37.6066260584536,-229.878696953144));
#228707=CARTESIAN_POINT('Ctrl Pts',(34.9651180517945,39.0963661267734,-226.745716744168));
#228708=CARTESIAN_POINT('Ctrl Pts',(37.952421164982,40.5877688592974,-223.611448112616));
#228709=CARTESIAN_POINT('Ctrl Pts',(40.9397242781695,42.0791715918215,-220.477179481064));
#228710=CARTESIAN_POINT('Ctrl Pts',(43.9221729224182,43.5721886941534,-217.341592947587));
#228711=CARTESIAN_POINT('Ctrl Pts',(46.8983471180018,45.0702630995771,-214.204978462744));
#228712=CARTESIAN_POINT('Ctrl Pts',(28.9236494148868,36.1483017803918,-233.01082974273));
#228713=CARTESIAN_POINT('Ctrl Pts',(31.9223177157407,37.6379530768432,-229.878939694123));
#228714=CARTESIAN_POINT('Ctrl Pts',(34.9173208817124,39.1272459095225,-226.745848865747));
#228715=CARTESIAN_POINT('Ctrl Pts',(37.9075126656038,40.6182282999103,-223.611482166239));
#228716=CARTESIAN_POINT('Ctrl Pts',(40.8977044494953,42.109210690298,-220.477115466732));
#228717=CARTESIAN_POINT('Ctrl Pts',(43.8830754570229,43.6018377843273,-217.341443930439));
#228718=CARTESIAN_POINT('Ctrl Pts',(46.8622654530928,45.0994691148216,-214.204774369339));
#228719=CARTESIAN_POINT('Ctrl Pts',(28.8701497243513,36.1801317847072,-233.011182834863));
#228720=CARTESIAN_POINT('Ctrl Pts',(31.871666643597,37.6692800952327,-229.879182435101));
#228721=CARTESIAN_POINT('Ctrl Pts',(34.8695237116303,39.1581256922717,-226.745980987327));
#228722=CARTESIAN_POINT('Ctrl Pts',(37.8626041662257,40.6486877405231,-223.611516219864));
#228723=CARTESIAN_POINT('Ctrl Pts',(40.8556846208211,42.1392497887745,-220.4770514524));
#228724=CARTESIAN_POINT('Ctrl Pts',(43.8439779916275,43.6314868745012,-217.341294913291));
#228725=CARTESIAN_POINT('Ctrl Pts',(46.8261837881837,45.128675130066,-214.204570275934));
#228726=CARTESIAN_POINT('Ctrl Pts',(28.818156654463,36.2102288606094,-233.012213872822));
#228727=CARTESIAN_POINT('Ctrl Pts',(31.8223098653572,37.6990724529492,-229.880007982271));
#228728=CARTESIAN_POINT('Ctrl Pts',(34.8228081429799,39.18767633626,-226.746603037528));
#228729=CARTESIAN_POINT('Ctrl Pts',(37.8185924512592,40.6780007601943,-223.611963071785));
#228730=CARTESIAN_POINT('Ctrl Pts',(40.8143767595385,42.1683251841286,-220.477323106043));
#228731=CARTESIAN_POINT('Ctrl Pts',(43.8054348260158,43.6603350812977,-217.341420791685));
#228732=CARTESIAN_POINT('Ctrl Pts',(46.7905804536569,45.1571425161278,-214.2046126078));
#228733=CARTESIAN_POINT('Ctrl Pts',(28.7632636728437,36.243359951239,-233.011888154992));
#228734=CARTESIAN_POINT('Ctrl Pts',(31.7703631777874,37.7316226214323,-229.879662179404));
#228735=CARTESIAN_POINT('Ctrl Pts',(34.7738161809111,39.2196944596949,-226.746236332649));
#228736=CARTESIAN_POINT('Ctrl Pts',(37.7725662199917,40.7095348345317,-223.611574672556));
#228737=CARTESIAN_POINT('Ctrl Pts',(40.7713162590722,42.1993752093685,-220.476913012461));
#228738=CARTESIAN_POINT('Ctrl Pts',(43.7653510607838,43.6909491168262,-217.340988222568));
#228739=CARTESIAN_POINT('Ctrl Pts',(46.7534875501661,45.1873665995436,-214.204156771482));
#228740=CARTESIAN_POINT('',(46.7405472321667,30.7185439590785,-225.418940742796));
#228741=CARTESIAN_POINT('Ctrl Pts',(54.6458252041307,35.5078877047659,-215.85005));
#228742=CARTESIAN_POINT('Ctrl Pts',(54.5943354599542,35.0871229746991,-216.179655766508));
#228743=CARTESIAN_POINT('Ctrl Pts',(54.4989704544248,34.6852639063571,-216.528294351258));
#228744=CARTESIAN_POINT('Ctrl Pts',(54.2127819562334,33.8548754267304,-217.317195844125));
#228745=CARTESIAN_POINT('Ctrl Pts',(54.0059798594749,33.4340164710517,-217.764515858296));
#228746=CARTESIAN_POINT('Ctrl Pts',(53.2992114884488,32.3315417080536,-219.068798253937));
#228747=CARTESIAN_POINT('Ctrl Pts',(52.6935858718955,31.7306722066013,-219.95737939011));
#228748=CARTESIAN_POINT('Ctrl Pts',(51.1420742506923,30.731323527294,-221.883755596029));
#228749=CARTESIAN_POINT('Ctrl Pts',(50.1720764170543,30.4163412364309,-222.887463984116));
#228750=CARTESIAN_POINT('Ctrl Pts',(48.7953703105921,30.3299008816871,-224.056790691687));
#228751=CARTESIAN_POINT('Ctrl Pts',(48.3973293063562,30.3422930432357,-224.368248809743));
#228752=CARTESIAN_POINT('Ctrl Pts',(47.582248831158,30.4570387035492,-224.938952843229));
#228753=CARTESIAN_POINT('Ctrl Pts',(47.1618710045203,30.5599614053015,-225.200460249291));
#228754=CARTESIAN_POINT('Ctrl Pts',(46.7405472321717,30.7185439590994,-225.41894074279));
#228755=CARTESIAN_POINT('',(46.4511396589728,30.4281656954994,-225.850049999692));
#228756=CARTESIAN_POINT('Ctrl Pts',(46.4511396588546,30.4281656952997,-225.850049999478));
#228757=CARTESIAN_POINT('Ctrl Pts',(46.4993753881247,30.4765632101155,-225.778199403668));
#228758=CARTESIAN_POINT('Ctrl Pts',(46.547609928457,30.5249595320058,-225.706349252241));
#228759=CARTESIAN_POINT('Ctrl Pts',(46.6440796088716,30.6217527775478,-225.56264542894));
#228760=CARTESIAN_POINT('Ctrl Pts',(46.6923132704823,30.6701482177691,-225.490793959434));
#228761=CARTESIAN_POINT('Ctrl Pts',(46.7405472321751,30.7185439590791,-225.418940742802));
#228762=CARTESIAN_POINT('',(45.7333210481289,31.2122413341206,-225.850044625428));
#228763=CARTESIAN_POINT('Ctrl Pts',(46.4511396584396,30.4281656950207,-225.85005));
#228764=CARTESIAN_POINT('Ctrl Pts',(46.3327936010765,30.5600059656552,-225.85005));
#228765=CARTESIAN_POINT('Ctrl Pts',(46.2137942830087,30.6912801197937,-225.85005));
#228766=CARTESIAN_POINT('Ctrl Pts',(45.9745262547338,30.9526355221877,-225.85005));
#228767=CARTESIAN_POINT('Ctrl Pts',(45.8542372584541,31.0827388231335,-225.85005));
#228768=CARTESIAN_POINT('Ctrl Pts',(45.7333160885807,31.2122314446859,-225.85005));
#228769=CARTESIAN_POINT('Ctrl Pts',(45.7333215220983,31.2122476865619,-225.850034141972));
#228770=CARTESIAN_POINT('Ctrl Pts',(45.3379480310533,31.4554802421263,-225.979545398304));
#228771=CARTESIAN_POINT('Ctrl Pts',(44.9654369203883,31.7493278392119,-226.049149720515));
#228772=CARTESIAN_POINT('Ctrl Pts',(44.2902370695759,32.435117692196,-226.049169157732));
#228773=CARTESIAN_POINT('Ctrl Pts',(44.0028843799733,32.8110880152495,-225.979845479737));
#228774=CARTESIAN_POINT('Ctrl Pts',(43.7661192039793,33.2092653548652,-225.85004993015));
#228775=CARTESIAN_POINT('Ctrl Pts',(48.0827620446562,42.0414223951255,-215.85005));
#228776=CARTESIAN_POINT('Ctrl Pts',(47.691890257726,41.9918377457907,-216.158510565839));
#228777=CARTESIAN_POINT('Ctrl Pts',(47.3178589833685,41.9044704486236,-216.483755325416));
#228778=CARTESIAN_POINT('Ctrl Pts',(46.5278541131957,41.6412341609588,-217.232695618651));
#228779=CARTESIAN_POINT('Ctrl Pts',(46.1204261816246,41.4485202650666,-217.663837570769));
#228780=CARTESIAN_POINT('Ctrl Pts',(44.9817998525948,40.7494982164769,-219.000277705729));
#228781=CARTESIAN_POINT('Ctrl Pts',(44.3453100117888,40.117856186638,-219.946031814402));
#228782=CARTESIAN_POINT('Ctrl Pts',(43.3187329856903,38.5182399992516,-221.954309494373));
#228783=CARTESIAN_POINT('Ctrl Pts',(43.0024705252185,37.5284133108539,-222.985431128923));
#228784=CARTESIAN_POINT('Ctrl Pts',(42.9307447595918,36.1378442918464,-224.156404719666));
#228785=CARTESIAN_POINT('Ctrl Pts',(42.9463038154196,35.7490409902397,-224.457196959694));
#228786=CARTESIAN_POINT('Ctrl Pts',(43.0642975219611,34.9494394059176,-225.008393072079));
#228787=CARTESIAN_POINT('Ctrl Pts',(43.1679394115603,34.5354819113177,-225.26038854254));
#228788=CARTESIAN_POINT('Ctrl Pts',(43.3259173910694,34.1204116753624,-225.468974352254));
#228789=CARTESIAN_POINT('Ctrl Pts',(28.918632420916,36.3202559369514,-232.85005));
#228790=CARTESIAN_POINT('Ctrl Pts',(29.1405722429424,36.1874419307081,-232.85005));
#228791=CARTESIAN_POINT('Ctrl Pts',(29.3442027713421,36.0636271479844,-232.85005));
#228792=CARTESIAN_POINT('Ctrl Pts',(29.7663007847196,35.8033260589225,-232.85005));
#228793=CARTESIAN_POINT('Ctrl Pts',(29.9787466996505,35.6703265943621,-232.85005));
#228794=CARTESIAN_POINT('Ctrl Pts',(30.6209255013567,35.2622379995143,-232.85005));
#228795=CARTESIAN_POINT('Ctrl Pts',(31.0479818197507,34.9825440512594,-232.85005));
#228796=CARTESIAN_POINT('Ctrl Pts',(32.3437566649085,34.1080837663653,-232.85005));
#228797=CARTESIAN_POINT('Ctrl Pts',(33.2007785122792,33.4934899779854,-232.85005));
#228798=CARTESIAN_POINT('Ctrl Pts',(35.7754719960827,31.5304296840008,-232.85005));
#228799=CARTESIAN_POINT('Ctrl Pts',(37.4639373139647,30.0758667472212,-232.85005));
#228800=CARTESIAN_POINT('Ctrl Pts',(40.5990894760027,27.0270783922585,-232.85005));
#228801=CARTESIAN_POINT('Ctrl Pts',(42.1044452521521,25.3726646453478,-232.85005));
#228802=CARTESIAN_POINT('Ctrl Pts',(44.7627079511811,22.0795000960729,-232.85005));
#228803=CARTESIAN_POINT('Ctrl Pts',(45.9624973465495,20.4083241018545,-232.85005));
#228804=CARTESIAN_POINT('Ctrl Pts',(47.0649763530314,18.681697915047,-232.85005));
#228805=CARTESIAN_POINT('Origin',(0.,-12.9675000200281,-215.85005));
#228806=CARTESIAN_POINT('',(53.9390346875574,-61.9113848028035,-215.85005));
#228807=CARTESIAN_POINT('Ctrl Pts',(53.7300151844417,-62.1425230012532,
-215.85005));
#228808=CARTESIAN_POINT('Ctrl Pts',(53.7649393991663,-62.1040873964302,
-215.85005));
#228809=CARTESIAN_POINT('Ctrl Pts',(53.7998169861779,-62.0656105112122,
-215.85005));
#228810=CARTESIAN_POINT('Ctrl Pts',(53.8694902457069,-61.9885636960997,
-215.85005));
#228811=CARTESIAN_POINT('Ctrl Pts',(53.9042848508501,-61.9499949024173,
-215.85005));
#228812=CARTESIAN_POINT('Ctrl Pts',(53.9390346875573,-61.9113848028035,
-215.85005));
#228813=CARTESIAN_POINT('',(48.06997860106,-67.6025450092472,-215.850048906121));
#228814=CARTESIAN_POINT('Origin',(48.1334350484927,-61.7961505568785,-215.85005));
#228815=CARTESIAN_POINT('Ctrl Pts',(48.0699790998778,-67.6025411378175,
-215.85005));
#228816=CARTESIAN_POINT('Ctrl Pts',(48.2218940855867,-67.4735199039321,
-215.85005));
#228817=CARTESIAN_POINT('Ctrl Pts',(48.3737209284913,-67.3434180280897,
-215.850049999999));
#228818=CARTESIAN_POINT('Ctrl Pts',(48.673346523466,-67.0844676986175,-215.850049999999));
#228819=CARTESIAN_POINT('Ctrl Pts',(48.8227466277686,-66.9542303125478,
-215.85005));
#228820=CARTESIAN_POINT('Ctrl Pts',(48.9715866554311,-66.8233021636441,
-215.85005));
#228821=CARTESIAN_POINT('Ctrl Pts',(26.2545891898305,-60.7273783411365,
-233.020937743651));
#228822=CARTESIAN_POINT('Ctrl Pts',(29.704767491125,-62.4315344808983,-229.869275405273));
#228823=CARTESIAN_POINT('Ctrl Pts',(33.1518809533354,-64.139871089189,-226.716620552092));
#228824=CARTESIAN_POINT('Ctrl Pts',(36.5949698446713,-65.8547248151706,
-223.563151715778));
#228825=CARTESIAN_POINT('Ctrl Pts',(40.038058736007,-67.5695785411523,-220.409682879464));
#228826=CARTESIAN_POINT('Ctrl Pts',(43.4771077064633,-69.2909019608329,
-217.255357871467));
#228827=CARTESIAN_POINT('Ctrl Pts',(46.911032093483,-71.0224993808136,-214.10099631368));
#228828=CARTESIAN_POINT('Ctrl Pts',(26.3772071408559,-60.6610527709189,
-233.021822686564));
#228829=CARTESIAN_POINT('Ctrl Pts',(29.8198922647338,-62.3656430824214,
-229.870183157334));
#228830=CARTESIAN_POINT('Ctrl Pts',(33.2595071470079,-64.0744068681985,
-226.717552132221));
#228831=CARTESIAN_POINT('Ctrl Pts',(36.6950887844903,-65.7896831337175,
-223.564108323038));
#228832=CARTESIAN_POINT('Ctrl Pts',(40.1306704219727,-67.5049593992365,
-220.410664513854));
#228833=CARTESIAN_POINT('Ctrl Pts',(43.5622034605361,-69.2267005231895,
-217.256365654455));
#228834=CARTESIAN_POINT('Ctrl Pts',(46.9885985225256,-70.9587167786769,
-214.102032318221));
#228835=CARTESIAN_POINT('Ctrl Pts',(26.4972071576729,-60.5976714014882,
-233.021374771214));
#228836=CARTESIAN_POINT('Ctrl Pts',(29.9328875356291,-62.3022271706743,
-229.870039558606));
#228837=CARTESIAN_POINT('Ctrl Pts',(33.3654481367504,-64.010966733861,-226.717674406878));
#228838=CARTESIAN_POINT('Ctrl Pts',(36.793844127674,-65.7263329827881,-223.564425346624));
#228839=CARTESIAN_POINT('Ctrl Pts',(40.2222401185977,-67.4416992317152,
-220.411176286369));
#228840=CARTESIAN_POINT('Ctrl Pts',(43.6464575126834,-69.1636354921494,
-217.256997787241));
#228841=CARTESIAN_POINT('Ctrl Pts',(47.0652610833278,-70.8962157902618,
-214.102692345356));
#228842=CARTESIAN_POINT('Ctrl Pts',(26.6170765305167,-60.5338892284733,
-233.020688145171));
#228843=CARTESIAN_POINT('Ctrl Pts',(30.045545113986,-62.238632000908,-229.869690768214));
#228844=CARTESIAN_POINT('Ctrl Pts',(33.4708476093749,-63.9475635251553,
-226.717626646141));
#228845=CARTESIAN_POINT('Ctrl Pts',(36.8918444428126,-65.6632431316632,
-223.564602851986));
#228846=CARTESIAN_POINT('Ctrl Pts',(40.3128412762504,-67.378922738171,-220.411579057831));
#228847=CARTESIAN_POINT('Ctrl Pts',(43.7295213469238,-69.1012807810974,
-217.257546349595));
#228848=CARTESIAN_POINT('Ctrl Pts',(47.140464436521,-70.8347129400802,-214.103279186265));
#228849=CARTESIAN_POINT('Ctrl Pts',(26.7369459033605,-60.4701070554585,
-233.020001519128));
#228850=CARTESIAN_POINT('Ctrl Pts',(30.1582026923428,-62.1750368311418,
-229.869341977822));
#228851=CARTESIAN_POINT('Ctrl Pts',(33.5762470819994,-63.8841603164497,
-226.717578885404));
#228852=CARTESIAN_POINT('Ctrl Pts',(36.9898447579513,-65.6001532805383,
-223.564780357348));
#228853=CARTESIAN_POINT('Ctrl Pts',(40.4034424339031,-67.3161462446269,
-220.411981829292));
#228854=CARTESIAN_POINT('Ctrl Pts',(43.8125851811644,-69.0389260700454,
-217.258094911949));
#228855=CARTESIAN_POINT('Ctrl Pts',(47.2156677897142,-70.7732100898985,
-214.103866027175));
#228856=CARTESIAN_POINT('Ctrl Pts',(26.8570455332274,-60.4056521569874,
-233.019306732319));
#228857=CARTESIAN_POINT('Ctrl Pts',(30.2708768025335,-62.1109922428301,
-229.868974562847));
#228858=CARTESIAN_POINT('Ctrl Pts',(33.6814570870323,-63.8205250164116,
-226.717508054876));
#228859=CARTESIAN_POINT('Ctrl Pts',(37.0874578686263,-65.5370390313854,
-223.564936035396));
#228860=CARTESIAN_POINT('Ctrl Pts',(40.4934586502203,-67.2535530463592,
-220.412364015916));
#228861=CARTESIAN_POINT('Ctrl Pts',(43.8948755984016,-68.9769508862391,
-217.258629913538));
#228862=CARTESIAN_POINT('Ctrl Pts',(47.289907411692,-70.7122816555241,-214.104447241908));
#228863=CARTESIAN_POINT('Ctrl Pts',(26.9773582084069,-60.3405190002037,
-233.018605415792));
#228864=CARTESIAN_POINT('Ctrl Pts',(30.383562017878,-62.046487235826,-229.868590727832));
#228865=CARTESIAN_POINT('Ctrl Pts',(33.786482884195,-63.7566420726074,-226.717416049128));
#228866=CARTESIAN_POINT('Ctrl Pts',(37.1846995203357,-65.4738805679581,
-223.56507131637));
#228867=CARTESIAN_POINT('Ctrl Pts',(40.5829161564765,-67.1911190633088,
-220.412726583613));
#228868=CARTESIAN_POINT('Ctrl Pts',(43.9764292691396,-68.9153271247727,
-217.259151804163));
#228869=CARTESIAN_POINT('Ctrl Pts',(47.3632316759027,-70.6518934365393,
-214.105023471352));
#228870=CARTESIAN_POINT('Ctrl Pts',(27.2179835587658,-60.2102526866361,
-233.017202782736));
#228871=CARTESIAN_POINT('Ctrl Pts',(30.608932448567,-61.9174772218177,-229.867823057804));
#228872=CARTESIAN_POINT('Ctrl Pts',(33.9965344785202,-63.628876184999,-226.717232037632));
#228873=CARTESIAN_POINT('Ctrl Pts',(37.3791828237546,-65.3475636411034,
-223.565341878319));
#228874=CARTESIAN_POINT('Ctrl Pts',(40.761831168989,-67.0662510972078,-220.413451719006));
#228875=CARTESIAN_POINT('Ctrl Pts',(44.1395366106154,-68.7920796018397,
-217.260195585412));
#228876=CARTESIAN_POINT('Ctrl Pts',(47.509880204324,-70.5311169985697,-214.10617593024));
#228877=CARTESIAN_POINT('Ctrl Pts',(27.4594610774215,-60.0772732757658,
-233.015774094218));
#228878=CARTESIAN_POINT('Ctrl Pts',(30.8343473371973,-61.7866254642456,
-229.866989782546));
#228879=CARTESIAN_POINT('Ctrl Pts',(34.2058492100272,-63.5001197459416,
-226.716963322528));
#228880=CARTESIAN_POINT('Ctrl Pts',(37.5721802072639,-65.2210699553996,
-223.565530811621));
#228881=CARTESIAN_POINT('Ctrl Pts',(40.9385112045005,-66.9420201648576,
-220.414098300713));
#228882=CARTESIAN_POINT('Ctrl Pts',(44.2996968466345,-68.6702379154868,
-217.261186869816));
#228883=CARTESIAN_POINT('Ctrl Pts',(47.6528670748933,-70.412501654795,-214.107308443709));
#228884=CARTESIAN_POINT('Ctrl Pts',(27.7016532108346,-59.9415372606891,
-233.014331652954));
#228885=CARTESIAN_POINT('Ctrl Pts',(31.05976276075,-61.6538447557032,-229.866107695338));
#228886=CARTESIAN_POINT('Ctrl Pts',(34.4144695478916,-63.3702479288391,
-226.716625256232));
#228887=CARTESIAN_POINT('Ctrl Pts',(37.7638186351444,-65.0942396965474,
-223.565650201608));
#228888=CARTESIAN_POINT('Ctrl Pts',(41.1131677223973,-66.8182314642556,
-220.414675146985));
#228889=CARTESIAN_POINT('Ctrl Pts',(44.4572046958943,-68.5495754713907,
-217.262129974306));
#228890=CARTESIAN_POINT('Ctrl Pts',(47.7925819070095,-70.295770952258,-214.1084263508));
#228891=CARTESIAN_POINT('Ctrl Pts',(28.1860374776607,-59.6700652305358,
-233.011446770425));
#228892=CARTESIAN_POINT('Ctrl Pts',(31.5105936078552,-61.3882833386183,
-229.864343520922));
#228893=CARTESIAN_POINT('Ctrl Pts',(34.8317102236203,-63.1105042946341,
-226.715949123638));
#228894=CARTESIAN_POINT('Ctrl Pts',(38.1470954909054,-64.8405791788429,
-223.565888981583));
#228895=CARTESIAN_POINT('Ctrl Pts',(41.4624807581906,-66.5706540630517,
-220.415828839529));
#228896=CARTESIAN_POINT('Ctrl Pts',(44.772220394414,-68.3082505831985,-217.264016183284));
#228897=CARTESIAN_POINT('Ctrl Pts',(48.0720115712419,-70.062309547184,-214.110662164981));
#228898=CARTESIAN_POINT('Ctrl Pts',(28.673279908832,-59.3875657071804,-233.008507940657));
#228899=CARTESIAN_POINT('Ctrl Pts',(31.9614269102671,-61.115004898578,-229.862385501452));
#228900=CARTESIAN_POINT('Ctrl Pts',(35.2461728642701,-62.846298987024,-226.714996249958));
#228901=CARTESIAN_POINT('Ctrl Pts',(38.5249351802734,-64.5855733702612,
-223.565849736452));
#228902=CARTESIAN_POINT('Ctrl Pts',(41.8036974962768,-66.3248477534984,
-220.416703222945));
#228903=CARTESIAN_POINT('Ctrl Pts',(45.0766243118393,-68.0716449683638,
-217.26570937755));
#228904=CARTESIAN_POINT('Ctrl Pts',(48.338349401543,-69.8363895329911,-214.112840467621));
#228905=CARTESIAN_POINT('Ctrl Pts',(29.1622830188973,-59.093703206177,-233.005601149464));
#228906=CARTESIAN_POINT('Ctrl Pts',(32.4119055964007,-60.8333256128672,
-229.860352517102));
#228907=CARTESIAN_POINT('Ctrl Pts',(35.6582030143032,-62.5766317072687,
-226.713886241748));
#228908=CARTESIAN_POINT('Ctrl Pts',(38.8983695571512,-64.3279278794606,
-223.565632722533));
#228909=CARTESIAN_POINT('Ctrl Pts',(42.1385360999994,-66.0792240516524,
-220.417379203317));
#228910=CARTESIAN_POINT('Ctrl Pts',(45.3727988408086,-67.8379178590787,
-217.267251393612));
#228911=CARTESIAN_POINT('Ctrl Pts',(48.5947562955792,-69.6157591498535,
-214.114999659484));
#228912=CARTESIAN_POINT('Ctrl Pts',(30.1402892390281,-58.5059782041702,
-232.999787567079));
#228913=CARTESIAN_POINT('Ctrl Pts',(33.312862968668,-60.2699670414456,-229.856286548401));
#228914=CARTESIAN_POINT('Ctrl Pts',(36.4822633143695,-62.0372971477581,
-226.711666225327));
#228915=CARTESIAN_POINT('Ctrl Pts',(39.645238310907,-63.8126368978593,-223.565198694695));
#228916=CARTESIAN_POINT('Ctrl Pts',(42.8082133074446,-65.5879766479605,
-220.418731164063));
#228917=CARTESIAN_POINT('Ctrl Pts',(45.9651478987472,-67.3704636405086,
-217.270335425737));
#228918=CARTESIAN_POINT('Ctrl Pts',(49.1075700836515,-69.1744983835783,
-214.119318043209));
#228919=CARTESIAN_POINT('Ctrl Pts',(31.1253296771952,-57.8727830755883,
-232.994119837029));
#228920=CARTESIAN_POINT('Ctrl Pts',(34.2123982630523,-59.6729838063912,
-229.851946789728));
#228921=CARTESIAN_POINT('Ctrl Pts',(37.2965847816597,-61.4760996503049,
-226.708845019593));
#228922=CARTESIAN_POINT('Ctrl Pts',(40.374466421429,-63.2867830742773,-223.564079694009));
#228923=CARTESIAN_POINT('Ctrl Pts',(43.4523480611983,-65.0974664982497,
-220.419314368426));
#228924=CARTESIAN_POINT('Ctrl Pts',(46.5245369999706,-66.9145532819642,
-217.272835132396));
#228925=CARTESIAN_POINT('Ctrl Pts',(49.5806341150271,-68.7543693866452,
-214.123609471056));
#228926=CARTESIAN_POINT('Ctrl Pts',(32.1087006613968,-57.191646012686,-232.989078118058));
#228927=CARTESIAN_POINT('Ctrl Pts',(35.1076397475695,-59.0371491145894,
-229.847995786691));
#228928=CARTESIAN_POINT('Ctrl Pts',(38.1040273439412,-60.8851347665649,
-226.706162642268));
#228929=CARTESIAN_POINT('Ctrl Pts',(41.0945558666574,-62.7399255565489,
-223.562922655666));
#228930=CARTESIAN_POINT('Ctrl Pts',(44.0850843893735,-64.5947163465329,
-220.419682669063));
#228931=CARTESIAN_POINT('Ctrl Pts',(47.0704902905866,-66.4550539448948,
-217.275009748779));
#228932=CARTESIAN_POINT('Ctrl Pts',(50.0397793224693,-68.3371871397263,
-214.127816818154));
#228933=CARTESIAN_POINT('Ctrl Pts',(34.0754426298001,-55.8293718868815,
-232.978994680116));
#228934=CARTESIAN_POINT('Ctrl Pts',(36.898122716604,-57.765479730986,-229.840093780616));
#228935=CARTESIAN_POINT('Ctrl Pts',(39.7189124685042,-59.7032049990848,
-226.700797887619));
#228936=CARTESIAN_POINT('Ctrl Pts',(42.5347347571142,-61.6462105210921,
-223.560608578979));
#228937=CARTESIAN_POINT('Ctrl Pts',(45.3505570457242,-63.5892160430994,
-220.420419270338));
#228938=CARTESIAN_POINT('Ctrl Pts',(48.1623968718184,-65.5360552707562,
-217.279358981544));
#228939=CARTESIAN_POINT('Ctrl Pts',(50.9580697373535,-67.5028226458884,
-214.13623151235));
#228940=CARTESIAN_POINT('Ctrl Pts',(36.0418015499852,-54.2678518298554,
-232.972801817804));
#228941=CARTESIAN_POINT('Ctrl Pts',(38.677172296014,-56.3317754242655,-229.834906922101));
#228942=CARTESIAN_POINT('Ctrl Pts',(41.3112311995406,-58.3966848422808,
-226.696862079201));
#228943=CARTESIAN_POINT('Ctrl Pts',(43.9416573065822,-60.4651362830048,
-223.558498608177));
#228944=CARTESIAN_POINT('Ctrl Pts',(46.5720834136237,-62.5335877237288,
-220.420135137153));
#228945=CARTESIAN_POINT('Ctrl Pts',(49.1998046996963,-64.6044563549465,
-217.281452032185));
#228946=CARTESIAN_POINT('Ctrl Pts',(51.8146256937275,-66.6895540609604,
-214.142095885467));
#228947=CARTESIAN_POINT('Ctrl Pts',(37.882123536986,-52.5752193780183,-232.970806720566));
#228948=CARTESIAN_POINT('Ctrl Pts',(40.3469003584876,-54.7858287675482,
-229.833381329414));
#228949=CARTESIAN_POINT('Ctrl Pts',(42.8110087314114,-56.9968033268292,
-226.695906966754));
#228950=CARTESIAN_POINT('Ctrl Pts',(45.2731441984033,-59.2095312210711,
-223.558332736904));
#228951=CARTESIAN_POINT('Ctrl Pts',(47.7352796653952,-61.4222591153131,
-220.420758507053));
#228952=CARTESIAN_POINT('Ctrl Pts',(50.1959790879104,-63.636130388643,-217.283078469976));
#228953=CARTESIAN_POINT('Ctrl Pts',(52.6494272678771,-65.857552778289,-214.145217662806));
#228954=CARTESIAN_POINT('Ctrl Pts',(39.7224455239868,-50.8825869261812,
-232.968811623327));
#228955=CARTESIAN_POINT('Ctrl Pts',(42.0166284209611,-53.2398821108309,
-229.831855736726));
#228956=CARTESIAN_POINT('Ctrl Pts',(44.3107862632822,-55.5969218113776,
-226.694951854308));
#228957=CARTESIAN_POINT('Ctrl Pts',(46.6046310902244,-57.9539261591375,
-223.55816686563));
#228958=CARTESIAN_POINT('Ctrl Pts',(48.8984759171666,-60.3109305068973,
-220.421381876952));
#228959=CARTESIAN_POINT('Ctrl Pts',(51.1921534761245,-62.6678044223395,
-217.284704907766));
#228960=CARTESIAN_POINT('Ctrl Pts',(53.4842288420267,-65.0255514956176,
-214.148339440146));
#228961=CARTESIAN_POINT('Ctrl Pts',(41.4461104147051,-49.0481855160699,
-232.97166665431));
#228962=CARTESIAN_POINT('Ctrl Pts',(43.5856625816949,-51.5719501776712,
-229.834567875703));
#228963=CARTESIAN_POINT('Ctrl Pts',(45.725755460948,-54.09499526448,-226.697476434552));
#228964=CARTESIAN_POINT('Ctrl Pts',(47.8671575840062,-56.616542818236,-223.560361067685));
#228965=CARTESIAN_POINT('Ctrl Pts',(50.0085597070645,-59.138090371992,-220.423245700818));
#228966=CARTESIAN_POINT('Ctrl Pts',(52.1509051960796,-61.6584905278127,
-217.286128821816));
#228967=CARTESIAN_POINT('Ctrl Pts',(54.2979333072227,-64.1740643125789,
-214.148798365297));
#228968=CARTESIAN_POINT('Ctrl Pts',(42.9734424791526,-47.1926155685251,
-232.978313839575));
#228969=CARTESIAN_POINT('Ctrl Pts',(44.9946071331279,-49.8757842370209,
-229.840273609375));
#228970=CARTESIAN_POINT('Ctrl Pts',(47.0170439436796,-52.5576635978524,
-226.702063718992));
#228971=CARTESIAN_POINT('Ctrl Pts',(49.0424058070309,-55.2367916852255,
-223.563495724472));
#228972=CARTESIAN_POINT('Ctrl Pts',(51.0677676703821,-57.9159197725986,
-220.424927729951));
#228973=CARTESIAN_POINT('Ctrl Pts',(53.0955326872786,-60.5927163347612,
-217.286025395512));
#228974=CARTESIAN_POINT('Ctrl Pts',(55.1321416284158,-63.2617424152049,
-214.146274180285));
#228975=CARTESIAN_POINT('Ctrl Pts',(43.7371085113763,-46.2648305947527,
-232.981637432207));
#228976=CARTESIAN_POINT('Ctrl Pts',(45.6990794088443,-49.0277012666958,
-229.84312647621));
#228977=CARTESIAN_POINT('Ctrl Pts',(47.6626881850455,-51.7889977645385,
-226.704357361211));
#228978=CARTESIAN_POINT('Ctrl Pts',(49.6300299185432,-54.5469161187202,
-223.565063052865));
#228979=CARTESIAN_POINT('Ctrl Pts',(51.5973716520409,-57.3048344729019,
-220.425768744518));
#228980=CARTESIAN_POINT('Ctrl Pts',(53.5678464328781,-60.0598292382354,
-217.285973682359));
#228981=CARTESIAN_POINT('Ctrl Pts',(55.5492457890124,-62.8055814665179,
-214.145012087778));
#228982=CARTESIAN_POINT('Ctrl Pts',(44.4530216283881,-45.330501487166,-232.985755113274));
#228983=CARTESIAN_POINT('Ctrl Pts',(46.364564734047,-48.1716118824616,-229.846604427224));
#228984=CARTESIAN_POINT('Ctrl Pts',(48.2780837959556,-51.0109018738896,
-226.707080446303));
#228985=CARTESIAN_POINT('Ctrl Pts',(50.19592152344,-53.846435222383,-223.566845772292));
#228986=CARTESIAN_POINT('Ctrl Pts',(52.1137592509244,-56.6819685708763,
-220.42661109828));
#228987=CARTESIAN_POINT('Ctrl Pts',(54.0353913811122,-59.5141054680716,
-217.285678387203));
#228988=CARTESIAN_POINT('Ctrl Pts',(55.9686189515471,-62.3368927213004,
-214.143346745665));
#228989=CARTESIAN_POINT('Ctrl Pts',(45.122678945944,-44.3985758751927,-232.990284156912));
#228990=CARTESIAN_POINT('Ctrl Pts',(46.9953289795326,-47.3107844763396,
-229.850249364904));
#228991=CARTESIAN_POINT('Ctrl Pts',(48.8702338796761,-50.2209949619586,
-226.709744329754));
#228992=CARTESIAN_POINT('Ctrl Pts',(50.7497258393681,-53.1273622037278,
-223.56843670589));
#228993=CARTESIAN_POINT('Ctrl Pts',(52.62921779906,-56.033729445497,-220.427129082025));
#228994=CARTESIAN_POINT('Ctrl Pts',(54.5128930537055,-58.9365113017985,
-217.285019110898));
#228995=CARTESIAN_POINT('Ctrl Pts',(56.4076769323115,-61.8306798185293,
-214.141539423862));
#228996=CARTESIAN_POINT('Ctrl Pts',(45.457507604722,-43.9326130692061,-232.99254867873));
#228997=CARTESIAN_POINT('Ctrl Pts',(47.3107111022754,-46.8803707732786,
-229.852071833745));
#228998=CARTESIAN_POINT('Ctrl Pts',(49.1663089215364,-49.8260415059931,
-226.711076271479));
#228999=CARTESIAN_POINT('Ctrl Pts',(51.0266279973321,-52.7678256944002,
-223.569232172689));
#229000=CARTESIAN_POINT('Ctrl Pts',(52.8869470731278,-55.7096098828074,
-220.427388073898));
#229001=CARTESIAN_POINT('Ctrl Pts',(54.7516438900022,-58.6477142186619,
-217.284689472746));
#229002=CARTESIAN_POINT('Ctrl Pts',(56.6272059226936,-61.5775733671438,
-214.14063576296));
#229003=CARTESIAN_POINT('Ctrl Pts',(45.7807674564663,-43.4672624822902,
-232.994913812328));
#229004=CARTESIAN_POINT('Ctrl Pts',(47.617410659328,-46.4487812870827,-229.853931471351));
#229005=CARTESIAN_POINT('Ctrl Pts',(49.4565719492878,-49.4281424234071,
-226.71238699417));
#229006=CARTESIAN_POINT('Ctrl Pts',(51.3005099358702,-52.4036466369632,
-223.569971790265));
#229007=CARTESIAN_POINT('Ctrl Pts',(53.1444479224527,-55.3791508505193,
-220.427556586359));
#229008=CARTESIAN_POINT('Ctrl Pts',(54.992887213388,-58.3509530949211,-217.284258923378));
#229009=CARTESIAN_POINT('Ctrl Pts',(56.8516818382195,-61.3150753857701,
-214.139681306367));
#229010=CARTESIAN_POINT('Ctrl Pts',(46.0926567139982,-43.0036690826345,
-232.997311586148));
#229011=CARTESIAN_POINT('Ctrl Pts',(47.9159791152656,-46.0164399058077,
-229.855739900183));
#229012=CARTESIAN_POINT('Ctrl Pts',(49.7419098599322,-49.0270196364001,
-226.713581949947));
#229013=CARTESIAN_POINT('Ctrl Pts',(51.5725780231494,-52.0338565143131,
-223.570570609253));
#229014=CARTESIAN_POINT('Ctrl Pts',(53.4032461863666,-55.0406933922261,
-220.427559268559));
#229015=CARTESIAN_POINT('Ctrl Pts',(55.2384359222485,-58.0439012335412,
-217.283679691665));
#229016=CARTESIAN_POINT('Ctrl Pts',(57.083299585097,-61.0401022731089,-214.13864916931));
#229017=CARTESIAN_POINT('Ctrl Pts',(46.2486013427642,-42.7718723828066,
-232.998510473058));
#229018=CARTESIAN_POINT('Ctrl Pts',(48.0652633432344,-45.8002692151702,
-229.856644114599));
#229019=CARTESIAN_POINT('Ctrl Pts',(49.8845788152544,-48.8264582428966,
-226.714179427834));
#229020=CARTESIAN_POINT('Ctrl Pts',(51.708612066789,-51.848961452988,-223.570870018747));
#229021=CARTESIAN_POINT('Ctrl Pts',(53.5326453183235,-54.8714646630795,
-220.427560609659));
#229022=CARTESIAN_POINT('Ctrl Pts',(55.3612102766787,-57.8903753028513,
-217.283390075808));
#229023=CARTESIAN_POINT('Ctrl Pts',(57.1991084585358,-60.9026157167782,
-214.13813310078));
#229024=CARTESIAN_POINT('Ctrl Pts',(46.4017035779887,-42.5405150976846,
-232.999717286874));
#229025=CARTESIAN_POINT('Ctrl Pts',(48.2125150982371,-45.5839105491989,
-229.857535197574));
#229026=CARTESIAN_POINT('Ctrl Pts',(50.0260166354934,-48.6250910294446,
-226.714747674137));
#229027=CARTESIAN_POINT('Ctrl Pts',(51.844192559889,-51.6626639281839,-223.571133990991));
#229028=CARTESIAN_POINT('Ctrl Pts',(53.6623684842846,-54.7002368269232,
-220.427520307844));
#229029=CARTESIAN_POINT('Ctrl Pts',(55.4850604557961,-57.7342773380644,
-217.283063148945));
#229030=CARTESIAN_POINT('Ctrl Pts',(57.3167022282962,-60.7620113048676,
-214.137597228726));
#229031=CARTESIAN_POINT('Ctrl Pts',(46.5519897086414,-42.3097409936012,
-233.000922137489));
#229032=CARTESIAN_POINT('Ctrl Pts',(48.3578050935127,-45.3674166545976,
-229.858400212826));
#229033=CARTESIAN_POINT('Ctrl Pts',(50.166334738395,-48.4228838232303,-226.715273522923));
#229034=CARTESIAN_POINT('Ctrl Pts',(51.9794693444289,-51.4748446769843,
-223.571351034937));
#229035=CARTESIAN_POINT('Ctrl Pts',(53.7926039504629,-54.5268055307383,
-220.427428546952));
#229036=CARTESIAN_POINT('Ctrl Pts',(55.6102096831407,-57.5753202178,-217.28269273506));
#229037=CARTESIAN_POINT('Ctrl Pts',(57.4363509894997,-60.6179092484165,
-214.137036747929));
#229038=CARTESIAN_POINT('Ctrl Pts',(46.6271327739678,-42.1943539415595,
-233.001524562797));
#229039=CARTESIAN_POINT('Ctrl Pts',(48.4304500911505,-45.2591697072969,
-229.858832720452));
#229040=CARTESIAN_POINT('Ctrl Pts',(50.2364937898458,-48.3217802201232,
-226.715536447315));
#229041=CARTESIAN_POINT('Ctrl Pts',(52.0471077366989,-51.3809350513845,
-223.571459556911));
#229042=CARTESIAN_POINT('Ctrl Pts',(53.857721683552,-54.4400898826458,-220.427382666507));
#229043=CARTESIAN_POINT('Ctrl Pts',(55.672784296813,-57.4958416576678,-217.282507528118));
#229044=CARTESIAN_POINT('Ctrl Pts',(57.4961753701015,-60.5458582201909,
-214.136756507531));
#229045=CARTESIAN_POINT('Ctrl Pts',(46.7015718287581,-42.0791126910049,
-233.00212648283));
#229046=CARTESIAN_POINT('Ctrl Pts',(48.5026046671152,-45.1508889484801,
-229.859258692179));
#229047=CARTESIAN_POINT('Ctrl Pts',(50.3063729152009,-48.2204666245557,
-226.715788761507));
#229048=CARTESIAN_POINT('Ctrl Pts',(52.1146701884246,-51.2866450128194,
-223.571556342237));
#229049=CARTESIAN_POINT('Ctrl Pts',(53.9229674616482,-54.3528234010831,
-220.427323922968));
#229050=CARTESIAN_POINT('Ctrl Pts',(55.7356836352042,-57.4156483458129,
-217.282311452432));
#229051=CARTESIAN_POINT('Ctrl Pts',(57.5565134471849,-60.4729328402728,
-214.136470106837));
#229052=CARTESIAN_POINT('Ctrl Pts',(46.7753102520778,-41.9640352485997,
-233.002726574857));
#229053=CARTESIAN_POINT('Ctrl Pts',(48.5742777683907,-45.0425809377688,
-229.859676400769));
#229054=CARTESIAN_POINT('Ctrl Pts',(50.3759860497308,-48.1189387987811,
-226.716028769071));
#229055=CARTESIAN_POINT('Ctrl Pts',(52.1821753368859,-51.191959764097,-223.571639944857));
#229056=CARTESIAN_POINT('Ctrl Pts',(53.9883646240409,-54.264980729413,-220.427251120643));
#229057=CARTESIAN_POINT('Ctrl Pts',(55.7989353732621,-57.3347046065519,
-217.282103770803));
#229058=CARTESIAN_POINT('Ctrl Pts',(57.6173986625019,-60.3990859831037,
-214.136176919604));
#229059=CARTESIAN_POINT('Ctrl Pts',(46.8121794637376,-41.9064965273971,
-233.003026620871));
#229060=CARTESIAN_POINT('Ctrl Pts',(48.6101143190285,-44.9884269324132,
-229.859885255064));
#229061=CARTESIAN_POINT('Ctrl Pts',(50.4107926169958,-48.0681748858937,
-226.716148772852));
#229062=CARTESIAN_POINT('Ctrl Pts',(52.2159279111165,-51.1446171397359,
-223.571681746167));
#229063=CARTESIAN_POINT('Ctrl Pts',(54.0210632052373,-54.221059393578,-220.427214719482));
#229064=CARTESIAN_POINT('Ctrl Pts',(55.8305612422911,-57.2942327369214,
-217.281999929988));
#229065=CARTESIAN_POINT('Ctrl Pts',(57.6478412701604,-60.3621625545191,
-214.136030325987));
#229066=CARTESIAN_POINT('Ctrl Pts',(46.8488735184923,-41.8489987585935,
-233.003326208986));
#229067=CARTESIAN_POINT('Ctrl Pts',(48.645830502103,-44.9342661136713,-229.860092042457));
#229068=CARTESIAN_POINT('Ctrl Pts',(50.4455326865456,-48.0173574158033,
-226.716265699565));
#229069=CARTESIAN_POINT('Ctrl Pts',(52.2496661584613,-51.0971757139789,
-223.571720251843));
#229070=CARTESIAN_POINT('Ctrl Pts',(54.053799630377,-54.1769940121544,-220.427174804122));
#229071=CARTESIAN_POINT('Ctrl Pts',(55.8622752088309,-57.2535732626049,
-217.281893188185));
#229072=CARTESIAN_POINT('Ctrl Pts',(57.6784206589513,-60.3250087601744,
-214.135882035655));
#229073=CARTESIAN_POINT('Ctrl Pts',(46.8853928444761,-41.791544195152,-233.003625168491));
#229074=CARTESIAN_POINT('Ctrl Pts',(48.681427442577,-44.8800992987762,-229.860296540463));
#229075=CARTESIAN_POINT('Ctrl Pts',(50.4802079998591,-47.9664858608819,
-226.716379335157));
#229076=CARTESIAN_POINT('Ctrl Pts',(52.2833924017896,-51.0496336439922,
-223.57175528194));
#229077=CARTESIAN_POINT('Ctrl Pts',(54.0865768037201,-54.1327814271025,
-220.427131228723));
#229078=CARTESIAN_POINT('Ctrl Pts',(55.8940807177617,-57.2127217368356,
-217.281783456688));
#229079=CARTESIAN_POINT('Ctrl Pts',(57.7091409883845,-60.287618730288,-214.135731970477));
#229080=CARTESIAN_POINT('Ctrl Pts',(46.9219121704599,-41.7340896317106,
-233.003924127997));
#229081=CARTESIAN_POINT('Ctrl Pts',(48.7170243830511,-44.8259324838809,
-229.860501038468));
#229082=CARTESIAN_POINT('Ctrl Pts',(50.5148833131725,-47.9156143059604,
-226.716492970748));
#229083=CARTESIAN_POINT('Ctrl Pts',(52.3171186451179,-51.0020915740055,
-223.571790312035));
#229084=CARTESIAN_POINT('Ctrl Pts',(54.1193539770633,-54.0885688420506,
-220.427087653323));
#229085=CARTESIAN_POINT('Ctrl Pts',(55.9258862266926,-57.1718702110663,
-217.28167372519));
#229086=CARTESIAN_POINT('Ctrl Pts',(57.7398613178177,-60.2502287004015,
-214.1355819053));
#229087=CARTESIAN_POINT('Ctrl Pts',(46.9566286849537,-41.6781739629451,
-233.004786483119));
#229088=CARTESIAN_POINT('Ctrl Pts',(48.7510652266437,-44.7730579825931,
-229.861179418927));
#229089=CARTESIAN_POINT('Ctrl Pts',(50.5482471004081,-47.8657963569279,
-226.716997721658));
#229090=CARTESIAN_POINT('Ctrl Pts',(52.3497454436632,-50.9553990731154,
-223.572150029539));
#229091=CARTESIAN_POINT('Ctrl Pts',(54.1512437869183,-54.045001789303,-220.427302337419));
#229092=CARTESIAN_POINT('Ctrl Pts',(55.9569880950718,-57.1314927928873,
-217.28177244287));
#229093=CARTESIAN_POINT('Ctrl Pts',(57.7699448315789,-60.2132374154909,
-214.135620383829));
#229094=CARTESIAN_POINT('Ctrl Pts',(46.9944270680642,-41.6193123752663,
-233.004519986905));
#229095=CARTESIAN_POINT('Ctrl Pts',(48.7878616654988,-44.7175816808496,
-229.860902939557));
#229096=CARTESIAN_POINT('Ctrl Pts',(50.5840414119712,-47.8137084153908,
-226.716710153573));
#229097=CARTESIAN_POINT('Ctrl Pts',(52.3845374377678,-50.9067036630134,
-223.571849766529));
#229098=CARTESIAN_POINT('Ctrl Pts',(54.1850334635645,-53.999698910636,-220.426989379484));
#229099=CARTESIAN_POINT('Ctrl Pts',(55.9897753069174,-57.0895865666151,
-217.281445207064));
#229100=CARTESIAN_POINT('Ctrl Pts',(57.8017289442242,-60.1747340778167,
-214.135276372889));
#229101=CARTESIAN_POINT('',(42.5905577899916,-59.5881438265759,-225.000659040692));
#229102=CARTESIAN_POINT('Ctrl Pts',(48.0699773995699,-67.6025469094394,
-215.850046920284));
#229103=CARTESIAN_POINT('Ctrl Pts',(47.7935023710083,-67.6024435901635,
-216.017223628435));
#229104=CARTESIAN_POINT('Ctrl Pts',(47.5226056108187,-67.582824338481,-216.193667415816));
#229105=CARTESIAN_POINT('Ctrl Pts',(46.977436852346,-67.5066353741775,-216.573412312879));
#229106=CARTESIAN_POINT('Ctrl Pts',(46.7040353171343,-67.4475753904985,
-216.777867265333));
#229107=CARTESIAN_POINT('Ctrl Pts',(45.9194030179712,-67.2207720759173,
-217.404700028598));
#229108=CARTESIAN_POINT('Ctrl Pts',(45.4358292265538,-67.0029495672137,
-217.845716150032));
#229109=CARTESIAN_POINT('Ctrl Pts',(44.3014622491286,-66.3069334262244,
-219.018073172323));
#229110=CARTESIAN_POINT('Ctrl Pts',(43.7134054388236,-65.7467619649099,
-219.774958898585));
#229111=CARTESIAN_POINT('Ctrl Pts',(42.671590937337,-64.2628736065213,-221.493288736666));
#229112=CARTESIAN_POINT('Ctrl Pts',(42.3167080561812,-63.2947927751779,
-222.43402647705));
#229113=CARTESIAN_POINT('Ctrl Pts',(42.1771404629389,-61.8708033766555,
-223.580484791701));
#229114=CARTESIAN_POINT('Ctrl Pts',(42.1800068789037,-61.4303388698659,
-223.906345139465));
#229115=CARTESIAN_POINT('Ctrl Pts',(42.2949054530161,-60.5240489278744,
-224.504112440003));
#229116=CARTESIAN_POINT('Ctrl Pts',(42.408777306269,-60.0550288946459,-224.777157735681));
#229117=CARTESIAN_POINT('Ctrl Pts',(42.5905622784972,-59.5881432109375,
-225.000654103808));
#229118=CARTESIAN_POINT('Ctrl Pts',(41.9650124840222,-58.9506172433346,
-225.850033985948));
#229119=CARTESIAN_POINT('Ctrl Pts',(42.1735122754178,-59.1631093475985,
-225.566889535856));
#229120=CARTESIAN_POINT('Ctrl Pts',(42.3820244017841,-59.3756157357695,
-225.283764882133));
#229121=CARTESIAN_POINT('Ctrl Pts',(42.590551250619,-59.5881391761779,-225.000663880113));
#229122=CARTESIAN_POINT('Ctrl Pts',(46.0300272746615,-56.2113956834816,
-225.073027562072));
#229123=CARTESIAN_POINT('Ctrl Pts',(46.4556946111428,-56.0546198433881,
-224.882973868584));
#229124=CARTESIAN_POINT('Ctrl Pts',(46.8821025220939,-55.9535510454092,
-224.650935135084));
#229125=CARTESIAN_POINT('Ctrl Pts',(47.8275283497954,-55.8299386675253,
-224.064731751774));
#229126=CARTESIAN_POINT('Ctrl Pts',(48.3429266049596,-55.835913891429,-223.692840875377));
#229127=CARTESIAN_POINT('Ctrl Pts',(49.8207751121238,-56.031385302888,-222.507098599534));
#229128=CARTESIAN_POINT('Ctrl Pts',(50.7673640957262,-56.4134990790704,
-221.576308252714));
#229129=CARTESIAN_POINT('Ctrl Pts',(52.1947859669311,-57.4789725689598,
-219.875568079017));
#229130=CARTESIAN_POINT('Ctrl Pts',(52.7242457809075,-58.0629688538461,
-219.129990774748));
#229131=CARTESIAN_POINT('Ctrl Pts',(53.3981925598294,-59.2055512880101,
-217.935308076124));
#229132=CARTESIAN_POINT('Ctrl Pts',(53.6140169907078,-59.7152280480568,
-217.464070022383));
#229133=CARTESIAN_POINT('Ctrl Pts',(53.823623756443,-60.5278747738901,-216.806115800707));
#229134=CARTESIAN_POINT('Ctrl Pts',(53.8746160000559,-60.8015922181664,
-216.59808676812));
#229135=CARTESIAN_POINT('Ctrl Pts',(53.9357818734408,-61.3524150136747,
-216.207348054255));
#229136=CARTESIAN_POINT('Ctrl Pts',(53.9476675105347,-61.6291888829114,
-216.023694309118));
#229137=CARTESIAN_POINT('Ctrl Pts',(53.9390346875573,-61.9113848028035,
-215.85005));
#229138=CARTESIAN_POINT('Origin',(-296.501483394397,-25.4138432731711,-232.85005));
#229139=CARTESIAN_POINT('Origin',(-296.501483394397,-25.4138432731711,-232.85005));
#229140=CARTESIAN_POINT('Origin',(-296.501483394397,-25.4138432731711,-232.85005));
#229141=CARTESIAN_POINT('Ctrl Pts',(47.8524635552839,9.39108009190695,-232.85005));
#229142=CARTESIAN_POINT('Ctrl Pts',(47.8251207475469,9.27869452829692,-232.85005));
#229143=CARTESIAN_POINT('Ctrl Pts',(47.7988578503937,9.16605178669897,-232.850050000002));
#229144=CARTESIAN_POINT('Ctrl Pts',(47.748545239995,8.94041318528332,-232.850050000002));
#229145=CARTESIAN_POINT('Ctrl Pts',(47.724495099355,8.82742853781197,-232.85005));
#229146=CARTESIAN_POINT('Ctrl Pts',(47.7015450634132,8.71421534318054,-232.85005));
#229147=CARTESIAN_POINT('Origin',(-296.501483394397,-25.4138432731711,-232.85005));
#229148=CARTESIAN_POINT('',(47.8903177140771,0.753846963912772,-232.850053817009));
#229149=CARTESIAN_POINT('',(47.9312868154534,-1.80167576439666,-232.850051862368));
#229150=CARTESIAN_POINT('Origin',(-636.934816028482,-11.5034818258361,-232.85005));
#229151=CARTESIAN_POINT('Ctrl Pts',(47.8903230579921,0.75384761155793,-232.85005));
#229152=CARTESIAN_POINT('Ctrl Pts',(47.9416806402025,0.330080749513371,
-232.85005));
#229153=CARTESIAN_POINT('Ctrl Pts',(47.9708351916769,-0.0957528761675352,
-232.850050000016));
#229154=CARTESIAN_POINT('Ctrl Pts',(47.9845049252711,-0.949121595702693,
-232.850050000016));
#229155=CARTESIAN_POINT('Ctrl Pts',(47.9690400279578,-1.37636719046752,
-232.85005));
#229156=CARTESIAN_POINT('Ctrl Pts',(47.931289209931,-1.8016759769328,-232.85005));
#229157=CARTESIAN_POINT('Origin',(-296.501483394397,-25.4138432731711,-232.85005));
#229158=CARTESIAN_POINT('',(47.9981322791795,-9.91532742768912,-232.850009339772));
#229159=CARTESIAN_POINT('',(47.997728950092,-13.2576713000527,-232.850013208975));
#229160=CARTESIAN_POINT('Origin',(-636.934816028482,-11.5034818258361,-232.85005));
#229161=CARTESIAN_POINT('Ctrl Pts',(47.9981596989455,-9.91572581758462,
-232.85005));
#229162=CARTESIAN_POINT('Ctrl Pts',(48.0735876072948,-10.4686220040327,
-232.85005));
#229163=CARTESIAN_POINT('Ctrl Pts',(48.111732737437,-11.0279091079018,-232.850050000004));
#229164=CARTESIAN_POINT('Ctrl Pts',(48.1116193885485,-12.1445472383142,
-232.850050000004));
#229165=CARTESIAN_POINT('Ctrl Pts',(48.0733656267235,-12.7040603360745,
-232.85005));
#229166=CARTESIAN_POINT('Ctrl Pts',(47.9977546165575,-13.2572998177683,
-232.85005));
#229167=CARTESIAN_POINT('Origin',(-296.501483394397,-25.4138432731711,-232.85005));
#229168=CARTESIAN_POINT('',(47.9291893708826,-21.3522304066337,-232.850051757442));
#229169=CARTESIAN_POINT('',(47.8870567810509,-23.9416215055321,-232.850052596546));
#229170=CARTESIAN_POINT('Origin',(-636.934816028482,-11.5034818258361,-232.85005));
#229171=CARTESIAN_POINT('Ctrl Pts',(47.9291915823105,-21.3522302047528,
-232.85005));
#229172=CARTESIAN_POINT('Ctrl Pts',(47.9685182384575,-21.7830192761799,
-232.85005));
#229173=CARTESIAN_POINT('Ctrl Pts',(47.9846715385175,-22.2158717781124,
-232.850050000025));
#229174=CARTESIAN_POINT('Ctrl Pts',(47.9706154668222,-23.0806717086304,
-232.850050000025));
#229175=CARTESIAN_POINT('Ctrl Pts',(47.9403670434393,-23.5122314437053,
-232.85005));
#229176=CARTESIAN_POINT('Ctrl Pts',(47.8870605128751,-23.9416219688181,
-232.85005));
#229177=CARTESIAN_POINT('Origin',(-296.501483394397,-25.4138432731711,-232.85005));
#229178=CARTESIAN_POINT('Origin',(-296.501483394397,-25.4138432731711,-232.85005));
#229179=CARTESIAN_POINT('Origin',(7.14692237356698E-14,623.509175991979,
-232.85005));
#229180=CARTESIAN_POINT('Origin',(0.128459562639233,-12.6359082483571,-225.85005));
#229181=CARTESIAN_POINT('',(46.7347424436738,30.7127197009669,-225.85005));
#229182=CARTESIAN_POINT('',(53.8170476734233,37.8187794096849,-225.85005));
#229183=CARTESIAN_POINT('Origin',(48.892180948596,36.2913696007177,-225.85005));
#229184=CARTESIAN_POINT('Origin',(-636.934816028482,-11.5034818258361,-234.75005));
#229185=CARTESIAN_POINT('',(47.9849429580539,-16.0452820755244,-232.250052142049));
#229186=CARTESIAN_POINT('Ctrl Pts',(47.9849415007718,-16.0452825742631,
-232.250056396759));
#229187=CARTESIAN_POINT('Ctrl Pts',(47.9880651131551,-15.5742306821435,
-232.306343147701));
#229188=CARTESIAN_POINT('Ctrl Pts',(47.9906783186251,-15.1065446149,-232.390988202577));
#229189=CARTESIAN_POINT('Ctrl Pts',(47.9942849350889,-14.320313988702,-232.579502137916));
#229190=CARTESIAN_POINT('Ctrl Pts',(47.9949617724352,-14.1407707776584,
-232.63620114363));
#229191=CARTESIAN_POINT('Ctrl Pts',(47.9965339240141,-13.6931733666124,
-232.756352689264));
#229192=CARTESIAN_POINT('Ctrl Pts',(47.9971930434381,-13.4765686882966,
-232.806954412833));
#229193=CARTESIAN_POINT('Ctrl Pts',(47.9977536577186,-13.2576742406487,
-232.849976417951));
#229194=CARTESIAN_POINT('',(47.9866836135147,-7.23226647128749,-232.25005191098));
#229195=CARTESIAN_POINT('Ctrl Pts',(47.9866823371376,-7.23226600773658,
-232.250055704934));
#229196=CARTESIAN_POINT('Ctrl Pts',(47.9895098141047,-7.68567315065749,
-232.306404893475));
#229197=CARTESIAN_POINT('Ctrl Pts',(47.9918619737062,-8.13535273752232,
-232.390421945344));
#229198=CARTESIAN_POINT('Ctrl Pts',(47.995107332478,-8.89528528307897,-232.579944924862));
#229199=CARTESIAN_POINT('Ctrl Pts',(47.9956980243111,-9.06520173917856,
-232.636698278921));
#229200=CARTESIAN_POINT('Ctrl Pts',(47.9971000735034,-9.49971705152388,
-232.757828882289));
#229201=CARTESIAN_POINT('Ctrl Pts',(47.9976741114909,-9.70630395457126,
-232.807646456627));
#229202=CARTESIAN_POINT('Ctrl Pts',(47.9981587677023,-9.91532414481652,
-232.849968679543));
#229203=CARTESIAN_POINT('Origin',(-636.934816028482,-11.5034818258361,-232.25005));
#229204=CARTESIAN_POINT('Origin',(-636.934816028482,-11.5034818258361,-234.75005));
#229205=CARTESIAN_POINT('',(47.8275275119674,3.86645886896208,-232.25005));
#229206=CARTESIAN_POINT('',(47.964414121789,-4.51936150138566,-232.250085462548));
#229207=CARTESIAN_POINT('Origin',(-636.934816028482,-11.5034818258361,-232.25005));
#229208=CARTESIAN_POINT('Ctrl Pts',(47.9312856139398,-1.80167637106908,
-232.850055542859));
#229209=CARTESIAN_POINT('Ctrl Pts',(47.9394982187954,-2.38141739947619,
-232.757175193342));
#229210=CARTESIAN_POINT('Ctrl Pts',(47.9438448367591,-2.72209125825006,
-232.634139478141));
#229211=CARTESIAN_POINT('Ctrl Pts',(47.9546121728049,-3.60581024688955,
-232.397143115093));
#229212=CARTESIAN_POINT('Ctrl Pts',(47.9597127880174,-4.06055719278633,
-232.308472253132));
#229213=CARTESIAN_POINT('Ctrl Pts',(47.9643913372341,-4.51935999242227,
-232.250120925096));
#229214=CARTESIAN_POINT('Ctrl Pts',(47.8275275119675,3.86645886896215,-232.250050000001));
#229215=CARTESIAN_POINT('Ctrl Pts',(47.8393033810286,3.34181977921867,-232.308606692494));
#229216=CARTESIAN_POINT('Ctrl Pts',(47.8504216708135,2.81940125771994,-232.399682736104));
#229217=CARTESIAN_POINT('Ctrl Pts',(47.8640428170577,2.14390431818647,-232.555058644712));
#229218=CARTESIAN_POINT('Ctrl Pts',(47.8678682595302,1.94983002712611,-232.604470061216));
#229219=CARTESIAN_POINT('Ctrl Pts',(47.8765736965627,1.50418121395801,-232.718114713146));
#229220=CARTESIAN_POINT('Ctrl Pts',(47.8835694576844,1.13072531539176,-232.79486347822));
#229221=CARTESIAN_POINT('Ctrl Pts',(47.8903149889077,0.753848021453941,
-232.850061370667));
#229222=CARTESIAN_POINT('Origin',(-636.934816028482,-11.5034818258361,-234.75005));
#229223=CARTESIAN_POINT('',(47.7599172087245,-29.6370001055535,-232.25005));
#229224=CARTESIAN_POINT('Ctrl Pts',(47.7599172087245,-29.6370001055535,
-232.25005));
#229225=CARTESIAN_POINT('Ctrl Pts',(47.7493722429097,-30.0351623619991,
-232.296082730074));
#229226=CARTESIAN_POINT('Ctrl Pts',(47.7385258657941,-30.4314329746859,
-232.367779772163));
#229227=CARTESIAN_POINT('Ctrl Pts',(47.7172003916566,-31.187345806892,-232.567309385582));
#229228=CARTESIAN_POINT('Ctrl Pts',(47.7067067250054,-31.5486321455587,
-232.692442513232));
#229229=CARTESIAN_POINT('Ctrl Pts',(47.6963708708293,-31.895640436697,-232.849812673883));
#229230=CARTESIAN_POINT('Origin',(-636.934816028482,-11.5034818258361,-232.25005));
#229231=CARTESIAN_POINT('Origin',(-636.934816028482,-11.5034818258361,-234.75005));
#229232=CARTESIAN_POINT('',(47.9620917742134,-18.7116135554145,-232.250083778217));
#229233=CARTESIAN_POINT('',(47.8203127443142,-27.1915604710334,-232.250049983782));
#229234=CARTESIAN_POINT('Origin',(-636.934816028482,-11.5034818258361,-232.25005));
#229235=CARTESIAN_POINT('Ctrl Pts',(47.8870548777005,-23.9416222224618,
-232.850057734118));
#229236=CARTESIAN_POINT('Ctrl Pts',(47.8808419217875,-24.2836965162462,
-232.800020744849));
#229237=CARTESIAN_POINT('Ctrl Pts',(47.8744102330396,-24.6236650946738,
-232.733213391966));
#229238=CARTESIAN_POINT('Ctrl Pts',(47.8666304747006,-25.0195680911603,
-232.639069109827));
#229239=CARTESIAN_POINT('Ctrl Pts',(47.8654339475289,-25.0799470332769,
-232.624108273732));
#229240=CARTESIAN_POINT('Ctrl Pts',(47.8619240948933,-25.2566749049009,
-232.580479584125));
#229241=CARTESIAN_POINT('Ctrl Pts',(47.8588236469908,-25.4102068712725,
-232.544854491086));
#229242=CARTESIAN_POINT('Ctrl Pts',(47.8446425337259,-26.1008593428925,
-232.395217345887));
#229243=CARTESIAN_POINT('Ctrl Pts',(47.8328230396433,-26.6455101093032,
-232.305849122883));
#229244=CARTESIAN_POINT('Ctrl Pts',(47.8203127558795,-27.1915604680009,
-232.250049951514));
#229245=CARTESIAN_POINT('Ctrl Pts',(47.9620703905618,-18.7116148344343,
-232.250117556434));
#229246=CARTESIAN_POINT('Ctrl Pts',(47.9573554139265,-19.1596188894641,
-232.306669891439));
#229247=CARTESIAN_POINT('Ctrl Pts',(47.9522383472777,-19.6037872884333,
-232.393382749302));
#229248=CARTESIAN_POINT('Ctrl Pts',(47.9411866433024,-20.4904993022866,
-232.635960657363));
#229249=CARTESIAN_POINT('Ctrl Pts',(47.937212253039,-20.7942559961686,-232.756243969882));
#229250=CARTESIAN_POINT('Ctrl Pts',(47.9291882608127,-21.3522298073388,
-232.850055227));
#229251=CARTESIAN_POINT('Origin',(7.14692237356698E-14,623.509175991979,
-234.75005));
#229252=CARTESIAN_POINT('Origin',(7.14692237356698E-14,623.509175991979,
-232.25005));
#229253=CARTESIAN_POINT('Origin',(49.9798730220992,-67.1190133783941,-228.35005));
#229254=CARTESIAN_POINT('',(42.5792116384512,-59.576583500476,-225.85005));
#229255=CARTESIAN_POINT('Origin',(48.892180948596,36.2913696007177,-218.306418983907));
#229256=CARTESIAN_POINT('',(46.7347424436738,30.7127197009669,-225.85005));
#229257=CARTESIAN_POINT('Origin',(53.8170476734233,37.8187794096849,-228.35005));
#229258=CARTESIAN_POINT('Ctrl Pts',(47.6009947863409,-32.6895605159758,
-233.446187702606));
#229259=CARTESIAN_POINT('Ctrl Pts',(49.8025157165519,-35.2628848633458,
-230.069700789871));
#229260=CARTESIAN_POINT('Ctrl Pts',(52.004194845104,-37.8467163541935,-226.701486649479));
#229261=CARTESIAN_POINT('Ctrl Pts',(54.2056301169259,-40.4346768564372,
-223.336322656971));
#229262=CARTESIAN_POINT('Ctrl Pts',(56.4070653887478,-43.0226373586808,
-219.971158664462));
#229263=CARTESIAN_POINT('Ctrl Pts',(58.6083138625641,-45.6150709680905,
-216.609349785985));
#229264=CARTESIAN_POINT('Ctrl Pts',(60.8093841578956,-48.2097095522884,
-213.249138279223));
#229265=CARTESIAN_POINT('Ctrl Pts',(47.1654872359782,-30.7268333335968,
-233.215238694904));
#229266=CARTESIAN_POINT('Ctrl Pts',(49.3424661286879,-33.1216582244425,
-229.854296748355));
#229267=CARTESIAN_POINT('Ctrl Pts',(51.5175746565146,-35.5225299367126,
-226.496223095384));
#229268=CARTESIAN_POINT('Ctrl Pts',(53.691970049721,-37.9257105515243,-223.139241204672));
#229269=CARTESIAN_POINT('Ctrl Pts',(55.8663654429275,-40.3288911663362,
-219.782259313959));
#229270=CARTESIAN_POINT('Ctrl Pts',(58.0399820141948,-42.7345941518082,
-216.426471773175));
#229271=CARTESIAN_POINT('Ctrl Pts',(60.2132186858487,-45.1415311212291,
-213.071269036894));
#229272=CARTESIAN_POINT('Ctrl Pts',(47.0914518599014,-28.7082056053768,
-233.076532045377));
#229273=CARTESIAN_POINT('Ctrl Pts',(49.2577871721353,-30.9207984180132,
-229.722627951761));
#229274=CARTESIAN_POINT('Ctrl Pts',(51.4233225017517,-33.1352914201321,
-226.36927473658));
#229275=CARTESIAN_POINT('Ctrl Pts',(53.588559980291,-35.3505224606949,-223.016143793358));
#229276=CARTESIAN_POINT('Ctrl Pts',(55.7537974588302,-37.5657535012578,
-219.663012850137));
#229277=CARTESIAN_POINT('Ctrl Pts',(57.9187078478837,-39.7817869473385,
-216.310121456173));
#229278=CARTESIAN_POINT('Ctrl Pts',(60.0834610972678,-41.9982150734171,
-212.9573503068));
#229279=CARTESIAN_POINT('Ctrl Pts',(47.338918326904,-26.7547399443242,-232.989202284253));
#229280=CARTESIAN_POINT('Ctrl Pts',(49.5169190710851,-28.779613867576,-229.63849750905));
#229281=CARTESIAN_POINT('Ctrl Pts',(51.6953679974136,-30.8032553785755,
-226.287341083189));
#229282=CARTESIAN_POINT('Ctrl Pts',(53.8739882225852,-32.826417079771,-222.936006744139));
#229283=CARTESIAN_POINT('Ctrl Pts',(56.0526084477568,-34.8495787809666,
-219.584672405089));
#229284=CARTESIAN_POINT('Ctrl Pts',(58.2314156201025,-36.8722190976995,
-216.233145260744));
#229285=CARTESIAN_POINT('Ctrl Pts',(60.4103139494413,-38.8946025877681,
-212.88152253822));
#229286=CARTESIAN_POINT('Ctrl Pts',(47.4007849436546,-26.2663735290611,
-232.967369843972));
#229287=CARTESIAN_POINT('Ctrl Pts',(49.5817020458226,-28.2443177299668,
-229.617464898372));
#229288=CARTESIAN_POINT('Ctrl Pts',(51.7633793713291,-30.2202463681864,
-226.266857669841));
#229289=CARTESIAN_POINT('Ctrl Pts',(53.9453452831587,-32.19539073454,-222.915972481834));
#229290=CARTESIAN_POINT('Ctrl Pts',(56.1273111949884,-34.1705351008938,
-219.565087293826));
#229291=CARTESIAN_POINT('Ctrl Pts',(58.3095925631572,-36.1448271352898,
-216.213901211887));
#229292=CARTESIAN_POINT('Ctrl Pts',(60.4920271624846,-38.1186994663558,
-212.862565596074));
#229293=CARTESIAN_POINT('Ctrl Pts',(47.4827081594745,-25.7820909390022,
-232.948908323096));
#229294=CARTESIAN_POINT('Ctrl Pts',(49.667931620883,-27.7127600601,-229.599541574634));
#229295=CARTESIAN_POINT('Ctrl Pts',(51.854254699843,-29.6406887254791,-226.249310199414));
#229296=CARTESIAN_POINT('Ctrl Pts',(54.0409905357308,-31.5675524127984,
-222.898733386289));
#229297=CARTESIAN_POINT('Ctrl Pts',(56.2277263716187,-33.4944161001178,
-219.548156573164));
#229298=CARTESIAN_POINT('Ctrl Pts',(58.4149145994856,-35.4201220699693,
-216.197206631876));
#229299=CARTESIAN_POINT('Ctrl Pts',(60.6023211750695,-37.3452584113098,
-212.84607035725));
#229300=CARTESIAN_POINT('Ctrl Pts',(47.5841424907316,-25.3031332383162,
-232.93329091056));
#229301=CARTESIAN_POINT('Ctrl Pts',(49.7751430286533,-27.1862918963392,
-229.584271284343));
#229302=CARTESIAN_POINT('Ctrl Pts',(51.9676091114587,-29.0660086976874,
-226.234288856273));
#229303=CARTESIAN_POINT('Ctrl Pts',(54.1606184685044,-30.9443917197372,
-222.883917182185));
#229304=CARTESIAN_POINT('Ctrl Pts',(56.3536278255502,-32.822774741787,-219.533545508098));
#229305=CARTESIAN_POINT('Ctrl Pts',(58.5472344262499,-34.6997069346566,
-216.182754549711));
#229306=CARTESIAN_POINT('Ctrl Pts',(60.7411272633344,-36.5759265044021,
-212.831752983035));
#229307=CARTESIAN_POINT('Ctrl Pts',(47.6095010735459,-25.1833938131447,
-232.929386557426));
#229308=CARTESIAN_POINT('Ctrl Pts',(49.8019458805959,-27.054674855399,-229.58045371177));
#229309=CARTESIAN_POINT('Ctrl Pts',(51.9959477143626,-28.9223386907395,
-226.230533520487));
#229310=CARTESIAN_POINT('Ctrl Pts',(54.1905254516978,-30.7886015464719,
-222.88021313116));
#229311=CARTESIAN_POINT('Ctrl Pts',(56.3851031890331,-32.6548644022043,
-219.529892741831));
#229312=CARTESIAN_POINT('Ctrl Pts',(58.5803143829409,-34.5196031508285,
-216.179141529169));
#229313=CARTESIAN_POINT('Ctrl Pts',(60.7758287854006,-36.3835935276752,
-212.828173639481));
#229314=CARTESIAN_POINT('Ctrl Pts',(47.6360799530631,-25.0639872883753,
-232.925661119858));
#229315=CARTESIAN_POINT('Ctrl Pts',(49.8300607835295,-26.9233759839715,
-229.576802907687));
#229316=CARTESIAN_POINT('Ctrl Pts',(52.0256918558292,-28.7789735949605,
-226.226936900208));
#229317=CARTESIAN_POINT('Ctrl Pts',(54.2219318772968,-30.6331037731025,
-222.876661247257));
#229318=CARTESIAN_POINT('Ctrl Pts',(56.4181718987644,-32.4872339512444,
-219.526385594307));
#229319=CARTESIAN_POINT('Ctrl Pts',(58.6150821083144,-34.339767514325,-216.175669238136));
#229320=CARTESIAN_POINT('Ctrl Pts',(60.8123126810755,-36.1915173917436,
-212.824730931321));
#229321=CARTESIAN_POINT('Ctrl Pts',(47.6638721879803,-24.9449332806664,
-232.922108625287));
#229322=CARTESIAN_POINT('Ctrl Pts',(49.8594817505659,-26.7924165735007,
-229.57331360468));
#229323=CARTESIAN_POINT('Ctrl Pts',(52.0568366301129,-28.6359358440905,
-226.223494218563));
#229324=CARTESIAN_POINT('Ctrl Pts',(54.2548339484627,-30.4779217969194,
-222.873257153795));
#229325=CARTESIAN_POINT('Ctrl Pts',(56.4528312668125,-32.3199077497483,
-219.523020089027));
#229326=CARTESIAN_POINT('Ctrl Pts',(58.6515360594894,-34.1602251482123,
-216.172334004182));
#229327=CARTESIAN_POINT('Ctrl Pts',(60.85057856534,-35.9997238912687,-212.821421441686));
#229328=CARTESIAN_POINT('Ctrl Pts',(47.6656092026626,-24.9374924051846,
-232.921886594377));
#229329=CARTESIAN_POINT('Ctrl Pts',(49.8613205610057,-26.7842316103463,
-229.573095523243));
#229330=CARTESIAN_POINT('Ctrl Pts',(52.0587831785056,-28.6269959846611,
-226.223279050959));
#229331=CARTESIAN_POINT('Ctrl Pts',(54.2568903279106,-30.468222923408,-222.873044397953));
#229332=CARTESIAN_POINT('Ctrl Pts',(56.4549974773155,-32.3094498621548,
-219.522809744947));
#229333=CARTESIAN_POINT('Ctrl Pts',(58.6538144314378,-34.1490037503303,
-216.17212555206));
#229334=CARTESIAN_POINT('Ctrl Pts',(60.8529701831065,-35.987736797489,-212.821214598585));
#229335=CARTESIAN_POINT('Ctrl Pts',(47.6673509571934,-24.9300529067585,
-232.921665239305));
#229336=CARTESIAN_POINT('Ctrl Pts',(49.8631644734026,-26.7760479732408,
-229.5728780729));
#229337=CARTESIAN_POINT('Ctrl Pts',(52.0607351982457,-28.6180574039478,
-226.223064484881));
#229338=CARTESIAN_POINT('Ctrl Pts',(54.2589525498347,-30.4585252835005,
-222.872832219598));
#229339=CARTESIAN_POINT('Ctrl Pts',(56.4571699014236,-32.2989931630532,
-219.522599954314));
#229340=CARTESIAN_POINT('Ctrl Pts',(58.6560993902921,-34.1377834980502,
-216.171917635457));
#229341=CARTESIAN_POINT('Ctrl Pts',(60.8553687618446,-35.9757508077661,
-212.821008275995));
#229342=CARTESIAN_POINT('Ctrl Pts',(47.6690974499491,-24.9226147901915,
-232.921444558725));
#229343=CARTESIAN_POINT('Ctrl Pts',(49.8650134863522,-26.7678656673941,
-229.572661252457));
#229344=CARTESIAN_POINT('Ctrl Pts',(52.0626926881854,-28.6091201074371,
-226.222850519243));
#229345=CARTESIAN_POINT('Ctrl Pts',(54.261020613352,-30.4488288829175,-222.87262061773));
#229346=CARTESIAN_POINT('Ctrl Pts',(56.4593485385187,-32.2885376583978,
-219.522390716218));
#229347=CARTESIAN_POINT('Ctrl Pts',(58.65839093571,-34.1265643975113,-216.171710253535));
#229348=CARTESIAN_POINT('Ctrl Pts',(60.8577743014912,-35.9637659284024,
-212.820802473134));
#229349=CARTESIAN_POINT('Ctrl Pts',(47.6708439427048,-24.9151766736244,
-232.921223878144));
#229350=CARTESIAN_POINT('Ctrl Pts',(49.8668624993017,-26.7596833615473,
-229.572444432014));
#229351=CARTESIAN_POINT('Ctrl Pts',(52.064650178125,-28.6001828109265,-226.222636553605));
#229352=CARTESIAN_POINT('Ctrl Pts',(54.2630886768694,-30.4391324823344,
-222.872409015864));
#229353=CARTESIAN_POINT('Ctrl Pts',(56.4615271756139,-32.2780821537422,
-219.522181478123));
#229354=CARTESIAN_POINT('Ctrl Pts',(58.6606824811278,-34.1153452969724,
-216.171502871612));
#229355=CARTESIAN_POINT('Ctrl Pts',(60.8601798411379,-35.9517810490386,
-212.820596670274));
#229356=CARTESIAN_POINT('Ctrl Pts',(47.6712594337893,-24.9108968675569,
-232.921857349187));
#229357=CARTESIAN_POINT('Ctrl Pts',(49.8674442055454,-26.7545468321646,
-229.573062291402));
#229358=CARTESIAN_POINT('Ctrl Pts',(52.0653826207377,-28.5942132778735,
-226.223242591862));
#229359=CARTESIAN_POINT('Ctrl Pts',(54.2639659675545,-30.4323399214299,
-222.873005200592));
#229360=CARTESIAN_POINT('Ctrl Pts',(56.4625493143714,-32.2704665649863,
-219.522767809321));
#229361=CARTESIAN_POINT('Ctrl Pts',(58.6618430388141,-34.1069173291204,
-216.172081363551));
#229362=CARTESIAN_POINT('Ctrl Pts',(60.8614757011049,-35.9425461532316,
-212.821168459392));
#229363=CARTESIAN_POINT('Ctrl Pts',(47.6722605345507,-24.9052129322023,
-232.922111326828));
#229364=CARTESIAN_POINT('Ctrl Pts',(49.8685827056453,-26.7480556997355,
-229.573309285042));
#229365=CARTESIAN_POINT('Ctrl Pts',(52.0666525755381,-28.5869233597964,
-226.223484274919));
#229366=CARTESIAN_POINT('Ctrl Pts',(54.2653650437259,-30.4242549380612,
-222.873242451443));
#229367=CARTESIAN_POINT('Ctrl Pts',(56.4640775119137,-32.2615865163259,
-219.523000627968));
#229368=CARTESIAN_POINT('Ctrl Pts',(58.6634978294311,-34.0972461434794,
-216.172310647723));
#229369=CARTESIAN_POINT('Ctrl Pts',(60.8632558396737,-35.9320858909674,
-212.821394718674));
#229370=CARTESIAN_POINT('Ctrl Pts',(47.6742627360736,-24.8938450614933,
-232.922619282109));
#229371=CARTESIAN_POINT('Ctrl Pts',(49.8708597058451,-26.7350734348772,
-229.573803272322));
#229372=CARTESIAN_POINT('Ctrl Pts',(52.069192485139,-28.5723435236424,-226.223967641033));
#229373=CARTESIAN_POINT('Ctrl Pts',(54.2681631960686,-30.4080849713239,
-222.873716953146));
#229374=CARTESIAN_POINT('Ctrl Pts',(56.4671339069982,-32.2438264190054,
-219.523466265261));
#229375=CARTESIAN_POINT('Ctrl Pts',(58.666807410665,-34.0779037721973,-216.172769216067));
#229376=CARTESIAN_POINT('Ctrl Pts',(60.8668161168113,-35.9111653664389,
-212.821847237238));
#229377=CARTESIAN_POINT('Ctrl Pts',(47.6762483602964,-24.8824767178353,
-232.923127796013));
#229378=CARTESIAN_POINT('Ctrl Pts',(49.8731187515493,-26.722089328055,-229.574297740375));
#229379=CARTESIAN_POINT('Ctrl Pts',(52.0717130787027,-28.557760578718,-226.224451450989));
#229380=CARTESIAN_POINT('Ctrl Pts',(54.2709406860775,-30.3919106496837,
-222.874191872023));
#229381=CARTESIAN_POINT('Ctrl Pts',(56.4701682934522,-32.2260607206496,
-219.523932293058));
#229382=CARTESIAN_POINT('Ctrl Pts',(58.6700936511245,-34.0585545809213,
-216.173228160698));
#229383=CARTESIAN_POINT('Ctrl Pts',(60.8703517304133,-35.8902368104956,
-212.822300122054));
#229384=CARTESIAN_POINT('Ctrl Pts',(47.6782174267913,-24.8711079134889,
-232.92363686464));
#229385=CARTESIAN_POINT('Ctrl Pts',(49.8753598495424,-26.7091034156505,
-229.574792687293));
#229386=CARTESIAN_POINT('Ctrl Pts',(52.0742143523489,-28.5431745827215,
-226.224935704284));
#229387=CARTESIAN_POINT('Ctrl Pts',(54.2736974997456,-30.3757320511356,
-222.874667208678));
#229388=CARTESIAN_POINT('Ctrl Pts',(56.4731806471424,-32.2082895195496,
-219.524398713072));
#229389=CARTESIAN_POINT('Ctrl Pts',(58.6733565172052,-34.0391986871267,
-216.173687484148));
#229390=CARTESIAN_POINT('Ctrl Pts',(60.8738626376389,-35.8693003593042,
-212.822753376317));
#229391=CARTESIAN_POINT('Ctrl Pts',(47.6821555597811,-24.8483703047961,
-232.924655001894));
#229392=CARTESIAN_POINT('Ctrl Pts',(49.8798420455288,-26.6831315908415,
-229.575782581129));
#229393=CARTESIAN_POINT('Ctrl Pts',(52.0792168996413,-28.5140025907287,
-226.225904210874));
#229394=CARTESIAN_POINT('Ctrl Pts',(54.2792111270821,-30.3433748540391,
-222.875617881988));
#229395=CARTESIAN_POINT('Ctrl Pts',(56.4792053545228,-32.1727471173495,
-219.525331553101));
#229396=CARTESIAN_POINT('Ctrl Pts',(58.6798822493665,-34.0004868995374,
-216.174606131045));
#229397=CARTESIAN_POINT('Ctrl Pts',(60.88088445209,-35.8274274569215,-212.823659884843));
#229398=CARTESIAN_POINT('Ctrl Pts',(47.6860274619745,-24.8256308534282,
-232.925675358015));
#229399=CARTESIAN_POINT('Ctrl Pts',(49.8842524507179,-26.657152543721,-229.576774390365));
#229400=CARTESIAN_POINT('Ctrl Pts',(52.0841421672651,-28.4848183944506,
-226.22687449075));
#229401=CARTESIAN_POINT('Ctrl Pts',(54.2846420490225,-30.3110005493018,
-222.876570226337));
#229402=CARTESIAN_POINT('Ctrl Pts',(56.4851419307799,-32.1371827041529,
-219.526265961925));
#229403=CARTESIAN_POINT('Ctrl Pts',(58.6863144839206,-33.9617483018504,
-216.17552629313));
#229404=CARTESIAN_POINT('Ctrl Pts',(60.887807440924,-35.7855229735214,-212.824567871073));
#229405=CARTESIAN_POINT('Ctrl Pts',(47.6898332885707,-24.8028896565292,
-232.926697902178));
#229406=CARTESIAN_POINT('Ctrl Pts',(49.8885911188174,-26.6311665651389,
-229.577768100455));
#229407=CARTESIAN_POINT('Ctrl Pts',(52.0889901241519,-28.455622455455,-226.227846540711));
#229408=CARTESIAN_POINT('Ctrl Pts',(54.2899901539046,-30.2786097609959,
-222.877524247479));
#229409=CARTESIAN_POINT('Ctrl Pts',(56.4909901836572,-32.1015970665369,
-219.527201954246));
#229410=CARTESIAN_POINT('Ctrl Pts',(58.6926529531334,-33.9229838341469,
-216.176447991634));
#229411=CARTESIAN_POINT('Ctrl Pts',(60.8946312627443,-35.7435879987355,
-212.825477361568));
#229412=CARTESIAN_POINT('Ctrl Pts',(47.6974449417632,-24.7574072627311,
-232.928742990504));
#229413=CARTESIAN_POINT('Ctrl Pts',(49.8972684550162,-26.5791946079747,
-229.579755520635));
#229414=CARTESIAN_POINT('Ctrl Pts',(52.0986860379256,-28.3972305774635,
-226.229790640633));
#229415=CARTESIAN_POINT('Ctrl Pts',(54.3006863636687,-30.2138281843841,
-222.879432289762));
#229416=CARTESIAN_POINT('Ctrl Pts',(56.5026866894118,-32.0304257913048,
-219.529073938891));
#229417=CARTESIAN_POINT('Ctrl Pts',(58.705329891559,-33.8454548987401,-216.178291388644));
#229418=CARTESIAN_POINT('Ctrl Pts',(60.9082789063849,-35.6597180491639,
-212.827296342558));
#229419=CARTESIAN_POINT('Ctrl Pts',(47.7047922944592,-24.7119178879782,
-232.930796830484));
#229420=CARTESIAN_POINT('Ctrl Pts',(49.9056588436001,-26.5271949252194,
-229.581750543243));
#229421=CARTESIAN_POINT('Ctrl Pts',(52.1080727087613,-28.3387917286268,
-226.231741819771));
#229422=CARTESIAN_POINT('Ctrl Pts',(54.3110513046474,-30.1489806733496,
-222.881347038));
#229423=CARTESIAN_POINT('Ctrl Pts',(56.5140299005335,-31.9591696180724,
-219.530952256228));
#229424=CARTESIAN_POINT('Ctrl Pts',(58.7176317671225,-33.7678224828936,
-216.180140930006));
#229425=CARTESIAN_POINT('Ctrl Pts',(60.9215298801705,-35.5757261336416,
-212.829121339267));
#229426=CARTESIAN_POINT('Ctrl Pts',(47.7118765658424,-24.6664222949089,
-232.932859181476));
#229427=CARTESIAN_POINT('Ctrl Pts',(49.9137627052303,-26.4751698404963,
-229.583753063685));
#229428=CARTESIAN_POINT('Ctrl Pts',(52.1171498878757,-28.280309601158,-226.233700065929));
#229429=CARTESIAN_POINT('Ctrl Pts',(54.321084090016,-30.084072222256,-222.883268552734));
#229430=CARTESIAN_POINT('Ctrl Pts',(56.5250182921564,-31.887834843354,-219.53283703954));
#229431=CARTESIAN_POINT('Ctrl Pts',(58.7295564557497,-33.6900941117383,
-216.181996801466));
#229432=CARTESIAN_POINT('Ctrl Pts',(60.9343814743951,-35.4916209740569,
-212.830952580145));
#229433=CARTESIAN_POINT('Ctrl Pts',(47.740213651375,-24.4844399226315,-232.941108585445));
#229434=CARTESIAN_POINT('Ctrl Pts',(49.9461781517511,-26.2670695016037,
-229.591763145452));
#229435=CARTESIAN_POINT('Ctrl Pts',(52.1534586043331,-28.0463810912831,
-226.241533050557));
#229436=CARTESIAN_POINT('Ctrl Pts',(54.3612152314905,-29.8244384178816,
-222.890954611672));
#229437=CARTESIAN_POINT('Ctrl Pts',(56.5689718586478,-31.6024957444801,
-219.540376172787));
#229438=CARTESIAN_POINT('Ctrl Pts',(58.7772552102583,-33.379180627117,-216.189420287308));
#229439=CARTESIAN_POINT('Ctrl Pts',(60.9857878512938,-35.1552003357181,
-212.838277543654));
#229440=CARTESIAN_POINT('Ctrl Pts',(47.764342072931,-24.3023583702358,-232.949493972115));
#229441=CARTESIAN_POINT('Ctrl Pts',(49.974009394549,-26.0585628024136,-229.599892861619));
#229442=CARTESIAN_POINT('Ctrl Pts',(52.1848154405255,-27.8117601296424,
-226.249478738948));
#229443=CARTESIAN_POINT('Ctrl Pts',(54.3960316866775,-29.5638295270311,
-222.898748539061));
#229444=CARTESIAN_POINT('Ctrl Pts',(56.6072479328295,-31.3158989244199,
-219.548018339173));
#229445=CARTESIAN_POINT('Ctrl Pts',(58.8189184722057,-33.0667317389572,
-216.196944624725));
#229446=CARTESIAN_POINT('Ctrl Pts',(61.0308035579046,-34.8169676574521,
-212.845701979688));
#229447=CARTESIAN_POINT('Ctrl Pts',(47.7843348584855,-24.1202237497555,
-232.95800139794));
#229448=CARTESIAN_POINT('Ctrl Pts',(49.99728150262,-25.8497978524297,-229.608138122646));
#229449=CARTESIAN_POINT('Ctrl Pts',(52.2112045262045,-27.5766829623168,
-226.257539270556));
#229450=CARTESIAN_POINT('Ctrl Pts',(54.4254782083431,-29.3025655601605,
-222.906657351959));
#229451=CARTESIAN_POINT('Ctrl Pts',(56.6397518904817,-31.0284481580042,
-219.555775433364));
#229452=CARTESIAN_POINT('Ctrl Pts',(58.8544142415175,-32.7532300084283,
-216.204585123186));
#229453=CARTESIAN_POINT('Ctrl Pts',(61.0692598838066,-34.4774822060492,
-212.853243959114));
#229454=CARTESIAN_POINT('Ctrl Pts',(47.8643060007033,-23.3916852678342,
-232.992031101241));
#229455=CARTESIAN_POINT('Ctrl Pts',(50.090369934904,-25.0147380524944,-229.641119166754));
#229456=CARTESIAN_POINT('Ctrl Pts',(52.3167608689203,-26.6363742930146,
-226.289781396988));
#229457=CARTESIAN_POINT('Ctrl Pts',(54.5432642950053,-28.2575096926779,
-222.938292603557));
#229458=CARTESIAN_POINT('Ctrl Pts',(56.7697677210903,-29.8786450923411,
-219.586803810126));
#229459=CARTESIAN_POINT('Ctrl Pts',(58.9963973187644,-31.499223086313,-216.235147117033));
#229460=CARTESIAN_POINT('Ctrl Pts',(61.2230851874141,-33.1195404004377,
-212.883411876817));
#229461=CARTESIAN_POINT('Ctrl Pts',(47.878298880158,-22.6624540792437,-233.028057892109));
#229462=CARTESIAN_POINT('Ctrl Pts',(50.1105261899139,-24.1755656136661,
-229.675981641008));
#229463=CARTESIAN_POINT('Ctrl Pts',(52.3426487730065,-25.6886770024113,
-226.323884260853));
#229464=CARTESIAN_POINT('Ctrl Pts',(54.5747380925437,-27.201784204638,-222.971780574238));
#229465=CARTESIAN_POINT('Ctrl Pts',(56.8068274120809,-28.7148914068648,
-219.619676887624));
#229466=CARTESIAN_POINT('Ctrl Pts',(59.0388786006661,-30.2279951799507,
-216.267565846653));
#229467=CARTESIAN_POINT('Ctrl Pts',(61.2709129905723,-31.7410962361218,
-212.915451703421));
#229468=CARTESIAN_POINT('Ctrl Pts',(47.8281547001989,-21.9381226823642,
-233.066054879848));
#229469=CARTESIAN_POINT('Ctrl Pts',(50.0590295861697,-23.3420565686501,
-229.712518150776));
#229470=CARTESIAN_POINT('Ctrl Pts',(52.2896542767201,-24.7475525298228,
-226.359471317301));
#229471=CARTESIAN_POINT('Ctrl Pts',(54.5201844975327,-26.1536136226082,
-223.006599089445));
#229472=CARTESIAN_POINT('Ctrl Pts',(56.7507147183453,-27.5596747153937,
-219.653726861588));
#229473=CARTESIAN_POINT('Ctrl Pts',(58.9811415508881,-28.9663610919618,
-216.301048580499));
#229474=CARTESIAN_POINT('Ctrl Pts',(61.2115183316506,-30.3733436736124,
-212.948461459071));
#229475=CARTESIAN_POINT('Ctrl Pts',(47.8030826102193,-21.5759569839245,
-233.085053373718));
#229476=CARTESIAN_POINT('Ctrl Pts',(50.0332812842976,-22.9253020461421,
-229.730786405659));
#229477=CARTESIAN_POINT('Ctrl Pts',(52.2631570285769,-24.2769902935286,
-226.377264845526));
#229478=CARTESIAN_POINT('Ctrl Pts',(54.4929077000272,-25.6295283315933,
-223.024008347048));
#229479=CARTESIAN_POINT('Ctrl Pts',(56.7226583714774,-26.9820663696581,
-219.67075184857));
#229480=CARTESIAN_POINT('Ctrl Pts',(58.9522730259992,-28.3355440479673,
-216.317789947423));
#229481=CARTESIAN_POINT('Ctrl Pts',(61.1818210021897,-29.6894673923576,
-212.964966336897));
#229482=CARTESIAN_POINT('Ctrl Pts',(47.761964930595,-21.2148494647643,-233.104496710832));
#229483=CARTESIAN_POINT('Ctrl Pts',(49.9896217363213,-22.5099538605863,
-229.749470483377));
#229484=CARTESIAN_POINT('Ctrl Pts',(52.2169611837896,-23.8081676354522,
-226.395455605453));
#229485=CARTESIAN_POINT('Ctrl Pts',(54.4441695190511,-25.1075159192911,
-223.041799887511));
#229486=CARTESIAN_POINT('Ctrl Pts',(56.6713778543125,-26.4068642031302,
-219.688144169568));
#229487=CARTESIAN_POINT('Ctrl Pts',(58.8984458054575,-27.7074649475142,
-216.33488775531));
#229488=CARTESIAN_POINT('Ctrl Pts',(61.1254428175118,-29.0086615021396,
-212.981818623129));
#229489=CARTESIAN_POINT('Ctrl Pts',(47.7047603197491,-20.8556613435138,
-233.124453388251));
#229490=CARTESIAN_POINT('Ctrl Pts',(49.9281792692869,-22.0972013968281,
-229.768548954079));
#229491=CARTESIAN_POINT('Ctrl Pts',(52.1513679132233,-23.3426563590316,
-226.413955402434));
#229492=CARTESIAN_POINT('Ctrl Pts',(54.374445390284,-24.58956219214,-223.059830549548));
#229493=CARTESIAN_POINT('Ctrl Pts',(56.5975228673448,-25.8364680252484,
-219.705705696663));
#229494=CARTESIAN_POINT('Ctrl Pts',(58.8204852380101,-27.0849692159872,
-216.352100946617));
#229495=CARTESIAN_POINT('Ctrl Pts',(61.0433852523227,-28.3342355002131,
-212.998740881412));
#229496=CARTESIAN_POINT('Ctrl Pts',(47.6761580143262,-20.6760672828885,
-233.134431726961));
#229497=CARTESIAN_POINT('Ctrl Pts',(49.8974580357697,-21.890825164949,-229.77808818943));
#229498=CARTESIAN_POINT('Ctrl Pts',(52.11857127794,-23.1099007208212,-226.423205300924));
#229499=CARTESIAN_POINT('Ctrl Pts',(54.3395833259005,-24.3305853285644,
-223.068845880567));
#229500=CARTESIAN_POINT('Ctrl Pts',(56.5605953738609,-25.5512699363075,
-219.714486460211));
#229501=CARTESIAN_POINT('Ctrl Pts',(58.7815049542864,-26.7737213502237,
-216.36070754227));
#229502=CARTESIAN_POINT('Ctrl Pts',(61.0023564697282,-27.9970224992499,
-213.007202010553));
#229503=CARTESIAN_POINT('Ctrl Pts',(47.6435322539531,-20.4969288626005,
-233.144529615889));
#229504=CARTESIAN_POINT('Ctrl Pts',(49.8622910488621,-21.6850934492459,
-229.78772367565));
#229505=CARTESIAN_POINT('Ctrl Pts',(52.0809282278205,-22.8779807020543,
-226.432534208105));
#229506=CARTESIAN_POINT('Ctrl Pts',(54.2994812233516,-24.0726404406297,
-223.077926048768));
#229507=CARTESIAN_POINT('Ctrl Pts',(56.5180342188827,-25.2673001792052,
-219.723317889431));
#229508=CARTESIAN_POINT('Ctrl Pts',(58.7365053698609,-26.4639027275198,
-216.369353764958));
#229509=CARTESIAN_POINT('Ctrl Pts',(60.9549262461142,-27.6614430666891,
-213.015693423744));
#229510=CARTESIAN_POINT('Ctrl Pts',(47.6068679344032,-20.3182727557442,
-233.154731928786));
#229511=CARTESIAN_POINT('Ctrl Pts',(49.8226916006283,-21.4801411515154,
-229.797451628545));
#229512=CARTESIAN_POINT('Ctrl Pts',(52.0384807122269,-22.6471217996642,
-226.441944079533));
#229513=CARTESIAN_POINT('Ctrl Pts',(54.254210599501,-23.8160385972306,-223.087077428057));
#229514=CARTESIAN_POINT('Ctrl Pts',(56.4699404867752,-24.984955394797,-219.732210776581));
#229515=CARTESIAN_POINT('Ctrl Pts',(58.6856178886063,-26.1559896665116,
-216.378053163374));
#229516=CARTESIAN_POINT('Ctrl Pts',(60.9012568321316,-27.3280508969457,
-213.024230834597));
#229517=CARTESIAN_POINT('Ctrl Pts',(47.6022848944595,-20.2959407423872,
-233.156007217897));
#229518=CARTESIAN_POINT('Ctrl Pts',(49.8177416695991,-21.4545221142991,
-229.798667622657));
#229519=CARTESIAN_POINT('Ctrl Pts',(52.0331747727777,-22.6182644368655,
-226.443120313462));
#229520=CARTESIAN_POINT('Ctrl Pts',(54.2485517715197,-23.7839633668058,
-223.088221350469));
#229521=CARTESIAN_POINT('Ctrl Pts',(56.4639287702618,-24.949662296746,-219.733322387475));
#229522=CARTESIAN_POINT('Ctrl Pts',(58.6792569534495,-26.1175005338857,
-216.379140588177));
#229523=CARTESIAN_POINT('Ctrl Pts',(60.8945481553838,-27.2863768757278,
-213.025298010954));
#229524=CARTESIAN_POINT('Ctrl Pts',(47.5976387390489,-20.2736162584332,
-233.157284142165));
#229525=CARTESIAN_POINT('Ctrl Pts',(49.8127224773379,-21.4289152517019,
-229.799885067328));
#229526=CARTESIAN_POINT('Ctrl Pts',(52.0277937637733,-22.5894236531258,
-226.444297819366));
#229527=CARTESIAN_POINT('Ctrl Pts',(54.2428121888309,-23.7519091227437,
-223.089366393269));
#229528=CARTESIAN_POINT('Ctrl Pts',(56.4578306138885,-24.9143945923615,
-219.734434967173));
#229529=CARTESIAN_POINT('Ctrl Pts',(58.6728040284611,-26.079041180752,-216.380228852809));
#229530=CARTESIAN_POINT('Ctrl Pts',(60.8877420013067,-27.2447370368634,
-213.02636591529));
#229531=CARTESIAN_POINT('Ctrl Pts',(47.592929427391,-20.2512993504693,-233.15856267521));
#229532=CARTESIAN_POINT('Ctrl Pts',(49.8076340463092,-21.4033208239495,
-229.801103960199));
#229533=CARTESIAN_POINT('Ctrl Pts',(52.0223377673611,-22.5605998880764,
-226.445476607082));
#229534=CARTESIAN_POINT('Ctrl Pts',(54.2369919941413,-23.7198764736633,
-223.090512575624));
#229535=CARTESIAN_POINT('Ctrl Pts',(56.4516462209215,-24.8791530592503,
-219.735548544168));
#229536=CARTESIAN_POINT('Ctrl Pts',(58.6662593777807,-26.0406125417595,
-216.381317991529));
#229537=CARTESIAN_POINT('Ctrl Pts',(60.880838695562,-27.2031324672545,-213.027434586363));
#229538=CARTESIAN_POINT('Ctrl Pts',(47.5917520994765,-20.2457201234783,
-233.158882308471));
#229539=CARTESIAN_POINT('Ctrl Pts',(49.8063619385521,-21.3969222170114,
-229.801408683416));
#229540=CARTESIAN_POINT('Ctrl Pts',(52.0209737682581,-22.553393946814,-226.445771304011));
#229541=CARTESIAN_POINT('Ctrl Pts',(54.235536945469,-23.7118683113933,-223.090799121214));
#229542=CARTESIAN_POINT('Ctrl Pts',(56.4501001226798,-24.8703426759725,
-219.735826938416));
#229543=CARTESIAN_POINT('Ctrl Pts',(58.6646232151106,-26.0310053820113,
-216.38159027621));
#229544=CARTESIAN_POINT('Ctrl Pts',(60.8791128691258,-27.1927313248522,
-213.027701754131));
#229545=CARTESIAN_POINT('Ctrl Pts',(47.590570824284,-20.2401413699817,-233.159202042285));
#229546=CARTESIAN_POINT('Ctrl Pts',(49.805085503368,-21.3905243872477,-229.801713497152));
#229547=CARTESIAN_POINT('Ctrl Pts',(52.0196050824424,-22.5461890692189,
-226.44606608106));
#229548=CARTESIAN_POINT('Ctrl Pts',(54.23407685855,-23.7038614988106,-223.091085738033));
#229549=CARTESIAN_POINT('Ctrl Pts',(56.4485486346576,-24.8615339284022,
-219.736105395004));
#229550=CARTESIAN_POINT('Ctrl Pts',(58.6629813195933,-26.0214001419017,
-216.381862615529));
#229551=CARTESIAN_POINT('Ctrl Pts',(60.8773809707203,-27.1823323867845,
-213.027968969829));
#229552=CARTESIAN_POINT('Ctrl Pts',(47.5893856011509,-20.2345630906963,
-233.159521876246));
#229553=CARTESIAN_POINT('Ctrl Pts',(49.8038047411002,-21.384127338717,-229.802018401381));
#229554=CARTESIAN_POINT('Ctrl Pts',(52.0182317111982,-22.5389852621582,
-226.446360938398));
#229555=CARTESIAN_POINT('Ctrl Pts',(54.2326117356213,-23.695856045427,-223.091372426396));
#229556=CARTESIAN_POINT('Ctrl Pts',(56.4469917600444,-24.8527268286958,
-219.736383914393));
#229557=CARTESIAN_POINT('Ctrl Pts',(58.661333695373,-26.0117968360436,-216.38213501004));
#229558=CARTESIAN_POINT('Ctrl Pts',(60.8756430054541,-27.1719356700459,
-213.028236234081));
#229559=CARTESIAN_POINT('Ctrl Pts',(47.5882003780178,-20.2289848114109,
-233.159841710208));
#229560=CARTESIAN_POINT('Ctrl Pts',(49.8025239788324,-21.3777302901863,
-229.80232330561));
#229561=CARTESIAN_POINT('Ctrl Pts',(52.016858339954,-22.5317814550976,-226.446655795734));
#229562=CARTESIAN_POINT('Ctrl Pts',(54.2311466126926,-23.6878505920434,
-223.091659114758));
#229563=CARTESIAN_POINT('Ctrl Pts',(56.4454348854312,-24.8439197289892,
-219.736662433782));
#229564=CARTESIAN_POINT('Ctrl Pts',(58.6596860711528,-26.0021935301855,
-216.382407404553));
#229565=CARTESIAN_POINT('Ctrl Pts',(60.8739050401878,-27.1615389533073,
-213.028503498334));
#229566=CARTESIAN_POINT('Ctrl Pts',(47.5869813026369,-20.2248085548944,
-233.160629240458));
#229567=CARTESIAN_POINT('Ctrl Pts',(49.8012014928958,-21.3726770899824,
-229.803070732654));
#229568=CARTESIAN_POINT('Ctrl Pts',(52.0154387418326,-22.5258822594507,
-226.447376788852));
#229569=CARTESIAN_POINT('Ctrl Pts',(54.2296316602861,-23.6811178430054,
-223.092358686209));
#229570=CARTESIAN_POINT('Ctrl Pts',(56.4438245787395,-24.8363534265602,
-219.737340583566));
#229571=CARTESIAN_POINT('Ctrl Pts',(58.6579824964894,-25.9938070865368,
-216.383069654941));
#229572=CARTESIAN_POINT('Ctrl Pts',(60.8721090250117,-27.1523390690596,
-213.029152473631));
#229573=CARTESIAN_POINT('Ctrl Pts',(47.5858317128383,-20.2171701221733,
-233.160261571908));
#229574=CARTESIAN_POINT('Ctrl Pts',(49.7999665889626,-21.3643065199923,
-229.802725125393));
#229575=CARTESIAN_POINT('Ctrl Pts',(52.0141165726974,-22.5167636487862,
-226.447045200389));
#229576=CARTESIAN_POINT('Ctrl Pts',(54.22822178586,-23.6712455217665,-223.092038389655));
#229577=CARTESIAN_POINT('Ctrl Pts',(56.4423269990226,-24.8257273947467,
-219.737031578921));
#229578=CARTESIAN_POINT('Ctrl Pts',(58.6563966485487,-25.9824210519681,
-216.382768874591));
#229579=CARTESIAN_POINT('Ctrl Pts',(60.8704347151645,-27.140190085957,-213.028858518708));
#229580=CARTESIAN_POINT('Ctrl Pts',(47.5835325332411,-20.2018932567312,
-233.159526234808));
#229581=CARTESIAN_POINT('Ctrl Pts',(49.7974967810963,-21.3475653800119,
-229.802033910872));
#229582=CARTESIAN_POINT('Ctrl Pts',(52.011472234427,-22.4985264274573,-226.446382023462));
#229583=CARTESIAN_POINT('Ctrl Pts',(54.2254020370079,-23.6515008792884,
-223.091397796547));
#229584=CARTESIAN_POINT('Ctrl Pts',(56.4393318395888,-24.8044753311196,
-219.73641356963));
#229585=CARTESIAN_POINT('Ctrl Pts',(58.6532249526671,-25.9596489828307,
-216.382167313891));
#229586=CARTESIAN_POINT('Ctrl Pts',(60.8670860954703,-27.1158921197517,
-213.028270608861));
#229587=CARTESIAN_POINT('Ctrl Pts',(47.5812532984532,-20.1866126886901,
-233.158794242262));
#229588=CARTESIAN_POINT('Ctrl Pts',(49.7950482868299,-21.3308210270913,
-229.801345761373));
#229589=CARTESIAN_POINT('Ctrl Pts',(52.0088506546361,-22.4802865538093,
-226.445721752729));
#229590=CARTESIAN_POINT('Ctrl Pts',(54.2226065119627,-23.6317541556473,
-223.090759984216));
#229591=CARTESIAN_POINT('Ctrl Pts',(56.4363623692893,-24.7832217574852,
-219.735798215704));
#229592=CARTESIAN_POINT('Ctrl Pts',(58.6500804360107,-25.9368759906632,
-216.38156832305));
#229593=CARTESIAN_POINT('Ctrl Pts',(60.8637661551428,-27.0915938204597,
-213.027685199469));
#229594=CARTESIAN_POINT('Ctrl Pts',(47.5789940164766,-20.1713284656181,
-233.15806557645));
#229595=CARTESIAN_POINT('Ctrl Pts',(49.7926211103158,-21.3140735095608,
-229.800660662664));
#229596=CARTESIAN_POINT('Ctrl Pts',(52.0062518326129,-22.4620440746829,
-226.445064375697));
#229597=CARTESIAN_POINT('Ctrl Pts',(54.2198352050027,-23.6120053955637,
-223.090124941524));
#229598=CARTESIAN_POINT('Ctrl Pts',(56.4334185773924,-24.7619667164447,
-219.735185507351));
#229599=CARTESIAN_POINT('Ctrl Pts',(58.6469630826069,-25.9141021151943,
-216.380971893111));
#229600=CARTESIAN_POINT('Ctrl Pts',(60.8604748729077,-27.0672952246279,
-213.027102282233));
#229601=CARTESIAN_POINT('Ctrl Pts',(47.5699568885701,-20.1101915733302,
-233.155150913204));
#229602=CARTESIAN_POINT('Ctrl Pts',(49.7829124042595,-21.2470834394385,
-229.797920267832));
#229603=CARTESIAN_POINT('Ctrl Pts',(51.9958565445205,-22.3890741581773,
-226.44243486757));
#229604=CARTESIAN_POINT('Ctrl Pts',(54.2087499771628,-23.5330103552298,
-223.087584770755));
#229605=CARTESIAN_POINT('Ctrl Pts',(56.421643409805,-24.6769465522823,-219.732734673941));
#229606=CARTESIAN_POINT('Ctrl Pts',(58.6344936689916,-25.8230066133188,
-216.378586173355));
#229607=CARTESIAN_POINT('Ctrl Pts',(60.847309743967,-26.9701008413005,-213.024770613288));
#229608=CARTESIAN_POINT('Ctrl Pts',(47.5612390015556,-20.0489962009945,
-233.152289471859));
#229609=CARTESIAN_POINT('Ctrl Pts',(49.7735447794099,-21.1800427364387,
-229.795228681509));
#229610=CARTESIAN_POINT('Ctrl Pts',(51.9858253784452,-22.3160625550462,
-226.43985165536));
#229611=CARTESIAN_POINT('Ctrl Pts',(54.1980522368575,-23.453982732959,-223.08508891153));
#229612=CARTESIAN_POINT('Ctrl Pts',(56.4102790952697,-24.5919029108718,
-219.730326167701));
#229613=CARTESIAN_POINT('Ctrl Pts',(58.6224588662923,-25.7318969799296,
-216.376241426438));
#229614=CARTESIAN_POINT('Ctrl Pts',(60.8346031435815,-26.87290171468,-213.022478817573));
#229615=CARTESIAN_POINT('Ctrl Pts',(47.552840900575,-19.9877453892004,-233.149480158731));
#229616=CARTESIAN_POINT('Ctrl Pts',(49.764518524335,-21.1129544864435,-229.792585026173));
#229617=CARTESIAN_POINT('Ctrl Pts',(51.976158307113,-22.2430122546447,-226.437313966284));
#229618=CARTESIAN_POINT('Ctrl Pts',(54.1877416326195,-23.3749253815565,
-223.082636672215));
#229619=CARTESIAN_POINT('Ctrl Pts',(56.399324958126,-24.5068385084684,-219.727959378147));
#229620=CARTESIAN_POINT('Ctrl Pts',(58.6108576613275,-25.6407757471239,
-216.373937091928));
#229621=CARTESIAN_POINT('Ctrl Pts',(60.8223537175678,-26.7757001729515,
-213.02022637406));
#229622=CARTESIAN_POINT('Ctrl Pts',(47.5360446986138,-19.8652437656123,
-233.143861532478));
#229623=CARTESIAN_POINT('Ctrl Pts',(49.7464660141853,-20.9787779864532,
-229.787297715501));
#229624=CARTESIAN_POINT('Ctrl Pts',(51.9568241644486,-22.0969116538416,
-226.432238588131));
#229625=CARTESIAN_POINT('Ctrl Pts',(54.1671204241435,-23.2168106787515,
-223.077732193586));
#229626=CARTESIAN_POINT('Ctrl Pts',(56.3774166838384,-24.3367097036616,
-219.723225799041));
#229627=CARTESIAN_POINT('Ctrl Pts',(58.5876552513978,-25.4585332815125,
-216.369328422911));
#229628=CARTESIAN_POINT('Ctrl Pts',(60.7978548655404,-26.5812970894946,
-213.015721487035));
#229629=CARTESIAN_POINT('Ctrl Pts',(47.5205275923637,-19.7425203876807,
-233.138451347457));
#229630=CARTESIAN_POINT('Ctrl Pts',(49.7297789491929,-20.8444113076799,
-229.782202077174));
#229631=CARTESIAN_POINT('Ctrl Pts',(51.9389463734439,-21.9506562752646,
-226.42734526098));
#229632=CARTESIAN_POINT('Ctrl Pts',(54.1480477377855,-23.0585770723389,
-223.073002160992));
#229633=CARTESIAN_POINT('Ctrl Pts',(56.3571491021271,-24.1664978694133,
-219.718659061004));
#229634=CARTESIAN_POINT('Ctrl Pts',(58.5661872185244,-25.276244433579,-216.364881382949));
#229635=CARTESIAN_POINT('Ctrl Pts',(60.7751846995537,-26.3868843615641,
-213.011373992336));
#229636=CARTESIAN_POINT('Ctrl Pts',(47.5062945476757,-19.6195995248629,
-233.133241732319));
#229637=CARTESIAN_POINT('Ctrl Pts',(49.7144600590333,-20.7098790140667,
-229.777291719128));
#229638=CARTESIAN_POINT('Ctrl Pts',(51.9225250540634,-21.8042698865183,
-226.422628306549));
#229639=CARTESIAN_POINT('Ctrl Pts',(54.1305210352282,-22.9002472192685,
-223.06844144768));
#229640=CARTESIAN_POINT('Ctrl Pts',(56.3385170163929,-23.9962245520186,
-219.714254588812));
#229641=CARTESIAN_POINT('Ctrl Pts',(58.5464456271153,-25.0939292676188,
-216.360591734734));
#229642=CARTESIAN_POINT('Ctrl Pts',(60.7543325255676,-26.1924804157199,
-213.007179917814));
#229643=CARTESIAN_POINT('Ctrl Pts',(47.3924301901722,-18.6362326223204,
-233.091564811217));
#229644=CARTESIAN_POINT('Ctrl Pts',(49.5919089377565,-19.6336206651606,
-229.73800885476));
#229645=CARTESIAN_POINT('Ctrl Pts',(51.7911544990196,-20.633178776548,-226.384892671102));
#229646=CARTESIAN_POINT('Ctrl Pts',(53.9903074147697,-21.6336083947046,
-223.031955741188));
#229647=CARTESIAN_POINT('Ctrl Pts',(56.1894603305198,-22.6340380128611,
-219.679018811274));
#229648=CARTESIAN_POINT('Ctrl Pts',(58.3885128958421,-23.6354079399365,
-216.326274549018));
#229649=CARTESIAN_POINT('Ctrl Pts',(60.5875151336786,-24.637248848966,-212.973627321642));
#229650=CARTESIAN_POINT('Ctrl Pts',(47.3611092111201,-17.6397302500457,
-233.062531430769));
#229651=CARTESIAN_POINT('Ctrl Pts',(49.5571768913406,-18.5464340199547,
-229.71043415307));
#229652=CARTESIAN_POINT('Ctrl Pts',(51.753139481442,-19.4535001698865,-226.358317180801));
#229653=CARTESIAN_POINT('Ctrl Pts',(53.9490641998496,-20.3607169575665,
-223.006196302843));
#229654=CARTESIAN_POINT('Ctrl Pts',(56.1449889182572,-21.2679337452465,
-219.654075424885));
#229655=CARTESIAN_POINT('Ctrl Pts',(58.3408717515618,-22.175311849639,-216.301949384044));
#229656=CARTESIAN_POINT('Ctrl Pts',(60.5367349311551,-23.0827722988975,
-212.949821974785));
#229657=CARTESIAN_POINT('Ctrl Pts',(47.4134504259477,-16.6473487128058,
-233.044455194982));
#229658=CARTESIAN_POINT('Ctrl Pts',(49.6106642054098,-17.4639704569693,
-229.692980964189));
#229659=CARTESIAN_POINT('Ctrl Pts',(51.808075938482,-18.2792435060293,-226.341309714209));
#229660=CARTESIAN_POINT('Ctrl Pts',(54.0055642141686,-19.0939722550291,
-222.989556757961));
#229661=CARTESIAN_POINT('Ctrl Pts',(56.2030524898552,-19.9087010040289,
-219.637803801712));
#229662=CARTESIAN_POINT('Ctrl Pts',(58.4006240585482,-20.7228430676927,
-216.285963294552));
#229663=CARTESIAN_POINT('Ctrl Pts',(60.5982364662104,-21.5366903458251,
-212.934078132851));
#229664=CARTESIAN_POINT('Ctrl Pts',(47.4396210333615,-16.1511579441859,
-233.035417077088));
#229665=CARTESIAN_POINT('Ctrl Pts',(49.6374078624443,-16.9227386754765,
-229.684254369749));
#229666=CARTESIAN_POINT('Ctrl Pts',(51.835544167002,-17.6921151741007,-226.332805980913));
#229667=CARTESIAN_POINT('Ctrl Pts',(54.0338142213281,-18.4605999037604,
-222.98123698552));
#229668=CARTESIAN_POINT('Ctrl Pts',(56.2320842756543,-19.2290846334201,
-219.629667990126));
#229669=CARTESIAN_POINT('Ctrl Pts',(58.4305002120414,-19.9966086767195,
-216.277970249807));
#229670=CARTESIAN_POINT('Ctrl Pts',(60.6289872337381,-20.7636493692889,
-212.926206211883));
#229671=CARTESIAN_POINT('Ctrl Pts',(47.4866458063998,-15.6558748576279,
-233.029111826755));
#229672=CARTESIAN_POINT('Ctrl Pts',(49.68616076798,-16.3826093301408,-229.678058258297));
#229673=CARTESIAN_POINT('Ctrl Pts',(51.8862243890013,-17.1062920942477,
-226.326700188893));
#229674=CARTESIAN_POINT('Ctrl Pts',(54.0864948338312,-17.8287356549779,
-222.97520798459));
#229675=CARTESIAN_POINT('Ctrl Pts',(56.2867652786612,-18.551179215708,-219.623715780286));
#229676=CARTESIAN_POINT('Ctrl Pts',(58.4872620760191,-19.2722889032489,
-216.272081643134));
#229677=CARTESIAN_POINT('Ctrl Pts',(60.6878681298499,-19.9927261544104,
-212.920372770536));
#229678=CARTESIAN_POINT('Ctrl Pts',(47.554307632397,-15.1637468311187,-233.025453073475));
#229679=CARTESIAN_POINT('Ctrl Pts',(49.7567152646595,-15.8456016742832,
-229.674306559616));
#229680=CARTESIAN_POINT('Ctrl Pts',(51.9599159483462,-16.5235645049904,
-226.322904658655));
#229681=CARTESIAN_POINT('Ctrl Pts',(54.1634104836589,-17.1999459798668,
-222.971380331423));
#229682=CARTESIAN_POINT('Ctrl Pts',(56.3669050189717,-17.8763274547433,
-219.619856004191));
#229683=CARTESIAN_POINT('Ctrl Pts',(58.5707224241369,-18.5510070650469,
-216.268204278443));
#229684=CARTESIAN_POINT('Ctrl Pts',(60.7746940090617,-19.2248286528632,
-212.916482666117));
#229685=CARTESIAN_POINT('Ctrl Pts',(47.5881385453956,-14.9176828178641,
-233.023623696835));
#229686=CARTESIAN_POINT('Ctrl Pts',(49.7919925129992,-15.5770978463543,
-229.672430710276));
#229687=CARTESIAN_POINT('Ctrl Pts',(51.9967617280187,-16.2322007103616,
-226.321006893536));
#229688=CARTESIAN_POINT('Ctrl Pts',(54.2018683085728,-16.8855511423113,
-222.96946650484));
#229689=CARTESIAN_POINT('Ctrl Pts',(56.4069748891269,-17.538901574261,-219.617926116144));
#229690=CARTESIAN_POINT('Ctrl Pts',(58.6124525981959,-18.1903661459459,
-216.266265596097));
#229691=CARTESIAN_POINT('Ctrl Pts',(60.8181069486676,-18.8408799020897,
-212.914537613908));
#229692=CARTESIAN_POINT('Ctrl Pts',(47.6271129859842,-14.672424944912,-233.022456269286));
#229693=CARTESIAN_POINT('Ctrl Pts',(49.8327089180398,-15.3093857877439,
-229.671166307109));
#229694=CARTESIAN_POINT('Ctrl Pts',(52.0393530559316,-15.9416180264796,
-226.319687040658));
#229695=CARTESIAN_POINT('Ctrl Pts',(54.2463813625237,-16.5719288708872,
-222.968103360071));
#229696=CARTESIAN_POINT('Ctrl Pts',(56.4534096691157,-17.2022397152948,
-219.616519679485));
#229697=CARTESIAN_POINT('Ctrl Pts',(58.6608611565012,-17.830482853318,-216.264830059583));
#229698=CARTESIAN_POINT('Ctrl Pts',(60.8685133335648,-18.4576836904079,
-212.913078722092));
#229699=CARTESIAN_POINT('Ctrl Pts',(47.6711899624377,-14.4281659124299,
-233.021940707592));
#229700=CARTESIAN_POINT('Ctrl Pts',(49.8788265984679,-15.0426590253955,
-229.670504307963));
#229701=CARTESIAN_POINT('Ctrl Pts',(52.0876575029478,-15.6520019918285,
-226.318937245156));
#229702=CARTESIAN_POINT('Ctrl Pts',(54.296923205648,-16.259253814469,-222.967284070276));
#229703=CARTESIAN_POINT('Ctrl Pts',(56.5061889083483,-16.8665056371095,
-219.615630895396));
#229704=CARTESIAN_POINT('Ctrl Pts',(58.7159343195776,-17.4715067819979,
-216.263892782403));
#229705=CARTESIAN_POINT('Ctrl Pts',(60.9259062922535,-18.0753740181923,
-212.912101903999));
#229706=CARTESIAN_POINT('Ctrl Pts',(47.6932284506644,-14.3060363961889,
-233.021682926744));
#229707=CARTESIAN_POINT('Ctrl Pts',(49.901885438682,-14.9092956442213,-229.670173308391));
#229708=CARTESIAN_POINT('Ctrl Pts',(52.1118097264559,-15.507193974503,-226.318562347407));
#229709=CARTESIAN_POINT('Ctrl Pts',(54.3221941272102,-16.1029162862599,
-222.966874425379));
#229710=CARTESIAN_POINT('Ctrl Pts',(56.5325785279645,-16.6986385980169,
-219.615186503351));
#229711=CARTESIAN_POINT('Ctrl Pts',(58.7434709011157,-17.2920187463379,
-216.263424143813));
#229712=CARTESIAN_POINT('Ctrl Pts',(60.9546027715979,-17.8842191820846,
-212.911613494952));
#229713=CARTESIAN_POINT('Ctrl Pts',(47.7165427070916,-14.1841566123428,
-233.021588374054));
#229714=CARTESIAN_POINT('Ctrl Pts',(49.9262946886754,-14.7761786009886,
-229.669993107177));
#229715=CARTESIAN_POINT('Ctrl Pts',(52.1373902989064,-15.3626276289524,
-226.318330125135));
#229716=CARTESIAN_POINT('Ctrl Pts',(54.3489722985157,-15.9468155679217,
-222.966600877007));
#229717=CARTESIAN_POINT('Ctrl Pts',(56.560554298125,-16.531003506891,-219.614871628879));
#229718=CARTESIAN_POINT('Ctrl Pts',(58.7726736592232,-17.1127575167165,
-216.263080155467));
#229719=CARTESIAN_POINT('Ctrl Pts',(60.9850459116547,-17.6932859799952,
-212.911245674445));
#229720=CARTESIAN_POINT('Ctrl Pts',(47.7411284099535,-14.0625507697344,
-233.021657357818));
#229721=CARTESIAN_POINT('Ctrl Pts',(49.9520501521893,-14.6433321699676,
-229.669963755451));
#229722=CARTESIAN_POINT('Ctrl Pts',(52.164395575698,-15.2183262074345,-226.318240561216));
#229723=CARTESIAN_POINT('Ctrl Pts',(54.3772547239517,-15.7909735318649,
-222.966463366842));
#229724=CARTESIAN_POINT('Ctrl Pts',(56.5901138722054,-16.3636208562953,
-219.614686172468));
#229725=CARTESIAN_POINT('Ctrl Pts',(58.8035410200603,-16.9337418020372,
-216.262860718253));
#229726=CARTESIAN_POINT('Ctrl Pts',(61.0172349543283,-17.5025911610169,
-212.910998351897));
#229727=CARTESIAN_POINT('Ctrl Pts',(47.7442016228112,-14.0473500394083,
-233.021665980788));
#229728=CARTESIAN_POINT('Ctrl Pts',(49.9552695851286,-14.62672636609,-229.669960086485));
#229729=CARTESIAN_POINT('Ctrl Pts',(52.167771235297,-15.2002885297448,-226.318229365726));
#229730=CARTESIAN_POINT('Ctrl Pts',(54.3807900271312,-15.7714932773578,
-222.966446178071));
#229731=CARTESIAN_POINT('Ctrl Pts',(56.5938088189654,-16.3426980249709,
-219.614662990416));
#229732=CARTESIAN_POINT('Ctrl Pts',(58.8073994401649,-16.9113648377023,
-216.262833288602));
#229733=CARTESIAN_POINT('Ctrl Pts',(61.0212585846625,-17.4787543086446,
-212.910967436579));
#229734=CARTESIAN_POINT('Ctrl Pts',(47.7476113419008,-14.0307623608562,
-233.021648099596));
#229735=CARTESIAN_POINT('Ctrl Pts',(49.9588045578851,-14.6087951143449,
-229.669924789137));
#229736=CARTESIAN_POINT('Ctrl Pts',(52.1714498515783,-15.180967081333,-226.318183716026));
#229737=CARTESIAN_POINT('Ctrl Pts',(54.3846185831211,-15.7507631661298,
-222.966392342634));
#229738=CARTESIAN_POINT('Ctrl Pts',(56.5977873146637,-16.3205592509265,
-219.614600969242));
#229739=CARTESIAN_POINT('Ctrl Pts',(58.8115349286387,-16.887797426467,-216.262765580964));
#229740=CARTESIAN_POINT('Ctrl Pts',(61.0255542724185,-17.4537483605921,
-212.910895097936));
#229741=CARTESIAN_POINT('Ctrl Pts',(47.7498680445413,-14.0193937377161,
-233.021742568709));
#229742=CARTESIAN_POINT('Ctrl Pts',(49.9612716248183,-14.5958520941202,
-229.670020033279));
#229743=CARTESIAN_POINT('Ctrl Pts',(52.1741145339256,-15.1664771156592,
-226.318278543544));
#229744=CARTESIAN_POINT('Ctrl Pts',(54.3874764662403,-15.7347368225257,
-222.966486672088));
#229745=CARTESIAN_POINT('Ctrl Pts',(56.600838398555,-16.3029965293923,-219.614694800631));
#229746=CARTESIAN_POINT('Ctrl Pts',(58.8147742803545,-16.8687098306404,
-216.262858729364));
#229747=CARTESIAN_POINT('Ctrl Pts',(61.0289796285328,-17.4331414974815,
-212.910987583833));
#229748=CARTESIAN_POINT('Ctrl Pts',(47.7521247471819,-14.008025114576,-233.021837037822));
#229749=CARTESIAN_POINT('Ctrl Pts',(49.9637386917516,-14.5829090738954,
-229.670115277422));
#229750=CARTESIAN_POINT('Ctrl Pts',(52.1767792162729,-15.1519871499853,
-226.318373371061));
#229751=CARTESIAN_POINT('Ctrl Pts',(54.3903343493595,-15.7187104789216,
-222.966581001541));
#229752=CARTESIAN_POINT('Ctrl Pts',(56.6038894824462,-16.2854338078579,
-219.61478863202));
#229753=CARTESIAN_POINT('Ctrl Pts',(58.8180136320704,-16.8496222348139,
-216.262951877763));
#229754=CARTESIAN_POINT('Ctrl Pts',(61.0324049846472,-17.4125346343709,
-212.91108006973));
#229755=CARTESIAN_POINT('Ctrl Pts',(47.7543654978573,-13.9966521764404,
-233.021931550365));
#229756=CARTESIAN_POINT('Ctrl Pts',(49.9661881993766,-14.5699622186276,
-229.67021053026));
#229757=CARTESIAN_POINT('Ctrl Pts',(52.1794248253455,-15.137493805192,-226.318468190145));
#229758=CARTESIAN_POINT('Ctrl Pts',(54.3931716728027,-15.7026812170992,
-222.966675309108));
#229759=CARTESIAN_POINT('Ctrl Pts',(56.60691852026,-16.2678686290064,-219.614882428071));
#229760=CARTESIAN_POINT('Ctrl Pts',(58.821229483535,-16.8305326445432,-216.263044982252));
#229761=CARTESIAN_POINT('Ctrl Pts',(61.0358053997983,-17.391926245276,-212.911172504828));
#229762=CARTESIAN_POINT('Ctrl Pts',(47.7565902716679,-13.9852750117499,
-233.022026107165));
#229763=CARTESIAN_POINT('Ctrl Pts',(49.9686201309427,-14.5570115979937,
-229.670305792423));
#229764=CARTESIAN_POINT('Ctrl Pts',(52.1820513513198,-15.1229971351898,
-226.318563001159));
#229765=CARTESIAN_POINT('Ctrl Pts',(54.3959884334715,-15.6866490761195,
-222.966769594939));
#229766=CARTESIAN_POINT('Ctrl Pts',(56.6099255156231,-16.2503010170492,
-219.614976188718));
#229767=CARTESIAN_POINT('Ctrl Pts',(58.8244218448074,-16.8114410702517,
-216.26313804258));
#229768=CARTESIAN_POINT('Ctrl Pts',(61.0391808904015,-17.371316327283,-212.911264888718));
#229769=CARTESIAN_POINT('Ctrl Pts',(47.7610398192893,-13.962520682369,-233.022215220766));
#229770=CARTESIAN_POINT('Ctrl Pts',(49.973483994075,-14.5311103567258,-229.670496316751));
#229771=CARTESIAN_POINT('Ctrl Pts',(52.1873044032685,-15.0940037951854,
-226.318752623187));
#229772=CARTESIAN_POINT('Ctrl Pts',(54.4016219548089,-15.6545847941602,
-222.9669581666));
#229773=CARTESIAN_POINT('Ctrl Pts',(56.6159395063494,-16.2151657931349,
-219.615163710013));
#229774=CARTESIAN_POINT('Ctrl Pts',(58.8308065673522,-16.7732579216688,
-216.263324163236));
#229775=CARTESIAN_POINT('Ctrl Pts',(61.0459318716081,-17.3300964912969,
-212.911449656498));
#229776=CARTESIAN_POINT('Ctrl Pts',(47.7654254592341,-13.9397494467436,
-233.022404511428));
#229777=CARTESIAN_POINT('Ctrl Pts',(49.9782775528494,-14.5051940539731,
-229.670686878432));
#229778=CARTESIAN_POINT('Ctrl Pts',(52.1924811227502,-15.064997154331,-226.318942212994));
#229779=CARTESIAN_POINT('Ctrl Pts',(54.4071732250129,-15.6225089955621,
-222.967146651374));
#229780=CARTESIAN_POINT('Ctrl Pts',(56.6218653272756,-16.1800208367931,
-219.615351089753));
#229781=CARTESIAN_POINT('Ctrl Pts',(58.8370973291551,-16.7350668370003,
-216.263510107308));
#229782=CARTESIAN_POINT('Ctrl Pts',(61.0525831546696,-17.2888705397188,
-212.911634219511));
#229783=CARTESIAN_POINT('Ctrl Pts',(47.7697469949171,-13.9169620127152,
-233.022593985349));
#229784=CARTESIAN_POINT('Ctrl Pts',(49.983000674726,-14.4792632474105,-229.670877481921));
#229785=CARTESIAN_POINT('Ctrl Pts',(52.1975814320602,-15.0359776440825,
-226.319131772858));
#229786=CARTESIAN_POINT('Ctrl Pts',(54.4126422197256,-15.5904219929251,
-222.967335049774));
#229787=CARTESIAN_POINT('Ctrl Pts',(56.627703007391,-16.1448663417677,-219.615538326691));
#229788=CARTESIAN_POINT('Ctrl Pts',(58.8432942103714,-16.6968678996294,
-216.263695872058));
#229789=CARTESIAN_POINT('Ctrl Pts',(61.0591348703587,-17.2476384491985,
-212.91181857376));
#229790=CARTESIAN_POINT('Ctrl Pts',(47.7783900662832,-13.8713871446584,
-233.022972933189));
#229791=CARTESIAN_POINT('Ctrl Pts',(49.9924469184794,-14.4274016342853,
-229.671258688898));
#229792=CARTESIAN_POINT('Ctrl Pts',(52.2077820506802,-14.9779386235856,
-226.319510892586));
#229793=CARTESIAN_POINT('Ctrl Pts',(54.423580209151,-15.5262479876512,-222.967711846576));
#229794=CARTESIAN_POINT('Ctrl Pts',(56.6393783676217,-16.0745573517168,
-219.615912800565));
#229795=CARTESIAN_POINT('Ctrl Pts',(58.8556879728042,-16.6204700248875,
-216.264067401558));
#229796=CARTESIAN_POINT('Ctrl Pts',(61.0722383017368,-17.1651742681581,
-212.91218728226));
#229797=CARTESIAN_POINT('Ctrl Pts',(47.7867767171158,-13.8257474826836,
-233.023352614608));
#229798=CARTESIAN_POINT('Ctrl Pts',(50.0016114126724,-14.3754820056756,
-229.6716400639));
#229799=CARTESIAN_POINT('Ctrl Pts',(52.2176770274244,-14.9198481253495,
-226.319889893413));
#229800=CARTESIAN_POINT('Ctrl Pts',(54.4341890960325,-15.4620291661139,
-222.968088298805));
#229801=CARTESIAN_POINT('Ctrl Pts',(56.6507011646406,-16.0042102068785,
-219.616286704198));
#229802=CARTESIAN_POINT('Ctrl Pts',(58.8677062133155,-16.5440407393228,
-216.264438214748));
#229803=CARTESIAN_POINT('Ctrl Pts',(61.0849434643637,-17.0826855313617,
-212.912555156691));
#229804=CARTESIAN_POINT('Ctrl Pts',(47.794905416537,-13.7800486938334,-233.0237330726));
#229805=CARTESIAN_POINT('Ctrl Pts',(50.0104931205382,-14.3235088264801,
-229.67202163298));
#229806=CARTESIAN_POINT('Ctrl Pts',(52.2272657548643,-14.8617096033744,
-226.320268783124));
#229807=CARTESIAN_POINT('Ctrl Pts',(54.4444686924125,-15.3977680306514,
-222.968464399553));
#229808=CARTESIAN_POINT('Ctrl Pts',(56.6616716299607,-15.9338264579286,
-219.616660015982));
#229809=CARTESIAN_POINT('Ctrl Pts',(58.8793495680496,-16.4675807101401,
-216.264808277961));
#229810=CARTESIAN_POINT('Ctrl Pts',(61.0972513955672,-17.0001720517288,
-212.912922153302));
#229811=CARTESIAN_POINT('Ctrl Pts',(47.9249646072757,-13.0488680722298,
-233.029820400472));
#229812=CARTESIAN_POINT('Ctrl Pts',(50.1526004463906,-13.4919379593521,
-229.678126738255));
#229813=CARTESIAN_POINT('Ctrl Pts',(52.3806853939039,-13.9314932517732,
-226.326331018504));
#229814=CARTESIAN_POINT('Ctrl Pts',(54.6089422344929,-14.3695898632513,
-222.974482011522));
#229815=CARTESIAN_POINT('Ctrl Pts',(56.8371990750819,-14.8076864747294,
-219.622633004539));
#229816=CARTESIAN_POINT('Ctrl Pts',(59.0656432437958,-15.2442202432178,
-216.270729289381));
#229817=CARTESIAN_POINT('Ctrl Pts',(61.2941782948235,-15.6799563776017,
-212.918794099076));
#229818=CARTESIAN_POINT('Ctrl Pts',(47.9883865798889,-12.3026122775794,
-233.036124708431));
#229819=CARTESIAN_POINT('Ctrl Pts',(50.2219072486975,-12.6466684930416,
-229.684291138819));
#229820=CARTESIAN_POINT('Ctrl Pts',(52.4554840800718,-12.9889576988494,
-226.332367209873));
#229821=CARTESIAN_POINT('Ctrl Pts',(54.6890840421723,-13.3305248173704,
-222.980406475497));
#229822=CARTESIAN_POINT('Ctrl Pts',(56.9226840042728,-13.6720919358914,
-219.628445741121));
#229823=CARTESIAN_POINT('Ctrl Pts',(59.1563087897256,-14.0128828330946,
-216.276445414441));
#229824=CARTESIAN_POINT('Ctrl Pts',(61.3899461914607,-14.353280946091,-212.924425089962));
#229825=CARTESIAN_POINT('Ctrl Pts',(47.9834035327445,-11.5593373188707,
-233.042545221464));
#229826=CARTESIAN_POINT('Ctrl Pts',(50.2170610824398,-11.8031522322565,
-229.690412491071));
#229827=CARTESIAN_POINT('Ctrl Pts',(52.4507177144441,-12.0469951332675,
-226.33828118561));
#229828=CARTESIAN_POINT('Ctrl Pts',(54.684373970075,-12.2908494697823,-222.986150461423));
#229829=CARTESIAN_POINT('Ctrl Pts',(56.9180302257058,-12.5347038062971,
-219.634019737236));
#229830=CARTESIAN_POINT('Ctrl Pts',(59.1516860770602,-12.7785704359954,
-216.281889638136));
#229831=CARTESIAN_POINT('Ctrl Pts',(61.3853417234255,-13.0224432858052,
-212.92975985503));
#229832=CARTESIAN_POINT('Ctrl Pts',(47.9784204856001,-10.8160623601621,
-233.048965734498));
#229833=CARTESIAN_POINT('Ctrl Pts',(50.2122149161821,-10.9596359714715,
-229.696533843322));
#229834=CARTESIAN_POINT('Ctrl Pts',(52.4459513488164,-11.1050325676855,
-226.344195161346));
#229835=CARTESIAN_POINT('Ctrl Pts',(54.6796638979776,-11.2511741221942,
-222.991894447348));
#229836=CARTESIAN_POINT('Ctrl Pts',(56.9133764471387,-11.3973156767028,
-219.639593733351));
#229837=CARTESIAN_POINT('Ctrl Pts',(59.1470633643947,-11.5442580388962,
-216.287333861831));
#229838=CARTESIAN_POINT('Ctrl Pts',(61.3807372553903,-11.6916056255194,
-212.935094620098));
#229839=CARTESIAN_POINT('Ctrl Pts',(47.9050040452069,-10.0714896149287,
-233.055533041971));
#229840=CARTESIAN_POINT('Ctrl Pts',(50.1331992952188,-10.115921730292,-229.702631915958));
#229841=CARTESIAN_POINT('Ctrl Pts',(52.3616168326291,-10.1639774224541,
-226.349993898252));
#229842=CARTESIAN_POINT('Ctrl Pts',(54.5901116210639,-10.2135334694198,
-222.997453498015));
#229843=CARTESIAN_POINT('Ctrl Pts',(56.8186064094987,-10.2630895163856,
-219.644913097779));
#229844=CARTESIAN_POINT('Ctrl Pts',(59.0471872279132,-10.3142538392508,
-216.292479809858));
#229845=CARTESIAN_POINT('Ctrl Pts',(61.2758070478567,-10.3662378430004,
-212.940097419686));
#229846=CARTESIAN_POINT('Ctrl Pts',(47.7656170077038,-9.34368646884676,
-233.062037879842));
#229847=CARTESIAN_POINT('Ctrl Pts',(49.9819449608238,-9.2874213104565,-229.708539095772));
#229848=CARTESIAN_POINT('Ctrl Pts',(52.1991449367821,-9.23662705053824,
-226.355554581771));
#229849=CARTESIAN_POINT('Ctrl Pts',(54.4166431400134,-9.18805051768256,
-223.002741959001));
#229850=CARTESIAN_POINT('Ctrl Pts',(56.6341413432447,-9.13947398482688,
-219.649929336231));
#229851=CARTESIAN_POINT('Ctrl Pts',(58.8519736255103,-9.09328518499885,
-216.297310379527));
#229852=CARTESIAN_POINT('Ctrl Pts',(61.069957421301,-9.04829813924799,-212.94477788882));
#229853=CARTESIAN_POINT('Ctrl Pts',(47.7569053178599,-9.29819877221664,
-233.062444432209));
#229854=CARTESIAN_POINT('Ctrl Pts',(49.9724915649241,-9.23564003421678,
-229.708908294511));
#229855=CARTESIAN_POINT('Ctrl Pts',(52.1889904432917,-9.1786676522935,-226.355902124491));
#229856=CARTESIAN_POINT('Ctrl Pts',(54.4058013599478,-9.12395783319898,
-223.003072487813));
#229857=CARTESIAN_POINT('Ctrl Pts',(56.6226122766038,-9.06924801410446,
-219.650242851134));
#229858=CARTESIAN_POINT('Ctrl Pts',(58.8397727753602,-9.01697464410811,
-216.297612290131));
#229859=CARTESIAN_POINT('Ctrl Pts',(61.0570918196413,-8.96592690776347,
-212.945070418141));
#229860=CARTESIAN_POINT('Ctrl Pts',(47.7479382353889,-9.25277671838467,
-233.062850739409));
#229861=CARTESIAN_POINT('Ctrl Pts',(49.9627575429261,-9.18391816356222,
-229.70927675202));
#229862=CARTESIAN_POINT('Ctrl Pts',(52.1785315662453,-9.12076168624719,
-226.356248750518));
#229863=CARTESIAN_POINT('Ctrl Pts',(54.394631899532,-9.05991249164631,-223.003401978127));
#229864=CARTESIAN_POINT('Ctrl Pts',(56.6107322328186,-8.99906329704543,
-219.650555205738));
#229865=CARTESIAN_POINT('Ctrl Pts',(58.827198181488,-8.9406991939707,-216.297912995698));
#229866=CARTESIAN_POINT('Ctrl Pts',(61.0438299379249,-8.88358449709214,
-212.945361716967));
#229867=CARTESIAN_POINT('Ctrl Pts',(47.7387173442106,-9.207425908897,-233.06325682779));
#229868=CARTESIAN_POINT('Ctrl Pts',(49.9527439997195,-9.13226010185821,
-229.709644459743));
#229869=CARTESIAN_POINT('Ctrl Pts',(52.1677689925887,-9.06291255266274,
-226.356594439508));
#229870=CARTESIAN_POINT('Ctrl Pts',(54.383135035575,-8.99591694925441,-223.003730400442));
#229871=CARTESIAN_POINT('Ctrl Pts',(56.5985010785614,-8.92892134584607,
-219.650866361376));
#229872=CARTESIAN_POINT('Ctrl Pts',(58.8142493132399,-8.86445947120716,
-216.2982124531));
#229873=CARTESIAN_POINT('Ctrl Pts',(61.030170850553,-8.80127069719074,-212.945651738761));
#229874=CARTESIAN_POINT('Ctrl Pts',(47.7341068986215,-9.18475050415316,
-233.063459871981));
#229875=CARTESIAN_POINT('Ctrl Pts',(49.9477372281162,-9.10643107100621,
-229.709828313605));
#229876=CARTESIAN_POINT('Ctrl Pts',(52.1623877057604,-9.03398798587052,
-226.356767284002));
#229877=CARTESIAN_POINT('Ctrl Pts',(54.3773866035966,-8.96391917805846,
-223.003894611599));
#229878=CARTESIAN_POINT('Ctrl Pts',(56.5923855014328,-8.89385037024639,
-219.651021939195));
#229879=CARTESIAN_POINT('Ctrl Pts',(58.8077748791159,-8.8263396098254,-216.298362181801));
#229880=CARTESIAN_POINT('Ctrl Pts',(61.0233413068671,-8.76011379724005,
-212.945796749657));
#229881=CARTESIAN_POINT('Ctrl Pts',(47.7294330017316,-9.16209291048223,
-233.063662861321));
#229882=CARTESIAN_POINT('Ctrl Pts',(49.9426605766967,-9.08061799234707,
-229.710011979809));
#229883=CARTESIAN_POINT('Ctrl Pts',(52.1569304950676,-9.0050776271462,-226.356939894011));
#229884=CARTESIAN_POINT('Ctrl Pts',(54.3715563208665,-8.93193385660108,
-223.004058555517));
#229885=CARTESIAN_POINT('Ctrl Pts',(56.5861821466654,-8.85879008605595,
-219.651177217023));
#229886=CARTESIAN_POINT('Ctrl Pts',(58.8012068762785,-8.78822868023012,
-216.29851159821));
#229887=CARTESIAN_POINT('Ctrl Pts',(61.0164124615696,-8.71896404992253,
-212.945941441045));
#229888=CARTESIAN_POINT('Ctrl Pts',(47.724695856798,-9.13945382791814,-233.06386579822));
#229889=CARTESIAN_POINT('Ctrl Pts',(49.9375141864838,-9.05482141596443,
-229.710195456012));
#229890=CARTESIAN_POINT('Ctrl Pts',(52.1513974481024,-8.97618190118969,
-226.357112265619));
#229891=CARTESIAN_POINT('Ctrl Pts',(54.3656442227822,-8.89996129157268,
-223.00422222707));
#229892=CARTESIAN_POINT('Ctrl Pts',(56.579890997462,-8.82374068195567,-219.651332188522));
#229893=CARTESIAN_POINT('Ctrl Pts',(58.7945452376739,-8.75012676166283,
-216.298660695422));
#229894=CARTESIAN_POINT('Ctrl Pts',(61.0093841977678,-8.67782142864838,
-212.946085805591));
#229895=CARTESIAN_POINT('Ctrl Pts',(47.7235115705647,-9.13379405727712,
-233.063916532445));
#229896=CARTESIAN_POINT('Ctrl Pts',(49.9362275889306,-9.04837227186877,
-229.710241325062));
#229897=CARTESIAN_POINT('Ctrl Pts',(52.1500141863611,-8.96895796970056,
-226.357155358521));
#229898=CARTESIAN_POINT('Ctrl Pts',(54.3641661982611,-8.89196815031558,
-223.004263144959));
#229899=CARTESIAN_POINT('Ctrl Pts',(56.5783182101612,-8.8149783309306,-219.651370931397));
#229900=CARTESIAN_POINT('Ctrl Pts',(58.7928798280227,-8.740601282021,-216.298697969725));
#229901=CARTESIAN_POINT('Ctrl Pts',(61.0076271318174,-8.66753577332984,
-212.946121896728));
#229902=CARTESIAN_POINT('Ctrl Pts',(47.7223233313458,-9.1281354435798,-233.063967263389));
#229903=CARTESIAN_POINT('Ctrl Pts',(49.9349366327123,-9.04192415916445,
-229.710287182234));
#229904=CARTESIAN_POINT('Ctrl Pts',(52.1486261848584,-8.96173495275868,
-226.357198436518));
#229905=CARTESIAN_POINT('Ctrl Pts',(54.362683060283,-8.88397580633452,-223.004304045819));
#229906=CARTESIAN_POINT('Ctrl Pts',(56.5767399357077,-8.80621665991036,
-219.651409655121));
#229907=CARTESIAN_POINT('Ctrl Pts',(58.7912085661337,-8.73107636556752,
-216.298735224073));
#229908=CARTESIAN_POINT('Ctrl Pts',(61.0058638522065,-8.6572505633881,-212.946157967432));
#229909=CARTESIAN_POINT('Ctrl Pts',(47.7211311423516,-9.12247799776195,
-233.064017991084));
#229910=CARTESIAN_POINT('Ctrl Pts',(49.9336413200512,-9.03547708644307,
-229.710333027481));
#229911=CARTESIAN_POINT('Ctrl Pts',(52.1472334449741,-8.95451285699648,
-226.357241499541));
#229912=CARTESIAN_POINT('Ctrl Pts',(54.3611948094061,-8.87598426441826,
-223.004344929563));
#229913=CARTESIAN_POINT('Ctrl Pts',(56.5751561738381,-8.79745567184005,
-219.651448359586));
#229914=CARTESIAN_POINT('Ctrl Pts',(58.7895314509544,-8.72155201353807,
-216.298772458348));
#229915=CARTESIAN_POINT('Ctrl Pts',(61.004094357101,-8.64696579840547,-212.94619401758));
#229916=CARTESIAN_POINT('Ctrl Pts',(47.7199389533574,-9.11682055194411,
-233.06406871878));
#229917=CARTESIAN_POINT('Ctrl Pts',(49.9323460073902,-9.02903001372169,
-229.710378872728));
#229918=CARTESIAN_POINT('Ctrl Pts',(52.1458407050898,-8.94729076123427,
-226.357284562563));
#229919=CARTESIAN_POINT('Ctrl Pts',(54.3597065585291,-8.86799272250201,
-223.004385813307));
#229920=CARTESIAN_POINT('Ctrl Pts',(56.5735724119685,-8.78869468376974,
-219.651487064051));
#229921=CARTESIAN_POINT('Ctrl Pts',(58.7878543357751,-8.71202766150863,
-216.298809692624));
#229922=CARTESIAN_POINT('Ctrl Pts',(61.0023248619954,-8.63668103342285,
-212.946230067727));
#229923=CARTESIAN_POINT('Ctrl Pts',(47.7182360912236,-9.10778365437469,
-233.063849433542));
#229924=CARTESIAN_POINT('Ctrl Pts',(49.9305863062102,-9.01935713306031,
-229.710182118577));
#229925=CARTESIAN_POINT('Ctrl Pts',(52.1440124956181,-8.93694685535236,
-226.357101968979));
#229926=CARTESIAN_POINT('Ctrl Pts',(54.3578060024431,-8.85696406828125,
-223.004214571289));
#229927=CARTESIAN_POINT('Ctrl Pts',(56.5715995092681,-8.77698128121015,
-219.6513271736));
#229928=CARTESIAN_POINT('Ctrl Pts',(58.7858047409113,-8.69961462920092,
-216.298657989792));
#229929=CARTESIAN_POINT('Ctrl Pts',(61.0001966476166,-8.62356104366905,
-212.946085129856));
#229930=CARTESIAN_POINT('Ctrl Pts',(47.716754038316,-9.10015869973864,-233.063744037883));
#229931=CARTESIAN_POINT('Ctrl Pts',(49.9290284754874,-9.01103194700285,
-229.71008770866));
#229932=CARTESIAN_POINT('Ctrl Pts',(52.1423745037473,-8.92790717652798,
-226.357014582869));
#229933=CARTESIAN_POINT('Ctrl Pts',(54.3560864243857,-8.84720424996069,
-223.004132836908));
#229934=CARTESIAN_POINT('Ctrl Pts',(56.5697983450241,-8.7665013233934,-219.651251090947));
#229935=CARTESIAN_POINT('Ctrl Pts',(58.78392037252,-8.68840842352587,-216.298586025925));
#229936=CARTESIAN_POINT('Ctrl Pts',(60.9982283640248,-8.61162556319128,
-212.946016581829));
#229937=CARTESIAN_POINT('Ctrl Pts',(47.7137899325008,-9.08490879046653,
-233.063533246565));
#229938=CARTESIAN_POINT('Ctrl Pts',(49.9259128140418,-8.99438157488791,
-229.709898888829));
#229939=CARTESIAN_POINT('Ctrl Pts',(52.1390985200058,-8.90982781887923,
-226.356839810649));
#229940=CARTESIAN_POINT('Ctrl Pts',(54.3526472682709,-8.82768461331957,
-223.003969368145));
#229941=CARTESIAN_POINT('Ctrl Pts',(56.5661960165361,-8.74554140775991,
-219.65109892564));
#229942=CARTESIAN_POINT('Ctrl Pts',(58.7801516357373,-8.66599601217575,
-216.29844209819));
#229943=CARTESIAN_POINT('Ctrl Pts',(60.994291796841,-8.58775460223573,-212.945879485775));
#229944=CARTESIAN_POINT('Ctrl Pts',(47.7108458380545,-9.0696549360132,-233.063325140892));
#229945=CARTESIAN_POINT('Ctrl Pts',(49.9228183148681,-8.97772727901907,
-229.709712530571));
#229946=CARTESIAN_POINT('Ctrl Pts',(52.1358449148446,-8.89174460779308,
-226.356667358174));
#229947=CARTESIAN_POINT('Ctrl Pts',(54.3492317256771,-8.80816120630022,
-223.003808105078));
#229948=CARTESIAN_POINT('Ctrl Pts',(56.5626185365097,-8.72457780480736,
-219.650948851983));
#229949=CARTESIAN_POINT('Ctrl Pts',(58.7764090043429,-8.64358001183346,
-216.29830017932));
#229950=CARTESIAN_POINT('Ctrl Pts',(60.9903826008572,-8.56388015589151,
-212.945744329977));
#229951=CARTESIAN_POINT('Ctrl Pts',(47.7079217613744,-9.05439718416747,
-233.063119714194));
#229952=CARTESIAN_POINT('Ctrl Pts',(49.9197449843438,-8.96106910734242,
-229.709528628916));
#229953=CARTESIAN_POINT('Ctrl Pts',(52.1326136936507,-8.87365758922025,
-226.356497221309));
#229954=CARTESIAN_POINT('Ctrl Pts',(54.3458398007892,-8.78863407215474,
-223.003649044211));
#229955=CARTESIAN_POINT('Ctrl Pts',(56.5590659079277,-8.70361055508924,
-219.650800867113));
#229956=CARTESIAN_POINT('Ctrl Pts',(58.7726924798428,-8.62116045955843,
-216.298160266832));
#229957=CARTESIAN_POINT('Ctrl Pts',(60.9865007760101,-8.54000225738003,
-212.945611112248));
#229958=CARTESIAN_POINT('Ctrl Pts',(47.6845291479335,-8.93233516940169,
-233.061476300607));
#229959=CARTESIAN_POINT('Ctrl Pts',(49.8951583401493,-8.82780373392919,
-229.708057415679));
#229960=CARTESIAN_POINT('Ctrl Pts',(52.1067639241,-8.72896144063768,-226.355136126385));
#229961=CARTESIAN_POINT('Ctrl Pts',(54.3187044016857,-8.63241699899096,
-223.002376557269));
#229962=CARTESIAN_POINT('Ctrl Pts',(56.5306448792714,-8.53587255734424,
-219.649616988152));
#229963=CARTESIAN_POINT('Ctrl Pts',(58.7429602838421,-8.44180404135816,
-216.297040966938));
#229964=CARTESIAN_POINT('Ctrl Pts',(60.9554461772338,-8.34897906928816,
-212.944545370418));
#229965=CARTESIAN_POINT('Ctrl Pts',(47.6624176231886,-8.81002372665067,
-233.060004253171));
#229966=CARTESIAN_POINT('Ctrl Pts',(49.8719264576024,-8.69429031390039,
-229.706743359295));
#229967=CARTESIAN_POINT('Ctrl Pts',(52.0823467043952,-8.58402161768034,
-226.353923176935));
#229968=CARTESIAN_POINT('Ctrl Pts',(54.2930805177033,-8.47596139420291,
-223.001244967003));
#229969=CARTESIAN_POINT('Ctrl Pts',(56.5038143310114,-8.36790117072548,
-219.648566757072));
#229970=CARTESIAN_POINT('Ctrl Pts',(58.7148989206583,-8.26222030325806,
-216.296050047426));
#229971=CARTESIAN_POINT('Ctrl Pts',(60.9261433256064,-8.15773494598065,
-212.943603641929));
#229972=CARTESIAN_POINT('Ctrl Pts',(47.6415907958571,-8.68748728842518,
-233.058700763469));
#229973=CARTESIAN_POINT('Ctrl Pts',(49.8500528218283,-8.56055336019126,
-229.705584368071));
#229974=CARTESIAN_POINT('Ctrl Pts',(52.0593649584596,-8.43886161373385,
-226.352856624949));
#229975=CARTESIAN_POINT('Ctrl Pts',(54.2689704157657,-8.31928937162988,
-223.000252784861));
#229976=CARTESIAN_POINT('Ctrl Pts',(56.4785758730718,-8.19971712952592,
-219.647648944772));
#229977=CARTESIAN_POINT('Ctrl Pts',(58.6885092193172,-8.08242819326595,
-216.295186431349));
#229978=CARTESIAN_POINT('Ctrl Pts',(60.8985922273728,-7.96628687259449,
-212.942784965869));
#229979=CARTESIAN_POINT('Ctrl Pts',(47.5999371411941,-8.4424144119742,-233.056093784063));
#229980=CARTESIAN_POINT('Ctrl Pts',(49.8063055502802,-8.29307945277301,
-229.703266385626));
#229981=CARTESIAN_POINT('Ctrl Pts',(52.0134014665884,-8.14854160584086,
-226.350723520978));
#229982=CARTESIAN_POINT('Ctrl Pts',(54.2207502118905,-8.00594532648383,
-222.998268420575));
#229983=CARTESIAN_POINT('Ctrl Pts',(56.4280989571927,-7.8633490471268,-219.645813320171));
#229984=CARTESIAN_POINT('Ctrl Pts',(58.6357298166351,-7.72284397328174,
-216.293459199193));
#229985=CARTESIAN_POINT('Ctrl Pts',(60.8434900309058,-7.58339072582217,
-212.941147613748));
#229986=CARTESIAN_POINT('Ctrl Pts',(47.563421718127,-8.1964416177969,-233.054159991154));
#229987=CARTESIAN_POINT('Ctrl Pts',(49.7679908920149,-8.02471146303938,
-229.70156787831));
#229988=CARTESIAN_POINT('Ctrl Pts',(51.9731795871583,-7.85734092078273,
-226.34917536569));
#229989=CARTESIAN_POINT('Ctrl Pts',(54.1785849234471,-7.6917356528382,-222.996841160495));
#229990=CARTESIAN_POINT('Ctrl Pts',(56.3839902597359,-7.52613038489368,
-219.644506955299));
#229991=CARTESIAN_POINT('Ctrl Pts',(58.5896369612844,-7.36242630195994,
-216.292240840726));
#229992=CARTESIAN_POINT('Ctrl Pts',(60.7953947813852,-7.19967881344745,
-212.94000219184));
#229993=CARTESIAN_POINT('Ctrl Pts',(47.5320802669249,-7.94976361170966,
-233.052889623343));
#229994=CARTESIAN_POINT('Ctrl Pts',(49.7351412982067,-7.7556448112324,-229.700481632561));
#229995=CARTESIAN_POINT('Ctrl Pts',(51.9387261626187,-7.5654468780096,-226.348205936691));
#229996=CARTESIAN_POINT('Ctrl Pts',(54.1424952790584,-7.37683668146129,
-222.995965483144));
#229997=CARTESIAN_POINT('Ctrl Pts',(56.3462643954981,-7.18822648491298,
-219.643725029598));
#229998=CARTESIAN_POINT('Ctrl Pts',(58.5502384998489,-7.00132626939384,
-216.291526839263));
#229999=CARTESIAN_POINT('Ctrl Pts',(60.7543073371829,-6.81528655387943,
-212.939344378339));
#230000=CARTESIAN_POINT('Ctrl Pts',(47.4693973645209,-7.45640759953517,
-233.050348887721));
#230001=CARTESIAN_POINT('Ctrl Pts',(49.6694421105903,-7.21751150761842,
-229.698309141063));
#230002=CARTESIAN_POINT('Ctrl Pts',(51.8698193135396,-6.98165879246334,
-226.346267078691));
#230003=CARTESIAN_POINT('Ctrl Pts',(54.0703159902812,-6.74703873870746,
-222.994214128443));
#230004=CARTESIAN_POINT('Ctrl Pts',(56.2708126670227,-6.51241868495157,
-219.642161178194));
#230005=CARTESIAN_POINT('Ctrl Pts',(58.4714415769781,-6.27912620426164,
-216.290098836338));
#230006=CARTESIAN_POINT('Ctrl Pts',(60.6721324487782,-6.0465020347434,-212.938028751337));
#230007=CARTESIAN_POINT('Ctrl Pts',(47.4274705119234,-6.96033315507766,
-233.050468098652));
#230008=CARTESIAN_POINT('Ctrl Pts',(49.6256461602249,-6.6766507592267,-229.698589268665));
#230009=CARTESIAN_POINT('Ctrl Pts',(51.8240141959171,-6.39514045095797,
-226.346644939574));
#230010=CARTESIAN_POINT('Ctrl Pts',(54.0224528528355,-6.11450731222085,
-222.994669506924));
#230011=CARTESIAN_POINT('Ctrl Pts',(56.220891509754,-5.83387417348373,-219.642694074275));
#230012=CARTESIAN_POINT('Ctrl Pts',(58.419407944269,-5.55418636991015,-216.29068621863));
#230013=CARTESIAN_POINT('Ctrl Pts',(60.6179613338852,-5.27497371477569,
-212.938660660107));
#230014=CARTESIAN_POINT('Ctrl Pts',(47.4064137512828,-6.46376836204135,
-233.053237209745));
#230015=CARTESIAN_POINT('Ctrl Pts',(49.6038760388037,-6.13507130643716,
-229.701318673814));
#230016=CARTESIAN_POINT('Ctrl Pts',(51.8014392198341,-5.80767781765755,
-226.34934009846));
#230017=CARTESIAN_POINT('Ctrl Pts',(53.999040049297,-5.48080969928608,-222.997335349492));
#230018=CARTESIAN_POINT('Ctrl Pts',(56.19664087876,-5.15394158091461,-219.645330600522));
#230019=CARTESIAN_POINT('Ctrl Pts',(58.3942830138637,-4.82763991403419,
-216.293298098971));
#230020=CARTESIAN_POINT('Ctrl Pts',(60.5919449770341,-4.50162265073271,
-212.941251066378));
#230021=CARTESIAN_POINT('Ctrl Pts',(47.3643002300016,-5.47063877596875,
-233.058775431931));
#230022=CARTESIAN_POINT('Ctrl Pts',(49.5603357959614,-5.05191240085809,
-229.706777484113));
#230023=CARTESIAN_POINT('Ctrl Pts',(51.7562892676681,-4.63275255105671,
-226.354730416234));
#230024=CARTESIAN_POINT('Ctrl Pts',(53.9522144422201,-4.21341447341654,
-223.002667034626));
#230025=CARTESIAN_POINT('Ctrl Pts',(56.148139616772,-3.79407639577637,-219.650603653018));
#230026=CARTESIAN_POINT('Ctrl Pts',(58.3440331530531,-3.37454700228228,
-216.298521859654));
#230027=CARTESIAN_POINT('Ctrl Pts',(60.5399122633319,-2.95492052264675,
-212.94643187892));
#230028=CARTESIAN_POINT('Ctrl Pts',(47.4059785054068,-4.47517271098946,
-233.07487888378));
#230029=CARTESIAN_POINT('Ctrl Pts',(49.6051283878,-3.96564508196357,-229.721994650771));
#230030=CARTESIAN_POINT('Ctrl Pts',(51.8041981735258,-3.45390472955758,
-226.369343135129));
#230031=CARTESIAN_POINT('Ctrl Pts',(54.0032355320804,-2.94127591256867,
-223.016786754993));
#230032=CARTESIAN_POINT('Ctrl Pts',(56.202272890635,-2.42864709557977,-219.664230374857));
#230033=CARTESIAN_POINT('Ctrl Pts',(58.4012751950854,-1.91505962733557,
-216.311776149656));
#230034=CARTESIAN_POINT('Ctrl Pts',(60.6002595528876,-1.40099202884052,
-212.959373373456));
#230035=CARTESIAN_POINT('Ctrl Pts',(47.5294508970783,-3.49440615205346,
-233.102402864825));
#230036=CARTESIAN_POINT('Ctrl Pts',(49.7371099711637,-2.89175495532409,
-229.747791831751));
#230037=CARTESIAN_POINT('Ctrl Pts',(51.9449186325461,-2.28501732803231,
-226.3940294043));
#230038=CARTESIAN_POINT('Ctrl Pts',(54.1527566412239,-1.67669958626741,
-223.040576342272));
#230039=CARTESIAN_POINT('Ctrl Pts',(56.3605946499017,-1.0683818445025,-219.687123280246));
#230040=CARTESIAN_POINT('Ctrl Pts',(58.5684718967623,-0.458344461962341,
-216.334011708901));
#230041=CARTESIAN_POINT('Ctrl Pts',(60.7763601725369,0.15253653159383,-212.981062249621));
#230042=CARTESIAN_POINT('Ctrl Pts',(47.5448849460372,-3.37181033218646,
-233.105843362456));
#230043=CARTESIAN_POINT('Ctrl Pts',(49.7536076690841,-2.75751868949416,
-229.751016479375));
#230044=CARTESIAN_POINT('Ctrl Pts',(51.9625086899236,-2.13890640284165,
-226.397115187946));
#230045=CARTESIAN_POINT('Ctrl Pts',(54.1714467798668,-1.51862754547975,
-223.043550040683));
#230046=CARTESIAN_POINT('Ctrl Pts',(56.38038486981,-0.898348688117847,-219.68998489342));
#230047=CARTESIAN_POINT('Ctrl Pts',(58.5893714844719,-0.276255066290686,
-216.336791153806));
#230048=CARTESIAN_POINT('Ctrl Pts',(60.798372749993,0.346727601648124,-212.983773359142));
#230049=CARTESIAN_POINT('Ctrl Pts',(47.5615915692654,-3.24943555854357,
-233.109464818529));
#230050=CARTESIAN_POINT('Ctrl Pts',(49.7714637647986,-2.62347002868952,
-229.7544084453));
#230051=CARTESIAN_POINT('Ctrl Pts',(51.9815466632923,-1.99294743735296,
-226.40036014233));
#230052=CARTESIAN_POINT('Ctrl Pts',(54.1916753900507,-1.36067182993002,
-223.046676420892));
#230053=CARTESIAN_POINT('Ctrl Pts',(56.401804116809,-0.728396222507082,
-219.692992699454));
#230054=CARTESIAN_POINT('Ctrl Pts',(58.6119918904791,-0.0942105190696879,
-216.339712230689));
#230055=CARTESIAN_POINT('Ctrl Pts',(60.8221984456974,0.540909515678286,
-212.986622360574));
#230056=CARTESIAN_POINT('Ctrl Pts',(47.5795644264693,-3.1273054400959,-233.113272591666));
#230057=CARTESIAN_POINT('Ctrl Pts',(49.7906742268616,-2.48963297721053,
-229.757972064269));
#230058=CARTESIAN_POINT('Ctrl Pts',(52.0020311559296,-1.84716370589099,
-226.403768144263));
#230059=CARTESIAN_POINT('Ctrl Pts',(54.2134437517945,-1.20285465735803,
-223.049959011375));
#230060=CARTESIAN_POINT('Ctrl Pts',(56.4248563476593,-0.558545608825073,
-219.696149878487));
#230061=CARTESIAN_POINT('Ctrl Pts',(58.6363398184349,0.0877694602078754,
-216.342777920879));
#230062=CARTESIAN_POINT('Ctrl Pts',(60.8478467270347,0.735064158177848,
-212.989612083611));
#230063=CARTESIAN_POINT('Ctrl Pts',(47.5885508550713,-3.06624038087206,
-233.115176478235));
#230064=CARTESIAN_POINT('Ctrl Pts',(49.8002794578931,-2.42271445147103,
-229.759753873753));
#230065=CARTESIAN_POINT('Ctrl Pts',(52.0122734022483,-1.77427184016,-226.405472145231));
#230066=CARTESIAN_POINT('Ctrl Pts',(54.2243279326664,-1.12394607107203,
-223.051600306617));
#230067=CARTESIAN_POINT('Ctrl Pts',(56.4363824630845,-0.473620301984068,
-219.697728468003));
#230068=CARTESIAN_POINT('Ctrl Pts',(58.6485137824127,0.178759449846657,
-216.344310765974));
#230069=CARTESIAN_POINT('Ctrl Pts',(60.8606708677034,0.832141479427629,
-212.99110694513));
#230070=CARTESIAN_POINT('Ctrl Pts',(47.5978538522586,-3.00523648529404,
-233.117126961161));
#230071=CARTESIAN_POINT('Ctrl Pts',(49.8102232873676,-2.35584882925707,
-229.761578609019));
#230072=CARTESIAN_POINT('Ctrl Pts',(52.0228772837467,-1.70142378458667,
-226.407216918259));
#230073=CARTESIAN_POINT('Ctrl Pts',(54.2355970556278,-1.04507212252995,
-223.053280662751));
#230074=CARTESIAN_POINT('Ctrl Pts',(56.448316827509,-0.388720460473239,
-219.699344407242));
#230075=CARTESIAN_POINT('Ctrl Pts',(58.6611196292105,0.269733294988998,
-216.345879769661));
#230076=CARTESIAN_POINT('Ctrl Pts',(60.873950656561,0.929211980164266,-212.992636991345));
#230077=CARTESIAN_POINT('Ctrl Pts',(47.6074726880044,-2.94429670427164,
-233.119124814901));
#230078=CARTESIAN_POINT('Ctrl Pts',(49.8205052535735,-2.2890391191441,-229.763446888111));
#230079=CARTESIAN_POINT('Ctrl Pts',(52.0338426588191,-1.6286224591917,-226.409003009738));
#230080=CARTESIAN_POINT('Ctrl Pts',(54.2472513064603,-0.966235601713411,
-223.055000571257));
#230081=CARTESIAN_POINT('Ctrl Pts',(56.4606599541014,-0.303848744235122,
-219.700998132776));
#230082=CARTESIAN_POINT('Ctrl Pts',(58.6741582110175,0.36068851501233,-216.347485336292));
#230083=CARTESIAN_POINT('Ctrl Pts',(60.8876872878579,1.02627337962685,-212.994202601728));
#230084=CARTESIAN_POINT('Ctrl Pts',(47.6122821058773,-2.91382681376045,
-233.120123741771));
#230085=CARTESIAN_POINT('Ctrl Pts',(49.8256462366764,-2.25563426408762,
-229.764381027656));
#230086=CARTESIAN_POINT('Ctrl Pts',(52.0393253463554,-1.59222179649422,
-226.409896055477));
#230087=CARTESIAN_POINT('Ctrl Pts',(54.2530784318765,-0.926817341305142,
-223.05586052551));
#230088=CARTESIAN_POINT('Ctrl Pts',(56.4668315173976,-0.261412886116064,
-219.701824995542));
#230089=CARTESIAN_POINT('Ctrl Pts',(58.680677501921,0.406166125023995,-216.348288119608));
#230090=CARTESIAN_POINT('Ctrl Pts',(60.8945556035063,1.07480407935814,-212.99498540692));
#230091=CARTESIAN_POINT('Ctrl Pts',(47.6166843338988,-2.89479809257736,
-233.118546667211));
#230092=CARTESIAN_POINT('Ctrl Pts',(49.8304641874375,-2.23319920218914,
-229.762886946434));
#230093=CARTESIAN_POINT('Ctrl Pts',(52.0445356905235,-1.56647045026326,
-226.408456344895));
#230094=CARTESIAN_POINT('Ctrl Pts',(54.2586738605045,-0.897786580916013,
-223.054464805284));
#230095=CARTESIAN_POINT('Ctrl Pts',(56.4728120304856,-0.229102711568775,
-219.700473265674));
#230096=CARTESIAN_POINT('Ctrl Pts',(58.6870347127076,0.44171613101905,-216.346968914843));
#230097=CARTESIAN_POINT('Ctrl Pts',(60.9012859052481,1.11357395216271,-212.993693318827));
#230098=CARTESIAN_POINT('Ctrl Pts',(47.6211124898449,-2.8723889492326,-233.117728387381));
#230099=CARTESIAN_POINT('Ctrl Pts',(49.8352745925261,-2.20751597714286,
-229.762108046517));
#230100=CARTESIAN_POINT('Ctrl Pts',(52.0497152441705,-1.53755916668926,
-226.407703586764));
#230101=CARTESIAN_POINT('Ctrl Pts',(54.2642183610334,-0.865666855062723,
-223.053733238581));
#230102=CARTESIAN_POINT('Ctrl Pts',(56.4787214778963,-0.193774543436184,
-219.699762890398));
#230103=CARTESIAN_POINT('Ctrl Pts',(58.6933043194368,0.480231871349857,
-216.346274307009));
#230104=CARTESIAN_POINT('Ctrl Pts',(60.9079135866709,1.15526652998651,-212.993011881675));
#230105=CARTESIAN_POINT('Ctrl Pts',(47.6255406457911,-2.84997980588785,
-233.116910107551));
#230106=CARTESIAN_POINT('Ctrl Pts',(49.8400849976146,-2.18183275209659,
-229.761329146599));
#230107=CARTESIAN_POINT('Ctrl Pts',(52.0548947978176,-1.50864788311527,
-226.406950828634));
#230108=CARTESIAN_POINT('Ctrl Pts',(54.2697628615623,-0.83354712920943,
-223.053001671879));
#230109=CARTESIAN_POINT('Ctrl Pts',(56.4846309253071,-0.158446375303592,
-219.699052515123));
#230110=CARTESIAN_POINT('Ctrl Pts',(58.699573926166,0.518747611680667,-216.345579699174));
#230111=CARTESIAN_POINT('Ctrl Pts',(60.9145412680937,1.1969591078103,-212.992330444524));
#230112=CARTESIAN_POINT('Ctrl Pts',(47.6299049832871,-2.82756442152549,
-233.116092453226));
#230113=CARTESIAN_POINT('Ctrl Pts',(49.8448255724277,-2.15613841592184,
-229.760550756022));
#230114=CARTESIAN_POINT('Ctrl Pts',(52.0599987949363,-1.47972090207117,
-226.406198468922));
#230115=CARTESIAN_POINT('Ctrl Pts',(54.2752261916461,-0.801407134891986,
-223.052270410334));
#230116=CARTESIAN_POINT('Ctrl Pts',(56.4904535883559,-0.123093367712802,
-219.698342351745));
#230117=CARTESIAN_POINT('Ctrl Pts',(58.7057512556755,0.557292721778429,
-216.344885224803));
#230118=CARTESIAN_POINT('Ctrl Pts',(60.9210712376979,1.23868559335551,-212.991649073236));
#230119=CARTESIAN_POINT('Ctrl Pts',(47.6342055660403,-2.80514285302076,
-233.11527543729));
#230120=CARTESIAN_POINT('Ctrl Pts',(49.8494963118054,-2.13043323572804,
-229.759772872591));
#230121=CARTESIAN_POINT('Ctrl Pts',(52.0650271669924,-1.4507786685942,-226.405446498001));
#230122=CARTESIAN_POINT('Ctrl Pts',(54.2806082192958,-0.769247485060314,
-223.051539438634));
#230123=CARTESIAN_POINT('Ctrl Pts',(56.4961892715991,-0.0877163015264225,
-219.697632379269));
#230124=CARTESIAN_POINT('Ctrl Pts',(58.7118360495897,0.595866264290071,
-216.344190859432));
#230125=CARTESIAN_POINT('Ctrl Pts',(60.9275031739158,1.28044489740776,-212.990967740646));
#230126=CARTESIAN_POINT('Ctrl Pts',(47.6686102280658,-2.62577030498296,
-233.108739309799));
#230127=CARTESIAN_POINT('Ctrl Pts',(49.8868622268275,-1.92479179417762,
-229.753549805137));
#230128=CARTESIAN_POINT('Ctrl Pts',(52.1052541434417,-1.21924080077849,
-226.399430730627));
#230129=CARTESIAN_POINT('Ctrl Pts',(54.3236644404932,-0.511970286406943,
-223.045691665041));
#230130=CARTESIAN_POINT('Ctrl Pts',(56.5420747375447,0.195300227964602,
-219.691952599455));
#230131=CARTESIAN_POINT('Ctrl Pts',(58.7605144009039,0.904454604383199,
-216.338635936458));
#230132=CARTESIAN_POINT('Ctrl Pts',(60.9789586636595,1.61451932982577,-212.985517079921));
#230133=CARTESIAN_POINT('Ctrl Pts',(47.6989353797486,-2.4460016880478,-233.102243720839));
#230134=CARTESIAN_POINT('Ctrl Pts',(49.9197589274877,-1.71845616621595,
-229.747358791629));
#230135=CARTESIAN_POINT('Ctrl Pts',(52.1406411035373,-0.986726750840026,
-226.393439406672));
#230136=CARTESIAN_POINT('Ctrl Pts',(54.3615170914844,-0.253435215006592,
-223.039861978631));
#230137=CARTESIAN_POINT('Ctrl Pts',(56.5823930794315,0.479856320826842,
-219.686284550589));
#230138=CARTESIAN_POINT('Ctrl Pts',(58.8032699357002,1.21486234957556,-216.333087493431));
#230139=CARTESIAN_POINT('Ctrl Pts',(61.0241393837606,1.95069381201327,-212.980068394613));
#230140=CARTESIAN_POINT('Ctrl Pts',(47.725208148176,-2.26586793370592,-233.095797498554));
#230141=CARTESIAN_POINT('Ctrl Pts',(49.9481820104395,-1.51156427070571,
-229.741201508812));
#230142=CARTESIAN_POINT('Ctrl Pts',(52.171153048358,-0.753464571140378,
-226.387470648604));
#230143=CARTESIAN_POINT('Ctrl Pts',(54.3941000891112,0.00604443117689846,
-223.034045756));
#230144=CARTESIAN_POINT('Ctrl Pts',(56.6170471298644,0.765553433494175,
-219.680620863394));
#230145=CARTESIAN_POINT('Ctrl Pts',(58.8399741136204,1.52661141375358,-216.32753645248));
#230146=CARTESIAN_POINT('Ctrl Pts',(61.0628850955307,2.28841296751785,-212.974611260487));
#230147=CARTESIAN_POINT('Ctrl Pts',(47.777753685031,-1.90560042502214,-233.082905053984));
#230148=CARTESIAN_POINT('Ctrl Pts',(50.0050281763432,-1.0977804796852,-229.72888694318));
#230149=CARTESIAN_POINT('Ctrl Pts',(52.2321769379993,-0.286940211741083,
-226.375533132468));
#230150=CARTESIAN_POINT('Ctrl Pts',(54.4592660843647,0.525003723543879,
-223.022413310737));
#230151=CARTESIAN_POINT('Ctrl Pts',(56.6863552307302,1.33694765882884,-219.669293489006));
#230152=CARTESIAN_POINT('Ctrl Pts',(58.9133824694609,2.15010954210964,-216.316434370579));
#230153=CARTESIAN_POINT('Ctrl Pts',(61.140376519071,2.96385127852703,-212.963696992235));
#230154=CARTESIAN_POINT('Ctrl Pts',(47.8141039634246,-1.54378581355141,
-233.070233320969));
#230155=CARTESIAN_POINT('Ctrl Pts',(50.043980577362,-0.681755118427429,
-229.716715414099));
#230156=CARTESIAN_POINT('Ctrl Pts',(52.2736848111942,0.182550353550442,
-226.363684359704));
#230157=CARTESIAN_POINT('Ctrl Pts',(54.5033194303334,1.04768172667892,-223.010825413529));
#230158=CARTESIAN_POINT('Ctrl Pts',(56.7329540494726,1.91281309980739,-219.657966467354));
#230159=CARTESIAN_POINT('Ctrl Pts',(58.9625137255313,2.77885743664385,-216.305299102755));
#230160=CARTESIAN_POINT('Ctrl Pts',(61.192035920041,3.64533504273501,-212.952721389729));
#230161=CARTESIAN_POINT('Ctrl Pts',(47.8343566648447,-1.18129562201859,
-233.057735449668));
#230162=CARTESIAN_POINT('Ctrl Pts',(50.0649792011103,-0.264693413707682,
-229.704700485746));
#230163=CARTESIAN_POINT('Ctrl Pts',(52.2954559925465,0.653414022650932,
-226.351982116141));
#230164=CARTESIAN_POINT('Ctrl Pts',(54.525876562459,1.57206651464896,-222.999376095285));
#230165=CARTESIAN_POINT('Ctrl Pts',(56.7562971323714,2.49071900664698,-219.646770074429));
#230166=CARTESIAN_POINT('Ctrl Pts',(58.9866565003629,3.40997442959623,-216.294288989989));
#230167=CARTESIAN_POINT('Ctrl Pts',(61.2169859241647,4.32951560431301,-212.941866493395));
#230168=CARTESIAN_POINT('Ctrl Pts',(47.8748620676848,-0.456315238952961,
-233.032739707064));
#230169=CARTESIAN_POINT('Ctrl Pts',(50.106976448607,0.569429995731811,-229.68067062904));
#230170=CARTESIAN_POINT('Ctrl Pts',(52.3389983552511,1.59514136085191,-226.328577629014));
#230171=CARTESIAN_POINT('Ctrl Pts',(54.5709908267102,2.62083609058904,-222.976477458797));
#230172=CARTESIAN_POINT('Ctrl Pts',(56.8029832981692,3.64653082032617,-219.624377288579));
#230173=CARTESIAN_POINT('Ctrl Pts',(59.0349420500259,4.672208415501,-216.272268764454));
#230174=CARTESIAN_POINT('Ctrl Pts',(61.2668859324121,5.69787672746903,-212.920156700729));
#230175=CARTESIAN_POINT('Ctrl Pts',(47.8510697790929,0.272029506621824,
-233.008563181426));
#230176=CARTESIAN_POINT('Ctrl Pts',(50.0771558477705,1.40772928337885,-229.657271695028));
#230177=CARTESIAN_POINT('Ctrl Pts',(52.3034810716587,2.54196481575621,-226.305687299172));
#230178=CARTESIAN_POINT('Ctrl Pts',(54.5298878738176,3.67568259184972,-222.953998949698));
#230179=CARTESIAN_POINT('Ctrl Pts',(56.7562946759763,4.80940036794322,-219.602310600225));
#230180=CARTESIAN_POINT('Ctrl Pts',(58.9827932020866,5.94254191761289,-216.250506712501));
#230181=CARTESIAN_POINT('Ctrl Pts',(61.2093339293867,7.07541394960212,-212.898648776991));
#230182=CARTESIAN_POINT('Ctrl Pts',(47.7616858294571,0.998150138415235,
-232.985293804272));
#230183=CARTESIAN_POINT('Ctrl Pts',(49.9747881970607,2.24045815861694,-229.634704119062));
#230184=CARTESIAN_POINT('Ctrl Pts',(52.1886983731474,3.47997469249725,-226.283620725365));
#230185=CARTESIAN_POINT('Ctrl Pts',(54.4028959591866,4.71845222593428,-222.932344808848));
#230186=CARTESIAN_POINT('Ctrl Pts',(56.6170935452258,5.95692975937132,-219.581068892331));
#230187=CARTESIAN_POINT('Ctrl Pts',(58.8316104681301,7.19426601066472,-216.229583902017));
#230188=CARTESIAN_POINT('Ctrl Pts',(61.046277219474,8.43105358570855,-212.877995957148));
#230189=CARTESIAN_POINT('Ctrl Pts',(47.7393398420482,1.17968029636359,-232.979476459983));
#230190=CARTESIAN_POINT('Ctrl Pts',(49.9491962843832,2.44864037742646,-229.629062225071));
#230191=CARTESIAN_POINT('Ctrl Pts',(52.1600026985195,3.71447716168251,-226.278104081914));
#230192=CARTESIAN_POINT('Ctrl Pts',(54.3711479805289,4.97914463445542,-222.926931273635));
#230193=CARTESIAN_POINT('Ctrl Pts',(56.5822932625382,6.24381210722835,-219.575758465357));
#230194=CARTESIAN_POINT('Ctrl Pts',(58.7938147846409,7.50719703392768,-216.224353199397));
#230195=CARTESIAN_POINT('Ctrl Pts',(61.0055130419957,8.76996349473516,-212.872832752187));
#230196=CARTESIAN_POINT('Ctrl Pts',(47.7128809309633,1.36106465955398,-232.973714427979));
#230197=CARTESIAN_POINT('Ctrl Pts',(49.9190688863809,2.65647440303478,-229.623470833417));
#230198=CARTESIAN_POINT('Ctrl Pts',(52.1263647289421,3.94843444171322,-226.272637535688));
#230199=CARTESIAN_POINT('Ctrl Pts',(54.3340573658958,5.23909322841377,-222.921567986388));
#230200=CARTESIAN_POINT('Ctrl Pts',(56.5417500028495,6.52975201511432,-219.570498437088));
#230201=CARTESIAN_POINT('Ctrl Pts',(58.7498827079224,7.81898619339649,-216.219173942379));
#230202=CARTESIAN_POINT('Ctrl Pts',(60.9582225191604,9.10753070501037,-212.867722142776));
#230203=CARTESIAN_POINT('Ctrl Pts',(47.6822473288034,1.54226015711989,-232.968019332623));
#230204=CARTESIAN_POINT('Ctrl Pts',(49.8843891563535,2.86381435135825,-229.6179346096));
#230205=CARTESIAN_POINT('Ctrl Pts',(52.0878067306158,4.18161224455118,-226.267221321995));
#230206=CARTESIAN_POINT('Ctrl Pts',(54.2916843246343,5.49797977211644,-222.916251722872));
#230207=CARTESIAN_POINT('Ctrl Pts',(56.4955619186529,6.81434729968171,-219.565282123748));
#230208=CARTESIAN_POINT('Ctrl Pts',(58.6999487759841,8.12915246217079,-216.214037028638));
#230209=CARTESIAN_POINT('Ctrl Pts',(60.9045760974657,9.44319745618915,-212.862653075561));
#230210=CARTESIAN_POINT('Ctrl Pts',(47.6745889282634,1.58755903151136,-232.966595558784));
#230211=CARTESIAN_POINT('Ctrl Pts',(49.8757192238467,2.91564933843912,-229.616550553645));
#230212=CARTESIAN_POINT('Ctrl Pts',(52.0781672310342,4.23990669526066,-226.265867268572));
#230213=CARTESIAN_POINT('Ctrl Pts',(54.281091064319,5.56270140804211,-222.914922656992));
#230214=CARTESIAN_POINT('Ctrl Pts',(56.4840148976038,6.88549612082355,-219.563978045413));
#230215=CARTESIAN_POINT('Ctrl Pts',(58.6874652929996,8.20669402936436,-216.212752800202));
#230216=CARTESIAN_POINT('Ctrl Pts',(60.891164492042,9.52711414398385,-212.861385808758));
#230217=CARTESIAN_POINT('Ctrl Pts',(47.6666695671617,1.63284608999026,-232.96517598567));
#230218=CARTESIAN_POINT('Ctrl Pts',(49.8667647552568,2.96745344462007,-229.615169968288));
#230219=CARTESIAN_POINT('Ctrl Pts',(52.0682202296165,4.29815242923168,-226.264516384494));
#230220=CARTESIAN_POINT('Ctrl Pts',(54.2701676639963,5.62735666781534,-222.913596554258));
#230221=CARTESIAN_POINT('Ctrl Pts',(56.4721150983761,6.956560906399,-219.562676724022));
#230222=CARTESIAN_POINT('Ctrl Pts',(58.6746067250159,8.28413416941793,-216.211471242811));
#230223=CARTESIAN_POINT('Ctrl Pts',(60.8773556798765,9.61091205669726,-212.860121162684));
#230224=CARTESIAN_POINT('Ctrl Pts',(47.6584881964675,1.67812063274807,-232.963760828248));
#230225=CARTESIAN_POINT('Ctrl Pts',(49.8575254560703,3.01922438781437,-229.613792971254));
#230226=CARTESIAN_POINT('Ctrl Pts',(52.0579660735326,4.35634578681776,-226.263168720394));
#230227=CARTESIAN_POINT('Ctrl Pts',(54.2589150870478,5.6919405831028,-222.912273412552));
#230228=CARTESIAN_POINT('Ctrl Pts',(56.459864100563,7.02753537938784,-219.56137810471));
#230229=CARTESIAN_POINT('Ctrl Pts',(58.6613752354701,8.36146537341484,-216.210192263444));
#230230=CARTESIAN_POINT('Ctrl Pts',(60.8631523975563,9.69458248633691,-212.858859013292));
#230231=CARTESIAN_POINT('Ctrl Pts',(47.6543975111204,1.70075790412697,-232.963053249537));
#230232=CARTESIAN_POINT('Ctrl Pts',(49.8529058064771,3.04510985941153,-229.613104472738));
#230233=CARTESIAN_POINT('Ctrl Pts',(52.0528389954907,4.38544246561079,-226.262494888344));
#230234=CARTESIAN_POINT('Ctrl Pts',(54.2532887985736,5.72423254074652,-222.911611841699));
#230235=CARTESIAN_POINT('Ctrl Pts',(56.4537386016565,7.06302261588225,-219.560728795054));
#230236=CARTESIAN_POINT('Ctrl Pts',(58.6547594906971,8.4001309754133,-216.209552773761));
#230237=CARTESIAN_POINT('Ctrl Pts',(60.8560507563961,9.73641770115673,-212.858227938596));
#230238=CARTESIAN_POINT('Ctrl Pts',(47.6502413228594,1.72339204637661,-232.962346774948));
#230239=CARTESIAN_POINT('Ctrl Pts',(49.8482149490333,3.07098704024018,-229.612416871579));
#230240=CARTESIAN_POINT('Ctrl Pts',(52.0476351287711,4.41452605031363,-226.261821861581));
#230241=CARTESIAN_POINT('Ctrl Pts',(54.2475802160774,5.75650666229548,-222.910951011405));
#230242=CARTESIAN_POINT('Ctrl Pts',(56.4475253033837,7.09848727427732,-219.560080161228));
#230243=CARTESIAN_POINT('Ctrl Pts',(58.6480505159108,8.43876934344246,-216.208913928891));
#230244=CARTESIAN_POINT('Ctrl Pts',(60.8488504981511,9.77822104524949,-212.857597488374));
#230245=CARTESIAN_POINT('Ctrl Pts',(47.6460194974834,1.74602297076459,-232.961641432517));
#230246=CARTESIAN_POINT('Ctrl Pts',(49.8434528457034,3.09685564489722,-229.611730184141));
#230247=CARTESIAN_POINT('Ctrl Pts',(52.042354516691,4.44359608350473,-226.26114964818));
#230248=CARTESIAN_POINT('Ctrl Pts',(54.2417894607756,5.78876232686925,-222.91029092321));
#230249=CARTESIAN_POINT('Ctrl Pts',(56.4412244048602,7.13392857023377,-219.559432198239));
#230250=CARTESIAN_POINT('Ctrl Pts',(58.6412485837932,8.47737953915866,-216.208275719059));
#230251=CARTESIAN_POINT('Ctrl Pts',(60.8415519676109,9.81999143035988,-212.856967648949));
#230252=CARTESIAN_POINT('Ctrl Pts',(47.6439085847953,1.75733843295859,-232.961288761302));
#230253=CARTESIAN_POINT('Ctrl Pts',(49.8410717940384,3.10978994722575,-229.611386840422));
#230254=CARTESIAN_POINT('Ctrl Pts',(52.0397142106509,4.45813110010028,-226.26081354148));
#230255=CARTESIAN_POINT('Ctrl Pts',(54.2388940831247,5.80489015915614,-222.909960879112));
#230256=CARTESIAN_POINT('Ctrl Pts',(56.4380739555984,7.151649218212,-219.559108216744));
#230257=CARTESIAN_POINT('Ctrl Pts',(58.6378476177344,8.49668463701677,-216.207956614142));
#230258=CARTESIAN_POINT('Ctrl Pts',(60.8379027023408,9.84087662291507,-212.856652729236));
#230259=CARTESIAN_POINT('Ctrl Pts',(47.6422722132824,1.76718782952786,-232.960678696067));
#230260=CARTESIAN_POINT('Ctrl Pts',(49.8391375264504,3.12130996362475,-229.610790689353));
#230261=CARTESIAN_POINT('Ctrl Pts',(52.0375016868396,4.47128714932663,-226.260228329323));
#230262=CARTESIAN_POINT('Ctrl Pts',(54.2364107003475,5.81966765975101,-222.909384848415));
#230263=CARTESIAN_POINT('Ctrl Pts',(56.4353197138554,7.16804817017539,-219.558541367508));
#230264=CARTESIAN_POINT('Ctrl Pts',(58.6348306124533,8.51468948441525,-216.207397187139));
#230265=CARTESIAN_POINT('Ctrl Pts',(60.8346268351599,9.86047939512299,-212.856099681471));
#230266=CARTESIAN_POINT('Ctrl Pts',(47.6389054467951,1.78211913870348,-232.960962398579));
#230267=CARTESIAN_POINT('Ctrl Pts',(49.8355621025854,3.13772585835723,-229.611072178893));
#230268=CARTESIAN_POINT('Ctrl Pts',(52.033706981916,4.48921062136337,-226.260507824327));
#230269=CARTESIAN_POINT('Ctrl Pts',(54.2323930398121,5.83910740022999,-222.909662643248));
#230270=CARTESIAN_POINT('Ctrl Pts',(56.4310790977081,7.18900417909662,-219.558817462169));
#230271=CARTESIAN_POINT('Ctrl Pts',(58.6303629299522,8.5371712694402,-216.207671846982));
#230272=CARTESIAN_POINT('Ctrl Pts',(60.8299301929379,9.88449155844584,-212.856373094261));
#230273=CARTESIAN_POINT('Ctrl Pts',(47.6355386803079,1.79705044787909,-232.961246101092));
#230274=CARTESIAN_POINT('Ctrl Pts',(49.8319866787204,3.15414175308971,-229.611353668433));
#230275=CARTESIAN_POINT('Ctrl Pts',(52.0299122769924,4.5071340934001,-226.260787319329));
#230276=CARTESIAN_POINT('Ctrl Pts',(54.2283753792766,5.85854714070898,-222.90994043808));
#230277=CARTESIAN_POINT('Ctrl Pts',(56.4268384815609,7.20996018801785,-219.55909355683));
#230278=CARTESIAN_POINT('Ctrl Pts',(58.6258952474512,8.55965305446516,-216.207946506826));
#230279=CARTESIAN_POINT('Ctrl Pts',(60.825233550716,9.90850372176869,-212.856646507051));
#230280=CARTESIAN_POINT('Ctrl Pts',(47.6321910253286,1.81198694050772,-232.961532361149));
#230281=CARTESIAN_POINT('Ctrl Pts',(49.8284317983937,3.17056265356817,-229.61163754231));
#230282=CARTESIAN_POINT('Ctrl Pts',(52.026139583098,4.52506239807395,-226.261069085663));
#230283=CARTESIAN_POINT('Ctrl Pts',(54.22438120628,5.87799154637645,-222.910220412602));
#230284=CARTESIAN_POINT('Ctrl Pts',(56.422622829462,7.23092069467897,-219.559371739542));
#230285=CARTESIAN_POINT('Ctrl Pts',(58.6214540165528,8.58213917498653,-216.208223186853));
#230286=CARTESIAN_POINT('Ctrl Pts',(60.8205648517821,9.93252006210882,-212.856921883345));
#230287=CARTESIAN_POINT('Ctrl Pts',(47.628862493758,1.82692857762527,-232.96182118511));
#230288=CARTESIAN_POINT('Ctrl Pts',(49.8248974717912,3.18698851762863,-229.611923806209));
#230289=CARTESIAN_POINT('Ctrl Pts',(52.0223889083793,4.54299549104381,-226.26135312848));
#230290=CARTESIAN_POINT('Ctrl Pts',(54.2204105268588,5.89744057105422,-222.91050257153));
#230291=CARTESIAN_POINT('Ctrl Pts',(56.4184321453384,7.25188565106463,-219.559652014579));
#230292=CARTESIAN_POINT('Ctrl Pts',(58.6170392389817,8.60462958153552,-216.208501890991));
#230293=CARTESIAN_POINT('Ctrl Pts',(60.8159240956269,9.95654052871553,-212.857199226772));
#230294=CARTESIAN_POINT('Ctrl Pts',(47.602234241193,1.94646167456563,-232.964131776795));
#230295=CARTESIAN_POINT('Ctrl Pts',(49.7966228589716,3.3183954301123,-229.614213917398));
#230296=CARTESIAN_POINT('Ctrl Pts',(51.9923835106293,4.68646023480269,-226.263625471024));
#230297=CARTESIAN_POINT('Ctrl Pts',(54.1886450914894,6.05303276847634,-222.912759842952));
#230298=CARTESIAN_POINT('Ctrl Pts',(56.3849066723495,7.41960530214998,-219.561894214879));
#230299=CARTESIAN_POINT('Ctrl Pts',(58.5817210184137,8.78455283392743,-216.210731524094));
#230300=CARTESIAN_POINT('Ctrl Pts',(60.7787980463854,10.1487042615692,-212.859417974186));
#230301=CARTESIAN_POINT('Ctrl Pts',(47.5768298455065,2.06632401207208,-232.96660639255));
#230302=CARTESIAN_POINT('Ctrl Pts',(49.7696636517176,3.45012000579785,-229.616656935729));
#230303=CARTESIAN_POINT('Ctrl Pts',(51.9637873118318,4.83023142413465,-226.266043461076));
#230304=CARTESIAN_POINT('Ctrl Pts',(54.158383220178,6.2089205777349,-222.915156874141));
#230305=CARTESIAN_POINT('Ctrl Pts',(56.3529791285242,7.58760973133515,-219.564270287207));
#230306=CARTESIAN_POINT('Ctrl Pts',(58.5480957918528,8.96475038827362,-216.213090667097));
#230307=CARTESIAN_POINT('Ctrl Pts',(60.7434603178749,10.3411320720609,-212.861762587924));
#230308=CARTESIAN_POINT('Ctrl Pts',(47.5526556810106,2.18649568630384,-232.969248737689));
#230309=CARTESIAN_POINT('Ctrl Pts',(49.7440252884103,3.58214069800097,-229.619256142275));
#230310=CARTESIAN_POINT('Ctrl Pts',(51.9366046755093,4.97428639343047,-226.268610062602));
#230311=CARTESIAN_POINT('Ctrl Pts',(54.129628172195,6.36508038888444,-222.917696367826));
#230312=CARTESIAN_POINT('Ctrl Pts',(56.3226516688807,7.7558743843384,-219.56678267305));
#230313=CARTESIAN_POINT('Ctrl Pts',(58.5161645712576,9.14519694298261,-216.215581556974));
#230314=CARTESIAN_POINT('Ctrl Pts',(60.7099107655409,10.5337979996055,-212.864235131559));
#230315=CARTESIAN_POINT('Ctrl Pts',(47.4559590230269,2.66718238323085,-232.979818118251));
#230316=CARTESIAN_POINT('Ctrl Pts',(49.6414718351808,4.11022346681344,-229.629652968461));
#230317=CARTESIAN_POINT('Ctrl Pts',(51.8278741302197,5.55050627061373,-226.278876468708));
#230318=CARTESIAN_POINT('Ctrl Pts',(54.0146079802632,6.98971963348256,-222.927854342566));
#230319=CARTESIAN_POINT('Ctrl Pts',(56.2013418303068,8.4289329963514,-219.576832216423));
#230320=CARTESIAN_POINT('Ctrl Pts',(58.3884396888769,9.86698316181859,-216.225545116483));
#230321=CARTESIAN_POINT('Ctrl Pts',(60.5757125562048,11.3044617097837,-212.874125306097));
#230322=CARTESIAN_POINT('Ctrl Pts',(47.3789343509497,3.15281732296621,-232.993054381077));
#230323=CARTESIAN_POINT('Ctrl Pts',(49.5600425408639,4.64304306902027,-229.642534956489));
#230324=CARTESIAN_POINT('Ctrl Pts',(51.7417525219173,6.13126572956288,-226.291508540064));
#230325=CARTESIAN_POINT('Ctrl Pts',(53.9236899017093,7.61871011984863,-222.94028097047));
#230326=CARTESIAN_POINT('Ctrl Pts',(56.1056272815015,9.10615451013438,-219.589053400875));
#230327=CARTESIAN_POINT('Ctrl Pts',(58.2878135060677,10.5927527992689,-216.237608203082));
#230328=CARTESIAN_POINT('Ctrl Pts',(60.4701203002903,12.0789347832393,-212.886054712549));
#230329=CARTESIAN_POINT('Ctrl Pts',(47.3220782931503,3.64213739520988,-233.009326653747));
#230330=CARTESIAN_POINT('Ctrl Pts',(49.5001561272747,5.17923014873171,-229.65822098902));
#230331=CARTESIAN_POINT('Ctrl Pts',(51.6785800990322,6.71512263630363,-226.306791304678));
#230332=CARTESIAN_POINT('Ctrl Pts',(53.8571359353927,8.25054831515734,-222.955233810924));
#230333=CARTESIAN_POINT('Ctrl Pts',(56.0356917717532,9.78597399401105,-219.603676317171));
#230334=CARTESIAN_POINT('Ctrl Pts',(58.2143916305598,11.3208922926972,-216.251980359006));
#230335=CARTESIAN_POINT('Ctrl Pts',(60.3931615898891,12.8555608031383,-212.900215711346));
#230336=CARTESIAN_POINT('Ctrl Pts',(47.0946540619524,5.59941768418452,-233.074415744431));
#230337=CARTESIAN_POINT('Ctrl Pts',(49.2606104729176,7.3239784675775,-229.720965119143));
#230338=CARTESIAN_POINT('Ctrl Pts',(51.4258904074922,9.05055026326663,-226.367922363131));
#230339=CARTESIAN_POINT('Ctrl Pts',(53.5909200701262,10.7779010963922,-223.015045172743));
#230340=CARTESIAN_POINT('Ctrl Pts',(55.7559497327601,12.5052519295177,-219.662167982355));
#230341=CARTESIAN_POINT('Ctrl Pts',(57.9207041285279,14.2334502664104,-216.309468982699));
#230342=CARTESIAN_POINT('Ctrl Pts',(60.0853267482839,15.9620648827344,-212.956859706535));
#230343=CARTESIAN_POINT('Ctrl Pts',(47.1914720210979,7.6140088721643,-233.185323795226));
#230344=CARTESIAN_POINT('Ctrl Pts',(49.3672203068766,9.52128975296003,-229.826228944008));
#230345=CARTESIAN_POINT('Ctrl Pts',(51.5415920964213,11.4345056878504,-226.469384191172));
#230346=CARTESIAN_POINT('Ctrl Pts',(53.7154316537813,13.3500108047595,-223.113404278841));
#230347=CARTESIAN_POINT('Ctrl Pts',(55.8892712111413,15.2655159216685,-219.757424366509));
#230348=CARTESIAN_POINT('Ctrl Pts',(58.0625313135173,17.1835155618891,-216.402388112408));
#230349=CARTESIAN_POINT('Ctrl Pts',(60.2355063327765,19.10274141504,-213.047815750158));
#230350=CARTESIAN_POINT('Ctrl Pts',(47.6396641907623,9.56951109638858,-233.375524009166));
#230351=CARTESIAN_POINT('Ctrl Pts',(49.8405355389308,11.6556158167396,-230.003433166063));
#230352=CARTESIAN_POINT('Ctrl Pts',(52.0418116007037,13.7520462993107,-226.638133451275));
#230353=CARTESIAN_POINT('Ctrl Pts',(54.2429855256817,15.8525357612388,-223.275331821509));
#230354=CARTESIAN_POINT('Ctrl Pts',(56.4441594506596,17.9530252231669,-219.912530191744));
#230355=CARTESIAN_POINT('Ctrl Pts',(58.6452885751193,20.0579121947712,-216.552478218177));
#230356=CARTESIAN_POINT('Ctrl Pts',(60.846321628963,22.164968605821,-213.193734192871));
#230357=CARTESIAN_POINT('',(47.764389394009,6.457751620915,-232.249941470341));
#230358=CARTESIAN_POINT('Ctrl Pts',(47.7643209768376,6.45773200978314,-232.25005));
#230359=CARTESIAN_POINT('Ctrl Pts',(47.7428191347604,6.03142608206569,-232.25005));
#230360=CARTESIAN_POINT('Ctrl Pts',(47.736924890541,5.60456323298173,-232.25005));
#230361=CARTESIAN_POINT('Ctrl Pts',(47.7570432133228,4.73973393711202,-232.25005));
#230362=CARTESIAN_POINT('Ctrl Pts',(47.7839000023451,4.3022757671813,-232.25005));
#230363=CARTESIAN_POINT('Ctrl Pts',(47.8275275119679,3.86645886896212,-232.25005));
#230364=CARTESIAN_POINT('Ctrl Pts',(47.9644369063438,-4.51936301034905,
-232.25005));
#230365=CARTESIAN_POINT('Ctrl Pts',(47.9319477127382,-4.97119958827373,
-232.25005));
#230366=CARTESIAN_POINT('Ctrl Pts',(47.9174772002993,-5.4242563204813,-232.25005));
#230367=CARTESIAN_POINT('Ctrl Pts',(47.9248943476532,-6.33010682966948,
-232.25005));
#230368=CARTESIAN_POINT('Ctrl Pts',(47.9467635068849,-6.78180672474201,
-232.25005));
#230369=CARTESIAN_POINT('Ctrl Pts',(47.9866861404266,-7.23226624733622,
-232.25005));
#230370=CARTESIAN_POINT('Ctrl Pts',(47.9849458443841,-16.0452823276962,
-232.25005));
#230371=CARTESIAN_POINT('Ctrl Pts',(47.9462873350434,-16.4877633300649,
-232.25005));
#230372=CARTESIAN_POINT('Ctrl Pts',(47.925045029397,-16.9313785096498,-232.25005));
#230373=CARTESIAN_POINT('Ctrl Pts',(47.9174315480329,-17.8216218039863,
-232.25005));
#230374=CARTESIAN_POINT('Ctrl Pts',(47.9311272354818,-18.2671770665058,
-232.25005));
#230375=CARTESIAN_POINT('Ctrl Pts',(47.962113157865,-18.7116122763947,-232.25005));
#230376=CARTESIAN_POINT('',(47.7598796739981,-29.633055067729,-232.249824579212));
#230377=CARTESIAN_POINT('Ctrl Pts',(47.8203127214913,-27.1915604688603,
-232.25005));
#230378=CARTESIAN_POINT('Ctrl Pts',(47.7812806514964,-27.6015079559573,
-232.25005));
#230379=CARTESIAN_POINT('Ctrl Pts',(47.7568712560738,-28.0131227629508,
-232.250050000005));
#230380=CARTESIAN_POINT('Ctrl Pts',(47.7374545095719,-28.8282292839852,
-232.250050000005));
#230381=CARTESIAN_POINT('Ctrl Pts',(47.7417582300801,-29.2308218767449,
-232.25005));
#230382=CARTESIAN_POINT('Ctrl Pts',(47.7597386834877,-29.6330167878826,
-232.25005));
#230383=CARTESIAN_POINT('Ctrl Pts',(47.7600215786063,-29.6330588251263,
-232.249824579212));
#230384=CARTESIAN_POINT('Ctrl Pts',(47.7599867924269,-29.6343725853688,
-232.249899719474));
#230385=CARTESIAN_POINT('Ctrl Pts',(47.7599520024663,-29.6356863455112,
-232.249974859737));
#230386=CARTESIAN_POINT('Ctrl Pts',(47.7599172087245,-29.6370001055535,
-232.25005));
#230387=CARTESIAN_POINT('Ctrl Pts',(47.7644117008771,6.45952891261178,-232.25005));
#230388=CARTESIAN_POINT('Ctrl Pts',(47.7644272274268,6.45893708439671,-232.250013823447));
#230389=CARTESIAN_POINT('Ctrl Pts',(47.7644427532091,6.45834525616151,-232.249977646894));
#230390=CARTESIAN_POINT('Ctrl Pts',(47.7644582782241,6.45775342790618,-232.249941470341));
#230391=CARTESIAN_POINT('Origin',(48.1334350484927,-61.7961505568785,-218.306418983907));
#230392=CARTESIAN_POINT('Origin',(24.838300653577,28.3971299569735,-229.35005));
#230393=CARTESIAN_POINT('',(24.960358769668,29.3896529120211,-229.35005));
#230394=CARTESIAN_POINT('',(25.366775135568,29.2460791438418,-229.35005));
#230395=CARTESIAN_POINT('Origin',(-6.29739814579425E-15,-11.5034818258363,
-229.35005));
#230396=CARTESIAN_POINT('',(39.8203148590359,15.2984308769399,-229.35005));
#230397=CARTESIAN_POINT('Origin',(38.9907249661392,14.740057695632,-229.35005));
#230398=CARTESIAN_POINT('',(39.989972084972,14.7788545447883,-229.35005));
#230399=CARTESIAN_POINT('Origin',(-636.934816028482,-11.5034818258361,-229.35005));
#230400=CARTESIAN_POINT('Origin',(38.9907249661392,-37.7470213473046,-229.35005));
#230401=CARTESIAN_POINT('',(39.989972084972,-37.7858181964606,-229.35005));
#230402=CARTESIAN_POINT('',(39.8203148590358,-38.3053945286125,-229.35005));
#230403=CARTESIAN_POINT('Origin',(-6.29739814579425E-15,-11.5034818258363,
-229.35005));
#230404=CARTESIAN_POINT('Origin',(22.9178089794592,-52.5372975341153,-229.35005));
#230405=CARTESIAN_POINT('',(23.4054219364689,-53.410357442802,-229.35005));
#230406=CARTESIAN_POINT('',(22.9516892713016,-53.5367234322311,-229.35005));
#230407=CARTESIAN_POINT('Origin',(48.892180948596,36.2913696007177,-218.35005));
#230408=CARTESIAN_POINT('',(48.892180948596,32.9413696007177,-218.35005));
#230409=CARTESIAN_POINT('Origin',(48.892180948596,36.2913696007177,-218.35005));
#230410=CARTESIAN_POINT('Origin',(48.892180948596,36.2913696007177,-218.35005));
#230411=CARTESIAN_POINT('',(48.892180948596,32.9413696007177,-218.35005));
#230412=CARTESIAN_POINT('Origin',(48.1334350484927,-61.7961505568785,-218.35005));
#230413=CARTESIAN_POINT('',(48.1334350484927,-65.1461505568793,-218.35005));
#230414=CARTESIAN_POINT('Origin',(48.1334350484927,-61.7961505568785,-218.35005));
#230415=CARTESIAN_POINT('Origin',(48.1334350484927,-61.7961505568785,-218.35005));
#230416=CARTESIAN_POINT('',(48.1334350484927,-65.1461505568793,-218.35005));
#230417=CARTESIAN_POINT('Origin',(0.127542579976414,-12.8706479699377,-228.35005));
#230418=CARTESIAN_POINT('Origin',(55.2047656166361,-61.9923285455256,-228.35005));
#230419=CARTESIAN_POINT('Origin',(48.1954151687739,-68.8699303295103,-228.35005));
#230420=CARTESIAN_POINT('Origin',(0.127542579976414,-12.8706479699377,-228.35005));
#230421=CARTESIAN_POINT('Origin',(0.128459562639233,-12.6359082483571,-228.35005));
#230422=CARTESIAN_POINT('Origin',(48.6323674899383,42.9861279943057,-228.35005));
#230423=CARTESIAN_POINT('Origin',(55.5877717798047,36.0539745652106,-228.35005));
#230424=CARTESIAN_POINT('Origin',(0.128459562639233,-12.6359082483571,-228.35005));
#230425=CARTESIAN_POINT('Origin',(51.397926952212,-43.6786252257833,-167.906149834141));
#230426=CARTESIAN_POINT('Origin',(51.7304496786285,-70.1559157828803,-167.906149834141));
#230427=CARTESIAN_POINT('Origin',(0.,-12.9675000200281,-167.906149834141));
#230428=CARTESIAN_POINT('Origin',(51.3278340104563,17.8606293780317,-167.906149834141));
#230429=CARTESIAN_POINT('Origin',(51.6000409161409,44.3386087195339,-167.906149834141));
#230430=CARTESIAN_POINT('Origin',(0.,-12.9675000200281,-167.906149834141));
#230431=CARTESIAN_POINT('Ctrl Pts',(-43.8493461424558,-78.8521074299086,
-211.864982076876));
#230432=CARTESIAN_POINT('Ctrl Pts',(-21.0752244585295,-62.961249057474,
-239.042379319384));
#230433=CARTESIAN_POINT('Ctrl Pts',(-40.4601948759454,-78.0802943160701,
-211.86498207687));
#230434=CARTESIAN_POINT('Ctrl Pts',(-19.8470357167519,-61.333671538836,
-239.042379319393));
#230435=CARTESIAN_POINT('Ctrl Pts',(-36.4842840549755,-77.5339017897621,
-211.864982076872));
#230436=CARTESIAN_POINT('Ctrl Pts',(-17.4751640410206,-60.0398805476777,
-239.042379319393));
#230437=CARTESIAN_POINT('Ctrl Pts',(-31.6477754280485,-77.4599324799423,
-211.864982076871));
#230438=CARTESIAN_POINT('Ctrl Pts',(-14.5387717509043,-59.7364199365376,
-239.042379319393));
#230439=CARTESIAN_POINT('Ctrl Pts',(-29.3183793276549,-77.5317048145231,
-211.864982076871));
#230440=CARTESIAN_POINT('Ctrl Pts',(-13.1728997877445,-59.8076087424511,
-239.042379319393));
#230441=CARTESIAN_POINT('Ctrl Pts',(-27.7276393867415,-77.6574160379369,
-211.864982076871));
#230442=CARTESIAN_POINT('Ctrl Pts',(-12.3078514256087,-59.9884330330066,
-239.042379319393));
#230443=CARTESIAN_POINT('Ctrl Pts',(-26.1251285606442,-77.8260872807418,
-211.864982076871));
#230444=CARTESIAN_POINT('Ctrl Pts',(-11.4850984575113,-60.2258797863292,
-239.042379319393));
#230445=CARTESIAN_POINT('Ctrl Pts',(-24.504034109899,-77.9574724885703,
-211.864982076871));
#230446=CARTESIAN_POINT('Ctrl Pts',(-10.6757840293104,-60.3962257939897,
-239.042379319393));
#230447=CARTESIAN_POINT('Ctrl Pts',(-21.9997405622719,-78.0300903453287,
-211.864982076871));
#230448=CARTESIAN_POINT('Ctrl Pts',(-9.48446360027414,-60.4742901256445,
-239.042379319393));
#230449=CARTESIAN_POINT('Ctrl Pts',(-19.4557251513172,-77.9671468699367,
-211.864982076871));
#230450=CARTESIAN_POINT('Ctrl Pts',(-8.31856484927211,-60.385504961024,
-239.042379319393));
#230451=CARTESIAN_POINT('Ctrl Pts',(-17.7580995848034,-77.8323435614113,
-211.864982076871));
#230452=CARTESIAN_POINT('Ctrl Pts',(-7.55969975399382,-60.2185931298735,
-239.042379319393));
#230453=CARTESIAN_POINT('Ctrl Pts',(-16.0218744898441,-77.6472898528508,
-211.864982076871));
#230454=CARTESIAN_POINT('Ctrl Pts',(-6.78854926351807,-59.9912329899662,
-239.042379319393));
#230455=CARTESIAN_POINT('Ctrl Pts',(-14.2242428743346,-77.5073035049326,
-211.864982076871));
#230456=CARTESIAN_POINT('Ctrl Pts',(-5.98348432758041,-59.8179657745908,
-239.042379319393));
#230457=CARTESIAN_POINT('Ctrl Pts',(-11.5028152109754,-77.4528279485756,
-211.864982076871));
#230458=CARTESIAN_POINT('Ctrl Pts',(-4.76588582139345,-59.7403137615462,
-239.042379319393));
#230459=CARTESIAN_POINT('Ctrl Pts',(-8.76522200381794,-77.5576352824452,
-211.864982076872));
#230460=CARTESIAN_POINT('Ctrl Pts',(-3.56229847767841,-59.8420012365378,
-239.042379319393));
#230461=CARTESIAN_POINT('Ctrl Pts',(-6.93562803804477,-77.7358880723896,
-211.864982076871));
#230462=CARTESIAN_POINT('Ctrl Pts',(-2.78461998053008,-60.0255540781957,
-239.042379319393));
#230463=CARTESIAN_POINT('Ctrl Pts',(-5.53332725337535,-77.9148333735951,
-211.864982076871));
#230464=CARTESIAN_POINT('Ctrl Pts',(-2.20326121884502,-60.2085554263816,
-239.042379319393));
#230465=CARTESIAN_POINT('Ctrl Pts',(-4.54456283515166,-78.025500619718,
-211.864982076871));
#230466=CARTESIAN_POINT('Ctrl Pts',(-1.80191868227511,-60.318198378429,
-239.042379319393));
#230467=CARTESIAN_POINT('Ctrl Pts',(-3.03559134111532,-78.1451797699688,
-211.864982076871));
#230468=CARTESIAN_POINT('Ctrl Pts',(-1.20446149167326,-60.4340132220253,
-239.042379319393));
#230469=CARTESIAN_POINT('Ctrl Pts',(-1.5148280855032,-78.2155854299247,
-211.864982076871));
#230470=CARTESIAN_POINT('Ctrl Pts',(-0.606254863140601,-60.5036064966923,
-239.042379319393));
#230471=CARTESIAN_POINT('Ctrl Pts',(-0.502991918578145,-78.2289825342829,
-211.864982076871));
#230472=CARTESIAN_POINT('Ctrl Pts',(-0.203385156708754,-60.5196440064212,
-239.042379319393));
#230473=CARTESIAN_POINT('Ctrl Pts',(0.502991918602468,-78.2289825342829,
-211.864982076871));
#230474=CARTESIAN_POINT('Ctrl Pts',(0.203385156705297,-60.5196440064212,
-239.042379319393));
#230475=CARTESIAN_POINT('Ctrl Pts',(1.51482689495333,-78.2155855032342,
-211.864982076871));
#230476=CARTESIAN_POINT('Ctrl Pts',(0.606259313960994,-60.5036065477656,
-239.042379319393));
#230477=CARTESIAN_POINT('Ctrl Pts',(3.0355887465281,-78.1451799566583,-211.864982076871));
#230478=CARTESIAN_POINT('Ctrl Pts',(1.204456703078,-60.434013319996,-239.042379319393));
#230479=CARTESIAN_POINT('Ctrl Pts',(4.54456624804472,-78.0255001346635,
-211.864982076871));
#230480=CARTESIAN_POINT('Ctrl Pts',(1.80191683140721,-60.3181991676866,
-239.042379319393));
#230481=CARTESIAN_POINT('Ctrl Pts',(5.5333272533997,-77.9148333735951,-211.864982076871));
#230482=CARTESIAN_POINT('Ctrl Pts',(2.20326121884159,-60.2085554263816,
-239.042379319393));
#230483=CARTESIAN_POINT('Ctrl Pts',(6.93562803806916,-77.7358880723894,
-211.864982076871));
#230484=CARTESIAN_POINT('Ctrl Pts',(2.78461998052664,-60.0255540781959,
-239.042379319393));
#230485=CARTESIAN_POINT('Ctrl Pts',(8.76522200384232,-77.5576352824453,
-211.864982076871));
#230486=CARTESIAN_POINT('Ctrl Pts',(3.56229847767494,-59.8420012365377,
-239.042379319393));
#230487=CARTESIAN_POINT('Ctrl Pts',(11.5028152109998,-77.4528279485751,
-211.864982076871));
#230488=CARTESIAN_POINT('Ctrl Pts',(4.7658858213899,-59.7403137615466,-239.042379319393));
#230489=CARTESIAN_POINT('Ctrl Pts',(14.2242428743589,-77.5073035049326,
-211.864982076871));
#230490=CARTESIAN_POINT('Ctrl Pts',(5.98348432757681,-59.8179657745909,
-239.042379319393));
#230491=CARTESIAN_POINT('Ctrl Pts',(16.0218744898684,-77.6472898528505,
-211.864982076871));
#230492=CARTESIAN_POINT('Ctrl Pts',(6.78854926351442,-59.9912329899664,
-239.042379319393));
#230493=CARTESIAN_POINT('Ctrl Pts',(17.7580995848278,-77.832343561411,-211.864982076871));
#230494=CARTESIAN_POINT('Ctrl Pts',(7.55969975399014,-60.2185931298737,
-239.042379319393));
#230495=CARTESIAN_POINT('Ctrl Pts',(19.4557251513416,-77.9671468699364,
-211.864982076871));
#230496=CARTESIAN_POINT('Ctrl Pts',(8.31856484926843,-60.3855049610241,
-239.042379319393));
#230497=CARTESIAN_POINT('Ctrl Pts',(21.9997405622963,-78.0300903453282,
-211.864982076871));
#230498=CARTESIAN_POINT('Ctrl Pts',(9.48446360027046,-60.4742901256449,
-239.042379319393));
#230499=CARTESIAN_POINT('Ctrl Pts',(24.5040341099234,-77.9574724885699,
-211.864982076871));
#230500=CARTESIAN_POINT('Ctrl Pts',(10.6757840293067,-60.39622579399,-239.042379319393));
#230501=CARTESIAN_POINT('Ctrl Pts',(26.1251285606686,-77.8260872807413,
-211.864982076871));
#230502=CARTESIAN_POINT('Ctrl Pts',(11.4850984575076,-60.2258797863295,
-239.042379319393));
#230503=CARTESIAN_POINT('Ctrl Pts',(27.7276393867659,-77.6574160379364,
-211.864982076871));
#230504=CARTESIAN_POINT('Ctrl Pts',(12.307851425605,-59.9884330330069,-239.042379319393));
#230505=CARTESIAN_POINT('Ctrl Pts',(29.3183793276793,-77.5317048145225,
-211.864982076871));
#230506=CARTESIAN_POINT('Ctrl Pts',(13.1728997877408,-59.8076087424512,
-239.042379319393));
#230507=CARTESIAN_POINT('Ctrl Pts',(31.6477754280729,-77.4599324799418,
-211.864982076871));
#230508=CARTESIAN_POINT('Ctrl Pts',(14.5387717509006,-59.7364199365383,
-239.042379319393));
#230509=CARTESIAN_POINT('Ctrl Pts',(36.4842840550008,-77.5339017897612,
-211.864982076871));
#230510=CARTESIAN_POINT('Ctrl Pts',(17.4751640410175,-60.0398805476776,
-239.042379319393));
#230511=CARTESIAN_POINT('Ctrl Pts',(40.4601948759724,-78.0802943160702,
-211.864982076872));
#230512=CARTESIAN_POINT('Ctrl Pts',(19.8470357167496,-61.3336715388389,
-239.042379319392));
#230513=CARTESIAN_POINT('Ctrl Pts',(43.8493461424807,-78.8521074299069,
-211.864982076868));
#230514=CARTESIAN_POINT('Ctrl Pts',(21.0752244585277,-62.9612490574688,
-239.0423793194));
#230515=CARTESIAN_POINT('Ctrl Pts',(25.5478248690252,37.5021404050027,-238.870094813919));
#230516=CARTESIAN_POINT('Ctrl Pts',(31.0974823253722,43.1081780439896,-229.864162540276));
#230517=CARTESIAN_POINT('Ctrl Pts',(36.6471397817123,48.7142156829799,-220.858230266689));
#230518=CARTESIAN_POINT('Ctrl Pts',(42.1967972380602,54.3202533219665,-211.852297993045));
#230519=CARTESIAN_POINT('Ctrl Pts',(23.7340150363558,36.8170136325857,-238.870094813938));
#230520=CARTESIAN_POINT('Ctrl Pts',(28.8928311974199,42.3227771550256,-229.864162540312));
#230521=CARTESIAN_POINT('Ctrl Pts',(34.0516473584841,47.8285406774658,-220.858230266679));
#230522=CARTESIAN_POINT('Ctrl Pts',(39.2104635195483,53.3343041999057,-211.852297993053));
#230523=CARTESIAN_POINT('Ctrl Pts',(21.2241728789609,36.320693756165,-238.870094813932));
#230524=CARTESIAN_POINT('Ctrl Pts',(25.8876894275506,41.7749009515431,-229.864162540305));
#230525=CARTESIAN_POINT('Ctrl Pts',(30.5512059761403,47.2291081469212,-220.858230266679));
#230526=CARTESIAN_POINT('Ctrl Pts',(35.21472252473,52.6833153422993,-211.852297993052));
#230527=CARTESIAN_POINT('Ctrl Pts',(18.1531449537935,36.3323039390022,-238.870094813935));
#230528=CARTESIAN_POINT('Ctrl Pts',(22.2007701700553,41.8486188105145,-229.864162540308));
#230529=CARTESIAN_POINT('Ctrl Pts',(26.2483953863169,47.3649336820266,-220.85823026668));
#230530=CARTESIAN_POINT('Ctrl Pts',(30.2960206025786,52.8812485535388,-211.852297993052));
#230531=CARTESIAN_POINT('Ctrl Pts',(16.4944071585121,36.4865308984241,-238.870094813934));
#230532=CARTESIAN_POINT('Ctrl Pts',(20.2017948578975,42.0687249742654,-229.864162540306));
#230533=CARTESIAN_POINT('Ctrl Pts',(23.9091825572828,47.6509190501065,-220.858230266679));
#230534=CARTESIAN_POINT('Ctrl Pts',(27.6165702566681,53.2331131259477,-211.852297993052));
#230535=CARTESIAN_POINT('Ctrl Pts',(15.4128369679802,36.6843043274095,-238.870094813934));
#230536=CARTESIAN_POINT('Ctrl Pts',(18.8901600859934,42.3335714329084,-229.864162540306));
#230537=CARTESIAN_POINT('Ctrl Pts',(22.3674832040067,47.9828385384071,-220.858230266679));
#230538=CARTESIAN_POINT('Ctrl Pts',(25.8448063220201,53.632105643906,-211.852297993052));
#230539=CARTESIAN_POINT('Ctrl Pts',(14.3520270002835,36.9260614299673,-238.870094813935));
#230540=CARTESIAN_POINT('Ctrl Pts',(17.5982791985805,42.6550627945494,-229.864162540306));
#230541=CARTESIAN_POINT('Ctrl Pts',(20.8445313968775,48.3840641591314,-220.858230266679));
#230542=CARTESIAN_POINT('Ctrl Pts',(24.0907835951745,54.1130655237135,-211.852297993052));
#230543=CARTESIAN_POINT('Ctrl Pts',(13.2987772727661,37.1178867569915,-238.870094813935));
#230544=CARTESIAN_POINT('Ctrl Pts',(16.2995186126252,42.9177482501692,-229.864162540307));
#230545=CARTESIAN_POINT('Ctrl Pts',(19.3002599524843,48.7176097433469,-220.858230266679));
#230546=CARTESIAN_POINT('Ctrl Pts',(22.3010012923435,54.5174712365246,-211.852297993051));
#230547=CARTESIAN_POINT('Ctrl Pts',(11.7222378941044,37.2692384770327,-238.870094813934));
#230548=CARTESIAN_POINT('Ctrl Pts',(14.3287171552671,43.1379437466391,-229.864162540307));
#230549=CARTESIAN_POINT('Ctrl Pts',(16.9351964164299,49.0066490162454,-220.858230266679));
#230550=CARTESIAN_POINT('Ctrl Pts',(19.5416756775926,54.8753542858517,-211.852297993052));
#230551=CARTESIAN_POINT('Ctrl Pts',(10.1381417281494,37.288217650217,-238.870094813935));
#230552=CARTESIAN_POINT('Ctrl Pts',(12.3460138186247,43.1833567383484,-229.864162540307));
#230553=CARTESIAN_POINT('Ctrl Pts',(14.5538859091001,49.0784958264797,-220.858230266679));
#230554=CARTESIAN_POINT('Ctrl Pts',(16.7617579995755,54.973634914611,-211.852297993051));
#230555=CARTESIAN_POINT('Ctrl Pts',(9.0694859968433,37.2108732070893,-238.870094813934));
#230556=CARTESIAN_POINT('Ctrl Pts',(11.0234698129422,43.0965115564161,-229.864162540306));
#230557=CARTESIAN_POINT('Ctrl Pts',(12.9774536290411,48.9821499057428,-220.858230266679));
#230558=CARTESIAN_POINT('Ctrl Pts',(14.93143744514,54.8677882550696,-211.852297993052));
#230559=CARTESIAN_POINT('Ctrl Pts',(8.09600002160285,37.0974623895316,-238.870094813934));
#230560=CARTESIAN_POINT('Ctrl Pts',(9.83246501086473,42.9648667488742,-229.864162540306));
#230561=CARTESIAN_POINT('Ctrl Pts',(11.5689300001266,48.8322711082166,-220.858230266679));
#230562=CARTESIAN_POINT('Ctrl Pts',(13.3053949893885,54.6996754675592,-211.852297993052));
#230563=CARTESIAN_POINT('Ctrl Pts',(7.21039615408183,37.0252028273246,-238.870094813934));
#230564=CARTESIAN_POINT('Ctrl Pts',(8.76313299670731,42.8850718970782,-229.864162540307));
#230565=CARTESIAN_POINT('Ctrl Pts',(10.3158698393328,48.7449409668318,-220.858230266679));
#230566=CARTESIAN_POINT('Ctrl Pts',(11.8686066819583,54.6048100365855,-211.852297993052));
#230567=CARTESIAN_POINT('Ctrl Pts',(5.85470835560891,37.0124469887412,-238.870094813934));
#230568=CARTESIAN_POINT('Ctrl Pts',(7.14898080710293,42.8806994061336,-229.864162540306));
#230569=CARTESIAN_POINT('Ctrl Pts',(8.44325325859696,48.7489518235258,-220.858230266679));
#230570=CARTESIAN_POINT('Ctrl Pts',(9.73752571009099,54.6172042409181,-211.852297993051));
#230571=CARTESIAN_POINT('Ctrl Pts',(4.4991133918818,37.0982029765426,-238.870094813934));
#230572=CARTESIAN_POINT('Ctrl Pts',(5.53799235246699,42.9924849109515,-229.864162540307));
#230573=CARTESIAN_POINT('Ctrl Pts',(6.57687131305217,48.8867668453602,-220.858230266679));
#230574=CARTESIAN_POINT('Ctrl Pts',(7.61575027363735,54.7810487797691,-211.852297993052));
#230575=CARTESIAN_POINT('Ctrl Pts',(3.61373337750269,37.2187456251595,-238.870094813934));
#230576=CARTESIAN_POINT('Ctrl Pts',(4.47509554657543,43.143583333024,-229.864162540306));
#230577=CARTESIAN_POINT('Ctrl Pts',(5.33645771564818,49.0684210408883,-220.858230266679));
#230578=CARTESIAN_POINT('Ctrl Pts',(6.19781988472092,54.9932587487528,-211.852297993052));
#230579=CARTESIAN_POINT('Ctrl Pts',(2.91021678336389,37.3395607013659,-238.870094813934));
#230580=CARTESIAN_POINT('Ctrl Pts',(3.621152681702,43.2962952860814,-229.864162540307));
#230581=CARTESIAN_POINT('Ctrl Pts',(4.33208858004011,49.2530298707968,-220.858230266679));
#230582=CARTESIAN_POINT('Ctrl Pts',(5.04302447837822,55.2097644555123,-211.852297993052));
#230583=CARTESIAN_POINT('Ctrl Pts',(2.37632997378629,37.4191211557246,-238.870094813935));
#230584=CARTESIAN_POINT('Ctrl Pts',(2.9659120800303,43.3985012706933,-229.864162540306));
#230585=CARTESIAN_POINT('Ctrl Pts',(3.5554941862743,49.3778813856621,-220.858230266679));
#230586=CARTESIAN_POINT('Ctrl Pts',(4.14507629251831,55.3572615006307,-211.852297993052));
#230587=CARTESIAN_POINT('Ctrl Pts',(1.58453082874124,37.5028233147248,-238.870094813934));
#230588=CARTESIAN_POINT('Ctrl Pts',(1.98012592383798,43.5079032854707,-229.864162540307));
#230589=CARTESIAN_POINT('Ctrl Pts',(2.37572101893471,49.5129832562166,-220.858230266679));
#230590=CARTESIAN_POINT('Ctrl Pts',(2.77131611403145,55.5180632269626,-211.852297993052));
#230591=CARTESIAN_POINT('Ctrl Pts',(0.79519346259745,37.5528208103196,-238.870094813934));
#230592=CARTESIAN_POINT('Ctrl Pts',(0.991502132242674,43.5735821125591,
-229.864162540306));
#230593=CARTESIAN_POINT('Ctrl Pts',(1.1878108018879,49.5943434147985,-220.858230266679));
#230594=CARTESIAN_POINT('Ctrl Pts',(1.38411947153312,55.615104717038,-211.852297993052));
#230595=CARTESIAN_POINT('Ctrl Pts',(0.266260901836723,37.5640986908796,
-238.870094813934));
#230596=CARTESIAN_POINT('Ctrl Pts',(0.330758472424439,43.5882172364105,
-229.864162540306));
#230597=CARTESIAN_POINT('Ctrl Pts',(0.395256043012154,49.6123357819414,
-220.858230266679));
#230598=CARTESIAN_POINT('Ctrl Pts',(0.45975361359987,55.6364543274722,-211.852297993052));
#230599=CARTESIAN_POINT('Ctrl Pts',(-0.266261156428491,37.5640986908796,
-238.870094813935));
#230600=CARTESIAN_POINT('Ctrl Pts',(-0.330758075650379,43.5882172364105,
-229.864162540306));
#230601=CARTESIAN_POINT('Ctrl Pts',(-0.395254994872268,49.6123357819414,
-220.858230266679));
#230602=CARTESIAN_POINT('Ctrl Pts',(-0.459751914094156,55.6364543274723,
-211.852297993052));
#230603=CARTESIAN_POINT('Ctrl Pts',(-0.795196360647825,37.5528209283231,
-238.870094813934));
#230604=CARTESIAN_POINT('Ctrl Pts',(-0.991503022362771,43.5735822101004,
-229.864162540306));
#230605=CARTESIAN_POINT('Ctrl Pts',(-1.18780968407772,49.5943434918777,
-220.858230266679));
#230606=CARTESIAN_POINT('Ctrl Pts',(-1.38411634579266,55.6151047736551,
-211.852297993051));
#230607=CARTESIAN_POINT('Ctrl Pts',(-1.58452896877659,37.5028231831529,
-238.870094813935));
#230608=CARTESIAN_POINT('Ctrl Pts',(-1.98012255687567,43.5079033550423,
-229.864162540307));
#230609=CARTESIAN_POINT('Ctrl Pts',(-2.37571614497474,49.5129835269317,
-220.858230266679));
#230610=CARTESIAN_POINT('Ctrl Pts',(-2.77130973307382,55.5180636988211,
-211.852297993052));
#230611=CARTESIAN_POINT('Ctrl Pts',(-2.37632882947295,37.4191215872896,
-238.870094813934));
#230612=CARTESIAN_POINT('Ctrl Pts',(-2.96591227679258,43.3985013387235,
-229.864162540306));
#230613=CARTESIAN_POINT('Ctrl Pts',(-3.5554957241122,49.3778810901573,-220.858230266679));
#230614=CARTESIAN_POINT('Ctrl Pts',(-4.14507917143183,55.3572608415911,
-211.852297993052));
#230615=CARTESIAN_POINT('Ctrl Pts',(-2.91021703795575,37.3395607013659,
-238.870094813934));
#230616=CARTESIAN_POINT('Ctrl Pts',(-3.62115228492807,43.2962952860814,
-229.864162540307));
#230617=CARTESIAN_POINT('Ctrl Pts',(-4.33208753190037,49.2530298707968,
-220.858230266679));
#230618=CARTESIAN_POINT('Ctrl Pts',(-5.0430227788727,55.2097644555124,-211.852297993052));
#230619=CARTESIAN_POINT('Ctrl Pts',(-3.61373363209456,37.2187456251595,
-238.870094813934));
#230620=CARTESIAN_POINT('Ctrl Pts',(-4.47509514980151,43.143583333024,-229.864162540306));
#230621=CARTESIAN_POINT('Ctrl Pts',(-5.33645666750845,49.0684210408883,
-220.858230266679));
#230622=CARTESIAN_POINT('Ctrl Pts',(-6.1978181852154,54.9932587487528,-211.852297993052));
#230623=CARTESIAN_POINT('Ctrl Pts',(-4.49911364647367,37.0982029765426,
-238.870094813935));
#230624=CARTESIAN_POINT('Ctrl Pts',(-5.53799195569307,42.9924849109514,
-229.864162540306));
#230625=CARTESIAN_POINT('Ctrl Pts',(-6.57687026491244,48.8867668453602,
-220.858230266679));
#230626=CARTESIAN_POINT('Ctrl Pts',(-7.61574857413184,54.781048779769,-211.852297993052));
#230627=CARTESIAN_POINT('Ctrl Pts',(-5.85470861020079,37.0124469887413,
-238.870094813934));
#230628=CARTESIAN_POINT('Ctrl Pts',(-7.14898041032902,42.8806994061337,
-229.864162540306));
#230629=CARTESIAN_POINT('Ctrl Pts',(-8.44325221045725,48.7489518235258,
-220.858230266679));
#230630=CARTESIAN_POINT('Ctrl Pts',(-9.73752401058548,54.6172042409182,
-211.852297993052));
#230631=CARTESIAN_POINT('Ctrl Pts',(-7.21039640867369,37.0252028273246,
-238.870094813935));
#230632=CARTESIAN_POINT('Ctrl Pts',(-8.7631325999334,42.8850718970782,-229.864162540307));
#230633=CARTESIAN_POINT('Ctrl Pts',(-10.3158687911931,48.7449409668318,
-220.858230266679));
#230634=CARTESIAN_POINT('Ctrl Pts',(-11.8686049824528,54.6048100365855,
-211.852297993051));
#230635=CARTESIAN_POINT('Ctrl Pts',(-8.09600027619472,37.0974623895316,
-238.870094813934));
#230636=CARTESIAN_POINT('Ctrl Pts',(-9.83246461409083,42.9648667488742,
-229.864162540306));
#230637=CARTESIAN_POINT('Ctrl Pts',(-11.5689289519869,48.8322711082166,
-220.858230266679));
#230638=CARTESIAN_POINT('Ctrl Pts',(-13.305393289883,54.6996754675591,-211.852297993052));
#230639=CARTESIAN_POINT('Ctrl Pts',(-9.06948625143518,37.2108732070893,
-238.870094813935));
#230640=CARTESIAN_POINT('Ctrl Pts',(-11.0234694161683,43.0965115564161,
-229.864162540306));
#230641=CARTESIAN_POINT('Ctrl Pts',(-12.9774525809014,48.9821499057428,
-220.858230266679));
#230642=CARTESIAN_POINT('Ctrl Pts',(-14.9314357456345,54.8677882550697,
-211.852297993052));
#230643=CARTESIAN_POINT('Ctrl Pts',(-10.1381419827413,37.288217650217,-238.870094813934));
#230644=CARTESIAN_POINT('Ctrl Pts',(-12.3460134218509,43.1833567383484,
-229.864162540306));
#230645=CARTESIAN_POINT('Ctrl Pts',(-14.5538848609604,49.0784958264796,
-220.858230266679));
#230646=CARTESIAN_POINT('Ctrl Pts',(-16.76175630007,54.9736349146109,-211.852297993052));
#230647=CARTESIAN_POINT('Ctrl Pts',(-11.7222381486963,37.2692384770326,
-238.870094813935));
#230648=CARTESIAN_POINT('Ctrl Pts',(-14.3287167584933,43.1379437466391,
-229.864162540307));
#230649=CARTESIAN_POINT('Ctrl Pts',(-16.9351953682902,49.0066490162454,
-220.858230266679));
#230650=CARTESIAN_POINT('Ctrl Pts',(-19.5416739780872,54.8753542858518,
-211.852297993052));
#230651=CARTESIAN_POINT('Ctrl Pts',(-13.2987775273579,37.1178867569916,
-238.870094813934));
#230652=CARTESIAN_POINT('Ctrl Pts',(-16.2995182158513,42.9177482501693,
-229.864162540306));
#230653=CARTESIAN_POINT('Ctrl Pts',(-19.3002589043446,48.7176097433469,
-220.858230266679));
#230654=CARTESIAN_POINT('Ctrl Pts',(-22.300999592838,54.5174712365245,-211.852297993052));
#230655=CARTESIAN_POINT('Ctrl Pts',(-14.3520272548754,36.9260614299673,
-238.870094813934));
#230656=CARTESIAN_POINT('Ctrl Pts',(-17.5982788018066,42.6550627945494,
-229.864162540306));
#230657=CARTESIAN_POINT('Ctrl Pts',(-20.8445303487378,48.3840641591314,
-220.858230266679));
#230658=CARTESIAN_POINT('Ctrl Pts',(-24.0907818956689,54.1130655237136,
-211.852297993052));
#230659=CARTESIAN_POINT('Ctrl Pts',(-15.4128372225721,36.6843043274095,
-238.870094813934));
#230660=CARTESIAN_POINT('Ctrl Pts',(-18.8901596892196,42.3335714329084,
-229.864162540306));
#230661=CARTESIAN_POINT('Ctrl Pts',(-22.367482155867,47.9828385384072,-220.858230266679));
#230662=CARTESIAN_POINT('Ctrl Pts',(-25.8448046225145,53.632105643906,-211.852297993052));
#230663=CARTESIAN_POINT('Ctrl Pts',(-16.494407413104,36.4865308984241,-238.870094813934));
#230664=CARTESIAN_POINT('Ctrl Pts',(-20.2017944611236,42.0687249742654,
-229.864162540306));
#230665=CARTESIAN_POINT('Ctrl Pts',(-23.9091815091431,47.6509190501066,
-220.858230266679));
#230666=CARTESIAN_POINT('Ctrl Pts',(-27.6165685571627,53.2331131259478,
-211.852297993052));
#230667=CARTESIAN_POINT('Ctrl Pts',(-18.1531452083854,36.3323039390022,
-238.870094813935));
#230668=CARTESIAN_POINT('Ctrl Pts',(-22.2007697732813,41.8486188105144,
-229.864162540307));
#230669=CARTESIAN_POINT('Ctrl Pts',(-26.2483943381771,47.3649336820265,
-220.858230266679));
#230670=CARTESIAN_POINT('Ctrl Pts',(-30.2960189030729,52.8812485535387,
-211.852297993051));
#230671=CARTESIAN_POINT('Ctrl Pts',(-21.2241730962565,36.3206937563061,
-238.870094813934));
#230672=CARTESIAN_POINT('Ctrl Pts',(-25.8876889860007,41.7749009524383,
-229.864162540306));
#230673=CARTESIAN_POINT('Ctrl Pts',(-30.5512048757446,47.2291081485709,
-220.85823026668));
#230674=CARTESIAN_POINT('Ctrl Pts',(-35.2147207654887,52.6833153447033,
-211.852297993052));
#230675=CARTESIAN_POINT('Ctrl Pts',(-23.7340152164193,36.8170136178475,
-238.870094813936));
#230676=CARTESIAN_POINT('Ctrl Pts',(-28.8928307114097,42.3227771387571,
-229.864162540307));
#230677=CARTESIAN_POINT('Ctrl Pts',(-34.0516462064001,47.8285406596655,
-220.858230266679));
#230678=CARTESIAN_POINT('Ctrl Pts',(-39.2104617013909,53.3343041805747,
-211.85229799305));
#230679=CARTESIAN_POINT('Ctrl Pts',(-25.547825019704,37.5021403657523,-238.870094813925));
#230680=CARTESIAN_POINT('Ctrl Pts',(-31.0974818022918,43.1081779989934,
-229.864162540309));
#230681=CARTESIAN_POINT('Ctrl Pts',(-36.6471385848807,48.7142156322395,
-220.858230266681));
#230682=CARTESIAN_POINT('Ctrl Pts',(-42.1967953674649,54.320253265481,-211.852297993061));
#230683=CARTESIAN_POINT('Ctrl Pts',(48.9714493645238,-32.4976365372143,
-239.032601429863));
#230684=CARTESIAN_POINT('Ctrl Pts',(68.1913744168868,-58.588595799019,-211.730755606268));
#230685=CARTESIAN_POINT('Ctrl Pts',(47.6504140161628,-30.9809716432943,
-239.032601429841));
#230686=CARTESIAN_POINT('Ctrl Pts',(66.0438929094031,-54.9590042342752,
-211.730755606272));
#230687=CARTESIAN_POINT('Ctrl Pts',(46.5919797891444,-28.6187972486599,
-239.032601429843));
#230688=CARTESIAN_POINT('Ctrl Pts',(64.3781819143446,-49.9473558418611,
-211.730755606271));
#230689=CARTESIAN_POINT('Ctrl Pts',(46.3023719972087,-25.6595919193811,
-239.032601429843));
#230690=CARTESIAN_POINT('Ctrl Pts',(63.9692632136205,-43.762285990858,-211.730755606272));
#230691=CARTESIAN_POINT('Ctrl Pts',(46.3453291243135,-24.2216224913335,
-239.032601429843));
#230692=CARTESIAN_POINT('Ctrl Pts',(64.0706036090694,-40.7439486410264,
-211.730755606272));
#230693=CARTESIAN_POINT('Ctrl Pts',(46.4942182564745,-23.2800468285249,
-239.032601429843));
#230694=CARTESIAN_POINT('Ctrl Pts',(64.3397924421248,-38.7400276918009,
-211.730755606272));
#230695=CARTESIAN_POINT('Ctrl Pts',(46.6823308842909,-22.4376754428628,
-239.032601429843));
#230696=CARTESIAN_POINT('Ctrl Pts',(64.6771567767455,-36.9265599675944,
-211.730755606272));
#230697=CARTESIAN_POINT('Ctrl Pts',(46.8110566085946,-21.6771313665435,
-239.032601429843));
#230698=CARTESIAN_POINT('Ctrl Pts',(64.9159602271999,-35.2663729129392,
-211.730755606272));
#230699=CARTESIAN_POINT('Ctrl Pts',(46.8864232013851,-20.5344885406242,
-239.032601429843));
#230700=CARTESIAN_POINT('Ctrl Pts',(65.0656320382587,-32.7370789599851,
-211.730755606271));
#230701=CARTESIAN_POINT('Ctrl Pts',(46.845613352649,-19.389471894004,-239.032601429842));
#230702=CARTESIAN_POINT('Ctrl Pts',(65.0024851991802,-30.205094760215,-211.730755606272));
#230703=CARTESIAN_POINT('Ctrl Pts',(46.739717205202,-18.6241517464968,-239.032601429843));
#230704=CARTESIAN_POINT('Ctrl Pts',(64.8208630220631,-28.539554521699,-211.730755606272));
#230705=CARTESIAN_POINT('Ctrl Pts',(46.5950583390951,-17.8704826264274,
-239.032601429843));
#230706=CARTESIAN_POINT('Ctrl Pts',(64.5773028603203,-26.9236650389039,
-211.730755606272));
#230707=CARTESIAN_POINT('Ctrl Pts',(46.4891834572756,-17.1171663742141,
-239.032601429843));
#230708=CARTESIAN_POINT('Ctrl Pts',(64.4023778490554,-25.3332388913667,
-211.730755606272));
#230709=CARTESIAN_POINT('Ctrl Pts',(46.4453565014347,-15.9661997524868,
-239.032601429843));
#230710=CARTESIAN_POINT('Ctrl Pts',(64.3295185111446,-22.9500603856902,
-211.730755606271));
#230711=CARTESIAN_POINT('Ctrl Pts',(46.5193900629931,-14.8111705824743,
-239.032601429843));
#230712=CARTESIAN_POINT('Ctrl Pts',(64.443529180052,-20.5764219053293,-211.730755606272));
#230713=CARTESIAN_POINT('Ctrl Pts',(46.6471770799421,-14.0499533302827,
-239.032601429843));
#230714=CARTESIAN_POINT('Ctrl Pts',(64.6432253119956,-19.0049914961272,
-211.730755606272));
#230715=CARTESIAN_POINT('Ctrl Pts',(46.7740202606564,-13.4754604930206,
-239.032601429843));
#230716=CARTESIAN_POINT('Ctrl Pts',(64.8432542225078,-17.8091893041105,
-211.730755606272));
#230717=CARTESIAN_POINT('Ctrl Pts',(46.8513541209764,-13.0740155121622,
-239.032601429843));
#230718=CARTESIAN_POINT('Ctrl Pts',(64.9641969010104,-16.980210969671,-211.730755606271));
#230719=CARTESIAN_POINT('Ctrl Pts',(46.9348053643729,-12.4640324698742,
-239.032601429843));
#230720=CARTESIAN_POINT('Ctrl Pts',(65.0935448562552,-15.7339405894364,
-211.730755606272));
#230721=CARTESIAN_POINT('Ctrl Pts',(46.9850328086675,-11.8494593400854,
-239.032601429843));
#230722=CARTESIAN_POINT('Ctrl Pts',(65.171164912913,-14.4848476258101,-211.730755606272));
#230723=CARTESIAN_POINT('Ctrl Pts',(46.9961709729731,-11.4388750292095,
-239.032601429843));
#230724=CARTESIAN_POINT('Ctrl Pts',(65.1884659210897,-13.6502250547399,
-211.730755606272));
#230725=CARTESIAN_POINT('Ctrl Pts',(46.9961709729731,-11.0289590886771,
-239.032601429843));
#230726=CARTESIAN_POINT('Ctrl Pts',(65.1884659210897,-12.8146289801201,
-211.730755606272));
#230727=CARTESIAN_POINT('Ctrl Pts',(46.9850328086376,-10.6183760206315,
-239.032601429842));
#230728=CARTESIAN_POINT('Ctrl Pts',(65.1711648319807,-11.980003483899,-211.730755606272));
#230729=CARTESIAN_POINT('Ctrl Pts',(46.9348056898163,-10.0038043022318,
-239.032601429843));
#230730=CARTESIAN_POINT('Ctrl Pts',(65.093544987819,-10.7309166067835,-211.730755606272));
#230731=CARTESIAN_POINT('Ctrl Pts',(46.8513537675148,-9.39381595500219,
-239.032601429843));
#230732=CARTESIAN_POINT('Ctrl Pts',(64.9641971936048,-9.48464435696854,
-211.730755606272));
#230733=CARTESIAN_POINT('Ctrl Pts',(46.7740202606564,-8.99237362486574,
-239.032601429843));
#230734=CARTESIAN_POINT('Ctrl Pts',(64.8432542225078,-8.65566473074882,
-211.730755606272));
#230735=CARTESIAN_POINT('Ctrl Pts',(46.6471770799421,-8.41788078760364,
-239.032601429843));
#230736=CARTESIAN_POINT('Ctrl Pts',(64.6432253119957,-7.45986253873205,
-211.730755606272));
#230737=CARTESIAN_POINT('Ctrl Pts',(46.5193900629931,-7.65666353541205,
-239.032601429843));
#230738=CARTESIAN_POINT('Ctrl Pts',(64.4435291800518,-5.88843212952995,
-211.730755606271));
#230739=CARTESIAN_POINT('Ctrl Pts',(46.4453565014347,-6.50163436539958,
-239.032601429843));
#230740=CARTESIAN_POINT('Ctrl Pts',(64.3295185111447,-3.51479364916907,
-211.730755606272));
#230741=CARTESIAN_POINT('Ctrl Pts',(46.4891834572756,-5.35066774367227,
-239.032601429843));
#230742=CARTESIAN_POINT('Ctrl Pts',(64.4023778490553,-1.13161514349255,
-211.730755606272));
#230743=CARTESIAN_POINT('Ctrl Pts',(46.5950583390951,-4.59735149145896,
-239.032601429843));
#230744=CARTESIAN_POINT('Ctrl Pts',(64.5773028603203,0.458811004044723,
-211.730755606272));
#230745=CARTESIAN_POINT('Ctrl Pts',(46.739717205202,-3.84368237138963,-239.032601429843));
#230746=CARTESIAN_POINT('Ctrl Pts',(64.8208630220631,2.07470048683978,-211.730755606272));
#230747=CARTESIAN_POINT('Ctrl Pts',(46.8456133526491,-3.07836222388228,
-239.032601429843));
#230748=CARTESIAN_POINT('Ctrl Pts',(65.0024851991801,3.74024072535572,-211.730755606271));
#230749=CARTESIAN_POINT('Ctrl Pts',(46.8864232013849,-1.93334557726219,
-239.032601429842));
#230750=CARTESIAN_POINT('Ctrl Pts',(65.0656320382587,6.27222492512578,-211.730755606272));
#230751=CARTESIAN_POINT('Ctrl Pts',(46.8110566085948,-0.790702751342818,
-239.032601429843));
#230752=CARTESIAN_POINT('Ctrl Pts',(64.9159602271998,8.80151887808002,-211.730755606272));
#230753=CARTESIAN_POINT('Ctrl Pts',(46.6823308842909,-0.0301586750235619,
-239.032601429843));
#230754=CARTESIAN_POINT('Ctrl Pts',(64.6771567767455,10.4617059327352,-211.730755606272));
#230755=CARTESIAN_POINT('Ctrl Pts',(46.4942182564745,0.812212710638539,
-239.032601429843));
#230756=CARTESIAN_POINT('Ctrl Pts',(64.3397924421248,12.2751736569417,-211.730755606272));
#230757=CARTESIAN_POINT('Ctrl Pts',(46.3453291243136,1.75378837344716,-239.032601429843));
#230758=CARTESIAN_POINT('Ctrl Pts',(64.0706036090695,14.2790946061672,-211.730755606272));
#230759=CARTESIAN_POINT('Ctrl Pts',(46.3023719972086,3.1917578014948,-239.032601429843));
#230760=CARTESIAN_POINT('Ctrl Pts',(63.9692632136205,17.2974319559987,-211.730755606272));
#230761=CARTESIAN_POINT('Ctrl Pts',(46.5821989973795,6.05102323992199,-239.032601429842));
#230762=CARTESIAN_POINT('Ctrl Pts',(64.3643716897167,23.2736162661097,-211.730755606271));
#230763=CARTESIAN_POINT('Ctrl Pts',(47.566430740579,8.32255892669279,-239.032601429843));
#230764=CARTESIAN_POINT('Ctrl Pts',(65.9117879843948,28.0899407880831,-211.730755606275));
#230765=CARTESIAN_POINT('Ctrl Pts',(48.7769866795674,9.7996450480234,-239.032601429843));
#230766=CARTESIAN_POINT('Ctrl Pts',(67.8755806199084,31.5767606755659,-211.730755606259));
#230767=CARTESIAN_POINT('Origin',(-296.501483394397,-25.4138432731711,-235.35005));
#230768=CARTESIAN_POINT('Origin',(-6.29739814579425E-15,-11.5034818258363,
-234.75005));
#230769=CARTESIAN_POINT('',(42.9727564520429,17.4202489659096,-234.75005));
#230770=CARTESIAN_POINT('',(42.9727564520429,17.4202489659097,-234.75005));
#230771=CARTESIAN_POINT('',(27.3749781671338,32.4720860539414,-234.75005));
#230772=CARTESIAN_POINT('',(27.3749781671338,32.4720860539414,-234.75005));
#230773=CARTESIAN_POINT('Origin',(-6.29739814579425E-15,-11.5034818258363,
-234.75005));
#230774=CARTESIAN_POINT('Origin',(38.9907249661392,14.740057695632,-234.75005));
#230775=CARTESIAN_POINT('',(43.7871111365364,14.9262825715819,-234.75005));
#230776=CARTESIAN_POINT('',(43.7871111365364,14.9262825715819,-234.75005));
#230777=CARTESIAN_POINT('Origin',(38.9907249661392,14.740057695632,-234.75005));
#230778=CARTESIAN_POINT('Origin',(-636.934816028482,-11.5034818258361,-234.75005));
#230779=CARTESIAN_POINT('',(43.7871111365364,-37.9332462232544,-234.75005));
#230780=CARTESIAN_POINT('',(43.7871111365364,-37.9332462232544,-234.75005));
#230781=CARTESIAN_POINT('Origin',(-636.934816028482,-11.5034818258361,-234.75005));
#230782=CARTESIAN_POINT('Origin',(38.9907249661392,-37.7470213473046,-234.75005));
#230783=CARTESIAN_POINT('',(42.9727564520428,-40.4272126175822,-234.75005));
#230784=CARTESIAN_POINT('',(42.9727564520428,-40.4272126175822,-234.75005));
#230785=CARTESIAN_POINT('Origin',(38.9907249661392,-37.7470213473046,-234.75005));
#230786=CARTESIAN_POINT('Origin',(-6.29739814579425E-15,-11.5034818258363,
-234.75005));
#230787=CARTESIAN_POINT('',(25.258351173106,-56.7279850958119,-234.75005));
#230788=CARTESIAN_POINT('',(25.258351173106,-56.7279850958119,-234.75005));
#230789=CARTESIAN_POINT('Origin',(-6.29739814579425E-15,-11.5034818258363,
-234.75005));
#230790=CARTESIAN_POINT('Origin',(22.9178089794592,-52.5372975341153,-234.75005));
#230791=CARTESIAN_POINT('',(23.0804343803032,-57.3345418450714,-234.75005));
#230792=CARTESIAN_POINT('',(23.0804343803032,-57.3345418450714,-234.75005));
#230793=CARTESIAN_POINT('Origin',(22.9178089794592,-52.5372975341153,-234.75005));
#230794=CARTESIAN_POINT('Origin',(7.14692237356698E-14,623.509175991979,
-234.75005));
#230795=CARTESIAN_POINT('Origin',(7.14692237356698E-14,623.509175991979,
-234.75005));
#230796=CARTESIAN_POINT('Origin',(-2.61456814389029E-14,-173.57701443073,
-234.75005));
#230797=CARTESIAN_POINT('',(25.4241796108136,33.1612401412018,-234.75005));
#230798=CARTESIAN_POINT('Origin',(-2.61456814389029E-14,-173.57701443073,
-234.75005));
#230799=CARTESIAN_POINT('',(25.4241796108136,33.1612401412018,-234.75005));
#230800=CARTESIAN_POINT('Origin',(24.838300653577,28.3971299569735,-234.75005));
#230801=CARTESIAN_POINT('Origin',(24.838300653577,28.3971299569735,-234.75005));
#230802=CARTESIAN_POINT('Origin',(11.4589044897296,-32.0203896799758,-234.75005));
#230803=CARTESIAN_POINT('',(23.121090730514,-58.5338529228103,-234.75005));
#230804=CARTESIAN_POINT('Origin',(7.14692237356698E-14,623.509175991979,
-234.75005));
#230805=CARTESIAN_POINT('',(25.5706493501227,34.3522676872588,-234.75005));
#230806=CARTESIAN_POINT('Origin',(-2.61456814389029E-14,-173.57701443073,
-234.75005));
#230807=CARTESIAN_POINT('',(28.0091475455229,33.4908250781833,-234.75005));
#230808=CARTESIAN_POINT('Origin',(24.838300653577,28.3971299569735,-234.75005));
#230809=CARTESIAN_POINT('',(43.9682643235187,18.0902967834791,-234.75005));
#230810=CARTESIAN_POINT('Origin',(-6.29739814579425E-15,-11.5034818258363,
-234.75005));
#230811=CARTESIAN_POINT('',(44.9862076791357,14.9728387905693,-234.75005));
#230812=CARTESIAN_POINT('Origin',(38.9907249661392,14.740057695632,-234.75005));
#230813=CARTESIAN_POINT('',(44.9862076791357,-37.9798024422418,-234.75005));
#230814=CARTESIAN_POINT('Origin',(-636.934816028482,-11.5034818258361,-234.75005));
#230815=CARTESIAN_POINT('',(43.9682643235187,-41.0972604351516,-234.75005));
#230816=CARTESIAN_POINT('Origin',(38.9907249661392,-37.7470213473046,-234.75005));
#230817=CARTESIAN_POINT('',(25.8434867215177,-57.775656986236,-234.75005));
#230818=CARTESIAN_POINT('Origin',(-6.29739814579425E-15,-11.5034818258363,
-234.75005));
#230819=CARTESIAN_POINT('Origin',(22.9178089794592,-52.5372975341153,-234.75005));
#230820=CARTESIAN_POINT('Origin',(22.9178089794592,-52.5372975341153,-234.75005));
#230821=CARTESIAN_POINT('',(25.8434867215177,-57.775656986236,-234.75005));
#230822=CARTESIAN_POINT('',(23.121090730514,-58.5338529228103,-234.75005));
#230823=CARTESIAN_POINT('Origin',(7.14692237356698E-14,623.509175991979,
-234.75005));
#230824=CARTESIAN_POINT('Origin',(-2.61456814389029E-14,-173.57701443073,
-234.75005));
#230825=CARTESIAN_POINT('',(25.5706493501227,34.3522676872588,-234.75005));
#230826=CARTESIAN_POINT('Origin',(24.838300653577,28.3971299569735,-234.75005));
#230827=CARTESIAN_POINT('',(28.0091475455229,33.4908250781833,-234.75005));
#230828=CARTESIAN_POINT('Origin',(-6.29739814579425E-15,-11.5034818258363,
-234.75005));
#230829=CARTESIAN_POINT('',(43.9682643235187,18.0902967834791,-234.75005));
#230830=CARTESIAN_POINT('Origin',(38.9907249661392,14.740057695632,-234.75005));
#230831=CARTESIAN_POINT('',(44.9862076791357,14.9728387905693,-234.75005));
#230832=CARTESIAN_POINT('Origin',(-636.934816028482,-11.5034818258361,-234.75005));
#230833=CARTESIAN_POINT('',(44.9862076791357,-37.9798024422418,-234.75005));
#230834=CARTESIAN_POINT('Origin',(38.9907249661392,-37.7470213473046,-234.75005));
#230835=CARTESIAN_POINT('',(43.9682643235187,-41.0972604351516,-234.75005));
#230836=CARTESIAN_POINT('Origin',(-6.29739814579425E-15,-11.5034818258363,
-234.75005));
#230837=CARTESIAN_POINT('Ctrl Pts',(48.1560655127274,-41.999274229607,-235.35005));
#230838=CARTESIAN_POINT('Ctrl Pts',(51.9279919200935,-48.6191351285365,
-228.68335));
#230839=CARTESIAN_POINT('Ctrl Pts',(55.7004001286368,-55.2387363218615,
-222.01665));
#230840=CARTESIAN_POINT('Ctrl Pts',(59.4732891526772,-61.8580772083615,
-215.34995));
#230841=CARTESIAN_POINT('Ctrl Pts',(59.5110180429176,-61.9242706172265,
-215.283283));
#230842=CARTESIAN_POINT('Ctrl Pts',(59.548746933158,-61.9904640260915,-215.216616));
#230843=CARTESIAN_POINT('Ctrl Pts',(59.5864758233984,-62.0566574349565,
-215.149949));
#230844=CARTESIAN_POINT('Ctrl Pts',(48.2756382252007,-41.8104563330539,
-235.35005));
#230845=CARTESIAN_POINT('Ctrl Pts',(52.0407670149459,-48.4530353242655,
-228.68335));
#230846=CARTESIAN_POINT('Ctrl Pts',(55.8063647406712,-55.0953754160451,
-222.01665));
#230847=CARTESIAN_POINT('Ctrl Pts',(59.57243049321,-61.7374760219621,-215.34995));
#230848=CARTESIAN_POINT('Ctrl Pts',(59.6100911507354,-61.8038970280213,
-215.283283));
#230849=CARTESIAN_POINT('Ctrl Pts',(59.6477518082608,-61.8703180340805,
-215.216616));
#230850=CARTESIAN_POINT('Ctrl Pts',(59.6854124657861,-61.9367390401396,
-215.149949));
#230851=CARTESIAN_POINT('Ctrl Pts',(48.3910626922776,-41.5900298422911,
-235.35005));
#230852=CARTESIAN_POINT('Ctrl Pts',(52.1903238662186,-48.2138133273298,
-228.68335));
#230853=CARTESIAN_POINT('Ctrl Pts',(55.9900266043744,-54.8373975226491,
-222.01665));
#230854=CARTESIAN_POINT('Ctrl Pts',(59.790170143516,-61.4607818737039,-215.34995));
#230855=CARTESIAN_POINT('Ctrl Pts',(59.8281715789074,-61.5270157172145,
-215.283283));
#230856=CARTESIAN_POINT('Ctrl Pts',(59.8661730142988,-61.593249560725,-215.216616));
#230857=CARTESIAN_POINT('Ctrl Pts',(59.9041744496902,-61.6594834042356,
-215.149949));
#230858=CARTESIAN_POINT('Ctrl Pts',(48.5387172079886,-41.2798109487642,
-235.35005));
#230859=CARTESIAN_POINT('Ctrl Pts',(52.4230972161915,-47.8204177760876,
-228.68335));
#230860=CARTESIAN_POINT('Ctrl Pts',(56.3078726256209,-54.3608781649969,
-222.01665));
#230861=CARTESIAN_POINT('Ctrl Pts',(60.1930428686919,-60.9011916159786,
-215.34995));
#230862=CARTESIAN_POINT('Ctrl Pts',(60.2318945711226,-60.9665947504884,
-215.283283000001));
#230863=CARTESIAN_POINT('Ctrl Pts',(60.2707462735533,-61.0319978849983,
-215.216616));
#230864=CARTESIAN_POINT('Ctrl Pts',(60.309597975984,-61.0974010195081,-215.149949));
#230865=CARTESIAN_POINT('Ctrl Pts',(48.6371642419829,-41.0193984169334,
-235.35005));
#230866=CARTESIAN_POINT('Ctrl Pts',(52.6688606290506,-47.3486283864447,
-228.68335));
#230867=CARTESIAN_POINT('Ctrl Pts',(56.7009009677878,-53.6777576502171,
-222.01665));
#230868=CARTESIAN_POINT('Ctrl Pts',(60.7332848610003,-60.0067857712577,
-215.34995));
#230869=CARTESIAN_POINT('Ctrl Pts',(60.7736086999325,-60.0700760524681,
-215.283283));
#230870=CARTESIAN_POINT('Ctrl Pts',(60.8139325388646,-60.1333663336785,
-215.216616));
#230871=CARTESIAN_POINT('Ctrl Pts',(60.8542563777967,-60.1966566148889,
-215.149949));
#230872=CARTESIAN_POINT('Ctrl Pts',(48.7259447515556,-40.7557132274099,
-235.35005));
#230873=CARTESIAN_POINT('Ctrl Pts',(52.8863489207853,-46.8366038296761,
-228.68335));
#230874=CARTESIAN_POINT('Ctrl Pts',(57.0470401243311,-52.9174317848832,
-222.016650000001));
#230875=CARTESIAN_POINT('Ctrl Pts',(61.2080181081436,-58.9981967263321,
-215.349950000001));
#230876=CARTESIAN_POINT('Ctrl Pts',(61.2496278879817,-59.0590043757466,
-215.283283000001));
#230877=CARTESIAN_POINT('Ctrl Pts',(61.2912376678198,-59.1198120251611,
-215.216616));
#230878=CARTESIAN_POINT('Ctrl Pts',(61.332847447658,-59.1806196745756,-215.149949000001));
#230879=CARTESIAN_POINT('Ctrl Pts',(48.7945150938174,-40.4960542325497,
-235.35005));
#230880=CARTESIAN_POINT('Ctrl Pts',(53.0535779259056,-46.3256171279293,
-228.68335));
#230881=CARTESIAN_POINT('Ctrl Pts',(57.3128652259323,-52.1551472055685,
-222.01665));
#230882=CARTESIAN_POINT('Ctrl Pts',(61.572376853754,-57.9846441771198,-215.34995));
#230883=CARTESIAN_POINT('Ctrl Pts',(61.6149719700322,-58.0429391468354,
-215.283283));
#230884=CARTESIAN_POINT('Ctrl Pts',(61.6575670863105,-58.1012341165509,
-215.216616));
#230885=CARTESIAN_POINT('Ctrl Pts',(61.7001622025887,-58.1595290862664,
-215.149949));
#230886=CARTESIAN_POINT('Ctrl Pts',(48.8537891615446,-40.2227290210882,
-235.35005));
#230887=CARTESIAN_POINT('Ctrl Pts',(53.184407479365,-45.7839380160283,-228.68335));
#230888=CARTESIAN_POINT('Ctrl Pts',(57.5151818684938,-51.3451352378197,
-222.01665));
#230889=CARTESIAN_POINT('Ctrl Pts',(61.8461122714633,-56.9063204848096,
-215.349950000001));
#230890=CARTESIAN_POINT('Ctrl Pts',(61.889421575493,-56.9619323372794,-215.283283000001));
#230891=CARTESIAN_POINT('Ctrl Pts',(61.9327308795227,-57.0175441897493,
-215.216616));
#230892=CARTESIAN_POINT('Ctrl Pts',(61.9760401835524,-57.0731560422192,
-215.149949000001));
#230893=CARTESIAN_POINT('Ctrl Pts',(48.8993219763807,-39.9191637201113,
-235.35005));
#230894=CARTESIAN_POINT('Ctrl Pts',(53.2653672535676,-45.2450247261708,
-228.68335));
#230895=CARTESIAN_POINT('Ctrl Pts',(57.631494193953,-50.5708856635808,-222.01665));
#230896=CARTESIAN_POINT('Ctrl Pts',(61.9977027895214,-55.8967464260103,
-215.34995));
#230897=CARTESIAN_POINT('Ctrl Pts',(62.0413648754771,-55.9500050336346,
-215.283283));
#230898=CARTESIAN_POINT('Ctrl Pts',(62.0850269614327,-56.0032636412589,
-215.216616));
#230899=CARTESIAN_POINT('Ctrl Pts',(62.1286890473884,-56.0565222488832,
-215.149949));
#230900=CARTESIAN_POINT('Ctrl Pts',(48.9214109907111,-39.6817730556917,
-235.35005));
#230901=CARTESIAN_POINT('Ctrl Pts',(53.2924626390134,-44.9053881830262,
-228.68335));
#230902=CARTESIAN_POINT('Ctrl Pts',(57.6635282520289,-50.1290038777392,
-222.01665));
#230903=CARTESIAN_POINT('Ctrl Pts',(62.0346078304961,-55.3526201213579,
-215.34995));
#230904=CARTESIAN_POINT('Ctrl Pts',(62.0783186262807,-55.4048562837941,
-215.283283));
#230905=CARTESIAN_POINT('Ctrl Pts',(62.1220294220654,-55.4570924462303,
-215.216616));
#230906=CARTESIAN_POINT('Ctrl Pts',(62.1657402178501,-55.5093286086665,
-215.149949));
#230907=CARTESIAN_POINT('Ctrl Pts',(48.9276804568491,-39.5283381317121,
-235.35005));
#230908=CARTESIAN_POINT('Ctrl Pts',(53.2999213760692,-44.7204933330714,
-228.68335));
#230909=CARTESIAN_POINT('Ctrl Pts',(57.6721622952894,-49.9126485344307,
-222.01665));
#230910=CARTESIAN_POINT('Ctrl Pts',(62.0444032145095,-55.1048037357899,
-215.34995));
#230911=CARTESIAN_POINT('Ctrl Pts',(62.0881256237017,-55.1567252878035,
-215.283283));
#230912=CARTESIAN_POINT('Ctrl Pts',(62.1318480328939,-55.2086468398171,
-215.216616));
#230913=CARTESIAN_POINT('Ctrl Pts',(62.1755704420861,-55.2605683918307,
-215.149949));
#230914=CARTESIAN_POINT('Ctrl Pts',(48.4015825627194,-42.4301635567086,
-234.916111528175));
#230915=CARTESIAN_POINT('Ctrl Pts',(51.8161020106309,-48.4227195017014,
-228.881144730288));
#230916=CARTESIAN_POINT('Ctrl Pts',(55.2310162579792,-54.4150626175587,
-222.846177932402));
#230917=CARTESIAN_POINT('Ctrl Pts',(58.6463245735781,-60.4071924582901,
-216.811211134516));
#230918=CARTESIAN_POINT('',(55.4860418356793,-47.316570933751,-225.35));
#230919=CARTESIAN_POINT('Ctrl Pts',(24.4127870505286,-62.4913878448826,
-235.35005));
#230920=CARTESIAN_POINT('Ctrl Pts',(30.252655437952,-66.705065059021,-228.68335));
#230921=CARTESIAN_POINT('Ctrl Pts',(36.0925246020991,-70.9187639624533,
-222.01665));
#230922=CARTESIAN_POINT('Ctrl Pts',(41.9323946221365,-75.1324845521997,
-215.34995));
#230923=CARTESIAN_POINT('Ctrl Pts',(41.990793322337,-75.1746217580972,-215.283283));
#230924=CARTESIAN_POINT('Ctrl Pts',(42.0491920225373,-75.2167589639946,
-215.216616));
#230925=CARTESIAN_POINT('Ctrl Pts',(42.1075907227377,-75.2588961698921,
-215.149949));
#230926=CARTESIAN_POINT('Ctrl Pts',(24.4238355020022,-62.4909941277675,
-235.35005));
#230927=CARTESIAN_POINT('Ctrl Pts',(30.2665958673131,-66.7045508406744,
-228.68335));
#230928=CARTESIAN_POINT('Ctrl Pts',(36.1093567495128,-70.9181220131437,
-222.01665));
#230929=CARTESIAN_POINT('Ctrl Pts',(41.9521182016317,-75.1317076431822,
-215.34995));
#230930=CARTESIAN_POINT('Ctrl Pts',(42.0105458161529,-75.1738434994826,
-215.283283));
#230931=CARTESIAN_POINT('Ctrl Pts',(42.0689734306741,-75.215979355783,-215.216616));
#230932=CARTESIAN_POINT('Ctrl Pts',(42.1274010451954,-75.2581152120834,
-215.149949));
#230933=CARTESIAN_POINT('Ctrl Pts',(24.4348839534758,-62.4906004106524,
-235.35005));
#230934=CARTESIAN_POINT('Ctrl Pts',(30.2805362966741,-66.7040366223279,
-228.68335));
#230935=CARTESIAN_POINT('Ctrl Pts',(36.1261888969267,-70.9174800638341,
-222.01665));
#230936=CARTESIAN_POINT('Ctrl Pts',(41.971841781127,-75.1309307341648,-215.34995));
#230937=CARTESIAN_POINT('Ctrl Pts',(42.030298309969,-75.1730652408681,-215.283283));
#230938=CARTESIAN_POINT('Ctrl Pts',(42.088754838811,-75.2151997475714,-215.216616));
#230939=CARTESIAN_POINT('Ctrl Pts',(42.147211367653,-75.2573342542747,-215.149949));
#230940=CARTESIAN_POINT('Ctrl Pts',(24.4459324049493,-62.4902066935372,
-235.35005));
#230941=CARTESIAN_POINT('Ctrl Pts',(30.2944767260352,-66.7035224039813,
-228.68335));
#230942=CARTESIAN_POINT('Ctrl Pts',(36.1430210443405,-70.9168381145244,
-222.01665));
#230943=CARTESIAN_POINT('Ctrl Pts',(41.9915653606222,-75.1301538251473,
-215.34995));
#230944=CARTESIAN_POINT('Ctrl Pts',(42.050050803785,-75.1722869822535,-215.283283));
#230945=CARTESIAN_POINT('Ctrl Pts',(42.1085362469478,-75.2144201393598,
-215.216616));
#230946=CARTESIAN_POINT('Ctrl Pts',(42.1670216901106,-75.256553296466,-215.149949));
#230947=CARTESIAN_POINT('Ctrl Pts',(24.5840380483692,-62.4852852295981,
-235.35005));
#230948=CARTESIAN_POINT('Ctrl Pts',(30.4687320930486,-66.6970946746494,
-228.68335));
#230949=CARTESIAN_POINT('Ctrl Pts',(36.3534228870133,-70.9088137481542,
-222.01665));
#230950=CARTESIAN_POINT('Ctrl Pts',(42.2381101043121,-75.120442462429,-215.34995));
#230951=CARTESIAN_POINT('Ctrl Pts',(42.2969569764852,-75.1625587495718,
-215.283283));
#230952=CARTESIAN_POINT('Ctrl Pts',(42.3558038486582,-75.2046750367146,
-215.216616));
#230953=CARTESIAN_POINT('Ctrl Pts',(42.4146507208312,-75.2467913238573,
-215.149949));
#230954=CARTESIAN_POINT('Ctrl Pts',(24.7878826649652,-62.4682791689329,
-235.35005));
#230955=CARTESIAN_POINT('Ctrl Pts',(30.7858798041607,-66.6737307701245,
-228.68335));
#230956=CARTESIAN_POINT('Ctrl Pts',(36.7838683264116,-70.8789174633912,
-222.01665));
#230957=CARTESIAN_POINT('Ctrl Pts',(42.781847274702,-75.0838392837,-215.34995));
#230958=CARTESIAN_POINT('Ctrl Pts',(42.8418270641849,-75.1258885019031,
-215.283283));
#230959=CARTESIAN_POINT('Ctrl Pts',(42.9018068536678,-75.1679377201062,
-215.216616));
#230960=CARTESIAN_POINT('Ctrl Pts',(42.9617866431507,-75.2099869383093,
-215.149949));
#230961=CARTESIAN_POINT('Ctrl Pts',(25.048207175495,-62.4347017437458,-235.35005));
#230962=CARTESIAN_POINT('Ctrl Pts',(31.2985071141138,-66.6007006042259,
-228.68335));
#230963=CARTESIAN_POINT('Ctrl Pts',(37.5487936188611,-70.7661908933779,
-222.01665));
#230964=CARTESIAN_POINT('Ctrl Pts',(43.7990648514606,-74.9311726743249,
-215.34995));
#230965=CARTESIAN_POINT('Ctrl Pts',(43.8615675637866,-74.9728224921344,
-215.283283));
#230966=CARTESIAN_POINT('Ctrl Pts',(43.9240702761126,-75.0144723099439,
-215.216616));
#230967=CARTESIAN_POINT('Ctrl Pts',(43.9865729884385,-75.0561221277533,
-215.149949));
#230968=CARTESIAN_POINT('Ctrl Pts',(25.2812199560259,-62.390732268219,-235.35005));
#230969=CARTESIAN_POINT('Ctrl Pts',(31.8143029221326,-66.4798048243852,
-228.68335));
#230970=CARTESIAN_POINT('Ctrl Pts',(38.3473707133638,-70.5681428074098,
-222.01665));
#230971=CARTESIAN_POINT('Ctrl Pts',(44.8804206737979,-74.6557463029982,
-215.34995));
#230972=CARTESIAN_POINT('Ctrl Pts',(44.9457511734022,-74.6966223379541,
-215.283283));
#230973=CARTESIAN_POINT('Ctrl Pts',(45.0110816730065,-74.73749837291,-215.216616));
#230974=CARTESIAN_POINT('Ctrl Pts',(45.0764121726109,-74.7783744078659,
-215.149949));
#230975=CARTESIAN_POINT('Ctrl Pts',(25.5015868365187,-62.3415392578964,
-235.35005));
#230976=CARTESIAN_POINT('Ctrl Pts',(32.299209143815,-66.325492796133,-228.68335));
#230977=CARTESIAN_POINT('Ctrl Pts',(39.0968174546589,-70.3085029414293,
-222.01665));
#230978=CARTESIAN_POINT('Ctrl Pts',(45.8944083573785,-74.2905697967455,
-215.34995));
#230979=CARTESIAN_POINT('Ctrl Pts',(45.9623842664057,-74.3303904652987,
-215.283283));
#230980=CARTESIAN_POINT('Ctrl Pts',(46.0303601754329,-74.3702111338518,
-215.216616));
#230981=CARTESIAN_POINT('Ctrl Pts',(46.0983360844601,-74.410031802405,-215.149949));
#230982=CARTESIAN_POINT('Ctrl Pts',(25.7300777644121,-62.275287851211,-235.35005));
#230983=CARTESIAN_POINT('Ctrl Pts',(32.7889564583827,-66.1223030781061,
-228.68335));
#230984=CARTESIAN_POINT('Ctrl Pts',(39.8478250972557,-69.9681827947029,
-222.01665));
#230985=CARTESIAN_POINT('Ctrl Pts',(46.906679573783,-73.8129271161338,-215.34995));
#230986=CARTESIAN_POINT('Ctrl Pts',(46.9772681185483,-73.8513745593482,
-215.283283));
#230987=CARTESIAN_POINT('Ctrl Pts',(47.0478566633135,-73.8898220025625,
-215.216616));
#230988=CARTESIAN_POINT('Ctrl Pts',(47.1184452080788,-73.9282694457768,
-215.149949));
#230989=CARTESIAN_POINT('Ctrl Pts',(25.9496411726737,-62.2064433802863,
-235.35005));
#230990=CARTESIAN_POINT('Ctrl Pts',(33.2328325215974,-65.8962682476017,
-228.68335));
#230991=CARTESIAN_POINT('Ctrl Pts',(40.5160203632138,-69.5847817101261,
-222.01665));
#230992=CARTESIAN_POINT('Ctrl Pts',(47.7991999531534,-73.2719838903286,
-215.34995));
#230993=CARTESIAN_POINT('Ctrl Pts',(47.8720317490528,-73.3088559121307,
-215.283283));
#230994=CARTESIAN_POINT('Ctrl Pts',(47.9448635449522,-73.3457279339327,
-215.216616));
#230995=CARTESIAN_POINT('Ctrl Pts',(48.0176953408516,-73.3825999557347,
-215.149949));
#230996=CARTESIAN_POINT('Ctrl Pts',(26.2296171960789,-62.0929811520229,
-235.35005));
#230997=CARTESIAN_POINT('Ctrl Pts',(33.5992240749579,-65.6911775370676,
-228.68335));
#230998=CARTESIAN_POINT('Ctrl Pts',(40.9688364442604,-69.2879023661194,
-222.01665));
#230999=CARTESIAN_POINT('Ctrl Pts',(48.3384489792287,-72.8831557643943,
-215.34995));
#231000=CARTESIAN_POINT('Ctrl Pts',(48.4121451045784,-72.919108298377,-215.283283));
#231001=CARTESIAN_POINT('Ctrl Pts',(48.485841229928,-72.9550608323598,-215.216616));
#231002=CARTESIAN_POINT('Ctrl Pts',(48.5595373552777,-72.9910133663425,
-215.149949));
#231003=CARTESIAN_POINT('Ctrl Pts',(26.4137508499222,-62.0144582859218,
-235.35005));
#231004=CARTESIAN_POINT('Ctrl Pts',(33.8110251833904,-65.5692400768433,
-228.68335));
#231005=CARTESIAN_POINT('Ctrl Pts',(41.2083125347321,-69.1224537201152,
-222.01665));
#231006=CARTESIAN_POINT('Ctrl Pts',(48.6056072289401,-72.6740993398878,
-215.34995));
#231007=CARTESIAN_POINT('Ctrl Pts',(48.6795801758822,-72.7096157960855,
-215.283283));
#231008=CARTESIAN_POINT('Ctrl Pts',(48.7535531228243,-72.7451322522832,
-215.216616));
#231009=CARTESIAN_POINT('Ctrl Pts',(48.8275260697664,-72.780648708481,-215.149949));
#231010=CARTESIAN_POINT('Ctrl Pts',(26.60131676328,-61.915483833886,-235.35005));
#231011=CARTESIAN_POINT('Ctrl Pts',(33.9746898504281,-65.4717344596898,
-228.68335));
#231012=CARTESIAN_POINT('Ctrl Pts',(41.3480800753329,-69.0263711060389,
-222.01665));
#231013=CARTESIAN_POINT('Ctrl Pts',(48.7214815967444,-72.5793938958684,
-215.34995));
#231014=CARTESIAN_POINT('Ctrl Pts',(48.7952156119585,-72.6149241237667,
-215.283283));
#231015=CARTESIAN_POINT('Ctrl Pts',(48.8689496271726,-72.6504543516649,
-215.216616));
#231016=CARTESIAN_POINT('Ctrl Pts',(48.9426836423867,-72.6859845795632,
-215.149949));
#231017=CARTESIAN_POINT('',(33.2187488845874,-68.8101802592752,-225.35));
#231018=CARTESIAN_POINT('Ctrl Pts',(27.0930165135311,-62.1526330725429,
-234.905475377596));
#231019=CARTESIAN_POINT('Ctrl Pts',(33.75885046978,-65.3675653924474,-228.878503713969));
#231020=CARTESIAN_POINT('Ctrl Pts',(40.424698326436,-68.5811786244384,-222.851532050343));
#231021=CARTESIAN_POINT('Ctrl Pts',(47.0905557676078,-71.7934728593479,
-216.824560386716));
#231022=CARTESIAN_POINT('Ctrl Pts',(29.0709882823152,37.525873057636,-235.35005));
#231023=CARTESIAN_POINT('Ctrl Pts',(35.5332604733831,40.6579014073498,-228.683350000001));
#231024=CARTESIAN_POINT('Ctrl Pts',(41.9930962102693,43.771133049519,-222.01665));
#231025=CARTESIAN_POINT('Ctrl Pts',(48.4493862544499,46.8657485296993,-215.34995));
#231026=CARTESIAN_POINT('Ctrl Pts',(48.5139491548917,46.8966946845011,-215.283283));
#231027=CARTESIAN_POINT('Ctrl Pts',(48.5785120553335,46.9276408393029,-215.216616));
#231028=CARTESIAN_POINT('Ctrl Pts',(48.6430749557753,46.9585869941047,-215.149949));
#231029=CARTESIAN_POINT('Ctrl Pts',(28.9262831839988,37.6116730896339,-235.35005));
#231030=CARTESIAN_POINT('Ctrl Pts',(35.404815368487,40.7403542996618,-228.683350000001));
#231031=CARTESIAN_POINT('Ctrl Pts',(41.8809828830328,43.8508119821702,-222.01665));
#231032=CARTESIAN_POINT('Ctrl Pts',(48.3537103198215,46.9432211795102,-215.34995));
#231033=CARTESIAN_POINT('Ctrl Pts',(48.4184375941894,46.9741452714836,-215.283283));
#231034=CARTESIAN_POINT('Ctrl Pts',(48.4831648685572,47.005069363457,-215.216616));
#231035=CARTESIAN_POINT('Ctrl Pts',(48.5478921429251,47.0359934554304,-215.149949));
#231036=CARTESIAN_POINT('Ctrl Pts',(28.7510590357854,37.7017381212741,-235.35005));
#231037=CARTESIAN_POINT('Ctrl Pts',(35.2153249135404,40.8559840579253,-228.683350000001));
#231038=CARTESIAN_POINT('Ctrl Pts',(41.67737658309,43.9932018113665,-222.01665));
#231039=CARTESIAN_POINT('Ctrl Pts',(48.1362091874323,47.1135549465408,-215.34995));
#231040=CARTESIAN_POINT('Ctrl Pts',(48.2007975134757,47.1447584778926,-215.283283));
#231041=CARTESIAN_POINT('Ctrl Pts',(48.2653858395191,47.1759620092443,-215.216616));
#231042=CARTESIAN_POINT('Ctrl Pts',(48.3299741655626,47.207165540596,-215.149949));
#231043=CARTESIAN_POINT('Ctrl Pts',(28.5095079111441,37.8154098604791,-235.350050000001));
#231044=CARTESIAN_POINT('Ctrl Pts',(34.9092271504532,41.0352703241457,-228.683350000001));
#231045=CARTESIAN_POINT('Ctrl Pts',(41.3069791618872,44.2400465335893,-222.016650000001));
#231046=CARTESIAN_POINT('Ctrl Pts',(47.7018738162952,47.429883386524,-215.34995));
#231047=CARTESIAN_POINT('Ctrl Pts',(47.7658227628392,47.4617817550534,-215.283283));
#231048=CARTESIAN_POINT('Ctrl Pts',(47.8297717093833,47.4936801235827,-215.216616));
#231049=CARTESIAN_POINT('Ctrl Pts',(47.8937206559274,47.525578492112,-215.149949));
#231050=CARTESIAN_POINT('Ctrl Pts',(28.3066649003232,37.8966208237621,-235.35005));
#231051=CARTESIAN_POINT('Ctrl Pts',(34.5530956045189,41.2282169831045,-228.68335));
#231052=CARTESIAN_POINT('Ctrl Pts',(40.7978279568429,44.5468276894782,-222.01665));
#231053=CARTESIAN_POINT('Ctrl Pts',(47.0400956910773,47.8525776841313,-215.34995));
#231054=CARTESIAN_POINT('Ctrl Pts',(47.1025183684196,47.8856351840778,-215.283283));
#231055=CARTESIAN_POINT('Ctrl Pts',(47.1649410457619,47.9186926840244,-215.216616));
#231056=CARTESIAN_POINT('Ctrl Pts',(47.2273637231043,47.9517501839709,-215.149949));
#231057=CARTESIAN_POINT('Ctrl Pts',(28.0997724400839,37.970731452037,-235.35005));
#231058=CARTESIAN_POINT('Ctrl Pts',(34.1684829306694,41.4070992755122,-228.683350000001));
#231059=CARTESIAN_POINT('Ctrl Pts',(40.2357864490083,44.8327392792855,-222.01665));
#231060=CARTESIAN_POINT('Ctrl Pts',(46.3010499603476,48.2477545207809,-215.34995));
#231061=CARTESIAN_POINT('Ctrl Pts',(46.361702595461,48.2819046731959,-215.283283));
#231062=CARTESIAN_POINT('Ctrl Pts',(46.4223552305744,48.3160548256108,-215.216616));
#231063=CARTESIAN_POINT('Ctrl Pts',(46.4830078656878,48.3502049780258,-215.149949));
#231064=CARTESIAN_POINT('Ctrl Pts',(27.9025329741163,38.0324522529201,-235.35005));
#231065=CARTESIAN_POINT('Ctrl Pts',(33.7896008939784,41.5559827385479,-228.683350000001));
#231066=CARTESIAN_POINT('Ctrl Pts',(39.6755763327887,45.0712058294971,-222.01665));
#231067=CARTESIAN_POINT('Ctrl Pts',(45.5599690892415,48.5782013338904,-215.349950000001));
#231068=CARTESIAN_POINT('Ctrl Pts',(45.618813016806,48.6132712889344,-215.283283000001));
#231069=CARTESIAN_POINT('Ctrl Pts',(45.6776569443706,48.6483412439783,-215.216616));
#231070=CARTESIAN_POINT('Ctrl Pts',(45.7365008719351,48.6834111990222,-215.149949000001));
#231071=CARTESIAN_POINT('Ctrl Pts',(27.6836295517497,38.0888474954169,-235.35005));
#231072=CARTESIAN_POINT('Ctrl Pts',(33.3812146101381,41.6857034969331,-228.68335));
#231073=CARTESIAN_POINT('Ctrl Pts',(39.0780453981879,45.2768392802963,-222.01665));
#231074=CARTESIAN_POINT('Ctrl Pts',(44.773784383473,48.8623098007285,-215.34995));
#231075=CARTESIAN_POINT('Ctrl Pts',(44.8307417733259,48.8981645059328,-215.283283));
#231076=CARTESIAN_POINT('Ctrl Pts',(44.8876991631787,48.9340192111371,-215.216616));
#231077=CARTESIAN_POINT('Ctrl Pts',(44.9446565530316,48.9698739163414,-215.149949));
#231078=CARTESIAN_POINT('Ctrl Pts',(27.4619512217085,38.1391172889764,-235.35005));
#231079=CARTESIAN_POINT('Ctrl Pts',(32.9867338744792,41.7852023290646,-228.683350000001));
#231080=CARTESIAN_POINT('Ctrl Pts',(38.511124795091,45.4283250387717,-222.016650000001));
#231081=CARTESIAN_POINT('Ctrl Pts',(44.0349491888799,49.0685138787004,-215.349950000001));
#231082=CARTESIAN_POINT('Ctrl Pts',(44.0901874328179,49.1049157670997,-215.283283000001));
#231083=CARTESIAN_POINT('Ctrl Pts',(44.1454256767557,49.141317655499,-215.216616));
#231084=CARTESIAN_POINT('Ctrl Pts',(44.2006639206936,49.1777195438983,-215.149949000001));
#231085=CARTESIAN_POINT('Ctrl Pts',(27.272251770635,38.1696450547512,-235.35005));
#231086=CARTESIAN_POINT('Ctrl Pts',(32.7234828694691,41.832799228952,-228.68335));
#231087=CARTESIAN_POINT('Ctrl Pts',(38.1745805518739,45.4949461119472,-222.01665));
#231088=CARTESIAN_POINT('Ctrl Pts',(43.625485383249,49.1560953813671,-215.34995));
#231089=CARTESIAN_POINT('Ctrl Pts',(43.6799944315629,49.1927068740612,-215.283283));
#231090=CARTESIAN_POINT('Ctrl Pts',(43.7345034798766,49.2293183667554,-215.216616));
#231091=CARTESIAN_POINT('Ctrl Pts',(43.7890125281904,49.2659298594496,-215.149949));
#231092=CARTESIAN_POINT('Ctrl Pts',(27.1569075795172,38.1844371310006,-235.35005));
#231093=CARTESIAN_POINT('Ctrl Pts',(32.5837764342019,41.8536056393876,-228.68335));
#231094=CARTESIAN_POINT('Ctrl Pts',(38.0106452875494,45.5227741479461,-222.01665));
#231095=CARTESIAN_POINT('Ctrl Pts',(43.4375141409548,49.1919426564936,-215.34995));
#231096=CARTESIAN_POINT('Ctrl Pts',(43.4917828294889,49.2286343415791,-215.283283));
#231097=CARTESIAN_POINT('Ctrl Pts',(43.5460515180229,49.2653260266646,-215.216616));
#231098=CARTESIAN_POINT('Ctrl Pts',(43.600320206557,49.30201771175,-215.149949));
#231099=CARTESIAN_POINT('Ctrl Pts',(29.5524353619882,37.7591803693089,-234.853368133768));
#231100=CARTESIAN_POINT('Ctrl Pts',(35.3897707041939,40.5875346064766,-228.831260854445));
#231101=CARTESIAN_POINT('Ctrl Pts',(41.225095491082,43.4005549188572,-222.809153575121));
#231102=CARTESIAN_POINT('Ctrl Pts',(47.0575921287078,46.1983743823903,-216.787046295788));
#231103=CARTESIAN_POINT('',(35.2972108607157,43.6881898936869,-225.35));
#231104=CARTESIAN_POINT('Ctrl Pts',(48.9291851287222,16.4845500982845,-235.35005));
#231105=CARTESIAN_POINT('Ctrl Pts',(53.3017114728827,20.6931427899333,-228.68335));
#231106=CARTESIAN_POINT('Ctrl Pts',(57.6742344655836,24.9017353436595,-222.01665));
#231107=CARTESIAN_POINT('Ctrl Pts',(62.0467541066728,29.1103277631972,-215.34995));
#231108=CARTESIAN_POINT('Ctrl Pts',(62.0904793030837,29.1524136873926,-215.283283));
#231109=CARTESIAN_POINT('Ctrl Pts',(62.1342044994946,29.194499611588,-215.216616));
#231110=CARTESIAN_POINT('Ctrl Pts',(62.1779296959055,29.2365855357833,-215.149949));
#231111=CARTESIAN_POINT('Ctrl Pts',(48.9286835714312,16.4968248922029,-235.35005));
#231112=CARTESIAN_POINT('Ctrl Pts',(53.3011147739234,20.7079343778016,-228.68335));
#231113=CARTESIAN_POINT('Ctrl Pts',(57.6735437421284,24.9190437709811,-222.01665));
#231114=CARTESIAN_POINT('Ctrl Pts',(62.0459704759518,29.1301530740427,-215.34995));
#231115=CARTESIAN_POINT('Ctrl Pts',(62.08969474329,29.1722641670733,-215.283283));
#231116=CARTESIAN_POINT('Ctrl Pts',(62.1334190106282,29.2143752601038,-215.216616));
#231117=CARTESIAN_POINT('Ctrl Pts',(62.1771432779665,29.2564863531345,-215.149949));
#231118=CARTESIAN_POINT('Ctrl Pts',(48.9281820141402,16.5090996861212,-235.35005));
#231119=CARTESIAN_POINT('Ctrl Pts',(53.3005180749641,20.72272596567,-228.68335));
#231120=CARTESIAN_POINT('Ctrl Pts',(57.6728530186733,24.9363521983027,-222.01665));
#231121=CARTESIAN_POINT('Ctrl Pts',(62.0451868452307,29.1499783848881,-215.34995));
#231122=CARTESIAN_POINT('Ctrl Pts',(62.0889101834963,29.1921146467539,-215.283283));
#231123=CARTESIAN_POINT('Ctrl Pts',(62.1326335217618,29.2342509086198,-215.216616));
#231124=CARTESIAN_POINT('Ctrl Pts',(62.1763568600274,29.2763871704856,-215.149949));
#231125=CARTESIAN_POINT('Ctrl Pts',(48.9276804568491,16.5213744800396,-235.35005));
#231126=CARTESIAN_POINT('Ctrl Pts',(53.2999213760048,20.7375175535383,-228.68335));
#231127=CARTESIAN_POINT('Ctrl Pts',(57.6721622952182,24.9536606256242,-222.01665));
#231128=CARTESIAN_POINT('Ctrl Pts',(62.0444032145096,29.1698036957335,-215.34995));
#231129=CARTESIAN_POINT('Ctrl Pts',(62.0881256237025,29.2119651264346,-215.283283));
#231130=CARTESIAN_POINT('Ctrl Pts',(62.1318480328954,29.2541265571357,-215.216616));
#231131=CARTESIAN_POINT('Ctrl Pts',(62.1755704420884,29.2962879878368,-215.149949));
#231132=CARTESIAN_POINT('Ctrl Pts',(48.9214109907111,16.6748094040191,-235.35005));
#231133=CARTESIAN_POINT('Ctrl Pts',(53.2924626390134,20.9224124018924,-228.68335));
#231134=CARTESIAN_POINT('Ctrl Pts',(57.663528252029,25.170015967144,-222.01665));
#231135=CARTESIAN_POINT('Ctrl Pts',(62.0346078304961,29.4176200813015,-215.34995));
#231136=CARTESIAN_POINT('Ctrl Pts',(62.0783186262808,29.4600961224431,-215.283283));
#231137=CARTESIAN_POINT('Ctrl Pts',(62.1220294220655,29.5025721635847,-215.216616));
#231138=CARTESIAN_POINT('Ctrl Pts',(62.1657402178502,29.5450482047262,-215.149949));
#231139=CARTESIAN_POINT('Ctrl Pts',(48.8992712925998,16.9131404133547,-235.35005));
#231140=CARTESIAN_POINT('Ctrl Pts',(53.2652870417935,21.2619501899207,-228.68335));
#231141=CARTESIAN_POINT('Ctrl Pts',(57.6313776897902,25.6107124643303,-222.01665));
#231142=CARTESIAN_POINT('Ctrl Pts',(61.9975402416511,29.9594276183431,-215.34995));
#231143=CARTESIAN_POINT('Ctrl Pts',(62.0412018671697,30.0029147698833,-215.283283));
#231144=CARTESIAN_POINT('Ctrl Pts',(62.0848634926883,30.0464019214233,-215.216616));
#231145=CARTESIAN_POINT('Ctrl Pts',(62.1285251182069,30.0898890729635,-215.149949));
#231146=CARTESIAN_POINT('Ctrl Pts',(48.8533444192211,17.2181014412188,-235.35005));
#231147=CARTESIAN_POINT('Ctrl Pts',(53.1855995667747,21.7941761255924,-228.68335));
#231148=CARTESIAN_POINT('Ctrl Pts',(57.5179747573295,26.3699864363254,-222.01665));
#231149=CARTESIAN_POINT('Ctrl Pts',(61.8504540244681,30.9455347714532,-215.34995));
#231150=CARTESIAN_POINT('Ctrl Pts',(61.8937788171395,30.9912902548045,-215.283283));
#231151=CARTESIAN_POINT('Ctrl Pts',(61.9371036098109,31.0370457381558,-215.216616));
#231152=CARTESIAN_POINT('Ctrl Pts',(61.9804284024823,31.082801221507,-215.149949));
#231153=CARTESIAN_POINT('Ctrl Pts',(48.793774157437,17.4925774935122,-235.35005));
#231154=CARTESIAN_POINT('Ctrl Pts',(53.0569741223029,22.3329163118503,-228.68335));
#231155=CARTESIAN_POINT('Ctrl Pts',(57.3203153214379,27.1726388120429,-222.01665));
#231156=CARTESIAN_POINT('Ctrl Pts',(61.5837608612094,32.0117507116806,-215.34995));
#231157=CARTESIAN_POINT('Ctrl Pts',(61.6263953166071,32.060141830677,-215.283283));
#231158=CARTESIAN_POINT('Ctrl Pts',(61.6690297720048,32.1085329496734,-215.216616));
#231159=CARTESIAN_POINT('Ctrl Pts',(61.7116642274025,32.1569240686698,-215.149949));
#231160=CARTESIAN_POINT('Ctrl Pts',(48.7243271460874,17.7538206185435,-235.35005));
#231161=CARTESIAN_POINT('Ctrl Pts',(52.8915700395936,22.8426678835018,-228.68335));
#231162=CARTESIAN_POINT('Ctrl Pts',(57.0589527628024,27.9304206519508,-222.01665));
#231163=CARTESIAN_POINT('Ctrl Pts',(61.2264100602501,33.0170891792215,-215.34995));
#231164=CARTESIAN_POINT('Ctrl Pts',(61.2680846332245,33.0679558644942,-215.283283));
#231165=CARTESIAN_POINT('Ctrl Pts',(61.309759206199,33.1188225497669,-215.216616));
#231166=CARTESIAN_POINT('Ctrl Pts',(61.3514337791735,33.1696892350396,-215.149949));
#231167=CARTESIAN_POINT('Ctrl Pts',(48.6354732464631,18.0177190827397,-235.35005));
#231168=CARTESIAN_POINT('Ctrl Pts',(52.6780922604543,23.3513726702934,-228.68335));
#231169=CARTESIAN_POINT('Ctrl Pts',(56.7208284608432,28.6833361882777,-222.01665));
#231170=CARTESIAN_POINT('Ctrl Pts',(60.7635813168395,34.0136255628538,-215.34995));
#231171=CARTESIAN_POINT('Ctrl Pts',(60.8040088453995,34.0669284565996,-215.283283));
#231172=CARTESIAN_POINT('Ctrl Pts',(60.8444363739595,34.1202313503453,-215.216616));
#231173=CARTESIAN_POINT('Ctrl Pts',(60.8848639025194,34.1735342440911,-215.149949));
#231174=CARTESIAN_POINT('Ctrl Pts',(48.5352774797299,18.2802794424427,-235.35005));
#231175=CARTESIAN_POINT('Ctrl Pts',(52.4343101169869,23.8247568642913,-228.68335));
#231176=CARTESIAN_POINT('Ctrl Pts',(56.3334174156944,29.3668400879758,-222.016650000001));
#231177=CARTESIAN_POINT('Ctrl Pts',(60.2324571773606,34.9065517584836,-215.349950000001));
#231178=CARTESIAN_POINT('Ctrl Pts',(60.2714475749772,34.9619488751887,-215.283283000001));
#231179=CARTESIAN_POINT('Ctrl Pts',(60.3104379725939,35.0173459918937,-215.216616));
#231180=CARTESIAN_POINT('Ctrl Pts',(60.3494283702106,35.0727431085988,-215.149949000001));
#231181=CARTESIAN_POINT('Ctrl Pts',(48.3890207412154,18.5878255918932,-235.35005));
#231182=CARTESIAN_POINT('Ctrl Pts',(52.1962991404372,24.228375758149,-228.68335));
#231183=CARTESIAN_POINT('Ctrl Pts',(56.0035911516163,29.8657278812732,-222.01665));
#231184=CARTESIAN_POINT('Ctrl Pts',(59.810707037304,35.4999122879811,-215.34995));
#231185=CARTESIAN_POINT('Ctrl Pts',(59.8487781961609,35.5562541320482,-215.283283));
#231186=CARTESIAN_POINT('Ctrl Pts',(59.8868493550178,35.6125959761153,-215.216616));
#231187=CARTESIAN_POINT('Ctrl Pts',(59.9249205138747,35.6689378201824,-215.149949));
#231188=CARTESIAN_POINT('Ctrl Pts',(48.2711217441656,18.8106246802399,-235.35005));
#231189=CARTESIAN_POINT('Ctrl Pts',(52.0406861996216,24.475501377336,-228.68335));
#231190=CARTESIAN_POINT('Ctrl Pts',(55.8102121224059,30.1365835498488,-222.01665));
#231191=CARTESIAN_POINT('Ctrl Pts',(59.5794745156759,35.7939072308497,-215.34995));
#231192=CARTESIAN_POINT('Ctrl Pts',(59.6171671396086,35.8504804676597,-215.283283));
#231193=CARTESIAN_POINT('Ctrl Pts',(59.6548597635413,35.9070537044696,-215.216616));
#231194=CARTESIAN_POINT('Ctrl Pts',(59.692552387474,35.9636269412797,-215.149949));
#231195=CARTESIAN_POINT('Ctrl Pts',(48.1560655143106,18.9923105754345,-235.35005));
#231196=CARTESIAN_POINT('Ctrl Pts',(51.9286217775904,24.6399928719346,-228.68335));
#231197=CARTESIAN_POINT('Ctrl Pts',(55.7011108008251,30.2835687301176,-222.01665));
#231198=CARTESIAN_POINT('Ctrl Pts',(59.4732891526392,35.9230771683515,-215.34995));
#231199=CARTESIAN_POINT('Ctrl Pts',(59.5110109361573,35.9794722527339,-215.283283));
#231200=CARTESIAN_POINT('Ctrl Pts',(59.5487327196755,36.0358673371162,-215.216616));
#231201=CARTESIAN_POINT('Ctrl Pts',(59.5864545031936,36.0922624214986,-215.149949));
#231202=CARTESIAN_POINT('Ctrl Pts',(48.1468610159222,19.00684544705,-235.35005));
#231203=CARTESIAN_POINT('Ctrl Pts',(51.9196566238279,24.6531521915024,-228.68335));
#231204=CARTESIAN_POINT('Ctrl Pts',(55.6923826950986,30.2953275445391,-222.01665));
#231205=CARTESIAN_POINT('Ctrl Pts',(59.4647943235962,35.9334107633517,-215.34995));
#231206=CARTESIAN_POINT('Ctrl Pts',(59.5025184398812,35.9897915955398,-215.283283));
#231207=CARTESIAN_POINT('Ctrl Pts',(59.5402425561662,36.046172427728,-215.216616));
#231208=CARTESIAN_POINT('Ctrl Pts',(59.5779666724512,36.102553259916,-215.149949));
#231209=CARTESIAN_POINT('Ctrl Pts',(48.1376565175338,19.0213803186655,-235.35005));
#231210=CARTESIAN_POINT('Ctrl Pts',(51.9106914700654,24.6663115110703,-228.68335));
#231211=CARTESIAN_POINT('Ctrl Pts',(55.6836545893721,30.3070863589606,-222.01665));
#231212=CARTESIAN_POINT('Ctrl Pts',(59.4562994945533,35.9437443583519,-215.34995));
#231213=CARTESIAN_POINT('Ctrl Pts',(59.4940259436051,36.0001109383457,-215.283283));
#231214=CARTESIAN_POINT('Ctrl Pts',(59.5317523926569,36.0564775183397,-215.216616));
#231215=CARTESIAN_POINT('Ctrl Pts',(59.5694788417088,36.1128440983336,-215.149949));
#231216=CARTESIAN_POINT('Ctrl Pts',(48.1284520191454,19.0359151902811,-235.35005));
#231217=CARTESIAN_POINT('Ctrl Pts',(51.9017263163029,24.6794708306382,-228.68335));
#231218=CARTESIAN_POINT('Ctrl Pts',(55.6749264836457,30.3188451733821,-222.01665));
#231219=CARTESIAN_POINT('Ctrl Pts',(59.4478046655104,35.9540779533519,-215.34995));
#231220=CARTESIAN_POINT('Ctrl Pts',(59.485533447329,36.0104302811517,-215.283283));
#231221=CARTESIAN_POINT('Ctrl Pts',(59.5232622291477,36.0667826089514,-215.216616));
#231222=CARTESIAN_POINT('Ctrl Pts',(59.5609910109663,36.1231349367511,-215.149949));
#231223=CARTESIAN_POINT('',(55.4860418356284,22.8455890891576,-225.35));
#231224=CARTESIAN_POINT('Ctrl Pts',(48.4260896922586,19.3965417854656,-234.872874618363));
#231225=CARTESIAN_POINT('Ctrl Pts',(51.8397102119512,24.5067087698627,-228.840465153427));
#231226=CARTESIAN_POINT('Ctrl Pts',(55.2532709224339,29.6135143043896,-222.808055688492));
#231227=CARTESIAN_POINT('Ctrl Pts',(58.6665914736623,34.7169872964315,-216.775646223556));
#231228=CARTESIAN_POINT('Origin',(41.5452362233251,-63.7990866568863,-205.34995));
#231229=CARTESIAN_POINT('',(48.8319431829163,-72.7145462807723,-205.34995));
#231230=CARTESIAN_POINT('',(41.9984355604289,-75.3045692187324,-205.34995));
#231231=CARTESIAN_POINT('Origin',(0.,-12.9675000200281,-205.34995));
#231232=CARTESIAN_POINT('',(59.6081272922882,-61.9689221688742,-205.34995));
#231233=CARTESIAN_POINT('Origin',(50.7133971693864,-54.6569255427236,-205.34995));
#231234=CARTESIAN_POINT('',(62.2188176672479,-55.1116977796555,-205.34995));
#231235=CARTESIAN_POINT('Origin',(50.7133971693864,28.7219255026674,-205.34995));
#231236=CARTESIAN_POINT('',(59.6081272922883,36.0339221288179,-205.34995));
#231237=CARTESIAN_POINT('',(62.218817667248,29.176697739599,-205.34995));
#231238=CARTESIAN_POINT('Origin',(0.,-12.9675000200281,-205.34995));
#231239=CARTESIAN_POINT('',(48.5592309447134,47.0014027710106,-205.34995));
#231240=CARTESIAN_POINT('Origin',(41.3132181298675,38.0528376956935,-205.34995));
#231241=CARTESIAN_POINT('',(43.4702127313761,49.3634032389879,-205.34995));
#231242=CARTESIAN_POINT('Origin',(0.,990.91999998,-205.34995));
#231243=CARTESIAN_POINT('Origin',(-476.643301415307,-33.8122127813758,-179.64995));
#231244=CARTESIAN_POINT('',(44.0225733573905,52.2597994838836,-179.64995));
#231245=CARTESIAN_POINT('Origin',(0.,-178.58000002,-179.64995));
#231246=CARTESIAN_POINT('',(42.1144903105792,-78.2508795831687,-179.64995));
#231247=CARTESIAN_POINT('Origin',(0.,990.91999998,-179.64995));
#231248=CARTESIAN_POINT('',(50.6979144815776,-74.9976066350312,-179.64995));
#231249=CARTESIAN_POINT('Origin',(41.5452362233251,-63.7990866568863,-179.64995));
#231250=CARTESIAN_POINT('',(61.8858792604563,-63.8413696154326,-179.64995));
#231251=CARTESIAN_POINT('Origin',(0.,-12.9675000200281,-179.64995));
#231252=CARTESIAN_POINT('',(65.1651121384123,-55.2281553161325,-179.64995));
#231253=CARTESIAN_POINT('Origin',(50.7133971693864,-54.6569255427236,-179.64995));
#231254=CARTESIAN_POINT('',(65.1651121384124,29.2931552760762,-179.64995));
#231255=CARTESIAN_POINT('Origin',(-1004.,-12.967500020028,-179.64995));
#231256=CARTESIAN_POINT('',(61.8858792604563,37.9063695753764,-179.64995));
#231257=CARTESIAN_POINT('Origin',(50.7133971693864,28.7219255026673,-179.64995));
#231258=CARTESIAN_POINT('',(50.4147813349261,49.2929407301111,-179.64995));
#231259=CARTESIAN_POINT('Origin',(0.,-12.9675000200281,-179.64995));
#231260=CARTESIAN_POINT('Origin',(41.3132181298675,38.0528376956935,-179.64995));
#231261=CARTESIAN_POINT('Origin',(-476.643301415307,-33.8122127813758,-205.34995));
#231262=CARTESIAN_POINT('Origin',(-1004.,-12.967500020028,-179.64995));
#231263=CARTESIAN_POINT('',(65.1651121384124,-55.2281553161325,-179.64995));
#231264=CARTESIAN_POINT('',(65.1651121384125,29.293155276076,-179.64995));
#231265=CARTESIAN_POINT('Origin',(50.7133971693864,28.7219255026673,-179.64995));
#231266=CARTESIAN_POINT('',(61.8858792604564,37.9063695753764,-179.64995));
#231267=CARTESIAN_POINT('Origin',(0.,-12.9675000200281,-179.64995));
#231268=CARTESIAN_POINT('',(50.4147813349261,49.292940730111,-179.64995));
#231269=CARTESIAN_POINT('Origin',(41.3132181298675,38.0528376956935,-179.64995));
#231270=CARTESIAN_POINT('',(44.0225733573905,52.2597994838836,-179.64995));
#231271=CARTESIAN_POINT('Origin',(0.,-178.58000002,-179.64995));
#231272=CARTESIAN_POINT('Origin',(0.,990.91999998,-179.64995));
#231273=CARTESIAN_POINT('',(42.1144903105791,-78.2508795831687,-179.64995));
#231274=CARTESIAN_POINT('Origin',(41.5452362233251,-63.7990866568863,-179.64995));
#231275=CARTESIAN_POINT('',(50.6979144815776,-74.9976066350312,-179.64995));
#231276=CARTESIAN_POINT('Origin',(0.,-12.9675000200281,-179.64995));
#231277=CARTESIAN_POINT('',(61.8858792604563,-63.8413696154326,-179.64995));
#231278=CARTESIAN_POINT('Origin',(50.7133971693864,-54.6569255427236,-179.64995));
#231279=CARTESIAN_POINT('Ctrl Pts',(48.9276804568491,-39.5283381317121,
-235.35005));
#231280=CARTESIAN_POINT('Ctrl Pts',(53.2999213760692,-44.7204933330714,
-228.68335));
#231281=CARTESIAN_POINT('Ctrl Pts',(57.6721622952894,-49.9126485344307,
-222.01665));
#231282=CARTESIAN_POINT('Ctrl Pts',(62.0444032145095,-55.1048037357899,
-215.34995));
#231283=CARTESIAN_POINT('Ctrl Pts',(49.0194233450359,-37.283081077169,-235.35005));
#231284=CARTESIAN_POINT('Ctrl Pts',(53.4090672042376,-42.0148742220589,
-228.683350000001));
#231285=CARTESIAN_POINT('Ctrl Pts',(57.7985067146479,-46.7466590436653,
-222.016650000001));
#231286=CARTESIAN_POINT('Ctrl Pts',(62.1877418657617,-51.4784358040522,
-215.34995));
#231287=CARTESIAN_POINT('Ctrl Pts',(49.1841844420714,-32.7087365060477,
-235.35005));
#231288=CARTESIAN_POINT('Ctrl Pts',(53.600359505658,-36.5883830285289,-228.68335));
#231289=CARTESIAN_POINT('Ctrl Pts',(58.0165345692446,-40.4680295510101,
-222.01665));
#231290=CARTESIAN_POINT('Ctrl Pts',(62.4327096328312,-44.3476760734913,
-215.34995));
#231291=CARTESIAN_POINT('Ctrl Pts',(49.3659986639477,-25.6715165814334,
-235.35005));
#231292=CARTESIAN_POINT('Ctrl Pts',(53.8070961606803,-28.4006856868431,
-228.68335));
#231293=CARTESIAN_POINT('Ctrl Pts',(58.2481936574129,-31.1298547922528,
-222.01665));
#231294=CARTESIAN_POINT('Ctrl Pts',(62.6892911541455,-33.8590238976625,
-215.34995));
#231295=CARTESIAN_POINT('Ctrl Pts',(49.4760453414413,-18.5583238061847,
-235.35005));
#231296=CARTESIAN_POINT('Ctrl Pts',(53.9314601157808,-20.1883767671888,
-228.68335));
#231297=CARTESIAN_POINT('Ctrl Pts',(58.3868748901203,-21.8184297281929,
-222.01665));
#231298=CARTESIAN_POINT('Ctrl Pts',(62.8422896644598,-23.448482689197,-215.34995));
#231299=CARTESIAN_POINT('Ctrl Pts',(49.5,-13.8395357876534,-235.35005));
#231300=CARTESIAN_POINT('Ctrl Pts',(53.9589513940208,-14.7196423822522,
-228.68335));
#231301=CARTESIAN_POINT('Ctrl Pts',(58.4179027880416,-15.599748976851,-222.01665));
#231302=CARTESIAN_POINT('Ctrl Pts',(62.8768541820624,-16.4798555714498,
-215.34995));
#231303=CARTESIAN_POINT('Ctrl Pts',(49.5,-11.5034818258362,-235.35005));
#231304=CARTESIAN_POINT('Ctrl Pts',(53.9589513940208,-11.9914878905669,
-228.68335));
#231305=CARTESIAN_POINT('Ctrl Pts',(58.4179027880416,-12.4794939552975,
-222.01665));
#231306=CARTESIAN_POINT('Ctrl Pts',(62.8768541820624,-12.9675000200282,
-215.34995));
#231307=CARTESIAN_POINT('Ctrl Pts',(49.5,-11.5034818258362,-235.35005));
#231308=CARTESIAN_POINT('Ctrl Pts',(53.9589513940208,-11.9914878905669,
-228.68335));
#231309=CARTESIAN_POINT('Ctrl Pts',(58.4179027880416,-12.4794939552975,
-222.01665));
#231310=CARTESIAN_POINT('Ctrl Pts',(62.8768541820624,-12.9675000200282,
-215.34995));
#231311=CARTESIAN_POINT('Ctrl Pts',(62.9214436960026,-12.9723800806755,
-215.283283));
#231312=CARTESIAN_POINT('Ctrl Pts',(62.9660332099428,-12.9772601413228,
-215.216616));
#231313=CARTESIAN_POINT('Ctrl Pts',(63.010622723883,-12.9821402019701,-215.149949));
#231314=CARTESIAN_POINT('Ctrl Pts',(49.5,-9.16742786401911,-235.35005));
#231315=CARTESIAN_POINT('Ctrl Pts',(53.9589513940208,-9.26333339888158,
-228.68335));
#231316=CARTESIAN_POINT('Ctrl Pts',(58.4179027880416,-9.35923893374405,
-222.01665));
#231317=CARTESIAN_POINT('Ctrl Pts',(62.8768541820624,-9.45514446860653,
-215.34995));
#231318=CARTESIAN_POINT('Ctrl Pts',(62.9214436960026,-9.45610352395515,
-215.283283));
#231319=CARTESIAN_POINT('Ctrl Pts',(62.9660332099428,-9.45706257930377,
-215.216616));
#231320=CARTESIAN_POINT('Ctrl Pts',(63.010622723883,-9.4580216346524,-215.149949));
#231321=CARTESIAN_POINT('Ctrl Pts',(49.4760453034623,-4.44863709409477,
-235.35005));
#231322=CARTESIAN_POINT('Ctrl Pts',(53.9314600904615,-3.79459717968296,
-228.68335));
#231323=CARTESIAN_POINT('Ctrl Pts',(58.3868748774607,-3.14055726527114,
-222.01665));
#231324=CARTESIAN_POINT('Ctrl Pts',(62.8422896644599,-2.48651735085932,
-215.34995));
#231325=CARTESIAN_POINT('Ctrl Pts',(62.8868438123299,-2.47997695171521,
-215.283283));
#231326=CARTESIAN_POINT('Ctrl Pts',(62.9313979601999,-2.47343655257108,
-215.216616));
#231327=CARTESIAN_POINT('Ctrl Pts',(62.9759521080699,-2.46689615342696,
-215.149949));
#231328=CARTESIAN_POINT('Ctrl Pts',(49.3659992921549,2.6645466712911,-235.350050000001));
#231329=CARTESIAN_POINT('Ctrl Pts',(53.8070965794851,4.41770573339612,-228.683350000001));
#231330=CARTESIAN_POINT('Ctrl Pts',(58.2481938668153,6.17086479550113,-222.016650000001));
#231331=CARTESIAN_POINT('Ctrl Pts',(62.6892911541455,7.92402385760615,-215.349950000001));
#231332=CARTESIAN_POINT('Ctrl Pts',(62.7337021270188,7.9415554482272,-215.283283000001));
#231333=CARTESIAN_POINT('Ctrl Pts',(62.7781130998921,7.95908703884825,-215.216616));
#231334=CARTESIAN_POINT('Ctrl Pts',(62.8225240727654,7.9766186294693,-215.149949000001));
#231335=CARTESIAN_POINT('Ctrl Pts',(49.1841830823307,9.70178317521733,-235.35005));
#231336=CARTESIAN_POINT('Ctrl Pts',(53.6003585991642,12.6054141279565,-228.68335));
#231337=CARTESIAN_POINT('Ctrl Pts',(58.0165341159977,15.5090450806958,-222.01665));
#231338=CARTESIAN_POINT('Ctrl Pts',(62.4327096328312,18.412676033435,-215.34995));
#231339=CARTESIAN_POINT('Ctrl Pts',(62.4768713879996,18.4417123429624,-215.283283));
#231340=CARTESIAN_POINT('Ctrl Pts',(62.5210331431679,18.4707486524898,-215.216616));
#231341=CARTESIAN_POINT('Ctrl Pts',(62.5651948983362,18.4997849620172,-215.149949));
#231342=CARTESIAN_POINT('Ctrl Pts',(49.0194233450359,14.2761174254963,-235.35005));
#231343=CARTESIAN_POINT('Ctrl Pts',(53.4090672042376,18.031898440925,-228.68335));
#231344=CARTESIAN_POINT('Ctrl Pts',(57.7985067146477,21.7876711330703,-222.01665));
#231345=CARTESIAN_POINT('Ctrl Pts',(62.1877418657617,25.5434357639959,-215.34995));
#231346=CARTESIAN_POINT('Ctrl Pts',(62.2316342172729,25.5809934103052,-215.283283));
#231347=CARTESIAN_POINT('Ctrl Pts',(62.275526568784,25.6185510566144,-215.216616));
#231348=CARTESIAN_POINT('Ctrl Pts',(62.3194189202952,25.6561087029237,-215.149949));
#231349=CARTESIAN_POINT('Ctrl Pts',(48.9276804568491,16.5213744800396,-235.35005));
#231350=CARTESIAN_POINT('Ctrl Pts',(53.2999213760048,20.7375175535383,-228.68335));
#231351=CARTESIAN_POINT('Ctrl Pts',(57.6721622952182,24.9536606256242,-222.01665));
#231352=CARTESIAN_POINT('Ctrl Pts',(62.0444032145096,29.1698036957335,-215.34995));
#231353=CARTESIAN_POINT('Ctrl Pts',(62.0881256237025,29.2119651264346,-215.283283));
#231354=CARTESIAN_POINT('Ctrl Pts',(62.1318480328954,29.2541265571357,-215.216616));
#231355=CARTESIAN_POINT('Ctrl Pts',(62.1755704420884,29.2962879878368,-215.149949));
#231356=CARTESIAN_POINT('Origin',(-1004.,-12.967500020028,-205.34995));
#231357=CARTESIAN_POINT('Ctrl Pts',(27.1569075795172,38.1844371310006,-235.35005));
#231358=CARTESIAN_POINT('Ctrl Pts',(32.5837764342019,41.8536056393876,-228.68335));
#231359=CARTESIAN_POINT('Ctrl Pts',(38.0106452875494,45.5227741479461,-222.01665));
#231360=CARTESIAN_POINT('Ctrl Pts',(43.4375141409548,49.1919426564936,-215.34995));
#231361=CARTESIAN_POINT('Ctrl Pts',(43.4917828294889,49.2286343415791,-215.283283));
#231362=CARTESIAN_POINT('Ctrl Pts',(43.5460515180229,49.2653260266646,-215.216616));
#231363=CARTESIAN_POINT('Ctrl Pts',(43.600320206557,49.30201771175,-215.149949));
#231364=CARTESIAN_POINT('Ctrl Pts',(22.7175376169318,38.7537549124104,-235.35005));
#231365=CARTESIAN_POINT('Ctrl Pts',(27.2067518411579,42.6544032575593,-228.68335));
#231366=CARTESIAN_POINT('Ctrl Pts',(31.7011009472754,46.5938202572852,-222.01665));
#231367=CARTESIAN_POINT('Ctrl Pts',(36.2028725106807,50.5716334315145,-215.34995));
#231368=CARTESIAN_POINT('Ctrl Pts',(36.2478902263148,50.6114115632568,-215.283283));
#231369=CARTESIAN_POINT('Ctrl Pts',(36.2929079419489,50.6511896949991,-215.216616));
#231370=CARTESIAN_POINT('Ctrl Pts',(36.3379256575829,50.6909678267414,-215.149949));
#231371=CARTESIAN_POINT('Ctrl Pts',(13.711356444076,39.6240660636921,-235.35005));
#231372=CARTESIAN_POINT('Ctrl Pts',(16.3741503826813,43.8592570013518,-228.68335));
#231373=CARTESIAN_POINT('Ctrl Pts',(19.0446466451262,48.1913695751969,-222.01665));
#231374=CARTESIAN_POINT('Ctrl Pts',(21.7262765934597,52.6194725853171,-215.34995));
#231375=CARTESIAN_POINT('Ctrl Pts',(21.753092892943,52.6637536154183,-215.283283));
#231376=CARTESIAN_POINT('Ctrl Pts',(21.7799091924264,52.7080346455195,-215.216616));
#231377=CARTESIAN_POINT('Ctrl Pts',(21.8067254919097,52.7523156756207,-215.149949));
#231378=CARTESIAN_POINT('Ctrl Pts',(-5.03069808033274E-14,40.0660654363212,
-235.350050000001));
#231379=CARTESIAN_POINT('Ctrl Pts',(-2.50315176572591E-14,44.4636082157172,
-228.683350000001));
#231380=CARTESIAN_POINT('Ctrl Pts',(3.67646180426256E-14,48.9871491221026,
-222.016650000001));
#231381=CARTESIAN_POINT('Ctrl Pts',(-2.42861286636753E-14,53.6354775956494,
-215.34995));
#231382=CARTESIAN_POINT('Ctrl Pts',(-2.48966361307383E-14,53.6819608803848,
-215.283283));
#231383=CARTESIAN_POINT('Ctrl Pts',(-2.55071435978013E-14,53.7284441651203,
-215.216616));
#231384=CARTESIAN_POINT('Ctrl Pts',(-2.61176510648644E-14,53.7749274498558,
-215.149949));
#231385=CARTESIAN_POINT('Ctrl Pts',(-13.7113564440761,39.6240660636921,
-235.35005));
#231386=CARTESIAN_POINT('Ctrl Pts',(-16.3741503826814,43.8592570013518,
-228.68335));
#231387=CARTESIAN_POINT('Ctrl Pts',(-19.0446466451262,48.1913695751964,
-222.01665));
#231388=CARTESIAN_POINT('Ctrl Pts',(-21.7262765934598,52.619472585317,-215.34995));
#231389=CARTESIAN_POINT('Ctrl Pts',(-21.7530928929431,52.6637536154182,
-215.283283));
#231390=CARTESIAN_POINT('Ctrl Pts',(-21.7799091924265,52.7080346455194,
-215.216616));
#231391=CARTESIAN_POINT('Ctrl Pts',(-21.8067254919098,52.7523156756206,
-215.149949));
#231392=CARTESIAN_POINT('Ctrl Pts',(-22.7175376169319,38.7537549124104,
-235.350050000001));
#231393=CARTESIAN_POINT('Ctrl Pts',(-27.206751841158,42.6544032575593,-228.68335));
#231394=CARTESIAN_POINT('Ctrl Pts',(-31.7011009472754,46.5938202572849,
-222.01665));
#231395=CARTESIAN_POINT('Ctrl Pts',(-36.2028725106808,50.5716334315145,
-215.34995));
#231396=CARTESIAN_POINT('Ctrl Pts',(-36.2478902263149,50.6114115632568,
-215.283283));
#231397=CARTESIAN_POINT('Ctrl Pts',(-36.2929079419489,50.6511896949991,
-215.216616));
#231398=CARTESIAN_POINT('Ctrl Pts',(-36.337925657583,50.6909678267414,-215.149949));
#231399=CARTESIAN_POINT('Ctrl Pts',(-27.1569075795173,38.1844371310006,
-235.35005));
#231400=CARTESIAN_POINT('Ctrl Pts',(-32.5837764342019,41.8536056393876,
-228.68335));
#231401=CARTESIAN_POINT('Ctrl Pts',(-38.0106452875494,45.5227741479461,
-222.01665));
#231402=CARTESIAN_POINT('Ctrl Pts',(-43.4375141409549,49.1919426564936,
-215.34995));
#231403=CARTESIAN_POINT('Ctrl Pts',(-43.491782829489,49.2286343415791,-215.283283));
#231404=CARTESIAN_POINT('Ctrl Pts',(-43.546051518023,49.2653260266646,-215.216616));
#231405=CARTESIAN_POINT('Ctrl Pts',(-43.6003202065571,49.30201771175,-215.149949));
#231406=CARTESIAN_POINT('Origin',(0.,-178.58000002,-205.34995));
#231407=CARTESIAN_POINT('Origin',(-296.501483394397,-25.4138432731711,-235.35005));
#231408=CARTESIAN_POINT('Ctrl Pts',(-24.4459324049495,-62.4902066935372,
-235.35005));
#231409=CARTESIAN_POINT('Ctrl Pts',(-30.2944767260349,-66.7035224039814,
-228.68335));
#231410=CARTESIAN_POINT('Ctrl Pts',(-36.1430210443398,-70.9168381145246,
-222.01665));
#231411=CARTESIAN_POINT('Ctrl Pts',(-41.991565360621,-75.1301538251475,
-215.34995));
#231412=CARTESIAN_POINT('Ctrl Pts',(-42.0500508037838,-75.1722869822537,
-215.283283));
#231413=CARTESIAN_POINT('Ctrl Pts',(-42.1085362469466,-75.21442013936,-215.216616));
#231414=CARTESIAN_POINT('Ctrl Pts',(-42.1670216901095,-75.2565532964662,
-215.149949));
#231415=CARTESIAN_POINT('Ctrl Pts',(-20.4621956228808,-62.6321691537996,
-235.35005));
#231416=CARTESIAN_POINT('Ctrl Pts',(-25.267980358079,-66.8889339565476,
-228.68335));
#231417=CARTESIAN_POINT('Ctrl Pts',(-30.0738587790242,-71.1483055815339,
-222.01665));
#231418=CARTESIAN_POINT('Ctrl Pts',(-34.8798403105591,-75.4102836728986,
-215.34995));
#231419=CARTESIAN_POINT('Ctrl Pts',(-34.9279001258744,-75.4529034538122,
-215.283283));
#231420=CARTESIAN_POINT('Ctrl Pts',(-34.9759599411898,-75.4955232347258,
-215.216616));
#231421=CARTESIAN_POINT('Ctrl Pts',(-35.0240197565051,-75.5381430156395,
-215.149949));
#231422=CARTESIAN_POINT('Ctrl Pts',(-12.3633338208145,-62.8510026026509,
-235.35005));
#231423=CARTESIAN_POINT('Ctrl Pts',(-15.1854795229237,-67.1680657809434,
-228.68335));
#231424=CARTESIAN_POINT('Ctrl Pts',(-18.0077657557388,-71.4916460146837,
-222.01665));
#231425=CARTESIAN_POINT('Ctrl Pts',(-20.8302066559562,-75.8217424142497,
-215.34995));
#231426=CARTESIAN_POINT('Ctrl Pts',(-20.8584310649584,-75.8650433782453,
-215.283283));
#231427=CARTESIAN_POINT('Ctrl Pts',(-20.8866554739606,-75.908344342241,
-215.216616));
#231428=CARTESIAN_POINT('Ctrl Pts',(-20.9148798829627,-75.9516453062367,
-215.149949));
#231429=CARTESIAN_POINT('Ctrl Pts',(-1.09287578986539E-13,-62.9629927582852,
-235.35005));
#231430=CARTESIAN_POINT('Ctrl Pts',(1.49836951995733E-13,-67.3083190291539,
-228.683350000001));
#231431=CARTESIAN_POINT('Ctrl Pts',(3.24284869790415E-13,-71.6621174720752,
-222.016650000001));
#231432=CARTESIAN_POINT('Ctrl Pts',(5.36029554076834E-13,-76.0243869305461,
-215.349950000001));
#231433=CARTESIAN_POINT('Ctrl Pts',(5.38147000919697E-13,-76.0680096251308,
-215.283283000001));
#231434=CARTESIAN_POINT('Ctrl Pts',(5.40264447762562E-13,-76.1116323197155,
-215.216616000001));
#231435=CARTESIAN_POINT('Ctrl Pts',(5.42381894605426E-13,-76.1552550143002,
-215.149949000001));
#231436=CARTESIAN_POINT('Ctrl Pts',(12.3633338208143,-62.8510026026509,
-235.35005));
#231437=CARTESIAN_POINT('Ctrl Pts',(15.185479522924,-67.1680657809432,-228.68335));
#231438=CARTESIAN_POINT('Ctrl Pts',(18.0077657557395,-71.4916460146835,
-222.01665));
#231439=CARTESIAN_POINT('Ctrl Pts',(20.8302066559573,-75.8217424142497,
-215.34995));
#231440=CARTESIAN_POINT('Ctrl Pts',(20.8584310649595,-75.8650433782453,
-215.283283));
#231441=CARTESIAN_POINT('Ctrl Pts',(20.8866554739617,-75.908344342241,-215.216616));
#231442=CARTESIAN_POINT('Ctrl Pts',(20.9148798829638,-75.9516453062367,
-215.149949));
#231443=CARTESIAN_POINT('Ctrl Pts',(20.4621956228805,-62.6321691537997,
-235.35005));
#231444=CARTESIAN_POINT('Ctrl Pts',(25.2679803580793,-66.8889339565475,
-228.68335));
#231445=CARTESIAN_POINT('Ctrl Pts',(30.0738587790249,-71.1483055815338,
-222.01665));
#231446=CARTESIAN_POINT('Ctrl Pts',(34.8798403105602,-75.4102836728983,
-215.34995));
#231447=CARTESIAN_POINT('Ctrl Pts',(34.9279001258756,-75.4529034538119,
-215.283283));
#231448=CARTESIAN_POINT('Ctrl Pts',(34.975959941191,-75.4955232347256,-215.216616));
#231449=CARTESIAN_POINT('Ctrl Pts',(35.0240197565063,-75.5381430156392,
-215.149949));
#231450=CARTESIAN_POINT('Ctrl Pts',(24.4459324049493,-62.4902066935372,
-235.35005));
#231451=CARTESIAN_POINT('Ctrl Pts',(30.2944767260352,-66.7035224039813,
-228.68335));
#231452=CARTESIAN_POINT('Ctrl Pts',(36.1430210443405,-70.9168381145244,
-222.01665));
#231453=CARTESIAN_POINT('Ctrl Pts',(41.9915653606222,-75.1301538251473,
-215.34995));
#231454=CARTESIAN_POINT('Ctrl Pts',(42.050050803785,-75.1722869822535,-215.283283));
#231455=CARTESIAN_POINT('Ctrl Pts',(42.1085362469478,-75.2144201393598,
-215.216616));
#231456=CARTESIAN_POINT('Ctrl Pts',(42.1670216901106,-75.256553296466,-215.149949));
#231457=CARTESIAN_POINT('Origin',(0.,-12.9675000200281,-218.35005));
#231458=CARTESIAN_POINT('Ctrl Pts',(7312.83864083626,-22580.9607088348,
-376.75075701007));
#231459=CARTESIAN_POINT('Ctrl Pts',(6830.77747415825,-19700.0678309805,
-349.81728900813));
#231460=CARTESIAN_POINT('Ctrl Pts',(6348.71630748024,-16819.1749531262,
-322.88382100619));
#231461=CARTESIAN_POINT('Ctrl Pts',(5866.65514080223,-13938.2820752719,
-295.95035300425));
#231462=CARTESIAN_POINT('Ctrl Pts',(5625.62455746322,-12497.8356363448,
-282.483619003281));
#231463=CARTESIAN_POINT('Ctrl Pts',(5384.59397412422,-11057.3891974177,
-269.01688500231));
#231464=CARTESIAN_POINT('Ctrl Pts',(5143.56339078521,-9616.94275849054,
-255.55015100134));
#231465=CARTESIAN_POINT('Ctrl Pts',(5023.0480991157,-8896.71953902697,-248.816784000855));
#231466=CARTESIAN_POINT('Ctrl Pts',(4902.5328074462,-8176.49631956341,-242.083417000367));
#231467=CARTESIAN_POINT('Ctrl Pts',(4782.0175157767,-7456.27310009984,-235.350049999879));
#231468=CARTESIAN_POINT('Ctrl Pts',(4662.69544481679,-6743.18080360126,
-228.683349999394));
#231469=CARTESIAN_POINT('Ctrl Pts',(4544.55443977813,-6017.25926759624,
-222.01665));
#231470=CARTESIAN_POINT('Ctrl Pts',(4428.35272571124,-5278.63127980493,
-215.34995));
#231471=CARTESIAN_POINT('Ctrl Pts',(4427.19070857058,-5271.24499992702,
-215.283283));
#231472=CARTESIAN_POINT('Ctrl Pts',(4426.02869142993,-5263.85872004911,
-215.216616));
#231473=CARTESIAN_POINT('Ctrl Pts',(4424.86667428927,-5256.4724401712,-215.149949));
#231474=CARTESIAN_POINT('Ctrl Pts',(5678.44144856441,-17578.5062585325,
-376.75075700783));
#231475=CARTESIAN_POINT('Ctrl Pts',(5307.04370444825,-15333.6138629625,
-349.817289006321));
#231476=CARTESIAN_POINT('Ctrl Pts',(4935.64596033209,-13088.7214673926,
-322.883821004812));
#231477=CARTESIAN_POINT('Ctrl Pts',(4564.24821621593,-10843.8290718226,
-295.950353003305));
#231478=CARTESIAN_POINT('Ctrl Pts',(4378.54934415786,-9721.38287403765,
-282.48361900255));
#231479=CARTESIAN_POINT('Ctrl Pts',(4192.85047209977,-8598.93667625267,
-269.016885001796));
#231480=CARTESIAN_POINT('Ctrl Pts',(4007.1516000417,-7476.4904784677,-255.550151001042));
#231481=CARTESIAN_POINT('Ctrl Pts',(3914.30216401265,-6915.26737957521,
-248.816784000665));
#231482=CARTESIAN_POINT('Ctrl Pts',(3821.45272798362,-6354.04428068272,
-242.083417000286));
#231483=CARTESIAN_POINT('Ctrl Pts',(3728.60329195457,-5792.82118179023,
-235.350049999906));
#231484=CARTESIAN_POINT('Ctrl Pts',(3636.67315727236,-5237.15474724321,
-228.683349999529));
#231485=CARTESIAN_POINT('Ctrl Pts',(3545.66125393428,-4671.51484522691,
-222.01665));
#231486=CARTESIAN_POINT('Ctrl Pts',(3456.15702691661,-4095.9969311378,-215.34995));
#231487=CARTESIAN_POINT('Ctrl Pts',(3455.26198464644,-4090.24175199691,
-215.283283));
#231488=CARTESIAN_POINT('Ctrl Pts',(3454.36694237628,-4084.48657285602,
-215.216616));
#231489=CARTESIAN_POINT('Ctrl Pts',(3453.47190010611,-4078.73139371513,
-215.149949));
#231490=CARTESIAN_POINT('Ctrl Pts',(4044.04425629255,-12576.0518082303,
-376.750757005589));
#231491=CARTESIAN_POINT('Ctrl Pts',(3783.30993473824,-10967.1598949446,
-349.817289004512));
#231492=CARTESIAN_POINT('Ctrl Pts',(3522.57561318394,-9358.26798165898,
-322.883821003436));
#231493=CARTESIAN_POINT('Ctrl Pts',(3261.84129162964,-7749.37606837333,
-295.950353002358));
#231494=CARTESIAN_POINT('Ctrl Pts',(3131.47413085249,-6944.9301117305,-282.483619001821));
#231495=CARTESIAN_POINT('Ctrl Pts',(3001.10697007533,-6140.48415508768,
-269.016885001282));
#231496=CARTESIAN_POINT('Ctrl Pts',(2870.73980929818,-5336.03819844486,
-255.550151000744));
#231497=CARTESIAN_POINT('Ctrl Pts',(2805.5562289096,-4933.81522012345,-248.816784000475));
#231498=CARTESIAN_POINT('Ctrl Pts',(2740.37264852102,-4531.59224180204,
-242.083417000204));
#231499=CARTESIAN_POINT('Ctrl Pts',(2675.18906813245,-4129.36926348062,
-235.350049999933));
#231500=CARTESIAN_POINT('Ctrl Pts',(2610.65086972792,-3731.12869088517,
-228.683349999664));
#231501=CARTESIAN_POINT('Ctrl Pts',(2546.76806809043,-3325.77042285759,
-222.01665));
#231502=CARTESIAN_POINT('Ctrl Pts',(2483.96132812197,-2913.36258247067,
-215.34995));
#231503=CARTESIAN_POINT('Ctrl Pts',(2483.3332607223,-2909.2385040668,-215.283283));
#231504=CARTESIAN_POINT('Ctrl Pts',(2482.70519332262,-2905.11442566293,
-215.216616));
#231505=CARTESIAN_POINT('Ctrl Pts',(2482.07712592294,-2900.99034725906,
-215.149949));
#231506=CARTESIAN_POINT('Ctrl Pts',(2409.6470640207,-7573.59735792804,-376.750757003348));
#231507=CARTESIAN_POINT('Ctrl Pts',(2259.57616502824,-6600.7059269267,-349.817289002703));
#231508=CARTESIAN_POINT('Ctrl Pts',(2109.5052660358,-5627.81449592536,-322.883821002058));
#231509=CARTESIAN_POINT('Ctrl Pts',(1959.43436704334,-4654.92306492402,
-295.950353001413));
#231510=CARTESIAN_POINT('Ctrl Pts',(1884.39891754712,-4168.47734942335,
-282.483619001091));
#231511=CARTESIAN_POINT('Ctrl Pts',(1809.36346805089,-3682.03163392268,
-269.016885000768));
#231512=CARTESIAN_POINT('Ctrl Pts',(1734.32801855467,-3195.58591842202,
-255.550151000446));
#231513=CARTESIAN_POINT('Ctrl Pts',(1696.81029380655,-2952.36306067169,
-248.816784000284));
#231514=CARTESIAN_POINT('Ctrl Pts',(1659.29256905844,-2709.14020292135,
-242.083417000122));
#231515=CARTESIAN_POINT('Ctrl Pts',(1621.77484431033,-2465.91734517101,
-235.35004999996));
#231516=CARTESIAN_POINT('Ctrl Pts',(1584.62858218348,-2225.10263452712,
-228.683349999799));
#231517=CARTESIAN_POINT('Ctrl Pts',(1547.87488224658,-1980.02600048826,
-222.01665));
#231518=CARTESIAN_POINT('Ctrl Pts',(1511.76562932734,-1730.72823380353,
-215.34995));
#231519=CARTESIAN_POINT('Ctrl Pts',(1511.40453679815,-1728.23525613669,
-215.283283));
#231520=CARTESIAN_POINT('Ctrl Pts',(1511.04344426897,-1725.74227846985,
-215.216616));
#231521=CARTESIAN_POINT('Ctrl Pts',(1510.68235173978,-1723.249300803,-215.149949));
#231522=CARTESIAN_POINT('Ctrl Pts',(1864.84799993008,-5906.11254116062,
-376.750757002601));
#231523=CARTESIAN_POINT('Ctrl Pts',(1751.66490845825,-5145.22127092072,
-349.8172890021));
#231524=CARTESIAN_POINT('Ctrl Pts',(1638.48181698641,-4384.33000068082,
-322.883821001599));
#231525=CARTESIAN_POINT('Ctrl Pts',(1525.29872551458,-3623.43873044092,
-295.950353001097));
#231526=CARTESIAN_POINT('Ctrl Pts',(1468.70717977866,-3242.99309532097,
-282.483619000847));
#231527=CARTESIAN_POINT('Ctrl Pts',(1412.11563404274,-2862.54746020102,
-269.016885000597));
#231528=CARTESIAN_POINT('Ctrl Pts',(1355.52408830682,-2482.10182508107,
-255.550151000346));
#231529=CARTESIAN_POINT('Ctrl Pts',(1327.22831543887,-2291.87900752109,
-248.816784000221));
#231530=CARTESIAN_POINT('Ctrl Pts',(1298.93254257091,-2101.65618996112,
-242.083417000095));
#231531=CARTESIAN_POINT('Ctrl Pts',(1270.63676970295,-1911.43337240115,
-235.350049999969));
#231532=CARTESIAN_POINT('Ctrl Pts',(1242.621153002,-1723.09394907444,-228.683349999844));
#231533=CARTESIAN_POINT('Ctrl Pts',(1214.91048696529,-1531.44452636515,
-222.01665));
#231534=CARTESIAN_POINT('Ctrl Pts',(1187.70039639579,-1336.51678424783,
-215.34995));
#231535=CARTESIAN_POINT('Ctrl Pts',(1187.4282954901,-1334.56750682665,-215.283283));
#231536=CARTESIAN_POINT('Ctrl Pts',(1187.15619458441,-1332.61822940548,
-215.216616));
#231537=CARTESIAN_POINT('Ctrl Pts',(1186.88409367872,-1330.66895198431,
-215.149949));
#231538=CARTESIAN_POINT('Ctrl Pts',(1320.04893583946,-4238.62772439321,
-376.750757001854));
#231539=CARTESIAN_POINT('Ctrl Pts',(1243.75365188824,-3689.73661491475,
-349.817289001497));
#231540=CARTESIAN_POINT('Ctrl Pts',(1167.45836793703,-3140.84550543629,
-322.883821001139));
#231541=CARTESIAN_POINT('Ctrl Pts',(1091.16308398581,-2591.95439595782,
-295.950353000782));
#231542=CARTESIAN_POINT('Ctrl Pts',(1053.0154420102,-2317.50884121858,-282.483619000604));
#231543=CARTESIAN_POINT('Ctrl Pts',(1014.86780003459,-2043.06328647936,
-269.016885000425));
#231544=CARTESIAN_POINT('Ctrl Pts',(976.720158058986,-1768.61773174013,
-255.550151000247));
#231545=CARTESIAN_POINT('Ctrl Pts',(957.646337071182,-1631.39495437051,
-248.816784000158));
#231546=CARTESIAN_POINT('Ctrl Pts',(938.572516083378,-1494.17217700089,
-242.083417000068));
#231547=CARTESIAN_POINT('Ctrl Pts',(919.498695095574,-1356.94939963128,
-235.350049999978));
#231548=CARTESIAN_POINT('Ctrl Pts',(900.61372382052,-1221.08526362176,-228.683349999889));
#231549=CARTESIAN_POINT('Ctrl Pts',(881.946091684011,-1082.86305224204,
-222.01665));
#231550=CARTESIAN_POINT('Ctrl Pts',(863.635163464249,-942.305334692116,
-215.34995));
#231551=CARTESIAN_POINT('Ctrl Pts',(863.452054182054,-940.899757516616,
-215.283283));
#231552=CARTESIAN_POINT('Ctrl Pts',(863.268944899859,-939.494180341118,
-215.216616));
#231553=CARTESIAN_POINT('Ctrl Pts',(863.085835617665,-938.088603165619,
-215.149949));
#231554=CARTESIAN_POINT('Ctrl Pts',(775.24987174884,-2571.1429076258,-376.750757001107));
#231555=CARTESIAN_POINT('Ctrl Pts',(735.842395318242,-2234.25195890877,
-349.817289000894));
#231556=CARTESIAN_POINT('Ctrl Pts',(696.434918887644,-1897.36101019174,
-322.883821000681));
#231557=CARTESIAN_POINT('Ctrl Pts',(657.027442457046,-1560.47006147472,
-295.950353000467));
#231558=CARTESIAN_POINT('Ctrl Pts',(637.323704241746,-1392.0245871162,-282.483619000361));
#231559=CARTESIAN_POINT('Ctrl Pts',(617.619966026447,-1223.57911275769,
-269.016885000254));
#231560=CARTESIAN_POINT('Ctrl Pts',(597.916227811148,-1055.13363839918,
-255.550151000147));
#231561=CARTESIAN_POINT('Ctrl Pts',(588.064358703498,-970.910901219922,
-248.816784000094));
#231562=CARTESIAN_POINT('Ctrl Pts',(578.212489595849,-886.688164040665,
-242.083417000041));
#231563=CARTESIAN_POINT('Ctrl Pts',(568.360620488199,-802.465426861409,
-235.350049999987));
#231564=CARTESIAN_POINT('Ctrl Pts',(558.606294639041,-719.076578169076,
-228.683349999934));
#231565=CARTESIAN_POINT('Ctrl Pts',(548.981696402727,-634.281578118933,
-222.01665));
#231566=CARTESIAN_POINT('Ctrl Pts',(539.569930532705,-548.093885136405,
-215.34995));
#231567=CARTESIAN_POINT('Ctrl Pts',(539.475812874006,-547.23200820658,-215.283283));
#231568=CARTESIAN_POINT('Ctrl Pts',(539.381695215308,-546.370131276755,
-215.216616));
#231569=CARTESIAN_POINT('Ctrl Pts',(539.287577556609,-545.50825434693,-215.149949));
#231570=CARTESIAN_POINT('Ctrl Pts',(593.650183718634,-2015.31463536999,
-376.750757000858));
#231571=CARTESIAN_POINT('Ctrl Pts',(566.538643128242,-1749.09040690678,
-349.817289000693));
#231572=CARTESIAN_POINT('Ctrl Pts',(539.427102537849,-1482.86617844356,
-322.883821000528));
#231573=CARTESIAN_POINT('Ctrl Pts',(512.315561947457,-1216.64194998035,
-295.950353000362));
#231574=CARTESIAN_POINT('Ctrl Pts',(498.759791652261,-1083.52983574874,
-282.48361900028));
#231575=CARTESIAN_POINT('Ctrl Pts',(485.204021357065,-950.417721517136,
-269.016885000197));
#231576=CARTESIAN_POINT('Ctrl Pts',(471.648251061869,-817.305607285529,
-255.550151000114));
#231577=CARTESIAN_POINT('Ctrl Pts',(464.87036591427,-750.749550169726,-248.816784000073));
#231578=CARTESIAN_POINT('Ctrl Pts',(458.092480766672,-684.193493053923,
-242.083417000031));
#231579=CARTESIAN_POINT('Ctrl Pts',(451.314595619074,-617.637435938119,
-235.35004999999));
#231580=CARTESIAN_POINT('Ctrl Pts',(444.603818245215,-551.740349684848,
-228.683349999949));
#231581=CARTESIAN_POINT('Ctrl Pts',(437.993564642299,-484.754420077896,
-222.01665));
#231582=CARTESIAN_POINT('Ctrl Pts',(431.54818622219,-416.690068617835,-215.34995));
#231583=CARTESIAN_POINT('Ctrl Pts',(431.48373243799,-416.009425103234,-215.283283));
#231584=CARTESIAN_POINT('Ctrl Pts',(431.419278653791,-415.328781588633,
-215.216616));
#231585=CARTESIAN_POINT('Ctrl Pts',(431.354824869591,-414.648138074033,
-215.149949));
#231586=CARTESIAN_POINT('Ctrl Pts',(412.050495688428,-1459.48636311419,
-376.750757000609));
#231587=CARTESIAN_POINT('Ctrl Pts',(397.234890938242,-1263.92885490479,
-349.817289000492));
#231588=CARTESIAN_POINT('Ctrl Pts',(382.419286188055,-1068.37134669538,
-322.883821000374));
#231589=CARTESIAN_POINT('Ctrl Pts',(367.603681437869,-872.813838485983,
-295.950353000257));
#231590=CARTESIAN_POINT('Ctrl Pts',(360.195879062775,-775.035084381282,
-282.483619000199));
#231591=CARTESIAN_POINT('Ctrl Pts',(352.788076687683,-677.256330276581,
-269.016885000139));
#231592=CARTESIAN_POINT('Ctrl Pts',(345.380274312589,-579.477576171881,
-255.550151000081));
#231593=CARTESIAN_POINT('Ctrl Pts',(341.676373125042,-530.58819911953,-248.816784000052));
#231594=CARTESIAN_POINT('Ctrl Pts',(337.972471937496,-481.69882206718,-242.083417000022));
#231595=CARTESIAN_POINT('Ctrl Pts',(334.26857074995,-432.80944501483,-235.350049999993));
#231596=CARTESIAN_POINT('Ctrl Pts',(330.601341851388,-384.404121200621,
-228.683349999963));
#231597=CARTESIAN_POINT('Ctrl Pts',(327.005432881871,-335.22726203686,-222.01665));
#231598=CARTESIAN_POINT('Ctrl Pts',(323.526441911676,-285.286252099265,
-215.34995));
#231599=CARTESIAN_POINT('Ctrl Pts',(323.491652001974,-284.786841999889,
-215.283283));
#231600=CARTESIAN_POINT('Ctrl Pts',(323.456862092273,-284.287431900513,
-215.216616));
#231601=CARTESIAN_POINT('Ctrl Pts',(323.422072182572,-283.788021801137,
-215.149949));
#231602=CARTESIAN_POINT('Ctrl Pts',(230.450807658222,-903.658090858384,
-376.75075700036));
#231603=CARTESIAN_POINT('Ctrl Pts',(227.931138748241,-778.767302902795,
-349.817289000291));
#231604=CARTESIAN_POINT('Ctrl Pts',(225.411469838261,-653.876514947205,
-322.883821000222));
#231605=CARTESIAN_POINT('Ctrl Pts',(222.891800928281,-528.985726991616,
-295.950353000152));
#231606=CARTESIAN_POINT('Ctrl Pts',(221.63196647329,-466.540333013821,-282.483619000117));
#231607=CARTESIAN_POINT('Ctrl Pts',(220.3721320183,-404.094939036027,-269.016885000082));
#231608=CARTESIAN_POINT('Ctrl Pts',(219.11229756331,-341.649545058231,-255.550151000048));
#231609=CARTESIAN_POINT('Ctrl Pts',(218.482380335815,-310.426848069334,
-248.816784000031));
#231610=CARTESIAN_POINT('Ctrl Pts',(217.85246310832,-279.204151080437,-242.083417000013));
#231611=CARTESIAN_POINT('Ctrl Pts',(217.222545880824,-247.981454091539,
-235.350049999996));
#231612=CARTESIAN_POINT('Ctrl Pts',(216.598865457562,-217.067892716394,
-228.683349999979));
#231613=CARTESIAN_POINT('Ctrl Pts',(216.017301121443,-185.700103995824,
-222.01665));
#231614=CARTESIAN_POINT('Ctrl Pts',(215.504697601161,-153.882435580695,
-215.34995));
#231615=CARTESIAN_POINT('Ctrl Pts',(215.499571565958,-153.564258896543,
-215.283283));
#231616=CARTESIAN_POINT('Ctrl Pts',(215.494445530756,-153.246082212392,
-215.216616));
#231617=CARTESIAN_POINT('Ctrl Pts',(215.489319495554,-152.92790552824,-215.149949));
#231618=CARTESIAN_POINT('Ctrl Pts',(169.91757831482,-718.38200010645,-376.750757000277));
#231619=CARTESIAN_POINT('Ctrl Pts',(171.496554684908,-617.046785568798,
-349.817289000224));
#231620=CARTESIAN_POINT('Ctrl Pts',(173.075531054996,-515.711571031146,
-322.883821000171));
#231621=CARTESIAN_POINT('Ctrl Pts',(174.654507425084,-414.376356493494,
-295.950353000117));
#231622=CARTESIAN_POINT('Ctrl Pts',(175.443995610129,-363.708749224667,
-282.48361900009));
#231623=CARTESIAN_POINT('Ctrl Pts',(176.233483795173,-313.041141955842,
-269.016885000063));
#231624=CARTESIAN_POINT('Ctrl Pts',(177.022971980217,-262.373534687016,
-255.550151000037));
#231625=CARTESIAN_POINT('Ctrl Pts',(177.417716072739,-237.039731052603,
-248.816784000024));
#231626=CARTESIAN_POINT('Ctrl Pts',(177.812460165261,-211.70592741819,-242.08341700001));
#231627=CARTESIAN_POINT('Ctrl Pts',(178.207204257783,-186.372123783777,
-235.350049999997));
#231628=CARTESIAN_POINT('Ctrl Pts',(178.598039992953,-161.289149888318,
-228.683349999984));
#231629=CARTESIAN_POINT('Ctrl Pts',(179.021257201301,-135.857717982145,
-222.01665));
#231630=CARTESIAN_POINT('Ctrl Pts',(179.497449497656,-110.081163407838,
-215.34995));
#231631=CARTESIAN_POINT('Ctrl Pts',(179.50221142062,-109.823397862094,-215.283283));
#231632=CARTESIAN_POINT('Ctrl Pts',(179.506973343583,-109.565632316351,
-215.216616));
#231633=CARTESIAN_POINT('Ctrl Pts',(179.511735266547,-109.307866770608,
-215.149949));
#231634=CARTESIAN_POINT('Ctrl Pts',(109.384348971418,-533.105909354515,
-376.750757000194));
#231635=CARTESIAN_POINT('Ctrl Pts',(115.061970621574,-455.3262682348,-349.817289000156));
#231636=CARTESIAN_POINT('Ctrl Pts',(120.739592271731,-377.546627115086,
-322.883821000119));
#231637=CARTESIAN_POINT('Ctrl Pts',(126.417213921888,-299.766985995371,
-295.950353000081));
#231638=CARTESIAN_POINT('Ctrl Pts',(129.256024746967,-260.877165435514,
-282.483619000063));
#231639=CARTESIAN_POINT('Ctrl Pts',(132.094835572045,-221.987344875657,
-269.016885000044));
#231640=CARTESIAN_POINT('Ctrl Pts',(134.933646397123,-183.097524315799,
-255.550151000025));
#231641=CARTESIAN_POINT('Ctrl Pts',(136.353051809663,-163.652614035871,
-248.816784000016));
#231642=CARTESIAN_POINT('Ctrl Pts',(137.772457222202,-144.207703755942,
-242.083417000007));
#231643=CARTESIAN_POINT('Ctrl Pts',(139.191862634741,-124.762793476013,
-235.350049999998));
#231644=CARTESIAN_POINT('Ctrl Pts',(140.597214528344,-105.510407060242,
-228.683349999989));
#231645=CARTESIAN_POINT('Ctrl Pts',(142.025213281158,-86.0153319684663,
-222.01665));
#231646=CARTESIAN_POINT('Ctrl Pts',(143.490201394151,-66.2798912349809,
-215.34995));
#231647=CARTESIAN_POINT('Ctrl Pts',(143.504851275281,-66.082536827646,-215.283283));
#231648=CARTESIAN_POINT('Ctrl Pts',(143.519501156411,-65.8851824203112,
-215.216616));
#231649=CARTESIAN_POINT('Ctrl Pts',(143.534151037541,-65.6878280129763,
-215.149949));
#231650=CARTESIAN_POINT('Ctrl Pts',(48.8511196280154,-347.82981860258,-376.750757000109));
#231651=CARTESIAN_POINT('Ctrl Pts',(58.6273865582409,-293.605750900803,
-349.817289000088));
#231652=CARTESIAN_POINT('Ctrl Pts',(68.4036534884664,-239.381683199026,
-322.883821000067));
#231653=CARTESIAN_POINT('Ctrl Pts',(78.179920418692,-185.157615497249,-295.950353000046));
#231654=CARTESIAN_POINT('Ctrl Pts',(83.0680538838047,-158.04558164636,-282.483619000036));
#231655=CARTESIAN_POINT('Ctrl Pts',(87.9561873489175,-130.933547795471,
-269.016885000025));
#231656=CARTESIAN_POINT('Ctrl Pts',(92.8443208140303,-103.821513944583,
-255.550151000015));
#231657=CARTESIAN_POINT('Ctrl Pts',(95.2883875465867,-90.2654970191385,
-248.816784000009));
#231658=CARTESIAN_POINT('Ctrl Pts',(97.7324542791431,-76.7094800936942,
-242.083417000004));
#231659=CARTESIAN_POINT('Ctrl Pts',(100.176521011699,-63.1534631682499,
-235.350049999999));
#231660=CARTESIAN_POINT('Ctrl Pts',(102.596389063735,-49.7316642321664,
-228.683349999994));
#231661=CARTESIAN_POINT('Ctrl Pts',(105.029169361015,-36.1729459547875,
-222.01665));
#231662=CARTESIAN_POINT('Ctrl Pts',(107.482953290646,-22.4786190621241,
-215.34995));
#231663=CARTESIAN_POINT('Ctrl Pts',(107.507491129942,-22.3416757931975,
-215.283283));
#231664=CARTESIAN_POINT('Ctrl Pts',(107.532028969239,-22.2047325242709,
-215.216616));
#231665=CARTESIAN_POINT('Ctrl Pts',(107.556566808535,-22.0677892553443,
-215.149949));
#231666=CARTESIAN_POINT('Ctrl Pts',(28.673376513548,-286.071121685269,-376.750757000082));
#231667=CARTESIAN_POINT('Ctrl Pts',(39.8158585371298,-239.698911789471,
-349.817289000066));
#231668=CARTESIAN_POINT('Ctrl Pts',(50.9583405607115,-193.326701893672,
-322.88382100005));
#231669=CARTESIAN_POINT('Ctrl Pts',(62.1008225842933,-146.954491997874,
-295.950353000034));
#231670=CARTESIAN_POINT('Ctrl Pts',(67.6720635960841,-123.768387049975,
-282.483619000027));
#231671=CARTESIAN_POINT('Ctrl Pts',(73.243304607875,-100.582282102076,-269.016885000018));
#231672=CARTESIAN_POINT('Ctrl Pts',(78.8145456196659,-77.3961771541774,
-255.550151000011));
#231673=CARTESIAN_POINT('Ctrl Pts',(81.6001661255613,-65.8031246802278,
-248.816784000007));
#231674=CARTESIAN_POINT('Ctrl Pts',(84.3857866314568,-54.2100722062783,
-242.083417000003));
#231675=CARTESIAN_POINT('Ctrl Pts',(87.1714071373522,-42.6170197323288,
-235.350049999999));
#231676=CARTESIAN_POINT('Ctrl Pts',(89.9294472421992,-31.1387499561412,
-228.683349999995));
#231677=CARTESIAN_POINT('Ctrl Pts',(92.6971547209677,-19.5588172835613,
-222.01665));
#231678=CARTESIAN_POINT('Ctrl Pts',(95.4805372561441,-7.8781950045052,-215.34995));
#231679=CARTESIAN_POINT('Ctrl Pts',(95.508371081496,-7.76138878171465,-215.283283));
#231680=CARTESIAN_POINT('Ctrl Pts',(95.5362049068479,-7.64458255892409,
-215.216616));
#231681=CARTESIAN_POINT('Ctrl Pts',(95.5640387321998,-7.52777633613354,
-215.149949));
#231682=CARTESIAN_POINT('Ctrl Pts',(8.49563339908065,-224.312424767957,
-376.750757000054));
#231683=CARTESIAN_POINT('Ctrl Pts',(21.0043305160186,-185.792072678138,
-349.817289000044));
#231684=CARTESIAN_POINT('Ctrl Pts',(33.5130276329566,-147.271720588319,
-322.883821000033));
#231685=CARTESIAN_POINT('Ctrl Pts',(46.0217247498946,-108.7513684985,-295.950353000022));
#231686=CARTESIAN_POINT('Ctrl Pts',(52.2760733083635,-89.4911924535907,
-282.483619000017));
#231687=CARTESIAN_POINT('Ctrl Pts',(58.5304218668325,-70.2310164086813,
-269.016885000012));
#231688=CARTESIAN_POINT('Ctrl Pts',(64.7847704253015,-50.9708403637719,
-255.550151000007));
#231689=CARTESIAN_POINT('Ctrl Pts',(67.911944704536,-41.3407523413171,-248.816784000005));
#231690=CARTESIAN_POINT('Ctrl Pts',(71.0391189837705,-31.7106643188625,
-242.083417000002));
#231691=CARTESIAN_POINT('Ctrl Pts',(74.166293263005,-22.0805762964077,-235.35005));
#231692=CARTESIAN_POINT('Ctrl Pts',(77.2625054206629,-12.5458356801159,
-228.683349999997));
#231693=CARTESIAN_POINT('Ctrl Pts',(80.3651400809202,-2.94468861233498,
-222.01665));
#231694=CARTESIAN_POINT('Ctrl Pts',(83.4781212216425,6.72222905311371,-215.34995));
#231695=CARTESIAN_POINT('Ctrl Pts',(83.5092510330498,6.81889822976819,-215.283283));
#231696=CARTESIAN_POINT('Ctrl Pts',(83.5403808444571,6.91556740642268,-215.216616));
#231697=CARTESIAN_POINT('Ctrl Pts',(83.5715106558644,7.01223658307716,-215.149949));
#231698=CARTESIAN_POINT('Ctrl Pts',(-11.6821097153867,-162.553727850645,
-376.750757000025));
#231699=CARTESIAN_POINT('Ctrl Pts',(2.1928024949075,-131.885233566805,-349.81728900002));
#231700=CARTESIAN_POINT('Ctrl Pts',(16.0677147052017,-101.216739282966,
-322.883821000016));
#231701=CARTESIAN_POINT('Ctrl Pts',(29.9426269154959,-70.548244999126,-295.95035300001));
#231702=CARTESIAN_POINT('Ctrl Pts',(36.880083020643,-55.2139978572062,-282.483619000008));
#231703=CARTESIAN_POINT('Ctrl Pts',(43.81753912579,-39.8797507152863,-269.016885000005));
#231704=CARTESIAN_POINT('Ctrl Pts',(50.7549952309371,-24.5455035733664,
-255.550151000003));
#231705=CARTESIAN_POINT('Ctrl Pts',(54.2237232835107,-16.8783800024065,
-248.816784000002));
#231706=CARTESIAN_POINT('Ctrl Pts',(57.6924513360842,-9.21125643144658,
-242.083417000001));
#231707=CARTESIAN_POINT('Ctrl Pts',(61.1611793886578,-1.54413286048666,
-235.35005));
#231708=CARTESIAN_POINT('Ctrl Pts',(64.5955635991267,6.04707859590932,-228.683349999999));
#231709=CARTESIAN_POINT('Ctrl Pts',(68.0331254408726,13.6694400588913,-222.01665));
#231710=CARTESIAN_POINT('Ctrl Pts',(71.4757051871408,21.3226531107326,-215.34995));
#231711=CARTESIAN_POINT('Ctrl Pts',(71.5101309846035,21.3991852412511,-215.283283));
#231712=CARTESIAN_POINT('Ctrl Pts',(71.5445567820663,21.4757173717695,-215.216616));
#231713=CARTESIAN_POINT('Ctrl Pts',(71.578982579529,21.5522495022879,-215.149949));
#231714=CARTESIAN_POINT('Ctrl Pts',(-18.4080240868758,-141.967495544875,
-376.750757000016));
#231715=CARTESIAN_POINT('Ctrl Pts',(-4.07770684546288,-113.916287196361,
-349.817289000013));
#231716=CARTESIAN_POINT('Ctrl Pts',(10.25261039595,-85.865078847848,-322.88382100001));
#231717=CARTESIAN_POINT('Ctrl Pts',(24.582927637363,-57.8138704993346,-295.950353000006));
#231718=CARTESIAN_POINT('Ctrl Pts',(31.7480862580694,-43.7882663250779,
-282.483619000005));
#231719=CARTESIAN_POINT('Ctrl Pts',(38.9132448787759,-29.7626621508213,
-269.016885000003));
#231720=CARTESIAN_POINT('Ctrl Pts',(46.0784034994824,-15.7370579765646,
-255.550151000002));
#231721=CARTESIAN_POINT('Ctrl Pts',(49.6609828098356,-8.72425588943629,
-248.816784000002));
#231722=CARTESIAN_POINT('Ctrl Pts',(53.2435621201888,-1.71145380230796,
-242.083417000001));
#231723=CARTESIAN_POINT('Ctrl Pts',(56.826141430542,5.30134828482038,-235.35005));
#231724=CARTESIAN_POINT('Ctrl Pts',(60.3732496586146,12.2447166879177,-228.683349999999));
#231725=CARTESIAN_POINT('Ctrl Pts',(63.9224538941901,19.2074829493001,-222.01665));
#231726=CARTESIAN_POINT('Ctrl Pts',(67.4748998423069,26.1894611299389,-215.34995));
#231727=CARTESIAN_POINT('Ctrl Pts',(67.5104243017881,26.2592809117453,-215.283283));
#231728=CARTESIAN_POINT('Ctrl Pts',(67.5459487612693,26.3291006935517,-215.216616));
#231729=CARTESIAN_POINT('Ctrl Pts',(67.5814732207505,26.3989204753581,-215.149949));
#231730=CARTESIAN_POINT('Ctrl Pts',(-25.1339384583649,-121.381263239104,
-376.750757000007));
#231731=CARTESIAN_POINT('Ctrl Pts',(-10.3482161858333,-95.9473408259171,
-349.817289000005));
#231732=CARTESIAN_POINT('Ctrl Pts',(4.4375060866984,-70.5134184127302,-322.883821000004));
#231733=CARTESIAN_POINT('Ctrl Pts',(19.22322835923,-45.0794959995432,-295.950353000003));
#231734=CARTESIAN_POINT('Ctrl Pts',(26.6160894954959,-32.3625347929498,
-282.483619000002));
#231735=CARTESIAN_POINT('Ctrl Pts',(34.0089506317617,-19.6455735863562,
-269.016885000001));
#231736=CARTESIAN_POINT('Ctrl Pts',(41.4018117680275,-6.9286123797628,-255.550151000001));
#231737=CARTESIAN_POINT('Ctrl Pts',(45.0982423361605,-0.570131776466063,
-248.816784000001));
#231738=CARTESIAN_POINT('Ctrl Pts',(48.7946729042934,5.78834882683067,-242.083417));
#231739=CARTESIAN_POINT('Ctrl Pts',(52.4911034724263,12.1468294301274,-235.35005));
#231740=CARTESIAN_POINT('Ctrl Pts',(56.1509357181025,18.4423547799261,-228.68335));
#231741=CARTESIAN_POINT('Ctrl Pts',(59.8117823475076,24.7455258397088,-222.01665));
#231742=CARTESIAN_POINT('Ctrl Pts',(63.4740944974731,31.0562691491453,-215.34995));
#231743=CARTESIAN_POINT('Ctrl Pts',(63.5107176189727,31.1193765822396,-215.283283));
#231744=CARTESIAN_POINT('Ctrl Pts',(63.5473407404724,31.1824840153339,-215.216616));
#231745=CARTESIAN_POINT('Ctrl Pts',(63.5839638619721,31.2455914484283,-215.149949));
#231746=CARTESIAN_POINT('Ctrl Pts',(-31.859852829854,-100.795030933333,
-376.750756999998));
#231747=CARTESIAN_POINT('Ctrl Pts',(-16.6187255262036,-77.9783944554729,
-349.817288999998));
#231748=CARTESIAN_POINT('Ctrl Pts',(-1.37759822255324,-55.1617579776124,
-322.883820999999));
#231749=CARTESIAN_POINT('Ctrl Pts',(13.8635290810972,-32.3451214997519,
-295.950352999999));
#231750=CARTESIAN_POINT('Ctrl Pts',(21.4840927329223,-20.9368032608216,
-282.483618999999));
#231751=CARTESIAN_POINT('Ctrl Pts',(29.1046563847475,-9.52848502189127,
-269.016885));
#231752=CARTESIAN_POINT('Ctrl Pts',(36.7252200365728,1.87983321703902,-255.550151));
#231753=CARTESIAN_POINT('Ctrl Pts',(40.5355018624854,7.58399233650416,-248.816784));
#231754=CARTESIAN_POINT('Ctrl Pts',(44.345783688398,13.2881514559693,-242.083417));
#231755=CARTESIAN_POINT('Ctrl Pts',(48.1560655143106,18.9923105754345,-235.35005));
#231756=CARTESIAN_POINT('Ctrl Pts',(51.9286217775904,24.6399928719346,-228.68335));
#231757=CARTESIAN_POINT('Ctrl Pts',(55.7011108008251,30.2835687301176,-222.01665));
#231758=CARTESIAN_POINT('Ctrl Pts',(59.4732891526392,35.9230771683515,-215.34995));
#231759=CARTESIAN_POINT('Ctrl Pts',(59.5110109361573,35.9794722527339,-215.283283));
#231760=CARTESIAN_POINT('Ctrl Pts',(59.5487327196755,36.0358673371162,-215.216616));
#231761=CARTESIAN_POINT('Ctrl Pts',(59.5864545031936,36.0922624214986,-215.149949));
#231762=CARTESIAN_POINT('Ctrl Pts',(-33.5413314227263,-95.6484728568909,
-376.750756999995));
#231763=CARTESIAN_POINT('Ctrl Pts',(-18.1863528612963,-73.4861578628619,
-349.817288999997));
#231764=CARTESIAN_POINT('Ctrl Pts',(-2.83137429986615,-51.3238428688329,
-322.883820999997));
#231765=CARTESIAN_POINT('Ctrl Pts',(12.5236042615639,-29.161527874804,-295.950352999998));
#231766=CARTESIAN_POINT('Ctrl Pts',(20.201093542279,-18.0803703777895,-282.483618999998));
#231767=CARTESIAN_POINT('Ctrl Pts',(27.878582822994,-6.99921288077501,-269.016884999999));
#231768=CARTESIAN_POINT('Ctrl Pts',(35.556072103709,4.08194461623947,-255.550151));
#231769=CARTESIAN_POINT('Ctrl Pts',(39.3948167440666,9.62252336474671,-248.816784));
#231770=CARTESIAN_POINT('Ctrl Pts',(43.2335613844241,15.163102113254,-242.083417));
#231771=CARTESIAN_POINT('Ctrl Pts',(47.0723060247816,20.7036808617612,-235.35005));
#231772=CARTESIAN_POINT('Ctrl Pts',(50.8730432924624,26.1894023949367,-228.683350000001));
#231773=CARTESIAN_POINT('Ctrl Pts',(54.6734429141545,31.6680794527198,-222.01665));
#231774=CARTESIAN_POINT('Ctrl Pts',(58.4730878164307,37.1397791731531,-215.34995));
#231775=CARTESIAN_POINT('Ctrl Pts',(58.5110842654535,37.1944961703575,-215.283283));
#231776=CARTESIAN_POINT('Ctrl Pts',(58.5490807144762,37.2492131675618,-215.216616));
#231777=CARTESIAN_POINT('Ctrl Pts',(58.587077163499,37.3039301647661,-215.149949));
#231778=CARTESIAN_POINT('Ctrl Pts',(-41.2301579830855,-81.5182387771612,
-376.750756999989));
#231779=CARTESIAN_POINT('Ctrl Pts',(-24.8836555508694,-61.3775485896441,
-349.817288999991));
#231780=CARTESIAN_POINT('Ctrl Pts',(-8.53715311865333,-41.2368584021269,
-322.883820999993));
#231781=CARTESIAN_POINT('Ctrl Pts',(7.80934931356275,-21.0961682146096,
-295.950352999996));
#231782=CARTESIAN_POINT('Ctrl Pts',(15.9826005296708,-11.025823120851,-282.483618999996));
#231783=CARTESIAN_POINT('Ctrl Pts',(24.1558517457789,-0.955478027092413,
-269.016884999998));
#231784=CARTESIAN_POINT('Ctrl Pts',(32.3291029618869,9.1148670666662,-255.550150999998));
#231785=CARTESIAN_POINT('Ctrl Pts',(36.4157285699409,14.1500396135455,-248.816783999999));
#231786=CARTESIAN_POINT('Ctrl Pts',(40.5023541779949,19.1852121604248,-242.083416999999));
#231787=CARTESIAN_POINT('Ctrl Pts',(44.588979786049,24.2203847073041,-235.35005));
#231788=CARTESIAN_POINT('Ctrl Pts',(48.6351437544193,29.2057040606499,-228.683350000001));
#231789=CARTESIAN_POINT('Ctrl Pts',(52.6799616741893,34.1756765917424,-222.01665));
#231790=CARTESIAN_POINT('Ctrl Pts',(56.7225263698862,39.1304491224114,-215.34995));
#231791=CARTESIAN_POINT('Ctrl Pts',(56.7629520168432,39.1799968477181,-215.283283));
#231792=CARTESIAN_POINT('Ctrl Pts',(56.8033776638002,39.2295445730248,-215.216616));
#231793=CARTESIAN_POINT('Ctrl Pts',(56.8438033107571,39.2790922983315,-215.149949));
#231794=CARTESIAN_POINT('Ctrl Pts',(-61.5202391452974,-58.1759617860395,
-376.750756999982));
#231795=CARTESIAN_POINT('Ctrl Pts',(-42.2054487986876,-41.4892341751692,
-349.817288999985));
#231796=CARTESIAN_POINT('Ctrl Pts',(-22.8906584520777,-24.8025065642989,
-322.883820999989));
#231797=CARTESIAN_POINT('Ctrl Pts',(-3.5758681054679,-8.11577895342853,
-295.950352999993));
#231798=CARTESIAN_POINT('Ctrl Pts',(6.08152706783702,0.227584852006628,
-282.483618999994));
#231799=CARTESIAN_POINT('Ctrl Pts',(15.738922241142,8.57094865744179,-269.016884999996));
#231800=CARTESIAN_POINT('Ctrl Pts',(25.3963174144469,16.9143124628769,-255.550150999997));
#231801=CARTESIAN_POINT('Ctrl Pts',(30.2250150010993,21.0859943655945,-248.816783999999));
#231802=CARTESIAN_POINT('Ctrl Pts',(35.0537125877518,25.2576762683121,-242.083416999999));
#231803=CARTESIAN_POINT('Ctrl Pts',(39.8824101744042,29.4293581710297,-235.35005));
#231804=CARTESIAN_POINT('Ctrl Pts',(44.6632988740601,33.5597362925323,-228.683350000001));
#231805=CARTESIAN_POINT('Ctrl Pts',(49.4410603210161,37.6624224459266,-222.01665));
#231806=CARTESIAN_POINT('Ctrl Pts',(54.214059251162,41.7376821955923,-215.34995));
#231807=CARTESIAN_POINT('Ctrl Pts',(54.2617892404634,41.778434793089,-215.283283));
#231808=CARTESIAN_POINT('Ctrl Pts',(54.3095192297649,41.8191873905857,-215.216616));
#231809=CARTESIAN_POINT('Ctrl Pts',(54.3572492190663,41.8599399880823,-215.149949));
#231810=CARTESIAN_POINT('Ctrl Pts',(-86.4308715045652,-38.5465561709931,
-376.75075699998));
#231811=CARTESIAN_POINT('Ctrl Pts',(-63.394599877538,-24.7210691437011,
-349.817288999984));
#231812=CARTESIAN_POINT('Ctrl Pts',(-40.3583282505107,-10.8955821164091,
-322.883820999988));
#231813=CARTESIAN_POINT('Ctrl Pts',(-17.3220566234834,2.92990491088294,
-295.950352999991));
#231814=CARTESIAN_POINT('Ctrl Pts',(-5.80392080996978,9.84264842452895,
-282.483618999993));
#231815=CARTESIAN_POINT('Ctrl Pts',(5.71421500354386,16.755391938175,-269.016884999996));
#231816=CARTESIAN_POINT('Ctrl Pts',(17.2323508170575,23.668135451821,-255.550150999997));
#231817=CARTESIAN_POINT('Ctrl Pts',(22.9914187238143,27.1245072086439,-248.816783999998));
#231818=CARTESIAN_POINT('Ctrl Pts',(28.7504866305711,30.580878965467,-242.083416999999));
#231819=CARTESIAN_POINT('Ctrl Pts',(34.509554537328,34.03725072229,-235.35005));
#231820=CARTESIAN_POINT('Ctrl Pts',(40.2116019697604,37.4594009765702,-228.683350000001));
#231821=CARTESIAN_POINT('Ctrl Pts',(45.9096065172025,40.8490096838924,-222.01665));
#231822=CARTESIAN_POINT('Ctrl Pts',(51.6016474095961,44.2063892516083,-215.34995));
#231823=CARTESIAN_POINT('Ctrl Pts',(51.65856781852,44.2399630472854,-215.283283));
#231824=CARTESIAN_POINT('Ctrl Pts',(51.715488227444,44.2735368429626,-215.216616));
#231825=CARTESIAN_POINT('Ctrl Pts',(51.7724086363679,44.3071106386397,-215.149949));
#231826=CARTESIAN_POINT('Ctrl Pts',(-101.966904434915,-30.8346247983327,
-376.750756999984));
#231827=CARTESIAN_POINT('Ctrl Pts',(-76.6679969066201,-18.0147641121609,
-349.817288999987));
#231828=CARTESIAN_POINT('Ctrl Pts',(-51.3690893783256,-5.19490342598898,
-322.88382099999));
#231829=CARTESIAN_POINT('Ctrl Pts',(-26.070181850031,7.62495726018286,-295.950352999994));
#231830=CARTESIAN_POINT('Ctrl Pts',(-13.4207280858838,14.0348876032688,
-282.483618999995));
#231831=CARTESIAN_POINT('Ctrl Pts',(-0.771274321736487,20.4448179463547,
-269.016884999996));
#231832=CARTESIAN_POINT('Ctrl Pts',(11.8781794424108,26.8547482894406,-255.550150999998));
#231833=CARTESIAN_POINT('Ctrl Pts',(18.2029063244844,30.0597134609836,-248.816783999999));
#231834=CARTESIAN_POINT('Ctrl Pts',(24.5276332065581,33.2646786325266,-242.083416999999));
#231835=CARTESIAN_POINT('Ctrl Pts',(30.8523600886317,36.4696438040695,-235.35005));
#231836=CARTESIAN_POINT('Ctrl Pts',(37.1144659124669,39.6428766471814,-228.683350000001));
#231837=CARTESIAN_POINT('Ctrl Pts',(43.3732515923186,42.7902567304839,-222.01665));
#231838=CARTESIAN_POINT('Ctrl Pts',(49.6271914214616,45.9120323459617,-215.34995));
#231839=CARTESIAN_POINT('Ctrl Pts',(49.6897308197531,45.9432501021165,-215.283283));
#231840=CARTESIAN_POINT('Ctrl Pts',(49.7522702180445,45.9744678582713,-215.216616));
#231841=CARTESIAN_POINT('Ctrl Pts',(49.8148096163359,46.005685614426,-215.149949));
#231842=CARTESIAN_POINT('Ctrl Pts',(-107.993804890233,-28.9044482397935,
-376.750756999988));
#231843=CARTESIAN_POINT('Ctrl Pts',(-81.8862252383193,-16.2510537069498,
-349.81728899999));
#231844=CARTESIAN_POINT('Ctrl Pts',(-55.7786455864053,-3.5976591741061,
-322.883820999992));
#231845=CARTESIAN_POINT('Ctrl Pts',(-29.6710659344913,9.05573535873763,
-295.950352999994));
#231846=CARTESIAN_POINT('Ctrl Pts',(-16.6172761085343,15.3824326251595,
-282.483618999996));
#231847=CARTESIAN_POINT('Ctrl Pts',(-3.5634862825773,21.7091298915814,-269.016884999997));
#231848=CARTESIAN_POINT('Ctrl Pts',(9.49030354337971,28.0358271580032,-255.550150999998));
#231849=CARTESIAN_POINT('Ctrl Pts',(16.0171984563582,31.1991757912142,-248.816783999999));
#231850=CARTESIAN_POINT('Ctrl Pts',(22.5440933693367,34.3625244244251,-242.083416999999));
#231851=CARTESIAN_POINT('Ctrl Pts',(29.0709882823152,37.525873057636,-235.35005));
#231852=CARTESIAN_POINT('Ctrl Pts',(35.5332604733831,40.6579014073498,-228.683350000001));
#231853=CARTESIAN_POINT('Ctrl Pts',(41.9930962102693,43.771133049519,-222.01665));
#231854=CARTESIAN_POINT('Ctrl Pts',(48.4493862544499,46.8657485296993,-215.34995));
#231855=CARTESIAN_POINT('Ctrl Pts',(48.5139491548917,46.8966946845011,-215.283283));
#231856=CARTESIAN_POINT('Ctrl Pts',(48.5785120553335,46.9276408393029,-215.216616));
#231857=CARTESIAN_POINT('Ctrl Pts',(48.6430749557753,46.9585869941047,-215.149949));
#231858=CARTESIAN_POINT('Ctrl Pts',(-132.101406711508,-21.1837420056372,
-376.750756999997));
#231859=CARTESIAN_POINT('Ctrl Pts',(-102.759138565116,-9.1962120861059,
-349.817288999997));
#231860=CARTESIAN_POINT('Ctrl Pts',(-73.4168704187245,2.79131783342537,
-322.883820999998));
#231861=CARTESIAN_POINT('Ctrl Pts',(-44.0746022723325,14.7788477529567,
-295.950352999998));
#231862=CARTESIAN_POINT('Ctrl Pts',(-29.4034681991366,20.7726127127223,
-282.483618999999));
#231863=CARTESIAN_POINT('Ctrl Pts',(-14.7323341259406,26.766377672488,-269.016884999999));
#231864=CARTESIAN_POINT('Ctrl Pts',(-0.0612000527446133,32.7601426322536,
-255.550151));
#231865=CARTESIAN_POINT('Ctrl Pts',(7.27436698385337,35.7570251121364,-248.816784));
#231866=CARTESIAN_POINT('Ctrl Pts',(14.6099340204513,38.7539075920192,-242.083417));
#231867=CARTESIAN_POINT('Ctrl Pts',(21.9455010570494,41.7507900719021,-235.35005));
#231868=CARTESIAN_POINT('Ctrl Pts',(29.2084387170473,44.7180004480236,-228.68335));
#231869=CARTESIAN_POINT('Ctrl Pts',(36.4724746820719,47.694638325659,-222.016650000001));
#231870=CARTESIAN_POINT('Ctrl Pts',(43.7381655864028,50.6806132646498,-215.34995));
#231871=CARTESIAN_POINT('Ctrl Pts',(43.810822495446,50.7104730140397,-215.283283));
#231872=CARTESIAN_POINT('Ctrl Pts',(43.8834794044894,50.7403327634296,-215.216616));
#231873=CARTESIAN_POINT('Ctrl Pts',(43.9561363135327,50.7701925128195,-215.149949));
#231874=CARTESIAN_POINT('Ctrl Pts',(-156.209008532784,-13.4630357714808,
-376.750757000006));
#231875=CARTESIAN_POINT('Ctrl Pts',(-123.632051891913,-2.14137046526198,
-349.817289000005));
#231876=CARTESIAN_POINT('Ctrl Pts',(-91.0550952510435,9.18029484095685,
-322.883821000004));
#231877=CARTESIAN_POINT('Ctrl Pts',(-58.4781386101737,20.5019601471757,
-295.950353000003));
#231878=CARTESIAN_POINT('Ctrl Pts',(-42.1896602897388,26.1627928002851,
-282.483619000002));
#231879=CARTESIAN_POINT('Ctrl Pts',(-25.9011819693039,31.8236254533946,
-269.016885000001));
#231880=CARTESIAN_POINT('Ctrl Pts',(-9.61270364886893,37.484458106504,-255.550151000001));
#231881=CARTESIAN_POINT('Ctrl Pts',(-1.46846448865147,40.3148744330587,
-248.816784000001));
#231882=CARTESIAN_POINT('Ctrl Pts',(6.67577467156599,43.1452907596133,-242.083417));
#231883=CARTESIAN_POINT('Ctrl Pts',(14.8200138317834,45.9757070861681,-235.35005));
#231884=CARTESIAN_POINT('Ctrl Pts',(22.8836169607117,48.7780994886975,-228.68335));
#231885=CARTESIAN_POINT('Ctrl Pts',(30.9518531538746,51.6181436017991,-222.016650000001));
#231886=CARTESIAN_POINT('Ctrl Pts',(39.0269449183556,54.4954779996004,-215.349950000001));
#231887=CARTESIAN_POINT('Ctrl Pts',(39.1076958360005,54.5242513435783,-215.283283000001));
#231888=CARTESIAN_POINT('Ctrl Pts',(39.1884467536454,54.5530246875563,-215.216616));
#231889=CARTESIAN_POINT('Ctrl Pts',(39.2691976712902,54.5817980315343,-215.149949000001));
#231890=CARTESIAN_POINT('Ctrl Pts',(-180.316610354058,-5.74232953732446,
-376.750757000015));
#231891=CARTESIAN_POINT('Ctrl Pts',(-144.50496521871,4.91347115558193,-349.817289000013));
#231892=CARTESIAN_POINT('Ctrl Pts',(-108.693320083363,15.5692718484884,
-322.88382100001));
#231893=CARTESIAN_POINT('Ctrl Pts',(-72.8816749480149,26.2250725413947,
-295.950353000006));
#231894=CARTESIAN_POINT('Ctrl Pts',(-54.975852380341,31.5529728878479,-282.483619000005));
#231895=CARTESIAN_POINT('Ctrl Pts',(-37.0700298126672,36.8808732343011,
-269.016885000003));
#231896=CARTESIAN_POINT('Ctrl Pts',(-19.1642072449932,42.2087735807543,
-255.550151000002));
#231897=CARTESIAN_POINT('Ctrl Pts',(-10.2112959611563,44.8727237539809,
-248.816784000002));
#231898=CARTESIAN_POINT('Ctrl Pts',(-1.25838467731937,47.5366739272075,
-242.083417000001));
#231899=CARTESIAN_POINT('Ctrl Pts',(7.69452660651757,50.2006241004341,-235.35005));
#231900=CARTESIAN_POINT('Ctrl Pts',(16.558795204376,52.8381985293713,-228.68335));
#231901=CARTESIAN_POINT('Ctrl Pts',(25.4312316256772,55.5416488779391,-222.016650000001));
#231902=CARTESIAN_POINT('Ctrl Pts',(34.3157242503085,58.3103427345509,-215.349950000001));
#231903=CARTESIAN_POINT('Ctrl Pts',(34.4045691765549,58.3380296731169,-215.283283000001));
#231904=CARTESIAN_POINT('Ctrl Pts',(34.4934141028013,58.365716611683,-215.216616));
#231905=CARTESIAN_POINT('Ctrl Pts',(34.5822590290476,58.3934035502491,-215.149949000001));
#231906=CARTESIAN_POINT('Ctrl Pts',(-252.639415817883,17.4197891651448,
-376.750757000044));
#231907=CARTESIAN_POINT('Ctrl Pts',(-207.123705199102,26.0779960181138,
-349.817289000036));
#231908=CARTESIAN_POINT('Ctrl Pts',(-161.60799458032,34.7362028710828,-322.883821000027));
#231909=CARTESIAN_POINT('Ctrl Pts',(-116.092283961538,43.3944097240518,
-295.950353000018));
#231910=CARTESIAN_POINT('Ctrl Pts',(-93.3344286521477,47.7235131505364,
-282.483619000015));
#231911=CARTESIAN_POINT('Ctrl Pts',(-70.576573342757,52.0526165770209,-269.01688500001));
#231912=CARTESIAN_POINT('Ctrl Pts',(-47.8187180333662,56.3817200035054,
-255.550151000006));
#231913=CARTESIAN_POINT('Ctrl Pts',(-36.4397903786708,58.5462717167477,
-248.816784000004));
#231914=CARTESIAN_POINT('Ctrl Pts',(-25.0608627239755,60.7108234299899,
-242.083417000002));
#231915=CARTESIAN_POINT('Ctrl Pts',(-13.6819350692801,62.8753751432322,
-235.35005));
#231916=CARTESIAN_POINT('Ctrl Pts',(-2.41567006463117,65.0184956513928,
-228.683349999998));
#231917=CARTESIAN_POINT('Ctrl Pts',(8.86936704108513,67.3121647063593,-222.016650000002));
#231918=CARTESIAN_POINT('Ctrl Pts',(20.1820622461672,69.7549369394024,-215.349950000001));
#231919=CARTESIAN_POINT('Ctrl Pts',(20.2951891982182,69.7793646617328,-215.283283000001));
#231920=CARTESIAN_POINT('Ctrl Pts',(20.4083161502691,69.8037923840631,-215.216616));
#231921=CARTESIAN_POINT('Ctrl Pts',(20.5214431023201,69.8282201063935,-215.149949000001));
#231922=CARTESIAN_POINT('Ctrl Pts',(-324.962221281708,40.581907867614,-376.750757000072));
#231923=CARTESIAN_POINT('Ctrl Pts',(-269.742445179492,47.2425208806457,
-349.817289000059));
#231924=CARTESIAN_POINT('Ctrl Pts',(-214.522669077277,53.9031338936774,
-322.883821000045));
#231925=CARTESIAN_POINT('Ctrl Pts',(-159.302892975062,60.563746906709,-295.950353000031));
#231926=CARTESIAN_POINT('Ctrl Pts',(-131.693004923954,63.8940534132249,
-282.483619000024));
#231927=CARTESIAN_POINT('Ctrl Pts',(-104.083116872847,67.2243599197407,
-269.016885000017));
#231928=CARTESIAN_POINT('Ctrl Pts',(-76.4732288217392,70.5546664262565,
-255.55015100001));
#231929=CARTESIAN_POINT('Ctrl Pts',(-62.6682847961853,72.2198196795144,
-248.816784000007));
#231930=CARTESIAN_POINT('Ctrl Pts',(-48.8633407706315,73.8849729327724,
-242.083417000003));
#231931=CARTESIAN_POINT('Ctrl Pts',(-35.0583967450777,75.5501261860303,
-235.35005));
#231932=CARTESIAN_POINT('Ctrl Pts',(-21.3901353336382,77.1987927734144,
-228.683349999997));
#231933=CARTESIAN_POINT('Ctrl Pts',(-7.69249754350693,79.0826805347794,
-222.016650000002));
#231934=CARTESIAN_POINT('Ctrl Pts',(6.0484002420259,81.199531144254,-215.349950000001));
#231935=CARTESIAN_POINT('Ctrl Pts',(6.18580921988141,81.2206996503486,-215.283283000001));
#231936=CARTESIAN_POINT('Ctrl Pts',(6.32321819773692,81.2418681564432,-215.216616000001));
#231937=CARTESIAN_POINT('Ctrl Pts',(6.46062717559243,81.2630366625378,-215.149949000001));
#231938=CARTESIAN_POINT('Ctrl Pts',(-397.285026745533,63.7440265700833,
-376.750757000099));
#231939=CARTESIAN_POINT('Ctrl Pts',(-332.361185159884,68.4070457431775,
-349.81728900008));
#231940=CARTESIAN_POINT('Ctrl Pts',(-267.437343574235,73.0700649162719,
-322.883821000062));
#231941=CARTESIAN_POINT('Ctrl Pts',(-202.513501988586,77.7330840893662,
-295.950353000043));
#231942=CARTESIAN_POINT('Ctrl Pts',(-170.051581195761,80.0645936759133,
-282.483619000033));
#231943=CARTESIAN_POINT('Ctrl Pts',(-137.589660402937,82.3961032624605,
-269.016885000024));
#231944=CARTESIAN_POINT('Ctrl Pts',(-105.127739610112,84.7276128490076,
-255.550151000015));
#231945=CARTESIAN_POINT('Ctrl Pts',(-88.8967792136999,85.8933676422812,
-248.81678400001));
#231946=CARTESIAN_POINT('Ctrl Pts',(-72.6658188172876,87.0591224355548,
-242.083417000005));
#231947=CARTESIAN_POINT('Ctrl Pts',(-56.4348584208753,88.2248772288284,
-235.35005));
#231948=CARTESIAN_POINT('Ctrl Pts',(-40.3646006026454,89.3790898954359,
-228.683349999995));
#231949=CARTESIAN_POINT('Ctrl Pts',(-24.254362128099,90.8531963631996,-222.016650000002));
#231950=CARTESIAN_POINT('Ctrl Pts',(-8.08526176211542,92.6441253491055,
-215.349950000002));
#231951=CARTESIAN_POINT('Ctrl Pts',(-7.92357075845534,92.6620346389644,
-215.283283000002));
#231952=CARTESIAN_POINT('Ctrl Pts',(-7.76187975479526,92.6799439288233,
-215.216616000002));
#231953=CARTESIAN_POINT('Ctrl Pts',(-7.60018875113518,92.6978532186822,
-215.149949000001));
#231954=CARTESIAN_POINT('Ctrl Pts',(-614.253443137008,133.230382677491,
-376.750757000185));
#231955=CARTESIAN_POINT('Ctrl Pts',(-520.217405101058,131.900620330773,
-349.81728900015));
#231956=CARTESIAN_POINT('Ctrl Pts',(-426.181367065107,130.570857984055,
-322.883821000115));
#231957=CARTESIAN_POINT('Ctrl Pts',(-332.145329029157,129.241095637338,
-295.950353000079));
#231958=CARTESIAN_POINT('Ctrl Pts',(-285.127310011182,128.576214463979,
-282.483619000062));
#231959=CARTESIAN_POINT('Ctrl Pts',(-238.109290993206,127.91133329062,-269.016885000044));
#231960=CARTESIAN_POINT('Ctrl Pts',(-191.091271975231,127.246452117261,
-255.550151000026));
#231961=CARTESIAN_POINT('Ctrl Pts',(-167.582262466243,126.914011530581,
-248.816784000018));
#231962=CARTESIAN_POINT('Ctrl Pts',(-144.073252957256,126.581570943902,
-242.083417000009));
#231963=CARTESIAN_POINT('Ctrl Pts',(-120.564243448268,126.249130357223,
-235.35005));
#231964=CARTESIAN_POINT('Ctrl Pts',(-97.2879964096667,125.9199812615,-228.683349999992));
#231965=CARTESIAN_POINT('Ctrl Pts',(-73.9399558818752,126.16474384846,-222.016650000005));
#231966=CARTESIAN_POINT('Ctrl Pts',(-50.4862477745394,126.97790796366,-215.349950000003));
#231967=CARTESIAN_POINT('Ctrl Pts',(-50.2517106934656,126.986039604812,
-215.283283000003));
#231968=CARTESIAN_POINT('Ctrl Pts',(-50.0171736123918,126.994171245964,
-215.216616000002));
#231969=CARTESIAN_POINT('Ctrl Pts',(-49.782636531318,127.002302887115,-215.149949000002));
#231970=CARTESIAN_POINT('Ctrl Pts',(-831.221859528483,202.716738784898,
-376.75075700027));
#231971=CARTESIAN_POINT('Ctrl Pts',(-708.073625042231,195.394194918369,
-349.817289000218));
#231972=CARTESIAN_POINT('Ctrl Pts',(-584.92539055598,188.071651051839,-322.883821000167));
#231973=CARTESIAN_POINT('Ctrl Pts',(-461.777156069728,180.749107185309,
-295.950353000116));
#231974=CARTESIAN_POINT('Ctrl Pts',(-400.203038826602,177.087835252044,
-282.48361900009));
#231975=CARTESIAN_POINT('Ctrl Pts',(-338.628921583476,173.426563318779,
-269.016885000064));
#231976=CARTESIAN_POINT('Ctrl Pts',(-277.05480434035,169.765291385514,-255.550151000039));
#231977=CARTESIAN_POINT('Ctrl Pts',(-246.267745718787,167.934655418882,
-248.816784000026));
#231978=CARTESIAN_POINT('Ctrl Pts',(-215.480687097224,166.10401945225,-242.083417000013));
#231979=CARTESIAN_POINT('Ctrl Pts',(-184.693628475661,164.273383485617,
-235.35005));
#231980=CARTESIAN_POINT('Ctrl Pts',(-154.211392216688,162.460872627565,
-228.683349999988));
#231981=CARTESIAN_POINT('Ctrl Pts',(-123.625549635651,161.47629133372,-222.016650000007));
#231982=CARTESIAN_POINT('Ctrl Pts',(-92.8872337869633,161.311690578215,
-215.349950000004));
#231983=CARTESIAN_POINT('Ctrl Pts',(-92.5798506284758,161.31004457066,-215.283283000004));
#231984=CARTESIAN_POINT('Ctrl Pts',(-92.2724674699883,161.308398563104,
-215.216616000004));
#231985=CARTESIAN_POINT('Ctrl Pts',(-91.9650843115009,161.306752555549,
-215.149949000004));
#231986=CARTESIAN_POINT('Ctrl Pts',(-1048.19027591996,272.203094892306,
-376.750757000354));
#231987=CARTESIAN_POINT('Ctrl Pts',(-895.929844983404,258.887769505964,
-349.817289000287));
#231988=CARTESIAN_POINT('Ctrl Pts',(-743.669414046851,245.572444119622,
-322.883821000219));
#231989=CARTESIAN_POINT('Ctrl Pts',(-591.408983110298,232.257118733281,
-295.950353000152));
#231990=CARTESIAN_POINT('Ctrl Pts',(-515.278767642022,225.59945604011,-282.483619000118));
#231991=CARTESIAN_POINT('Ctrl Pts',(-439.148552173745,218.941793346939,
-269.016885000084));
#231992=CARTESIAN_POINT('Ctrl Pts',(-363.018336705469,212.284130653768,
-255.550151000051));
#231993=CARTESIAN_POINT('Ctrl Pts',(-324.953228971331,208.955299307182,
-248.816784000034));
#231994=CARTESIAN_POINT('Ctrl Pts',(-286.888121237192,205.626467960597,
-242.083417000017));
#231995=CARTESIAN_POINT('Ctrl Pts',(-248.823013503054,202.297636614011,
-235.35005));
#231996=CARTESIAN_POINT('Ctrl Pts',(-211.134788023709,199.001763993629,
-228.683349999984));
#231997=CARTESIAN_POINT('Ctrl Pts',(-173.311143389428,196.787838818981,
-222.016650000008));
#231998=CARTESIAN_POINT('Ctrl Pts',(-135.288219799387,195.64547319277,-215.349950000004));
#231999=CARTESIAN_POINT('Ctrl Pts',(-134.907990563486,195.634049536507,
-215.283283000005));
#232000=CARTESIAN_POINT('Ctrl Pts',(-134.527761327585,195.622625880244,
-215.216616000005));
#232001=CARTESIAN_POINT('Ctrl Pts',(-134.147532091684,195.611202223982,
-215.149949000005));
#232002=CARTESIAN_POINT('Ctrl Pts',(-1699.09552509438,480.662163214529,
-376.75075700061));
#232003=CARTESIAN_POINT('Ctrl Pts',(-1459.49850480692,449.368493268751,
-349.817289000493));
#232004=CARTESIAN_POINT('Ctrl Pts',(-1219.90148451947,418.074823322972,
-322.883821000378));
#232005=CARTESIAN_POINT('Ctrl Pts',(-980.30446423201,386.781153377194,-295.950353000261));
#232006=CARTESIAN_POINT('Ctrl Pts',(-860.505954088282,371.134318404306,
-282.483619000203));
#232007=CARTESIAN_POINT('Ctrl Pts',(-740.707443944553,355.487483431416,
-269.016885000145));
#232008=CARTESIAN_POINT('Ctrl Pts',(-620.908933800825,339.840648458528,
-255.550151000087));
#232009=CARTESIAN_POINT('Ctrl Pts',(-561.009678728961,332.017230972083,
-248.816784000058));
#232010=CARTESIAN_POINT('Ctrl Pts',(-501.110423657097,324.193813485639,
-242.083417000029));
#232011=CARTESIAN_POINT('Ctrl Pts',(-441.211168585233,316.370395999194,
-235.35005));
#232012=CARTESIAN_POINT('Ctrl Pts',(-381.904975444773,308.624438091823,
-228.683349999972));
#232013=CARTESIAN_POINT('Ctrl Pts',(-322.367924650756,302.722481274762,
-222.016650000015));
#232014=CARTESIAN_POINT('Ctrl Pts',(-262.491177836659,298.646821036434,
-215.349950000008));
#232015=CARTESIAN_POINT('Ctrl Pts',(-261.892410368517,298.60606443405,-215.283283000008));
#232016=CARTESIAN_POINT('Ctrl Pts',(-261.293642900374,298.565307831665,
-215.216616000008));
#232017=CARTESIAN_POINT('Ctrl Pts',(-260.694875432232,298.524551229281,
-215.149949000007));
#232018=CARTESIAN_POINT('Ctrl Pts',(-2350.0007742688,689.121231536752,-376.750757000865));
#232019=CARTESIAN_POINT('Ctrl Pts',(-2023.06716463044,639.849217031537,
-349.8172890007));
#232020=CARTESIAN_POINT('Ctrl Pts',(-1696.13355499208,590.577202526323,
-322.883821000536));
#232021=CARTESIAN_POINT('Ctrl Pts',(-1369.19994535372,541.305188021109,
-295.95035300037));
#232022=CARTESIAN_POINT('Ctrl Pts',(-1205.73314053454,516.669180768502,
-282.483619000288));
#232023=CARTESIAN_POINT('Ctrl Pts',(-1042.26633571536,492.033173515894,
-269.016885000205));
#232024=CARTESIAN_POINT('Ctrl Pts',(-878.799530896182,467.397166263287,
-255.550151000123));
#232025=CARTESIAN_POINT('Ctrl Pts',(-797.066128486591,455.079162636984,
-248.816784000082));
#232026=CARTESIAN_POINT('Ctrl Pts',(-715.332726077001,442.76115901068,-242.083417000041));
#232027=CARTESIAN_POINT('Ctrl Pts',(-633.599323667412,430.443155384376,
-235.35005));
#232028=CARTESIAN_POINT('Ctrl Pts',(-552.675162865837,418.247112190016,
-228.68334999996));
#232029=CARTESIAN_POINT('Ctrl Pts',(-471.424705912085,408.657123730544,
-222.016650000021));
#232030=CARTESIAN_POINT('Ctrl Pts',(-389.694135873931,401.648168880098,
-215.34995000001));
#232031=CARTESIAN_POINT('Ctrl Pts',(-388.876830173548,401.578079331591,
-215.28328300001));
#232032=CARTESIAN_POINT('Ctrl Pts',(-388.059524473164,401.507989783086,
-215.216616000011));
#232033=CARTESIAN_POINT('Ctrl Pts',(-387.242218772781,401.43790023458,-215.149949000011));
#232034=CARTESIAN_POINT('Ctrl Pts',(-3000.90602344323,897.580299858975,
-376.75075700112));
#232035=CARTESIAN_POINT('Ctrl Pts',(-2586.63582445396,830.329940794324,
-349.817289000906));
#232036=CARTESIAN_POINT('Ctrl Pts',(-2172.36562546469,763.079581729674,
-322.883821000693));
#232037=CARTESIAN_POINT('Ctrl Pts',(-1758.09542647544,695.829222665023,
-295.95035300048));
#232038=CARTESIAN_POINT('Ctrl Pts',(-1550.9603269808,662.204043132698,-282.483619000373));
#232039=CARTESIAN_POINT('Ctrl Pts',(-1343.82522748617,628.578863600373,
-269.016885000266));
#232040=CARTESIAN_POINT('Ctrl Pts',(-1136.69012799154,594.953684068047,
-255.55015100016));
#232041=CARTESIAN_POINT('Ctrl Pts',(-1033.12257824422,578.141094301885,
-248.816784000106));
#232042=CARTESIAN_POINT('Ctrl Pts',(-929.555028496906,561.328504535722,
-242.083417000053));
#232043=CARTESIAN_POINT('Ctrl Pts',(-825.98747874959,544.515914769559,-235.35005));
#232044=CARTESIAN_POINT('Ctrl Pts',(-723.445350286901,527.86978628821,-228.683349999948));
#232045=CARTESIAN_POINT('Ctrl Pts',(-620.481487173413,514.591766186325,
-222.016650000027));
#232046=CARTESIAN_POINT('Ctrl Pts',(-516.897093911203,504.649516723762,
-215.349950000014));
#232047=CARTESIAN_POINT('Ctrl Pts',(-515.861249978578,504.550094229134,
-215.283283000013));
#232048=CARTESIAN_POINT('Ctrl Pts',(-514.825406045954,504.450671734507,
-215.216616000014));
#232049=CARTESIAN_POINT('Ctrl Pts',(-513.789562113329,504.351249239879,
-215.149949000014));
#232050=CARTESIAN_POINT('Ctrl Pts',(-4953.62177096649,1522.95750482565,
-376.750757001886));
#232051=CARTESIAN_POINT('Ctrl Pts',(-4277.34180392452,1401.77211208268,
-349.817289001526));
#232052=CARTESIAN_POINT('Ctrl Pts',(-3601.06183688254,1280.58671933972,
-322.883821001167));
#232053=CARTESIAN_POINT('Ctrl Pts',(-2924.78186984057,1159.40132659677,
-295.950353000808));
#232054=CARTESIAN_POINT('Ctrl Pts',(-2586.64188631958,1098.80863022529,
-282.483619000628));
#232055=CARTESIAN_POINT('Ctrl Pts',(-2248.50190279859,1038.21593385381,
-269.016885000448));
#232056=CARTESIAN_POINT('Ctrl Pts',(-1910.36191927761,977.623237482327,
-255.550151000268));
#232057=CARTESIAN_POINT('Ctrl Pts',(-1741.29192751712,947.326889296587,
-248.816784000179));
#232058=CARTESIAN_POINT('Ctrl Pts',(-1572.22193575662,917.030541110847,
-242.08341700009));
#232059=CARTESIAN_POINT('Ctrl Pts',(-1403.15194399613,886.734192925108,
-235.35005));
#232060=CARTESIAN_POINT('Ctrl Pts',(-1235.75591255009,856.737808582791,
-228.683349999911));
#232061=CARTESIAN_POINT('Ctrl Pts',(-1067.6518309574,832.395693553669,-222.016650000045));
#232062=CARTESIAN_POINT('Ctrl Pts',(-898.505968023019,813.653560254753,
-215.349950000023));
#232063=CARTESIAN_POINT('Ctrl Pts',(-896.814509393671,813.466138921761,
-215.283283000022));
#232064=CARTESIAN_POINT('Ctrl Pts',(-895.123050764323,813.278717588769,
-215.216616000022));
#232065=CARTESIAN_POINT('Ctrl Pts',(-893.431592134975,813.091296255777,
-215.149949000023));
#232066=CARTESIAN_POINT('Ctrl Pts',(-6906.33751848976,2148.33470979231,
-376.750757002651));
#232067=CARTESIAN_POINT('Ctrl Pts',(-5968.04778339507,1973.21428337105,
-349.817289002145));
#232068=CARTESIAN_POINT('Ctrl Pts',(-5029.75804830038,1798.09385694977,
-322.883821001641));
#232069=CARTESIAN_POINT('Ctrl Pts',(-4091.4683132057,1622.97343052851,-295.950353001135));
#232070=CARTESIAN_POINT('Ctrl Pts',(-3622.32344565836,1535.41321731788,
-282.483619000883));
#232071=CARTESIAN_POINT('Ctrl Pts',(-3153.17857811102,1447.85300410724,
-269.01688500063));
#232072=CARTESIAN_POINT('Ctrl Pts',(-2684.03371056368,1360.29279089661,
-255.550151000377));
#232073=CARTESIAN_POINT('Ctrl Pts',(-2449.46127679,1316.51268429129,-248.816784000251));
#232074=CARTESIAN_POINT('Ctrl Pts',(-2214.88884301634,1272.73257768597,
-242.083417000126));
#232075=CARTESIAN_POINT('Ctrl Pts',(-1980.31640924266,1228.95247108066,
-235.35005));
#232076=CARTESIAN_POINT('Ctrl Pts',(-1748.06647481329,1185.60583087737,
-228.683349999876));
#232077=CARTESIAN_POINT('Ctrl Pts',(-1514.82217474138,1150.19962092101,
-222.016650000063));
#232078=CARTESIAN_POINT('Ctrl Pts',(-1280.11484213483,1122.65760378574,
-215.349950000032));
#232079=CARTESIAN_POINT('Ctrl Pts',(-1277.76776880876,1122.38218361439,
-215.283283000032));
#232080=CARTESIAN_POINT('Ctrl Pts',(-1275.42069548269,1122.10676344303,
-215.216616000032));
#232081=CARTESIAN_POINT('Ctrl Pts',(-1273.07362215662,1121.83134327167,
-215.149949000032));
#232082=CARTESIAN_POINT('Ctrl Pts',(-8859.05326601302,2773.71191475898,
-376.750757003417));
#232083=CARTESIAN_POINT('Ctrl Pts',(-7658.75376286563,2544.6564546594,-349.817289002765));
#232084=CARTESIAN_POINT('Ctrl Pts',(-6458.45425971823,2315.60099455983,
-322.883821002114));
#232085=CARTESIAN_POINT('Ctrl Pts',(-5258.15475657084,2086.54553446025,
-295.950353001463));
#232086=CARTESIAN_POINT('Ctrl Pts',(-4658.00500499714,1972.01780441047,
-282.483619001138));
#232087=CARTESIAN_POINT('Ctrl Pts',(-4057.85525342344,1857.49007436067,
-269.016885000812));
#232088=CARTESIAN_POINT('Ctrl Pts',(-3457.70550184975,1742.96234431089,
-255.550151000486));
#232089=CARTESIAN_POINT('Ctrl Pts',(-3157.6306260629,1685.69847928599,-248.816784000324));
#232090=CARTESIAN_POINT('Ctrl Pts',(-2857.55575027604,1628.4346142611,-242.083417000162));
#232091=CARTESIAN_POINT('Ctrl Pts',(-2557.4808744892,1571.17074923621,-235.35005));
#232092=CARTESIAN_POINT('Ctrl Pts',(-2260.37703707648,1514.47385317195,
-228.683349999839));
#232093=CARTESIAN_POINT('Ctrl Pts',(-1961.99251852537,1468.00354828836,
-222.01665000008));
#232094=CARTESIAN_POINT('Ctrl Pts',(-1661.72371624665,1431.66164731674,
-215.349950000041));
#232095=CARTESIAN_POINT('Ctrl Pts',(-1658.72102822386,1431.29822830702,
-215.28328300004));
#232096=CARTESIAN_POINT('Ctrl Pts',(-1655.71834020106,1430.93480929729,
-215.216616000041));
#232097=CARTESIAN_POINT('Ctrl Pts',(-1652.71565217826,1430.57139028757,
-215.149949000041));
#232098=CARTESIAN_POINT('Ctrl Pts',(-14717.2005085828,4649.84352965899,
-376.750757005713));
#232099=CARTESIAN_POINT('Ctrl Pts',(-12730.8717012773,4258.98296852449,
-349.817289004623));
#232100=CARTESIAN_POINT('Ctrl Pts',(-10744.5428939718,3868.12240738999,
-322.883821003535));
#232101=CARTESIAN_POINT('Ctrl Pts',(-8758.21408666624,3477.26184625548,
-295.950353002446));
#232102=CARTESIAN_POINT('Ctrl Pts',(-7765.04968301347,3281.83156568823,
-282.483619001902));
#232103=CARTESIAN_POINT('Ctrl Pts',(-6771.88527936071,3086.40128512098,
-269.016885001358));
#232104=CARTESIAN_POINT('Ctrl Pts',(-5778.72087570795,2890.97100455373,
-255.550151000813));
#232105=CARTESIAN_POINT('Ctrl Pts',(-5282.13867388157,2793.2558642701,-248.816784000541));
#232106=CARTESIAN_POINT('Ctrl Pts',(-4785.55647205519,2695.54072398648,
-242.083417000271));
#232107=CARTESIAN_POINT('Ctrl Pts',(-4288.9742702288,2597.82558370285,-235.35005));
#232108=CARTESIAN_POINT('Ctrl Pts',(-3797.30872386605,2501.0779200557,-228.683349999731));
#232109=CARTESIAN_POINT('Ctrl Pts',(-3303.50354987733,2421.41533039039,
-222.016650000135));
#232110=CARTESIAN_POINT('Ctrl Pts',(-2806.55033858209,2358.67377790971,
-215.349950000068));
#232111=CARTESIAN_POINT('Ctrl Pts',(-2801.58080646913,2358.0463623849,-215.283283000067));
#232112=CARTESIAN_POINT('Ctrl Pts',(-2796.61127435617,2357.41894686008,
-215.216616000068));
#232113=CARTESIAN_POINT('Ctrl Pts',(-2791.64174224321,2356.79153133527,
-215.149949000068));
#232114=CARTESIAN_POINT('Ctrl Pts',(-20575.3477511526,6525.97514455899,
-376.750757008008));
#232115=CARTESIAN_POINT('Ctrl Pts',(-17802.9896396889,5973.30948238956,
-349.817289006482));
#232116=CARTESIAN_POINT('Ctrl Pts',(-15030.6315282253,5420.64382022014,
-322.883821004956));
#232117=CARTESIAN_POINT('Ctrl Pts',(-12258.2734167616,4867.97815805071,
-295.950353003429));
#232118=CARTESIAN_POINT('Ctrl Pts',(-10872.0943610298,4591.645326966,-282.483619002666));
#232119=CARTESIAN_POINT('Ctrl Pts',(-9485.91530529798,4315.31249588128,
-269.016885001903));
#232120=CARTESIAN_POINT('Ctrl Pts',(-8099.73624956616,4038.97966479657,
-255.55015100114));
#232121=CARTESIAN_POINT('Ctrl Pts',(-7406.64672170025,3900.81324925421,
-248.816784000758));
#232122=CARTESIAN_POINT('Ctrl Pts',(-6713.55719383433,3762.64683371185,
-242.083417000379));
#232123=CARTESIAN_POINT('Ctrl Pts',(-6020.46766596842,3624.4804181695,-235.35005));
#232124=CARTESIAN_POINT('Ctrl Pts',(-5334.24041065563,3487.68198693944,
-228.683349999624));
#232125=CARTESIAN_POINT('Ctrl Pts',(-4645.01458122929,3374.82711249242,
-222.016650000188));
#232126=CARTESIAN_POINT('Ctrl Pts',(-3951.37696091755,3285.68590850268,
-215.349950000095));
#232127=CARTESIAN_POINT('Ctrl Pts',(-3944.44058471441,3284.79449646278,
-215.283283000095));
#232128=CARTESIAN_POINT('Ctrl Pts',(-3937.50420851128,3283.90308442287,
-215.216616000095));
#232129=CARTESIAN_POINT('Ctrl Pts',(-3930.56783230814,3283.01167238296,
-215.149949000095));
#232130=CARTESIAN_POINT('Ctrl Pts',(-26433.4949937224,8402.106759459,-376.750757010304));
#232131=CARTESIAN_POINT('Ctrl Pts',(-22875.1075781007,7687.63599625465,
-349.81728900834));
#232132=CARTESIAN_POINT('Ctrl Pts',(-19316.7201624788,6973.16523305029,
-322.883821006377));
#232133=CARTESIAN_POINT('Ctrl Pts',(-15758.332746857,6258.69446984594,-295.950353004413));
#232134=CARTESIAN_POINT('Ctrl Pts',(-13979.1390390461,5901.45908824376,
-282.48361900343));
#232135=CARTESIAN_POINT('Ctrl Pts',(-12199.9453312353,5544.22370664158,
-269.016885002448));
#232136=CARTESIAN_POINT('Ctrl Pts',(-10420.7516234244,5186.98832503941,
-255.550151001467));
#232137=CARTESIAN_POINT('Ctrl Pts',(-9531.15476951892,5008.37063423832,
-248.816784000976));
#232138=CARTESIAN_POINT('Ctrl Pts',(-8641.55791561347,4829.75294343723,
-242.083417000487));
#232139=CARTESIAN_POINT('Ctrl Pts',(-7751.96106170802,4651.13525263614,
-235.35005));
#232140=CARTESIAN_POINT('Ctrl Pts',(-6871.1720974452,4474.28605382318,-228.683349999516));
#232141=CARTESIAN_POINT('Ctrl Pts',(-5986.52561258124,4328.23889459445,
-222.016650000243));
#232142=CARTESIAN_POINT('Ctrl Pts',(-5096.20358325299,4212.69803909567,
-215.349950000122));
#232143=CARTESIAN_POINT('Ctrl Pts',(-5087.30036295968,4211.54263054066,
-215.283283000121));
#232144=CARTESIAN_POINT('Ctrl Pts',(-5078.39714266638,4210.38722198566,
-215.216616000122));
#232145=CARTESIAN_POINT('Ctrl Pts',(-5069.49392237307,4209.23181343066,
-215.149949000122));
#232146=CARTESIAN_POINT('Origin',(0.,-12.9675000200281,-218.35005));
#232147=CARTESIAN_POINT('Ctrl Pts',(-10765.646428189,-1979.29526939781,
-376.750757000846));
#232148=CARTESIAN_POINT('Ctrl Pts',(-9257.10677574949,-1902.78686830728,
-349.817289000686));
#232149=CARTESIAN_POINT('Ctrl Pts',(-7748.56712330994,-1826.27846721676,
-322.883821000524));
#232150=CARTESIAN_POINT('Ctrl Pts',(-6240.0274708704,-1749.77006612623,
-295.950353000363));
#232151=CARTESIAN_POINT('Ctrl Pts',(-5485.75764465062,-1711.51586558096,
-282.483619000282));
#232152=CARTESIAN_POINT('Ctrl Pts',(-4731.48781843085,-1673.2616650357,
-269.016885000202));
#232153=CARTESIAN_POINT('Ctrl Pts',(-3977.21799221108,-1635.00746449044,
-255.550151000121));
#232154=CARTESIAN_POINT('Ctrl Pts',(-3600.08307910119,-1615.8803642178,
-248.816784000081));
#232155=CARTESIAN_POINT('Ctrl Pts',(-3222.9481659913,-1596.75326394517,
-242.083417000041));
#232156=CARTESIAN_POINT('Ctrl Pts',(-2845.81325288141,-1577.62616367254,
-235.35005));
#232157=CARTESIAN_POINT('Ctrl Pts',(-2472.41234881222,-1558.68844063033,
-228.68334999996));
#232158=CARTESIAN_POINT('Ctrl Pts',(-2099.07452015968,-1540.45097924114,
-222.01665));
#232159=CARTESIAN_POINT('Ctrl Pts',(-1725.79722689738,-1522.91379824522,
-215.34994999996));
#232160=CARTESIAN_POINT('Ctrl Pts',(-1722.06445396475,-1522.73842643524,
-215.28328299996));
#232161=CARTESIAN_POINT('Ctrl Pts',(-1718.33168103213,-1522.56305462527,
-215.21661599996));
#232162=CARTESIAN_POINT('Ctrl Pts',(-1714.5989080995,-1522.3876828153,-215.14994899996));
#232163=CARTESIAN_POINT('Ctrl Pts',(-8392.35568812379,-1534.61913504983,
-376.750757000658));
#232164=CARTESIAN_POINT('Ctrl Pts',(-7213.78531733318,-1478.38877237011,
-349.817289000532));
#232165=CARTESIAN_POINT('Ctrl Pts',(-6035.21494654257,-1422.15840969038,
-322.883821000408));
#232166=CARTESIAN_POINT('Ctrl Pts',(-4856.64457575196,-1365.92804701065,
-295.950353000282));
#232167=CARTESIAN_POINT('Ctrl Pts',(-4267.35939035666,-1337.81286567079,
-282.48361900022));
#232168=CARTESIAN_POINT('Ctrl Pts',(-3678.07420496136,-1309.69768433093,
-269.016885000157));
#232169=CARTESIAN_POINT('Ctrl Pts',(-3088.78901956605,-1281.58250299106,
-255.550151000094));
#232170=CARTESIAN_POINT('Ctrl Pts',(-2794.1464268684,-1267.52491232113,
-248.816784000063));
#232171=CARTESIAN_POINT('Ctrl Pts',(-2499.50383417074,-1253.4673216512,
-242.083417000031));
#232172=CARTESIAN_POINT('Ctrl Pts',(-2204.8612414731,-1239.40973098127,
-235.35005));
#232173=CARTESIAN_POINT('Ctrl Pts',(-1913.13590216849,-1225.49132437738,
-228.683349999968));
#232174=CARTESIAN_POINT('Ctrl Pts',(-1621.45955977666,-1212.11656254984,
-222.01665));
#232175=CARTESIAN_POINT('Ctrl Pts',(-1329.83024235737,-1199.28546008462,
-215.349949999969));
#232176=CARTESIAN_POINT('Ctrl Pts',(-1326.91394918317,-1199.15714905996,
-215.283282999969));
#232177=CARTESIAN_POINT('Ctrl Pts',(-1323.99765600898,-1199.02883803529,
-215.216615999969));
#232178=CARTESIAN_POINT('Ctrl Pts',(-1321.08136283478,-1198.90052701063,
-215.149948999969));
#232179=CARTESIAN_POINT('Ctrl Pts',(-6019.06494805854,-1089.94300070186,
-376.750757000469));
#232180=CARTESIAN_POINT('Ctrl Pts',(-5170.46385891687,-1053.99067643293,
-349.817289000379));
#232181=CARTESIAN_POINT('Ctrl Pts',(-4321.8627697752,-1018.03835216401,
-322.88382100029));
#232182=CARTESIAN_POINT('Ctrl Pts',(-3473.26168063352,-982.086027895082,
-295.950353000201));
#232183=CARTESIAN_POINT('Ctrl Pts',(-3048.96113606269,-964.10986576062,
-282.483619000157));
#232184=CARTESIAN_POINT('Ctrl Pts',(-2624.66059149186,-946.133703626157,
-269.016885000112));
#232185=CARTESIAN_POINT('Ctrl Pts',(-2200.36004692103,-928.157541491694,
-255.550151000067));
#232186=CARTESIAN_POINT('Ctrl Pts',(-1988.2097746356,-919.169460424462,
-248.816784000044));
#232187=CARTESIAN_POINT('Ctrl Pts',(-1776.05950235019,-910.181379357231,
-242.083417000023));
#232188=CARTESIAN_POINT('Ctrl Pts',(-1563.90923006478,-901.19329829,-235.35005));
#232189=CARTESIAN_POINT('Ctrl Pts',(-1353.85945552476,-892.294208124424,
-228.683349999978));
#232190=CARTESIAN_POINT('Ctrl Pts',(-1143.84459939364,-883.782145858533,
-222.01665));
#232191=CARTESIAN_POINT('Ctrl Pts',(-933.863257817356,-875.657121924021,
-215.349949999977));
#232192=CARTESIAN_POINT('Ctrl Pts',(-931.763444401592,-875.575871684668,
-215.283282999978));
#232193=CARTESIAN_POINT('Ctrl Pts',(-929.663630985828,-875.494621445315,
-215.216615999977));
#232194=CARTESIAN_POINT('Ctrl Pts',(-927.563817570064,-875.413371205962,
-215.149948999978));
#232195=CARTESIAN_POINT('Ctrl Pts',(-3645.77420799329,-645.266866353884,
-376.75075700028));
#232196=CARTESIAN_POINT('Ctrl Pts',(-3127.14240050056,-629.592580495759,
-349.817289000227));
#232197=CARTESIAN_POINT('Ctrl Pts',(-2608.51059300782,-613.918294637635,
-322.883821000173));
#232198=CARTESIAN_POINT('Ctrl Pts',(-2089.87878551509,-598.24400877951,
-295.95035300012));
#232199=CARTESIAN_POINT('Ctrl Pts',(-1830.56288176873,-590.406865850448,
-282.483619000093));
#232200=CARTESIAN_POINT('Ctrl Pts',(-1571.24697802237,-582.569722921386,
-269.016885000067));
#232201=CARTESIAN_POINT('Ctrl Pts',(-1311.931074276,-574.732579992324,-255.55015100004));
#232202=CARTESIAN_POINT('Ctrl Pts',(-1182.27312240282,-570.814008527792,
-248.816784000027));
#232203=CARTESIAN_POINT('Ctrl Pts',(-1052.61517052964,-566.895437063261,
-242.083417000014));
#232204=CARTESIAN_POINT('Ctrl Pts',(-922.957218656454,-562.97686559873,
-235.35005));
#232205=CARTESIAN_POINT('Ctrl Pts',(-794.583008881026,-559.097091871471,
-228.683349999987));
#232206=CARTESIAN_POINT('Ctrl Pts',(-666.229639010622,-555.447729167229,
-222.01665));
#232207=CARTESIAN_POINT('Ctrl Pts',(-537.896273277345,-552.028783763422,
-215.349949999987));
#232208=CARTESIAN_POINT('Ctrl Pts',(-536.612939620012,-551.994594309379,
-215.283282999987));
#232209=CARTESIAN_POINT('Ctrl Pts',(-535.329605962679,-551.960404855337,
-215.216615999987));
#232210=CARTESIAN_POINT('Ctrl Pts',(-534.046272305346,-551.926215401294,
-215.149948999987));
#232211=CARTESIAN_POINT('Ctrl Pts',(-2854.6772946382,-497.041488237892,
-376.750757000217));
#232212=CARTESIAN_POINT('Ctrl Pts',(-2446.03524769512,-488.126548516702,
-349.817289000176));
#232213=CARTESIAN_POINT('Ctrl Pts',(-2037.39320075203,-479.211608795511,
-322.883821000135));
#232214=CARTESIAN_POINT('Ctrl Pts',(-1628.75115380895,-470.29666907432,
-295.950353000093));
#232215=CARTESIAN_POINT('Ctrl Pts',(-1424.43013033741,-465.839199213724,
-282.483619000073));
#232216=CARTESIAN_POINT('Ctrl Pts',(-1220.10910686587,-461.381729353129,
-269.016885000052));
#232217=CARTESIAN_POINT('Ctrl Pts',(-1015.78808339432,-456.924259492534,
-255.550151000031));
#232218=CARTESIAN_POINT('Ctrl Pts',(-913.627571658554,-454.695524562236,
-248.816784000021));
#232219=CARTESIAN_POINT('Ctrl Pts',(-811.467059922784,-452.466789631938,
-242.083417000011));
#232220=CARTESIAN_POINT('Ctrl Pts',(-709.306548187014,-450.23805470164,
-235.35005));
#232221=CARTESIAN_POINT('Ctrl Pts',(-608.157526666449,-448.03138645382,
-228.68334999999));
#232222=CARTESIAN_POINT('Ctrl Pts',(-507.024652216282,-446.002923603462,
-222.01665));
#232223=CARTESIAN_POINT('Ctrl Pts',(-405.907278430675,-444.152671043223,
-215.34994999999));
#232224=CARTESIAN_POINT('Ctrl Pts',(-404.896104692818,-444.134168517617,
-215.283282999989));
#232225=CARTESIAN_POINT('Ctrl Pts',(-403.884930954962,-444.115665992011,
-215.21661599999));
#232226=CARTESIAN_POINT('Ctrl Pts',(-402.873757217106,-444.097163466405,
-215.14994899999));
#232227=CARTESIAN_POINT('Ctrl Pts',(-2063.58038128312,-348.816110121901,
-376.750757000154));
#232228=CARTESIAN_POINT('Ctrl Pts',(-1764.92809488968,-346.660516537644,
-349.817289000125));
#232229=CARTESIAN_POINT('Ctrl Pts',(-1466.27580849624,-344.504922953386,
-322.883821000096));
#232230=CARTESIAN_POINT('Ctrl Pts',(-1167.6235221028,-342.349329369129,
-295.950353000066));
#232231=CARTESIAN_POINT('Ctrl Pts',(-1018.29737890609,-341.271532577001,
-282.483619000052));
#232232=CARTESIAN_POINT('Ctrl Pts',(-868.971235709368,-340.193735784872,
-269.016885000037));
#232233=CARTESIAN_POINT('Ctrl Pts',(-719.64509251265,-339.115938992743,
-255.550151000022));
#232234=CARTESIAN_POINT('Ctrl Pts',(-644.982020914291,-338.577040596679,
-248.816784000015));
#232235=CARTESIAN_POINT('Ctrl Pts',(-570.318949315933,-338.038142200615,
-242.083417000008));
#232236=CARTESIAN_POINT('Ctrl Pts',(-495.655877717574,-337.49924380455,
-235.35005));
#232237=CARTESIAN_POINT('Ctrl Pts',(-421.732044451872,-336.96568103617,
-228.683349999993));
#232238=CARTESIAN_POINT('Ctrl Pts',(-347.819665421942,-336.558118039694,
-222.01665));
#232239=CARTESIAN_POINT('Ctrl Pts',(-273.918283584005,-336.276558323023,
-215.349949999993));
#232240=CARTESIAN_POINT('Ctrl Pts',(-273.179269765626,-336.273742725853,
-215.283282999993));
#232241=CARTESIAN_POINT('Ctrl Pts',(-272.440255947246,-336.270927128685,
-215.216615999993));
#232242=CARTESIAN_POINT('Ctrl Pts',(-271.701242128866,-336.268111531515,
-215.149948999993));
#232243=CARTESIAN_POINT('Ctrl Pts',(-1272.48346792803,-200.59073200591,
-376.750757000092));
#232244=CARTESIAN_POINT('Ctrl Pts',(-1083.82094208424,-205.194484558586,
-349.817289000074));
#232245=CARTESIAN_POINT('Ctrl Pts',(-895.15841624045,-209.798237111262,
-322.883821000057));
#232246=CARTESIAN_POINT('Ctrl Pts',(-706.49589039666,-214.401989663939,
-295.950353000039));
#232247=CARTESIAN_POINT('Ctrl Pts',(-612.164627474765,-216.703865940277,
-282.483619000031));
#232248=CARTESIAN_POINT('Ctrl Pts',(-517.83336455287,-219.005742216615,
-269.016885000022));
#232249=CARTESIAN_POINT('Ctrl Pts',(-423.502101630976,-221.307618492953,
-255.550151000013));
#232250=CARTESIAN_POINT('Ctrl Pts',(-376.336470170028,-222.458556631122,
-248.816784000009));
#232251=CARTESIAN_POINT('Ctrl Pts',(-329.170838709081,-223.609494769291,
-242.083417000004));
#232252=CARTESIAN_POINT('Ctrl Pts',(-282.005207248134,-224.760432907461,
-235.35005));
#232253=CARTESIAN_POINT('Ctrl Pts',(-235.306562237295,-225.899975618519,
-228.683349999995));
#232254=CARTESIAN_POINT('Ctrl Pts',(-188.614678627603,-227.113312475926,
-222.01665));
#232255=CARTESIAN_POINT('Ctrl Pts',(-141.929288737335,-228.400445602824,
-215.349949999996));
#232256=CARTESIAN_POINT('Ctrl Pts',(-141.462434838432,-228.413316934091,
-215.283282999995));
#232257=CARTESIAN_POINT('Ctrl Pts',(-140.995580939529,-228.426188265358,
-215.216615999995));
#232258=CARTESIAN_POINT('Ctrl Pts',(-140.528727040626,-228.439059596626,
-215.149948999996));
#232259=CARTESIAN_POINT('Ctrl Pts',(-1008.78449680967,-151.182272633913,
-376.750757000071));
#232260=CARTESIAN_POINT('Ctrl Pts',(-856.785224482427,-158.039140565566,
-349.817289000057));
#232261=CARTESIAN_POINT('Ctrl Pts',(-704.785952155186,-164.896008497221,
-322.883821000044));
#232262=CARTESIAN_POINT('Ctrl Pts',(-552.786679827945,-171.752876428875,
-295.95035300003));
#232263=CARTESIAN_POINT('Ctrl Pts',(-476.787043664325,-175.181310394702,
-282.483619000024));
#232264=CARTESIAN_POINT('Ctrl Pts',(-400.787407500704,-178.609744360529,
-269.016885000016));
#232265=CARTESIAN_POINT('Ctrl Pts',(-324.787771337084,-182.038178326357,
-255.55015100001));
#232266=CARTESIAN_POINT('Ctrl Pts',(-286.787953255274,-183.75239530927,
-248.816784000007));
#232267=CARTESIAN_POINT('Ctrl Pts',(-248.788135173463,-185.466612292184,
-242.083417000003));
#232268=CARTESIAN_POINT('Ctrl Pts',(-210.788317091653,-187.180829275097,
-235.35005));
#232269=CARTESIAN_POINT('Ctrl Pts',(-173.164734832436,-188.878073812635,
-228.683349999997));
#232270=CARTESIAN_POINT('Ctrl Pts',(-135.546349696156,-190.631710621336,
-222.01665));
#232271=CARTESIAN_POINT('Ctrl Pts',(-97.932957121778,-192.441741362757,
-215.349949999997));
#232272=CARTESIAN_POINT('Ctrl Pts',(-97.5568231960341,-192.45984167017,
-215.283282999997));
#232273=CARTESIAN_POINT('Ctrl Pts',(-97.1806892702902,-192.477941977583,
-215.216615999996));
#232274=CARTESIAN_POINT('Ctrl Pts',(-96.8045553445463,-192.496042284996,
-215.149948999996));
#232275=CARTESIAN_POINT('Ctrl Pts',(-745.085525691306,-101.773813261915,
-376.75075700005));
#232276=CARTESIAN_POINT('Ctrl Pts',(-629.749506880614,-110.883796572547,
-349.81728900004));
#232277=CARTESIAN_POINT('Ctrl Pts',(-514.413488069922,-119.993779883179,
-322.88382100003));
#232278=CARTESIAN_POINT('Ctrl Pts',(-399.07746925923,-129.103763193811,
-295.950353000021));
#232279=CARTESIAN_POINT('Ctrl Pts',(-341.409459853884,-133.658754849127,
-282.483619000017));
#232280=CARTESIAN_POINT('Ctrl Pts',(-283.741450448538,-138.213746504444,
-269.016885000012));
#232281=CARTESIAN_POINT('Ctrl Pts',(-226.073441043192,-142.76873815976,
-255.550151000007));
#232282=CARTESIAN_POINT('Ctrl Pts',(-197.239436340519,-145.046233987418,
-248.816784000005));
#232283=CARTESIAN_POINT('Ctrl Pts',(-168.405431637847,-147.323729815076,
-242.083417000002));
#232284=CARTESIAN_POINT('Ctrl Pts',(-139.571426935173,-149.601225642734,
-235.35005));
#232285=CARTESIAN_POINT('Ctrl Pts',(-111.022907427576,-151.856172006752,
-228.683349999998));
#232286=CARTESIAN_POINT('Ctrl Pts',(-82.4780207647092,-154.150108766748,
-222.01665));
#232287=CARTESIAN_POINT('Ctrl Pts',(-53.9366255062213,-156.48303712269,
-215.349949999998));
#232288=CARTESIAN_POINT('Ctrl Pts',(-53.6512115536363,-156.506366406249,
-215.283282999997));
#232289=CARTESIAN_POINT('Ctrl Pts',(-53.3657976010514,-156.529695689807,
-215.216615999998));
#232290=CARTESIAN_POINT('Ctrl Pts',(-53.0803836484664,-156.553024973366,
-215.149948999998));
#232291=CARTESIAN_POINT('Ctrl Pts',(-481.386554572944,-52.3653538899179,
-376.750757000028));
#232292=CARTESIAN_POINT('Ctrl Pts',(-402.713789278801,-63.7284525795279,
-349.817289000023));
#232293=CARTESIAN_POINT('Ctrl Pts',(-324.041023984658,-75.0915512691379,
-322.883821000018));
#232294=CARTESIAN_POINT('Ctrl Pts',(-245.368258690515,-86.4546499587479,
-295.950353000012));
#232295=CARTESIAN_POINT('Ctrl Pts',(-206.031876043444,-92.1361993035529,
-282.48361900001));
#232296=CARTESIAN_POINT('Ctrl Pts',(-166.695493396372,-97.8177486483579,
-269.016885000007));
#232297=CARTESIAN_POINT('Ctrl Pts',(-127.359110749301,-103.499297993163,
-255.550151000004));
#232298=CARTESIAN_POINT('Ctrl Pts',(-107.690919425765,-106.340072665565,
-248.816784000003));
#232299=CARTESIAN_POINT('Ctrl Pts',(-88.0227281022291,-109.180847337968,
-242.083417000002));
#232300=CARTESIAN_POINT('Ctrl Pts',(-68.3545367786933,-112.02162201037,
-235.35005));
#232301=CARTESIAN_POINT('Ctrl Pts',(-48.8810800227174,-114.834270200868,
-228.683349999999));
#232302=CARTESIAN_POINT('Ctrl Pts',(-29.4096918332626,-117.668506912158,
-222.01665));
#232303=CARTESIAN_POINT('Ctrl Pts',(-9.94029389066457,-120.524332882624,
-215.349949999999));
#232304=CARTESIAN_POINT('Ctrl Pts',(-9.74559991123855,-120.552891142328,
-215.283282999999));
#232305=CARTESIAN_POINT('Ctrl Pts',(-9.55090593181253,-120.581449402032,
-215.216615999999));
#232306=CARTESIAN_POINT('Ctrl Pts',(-9.3562119523865,-120.610007661736,
-215.149948999999));
#232307=CARTESIAN_POINT('Ctrl Pts',(-393.48689753349,-35.8958674325856,
-376.750757000021));
#232308=CARTESIAN_POINT('Ctrl Pts',(-327.035216744864,-48.0100045818548,
-349.817289000017));
#232309=CARTESIAN_POINT('Ctrl Pts',(-260.583535956237,-60.1241417311241,
-322.883821000013));
#232310=CARTESIAN_POINT('Ctrl Pts',(-194.13185516761,-72.2382788803934,
-295.950353000009));
#232311=CARTESIAN_POINT('Ctrl Pts',(-160.906014773297,-78.2953474550281,
-282.483619000007));
#232312=CARTESIAN_POINT('Ctrl Pts',(-127.680174378983,-84.3524160296627,
-269.016885000005));
#232313=CARTESIAN_POINT('Ctrl Pts',(-94.45433398467,-90.4094846042973,-255.550151000003));
#232314=CARTESIAN_POINT('Ctrl Pts',(-77.8414137875133,-93.4380188916147,
-248.816784000002));
#232315=CARTESIAN_POINT('Ctrl Pts',(-61.2284935903567,-96.466553178932,
-242.083417000001));
#232316=CARTESIAN_POINT('Ctrl Pts',(-44.6155733932,-99.4950874662493,-235.35005));
#232317=CARTESIAN_POINT('Ctrl Pts',(-28.167137554431,-102.493636265573,
-228.683349999999));
#232318=CARTESIAN_POINT('Ctrl Pts',(-11.7202488561137,-105.507972960628,
-222.01665));
#232319=CARTESIAN_POINT('Ctrl Pts',(4.72514998118767,-108.538098135935,
-215.349949999999));
#232320=CARTESIAN_POINT('Ctrl Pts',(4.88960396956071,-108.568399387688,
-215.283282999999));
#232321=CARTESIAN_POINT('Ctrl Pts',(5.05405795793375,-108.59870063944,-215.216615999999));
#232322=CARTESIAN_POINT('Ctrl Pts',(5.2185119463068,-108.629001891193,-215.149948999999));
#232323=CARTESIAN_POINT('Ctrl Pts',(-305.587240494037,-19.4263809752531,
-376.750757000014));
#232324=CARTESIAN_POINT('Ctrl Pts',(-251.356644210927,-32.2915565841817,
-349.817289000011));
#232325=CARTESIAN_POINT('Ctrl Pts',(-197.126047927816,-45.1567321931103,
-322.883821000009));
#232326=CARTESIAN_POINT('Ctrl Pts',(-142.895451644705,-58.0219078020389,
-295.950353000006));
#232327=CARTESIAN_POINT('Ctrl Pts',(-115.78015350315,-64.4544956065032,
-282.483619000005));
#232328=CARTESIAN_POINT('Ctrl Pts',(-88.6648553615948,-70.8870834109675,
-269.016885000003));
#232329=CARTESIAN_POINT('Ctrl Pts',(-61.5495572200395,-77.3196712154318,
-255.550151000002));
#232330=CARTESIAN_POINT('Ctrl Pts',(-47.9919081492619,-80.5359651176639,
-248.816784000002));
#232331=CARTESIAN_POINT('Ctrl Pts',(-34.4342590784842,-83.7522590198961,
-242.083417000001));
#232332=CARTESIAN_POINT('Ctrl Pts',(-20.8766100077067,-86.9685529221282,
-235.35005));
#232333=CARTESIAN_POINT('Ctrl Pts',(-7.45319508614462,-90.1530023302789,
-228.68335));
#232334=CARTESIAN_POINT('Ctrl Pts',(5.96919412103514,-93.3474390090985,
-222.01665));
#232335=CARTESIAN_POINT('Ctrl Pts',(19.3905938530399,-96.5518633892461,
-215.34995));
#232336=CARTESIAN_POINT('Ctrl Pts',(19.52480785036,-96.5839076330473,-215.283283));
#232337=CARTESIAN_POINT('Ctrl Pts',(19.6590218476801,-96.6159518768485,
-215.216616));
#232338=CARTESIAN_POINT('Ctrl Pts',(19.7932358450001,-96.6479961206498,
-215.149949));
#232339=CARTESIAN_POINT('Ctrl Pts',(-217.687583454584,-2.9568945179205,
-376.750757000007));
#232340=CARTESIAN_POINT('Ctrl Pts',(-175.67807167699,-16.5731085865084,
-349.817289000006));
#232341=CARTESIAN_POINT('Ctrl Pts',(-133.668559899395,-30.1893226550964,
-322.883821000005));
#232342=CARTESIAN_POINT('Ctrl Pts',(-91.6590481218006,-43.8055367236842,
-295.950353000003));
#232343=CARTESIAN_POINT('Ctrl Pts',(-70.6542922330034,-50.6136437579782,
-282.483619000003));
#232344=CARTESIAN_POINT('Ctrl Pts',(-49.6495363442062,-57.4217507922722,
-269.016885000001));
#232345=CARTESIAN_POINT('Ctrl Pts',(-28.644780455409,-64.2298578265662,
-255.550151000001));
#232346=CARTESIAN_POINT('Ctrl Pts',(-18.1424025110104,-67.6339113437132,
-248.816784000001));
#232347=CARTESIAN_POINT('Ctrl Pts',(-7.64002456661188,-71.0379648608601,
-242.083417000001));
#232348=CARTESIAN_POINT('Ctrl Pts',(2.8623533777867,-74.4420183780071,-235.35005));
#232349=CARTESIAN_POINT('Ctrl Pts',(13.2607473821417,-77.8123683949843,
-228.68335));
#232350=CARTESIAN_POINT('Ctrl Pts',(23.658637098184,-81.1869050575687,-222.01665));
#232351=CARTESIAN_POINT('Ctrl Pts',(34.0560377248921,-84.5656286425572,
-215.34995));
#232352=CARTESIAN_POINT('Ctrl Pts',(34.1600117311593,-84.599415878407,-215.283283));
#232353=CARTESIAN_POINT('Ctrl Pts',(34.2639857374263,-84.6332031142567,
-215.216616));
#232354=CARTESIAN_POINT('Ctrl Pts',(34.3679597436934,-84.6669903501065,
-215.149949));
#232355=CARTESIAN_POINT('Ctrl Pts',(-188.387697774766,2.53293430119023,
-376.750757000005));
#232356=CARTESIAN_POINT('Ctrl Pts',(-150.451880832343,-11.3336259206174,
-349.817289000004));
#232357=CARTESIAN_POINT('Ctrl Pts',(-112.516063889921,-25.2001861424251,
-322.883821000003));
#232358=CARTESIAN_POINT('Ctrl Pts',(-74.580246947499,-39.0667463642328,
-295.950353000002));
#232359=CARTESIAN_POINT('Ctrl Pts',(-55.6123384762878,-46.0000264751366,
-282.483619000002));
#232360=CARTESIAN_POINT('Ctrl Pts',(-36.6444300050767,-52.9333065860405,
-269.016885000001));
#232361=CARTESIAN_POINT('Ctrl Pts',(-17.6765215338656,-59.8665866969443,
-255.550151000001));
#232362=CARTESIAN_POINT('Ctrl Pts',(-8.19256729825999,-63.3332267523963,
-248.816784000001));
#232363=CARTESIAN_POINT('Ctrl Pts',(1.29138693734558,-66.7998668078482,
-242.083417));
#232364=CARTESIAN_POINT('Ctrl Pts',(10.7753411729511,-70.2665068633001,
-235.35005));
#232365=CARTESIAN_POINT('Ctrl Pts',(20.1653948715705,-73.6988237498861,
-228.68335));
#232366=CARTESIAN_POINT('Ctrl Pts',(29.5551180905669,-77.1333937403921,
-222.01665));
#232367=CARTESIAN_POINT('Ctrl Pts',(38.9445190155095,-80.5702170603276,
-215.34995));
#232368=CARTESIAN_POINT('Ctrl Pts',(39.038413024759,-80.6045852935269,-215.283283));
#232369=CARTESIAN_POINT('Ctrl Pts',(39.1323070340084,-80.6389535267262,
-215.216616));
#232370=CARTESIAN_POINT('Ctrl Pts',(39.2262010432579,-80.6733217599254,
-215.149949));
#232371=CARTESIAN_POINT('Ctrl Pts',(-159.087812094948,8.022763120301,-376.750757000003));
#232372=CARTESIAN_POINT('Ctrl Pts',(-125.225689987698,-6.09414325472644,
-349.817289000002));
#232373=CARTESIAN_POINT('Ctrl Pts',(-91.3635678804476,-20.2110496297539,
-322.883821000001));
#232374=CARTESIAN_POINT('Ctrl Pts',(-57.5014457731974,-34.3279560047813,
-295.950353000001));
#232375=CARTESIAN_POINT('Ctrl Pts',(-40.5703847195723,-41.386409192295,
-282.483619000001));
#232376=CARTESIAN_POINT('Ctrl Pts',(-23.6393236659472,-48.4448623798088,
-269.016885));
#232377=CARTESIAN_POINT('Ctrl Pts',(-6.70826261232206,-55.5033155673225,
-255.550151000001));
#232378=CARTESIAN_POINT('Ctrl Pts',(1.75726791449049,-59.0325421610793,
-248.816784));
#232379=CARTESIAN_POINT('Ctrl Pts',(10.222798441303,-62.5617687548362,-242.083417));
#232380=CARTESIAN_POINT('Ctrl Pts',(18.6883289681156,-66.090995348593,-235.35005));
#232381=CARTESIAN_POINT('Ctrl Pts',(27.0700423609993,-69.585279104788,-228.68335));
#232382=CARTESIAN_POINT('Ctrl Pts',(35.4515990829499,-73.0798824232155,
-222.01665));
#232383=CARTESIAN_POINT('Ctrl Pts',(43.833000306127,-76.574805478098,-215.34995));
#232384=CARTESIAN_POINT('Ctrl Pts',(43.9168143183588,-76.6097547086468,
-215.283283));
#232385=CARTESIAN_POINT('Ctrl Pts',(44.0006283305905,-76.6447039391955,
-215.216616));
#232386=CARTESIAN_POINT('Ctrl Pts',(44.0844423428223,-76.6796531697443,
-215.149949));
#232387=CARTESIAN_POINT('Ctrl Pts',(-129.78792641513,13.512591939412,-376.750757));
#232388=CARTESIAN_POINT('Ctrl Pts',(-99.9994991430521,-0.854660588835203,
-349.817289000001));
#232389=CARTESIAN_POINT('Ctrl Pts',(-70.211071870974,-15.2219131170825,
-322.883821));
#232390=CARTESIAN_POINT('Ctrl Pts',(-40.4226445988958,-29.5891656453297,
-295.950353));
#232391=CARTESIAN_POINT('Ctrl Pts',(-25.5284309628568,-36.7727919094533,
-282.483619));
#232392=CARTESIAN_POINT('Ctrl Pts',(-10.6342173268177,-43.9564181735769,
-269.016885));
#232393=CARTESIAN_POINT('Ctrl Pts',(4.25999630922143,-51.1400444377006,
-255.550151));
#232394=CARTESIAN_POINT('Ctrl Pts',(11.707103127241,-54.7318575697624,-248.816784));
#232395=CARTESIAN_POINT('Ctrl Pts',(19.1542099452605,-58.3236707018242,
-242.083417));
#232396=CARTESIAN_POINT('Ctrl Pts',(26.60131676328,-61.915483833886,-235.35005));
#232397=CARTESIAN_POINT('Ctrl Pts',(33.9746898504281,-65.4717344596898,
-228.68335));
#232398=CARTESIAN_POINT('Ctrl Pts',(41.3480800753329,-69.0263711060389,
-222.01665));
#232399=CARTESIAN_POINT('Ctrl Pts',(48.7214815967444,-72.5793938958684,
-215.34995));
#232400=CARTESIAN_POINT('Ctrl Pts',(48.7952156119585,-72.6149241237667,
-215.283283));
#232401=CARTESIAN_POINT('Ctrl Pts',(48.8689496271726,-72.6504543516649,
-215.216616));
#232402=CARTESIAN_POINT('Ctrl Pts',(48.9426836423867,-72.6859845795632,
-215.149949));
#232403=CARTESIAN_POINT('Ctrl Pts',(-122.462954995176,14.8850491441897,
-376.750756999999));
#232404=CARTESIAN_POINT('Ctrl Pts',(-93.6929514318907,0.455210077637512,
-349.817289));
#232405=CARTESIAN_POINT('Ctrl Pts',(-64.9229478686056,-13.9746289889147,
-322.883821));
#232406=CARTESIAN_POINT('Ctrl Pts',(-36.1529443053205,-28.4044680554669,
-295.950353));
#232407=CARTESIAN_POINT('Ctrl Pts',(-21.7679425236779,-35.619387588743,
-282.483619));
#232408=CARTESIAN_POINT('Ctrl Pts',(-7.38294074203528,-42.834307122019,
-269.016885));
#232409=CARTESIAN_POINT('Ctrl Pts',(7.00206103960729,-50.0492266552951,
-255.550151));
#232410=CARTESIAN_POINT('Ctrl Pts',(14.1945619304286,-53.6566864219332,
-248.816784));
#232411=CARTESIAN_POINT('Ctrl Pts',(21.3870628212499,-57.2641461885712,
-242.083417));
#232412=CARTESIAN_POINT('Ctrl Pts',(28.5795637120712,-60.8716059552093,
-235.35005));
#232413=CARTESIAN_POINT('Ctrl Pts',(35.7008517227853,-64.4433482984152,
-228.68335));
#232414=CARTESIAN_POINT('Ctrl Pts',(42.8222003234286,-68.0129932767448,
-222.01665));
#232415=CARTESIAN_POINT('Ctrl Pts',(49.9436019193987,-71.5805410003109,
-215.34995));
#232416=CARTESIAN_POINT('Ctrl Pts',(50.0148159353584,-71.6162164775466,
-215.283283));
#232417=CARTESIAN_POINT('Ctrl Pts',(50.0860299513181,-71.6518919547823,
-215.216616));
#232418=CARTESIAN_POINT('Ctrl Pts',(50.1572439672778,-71.687567432018,-215.149949));
#232419=CARTESIAN_POINT('Ctrl Pts',(-103.0219124536,22.8222305961756,-376.750757000007));
#232420=CARTESIAN_POINT('Ctrl Pts',(-77.174697282254,7.34909250165779,-349.817289000007));
#232421=CARTESIAN_POINT('Ctrl Pts',(-51.3274821109085,-8.12404559286004,
-322.883821000005));
#232422=CARTESIAN_POINT('Ctrl Pts',(-25.480266939563,-23.5971836873778,
-295.950353000003));
#232423=CARTESIAN_POINT('Ctrl Pts',(-12.5566593538902,-31.3337527346368,
-282.483619000003));
#232424=CARTESIAN_POINT('Ctrl Pts',(0.366948231782582,-39.0703217818957,
-269.016885000003));
#232425=CARTESIAN_POINT('Ctrl Pts',(13.2905558174553,-46.8068908291546,
-255.550151000002));
#232426=CARTESIAN_POINT('Ctrl Pts',(19.7523596102917,-50.6751753527841,
-248.816784000002));
#232427=CARTESIAN_POINT('Ctrl Pts',(26.2141634031281,-54.5434598764135,
-242.083417000001));
#232428=CARTESIAN_POINT('Ctrl Pts',(32.6759671959645,-58.411744400043,-235.350050000001));
#232429=CARTESIAN_POINT('Ctrl Pts',(39.0737927334262,-62.2417290769038,
-228.683350000001));
#232430=CARTESIAN_POINT('Ctrl Pts',(45.4718450018044,-66.0691978041651,
-222.01665));
#232431=CARTESIAN_POINT('Ctrl Pts',(51.8701148758579,-69.894150514329,-215.34995));
#232432=CARTESIAN_POINT('Ctrl Pts',(51.9340975745985,-69.9324000414307,
-215.283283));
#232433=CARTESIAN_POINT('Ctrl Pts',(51.998080273339,-69.9706495685323,-215.216616));
#232434=CARTESIAN_POINT('Ctrl Pts',(52.0620629720796,-70.0088990956339,
-215.149949));
#232435=CARTESIAN_POINT('Ctrl Pts',(-71.4332298554826,45.3676034181815,
-376.750756999996));
#232436=CARTESIAN_POINT('Ctrl Pts',(-50.4371334176971,26.5324811107851,
-349.817288999997));
#232437=CARTESIAN_POINT('Ctrl Pts',(-29.4410369799117,7.69735880338874,
-322.883820999997));
#232438=CARTESIAN_POINT('Ctrl Pts',(-8.44494054212614,-11.1377635040076,
-295.950352999998));
#232439=CARTESIAN_POINT('Ctrl Pts',(2.05310767676661,-20.5553246577058,
-282.483618999998));
#232440=CARTESIAN_POINT('Ctrl Pts',(12.5511558956594,-29.972885811404,-269.016884999999));
#232441=CARTESIAN_POINT('Ctrl Pts',(23.0492041145521,-39.3904469651022,
-255.550150999999));
#232442=CARTESIAN_POINT('Ctrl Pts',(28.2982282239985,-44.0992275419513,
-248.816783999999));
#232443=CARTESIAN_POINT('Ctrl Pts',(33.5472523334448,-48.8080081188004,
-242.083416999999));
#232444=CARTESIAN_POINT('Ctrl Pts',(38.7962764428913,-53.5167886956495,
-235.35005));
#232445=CARTESIAN_POINT('Ctrl Pts',(43.9933300166005,-58.1789476826288,
-228.68335));
#232446=CARTESIAN_POINT('Ctrl Pts',(49.1909136386903,-62.839044754287,-222.01665));
#232447=CARTESIAN_POINT('Ctrl Pts',(54.3890197977427,-67.4970794092701,
-215.34995));
#232448=CARTESIAN_POINT('Ctrl Pts',(54.4410008593333,-67.5436597558199,
-215.283283));
#232449=CARTESIAN_POINT('Ctrl Pts',(54.4929819209238,-67.5902401023698,
-215.216616));
#232450=CARTESIAN_POINT('Ctrl Pts',(54.5449629825143,-67.6368204489196,
-215.149949));
#232451=CARTESIAN_POINT('Ctrl Pts',(-45.0390725903934,73.7599134480721,
-376.750757000003));
#232452=CARTESIAN_POINT('Ctrl Pts',(-28.0469137085574,50.6061693294573,
-349.817289000002));
#232453=CARTESIAN_POINT('Ctrl Pts',(-11.0547548267215,27.4524252108426,
-322.883821000002));
#232454=CARTESIAN_POINT('Ctrl Pts',(5.93740405511448,4.29868109222778,-295.950353000001));
#232455=CARTESIAN_POINT('Ctrl Pts',(14.4334834960324,-7.2781909670796,-282.483619000001));
#232456=CARTESIAN_POINT('Ctrl Pts',(22.9295629369504,-18.855063026387,-269.016885000001));
#232457=CARTESIAN_POINT('Ctrl Pts',(31.4256423778684,-30.4319350856944,
-255.550151000001));
#232458=CARTESIAN_POINT('Ctrl Pts',(35.6736820983274,-36.2203711153481,
-248.816784000001));
#232459=CARTESIAN_POINT('Ctrl Pts',(39.9217218187864,-42.0088071450018,
-242.083417000001));
#232460=CARTESIAN_POINT('Ctrl Pts',(44.1697615392454,-47.7972431746554,
-235.35005));
#232461=CARTESIAN_POINT('Ctrl Pts',(48.3757414604919,-53.5283679564908,
-228.68335));
#232462=CARTESIAN_POINT('Ctrl Pts',(52.582425249623,-59.2584041216488,-222.01665));
#232463=CARTESIAN_POINT('Ctrl Pts',(56.7898089004066,-64.9873508559399,
-215.34995));
#232464=CARTESIAN_POINT('Ctrl Pts',(56.8318827369145,-65.0446403232828,
-215.283283));
#232465=CARTESIAN_POINT('Ctrl Pts',(56.8739565734223,-65.1019297906258,
-215.216616));
#232466=CARTESIAN_POINT('Ctrl Pts',(56.9160304099302,-65.1592192579687,
-215.149949));
#232467=CARTESIAN_POINT('Ctrl Pts',(-34.4954719600033,91.6721063226136,
-376.750757));
#232468=CARTESIAN_POINT('Ctrl Pts',(-18.9810705532065,65.8496728858911,
-349.817289000001));
#232469=CARTESIAN_POINT('Ctrl Pts',(-3.46666914640964,40.0272394491684,
-322.883821));
#232470=CARTESIAN_POINT('Ctrl Pts',(12.0477322603872,14.2048060124459,-295.950353));
#232471=CARTESIAN_POINT('Ctrl Pts',(19.8049329637856,1.2935892940846,-282.483619));
#232472=CARTESIAN_POINT('Ctrl Pts',(27.562133667184,-11.6176274242767,-269.016885));
#232473=CARTESIAN_POINT('Ctrl Pts',(35.3193343705824,-24.528844142638,-255.550151));
#232474=CARTESIAN_POINT('Ctrl Pts',(39.1979347222817,-30.9844525018186,
-248.816784));
#232475=CARTESIAN_POINT('Ctrl Pts',(43.0765350739809,-37.4400608609993,
-242.083417));
#232476=CARTESIAN_POINT('Ctrl Pts',(46.9551354256801,-43.8956692201799,
-235.35005));
#232477=CARTESIAN_POINT('Ctrl Pts',(50.7953337936991,-50.2873606649132,
-228.68335));
#232478=CARTESIAN_POINT('Ctrl Pts',(54.6361431746697,-56.6785834369767,
-222.01665));
#232479=CARTESIAN_POINT('Ctrl Pts',(58.477561814447,-63.069336786611,-215.34995));
#232480=CARTESIAN_POINT('Ctrl Pts',(58.5159760008448,-63.1332443201074,
-215.283283));
#232481=CARTESIAN_POINT('Ctrl Pts',(58.5543901872426,-63.1971518536037,
-215.216616));
#232482=CARTESIAN_POINT('Ctrl Pts',(58.5928043736403,-63.2610593871,-215.149949));
#232483=CARTESIAN_POINT('Ctrl Pts',(-31.8464935875069,98.4079754366887,
-376.750756999999));
#232484=CARTESIAN_POINT('Ctrl Pts',(-16.6079109017479,71.6637374050134,
-349.817289));
#232485=CARTESIAN_POINT('Ctrl Pts',(-1.36932821598904,44.919499373338,-322.883821));
#232486=CARTESIAN_POINT('Ctrl Pts',(13.8692544697699,18.1752613416626,-295.950353));
#232487=CARTESIAN_POINT('Ctrl Pts',(21.4885458126493,4.80314232582491,-282.483619));
#232488=CARTESIAN_POINT('Ctrl Pts',(29.1078371555287,-8.56897669001278,
-269.016885));
#232489=CARTESIAN_POINT('Ctrl Pts',(36.7271284984082,-21.9410957058504,
-255.550151));
#232490=CARTESIAN_POINT('Ctrl Pts',(40.5367741698479,-28.6271552137693,
-248.816784));
#232491=CARTESIAN_POINT('Ctrl Pts',(44.3464198412877,-35.3132147216881,
-242.083417));
#232492=CARTESIAN_POINT('Ctrl Pts',(48.1560655127274,-41.999274229607,-235.35005));
#232493=CARTESIAN_POINT('Ctrl Pts',(51.9279919200935,-48.6191351285365,
-228.68335));
#232494=CARTESIAN_POINT('Ctrl Pts',(55.7004001286368,-55.2387363218615,
-222.01665));
#232495=CARTESIAN_POINT('Ctrl Pts',(59.4732891526772,-61.8580772083615,
-215.34995));
#232496=CARTESIAN_POINT('Ctrl Pts',(59.5110180429176,-61.9242706172265,
-215.283283));
#232497=CARTESIAN_POINT('Ctrl Pts',(59.548746933158,-61.9904640260915,-215.216616));
#232498=CARTESIAN_POINT('Ctrl Pts',(59.5864758233984,-62.0566574349565,
-215.149949));
#232499=CARTESIAN_POINT('Ctrl Pts',(-21.2505800975213,125.351451892989,
-376.750756999997));
#232500=CARTESIAN_POINT('Ctrl Pts',(-7.11527229591406,94.9199954815027,
-349.817288999997));
#232501=CARTESIAN_POINT('Ctrl Pts',(7.02003550569317,64.4885390700161,-322.883820999998));
#232502=CARTESIAN_POINT('Ctrl Pts',(21.1553433073004,34.0570826585295,-295.950352999998));
#232503=CARTESIAN_POINT('Ctrl Pts',(28.222997208104,18.8413544527863,-282.483618999999));
#232504=CARTESIAN_POINT('Ctrl Pts',(35.2906511089077,3.62562624704296,-269.016884999999));
#232505=CARTESIAN_POINT('Ctrl Pts',(42.3583050097113,-11.5901019587003,
-255.550151));
#232506=CARTESIAN_POINT('Ctrl Pts',(45.8921319601131,-19.197966061572,-248.816784));
#232507=CARTESIAN_POINT('Ctrl Pts',(49.4259589105149,-26.8058301644436,
-242.083417));
#232508=CARTESIAN_POINT('Ctrl Pts',(52.9597858609167,-34.4136942673153,
-235.35005));
#232509=CARTESIAN_POINT('Ctrl Pts',(56.458624425671,-41.9462329830297,-228.68335));
#232510=CARTESIAN_POINT('Ctrl Pts',(59.957427944505,-49.4793478614006,-222.01665));
#232511=CARTESIAN_POINT('Ctrl Pts',(63.4561985055979,-57.0130388953633,
-215.34995));
#232512=CARTESIAN_POINT('Ctrl Pts',(63.4911862112088,-57.0883758057029,
-215.283283));
#232513=CARTESIAN_POINT('Ctrl Pts',(63.5261739168198,-57.1637127160426,
-215.216616));
#232514=CARTESIAN_POINT('Ctrl Pts',(63.5611616224307,-57.2390496263822,
-215.149949));
#232515=CARTESIAN_POINT('Ctrl Pts',(-10.6546666075359,152.29492834929,-376.750756999995));
#232516=CARTESIAN_POINT('Ctrl Pts',(2.37736630991967,118.176253557992,-349.817288999995));
#232517=CARTESIAN_POINT('Ctrl Pts',(15.4093992273753,84.0575787666943,-322.883820999996));
#232518=CARTESIAN_POINT('Ctrl Pts',(28.4414321448309,49.9389039753965,-295.950352999998));
#232519=CARTESIAN_POINT('Ctrl Pts',(34.9574486035587,32.8795665797476,-282.483618999998));
#232520=CARTESIAN_POINT('Ctrl Pts',(41.4734650622865,15.8202291840987,-269.016884999999));
#232521=CARTESIAN_POINT('Ctrl Pts',(47.9894815210143,-1.2391082115502,-255.550151));
#232522=CARTESIAN_POINT('Ctrl Pts',(51.2474897503782,-9.76877690937465,
-248.816784));
#232523=CARTESIAN_POINT('Ctrl Pts',(54.5054979797421,-18.2984456071991,
-242.083417));
#232524=CARTESIAN_POINT('Ctrl Pts',(57.763506209106,-26.8281143050236,-235.35005));
#232525=CARTESIAN_POINT('Ctrl Pts',(60.9892569312485,-35.273330837523,-228.683350000001));
#232526=CARTESIAN_POINT('Ctrl Pts',(64.2144557603733,-43.7199594009398,
-222.016650000001));
#232527=CARTESIAN_POINT('Ctrl Pts',(67.4391078585187,-52.1680005823651,
-215.349950000001));
#232528=CARTESIAN_POINT('Ctrl Pts',(67.4713543795001,-52.2524809941794,
-215.283283000001));
#232529=CARTESIAN_POINT('Ctrl Pts',(67.5036009004816,-52.3369614059937,
-215.216616));
#232530=CARTESIAN_POINT('Ctrl Pts',(67.535847421463,-52.4214418178079,-215.149949000001));
#232531=CARTESIAN_POINT('Ctrl Pts',(-0.0587531175507312,179.238404805591,
-376.750756999993));
#232532=CARTESIAN_POINT('Ctrl Pts',(11.8700049157533,141.432511634481,-349.817288999993));
#232533=CARTESIAN_POINT('Ctrl Pts',(23.7987629490573,103.626618463372,-322.883820999995));
#232534=CARTESIAN_POINT('Ctrl Pts',(35.7275209823613,65.8207252922634,-295.950352999997));
#232535=CARTESIAN_POINT('Ctrl Pts',(41.6918999990133,46.9177787067089,-282.483618999997));
#232536=CARTESIAN_POINT('Ctrl Pts',(47.6562790156653,28.0148321211544,-269.016884999998));
#232537=CARTESIAN_POINT('Ctrl Pts',(53.6206580323173,9.11188553559992,-255.550150999999));
#232538=CARTESIAN_POINT('Ctrl Pts',(56.6028475406433,-0.339587757177323,
-248.816784));
#232539=CARTESIAN_POINT('Ctrl Pts',(59.5850370489693,-9.79106104995457,
-242.083416999999));
#232540=CARTESIAN_POINT('Ctrl Pts',(62.5672265572953,-19.2425343427318,
-235.35005));
#232541=CARTESIAN_POINT('Ctrl Pts',(65.519889436826,-28.6004286920162,-228.683350000001));
#232542=CARTESIAN_POINT('Ctrl Pts',(68.4714835762416,-37.9605709404789,
-222.016650000001));
#232543=CARTESIAN_POINT('Ctrl Pts',(71.4220172114394,-47.322962269367,-215.349950000001));
#232544=CARTESIAN_POINT('Ctrl Pts',(71.4515225477914,-47.4165861826559,
-215.283283000001));
#232545=CARTESIAN_POINT('Ctrl Pts',(71.4810278841433,-47.5102100959448,
-215.216616));
#232546=CARTESIAN_POINT('Ctrl Pts',(71.5105332204953,-47.6038340092336,
-215.149949000001));
#232547=CARTESIAN_POINT('Ctrl Pts',(31.728987352405,260.068834174492,-376.750756999986));
#232548=CARTESIAN_POINT('Ctrl Pts',(40.3479207332542,211.20128586395,-349.817288999988));
#232549=CARTESIAN_POINT('Ctrl Pts',(48.9668541141034,162.333737553407,-322.883820999991));
#232550=CARTESIAN_POINT('Ctrl Pts',(57.5857874949526,113.466189242864,-295.950352999994));
#232551=CARTESIAN_POINT('Ctrl Pts',(61.8952541853772,89.0324150875929,-282.483618999995));
#232552=CARTESIAN_POINT('Ctrl Pts',(66.2047208758018,64.5986409323216,-269.016884999996));
#232553=CARTESIAN_POINT('Ctrl Pts',(70.5141875662264,40.1648667770503,-255.550150999998));
#232554=CARTESIAN_POINT('Ctrl Pts',(72.6689209114386,27.9479796994146,-248.816783999999));
#232555=CARTESIAN_POINT('Ctrl Pts',(74.8236542566509,15.731092621779,-242.083416999999));
#232556=CARTESIAN_POINT('Ctrl Pts',(76.9783876018632,3.51420554414337,-235.35005));
#232557=CARTESIAN_POINT('Ctrl Pts',(79.1117869535586,-8.58172225549588,
-228.683350000001));
#232558=CARTESIAN_POINT('Ctrl Pts',(81.2425670238464,-20.6824055590965,
-222.016650000001));
#232559=CARTESIAN_POINT('Ctrl Pts',(83.3707452702016,-32.7878473303725,
-215.349950000001));
#232560=CARTESIAN_POINT('Ctrl Pts',(83.3920270526652,-32.9089017480852,
-215.283283000001));
#232561=CARTESIAN_POINT('Ctrl Pts',(83.4133088351287,-33.0299561657981,
-215.216616));
#232562=CARTESIAN_POINT('Ctrl Pts',(83.4345906175922,-33.1510105835108,
-215.149949000001));
#232563=CARTESIAN_POINT('Ctrl Pts',(63.5167278223608,340.899263543393,-376.750756999979));
#232564=CARTESIAN_POINT('Ctrl Pts',(68.8258365507552,280.970060093418,-349.817288999983));
#232565=CARTESIAN_POINT('Ctrl Pts',(74.1349452791495,221.040856643441,-322.883820999986));
#232566=CARTESIAN_POINT('Ctrl Pts',(79.4440540075439,161.111653193465,-295.950352999991));
#232567=CARTESIAN_POINT('Ctrl Pts',(82.098608371741,131.147051468477,-282.483618999993));
#232568=CARTESIAN_POINT('Ctrl Pts',(84.7531627359382,101.182449743489,-269.016884999995));
#232569=CARTESIAN_POINT('Ctrl Pts',(87.4077171001354,71.2178480185007,-255.550150999997));
#232570=CARTESIAN_POINT('Ctrl Pts',(88.734994282234,56.2355471560066,-248.816783999998));
#232571=CARTESIAN_POINT('Ctrl Pts',(90.0622714643326,41.2532462935126,-242.083416999999));
#232572=CARTESIAN_POINT('Ctrl Pts',(91.3895486464312,26.2709454310185,-235.35005));
#232573=CARTESIAN_POINT('Ctrl Pts',(92.7036844702911,11.4369841810244,-228.683350000001));
#232574=CARTESIAN_POINT('Ctrl Pts',(94.0136504714512,-3.40424017771396,
-222.016650000001));
#232575=CARTESIAN_POINT('Ctrl Pts',(95.3194733289638,-18.252732391378,-215.349950000001));
#232576=CARTESIAN_POINT('Ctrl Pts',(95.3325315575389,-18.4012173135146,
-215.283283000001));
#232577=CARTESIAN_POINT('Ctrl Pts',(95.345589786114,-18.5497022356513,-215.216616000001));
#232578=CARTESIAN_POINT('Ctrl Pts',(95.3586480146891,-18.698187157788,-215.149949000001));
#232579=CARTESIAN_POINT('Ctrl Pts',(95.3044682923166,421.729692912295,-376.750756999971));
#232580=CARTESIAN_POINT('Ctrl Pts',(97.3037523682561,350.738834322885,-349.817288999976));
#232581=CARTESIAN_POINT('Ctrl Pts',(99.3030364441956,279.747975733475,-322.883820999982));
#232582=CARTESIAN_POINT('Ctrl Pts',(101.302320520135,208.757117144065,-295.950352999988));
#232583=CARTESIAN_POINT('Ctrl Pts',(102.301962558105,173.261687849361,-282.48361899999));
#232584=CARTESIAN_POINT('Ctrl Pts',(103.301604596075,137.766258554656,-269.016884999993));
#232585=CARTESIAN_POINT('Ctrl Pts',(104.301246634044,102.270829259951,-255.550150999996));
#232586=CARTESIAN_POINT('Ctrl Pts',(104.801067653029,84.5231146125986,-248.816783999998));
#232587=CARTESIAN_POINT('Ctrl Pts',(105.300888672014,66.7753999652462,-242.083416999998));
#232588=CARTESIAN_POINT('Ctrl Pts',(105.800709690999,49.0276853178937,-235.35005));
#232589=CARTESIAN_POINT('Ctrl Pts',(106.295581987024,31.4556906175448,-228.683350000001));
#232590=CARTESIAN_POINT('Ctrl Pts',(106.784733919056,13.8739252036685,-222.016650000002));
#232591=CARTESIAN_POINT('Ctrl Pts',(107.268201387726,-3.71761745238349,
-215.349950000002));
#232592=CARTESIAN_POINT('Ctrl Pts',(107.273036062413,-3.89353287894403,
-215.283283000002));
#232593=CARTESIAN_POINT('Ctrl Pts',(107.277870737099,-4.06944830550458,
-215.216616000002));
#232594=CARTESIAN_POINT('Ctrl Pts',(107.282705411786,-4.24536373206513,
-215.149949000001));
#232595=CARTESIAN_POINT('Ctrl Pts',(190.667689702184,664.220981018999,-376.750756999951));
#232596=CARTESIAN_POINT('Ctrl Pts',(182.737499820759,560.045157011288,-349.81728899996));
#232597=CARTESIAN_POINT('Ctrl Pts',(174.807309939334,455.869333003578,-322.883820999969));
#232598=CARTESIAN_POINT('Ctrl Pts',(166.877120057909,351.693508995868,-295.950352999979));
#232599=CARTESIAN_POINT('Ctrl Pts',(162.912025117196,299.605596992013,-282.483618999983));
#232600=CARTESIAN_POINT('Ctrl Pts',(158.946930176484,247.517684988157,-269.016884999988));
#232601=CARTESIAN_POINT('Ctrl Pts',(154.981835235771,195.429772984302,-255.550150999993));
#232602=CARTESIAN_POINT('Ctrl Pts',(152.999287765415,169.385816982375,-248.816783999995));
#232603=CARTESIAN_POINT('Ctrl Pts',(151.016740295059,143.341860980447,-242.083416999997));
#232604=CARTESIAN_POINT('Ctrl Pts',(149.034192824703,117.297904978519,-235.35005));
#232605=CARTESIAN_POINT('Ctrl Pts',(147.071274537221,91.5118099271058,-228.683350000003));
#232606=CARTESIAN_POINT('Ctrl Pts',(145.09798426187,65.708421347816,-222.016650000002));
#232607=CARTESIAN_POINT('Ctrl Pts',(143.114385564013,39.8877273646,-215.349950000003));
#232608=CARTESIAN_POINT('Ctrl Pts',(143.094549577034,39.6295204247678,-215.283283000003));
#232609=CARTESIAN_POINT('Ctrl Pts',(143.074713590055,39.3713134849356,-215.216616000002));
#232610=CARTESIAN_POINT('Ctrl Pts',(143.054877603077,39.1131065451034,-215.149949000002));
#232611=CARTESIAN_POINT('Ctrl Pts',(286.030911112051,906.712269125702,-376.750756999929));
#232612=CARTESIAN_POINT('Ctrl Pts',(268.171247273262,769.351479699691,-349.817288999943));
#232613=CARTESIAN_POINT('Ctrl Pts',(250.311583434473,631.990690273681,-322.883820999956));
#232614=CARTESIAN_POINT('Ctrl Pts',(232.451919595683,494.62990084767,-295.95035299997));
#232615=CARTESIAN_POINT('Ctrl Pts',(223.522087676288,425.949506134664,-282.483618999976));
#232616=CARTESIAN_POINT('Ctrl Pts',(214.592255756894,357.269111421658,-269.016884999983));
#232617=CARTESIAN_POINT('Ctrl Pts',(205.662423837499,288.588716708654,-255.55015099999));
#232618=CARTESIAN_POINT('Ctrl Pts',(201.197507877801,254.24851935215,-248.816783999994));
#232619=CARTESIAN_POINT('Ctrl Pts',(196.732591918104,219.908321995647,-242.083416999997));
#232620=CARTESIAN_POINT('Ctrl Pts',(192.267675958407,185.568124639145,-235.35005));
#232621=CARTESIAN_POINT('Ctrl Pts',(187.846967087419,151.567929236667,-228.683350000004));
#232622=CARTESIAN_POINT('Ctrl Pts',(183.411234604685,117.542917491964,-222.016650000003));
#232623=CARTESIAN_POINT('Ctrl Pts',(178.960569740299,83.4930721815835,-215.349950000004));
#232624=CARTESIAN_POINT('Ctrl Pts',(178.916063091656,83.1525737284796,-215.283283000004));
#232625=CARTESIAN_POINT('Ctrl Pts',(178.871556443012,82.8120752753758,-215.216616000004));
#232626=CARTESIAN_POINT('Ctrl Pts',(178.827049794367,82.4715768222719,-215.149949000004));
#232627=CARTESIAN_POINT('Ctrl Pts',(381.394132521918,1149.20355723241,-376.750756999909));
#232628=CARTESIAN_POINT('Ctrl Pts',(353.604994725765,978.657802388094,-349.817288999926));
#232629=CARTESIAN_POINT('Ctrl Pts',(325.815856929611,808.112047543783,-322.883820999944));
#232630=CARTESIAN_POINT('Ctrl Pts',(298.026719133457,637.566292699472,-295.950352999961));
#232631=CARTESIAN_POINT('Ctrl Pts',(284.13215023538,552.293415277316,-282.48361899997));
#232632=CARTESIAN_POINT('Ctrl Pts',(270.237581337303,467.02053785516,-269.016884999978));
#232633=CARTESIAN_POINT('Ctrl Pts',(256.343012439226,381.747660433005,-255.550150999987));
#232634=CARTESIAN_POINT('Ctrl Pts',(249.395727990188,339.111221721927,-248.816783999992));
#232635=CARTESIAN_POINT('Ctrl Pts',(242.448443541149,296.474783010849,-242.083416999996));
#232636=CARTESIAN_POINT('Ctrl Pts',(235.501159092111,253.83834429977,-235.35005));
#232637=CARTESIAN_POINT('Ctrl Pts',(228.622659637617,211.624048546228,-228.683350000005));
#232638=CARTESIAN_POINT('Ctrl Pts',(221.724484947499,169.377413636111,-222.016650000005));
#232639=CARTESIAN_POINT('Ctrl Pts',(214.806753916586,127.098416998567,-215.349950000004));
#232640=CARTESIAN_POINT('Ctrl Pts',(214.737576606277,126.675627032191,-215.283283000005));
#232641=CARTESIAN_POINT('Ctrl Pts',(214.668399295968,126.252837065816,-215.216616000005));
#232642=CARTESIAN_POINT('Ctrl Pts',(214.599221985659,125.83004709944,-215.149949000005));
#232643=CARTESIAN_POINT('Ctrl Pts',(667.483796751521,1876.67742155251,-376.750756999846));
#232644=CARTESIAN_POINT('Ctrl Pts',(609.906237083273,1606.57677045331,-349.817288999875));
#232645=CARTESIAN_POINT('Ctrl Pts',(552.328677415026,1336.47611935409,-322.883820999905));
#232646=CARTESIAN_POINT('Ctrl Pts',(494.751117746779,1066.37546825488,-295.950352999934));
#232647=CARTESIAN_POINT('Ctrl Pts',(465.962337912655,931.325142705271,-282.483618999949));
#232648=CARTESIAN_POINT('Ctrl Pts',(437.173558078531,796.274817155664,-269.016884999963));
#232649=CARTESIAN_POINT('Ctrl Pts',(408.384778244408,661.224491606058,-255.550150999978));
#232650=CARTESIAN_POINT('Ctrl Pts',(393.990388327346,593.699328831254,-248.816783999986));
#232651=CARTESIAN_POINT('Ctrl Pts',(379.595998410284,526.174166056451,-242.083416999993));
#232652=CARTESIAN_POINT('Ctrl Pts',(365.201608493222,458.649003281647,-235.35005));
#232653=CARTESIAN_POINT('Ctrl Pts',(350.94973728821,391.792406474911,-228.683350000008));
#232654=CARTESIAN_POINT('Ctrl Pts',(336.664235975943,324.880902068554,-222.016650000008));
#232655=CARTESIAN_POINT('Ctrl Pts',(322.345306445446,257.914451449517,-215.349950000008));
#232656=CARTESIAN_POINT('Ctrl Pts',(322.202117150141,257.244786943327,-215.283283000008));
#232657=CARTESIAN_POINT('Ctrl Pts',(322.058927854835,256.575122437136,-215.216616000008));
#232658=CARTESIAN_POINT('Ctrl Pts',(321.91573855953,255.905457930946,-215.149949000007));
#232659=CARTESIAN_POINT('Ctrl Pts',(953.573460981123,2604.15128587263,-376.750756999783));
#232660=CARTESIAN_POINT('Ctrl Pts',(866.207479440782,2234.49573851851,-349.817288999824));
#232661=CARTESIAN_POINT('Ctrl Pts',(778.841497900441,1864.8401911644,-322.883820999866));
#232662=CARTESIAN_POINT('Ctrl Pts',(691.4755163601,1495.18464381028,-295.950352999906));
#232663=CARTESIAN_POINT('Ctrl Pts',(647.79252558993,1310.35687013323,-282.483618999927));
#232664=CARTESIAN_POINT('Ctrl Pts',(604.109534819759,1125.52909645617,-269.016884999948));
#232665=CARTESIAN_POINT('Ctrl Pts',(560.426544049589,940.701322779111,-255.550150999969));
#232666=CARTESIAN_POINT('Ctrl Pts',(538.585048664503,848.287435940582,-248.81678399998));
#232667=CARTESIAN_POINT('Ctrl Pts',(516.743553279418,755.873549102053,-242.08341699999));
#232668=CARTESIAN_POINT('Ctrl Pts',(494.902057894333,663.459662263524,-235.35005));
#232669=CARTESIAN_POINT('Ctrl Pts',(473.276814938803,571.960764403594,-228.683350000011));
#232670=CARTESIAN_POINT('Ctrl Pts',(451.603987004386,480.384390500996,-222.016650000011));
#232671=CARTESIAN_POINT('Ctrl Pts',(429.883858974306,388.730485900468,-215.34995000001));
#232672=CARTESIAN_POINT('Ctrl Pts',(429.666657694005,387.813946854463,-215.28328300001));
#232673=CARTESIAN_POINT('Ctrl Pts',(429.449456413704,386.897407808457,-215.216616000011));
#232674=CARTESIAN_POINT('Ctrl Pts',(429.232255133403,385.980868762451,-215.149949000011));
#232675=CARTESIAN_POINT('Ctrl Pts',(1239.66312521072,3331.62515019274,-376.750756999719));
#232676=CARTESIAN_POINT('Ctrl Pts',(1122.50872179829,2862.41470658373,-349.817288999773));
#232677=CARTESIAN_POINT('Ctrl Pts',(1005.35431838586,2393.20426297471,-322.883820999826));
#232678=CARTESIAN_POINT('Ctrl Pts',(888.199914973422,1923.99381936569,-295.95035299988));
#232679=CARTESIAN_POINT('Ctrl Pts',(829.622713267204,1689.38859756118,-282.483618999906));
#232680=CARTESIAN_POINT('Ctrl Pts',(771.045511560987,1454.78337575667,-269.016884999933));
#232681=CARTESIAN_POINT('Ctrl Pts',(712.46830985477,1220.17815395216,-255.55015099996));
#232682=CARTESIAN_POINT('Ctrl Pts',(683.179709001661,1102.87554304991,-248.816783999974));
#232683=CARTESIAN_POINT('Ctrl Pts',(653.891108148553,985.572932147655,-242.083416999987));
#232684=CARTESIAN_POINT('Ctrl Pts',(624.602507295445,868.2703212454,-235.35005));
#232685=CARTESIAN_POINT('Ctrl Pts',(595.603892589396,752.129122332277,-228.683350000014));
#232686=CARTESIAN_POINT('Ctrl Pts',(566.54373803283,635.887878933439,-222.016650000014));
#232687=CARTESIAN_POINT('Ctrl Pts',(537.422411503166,519.546520351418,-215.349950000014));
#232688=CARTESIAN_POINT('Ctrl Pts',(537.131198237869,518.383106765598,-215.283283000013));
#232689=CARTESIAN_POINT('Ctrl Pts',(536.839984972572,517.219693179777,-215.216616000014));
#232690=CARTESIAN_POINT('Ctrl Pts',(536.548771707275,516.056279593957,-215.149949000014));
#232691=CARTESIAN_POINT('Ctrl Pts',(2097.93211789953,5514.04674315307,-376.750756999531));
#232692=CARTESIAN_POINT('Ctrl Pts',(1891.41244887082,4746.17161077935,-349.81728899962));
#232693=CARTESIAN_POINT('Ctrl Pts',(1684.8927798421,3978.29647840563,-322.88382099971));
#232694=CARTESIAN_POINT('Ctrl Pts',(1478.37311081339,3210.42134603191,-295.950352999799));
#232695=CARTESIAN_POINT('Ctrl Pts',(1375.11327629903,2826.48377984504,-282.483618999843));
#232696=CARTESIAN_POINT('Ctrl Pts',(1271.85344178467,2442.54621365819,-269.016884999889));
#232697=CARTESIAN_POINT('Ctrl Pts',(1168.59360727031,2058.60864747133,-255.550150999933));
#232698=CARTESIAN_POINT('Ctrl Pts',(1116.96369001313,1866.6398643779,-248.816783999956));
#232699=CARTESIAN_POINT('Ctrl Pts',(1065.33377275596,1674.67108128446,-242.083416999977));
#232700=CARTESIAN_POINT('Ctrl Pts',(1013.70385549878,1482.70229819103,-235.35005));
#232701=CARTESIAN_POINT('Ctrl Pts',(962.585125541175,1292.63419611833,-228.683350000023));
#232702=CARTESIAN_POINT('Ctrl Pts',(911.362991118159,1102.39834423077,-222.016650000023));
#232703=CARTESIAN_POINT('Ctrl Pts',(860.038069089746,911.99462370427,-215.349950000023));
#232704=CARTESIAN_POINT('Ctrl Pts',(859.524819869462,910.090586499004,-215.283283000022));
#232705=CARTESIAN_POINT('Ctrl Pts',(859.011570649176,908.186549293739,-215.216616000022));
#232706=CARTESIAN_POINT('Ctrl Pts',(858.498321428892,906.282512088474,-215.149949000023));
#232707=CARTESIAN_POINT('Ctrl Pts',(2956.20111058834,7696.4683361134,-376.750756999341));
#232708=CARTESIAN_POINT('Ctrl Pts',(2660.31617594335,6629.92851497498,-349.817288999467));
#232709=CARTESIAN_POINT('Ctrl Pts',(2364.43124129834,5563.38869383655,-322.883820999593));
#232710=CARTESIAN_POINT('Ctrl Pts',(2068.54630665335,4496.84887269812,-295.950352999718));
#232711=CARTESIAN_POINT('Ctrl Pts',(1920.60383933086,3963.57896212891,-282.48361899978));
#232712=CARTESIAN_POINT('Ctrl Pts',(1772.66137200836,3430.3090515597,-269.016884999844));
#232713=CARTESIAN_POINT('Ctrl Pts',(1624.71890468586,2897.03914099049,-255.550150999906));
#232714=CARTESIAN_POINT('Ctrl Pts',(1550.74767102461,2630.40418570588,-248.816783999938));
#232715=CARTESIAN_POINT('Ctrl Pts',(1476.77643736336,2363.76923042127,-242.083416999969));
#232716=CARTESIAN_POINT('Ctrl Pts',(1402.80520370211,2097.13427513666,-235.35005));
#232717=CARTESIAN_POINT('Ctrl Pts',(1329.56635849295,1833.13926990437,-228.683350000032));
#232718=CARTESIAN_POINT('Ctrl Pts',(1256.18224420349,1568.9088095281,-222.016650000032));
#232719=CARTESIAN_POINT('Ctrl Pts',(1182.65372667633,1304.44272705712,-215.349950000032));
#232720=CARTESIAN_POINT('Ctrl Pts',(1181.91844150105,1301.79806623241,-215.283283000032));
#232721=CARTESIAN_POINT('Ctrl Pts',(1181.18315632578,1299.1534054077,-215.216616000032));
#232722=CARTESIAN_POINT('Ctrl Pts',(1180.44787115051,1296.50874458299,-215.149949000032));
#232723=CARTESIAN_POINT('Ctrl Pts',(3814.47010327714,9878.88992907374,-376.750756999153));
#232724=CARTESIAN_POINT('Ctrl Pts',(3429.21990301587,8513.68541917061,-349.817288999315));
#232725=CARTESIAN_POINT('Ctrl Pts',(3043.96970275459,7148.48090926748,-322.883820999476));
#232726=CARTESIAN_POINT('Ctrl Pts',(2658.71950249332,5783.27639936434,-295.950352999637));
#232727=CARTESIAN_POINT('Ctrl Pts',(2466.09440236268,5100.67414441278,-282.483618999717));
#232728=CARTESIAN_POINT('Ctrl Pts',(2273.46930223204,4418.07188946121,-269.016884999799));
#232729=CARTESIAN_POINT('Ctrl Pts',(2080.84420210141,3735.46963450965,-255.550150999879));
#232730=CARTESIAN_POINT('Ctrl Pts',(1984.53165203609,3394.16850703386,-248.81678399992));
#232731=CARTESIAN_POINT('Ctrl Pts',(1888.21910197076,3052.86737955808,-242.08341699996));
#232732=CARTESIAN_POINT('Ctrl Pts',(1791.90655190545,2711.56625208229,-235.35005));
#232733=CARTESIAN_POINT('Ctrl Pts',(1696.54759144473,2373.64434369042,-228.683350000041));
#232734=CARTESIAN_POINT('Ctrl Pts',(1601.00149728882,2035.41927482542,-222.016650000041));
#232735=CARTESIAN_POINT('Ctrl Pts',(1505.26938426291,1696.89083040998,-215.349950000041));
#232736=CARTESIAN_POINT('Ctrl Pts',(1504.31206313264,1693.50554596582,-215.28328300004));
#232737=CARTESIAN_POINT('Ctrl Pts',(1503.35474200239,1690.12026152166,-215.216616000041));
#232738=CARTESIAN_POINT('Ctrl Pts',(1502.39742087213,1686.7349770775,-215.149949000041));
#232739=CARTESIAN_POINT('Origin',(-636.934816028482,-11.5034818258361,-229.35005));
#232740=CARTESIAN_POINT('Origin',(-636.934816028482,-11.5034818258361,-229.35005));
#232741=CARTESIAN_POINT('Origin',(-636.934816028482,-11.5034818258361,-229.35005));
#232742=CARTESIAN_POINT('Origin',(-636.934816028482,-11.5034818258361,-229.35005));
#232743=CARTESIAN_POINT('Origin',(-636.934816028482,-11.5034818258361,-229.35005));
#232744=CARTESIAN_POINT('Origin',(0.,-32.21456093117,-229.35005));
#232745=CARTESIAN_POINT('Origin',(0.,-33.21456093117,-229.35005));
#232746=CARTESIAN_POINT('Origin',(-2.22174260618994E-13,-11.0034818258363,
-229.35005));
#232747=CARTESIAN_POINT('Origin',(-2.22174260618994E-13,-12.0034818258363,
-229.35005));
#232748=CARTESIAN_POINT('Origin',(-1.54373336646987E-15,-42.8201004838369,
-229.35005));
#232749=CARTESIAN_POINT('Origin',(-1.23757166668304E-15,-43.8201004838368,
-229.35005));
#232750=CARTESIAN_POINT('Origin',(-2.8425373731103E-15,9.20759727949731,
-229.35005));
#232751=CARTESIAN_POINT('Origin',(-2.53637567332344E-15,10.2075972794973,
-229.35005));
#232752=CARTESIAN_POINT('Origin',(-1.54373336646988E-15,19.8131368321642,
-229.35005));
#232753=CARTESIAN_POINT('Origin',(-1.23757166668304E-15,20.8131368321642,
-229.35005));
#232754=CARTESIAN_POINT('Origin',(-2.61456814389029E-14,-173.57701443073,
-229.35005));
#232755=CARTESIAN_POINT('Origin',(7.14692237356698E-14,623.509175991979,
-229.35005));
#232756=CARTESIAN_POINT('Origin',(-2.61456814389029E-14,-173.57701443073,
-229.35005));
#232757=CARTESIAN_POINT('Origin',(-2.61456814389029E-14,-173.57701443073,
-232.25005));
#232758=CARTESIAN_POINT('Origin',(-2.61456814389029E-14,-173.57701443073,
-229.35005));
#232759=CARTESIAN_POINT('Origin',(-2.61456814389029E-14,-173.57701443073,
-232.25005));
#232760=CARTESIAN_POINT('Origin',(11.4589044897296,-32.0203896799758,-232.25005));
#232761=CARTESIAN_POINT('Origin',(0.,-32.21456093117,-229.35005));
#232762=CARTESIAN_POINT('Origin',(0.,-33.21456093117,-229.35005));
#232763=CARTESIAN_POINT('Origin',(-3.33261390928491E-13,-21.6090213785032,
-229.35005));
#232764=CARTESIAN_POINT('Origin',(-3.33261390928491E-13,-22.6090213785032,
-229.35005));
#232765=CARTESIAN_POINT('Origin',(-2.22174260618994E-13,-11.0034818258363,
-229.35005));
#232766=CARTESIAN_POINT('Origin',(-2.22174260618994E-13,-12.0034818258363,
-229.35005));
#232767=CARTESIAN_POINT('Origin',(-1.11087130309497E-13,-0.397942273169518,
-229.35005));
#232768=CARTESIAN_POINT('Origin',(-1.11087130309497E-13,-1.3979422731695,
-229.35005));
#232769=CARTESIAN_POINT('Origin',(-1.54373336646987E-15,-42.8201004838369,
-229.35005));
#232770=CARTESIAN_POINT('Origin',(-1.23757166668304E-15,-43.8201004838368,
-229.35005));
#232771=CARTESIAN_POINT('Origin',(-2.8425373731103E-15,9.20759727949731,
-229.35005));
#232772=CARTESIAN_POINT('Origin',(-2.53637567332344E-15,10.2075972794973,
-229.35005));
#232773=CARTESIAN_POINT('Origin',(-1.54373336646988E-15,19.8131368321642,
-229.35005));
#232774=CARTESIAN_POINT('Origin',(-1.23757166668304E-15,20.8131368321642,
-229.35005));
#232775=CARTESIAN_POINT('Origin',(-2.61456814389029E-14,-173.57701443073,
-229.35005));
#232776=CARTESIAN_POINT('Origin',(-2.61456814389029E-14,-173.57701443073,
-229.35005));
#232777=CARTESIAN_POINT('Origin',(7.14692237356698E-14,623.509175991979,
-229.35005));
#232778=CARTESIAN_POINT('Origin',(7.14692237356698E-14,623.509175991979,
-229.35005));
#232779=CARTESIAN_POINT('Origin',(-6.29739814579425E-15,-11.5034818258363,
-229.35005));
#232780=CARTESIAN_POINT('Origin',(-6.29739814579425E-15,-11.5034818258363,
-229.35005));
#232781=CARTESIAN_POINT('Origin',(-6.29739814579425E-15,-11.5034818258363,
-229.35005));
#232782=CARTESIAN_POINT('Origin',(-6.29739814579425E-15,-11.5034818258363,
-229.35005));
#232783=CARTESIAN_POINT('Origin',(0.,-32.21456093117,-229.35005));
#232784=CARTESIAN_POINT('Origin',(0.,-32.21456093117,-229.35005));
#232785=CARTESIAN_POINT('Origin',(0.,-33.21456093117,-229.35005));
#232786=CARTESIAN_POINT('Origin',(0.,-33.21456093117,-229.35005));
#232787=CARTESIAN_POINT('Origin',(-3.33261390928491E-13,-21.6090213785032,
-229.35005));
#232788=CARTESIAN_POINT('Origin',(-3.33261390928491E-13,-21.6090213785032,
-229.35005));
#232789=CARTESIAN_POINT('Origin',(-3.33261390928491E-13,-22.6090213785032,
-229.35005));
#232790=CARTESIAN_POINT('Origin',(-3.33261390928491E-13,-22.6090213785032,
-229.35005));
#232791=CARTESIAN_POINT('Origin',(-2.22174260618994E-13,-11.0034818258363,
-229.35005));
#232792=CARTESIAN_POINT('Origin',(-2.22174260618994E-13,-11.0034818258363,
-229.35005));
#232793=CARTESIAN_POINT('Origin',(-2.22174260618994E-13,-12.0034818258363,
-229.35005));
#232794=CARTESIAN_POINT('Origin',(-2.22174260618994E-13,-12.0034818258363,
-229.35005));
#232795=CARTESIAN_POINT('Origin',(-1.11087130309497E-13,-0.397942273169518,
-229.35005));
#232796=CARTESIAN_POINT('Origin',(-1.11087130309497E-13,-0.397942273169518,
-229.35005));
#232797=CARTESIAN_POINT('Origin',(-1.11087130309497E-13,-1.3979422731695,
-229.35005));
#232798=CARTESIAN_POINT('Origin',(-1.11087130309497E-13,-1.3979422731695,
-229.35005));
#232799=CARTESIAN_POINT('Origin',(-1.54373336646987E-15,-42.8201004838369,
-229.35005));
#232800=CARTESIAN_POINT('Origin',(-1.54373336646987E-15,-42.8201004838369,
-229.35005));
#232801=CARTESIAN_POINT('Origin',(-1.23757166668304E-15,-43.8201004838368,
-229.35005));
#232802=CARTESIAN_POINT('Origin',(-1.23757166668304E-15,-43.8201004838368,
-229.35005));
#232803=CARTESIAN_POINT('Origin',(-2.8425373731103E-15,9.20759727949731,
-229.35005));
#232804=CARTESIAN_POINT('Origin',(-2.8425373731103E-15,9.20759727949731,
-229.35005));
#232805=CARTESIAN_POINT('Origin',(-2.53637567332344E-15,10.2075972794973,
-229.35005));
#232806=CARTESIAN_POINT('Origin',(-2.53637567332344E-15,10.2075972794973,
-229.35005));
#232807=CARTESIAN_POINT('Origin',(-1.54373336646988E-15,19.8131368321642,
-229.35005));
#232808=CARTESIAN_POINT('Origin',(-1.54373336646988E-15,19.8131368321642,
-229.35005));
#232809=CARTESIAN_POINT('Origin',(-1.23757166668304E-15,20.8131368321642,
-229.35005));
#232810=CARTESIAN_POINT('Origin',(-1.23757166668304E-15,20.8131368321642,
-229.35005));
#232811=CARTESIAN_POINT('Origin',(-48.892180948596,36.2913696007177,-227.85005));
#232812=CARTESIAN_POINT('Origin',(-47.392180948596,37.1573950045021,-220.195349461621));
#232813=CARTESIAN_POINT('',(-47.392180948596,37.1573950045021,-221.195349461621));
#232814=CARTESIAN_POINT('',(-47.392180948596,37.1573950045021,-223.85005));
#232815=CARTESIAN_POINT('',(-47.392180948596,37.1573950045021,-220.195349461621));
#232816=CARTESIAN_POINT('',(-48.892180948596,38.0234204082866,-221.195349461621));
#232817=CARTESIAN_POINT('Ctrl Pts',(-48.8921809485959,38.0234204082865,
-221.195349461621));
#232818=CARTESIAN_POINT('Ctrl Pts',(-48.142180948596,37.5904077063944,-220.945349461621));
#232819=CARTESIAN_POINT('Ctrl Pts',(-47.3921809485961,37.1573950045022,
-221.195349461621));
#232820=CARTESIAN_POINT('',(-48.892180948596,38.0234204082866,-223.85005));
#232821=CARTESIAN_POINT('',(-48.892180948596,38.0234204082866,-220.195349461621));
#232822=CARTESIAN_POINT('Ctrl Pts',(-47.3921809485959,37.1573950045021,
-223.85005));
#232823=CARTESIAN_POINT('Ctrl Pts',(-48.142180948596,37.5904077063944,-223.417037298108));
#232824=CARTESIAN_POINT('Ctrl Pts',(-48.892180948596,38.0234204082866,-223.85005));
#232825=CARTESIAN_POINT('Origin',(-47.392180948596,35.4253441969333,-220.195349461621));
#232826=CARTESIAN_POINT('',(-47.392180948596,35.4253441969333,-221.195349461621));
#232827=CARTESIAN_POINT('',(-47.392180948596,35.4253441969333,-223.85005));
#232828=CARTESIAN_POINT('',(-47.392180948596,35.4253441969333,-220.195349461621));
#232829=CARTESIAN_POINT('Ctrl Pts',(-47.392180948596,37.1573950045021,-221.195349461621));
#232830=CARTESIAN_POINT('Ctrl Pts',(-47.392180948596,36.2913696007178,-220.945349461621));
#232831=CARTESIAN_POINT('Ctrl Pts',(-47.392180948596,35.4253441969335,-221.195349461621));
#232832=CARTESIAN_POINT('Ctrl Pts',(-47.392180948596,35.4253441969333,-223.85005));
#232833=CARTESIAN_POINT('Ctrl Pts',(-47.392180948596,36.2913696007177,-223.417037298108));
#232834=CARTESIAN_POINT('Ctrl Pts',(-47.392180948596,37.1573950045021,-223.85005));
#232835=CARTESIAN_POINT('Origin',(-48.892180948596,34.5593187931488,-220.195349461621));
#232836=CARTESIAN_POINT('',(-48.892180948596,34.5593187931488,-221.195349461621));
#232837=CARTESIAN_POINT('',(-48.892180948596,34.5593187931488,-223.85005));
#232838=CARTESIAN_POINT('',(-48.892180948596,34.5593187931488,-220.195349461621));
#232839=CARTESIAN_POINT('Ctrl Pts',(-47.3921809485961,35.4253441969333,
-221.195349461621));
#232840=CARTESIAN_POINT('Ctrl Pts',(-48.1421809485961,34.992331495041,-220.945349461621));
#232841=CARTESIAN_POINT('Ctrl Pts',(-48.8921809485962,34.5593187931488,
-221.195349461621));
#232842=CARTESIAN_POINT('Ctrl Pts',(-48.8921809485961,34.5593187931488,
-223.85005));
#232843=CARTESIAN_POINT('Ctrl Pts',(-48.142180948596,34.9923314950411,-223.417037298108));
#232844=CARTESIAN_POINT('Ctrl Pts',(-47.392180948596,35.4253441969333,-223.85005));
#232845=CARTESIAN_POINT('Origin',(-50.392180948596,35.4253441969333,-220.195349461621));
#232846=CARTESIAN_POINT('',(-50.392180948596,35.4253441969323,-221.19534946162));
#232847=CARTESIAN_POINT('',(-50.392180948596,35.4253441969333,-223.85005));
#232848=CARTESIAN_POINT('',(-50.392180948596,35.4253441969333,-220.195349461621));
#232849=CARTESIAN_POINT('Ctrl Pts',(-48.892180948596,34.5593187931489,-221.195349461621));
#232850=CARTESIAN_POINT('Ctrl Pts',(-49.6421809485958,34.992331495041,-220.945349461621));
#232851=CARTESIAN_POINT('Ctrl Pts',(-50.3921809485955,35.425344196933,-221.195349461621));
#232852=CARTESIAN_POINT('Ctrl Pts',(-50.3921809485959,35.4253441969333,
-223.85005));
#232853=CARTESIAN_POINT('Ctrl Pts',(-49.642180948596,34.9923314950411,-223.417037298108));
#232854=CARTESIAN_POINT('Ctrl Pts',(-48.892180948596,34.5593187931488,-223.85005));
#232855=CARTESIAN_POINT('Origin',(-50.392180948596,37.1573950045021,-220.195349461621));
#232856=CARTESIAN_POINT('',(-50.392180948596,37.1573950045021,-221.195349461621));
#232857=CARTESIAN_POINT('',(-50.392180948596,37.1573950045021,-223.85005));
#232858=CARTESIAN_POINT('',(-50.392180948596,37.1573950045021,-220.195349461621));
#232859=CARTESIAN_POINT('Ctrl Pts',(-50.392180948596,35.4253441969326,-221.195349461621));
#232860=CARTESIAN_POINT('Ctrl Pts',(-50.392180948596,36.2913696007175,-220.945349461621));
#232861=CARTESIAN_POINT('Ctrl Pts',(-50.392180948596,37.1573950045023,-221.195349461621));
#232862=CARTESIAN_POINT('Ctrl Pts',(-50.392180948596,37.1573950045022,-223.85005));
#232863=CARTESIAN_POINT('Ctrl Pts',(-50.392180948596,36.2913696007177,-223.417037298108));
#232864=CARTESIAN_POINT('Ctrl Pts',(-50.392180948596,35.4253441969332,-223.85005));
#232865=CARTESIAN_POINT('Origin',(-48.892180948596,38.0234204082866,-220.195349461621));
#232866=CARTESIAN_POINT('Ctrl Pts',(-50.3921809485959,37.1573950045022,
-221.195349461621));
#232867=CARTESIAN_POINT('Ctrl Pts',(-49.642180948596,37.5904077063944,-220.945349461621));
#232868=CARTESIAN_POINT('Ctrl Pts',(-48.8921809485962,38.0234204082865,
-221.195349461621));
#232869=CARTESIAN_POINT('Ctrl Pts',(-48.892180948596,38.0234204082866,-223.85005));
#232870=CARTESIAN_POINT('Ctrl Pts',(-49.642180948596,37.5904077063944,-223.417037298108));
#232871=CARTESIAN_POINT('Ctrl Pts',(-50.392180948596,37.1573950045022,-223.85005));
#232872=CARTESIAN_POINT('Origin',(-48.892180948596,36.2913696007177,-221.35005));
#232873=CARTESIAN_POINT('',(-48.892180948596,36.2913696007177,-220.195349461621));
#232874=CARTESIAN_POINT('',(-48.892180948596,34.2913696007177,-221.35005));
#232875=CARTESIAN_POINT('Origin',(-48.892180948596,36.2913696007177,-223.85005));
#232876=CARTESIAN_POINT('Origin',(-48.892180948596,36.2913696007177,-223.85005));
#232877=CARTESIAN_POINT('Origin',(-48.892180948596,36.2913696007177,-223.85005));
#232878=CARTESIAN_POINT('Origin',(-48.892180948596,36.2913696007177,-223.85005));
#232879=CARTESIAN_POINT('Origin',(-48.892180948596,36.2913696007177,-223.85005));
#232880=CARTESIAN_POINT('Origin',(-48.892180948596,36.2913696007177,-223.85005));
#232881=CARTESIAN_POINT('Origin',(-48.892180948596,36.2913696007177,-223.85005));
#232882=CARTESIAN_POINT('Origin',(-48.892180948596,36.2913696007177,-223.85005));
#232883=CARTESIAN_POINT('Origin',(-48.892180948596,36.2913696007177,-223.85005));
#232884=CARTESIAN_POINT('Origin',(-48.892180948596,36.2913696007177,-223.85005));
#232885=CARTESIAN_POINT('Origin',(-48.892180948596,36.2913696007177,-223.85005));
#232886=CARTESIAN_POINT('Origin',(-48.892180948596,36.2913696007177,-223.85005));
#232887=CARTESIAN_POINT('Origin',(-48.892180948596,36.2913696007177,-223.60005));
#232888=CARTESIAN_POINT('',(-48.892180948596,33.2913696007177,-223.85005));
#232889=CARTESIAN_POINT('Origin',(-48.892180948596,36.2913696007177,-223.85005));
#232890=CARTESIAN_POINT('',(-48.892180948596,33.0413696007177,-223.60005));
#232891=CARTESIAN_POINT('Origin',(-48.892180948596,33.2913696007177,-223.60005));
#232892=CARTESIAN_POINT('',(-48.892180948596,39.5413696007177,-223.60005));
#232893=CARTESIAN_POINT('Origin',(-48.892180948596,36.2913696007177,-223.60005));
#232894=CARTESIAN_POINT('Origin',(-48.892180948596,36.2913696007177,-223.60005));
#232895=CARTESIAN_POINT('Origin',(-48.892180948596,36.2913696007177,-218.35005));
#232896=CARTESIAN_POINT('',(-48.892180948596,39.5413696007177,-218.35005));
#232897=CARTESIAN_POINT('Origin',(-48.892180948596,36.2913696007177,-218.35005));
#232898=CARTESIAN_POINT('Origin',(-48.892180948596,36.2913696007177,-223.85005));
#232899=CARTESIAN_POINT('Origin',(-48.892180948596,36.2913696007177,-223.85005));
#232900=CARTESIAN_POINT('',(-48.892180948596,39.5413696007177,-223.85005));
#232901=CARTESIAN_POINT('Origin',(-12.9675000200281,-12.9675000200282,-32.54995));
#232902=CARTESIAN_POINT('',(-62.557372991106,-15.4675000200284,-32.54995));
#232903=CARTESIAN_POINT('',(-66.8875000100281,-17.9675000200284,-32.54995));
#232904=CARTESIAN_POINT('Origin',(-66.8875000100282,-12.9675000200284,-32.54995));
#232905=CARTESIAN_POINT('',(-71.2176270289503,-15.4675000200284,-32.54995));
#232906=CARTESIAN_POINT('Origin',(-66.8875000100282,-12.9675000200284,-32.54995));
#232907=CARTESIAN_POINT('',(-71.2176270289504,-10.4675000200284,-32.54995));
#232908=CARTESIAN_POINT('Origin',(-66.8875000100282,-12.9675000200284,-32.54995));
#232909=CARTESIAN_POINT('',(-66.8875000100282,-7.96750002002839,-32.54995));
#232910=CARTESIAN_POINT('Origin',(-66.8875000100282,-12.9675000200284,-32.54995));
#232911=CARTESIAN_POINT('',(-62.557372991106,-10.4675000200284,-32.54995));
#232912=CARTESIAN_POINT('Origin',(-66.8875000100282,-12.9675000200284,-32.54995));
#232913=CARTESIAN_POINT('Origin',(-66.8875000100282,-12.9675000200284,-32.54995));
#232914=CARTESIAN_POINT('Origin',(-66.8875000100282,-12.9675000200284,-32.54995));
#232915=CARTESIAN_POINT('',(-69.7742513559762,-17.9675000200284,-31.7764473081038));
#232916=CARTESIAN_POINT('Ctrl Pts',(-69.7742513559762,-17.9675000200284,
-31.7764473081038));
#232917=CARTESIAN_POINT('Ctrl Pts',(-70.5477540478725,-16.6277540578728,
-32.5499500000001));
#232918=CARTESIAN_POINT('Ctrl Pts',(-71.2176270289503,-15.4675000200284,
-32.5499500000001));
#232919=CARTESIAN_POINT('Ctrl Pts',(-66.8875000100281,-17.9675000200284,
-32.54995));
#232920=CARTESIAN_POINT('Ctrl Pts',(-68.2272459721837,-17.9675000200284,
-32.54995));
#232921=CARTESIAN_POINT('Ctrl Pts',(-69.7742513559762,-17.9675000200284,
-31.7764473081038));
#232922=CARTESIAN_POINT('Origin',(-66.8875000100282,-12.9675000200284,-32.54995));
#232923=CARTESIAN_POINT('',(-72.6610027019244,-12.9675000200284,-31.7764473081038));
#232924=CARTESIAN_POINT('Ctrl Pts',(-71.2176270289503,-15.4675000200284,
-32.5499500000001));
#232925=CARTESIAN_POINT('Ctrl Pts',(-71.8875000100281,-14.307245982184,
-32.5499500000001));
#232926=CARTESIAN_POINT('Ctrl Pts',(-72.6610027019243,-12.9675000200284,
-31.7764473081039));
#232927=CARTESIAN_POINT('Ctrl Pts',(-72.6610027019244,-12.9675000200284,
-31.7764473081038));
#232928=CARTESIAN_POINT('Ctrl Pts',(-71.8875000100282,-11.6277540578728,
-32.5499500000001));
#232929=CARTESIAN_POINT('Ctrl Pts',(-71.2176270289504,-10.4675000200284,
-32.5499500000001));
#232930=CARTESIAN_POINT('Origin',(-66.8875000100282,-12.9675000200284,-32.54995));
#232931=CARTESIAN_POINT('',(-69.7742513559763,-7.96750002002841,-31.7764473081038));
#232932=CARTESIAN_POINT('Ctrl Pts',(-71.2176270289504,-10.4675000200284,
-32.5499500000001));
#232933=CARTESIAN_POINT('Ctrl Pts',(-70.5477540478726,-9.30724598218405,
-32.5499500000001));
#232934=CARTESIAN_POINT('Ctrl Pts',(-69.7742513559763,-7.96750002002843,
-31.7764473081038));
#232935=CARTESIAN_POINT('Ctrl Pts',(-69.7742513559763,-7.96750002002841,
-31.7764473081038));
#232936=CARTESIAN_POINT('Ctrl Pts',(-68.2272459721838,-7.96750002002841,
-32.54995));
#232937=CARTESIAN_POINT('Ctrl Pts',(-66.8875000100282,-7.9675000200284,
-32.54995));
#232938=CARTESIAN_POINT('Origin',(-66.8875000100282,-12.9675000200284,-32.54995));
#232939=CARTESIAN_POINT('',(-64.0007486640801,-7.96750002002838,-31.7764473081038));
#232940=CARTESIAN_POINT('Ctrl Pts',(-66.8875000100282,-7.9675000200284,
-32.54995));
#232941=CARTESIAN_POINT('Ctrl Pts',(-65.5477540478726,-7.9675000200284,
-32.54995));
#232942=CARTESIAN_POINT('Ctrl Pts',(-64.0007486640801,-7.96750002002839,
-31.7764473081038));
#232943=CARTESIAN_POINT('Ctrl Pts',(-64.0007486640801,-7.96750002002838,
-31.7764473081038));
#232944=CARTESIAN_POINT('Ctrl Pts',(-63.2272459721838,-9.30724598218399,
-32.54995));
#232945=CARTESIAN_POINT('Ctrl Pts',(-62.557372991106,-10.4675000200284,
-32.54995));
#232946=CARTESIAN_POINT('Origin',(-66.8875000100282,-12.9675000200284,-32.54995));
#232947=CARTESIAN_POINT('',(-61.1139973181319,-12.9675000200284,-31.7764473081038));
#232948=CARTESIAN_POINT('Ctrl Pts',(-62.557372991106,-10.4675000200284,
-32.54995));
#232949=CARTESIAN_POINT('Ctrl Pts',(-61.8875000100282,-11.6277540578727,
-32.54995));
#232950=CARTESIAN_POINT('Ctrl Pts',(-61.113997318132,-12.9675000200284,
-31.7764473081038));
#232951=CARTESIAN_POINT('Ctrl Pts',(-61.1139973181319,-12.9675000200284,
-31.7764473081037));
#232952=CARTESIAN_POINT('Ctrl Pts',(-61.8875000100282,-14.307245982184,
-32.54995));
#232953=CARTESIAN_POINT('Ctrl Pts',(-62.557372991106,-15.4675000200284,
-32.54995));
#232954=CARTESIAN_POINT('Origin',(-66.8875000100282,-12.9675000200284,-32.54995));
#232955=CARTESIAN_POINT('',(-64.00074866408,-17.9675000200283,-31.7764473081038));
#232956=CARTESIAN_POINT('Ctrl Pts',(-62.557372991106,-15.4675000200284,
-32.54995));
#232957=CARTESIAN_POINT('Ctrl Pts',(-63.2272459721838,-16.6277540578727,
-32.54995));
#232958=CARTESIAN_POINT('Ctrl Pts',(-64.00074866408,-17.9675000200283,-31.7764473081038));
#232959=CARTESIAN_POINT('Ctrl Pts',(-64.00074866408,-17.9675000200283,-31.7764473081038));
#232960=CARTESIAN_POINT('Ctrl Pts',(-65.5477540478725,-17.9675000200283,
-32.54995));
#232961=CARTESIAN_POINT('Ctrl Pts',(-66.8875000100281,-17.9675000200284,
-32.54995));
#232962=CARTESIAN_POINT('Origin',(-12.9675000200281,-12.9675000200282,-28.54995));
#232963=CARTESIAN_POINT('',(-66.8875000100281,-17.9675000200283,-28.54995));
#232964=CARTESIAN_POINT('',(-71.2176270289503,-15.4675000200284,-28.54995));
#232965=CARTESIAN_POINT('Origin',(-66.8875000100282,-12.9675000200284,-28.54995));
#232966=CARTESIAN_POINT('',(-62.557372991106,-15.4675000200284,-28.54995));
#232967=CARTESIAN_POINT('Origin',(-66.8875000100282,-12.9675000200284,-28.54995));
#232968=CARTESIAN_POINT('',(-62.557372991106,-10.4675000200284,-28.54995));
#232969=CARTESIAN_POINT('Origin',(-66.8875000100282,-12.9675000200284,-28.54995));
#232970=CARTESIAN_POINT('',(-66.8875000100282,-7.9675000200284,-28.54995));
#232971=CARTESIAN_POINT('Origin',(-66.8875000100282,-12.9675000200284,-28.54995));
#232972=CARTESIAN_POINT('',(-71.2176270289503,-10.4675000200284,-28.54995));
#232973=CARTESIAN_POINT('Origin',(-66.8875000100282,-12.9675000200284,-28.54995));
#232974=CARTESIAN_POINT('Origin',(-66.8875000100282,-12.9675000200284,-28.54995));
#232975=CARTESIAN_POINT('Origin',(-66.8875000100282,-12.9675000200284,-28.54995));
#232976=CARTESIAN_POINT('',(-64.0007486640798,-17.9675000200283,-28.9965319873851));
#232977=CARTESIAN_POINT('Ctrl Pts',(-64.0007486640717,-17.9675000200283,
-28.9965319873876));
#232978=CARTESIAN_POINT('Ctrl Pts',(-65.5477540478691,-17.9675000200284,
-28.54995));
#232979=CARTESIAN_POINT('Ctrl Pts',(-66.887500010028,-17.9675000200283,
-28.54995));
#232980=CARTESIAN_POINT('Ctrl Pts',(-62.557372991106,-15.4675000200284,
-28.54995));
#232981=CARTESIAN_POINT('Ctrl Pts',(-63.2272459721854,-16.6277540578755,
-28.54995));
#232982=CARTESIAN_POINT('Ctrl Pts',(-64.000748664084,-17.9675000200353,
-28.9965319873875));
#232983=CARTESIAN_POINT('Origin',(-66.8875000100282,-12.9675000200284,-28.54995));
#232984=CARTESIAN_POINT('',(-61.1139973181319,-12.9675000200284,-28.9965319873852));
#232985=CARTESIAN_POINT('Ctrl Pts',(-61.1139973181278,-12.9675000200213,
-28.9965319873876));
#232986=CARTESIAN_POINT('Ctrl Pts',(-61.8875000100265,-14.3072459821811,
-28.54995));
#232987=CARTESIAN_POINT('Ctrl Pts',(-62.557372991106,-15.4675000200284,
-28.54995));
#232988=CARTESIAN_POINT('Ctrl Pts',(-62.557372991106,-10.4675000200284,
-28.54995));
#232989=CARTESIAN_POINT('Ctrl Pts',(-61.8875000100266,-11.6277540578756,
-28.54995));
#232990=CARTESIAN_POINT('Ctrl Pts',(-61.1139973181279,-12.9675000200354,
-28.9965319873876));
#232991=CARTESIAN_POINT('Origin',(-66.8875000100282,-12.9675000200284,-28.54995));
#232992=CARTESIAN_POINT('',(-64.0007486640801,-7.96750002002838,-28.9965319873852));
#232993=CARTESIAN_POINT('Ctrl Pts',(-64.0007486640842,-7.96750002002133,
-28.9965319873875));
#232994=CARTESIAN_POINT('Ctrl Pts',(-63.2272459721855,-9.30724598218116,
-28.54995));
#232995=CARTESIAN_POINT('Ctrl Pts',(-62.557372991106,-10.4675000200284,
-28.54995));
#232996=CARTESIAN_POINT('Ctrl Pts',(-66.8875000100282,-7.9675000200284,
-28.54995));
#232997=CARTESIAN_POINT('Ctrl Pts',(-65.5477540478693,-7.96750002002839,
-28.54995));
#232998=CARTESIAN_POINT('Ctrl Pts',(-64.0007486640719,-7.96750002002839,
-28.9965319873876));
#232999=CARTESIAN_POINT('Origin',(-66.8875000100282,-12.9675000200284,-28.54995));
#233000=CARTESIAN_POINT('',(-69.7742513559763,-7.96750002002841,-28.9965319873852));
#233001=CARTESIAN_POINT('Ctrl Pts',(-69.7742513559845,-7.96750002002841,
-28.9965319873875));
#233002=CARTESIAN_POINT('Ctrl Pts',(-68.2272459721871,-7.9675000200284,
-28.54995));
#233003=CARTESIAN_POINT('Ctrl Pts',(-66.8875000100282,-7.9675000200284,
-28.54995));
#233004=CARTESIAN_POINT('Ctrl Pts',(-71.2176270289503,-10.4675000200284,
-28.54995));
#233005=CARTESIAN_POINT('Ctrl Pts',(-70.5477540478709,-9.30724598218117,
-28.54995));
#233006=CARTESIAN_POINT('Ctrl Pts',(-69.7742513559722,-7.96750002002137,
-28.9965319873875));
#233007=CARTESIAN_POINT('Origin',(-66.8875000100282,-12.9675000200284,-28.54995));
#233008=CARTESIAN_POINT('',(-72.6610027019244,-12.9675000200284,-28.9965319873853));
#233009=CARTESIAN_POINT('Ctrl Pts',(-72.6610027019285,-12.9675000200355,
-28.9965319873875));
#233010=CARTESIAN_POINT('Ctrl Pts',(-71.8875000100298,-11.6277540578756,
-28.54995));
#233011=CARTESIAN_POINT('Ctrl Pts',(-71.2176270289503,-10.4675000200284,
-28.54995));
#233012=CARTESIAN_POINT('Ctrl Pts',(-71.2176270289503,-15.4675000200284,
-28.5499499999999));
#233013=CARTESIAN_POINT('Ctrl Pts',(-71.8875000100297,-14.3072459821812,
-28.5499499999999));
#233014=CARTESIAN_POINT('Ctrl Pts',(-72.6610027019284,-12.9675000200213,
-28.9965319873875));
#233015=CARTESIAN_POINT('Origin',(-66.8875000100282,-12.9675000200284,-28.54995));
#233016=CARTESIAN_POINT('',(-69.7742513559762,-17.9675000200284,-28.9965319873853));
#233017=CARTESIAN_POINT('Ctrl Pts',(-66.887500010028,-17.9675000200283,
-28.54995));
#233018=CARTESIAN_POINT('Ctrl Pts',(-68.227245972187,-17.9675000200284,
-28.54995));
#233019=CARTESIAN_POINT('Ctrl Pts',(-69.7742513559844,-17.9675000200284,
-28.9965319873875));
#233020=CARTESIAN_POINT('Ctrl Pts',(-69.7742513559721,-17.9675000200355,
-28.9965319873875));
#233021=CARTESIAN_POINT('Ctrl Pts',(-70.5477540478708,-16.6277540578756,
-28.5499499999999));
#233022=CARTESIAN_POINT('Ctrl Pts',(-71.2176270289503,-15.4675000200284,
-28.5499499999999));
#233023=CARTESIAN_POINT('Origin',(-64.00074866408,-17.9675000200283,-32.54995));
#233024=CARTESIAN_POINT('',(-64.00074866408,-17.9675000200283,-32.54995));
#233025=CARTESIAN_POINT('',(-69.7742513559762,-17.9675000200284,-32.54995));
#233026=CARTESIAN_POINT('Origin',(-61.1139973181319,-12.9675000200284,-32.54995));
#233027=CARTESIAN_POINT('',(-61.1139973181319,-12.9675000200284,-32.54995));
#233028=CARTESIAN_POINT('Origin',(-64.0007486640801,-7.96750002002838,-32.54995));
#233029=CARTESIAN_POINT('',(-64.0007486640801,-7.96750002002838,-32.54995));
#233030=CARTESIAN_POINT('Origin',(-69.7742513559763,-7.96750002002841,-32.54995));
#233031=CARTESIAN_POINT('',(-69.7742513559763,-7.96750002002841,-32.54995));
#233032=CARTESIAN_POINT('Origin',(-72.6610027019244,-12.9675000200284,-32.54995));
#233033=CARTESIAN_POINT('',(-72.6610027019244,-12.9675000200284,-32.54995));
#233034=CARTESIAN_POINT('Origin',(-69.7742513559762,-17.9675000200284,-32.54995));
#233035=CARTESIAN_POINT('Origin',(0.,8.39884049934975E-16,-32.54995));
#233036=CARTESIAN_POINT('',(-2.5,49.5898729710778,-32.54995));
#233037=CARTESIAN_POINT('',(-5.,53.91999999,-32.54995));
#233038=CARTESIAN_POINT('Origin',(-1.73472347597681E-15,53.91999999,-32.54995));
#233039=CARTESIAN_POINT('',(-2.5,58.2501270089222,-32.54995));
#233040=CARTESIAN_POINT('Origin',(-1.73472347597681E-15,53.91999999,-32.54995));
#233041=CARTESIAN_POINT('',(2.5,58.2501270089222,-32.54995));
#233042=CARTESIAN_POINT('Origin',(-1.73472347597681E-15,53.91999999,-32.54995));
#233043=CARTESIAN_POINT('',(5.,53.91999999,-32.54995));
#233044=CARTESIAN_POINT('Origin',(-1.73472347597681E-15,53.91999999,-32.54995));
#233045=CARTESIAN_POINT('',(2.5,49.5898729710778,-32.54995));
#233046=CARTESIAN_POINT('Origin',(-1.73472347597681E-15,53.91999999,-32.54995));
#233047=CARTESIAN_POINT('Origin',(-1.73472347597681E-15,53.91999999,-32.54995));
#233048=CARTESIAN_POINT('Origin',(-1.73472347597681E-15,53.91999999,-32.54995));
#233049=CARTESIAN_POINT('',(-5.,56.8067513359481,-31.7764473081038));
#233050=CARTESIAN_POINT('Ctrl Pts',(-4.99999999999996,56.8067513359481,
-31.7764473081038));
#233051=CARTESIAN_POINT('Ctrl Pts',(-3.66025403784437,57.5802540278444,
-32.54995));
#233052=CARTESIAN_POINT('Ctrl Pts',(-2.49999999999999,58.2501270089222,
-32.54995));
#233053=CARTESIAN_POINT('Ctrl Pts',(-5.,53.91999999,-32.54995));
#233054=CARTESIAN_POINT('Ctrl Pts',(-5.,55.2597459521556,-32.54995));
#233055=CARTESIAN_POINT('Ctrl Pts',(-5.,56.8067513359481,-31.7764473081038));
#233056=CARTESIAN_POINT('Origin',(-1.73472347597681E-15,53.91999999,-32.54995));
#233057=CARTESIAN_POINT('',(-1.66200633571292E-14,59.6935026818963,-31.7764473081038));
#233058=CARTESIAN_POINT('Ctrl Pts',(-2.49999999999999,58.2501270089222,
-32.54995));
#233059=CARTESIAN_POINT('Ctrl Pts',(-1.33974596215561,58.91999999,-32.54995));
#233060=CARTESIAN_POINT('Ctrl Pts',(-9.88775234870751E-15,59.6935026818962,
-31.7764473081038));
#233061=CARTESIAN_POINT('Ctrl Pts',(1.40342291401011E-14,59.6935026818963,
-31.7764473081037));
#233062=CARTESIAN_POINT('Ctrl Pts',(1.33974596215562,58.91999999,-32.54995));
#233063=CARTESIAN_POINT('Ctrl Pts',(2.5,58.2501270089222,-32.54995));
#233064=CARTESIAN_POINT('Origin',(-1.73472347597681E-15,53.91999999,-32.54995));
#233065=CARTESIAN_POINT('',(5.,56.8067513359482,-31.7764473081038));
#233066=CARTESIAN_POINT('Ctrl Pts',(2.5,58.2501270089222,-32.54995));
#233067=CARTESIAN_POINT('Ctrl Pts',(3.66025403784437,57.5802540278444,-32.54995));
#233068=CARTESIAN_POINT('Ctrl Pts',(4.99999999999995,56.8067513359482,-31.7764473081038));
#233069=CARTESIAN_POINT('Ctrl Pts',(5.,56.8067513359482,-31.7764473081037));
#233070=CARTESIAN_POINT('Ctrl Pts',(5.,55.2597459521556,-32.54995));
#233071=CARTESIAN_POINT('Ctrl Pts',(5.,53.91999999,-32.54995));
#233072=CARTESIAN_POINT('Origin',(-1.73472347597681E-15,53.91999999,-32.54995));
#233073=CARTESIAN_POINT('',(5.,51.0332486440519,-31.7764473081038));
#233074=CARTESIAN_POINT('Ctrl Pts',(5.,53.91999999,-32.54995));
#233075=CARTESIAN_POINT('Ctrl Pts',(5.,52.5802540278444,-32.54995));
#233076=CARTESIAN_POINT('Ctrl Pts',(5.,51.0332486440519,-31.7764473081038));
#233077=CARTESIAN_POINT('Ctrl Pts',(4.99999999999998,51.0332486440519,-31.7764473081038));
#233078=CARTESIAN_POINT('Ctrl Pts',(3.66025403784436,50.2597459521556,-32.54995));
#233079=CARTESIAN_POINT('Ctrl Pts',(2.49999999999997,49.5898729710778,-32.54995));
#233080=CARTESIAN_POINT('Origin',(-1.73472347597681E-15,53.91999999,-32.54995));
#233081=CARTESIAN_POINT('',(-2.79122613421945E-15,48.1464972981038,-31.7764473081038));
#233082=CARTESIAN_POINT('Ctrl Pts',(2.49999999999997,49.5898729710778,-32.54995));
#233083=CARTESIAN_POINT('Ctrl Pts',(1.33974596215561,48.91999999,-32.54995));
#233084=CARTESIAN_POINT('Ctrl Pts',(3.60424521098048E-14,48.1464972981038,
-31.7764473081038));
#233085=CARTESIAN_POINT('Ctrl Pts',(-3.50855728502523E-15,48.1464972981038,
-31.7764473081038));
#233086=CARTESIAN_POINT('Ctrl Pts',(-1.3397459621556,48.9199999900001,-32.5499500000001));
#233087=CARTESIAN_POINT('Ctrl Pts',(-2.49999999999997,49.5898729710779,
-32.5499500000001));
#233088=CARTESIAN_POINT('Origin',(-1.73472347597681E-15,53.91999999,-32.54995));
#233089=CARTESIAN_POINT('',(-5.,51.0332486440519,-31.7764473081037));
#233090=CARTESIAN_POINT('Ctrl Pts',(-2.49999999999997,49.5898729710779,
-32.5499500000001));
#233091=CARTESIAN_POINT('Ctrl Pts',(-3.66025403784436,50.2597459521557,
-32.5499500000001));
#233092=CARTESIAN_POINT('Ctrl Pts',(-4.99999999999998,51.0332486440519,
-31.7764473081038));
#233093=CARTESIAN_POINT('Ctrl Pts',(-5.,51.0332486440519,-31.7764473081038));
#233094=CARTESIAN_POINT('Ctrl Pts',(-5.,52.5802540278444,-32.54995));
#233095=CARTESIAN_POINT('Ctrl Pts',(-5.,53.91999999,-32.54995));
#233096=CARTESIAN_POINT('Origin',(0.,2.17747716649809E-16,-28.54995));
#233097=CARTESIAN_POINT('',(-5.,53.91999999,-28.54995));
#233098=CARTESIAN_POINT('',(-2.5,58.2501270089222,-28.54995));
#233099=CARTESIAN_POINT('Origin',(-1.73472347597681E-15,53.91999999,-28.54995));
#233100=CARTESIAN_POINT('',(-2.5,49.5898729710778,-28.54995));
#233101=CARTESIAN_POINT('Origin',(-1.73472347597681E-15,53.91999999,-28.54995));
#233102=CARTESIAN_POINT('',(2.5,49.5898729710778,-28.54995));
#233103=CARTESIAN_POINT('Origin',(-1.73472347597681E-15,53.91999999,-28.54995));
#233104=CARTESIAN_POINT('',(5.,53.91999999,-28.54995));
#233105=CARTESIAN_POINT('Origin',(-1.73472347597681E-15,53.91999999,-28.54995));
#233106=CARTESIAN_POINT('',(2.5,58.2501270089222,-28.54995));
#233107=CARTESIAN_POINT('Origin',(-1.73472347597681E-15,53.91999999,-28.54995));
#233108=CARTESIAN_POINT('Origin',(-1.73472347597681E-15,53.91999999,-28.54995));
#233109=CARTESIAN_POINT('Origin',(-1.73472347597681E-15,53.91999999,-28.54995));
#233110=CARTESIAN_POINT('',(-5.,51.0332486440517,-28.9965319873851));
#233111=CARTESIAN_POINT('Ctrl Pts',(-5.,51.0332486440436,-28.9965319873876));
#233112=CARTESIAN_POINT('Ctrl Pts',(-5.,52.5802540278411,-28.54995));
#233113=CARTESIAN_POINT('Ctrl Pts',(-5.,53.91999999,-28.54995));
#233114=CARTESIAN_POINT('Ctrl Pts',(-2.49999999999998,49.5898729710779,
-28.54995));
#233115=CARTESIAN_POINT('Ctrl Pts',(-3.66025403784716,50.2597459521573,
-28.54995));
#233116=CARTESIAN_POINT('Ctrl Pts',(-5.00000000000693,51.0332486440559,
-28.9965319873875));
#233117=CARTESIAN_POINT('Origin',(-1.73472347597681E-15,53.91999999,-28.54995));
#233118=CARTESIAN_POINT('',(-3.91685175604228E-15,48.1464972981038,-28.9965319873852));
#233119=CARTESIAN_POINT('Ctrl Pts',(7.06240095952727E-12,48.1464972980997,
-28.9965319873875));
#233120=CARTESIAN_POINT('Ctrl Pts',(-1.33974596215276,48.9199999899984,
-28.54995));
#233121=CARTESIAN_POINT('Ctrl Pts',(-2.49999999999998,49.5898729710779,
-28.54995));
#233122=CARTESIAN_POINT('Ctrl Pts',(2.49999999999996,49.5898729710778,-28.54995));
#233123=CARTESIAN_POINT('Ctrl Pts',(1.33974596215275,48.9199999899984,-28.54995));
#233124=CARTESIAN_POINT('Ctrl Pts',(-7.05906782420426E-12,48.1464972980997,
-28.9965319873875));
#233125=CARTESIAN_POINT('Origin',(-1.73472347597681E-15,53.91999999,-28.54995));
#233126=CARTESIAN_POINT('',(5.,51.0332486440519,-28.9965319873852));
#233127=CARTESIAN_POINT('Ctrl Pts',(5.00000000000706,51.033248644056,-28.9965319873876));
#233128=CARTESIAN_POINT('Ctrl Pts',(3.6602540378472,50.2597459521573,-28.54995));
#233129=CARTESIAN_POINT('Ctrl Pts',(2.49999999999996,49.5898729710778,-28.54995));
#233130=CARTESIAN_POINT('Ctrl Pts',(5.,53.91999999,-28.54995));
#233131=CARTESIAN_POINT('Ctrl Pts',(5.,52.5802540278411,-28.54995));
#233132=CARTESIAN_POINT('Ctrl Pts',(5.,51.0332486440438,-28.9965319873875));
#233133=CARTESIAN_POINT('Origin',(-1.73472347597681E-15,53.91999999,-28.54995));
#233134=CARTESIAN_POINT('',(5.,56.8067513359482,-28.9965319873852));
#233135=CARTESIAN_POINT('Ctrl Pts',(5.,56.8067513359563,-28.9965319873876));
#233136=CARTESIAN_POINT('Ctrl Pts',(5.,55.2597459521589,-28.54995));
#233137=CARTESIAN_POINT('Ctrl Pts',(5.,53.91999999,-28.54995));
#233138=CARTESIAN_POINT('Ctrl Pts',(2.49999999999998,58.2501270089222,-28.54995));
#233139=CARTESIAN_POINT('Ctrl Pts',(3.66025403784719,57.5802540278428,-28.54995));
#233140=CARTESIAN_POINT('Ctrl Pts',(5.000000000007,56.8067513359441,-28.9965319873876));
#233141=CARTESIAN_POINT('Origin',(-1.73472347597681E-15,53.91999999,-28.54995));
#233142=CARTESIAN_POINT('',(-1.57929637069991E-14,59.6935026818963,-28.9965319873852));
#233143=CARTESIAN_POINT('Ctrl Pts',(-7.06778525504927E-12,59.6935026819004,
-28.9965319873876));
#233144=CARTESIAN_POINT('Ctrl Pts',(1.33974596215276,58.9199999900017,-28.54995));
#233145=CARTESIAN_POINT('Ctrl Pts',(2.49999999999998,58.2501270089222,-28.54995));
#233146=CARTESIAN_POINT('Ctrl Pts',(-2.5,58.2501270089222,-28.54995));
#233147=CARTESIAN_POINT('Ctrl Pts',(-1.33974596215277,58.9199999900016,
-28.54995));
#233148=CARTESIAN_POINT('Ctrl Pts',(7.07624629086929E-12,59.6935026819003,
-28.9965319873875));
#233149=CARTESIAN_POINT('Origin',(-1.73472347597681E-15,53.91999999,-28.54995));
#233150=CARTESIAN_POINT('',(-5.,56.8067513359481,-28.9965319873852));
#233151=CARTESIAN_POINT('Ctrl Pts',(-5.,53.91999999,-28.54995));
#233152=CARTESIAN_POINT('Ctrl Pts',(-5.,55.2597459521589,-28.54995));
#233153=CARTESIAN_POINT('Ctrl Pts',(-5.,56.8067513359563,-28.9965319873876));
#233154=CARTESIAN_POINT('Ctrl Pts',(-5.00000000000706,56.806751335944,-28.9965319873876));
#233155=CARTESIAN_POINT('Ctrl Pts',(-3.66025403784722,57.5802540278427,
-28.54995));
#233156=CARTESIAN_POINT('Ctrl Pts',(-2.5,58.2501270089222,-28.54995));
#233157=CARTESIAN_POINT('Origin',(-5.,51.0332486440519,-32.54995));
#233158=CARTESIAN_POINT('',(-5.,51.0332486440519,-32.54995));
#233159=CARTESIAN_POINT('',(-5.,56.8067513359481,-32.54995));
#233160=CARTESIAN_POINT('Origin',(-3.63207727782644E-15,48.1464972981038,
-32.54995));
#233161=CARTESIAN_POINT('',(-3.63207727782644E-15,48.1464972981038,-32.54995));
#233162=CARTESIAN_POINT('Origin',(5.,51.0332486440519,-32.54995));
#233163=CARTESIAN_POINT('',(5.,51.0332486440519,-32.54995));
#233164=CARTESIAN_POINT('Origin',(5.,56.8067513359482,-32.54995));
#233165=CARTESIAN_POINT('',(5.,56.8067513359482,-32.54995));
#233166=CARTESIAN_POINT('Origin',(-1.56125112837912E-14,59.6935026818963,
-32.54995));
#233167=CARTESIAN_POINT('',(-1.56125112837912E-14,59.6935026818963,-32.54995));
#233168=CARTESIAN_POINT('Origin',(-5.,56.8067513359481,-32.54995));
#233169=CARTESIAN_POINT('Origin',(47.392180948596,-60.9300389954978,-220.195349461621));
#233170=CARTESIAN_POINT('',(47.392180948596,-60.9300389954978,-221.195349461621));
#233171=CARTESIAN_POINT('',(47.392180948596,-60.9300389954978,-223.85005));
#233172=CARTESIAN_POINT('',(47.392180948596,-60.9300389954978,-220.195349461621));
#233173=CARTESIAN_POINT('',(48.892180948596,-60.0640135917134,-223.85005));
#233174=CARTESIAN_POINT('Ctrl Pts',(47.392180948596,-60.9300389954978,-223.85005));
#233175=CARTESIAN_POINT('Ctrl Pts',(48.142180948596,-60.4970262936056,-223.417037298108));
#233176=CARTESIAN_POINT('Ctrl Pts',(48.8921809485959,-60.0640135917134,
-223.85005));
#233177=CARTESIAN_POINT('',(48.892180948596,-60.0640135917134,-221.195349461621));
#233178=CARTESIAN_POINT('',(48.892180948596,-60.0640135917134,-220.195349461621));
#233179=CARTESIAN_POINT('Ctrl Pts',(48.892180948596,-60.0640135917134,-221.195349461621));
#233180=CARTESIAN_POINT('Ctrl Pts',(48.142180948596,-60.4970262936056,-220.945349461621));
#233181=CARTESIAN_POINT('Ctrl Pts',(47.392180948596,-60.9300389954978,-221.195349461621));
#233182=CARTESIAN_POINT('Origin',(47.392180948596,-62.6620898030667,-220.195349461621));
#233183=CARTESIAN_POINT('',(47.392180948596,-62.6620898030667,-221.195349461621));
#233184=CARTESIAN_POINT('',(47.392180948596,-62.6620898030667,-223.85005));
#233185=CARTESIAN_POINT('',(47.392180948596,-62.6620898030667,-220.195349461621));
#233186=CARTESIAN_POINT('Ctrl Pts',(47.392180948596,-62.6620898030667,-223.85005));
#233187=CARTESIAN_POINT('Ctrl Pts',(47.392180948596,-61.7960643992823,-223.417037298108));
#233188=CARTESIAN_POINT('Ctrl Pts',(47.392180948596,-60.9300389954978,-223.85005));
#233189=CARTESIAN_POINT('Ctrl Pts',(47.392180948596,-60.9300389954978,-221.195349461621));
#233190=CARTESIAN_POINT('Ctrl Pts',(47.392180948596,-61.7960643992822,-220.945349461621));
#233191=CARTESIAN_POINT('Ctrl Pts',(47.392180948596,-62.6620898030667,-221.195349461621));
#233192=CARTESIAN_POINT('Origin',(48.892180948596,-63.5281152068512,-220.195349461621));
#233193=CARTESIAN_POINT('',(48.892180948596,-63.5281152068512,-221.195349461621));
#233194=CARTESIAN_POINT('',(48.892180948596,-63.5281152068512,-223.85005));
#233195=CARTESIAN_POINT('',(48.892180948596,-63.5281152068512,-220.195349461621));
#233196=CARTESIAN_POINT('Ctrl Pts',(48.892180948596,-63.5281152068512,-223.85005));
#233197=CARTESIAN_POINT('Ctrl Pts',(48.142180948596,-63.095102504959,-223.417037298108));
#233198=CARTESIAN_POINT('Ctrl Pts',(47.3921809485961,-62.6620898030668,
-223.85005));
#233199=CARTESIAN_POINT('Ctrl Pts',(47.392180948596,-62.6620898030667,-221.195349461621));
#233200=CARTESIAN_POINT('Ctrl Pts',(48.142180948596,-63.095102504959,-220.945349461621));
#233201=CARTESIAN_POINT('Ctrl Pts',(48.892180948596,-63.5281152068512,-221.195349461621));
#233202=CARTESIAN_POINT('Origin',(50.392180948596,-62.6620898030667,-220.195349461621));
#233203=CARTESIAN_POINT('',(50.392180948596,-62.6620898030677,-221.19534946162));
#233204=CARTESIAN_POINT('',(50.392180948596,-62.6620898030667,-223.85005));
#233205=CARTESIAN_POINT('',(50.392180948596,-62.6620898030667,-220.195349461621));
#233206=CARTESIAN_POINT('Ctrl Pts',(50.392180948596,-62.6620898030667,-223.85005));
#233207=CARTESIAN_POINT('Ctrl Pts',(49.642180948596,-63.0951025049589,-223.417037298108));
#233208=CARTESIAN_POINT('Ctrl Pts',(48.8921809485959,-63.5281152068512,
-223.85005));
#233209=CARTESIAN_POINT('Ctrl Pts',(48.8921809485958,-63.5281152068512,
-221.195349461621));
#233210=CARTESIAN_POINT('Ctrl Pts',(49.6421809485957,-63.0951025049591,
-220.945349461621));
#233211=CARTESIAN_POINT('Ctrl Pts',(50.3921809485954,-62.662089803067,-221.195349461621));
#233212=CARTESIAN_POINT('Origin',(50.392180948596,-60.9300389954978,-220.195349461621));
#233213=CARTESIAN_POINT('',(50.392180948596,-60.9300389954978,-221.195349461621));
#233214=CARTESIAN_POINT('',(50.392180948596,-60.9300389954978,-223.85005));
#233215=CARTESIAN_POINT('',(50.392180948596,-60.9300389954978,-220.195349461621));
#233216=CARTESIAN_POINT('Ctrl Pts',(50.392180948596,-60.9300389954978,-223.85005));
#233217=CARTESIAN_POINT('Ctrl Pts',(50.392180948596,-61.7960643992822,-223.417037298108));
#233218=CARTESIAN_POINT('Ctrl Pts',(50.392180948596,-62.6620898030667,-223.85005));
#233219=CARTESIAN_POINT('Ctrl Pts',(50.392180948596,-62.6620898030672,-221.195349461621));
#233220=CARTESIAN_POINT('Ctrl Pts',(50.392180948596,-61.7960643992825,-220.945349461621));
#233221=CARTESIAN_POINT('Ctrl Pts',(50.392180948596,-60.9300389954979,-221.195349461621));
#233222=CARTESIAN_POINT('Origin',(48.892180948596,-60.0640135917134,-220.195349461621));
#233223=CARTESIAN_POINT('Ctrl Pts',(48.892180948596,-60.0640135917134,-223.85005));
#233224=CARTESIAN_POINT('Ctrl Pts',(49.642180948596,-60.4970262936056,-223.417037298108));
#233225=CARTESIAN_POINT('Ctrl Pts',(50.392180948596,-60.9300389954978,-223.85005));
#233226=CARTESIAN_POINT('Ctrl Pts',(50.3921809485959,-60.9300389954977,
-221.195349461621));
#233227=CARTESIAN_POINT('Ctrl Pts',(49.642180948596,-60.4970262936056,-220.945349461621));
#233228=CARTESIAN_POINT('Ctrl Pts',(48.8921809485961,-60.0640135917134,
-221.195349461621));
#233229=CARTESIAN_POINT('Origin',(48.892180948596,-61.7960643992823,-221.35005));
#233230=CARTESIAN_POINT('',(48.892180948596,-61.7960643992823,-220.195349461621));
#233231=CARTESIAN_POINT('',(48.892180948596,-63.7960643992823,-221.35005));
#233232=CARTESIAN_POINT('Origin',(48.892180948596,-61.7960643992823,-223.85005));
#233233=CARTESIAN_POINT('Origin',(48.892180948596,-61.7960643992823,-223.85005));
#233234=CARTESIAN_POINT('Origin',(48.892180948596,-61.7960643992823,-223.85005));
#233235=CARTESIAN_POINT('Origin',(48.892180948596,-61.7960643992823,-223.85005));
#233236=CARTESIAN_POINT('Origin',(48.892180948596,-61.7960643992823,-223.85005));
#233237=CARTESIAN_POINT('Origin',(48.892180948596,-61.7960643992823,-223.85005));
#233238=CARTESIAN_POINT('Origin',(48.892180948596,-61.7960643992823,-223.85005));
#233239=CARTESIAN_POINT('Origin',(48.892180948596,-61.7960643992823,-223.85005));
#233240=CARTESIAN_POINT('Origin',(48.892180948596,-61.7960643992823,-223.85005));
#233241=CARTESIAN_POINT('Origin',(48.892180948596,-61.7960643992823,-223.85005));
#233242=CARTESIAN_POINT('Origin',(48.892180948596,-61.7960643992823,-223.85005));
#233243=CARTESIAN_POINT('Origin',(48.892180948596,-61.7960643992823,-223.85005));
#233244=CARTESIAN_POINT('Origin',(48.892180948596,-61.7960643992823,-223.60005));
#233245=CARTESIAN_POINT('',(48.892180948596,-64.7960643992823,-223.85005));
#233246=CARTESIAN_POINT('Origin',(48.892180948596,-61.7960643992823,-223.85005));
#233247=CARTESIAN_POINT('',(48.892180948596,-65.0460643992823,-223.60005));
#233248=CARTESIAN_POINT('Origin',(48.892180948596,-64.7960643992823,-223.60005));
#233249=CARTESIAN_POINT('',(48.892180948596,-58.5460643992823,-223.60005));
#233250=CARTESIAN_POINT('Origin',(48.892180948596,-61.7960643992823,-223.60005));
#233251=CARTESIAN_POINT('Origin',(48.892180948596,-61.7960643992823,-223.60005));
#233252=CARTESIAN_POINT('Origin',(48.892180948596,-61.7960643992823,-218.35005));
#233253=CARTESIAN_POINT('',(48.892180948596,-58.5460643992823,-218.35005));
#233254=CARTESIAN_POINT('Origin',(48.892180948596,-61.7960643992823,-218.35005));
#233255=CARTESIAN_POINT('Origin',(48.892180948596,-61.7960643992823,-223.85005));
#233256=CARTESIAN_POINT('Origin',(48.892180948596,-61.7960643992823,-223.85005));
#233257=CARTESIAN_POINT('',(48.892180948596,-58.5460643992823,-223.85005));
#233258=CARTESIAN_POINT('Origin',(35.64,75.4199999800001,-156.84995));
#233259=CARTESIAN_POINT('',(54.068191350826,75.4199999800001,-165.506240402784));
#233260=CARTESIAN_POINT('Origin',(54.068191350826,75.4199999800001,-156.84995));
#233261=CARTESIAN_POINT('',(55.5347128540504,71.1699999800001,-157.666957010302));
#233262=CARTESIAN_POINT('',(55.5347128540504,79.6699999800001,-157.666957010302));
#233263=CARTESIAN_POINT('Origin',(35.6422492679874,75.4199999800001,-156.798433293361));
#233264=CARTESIAN_POINT('',(55.5347128540504,71.1699999800001,-156.032942989698));
#233265=CARTESIAN_POINT('Ctrl Pts',(55.5347128540504,71.1699999800001,-157.666957010302));
#233266=CARTESIAN_POINT('Ctrl Pts',(55.5128901885938,71.0676625433561,-157.666004212151));
#233267=CARTESIAN_POINT('Ctrl Pts',(55.4895752701877,70.9585129098176,-157.644597099288));
#233268=CARTESIAN_POINT('Ctrl Pts',(55.4465989628004,70.7576504297677,-157.559247888691));
#233269=CARTESIAN_POINT('Ctrl Pts',(55.4269405591479,70.6659422090179,-157.495293401921));
#233270=CARTESIAN_POINT('Ctrl Pts',(55.3963403195744,70.5233317827474,-157.349523662669));
#233271=CARTESIAN_POINT('Ctrl Pts',(55.3831763635442,70.4620669759979,-157.258753516933));
#233272=CARTESIAN_POINT('Ctrl Pts',(55.3656791431848,70.3806748728845,-157.059753990808));
#233273=CARTESIAN_POINT('Ctrl Pts',(55.361351080024,70.3605621082167,-156.951518209892));
#233274=CARTESIAN_POINT('Ctrl Pts',(55.361351080024,70.3605621082167,-156.748381790108));
#233275=CARTESIAN_POINT('Ctrl Pts',(55.3656791431848,70.3806748728845,-156.640146009192));
#233276=CARTESIAN_POINT('Ctrl Pts',(55.3831763635442,70.4620669759979,-156.441146483066));
#233277=CARTESIAN_POINT('Ctrl Pts',(55.3963403195744,70.5233317827474,-156.350376337331));
#233278=CARTESIAN_POINT('Ctrl Pts',(55.4269405591479,70.6659422090179,-156.204606598079));
#233279=CARTESIAN_POINT('Ctrl Pts',(55.4465989628004,70.7576504297677,-156.140652111309));
#233280=CARTESIAN_POINT('Ctrl Pts',(55.4895752701877,70.9585129098176,-156.055302900712));
#233281=CARTESIAN_POINT('Ctrl Pts',(55.5128901885938,71.0676625433561,-156.033895787849));
#233282=CARTESIAN_POINT('Ctrl Pts',(55.5347128540504,71.1699999800001,-156.032942989698));
#233283=CARTESIAN_POINT('',(55.5347128540504,79.6699999800001,-156.032942989698));
#233284=CARTESIAN_POINT('Origin',(35.6422492679874,75.4199999800001,-156.901466706639));
#233285=CARTESIAN_POINT('Ctrl Pts',(55.5347128540504,79.6699999800001,-156.032942989698));
#233286=CARTESIAN_POINT('Ctrl Pts',(55.5128901885938,79.7723374166442,-156.033895787849));
#233287=CARTESIAN_POINT('Ctrl Pts',(55.4895752701877,79.8814870501826,-156.055302900712));
#233288=CARTESIAN_POINT('Ctrl Pts',(55.4465989628004,80.0823495302325,-156.140652111309));
#233289=CARTESIAN_POINT('Ctrl Pts',(55.4269405591479,80.1740577509823,-156.204606598079));
#233290=CARTESIAN_POINT('Ctrl Pts',(55.3963403195744,80.3166681772527,-156.350376337331));
#233291=CARTESIAN_POINT('Ctrl Pts',(55.3831763635442,80.3779329840023,-156.441146483066));
#233292=CARTESIAN_POINT('Ctrl Pts',(55.3656791431848,80.4593250871157,-156.640146009192));
#233293=CARTESIAN_POINT('Ctrl Pts',(55.361351080024,80.4794378517835,-156.748381790108));
#233294=CARTESIAN_POINT('Ctrl Pts',(55.361351080024,80.4794378517835,-156.951518209892));
#233295=CARTESIAN_POINT('Ctrl Pts',(55.3656791431848,80.4593250871157,-157.059753990808));
#233296=CARTESIAN_POINT('Ctrl Pts',(55.3831763635442,80.3779329840023,-157.258753516933));
#233297=CARTESIAN_POINT('Ctrl Pts',(55.3963403195744,80.3166681772527,-157.349523662669));
#233298=CARTESIAN_POINT('Ctrl Pts',(55.4269405591479,80.1740577509823,-157.495293401921));
#233299=CARTESIAN_POINT('Ctrl Pts',(55.4465989628004,80.0823495302325,-157.559247888691));
#233300=CARTESIAN_POINT('Ctrl Pts',(55.4895752701877,79.8814870501826,-157.644597099288));
#233301=CARTESIAN_POINT('Ctrl Pts',(55.5128901885938,79.7723374166442,-157.666004212151));
#233302=CARTESIAN_POINT('Ctrl Pts',(55.5347128540504,79.6699999800001,-157.666957010302));
#233303=CARTESIAN_POINT('Origin',(53.8419119874809,75.4199999800001,-156.84995));
#233304=CARTESIAN_POINT('',(53.8419119874809,75.4199999800001,-148.04995));
#233305=CARTESIAN_POINT('',(53.8419119874809,75.4199999800001,-165.64995));
#233306=CARTESIAN_POINT('Origin',(53.8419119874809,75.4199999800001,-156.84995));
#233307=CARTESIAN_POINT('Origin',(53.8419119874809,75.4199999800001,-156.84995));
#233308=CARTESIAN_POINT('Origin',(53.8419119874809,75.4199999800001,-165.39995));
#233309=CARTESIAN_POINT('Origin',(52.25,75.4199999800001,-156.84995));
#233310=CARTESIAN_POINT('',(52.,75.4199999800001,-165.39995));
#233311=CARTESIAN_POINT('Origin',(52.,75.4199999800001,-156.84995));
#233312=CARTESIAN_POINT('',(52.25,75.4199999800001,-165.64995));
#233313=CARTESIAN_POINT('Origin',(52.25,75.4199999800001,-165.39995));
#233314=CARTESIAN_POINT('',(52.25,75.4199999800001,-148.04995));
#233315=CARTESIAN_POINT('Origin',(52.25,75.4199999800001,-156.84995));
#233316=CARTESIAN_POINT('Origin',(52.25,75.4199999800001,-156.84995));
#233317=CARTESIAN_POINT('Origin',(54.,79.6699999800001,-156.84995));
#233318=CARTESIAN_POINT('',(54.,79.6699999800001,-156.09995));
#233319=CARTESIAN_POINT('',(54.,79.6699999800001,-157.59995));
#233320=CARTESIAN_POINT('Origin',(54.,79.6699999800001,-156.84995));
#233321=CARTESIAN_POINT('',(54.,71.1699999800001,-156.09995));
#233322=CARTESIAN_POINT('',(54.,79.6699999800001,-156.09995));
#233323=CARTESIAN_POINT('',(54.,71.1699999800001,-157.59995));
#233324=CARTESIAN_POINT('Origin',(54.,71.1699999800001,-156.84995));
#233325=CARTESIAN_POINT('',(54.,79.6699999800001,-157.59995));
#233326=CARTESIAN_POINT('Origin',(54.,79.6699999800001,-157.59995));
#233327=CARTESIAN_POINT('',(54.,79.6699999800001,-157.59995));
#233328=CARTESIAN_POINT('',(54.,71.1699999800001,-157.59995));
#233329=CARTESIAN_POINT('Origin',(54.,71.1699999800001,-156.84995));
#233330=CARTESIAN_POINT('',(54.,71.1699999800001,-156.09995));
#233331=CARTESIAN_POINT('Origin',(54.,79.6699999800001,-156.09995));
#233332=CARTESIAN_POINT('',(54.,79.6699999800001,-156.09995));
#233333=CARTESIAN_POINT('Origin',(54.,79.6699999800001,-156.84995));
#233334=CARTESIAN_POINT('Origin',(49.,75.4199999800001,-156.84995));
#233335=CARTESIAN_POINT('',(49.,75.4199999800001,-149.04995));
#233336=CARTESIAN_POINT('Origin',(49.,75.4199999800001,-156.84995));
#233337=CARTESIAN_POINT('Origin',(49.,75.4199999800001,-156.84995));
#233338=CARTESIAN_POINT('',(52.,75.4199999800001,-149.04995));
#233339=CARTESIAN_POINT('Origin',(52.,75.4199999800001,-156.84995));
#233340=CARTESIAN_POINT('',(49.,75.4199999800001,-149.04995));
#233341=CARTESIAN_POINT('Origin',(27.1098413022335,75.4199999800001,-156.84995));
#233342=CARTESIAN_POINT('',(27.1098413022335,75.4199999800001,-148.04995));
#233343=CARTESIAN_POINT('Origin',(52.,92.9199999800001,-126.84995));
#233344=CARTESIAN_POINT('Origin',(-44.5079524583208,-57.4754524783487,-39.8944822890418));
#233345=CARTESIAN_POINT('',(-46.5079524583208,-57.4754524783487,-40.4194822890418));
#233346=CARTESIAN_POINT('Origin',(-44.5079524583208,-57.4754524783487,-40.4194822890418));
#233347=CARTESIAN_POINT('',(-45.9829524583208,-57.4754524783487,-39.8944822890418));
#233348=CARTESIAN_POINT('',(-45.9829524583208,-57.4754524783487,-39.8944822890418));
#233349=CARTESIAN_POINT('Origin',(-44.5079524583208,-57.4754524783487,-39.8944822890418));
#233350=CARTESIAN_POINT('Origin',(-44.5079524583208,-57.4754524783487,-39.8944822890418));
#233351=CARTESIAN_POINT('Origin',(-44.5079524583208,-57.4754524783487,-39.8944822890418));
#233352=CARTESIAN_POINT('',(-46.5079524583208,-57.4754524783487,-55.24995));
#233353=CARTESIAN_POINT('Origin',(-44.5079524583208,-57.4754524783487,-55.24995));
#233354=CARTESIAN_POINT('',(-46.5079524583208,-57.4754524783487,-39.8944822890418));
#233355=CARTESIAN_POINT('Origin',(0.,45.41999998,-55.24995));
#233356=CARTESIAN_POINT('',(-47.0079524583208,-57.4754524783487,-55.24995));
#233357=CARTESIAN_POINT('Origin',(-44.5079524583208,-57.4754524783487,-55.24995));
#233358=CARTESIAN_POINT('Origin',(-44.5079524583208,-57.4754524783487,-48.1788821881345));
#233359=CARTESIAN_POINT('',(-47.0079524583208,-57.4754524783487,-179.64995));
#233360=CARTESIAN_POINT('Origin',(-44.5079524583208,-57.4754524783487,-179.64995));
#233361=CARTESIAN_POINT('',(-47.0079524583208,-57.4754524783487,-48.1788821881345));
#233362=CARTESIAN_POINT('Origin',(-44.5079524583208,-57.4754524783487,-179.64995));
#233363=CARTESIAN_POINT('Origin',(48.,93.4199999800001,-86.84995));
#233364=CARTESIAN_POINT('',(48.,93.4199999800001,-79.84995));
#233365=CARTESIAN_POINT('',(48.,92.9199999800001,-80.34995));
#233366=CARTESIAN_POINT('Origin',(48.,93.4199999800001,-80.34995));
#233367=CARTESIAN_POINT('',(54.5,92.9199999800001,-86.84995));
#233368=CARTESIAN_POINT('Origin',(48.,92.9199999800001,-86.84995));
#233369=CARTESIAN_POINT('',(55.,93.4199999800001,-86.84995));
#233370=CARTESIAN_POINT('Origin',(54.5,93.4199999800001,-86.84995));
#233371=CARTESIAN_POINT('Origin',(48.,93.4199999800001,-86.84995));
#233372=CARTESIAN_POINT('Origin',(54.5,93.4199999800001,-86.84995));
#233373=CARTESIAN_POINT('',(54.5,92.9199999800001,-182.84995));
#233374=CARTESIAN_POINT('',(55.,93.4199999800001,-182.84995));
#233375=CARTESIAN_POINT('Origin',(54.5,93.4199999800001,-182.84995));
#233376=CARTESIAN_POINT('',(55.,93.4199999800001,-86.84995));
#233377=CARTESIAN_POINT('',(54.5,92.9199999800001,-182.84995));
#233378=CARTESIAN_POINT('Origin',(-51.,93.4199999800001,-80.34995));
#233379=CARTESIAN_POINT('',(-51.,93.4199999800001,-79.84995));
#233380=CARTESIAN_POINT('',(-51.,92.9199999800001,-80.34995));
#233381=CARTESIAN_POINT('Origin',(-51.,93.4199999800001,-80.34995));
#233382=CARTESIAN_POINT('',(-51.,92.9199999800001,-80.34995));
#233383=CARTESIAN_POINT('',(-51.,93.4199999800001,-79.84995));
#233384=CARTESIAN_POINT('Origin',(48.,93.4199999800001,-182.84995));
#233385=CARTESIAN_POINT('',(48.,92.9199999800001,-189.34995));
#233386=CARTESIAN_POINT('',(48.,93.4199999800001,-189.84995));
#233387=CARTESIAN_POINT('Origin',(48.,93.4199999800001,-189.34995));
#233388=CARTESIAN_POINT('Origin',(48.,93.4199999800001,-182.84995));
#233389=CARTESIAN_POINT('Origin',(48.,92.9199999800001,-182.84995));
#233390=CARTESIAN_POINT('Origin',(-51.,93.4199999800001,-86.84995));
#233391=CARTESIAN_POINT('',(-58.,93.4199999800001,-86.84995));
#233392=CARTESIAN_POINT('',(-57.5,92.9199999800001,-86.84995));
#233393=CARTESIAN_POINT('Origin',(-57.5,93.4199999800001,-86.84995));
#233394=CARTESIAN_POINT('Origin',(-51.,92.9199999800001,-86.84995));
#233395=CARTESIAN_POINT('Origin',(-51.,93.4199999800001,-86.84995));
#233396=CARTESIAN_POINT('Origin',(48.,93.4199999800001,-189.34995));
#233397=CARTESIAN_POINT('',(-51.,92.9199999800001,-189.34995));
#233398=CARTESIAN_POINT('',(-51.,93.4199999800001,-189.84995));
#233399=CARTESIAN_POINT('Origin',(-51.,93.4199999800001,-189.34995));
#233400=CARTESIAN_POINT('',(48.,93.4199999800001,-189.84995));
#233401=CARTESIAN_POINT('',(-51.,92.9199999800001,-189.34995));
#233402=CARTESIAN_POINT('Origin',(-57.5,93.4199999800001,-182.84995));
#233403=CARTESIAN_POINT('',(-58.,93.4199999800001,-182.84995));
#233404=CARTESIAN_POINT('',(-57.5,92.9199999800001,-182.84995));
#233405=CARTESIAN_POINT('Origin',(-57.5,93.4199999800001,-182.84995));
#233406=CARTESIAN_POINT('',(-57.5,92.9199999800001,-182.84995));
#233407=CARTESIAN_POINT('',(-58.,93.4199999800001,-86.84995));
#233408=CARTESIAN_POINT('Origin',(-51.,93.4199999800001,-182.84995));
#233409=CARTESIAN_POINT('Origin',(-51.,92.9199999800001,-182.84995));
#233410=CARTESIAN_POINT('Origin',(-51.,93.4199999800001,-182.84995));
#233411=CARTESIAN_POINT('Origin',(-58.,105.91999998,-86.84995));
#233412=CARTESIAN_POINT('',(-58.,94.4199999800001,-182.84995));
#233413=CARTESIAN_POINT('',(-58.,105.91999998,-182.84995));
#233414=CARTESIAN_POINT('',(-58.,94.4199999800001,-86.84995));
#233415=CARTESIAN_POINT('',(-58.,105.91999998,-86.84995));
#233416=CARTESIAN_POINT('',(-58.,94.4199999800001,-86.84995));
#233417=CARTESIAN_POINT('Origin',(-51.,105.91999998,-182.84995));
#233418=CARTESIAN_POINT('',(-51.,94.4199999800001,-189.84995));
#233419=CARTESIAN_POINT('',(-51.,105.91999998,-189.84995));
#233420=CARTESIAN_POINT('Origin',(-51.,94.4199999800001,-182.84995));
#233421=CARTESIAN_POINT('Origin',(-51.,105.91999998,-86.84995));
#233422=CARTESIAN_POINT('',(-51.,94.4199999800001,-79.84995));
#233423=CARTESIAN_POINT('',(-51.,105.91999998,-79.84995));
#233424=CARTESIAN_POINT('Origin',(-51.,94.4199999800001,-86.84995));
#233425=CARTESIAN_POINT('Origin',(-55.,92.9199999800001,-82.84995));
#233426=CARTESIAN_POINT('',(-55.,91.9199999800001,-86.84995));
#233427=CARTESIAN_POINT('',(-55.,59.91999998,-86.84995));
#233428=CARTESIAN_POINT('',(-55.,92.9199999800001,-86.84995));
#233429=CARTESIAN_POINT('',(-55.,91.9199999800001,-182.84995));
#233430=CARTESIAN_POINT('',(-55.,91.9199999800001,-86.84995));
#233431=CARTESIAN_POINT('',(-55.,59.91999998,-182.84995));
#233432=CARTESIAN_POINT('',(-55.,92.9199999800001,-182.84995));
#233433=CARTESIAN_POINT('',(-55.,59.91999998,-182.84995));
#233434=CARTESIAN_POINT('',(-55.,75.4199999800001,-120.64995));
#233435=CARTESIAN_POINT('Origin',(-55.,75.4199999800001,-112.84995));
#233436=CARTESIAN_POINT('',(-55.,75.4199999800001,-164.64995));
#233437=CARTESIAN_POINT('Origin',(-55.,75.4199999800001,-156.84995));
#233438=CARTESIAN_POINT('Origin',(-51.,91.9199999800001,-86.84995));
#233439=CARTESIAN_POINT('',(-56.,92.9199999800001,-86.84995));
#233440=CARTESIAN_POINT('Origin',(-56.,91.9199999800001,-86.84995));
#233441=CARTESIAN_POINT('',(-51.,91.9199999800001,-82.84995));
#233442=CARTESIAN_POINT('Origin',(-51.,91.9199999800001,-86.84995));
#233443=CARTESIAN_POINT('',(-51.,92.9199999800001,-81.84995));
#233444=CARTESIAN_POINT('Origin',(-51.,91.9199999800001,-81.84995));
#233445=CARTESIAN_POINT('Origin',(-51.,92.9199999800001,-86.84995));
#233446=CARTESIAN_POINT('Origin',(-56.,91.9199999800001,-182.84995));
#233447=CARTESIAN_POINT('',(-56.,92.9199999800001,-182.84995));
#233448=CARTESIAN_POINT('Origin',(-56.,91.9199999800001,-182.84995));
#233449=CARTESIAN_POINT('',(-56.,92.9199999800001,-182.84995));
#233450=CARTESIAN_POINT('Origin',(-51.,91.9199999800001,-182.84995));
#233451=CARTESIAN_POINT('',(-51.,91.9199999800001,-186.84995));
#233452=CARTESIAN_POINT('',(-51.,92.9199999800001,-187.84995));
#233453=CARTESIAN_POINT('Origin',(-51.,91.9199999800001,-187.84995));
#233454=CARTESIAN_POINT('Origin',(-51.,91.9199999800001,-182.84995));
#233455=CARTESIAN_POINT('Origin',(-51.,92.9199999800001,-182.84995));
#233456=CARTESIAN_POINT('Origin',(-51.,92.9199999800001,-182.84995));
#233457=CARTESIAN_POINT('',(-51.,59.91999998,-186.84995));
#233458=CARTESIAN_POINT('',(-51.,92.9199999800001,-186.84995));
#233459=CARTESIAN_POINT('Origin',(-51.,59.91999998,-182.84995));
#233460=CARTESIAN_POINT('Origin',(-51.,59.91999998,-182.84995));
#233461=CARTESIAN_POINT('',(-51.,58.91999998,-185.84995));
#233462=CARTESIAN_POINT('Origin',(-51.,59.91999998,-185.84995));
#233463=CARTESIAN_POINT('',(-54.,58.91999998,-182.84995));
#233464=CARTESIAN_POINT('Origin',(-51.,58.91999998,-182.84995));
#233465=CARTESIAN_POINT('Origin',(-54.,59.91999998,-182.84995));
#233466=CARTESIAN_POINT('Origin',(-51.,59.91999998,-86.84995));
#233467=CARTESIAN_POINT('',(-54.,58.91999998,-86.84995));
#233468=CARTESIAN_POINT('Origin',(-54.,59.91999998,-86.84995));
#233469=CARTESIAN_POINT('',(-51.,58.91999998,-83.84995));
#233470=CARTESIAN_POINT('Origin',(-51.,58.91999998,-86.84995));
#233471=CARTESIAN_POINT('',(-51.,59.91999998,-82.84995));
#233472=CARTESIAN_POINT('Origin',(-51.,59.91999998,-83.84995));
#233473=CARTESIAN_POINT('Origin',(-51.,59.91999998,-86.84995));
#233474=CARTESIAN_POINT('Origin',(-54.,59.91999998,-82.84995));
#233475=CARTESIAN_POINT('',(-54.,58.91999998,-86.84995));
#233476=CARTESIAN_POINT('Origin',(-51.,92.9199999800001,-86.84995));
#233477=CARTESIAN_POINT('',(-51.,92.9199999800001,-82.84995));
#233478=CARTESIAN_POINT('Origin',(48.,92.9199999800001,-86.84995));
#233479=CARTESIAN_POINT('',(48.,59.91999998,-82.84995));
#233480=CARTESIAN_POINT('',(48.,91.9199999800001,-82.84995));
#233481=CARTESIAN_POINT('',(48.,92.9199999800001,-82.84995));
#233482=CARTESIAN_POINT('',(52.,59.91999998,-86.84995));
#233483=CARTESIAN_POINT('Origin',(48.,59.91999998,-86.84995));
#233484=CARTESIAN_POINT('',(52.,91.9199999800001,-86.84995));
#233485=CARTESIAN_POINT('',(52.,92.9199999800001,-86.84995));
#233486=CARTESIAN_POINT('Origin',(48.,91.9199999800001,-86.84995));
#233487=CARTESIAN_POINT('Origin',(51.,59.91999998,-82.84995));
#233488=CARTESIAN_POINT('',(51.,58.91999998,-182.84995));
#233489=CARTESIAN_POINT('',(52.,59.91999998,-182.84995));
#233490=CARTESIAN_POINT('Origin',(51.,59.91999998,-182.84995));
#233491=CARTESIAN_POINT('',(52.,59.91999998,-182.84995));
#233492=CARTESIAN_POINT('',(51.,58.91999998,-86.84995));
#233493=CARTESIAN_POINT('Origin',(51.,59.91999998,-86.84995));
#233494=CARTESIAN_POINT('',(51.,58.91999998,-86.84995));
#233495=CARTESIAN_POINT('Origin',(48.,59.91999998,-86.84995));
#233496=CARTESIAN_POINT('',(48.,58.91999998,-83.84995));
#233497=CARTESIAN_POINT('Origin',(48.,59.91999998,-83.84995));
#233498=CARTESIAN_POINT('Origin',(48.,58.91999998,-86.84995));
#233499=CARTESIAN_POINT('Origin',(48.,59.91999998,-182.84995));
#233500=CARTESIAN_POINT('',(48.,58.91999998,-185.84995));
#233501=CARTESIAN_POINT('',(48.,59.91999998,-186.84995));
#233502=CARTESIAN_POINT('Origin',(48.,59.91999998,-185.84995));
#233503=CARTESIAN_POINT('Origin',(48.,59.91999998,-182.84995));
#233504=CARTESIAN_POINT('Origin',(48.,58.91999998,-182.84995));
#233505=CARTESIAN_POINT('Origin',(48.,92.9199999800001,-182.84995));
#233506=CARTESIAN_POINT('',(52.,91.9199999800001,-182.84995));
#233507=CARTESIAN_POINT('',(52.,92.9199999800001,-182.84995));
#233508=CARTESIAN_POINT('',(48.,91.9199999800001,-186.84995));
#233509=CARTESIAN_POINT('',(48.,92.9199999800001,-186.84995));
#233510=CARTESIAN_POINT('Origin',(48.,91.9199999800001,-182.84995));
#233511=CARTESIAN_POINT('Origin',(48.,91.9199999800001,-182.84995));
#233512=CARTESIAN_POINT('',(48.,92.9199999800001,-187.84995));
#233513=CARTESIAN_POINT('Origin',(48.,91.9199999800001,-187.84995));
#233514=CARTESIAN_POINT('',(53.,92.9199999800001,-182.84995));
#233515=CARTESIAN_POINT('Origin',(48.,92.9199999800001,-182.84995));
#233516=CARTESIAN_POINT('Origin',(53.,91.9199999800001,-182.84995));
#233517=CARTESIAN_POINT('Origin',(53.,91.9199999800001,-182.84995));
#233518=CARTESIAN_POINT('',(53.,92.9199999800001,-86.84995));
#233519=CARTESIAN_POINT('',(53.,92.9199999800001,-182.84995));
#233520=CARTESIAN_POINT('Origin',(53.,91.9199999800001,-86.84995));
#233521=CARTESIAN_POINT('',(52.,91.9199999800001,-86.84995));
#233522=CARTESIAN_POINT('Origin',(48.,91.9199999800001,-86.84995));
#233523=CARTESIAN_POINT('',(48.,92.9199999800001,-81.84995));
#233524=CARTESIAN_POINT('Origin',(48.,92.9199999800001,-86.84995));
#233525=CARTESIAN_POINT('Origin',(48.,91.9199999800001,-81.84995));
#233526=CARTESIAN_POINT('Origin',(52.,92.9199999800001,-82.84995));
#233527=CARTESIAN_POINT('',(52.,75.4199999800001,-120.64995));
#233528=CARTESIAN_POINT('Origin',(52.,75.4199999800001,-112.84995));
#233529=CARTESIAN_POINT('',(52.,75.4199999800001,-164.64995));
#233530=CARTESIAN_POINT('Origin',(52.,75.4199999800001,-156.84995));
#233531=CARTESIAN_POINT('Origin',(48.,105.91999998,-86.84995));
#233532=CARTESIAN_POINT('',(48.,94.4199999800001,-79.84995));
#233533=CARTESIAN_POINT('',(48.,105.91999998,-79.84995));
#233534=CARTESIAN_POINT('',(55.,94.4199999800001,-86.84995));
#233535=CARTESIAN_POINT('',(55.,105.91999998,-86.84995));
#233536=CARTESIAN_POINT('Origin',(48.,94.4199999800001,-86.84995));
#233537=CARTESIAN_POINT('Origin',(48.,105.91999998,-182.84995));
#233538=CARTESIAN_POINT('',(55.,94.4199999800001,-182.84995));
#233539=CARTESIAN_POINT('',(55.,105.91999998,-182.84995));
#233540=CARTESIAN_POINT('',(48.,94.4199999800001,-189.84995));
#233541=CARTESIAN_POINT('',(48.,105.91999998,-189.84995));
#233542=CARTESIAN_POINT('Origin',(48.,94.4199999800001,-182.84995));
#233543=CARTESIAN_POINT('Origin',(-51.,91.9199999800001,-81.84995));
#233544=CARTESIAN_POINT('',(48.,92.9199999800001,-81.84995));
#233545=CARTESIAN_POINT('',(-1.5,91.9199999800001,-82.84995));
#233546=CARTESIAN_POINT('Origin',(-55.,92.9199999800001,-82.84995));
#233547=CARTESIAN_POINT('',(48.,59.91999998,-82.84995));
#233548=CARTESIAN_POINT('Origin',(-55.,59.91999998,-83.84995));
#233549=CARTESIAN_POINT('',(-1.5,58.91999998,-83.84995));
#233550=CARTESIAN_POINT('Origin',(-1.5,58.91999998,0.));
#233551=CARTESIAN_POINT('',(48.,58.91999998,-185.84995));
#233552=CARTESIAN_POINT('Origin',(-55.,59.91999998,-185.84995));
#233553=CARTESIAN_POINT('',(-1.5,59.91999998,-186.84995));
#233554=CARTESIAN_POINT('Origin',(-55.,92.9199999800001,-186.84995));
#233555=CARTESIAN_POINT('',(48.,91.9199999800001,-186.84995));
#233556=CARTESIAN_POINT('Origin',(-51.,91.9199999800001,-187.84995));
#233557=CARTESIAN_POINT('',(-1.5,92.9199999800001,-187.84995));
#233558=CARTESIAN_POINT('Origin',(-51.,92.9199999800001,-182.84995));
#233559=CARTESIAN_POINT('Origin',(48.,105.91999998,-189.84995));
#233560=CARTESIAN_POINT('',(48.,94.4199999800001,-189.84995));
#233561=CARTESIAN_POINT('Origin',(-51.,105.91999998,-79.84995));
#233562=CARTESIAN_POINT('',(-51.,94.4199999800001,-79.84995));
#233563=CARTESIAN_POINT('Origin',(151.5,75.4199999800001,-112.84995));
#233564=CARTESIAN_POINT('',(151.5,75.4199999800001,-120.64995));
#233565=CARTESIAN_POINT('Origin',(151.5,75.4199999800001,-156.84995));
#233566=CARTESIAN_POINT('',(151.5,75.4199999800001,-164.64995));
#233567=CARTESIAN_POINT('Origin',(55.,105.91999998,-86.84995));
#233568=CARTESIAN_POINT('',(55.,94.4199999800001,-86.84995));
#233569=CARTESIAN_POINT('Origin',(55.01,94.4199999800001,-52.64995));
#233570=CARTESIAN_POINT('Origin',(35.64,75.4199999800001,-112.84995));
#233571=CARTESIAN_POINT('',(54.068191350826,75.4199999800001,-121.506240402785));
#233572=CARTESIAN_POINT('Origin',(54.068191350826,75.4199999800001,-112.84995));
#233573=CARTESIAN_POINT('',(55.5347128540504,71.1699999800001,-113.666957010302));
#233574=CARTESIAN_POINT('',(55.5347128540504,79.6699999800001,-113.666957010302));
#233575=CARTESIAN_POINT('Origin',(35.6422492679874,75.4199999800001,-112.798433293361));
#233576=CARTESIAN_POINT('',(55.5347128540504,71.1699999800001,-112.032942989698));
#233577=CARTESIAN_POINT('Ctrl Pts',(55.5347128540504,71.1699999800001,-113.666957010302));
#233578=CARTESIAN_POINT('Ctrl Pts',(55.5128901885938,71.0676625433561,-113.666004212151));
#233579=CARTESIAN_POINT('Ctrl Pts',(55.4895752701877,70.9585129098177,-113.644597099288));
#233580=CARTESIAN_POINT('Ctrl Pts',(55.4465989628004,70.7576504297677,-113.559247888691));
#233581=CARTESIAN_POINT('Ctrl Pts',(55.4269405591479,70.6659422090179,-113.495293401921));
#233582=CARTESIAN_POINT('Ctrl Pts',(55.3963403195744,70.5233317827474,-113.349523662669));
#233583=CARTESIAN_POINT('Ctrl Pts',(55.3831763635442,70.4620669759979,-113.258753516934));
#233584=CARTESIAN_POINT('Ctrl Pts',(55.3656791431848,70.3806748728845,-113.059753990808));
#233585=CARTESIAN_POINT('Ctrl Pts',(55.361351080024,70.3605621082167,-112.951518209892));
#233586=CARTESIAN_POINT('Ctrl Pts',(55.361351080024,70.3605621082167,-112.748381790108));
#233587=CARTESIAN_POINT('Ctrl Pts',(55.3656791431848,70.3806748728845,-112.640146009192));
#233588=CARTESIAN_POINT('Ctrl Pts',(55.3831763635442,70.4620669759979,-112.441146483067));
#233589=CARTESIAN_POINT('Ctrl Pts',(55.3963403195744,70.5233317827474,-112.350376337331));
#233590=CARTESIAN_POINT('Ctrl Pts',(55.4269405591479,70.6659422090179,-112.204606598079));
#233591=CARTESIAN_POINT('Ctrl Pts',(55.4465989628004,70.7576504297677,-112.140652111309));
#233592=CARTESIAN_POINT('Ctrl Pts',(55.4895752701877,70.9585129098177,-112.055302900712));
#233593=CARTESIAN_POINT('Ctrl Pts',(55.5128901885938,71.0676625433561,-112.033895787849));
#233594=CARTESIAN_POINT('Ctrl Pts',(55.5347128540504,71.1699999800001,-112.032942989698));
#233595=CARTESIAN_POINT('',(55.5347128540504,79.6699999800001,-112.032942989698));
#233596=CARTESIAN_POINT('Origin',(35.6422492679874,75.4199999800001,-112.901466706639));
#233597=CARTESIAN_POINT('Ctrl Pts',(55.5347128540504,79.6699999800001,-112.032942989698));
#233598=CARTESIAN_POINT('Ctrl Pts',(55.5128901885938,79.7723374166442,-112.033895787849));
#233599=CARTESIAN_POINT('Ctrl Pts',(55.4895752701877,79.8814870501826,-112.055302900712));
#233600=CARTESIAN_POINT('Ctrl Pts',(55.4465989628004,80.0823495302325,-112.140652111309));
#233601=CARTESIAN_POINT('Ctrl Pts',(55.4269405591479,80.1740577509823,-112.204606598079));
#233602=CARTESIAN_POINT('Ctrl Pts',(55.3963403195744,80.3166681772527,-112.350376337331));
#233603=CARTESIAN_POINT('Ctrl Pts',(55.3831763635442,80.3779329840023,-112.441146483067));
#233604=CARTESIAN_POINT('Ctrl Pts',(55.3656791431848,80.4593250871157,-112.640146009192));
#233605=CARTESIAN_POINT('Ctrl Pts',(55.361351080024,80.4794378517835,-112.748381790108));
#233606=CARTESIAN_POINT('Ctrl Pts',(55.361351080024,80.4794378517835,-112.951518209892));
#233607=CARTESIAN_POINT('Ctrl Pts',(55.3656791431848,80.4593250871157,-113.059753990808));
#233608=CARTESIAN_POINT('Ctrl Pts',(55.3831763635442,80.3779329840023,-113.258753516933));
#233609=CARTESIAN_POINT('Ctrl Pts',(55.3963403195744,80.3166681772527,-113.349523662669));
#233610=CARTESIAN_POINT('Ctrl Pts',(55.4269405591479,80.1740577509823,-113.495293401921));
#233611=CARTESIAN_POINT('Ctrl Pts',(55.4465989628004,80.0823495302325,-113.559247888691));
#233612=CARTESIAN_POINT('Ctrl Pts',(55.4895752701877,79.8814870501826,-113.644597099288));
#233613=CARTESIAN_POINT('Ctrl Pts',(55.5128901885938,79.7723374166442,-113.666004212151));
#233614=CARTESIAN_POINT('Ctrl Pts',(55.5347128540504,79.6699999800001,-113.666957010302));
#233615=CARTESIAN_POINT('Origin',(53.8419119874809,75.4199999800001,-112.84995));
#233616=CARTESIAN_POINT('',(53.8419119874809,75.4199999800001,-104.04995));
#233617=CARTESIAN_POINT('',(53.8419119874809,75.4199999800001,-121.64995));
#233618=CARTESIAN_POINT('Origin',(53.8419119874809,75.4199999800001,-112.84995));
#233619=CARTESIAN_POINT('Origin',(53.8419119874809,75.4199999800001,-112.84995));
#233620=CARTESIAN_POINT('Origin',(53.8419119874809,75.4199999800001,-121.39995));
#233621=CARTESIAN_POINT('Origin',(52.25,75.4199999800001,-112.84995));
#233622=CARTESIAN_POINT('',(52.,75.4199999800001,-121.39995));
#233623=CARTESIAN_POINT('Origin',(52.,75.4199999800001,-112.84995));
#233624=CARTESIAN_POINT('',(52.25,75.4199999800001,-121.64995));
#233625=CARTESIAN_POINT('Origin',(52.25,75.4199999800001,-121.39995));
#233626=CARTESIAN_POINT('',(52.25,75.4199999800001,-104.04995));
#233627=CARTESIAN_POINT('Origin',(52.25,75.4199999800001,-112.84995));
#233628=CARTESIAN_POINT('Origin',(52.25,75.4199999800001,-112.84995));
#233629=CARTESIAN_POINT('Origin',(54.,79.6699999800001,-112.84995));
#233630=CARTESIAN_POINT('',(54.,79.6699999800001,-112.09995));
#233631=CARTESIAN_POINT('',(54.,79.6699999800001,-113.59995));
#233632=CARTESIAN_POINT('Origin',(54.,79.6699999800001,-112.84995));
#233633=CARTESIAN_POINT('',(54.,71.1699999800001,-112.09995));
#233634=CARTESIAN_POINT('',(54.,79.6699999800001,-112.09995));
#233635=CARTESIAN_POINT('',(54.,71.1699999800001,-113.59995));
#233636=CARTESIAN_POINT('Origin',(54.,71.1699999800001,-112.84995));
#233637=CARTESIAN_POINT('',(54.,79.6699999800001,-113.59995));
#233638=CARTESIAN_POINT('Origin',(54.,79.6699999800001,-113.59995));
#233639=CARTESIAN_POINT('',(54.,79.6699999800001,-113.59995));
#233640=CARTESIAN_POINT('',(54.,71.1699999800001,-113.59995));
#233641=CARTESIAN_POINT('Origin',(54.,71.1699999800001,-112.84995));
#233642=CARTESIAN_POINT('',(54.,71.1699999800001,-112.09995));
#233643=CARTESIAN_POINT('Origin',(54.,79.6699999800001,-112.09995));
#233644=CARTESIAN_POINT('',(54.,79.6699999800001,-112.09995));
#233645=CARTESIAN_POINT('Origin',(54.,79.6699999800001,-112.84995));
#233646=CARTESIAN_POINT('Origin',(49.,75.4199999800001,-112.84995));
#233647=CARTESIAN_POINT('',(49.,75.4199999800001,-105.04995));
#233648=CARTESIAN_POINT('Origin',(49.,75.4199999800001,-112.84995));
#233649=CARTESIAN_POINT('Origin',(49.,75.4199999800001,-112.84995));
#233650=CARTESIAN_POINT('',(52.,75.4199999800001,-105.04995));
#233651=CARTESIAN_POINT('Origin',(52.,75.4199999800001,-112.84995));
#233652=CARTESIAN_POINT('',(49.,75.4199999800001,-105.04995));
#233653=CARTESIAN_POINT('Origin',(27.1098413022335,75.4199999800001,-112.84995));
#233654=CARTESIAN_POINT('',(27.1098413022335,75.4199999800001,-104.04995));
#233655=CARTESIAN_POINT('Origin',(52.,92.9199999800001,-82.84995));
#233656=CARTESIAN_POINT('Origin',(48.6475142708864,46.7952694142692,-180.14995));
#233657=CARTESIAN_POINT('',(41.086116694801,39.9409786193705,-180.14995));
#233658=CARTESIAN_POINT('',(41.4396700853943,39.5874252287771,-179.64995));
#233659=CARTESIAN_POINT('Origin',(41.4396700853943,39.5874252287771,-180.14995));
#233660=CARTESIAN_POINT('',(48.6849040646875,46.8326592080703,-179.64995));
#233661=CARTESIAN_POINT('',(41.4396700853943,39.5874252287771,-179.64995));
#233662=CARTESIAN_POINT('',(48.2939608802931,47.1488228048625,-180.14995));
#233663=CARTESIAN_POINT('Ctrl Pts',(48.2939608802932,47.1488228048625,-180.14995));
#233664=CARTESIAN_POINT('Ctrl Pts',(48.2939608802932,47.1488228048625,-180.087184163359));
#233665=CARTESIAN_POINT('Ctrl Pts',(48.3037994668372,47.1409231885199,-180.020261450625));
#233666=CARTESIAN_POINT('Ctrl Pts',(48.3437200901627,47.1088207011521,-179.897213130352));
#233667=CARTESIAN_POINT('Ctrl Pts',(48.3737972006442,47.0846160842381,-179.84108638012));
#233668=CARTESIAN_POINT('Ctrl Pts',(48.443221456874,47.0286267129769,-179.752211869064));
#233669=CARTESIAN_POINT('Ctrl Pts',(48.4872746644709,46.9930450683611,-179.713637732877));
#233670=CARTESIAN_POINT('Ctrl Pts',(48.5836337459409,46.9149957840453,-179.662507580811));
#233671=CARTESIAN_POINT('Ctrl Pts',(48.6359363487773,46.8725251312072,-179.64995));
#233672=CARTESIAN_POINT('Ctrl Pts',(48.6849040646876,46.8326592080703,-179.64995));
#233673=CARTESIAN_POINT('',(48.2939608802931,47.1488228048625,-180.14995));
#233674=CARTESIAN_POINT('Origin',(40.7325633042078,40.2945320099637,-180.14995));
#233675=CARTESIAN_POINT('',(40.7325633042078,39.7945320099637,-180.14995));
#233676=CARTESIAN_POINT('',(40.7325633042078,39.2945320099637,-179.64995));
#233677=CARTESIAN_POINT('Origin',(40.7325633042078,39.2945320099637,-180.14995));
#233678=CARTESIAN_POINT('Origin',(40.7325633042078,40.2945320099637,-179.64995));
#233679=CARTESIAN_POINT('Origin',(40.7325633042078,40.2945320099637,-180.14995));
#233680=CARTESIAN_POINT('Origin',(39.9396700853943,39.2945320099637,-180.14995));
#233681=CARTESIAN_POINT('',(40.4396700853943,39.7945320099637,-180.14995));
#233682=CARTESIAN_POINT('',(40.4396700853943,39.2945320099637,-179.64995));
#233683=CARTESIAN_POINT('Origin',(40.4396700853943,39.2945320099637,-180.14995));
#233684=CARTESIAN_POINT('',(40.4396700853943,39.2945320099637,-179.64995));
#233685=CARTESIAN_POINT('',(40.7325633042078,39.7945320099637,-180.14995));
#233686=CARTESIAN_POINT('Origin',(40.4396700853943,40.2945320099637,-180.14995));
#233687=CARTESIAN_POINT('',(39.9396700853943,40.2945320099637,-180.14995));
#233688=CARTESIAN_POINT('',(39.4396700853942,40.2945320099637,-179.64995));
#233689=CARTESIAN_POINT('Origin',(39.4396700853942,40.2945320099637,-180.14995));
#233690=CARTESIAN_POINT('Origin',(40.4396700853943,40.2945320099637,-179.64995));
#233691=CARTESIAN_POINT('Origin',(40.4396700853943,40.2945320099637,-180.14995));
#233692=CARTESIAN_POINT('Origin',(39.4396700853942,49.9558747416749,-180.14995));
#233693=CARTESIAN_POINT('',(39.4396700853942,50.0426929113215,-179.64995));
#233694=CARTESIAN_POINT('',(39.9396700853943,49.9558747416749,-180.14995));
#233695=CARTESIAN_POINT('Ctrl Pts',(39.4396700853942,50.0426929113213,-179.64995));
#233696=CARTESIAN_POINT('Ctrl Pts',(39.5025092537829,50.0318525348131,-179.64995));
#233697=CARTESIAN_POINT('Ctrl Pts',(39.5695953475419,50.0202501005871,-179.662513814803));
#233698=CARTESIAN_POINT('Ctrl Pts',(39.6931562106457,49.9988279173233,-179.713808517639));
#233699=CARTESIAN_POINT('Ctrl Pts',(39.7496292333555,49.9890099683669,-179.752544364656));
#233700=CARTESIAN_POINT('Ctrl Pts',(39.8381537765163,49.973597171116,-179.841586696561));
#233701=CARTESIAN_POINT('Ctrl Pts',(39.8763752988257,49.9669287636703,-179.897554483501));
#233702=CARTESIAN_POINT('Ctrl Pts',(39.9271363480647,49.9580662763262,-180.020367660125));
#233703=CARTESIAN_POINT('Ctrl Pts',(39.9396700853942,49.9558747416746,-180.087215626338));
#233704=CARTESIAN_POINT('Ctrl Pts',(39.9396700853942,49.9558747416746,-180.14995));
#233705=CARTESIAN_POINT('',(39.4396700853942,49.9558747416749,-179.64995));
#233706=CARTESIAN_POINT('',(39.9396700853943,40.2945320099637,-180.14995));
#233707=CARTESIAN_POINT('Origin',(39.4396700853942,-64.8856746638358,-180.14995));
#233708=CARTESIAN_POINT('',(39.9396700853942,-65.3856746638358,-180.14995));
#233709=CARTESIAN_POINT('',(39.4396700853942,-65.3856746638358,-179.64995));
#233710=CARTESIAN_POINT('Origin',(39.4396700853942,-65.3856746638358,-180.14995));
#233711=CARTESIAN_POINT('',(39.4396700853942,-75.2524362554308,-179.64995));
#233712=CARTESIAN_POINT('',(39.4396700853942,-65.3856746638358,-179.64995));
#233713=CARTESIAN_POINT('',(39.9396700853942,-75.2524362554308,-180.14995));
#233714=CARTESIAN_POINT('Origin',(39.4396700853942,-75.2524362554308,-180.14995));
#233715=CARTESIAN_POINT('',(39.9396700853942,-75.2524362554308,-180.14995));
#233716=CARTESIAN_POINT('Origin',(40.4396700853942,-65.3856746638358,-180.14995));
#233717=CARTESIAN_POINT('',(40.4396700853942,-64.8856746638358,-180.14995));
#233718=CARTESIAN_POINT('',(40.4396700853943,-64.3856746638358,-179.64995));
#233719=CARTESIAN_POINT('Origin',(40.4396700853943,-64.3856746638358,-180.14995));
#233720=CARTESIAN_POINT('Origin',(40.4396700853942,-65.3856746638358,-179.64995));
#233721=CARTESIAN_POINT('Origin',(40.4396700853942,-65.3856746638358,-180.14995));
#233722=CARTESIAN_POINT('Origin',(39.9396700853942,-64.3856746638358,-180.14995));
#233723=CARTESIAN_POINT('',(40.7325633042077,-64.8856746638358,-180.14995));
#233724=CARTESIAN_POINT('',(40.7325633042078,-64.3856746638358,-179.64995));
#233725=CARTESIAN_POINT('Origin',(40.7325633042078,-64.3856746638358,-180.14995));
#233726=CARTESIAN_POINT('',(40.7325633042078,-64.3856746638358,-179.64995));
#233727=CARTESIAN_POINT('',(40.4396700853942,-64.8856746638358,-180.14995));
#233728=CARTESIAN_POINT('Origin',(40.7325633042077,-65.3856746638358,-180.14995));
#233729=CARTESIAN_POINT('',(41.086116694801,-65.0321212732425,-180.14995));
#233730=CARTESIAN_POINT('',(41.4396700853943,-64.6785678826493,-179.64995));
#233731=CARTESIAN_POINT('Origin',(41.4396700853943,-64.6785678826493,-180.14995));
#233732=CARTESIAN_POINT('Origin',(40.7325633042077,-65.3856746638358,-179.64995));
#233733=CARTESIAN_POINT('Origin',(40.7325633042077,-65.3856746638358,-180.14995));
#233734=CARTESIAN_POINT('Origin',(49.1137948708872,-72.3526926681422,-180.14995));
#233735=CARTESIAN_POINT('',(49.1484061576371,-72.3873039548922,-179.64995));
#233736=CARTESIAN_POINT('',(48.7602414802939,-72.7062460587355,-180.14995));
#233737=CARTESIAN_POINT('Ctrl Pts',(49.1484061576372,-72.3873039548922,
-179.64995));
#233738=CARTESIAN_POINT('Ctrl Pts',(49.0997901061269,-72.4275161617186,
-179.64995));
#233739=CARTESIAN_POINT('Ctrl Pts',(49.0478648385672,-72.470354734769,-179.662506414177));
#233740=CARTESIAN_POINT('Ctrl Pts',(48.9522061528442,-72.5490766792219,
-179.713622094328));
#233741=CARTESIAN_POINT('Ctrl Pts',(48.9084759486685,-72.5849631007156,
-179.752182677537));
#233742=CARTESIAN_POINT('Ctrl Pts',(48.8395335697769,-72.6414546742699,
-179.841043950726));
#233743=CARTESIAN_POINT('Ctrl Pts',(48.8096591731515,-72.6658815244501,
-179.89718443088));
#233744=CARTESIAN_POINT('Ctrl Pts',(48.7700107976248,-72.6982762551188,
-180.020252853856));
#233745=CARTESIAN_POINT('Ctrl Pts',(48.760241480294,-72.7062460587355,-180.087181792204));
#233746=CARTESIAN_POINT('Ctrl Pts',(48.760241480294,-72.7062460587355,-180.14995));
#233747=CARTESIAN_POINT('',(49.1137948708872,-72.3526926681422,-179.64995));
#233748=CARTESIAN_POINT('',(41.086116694801,-65.0321212732425,-180.14995));
#233749=CARTESIAN_POINT('Origin',(61.6666822880186,-45.93000002,-189.64995));
#233750=CARTESIAN_POINT('',(62.1666822880186,-45.93000002,-182.64995));
#233751=CARTESIAN_POINT('',(61.6666822880186,-46.43000002,-182.64995));
#233752=CARTESIAN_POINT('Origin',(61.6666822880186,-45.93000002,-182.64995));
#233753=CARTESIAN_POINT('',(61.6666822880186,-46.43000002,-189.64995));
#233754=CARTESIAN_POINT('',(61.6666822880186,-46.43000002,-236.10005));
#233755=CARTESIAN_POINT('',(62.1666822880186,-45.93000002,-189.64995));
#233756=CARTESIAN_POINT('Origin',(61.6666822880186,-45.93000002,-189.64995));
#233757=CARTESIAN_POINT('',(62.1666822880186,-45.93000002,-189.64995));
#233758=CARTESIAN_POINT('Origin',(59.1666822880186,-45.93000002,-182.64995));
#233759=CARTESIAN_POINT('',(59.1666822880186,-45.93000002,-179.64995));
#233760=CARTESIAN_POINT('',(59.1666822880186,-46.43000002,-180.14995));
#233761=CARTESIAN_POINT('Origin',(59.1666822880186,-45.93000002,-180.14995));
#233762=CARTESIAN_POINT('Origin',(59.1666822880186,-46.43000002,-182.64995));
#233763=CARTESIAN_POINT('Origin',(59.1666822880186,-45.93000002,-182.64995));
#233764=CARTESIAN_POINT('Origin',(51.5042290374232,-45.93000002,-180.14995));
#233765=CARTESIAN_POINT('',(51.9388724063314,-45.93000002,-179.64995));
#233766=CARTESIAN_POINT('',(51.9388724063314,-46.43000002,-180.14995));
#233767=CARTESIAN_POINT('Origin',(51.9388724063314,-45.93000002,-180.14995));
#233768=CARTESIAN_POINT('',(51.9388724063314,-46.43000002,-180.14995));
#233769=CARTESIAN_POINT('',(59.1666822880186,-45.93000002,-179.64995));
#233770=CARTESIAN_POINT('Origin',(51.9388724063314,-46.93000002,-180.14995));
#233771=CARTESIAN_POINT('',(50.9486043375898,-46.7908269190399,-179.64995));
#233772=CARTESIAN_POINT('',(51.4437383719606,-46.8604134695199,-180.14995));
#233773=CARTESIAN_POINT('Origin',(50.9486043375898,-46.7908269190399,-180.14995));
#233774=CARTESIAN_POINT('Origin',(51.9388724063314,-46.93000002,-180.14995));
#233775=CARTESIAN_POINT('Origin',(51.9388724063314,-46.93000002,-179.64995));
#233776=CARTESIAN_POINT('Origin',(52.1173462765794,-38.4747959130728,-180.14995));
#233777=CARTESIAN_POINT('',(50.1545486215213,-52.4408269190399,-179.64995));
#233778=CARTESIAN_POINT('',(50.6496826558921,-52.51041346952,-180.14995));
#233779=CARTESIAN_POINT('Origin',(50.1545486215213,-52.4408269190399,-180.14995));
#233780=CARTESIAN_POINT('',(52.6124803109501,-38.5443824635529,-180.14995));
#233781=CARTESIAN_POINT('',(50.0744984522816,-53.0104134695199,-179.64995));
#233782=CARTESIAN_POINT('Origin',(51.1448166902628,-52.58000002,-180.14995));
#233783=CARTESIAN_POINT('',(51.1448166902628,-53.58000002,-179.64995));
#233784=CARTESIAN_POINT('',(51.1448166902628,-53.08000002,-180.14995));
#233785=CARTESIAN_POINT('Origin',(51.1448166902628,-53.58000002,-180.14995));
#233786=CARTESIAN_POINT('Origin',(51.1448166902628,-52.58000002,-180.14995));
#233787=CARTESIAN_POINT('Origin',(51.1448166902628,-52.58000002,-179.64995));
#233788=CARTESIAN_POINT('Origin',(50.5696324866523,-53.58000002,-180.14995));
#233789=CARTESIAN_POINT('',(59.1666822880186,-53.58000002,-179.64995));
#233790=CARTESIAN_POINT('',(59.1666822880186,-53.08000002,-180.14995));
#233791=CARTESIAN_POINT('Origin',(59.1666822880186,-53.58000002,-180.14995));
#233792=CARTESIAN_POINT('',(59.1666822880186,-53.08000002,-180.14995));
#233793=CARTESIAN_POINT('',(51.1448166902628,-53.58000002,-179.64995));
#233794=CARTESIAN_POINT('Origin',(59.1666822880186,-53.58000002,-182.64995));
#233795=CARTESIAN_POINT('',(62.1666822880186,-53.58000002,-182.64995));
#233796=CARTESIAN_POINT('',(61.6666822880186,-53.08000002,-182.64995));
#233797=CARTESIAN_POINT('Origin',(61.6666822880186,-53.58000002,-182.64995));
#233798=CARTESIAN_POINT('Origin',(59.1666822880186,-53.08000002,-182.64995));
#233799=CARTESIAN_POINT('Origin',(59.1666822880186,-53.58000002,-182.64995));
#233800=CARTESIAN_POINT('Origin',(61.6666822880186,-53.58000002,-189.64995));
#233801=CARTESIAN_POINT('',(61.6666822880186,-53.08000002,-189.64995));
#233802=CARTESIAN_POINT('',(62.1666822880186,-53.58000002,-189.64995));
#233803=CARTESIAN_POINT('Origin',(61.6666822880186,-53.58000002,-189.64995));
#233804=CARTESIAN_POINT('',(61.6666822880186,-53.08000002,-236.10005));
#233805=CARTESIAN_POINT('',(62.1666822880186,-53.58000002,-189.64995));
#233806=CARTESIAN_POINT('Origin',(61.6666822880186,-53.9537553161325,-189.64995));
#233807=CARTESIAN_POINT('',(62.1666822880186,-53.9537553161325,-189.64995));
#233808=CARTESIAN_POINT('',(61.6666822880186,-54.4537553161325,-189.64995));
#233809=CARTESIAN_POINT('Origin',(61.6666822880186,-53.9537553161325,-189.64995));
#233810=CARTESIAN_POINT('',(62.1666822880186,-53.9537553161325,-182.64995));
#233811=CARTESIAN_POINT('',(62.1666822880186,-53.9537553161325,-189.64995));
#233812=CARTESIAN_POINT('',(61.6666822880186,-54.4537553161325,-182.64995));
#233813=CARTESIAN_POINT('Origin',(61.6666822880186,-53.9537553161325,-182.64995));
#233814=CARTESIAN_POINT('',(61.6666822880186,-54.4537553161325,-189.64995));
#233815=CARTESIAN_POINT('Origin',(59.1666822880186,-53.9537553161325,-182.64995));
#233816=CARTESIAN_POINT('',(59.1666822880186,-53.9537553161325,-179.64995));
#233817=CARTESIAN_POINT('',(59.1666822880186,-54.4537553161325,-180.14995));
#233818=CARTESIAN_POINT('Origin',(59.1666822880186,-53.9537553161325,-180.14995));
#233819=CARTESIAN_POINT('Origin',(59.1666822880186,-54.4537553161325,-182.64995));
#233820=CARTESIAN_POINT('Origin',(59.1666822880186,-53.9537553161325,-182.64995));
#233821=CARTESIAN_POINT('Origin',(62.1666822880186,-53.9537553161325,-180.14995));
#233822=CARTESIAN_POINT('',(53.361677340714,-53.9537553161325,-179.64995));
#233823=CARTESIAN_POINT('',(53.361677340714,-54.4537553161325,-180.14995));
#233824=CARTESIAN_POINT('Origin',(53.361677340714,-53.9537553161325,-180.14995));
#233825=CARTESIAN_POINT('',(53.361677340714,-54.4537553161325,-180.14995));
#233826=CARTESIAN_POINT('',(59.1666822880186,-53.9537553161325,-179.64995));
#233827=CARTESIAN_POINT('Origin',(53.361677340714,-54.9537553161325,-180.14995));
#233828=CARTESIAN_POINT('',(52.6545705595274,-55.6608620973191,-179.64995));
#233829=CARTESIAN_POINT('',(53.0081239501207,-55.3073087067258,-180.14995));
#233830=CARTESIAN_POINT('Origin',(52.6545705595274,-55.6608620973191,-180.14995));
#233831=CARTESIAN_POINT('Origin',(53.361677340714,-54.9537553161325,-180.14995));
#233832=CARTESIAN_POINT('Origin',(53.361677340714,-54.9537553161325,-179.64995));
#233833=CARTESIAN_POINT('Origin',(59.2455673951362,-62.2518589329279,-180.14995));
#233834=CARTESIAN_POINT('',(59.5991207857295,-61.8983055423346,-180.14995));
#233835=CARTESIAN_POINT('',(59.2791589653485,-62.2854505031402,-179.64995));
#233836=CARTESIAN_POINT('Ctrl Pts',(59.5991207857295,-61.8983055423347,
-180.14995));
#233837=CARTESIAN_POINT('Ctrl Pts',(59.5991207857295,-61.8983055423347,
-180.087180970045));
#233838=CARTESIAN_POINT('Ctrl Pts',(59.591125231612,-61.9080494267527,-180.020249867196));
#233839=CARTESIAN_POINT('Ctrl Pts',(59.558623384557,-61.947597642818,-179.89717444851));
#233840=CARTESIAN_POINT('Ctrl Pts',(59.5341151062373,-61.9773974043459,
-179.841029188496));
#233841=CARTESIAN_POINT('Ctrl Pts',(59.4774393533586,-62.0461626981974,
-179.752172507515));
#233842=CARTESIAN_POINT('Ctrl Pts',(59.4414409519271,-62.0897745954456,
-179.713616638591));
#233843=CARTESIAN_POINT('Ctrl Pts',(59.3624719505921,-62.1851765785503,
-179.662506000476));
#233844=CARTESIAN_POINT('Ctrl Pts',(59.3194982880101,-62.2369634695716,
-179.64995));
#233845=CARTESIAN_POINT('Ctrl Pts',(59.2791589653485,-62.2854505031402,
-179.64995));
#233846=CARTESIAN_POINT('',(59.5991207857295,-61.8983055423346,-180.14995));
#233847=CARTESIAN_POINT('',(52.6545705595274,-55.6608620973191,-179.64995));
#233848=CARTESIAN_POINT('Origin',(61.6666822880186,-37.78000002,-189.64995));
#233849=CARTESIAN_POINT('',(62.1666822880186,-37.78000002,-182.64995));
#233850=CARTESIAN_POINT('',(61.6666822880186,-38.28000002,-182.64995));
#233851=CARTESIAN_POINT('Origin',(61.6666822880186,-37.78000002,-182.64995));
#233852=CARTESIAN_POINT('',(61.6666822880186,-38.28000002,-189.64995));
#233853=CARTESIAN_POINT('',(61.6666822880186,-38.28000002,-236.10005));
#233854=CARTESIAN_POINT('',(62.1666822880186,-37.78000002,-189.64995));
#233855=CARTESIAN_POINT('Origin',(61.6666822880186,-37.78000002,-189.64995));
#233856=CARTESIAN_POINT('',(62.1666822880186,-37.78000002,-189.64995));
#233857=CARTESIAN_POINT('Origin',(59.1666822880186,-37.78000002,-182.64995));
#233858=CARTESIAN_POINT('',(59.1666822880186,-37.78000002,-179.64995));
#233859=CARTESIAN_POINT('',(59.1666822880186,-38.28000002,-180.14995));
#233860=CARTESIAN_POINT('Origin',(59.1666822880186,-37.78000002,-180.14995));
#233861=CARTESIAN_POINT('Origin',(59.1666822880186,-38.28000002,-182.64995));
#233862=CARTESIAN_POINT('Origin',(59.1666822880186,-37.78000002,-182.64995));
#233863=CARTESIAN_POINT('Origin',(52.7401871797155,-37.78000002,-180.14995));
#233864=CARTESIAN_POINT('',(53.1262583325313,-37.78000002,-179.64995));
#233865=CARTESIAN_POINT('',(53.1262583325313,-38.28000002,-180.14995));
#233866=CARTESIAN_POINT('Origin',(53.1262583325313,-37.78000002,-180.14995));
#233867=CARTESIAN_POINT('',(53.1262583325313,-38.28000002,-180.14995));
#233868=CARTESIAN_POINT('',(59.1666822880186,-37.78000002,-179.64995));
#233869=CARTESIAN_POINT('Origin',(53.1262583325313,-38.78000002,-180.14995));
#233870=CARTESIAN_POINT('',(52.1640112991968,-38.5078224183517,-179.64995));
#233871=CARTESIAN_POINT('',(52.6451348158641,-38.6439112191758,-180.14995));
#233872=CARTESIAN_POINT('Origin',(52.1640112991968,-38.5078224183517,-180.14995));
#233873=CARTESIAN_POINT('Origin',(53.1262583325313,-38.78000002,-180.14995));
#233874=CARTESIAN_POINT('Origin',(53.1262583325313,-38.78000002,-179.64995));
#233875=CARTESIAN_POINT('Origin',(57.4563699825363,-40.0047992274175,-180.14995));
#233876=CARTESIAN_POINT('',(52.0098956044577,-39.2393471721372,-179.64995));
#233877=CARTESIAN_POINT('',(52.5050296388285,-39.3089337226171,-180.14995));
#233878=CARTESIAN_POINT('Origin',(52.0098956044577,-39.2393471721372,-180.14995));
#233879=CARTESIAN_POINT('Origin',(57.4563699825363,-40.0047992274175,-180.14995));
#233880=CARTESIAN_POINT('Origin',(57.4563699825363,-40.0047992274175,-179.64995));
#233881=CARTESIAN_POINT('Origin',(52.1173462765794,-38.4747959130728,-180.14995));
#233882=CARTESIAN_POINT('',(51.2999564243458,-44.2908269190399,-179.64995));
#233883=CARTESIAN_POINT('',(51.7950904587165,-44.36041346952,-180.14995));
#233884=CARTESIAN_POINT('Origin',(51.2999564243458,-44.2908269190399,-180.14995));
#233885=CARTESIAN_POINT('',(52.6124803109501,-38.5443824635529,-180.14995));
#233886=CARTESIAN_POINT('',(50.0744984522816,-53.0104134695199,-179.64995));
#233887=CARTESIAN_POINT('Origin',(52.2902244930873,-44.43000002,-180.14995));
#233888=CARTESIAN_POINT('',(52.2902244930873,-45.43000002,-179.64995));
#233889=CARTESIAN_POINT('',(52.2902244930873,-44.93000002,-180.14995));
#233890=CARTESIAN_POINT('Origin',(52.2902244930873,-45.43000002,-180.14995));
#233891=CARTESIAN_POINT('Origin',(52.2902244930873,-44.43000002,-180.14995));
#233892=CARTESIAN_POINT('Origin',(52.2902244930873,-44.43000002,-179.64995));
#233893=CARTESIAN_POINT('Origin',(51.7150402894768,-45.43000002,-180.14995));
#233894=CARTESIAN_POINT('',(59.1666822880186,-45.43000002,-179.64995));
#233895=CARTESIAN_POINT('',(59.1666822880186,-44.93000002,-180.14995));
#233896=CARTESIAN_POINT('Origin',(59.1666822880186,-45.43000002,-180.14995));
#233897=CARTESIAN_POINT('',(59.1666822880186,-44.93000002,-180.14995));
#233898=CARTESIAN_POINT('',(52.2902244930873,-45.43000002,-179.64995));
#233899=CARTESIAN_POINT('Origin',(59.1666822880186,-45.43000002,-182.64995));
#233900=CARTESIAN_POINT('',(62.1666822880186,-45.43000002,-182.64995));
#233901=CARTESIAN_POINT('',(61.6666822880186,-44.93000002,-182.64995));
#233902=CARTESIAN_POINT('Origin',(61.6666822880186,-45.43000002,-182.64995));
#233903=CARTESIAN_POINT('Origin',(59.1666822880186,-44.93000002,-182.64995));
#233904=CARTESIAN_POINT('Origin',(59.1666822880186,-45.43000002,-182.64995));
#233905=CARTESIAN_POINT('Origin',(61.6666822880186,-45.43000002,-189.64995));
#233906=CARTESIAN_POINT('',(61.6666822880186,-44.93000002,-189.64995));
#233907=CARTESIAN_POINT('',(62.1666822880186,-45.43000002,-189.64995));
#233908=CARTESIAN_POINT('Origin',(61.6666822880186,-45.43000002,-189.64995));
#233909=CARTESIAN_POINT('',(61.6666822880186,-44.93000002,-236.10005));
#233910=CARTESIAN_POINT('',(62.1666822880186,-45.43000002,-189.64995));
#233911=CARTESIAN_POINT('Origin',(61.6666822880186,-29.63000002,-189.64995));
#233912=CARTESIAN_POINT('',(62.1666822880186,-29.63000002,-182.64995));
#233913=CARTESIAN_POINT('',(61.6666822880186,-30.13000002,-182.64995));
#233914=CARTESIAN_POINT('Origin',(61.6666822880186,-29.63000002,-182.64995));
#233915=CARTESIAN_POINT('',(61.6666822880186,-30.13000002,-189.64995));
#233916=CARTESIAN_POINT('',(61.6666822880186,-30.13000002,-236.10005));
#233917=CARTESIAN_POINT('',(62.1666822880186,-29.63000002,-189.64995));
#233918=CARTESIAN_POINT('Origin',(61.6666822880186,-29.63000002,-189.64995));
#233919=CARTESIAN_POINT('',(62.1666822880186,-29.63000002,-189.64995));
#233920=CARTESIAN_POINT('Origin',(59.1666822880186,-29.63000002,-182.64995));
#233921=CARTESIAN_POINT('',(59.1666822880186,-29.63000002,-179.64995));
#233922=CARTESIAN_POINT('',(59.1666822880186,-30.13000002,-180.14995));
#233923=CARTESIAN_POINT('Origin',(59.1666822880186,-29.63000002,-180.14995));
#233924=CARTESIAN_POINT('Origin',(59.1666822880186,-30.13000002,-182.64995));
#233925=CARTESIAN_POINT('Origin',(59.1666822880186,-29.63000002,-182.64995));
#233926=CARTESIAN_POINT('Origin',(55.9258311851596,-29.63000002,-180.14995));
#233927=CARTESIAN_POINT('',(56.294192362543,-29.63000002,-179.64995));
#233928=CARTESIAN_POINT('',(56.294192362543,-30.13000002,-180.14995));
#233929=CARTESIAN_POINT('Origin',(56.294192362543,-29.63000002,-180.14995));
#233930=CARTESIAN_POINT('',(56.294192362543,-30.13000002,-180.14995));
#233931=CARTESIAN_POINT('',(59.1666822880186,-29.63000002,-179.64995));
#233932=CARTESIAN_POINT('Origin',(56.294192362543,-30.63000002,-180.14995));
#233933=CARTESIAN_POINT('',(55.3400535089406,-30.3306356132208,-179.64995));
#233934=CARTESIAN_POINT('',(55.8171229357418,-30.4803178166104,-180.14995));
#233935=CARTESIAN_POINT('Origin',(55.3400535089406,-30.3306356132208,-180.14995));
#233936=CARTESIAN_POINT('Origin',(56.294192362543,-30.63000002,-180.14995));
#233937=CARTESIAN_POINT('Origin',(56.294192362543,-30.63000002,-179.64995));
#233938=CARTESIAN_POINT('Origin',(0.,-12.9675000200281,-180.14995));
#233939=CARTESIAN_POINT('',(53.2803342727705,-35.8848729013564,-179.64995));
#233940=CARTESIAN_POINT('',(53.7396474992599,-36.0824364606782,-180.14995));
#233941=CARTESIAN_POINT('Origin',(53.2803342727705,-35.8848729013564,-180.14995));
#233942=CARTESIAN_POINT('Origin',(0.,-12.9675000200281,-180.14995));
#233943=CARTESIAN_POINT('Origin',(0.,-12.9675000200281,-179.64995));
#233944=CARTESIAN_POINT('Origin',(54.1989607257493,-36.28000002,-180.14995));
#233945=CARTESIAN_POINT('',(54.1989607257493,-37.28000002,-179.64995));
#233946=CARTESIAN_POINT('',(54.1989607257493,-36.78000002,-180.14995));
#233947=CARTESIAN_POINT('Origin',(54.1989607257493,-37.28000002,-180.14995));
#233948=CARTESIAN_POINT('Origin',(54.1989607257493,-36.28000002,-180.14995));
#233949=CARTESIAN_POINT('Origin',(54.1989607257493,-36.28000002,-179.64995));
#233950=CARTESIAN_POINT('Origin',(53.4342104250764,-37.28000002,-180.14995));
#233951=CARTESIAN_POINT('',(59.1666822880186,-37.28000002,-179.64995));
#233952=CARTESIAN_POINT('',(59.1666822880186,-36.78000002,-180.14995));
#233953=CARTESIAN_POINT('Origin',(59.1666822880186,-37.28000002,-180.14995));
#233954=CARTESIAN_POINT('',(59.1666822880186,-36.78000002,-180.14995));
#233955=CARTESIAN_POINT('',(54.1989607257493,-37.28000002,-179.64995));
#233956=CARTESIAN_POINT('Origin',(59.1666822880186,-37.28000002,-182.64995));
#233957=CARTESIAN_POINT('',(62.1666822880186,-37.28000002,-182.64995));
#233958=CARTESIAN_POINT('',(61.6666822880186,-36.78000002,-182.64995));
#233959=CARTESIAN_POINT('Origin',(61.6666822880186,-37.28000002,-182.64995));
#233960=CARTESIAN_POINT('Origin',(59.1666822880186,-36.78000002,-182.64995));
#233961=CARTESIAN_POINT('Origin',(59.1666822880186,-37.28000002,-182.64995));
#233962=CARTESIAN_POINT('Origin',(61.6666822880186,-37.28000002,-189.64995));
#233963=CARTESIAN_POINT('',(61.6666822880186,-36.78000002,-189.64995));
#233964=CARTESIAN_POINT('',(62.1666822880186,-37.28000002,-189.64995));
#233965=CARTESIAN_POINT('Origin',(61.6666822880186,-37.28000002,-189.64995));
#233966=CARTESIAN_POINT('',(61.6666822880186,-36.78000002,-236.10005));
#233967=CARTESIAN_POINT('',(62.1666822880186,-37.28000002,-189.64995));
#233968=CARTESIAN_POINT('Origin',(61.6666822880186,-21.48000002,-189.64995));
#233969=CARTESIAN_POINT('',(62.1666822880186,-21.48000002,-182.64995));
#233970=CARTESIAN_POINT('',(61.6666822880186,-21.98000002,-182.64995));
#233971=CARTESIAN_POINT('Origin',(61.6666822880186,-21.48000002,-182.64995));
#233972=CARTESIAN_POINT('',(61.6666822880186,-21.98000002,-189.64995));
#233973=CARTESIAN_POINT('',(61.6666822880186,-21.98000002,-236.10005));
#233974=CARTESIAN_POINT('',(62.1666822880186,-21.48000002,-189.64995));
#233975=CARTESIAN_POINT('Origin',(61.6666822880186,-21.48000002,-189.64995));
#233976=CARTESIAN_POINT('',(62.1666822880186,-21.48000002,-189.64995));
#233977=CARTESIAN_POINT('Origin',(59.1666822880186,-21.48000002,-182.64995));
#233978=CARTESIAN_POINT('',(59.1666822880186,-21.48000002,-179.64995));
#233979=CARTESIAN_POINT('',(59.1666822880186,-21.98000002,-180.14995));
#233980=CARTESIAN_POINT('Origin',(59.1666822880186,-21.48000002,-180.14995));
#233981=CARTESIAN_POINT('Origin',(59.1666822880186,-21.98000002,-182.64995));
#233982=CARTESIAN_POINT('Origin',(59.1666822880186,-21.48000002,-182.64995));
#233983=CARTESIAN_POINT('Origin',(57.8015989722647,-21.48000002,-180.14995));
#233984=CARTESIAN_POINT('',(58.2281061322669,-21.48000002,-179.64995));
#233985=CARTESIAN_POINT('',(58.2281061322669,-21.98000002,-180.14995));
#233986=CARTESIAN_POINT('Origin',(58.2281061322669,-21.48000002,-180.14995));
#233987=CARTESIAN_POINT('',(58.2281061322669,-21.98000002,-180.14995));
#233988=CARTESIAN_POINT('',(59.1666822880186,-21.48000002,-179.64995));
#233989=CARTESIAN_POINT('Origin',(58.2281061322669,-22.48000002,-180.14995));
#233990=CARTESIAN_POINT('',(57.2411890791776,-22.3187712064411,-179.64995));
#233991=CARTESIAN_POINT('',(57.7346476057223,-22.3993856132206,-180.14995));
#233992=CARTESIAN_POINT('Origin',(57.2411890791776,-22.3187712064411,-180.14995));
#233993=CARTESIAN_POINT('Origin',(58.2281061322669,-22.48000002,-180.14995));
#233994=CARTESIAN_POINT('Origin',(58.2281061322669,-22.48000002,-179.64995));
#233995=CARTESIAN_POINT('Origin',(0.,-12.9675000200281,-180.14995));
#233996=CARTESIAN_POINT('',(56.051992088731,-27.8730084945768,-179.64995));
#233997=CARTESIAN_POINT('',(56.5351989170821,-28.0015042572884,-180.14995));
#233998=CARTESIAN_POINT('Origin',(56.051992088731,-27.8730084945768,-180.14995));
#233999=CARTESIAN_POINT('Origin',(0.,-12.9675000200281,-180.14995));
#234000=CARTESIAN_POINT('Origin',(0.,-12.9675000200281,-179.64995));
#234001=CARTESIAN_POINT('Origin',(57.0184057454332,-28.13000002,-180.14995));
#234002=CARTESIAN_POINT('',(57.0184057454332,-29.13000002,-179.64995));
#234003=CARTESIAN_POINT('',(57.0184057454332,-28.63000002,-180.14995));
#234004=CARTESIAN_POINT('Origin',(57.0184057454332,-29.13000002,-180.14995));
#234005=CARTESIAN_POINT('Origin',(57.0184057454332,-28.13000002,-180.14995));
#234006=CARTESIAN_POINT('Origin',(57.0184057454332,-28.13000002,-179.64995));
#234007=CARTESIAN_POINT('Origin',(56.3643157835779,-29.13000002,-180.14995));
#234008=CARTESIAN_POINT('',(59.1666822880186,-29.13000002,-179.64995));
#234009=CARTESIAN_POINT('',(59.1666822880186,-28.63000002,-180.14995));
#234010=CARTESIAN_POINT('Origin',(59.1666822880186,-29.13000002,-180.14995));
#234011=CARTESIAN_POINT('',(59.1666822880186,-28.63000002,-180.14995));
#234012=CARTESIAN_POINT('',(57.0184057454332,-29.13000002,-179.64995));
#234013=CARTESIAN_POINT('Origin',(59.1666822880186,-29.13000002,-182.64995));
#234014=CARTESIAN_POINT('',(62.1666822880186,-29.13000002,-182.64995));
#234015=CARTESIAN_POINT('',(61.6666822880186,-28.63000002,-182.64995));
#234016=CARTESIAN_POINT('Origin',(61.6666822880186,-29.13000002,-182.64995));
#234017=CARTESIAN_POINT('Origin',(59.1666822880186,-28.63000002,-182.64995));
#234018=CARTESIAN_POINT('Origin',(59.1666822880186,-29.13000002,-182.64995));
#234019=CARTESIAN_POINT('Origin',(61.6666822880186,-29.13000002,-189.64995));
#234020=CARTESIAN_POINT('',(61.6666822880186,-28.63000002,-189.64995));
#234021=CARTESIAN_POINT('',(62.1666822880186,-29.13000002,-189.64995));
#234022=CARTESIAN_POINT('Origin',(61.6666822880186,-29.13000002,-189.64995));
#234023=CARTESIAN_POINT('',(61.6666822880186,-28.63000002,-236.10005));
#234024=CARTESIAN_POINT('',(62.1666822880186,-29.13000002,-189.64995));
#234025=CARTESIAN_POINT('Origin',(61.6666822880186,-13.33000002,-189.64995));
#234026=CARTESIAN_POINT('',(62.1666822880186,-13.33000002,-182.64995));
#234027=CARTESIAN_POINT('',(61.6666822880186,-13.83000002,-182.64995));
#234028=CARTESIAN_POINT('Origin',(61.6666822880186,-13.33000002,-182.64995));
#234029=CARTESIAN_POINT('',(61.6666822880186,-13.83000002,-189.64995));
#234030=CARTESIAN_POINT('',(61.6666822880186,-13.83000002,-236.10005));
#234031=CARTESIAN_POINT('',(62.1666822880186,-13.33000002,-189.64995));
#234032=CARTESIAN_POINT('Origin',(61.6666822880186,-13.33000002,-189.64995));
#234033=CARTESIAN_POINT('',(62.1666822880186,-13.33000002,-189.64995));
#234034=CARTESIAN_POINT('Origin',(59.1666822880186,-13.33000002,-182.64995));
#234035=CARTESIAN_POINT('',(59.1666822880186,-13.33000002,-179.64995));
#234036=CARTESIAN_POINT('',(59.1666822880186,-13.83000002,-180.14995));
#234037=CARTESIAN_POINT('Origin',(59.1666822880186,-13.33000002,-180.14995));
#234038=CARTESIAN_POINT('Origin',(59.1666822880186,-13.83000002,-182.64995));
#234039=CARTESIAN_POINT('Origin',(59.1666822880186,-13.33000002,-182.64995));
#234040=CARTESIAN_POINT('Origin',(58.4936414813615,-13.33000002,-180.14995));
#234041=CARTESIAN_POINT('',(58.9842656455946,-13.33000002,-179.64995));
#234042=CARTESIAN_POINT('',(58.9842656455946,-13.83000002,-180.14995));
#234043=CARTESIAN_POINT('Origin',(58.9842656455946,-13.33000002,-180.14995));
#234044=CARTESIAN_POINT('',(58.9842656455946,-13.83000002,-180.14995));
#234045=CARTESIAN_POINT('',(59.1666822880186,-13.33000002,-179.64995));
#234046=CARTESIAN_POINT('Origin',(58.9842656455946,-14.33000002,-180.14995));
#234047=CARTESIAN_POINT('',(57.9845323295676,-14.3069067996615,-179.64995));
#234048=CARTESIAN_POINT('',(58.4843989875811,-14.3184534098307,-180.14995));
#234049=CARTESIAN_POINT('Origin',(57.9845323295676,-14.3069067996615,-180.14995));
#234050=CARTESIAN_POINT('Origin',(58.9842656455946,-14.33000002,-180.14995));
#234051=CARTESIAN_POINT('Origin',(58.9842656455946,-14.33000002,-179.64995));
#234052=CARTESIAN_POINT('Origin',(0.,-12.9675000200281,-180.14995));
#234053=CARTESIAN_POINT('',(57.588867600144,-19.8611440877971,-179.64995));
#234054=CARTESIAN_POINT('',(58.0853233553177,-19.9205720538985,-180.14995));
#234055=CARTESIAN_POINT('Origin',(57.588867600144,-19.8611440877971,-180.14995));
#234056=CARTESIAN_POINT('Origin',(0.,-12.9675000200281,-180.14995));
#234057=CARTESIAN_POINT('Origin',(0.,-12.9675000200281,-179.64995));
#234058=CARTESIAN_POINT('Origin',(58.5817791104913,-19.98000002,-180.14995));
#234059=CARTESIAN_POINT('',(58.5817791104913,-20.98000002,-179.64995));
#234060=CARTESIAN_POINT('',(58.5817791104913,-20.48000002,-180.14995));
#234061=CARTESIAN_POINT('Origin',(58.5817791104913,-20.98000002,-180.14995));
#234062=CARTESIAN_POINT('Origin',(58.5817791104913,-19.98000002,-180.14995));
#234063=CARTESIAN_POINT('Origin',(58.5817791104913,-19.98000002,-179.64995));
#234064=CARTESIAN_POINT('Origin',(58.0156215492899,-20.98000002,-180.14995));
#234065=CARTESIAN_POINT('',(59.1666822880186,-20.98000002,-179.64995));
#234066=CARTESIAN_POINT('',(59.1666822880186,-20.48000002,-180.14995));
#234067=CARTESIAN_POINT('Origin',(59.1666822880186,-20.98000002,-180.14995));
#234068=CARTESIAN_POINT('',(59.1666822880186,-20.48000002,-180.14995));
#234069=CARTESIAN_POINT('',(58.5817791104913,-20.98000002,-179.64995));
#234070=CARTESIAN_POINT('Origin',(59.1666822880186,-20.98000002,-182.64995));
#234071=CARTESIAN_POINT('',(62.1666822880186,-20.98000002,-182.64995));
#234072=CARTESIAN_POINT('',(61.6666822880186,-20.48000002,-182.64995));
#234073=CARTESIAN_POINT('Origin',(61.6666822880186,-20.98000002,-182.64995));
#234074=CARTESIAN_POINT('Origin',(59.1666822880186,-20.48000002,-182.64995));
#234075=CARTESIAN_POINT('Origin',(59.1666822880186,-20.98000002,-182.64995));
#234076=CARTESIAN_POINT('Origin',(61.6666822880186,-20.98000002,-189.64995));
#234077=CARTESIAN_POINT('',(61.6666822880186,-20.48000002,-189.64995));
#234078=CARTESIAN_POINT('',(62.1666822880186,-20.98000002,-189.64995));
#234079=CARTESIAN_POINT('Origin',(61.6666822880186,-20.98000002,-189.64995));
#234080=CARTESIAN_POINT('',(61.6666822880186,-20.48000002,-236.10005));
#234081=CARTESIAN_POINT('',(62.1666822880186,-20.98000002,-189.64995));
#234082=CARTESIAN_POINT('Origin',(61.6666822880186,-5.18000001999998,-189.64995));
#234083=CARTESIAN_POINT('',(62.1666822880186,-5.18000001999998,-182.64995));
#234084=CARTESIAN_POINT('',(61.6666822880186,-5.68000001999998,-182.64995));
#234085=CARTESIAN_POINT('Origin',(61.6666822880186,-5.18000001999998,-182.64995));
#234086=CARTESIAN_POINT('',(61.6666822880186,-5.68000001999998,-189.64995));
#234087=CARTESIAN_POINT('',(61.6666822880186,-5.68000001999998,-236.10005));
#234088=CARTESIAN_POINT('',(62.1666822880186,-5.18000001999998,-189.64995));
#234089=CARTESIAN_POINT('Origin',(61.6666822880186,-5.18000001999998,-189.64995));
#234090=CARTESIAN_POINT('',(62.1666822880186,-5.18000001999998,-189.64995));
#234091=CARTESIAN_POINT('Origin',(59.1666822880186,-5.18000001999998,-182.64995));
#234092=CARTESIAN_POINT('',(59.1666822880186,-5.18000001999998,-179.64995));
#234093=CARTESIAN_POINT('',(59.1666822880186,-5.68000001999998,-180.14995));
#234094=CARTESIAN_POINT('Origin',(59.1666822880186,-5.18000001999998,-180.14995));
#234095=CARTESIAN_POINT('Origin',(59.1666822880186,-5.68000001999998,-182.64995));
#234096=CARTESIAN_POINT('Origin',(59.1666822880186,-5.18000001999998,-182.64995));
#234097=CARTESIAN_POINT('Origin',(58.0443136211429,-5.18000001999998,-180.14995));
#234098=CARTESIAN_POINT('',(58.6082745331205,-5.18000001999998,-179.64995));
#234099=CARTESIAN_POINT('',(58.6082745331205,-5.68000001999998,-180.14995));
#234100=CARTESIAN_POINT('Origin',(58.6082745331205,-5.18000001999998,-180.14995));
#234101=CARTESIAN_POINT('',(58.6082745331205,-5.68000001999998,-180.14995));
#234102=CARTESIAN_POINT('',(59.1666822880186,-5.18000001999998,-179.64995));
#234103=CARTESIAN_POINT('Origin',(58.6082745331205,-6.18000001999998,-180.14995));
#234104=CARTESIAN_POINT('',(57.6149139478134,-6.29504239288181,-179.64995));
#234105=CARTESIAN_POINT('',(58.1115942404669,-6.2375212064409,-180.14995));
#234106=CARTESIAN_POINT('Origin',(57.6149139478134,-6.29504239288181,-180.14995));
#234107=CARTESIAN_POINT('Origin',(58.6082745331205,-6.18000001999998,-180.14995));
#234108=CARTESIAN_POINT('Origin',(58.6082745331205,-6.18000001999998,-179.64995));
#234109=CARTESIAN_POINT('Origin',(0.,-12.9675000200281,-180.14995));
#234110=CARTESIAN_POINT('',(57.9892195435792,-11.8492796810174,-179.64995));
#234111=CARTESIAN_POINT('',(58.48912660861,-11.8396398505087,-180.14995));
#234112=CARTESIAN_POINT('Origin',(57.9892195435792,-11.8492796810174,-180.14995));
#234113=CARTESIAN_POINT('Origin',(0.,-12.9675000200281,-180.14995));
#234114=CARTESIAN_POINT('Origin',(0.,-12.9675000200281,-179.64995));
#234115=CARTESIAN_POINT('Origin',(58.9890336736409,-11.83000002,-180.14995));
#234116=CARTESIAN_POINT('',(58.9890336736409,-12.83000002,-179.64995));
#234117=CARTESIAN_POINT('',(58.9890336736409,-12.33000002,-180.14995));
#234118=CARTESIAN_POINT('Origin',(58.9890336736409,-12.83000002,-180.14995));
#234119=CARTESIAN_POINT('Origin',(58.9890336736409,-11.83000002,-180.14995));
#234120=CARTESIAN_POINT('Origin',(58.9890336736409,-11.83000002,-179.64995));
#234121=CARTESIAN_POINT('Origin',(58.4965263391765,-12.83000002,-180.14995));
#234122=CARTESIAN_POINT('',(59.1666822880186,-12.83000002,-179.64995));
#234123=CARTESIAN_POINT('',(59.1666822880186,-12.33000002,-180.14995));
#234124=CARTESIAN_POINT('Origin',(59.1666822880186,-12.83000002,-180.14995));
#234125=CARTESIAN_POINT('',(59.1666822880186,-12.33000002,-180.14995));
#234126=CARTESIAN_POINT('',(58.9890336736409,-12.83000002,-179.64995));
#234127=CARTESIAN_POINT('Origin',(59.1666822880186,-12.83000002,-182.64995));
#234128=CARTESIAN_POINT('',(62.1666822880186,-12.83000002,-182.64995));
#234129=CARTESIAN_POINT('',(61.6666822880186,-12.33000002,-182.64995));
#234130=CARTESIAN_POINT('Origin',(61.6666822880186,-12.83000002,-182.64995));
#234131=CARTESIAN_POINT('Origin',(59.1666822880186,-12.33000002,-182.64995));
#234132=CARTESIAN_POINT('Origin',(59.1666822880186,-12.83000002,-182.64995));
#234133=CARTESIAN_POINT('Origin',(61.6666822880186,-12.83000002,-189.64995));
#234134=CARTESIAN_POINT('',(61.6666822880186,-12.33000002,-189.64995));
#234135=CARTESIAN_POINT('',(62.1666822880186,-12.83000002,-189.64995));
#234136=CARTESIAN_POINT('Origin',(61.6666822880186,-12.83000002,-189.64995));
#234137=CARTESIAN_POINT('',(61.6666822880186,-12.33000002,-236.10005));
#234138=CARTESIAN_POINT('',(62.1666822880186,-12.83000002,-189.64995));
#234139=CARTESIAN_POINT('Origin',(61.6666822880186,2.96999998000002,-189.64995));
#234140=CARTESIAN_POINT('',(62.1666822880186,2.96999998000002,-182.64995));
#234141=CARTESIAN_POINT('',(61.6666822880186,2.46999998000002,-182.64995));
#234142=CARTESIAN_POINT('Origin',(61.6666822880186,2.96999998000002,-182.64995));
#234143=CARTESIAN_POINT('',(61.6666822880186,2.46999998000002,-189.64995));
#234144=CARTESIAN_POINT('',(61.6666822880186,2.46999998000002,-236.10005));
#234145=CARTESIAN_POINT('',(62.1666822880186,2.96999998000002,-189.64995));
#234146=CARTESIAN_POINT('Origin',(61.6666822880186,2.96999998000002,-189.64995));
#234147=CARTESIAN_POINT('',(62.1666822880186,2.96999998000002,-189.64995));
#234148=CARTESIAN_POINT('Origin',(59.1666822880186,2.96999998000002,-182.64995));
#234149=CARTESIAN_POINT('',(59.1666822880186,2.96999998000002,-179.64995));
#234150=CARTESIAN_POINT('',(59.1666822880186,2.46999998000002,-180.14995));
#234151=CARTESIAN_POINT('Origin',(59.1666822880186,2.96999998000002,-180.14995));
#234152=CARTESIAN_POINT('Origin',(59.1666822880186,2.46999998000002,-182.64995));
#234153=CARTESIAN_POINT('Origin',(59.1666822880186,2.96999998000002,-182.64995));
#234154=CARTESIAN_POINT('Origin',(56.4263554888062,2.96999998000002,-180.14995));
#234155=CARTESIAN_POINT('',(57.077763566464,2.96999998000002,-179.64995));
#234156=CARTESIAN_POINT('',(57.077763566464,2.46999998000002,-180.14995));
#234157=CARTESIAN_POINT('Origin',(57.077763566464,2.96999998000002,-180.14995));
#234158=CARTESIAN_POINT('',(57.077763566464,2.46999998000002,-180.14995));
#234159=CARTESIAN_POINT('',(59.1666822880186,2.96999998000002,-179.64995));
#234160=CARTESIAN_POINT('Origin',(57.077763566464,1.96999998000002,-180.14995));
#234161=CARTESIAN_POINT('',(56.1103438449985,1.71682201389785,-179.64995));
#234162=CARTESIAN_POINT('',(56.5940537057312,1.84341099694893,-180.14995));
#234163=CARTESIAN_POINT('Origin',(56.1103438449985,1.71682201389785,-180.14995));
#234164=CARTESIAN_POINT('Origin',(57.077763566464,1.96999998000002,-180.14995));
#234165=CARTESIAN_POINT('Origin',(57.077763566464,1.96999998000002,-179.64995));
#234166=CARTESIAN_POINT('Origin',(0.,-12.9675000200281,-180.14995));
#234167=CARTESIAN_POINT('',(57.276884975832,-3.83741527423775,-179.64995));
#234168=CARTESIAN_POINT('',(57.7706512256236,-3.75870764711887,-180.14995));
#234169=CARTESIAN_POINT('Origin',(57.276884975832,-3.83741527423775,-180.14995));
#234170=CARTESIAN_POINT('Origin',(0.,-12.9675000200281,-180.14995));
#234171=CARTESIAN_POINT('Origin',(0.,-12.9675000200281,-179.64995));
#234172=CARTESIAN_POINT('Origin',(58.2644174754153,-3.68000001999999,-180.14995));
#234173=CARTESIAN_POINT('',(58.2644174754153,-4.68000001999999,-179.64995));
#234174=CARTESIAN_POINT('',(58.2644174754153,-4.18000001999998,-180.14995));
#234175=CARTESIAN_POINT('Origin',(58.2644174754153,-4.68000001999999,-180.14995));
#234176=CARTESIAN_POINT('Origin',(58.2644174754153,-3.68000001999999,-180.14995));
#234177=CARTESIAN_POINT('Origin',(58.2644174754153,-3.68000001999999,-179.64995));
#234178=CARTESIAN_POINT('Origin',(57.8362329664502,-4.68000001999999,-180.14995));
#234179=CARTESIAN_POINT('',(59.1666822880186,-4.68000001999999,-179.64995));
#234180=CARTESIAN_POINT('',(59.1666822880186,-4.18000001999998,-180.14995));
#234181=CARTESIAN_POINT('Origin',(59.1666822880186,-4.68000001999999,-180.14995));
#234182=CARTESIAN_POINT('',(59.1666822880186,-4.18000001999998,-180.14995));
#234183=CARTESIAN_POINT('',(58.2644174754153,-4.68000001999999,-179.64995));
#234184=CARTESIAN_POINT('Origin',(59.1666822880186,-4.68000001999999,-182.64995));
#234185=CARTESIAN_POINT('',(62.1666822880186,-4.68000001999999,-182.64995));
#234186=CARTESIAN_POINT('',(61.6666822880186,-4.18000001999998,-182.64995));
#234187=CARTESIAN_POINT('Origin',(61.6666822880186,-4.68000001999999,-182.64995));
#234188=CARTESIAN_POINT('Origin',(59.1666822880186,-4.18000001999998,-182.64995));
#234189=CARTESIAN_POINT('Origin',(59.1666822880186,-4.68000001999999,-182.64995));
#234190=CARTESIAN_POINT('Origin',(61.6666822880186,-4.68000001999999,-189.64995));
#234191=CARTESIAN_POINT('',(61.6666822880186,-4.18000001999998,-189.64995));
#234192=CARTESIAN_POINT('',(62.1666822880186,-4.68000001999999,-189.64995));
#234193=CARTESIAN_POINT('Origin',(61.6666822880186,-4.68000001999999,-189.64995));
#234194=CARTESIAN_POINT('',(61.6666822880186,-4.18000001999998,-236.10005));
#234195=CARTESIAN_POINT('',(62.1666822880186,-4.68000001999999,-189.64995));
#234196=CARTESIAN_POINT('Origin',(61.6666822880186,11.11999998,-189.64995));
#234197=CARTESIAN_POINT('',(62.1666822880186,11.11999998,-182.64995));
#234198=CARTESIAN_POINT('',(61.6666822880186,10.61999998,-182.64995));
#234199=CARTESIAN_POINT('Origin',(61.6666822880186,11.11999998,-182.64995));
#234200=CARTESIAN_POINT('',(61.6666822880186,10.61999998,-189.64995));
#234201=CARTESIAN_POINT('',(61.6666822880186,10.61999998,-236.10005));
#234202=CARTESIAN_POINT('',(62.1666822880186,11.11999998,-189.64995));
#234203=CARTESIAN_POINT('Origin',(61.6666822880186,11.11999998,-189.64995));
#234204=CARTESIAN_POINT('',(62.1666822880186,11.11999998,-189.64995));
#234205=CARTESIAN_POINT('Origin',(59.1666822880186,11.11999998,-182.64995));
#234206=CARTESIAN_POINT('',(59.1666822880186,11.11999998,-179.64995));
#234207=CARTESIAN_POINT('',(59.1666822880186,10.61999998,-180.14995));
#234208=CARTESIAN_POINT('Origin',(59.1666822880186,11.11999998,-180.14995));
#234209=CARTESIAN_POINT('Origin',(59.1666822880186,10.61999998,-182.64995));
#234210=CARTESIAN_POINT('Origin',(59.1666822880186,11.11999998,-182.64995));
#234211=CARTESIAN_POINT('Origin',(53.533913024817,11.11999998,-180.14995));
#234212=CARTESIAN_POINT('',(54.2951871140408,11.11999998,-179.64995));
#234213=CARTESIAN_POINT('',(54.2951871140408,10.61999998,-180.14995));
#234214=CARTESIAN_POINT('Origin',(54.2951871140408,11.11999998,-180.14995));
#234215=CARTESIAN_POINT('',(54.2951871140408,10.61999998,-180.14995));
#234216=CARTESIAN_POINT('',(59.1666822880186,11.11999998,-179.64995));
#234217=CARTESIAN_POINT('Origin',(54.2951871140408,10.11999998,-180.14995));
#234218=CARTESIAN_POINT('',(53.3749297053282,9.72868642067751,-179.64995));
#234219=CARTESIAN_POINT('',(53.8350584096845,9.92434320033877,-180.14995));
#234220=CARTESIAN_POINT('Origin',(53.3749297053282,9.72868642067751,-180.14995));
#234221=CARTESIAN_POINT('Origin',(54.2951871140408,10.11999998,-180.14995));
#234222=CARTESIAN_POINT('Origin',(54.2951871140408,10.11999998,-179.64995));
#234223=CARTESIAN_POINT('Origin',(0.,-12.9675000200281,-180.14995));
#234224=CARTESIAN_POINT('',(55.4089665961269,4.1744491325419,-179.64995));
#234225=CARTESIAN_POINT('',(55.8866301012659,4.32222455627096,-180.14995));
#234226=CARTESIAN_POINT('Origin',(55.4089665961269,4.1744491325419,-180.14995));
#234227=CARTESIAN_POINT('Origin',(0.,-12.9675000200281,-180.14995));
#234228=CARTESIAN_POINT('Origin',(0.,-12.9675000200281,-179.64995));
#234229=CARTESIAN_POINT('Origin',(56.3642936064049,4.46999998000001,-180.14995));
#234230=CARTESIAN_POINT('',(56.3642936064049,3.46999998000002,-179.64995));
#234231=CARTESIAN_POINT('',(56.3642936064049,3.96999998000001,-180.14995));
#234232=CARTESIAN_POINT('Origin',(56.3642936064049,3.46999998000002,-180.14995));
#234233=CARTESIAN_POINT('Origin',(56.3642936064049,4.46999998000001,-180.14995));
#234234=CARTESIAN_POINT('Origin',(56.3642936064049,4.46999998000001,-179.64995));
#234235=CARTESIAN_POINT('Origin',(55.9943844840627,3.46999998000002,-180.14995));
#234236=CARTESIAN_POINT('',(59.1666822880186,3.46999998000002,-179.64995));
#234237=CARTESIAN_POINT('',(59.1666822880186,3.96999998000001,-180.14995));
#234238=CARTESIAN_POINT('Origin',(59.1666822880186,3.46999998000002,-180.14995));
#234239=CARTESIAN_POINT('',(59.1666822880186,3.96999998000001,-180.14995));
#234240=CARTESIAN_POINT('',(56.3642936064049,3.46999998000002,-179.64995));
#234241=CARTESIAN_POINT('Origin',(59.1666822880186,3.46999998000002,-182.64995));
#234242=CARTESIAN_POINT('',(62.1666822880186,3.46999998000002,-182.64995));
#234243=CARTESIAN_POINT('',(61.6666822880186,3.96999998000001,-182.64995));
#234244=CARTESIAN_POINT('Origin',(61.6666822880186,3.46999998000002,-182.64995));
#234245=CARTESIAN_POINT('Origin',(59.1666822880186,3.96999998000001,-182.64995));
#234246=CARTESIAN_POINT('Origin',(59.1666822880186,3.46999998000002,-182.64995));
#234247=CARTESIAN_POINT('Origin',(61.6666822880186,3.46999998000002,-189.64995));
#234248=CARTESIAN_POINT('',(61.6666822880186,3.96999998000001,-189.64995));
#234249=CARTESIAN_POINT('',(62.1666822880186,3.46999998000002,-189.64995));
#234250=CARTESIAN_POINT('Origin',(61.6666822880186,3.46999998000002,-189.64995));
#234251=CARTESIAN_POINT('',(61.6666822880186,3.96999998000001,-236.10005));
#234252=CARTESIAN_POINT('',(62.1666822880186,3.46999998000002,-189.64995));
#234253=CARTESIAN_POINT('Origin',(61.6666822880186,19.26999998,-189.64995));
#234254=CARTESIAN_POINT('',(62.1666822880186,19.26999998,-182.64995));
#234255=CARTESIAN_POINT('',(61.6666822880186,18.76999998,-182.64995));
#234256=CARTESIAN_POINT('Origin',(61.6666822880186,19.26999998,-182.64995));
#234257=CARTESIAN_POINT('',(61.6666822880186,18.76999998,-189.64995));
#234258=CARTESIAN_POINT('',(61.6666822880186,18.76999998,-236.10005));
#234259=CARTESIAN_POINT('',(62.1666822880186,19.26999998,-189.64995));
#234260=CARTESIAN_POINT('Origin',(61.6666822880186,19.26999998,-189.64995));
#234261=CARTESIAN_POINT('',(62.1666822880186,19.26999998,-189.64995));
#234262=CARTESIAN_POINT('Origin',(59.1666822880186,19.26999998,-182.64995));
#234263=CARTESIAN_POINT('',(59.1666822880186,19.26999998,-179.64995));
#234264=CARTESIAN_POINT('',(59.1666822880186,18.76999998,-180.14995));
#234265=CARTESIAN_POINT('Origin',(59.1666822880186,19.26999998,-180.14995));
#234266=CARTESIAN_POINT('Origin',(59.1666822880186,18.76999998,-182.64995));
#234267=CARTESIAN_POINT('Origin',(59.1666822880186,19.26999998,-182.64995));
#234268=CARTESIAN_POINT('Origin',(51.746661977277,19.26999998,-180.14995));
#234269=CARTESIAN_POINT('',(52.3218461808875,19.26999998,-179.64995));
#234270=CARTESIAN_POINT('',(52.3218461808875,18.76999998,-180.14995));
#234271=CARTESIAN_POINT('Origin',(52.3218461808875,19.26999998,-180.14995));
#234272=CARTESIAN_POINT('',(52.3218461808875,18.76999998,-180.14995));
#234273=CARTESIAN_POINT('',(59.1666822880186,19.26999998,-179.64995));
#234274=CARTESIAN_POINT('Origin',(52.3218461808875,18.26999998,-180.14995));
#234275=CARTESIAN_POINT('',(51.3315781121459,18.1308268790399,-179.64995));
#234276=CARTESIAN_POINT('',(51.8267121465167,18.20041342952,-180.14995));
#234277=CARTESIAN_POINT('Origin',(51.3315781121459,18.1308268790399,-180.14995));
#234278=CARTESIAN_POINT('Origin',(52.3218461808875,18.26999998,-180.14995));
#234279=CARTESIAN_POINT('Origin',(52.3218461808875,18.26999998,-179.64995));
#234280=CARTESIAN_POINT('Origin',(52.1173462765794,12.5397958730165,-180.14995));
#234281=CARTESIAN_POINT('',(52.0098956044578,13.3043471320808,-179.64995));
#234282=CARTESIAN_POINT('',(52.5050296388285,13.3739336825608,-180.14995));
#234283=CARTESIAN_POINT('Origin',(52.0098956044578,13.3043471320808,-180.14995));
#234284=CARTESIAN_POINT('',(52.6124803109502,12.6093824234965,-180.14995));
#234285=CARTESIAN_POINT('',(61.1310018874833,-51.5956963488069,-179.64995));
#234286=CARTESIAN_POINT('Origin',(57.4563699825364,14.0697991873612,-180.14995));
#234287=CARTESIAN_POINT('',(52.2496341347737,12.2978223783642,-179.64995));
#234288=CARTESIAN_POINT('',(52.7229737572976,12.4589111791821,-180.14995));
#234289=CARTESIAN_POINT('Origin',(52.2496341347737,12.2978223783642,-180.14995));
#234290=CARTESIAN_POINT('Origin',(57.4563699825364,14.0697991873612,-180.14995));
#234291=CARTESIAN_POINT('Origin',(57.4563699825364,14.0697991873612,-179.64995));
#234292=CARTESIAN_POINT('Origin',(53.1963133798215,12.61999998,-180.14995));
#234293=CARTESIAN_POINT('',(53.1963133798215,11.61999998,-179.64995));
#234294=CARTESIAN_POINT('',(53.1963133798215,12.11999998,-180.14995));
#234295=CARTESIAN_POINT('Origin',(53.1963133798215,11.61999998,-180.14995));
#234296=CARTESIAN_POINT('Origin',(53.1963133798215,12.61999998,-180.14995));
#234297=CARTESIAN_POINT('Origin',(53.1963133798215,12.61999998,-179.64995));
#234298=CARTESIAN_POINT('Origin',(52.8475859784398,11.61999998,-180.14995));
#234299=CARTESIAN_POINT('',(59.1666822880186,11.61999998,-179.64995));
#234300=CARTESIAN_POINT('',(59.1666822880186,12.11999998,-180.14995));
#234301=CARTESIAN_POINT('Origin',(59.1666822880186,11.61999998,-180.14995));
#234302=CARTESIAN_POINT('',(59.1666822880186,12.11999998,-180.14995));
#234303=CARTESIAN_POINT('',(53.1963133798215,11.61999998,-179.64995));
#234304=CARTESIAN_POINT('Origin',(59.1666822880186,11.61999998,-182.64995));
#234305=CARTESIAN_POINT('',(62.1666822880186,11.61999998,-182.64995));
#234306=CARTESIAN_POINT('',(61.6666822880186,12.11999998,-182.64995));
#234307=CARTESIAN_POINT('Origin',(61.6666822880186,11.61999998,-182.64995));
#234308=CARTESIAN_POINT('Origin',(59.1666822880186,12.11999998,-182.64995));
#234309=CARTESIAN_POINT('Origin',(59.1666822880186,11.61999998,-182.64995));
#234310=CARTESIAN_POINT('Origin',(61.6666822880186,11.61999998,-189.64995));
#234311=CARTESIAN_POINT('',(61.6666822880186,12.11999998,-189.64995));
#234312=CARTESIAN_POINT('',(62.1666822880186,11.61999998,-189.64995));
#234313=CARTESIAN_POINT('Origin',(61.6666822880186,11.61999998,-189.64995));
#234314=CARTESIAN_POINT('',(61.6666822880186,12.11999998,-236.10005));
#234315=CARTESIAN_POINT('',(62.1666822880186,11.61999998,-189.64995));
#234316=CARTESIAN_POINT('Origin',(61.6666822880186,27.41999998,-189.64995));
#234317=CARTESIAN_POINT('',(62.1666822880186,27.41999998,-182.64995));
#234318=CARTESIAN_POINT('',(61.6666822880186,26.91999998,-182.64995));
#234319=CARTESIAN_POINT('Origin',(61.6666822880186,27.41999998,-182.64995));
#234320=CARTESIAN_POINT('',(61.6666822880186,26.91999998,-189.64995));
#234321=CARTESIAN_POINT('',(61.6666822880186,26.91999998,-236.10005));
#234322=CARTESIAN_POINT('',(62.1666822880186,27.41999998,-189.64995));
#234323=CARTESIAN_POINT('Origin',(61.6666822880186,27.41999998,-189.64995));
#234324=CARTESIAN_POINT('',(62.1666822880186,27.41999998,-189.64995));
#234325=CARTESIAN_POINT('Origin',(59.1666822880186,27.41999998,-182.64995));
#234326=CARTESIAN_POINT('',(59.1666822880186,27.41999998,-179.64995));
#234327=CARTESIAN_POINT('',(59.1666822880186,26.91999998,-180.14995));
#234328=CARTESIAN_POINT('Origin',(59.1666822880186,27.41999998,-180.14995));
#234329=CARTESIAN_POINT('Origin',(59.1666822880186,26.91999998,-182.64995));
#234330=CARTESIAN_POINT('Origin',(59.1666822880186,27.41999998,-182.64995));
#234331=CARTESIAN_POINT('Origin',(50.6012541744525,27.41999998,-180.14995));
#234332=CARTESIAN_POINT('',(51.176438378063,27.41999998,-179.64995));
#234333=CARTESIAN_POINT('',(51.176438378063,26.91999998,-180.14995));
#234334=CARTESIAN_POINT('Origin',(51.176438378063,27.41999998,-180.14995));
#234335=CARTESIAN_POINT('',(51.176438378063,26.91999998,-180.14995));
#234336=CARTESIAN_POINT('',(59.1666822880186,27.41999998,-179.64995));
#234337=CARTESIAN_POINT('Origin',(51.176438378063,26.41999998,-180.14995));
#234338=CARTESIAN_POINT('',(50.1861703093214,26.28082687904,-179.64995));
#234339=CARTESIAN_POINT('',(50.6813043436922,26.35041342952,-180.14995));
#234340=CARTESIAN_POINT('Origin',(50.1861703093214,26.28082687904,-180.14995));
#234341=CARTESIAN_POINT('Origin',(51.176438378063,26.41999998,-180.14995));
#234342=CARTESIAN_POINT('Origin',(51.176438378063,26.41999998,-179.64995));
#234343=CARTESIAN_POINT('Origin',(52.1173462765794,12.5397958730165,-180.14995));
#234344=CARTESIAN_POINT('',(50.9802260253899,20.63082687904,-179.64995));
#234345=CARTESIAN_POINT('',(51.4753600597607,20.70041342952,-180.14995));
#234346=CARTESIAN_POINT('Origin',(50.9802260253899,20.63082687904,-180.14995));
#234347=CARTESIAN_POINT('',(52.6124803109502,12.6093824234965,-180.14995));
#234348=CARTESIAN_POINT('',(61.1310018874833,-51.5956963488069,-179.64995));
#234349=CARTESIAN_POINT('Origin',(51.9704940941315,20.76999998,-180.14995));
#234350=CARTESIAN_POINT('',(51.9704940941315,19.76999998,-179.64995));
#234351=CARTESIAN_POINT('',(51.9704940941315,20.26999998,-180.14995));
#234352=CARTESIAN_POINT('Origin',(51.9704940941315,19.76999998,-180.14995));
#234353=CARTESIAN_POINT('Origin',(51.9704940941315,20.76999998,-180.14995));
#234354=CARTESIAN_POINT('Origin',(51.9704940941315,20.76999998,-179.64995));
#234355=CARTESIAN_POINT('Origin',(51.5358507252234,19.76999998,-180.14995));
#234356=CARTESIAN_POINT('',(59.1666822880186,19.76999998,-179.64995));
#234357=CARTESIAN_POINT('',(59.1666822880186,20.26999998,-180.14995));
#234358=CARTESIAN_POINT('Origin',(59.1666822880186,19.76999998,-180.14995));
#234359=CARTESIAN_POINT('',(59.1666822880186,20.26999998,-180.14995));
#234360=CARTESIAN_POINT('',(51.9704940941315,19.76999998,-179.64995));
#234361=CARTESIAN_POINT('Origin',(59.1666822880186,19.76999998,-182.64995));
#234362=CARTESIAN_POINT('',(62.1666822880186,19.76999998,-182.64995));
#234363=CARTESIAN_POINT('',(61.6666822880186,20.26999998,-182.64995));
#234364=CARTESIAN_POINT('Origin',(61.6666822880186,19.76999998,-182.64995));
#234365=CARTESIAN_POINT('Origin',(59.1666822880186,20.26999998,-182.64995));
#234366=CARTESIAN_POINT('Origin',(59.1666822880186,19.76999998,-182.64995));
#234367=CARTESIAN_POINT('Origin',(61.6666822880186,19.76999998,-189.64995));
#234368=CARTESIAN_POINT('',(61.6666822880186,20.26999998,-189.64995));
#234369=CARTESIAN_POINT('',(62.1666822880186,19.76999998,-189.64995));
#234370=CARTESIAN_POINT('Origin',(61.6666822880186,19.76999998,-189.64995));
#234371=CARTESIAN_POINT('',(61.6666822880186,20.26999998,-236.10005));
#234372=CARTESIAN_POINT('',(62.1666822880186,19.76999998,-189.64995));
#234373=CARTESIAN_POINT('Origin',(59.4002474757908,36.1278445718973,-180.14995));
#234374=CARTESIAN_POINT('',(59.4349689580299,36.1625660541364,-179.64995));
#234375=CARTESIAN_POINT('',(59.7538008663841,35.7742911813041,-180.14995));
#234376=CARTESIAN_POINT('Ctrl Pts',(59.4349689580299,36.1625660541365,-179.64995));
#234377=CARTESIAN_POINT('Ctrl Pts',(59.4751674290521,36.1139360589365,-179.64995));
#234378=CARTESIAN_POINT('Ctrl Pts',(59.517991405701,36.0619958343442,-179.662506459348));
#234379=CARTESIAN_POINT('Ctrl Pts',(59.5966866581669,35.9663093970947,-179.713622693033));
#234380=CARTESIAN_POINT('Ctrl Pts',(59.6325609826829,35.9225664005524,-179.752183794052));
#234381=CARTESIAN_POINT('Ctrl Pts',(59.689032648704,35.8536048925318,-179.841045572058));
#234382=CARTESIAN_POINT('Ctrl Pts',(59.7134506950769,35.8237224381175,-179.89718552734));
#234383=CARTESIAN_POINT('Ctrl Pts',(59.7458338457619,35.7840632466862,-180.020253182031));
#234384=CARTESIAN_POINT('Ctrl Pts',(59.7538008663841,35.7742911813041,-180.0871818826));
#234385=CARTESIAN_POINT('Ctrl Pts',(59.7538008663841,35.7742911813041,-180.14995));
#234386=CARTESIAN_POINT('',(52.8995100714853,29.6271071675918,-179.64995));
#234387=CARTESIAN_POINT('',(59.4002474757908,36.1278445718973,-179.64995));
#234388=CARTESIAN_POINT('',(53.2530634620785,29.2735537769986,-180.14995));
#234389=CARTESIAN_POINT('Origin',(52.8995100714853,29.6271071675918,-180.14995));
#234390=CARTESIAN_POINT('',(53.2530634620785,29.2735537769986,-180.14995));
#234391=CARTESIAN_POINT('Origin',(53.6066168526718,28.9200003864052,-180.14995));
#234392=CARTESIAN_POINT('',(53.6066168526718,27.9200003864053,-179.64995));
#234393=CARTESIAN_POINT('',(53.6066168526718,28.4200003864053,-180.14995));
#234394=CARTESIAN_POINT('Origin',(53.6066168526718,27.9200003864053,-180.14995));
#234395=CARTESIAN_POINT('Origin',(53.6066168526718,28.9200003864052,-180.14995));
#234396=CARTESIAN_POINT('Origin',(53.6066168526718,28.9200003864052,-179.64995));
#234397=CARTESIAN_POINT('Origin',(52.3995100714852,27.9200003864053,-180.14995));
#234398=CARTESIAN_POINT('',(59.1666822880186,27.9200003864053,-179.64995));
#234399=CARTESIAN_POINT('',(59.1666822880186,28.4200003864053,-180.14995));
#234400=CARTESIAN_POINT('Origin',(59.1666822880186,27.9200003864053,-180.14995));
#234401=CARTESIAN_POINT('',(59.1666822880186,28.4200003864053,-180.14995));
#234402=CARTESIAN_POINT('',(53.6066168526718,27.9200003864053,-179.64995));
#234403=CARTESIAN_POINT('Origin',(59.1666822880186,27.9200003864053,-182.64995));
#234404=CARTESIAN_POINT('',(62.1666822880186,27.9200003864053,-182.64995));
#234405=CARTESIAN_POINT('',(61.6666822880186,28.4200003864053,-182.64995));
#234406=CARTESIAN_POINT('Origin',(61.6666822880186,27.9200003864053,-182.64995));
#234407=CARTESIAN_POINT('Origin',(59.1666822880186,28.4200003864053,-182.64995));
#234408=CARTESIAN_POINT('Origin',(59.1666822880186,27.9200003864053,-182.64995));
#234409=CARTESIAN_POINT('Origin',(61.6666822880186,27.9200003864053,-189.64995));
#234410=CARTESIAN_POINT('',(61.6666822880186,28.4200003864053,-189.64995));
#234411=CARTESIAN_POINT('',(62.1666822880186,27.9200003864053,-189.64995));
#234412=CARTESIAN_POINT('Origin',(61.6666822880186,27.9200003864053,-189.64995));
#234413=CARTESIAN_POINT('',(61.6666822880186,28.4200003864053,-189.64995));
#234414=CARTESIAN_POINT('',(62.1666822880186,27.9200003864053,-189.64995));
#234415=CARTESIAN_POINT('Origin',(53.361677340714,-54.9537553161325,-189.64995));
#234416=CARTESIAN_POINT('',(53.361677340714,-54.4537553161325,-189.64995));
#234417=CARTESIAN_POINT('',(53.361677340714,-54.4537553161325,-189.64995));
#234418=CARTESIAN_POINT('',(53.0081239501207,-55.3073087067258,-189.64995));
#234419=CARTESIAN_POINT('',(53.0081239501207,-55.3073087067258,-179.64995));
#234420=CARTESIAN_POINT('Origin',(53.361677340714,-54.9537553161325,-189.64995));
#234421=CARTESIAN_POINT('Origin',(40.7325633042077,-65.3856746638358,-189.64995));
#234422=CARTESIAN_POINT('',(41.086116694801,-65.0321212732425,-189.64995));
#234423=CARTESIAN_POINT('',(41.086116694801,-65.0321212732425,-189.64995));
#234424=CARTESIAN_POINT('',(40.7325633042077,-64.8856746638358,-189.64995));
#234425=CARTESIAN_POINT('',(40.7325633042077,-64.8856746638358,-179.64995));
#234426=CARTESIAN_POINT('Origin',(40.7325633042077,-65.3856746638358,-189.64995));
#234427=CARTESIAN_POINT('Origin',(53.6066168526718,28.9200003864052,-189.64995));
#234428=CARTESIAN_POINT('',(53.2530634620785,29.2735537769986,-189.64995));
#234429=CARTESIAN_POINT('',(53.2530634620785,29.2735537769986,-189.64995));
#234430=CARTESIAN_POINT('',(53.6066168526718,28.4200003864053,-189.64995));
#234431=CARTESIAN_POINT('',(53.6066168526718,28.4200003864053,-179.64995));
#234432=CARTESIAN_POINT('Origin',(53.6066168526718,28.9200003864052,-189.64995));
#234433=CARTESIAN_POINT('Origin',(40.7325633042078,40.2945320099637,-189.64995));
#234434=CARTESIAN_POINT('',(40.7325633042078,39.7945320099637,-189.64995));
#234435=CARTESIAN_POINT('',(40.7325633042078,39.7945320099637,-189.64995));
#234436=CARTESIAN_POINT('',(41.086116694801,39.9409786193705,-189.64995));
#234437=CARTESIAN_POINT('',(41.086116694801,39.9409786193705,-179.64995));
#234438=CARTESIAN_POINT('Origin',(40.7325633042078,40.2945320099637,-189.64995));
#234439=CARTESIAN_POINT('Origin',(40.4396700853943,40.2945320099637,-189.64995));
#234440=CARTESIAN_POINT('',(39.9396700853943,40.2945320099637,-189.64995));
#234441=CARTESIAN_POINT('',(39.9396700853943,40.2945320099637,-189.64995));
#234442=CARTESIAN_POINT('',(40.4396700853943,39.7945320099637,-189.64995));
#234443=CARTESIAN_POINT('',(40.4396700853943,39.7945320099637,-179.64995));
#234444=CARTESIAN_POINT('Origin',(40.4396700853943,40.2945320099637,-189.64995));
#234445=CARTESIAN_POINT('Origin',(51.176438378063,26.41999998,-171.64995));
#234446=CARTESIAN_POINT('',(51.176438378063,26.91999998,-189.64995));
#234447=CARTESIAN_POINT('',(51.176438378063,26.91999998,-236.10005));
#234448=CARTESIAN_POINT('',(50.6813043436922,26.35041342952,-189.64995));
#234449=CARTESIAN_POINT('',(50.6813043436922,26.35041342952,-171.64995));
#234450=CARTESIAN_POINT('Origin',(51.176438378063,26.41999998,-189.64995));
#234451=CARTESIAN_POINT('Origin',(52.3218461808875,18.26999998,-171.64995));
#234452=CARTESIAN_POINT('',(52.3218461808875,18.76999998,-189.64995));
#234453=CARTESIAN_POINT('',(52.3218461808875,18.76999998,-236.10005));
#234454=CARTESIAN_POINT('',(51.8267121465167,18.20041342952,-189.64995));
#234455=CARTESIAN_POINT('',(51.8267121465167,18.20041342952,-171.64995));
#234456=CARTESIAN_POINT('Origin',(52.3218461808875,18.26999998,-189.64995));
#234457=CARTESIAN_POINT('Origin',(54.2951871140408,10.11999998,-179.64995));
#234458=CARTESIAN_POINT('',(54.2951871140408,10.61999998,-189.64995));
#234459=CARTESIAN_POINT('',(54.2951871140408,10.61999998,-189.64995));
#234460=CARTESIAN_POINT('',(53.8350584096845,9.92434320033877,-189.64995));
#234461=CARTESIAN_POINT('',(53.8350584096845,9.92434320033877,-179.64995));
#234462=CARTESIAN_POINT('Origin',(54.2951871140408,10.11999998,-189.64995));
#234463=CARTESIAN_POINT('Origin',(57.077763566464,1.96999998000002,-179.64995));
#234464=CARTESIAN_POINT('',(57.077763566464,2.46999998000002,-189.64995));
#234465=CARTESIAN_POINT('',(57.077763566464,2.46999998000002,-189.64995));
#234466=CARTESIAN_POINT('',(56.5940537057312,1.84341099694893,-189.64995));
#234467=CARTESIAN_POINT('',(56.5940537057312,1.84341099694893,-179.64995));
#234468=CARTESIAN_POINT('Origin',(57.077763566464,1.96999998000002,-189.64995));
#234469=CARTESIAN_POINT('Origin',(58.6082745331205,-6.18000001999998,-179.64995));
#234470=CARTESIAN_POINT('',(58.6082745331205,-5.68000001999998,-189.64995));
#234471=CARTESIAN_POINT('',(58.6082745331205,-5.68000001999998,-189.64995));
#234472=CARTESIAN_POINT('',(58.1115942404669,-6.2375212064409,-189.64995));
#234473=CARTESIAN_POINT('',(58.1115942404669,-6.2375212064409,-179.64995));
#234474=CARTESIAN_POINT('Origin',(58.6082745331205,-6.18000001999998,-189.64995));
#234475=CARTESIAN_POINT('Origin',(58.9842656455946,-14.33000002,-179.64995));
#234476=CARTESIAN_POINT('',(58.9842656455946,-13.83000002,-189.64995));
#234477=CARTESIAN_POINT('',(58.9842656455946,-13.83000002,-189.64995));
#234478=CARTESIAN_POINT('',(58.4843989875811,-14.3184534098307,-189.64995));
#234479=CARTESIAN_POINT('',(58.4843989875811,-14.3184534098307,-179.64995));
#234480=CARTESIAN_POINT('Origin',(58.9842656455946,-14.33000002,-189.64995));
#234481=CARTESIAN_POINT('Origin',(58.9890336736409,-11.83000002,-179.64995));
#234482=CARTESIAN_POINT('',(58.48912660861,-11.8396398505087,-189.64995));
#234483=CARTESIAN_POINT('',(58.48912660861,-11.8396398505087,-179.64995));
#234484=CARTESIAN_POINT('',(58.9890336736409,-12.33000002,-189.64995));
#234485=CARTESIAN_POINT('',(58.9890336736409,-12.33000002,-179.64995));
#234486=CARTESIAN_POINT('Origin',(58.9890336736409,-11.83000002,-189.64995));
#234487=CARTESIAN_POINT('Origin',(58.2644174754153,-3.68000001999999,-179.64995));
#234488=CARTESIAN_POINT('',(57.7706512256236,-3.75870764711887,-189.64995));
#234489=CARTESIAN_POINT('',(57.7706512256236,-3.75870764711887,-179.64995));
#234490=CARTESIAN_POINT('',(58.2644174754153,-4.18000001999998,-189.64995));
#234491=CARTESIAN_POINT('',(58.2644174754153,-4.18000001999998,-179.64995));
#234492=CARTESIAN_POINT('Origin',(58.2644174754153,-3.68000001999999,-189.64995));
#234493=CARTESIAN_POINT('Origin',(56.3642936064049,4.46999998000001,-179.64995));
#234494=CARTESIAN_POINT('',(55.8866301012659,4.32222455627096,-189.64995));
#234495=CARTESIAN_POINT('',(55.8866301012659,4.32222455627096,-179.64995));
#234496=CARTESIAN_POINT('',(56.3642936064049,3.96999998000001,-189.64995));
#234497=CARTESIAN_POINT('',(56.3642936064049,3.96999998000001,-179.64995));
#234498=CARTESIAN_POINT('Origin',(56.3642936064049,4.46999998000001,-189.64995));
#234499=CARTESIAN_POINT('Origin',(53.1963133798215,12.61999998,-179.64995));
#234500=CARTESIAN_POINT('',(52.7229737572976,12.4589111791821,-189.64995));
#234501=CARTESIAN_POINT('',(52.7229737572976,12.4589111791821,-179.64995));
#234502=CARTESIAN_POINT('',(53.1963133798215,12.11999998,-189.64995));
#234503=CARTESIAN_POINT('',(53.1963133798215,12.11999998,-179.64995));
#234504=CARTESIAN_POINT('Origin',(53.1963133798215,12.61999998,-189.64995));
#234505=CARTESIAN_POINT('Origin',(51.9704940941315,20.76999998,-236.10005));
#234506=CARTESIAN_POINT('',(51.4753600597607,20.70041342952,-189.64995));
#234507=CARTESIAN_POINT('',(51.4753600597607,20.70041342952,-171.64995));
#234508=CARTESIAN_POINT('',(51.9704940941315,20.26999998,-189.64995));
#234509=CARTESIAN_POINT('',(51.9704940941315,20.26999998,-236.10005));
#234510=CARTESIAN_POINT('Origin',(51.9704940941315,20.76999998,-189.64995));
#234511=CARTESIAN_POINT('Origin',(58.5817791104913,-19.98000002,-179.64995));
#234512=CARTESIAN_POINT('',(58.0853233553177,-19.9205720538985,-189.64995));
#234513=CARTESIAN_POINT('',(58.0853233553177,-19.9205720538985,-179.64995));
#234514=CARTESIAN_POINT('',(58.5817791104913,-20.48000002,-189.64995));
#234515=CARTESIAN_POINT('',(58.5817791104913,-20.48000002,-179.64995));
#234516=CARTESIAN_POINT('Origin',(58.5817791104913,-19.98000002,-189.64995));
#234517=CARTESIAN_POINT('Origin',(58.2281061322669,-22.48000002,-179.64995));
#234518=CARTESIAN_POINT('',(58.2281061322669,-21.98000002,-189.64995));
#234519=CARTESIAN_POINT('',(58.2281061322669,-21.98000002,-189.64995));
#234520=CARTESIAN_POINT('',(57.7346476057223,-22.3993856132206,-189.64995));
#234521=CARTESIAN_POINT('',(57.7346476057223,-22.3993856132206,-179.64995));
#234522=CARTESIAN_POINT('Origin',(58.2281061322669,-22.48000002,-189.64995));
#234523=CARTESIAN_POINT('Origin',(57.0184057454332,-28.13000002,-179.64995));
#234524=CARTESIAN_POINT('',(56.5351989170821,-28.0015042572884,-189.64995));
#234525=CARTESIAN_POINT('',(56.5351989170821,-28.0015042572884,-179.64995));
#234526=CARTESIAN_POINT('',(57.0184057454332,-28.63000002,-189.64995));
#234527=CARTESIAN_POINT('',(57.0184057454332,-28.63000002,-179.64995));
#234528=CARTESIAN_POINT('Origin',(57.0184057454332,-28.13000002,-189.64995));
#234529=CARTESIAN_POINT('Origin',(56.294192362543,-30.63000002,-179.64995));
#234530=CARTESIAN_POINT('',(56.294192362543,-30.13000002,-189.64995));
#234531=CARTESIAN_POINT('',(56.294192362543,-30.13000002,-189.64995));
#234532=CARTESIAN_POINT('',(55.8171229357418,-30.4803178166104,-189.64995));
#234533=CARTESIAN_POINT('',(55.8171229357418,-30.4803178166104,-179.64995));
#234534=CARTESIAN_POINT('Origin',(56.294192362543,-30.63000002,-189.64995));
#234535=CARTESIAN_POINT('Origin',(53.1262583325313,-38.78000002,-179.64995));
#234536=CARTESIAN_POINT('',(53.1262583325313,-38.28000002,-189.64995));
#234537=CARTESIAN_POINT('',(53.1262583325313,-38.28000002,-189.64995));
#234538=CARTESIAN_POINT('',(52.6451348158641,-38.6439112191758,-189.64995));
#234539=CARTESIAN_POINT('',(52.6451348158641,-38.6439112191758,-179.64995));
#234540=CARTESIAN_POINT('Origin',(53.1262583325313,-38.78000002,-189.64995));
#234541=CARTESIAN_POINT('Origin',(54.1989607257493,-36.28000002,-179.64995));
#234542=CARTESIAN_POINT('',(53.7396474992599,-36.0824364606782,-189.64995));
#234543=CARTESIAN_POINT('',(53.7396474992599,-36.0824364606782,-179.64995));
#234544=CARTESIAN_POINT('',(54.1989607257493,-36.78000002,-189.64995));
#234545=CARTESIAN_POINT('',(54.1989607257493,-36.78000002,-179.64995));
#234546=CARTESIAN_POINT('Origin',(54.1989607257493,-36.28000002,-189.64995));
#234547=CARTESIAN_POINT('Origin',(52.2902244930873,-44.43000002,-236.10005));
#234548=CARTESIAN_POINT('',(51.7950904587165,-44.36041346952,-189.64995));
#234549=CARTESIAN_POINT('',(51.7950904587165,-44.36041346952,-171.64995));
#234550=CARTESIAN_POINT('',(52.2902244930873,-44.93000002,-189.64995));
#234551=CARTESIAN_POINT('',(52.2902244930873,-44.93000002,-236.10005));
#234552=CARTESIAN_POINT('Origin',(52.2902244930873,-44.43000002,-189.64995));
#234553=CARTESIAN_POINT('Origin',(51.9388724063314,-46.93000002,-171.64995));
#234554=CARTESIAN_POINT('',(51.9388724063314,-46.43000002,-189.64995));
#234555=CARTESIAN_POINT('',(51.9388724063314,-46.43000002,-236.10005));
#234556=CARTESIAN_POINT('',(51.4437383719606,-46.86041346952,-189.64995));
#234557=CARTESIAN_POINT('',(51.4437383719606,-46.8604134695199,-171.64995));
#234558=CARTESIAN_POINT('Origin',(51.9388724063314,-46.93000002,-189.64995));
#234559=CARTESIAN_POINT('Origin',(51.1448166902628,-52.58000002,-236.10005));
#234560=CARTESIAN_POINT('',(50.6496826558921,-52.51041346952,-189.64995));
#234561=CARTESIAN_POINT('',(50.6496826558921,-52.51041346952,-171.64995));
#234562=CARTESIAN_POINT('',(51.1448166902628,-53.08000002,-189.64995));
#234563=CARTESIAN_POINT('',(51.1448166902628,-53.08000002,-236.10005));
#234564=CARTESIAN_POINT('Origin',(51.1448166902628,-52.58000002,-189.64995));
#234565=CARTESIAN_POINT('Origin',(40.4396700853942,-65.3856746638358,-189.64995));
#234566=CARTESIAN_POINT('',(40.4396700853942,-64.8856746638358,-189.64995));
#234567=CARTESIAN_POINT('',(40.4396700853942,-64.8856746638358,-189.64995));
#234568=CARTESIAN_POINT('',(39.9396700853942,-65.3856746638358,-189.64995));
#234569=CARTESIAN_POINT('',(39.9396700853942,-65.3856746638358,-179.64995));
#234570=CARTESIAN_POINT('Origin',(40.4396700853942,-65.3856746638358,-189.64995));
#234571=CARTESIAN_POINT('Origin',(50.5696324866523,-53.08000002,-179.64995));
#234572=CARTESIAN_POINT('Origin',(0.,-12.9675000200281,-179.64995));
#234573=CARTESIAN_POINT('',(8.67557705647162E-17,53.4196191598902,-179.64995));
#234574=CARTESIAN_POINT('Origin',(0.,-178.58000002,-179.64995));
#234575=CARTESIAN_POINT('',(-1.57577820804084E-14,-75.2524362554308,-179.64995));
#234576=CARTESIAN_POINT('',(8.67557705647162E-17,53.4196191598902,-179.64995));
#234577=CARTESIAN_POINT('',(-1.57577820804084E-14,-75.2524362554308,-179.64995));
#234578=CARTESIAN_POINT('Origin',(0.,-12.9675000200281,-179.64995));
#234579=CARTESIAN_POINT('',(59.1666822880186,28.4200003864053,-179.64995));
#234580=CARTESIAN_POINT('',(59.1666822880186,28.4200003864053,-179.64995));
#234581=CARTESIAN_POINT('',(59.1666822880186,28.4200003864053,-179.64995));
#234582=CARTESIAN_POINT('',(59.1666822880186,28.4200003864053,-179.64995));
#234583=CARTESIAN_POINT('',(59.1666822880186,28.4200003864053,-179.64995));
#234584=CARTESIAN_POINT('',(59.1666822880186,28.4200003864053,-179.64995));
#234585=CARTESIAN_POINT('',(59.1666822880186,28.4200003864053,-179.64995));
#234586=CARTESIAN_POINT('',(59.1666822880186,28.4200003864053,-179.64995));
#234587=CARTESIAN_POINT('',(59.1666822880186,28.4200003864053,-179.64995));
#234588=CARTESIAN_POINT('',(59.1666822880186,28.4200003864053,-179.64995));
#234589=CARTESIAN_POINT('',(59.1666822880186,28.4200003864053,-179.64995));
#234590=CARTESIAN_POINT('Origin',(62.1666822880186,-54.4537553161325,-189.64995));
#234591=CARTESIAN_POINT('',(62.1666822880186,-54.4537553161325,-189.64995));
#234592=CARTESIAN_POINT('Origin',(0.,-178.58000002,-189.64995));
#234593=CARTESIAN_POINT('',(39.9396700853943,49.9558747416749,-189.64995));
#234594=CARTESIAN_POINT('',(39.9396700853943,49.9558747416749,-189.64995));
#234595=CARTESIAN_POINT('',(8.67557705647162E-17,53.4196191598902,-189.64995));
#234596=CARTESIAN_POINT('Origin',(0.,-178.58000002,-189.64995));
#234597=CARTESIAN_POINT('',(8.67557705647162E-17,53.4196191598902,-189.64995));
#234598=CARTESIAN_POINT('Origin',(39.9396700853943,49.9558747416749,-189.64995));
#234599=CARTESIAN_POINT('',(39.9396700853943,49.9558747416749,-189.64995));
#234600=CARTESIAN_POINT('Origin',(39.9396700853942,-64.8856746638358,-189.64995));
#234601=CARTESIAN_POINT('',(39.9396700853942,-64.8856746638358,-189.64995));
#234602=CARTESIAN_POINT('Origin',(39.9396700853942,-64.8856746638358,-189.64995));
#234603=CARTESIAN_POINT('',(39.9396700853942,-75.2524362554308,-189.64995));
#234604=CARTESIAN_POINT('',(39.9396700853942,-75.2524362554308,-189.64995));
#234605=CARTESIAN_POINT('',(39.9396700853942,-64.8856746638358,-189.64995));
#234606=CARTESIAN_POINT('Origin',(50.5696324866523,-53.08000002,-236.10005));
#234607=CARTESIAN_POINT('',(0.,-53.08000002,-189.64995));
#234608=CARTESIAN_POINT('Origin',(51.5042290374232,-46.43000002,-236.10005));
#234609=CARTESIAN_POINT('',(0.,-46.43000002,-189.64995));
#234610=CARTESIAN_POINT('Origin',(57.8362329664502,-4.18000001999998,-236.10005));
#234611=CARTESIAN_POINT('',(0.,-4.18000001999998,-189.64995));
#234612=CARTESIAN_POINT('Origin',(56.4263554888062,2.46999998000002,-236.10005));
#234613=CARTESIAN_POINT('',(0.,2.46999998000002,-189.64995));
#234614=CARTESIAN_POINT('Origin',(55.9943844840627,3.96999998000001,-236.10005));
#234615=CARTESIAN_POINT('',(2.25916865206423E-15,3.96999998000003,-189.64995));
#234616=CARTESIAN_POINT('Origin',(53.533913024817,10.61999998,-236.10005));
#234617=CARTESIAN_POINT('',(2.64564592552133E-15,10.61999998,-189.64995));
#234618=CARTESIAN_POINT('Origin',(51.746661977277,18.76999998,-236.10005));
#234619=CARTESIAN_POINT('',(0.,18.76999998,-189.64995));
#234620=CARTESIAN_POINT('Origin',(51.7150402894768,-44.93000002,-236.10005));
#234621=CARTESIAN_POINT('',(0.,-44.93000002,-189.64995));
#234622=CARTESIAN_POINT('Origin',(58.4965263391765,-12.33000002,-236.10005));
#234623=CARTESIAN_POINT('',(0.,-12.33000002,-189.64995));
#234624=CARTESIAN_POINT('Origin',(58.0443136211429,-5.68000001999998,-236.10005));
#234625=CARTESIAN_POINT('',(-1.15390281302924E-15,-5.68000001999999,-189.64995));
#234626=CARTESIAN_POINT('Origin',(62.1666822880186,28.4200003864053,-189.64995));
#234627=CARTESIAN_POINT('',(62.1666822880186,28.4200003864053,-189.64995));
#234628=CARTESIAN_POINT('',(62.1666822880186,-54.4537553161326,-182.64995));
#234629=CARTESIAN_POINT('Origin',(59.1666822880186,28.4200003864053,-182.64995));
#234630=CARTESIAN_POINT('Origin',(0.,-12.9675000200281,-179.64995));
#234631=CARTESIAN_POINT('Origin',(0.,-12.9675000200281,-189.64995));
#234632=CARTESIAN_POINT('Origin',(58.0156215492899,-20.48000002,-236.10005));
#234633=CARTESIAN_POINT('',(0.,-20.48000002,-189.64995));
#234634=CARTESIAN_POINT('Origin',(58.4936414813615,-13.83000002,-236.10005));
#234635=CARTESIAN_POINT('',(0.,-13.83000002,-189.64995));
#234636=CARTESIAN_POINT('Origin',(62.1666822880186,28.4200003864053,-189.64995));
#234637=CARTESIAN_POINT('',(62.1666822880186,28.4200003864053,-189.64995));
#234638=CARTESIAN_POINT('',(62.1666822880186,-54.4537553161326,-182.64995));
#234639=CARTESIAN_POINT('Origin',(59.1666822880186,28.4200003864053,-182.64995));
#234640=CARTESIAN_POINT('Origin',(0.,-12.9675000200281,-179.64995));
#234641=CARTESIAN_POINT('Origin',(0.,-12.9675000200281,-189.64995));
#234642=CARTESIAN_POINT('Origin',(56.3643157835779,-28.63000002,-236.10005));
#234643=CARTESIAN_POINT('',(4.30053584389595E-15,-28.63000002,-189.64995));
#234644=CARTESIAN_POINT('Origin',(57.8015989722647,-21.98000002,-236.10005));
#234645=CARTESIAN_POINT('',(0.,-21.98000002,-189.64995));
#234646=CARTESIAN_POINT('Origin',(62.1666822880186,28.4200003864053,-189.64995));
#234647=CARTESIAN_POINT('',(62.1666822880186,28.4200003864053,-189.64995));
#234648=CARTESIAN_POINT('',(62.1666822880186,-54.4537553161326,-182.64995));
#234649=CARTESIAN_POINT('Origin',(59.1666822880186,28.4200003864053,-182.64995));
#234650=CARTESIAN_POINT('Origin',(0.,-12.9675000200281,-179.64995));
#234651=CARTESIAN_POINT('Origin',(0.,-12.9675000200281,-189.64995));
#234652=CARTESIAN_POINT('Origin',(53.4342104250764,-36.78000002,-236.10005));
#234653=CARTESIAN_POINT('',(0.,-36.78000002,-189.64995));
#234654=CARTESIAN_POINT('Origin',(55.9258311851596,-30.13000002,-236.10005));
#234655=CARTESIAN_POINT('',(4.55435325611026E-15,-30.13000002,-189.64995));
#234656=CARTESIAN_POINT('Origin',(62.1666822880186,28.4200003864053,-189.64995));
#234657=CARTESIAN_POINT('',(62.1666822880186,28.4200003864053,-189.64995));
#234658=CARTESIAN_POINT('',(62.1666822880186,-54.4537553161326,-182.64995));
#234659=CARTESIAN_POINT('Origin',(59.1666822880186,28.4200003864053,-182.64995));
#234660=CARTESIAN_POINT('Origin',(0.,-12.9675000200281,-179.64995));
#234661=CARTESIAN_POINT('Origin',(0.,-12.9675000200281,-189.64995));
#234662=CARTESIAN_POINT('Origin',(51.5358507252234,20.26999998,-236.10005));
#234663=CARTESIAN_POINT('',(-6.60299801904499E-15,20.26999998,-189.64995));
#234664=CARTESIAN_POINT('Origin',(50.6012541744525,26.91999998,-236.10005));
#234665=CARTESIAN_POINT('',(0.,26.91999998,-189.64995));
#234666=CARTESIAN_POINT('Origin',(62.1666822880186,28.4200003864053,-189.64995));
#234667=CARTESIAN_POINT('',(62.1666822880186,28.4200003864053,-189.64995));
#234668=CARTESIAN_POINT('',(62.1666822880186,-54.4537553161326,-182.64995));
#234669=CARTESIAN_POINT('Origin',(59.1666822880186,28.4200003864053,-182.64995));
#234670=CARTESIAN_POINT('Origin',(52.6124803109502,12.6093824234965,-171.64995));
#234671=CARTESIAN_POINT('',(55.1183933044755,-5.22111501756238,-189.64995));
#234672=CARTESIAN_POINT('Origin',(57.4563699825363,-40.0047992274175,-179.64995));
#234673=CARTESIAN_POINT('',(52.5050296388285,-39.3089337226172,-189.64995));
#234674=CARTESIAN_POINT('',(52.5050296388285,-39.3089337226171,-171.64995));
#234675=CARTESIAN_POINT('Origin',(57.4563699825363,-40.0047992274175,-189.64995));
#234676=CARTESIAN_POINT('Origin',(52.6124803109501,-38.5443824635529,-171.64995));
#234677=CARTESIAN_POINT('',(55.1183933044754,-20.7138850224938,-189.64995));
#234678=CARTESIAN_POINT('Origin',(57.4563699825364,14.0697991873612,-179.64995));
#234679=CARTESIAN_POINT('',(52.5050296388285,13.3739336825608,-189.64995));
#234680=CARTESIAN_POINT('',(52.5050296388285,13.3739336825608,-171.64995));
#234681=CARTESIAN_POINT('Origin',(57.4563699825364,14.0697991873612,-189.64995));
#234682=CARTESIAN_POINT('Origin',(52.8475859784398,12.11999998,-236.10005));
#234683=CARTESIAN_POINT('',(0.,12.11999998,-189.64995));
#234684=CARTESIAN_POINT('Origin',(0.,-12.9675000200281,-189.64995));
#234685=CARTESIAN_POINT('',(52.3995100714852,28.4200003864053,-189.64995));
#234686=CARTESIAN_POINT('',(62.1666822880186,28.4200003864053,-189.64995));
#234687=CARTESIAN_POINT('',(55.1183933044755,-5.22111501756237,-189.64995));
#234688=CARTESIAN_POINT('',(62.1666822880186,28.4200003864053,-189.64995));
#234689=CARTESIAN_POINT('Origin',(0.,-12.9675000200281,-189.64995));
#234690=CARTESIAN_POINT('',(62.1666822880186,28.4200003864053,-189.64995));
#234691=CARTESIAN_POINT('Origin',(0.,-12.9675000200281,-189.64995));
#234692=CARTESIAN_POINT('',(62.1666822880186,28.4200003864053,-189.64995));
#234693=CARTESIAN_POINT('',(0.,-38.28000002,-189.64995));
#234694=CARTESIAN_POINT('',(62.1666822880186,28.4200003864053,-189.64995));
#234695=CARTESIAN_POINT('',(55.1183933044754,-20.7138850224938,-189.64995));
#234696=CARTESIAN_POINT('',(62.1666822880186,28.4200003864053,-189.64995));
#234697=CARTESIAN_POINT('',(59.5991207857295,-61.8983055423346,-189.64995));
#234698=CARTESIAN_POINT('',(59.5991207857295,-61.8983055423346,-189.64995));
#234699=CARTESIAN_POINT('',(48.7602414802939,-72.7062460587355,-189.64995));
#234700=CARTESIAN_POINT('Origin',(0.,-12.9675000200281,-189.64995));
#234701=CARTESIAN_POINT('',(48.7602414802939,-72.7062460587355,-189.64995));
#234702=CARTESIAN_POINT('',(-1.57577820804084E-14,-75.2524362554308,-189.64995));
#234703=CARTESIAN_POINT('',(-1.57577820804084E-14,-75.2524362554308,-189.64995));
#234704=CARTESIAN_POINT('',(8.67557705647162E-17,53.4196191598902,-189.64995));
#234705=CARTESIAN_POINT('',(39.9396700853943,39.7945320099637,-189.64995));
#234706=CARTESIAN_POINT('',(48.2939608802931,47.1488228048625,-189.64995));
#234707=CARTESIAN_POINT('',(48.2939608802931,47.1488228048625,-189.64995));
#234708=CARTESIAN_POINT('',(59.7538008663841,35.7742911813041,-189.64995));
#234709=CARTESIAN_POINT('Origin',(0.,-12.9675000200281,-189.64995));
#234710=CARTESIAN_POINT('',(59.7538008663841,35.7742911813041,-189.64995));
#234711=CARTESIAN_POINT('Origin',(52.6124803109502,12.6093824234965,-171.64995));
#234712=CARTESIAN_POINT('Origin',(52.7401871797155,-38.28000002,-236.10005));
#234713=CARTESIAN_POINT('Origin',(59.1666822880186,28.4200003864053,-182.64995));
#234714=CARTESIAN_POINT('',(62.1666822880186,-54.4537553161326,-182.64995));
#234715=CARTESIAN_POINT('Origin',(62.1666822880186,28.4200003864053,-189.64995));
#234716=CARTESIAN_POINT('Origin',(59.1666822880186,28.4200003864053,-182.64995));
#234717=CARTESIAN_POINT('',(62.1666822880186,-54.4537553161326,-182.64995));
#234718=CARTESIAN_POINT('Origin',(62.1666822880186,28.4200003864053,-189.64995));
#234719=CARTESIAN_POINT('Origin',(59.1666822880186,28.4200003864053,-182.64995));
#234720=CARTESIAN_POINT('',(62.1666822880186,-54.4537553161326,-182.64995));
#234721=CARTESIAN_POINT('Origin',(62.1666822880186,28.4200003864053,-189.64995));
#234722=CARTESIAN_POINT('Origin',(59.1666822880186,28.4200003864053,-182.64995));
#234723=CARTESIAN_POINT('',(62.1666822880186,-54.4537553161326,-182.64995));
#234724=CARTESIAN_POINT('Origin',(62.1666822880186,28.4200003864053,-189.64995));
#234725=CARTESIAN_POINT('Origin',(0.,-12.9675000200281,-179.64995));
#234726=CARTESIAN_POINT('Origin',(59.1666822880186,28.4200003864053,-182.64995));
#234727=CARTESIAN_POINT('',(62.1666822880186,-54.4537553161326,-182.64995));
#234728=CARTESIAN_POINT('Origin',(62.1666822880186,28.4200003864053,-189.64995));
#234729=CARTESIAN_POINT('Origin',(0.,-12.9675000200281,-179.64995));
#234730=CARTESIAN_POINT('Origin',(52.6124803109501,-38.5443824635529,-171.64995));
#234731=CARTESIAN_POINT('Origin',(59.1666822880186,28.4200003864053,-182.64995));
#234732=CARTESIAN_POINT('',(62.1666822880186,-54.4537553161326,-182.64995));
#234733=CARTESIAN_POINT('Origin',(62.1666822880186,28.4200003864053,-189.64995));
#234734=CARTESIAN_POINT('Origin',(48.7602414802939,-72.7062460587355,-189.64995));
#234735=CARTESIAN_POINT('',(48.7602414802939,-72.7062460587355,-189.64995));
#234736=CARTESIAN_POINT('Origin',(-1.57577820804084E-14,-75.2524362554308,
-189.64995));
#234737=CARTESIAN_POINT('',(-1.57577820804084E-14,-75.2524362554308,-189.64995));
#234738=CARTESIAN_POINT('Origin',(0.,-120.,224.35005));
#234739=CARTESIAN_POINT('Origin',(39.9396700853943,39.7945320099637,-189.64995));
#234740=CARTESIAN_POINT('Origin',(48.2939608802931,47.1488228048625,-189.64995));
#234741=CARTESIAN_POINT('',(48.2939608802931,47.1488228048625,-189.64995));
#234742=CARTESIAN_POINT('Origin',(0.,-12.9675000200281,-189.64995));
#234743=CARTESIAN_POINT('',(59.7538008663841,35.7742911813041,-189.64995));
#234744=CARTESIAN_POINT('Origin',(59.7538008663841,35.7742911813041,-189.64995));
#234745=CARTESIAN_POINT('Origin',(52.3995100714852,28.4200003864053,-189.64995));
#234746=CARTESIAN_POINT('Origin',(59.5991207857295,-61.8983055423346,-189.64995));
#234747=CARTESIAN_POINT('',(59.5991207857295,-61.8983055423346,-189.64995));
#234748=CARTESIAN_POINT('Origin',(0.,-12.9675000200281,-189.64995));
#234749=CARTESIAN_POINT('Origin',(12.9675000200281,-12.967500020028,-32.54995));
#234750=CARTESIAN_POINT('',(62.5573729911059,-10.4675000200275,-32.54995));
#234751=CARTESIAN_POINT('',(66.8875000100281,-7.96750002002744,-32.54995));
#234752=CARTESIAN_POINT('Origin',(66.8875000100282,-12.9675000200274,-32.54995));
#234753=CARTESIAN_POINT('',(71.2176270289503,-10.4675000200274,-32.54995));
#234754=CARTESIAN_POINT('Origin',(66.8875000100282,-12.9675000200274,-32.54995));
#234755=CARTESIAN_POINT('',(71.2176270289504,-15.4675000200274,-32.54995));
#234756=CARTESIAN_POINT('Origin',(66.8875000100282,-12.9675000200274,-32.54995));
#234757=CARTESIAN_POINT('',(66.8875000100282,-17.9675000200275,-32.54995));
#234758=CARTESIAN_POINT('Origin',(66.8875000100282,-12.9675000200274,-32.54995));
#234759=CARTESIAN_POINT('',(62.557372991106,-15.4675000200275,-32.54995));
#234760=CARTESIAN_POINT('Origin',(66.8875000100282,-12.9675000200274,-32.54995));
#234761=CARTESIAN_POINT('Origin',(66.8875000100282,-12.9675000200274,-32.54995));
#234762=CARTESIAN_POINT('Origin',(66.8875000100282,-12.9675000200274,-32.54995));
#234763=CARTESIAN_POINT('',(69.7742513559762,-7.96750002002741,-31.7764473081038));
#234764=CARTESIAN_POINT('Ctrl Pts',(69.7742513559762,-7.96750002002744,
-31.7764473081038));
#234765=CARTESIAN_POINT('Ctrl Pts',(70.5477540478725,-9.30724598218304,
-32.5499500000001));
#234766=CARTESIAN_POINT('Ctrl Pts',(71.2176270289503,-10.4675000200274,
-32.5499500000001));
#234767=CARTESIAN_POINT('Ctrl Pts',(66.8875000100281,-7.96750002002744,
-32.54995));
#234768=CARTESIAN_POINT('Ctrl Pts',(68.2272459721837,-7.96750002002743,
-32.54995));
#234769=CARTESIAN_POINT('Ctrl Pts',(69.7742513559762,-7.96750002002741,
-31.7764473081038));
#234770=CARTESIAN_POINT('Origin',(66.8875000100282,-12.9675000200274,-32.54995));
#234771=CARTESIAN_POINT('',(72.6610027019244,-12.9675000200274,-31.7764473081038));
#234772=CARTESIAN_POINT('Ctrl Pts',(71.2176270289503,-10.4675000200274,
-32.5499500000001));
#234773=CARTESIAN_POINT('Ctrl Pts',(71.8875000100281,-11.6277540578718,
-32.5499500000001));
#234774=CARTESIAN_POINT('Ctrl Pts',(72.6610027019244,-12.9675000200274,
-31.7764473081038));
#234775=CARTESIAN_POINT('Ctrl Pts',(72.6610027019244,-12.9675000200274,
-31.7764473081038));
#234776=CARTESIAN_POINT('Ctrl Pts',(71.8875000100282,-14.307245982183,-32.5499500000001));
#234777=CARTESIAN_POINT('Ctrl Pts',(71.2176270289504,-15.4675000200274,
-32.5499500000001));
#234778=CARTESIAN_POINT('Origin',(66.8875000100282,-12.9675000200274,-32.54995));
#234779=CARTESIAN_POINT('',(69.7742513559763,-17.9675000200274,-31.7764473081038));
#234780=CARTESIAN_POINT('Ctrl Pts',(71.2176270289504,-15.4675000200274,
-32.5499500000001));
#234781=CARTESIAN_POINT('Ctrl Pts',(70.5477540478726,-16.6277540578718,
-32.5499500000001));
#234782=CARTESIAN_POINT('Ctrl Pts',(69.7742513559763,-17.9675000200274,
-31.7764473081038));
#234783=CARTESIAN_POINT('Ctrl Pts',(69.7742513559763,-17.9675000200274,
-31.7764473081038));
#234784=CARTESIAN_POINT('Ctrl Pts',(68.2272459721838,-17.9675000200274,
-32.54995));
#234785=CARTESIAN_POINT('Ctrl Pts',(66.8875000100282,-17.9675000200274,
-32.54995));
#234786=CARTESIAN_POINT('Origin',(66.8875000100282,-12.9675000200274,-32.54995));
#234787=CARTESIAN_POINT('',(64.0007486640801,-17.9675000200275,-31.7764473081038));
#234788=CARTESIAN_POINT('Ctrl Pts',(66.8875000100282,-17.9675000200274,
-32.54995));
#234789=CARTESIAN_POINT('Ctrl Pts',(65.5477540478726,-17.9675000200274,
-32.54995));
#234790=CARTESIAN_POINT('Ctrl Pts',(64.0007486640801,-17.9675000200275,
-31.7764473081038));
#234791=CARTESIAN_POINT('Ctrl Pts',(64.0007486640801,-17.9675000200274,
-31.7764473081038));
#234792=CARTESIAN_POINT('Ctrl Pts',(63.2272459721838,-16.6277540578719,
-32.54995));
#234793=CARTESIAN_POINT('Ctrl Pts',(62.557372991106,-15.4675000200275,-32.54995));
#234794=CARTESIAN_POINT('Origin',(66.8875000100282,-12.9675000200274,-32.54995));
#234795=CARTESIAN_POINT('',(61.1139973181319,-12.9675000200275,-31.7764473081038));
#234796=CARTESIAN_POINT('Ctrl Pts',(62.557372991106,-15.4675000200275,-32.54995));
#234797=CARTESIAN_POINT('Ctrl Pts',(61.8875000100282,-14.3072459821831,
-32.54995));
#234798=CARTESIAN_POINT('Ctrl Pts',(61.1139973181319,-12.9675000200275,
-31.7764473081037));
#234799=CARTESIAN_POINT('Ctrl Pts',(61.1139973181319,-12.9675000200275,
-31.7764473081037));
#234800=CARTESIAN_POINT('Ctrl Pts',(61.8875000100281,-11.6277540578719,
-32.5499499999999));
#234801=CARTESIAN_POINT('Ctrl Pts',(62.5573729911059,-10.4675000200275,
-32.5499499999999));
#234802=CARTESIAN_POINT('Origin',(66.8875000100282,-12.9675000200274,-32.54995));
#234803=CARTESIAN_POINT('',(64.00074866408,-7.96750002002747,-31.7764473081038));
#234804=CARTESIAN_POINT('Ctrl Pts',(62.5573729911059,-10.4675000200275,
-32.5499499999999));
#234805=CARTESIAN_POINT('Ctrl Pts',(63.2272459721837,-9.3072459821831,-32.54995));
#234806=CARTESIAN_POINT('Ctrl Pts',(64.00074866408,-7.9675000200275,-31.7764473081037));
#234807=CARTESIAN_POINT('Ctrl Pts',(64.00074866408,-7.96750002002747,-31.7764473081038));
#234808=CARTESIAN_POINT('Ctrl Pts',(65.5477540478725,-7.96750002002745,
-32.54995));
#234809=CARTESIAN_POINT('Ctrl Pts',(66.8875000100281,-7.96750002002744,
-32.54995));
#234810=CARTESIAN_POINT('Origin',(12.9675000200281,-12.967500020028,-28.54995));
#234811=CARTESIAN_POINT('',(66.8875000100281,-7.96750002002746,-28.54995));
#234812=CARTESIAN_POINT('',(71.2176270289503,-10.4675000200274,-28.54995));
#234813=CARTESIAN_POINT('Origin',(66.8875000100282,-12.9675000200274,-28.54995));
#234814=CARTESIAN_POINT('',(62.5573729911059,-10.4675000200275,-28.54995));
#234815=CARTESIAN_POINT('Origin',(66.8875000100282,-12.9675000200274,-28.54995));
#234816=CARTESIAN_POINT('',(62.557372991106,-15.4675000200275,-28.54995));
#234817=CARTESIAN_POINT('Origin',(66.8875000100282,-12.9675000200274,-28.54995));
#234818=CARTESIAN_POINT('',(66.8875000100282,-17.9675000200275,-28.54995));
#234819=CARTESIAN_POINT('Origin',(66.8875000100282,-12.9675000200274,-28.54995));
#234820=CARTESIAN_POINT('',(71.2176270289504,-15.4675000200274,-28.54995));
#234821=CARTESIAN_POINT('Origin',(66.8875000100282,-12.9675000200274,-28.54995));
#234822=CARTESIAN_POINT('Origin',(66.8875000100282,-12.9675000200274,-28.54995));
#234823=CARTESIAN_POINT('Origin',(66.8875000100282,-12.9675000200274,-28.54995));
#234824=CARTESIAN_POINT('',(64.0007486640797,-7.96750002002747,-28.9965319873851));
#234825=CARTESIAN_POINT('Ctrl Pts',(64.0007486640716,-7.96750002002748,
-28.9965319873876));
#234826=CARTESIAN_POINT('Ctrl Pts',(65.5477540478691,-7.96750002002746,
-28.54995));
#234827=CARTESIAN_POINT('Ctrl Pts',(66.8875000100281,-7.96750002002745,
-28.54995));
#234828=CARTESIAN_POINT('Ctrl Pts',(62.5573729911059,-10.4675000200275,
-28.54995));
#234829=CARTESIAN_POINT('Ctrl Pts',(63.2272459721853,-9.30724598218033,
-28.54995));
#234830=CARTESIAN_POINT('Ctrl Pts',(64.000748664084,-7.96750002002055,-28.9965319873875));
#234831=CARTESIAN_POINT('Origin',(66.8875000100282,-12.9675000200274,-28.54995));
#234832=CARTESIAN_POINT('',(61.1139973181319,-12.9675000200275,-28.9965319873852));
#234833=CARTESIAN_POINT('Ctrl Pts',(61.1139973181278,-12.9675000200346,
-28.9965319873876));
#234834=CARTESIAN_POINT('Ctrl Pts',(61.8875000100265,-11.6277540578747,
-28.54995));
#234835=CARTESIAN_POINT('Ctrl Pts',(62.5573729911059,-10.4675000200275,
-28.54995));
#234836=CARTESIAN_POINT('Ctrl Pts',(62.557372991106,-15.4675000200275,-28.54995));
#234837=CARTESIAN_POINT('Ctrl Pts',(61.8875000100266,-14.3072459821803,
-28.54995));
#234838=CARTESIAN_POINT('Ctrl Pts',(61.1139973181278,-12.9675000200204,
-28.9965319873876));
#234839=CARTESIAN_POINT('Origin',(66.8875000100282,-12.9675000200274,-28.54995));
#234840=CARTESIAN_POINT('',(64.0007486640801,-17.9675000200275,-28.9965319873852));
#234841=CARTESIAN_POINT('Ctrl Pts',(64.0007486640842,-17.9675000200345,
-28.9965319873876));
#234842=CARTESIAN_POINT('Ctrl Pts',(63.2272459721855,-16.6277540578747,
-28.54995));
#234843=CARTESIAN_POINT('Ctrl Pts',(62.557372991106,-15.4675000200275,-28.54995));
#234844=CARTESIAN_POINT('Ctrl Pts',(66.8875000100282,-17.9675000200274,
-28.54995));
#234845=CARTESIAN_POINT('Ctrl Pts',(65.5477540478693,-17.9675000200274,
-28.54995));
#234846=CARTESIAN_POINT('Ctrl Pts',(64.000748664072,-17.9675000200275,-28.9965319873876));
#234847=CARTESIAN_POINT('Origin',(66.8875000100282,-12.9675000200274,-28.54995));
#234848=CARTESIAN_POINT('',(69.7742513559763,-17.9675000200274,-28.9965319873852));
#234849=CARTESIAN_POINT('Ctrl Pts',(69.7742513559845,-17.9675000200274,
-28.9965319873875));
#234850=CARTESIAN_POINT('Ctrl Pts',(68.2272459721871,-17.9675000200274,
-28.54995));
#234851=CARTESIAN_POINT('Ctrl Pts',(66.8875000100282,-17.9675000200274,
-28.54995));
#234852=CARTESIAN_POINT('Ctrl Pts',(71.2176270289503,-15.4675000200274,
-28.54995));
#234853=CARTESIAN_POINT('Ctrl Pts',(70.5477540478709,-16.6277540578746,
-28.54995));
#234854=CARTESIAN_POINT('Ctrl Pts',(69.7742513559722,-17.9675000200345,
-28.9965319873875));
#234855=CARTESIAN_POINT('Origin',(66.8875000100282,-12.9675000200274,-28.54995));
#234856=CARTESIAN_POINT('',(72.6610027019244,-12.9675000200274,-28.9965319873853));
#234857=CARTESIAN_POINT('Ctrl Pts',(72.6610027019285,-12.9675000200203,
-28.9965319873875));
#234858=CARTESIAN_POINT('Ctrl Pts',(71.8875000100298,-14.3072459821802,
-28.54995));
#234859=CARTESIAN_POINT('Ctrl Pts',(71.2176270289503,-15.4675000200274,
-28.54995));
#234860=CARTESIAN_POINT('Ctrl Pts',(71.2176270289503,-10.4675000200274,
-28.54995));
#234861=CARTESIAN_POINT('Ctrl Pts',(71.8875000100298,-11.6277540578746,
-28.54995));
#234862=CARTESIAN_POINT('Ctrl Pts',(72.6610027019285,-12.9675000200345,
-28.9965319873875));
#234863=CARTESIAN_POINT('Origin',(66.8875000100282,-12.9675000200274,-28.54995));
#234864=CARTESIAN_POINT('',(69.7742513559762,-7.96750002002741,-28.9965319873852));
#234865=CARTESIAN_POINT('Ctrl Pts',(66.8875000100281,-7.96750002002745,
-28.54995));
#234866=CARTESIAN_POINT('Ctrl Pts',(68.227245972187,-7.96750002002743,-28.54995));
#234867=CARTESIAN_POINT('Ctrl Pts',(69.7742513559844,-7.96750002002742,
-28.9965319873875));
#234868=CARTESIAN_POINT('Ctrl Pts',(69.7742513559721,-7.96750002002036,
-28.9965319873875));
#234869=CARTESIAN_POINT('Ctrl Pts',(70.5477540478708,-9.3072459821802,-28.54995));
#234870=CARTESIAN_POINT('Ctrl Pts',(71.2176270289503,-10.4675000200274,
-28.54995));
#234871=CARTESIAN_POINT('Origin',(64.00074866408,-7.96750002002747,-32.54995));
#234872=CARTESIAN_POINT('',(64.00074866408,-7.96750002002747,-32.54995));
#234873=CARTESIAN_POINT('',(69.7742513559762,-7.96750002002741,-32.54995));
#234874=CARTESIAN_POINT('Origin',(61.1139973181319,-12.9675000200275,-32.54995));
#234875=CARTESIAN_POINT('',(61.1139973181319,-12.9675000200275,-32.54995));
#234876=CARTESIAN_POINT('Origin',(64.0007486640801,-17.9675000200275,-32.54995));
#234877=CARTESIAN_POINT('',(64.0007486640801,-17.9675000200275,-32.54995));
#234878=CARTESIAN_POINT('Origin',(69.7742513559763,-17.9675000200274,-32.54995));
#234879=CARTESIAN_POINT('',(69.7742513559763,-17.9675000200274,-32.54995));
#234880=CARTESIAN_POINT('Origin',(72.6610027019244,-12.9675000200274,-32.54995));
#234881=CARTESIAN_POINT('',(72.6610027019244,-12.9675000200274,-32.54995));
#234882=CARTESIAN_POINT('Origin',(69.7742513559762,-7.96750002002741,-32.54995));
#234883=CARTESIAN_POINT('Origin',(0.,-25.9350000400563,-32.54995));
#234884=CARTESIAN_POINT('',(2.5,-75.5248730111341,-32.54995));
#234885=CARTESIAN_POINT('',(5.,-79.8550000300563,-32.54995));
#234886=CARTESIAN_POINT('Origin',(1.73472347597681E-15,-79.8550000300563,
-32.54995));
#234887=CARTESIAN_POINT('',(2.5,-84.1851270489785,-32.54995));
#234888=CARTESIAN_POINT('Origin',(1.73472347597681E-15,-79.8550000300563,
-32.54995));
#234889=CARTESIAN_POINT('',(-2.5,-84.1851270489785,-32.54995));
#234890=CARTESIAN_POINT('Origin',(1.73472347597681E-15,-79.8550000300563,
-32.54995));
#234891=CARTESIAN_POINT('',(-5.,-79.8550000300563,-32.54995));
#234892=CARTESIAN_POINT('Origin',(1.73472347597681E-15,-79.8550000300563,
-32.54995));
#234893=CARTESIAN_POINT('',(-2.5,-75.5248730111341,-32.54995));
#234894=CARTESIAN_POINT('Origin',(1.73472347597681E-15,-79.8550000300563,
-32.54995));
#234895=CARTESIAN_POINT('Origin',(1.73472347597681E-15,-79.8550000300563,
-32.54995));
#234896=CARTESIAN_POINT('Origin',(1.73472347597681E-15,-79.8550000300563,
-32.54995));
#234897=CARTESIAN_POINT('',(5.,-82.7417513760044,-31.7764473081038));
#234898=CARTESIAN_POINT('Ctrl Pts',(4.99999999999997,-82.7417513760044,
-31.7764473081038));
#234899=CARTESIAN_POINT('Ctrl Pts',(3.66025403784437,-83.5152540679007,
-32.54995));
#234900=CARTESIAN_POINT('Ctrl Pts',(2.49999999999999,-84.1851270489785,
-32.54995));
#234901=CARTESIAN_POINT('Ctrl Pts',(5.,-79.8550000300563,-32.54995));
#234902=CARTESIAN_POINT('Ctrl Pts',(5.,-81.1947459922119,-32.54995));
#234903=CARTESIAN_POINT('Ctrl Pts',(5.,-82.7417513760044,-31.7764473081038));
#234904=CARTESIAN_POINT('Origin',(1.73472347597681E-15,-79.8550000300563,
-32.54995));
#234905=CARTESIAN_POINT('',(1.66200633571292E-14,-85.6285027219525,-31.7764473081038));
#234906=CARTESIAN_POINT('Ctrl Pts',(2.49999999999999,-84.1851270489785,
-32.54995));
#234907=CARTESIAN_POINT('Ctrl Pts',(1.33974596215563,-84.8550000300563,
-32.54995));
#234908=CARTESIAN_POINT('Ctrl Pts',(6.04428732283895E-14,-85.6285027219525,
-31.7764473081038));
#234909=CARTESIAN_POINT('Ctrl Pts',(-1.4353188893285E-15,-85.6285027219525,
-31.7764473081038));
#234910=CARTESIAN_POINT('Ctrl Pts',(-1.33974596215561,-84.8550000300562,
-32.5499500000001));
#234911=CARTESIAN_POINT('Ctrl Pts',(-2.5,-84.1851270489784,-32.5499500000001));
#234912=CARTESIAN_POINT('Origin',(1.73472347597681E-15,-79.8550000300563,
-32.54995));
#234913=CARTESIAN_POINT('',(-5.,-82.7417513760044,-31.7764473081038));
#234914=CARTESIAN_POINT('Ctrl Pts',(-2.5,-84.1851270489784,-32.5499500000001));
#234915=CARTESIAN_POINT('Ctrl Pts',(-3.66025403784436,-83.5152540679006,
-32.5499500000001));
#234916=CARTESIAN_POINT('Ctrl Pts',(-4.99999999999996,-82.7417513760044,
-31.7764473081038));
#234917=CARTESIAN_POINT('Ctrl Pts',(-5.,-82.7417513760044,-31.7764473081038));
#234918=CARTESIAN_POINT('Ctrl Pts',(-5.,-81.1947459922119,-32.54995));
#234919=CARTESIAN_POINT('Ctrl Pts',(-5.,-79.8550000300563,-32.54995));
#234920=CARTESIAN_POINT('Origin',(1.73472347597681E-15,-79.8550000300563,
-32.54995));
#234921=CARTESIAN_POINT('',(-5.,-76.9682486841082,-31.7764473081038));
#234922=CARTESIAN_POINT('Ctrl Pts',(-5.,-79.8550000300563,-32.54995));
#234923=CARTESIAN_POINT('Ctrl Pts',(-5.,-78.5152540679007,-32.54995));
#234924=CARTESIAN_POINT('Ctrl Pts',(-5.,-76.9682486841082,-31.7764473081038));
#234925=CARTESIAN_POINT('Ctrl Pts',(-4.99999999999992,-76.9682486841082,
-31.7764473081038));
#234926=CARTESIAN_POINT('Ctrl Pts',(-3.66025403784435,-76.1947459922119,
-32.54995));
#234927=CARTESIAN_POINT('Ctrl Pts',(-2.5,-75.5248730111341,-32.54995));
#234928=CARTESIAN_POINT('Origin',(1.73472347597681E-15,-79.8550000300563,
-32.54995));
#234929=CARTESIAN_POINT('',(2.79122613421945E-15,-74.0814973381601,-31.7764473081038));
#234930=CARTESIAN_POINT('Ctrl Pts',(-2.50000000000003,-75.5248730111342,
-32.54995));
#234931=CARTESIAN_POINT('Ctrl Pts',(-1.33974596215564,-74.8550000300563,
-32.54995));
#234932=CARTESIAN_POINT('Ctrl Pts',(-3.65208917395811E-14,-74.0814973381601,
-31.7764473081038));
#234933=CARTESIAN_POINT('Ctrl Pts',(4.00294490246061E-14,-74.0814973381601,
-31.7764473081038));
#234934=CARTESIAN_POINT('Ctrl Pts',(1.33974596215562,-74.8550000300563,
-32.54995));
#234935=CARTESIAN_POINT('Ctrl Pts',(2.49999999999998,-75.5248730111341,
-32.54995));
#234936=CARTESIAN_POINT('Origin',(1.73472347597681E-15,-79.8550000300563,
-32.54995));
#234937=CARTESIAN_POINT('',(5.,-76.9682486841082,-31.7764473081038));
#234938=CARTESIAN_POINT('Ctrl Pts',(2.49999999999997,-75.5248730111341,
-32.5499500000001));
#234939=CARTESIAN_POINT('Ctrl Pts',(3.66025403784435,-76.194745992212,-32.5499500000001));
#234940=CARTESIAN_POINT('Ctrl Pts',(4.99999999999997,-76.9682486841082,
-31.7764473081038));
#234941=CARTESIAN_POINT('Ctrl Pts',(5.,-76.9682486841082,-31.7764473081038));
#234942=CARTESIAN_POINT('Ctrl Pts',(5.,-78.5152540679007,-32.54995));
#234943=CARTESIAN_POINT('Ctrl Pts',(5.,-79.8550000300563,-32.54995));
#234944=CARTESIAN_POINT('Origin',(0.,-25.9350000400563,-28.54995));
#234945=CARTESIAN_POINT('',(5.,-79.8550000300563,-28.54995));
#234946=CARTESIAN_POINT('',(2.5,-84.1851270489785,-28.54995));
#234947=CARTESIAN_POINT('Origin',(1.73472347597681E-15,-79.8550000300563,
-28.54995));
#234948=CARTESIAN_POINT('',(2.5,-75.5248730111341,-28.54995));
#234949=CARTESIAN_POINT('Origin',(1.73472347597681E-15,-79.8550000300563,
-28.54995));
#234950=CARTESIAN_POINT('',(-2.5,-75.5248730111341,-28.54995));
#234951=CARTESIAN_POINT('Origin',(1.73472347597681E-15,-79.8550000300563,
-28.54995));
#234952=CARTESIAN_POINT('',(-5.,-79.8550000300563,-28.54995));
#234953=CARTESIAN_POINT('Origin',(1.73472347597681E-15,-79.8550000300563,
-28.54995));
#234954=CARTESIAN_POINT('',(-2.5,-84.1851270489785,-28.54995));
#234955=CARTESIAN_POINT('Origin',(1.73472347597681E-15,-79.8550000300563,
-28.54995));
#234956=CARTESIAN_POINT('Origin',(1.73472347597681E-15,-79.8550000300563,
-28.54995));
#234957=CARTESIAN_POINT('Origin',(1.73472347597681E-15,-79.8550000300563,
-28.54995));
#234958=CARTESIAN_POINT('',(5.,-76.9682486841079,-28.9965319873851));
#234959=CARTESIAN_POINT('Ctrl Pts',(5.,-76.9682486840998,-28.9965319873876));
#234960=CARTESIAN_POINT('Ctrl Pts',(5.,-78.5152540678973,-28.54995));
#234961=CARTESIAN_POINT('Ctrl Pts',(5.,-79.8550000300563,-28.54995));
#234962=CARTESIAN_POINT('Ctrl Pts',(2.49999999999998,-75.5248730111342,
-28.54995));
#234963=CARTESIAN_POINT('Ctrl Pts',(3.66025403784715,-76.1947459922136,
-28.54995));
#234964=CARTESIAN_POINT('Ctrl Pts',(5.00000000000691,-76.9682486841122,
-28.9965319873875));
#234965=CARTESIAN_POINT('Origin',(1.73472347597681E-15,-79.8550000300563,
-28.54995));
#234966=CARTESIAN_POINT('',(3.91685175604228E-15,-74.0814973381601,-28.9965319873853));
#234967=CARTESIAN_POINT('Ctrl Pts',(-7.07188757544677E-12,-74.081497338156,
-28.9965319873875));
#234968=CARTESIAN_POINT('Ctrl Pts',(1.33974596215276,-74.8550000300547,
-28.54995));
#234969=CARTESIAN_POINT('Ctrl Pts',(2.49999999999998,-75.5248730111342,
-28.54995));
#234970=CARTESIAN_POINT('Ctrl Pts',(-2.49999999999996,-75.5248730111341,
-28.54995));
#234971=CARTESIAN_POINT('Ctrl Pts',(-1.33974596215275,-74.8550000300547,
-28.54995));
#234972=CARTESIAN_POINT('Ctrl Pts',(7.06804165007405E-12,-74.081497338156,
-28.9965319873876));
#234973=CARTESIAN_POINT('Origin',(1.73472347597681E-15,-79.8550000300563,
-28.54995));
#234974=CARTESIAN_POINT('',(-5.,-76.9682486841082,-28.9965319873852));
#234975=CARTESIAN_POINT('Ctrl Pts',(-5.00000000000705,-76.9682486841123,
-28.9965319873875));
#234976=CARTESIAN_POINT('Ctrl Pts',(-3.6602540378472,-76.1947459922136,
-28.54995));
#234977=CARTESIAN_POINT('Ctrl Pts',(-2.49999999999996,-75.5248730111341,
-28.54995));
#234978=CARTESIAN_POINT('Ctrl Pts',(-5.,-79.8550000300563,-28.54995));
#234979=CARTESIAN_POINT('Ctrl Pts',(-5.,-78.5152540678974,-28.54995));
#234980=CARTESIAN_POINT('Ctrl Pts',(-5.,-76.9682486841001,-28.9965319873875));
#234981=CARTESIAN_POINT('Origin',(1.73472347597681E-15,-79.8550000300563,
-28.54995));
#234982=CARTESIAN_POINT('',(-5.,-82.7417513760044,-28.9965319873853));
#234983=CARTESIAN_POINT('Ctrl Pts',(-5.,-82.7417513760125,-28.9965319873876));
#234984=CARTESIAN_POINT('Ctrl Pts',(-5.,-81.1947459922152,-28.54995));
#234985=CARTESIAN_POINT('Ctrl Pts',(-5.,-79.8550000300563,-28.54995));
#234986=CARTESIAN_POINT('Ctrl Pts',(-2.49999999999998,-84.1851270489784,
-28.5499499999999));
#234987=CARTESIAN_POINT('Ctrl Pts',(-3.66025403784722,-83.515254067899,
-28.54995));
#234988=CARTESIAN_POINT('Ctrl Pts',(-5.00000000000709,-82.7417513760002,
-28.9965319873875));
#234989=CARTESIAN_POINT('Origin',(1.73472347597681E-15,-79.8550000300563,
-28.54995));
#234990=CARTESIAN_POINT('',(1.57929637069991E-14,-85.6285027219525,-28.9965319873853));
#234991=CARTESIAN_POINT('Ctrl Pts',(7.10342416350341E-12,-85.6285027219566,
-28.9965319873875));
#234992=CARTESIAN_POINT('Ctrl Pts',(-1.33974596215273,-84.8550000300579,
-28.54995));
#234993=CARTESIAN_POINT('Ctrl Pts',(-2.49999999999995,-84.1851270489784,
-28.5499499999999));
#234994=CARTESIAN_POINT('Ctrl Pts',(2.49999999999998,-84.1851270489785,
-28.54995));
#234995=CARTESIAN_POINT('Ctrl Pts',(1.33974596215279,-84.8550000300579,
-28.54995));
#234996=CARTESIAN_POINT('Ctrl Pts',(-7.00830160928372E-12,-85.6285027219566,
-28.9965319873875));
#234997=CARTESIAN_POINT('Origin',(1.73472347597681E-15,-79.8550000300563,
-28.54995));
#234998=CARTESIAN_POINT('',(5.,-82.7417513760044,-28.9965319873853));
#234999=CARTESIAN_POINT('Ctrl Pts',(5.,-79.8550000300563,-28.54995));
#235000=CARTESIAN_POINT('Ctrl Pts',(5.,-81.1947459922152,-28.54995));
#235001=CARTESIAN_POINT('Ctrl Pts',(5.,-82.7417513760126,-28.9965319873876));
#235002=CARTESIAN_POINT('Ctrl Pts',(5.00000000000707,-82.7417513760004,
-28.9965319873876));
#235003=CARTESIAN_POINT('Ctrl Pts',(3.66025403784723,-83.515254067899,-28.54995));
#235004=CARTESIAN_POINT('Ctrl Pts',(2.50000000000001,-84.1851270489785,
-28.54995));
#235005=CARTESIAN_POINT('Origin',(5.,-76.9682486841082,-32.54995));
#235006=CARTESIAN_POINT('',(5.,-76.9682486841082,-32.54995));
#235007=CARTESIAN_POINT('',(5.,-82.7417513760044,-32.54995));
#235008=CARTESIAN_POINT('Origin',(3.63207727782644E-15,-74.0814973381601,
-32.54995));
#235009=CARTESIAN_POINT('',(3.63207727782644E-15,-74.0814973381601,-32.54995));
#235010=CARTESIAN_POINT('Origin',(-5.,-76.9682486841082,-32.54995));
#235011=CARTESIAN_POINT('',(-5.,-76.9682486841082,-32.54995));
#235012=CARTESIAN_POINT('Origin',(-5.,-82.7417513760044,-32.54995));
#235013=CARTESIAN_POINT('',(-5.,-82.7417513760044,-32.54995));
#235014=CARTESIAN_POINT('Origin',(1.56125112837912E-14,-85.6285027219525,
-32.54995));
#235015=CARTESIAN_POINT('',(1.56125112837912E-14,-85.6285027219525,-32.54995));
#235016=CARTESIAN_POINT('Origin',(5.,-82.7417513760044,-32.54995));
#235017=CARTESIAN_POINT('Origin',(-47.392180948596,-60.9300389954978,-220.195349461621));
#235018=CARTESIAN_POINT('',(-47.392180948596,-60.9300389954978,-221.195349461621));
#235019=CARTESIAN_POINT('',(-47.392180948596,-60.9300389954978,-223.85005));
#235020=CARTESIAN_POINT('',(-47.392180948596,-60.9300389954978,-220.195349461621));
#235021=CARTESIAN_POINT('',(-48.892180948596,-60.0640135917134,-221.195349461621));
#235022=CARTESIAN_POINT('Ctrl Pts',(-48.8921809485959,-60.0640135917134,
-221.195349461621));
#235023=CARTESIAN_POINT('Ctrl Pts',(-48.142180948596,-60.4970262936056,
-220.945349461621));
#235024=CARTESIAN_POINT('Ctrl Pts',(-47.3921809485963,-60.9300389954976,
-221.195349461621));
#235025=CARTESIAN_POINT('',(-48.892180948596,-60.0640135917134,-223.85005));
#235026=CARTESIAN_POINT('',(-48.892180948596,-60.0640135917134,-220.195349461621));
#235027=CARTESIAN_POINT('Ctrl Pts',(-47.392180948596,-60.9300389954978,
-223.85005));
#235028=CARTESIAN_POINT('Ctrl Pts',(-48.142180948596,-60.4970262936056,
-223.417037298108));
#235029=CARTESIAN_POINT('Ctrl Pts',(-48.892180948596,-60.0640135917134,
-223.85005));
#235030=CARTESIAN_POINT('Origin',(-47.392180948596,-62.6620898030667,-220.195349461621));
#235031=CARTESIAN_POINT('',(-47.392180948596,-62.6620898030667,-221.195349461621));
#235032=CARTESIAN_POINT('',(-47.392180948596,-62.6620898030667,-223.85005));
#235033=CARTESIAN_POINT('',(-47.392180948596,-62.6620898030667,-220.195349461621));
#235034=CARTESIAN_POINT('Ctrl Pts',(-47.392180948596,-60.9300389954979,
-221.195349461621));
#235035=CARTESIAN_POINT('Ctrl Pts',(-47.392180948596,-61.7960643992822,
-220.945349461621));
#235036=CARTESIAN_POINT('Ctrl Pts',(-47.392180948596,-62.6620898030664,
-221.195349461621));
#235037=CARTESIAN_POINT('Ctrl Pts',(-47.392180948596,-62.6620898030667,
-223.85005));
#235038=CARTESIAN_POINT('Ctrl Pts',(-47.392180948596,-61.7960643992823,
-223.417037298108));
#235039=CARTESIAN_POINT('Ctrl Pts',(-47.392180948596,-60.9300389954978,
-223.85005));
#235040=CARTESIAN_POINT('Origin',(-48.892180948596,-63.5281152068512,-220.195349461621));
#235041=CARTESIAN_POINT('',(-48.892180948596,-63.5281152068512,-221.195349461621));
#235042=CARTESIAN_POINT('',(-48.892180948596,-63.5281152068512,-223.85005));
#235043=CARTESIAN_POINT('',(-48.892180948596,-63.5281152068512,-220.195349461621));
#235044=CARTESIAN_POINT('Ctrl Pts',(-47.392180948596,-62.6620898030668,
-221.195349461621));
#235045=CARTESIAN_POINT('Ctrl Pts',(-48.142180948596,-63.095102504959,-220.945349461621));
#235046=CARTESIAN_POINT('Ctrl Pts',(-48.8921809485959,-63.5281152068512,
-221.195349461621));
#235047=CARTESIAN_POINT('Ctrl Pts',(-48.892180948596,-63.5281152068512,
-223.85005));
#235048=CARTESIAN_POINT('Ctrl Pts',(-48.142180948596,-63.095102504959,-223.417037298108));
#235049=CARTESIAN_POINT('Ctrl Pts',(-47.392180948596,-62.6620898030667,
-223.85005));
#235050=CARTESIAN_POINT('Origin',(-50.392180948596,-62.6620898030667,-220.195349461621));
#235051=CARTESIAN_POINT('',(-50.392180948596,-62.6620898030677,-221.19534946162));
#235052=CARTESIAN_POINT('',(-50.392180948596,-62.6620898030667,-223.85005));
#235053=CARTESIAN_POINT('',(-50.392180948596,-62.6620898030667,-220.195349461621));
#235054=CARTESIAN_POINT('Ctrl Pts',(-48.892180948596,-63.5281152068511,
-221.195349461621));
#235055=CARTESIAN_POINT('Ctrl Pts',(-49.6421809485958,-63.095102504959,
-220.945349461621));
#235056=CARTESIAN_POINT('Ctrl Pts',(-50.3921809485956,-62.662089803067,
-221.195349461621));
#235057=CARTESIAN_POINT('Ctrl Pts',(-50.392180948596,-62.6620898030667,
-223.85005));
#235058=CARTESIAN_POINT('Ctrl Pts',(-49.642180948596,-63.0951025049589,
-223.417037298108));
#235059=CARTESIAN_POINT('Ctrl Pts',(-48.892180948596,-63.5281152068512,
-223.85005));
#235060=CARTESIAN_POINT('Origin',(-50.392180948596,-60.9300389954978,-220.195349461621));
#235061=CARTESIAN_POINT('',(-50.392180948596,-60.9300389954978,-221.195349461621));
#235062=CARTESIAN_POINT('',(-50.392180948596,-60.9300389954978,-223.85005));
#235063=CARTESIAN_POINT('',(-50.392180948596,-60.9300389954978,-220.195349461621));
#235064=CARTESIAN_POINT('Ctrl Pts',(-50.392180948596,-62.6620898030674,
-221.195349461621));
#235065=CARTESIAN_POINT('Ctrl Pts',(-50.392180948596,-61.7960643992827,
-220.945349461621));
#235066=CARTESIAN_POINT('Ctrl Pts',(-50.392180948596,-60.9300389954982,
-221.195349461621));
#235067=CARTESIAN_POINT('Ctrl Pts',(-50.392180948596,-60.9300389954978,
-223.85005));
#235068=CARTESIAN_POINT('Ctrl Pts',(-50.392180948596,-61.7960643992823,
-223.417037298108));
#235069=CARTESIAN_POINT('Ctrl Pts',(-50.392180948596,-62.6620898030667,
-223.85005));
#235070=CARTESIAN_POINT('Origin',(-48.892180948596,-60.0640135917134,-220.195349461621));
#235071=CARTESIAN_POINT('Ctrl Pts',(-50.392180948596,-60.9300389954978,
-221.195349461621));
#235072=CARTESIAN_POINT('Ctrl Pts',(-49.642180948596,-60.4970262936056,
-220.945349461621));
#235073=CARTESIAN_POINT('Ctrl Pts',(-48.8921809485959,-60.0640135917133,
-221.195349461621));
#235074=CARTESIAN_POINT('Ctrl Pts',(-48.892180948596,-60.0640135917134,
-223.85005));
#235075=CARTESIAN_POINT('Ctrl Pts',(-49.642180948596,-60.4970262936056,
-223.417037298108));
#235076=CARTESIAN_POINT('Ctrl Pts',(-50.392180948596,-60.9300389954978,
-223.85005));
#235077=CARTESIAN_POINT('Origin',(-48.892180948596,-61.7960643992823,-221.35005));
#235078=CARTESIAN_POINT('',(-48.892180948596,-61.7960643992823,-220.195349461621));
#235079=CARTESIAN_POINT('',(-48.892180948596,-63.7960643992823,-221.35005));
#235080=CARTESIAN_POINT('Origin',(-48.892180948596,-61.7960643992823,-223.85005));
#235081=CARTESIAN_POINT('Origin',(-48.892180948596,-61.7960643992823,-223.85005));
#235082=CARTESIAN_POINT('Origin',(-48.892180948596,-61.7960643992823,-223.85005));
#235083=CARTESIAN_POINT('Origin',(-48.892180948596,-61.7960643992823,-223.85005));
#235084=CARTESIAN_POINT('Origin',(-48.892180948596,-61.7960643992823,-223.85005));
#235085=CARTESIAN_POINT('Origin',(-48.892180948596,-61.7960643992823,-223.85005));
#235086=CARTESIAN_POINT('Origin',(-48.892180948596,-61.7960643992823,-223.85005));
#235087=CARTESIAN_POINT('Origin',(-48.892180948596,-61.7960643992823,-223.85005));
#235088=CARTESIAN_POINT('Origin',(-48.892180948596,-61.7960643992823,-223.85005));
#235089=CARTESIAN_POINT('Origin',(-48.892180948596,-61.7960643992823,-223.85005));
#235090=CARTESIAN_POINT('Origin',(-48.892180948596,-61.7960643992823,-223.85005));
#235091=CARTESIAN_POINT('Origin',(-48.892180948596,-61.7960643992823,-223.85005));
#235092=CARTESIAN_POINT('Origin',(-48.892180948596,-61.7960643992823,-223.60005));
#235093=CARTESIAN_POINT('',(-48.892180948596,-64.7960643992823,-223.85005));
#235094=CARTESIAN_POINT('Origin',(-48.892180948596,-61.7960643992823,-223.85005));
#235095=CARTESIAN_POINT('',(-48.892180948596,-65.0460643992823,-223.60005));
#235096=CARTESIAN_POINT('Origin',(-48.892180948596,-64.7960643992823,-223.60005));
#235097=CARTESIAN_POINT('',(-48.892180948596,-58.5460643992823,-223.60005));
#235098=CARTESIAN_POINT('Origin',(-48.892180948596,-61.7960643992823,-223.60005));
#235099=CARTESIAN_POINT('Origin',(-48.892180948596,-61.7960643992823,-223.60005));
#235100=CARTESIAN_POINT('Origin',(-48.892180948596,-61.7960643992823,-218.35005));
#235101=CARTESIAN_POINT('',(-48.892180948596,-58.5460643992823,-218.35005));
#235102=CARTESIAN_POINT('Origin',(-48.892180948596,-61.7960643992823,-218.35005));
#235103=CARTESIAN_POINT('Origin',(-48.892180948596,-61.7960643992823,-223.85005));
#235104=CARTESIAN_POINT('Origin',(-48.892180948596,-61.7960643992823,-223.85005));
#235105=CARTESIAN_POINT('',(-48.892180948596,-58.5460643992823,-223.85005));
#235106=CARTESIAN_POINT('Origin',(-14.75,97.3100982187845,-189.413464213672));
#235107=CARTESIAN_POINT('',(-14.,96.9977203019102,-189.84995));
#235108=CARTESIAN_POINT('',(-14.75,97.9199999800001,-189.84995));
#235109=CARTESIAN_POINT('Origin',(-14.7499999999998,96.9977203019109,-189.84995));
#235110=CARTESIAN_POINT('',(-14.,97.9199999800002,-188.561248242419));
#235111=CARTESIAN_POINT('Origin',(-14.7499999999994,97.9199999800002,-188.56124824242));
#235112=CARTESIAN_POINT('',(-14.,-43.3014970868467,-385.890101736374));
#235113=CARTESIAN_POINT('Origin',(-14.75,97.3100982187848,-80.2864357863281));
#235114=CARTESIAN_POINT('',(-14.,97.5344695959176,-80.59995));
#235115=CARTESIAN_POINT('',(-14.,97.9199999800001,-81.1386517575809));
#235116=CARTESIAN_POINT('',(-14.,-43.3014970868374,116.19020173637));
#235117=CARTESIAN_POINT('',(-14.1688463988223,97.9199999800001,-80.3240391180339));
#235118=CARTESIAN_POINT('Origin',(-14.7500000000031,97.9199999800002,-81.138651757583));
#235119=CARTESIAN_POINT('Origin',(-14.75,97.5344695959176,-80.59995));
#235120=CARTESIAN_POINT('Origin',(-14.75,97.5344695959176,-80.59995));
#235121=CARTESIAN_POINT('',(-14.75,97.9199999800001,-79.9566255694448));
#235122=CARTESIAN_POINT('Origin',(-14.75,97.9199999800001,-80.59995));
#235123=CARTESIAN_POINT('',(-14.75,97.5344695959176,-79.84995));
#235124=CARTESIAN_POINT('Origin',(-14.75,97.5344695959176,-80.59995));
#235125=CARTESIAN_POINT('Origin',(-14.75,97.5344695959176,-80.59995));
#235126=CARTESIAN_POINT('Origin',(48.,97.5344695959176,-80.59995));
#235127=CARTESIAN_POINT('',(-40.9309791607344,97.9199999800001,-79.9566255694448));
#235128=CARTESIAN_POINT('',(48.,97.9199999800001,-79.9566255694448));
#235129=CARTESIAN_POINT('',(-40.9309791607344,97.5344695959176,-79.84995));
#235130=CARTESIAN_POINT('Origin',(-40.9309791607344,97.5344695959176,-80.59995));
#235131=CARTESIAN_POINT('',(48.,97.5344695959176,-79.84995));
#235132=CARTESIAN_POINT('Origin',(-40.9309791607344,97.5344695959176,-80.59995));
#235133=CARTESIAN_POINT('',(-41.2284392666181,97.9199999800001,-80.0295257645779));
#235134=CARTESIAN_POINT('Origin',(-40.9309791607344,97.9199999800001,-80.59995));
#235135=CARTESIAN_POINT('Origin',(-40.9309791607344,97.5344695959176,-80.59995));
#235136=CARTESIAN_POINT('Origin',(-57.25,98.9199999800001,-173.84995));
#235137=CARTESIAN_POINT('',(-57.8072469207768,97.9199999800001,-173.103241263434));
#235138=CARTESIAN_POINT('',(-58.,97.5177878719661,-172.802905968413));
#235139=CARTESIAN_POINT('Origin',(-57.25,97.5177878719661,-172.802905968413));
#235140=CARTESIAN_POINT('',(-57.25,97.9199999800001,-173.84995));
#235141=CARTESIAN_POINT('Ctrl Pts',(-57.8072469207768,97.9199999800001,
-173.103241263434));
#235142=CARTESIAN_POINT('Ctrl Pts',(-57.6651860234659,97.9199999800001,
-173.36682332955));
#235143=CARTESIAN_POINT('Ctrl Pts',(-57.4409434098566,97.9199999800001,
-173.629467541839));
#235144=CARTESIAN_POINT('Ctrl Pts',(-57.25,97.9199999800001,-173.84995));
#235145=CARTESIAN_POINT('',(-58.,97.1699999800001,-173.84995));
#235146=CARTESIAN_POINT('Origin',(-57.25,97.1699999800001,-173.84995));
#235147=CARTESIAN_POINT('Origin',(-58.,98.9199999800001,-173.84995));
#235148=CARTESIAN_POINT('Origin',(-57.25,97.5177878719661,-172.802905968413));
#235149=CARTESIAN_POINT('',(-57.8822667063023,97.9199999800001,-172.833958057747));
#235150=CARTESIAN_POINT('Origin',(-57.25,97.5177878719661,-172.802905968413));
#235151=CARTESIAN_POINT('Origin',(-57.25,97.9199999800001,-172.802905968413));
#235152=CARTESIAN_POINT('Origin',(-57.25,-394.08000002,-134.84995));
#235153=CARTESIAN_POINT('',(-58.,97.9199999800001,-167.173500656049));
#235154=CARTESIAN_POINT('Origin',(-58.,-394.08000002,-134.84995));
#235155=CARTESIAN_POINT('Ctrl Pts',(-58.,97.9199999800002,-167.173500656049));
#235156=CARTESIAN_POINT('Ctrl Pts',(-58.,97.9199999800002,-168.594527486982));
#235157=CARTESIAN_POINT('Ctrl Pts',(-57.9835908722536,97.9199999800001,
-170.15643772184));
#235158=CARTESIAN_POINT('Ctrl Pts',(-57.9159202399799,97.9199999800001,
-172.088208331578));
#235159=CARTESIAN_POINT('Ctrl Pts',(-57.9005229085552,97.9199999800001,
-172.462234637024));
#235160=CARTESIAN_POINT('Ctrl Pts',(-57.8822667063024,97.9199999800001,
-172.833958057747));
#235161=CARTESIAN_POINT('Origin',(-57.25,-394.08000002,-134.84995));
#235162=CARTESIAN_POINT('',(-57.8822667063027,97.9199999800001,-96.8659419422532));
#235163=CARTESIAN_POINT('',(-58.,97.5177878719661,-96.8969940315874));
#235164=CARTESIAN_POINT('Origin',(-57.25,97.5177878719661,-96.8969940315874));
#235165=CARTESIAN_POINT('',(-58.,97.9199999800001,-102.526399343951));
#235166=CARTESIAN_POINT('Ctrl Pts',(-57.8822667063024,97.9199999800001,
-96.8659419422532));
#235167=CARTESIAN_POINT('Ctrl Pts',(-57.9005229085552,97.9199999800001,
-97.2376653629762));
#235168=CARTESIAN_POINT('Ctrl Pts',(-57.9159202399799,97.9199999800001,
-97.6116916684221));
#235169=CARTESIAN_POINT('Ctrl Pts',(-57.9835908722536,97.9199999800001,
-99.5434622781595));
#235170=CARTESIAN_POINT('Ctrl Pts',(-58.,97.9199999800002,-101.105372513018));
#235171=CARTESIAN_POINT('Ctrl Pts',(-58.,97.9199999800002,-102.526399343951));
#235172=CARTESIAN_POINT('Origin',(-58.,-394.08000002,-134.84995));
#235173=CARTESIAN_POINT('Origin',(-57.25,97.5177878719661,-96.8969940315875));
#235174=CARTESIAN_POINT('',(-57.8072469207768,97.9199999800001,-96.5966587365659));
#235175=CARTESIAN_POINT('Origin',(-57.25,97.5177878719662,-96.8969940315876));
#235176=CARTESIAN_POINT('Origin',(-57.25,97.9199999800001,-96.8969940315875));
#235177=CARTESIAN_POINT('Origin',(-57.25,98.9199999800001,-95.84995));
#235178=CARTESIAN_POINT('',(-57.25,97.9199999800001,-95.84995));
#235179=CARTESIAN_POINT('',(-58.,97.1699999800001,-95.84995));
#235180=CARTESIAN_POINT('Origin',(-57.25,97.1699999800001,-95.84995));
#235181=CARTESIAN_POINT('Ctrl Pts',(-57.25,97.9199999800001,-95.84995));
#235182=CARTESIAN_POINT('Ctrl Pts',(-57.4409434098566,97.9199999800001,
-96.0704324581614));
#235183=CARTESIAN_POINT('Ctrl Pts',(-57.6651860234659,97.9199999800001,
-96.3330766704501));
#235184=CARTESIAN_POINT('Ctrl Pts',(-57.8072469207768,97.9199999800001,
-96.5966587365659));
#235185=CARTESIAN_POINT('Origin',(-58.,98.9199999800001,-95.84995));
#235186=CARTESIAN_POINT('Origin',(-42.,98.9199999800001,-189.09995));
#235187=CARTESIAN_POINT('',(-42.,97.1699999800001,-189.84995));
#235188=CARTESIAN_POINT('',(-42.,97.9199999800001,-189.09995));
#235189=CARTESIAN_POINT('Origin',(-42.,97.1699999800001,-189.09995));
#235190=CARTESIAN_POINT('',(-40.5638593383655,97.9199999800001,-189.84995));
#235191=CARTESIAN_POINT('Ctrl Pts',(-42.,97.9199999800001,-189.09995));
#235192=CARTESIAN_POINT('Ctrl Pts',(-41.7587302410591,97.9199999800001,
-189.308895740408));
#235193=CARTESIAN_POINT('Ctrl Pts',(-41.4659359584444,97.9199999800001,
-189.555803560147));
#235194=CARTESIAN_POINT('Ctrl Pts',(-40.9977084033149,97.9199999800001,
-189.783413418928));
#235195=CARTESIAN_POINT('Ctrl Pts',(-40.7653076296235,97.9199999800001,
-189.84995));
#235196=CARTESIAN_POINT('Ctrl Pts',(-40.5638593383655,97.9199999800001,
-189.84995));
#235197=CARTESIAN_POINT('Origin',(-42.,98.9199999800001,-189.84995));
#235198=CARTESIAN_POINT('Origin',(-42.,98.9199999800001,-80.59995));
#235199=CARTESIAN_POINT('',(-42.,97.9199999800001,-80.59995));
#235200=CARTESIAN_POINT('Ctrl Pts',(-41.2284392666181,97.9199999800001,
-80.0295257645779));
#235201=CARTESIAN_POINT('Ctrl Pts',(-41.500014913968,97.9199999800001,-80.1711447838968));
#235202=CARTESIAN_POINT('Ctrl Pts',(-41.7725853995754,97.9199999800001,
-80.4030031788408));
#235203=CARTESIAN_POINT('Ctrl Pts',(-42.,97.9199999800001,-80.59995));
#235204=CARTESIAN_POINT('',(-42.,97.1699999800001,-79.84995));
#235205=CARTESIAN_POINT('Origin',(-42.,97.1699999800001,-80.59995));
#235206=CARTESIAN_POINT('Origin',(-42.,98.9199999800001,-79.84995));
#235207=CARTESIAN_POINT('Origin',(-13.5,-43.9113988480613,-385.453615950046));
#235208=CARTESIAN_POINT('',(-13.5,97.9199999800001,-186.413411979785));
#235209=CARTESIAN_POINT('',(-14.,97.9199999800001,-187.272546484838));
#235210=CARTESIAN_POINT('Origin',(-13.5000000000102,97.9199999800001,-187.272546484832));
#235211=CARTESIAN_POINT('',(-13.5,95.460587505094,-189.84995));
#235212=CARTESIAN_POINT('',(-13.5,91.2935952834256,-195.672489873167));
#235213=CARTESIAN_POINT('',(-14.,96.0754406238205,-189.84995));
#235214=CARTESIAN_POINT('Origin',(-13.4999999999996,96.0754406238209,-189.84995));
#235215=CARTESIAN_POINT('',(-14.,-43.9113988480614,-385.453615950046));
#235216=CARTESIAN_POINT('Origin',(-13.5,-43.9113988480525,115.753715950042));
#235217=CARTESIAN_POINT('',(-14.,97.9199999800001,-82.4273535151615));
#235218=CARTESIAN_POINT('',(-13.5,97.9199999800001,-83.2864880202152));
#235219=CARTESIAN_POINT('Origin',(-13.5000000000003,97.9199999800001,-82.4273535151615));
#235220=CARTESIAN_POINT('',(-14.,96.612189917828,-80.59995));
#235221=CARTESIAN_POINT('',(-14.,-43.9113988480525,115.753715950042));
#235222=CARTESIAN_POINT('',(-13.5,95.6849588822271,-80.1634642136719));
#235223=CARTESIAN_POINT('Ctrl Pts',(-13.5,95.6849588822271,-80.1634642136719));
#235224=CARTESIAN_POINT('Ctrl Pts',(-13.5654616428729,95.6849588822324,
-80.1634642136793));
#235225=CARTESIAN_POINT('Ctrl Pts',(-13.6308739481793,95.7090922288018,
-80.1748247725308));
#235226=CARTESIAN_POINT('Ctrl Pts',(-13.7518094841857,95.8019880554524,
-80.2185546590279));
#235227=CARTESIAN_POINT('Ctrl Pts',(-13.8072733639181,95.8707140107035,
-80.2509067929251));
#235228=CARTESIAN_POINT('Ctrl Pts',(-13.8998334172684,96.0423631189524,
-80.3317090882667));
#235229=CARTESIAN_POINT('Ctrl Pts',(-13.9368931960372,96.1452187774359,
-80.3801274772601));
#235230=CARTESIAN_POINT('Ctrl Pts',(-13.9869863364741,96.3694891476217,
-80.4857007649587));
#235231=CARTESIAN_POINT('Ctrl Pts',(-14.,96.4907937818967,-80.542803845684));
#235232=CARTESIAN_POINT('Ctrl Pts',(-14.,96.612189917828,-80.59995));
#235233=CARTESIAN_POINT('',(-13.5,91.2935952834259,-74.0274101268328));
#235234=CARTESIAN_POINT('Origin',(-14.,-394.08000002,-134.84995));
#235235=CARTESIAN_POINT('',(-14.,97.9199999800001,-134.84995));
#235236=CARTESIAN_POINT('',(-14.,-394.08000002,-80.59995));
#235237=CARTESIAN_POINT('Origin',(-14.,-394.08000002,-134.84995));
#235238=CARTESIAN_POINT('',(-14.,97.9199999800001,-134.84995));
#235239=CARTESIAN_POINT('',(-14.,105.91999998,-189.84995));
#235240=CARTESIAN_POINT('Origin',(-58.,105.91999998,-86.84995));
#235241=CARTESIAN_POINT('',(-58.,97.9199999800001,-182.84995));
#235242=CARTESIAN_POINT('',(-58.,97.1699999800001,-182.84995));
#235243=CARTESIAN_POINT('',(-58.,97.1699999800001,-173.84995));
#235244=CARTESIAN_POINT('',(-58.,94.4199999800001,-182.84995));
#235245=CARTESIAN_POINT('',(-58.,105.91999998,-182.84995));
#235246=CARTESIAN_POINT('',(-58.,94.4199999800001,-86.84995));
#235247=CARTESIAN_POINT('',(-58.,94.4199999800001,-86.84995));
#235248=CARTESIAN_POINT('',(-58.,97.1699999800001,-86.84995));
#235249=CARTESIAN_POINT('',(-58.,105.91999998,-86.84995));
#235250=CARTESIAN_POINT('',(-58.,97.1699999800001,-86.84995));
#235251=CARTESIAN_POINT('Origin',(11.75,97.3100982187845,-189.413464213672));
#235252=CARTESIAN_POINT('',(11.,97.9199999800002,-188.561248242419));
#235253=CARTESIAN_POINT('',(11.,96.9977203019102,-189.84995));
#235254=CARTESIAN_POINT('',(11.,-43.3014970868467,-385.890101736374));
#235255=CARTESIAN_POINT('',(11.75,97.9199999800001,-189.84995));
#235256=CARTESIAN_POINT('Origin',(11.7499999999996,97.9199999800003,-188.56124824242));
#235257=CARTESIAN_POINT('Origin',(11.7499999999998,96.9977203019108,-189.84995));
#235258=CARTESIAN_POINT('Origin',(11.75,97.3100982187848,-80.2864357863281));
#235259=CARTESIAN_POINT('',(11.,97.5344695959176,-80.59995));
#235260=CARTESIAN_POINT('',(11.1688463988223,97.9199999800001,-80.3240391180339));
#235261=CARTESIAN_POINT('Origin',(11.75,97.5344695959176,-80.59995));
#235262=CARTESIAN_POINT('',(11.,97.9199999800001,-81.1386517575809));
#235263=CARTESIAN_POINT('Origin',(11.7500000000205,97.9199999800002,-81.1386517575926));
#235264=CARTESIAN_POINT('',(11.,-43.3014970868374,116.19020173637));
#235265=CARTESIAN_POINT('Origin',(11.75,97.5344695959176,-80.59995));
#235266=CARTESIAN_POINT('',(11.75,97.5344695959176,-79.84995));
#235267=CARTESIAN_POINT('',(11.75,97.9199999800001,-79.9566255694448));
#235268=CARTESIAN_POINT('Origin',(11.75,97.5344695959176,-80.59995));
#235269=CARTESIAN_POINT('Origin',(11.75,97.9199999800001,-80.59995));
#235270=CARTESIAN_POINT('Origin',(11.75,97.5344695959176,-80.59995));
#235271=CARTESIAN_POINT('Origin',(-51.,97.5344695959176,-80.59995));
#235272=CARTESIAN_POINT('',(37.9309791607343,97.5344695959176,-79.84995));
#235273=CARTESIAN_POINT('',(37.9309791607343,97.9199999800001,-79.9566255694448));
#235274=CARTESIAN_POINT('Origin',(37.9309791607343,97.5344695959176,-80.59995));
#235275=CARTESIAN_POINT('',(-51.,97.9199999800001,-79.9566255694448));
#235276=CARTESIAN_POINT('',(-51.,97.5344695959176,-79.84995));
#235277=CARTESIAN_POINT('Origin',(37.9309791607343,97.5344695959176,-80.59995));
#235278=CARTESIAN_POINT('',(38.2284392666181,97.9199999800001,-80.0295257645779));
#235279=CARTESIAN_POINT('Origin',(37.9309791607343,97.5344695959176,-80.59995));
#235280=CARTESIAN_POINT('Origin',(37.9309791607343,97.9199999800001,-80.59995));
#235281=CARTESIAN_POINT('Origin',(54.25,98.9199999800001,-173.84995));
#235282=CARTESIAN_POINT('',(55.,97.1699999800001,-173.84995));
#235283=CARTESIAN_POINT('',(54.25,97.9199999800001,-173.84995));
#235284=CARTESIAN_POINT('Origin',(54.25,97.1699999800001,-173.84995));
#235285=CARTESIAN_POINT('',(54.8072469207768,97.9199999800001,-173.103241263434));
#235286=CARTESIAN_POINT('Ctrl Pts',(54.25,97.9199999800001,-173.84995));
#235287=CARTESIAN_POINT('Ctrl Pts',(54.4409434098567,97.9199999800001,-173.629467541839));
#235288=CARTESIAN_POINT('Ctrl Pts',(54.6651860234659,97.9199999800001,-173.36682332955));
#235289=CARTESIAN_POINT('Ctrl Pts',(54.8072469207768,97.9199999800001,-173.103241263434));
#235290=CARTESIAN_POINT('',(55.,97.5177878719661,-172.802905968413));
#235291=CARTESIAN_POINT('Origin',(54.25,97.5177878719661,-172.802905968413));
#235292=CARTESIAN_POINT('Origin',(55.,98.9199999800001,-173.84995));
#235293=CARTESIAN_POINT('Origin',(54.25,97.5177878719661,-172.802905968413));
#235294=CARTESIAN_POINT('',(54.8822667063023,97.9199999800001,-172.833958057747));
#235295=CARTESIAN_POINT('Origin',(54.25,97.9199999800001,-172.802905968413));
#235296=CARTESIAN_POINT('Origin',(54.25,97.5177878719661,-172.802905968413));
#235297=CARTESIAN_POINT('Origin',(54.25,-394.08000002,-134.84995));
#235298=CARTESIAN_POINT('',(55.,97.9199999800001,-167.173500656049));
#235299=CARTESIAN_POINT('Ctrl Pts',(54.8822667063024,97.9199999800001,-172.833958057747));
#235300=CARTESIAN_POINT('Ctrl Pts',(54.9005229085552,97.9199999800001,-172.462234637024));
#235301=CARTESIAN_POINT('Ctrl Pts',(54.9159202399799,97.9199999800001,-172.088208331578));
#235302=CARTESIAN_POINT('Ctrl Pts',(54.9835908722536,97.9199999800001,-170.15643772184));
#235303=CARTESIAN_POINT('Ctrl Pts',(55.,97.9199999800002,-168.594527486982));
#235304=CARTESIAN_POINT('Ctrl Pts',(55.,97.9199999800002,-167.173500656049));
#235305=CARTESIAN_POINT('Origin',(55.,-394.08000002,-134.84995));
#235306=CARTESIAN_POINT('Origin',(54.25,-394.08000002,-134.84995));
#235307=CARTESIAN_POINT('',(55.,97.9199999800001,-102.526399343951));
#235308=CARTESIAN_POINT('',(55.,97.5177878719661,-96.8969940315874));
#235309=CARTESIAN_POINT('Origin',(55.,-394.08000002,-134.84995));
#235310=CARTESIAN_POINT('',(54.8822667063027,97.9199999800001,-96.8659419422532));
#235311=CARTESIAN_POINT('Ctrl Pts',(55.,97.9199999800002,-102.526399343951));
#235312=CARTESIAN_POINT('Ctrl Pts',(55.,97.9199999800002,-101.105372513018));
#235313=CARTESIAN_POINT('Ctrl Pts',(54.9835908722536,97.9199999800001,-99.5434622781595));
#235314=CARTESIAN_POINT('Ctrl Pts',(54.9159202399799,97.9199999800001,-97.6116916684221));
#235315=CARTESIAN_POINT('Ctrl Pts',(54.9005229085552,97.9199999800001,-97.2376653629761));
#235316=CARTESIAN_POINT('Ctrl Pts',(54.8822667063024,97.9199999800001,-96.8659419422532));
#235317=CARTESIAN_POINT('Origin',(54.25,97.5177878719661,-96.8969940315874));
#235318=CARTESIAN_POINT('Origin',(54.25,97.5177878719661,-96.8969940315875));
#235319=CARTESIAN_POINT('',(54.8072469207768,97.9199999800001,-96.5966587365659));
#235320=CARTESIAN_POINT('Origin',(54.25,97.9199999800001,-96.8969940315875));
#235321=CARTESIAN_POINT('Origin',(54.25,97.5177878719662,-96.8969940315876));
#235322=CARTESIAN_POINT('Origin',(54.25,98.9199999800001,-95.84995));
#235323=CARTESIAN_POINT('',(54.25,97.9199999800001,-95.84995));
#235324=CARTESIAN_POINT('Ctrl Pts',(54.8072469207768,97.9199999800001,-96.5966587365659));
#235325=CARTESIAN_POINT('Ctrl Pts',(54.6651860234659,97.9199999800001,-96.3330766704501));
#235326=CARTESIAN_POINT('Ctrl Pts',(54.4409434098566,97.9199999800001,-96.0704324581614));
#235327=CARTESIAN_POINT('Ctrl Pts',(54.25,97.9199999800001,-95.84995));
#235328=CARTESIAN_POINT('',(55.,97.1699999800001,-95.84995));
#235329=CARTESIAN_POINT('Origin',(54.25,97.1699999800001,-95.84995));
#235330=CARTESIAN_POINT('Origin',(55.,98.9199999800001,-95.84995));
#235331=CARTESIAN_POINT('Origin',(39.,98.9199999800001,-189.09995));
#235332=CARTESIAN_POINT('',(37.5638593383657,97.9199999800001,-189.84995));
#235333=CARTESIAN_POINT('',(39.,97.1699999800001,-189.84995));
#235334=CARTESIAN_POINT('Origin',(39.,98.9199999800001,-189.84995));
#235335=CARTESIAN_POINT('',(39.,97.9199999800001,-189.09995));
#235336=CARTESIAN_POINT('Ctrl Pts',(37.5638593383655,97.9199999800001,-189.84995));
#235337=CARTESIAN_POINT('Ctrl Pts',(37.7653076296235,97.9199999800001,-189.84995));
#235338=CARTESIAN_POINT('Ctrl Pts',(37.9977084033149,97.9199999800001,-189.783413418928));
#235339=CARTESIAN_POINT('Ctrl Pts',(38.4659359584444,97.9199999800001,-189.555803560147));
#235340=CARTESIAN_POINT('Ctrl Pts',(38.7587302410591,97.9199999800001,-189.308895740408));
#235341=CARTESIAN_POINT('Ctrl Pts',(39.,97.9199999800001,-189.09995));
#235342=CARTESIAN_POINT('Origin',(39.,97.1699999800001,-189.09995));
#235343=CARTESIAN_POINT('Origin',(39.,98.9199999800001,-80.59995));
#235344=CARTESIAN_POINT('',(39.,97.9199999800001,-80.59995));
#235345=CARTESIAN_POINT('',(39.,97.1699999800001,-79.84995));
#235346=CARTESIAN_POINT('Origin',(39.,97.1699999800001,-80.59995));
#235347=CARTESIAN_POINT('Ctrl Pts',(39.,97.9199999800001,-80.59995));
#235348=CARTESIAN_POINT('Ctrl Pts',(38.7725853995754,97.9199999800001,-80.4030031788408));
#235349=CARTESIAN_POINT('Ctrl Pts',(38.5000149139681,97.9199999800001,-80.1711447838968));
#235350=CARTESIAN_POINT('Ctrl Pts',(38.2284392666181,97.9199999800001,-80.0295257645779));
#235351=CARTESIAN_POINT('Origin',(39.,98.9199999800001,-79.84995));
#235352=CARTESIAN_POINT('Origin',(10.5,-43.9113988480613,-385.453615950046));
#235353=CARTESIAN_POINT('',(11.,97.9199999800001,-187.272546484838));
#235354=CARTESIAN_POINT('',(10.5,97.9199999800001,-186.413411979785));
#235355=CARTESIAN_POINT('Origin',(10.5000000000105,97.9199999800001,-187.272546484831));
#235356=CARTESIAN_POINT('',(11.,96.0754406238205,-189.84995));
#235357=CARTESIAN_POINT('',(11.,-43.9113988480614,-385.453615950046));
#235358=CARTESIAN_POINT('',(10.5,95.460587505094,-189.84995));
#235359=CARTESIAN_POINT('Origin',(10.4999999999996,96.0754406238209,-189.84995));
#235360=CARTESIAN_POINT('',(10.5,91.2935952834256,-195.672489873167));
#235361=CARTESIAN_POINT('Origin',(10.5,-43.9113988480525,115.753715950042));
#235362=CARTESIAN_POINT('',(10.5,97.9199999800001,-83.2864880202152));
#235363=CARTESIAN_POINT('',(11.,97.9199999800001,-82.4273535151615));
#235364=CARTESIAN_POINT('Origin',(10.5,97.9199999800001,-82.427353515161));
#235365=CARTESIAN_POINT('',(10.5,95.6849588822271,-80.1634642136719));
#235366=CARTESIAN_POINT('',(10.5,91.2935952834259,-74.0274101268328));
#235367=CARTESIAN_POINT('',(11.,96.612189917828,-80.59995));
#235368=CARTESIAN_POINT('Ctrl Pts',(10.5,95.6849588822271,-80.1634642136719));
#235369=CARTESIAN_POINT('Ctrl Pts',(10.5156818609759,95.6849588822271,-80.163464213672));
#235370=CARTESIAN_POINT('Ctrl Pts',(10.5313200885977,95.6863393578606,-80.1641136250356));
#235371=CARTESIAN_POINT('Ctrl Pts',(10.5469160042521,95.6890782080141,-80.1654023178236));
#235372=CARTESIAN_POINT('Ctrl Pts',(10.5625645383606,95.6918262986678,-80.1666953584821));
#235373=CARTESIAN_POINT('Ctrl Pts',(10.5781708749757,95.6959420414388,-80.1686320420268));
#235374=CARTESIAN_POINT('Ctrl Pts',(10.5937322749933,95.7014506402686,-80.171224518524));
#235375=CARTESIAN_POINT('Ctrl Pts',(10.6092044253496,95.7069276455028,-80.1738021263301));
#235376=CARTESIAN_POINT('Ctrl Pts',(10.6246325584921,95.7137816788003,-80.1770280703136));
#235377=CARTESIAN_POINT('Ctrl Pts',(10.6400039678108,95.7220828322891,-80.1809357042478));
#235378=CARTESIAN_POINT('Ctrl Pts',(10.6547456182153,95.7300438916917,-80.1846832443837));
#235379=CARTESIAN_POINT('Ctrl Pts',(10.6694353917173,95.7393362069862,-80.1890578912298));
#235380=CARTESIAN_POINT('Ctrl Pts',(10.6840479045028,95.7500602195997,-80.1941073705498));
#235381=CARTESIAN_POINT('Ctrl Pts',(10.6864825086507,95.7518469571701,-80.1949486689273));
#235382=CARTESIAN_POINT('Ctrl Pts',(10.6889141998357,95.753672947647,-80.1958084301768));
#235383=CARTESIAN_POINT('Ctrl Pts',(10.6913425626005,95.7555384804021,-80.1966867914439));
#235384=CARTESIAN_POINT('Ctrl Pts',(10.7116040791809,95.7711039154339,-80.2040155693498));
#235385=CARTESIAN_POINT('Ctrl Pts',(10.7316297878809,95.7894211341418,-80.2126387195569));
#235386=CARTESIAN_POINT('Ctrl Pts',(10.7511868500182,95.8105123565252,-80.222567351155));
#235387=CARTESIAN_POINT('Ctrl Pts',(10.7583837688949,95.8182738400976,-80.2262210469743));
#235388=CARTESIAN_POINT('Ctrl Pts',(10.7655169157189,95.826410619207,-80.2300513643091));
#235389=CARTESIAN_POINT('Ctrl Pts',(10.772573602495,95.8349225100514,-80.2340582614315));
#235390=CARTESIAN_POINT('Ctrl Pts',(10.7920381169864,95.8584009253402,-80.2451105171968));
#235391=CARTESIAN_POINT('Ctrl Pts',(10.8109248100544,95.8847366103483,-80.2575078073411));
#235392=CARTESIAN_POINT('Ctrl Pts',(10.82895296563,95.9139165491847,-80.2712440047493));
#235393=CARTESIAN_POINT('Ctrl Pts',(10.8307439624858,95.9168154136021,-80.2726086194636));
#235394=CARTESIAN_POINT('Ctrl Pts',(10.8325264536709,95.9197423235926,-80.2739864363826));
#235395=CARTESIAN_POINT('Ctrl Pts',(10.834300140239,95.9226972461615,-80.2753774399745));
#235396=CARTESIAN_POINT('Ctrl Pts',(10.8371855095635,95.9275042075999,-80.2776402744384));
#235397=CARTESIAN_POINT('Ctrl Pts',(10.8402295435766,95.9326948651965,-80.2800837305874));
#235398=CARTESIAN_POINT('Ctrl Pts',(10.8431864058672,95.9378670615211,-80.2825184800336));
#235399=CARTESIAN_POINT('Ctrl Pts',(10.8462781372091,95.9432751731987,-80.2850642838054));
#235400=CARTESIAN_POINT('Ctrl Pts',(10.8492744231064,95.9486629966847,-80.2876005193099));
#235401=CARTESIAN_POINT('Ctrl Pts',(10.851919307303,95.9535221815782,-80.2898878650167));
#235402=CARTESIAN_POINT('Ctrl Pts',(10.8524805367969,95.9545532731783,-80.2903732268616));
#235403=CARTESIAN_POINT('Ctrl Pts',(10.8530260296046,95.9555604073977,-80.2908473092743));
#235404=CARTESIAN_POINT('Ctrl Pts',(10.8535534680192,95.956538501865,-80.2913077195793));
#235405=CARTESIAN_POINT('Ctrl Pts',(10.8649452601285,95.9776637148284,-80.3012518160527));
#235406=CARTESIAN_POINT('Ctrl Pts',(10.8761385017745,96.0004894960687,-80.3119968950234));
#235407=CARTESIAN_POINT('Ctrl Pts',(10.8869673939531,96.0250580069767,-80.3235624691653));
#235408=CARTESIAN_POINT('Ctrl Pts',(10.896634247271,96.0469900926667,-80.3338869517554));
#235409=CARTESIAN_POINT('Ctrl Pts',(10.9060105373242,96.0703106233711,-80.3448651281021));
#235410=CARTESIAN_POINT('Ctrl Pts',(10.9149649031813,96.0950201938376,-80.3564969392479));
#235411=CARTESIAN_POINT('Ctrl Pts',(10.9252600821156,96.123429737674,-80.3698704800424));
#235412=CARTESIAN_POINT('Ctrl Pts',(10.9350002950485,96.1536806995305,-80.384110852038));
#235413=CARTESIAN_POINT('Ctrl Pts',(10.9439706013777,96.1857608028677,-80.3992122761633));
#235414=CARTESIAN_POINT('Ctrl Pts',(10.9503835439419,96.2086951211178,-80.4100084030734));
#235415=CARTESIAN_POINT('Ctrl Pts',(10.9564026291807,96.2325638261801,-80.4212443842883));
#235416=CARTESIAN_POINT('Ctrl Pts',(10.9619397662556,96.2573539625288,-80.4329141211094));
#235417=CARTESIAN_POINT('Ctrl Pts',(10.9620475507384,96.2578365209317,-80.4331412811977));
#235418=CARTESIAN_POINT('Ctrl Pts',(10.9621551520677,96.2583194268068,-80.4333686048555));
#235419=CARTESIAN_POINT('Ctrl Pts',(10.9622625697312,96.2588026800681,-80.4335960920423));
#235420=CARTESIAN_POINT('Ctrl Pts',(10.9629080222422,96.2617064579087,-80.434963019707));
#235421=CARTESIAN_POINT('Ctrl Pts',(10.9637502581113,96.265559008235,-80.4367764944774));
#235422=CARTESIAN_POINT('Ctrl Pts',(10.9643453109648,96.2683234584993,-80.4380777533962));
#235423=CARTESIAN_POINT('Ctrl Pts',(10.9645704310761,96.2693693040028,-80.4385700450488));
#235424=CARTESIAN_POINT('Ctrl Pts',(10.9647607130506,96.270259013439,-80.4389888367266));
#235425=CARTESIAN_POINT('Ctrl Pts',(10.9648934963716,96.2708812896082,-80.4392817405416));
#235426=CARTESIAN_POINT('Ctrl Pts',(10.9684360128225,96.287482949737,-80.4470960998693));
#235427=CARTESIAN_POINT('Ctrl Pts',(10.9721210866807,96.306152102166,-80.4558840299471));
#235428=CARTESIAN_POINT('Ctrl Pts',(10.9757459570284,96.3269794923422,-80.4656881571978));
#235429=CARTESIAN_POINT('Ctrl Pts',(10.978979634052,96.3455592059914,-80.4744342302948));
#235430=CARTESIAN_POINT('Ctrl Pts',(10.9821648967382,96.3658572091196,-80.4839893529887));
#235431=CARTESIAN_POINT('Ctrl Pts',(10.9851264759707,96.3879150163117,-80.4943729948297));
#235432=CARTESIAN_POINT('Ctrl Pts',(10.9879212507746,96.4087304660878,-80.5041718009102));
#235433=CARTESIAN_POINT('Ctrl Pts',(10.9905166776936,96.4311137231632,-80.5147087337626));
#235434=CARTESIAN_POINT('Ctrl Pts',(10.9927398924504,96.4550683413436,-80.5259853943057));
#235435=CARTESIAN_POINT('Ctrl Pts',(10.9949001524002,96.478344636227,-80.5369427334761));
#235436=CARTESIAN_POINT('Ctrl Pts',(10.9967089624194,96.5031052705477,-80.5485988343262));
#235437=CARTESIAN_POINT('Ctrl Pts',(10.9979838985217,96.529313066776,-80.5609361188393));
#235438=CARTESIAN_POINT('Ctrl Pts',(10.9991586792015,96.5534620516668,-80.5723042207089));
#235439=CARTESIAN_POINT('Ctrl Pts',(10.9998799817883,96.5788399156019,-80.5842507595581));
#235440=CARTESIAN_POINT('Ctrl Pts',(10.9999863449063,96.6053774356702,-80.5967430818542));
#235441=CARTESIAN_POINT('Ctrl Pts',(10.9999954128483,96.6076398805487,-80.5978081094274));
#235442=CARTESIAN_POINT('Ctrl Pts',(11.,96.6099107273809,-80.5988770913113));
#235443=CARTESIAN_POINT('Ctrl Pts',(11.,96.612189917828,-80.59995));
#235444=CARTESIAN_POINT('',(11.,-43.9113988480525,115.753715950042));
#235445=CARTESIAN_POINT('Origin',(11.,-394.08000002,-134.84995));
#235446=CARTESIAN_POINT('',(11.,97.9199999800001,-134.84995));
#235447=CARTESIAN_POINT('',(11.,105.91999998,-189.84995));
#235448=CARTESIAN_POINT('Origin',(11.,-394.08000002,-134.84995));
#235449=CARTESIAN_POINT('',(11.,97.9199999800001,-134.84995));
#235450=CARTESIAN_POINT('',(11.,-394.08000002,-80.59995));
#235451=CARTESIAN_POINT('Origin',(-14.,91.2935952834256,-195.672489873167));
#235452=CARTESIAN_POINT('',(-14.,97.9199999800001,-186.413411979785));
#235453=CARTESIAN_POINT('',(48.,95.460587505094,-189.84995));
#235454=CARTESIAN_POINT('Origin',(-14.,91.2935952834259,-74.0274101268328));
#235455=CARTESIAN_POINT('',(-14.,97.9199999800001,-83.2864880202152));
#235456=CARTESIAN_POINT('',(10.5,95.6849588822271,-80.1634642136719));
#235457=CARTESIAN_POINT('Origin',(55.,105.91999998,-86.84995));
#235458=CARTESIAN_POINT('',(55.,97.9199999800001,-86.84995));
#235459=CARTESIAN_POINT('',(55.,97.1699999800001,-86.84995));
#235460=CARTESIAN_POINT('',(55.,97.1699999800001,-86.84995));
#235461=CARTESIAN_POINT('',(55.,94.4199999800001,-86.84995));
#235462=CARTESIAN_POINT('',(55.,105.91999998,-86.84995));
#235463=CARTESIAN_POINT('',(55.,94.4199999800001,-182.84995));
#235464=CARTESIAN_POINT('',(55.,94.4199999800001,-86.84995));
#235465=CARTESIAN_POINT('',(55.,97.1699999800001,-182.84995));
#235466=CARTESIAN_POINT('',(55.,105.91999998,-182.84995));
#235467=CARTESIAN_POINT('',(55.,97.1699999800001,-173.84995));
#235468=CARTESIAN_POINT('Origin',(-14.75,105.91999998,-80.59995));
#235469=CARTESIAN_POINT('',(-14.75,96.612189917828,-79.84995));
#235470=CARTESIAN_POINT('Origin',(-14.75,96.612189917828,-80.59995));
#235471=CARTESIAN_POINT('',(-14.75,105.91999998,-79.84995));
#235472=CARTESIAN_POINT('Ctrl Pts',(-14.75,96.612189917828,-79.84995));
#235473=CARTESIAN_POINT('Ctrl Pts',(-14.,96.612189917828,-79.84995));
#235474=CARTESIAN_POINT('Ctrl Pts',(-14.,96.612189917828,-80.59995));
#235475=CARTESIAN_POINT('Ctrl Pts',(-14.7499999999888,96.4109434379512,
-79.84995));
#235476=CARTESIAN_POINT('Ctrl Pts',(-14.0551300101178,96.4950766906307,
-79.8499500000001));
#235477=CARTESIAN_POINT('Ctrl Pts',(-14.,96.4907937818967,-80.542803845684));
#235478=CARTESIAN_POINT('Ctrl Pts',(-14.717465841188,96.2098486464843,-79.84995));
#235479=CARTESIAN_POINT('Ctrl Pts',(-14.087399369873,96.3554456062245,-79.8499500000001));
#235480=CARTESIAN_POINT('Ctrl Pts',(-13.9869863364741,96.3694891476217,
-80.4857007649587));
#235481=CARTESIAN_POINT('Ctrl Pts',(-14.5922329900902,95.8380606797986,
-79.84995));
#235482=CARTESIAN_POINT('Ctrl Pts',(-14.0888617253033,96.0821031793196,
-79.84995));
#235483=CARTESIAN_POINT('Ctrl Pts',(-13.9368931960372,96.1452187774359,
-80.3801274772601));
#235484=CARTESIAN_POINT('Ctrl Pts',(-14.4995835431726,95.6675499872971,
-79.84995));
#235485=CARTESIAN_POINT('Ctrl Pts',(-14.0613642943088,95.9469647180508,
-79.84995));
#235486=CARTESIAN_POINT('Ctrl Pts',(-13.8998334172684,96.0423631189524,
-80.3317090882667));
#235487=CARTESIAN_POINT('Ctrl Pts',(-14.2681834097938,95.3829957999329,
-79.84995));
#235488=CARTESIAN_POINT('Ctrl Pts',(-13.956965021564,95.7189955144651,-79.8499500000001));
#235489=CARTESIAN_POINT('Ctrl Pts',(-13.8072733639181,95.8707140107035,
-80.2509067929251));
#235490=CARTESIAN_POINT('Ctrl Pts',(-14.129523710464,95.2690641952365,-79.84995));
#235491=CARTESIAN_POINT('Ctrl Pts',(-13.8811942932893,95.6232014564904,
-79.8499499999988));
#235492=CARTESIAN_POINT('Ctrl Pts',(-13.7518094841857,95.8019880554524,
-80.2185546590279));
#235493=CARTESIAN_POINT('Ctrl Pts',(-13.8271848704487,95.1150645809588,
-79.84995));
#235494=CARTESIAN_POINT('Ctrl Pts',(-13.7038891791878,95.49503291722,-79.8499500000011));
#235495=CARTESIAN_POINT('Ctrl Pts',(-13.6308739481793,95.7090922288018,
-80.1748247725308));
#235496=CARTESIAN_POINT('Ctrl Pts',(-13.6636541071819,95.0750571210368,
-79.84995));
#235497=CARTESIAN_POINT('Ctrl Pts',(-13.6016004447884,95.4605875051159,
-79.84995));
#235498=CARTESIAN_POINT('Ctrl Pts',(-13.5654616428729,95.6849588822324,
-80.1634642136793));
#235499=CARTESIAN_POINT('Ctrl Pts',(-13.5,95.0750571210118,-79.84995));
#235500=CARTESIAN_POINT('Ctrl Pts',(-13.5,95.4605875050944,-79.84995));
#235501=CARTESIAN_POINT('Ctrl Pts',(-13.5,95.6849588822271,-80.1634642136719));
#235502=CARTESIAN_POINT('',(-13.5,95.0750571210118,-79.84995));
#235503=CARTESIAN_POINT('Origin',(-13.5,95.0750571210117,-80.59995));
#235504=CARTESIAN_POINT('Ctrl Pts',(-14.75,96.612189917828,-79.84995));
#235505=CARTESIAN_POINT('Ctrl Pts',(-14.7499999999888,96.4109434379512,
-79.84995));
#235506=CARTESIAN_POINT('Ctrl Pts',(-14.717465841188,96.2098486464843,-79.84995));
#235507=CARTESIAN_POINT('Ctrl Pts',(-14.5922329900902,95.8380606797986,
-79.84995));
#235508=CARTESIAN_POINT('Ctrl Pts',(-14.4995835431726,95.6675499872971,
-79.84995));
#235509=CARTESIAN_POINT('Ctrl Pts',(-14.2681834097938,95.3829957999329,
-79.84995));
#235510=CARTESIAN_POINT('Ctrl Pts',(-14.129523710464,95.2690641952365,-79.84995));
#235511=CARTESIAN_POINT('Ctrl Pts',(-13.8271848704487,95.1150645809588,
-79.84995));
#235512=CARTESIAN_POINT('Ctrl Pts',(-13.6636541071819,95.0750571210368,
-79.84995));
#235513=CARTESIAN_POINT('Ctrl Pts',(-13.5,95.0750571210118,-79.84995));
#235514=CARTESIAN_POINT('Origin',(-57.25,97.1699999800001,-86.84995));
#235515=CARTESIAN_POINT('',(-57.25,97.9199999800001,-182.84995));
#235516=CARTESIAN_POINT('Origin',(-57.25,97.1699999800001,-182.84995));
#235517=CARTESIAN_POINT('',(-57.25,97.9199999800001,-182.84995));
#235518=CARTESIAN_POINT('Origin',(-51.,97.1699999800001,-182.84995));
#235519=CARTESIAN_POINT('',(-51.,97.1699999800001,-189.84995));
#235520=CARTESIAN_POINT('',(-51.,97.9199999800001,-189.09995));
#235521=CARTESIAN_POINT('Origin',(-51.,97.1699999800001,-189.09995));
#235522=CARTESIAN_POINT('Origin',(-51.,97.1699999800001,-182.84995));
#235523=CARTESIAN_POINT('Origin',(-51.,97.9199999800001,-182.84995));
#235524=CARTESIAN_POINT('Origin',(-51.,97.1699999800001,-189.09995));
#235525=CARTESIAN_POINT('',(-51.,97.1699999800001,-189.84995));
#235526=CARTESIAN_POINT('',(-42.,97.9199999800001,-189.09995));
#235527=CARTESIAN_POINT('Origin',(-57.25,97.1699999800001,-86.84995));
#235528=CARTESIAN_POINT('',(-57.25,97.9199999800001,-86.84995));
#235529=CARTESIAN_POINT('Origin',(-57.25,97.1699999800001,-86.84995));
#235530=CARTESIAN_POINT('',(-57.25,97.9199999800001,-89.84995));
#235531=CARTESIAN_POINT('Origin',(-51.,97.1699999800001,-86.84995));
#235532=CARTESIAN_POINT('',(-51.,97.9199999800001,-80.59995));
#235533=CARTESIAN_POINT('',(-51.,97.1699999800001,-79.84995));
#235534=CARTESIAN_POINT('Origin',(-51.,97.1699999800001,-80.59995));
#235535=CARTESIAN_POINT('Origin',(-51.,97.9199999800001,-86.84995));
#235536=CARTESIAN_POINT('Origin',(-51.,97.1699999800001,-86.84995));
#235537=CARTESIAN_POINT('Origin',(48.,97.1699999800001,-80.59995));
#235538=CARTESIAN_POINT('',(-48.,97.9199999800001,-80.59995));
#235539=CARTESIAN_POINT('',(48.,97.1699999800001,-79.84995));
#235540=CARTESIAN_POINT('Origin',(-51.,105.91999998,-86.84995));
#235541=CARTESIAN_POINT('',(-51.,94.4199999800001,-79.84995));
#235542=CARTESIAN_POINT('Origin',(-51.,94.4199999800001,-86.84995));
#235543=CARTESIAN_POINT('',(-51.,105.91999998,-79.84995));
#235544=CARTESIAN_POINT('Origin',(-51.,105.91999998,-182.84995));
#235545=CARTESIAN_POINT('',(-51.,94.4199999800001,-189.84995));
#235546=CARTESIAN_POINT('Origin',(-51.,94.4199999800001,-182.84995));
#235547=CARTESIAN_POINT('',(-51.,105.91999998,-189.84995));
#235548=CARTESIAN_POINT('Origin',(55.01,94.4199999800001,-52.64995));
#235549=CARTESIAN_POINT('',(48.,94.4199999800001,-189.84995));
#235550=CARTESIAN_POINT('',(48.,94.4199999800001,-189.84995));
#235551=CARTESIAN_POINT('Origin',(48.,94.4199999800001,-182.84995));
#235552=CARTESIAN_POINT('',(48.,94.4199999800001,-79.84995));
#235553=CARTESIAN_POINT('Origin',(48.,94.4199999800001,-86.84995));
#235554=CARTESIAN_POINT('',(-51.,94.4199999800001,-79.84995));
#235555=CARTESIAN_POINT('Origin',(11.75,105.91999998,-80.59995));
#235556=CARTESIAN_POINT('',(11.75,96.612189917828,-79.84995));
#235557=CARTESIAN_POINT('Origin',(11.75,96.612189917828,-80.59995));
#235558=CARTESIAN_POINT('',(11.75,105.91999998,-79.84995));
#235559=CARTESIAN_POINT('Ctrl Pts',(11.,96.612189917828,-80.59995));
#235560=CARTESIAN_POINT('Ctrl Pts',(11.,96.6121899178279,-79.8499500000001));
#235561=CARTESIAN_POINT('Ctrl Pts',(11.75,96.612189917828,-79.84995));
#235562=CARTESIAN_POINT('Ctrl Pts',(11.,96.4907937818966,-80.542803845684));
#235563=CARTESIAN_POINT('Ctrl Pts',(11.0551300101177,96.4950766906306,-79.8499500000013));
#235564=CARTESIAN_POINT('Ctrl Pts',(11.7499999999888,96.4109434379512,-79.84995));
#235565=CARTESIAN_POINT('Ctrl Pts',(10.9869863364741,96.3694891476217,-80.4857007649587));
#235566=CARTESIAN_POINT('Ctrl Pts',(11.087399369873,96.3554456062245,-79.8499500000001));
#235567=CARTESIAN_POINT('Ctrl Pts',(11.717465841188,96.2098486464843,-79.84995));
#235568=CARTESIAN_POINT('Ctrl Pts',(10.9368931960372,96.1452187774359,-80.3801274772601));
#235569=CARTESIAN_POINT('Ctrl Pts',(11.0888617253033,96.0821031793196,-79.84995));
#235570=CARTESIAN_POINT('Ctrl Pts',(11.5922329900902,95.8380606797986,-79.84995));
#235571=CARTESIAN_POINT('Ctrl Pts',(10.8998334172684,96.0423631189524,-80.3317090882667));
#235572=CARTESIAN_POINT('Ctrl Pts',(11.061364294309,95.9469647180509,-79.84995));
#235573=CARTESIAN_POINT('Ctrl Pts',(11.4995835431726,95.6675499872971,-79.84995));
#235574=CARTESIAN_POINT('Ctrl Pts',(10.8072733639181,95.8707140107035,-80.2509067929251));
#235575=CARTESIAN_POINT('Ctrl Pts',(10.9569650215639,95.7189955144651,-79.84995));
#235576=CARTESIAN_POINT('Ctrl Pts',(11.2681834097938,95.3829957999329,-79.84995));
#235577=CARTESIAN_POINT('Ctrl Pts',(10.7518094841857,95.8019880554524,-80.2185546590279));
#235578=CARTESIAN_POINT('Ctrl Pts',(10.8811942932896,95.6232014564902,-79.8499499999989));
#235579=CARTESIAN_POINT('Ctrl Pts',(11.129523710464,95.2690641952365,-79.84995));
#235580=CARTESIAN_POINT('Ctrl Pts',(10.6308739481793,95.7090922288018,-80.1748247725308));
#235581=CARTESIAN_POINT('Ctrl Pts',(10.7038891791875,95.4950329172199,-79.8499500000012));
#235582=CARTESIAN_POINT('Ctrl Pts',(10.8271848704487,95.1150645809588,-79.84995));
#235583=CARTESIAN_POINT('Ctrl Pts',(10.5654616428729,95.6849588822324,-80.1634642136793));
#235584=CARTESIAN_POINT('Ctrl Pts',(10.6016004447886,95.4605875051159,-79.84995));
#235585=CARTESIAN_POINT('Ctrl Pts',(10.6636541071819,95.0750571210368,-79.84995));
#235586=CARTESIAN_POINT('Ctrl Pts',(10.5,95.6849588822271,-80.1634642136719));
#235587=CARTESIAN_POINT('Ctrl Pts',(10.5,95.4605875050944,-79.84995));
#235588=CARTESIAN_POINT('Ctrl Pts',(10.5,95.0750571210118,-79.84995));
#235589=CARTESIAN_POINT('',(10.5,95.0750571210118,-79.84995));
#235590=CARTESIAN_POINT('Origin',(10.5,95.0750571210117,-80.59995));
#235591=CARTESIAN_POINT('Ctrl Pts',(11.75,96.612189917828,-79.84995));
#235592=CARTESIAN_POINT('Ctrl Pts',(11.7499999999888,96.4109434379512,-79.84995));
#235593=CARTESIAN_POINT('Ctrl Pts',(11.717465841188,96.2098486464843,-79.84995));
#235594=CARTESIAN_POINT('Ctrl Pts',(11.5922329900902,95.8380606797986,-79.84995));
#235595=CARTESIAN_POINT('Ctrl Pts',(11.4995835431726,95.6675499872971,-79.84995));
#235596=CARTESIAN_POINT('Ctrl Pts',(11.2681834097938,95.3829957999329,-79.84995));
#235597=CARTESIAN_POINT('Ctrl Pts',(11.129523710464,95.2690641952365,-79.84995));
#235598=CARTESIAN_POINT('Ctrl Pts',(10.8271848704487,95.1150645809588,-79.84995));
#235599=CARTESIAN_POINT('Ctrl Pts',(10.6636541071819,95.0750571210368,-79.84995));
#235600=CARTESIAN_POINT('Ctrl Pts',(10.5,95.0750571210118,-79.84995));
#235601=CARTESIAN_POINT('Origin',(-14.,95.0750571210117,-80.59995));
#235602=CARTESIAN_POINT('',(-1.5,95.0750571210117,-79.84995));
#235603=CARTESIAN_POINT('Origin',(54.25,97.1699999800001,-86.84995));
#235604=CARTESIAN_POINT('',(54.25,97.9199999800001,-182.84995));
#235605=CARTESIAN_POINT('Origin',(54.25,97.1699999800001,-182.84995));
#235606=CARTESIAN_POINT('',(54.25,97.9199999800001,-182.84995));
#235607=CARTESIAN_POINT('Origin',(48.,97.1699999800001,-182.84995));
#235608=CARTESIAN_POINT('',(48.,97.1699999800001,-189.84995));
#235609=CARTESIAN_POINT('',(48.,97.9199999800001,-189.09995));
#235610=CARTESIAN_POINT('Origin',(48.,97.1699999800001,-189.09995));
#235611=CARTESIAN_POINT('Origin',(48.,97.9199999800001,-182.84995));
#235612=CARTESIAN_POINT('Origin',(48.,97.1699999800001,-182.84995));
#235613=CARTESIAN_POINT('Origin',(48.,97.1699999800001,-189.09995));
#235614=CARTESIAN_POINT('',(39.,97.9199999800001,-189.09995));
#235615=CARTESIAN_POINT('',(48.,97.1699999800001,-189.84995));
#235616=CARTESIAN_POINT('Origin',(54.25,97.1699999800001,-86.84995));
#235617=CARTESIAN_POINT('',(54.25,97.9199999800001,-86.84995));
#235618=CARTESIAN_POINT('Origin',(54.25,97.1699999800001,-86.84995));
#235619=CARTESIAN_POINT('',(54.25,97.9199999800001,-89.84995));
#235620=CARTESIAN_POINT('Origin',(48.,97.1699999800001,-86.84995));
#235621=CARTESIAN_POINT('',(48.,97.9199999800001,-80.59995));
#235622=CARTESIAN_POINT('',(48.,97.1699999800001,-79.84995));
#235623=CARTESIAN_POINT('Origin',(48.,97.1699999800001,-80.59995));
#235624=CARTESIAN_POINT('Origin',(48.,97.1699999800001,-86.84995));
#235625=CARTESIAN_POINT('Origin',(48.,97.9199999800001,-86.84995));
#235626=CARTESIAN_POINT('Origin',(-51.,97.1699999800001,-80.59995));
#235627=CARTESIAN_POINT('',(-51.,97.1699999800001,-79.84995));
#235628=CARTESIAN_POINT('',(45.,97.9199999800001,-80.59995));
#235629=CARTESIAN_POINT('Origin',(45.,97.9199999800001,-179.84995));
#235630=CARTESIAN_POINT('',(48.,97.9199999799999,-189.84995));
#235631=CARTESIAN_POINT('',(-51.,97.9199999799999,-189.84995));
#235632=CARTESIAN_POINT('Origin',(48.,105.91999998,-189.84995));
#235633=CARTESIAN_POINT('',(48.,105.91999998,-189.84995));
#235634=CARTESIAN_POINT('Origin',(-51.,105.91999998,-79.84995));
#235635=CARTESIAN_POINT('',(48.,105.91999998,-79.84995));
#235636=CARTESIAN_POINT('Origin',(48.,105.91999998,-86.84995));
#235637=CARTESIAN_POINT('Origin',(48.,105.91999998,-182.84995));
#235638=CARTESIAN_POINT('Origin',(44.5079524583208,31.5404524382925,235.35105));
#235639=CARTESIAN_POINT('',(44.507952458321,29.5404524382925,-52.1412));
#235640=CARTESIAN_POINT('',(44.5079524583209,29.5404524382925,-52.29995));
#235641=CARTESIAN_POINT('',(44.5079524583208,29.5404524382925,235.35105));
#235642=CARTESIAN_POINT('',(44.5079524583208,33.5404524382925,-52.64995));
#235643=CARTESIAN_POINT('Ctrl Pts',(44.5079524583208,33.5404524382925,-52.64995));
#235644=CARTESIAN_POINT('Ctrl Pts',(44.3548545542709,33.5404524382925,-52.6422157773399));
#235645=CARTESIAN_POINT('Ctrl Pts',(44.20228357332,33.522873307937,-52.6339954492238));
#235646=CARTESIAN_POINT('Ctrl Pts',(43.8989259410511,33.4520476875708,-52.6166046360311));
#235647=CARTESIAN_POINT('Ctrl Pts',(43.7494532049307,33.3978112619257,-52.6074716543951));
#235648=CARTESIAN_POINT('Ctrl Pts',(43.3701659866181,33.2066898065316,-52.5827363905734));
#235649=CARTESIAN_POINT('Ctrl Pts',(43.1586558164617,33.0405619760126,-52.56720589332));
#235650=CARTESIAN_POINT('Ctrl Pts',(42.8201807947071,32.6434822936339,-52.5385252711531));
#235651=CARTESIAN_POINT('Ctrl Pts',(42.6932650854895,32.4191782753192,-52.52620900716));
#235652=CARTESIAN_POINT('Ctrl Pts',(42.5294572327396,31.9312855999297,-52.4977486010956));
#235653=CARTESIAN_POINT('Ctrl Pts',(42.4955147520946,31.6718569742787,-52.4826152645993));
#235654=CARTESIAN_POINT('Ctrl Pts',(42.5288723018669,31.1486243083691,-52.4520933590879));
#235655=CARTESIAN_POINT('Ctrl Pts',(42.5981844499906,30.889977401297,-52.437005622842));
#235656=CARTESIAN_POINT('Ctrl Pts',(42.8283842527865,30.425478719589,-52.4099098664091));
#235657=CARTESIAN_POINT('Ctrl Pts',(42.9828916680193,30.2219875462947,-52.3968713548753));
#235658=CARTESIAN_POINT('Ctrl Pts',(43.3663701864947,29.8774589096907,-52.3674499782107));
#235659=CARTESIAN_POINT('Ctrl Pts',(43.5939982252634,29.7422747167445,-52.3520077588389));
#235660=CARTESIAN_POINT('Ctrl Pts',(44.0556467980409,29.5790367525449,-52.3239250203703));
#235661=CARTESIAN_POINT('Ctrl Pts',(44.2811108622566,29.5404524382925,-52.3114096174482));
#235662=CARTESIAN_POINT('Ctrl Pts',(44.507952458321,29.5404524382925,-52.29995));
#235663=CARTESIAN_POINT('',(46.4884569292028,31.8190238668641,-52.64995));
#235664=CARTESIAN_POINT('Origin',(44.5079524583208,31.5404524382925,-52.64995));
#235665=CARTESIAN_POINT('Ctrl Pts',(44.5079524583211,29.5404524382925,-52.1412));
#235666=CARTESIAN_POINT('Ctrl Pts',(44.3247135465072,29.5404524382925,-52.1504568905679));
#235667=CARTESIAN_POINT('Ctrl Pts',(44.1420161231988,29.5656268611773,-52.1604206801398));
#235668=CARTESIAN_POINT('Ctrl Pts',(43.7109798879774,29.6872198414568,-52.1857422946277));
#235669=CARTESIAN_POINT('Ctrl Pts',(43.4736864604903,29.8084243584665,-52.2012650509945));
#235670=CARTESIAN_POINT('Ctrl Pts',(43.0674816021137,30.1299064414062,-52.2311623291258));
#235671=CARTESIAN_POINT('Ctrl Pts',(42.9001540986214,30.3241179882545,-52.245247157081));
#235672=CARTESIAN_POINT('Ctrl Pts',(42.6416335239846,30.774204283096,-52.2715021909468));
#235673=CARTESIAN_POINT('Ctrl Pts',(42.5566346319212,31.0280187184028,-52.2863080330063));
#235674=CARTESIAN_POINT('Ctrl Pts',(42.4910511170322,31.549641664286,-52.3167360381829));
#235675=CARTESIAN_POINT('Ctrl Pts',(42.5094203902604,31.8122183820464,-52.3320530133855));
#235676=CARTESIAN_POINT('Ctrl Pts',(42.6440633687565,32.3087595709814,-52.3610179160734));
#235677=CARTESIAN_POINT('Ctrl Pts',(42.7564335035464,32.5387234706583,-52.3734994103579));
#235678=CARTESIAN_POINT('Ctrl Pts',(43.0697411860967,32.9558560535547,-52.4014935014093));
#235679=CARTESIAN_POINT('Ctrl Pts',(43.2721028320881,33.1355884690471,-52.416958632555));
#235680=CARTESIAN_POINT('Ctrl Pts',(43.7266339026704,33.3994643576703,-52.447617080786));
#235681=CARTESIAN_POINT('Ctrl Pts',(43.972394781555,33.4845697527202,-52.4625147060633));
#235682=CARTESIAN_POINT('Ctrl Pts',(44.4834801603881,33.556936973569,-52.490444503763));
#235683=CARTESIAN_POINT('Ctrl Pts',(44.743966207421,33.5432294366744,-52.5030419818516));
#235684=CARTESIAN_POINT('Ctrl Pts',(45.2513765607801,33.4159146504311,-52.5323887613926));
#235685=CARTESIAN_POINT('Ctrl Pts',(45.4927345544246,33.3011989232752,-52.5479275957456));
#235686=CARTESIAN_POINT('Ctrl Pts',(45.9088031766997,32.9904464827263,-52.5780102250637));
#235687=CARTESIAN_POINT('Ctrl Pts',(46.0819169579592,32.8004312724763,-52.5922977230811));
#235688=CARTESIAN_POINT('Ctrl Pts',(46.2845268385021,32.4687376590909,-52.612207596182));
#235689=CARTESIAN_POINT('Ctrl Pts',(46.3426893780983,32.3477280723218,-52.6191089213483));
#235690=CARTESIAN_POINT('Ctrl Pts',(46.4355872980842,32.0913303618597,-52.6340654544586));
#235691=CARTESIAN_POINT('Ctrl Pts',(46.4691386827723,31.9563670022371,-52.6419383171033));
#235692=CARTESIAN_POINT('Ctrl Pts',(46.4884569292029,31.8190238668635,-52.6499500000001));
#235693=CARTESIAN_POINT('Origin',(44.5079524583208,31.5404524382925,235.35105));
#235694=CARTESIAN_POINT('',(44.5079524583209,29.5404524382925,-51.4412));
#235695=CARTESIAN_POINT('',(44.507952458193,29.5404524382925,-51.5999500000129));
#235696=CARTESIAN_POINT('',(44.5079524583208,29.5404524382925,235.35105));
#235697=CARTESIAN_POINT('Ctrl Pts',(44.507952458321,29.5404524382925,-52.29995));
#235698=CARTESIAN_POINT('Ctrl Pts',(44.5456351337306,29.5404524382925,-52.2980463410057));
#235699=CARTESIAN_POINT('Ctrl Pts',(44.5833527227913,29.5415174066421,-52.2961098566617));
#235700=CARTESIAN_POINT('Ctrl Pts',(44.8762306266861,29.5581074238872,-52.2808303317015));
#235701=CARTESIAN_POINT('Ctrl Pts',(45.1262365572094,29.6213370764521,-52.2663562967642));
#235702=CARTESIAN_POINT('Ctrl Pts',(45.597903751345,29.8426585978762,-52.2360733323412));
#235703=CARTESIAN_POINT('Ctrl Pts',(45.8134393435507,30.0021996411661,-52.2205315928461));
#235704=CARTESIAN_POINT('Ctrl Pts',(46.1636689240197,30.389587657716,-52.1915398257226));
#235705=CARTESIAN_POINT('Ctrl Pts',(46.2975269516407,30.6113093304199,-52.179150014626));
#235706=CARTESIAN_POINT('Ctrl Pts',(46.4747895814738,31.0950501116668,-52.1509318023866));
#235707=CARTESIAN_POINT('Ctrl Pts',(46.5158274230668,31.3527181233366,-52.1359011683725));
#235708=CARTESIAN_POINT('Ctrl Pts',(46.4973503317335,31.8760198349414,-52.1053752351956));
#235709=CARTESIAN_POINT('Ctrl Pts',(46.4353859646996,32.1365641269858,-52.0901768181597));
#235710=CARTESIAN_POINT('Ctrl Pts',(46.2183725159575,32.607519480871,-52.0627044225164));
#235711=CARTESIAN_POINT('Ctrl Pts',(46.0696264259219,32.8153523985847,-52.0499916286466));
#235712=CARTESIAN_POINT('Ctrl Pts',(45.6964971586862,33.1700942756708,-52.0207951908128));
#235713=CARTESIAN_POINT('Ctrl Pts',(45.4734934122146,33.3113546790648,-52.0054093593214));
#235714=CARTESIAN_POINT('Ctrl Pts',(44.9798457017477,33.5023539189302,-51.9749003797879));
#235715=CARTESIAN_POINT('Ctrl Pts',(44.7132445891919,33.5478172614533,-51.9605357857066));
#235716=CARTESIAN_POINT('Ctrl Pts',(44.1908699228379,33.5315455130639,-51.9336717920495));
#235717=CARTESIAN_POINT('Ctrl Pts',(43.9399556743881,33.4749621780699,-51.9193457215013));
#235718=CARTESIAN_POINT('Ctrl Pts',(43.4638587352539,33.266716276669,-51.8892203468131));
#235719=CARTESIAN_POINT('Ctrl Pts',(43.2447120691995,33.1134614667662,-51.8736795310267));
#235720=CARTESIAN_POINT('Ctrl Pts',(42.883495283233,32.7353393673502,-51.8444029665401));
#235721=CARTESIAN_POINT('Ctrl Pts',(42.7430457982723,32.5160099599919,-51.8318575220992));
#235722=CARTESIAN_POINT('Ctrl Pts',(42.5532874534621,32.036216321252,-51.8038695598394));
#235723=CARTESIAN_POINT('Ctrl Pts',(42.5057248801028,31.7803536661032,-51.788944238289));
#235724=CARTESIAN_POINT('Ctrl Pts',(42.5104063276564,31.2573688010795,-51.7584367878293));
#235725=CARTESIAN_POINT('Ctrl Pts',(42.5654998955738,30.9952548269627,-51.7431468060059));
#235726=CARTESIAN_POINT('Ctrl Pts',(42.7701978299134,30.5184201146716,-51.7153314477889));
#235727=CARTESIAN_POINT('Ctrl Pts',(42.9136660376696,30.306512587328,-51.7028338192499));
#235728=CARTESIAN_POINT('Ctrl Pts',(43.2772642491842,29.9425079270756,-51.6738487081959));
#235729=CARTESIAN_POINT('Ctrl Pts',(43.4958968886054,29.795817128197,-51.6585253104048));
#235730=CARTESIAN_POINT('Ctrl Pts',(43.9809674611855,29.5930189970377,-51.6281054976679));
#235731=CARTESIAN_POINT('Ctrl Pts',(44.2432162131644,29.5404524383263,-51.6133239849614));
#235732=CARTESIAN_POINT('Ctrl Pts',(44.5079524580651,29.5404524382925,-51.5999500000129));
#235733=CARTESIAN_POINT('Ctrl Pts',(44.507952458321,29.5404524382925,-51.4412));
#235734=CARTESIAN_POINT('Ctrl Pts',(44.2835205459591,29.5404524382925,-51.452537884689));
#235735=CARTESIAN_POINT('Ctrl Pts',(44.060408947064,29.5782209797479,-51.4649106520451));
#235736=CARTESIAN_POINT('Ctrl Pts',(43.600354723926,29.7390446890627,-51.4928424311542));
#235737=CARTESIAN_POINT('Ctrl Pts',(43.3721726577259,29.8734763513654,-51.5082906901557));
#235738=CARTESIAN_POINT('Ctrl Pts',(42.9874338287575,30.2167497384021,-51.5377391239273));
#235739=CARTESIAN_POINT('Ctrl Pts',(42.8322220836105,30.4197176397976,-51.5508238034211));
#235740=CARTESIAN_POINT('Ctrl Pts',(42.6004293202525,30.8834252224738,-51.5778734124105));
#235741=CARTESIAN_POINT('Ctrl Pts',(42.5302307820271,31.1418277220128,-51.5929468915503));
#235742=CARTESIAN_POINT('Ctrl Pts',(42.4950690952893,31.6650230748981,-51.6234666204686));
#235743=CARTESIAN_POINT('Ctrl Pts',(42.5281472402474,31.9246519959457,-51.638611640863));
#235744=CARTESIAN_POINT('Ctrl Pts',(42.6903245105921,32.4130413675739,-51.6671010208747));
#235745=CARTESIAN_POINT('Ctrl Pts',(42.8164088542485,32.637658525451,-51.6794148597991));
#235746=CARTESIAN_POINT('Ctrl Pts',(43.1534652959873,33.0358936686857,-51.7080575188717));
#235747=CARTESIAN_POINT('Ctrl Pts',(43.364478565968,33.2028067206776,-51.7235858159412));
#235748=CARTESIAN_POINT('Ctrl Pts',(43.830419889728,33.4395637991918,-51.7540297237424));
#235749=CARTESIAN_POINT('Ctrl Pts',(44.0791181973968,33.5106841931608,-51.7686678466185));
#235750=CARTESIAN_POINT('Ctrl Pts',(44.5959203541677,33.5556751071966,-51.79608796974));
#235751=CARTESIAN_POINT('Ctrl Pts',(44.8592765093109,33.5267715625772,-51.8093472661401));
#235752=CARTESIAN_POINT('Ctrl Pts',(45.3605005505186,33.3686702778741,-51.8392794641832));
#235753=CARTESIAN_POINT('Ctrl Pts',(45.5933401003551,33.2407902593983,-51.8547719210234));
#235754=CARTESIAN_POINT('Ctrl Pts',(45.9888671080995,32.9083686699532,-51.8844488428499));
#235755=CARTESIAN_POINT('Ctrl Pts',(46.1501372598996,32.7098359294834,-51.8979859630138));
#235756=CARTESIAN_POINT('Ctrl Pts',(46.3954557319109,32.2529402210043,-51.924638212675));
#235757=CARTESIAN_POINT('Ctrl Pts',(46.4731638382971,31.996744828296,-51.9395829439163));
#235758=CARTESIAN_POINT('Ctrl Pts',(46.5236902380054,31.4741208800458,-51.9700693408976));
#235759=CARTESIAN_POINT('Ctrl Pts',(46.4980090848323,31.212901646118,-51.9853071295434));
#235760=CARTESIAN_POINT('Ctrl Pts',(46.3497242517928,30.7203434272596,-52.0140396923102));
#235761=CARTESIAN_POINT('Ctrl Pts',(46.2306336465384,30.4930439305853,-52.026389417297));
#235762=CARTESIAN_POINT('Ctrl Pts',(45.9056096715121,30.0851316905039,-52.0547064670867));
#235763=CARTESIAN_POINT('Ctrl Pts',(45.6989028260139,29.9116459531387,-52.0702089148879));
#235764=CARTESIAN_POINT('Ctrl Pts',(45.238573056588,29.6610301989817,-52.1007735487266));
#235765=CARTESIAN_POINT('Ctrl Pts',(44.9912718473802,29.5827827275061,-52.1155489658689));
#235766=CARTESIAN_POINT('Ctrl Pts',(44.6600861713746,29.5447870978041,-52.1333880589147));
#235767=CARTESIAN_POINT('Ctrl Pts',(44.5839791314037,29.5404524382925,-52.1373592732352));
#235768=CARTESIAN_POINT('Ctrl Pts',(44.5079524583211,29.5404524382925,-52.1412));
#235769=CARTESIAN_POINT('Origin',(44.5079524583208,31.5404524382925,235.35105));
#235770=CARTESIAN_POINT('',(44.5079524426195,29.5404524382925,-50.7412000015864));
#235771=CARTESIAN_POINT('',(44.5079524583207,29.5404524382925,-50.89995));
#235772=CARTESIAN_POINT('',(44.5079524583208,29.5404524382925,235.35105));
#235773=CARTESIAN_POINT('Ctrl Pts',(44.5079524580651,29.5404524382925,-51.5999500000129));
#235774=CARTESIAN_POINT('Ctrl Pts',(44.5081493673179,29.5404524382924,-51.599940052522));
#235775=CARTESIAN_POINT('Ctrl Pts',(44.5083462778614,29.5404524673725,-51.5999301041178));
#235776=CARTESIAN_POINT('Ctrl Pts',(44.7627038634985,29.5405275958781,-51.5870782385727));
#235777=CARTESIAN_POINT('Ctrl Pts',(45.0144847350904,29.5890492353315,-51.5729435206145));
#235778=CARTESIAN_POINT('Ctrl Pts',(45.4954760302278,29.7813442718332,-51.5430361256822));
#235779=CARTESIAN_POINT('Ctrl Pts',(45.7187617861315,29.9268804692804,-51.5275113369366));
#235780=CARTESIAN_POINT('Ctrl Pts',(46.0931857907529,30.2935768625855,-51.4979008179775));
#235781=CARTESIAN_POINT('Ctrl Pts',(46.241707454404,30.5100447027299,-51.4850571179078));
#235782=CARTESIAN_POINT('Ctrl Pts',(46.4463995242366,30.985003637967,-51.457351180019));
#235783=CARTESIAN_POINT('Ctrl Pts',(46.5016652543187,31.238498615233,-51.4425639730119));
#235784=CARTESIAN_POINT('Ctrl Pts',(46.5134570330975,31.7626294411718,-51.4119896748321));
#235785=CARTESIAN_POINT('Ctrl Pts',(46.465862850225,32.0283350076239,-51.3964901834558));
#235786=CARTESIAN_POINT('Ctrl Pts',(46.2738235919859,32.513261598713,-51.3682027989756));
#235787=CARTESIAN_POINT('Ctrl Pts',(46.135997236833,32.7296270969305,-51.3558448804301));
#235788=CARTESIAN_POINT('Ctrl Pts',(45.782620463481,33.1034209671638,-51.3270906188832));
#235789=CARTESIAN_POINT('Ctrl Pts',(45.5687864590191,33.2557554890865,-51.3118450306571));
#235790=CARTESIAN_POINT('Ctrl Pts',(45.0902866126965,33.4720690956454,-51.2813629574795));
#235791=CARTESIAN_POINT('Ctrl Pts',(44.8294053642904,33.5321786562759,-51.2664305242991));
#235792=CARTESIAN_POINT('Ctrl Pts',(44.3109920276729,33.5468055245127,-51.2398146253572));
#235793=CARTESIAN_POINT('Ctrl Pts',(44.0584917971278,33.5057281278676,-51.2262312871613));
#235794=CARTESIAN_POINT('Ctrl Pts',(43.5732154725709,33.328054025563,-51.1965338643904));
#235795=CARTESIAN_POINT('Ctrl Pts',(43.3463649249246,33.189685965016,-51.1810380596255));
#235796=CARTESIAN_POINT('Ctrl Pts',(42.9599322942034,32.8336714503139,-51.1511324419018));
#235797=CARTESIAN_POINT('Ctrl Pts',(42.8039167057754,32.6198105770137,-51.1379125580922));
#235798=CARTESIAN_POINT('Ctrl Pts',(42.5857129743017,32.1493364439137,-51.1104682336614));
#235799=CARTESIAN_POINT('Ctrl Pts',(42.5235781282351,31.8981751919542,-51.0958171606304));
#235800=CARTESIAN_POINT('Ctrl Pts',(42.4969894941382,31.3760742307904,-51.0653612712291));
#235801=CARTESIAN_POINT('Ctrl Pts',(42.5367477260569,31.1099059746523,-51.0498347896211));
#235802=CARTESIAN_POINT('Ctrl Pts',(42.7144151204012,30.6193907836024,-51.0212214034765));
#235803=CARTESIAN_POINT('Ctrl Pts',(42.8464254671907,30.398322385025,-51.0089084741443));
#235804=CARTESIAN_POINT('Ctrl Pts',(43.1892525940538,30.0145747762835,-50.9803968438328));
#235805=CARTESIAN_POINT('Ctrl Pts',(43.3980237487336,29.8566145876055,-50.9652429394571));
#235806=CARTESIAN_POINT('Ctrl Pts',(43.8693711210719,29.6266874739172,-50.9347251353981));
#235807=CARTESIAN_POINT('Ctrl Pts',(44.1284296497864,29.5589656500773,-50.9196627582983));
#235808=CARTESIAN_POINT('Ctrl Pts',(44.4314438908588,29.5415490019518,-50.9038470542835));
#235809=CARTESIAN_POINT('Ctrl Pts',(44.4697148774346,29.5404524382925,-50.9018816917915));
#235810=CARTESIAN_POINT('Ctrl Pts',(44.5079524583206,29.5404524382925,-50.89995));
#235811=CARTESIAN_POINT('Ctrl Pts',(44.5079524425794,29.5404524382925,-50.7412000007952));
#235812=CARTESIAN_POINT('Ctrl Pts',(44.2452561334393,29.5404524403601,-50.7544709320253));
#235813=CARTESIAN_POINT('Ctrl Pts',(43.9849786972769,29.5922110211334,-50.7691292914831));
#235814=CARTESIAN_POINT('Ctrl Pts',(43.5010903453052,29.7928033553668,-50.7994250448801));
#235815=CARTESIAN_POINT('Ctrl Pts',(43.2819599179859,29.9388901614813,-50.8147559735385));
#235816=CARTESIAN_POINT('Ctrl Pts',(42.9172875125919,30.3018574876075,-50.8437650952998));
#235817=CARTESIAN_POINT('Ctrl Pts',(42.773225484448,30.5133019264419,-50.8562828868087));
#235818=CARTESIAN_POINT('Ctrl Pts',(42.5671310964014,30.9894774249937,-50.8840597908909));
#235819=CARTESIAN_POINT('Ctrl Pts',(42.5112584037884,31.2514232116598,-50.8993399617797));
#235820=CARTESIAN_POINT('Ctrl Pts',(42.5050182585672,31.7744622727418,-50.9298505736762));
#235821=CARTESIAN_POINT('Ctrl Pts',(42.5518462004841,32.0305372605673,-50.9447882812993));
#235822=CARTESIAN_POINT('Ctrl Pts',(42.7401910787824,32.5107818792282,-50.9728025507212));
#235823=CARTESIAN_POINT('Ctrl Pts',(42.879887657652,32.7303817503275,-50.9853261188118));
#235824=CARTESIAN_POINT('Ctrl Pts',(43.2398585046255,33.1095652093879,-51.0145706970902));
#235825=CARTESIAN_POINT('Ctrl Pts',(43.4586032107541,33.2635390974229,-51.0301121797175));
#235826=CARTESIAN_POINT('Ctrl Pts',(43.9342139565177,33.4732767871518,-51.0602565033097));
#235827=CARTESIAN_POINT('Ctrl Pts',(44.1850336713978,33.5306166599398,-51.0745998638826));
#235828=CARTESIAN_POINT('Ctrl Pts',(44.7071273312422,33.548392843454,-51.1014935409689));
#235829=CARTESIAN_POINT('Ctrl Pts',(44.9735543568746,33.5038140543269,-51.1157899654104));
#235830=CARTESIAN_POINT('Ctrl Pts',(45.4676287468362,33.3145522441628,-51.1462698249691));
#235831=CARTESIAN_POINT('Ctrl Pts',(45.6911698647951,33.1739798064205,-51.1616627378082));
#235832=CARTESIAN_POINT('Ctrl Pts',(46.0654869628404,32.820401770524,-51.1908852372873));
#235833=CARTESIAN_POINT('Ctrl Pts',(46.2148924843005,32.6130713946132,-51.2036305608812));
#235834=CARTESIAN_POINT('Ctrl Pts',(46.4334291012576,32.1428534000483,-51.2310599438975));
#235835=CARTESIAN_POINT('Ctrl Pts',(46.4962429254979,31.8825168140543,-51.2462462447471));
#235836=CARTESIAN_POINT('Ctrl Pts',(46.5164335266262,31.3592013514549,-51.2767729800655));
#235837=CARTESIAN_POINT('Ctrl Pts',(46.4762096777092,31.101320734677,-51.2918160160442));
#235838=CARTESIAN_POINT('Ctrl Pts',(46.3004972586309,30.6170965329672,-51.3200624278106));
#235839=CARTESIAN_POINT('Ctrl Pts',(46.1674469680564,30.3950776435402,-51.332438841346));
#235840=CARTESIAN_POINT('Ctrl Pts',(45.8185759413347,30.0065582653918,-51.3613949748962));
#235841=CARTESIAN_POINT('Ctrl Pts',(45.6034971258212,29.8462486108739,-51.3769360567059));
#235842=CARTESIAN_POINT('Ctrl Pts',(45.1323997288438,29.6233229611646,-51.4072370231063));
#235843=CARTESIAN_POINT('Ctrl Pts',(44.8825177204272,29.5592755503712,-51.42172864901));
#235844=CARTESIAN_POINT('Ctrl Pts',(44.5875246136248,29.541638478946,-51.4371455691851));
#235845=CARTESIAN_POINT('Ctrl Pts',(44.5477195375851,29.5404524382925,-51.4391910407822));
#235846=CARTESIAN_POINT('Ctrl Pts',(44.507952458321,29.5404524382925,-51.4412));
#235847=CARTESIAN_POINT('Origin',(44.5079524583208,31.5404524382925,235.35105));
#235848=CARTESIAN_POINT('',(44.5079524583207,29.5404524382925,-50.0412));
#235849=CARTESIAN_POINT('',(44.5079524583207,29.5404524382925,-50.19995));
#235850=CARTESIAN_POINT('',(44.5079524583208,29.5404524382925,235.35105));
#235851=CARTESIAN_POINT('Ctrl Pts',(44.5079524583206,29.5404524382925,-50.89995));
#235852=CARTESIAN_POINT('Ctrl Pts',(44.7223870492869,29.5404524382924,-50.8891171614784));
#235853=CARTESIAN_POINT('Ctrl Pts',(44.9356705179706,29.5749306382515,-50.8773368613579));
#235854=CARTESIAN_POINT('Ctrl Pts',(45.388596365462,29.7257050768233,-50.8500582983187));
#235855=CARTESIAN_POINT('Ctrl Pts',(45.6188175437727,29.8567602462415,-50.8346055081911));
#235856=CARTESIAN_POINT('Ctrl Pts',(46.0172668306694,30.2017837993482,-50.8044134009588));
#235857=CARTESIAN_POINT('Ctrl Pts',(46.1809412372564,30.4130117124252,-50.7907173756756));
#235858=CARTESIAN_POINT('Ctrl Pts',(46.4126181451152,30.8789081377957,-50.7635400841957));
#235859=CARTESIAN_POINT('Ctrl Pts',(46.481496793499,31.1275673053499,-50.7490349660883));
#235860=CARTESIAN_POINT('Ctrl Pts',(46.5226921292547,31.6472471862232,-50.7187203063708));
#235861=CARTESIAN_POINT('Ctrl Pts',(46.490708585099,31.9136550356356,-50.7031798484884));
#235862=CARTESIAN_POINT('Ctrl Pts',(46.327395781776,32.4095726321365,-50.6742513220259));
#235863=CARTESIAN_POINT('Ctrl Pts',(46.2011360550349,32.6353821888252,-50.6618843827444));
#235864=CARTESIAN_POINT('Ctrl Pts',(45.8687191959684,33.0288137008287,-50.6336162127094));
#235865=CARTESIAN_POINT('Ctrl Pts',(45.6650438756082,33.1921243816843,-50.618563684427));
#235866=CARTESIAN_POINT('Ctrl Pts',(45.2010753834282,33.4351518281971,-50.5880365546913));
#235867=CARTESIAN_POINT('Ctrl Pts',(44.9440229078205,33.5102718024179,-50.5728597402943));
#235868=CARTESIAN_POINT('Ctrl Pts',(44.4274400923127,33.5548169790144,-50.5454636985625));
#235869=CARTESIAN_POINT('Ctrl Pts',(44.1732648218395,33.5284566265293,-50.532692322418));
#235870=CARTESIAN_POINT('Ctrl Pts',(43.6802205162023,33.3798298053096,-50.5034496879898));
#235871=CARTESIAN_POINT('Ctrl Pts',(43.4469659558143,33.2558972613171,-50.4880514002574));
#235872=CARTESIAN_POINT('Ctrl Pts',(43.0370244822471,32.9216899214035,-50.4575942019164));
#235873=CARTESIAN_POINT('Ctrl Pts',(42.8658645972105,32.7130212416766,-50.4433498468641));
#235874=CARTESIAN_POINT('Ctrl Pts',(42.621331652736,32.2515930595891,-50.416433202909));
#235875=CARTESIAN_POINT('Ctrl Pts',(42.5461252697442,32.0054783084443,-50.4020765090922));
#235876=CARTESIAN_POINT('Ctrl Pts',(42.4911498890836,31.4884695511673,-50.3719176649177));
#235877=CARTESIAN_POINT('Ctrl Pts',(42.5157620760352,31.2220369675854,-50.3563757642088));
#235878=CARTESIAN_POINT('Ctrl Pts',(42.6653547852825,30.7211280053138,-50.327156074743));
#235879=CARTESIAN_POINT('Ctrl Pts',(42.7861592882629,30.4907476085359,-50.3146487456099));
#235880=CARTESIAN_POINT('Ctrl Pts',(43.1087425797863,30.0882899618175,-50.2866140869383));
#235881=CARTESIAN_POINT('Ctrl Pts',(43.3075233072641,29.9201112674401,-50.2716668406986));
#235882=CARTESIAN_POINT('Ctrl Pts',(43.7642477394687,29.6650253207538,-50.2411539612058));
#235883=CARTESIAN_POINT('Ctrl Pts',(44.0192236691758,29.5830296156398,-50.225881507912));
#235884=CARTESIAN_POINT('Ctrl Pts',(44.357686330653,29.5446815888122,-50.2076645167837));
#235885=CARTESIAN_POINT('Ctrl Pts',(44.4328567771926,29.5404524382925,-50.203743694775));
#235886=CARTESIAN_POINT('Ctrl Pts',(44.5079524583205,29.5404524382925,-50.19995));
#235887=CARTESIAN_POINT('Ctrl Pts',(44.5079524583206,29.5404524382925,-50.0412));
#235888=CARTESIAN_POINT('Ctrl Pts',(44.4718396769997,29.5404524382925,-50.0430243508515));
#235889=CARTESIAN_POINT('Ctrl Pts',(44.4356964143001,29.5414305218481,-50.0448787690027));
#235890=CARTESIAN_POINT('Ctrl Pts',(44.1347625162448,29.5577637409606,-50.0605577779271));
#235891=CARTESIAN_POINT('Ctrl Pts',(43.8754935925516,29.6246561249279,-50.0756065917954));
#235892=CARTESIAN_POINT('Ctrl Pts',(43.4033453825172,29.8531064654309,-50.1061217801408));
#235893=CARTESIAN_POINT('Ctrl Pts',(43.1940137605603,30.0104595756638,-50.121286291831));
#235894=CARTESIAN_POINT('Ctrl Pts',(42.8500294412034,30.3931225943627,-50.1498247474887));
#235895=CARTESIAN_POINT('Ctrl Pts',(42.7173810615116,30.6136699299704,-50.1621376870145));
#235896=CARTESIAN_POINT('Ctrl Pts',(42.5381287939439,31.1035777460775,-50.1907156429541));
#235897=CARTESIAN_POINT('Ctrl Pts',(42.4975087939038,31.3697059799194,-50.2062397899282));
#235898=CARTESIAN_POINT('Ctrl Pts',(42.5224738071396,31.8920503217537,-50.2367098765352));
#235899=CARTESIAN_POINT('Ctrl Pts',(42.5838567543876,32.1434774629151,-50.2513764597696));
#235900=CARTESIAN_POINT('Ctrl Pts',(42.8005716030855,32.6144509620887,-50.2788499138881));
#235901=CARTESIAN_POINT('Ctrl Pts',(42.9557523429832,32.8286004468419,-50.292023374237));
#235902=CARTESIAN_POINT('Ctrl Pts',(43.3408593825313,33.1858084919308,-50.3218968368519));
#235903=CARTESIAN_POINT('Ctrl Pts',(43.5673259416073,33.3249747315708,-50.3373965234486));
#235904=CARTESIAN_POINT('Ctrl Pts',(44.0521514345071,33.5042740140904,-50.3671185721286));
#235905=CARTESIAN_POINT('Ctrl Pts',(44.3045692693176,33.5461702783005,-50.3807586875109));
#235906=CARTESIAN_POINT('Ctrl Pts',(44.8230662180689,33.5331907529982,-50.4073307628807));
#235907=CARTESIAN_POINT('Ctrl Pts',(45.0841320350819,33.4739130629318,-50.4222482572339));
#235908=CARTESIAN_POINT('Ctrl Pts',(45.5633868399102,33.2590953146877,-50.4527248403166));
#235909=CARTESIAN_POINT('Ctrl Pts',(45.7777631848714,33.1073829098469,-50.4679796814991));
#235910=CARTESIAN_POINT('Ctrl Pts',(46.1322836598823,32.7346771640365,-50.4967599837739));
#235911=CARTESIAN_POINT('Ctrl Pts',(46.2707407253182,32.5188152061094,-50.509128838544));
#235912=CARTESIAN_POINT('Ctrl Pts',(46.4643277872029,32.0345012181195,-50.5373804878434));
#235913=CARTESIAN_POINT('Ctrl Pts',(46.512768475601,31.7688589176576,-50.5528762887036));
#235914=CARTESIAN_POINT('Ctrl Pts',(46.5025796737736,31.2445334353493,-50.5834619418383));
#235915=CARTESIAN_POINT('Ctrl Pts',(46.4480603283826,30.9907976408417,-50.5982631965179));
#235916=CARTESIAN_POINT('Ctrl Pts',(46.2448247752994,30.5153615378464,-50.6259969691926));
#235917=CARTESIAN_POINT('Ctrl Pts',(46.0971000007615,30.298613993033,-50.6388061630299));
#235918=CARTESIAN_POINT('Ctrl Pts',(45.7239673879505,29.9307859133832,-50.6683844507841));
#235919=CARTESIAN_POINT('Ctrl Pts',(45.5010763917506,29.7844873078777,-50.683911533902));
#235920=CARTESIAN_POINT('Ctrl Pts',(45.0205425114124,29.5906216983497,-50.7138416294655));
#235921=CARTESIAN_POINT('Ctrl Pts',(44.7688353612694,29.5413084976514,-50.7279957103556));
#235922=CARTESIAN_POINT('Ctrl Pts',(44.5123839247908,29.5404561201211,-50.7409760231318));
#235923=CARTESIAN_POINT('Ctrl Pts',(44.5101681030411,29.540452438275,-50.7410880697314));
#235924=CARTESIAN_POINT('Ctrl Pts',(44.5079524425794,29.5404524382925,-50.7412000007953));
#235925=CARTESIAN_POINT('Origin',(44.5079524583208,31.5404524382925,235.35105));
#235926=CARTESIAN_POINT('',(44.5079524583207,29.5404524382925,-49.3412));
#235927=CARTESIAN_POINT('',(44.5079524583208,29.5404524382925,-49.49995));
#235928=CARTESIAN_POINT('',(44.5079524583208,29.5404524382925,235.35105));
#235929=CARTESIAN_POINT('Ctrl Pts',(44.5079524583205,29.5404524382925,-50.19995));
#235930=CARTESIAN_POINT('Ctrl Pts',(44.6854903835516,29.5404524382924,-50.1909811127192));
#235931=CARTESIAN_POINT('Ctrl Pts',(44.8625403587716,29.56408467282,-50.1813476022625));
#235932=CARTESIAN_POINT('Ctrl Pts',(45.28620891383,29.6796980413921,-50.156572594677));
#235933=CARTESIAN_POINT('Ctrl Pts',(45.5220741830687,29.7969970368165,-50.141235897267));
#235934=CARTESIAN_POINT('Ctrl Pts',(45.9387949613059,30.1181270424578,-50.1108176432552));
#235935=CARTESIAN_POINT('Ctrl Pts',(46.1144794508713,30.3200935055919,-50.0961376044075));
#235936=CARTESIAN_POINT('Ctrl Pts',(46.3715502505798,30.7712516860386,-50.0698200438814));
#235937=CARTESIAN_POINT('Ctrl Pts',(46.4541344793749,31.0141498381624,-50.0556509850076));
#235938=CARTESIAN_POINT('Ctrl Pts',(46.5252715707204,31.5275366066112,-50.0257034235147));
#235939=CARTESIAN_POINT('Ctrl Pts',(46.5093512265501,31.7937439167226,-50.0101746637582));
#235940=CARTESIAN_POINT('Ctrl Pts',(46.3761051620342,32.3003689583257,-49.9806215363314));
#235941=CARTESIAN_POINT('Ctrl Pts',(46.2617604432823,32.5362486897881,-49.9678384083179));
#235942=CARTESIAN_POINT('Ctrl Pts',(45.9507500216637,32.949176749041,-49.9400830025751));
#235943=CARTESIAN_POINT('Ctrl Pts',(45.7578157806442,33.1228486696454,-49.9252708909085));
#235944=CARTESIAN_POINT('Ctrl Pts',(45.3080776926849,33.3928271136546,-49.8946765840869));
#235945=CARTESIAN_POINT('Ctrl Pts',(45.0535188148037,33.4831006191545,-49.8791837636346));
#235946=CARTESIAN_POINT('Ctrl Pts',(44.5371087550905,33.556323037186,-49.8509600296639));
#235947=CARTESIAN_POINT('Ctrl Pts',(44.2810316527491,33.543724827296,-49.8385818257136));
#235948=CARTESIAN_POINT('Ctrl Pts',(43.7812887351337,33.4218568125833,-49.8097812550002));
#235949=CARTESIAN_POINT('Ctrl Pts',(43.5429243093868,33.3114488625768,-49.7945192936551));
#235950=CARTESIAN_POINT('Ctrl Pts',(43.1179787815527,33.0027190464296,-49.764047212715));
#235951=CARTESIAN_POINT('Ctrl Pts',(42.9366013104539,32.8058204339529,-49.7491414824884));
#235952=CARTESIAN_POINT('Ctrl Pts',(42.6671935620064,32.3625804136743,-49.7226036679059));
#235953=CARTESIAN_POINT('Ctrl Pts',(42.5778537182236,32.1227672258342,-49.7089183626068));
#235954=CARTESIAN_POINT('Ctrl Pts',(42.4919955194013,31.6129175222094,-49.6791771298953));
#235955=CARTESIAN_POINT('Ctrl Pts',(42.4999743107404,31.3471585975877,-49.6636745259591));
#235956=CARTESIAN_POINT('Ctrl Pts',(42.6180965880014,30.835474477271,-49.6338262856073));
#235957=CARTESIAN_POINT('Ctrl Pts',(42.7264862189083,30.5944607914065,-49.6206882864261));
#235958=CARTESIAN_POINT('Ctrl Pts',(43.0269238084561,30.1721073775051,-49.5931920944073));
#235959=CARTESIAN_POINT('Ctrl Pts',(43.2144480637339,29.9936415728931,-49.5785134635872));
#235960=CARTESIAN_POINT('Ctrl Pts',(43.6551267556531,29.7118567137799,-49.5480324669067));
#235961=CARTESIAN_POINT('Ctrl Pts',(43.9062190856509,29.6145713201919,-49.5325102566327));
#235962=CARTESIAN_POINT('Ctrl Pts',(44.281221150398,29.5500864982108,-49.51168503931));
#235963=CARTESIAN_POINT('Ctrl Pts',(44.3946043832944,29.5404524382925,-49.5056761348925));
#235964=CARTESIAN_POINT('Ctrl Pts',(44.5079524583208,29.5404524382925,-49.49995));
#235965=CARTESIAN_POINT('Ctrl Pts',(44.5079524583205,29.5404524382924,-49.3412));
#235966=CARTESIAN_POINT('Ctrl Pts',(44.4347306017759,29.5404524382925,-49.3448990326264));
#235967=CARTESIAN_POINT('Ctrl Pts',(44.36143495477,29.5444731844207,-49.3487190647722));
#235968=CARTESIAN_POINT('Ctrl Pts',(44.0247419395233,29.5816604188695,-49.366812800205));
#235969=CARTESIAN_POINT('Ctrl Pts',(43.769538862732,29.6629362233144,-49.3820757314461));
#235970=CARTESIAN_POINT('Ctrl Pts',(43.3120382640791,29.9167649498573,-49.4125911525099));
#235971=CARTESIAN_POINT('Ctrl Pts',(43.1127377910696,30.0844387239051,-49.4275499284887));
#235972=CARTESIAN_POINT('Ctrl Pts',(42.7891170628562,30.485949790652,-49.4556093879586));
#235973=CARTESIAN_POINT('Ctrl Pts',(42.6677358253903,30.7158435078294,-49.4680978123896));
#235974=CARTESIAN_POINT('Ctrl Pts',(42.516688318219,31.2162315094823,-49.497287112486));
#235975=CARTESIAN_POINT('Ctrl Pts',(42.491297617099,31.4826708114347,-49.5128294050999));
#235976=CARTESIAN_POINT('Ctrl Pts',(42.5448208218008,31.9999789945987,-49.5430057157845));
#235977=CARTESIAN_POINT('Ctrl Pts',(42.619361967759,32.2463704050013,-49.557378548058));
#235978=CARTESIAN_POINT('Ctrl Pts',(42.8625328016231,32.7082767065792,-49.5843230823167));
#235979=CARTESIAN_POINT('Ctrl Pts',(43.0328912932333,32.9172191858626,-49.5985050044065));
#235980=CARTESIAN_POINT('Ctrl Pts',(43.4416143774102,33.2525880935964,-49.6289345310327));
#235981=CARTESIAN_POINT('Ctrl Pts',(43.6745563136385,33.3772816950055,-49.6443392230793));
#235982=CARTESIAN_POINT('Ctrl Pts',(44.1672080797862,33.5274255373187,-49.6736062735878));
#235983=CARTESIAN_POINT('Ctrl Pts',(44.4212860495018,33.5545592635309,-49.6864103244151));
#235984=CARTESIAN_POINT('Ctrl Pts',(44.9379811137366,33.5115991391739,-49.7137658060544));
#235985=CARTESIAN_POINT('Ctrl Pts',(45.1952589178849,33.437268907295,-49.7289309694805));
#235986=CARTESIAN_POINT('Ctrl Pts',(45.6600354667484,33.1956337283898,-49.7594583129385));
#235987=CARTESIAN_POINT('Ctrl Pts',(45.864263122286,33.0328886673496,-49.7745222469268));
#235988=CARTESIAN_POINT('Ctrl Pts',(46.1977991581386,32.6404921391706,-49.8028167686727));
#235989=CARTESIAN_POINT('Ctrl Pts',(46.3246783953422,32.415196790911,-49.8151732460972));
#235990=CARTESIAN_POINT('Ctrl Pts',(46.4895428970062,31.9198546302735,-49.8440682054677));
#235991=CARTESIAN_POINT('Ctrl Pts',(46.5223640304513,31.6534620717256,-49.859607771383));
#235992=CARTESIAN_POINT('Ctrl Pts',(46.4827387391494,31.1335018402801,-49.889938784884));
#235993=CARTESIAN_POINT('Ctrl Pts',(46.4145831811994,30.8845641698543,-49.9044601489922));
#235994=CARTESIAN_POINT('Ctrl Pts',(46.1843616608845,30.418168117697,-49.9316665853681));
#235995=CARTESIAN_POINT('Ctrl Pts',(46.021523674798,30.2066536689454,-49.9453063152114));
#235996=CARTESIAN_POINT('Ctrl Pts',(45.6243740475149,29.8604261174862,-49.9754678826649));
#235997=CARTESIAN_POINT('Ctrl Pts',(45.394507714501,29.7285733411811,-49.9909260101993));
#235998=CARTESIAN_POINT('Ctrl Pts',(44.9399504315824,29.5756303575526,-50.0183502395666));
#235999=CARTESIAN_POINT('Ctrl Pts',(44.7245509498906,29.5404524382924,-50.0302578452263));
#236000=CARTESIAN_POINT('Ctrl Pts',(44.5079524583206,29.5404524382925,-50.0412));
#236001=CARTESIAN_POINT('Origin',(44.5079524583208,31.5404524382925,235.35105));
#236002=CARTESIAN_POINT('',(44.5079524583208,29.5404524382925,-48.6412));
#236003=CARTESIAN_POINT('',(44.5079524583208,29.5404524382925,-48.79995));
#236004=CARTESIAN_POINT('',(44.5079524583208,29.5404524382925,235.35105));
#236005=CARTESIAN_POINT('Ctrl Pts',(44.5079524583208,29.5404524382925,-49.49995));
#236006=CARTESIAN_POINT('Ctrl Pts',(44.6484656327225,29.5404524382925,-49.4928515345818));
#236007=CARTESIAN_POINT('Ctrl Pts',(44.7888806723387,29.5552566461249,-49.4853262373563));
#236008=CARTESIAN_POINT('Ctrl Pts',(45.1806504006529,29.6391837124542,-49.4630868832543));
#236009=CARTESIAN_POINT('Ctrl Pts',(45.4213938027402,29.7424116308721,-49.4479141580171));
#236010=CARTESIAN_POINT('Ctrl Pts',(45.854619835414,30.0381992846698,-49.4174012410385));
#236011=CARTESIAN_POINT('Ctrl Pts',(46.041702894108,30.2297530025382,-49.4023631678496));
#236012=CARTESIAN_POINT('Ctrl Pts',(46.323783766141,30.66472907859,-49.3754261622338));
#236013=CARTESIAN_POINT('Ctrl Pts',(46.4199950666918,30.9014832349083,-49.3622232035309));
#236014=CARTESIAN_POINT('Ctrl Pts',(46.520718713886,31.4074374884758,-49.3327092054061));
#236015=CARTESIAN_POINT('Ctrl Pts',(46.520782148984,31.6725038366582,-49.3172470017622));
#236016=CARTESIAN_POINT('Ctrl Pts',(46.4181877781362,32.1891466636479,-49.2871095035211));
#236017=CARTESIAN_POINT('Ctrl Pts',(46.3159074025737,32.4354702613398,-49.2735131832809));
#236018=CARTESIAN_POINT('Ctrl Pts',(46.0261962946597,32.8672514390045,-49.2462838968116));
#236019=CARTESIAN_POINT('Ctrl Pts',(45.8442148432103,33.050360574315,-49.2317498476999));
#236020=CARTESIAN_POINT('Ctrl Pts',(45.4129231573035,33.3436961542053,-49.201406169161));
#236021=CARTESIAN_POINT('Ctrl Pts',(45.1654925444267,33.4478912620257,-49.1858674087248));
#236022=CARTESIAN_POINT('Ctrl Pts',(44.653864715571,33.5515029361511,-49.1569989109002));
#236023=CARTESIAN_POINT('Ctrl Pts',(44.3954195531985,33.5536463187043,-49.144649867494));
#236024=CARTESIAN_POINT('Ctrl Pts',(43.8890919987703,33.4598239728255,-49.1163346517942));
#236025=CARTESIAN_POINT('Ctrl Pts',(43.6462066668259,33.3637312842641,-49.101261831097));
#236026=CARTESIAN_POINT('Ctrl Pts',(43.2051904152028,33.0809433095534,-49.070734523987));
#236027=CARTESIAN_POINT('Ctrl Pts',(43.0126306470048,32.8948361340484,-49.0555786350594));
#236028=CARTESIAN_POINT('Ctrl Pts',(42.7181155625902,32.4681458225661,-49.0282551441886));
#236029=CARTESIAN_POINT('Ctrl Pts',(42.6151406296482,32.2343021242018,-49.0154245650115));
#236030=CARTESIAN_POINT('Ctrl Pts',(42.5000340017128,31.732252165234,-48.9861383174051));
#236031=CARTESIAN_POINT('Ctrl Pts',(42.4921940754199,31.4680869181564,-48.9707286779922));
#236032=CARTESIAN_POINT('Ctrl Pts',(42.579542595888,30.9468134144484,-48.9403210569426));
#236033=CARTESIAN_POINT('Ctrl Pts',(42.6758149910805,30.6952460162276,-48.9261876720982));
#236034=CARTESIAN_POINT('Ctrl Pts',(42.9551155629621,30.2544432760503,-48.8992211777281));
#236035=CARTESIAN_POINT('Ctrl Pts',(43.1316771331268,30.0670398204614,-48.8848356799762));
#236036=CARTESIAN_POINT('Ctrl Pts',(43.5536933825864,29.7629099787529,-48.8546457466773));
#236037=CARTESIAN_POINT('Ctrl Pts',(43.7974425359341,29.6522098012248,-48.8391032355606));
#236038=CARTESIAN_POINT('Ctrl Pts',(44.2043250364462,29.5577537492186,-48.8157933167722));
#236039=CARTESIAN_POINT('Ctrl Pts',(44.3560483031499,29.5404524382925,-48.8076239166769));
#236040=CARTESIAN_POINT('Ctrl Pts',(44.5079524583209,29.5404524382925,-48.79995));
#236041=CARTESIAN_POINT('Ctrl Pts',(44.5079524583208,29.5404524382925,-48.6412));
#236042=CARTESIAN_POINT('Ctrl Pts',(44.3966865670165,29.5404524382925,-48.6468209468259));
#236043=CARTESIAN_POINT('Ctrl Pts',(44.2853796577939,29.5497358422582,-48.6527147317501));
#236044=CARTESIAN_POINT('Ctrl Pts',(43.912159951728,29.6127135730367,-48.6734059507855));
#236045=CARTESIAN_POINT('Ctrl Pts',(43.6606906762901,29.7092600291355,-48.6889256513018));
#236046=CARTESIAN_POINT('Ctrl Pts',(43.2190355200071,29.9898046404431,-48.7194198032597));
#236047=CARTESIAN_POINT('Ctrl Pts',(43.0309311224372,30.1677690648216,-48.7341131182042));
#236048=CARTESIAN_POINT('Ctrl Pts',(42.7293651132697,30.5891228335877,-48.7616371595765));
#236049=CARTESIAN_POINT('Ctrl Pts',(42.6203370049354,30.829583738668,-48.7747326591886));
#236050=CARTESIAN_POINT('Ctrl Pts',(42.5005919680911,31.3407357668696,-48.8045498608337));
#236051=CARTESIAN_POINT('Ctrl Pts',(42.4917660124846,31.6065536272709,-48.8200559026904));
#236052=CARTESIAN_POINT('Ctrl Pts',(42.5760576785285,32.1168053340831,-48.8498205855878));
#236053=CARTESIAN_POINT('Ctrl Pts',(42.6646798040309,32.3569439318746,-48.863562280121));
#236054=CARTESIAN_POINT('Ctrl Pts',(42.9327627204454,32.8010377406691,-48.8900580688071));
#236055=CARTESIAN_POINT('Ctrl Pts',(43.1135369753961,32.9984829249773,-48.9049492673491));
#236056=CARTESIAN_POINT('Ctrl Pts',(43.5375977426921,33.3085472673299,-48.9354155755059));
#236057=CARTESIAN_POINT('Ctrl Pts',(43.775702314129,33.4197000986306,-48.9506861351968));
#236058=CARTESIAN_POINT('Ctrl Pts',(44.2750891658946,33.5430335850107,-48.9795114610464));
#236059=CARTESIAN_POINT('Ctrl Pts',(44.5310529398885,33.5563922254494,-48.9919020831007));
#236060=CARTESIAN_POINT('Ctrl Pts',(45.0476916794559,33.4847389964617,-49.0200916015405));
#236061=CARTESIAN_POINT('Ctrl Pts',(45.3025978489709,33.3951962331301,-49.0355806532099));
#236062=CARTESIAN_POINT('Ctrl Pts',(45.7532539199965,33.1264529365426,-49.0661853097033));
#236063=CARTESIAN_POINT('Ctrl Pts',(45.9467399201863,32.9532851912744,-49.0810105901076));
#236064=CARTESIAN_POINT('Ctrl Pts',(46.2588354661981,32.5413320142359,-49.1087923802611));
#236065=CARTESIAN_POINT('Ctrl Pts',(46.3737882052089,32.3059733464028,-49.1215446136935));
#236066=CARTESIAN_POINT('Ctrl Pts',(46.508576223429,31.7998765958748,-49.151066924141));
#236067=CARTESIAN_POINT('Ctrl Pts',(46.5253118626813,31.5336364010089,-49.1665976021749));
#236068=CARTESIAN_POINT('Ctrl Pts',(46.4556867208825,31.01988806246,-49.1965662552569));
#236069=CARTESIAN_POINT('Ctrl Pts',(46.3737906753047,30.7766781966533,-49.210753497429));
#236070=CARTESIAN_POINT('Ctrl Pts',(46.1179762369941,30.3247075715368,-49.2371184505608));
#236071=CARTESIAN_POINT('Ctrl Pts',(45.9428653239357,30.1222324920566,-49.2517422737912));
#236072=CARTESIAN_POINT('Ctrl Pts',(45.5270038822513,29.7998629835924,-49.282153267877));
#236073=CARTESIAN_POINT('Ctrl Pts',(45.2914026904891,29.6818687965638,-49.2974969010036));
#236074=CARTESIAN_POINT('Ctrl Pts',(44.8662072647484,29.5645788470108,-49.3223979435477));
#236075=CARTESIAN_POINT('Ctrl Pts',(44.6873370504399,29.5404524382924,-49.332137822527));
#236076=CARTESIAN_POINT('Ctrl Pts',(44.5079524583205,29.5404524382924,-49.3412));
#236077=CARTESIAN_POINT('Origin',(44.5079524583208,31.5404524382925,235.35105));
#236078=CARTESIAN_POINT('',(44.5079524583208,29.5404524382925,-47.9412));
#236079=CARTESIAN_POINT('',(44.507952458321,29.5404524382925,-48.09995));
#236080=CARTESIAN_POINT('',(44.5079524583208,29.5404524382925,235.35105));
#236081=CARTESIAN_POINT('Ctrl Pts',(44.5079524583209,29.5404524382925,-48.79995));
#236082=CARTESIAN_POINT('Ctrl Pts',(44.6124054576492,29.5404524382925,-48.794673227863));
#236083=CARTESIAN_POINT('Ctrl Pts',(44.7169196208853,29.5486339379085,-48.7891547387667));
#236084=CARTESIAN_POINT('Ctrl Pts',(45.0755021322027,29.6053773611856,-48.7693847976788));
#236085=CARTESIAN_POINT('Ctrl Pts',(45.3202204921733,29.6946948534938,-48.7544169856902));
#236086=CARTESIAN_POINT('Ctrl Pts',(45.7682363932305,29.9650144896715,-48.7238997291241));
#236087=CARTESIAN_POINT('Ctrl Pts',(45.9658206989812,30.1458278721843,-48.7086444121576));
#236088=CARTESIAN_POINT('Ctrl Pts',(46.2720123503269,30.5645670818025,-48.6809629498817));
#236089=CARTESIAN_POINT('Ctrl Pts',(46.3813725344836,30.7957537575501,-48.6683907563767));
#236090=CARTESIAN_POINT('Ctrl Pts',(46.5098146029957,31.2940686287568,-48.6393223888897));
#236091=CARTESIAN_POINT('Ctrl Pts',(46.5248478732476,31.5571950157847,-48.6239733496464));
#236092=CARTESIAN_POINT('Ctrl Pts',(46.4524088657759,32.0784249813983,-48.593568268319));
#236093=CARTESIAN_POINT('Ctrl Pts',(46.3640405764904,32.3311197494686,-48.5789883387074));
#236094=CARTESIAN_POINT('Ctrl Pts',(46.0994768902361,32.7781044399352,-48.5525860176312));
#236095=CARTESIAN_POINT('Ctrl Pts',(45.9293137744679,32.9702837029562,-48.5383844635656));
#236096=CARTESIAN_POINT('Ctrl Pts',(45.5183631917647,33.2865592546567,-48.5083992973889));
#236097=CARTESIAN_POINT('Ctrl Pts',(45.2790807684743,33.4046389462523,-48.4928672013779));
#236098=CARTESIAN_POINT('Ctrl Pts',(44.773147586514,33.539691527979,-48.4633693600995));
#236099=CARTESIAN_POINT('Ctrl Pts',(44.5119607294398,33.5571963467212,-48.4506408544318));
#236100=CARTESIAN_POINT('Ctrl Pts',(43.9993908098511,33.49175967849,-48.4228382015996));
#236101=CARTESIAN_POINT('Ctrl Pts',(43.7528090648274,33.4102014134541,-48.4080025656435));
#236102=CARTESIAN_POINT('Ctrl Pts',(43.2952295341215,33.1531748205669,-48.3773898859768));
#236103=CARTESIAN_POINT('Ctrl Pts',(43.0905955767037,32.9766637978301,-48.3619039191536));
#236104=CARTESIAN_POINT('Ctrl Pts',(42.7712099849039,32.5642902218657,-48.3337415877487));
#236105=CARTESIAN_POINT('Ctrl Pts',(42.6553637021866,32.3357155711247,-48.3213403494153));
#236106=CARTESIAN_POINT('Ctrl Pts',(42.513629119446,31.8412311006041,-48.2924954219683));
#236107=CARTESIAN_POINT('Ctrl Pts',(42.4914536380871,31.5793346839613,-48.2772181309975));
#236108=CARTESIAN_POINT('Ctrl Pts',(42.549215271666,31.0571371659685,-48.2467566091145));
#236109=CARTESIAN_POINT('Ctrl Pts',(42.6304352239428,30.8020589290332,-48.2318770452933));
#236110=CARTESIAN_POINT('Ctrl Pts',(42.8821025646091,30.348418307425,-48.2054146756995));
#236111=CARTESIAN_POINT('Ctrl Pts',(43.0462671530581,30.1519640435191,-48.1916273905432));
#236112=CARTESIAN_POINT('Ctrl Pts',(43.4469111430654,29.824759237847,-48.1618441244399));
#236113=CARTESIAN_POINT('Ctrl Pts',(43.6819049491589,29.7000547860285,-48.1463354592563));
#236114=CARTESIAN_POINT('Ctrl Pts',(44.1207881906624,29.5686522320205,-48.1203313159722));
#236115=CARTESIAN_POINT('Ctrl Pts',(44.314015955622,29.5404524382925,-48.1097473130534));
#236116=CARTESIAN_POINT('Ctrl Pts',(44.5079524583212,29.5404524382925,-48.09995));
#236117=CARTESIAN_POINT('Ctrl Pts',(44.5079524583209,29.5404524382925,-47.9412));
#236118=CARTESIAN_POINT('Ctrl Pts',(44.3579755816972,29.5404524382925,-47.948776554133));
#236119=CARTESIAN_POINT('Ctrl Pts',(44.2081632822339,29.5573175881789,-47.9568366943373));
#236120=CARTESIAN_POINT('Ctrl Pts',(43.8028204437651,29.6501842668025,-47.9800224755263));
#236121=CARTESIAN_POINT('Ctrl Pts',(43.5586882082148,29.7602263932128,-47.995565146089));
#236122=CARTESIAN_POINT('Ctrl Pts',(43.1357136992404,30.0632679431852,-48.0257717470421));
#236123=CARTESIAN_POINT('Ctrl Pts',(42.9585946709616,30.2502405021384,-48.0401728387275));
#236124=CARTESIAN_POINT('Ctrl Pts',(42.6782261972195,30.6901236343595,-48.0671664596237));
#236125=CARTESIAN_POINT('Ctrl Pts',(42.5813335727787,30.9411492814144,-48.0812406491822));
#236126=CARTESIAN_POINT('Ctrl Pts',(42.4924132920601,31.4619564662418,-48.1116210682971));
#236127=CARTESIAN_POINT('Ctrl Pts',(42.4994572444471,31.7262244829687,-48.1270367026061));
#236128=CARTESIAN_POINT('Ctrl Pts',(42.613090509591,32.2286803782218,-48.1563466298292));
#236129=CARTESIAN_POINT('Ctrl Pts',(42.7153669457972,32.4628200369277,-48.1692109537427));
#236130=CARTESIAN_POINT('Ctrl Pts',(43.0086006049266,32.8903727011717,-48.1964948613361));
#236131=CARTESIAN_POINT('Ctrl Pts',(43.2006018186943,33.077050333196,-48.2116391714431));
#236132=CARTESIAN_POINT('Ctrl Pts',(43.6408310230128,33.3611914449707,-48.2421661848781));
#236133=CARTESIAN_POINT('Ctrl Pts',(43.8835045846324,33.4580233813017,-48.2572498687238));
#236134=CARTESIAN_POINT('Ctrl Pts',(44.3895029349291,33.5532900725682,-48.2855905803808));
#236135=CARTESIAN_POINT('Ctrl Pts',(44.6478181814517,33.551915588119,-48.2979314155088));
#236136=CARTESIAN_POINT('Ctrl Pts',(45.1597114761688,33.4498857052435,-48.326767188599));
#236137=CARTESIAN_POINT('Ctrl Pts',(45.4075316399209,33.3464037142673,-48.342304829183));
#236138=CARTESIAN_POINT('Ctrl Pts',(45.8398138956164,33.0542562520053,-48.3726638960428));
#236139=CARTESIAN_POINT('Ctrl Pts',(46.0223774204,32.8716225014001,-48.3872134850344));
#236140=CARTESIAN_POINT('Ctrl Pts',(46.3132107316458,32.4408213495401,-48.4144708790523));
#236141=CARTESIAN_POINT('Ctrl Pts',(46.4161338763291,32.1950578421958,-48.4280146847723));
#236142=CARTESIAN_POINT('Ctrl Pts',(46.5203614144427,31.6789251427172,-48.4581224255752));
#236143=CARTESIAN_POINT('Ctrl Pts',(46.5211382052541,31.4137751212621,-48.4735895101601));
#236144=CARTESIAN_POINT('Ctrl Pts',(46.4219675984017,30.9074071567246,-48.5031276414248));
#236145=CARTESIAN_POINT('Ctrl Pts',(46.3264795719479,30.6703358570656,-48.5163764440766));
#236146=CARTESIAN_POINT('Ctrl Pts',(46.0457312332532,30.2344824504535,-48.5432717213833));
#236147=CARTESIAN_POINT('Ctrl Pts',(45.8592424108637,30.0423568721471,-48.5582964541171));
#236148=CARTESIAN_POINT('Ctrl Pts',(45.4268711694178,29.7451935799646,-48.5888063114116));
#236149=CARTESIAN_POINT('Ctrl Pts',(45.1863687115451,29.6412061835209,-48.6039890160356));
#236150=CARTESIAN_POINT('Ctrl Pts',(44.7928315447917,29.5556772904819,-48.6263643778008));
#236151=CARTESIAN_POINT('Ctrl Pts',(44.6504483170862,29.5404524382925,-48.6340013730386));
#236152=CARTESIAN_POINT('Ctrl Pts',(44.5079524583208,29.5404524382925,-48.6412));
#236153=CARTESIAN_POINT('Origin',(44.5079524583208,31.5404524382925,235.35105));
#236154=CARTESIAN_POINT('',(44.507952458321,29.5404524382925,-47.2412));
#236155=CARTESIAN_POINT('',(44.5079524583209,29.5404524382925,-47.39995));
#236156=CARTESIAN_POINT('',(44.5079524583208,29.5404524382925,235.35105));
#236157=CARTESIAN_POINT('Ctrl Pts',(44.5079524583212,29.5404524382925,-48.09995));
#236158=CARTESIAN_POINT('Ctrl Pts',(44.5744456140837,29.5404524382925,-48.0965908888793));
#236159=CARTESIAN_POINT('Ctrl Pts',(44.6410122894404,29.5437682233701,-48.0931313532869));
#236160=CARTESIAN_POINT('Ctrl Pts',(44.9628032820804,29.5760206257622,-48.0759343730476));
#236161=CARTESIAN_POINT('Ctrl Pts',(45.2108608454448,29.6505409254038,-48.061229455472));
#236162=CARTESIAN_POINT('Ctrl Pts',(45.6741776139309,29.893919033943,-48.0307250219683));
#236163=CARTESIAN_POINT('Ctrl Pts',(45.8831629699355,30.0639777429019,-48.0152074230301));
#236164=CARTESIAN_POINT('Ctrl Pts',(46.2144966875535,30.4668425681303,-47.9867188329934));
#236165=CARTESIAN_POINT('Ctrl Pts',(46.3372422045201,30.6927293159444,-47.9744005154704));
#236166=CARTESIAN_POINT('Ctrl Pts',(46.4928262269163,31.1831112717244,-47.9457949013833));
#236167=CARTESIAN_POINT('Ctrl Pts',(46.5224008360514,31.4435209456006,-47.9306043370738));
#236168=CARTESIAN_POINT('Ctrl Pts',(46.4799450428868,31.9665016465536,-47.9000971295182));
#236169=CARTESIAN_POINT('Ctrl Pts',(46.4061727093305,32.2238843914121,-47.8850831360681));
#236170=CARTESIAN_POINT('Ctrl Pts',(46.1679504623852,32.6843749522474,-47.8582211866861));
#236171=CARTESIAN_POINT('Ctrl Pts',(46.0098765849212,32.8852330176666,-47.8449349925796));
#236172=CARTESIAN_POINT('Ctrl Pts',(45.620028909405,33.2233916342008,-47.8153776501455));
#236173=CARTESIAN_POINT('Ctrl Pts',(45.389622047513,33.3547451495957,-47.7999067778695));
#236174=CARTESIAN_POINT('Ctrl Pts',(44.8902269731069,33.5212152492233,-47.7698228854077));
#236175=CARTESIAN_POINT('Ctrl Pts',(44.6260583212529,33.554295754968,-47.7563202529318));
#236176=CARTESIAN_POINT('Ctrl Pts',(44.1077875119566,33.5166594429613,-47.7290404454297));
#236177=CARTESIAN_POINT('Ctrl Pts',(43.8584383109475,33.4492787656594,-47.7144785156966));
#236178=CARTESIAN_POINT('Ctrl Pts',(43.3897198382266,33.2198251838446,-47.6841073301254));
#236179=CARTESIAN_POINT('Ctrl Pts',(43.1765312949804,33.0563936078188,-47.6685706853269));
#236180=CARTESIAN_POINT('Ctrl Pts',(42.8332139627755,32.663281046047,-47.6397611462857));
#236181=CARTESIAN_POINT('Ctrl Pts',(42.7034498373582,32.4400428806018,-47.6274261091348));
#236182=CARTESIAN_POINT('Ctrl Pts',(42.5340872269857,31.953853028734,-47.5990650344425));
#236183=CARTESIAN_POINT('Ctrl Pts',(42.4972072082159,31.6951280328635,-47.5839727430167));
#236184=CARTESIAN_POINT('Ctrl Pts',(42.5244193618401,31.1718152306882,-47.5534461628898));
#236185=CARTESIAN_POINT('Ctrl Pts',(42.5907049592164,30.9123590996215,-47.5383112219109));
#236186=CARTESIAN_POINT('Ctrl Pts',(42.8154698231011,30.4451792389422,-47.5110590633713));
#236187=CARTESIAN_POINT('Ctrl Pts',(42.9675879904806,30.2399008772353,-47.498166940483));
#236188=CARTESIAN_POINT('Ctrl Pts',(43.3467828590477,29.8911246887345,-47.4688380789505));
#236189=CARTESIAN_POINT('Ctrl Pts',(43.5725128424477,29.7534030632497,-47.4534177373727));
#236190=CARTESIAN_POINT('Ctrl Pts',(44.0394865101384,29.5818720814861,-47.4248241052893));
#236191=CARTESIAN_POINT('Ctrl Pts',(44.2729285172036,29.5404524382925,-47.4118229743711));
#236192=CARTESIAN_POINT('Ctrl Pts',(44.5079524583209,29.5404524382925,-47.39995));
#236193=CARTESIAN_POINT('Ctrl Pts',(44.5079524583212,29.5404524382925,-47.2412));
#236194=CARTESIAN_POINT('Ctrl Pts',(44.3161695932765,29.5404524382925,-47.2508885152664));
#236195=CARTESIAN_POINT('Ctrl Pts',(44.1250598901523,29.5680293419666,-47.2613473499961));
#236196=CARTESIAN_POINT('Ctrl Pts',(43.6877393791654,29.6974352527612,-47.2872143116007));
#236197=CARTESIAN_POINT('Ctrl Pts',(43.4522787886795,29.8214387035994,-47.3027261120056));
#236198=CARTESIAN_POINT('Ctrl Pts',(43.050514532505,30.1474951765375,-47.3325324788435));
#236199=CARTESIAN_POINT('Ctrl Pts',(42.8857142674878,30.3434963463404,-47.3463775613027));
#236200=CARTESIAN_POINT('Ctrl Pts',(42.6326624757846,30.7964223289899,-47.3727982436239));
#236201=CARTESIAN_POINT('Ctrl Pts',(42.5506780675097,31.0512500957407,-47.3876631966844));
#236202=CARTESIAN_POINT('Ctrl Pts',(42.491337179176,31.573341120158,-47.418118506442));
#236203=CARTESIAN_POINT('Ctrl Pts',(42.5127455459109,31.8353792307101,-47.4334040628909));
#236204=CARTESIAN_POINT('Ctrl Pts',(42.6530492798312,32.3302810924118,-47.4622733381568));
#236205=CARTESIAN_POINT('Ctrl Pts',(42.7681912048292,32.5591352929089,-47.4746887324736));
#236206=CARTESIAN_POINT('Ctrl Pts',(43.0863482336752,32.9724749727599,-47.5028171771827));
#236207=CARTESIAN_POINT('Ctrl Pts',(43.2905260064056,33.149640493398,-47.5182991879222));
#236208=CARTESIAN_POINT('Ctrl Pts',(43.7474962882126,33.4080567439264,-47.5489216211438));
#236209=CARTESIAN_POINT('Ctrl Pts',(43.9939158737931,33.4903338565153,-47.563770031492));
#236210=CARTESIAN_POINT('Ctrl Pts',(44.5061868906327,33.5571755127349,-47.591598563127));
#236211=CARTESIAN_POINT('Ctrl Pts',(44.7672301534184,33.5404430936836,-47.6042985016686));
#236212=CARTESIAN_POINT('Ctrl Pts',(45.2734675098934,33.4069622838196,-47.6337658659344));
#236213=CARTESIAN_POINT('Ctrl Pts',(45.5131751696297,33.2895629917125,-47.6492995991183));
#236214=CARTESIAN_POINT('Ctrl Pts',(45.9251710929418,32.9744026848683,-47.6793050459922));
#236215=CARTESIAN_POINT('Ctrl Pts',(46.0959356868371,32.7826593326602,-47.6935242715538));
#236216=CARTESIAN_POINT('Ctrl Pts',(46.361805112398,32.3363515453863,-47.7199728131524));
#236217=CARTESIAN_POINT('Ctrl Pts',(46.4508870206064,32.0838984732078,-47.7344989812965));
#236218=CARTESIAN_POINT('Ctrl Pts',(46.5248028126764,31.5627978865617,-47.7648965155175));
#236219=CARTESIAN_POINT('Ctrl Pts',(46.5104917901831,31.2995581891282,-47.7802521645345));
#236220=CARTESIAN_POINT('Ctrl Pts',(46.3833906627011,30.8008628174555,-47.809342727882));
#236221=CARTESIAN_POINT('Ctrl Pts',(46.2746778676633,30.5694106870498,-47.821937021061));
#236222=CARTESIAN_POINT('Ctrl Pts',(45.969666662751,30.1498598706526,-47.849582521233));
#236223=CARTESIAN_POINT('Ctrl Pts',(45.7725848615113,29.9685035242572,-47.8648282890485));
#236224=CARTESIAN_POINT('Ctrl Pts',(45.3252623113295,29.6969122274837,-47.8953476089128));
#236225=CARTESIAN_POINT('Ctrl Pts',(45.0807212817331,29.6069066929765,-47.9103265303966));
#236226=CARTESIAN_POINT('Ctrl Pts',(44.7204630306518,29.5489141010597,-47.9302175608401));
#236227=CARTESIAN_POINT('Ctrl Pts',(44.6141790638268,29.5404524382925,-47.9358336285627));
#236228=CARTESIAN_POINT('Ctrl Pts',(44.5079524583209,29.5404524382925,-47.9412));
#236229=CARTESIAN_POINT('Origin',(44.5079524583208,31.5404524382925,235.35105));
#236230=CARTESIAN_POINT('',(44.5079524583209,29.5404524382925,-46.5412));
#236231=CARTESIAN_POINT('',(44.5079524583208,29.5404524382925,-46.69995));
#236232=CARTESIAN_POINT('',(44.5079524583208,29.5404524382925,235.35105));
#236233=CARTESIAN_POINT('Ctrl Pts',(44.5079524583209,29.5404524382925,-47.39995));
#236234=CARTESIAN_POINT('Ctrl Pts',(44.5385862697585,29.5404524382925,-47.398402436563));
#236235=CARTESIAN_POINT('Ctrl Pts',(44.5692449150485,29.5411562530311,-47.3968330906359));
#236236=CARTESIAN_POINT('Ctrl Pts',(44.8549461411357,29.5543055640908,-47.3820164720818));
#236237=CARTESIAN_POINT('Ctrl Pts',(45.1053514370633,29.614769287618,-47.3676029348738));
#236238=CARTESIAN_POINT('Ctrl Pts',(45.5789056016243,29.8306574967445,-47.3373831158073));
#236239=CARTESIAN_POINT('Ctrl Pts',(45.7959658777406,29.9875909690999,-47.3218404062562));
#236240=CARTESIAN_POINT('Ctrl Pts',(46.1507794359507,30.3711385593677,-47.2927290774974));
#236241=CARTESIAN_POINT('Ctrl Pts',(46.2873745175777,30.5918599420633,-47.2802845622801));
#236242=CARTESIAN_POINT('Ctrl Pts',(46.4698592437824,31.0739620758806,-47.2521619378074));
#236243=CARTESIAN_POINT('Ctrl Pts',(46.5136319627525,31.3308953616782,-47.2371741628025));
#236244=CARTESIAN_POINT('Ctrl Pts',(46.5009242215487,31.8541092063848,-47.2066533551947));
#236245=CARTESIAN_POINT('Ctrl Pts',(46.4418263610125,32.115332164523,-47.1914153493033));
#236246=CARTESIAN_POINT('Ctrl Pts',(46.2299515253067,32.5887586022814,-47.1637988071007));
#236247=CARTESIAN_POINT('Ctrl Pts',(46.0834190432785,32.7982891123863,-47.1511860853199));
#236248=CARTESIAN_POINT('Ctrl Pts',(45.7142823903956,33.1569274732217,-47.1220776995284));
#236249=CARTESIAN_POINT('Ctrl Pts',(45.4930970597846,33.3004822053262,-47.1067168131189));
#236250=CARTESIAN_POINT('Ctrl Pts',(45.0043512348937,33.4959368190476,-47.076325519365));
#236251=CARTESIAN_POINT('Ctrl Pts',(44.7410622240157,33.5444211633912,-47.0618420282549));
#236252=CARTESIAN_POINT('Ctrl Pts',(44.2215629831072,33.5361425256362,-47.035356428161));
#236253=CARTESIAN_POINT('Ctrl Pts',(43.9701894283288,33.4835330612488,-47.0211230588669));
#236254=CARTESIAN_POINT('Ctrl Pts',(43.4916145031828,33.2831374574593,-46.9911014679269));
#236255=CARTESIAN_POINT('Ctrl Pts',(43.2703946363235,33.1336745971244,-46.9755665164033));
#236256=CARTESIAN_POINT('Ctrl Pts',(42.9026520849897,32.7611573963193,-46.9461237585419));
#236257=CARTESIAN_POINT('Ctrl Pts',(42.7582353334241,32.5432425794276,-46.9334460915678));
#236258=CARTESIAN_POINT('Ctrl Pts',(42.5571969726149,32.0564042935838,-46.9050471915601));
#236259=CARTESIAN_POINT('Ctrl Pts',(42.5057433597907,31.7910081916521,-46.8895657522793));
#236260=CARTESIAN_POINT('Ctrl Pts',(42.5102196649355,31.2660288392693,-46.8589419567237));
#236261=CARTESIAN_POINT('Ctrl Pts',(42.562075607615,31.0114537827581,-46.8440917450939));
#236262=CARTESIAN_POINT('Ctrl Pts',(42.7601309479512,30.534330462305,-46.8162595514008));
#236263=CARTESIAN_POINT('Ctrl Pts',(42.9050384650336,30.3165894795373,-46.803563577602));
#236264=CARTESIAN_POINT('Ctrl Pts',(43.2735836319553,29.9447670489314,-46.7741005372179));
#236265=CARTESIAN_POINT('Ctrl Pts',(43.4950547252714,29.7957735283593,-46.7585665832752));
#236266=CARTESIAN_POINT('Ctrl Pts',(43.9739264157574,29.5963476757081,-46.7285582847079));
#236267=CARTESIAN_POINT('Ctrl Pts',(44.2253522821904,29.5442282597518,-46.714336565805));
#236268=CARTESIAN_POINT('Ctrl Pts',(44.4892092169482,29.540518289395,-46.7008987945092));
#236269=CARTESIAN_POINT('Ctrl Pts',(44.4985822109721,29.5404524382925,-46.7004233675475));
#236270=CARTESIAN_POINT('Ctrl Pts',(44.5079524583208,29.5404524382925,-46.69995));
#236271=CARTESIAN_POINT('Ctrl Pts',(44.5079524583209,29.5404524382925,-46.5412));
#236272=CARTESIAN_POINT('Ctrl Pts',(44.2750206967325,29.5404524382925,-46.5529672813349));
#236273=CARTESIAN_POINT('Ctrl Pts',(44.0436171059898,29.5811375043278,-46.5658440100673));
#236274=CARTESIAN_POINT('Ctrl Pts',(43.5779919124455,29.750534099846,-46.5943072668012));
#236275=CARTESIAN_POINT('Ctrl Pts',(43.3517741508507,29.8876095534671,-46.609733403351));
#236276=CARTESIAN_POINT('Ctrl Pts',(42.9714833604573,30.2353018099163,-46.6390860141403));
#236277=CARTESIAN_POINT('Ctrl Pts',(42.818754593579,30.4401216450187,-46.652014037059));
#236278=CARTESIAN_POINT('Ctrl Pts',(42.5925962041125,30.9066167014663,-46.6792262486851));
#236279=CARTESIAN_POINT('Ctrl Pts',(42.5255342845323,31.165868982169,-46.6943492983927));
#236280=CARTESIAN_POINT('Ctrl Pts',(42.4967479823186,31.689168175235,-46.7248750846549));
#236281=CARTESIAN_POINT('Ctrl Pts',(42.5328765237534,31.9480765534914,-46.7399780733865));
#236282=CARTESIAN_POINT('Ctrl Pts',(42.7008159887872,32.4347037634724,-46.7683646606355));
#236283=CARTESIAN_POINT('Ctrl Pts',(42.829848466505,32.6582156684402,-46.7806933874648));
#236284=CARTESIAN_POINT('Ctrl Pts',(43.1719235907866,33.05234873328,-46.8094699371344));
#236285=CARTESIAN_POINT('Ctrl Pts',(43.384684326379,33.216474148881,-46.8250052068699));
#236286=CARTESIAN_POINT('Ctrl Pts',(43.8528598735983,33.4473812640628,-46.8553913595732));
#236287=CARTESIAN_POINT('Ctrl Pts',(44.1020841695862,33.5155053329076,-46.8699686615892));
#236288=CARTESIAN_POINT('Ctrl Pts',(44.6200649949416,33.5546051745818,-46.8972765059215));
#236289=CARTESIAN_POINT('Ctrl Pts',(44.8840707818497,33.5223592468335,-46.9107285194261));
#236290=CARTESIAN_POINT('Ctrl Pts',(45.3838357237967,33.3575576767724,-46.9407824314656));
#236291=CARTESIAN_POINT('Ctrl Pts',(45.614731468157,33.2268929751676,-46.9562579107765));
#236292=CARTESIAN_POINT('Ctrl Pts',(46.0057124495535,32.8898748150369,-46.9858392424137));
#236293=CARTESIAN_POINT('Ctrl Pts',(46.1644228605177,32.6894824020146,-46.9991732521161));
#236294=CARTESIAN_POINT('Ctrl Pts',(46.4040654050629,32.2297076493302,-47.0259934460227));
#236295=CARTESIAN_POINT('Ctrl Pts',(46.4786262665402,31.9725573608446,-47.0409938795177));
#236296=CARTESIAN_POINT('Ctrl Pts',(46.5226958109817,31.449637970827,-47.0714975106021));
#236297=CARTESIAN_POINT('Ctrl Pts',(46.493898287438,31.189061856118,-47.0866977839601));
#236298=CARTESIAN_POINT('Ctrl Pts',(46.3397733179045,30.6982423831808,-47.1153289198815));
#236299=CARTESIAN_POINT('Ctrl Pts',(46.2177618156812,30.4720738797123,-47.1276513048442));
#236300=CARTESIAN_POINT('Ctrl Pts',(45.8876915650157,30.0681936211219,-47.1561056836762));
#236301=CARTESIAN_POINT('Ctrl Pts',(45.6791589195109,29.8974451963977,-47.171620529228));
#236302=CARTESIAN_POINT('Ctrl Pts',(45.2164325021904,29.6526125191079,-47.2021375642057));
#236303=CARTESIAN_POINT('Ctrl Pts',(44.9685222274539,29.5773440563874,-47.2168568624556));
#236304=CARTESIAN_POINT('Ctrl Pts',(44.6448390387497,29.5439616914782,-47.2341823901768));
#236305=CARTESIAN_POINT('Ctrl Pts',(44.5763581149533,29.5404524382925,-47.2377442728763));
#236306=CARTESIAN_POINT('Ctrl Pts',(44.5079524583212,29.5404524382925,-47.2412));
#236307=CARTESIAN_POINT('Origin',(44.5079524583208,31.5404524382925,235.35105));
#236308=CARTESIAN_POINT('',(44.5079524583208,29.5404524382925,-45.8412));
#236309=CARTESIAN_POINT('',(44.5079524583207,29.5404524382925,-45.99995));
#236310=CARTESIAN_POINT('',(44.5079524583208,29.5404524382925,235.35105));
#236311=CARTESIAN_POINT('Ctrl Pts',(44.5079524583208,29.5404524382925,-46.69995));
#236312=CARTESIAN_POINT('Ctrl Pts',(44.7634221597085,29.5404524382925,-46.6870441436742));
#236313=CARTESIAN_POINT('Ctrl Pts',(45.0167079303015,29.589399365833,-46.6728209967688));
#236314=CARTESIAN_POINT('Ctrl Pts',(45.4963350804654,29.782246040072,-46.642966426481));
#236315=CARTESIAN_POINT('Ctrl Pts',(45.7172167440047,29.9261789443176,-46.6276098507489));
#236316=CARTESIAN_POINT('Ctrl Pts',(46.0856905776233,30.2854618785066,-46.5985161493034));
#236317=CARTESIAN_POINT('Ctrl Pts',(46.2318559769274,30.4952754861833,-46.5859186555397));
#236318=CARTESIAN_POINT('Ctrl Pts',(46.4428749117245,30.9691110291161,-46.5582782488686));
#236319=CARTESIAN_POINT('Ctrl Pts',(46.5014952445848,31.230443724509,-46.5430338416374));
#236320=CARTESIAN_POINT('Ctrl Pts',(46.5132438034276,31.7536367431509,-46.5125142488833));
#236321=CARTESIAN_POINT('Ctrl Pts',(46.4690172667149,32.0104450524192,-46.497533764176));
#236322=CARTESIAN_POINT('Ctrl Pts',(46.2856638918802,32.4922730914056,-46.4694271285685));
#236323=CARTESIAN_POINT('Ctrl Pts',(46.1486110958527,32.7128281891428,-46.4569720773777));
#236324=CARTESIAN_POINT('Ctrl Pts',(45.7930339387648,33.0957325445022,-46.4278409340355));
#236325=CARTESIAN_POINT('Ctrl Pts',(45.5757221827446,33.2522295367099,-46.4122982508562));
#236326=CARTESIAN_POINT('Ctrl Pts',(45.1018590604176,33.4672095852471,-46.3820893118325));
#236327=CARTESIAN_POINT('Ctrl Pts',(44.8513900654416,33.5272115751659,-46.3676860238968));
#236328=CARTESIAN_POINT('Ctrl Pts',(44.330293025855,33.5502718640802,-46.3406885744799));
#236329=CARTESIAN_POINT('Ctrl Pts',(44.0644745713705,33.5087845471091,-46.3266226714005));
#236330=CARTESIAN_POINT('Ctrl Pts',(43.5689284293712,33.3256133365383,-46.2962461041419));
#236331=CARTESIAN_POINT('Ctrl Pts',(43.3435189490481,33.1874693230036,-46.2808296341347));
#236332=CARTESIAN_POINT('Ctrl Pts',(42.9650423651914,32.8379837252207,-46.2515163679118));
#236333=CARTESIAN_POINT('Ctrl Pts',(42.8133241594923,32.6324043451684,-46.2386471945678));
#236334=CARTESIAN_POINT('Ctrl Pts',(42.5894737850909,32.1647760861673,-46.2113688794594));
#236335=CARTESIAN_POINT('Ctrl Pts',(42.5236977456312,31.9051875424995,-46.1962262144121));
#236336=CARTESIAN_POINT('Ctrl Pts',(42.4975180126245,31.3818684021613,-46.1656992645591));
#236337=CARTESIAN_POINT('Ctrl Pts',(42.5348905306986,31.1232648562457,-46.150614057714));
#236338=CARTESIAN_POINT('Ctrl Pts',(42.7051865878793,30.6373624998062,-46.1222697535884));
#236339=CARTESIAN_POINT('Ctrl Pts',(42.8354315571282,30.4143037868051,-46.1099299903446));
#236340=CARTESIAN_POINT('Ctrl Pts',(43.1795641666072,30.0218623401139,-46.0810988391948));
#236341=CARTESIAN_POINT('Ctrl Pts',(43.3930324959205,29.8588870252188,-46.0655613677385));
#236342=CARTESIAN_POINT('Ctrl Pts',(43.8621051556262,29.6303887290692,-46.0352001517952));
#236343=CARTESIAN_POINT('Ctrl Pts',(44.1115351985903,29.5634963830909,-46.0206483810731));
#236344=CARTESIAN_POINT('Ctrl Pts',(44.4138625005384,29.5421105897467,-46.0047516132155));
#236345=CARTESIAN_POINT('Ctrl Pts',(44.4609318630954,29.5404524382925,-46.0023253934147));
#236346=CARTESIAN_POINT('Ctrl Pts',(44.5079524583205,29.5404524382925,-45.99995));
#236347=CARTESIAN_POINT('Ctrl Pts',(44.5079524583208,29.5404524382925,-45.8412));
#236348=CARTESIAN_POINT('Ctrl Pts',(44.5022154716987,29.5404524382925,-45.8414898219425));
#236349=CARTESIAN_POINT('Ctrl Pts',(44.4964774825353,29.5404771230488,-45.8417804145034));
#236350=CARTESIAN_POINT('Ctrl Pts',(44.225628805887,29.5428083781725,-45.8555311831271));
#236351=CARTESIAN_POINT('Ctrl Pts',(43.9636532182773,29.5977804007479,-45.870369055438));
#236352=CARTESIAN_POINT('Ctrl Pts',(43.4805739512511,29.8048301744746,-45.9008122773467));
#236353=CARTESIAN_POINT('Ctrl Pts',(43.2634245578498,29.9532995605386,-45.9161126197545));
#236354=CARTESIAN_POINT('Ctrl Pts',(42.9030110735591,30.3203699883661,-45.9450262625065));
#236355=CARTESIAN_POINT('Ctrl Pts',(42.7613022043802,30.5336564165181,-45.9574702320632));
#236356=CARTESIAN_POINT('Ctrl Pts',(42.5597712766962,31.0147940314356,-45.9855365929333));
#236357=CARTESIAN_POINT('Ctrl Pts',(42.5069794217426,31.2800702513212,-46.0010110390933));
#236358=CARTESIAN_POINT('Ctrl Pts',(42.5089148690073,31.8053205179484,-46.0316506379799));
#236359=CARTESIAN_POINT('Ctrl Pts',(42.5595843952006,32.0602593978939,-46.0465220726434));
#236360=CARTESIAN_POINT('Ctrl Pts',(42.7553405708373,32.538126635987,-46.0743976615322));
#236361=CARTESIAN_POINT('Ctrl Pts',(42.8990060877282,32.7563080204026,-46.0870481293797));
#236362=CARTESIAN_POINT('Ctrl Pts',(43.2655180517756,33.1298881303849,-46.1164597217674));
#236363=CARTESIAN_POINT('Ctrl Pts',(43.4863511240968,33.2800693374361,-46.1319960849263));
#236364=CARTESIAN_POINT('Ctrl Pts',(43.9644676206521,33.4819499974019,-46.1620378310411));
#236365=CARTESIAN_POINT('Ctrl Pts',(44.2157591859519,33.5353102708598,-46.1762889569765));
#236366=CARTESIAN_POINT('Ctrl Pts',(44.7353185376449,33.5450827675422,-46.2028211646412));
#236367=CARTESIAN_POINT('Ctrl Pts',(44.9987537971474,33.4973500700066,-46.2172515273537));
#236368=CARTESIAN_POINT('Ctrl Pts',(45.4881296745936,33.3032641670339,-46.247634729466));
#236369=CARTESIAN_POINT('Ctrl Pts',(45.7097790220382,33.1602900195349,-46.2630021234292));
#236370=CARTESIAN_POINT('Ctrl Pts',(46.0799306317879,32.802639931508,-46.2921329583388));
#236371=CARTESIAN_POINT('Ctrl Pts',(46.2270254294274,32.5935422094754,-46.3047697633476));
#236372=CARTESIAN_POINT('Ctrl Pts',(46.44020931316,32.1207428492108,-46.3323497260297));
#236373=CARTESIAN_POINT('Ctrl Pts',(46.5000374921706,31.8596895511266,-46.3475778350846));
#236374=CARTESIAN_POINT('Ctrl Pts',(46.5142132434518,31.336447266412,-46.378100301693));
#236375=CARTESIAN_POINT('Ctrl Pts',(46.471135563201,31.0793242663112,-46.3930991433656));
#236376=CARTESIAN_POINT('Ctrl Pts',(46.2899800201273,30.5968035588861,-46.421246184632));
#236377=CARTESIAN_POINT('Ctrl Pts',(46.1540839723624,30.3758276835107,-46.4336753723152));
#236378=CARTESIAN_POINT('Ctrl Pts',(45.8004382557608,29.9912982794807,-46.4627563401128));
#236379=CARTESIAN_POINT('Ctrl Pts',(45.5837639785997,29.8336984212671,-46.4782989859655));
#236380=CARTESIAN_POINT('Ctrl Pts',(45.110685309495,29.6164229725457,-46.5085352450368));
#236381=CARTESIAN_POINT('Ctrl Pts',(44.8603789999663,29.5552536172194,-46.5229643625627));
#236382=CARTESIAN_POINT('Ctrl Pts',(44.5728436713501,29.5412413009968,-46.5378988075647));
#236383=CARTESIAN_POINT('Ctrl Pts',(44.5403843976071,29.5404524382925,-46.5395615984733));
#236384=CARTESIAN_POINT('Ctrl Pts',(44.5079524583209,29.5404524382925,-46.5412));
#236385=CARTESIAN_POINT('Origin',(44.5079524583208,31.5404524382925,235.35105));
#236386=CARTESIAN_POINT('',(44.5079524583206,29.5404524382925,-45.1412));
#236387=CARTESIAN_POINT('',(44.5079524583207,29.5404524382925,-45.29995));
#236388=CARTESIAN_POINT('',(44.5079524583208,29.5404524382925,235.35105));
#236389=CARTESIAN_POINT('Ctrl Pts',(44.5079524583205,29.5404524382925,-45.99995));
#236390=CARTESIAN_POINT('Ctrl Pts',(44.7240341783058,29.5404524382924,-45.98903395157));
#236391=CARTESIAN_POINT('Ctrl Pts',(44.938983568184,29.5754617603926,-45.9771540011326));
#236392=CARTESIAN_POINT('Ctrl Pts',(45.3934223399187,29.7280193428665,-45.9497469995979));
#236393=CARTESIAN_POINT('Ctrl Pts',(45.6235066166138,29.8598248835729,-45.9342792396572));
#236394=CARTESIAN_POINT('Ctrl Pts',(46.0126086329668,30.1987326944784,-45.904737715041));
#236395=CARTESIAN_POINT('Ctrl Pts',(46.1702640354104,30.3998975962579,-45.8914823657854));
#236396=CARTESIAN_POINT('Ctrl Pts',(46.4075506261196,30.8608586977112,-45.8645929682006));
#236397=CARTESIAN_POINT('Ctrl Pts',(46.4808032996821,31.1183931583427,-45.8495701246638));
#236398=CARTESIAN_POINT('Ctrl Pts',(46.5221964566864,31.6414114969648,-45.8190607215775));
#236399=CARTESIAN_POINT('Ctrl Pts',(46.4921105345372,31.9017103260244,-45.8038766232157));
#236400=CARTESIAN_POINT('Ctrl Pts',(46.3355658352113,32.3918035295961,-45.7752878530074));
#236401=CARTESIAN_POINT('Ctrl Pts',(46.2123360749619,32.6175049280227,-45.7629716071216));
#236402=CARTESIAN_POINT('Ctrl Pts',(45.8801698696392,33.0196993788101,-45.7344605139352));
#236403=CARTESIAN_POINT('Ctrl Pts',(45.6708872053655,33.1893026908311,-45.7189411779443));
#236404=CARTESIAN_POINT('Ctrl Pts',(45.2071836024942,33.4317209591311,-45.6884451976239));
#236405=CARTESIAN_POINT('Ctrl Pts',(44.9590301385519,33.5057478068633,-45.6737498276761));
#236406=CARTESIAN_POINT('Ctrl Pts',(44.4433865345556,33.556442345961,-45.6462218767648));
#236407=CARTESIAN_POINT('Ctrl Pts',(44.1806495873855,33.5307494348343,-45.6331322606765));
#236408=CARTESIAN_POINT('Ctrl Pts',(43.6780573849142,33.3791104429147,-45.6033194291989));
#236409=CARTESIAN_POINT('Ctrl Pts',(43.443372877091,33.2539440762327,-45.5878129166744));
#236410=CARTESIAN_POINT('Ctrl Pts',(43.0434688824404,32.92598197317,-45.558044945926));
#236411=CARTESIAN_POINT('Ctrl Pts',(42.8797237890234,32.7292280437918,-45.5442952436542));
#236412=CARTESIAN_POINT('Ctrl Pts',(42.62897202752,32.2751157560239,-45.5178053602011));
#236413=CARTESIAN_POINT('Ctrl Pts',(42.5482579097413,32.0198732233237,-45.5029162124602));
#236414=CARTESIAN_POINT('Ctrl Pts',(42.4915404084121,31.4976079376924,-45.4724507374651));
#236415=CARTESIAN_POINT('Ctrl Pts',(42.5142226926513,31.2358064071097,-45.4571789815144));
#236416=CARTESIAN_POINT('Ctrl Pts',(42.6569030502025,30.7415984948477,-45.4283501866325));
#236417=CARTESIAN_POINT('Ctrl Pts',(42.7732157490531,30.5132084208191,-45.4159577362715));
#236418=CARTESIAN_POINT('Ctrl Pts',(43.0934140220219,30.1014750791851,-45.3877730232199));
#236419=CARTESIAN_POINT('Ctrl Pts',(43.2983488591958,29.9253979250698,-45.3722845110099));
#236420=CARTESIAN_POINT('Ctrl Pts',(43.7563294483999,29.6692920033258,-45.3416784235187));
#236421=CARTESIAN_POINT('Ctrl Pts',(44.0030174043805,29.5882097547967,-45.3268513057966));
#236422=CARTESIAN_POINT('Ctrl Pts',(44.3412934170194,29.5456546263191,-45.3085210366905));
#236423=CARTESIAN_POINT('Ctrl Pts',(44.4246638835946,29.5404524382925,-45.3041575845909));
#236424=CARTESIAN_POINT('Ctrl Pts',(44.5079524583205,29.5404524382925,-45.29995));
#236425=CARTESIAN_POINT('Ctrl Pts',(44.5079524583204,29.5404524382925,-45.1412));
#236426=CARTESIAN_POINT('Ctrl Pts',(44.453989401799,29.5404524382925,-45.1439261137058));
#236427=CARTESIAN_POINT('Ctrl Pts',(44.3999676844034,29.5426363555454,-45.1467188884369));
#236428=CARTESIAN_POINT('Ctrl Pts',(44.090661592359,29.5677625605685,-45.16307730719));
#236429=CARTESIAN_POINT('Ctrl Pts',(43.8416942855719,29.6373763353863,-45.1776850763449));
#236430=CARTESIAN_POINT('Ctrl Pts',(43.3746203408012,29.8711936598925,-45.2081004592373));
#236431=CARTESIAN_POINT('Ctrl Pts',(43.1627237662458,30.0367068232225,-45.2236325491326));
#236432=CARTESIAN_POINT('Ctrl Pts',(42.823140996294,30.4328820248057,-45.2523427519976));
#236433=CARTESIAN_POINT('Ctrl Pts',(42.6955750254693,30.6569419248553,-45.2646618867162));
#236434=CARTESIAN_POINT('Ctrl Pts',(42.5304948927697,31.1444459730064,-45.2930996228583));
#236435=CARTESIAN_POINT('Ctrl Pts',(42.4958786190386,31.4037163382607,-45.3082237274982));
#236436=CARTESIAN_POINT('Ctrl Pts',(42.5278284712106,31.9269737719412,-45.3387470777962));
#236437=CARTESIAN_POINT('Ctrl Pts',(42.5964483318677,32.1858092253091,-45.353845812576));
#236438=CARTESIAN_POINT('Ctrl Pts',(42.8254044147858,32.6509239144061,-45.3809775027733));
#236439=CARTESIAN_POINT('Ctrl Pts',(42.9793632085116,32.8548238030901,-45.393980999241));
#236440=CARTESIAN_POINT('Ctrl Pts',(43.3624287974014,33.2008437030265,-45.4234250106547));
#236441=CARTESIAN_POINT('Ctrl Pts',(43.5903791368553,33.3368878869678,-45.4389085952233));
#236442=CARTESIAN_POINT('Ctrl Pts',(44.0769545501717,33.5098428398493,-45.468534003695));
#236443=CARTESIAN_POINT('Ctrl Pts',(44.3297006140375,33.5485402683169,-45.481959151808));
#236444=CARTESIAN_POINT('Ctrl Pts',(44.8478603800196,33.5291141275632,-45.5087022196127));
#236445=CARTESIAN_POINT('Ctrl Pts',(45.1081882037782,33.4665837408536,-45.5236773022318));
#236446=CARTESIAN_POINT('Ctrl Pts',(45.5844612835644,33.2459261732775,-45.5541735821497));
#236447=CARTESIAN_POINT('Ctrl Pts',(45.79670482814,33.091789441947,-45.569391387728));
#236448=CARTESIAN_POINT('Ctrl Pts',(46.146743368762,32.7148297512957,-45.5980693443669));
#236449=CARTESIAN_POINT('Ctrl Pts',(46.2827292336687,32.4969875397012,-45.6104021190845));
#236450=CARTESIAN_POINT('Ctrl Pts',(46.4702393518327,32.0102802668572,-45.6387933766671));
#236451=CARTESIAN_POINT('Ctrl Pts',(46.5153592165028,31.7444046244669,-45.6543027891398));
#236452=CARTESIAN_POINT('Ctrl Pts',(46.4988869912188,31.220870303568,-45.6848422911923));
#236453=CARTESIAN_POINT('Ctrl Pts',(46.4414444257323,30.9680918530516,-45.6995877008058));
#236454=CARTESIAN_POINT('Ctrl Pts',(46.2324918331374,30.4945357045964,-45.7272118094657));
#236455=CARTESIAN_POINT('Ctrl Pts',(46.0816270318465,30.2788872737542,-45.7401631914179));
#236456=CARTESIAN_POINT('Ctrl Pts',(45.7034218547755,29.9155231302639,-45.7698675375889));
#236457=CARTESIAN_POINT('Ctrl Pts',(45.4789928828164,29.7722287266809,-45.7853846938386));
#236458=CARTESIAN_POINT('Ctrl Pts',(45.0018909428738,29.5865698837846,-45.8149020501006));
#236459=CARTESIAN_POINT('Ctrl Pts',(44.7559254591354,29.5404524382925,-45.8286728631075));
#236460=CARTESIAN_POINT('Ctrl Pts',(44.5079524583208,29.5404524382925,-45.8412));
#236461=CARTESIAN_POINT('Origin',(44.5079524583208,31.5404524382925,235.35105));
#236462=CARTESIAN_POINT('',(44.5079524583207,29.5404524382925,-44.4412));
#236463=CARTESIAN_POINT('',(44.5079524583208,29.5404524382925,-44.59995));
#236464=CARTESIAN_POINT('',(44.5079524583208,29.5404524382925,235.35105));
#236465=CARTESIAN_POINT('Ctrl Pts',(44.5079524583205,29.5404524382925,-45.29995));
#236466=CARTESIAN_POINT('Ctrl Pts',(44.6831064556053,29.5404524382924,-45.2911015443453));
#236467=CARTESIAN_POINT('Ctrl Pts',(44.857829962428,29.5634544131417,-45.2816039453387));
#236468=CARTESIAN_POINT('Ctrl Pts',(45.2827974821138,29.6778151885987,-45.2567998504311));
#236469=CARTESIAN_POINT('Ctrl Pts',(45.5217970209404,29.7963450607897,-45.241268914952));
#236470=CARTESIAN_POINT('Ctrl Pts',(45.9320530989472,30.1133579785335,-45.2112973273572));
#236471=CARTESIAN_POINT('Ctrl Pts',(46.1018169346224,30.3058251526975,-45.1971075467743));
#236472=CARTESIAN_POINT('Ctrl Pts',(46.3655141983934,30.7532564348906,-45.1707359701659));
#236473=CARTESIAN_POINT('Ctrl Pts',(46.4534091422272,31.0061103541599,-45.1561199549078));
#236474=CARTESIAN_POINT('Ctrl Pts',(46.524869168667,31.5274239240777,-45.1257099966626));
#236475=CARTESIAN_POINT('Ctrl Pts',(46.5093574179189,31.7904741309232,-45.1103654012633));
#236476=CARTESIAN_POINT('Ctrl Pts',(46.3800267025948,32.2885362423146,-45.0813117780989));
#236477=CARTESIAN_POINT('Ctrl Pts',(46.2702368122052,32.5195472051907,-45.0687537454164));
#236478=CARTESIAN_POINT('Ctrl Pts',(45.9632621065272,32.9377470444799,-45.04104845632));
#236479=CARTESIAN_POINT('Ctrl Pts',(45.7653451545317,33.1181992899511,-45.0257868678448));
#236480=CARTESIAN_POINT('Ctrl Pts',(45.3168711128907,33.3876739989669,-44.9952711105735));
#236481=CARTESIAN_POINT('Ctrl Pts',(45.0720361186089,33.4765347030518,-44.9803107294253));
#236482=CARTESIAN_POINT('Ctrl Pts',(44.5625491782828,33.5562348996007,-44.9522478034216));
#236483=CARTESIAN_POINT('Ctrl Pts',(44.302783322966,33.5465111301388,-44.9397619469871));
#236484=CARTESIAN_POINT('Ctrl Pts',(43.7938723662163,33.4273407412923,-44.9105769046652));
#236485=CARTESIAN_POINT('Ctrl Pts',(43.5503786996964,33.3162040114379,-44.8950345674939));
#236486=CARTESIAN_POINT('Ctrl Pts',(43.1290006863336,33.0113526575919,-44.8648558325969));
#236487=CARTESIAN_POINT('Ctrl Pts',(42.9528100966551,32.8236637893987,-44.850480751558));
#236488=CARTESIAN_POINT('Ctrl Pts',(42.6742198811008,32.3822500725316,-44.823532322921));
#236489=CARTESIAN_POINT('Ctrl Pts',(42.5783605788317,32.1303218393198,-44.8093590483934));
#236490=CARTESIAN_POINT('Ctrl Pts',(42.4920585623774,31.6087392769756,-44.7789333989233));
#236491=CARTESIAN_POINT('Ctrl Pts',(42.5004277129626,31.344643696309,-44.7635278233844));
#236492=CARTESIAN_POINT('Ctrl Pts',(42.6165141486793,30.8428644390454,-44.7342573667107));
#236493=CARTESIAN_POINT('Ctrl Pts',(42.7199543360269,30.6092172883687,-44.7214486628838));
#236494=CARTESIAN_POINT('Ctrl Pts',(43.015322549558,30.1831022028816,-44.6940988509345));
#236495=CARTESIAN_POINT('Ctrl Pts',(43.2082534171648,29.9973759763086,-44.6789353257623));
#236496=CARTESIAN_POINT('Ctrl Pts',(43.6497916133081,29.7154905600108,-44.6484079756019));
#236497=CARTESIAN_POINT('Ctrl Pts',(43.8928167802752,29.619890520246,-44.6333424596215));
#236498=CARTESIAN_POINT('Ctrl Pts',(44.266572491274,29.5513737199171,-44.6124626064141));
#236499=CARTESIAN_POINT('Ctrl Pts',(44.3872684849238,29.5404524382925,-44.6060467308962));
#236500=CARTESIAN_POINT('Ctrl Pts',(44.5079524583208,29.5404524382925,-44.59995));
#236501=CARTESIAN_POINT('Ctrl Pts',(44.5079524583206,29.5404524382925,-44.4412));
#236502=CARTESIAN_POINT('Ctrl Pts',(44.4179560317545,29.5404524382925,-44.4457464528466));
#236503=CARTESIAN_POINT('Ctrl Pts',(44.3278798180189,29.5465262057059,-44.4504740879429));
#236504=CARTESIAN_POINT('Ctrl Pts',(43.9831082131655,29.5934338475753,-44.4692594506486));
#236505=CARTESIAN_POINT('Ctrl Pts',(43.7370151701557,29.6771307723575,-44.4841327758596));
#236506=CARTESIAN_POINT('Ctrl Pts',(43.2812609719127,29.9382893707129,-44.514773759936));
#236507=CARTESIAN_POINT('Ctrl Pts',(43.0779906547877,30.1167451235776,-44.5302475594717));
#236508=CARTESIAN_POINT('Ctrl Pts',(42.7622648760976,30.5319904552972,-44.5583087634371));
#236509=CARTESIAN_POINT('Ctrl Pts',(42.6485142554119,30.7613997407827,-44.5707552593119));
#236510=CARTESIAN_POINT('Ctrl Pts',(42.5110459693418,31.2571251269908,-44.5996725735074));
#236511=CARTESIAN_POINT('Ctrl Pts',(42.4911590580502,31.5194374102933,-44.6149741233667));
#236512=CARTESIAN_POINT('Ctrl Pts',(42.5536279591984,32.0413032991974,-44.6454163002194));
#236513=CARTESIAN_POINT('Ctrl Pts',(42.6371243081353,32.2956279523115,-44.6602519049844));
#236514=CARTESIAN_POINT('Ctrl Pts',(42.8929170649657,32.7471340129964,-44.6865897585244));
#236515=CARTESIAN_POINT('Ctrl Pts',(43.0589807232594,32.9422382092658,-44.7005527156242));
#236516=CARTESIAN_POINT('Ctrl Pts',(43.4629675598221,33.2660096743689,-44.7304047170464));
#236517=CARTESIAN_POINT('Ctrl Pts',(43.699349010087,33.3886162552127,-44.7459222955409));
#236518=CARTESIAN_POINT('Ctrl Pts',(44.2031855128028,33.534217213492,-44.7756218774485));
#236519=CARTESIAN_POINT('Ctrl Pts',(44.4653512181745,33.5569210687365,-44.7885675291671));
#236520=CARTESIAN_POINT('Ctrl Pts',(44.9798927431999,33.5008773729275,-44.81619582216));
#236521=CARTESIAN_POINT('Ctrl Pts',(45.2275032384634,33.4241205406563,-44.8309433868845));
#236522=CARTESIAN_POINT('Ctrl Pts',(45.6890414504843,33.1763967931192,-44.8614847188126));
#236523=CARTESIAN_POINT('Ctrl Pts',(45.8966665366623,33.0042789598065,-44.8769936572313));
#236524=CARTESIAN_POINT('Ctrl Pts',(46.2242186954592,32.598382047906,-44.9053796457791));
#236525=CARTESIAN_POINT('Ctrl Pts',(46.3447705551076,32.3716503365251,-44.9177134559364));
#236526=CARTESIAN_POINT('Ctrl Pts',(46.4959838624084,31.8799614896161,-44.9463953053395));
#236527=CARTESIAN_POINT('Ctrl Pts',(46.5232288432502,31.6190601159817,-44.9616145521348));
#236528=CARTESIAN_POINT('Ctrl Pts',(46.4759396008089,31.0962780192718,-44.9921101744429));
#236529=CARTESIAN_POINT('Ctrl Pts',(46.3998078168068,30.8395989271094,-45.0070831214857));
#236530=CARTESIAN_POINT('Ctrl Pts',(46.1573336640018,30.3812567907015,-45.0338197461095));
#236531=CARTESIAN_POINT('Ctrl Pts',(45.9973494732639,30.1817923541179,-45.0472526727982));
#236532=CARTESIAN_POINT('Ctrl Pts',(45.6041039612921,29.8470594943569,-45.0768817497333));
#236533=CARTESIAN_POINT('Ctrl Pts',(45.3722364681844,29.7177776170265,-45.0923659876171));
#236534=CARTESIAN_POINT('Ctrl Pts',(44.9232662992318,29.5729351996776,-45.1192716998146));
#236535=CARTESIAN_POINT('Ctrl Pts',(44.7160934399501,29.5404524382924,-45.1306851029699));
#236536=CARTESIAN_POINT('Ctrl Pts',(44.5079524583204,29.5404524382925,-45.1412));
#236537=CARTESIAN_POINT('Origin',(44.5079524583208,31.5404524382925,235.35105));
#236538=CARTESIAN_POINT('',(44.5079524242327,29.5404524382925,-43.7412000034441));
#236539=CARTESIAN_POINT('',(44.5079524583208,29.5404524382925,-43.89995));
#236540=CARTESIAN_POINT('',(44.5079524583208,29.5404524382925,235.35105));
#236541=CARTESIAN_POINT('Ctrl Pts',(44.5079524583208,29.5404524382925,-44.59995));
#236542=CARTESIAN_POINT('Ctrl Pts',(44.642339938529,29.5404524382925,-44.593160993311));
#236543=CARTESIAN_POINT('Ctrl Pts',(44.7766721619236,29.5539942657462,-44.5859798081267));
#236544=CARTESIAN_POINT('Ctrl Pts',(45.1693450251753,29.6343535962872,-44.5637988882803));
#236545=CARTESIAN_POINT('Ctrl Pts',(45.4165147170008,29.7390235784544,-44.5482594585907));
#236546=CARTESIAN_POINT('Ctrl Pts',(45.8471439365854,30.0331498249402,-44.5179261855149));
#236547=CARTESIAN_POINT('Ctrl Pts',(46.028736473741,30.2165750271646,-44.503402565015));
#236548=CARTESIAN_POINT('Ctrl Pts',(46.3176982733281,30.6490097610465,-44.4761920701588));
#236549=CARTESIAN_POINT('Ctrl Pts',(46.4195489627073,30.8957079140314,-44.4625600972487));
#236550=CARTESIAN_POINT('Ctrl Pts',(46.5210517322009,31.4126902081891,-44.4324027967562));
#236551=CARTESIAN_POINT('Ctrl Pts',(46.5204274521103,31.6776992107825,-44.4169439382716));
#236552=CARTESIAN_POINT('Ctrl Pts',(46.4186671045854,32.1833764457246,-44.3874460995666));
#236553=CARTESIAN_POINT('Ctrl Pts',(46.3219722630003,32.4199192153922,-44.3742731409743));
#236554=CARTESIAN_POINT('Ctrl Pts',(46.0390007857604,32.8543077978268,-44.3473082788628));
#236555=CARTESIAN_POINT('Ctrl Pts',(45.8515213356259,33.0454780259863,-44.3322613658288));
#236556=CARTESIAN_POINT('Ctrl Pts',(45.4177261184771,33.3403443524165,-44.3017465667526));
#236557=CARTESIAN_POINT('Ctrl Pts',(45.1768228991778,33.4430640954207,-44.2865805896286));
#236558=CARTESIAN_POINT('Ctrl Pts',(44.6734851563212,33.5498467323824,-44.258038405184));
#236559=CARTESIAN_POINT('Ctrl Pts',(44.4161796862212,33.5545630193631,-44.2457253680806));
#236560=CARTESIAN_POINT('Ctrl Pts',(43.9022440434096,33.4650792961969,-44.2171523490041));
#236561=CARTESIAN_POINT('Ctrl Pts',(43.6514052987463,33.3672998390698,-44.2016285392052));
#236562=CARTESIAN_POINT('Ctrl Pts',(43.2113823922517,33.0846862629223,-44.1711565006768));
#236563=CARTESIAN_POINT('Ctrl Pts',(43.0242473671213,32.9058857393626,-44.1564877704071));
#236564=CARTESIAN_POINT('Ctrl Pts',(42.7245661986959,32.4828630659587,-44.1290102713141));
#236565=CARTESIAN_POINT('Ctrl Pts',(42.6166049835928,32.2414781966625,-44.1158431692384));
#236566=CARTESIAN_POINT('Ctrl Pts',(42.4995716529647,31.7294384786342,-44.0859741856868));
#236567=CARTESIAN_POINT('Ctrl Pts',(42.4921606566817,31.463720544598,-44.070473972868));
#236568=CARTESIAN_POINT('Ctrl Pts',(42.5790686739269,30.9541411633263,-44.0407485089605));
#236569=CARTESIAN_POINT('Ctrl Pts',(42.6688901519482,30.7145457254872,-44.0271004103369));
#236570=CARTESIAN_POINT('Ctrl Pts',(42.9391868848949,30.2718796653486,-44.0005344264075));
#236571=CARTESIAN_POINT('Ctrl Pts',(43.1209684281317,30.0753491108694,-43.9856190182295));
#236572=CARTESIAN_POINT('Ctrl Pts',(43.5465056506158,29.7675167644448,-43.9551432221714));
#236573=CARTESIAN_POINT('Ctrl Pts',(43.7850432714683,29.6576092639034,-43.939887107773));
#236574=CARTESIAN_POINT('Ctrl Pts',(44.1921841661629,29.5591720533483,-43.9164480182645));
#236575=CARTESIAN_POINT('Ctrl Pts',(44.3499432647089,29.5404524382925,-43.9079323319158));
#236576=CARTESIAN_POINT('Ctrl Pts',(44.5079524583209,29.5404524382925,-43.89995));
#236577=CARTESIAN_POINT('Ctrl Pts',(44.5079524241436,29.5404524382925,-43.7412000017266));
#236578=CARTESIAN_POINT('Ctrl Pts',(44.3803294603659,29.5404524404734,-43.7476472776332));
#236579=CARTESIAN_POINT('Ctrl Pts',(44.2527261738062,29.552665552809,-43.754449775196));
#236580=CARTESIAN_POINT('Ctrl Pts',(43.8725994012209,29.6264475978516,-43.7758050522766));
#236581=CARTESIAN_POINT('Ctrl Pts',(43.6303461307986,29.7247231950921,-43.7909096105657));
#236582=CARTESIAN_POINT('Ctrl Pts',(43.1916672495306,30.0115026419363,-43.8214352559901));
#236583=CARTESIAN_POINT('Ctrl Pts',(43.0007627119394,30.1992902156302,-43.8365565373459));
#236584=CARTESIAN_POINT('Ctrl Pts',(42.7100359367441,30.6285242246839,-43.8637628410279));
#236585=CARTESIAN_POINT('Ctrl Pts',(42.6091249039369,30.8632454746232,-43.8766962604526));
#236586=CARTESIAN_POINT('Ctrl Pts',(42.4983798358489,31.3664931807484,-43.9060523766432));
#236587=CARTESIAN_POINT('Ctrl Pts',(42.4928967333233,31.6309557211211,-43.9214793581649));
#236588=CARTESIAN_POINT('Ctrl Pts',(42.5848914825434,32.150843351761,-43.9518061366189));
#236589=CARTESIAN_POINT('Ctrl Pts',(42.6829966663639,32.4008099978702,-43.9657670410182));
#236590=CARTESIAN_POINT('Ctrl Pts',(42.9654575479,32.8388874305972,-43.9928137002469));
#236591=CARTESIAN_POINT('Ctrl Pts',(43.1436679299149,33.0250093423903,-44.00724511456));
#236592=CARTESIAN_POINT('Ctrl Pts',(43.5685156767946,33.3259059398677,-44.0374837869095));
#236593=CARTESIAN_POINT('Ctrl Pts',(43.8133949851612,33.4346525615901,-44.0530264126543));
#236594=CARTESIAN_POINT('Ctrl Pts',(44.3232693350104,33.5484317331885,-44.0821028799755));
#236595=CARTESIAN_POINT('Ctrl Pts',(44.5825690326208,33.5555248442344,-44.094529879345));
#236596=CARTESIAN_POINT('Ctrl Pts',(45.0909771812048,33.4709483696994,-44.1226805315619));
#236597=CARTESIAN_POINT('Ctrl Pts',(45.3351637700046,33.3795900699776,-44.1376810030051));
#236598=CARTESIAN_POINT('Ctrl Pts',(45.7811116310906,33.1055021349579,-44.1682036947369));
#236599=CARTESIAN_POINT('Ctrl Pts',(45.977200356899,32.9230817842003,-44.1834303276808));
#236600=CARTESIAN_POINT('Ctrl Pts',(46.2798872528161,32.5019380996975,-44.2110048667188));
#236601=CARTESIAN_POINT('Ctrl Pts',(46.3873266523313,32.2699612592433,-44.2236453187778));
#236602=CARTESIAN_POINT('Ctrl Pts',(46.5117827927508,31.7705185615192,-44.2527794761451));
#236603=CARTESIAN_POINT('Ctrl Pts',(46.5246684048428,31.5070611576783,-44.2681478247025));
#236604=CARTESIAN_POINT('Ctrl Pts',(46.4478414140236,30.986227172029,-44.2985298071987));
#236605=CARTESIAN_POINT('Ctrl Pts',(46.3573542415884,30.7342562999992,-44.3129523666769));
#236606=CARTESIAN_POINT('Ctrl Pts',(46.0889152695432,30.2892942828932,-44.3394914653767));
#236607=CARTESIAN_POINT('Ctrl Pts',(45.916967928119,30.0984158729122,-44.353745213672));
#236608=CARTESIAN_POINT('Ctrl Pts',(45.502919501942,29.7854643750258,-44.3837899255959));
#236609=CARTESIAN_POINT('Ctrl Pts',(45.2623788433696,29.6694109472359,-44.3993264859628));
#236610=CARTESIAN_POINT('Ctrl Pts',(44.8430821442132,29.5615471791281,-44.4236546054688));
#236611=CARTESIAN_POINT('Ctrl Pts',(44.6756872488009,29.5404524382924,-44.4327263489368));
#236612=CARTESIAN_POINT('Ctrl Pts',(44.5079524583206,29.5404524382925,-44.4412));
#236613=CARTESIAN_POINT('Origin',(44.5079524583208,31.5404524382925,235.35105));
#236614=CARTESIAN_POINT('',(44.5079524583209,29.5404524382925,-43.0412));
#236615=CARTESIAN_POINT('',(44.507952458321,29.5404524382925,-43.19995));
#236616=CARTESIAN_POINT('',(44.5079524583208,29.5404524382925,235.35105));
#236617=CARTESIAN_POINT('Ctrl Pts',(44.5079524583209,29.5404524382925,-43.89995));
#236618=CARTESIAN_POINT('Ctrl Pts',(44.603059908934,29.5404524382925,-43.8951453476813));
#236619=CARTESIAN_POINT('Ctrl Pts',(44.6982377848346,29.547235565763,-43.8901392963898));
#236620=CARTESIAN_POINT('Ctrl Pts',(45.0574337791752,29.5989155974678,-43.8704860455296));
#236621=CARTESIAN_POINT('Ctrl Pts',(45.3117580344694,29.689679706868,-43.8549907684955));
#236622=CARTESIAN_POINT('Ctrl Pts',(45.7608770804952,29.9604869064725,-43.8244035624881));
#236623=CARTESIAN_POINT('Ctrl Pts',(45.9534396256205,30.1344968411654,-43.8096003694657));
#236624=CARTESIAN_POINT('Ctrl Pts',(46.2637198088779,30.5480801576235,-43.7818627423445));
#236625=CARTESIAN_POINT('Ctrl Pts',(46.3776550531411,30.7843111631185,-43.769058241052));
#236626=CARTESIAN_POINT('Ctrl Pts',(46.5098623795721,31.291290795844,-43.739484429143));
#236627=CARTESIAN_POINT('Ctrl Pts',(46.5252340649997,31.5574746018566,-43.7239570404589));
#236628=CARTESIAN_POINT('Ctrl Pts',(46.4530799665626,32.0706154970375,-43.6940238215734));
#236629=CARTESIAN_POINT('Ctrl Pts',(46.3700330713194,32.3133027105304,-43.679867067453));
#236630=CARTESIAN_POINT('Ctrl Pts',(46.1121178894357,32.76391200395,-43.6535815253368));
#236631=CARTESIAN_POINT('Ctrl Pts',(45.9360480411527,32.9655352087732,-43.6388631639973));
#236632=CARTESIAN_POINT('Ctrl Pts',(45.5187506415874,33.2858295266088,-43.6084401543713));
#236633=CARTESIAN_POINT('Ctrl Pts',(45.2827087082266,33.4026601704208,-43.5931081924722));
#236634=CARTESIAN_POINT('Ctrl Pts',(44.7860837297113,33.5371928248204,-43.5640957489453));
#236635=CARTESIAN_POINT('Ctrl Pts',(44.5309508061643,33.5563352546136,-43.5515750827623));
#236636=CARTESIAN_POINT('Ctrl Pts',(44.0155060442822,33.4969435221183,-43.5238035088456));
#236637=CARTESIAN_POINT('Ctrl Pts',(43.7606844094674,33.4144629094121,-43.508524707106));
#236638=CARTESIAN_POINT('Ctrl Pts',(43.3044851377979,33.1585308360496,-43.4780136790564));
#236639=CARTESIAN_POINT('Ctrl Pts',(43.1060554657483,32.9900126717666,-43.4630742662814));
#236640=CARTESIAN_POINT('Ctrl Pts',(42.7841720446195,32.5869171958619,-43.4350563604152));
#236641=CARTESIAN_POINT('Ctrl Pts',(42.6637568048127,32.3562078867747,-43.4225357344948));
#236642=CARTESIAN_POINT('Ctrl Pts',(42.5151465049839,31.8549482478058,-43.3932955888883));
#236643=CARTESIAN_POINT('Ctrl Pts',(42.4910596025346,31.5885214446032,-43.3777540253681));
#236644=CARTESIAN_POINT('Ctrl Pts',(42.5470143797582,31.0717170336357,-43.347607101395));
#236645=CARTESIAN_POINT('Ctrl Pts',(42.6226692072067,30.8257900127035,-43.3332613585073));
#236646=CARTESIAN_POINT('Ctrl Pts',(42.8681218263821,30.3646852855505,-43.3063635827567));
#236647=CARTESIAN_POINT('Ctrl Pts',(43.0398239167052,30.1562018617983,-43.2920764939474));
#236648=CARTESIAN_POINT('Ctrl Pts',(43.4505880991027,29.8227809092919,-43.2616006701789));
#236649=CARTESIAN_POINT('Ctrl Pts',(43.6840525405724,29.6993630562494,-43.2462067914622));
#236650=CARTESIAN_POINT('Ctrl Pts',(44.1209885676691,29.5686285361039,-43.2203205021658));
#236651=CARTESIAN_POINT('Ctrl Pts',(44.3140975965614,29.5404524382925,-43.2097431887043));
#236652=CARTESIAN_POINT('Ctrl Pts',(44.5079524583211,29.5404524382925,-43.19995));
#236653=CARTESIAN_POINT('Ctrl Pts',(44.507952458321,29.5404524382925,-43.0412));
#236654=CARTESIAN_POINT('Ctrl Pts',(44.3428859486929,29.5404524382925,-43.0495388544547));
#236655=CARTESIAN_POINT('Ctrl Pts',(44.1781468636118,29.5608813377326,-43.0584570109277));
#236656=CARTESIAN_POINT('Ctrl Pts',(43.7649541967093,29.6654079696292,-43.0823794328861));
#236657=CARTESIAN_POINT('Ctrl Pts',(43.5273568621061,29.7779947973286,-43.0976661928062));
#236658=CARTESIAN_POINT('Ctrl Pts',(43.1050131171097,30.0906239217968,-43.1281205663205));
#236659=CARTESIAN_POINT('Ctrl Pts',(42.9254061612222,30.2891170907883,-43.1429833612949));
#236660=CARTESIAN_POINT('Ctrl Pts',(42.6598793539486,30.7348529120131,-43.1693979121089));
#236661=CARTESIAN_POINT('Ctrl Pts',(42.5726418801136,30.9756224182398,-43.1832515821635));
#236662=CARTESIAN_POINT('Ctrl Pts',(42.4913795134358,31.486646825032,-43.2130613392264));
#236663=CARTESIAN_POINT('Ctrl Pts',(42.5018432963734,31.7525710885968,-43.2285735879343));
#236664=CARTESIAN_POINT('Ctrl Pts',(42.624719030887,32.2626892444508,-43.2583304803591));
#236665=CARTESIAN_POINT('Ctrl Pts',(42.7349791408251,32.5020849505867,-43.2713469521728));
#236666=CARTESIAN_POINT('Ctrl Pts',(43.0387262026938,32.9215023104342,-43.298924697696));
#236667=CARTESIAN_POINT('Ctrl Pts',(43.2279501527227,33.0984906909758,-43.3136461024127));
#236668=CARTESIAN_POINT('Ctrl Pts',(43.6714863524154,33.3766246271964,-43.3441649698443));
#236669=CARTESIAN_POINT('Ctrl Pts',(43.9236795714655,33.4717364109192,-43.3596793980406));
#236670=CARTESIAN_POINT('Ctrl Pts',(44.4385215547572,33.555409714008,-43.3881287331745));
#236671=CARTESIAN_POINT('Ctrl Pts',(44.6953769497797,33.5478762279429,-43.4004518111039));
#236672=CARTESIAN_POINT('Ctrl Pts',(45.197449818442,33.4357242928857,-43.4290867009739));
#236673=CARTESIAN_POINT('Ctrl Pts',(45.4374779135517,33.3302642656819,-43.4442883933999));
#236674=CARTESIAN_POINT('Ctrl Pts',(45.8681775614868,33.03043806965,-43.4747914729141));
#236675=CARTESIAN_POINT('Ctrl Pts',(46.053507925471,32.8372080082199,-43.4897898965651));
#236676=CARTESIAN_POINT('Ctrl Pts',(46.3316672499433,32.3996557394439,-43.5166039318131));
#236677=CARTESIAN_POINT('Ctrl Pts',(46.4257506445691,32.1619652677515,-43.5299450849482));
#236678=CARTESIAN_POINT('Ctrl Pts',(46.5218971753613,31.6547961984845,-43.5595299473221));
#236679=CARTESIAN_POINT('Ctrl Pts',(46.5194842072782,31.3894908419828,-43.575006093118));
#236680=CARTESIAN_POINT('Ctrl Pts',(46.4120838797738,30.8743568889704,-43.6050555737104));
#236681=CARTESIAN_POINT('Ctrl Pts',(46.3079122710583,30.6296804578189,-43.6185002122192));
#236682=CARTESIAN_POINT('Ctrl Pts',(46.014894866714,30.200790903147,-43.6458121876587));
#236683=CARTESIAN_POINT('Ctrl Pts',(45.8311998526572,30.0190893402774,-43.6603917485845));
#236684=CARTESIAN_POINT('Ctrl Pts',(45.396995209647,29.7292679042007,-43.6907800884619));
#236685=CARTESIAN_POINT('Ctrl Pts',(45.1484211192914,29.6271804045484,-43.7063151433583));
#236686=CARTESIAN_POINT('Ctrl Pts',(44.7618975791812,29.5525429758403,-43.7280185219813));
#236687=CARTESIAN_POINT('Ctrl Pts',(44.6349332753986,29.5404524361225,-43.7347851641561));
#236688=CARTESIAN_POINT('Ctrl Pts',(44.5079524241435,29.5404524382925,-43.7412000017266));
#236689=CARTESIAN_POINT('Origin',(44.5079524583208,31.5404524382925,235.35105));
#236690=CARTESIAN_POINT('',(44.507952458321,29.5404524382925,-42.3412));
#236691=CARTESIAN_POINT('',(44.5079524583208,29.5404524382925,-42.49995));
#236692=CARTESIAN_POINT('',(44.5079524583208,29.5404524382925,235.35105));
#236693=CARTESIAN_POINT('Ctrl Pts',(44.5079524583211,29.5404524382925,-43.19995));
#236694=CARTESIAN_POINT('Ctrl Pts',(44.5665991045952,29.5404524382925,-43.1969872800113));
#236695=CARTESIAN_POINT('Ctrl Pts',(44.6253064126613,29.5430318780239,-43.1939462618424));
#236696=CARTESIAN_POINT('Ctrl Pts',(44.9481088323641,29.5715417421349,-43.176807343547));
#236697=CARTESIAN_POINT('Ctrl Pts',(45.2050074234444,29.6471957029399,-43.1616227285026));
#236698=CARTESIAN_POINT('Ctrl Pts',(45.6684267639518,29.8911636944158,-43.1310959083313));
#236699=CARTESIAN_POINT('Ctrl Pts',(45.8717274789806,30.0548560670756,-43.1160511717391));
#236700=CARTESIAN_POINT('Ctrl Pts',(46.203386444063,30.4489875554122,-43.0878008731286));
#236701=CARTESIAN_POINT('Ctrl Pts',(46.3292265161237,30.6751460267372,-43.0754262073408));
#236702=CARTESIAN_POINT('Ctrl Pts',(46.4914873929182,31.1714524684933,-43.0464749982383));
#236703=CARTESIAN_POINT('Ctrl Pts',(46.5229035490332,31.437869230895,-43.0309340204315));
#236704=CARTESIAN_POINT('Ctrl Pts',(46.480645147573,31.9573565188901,-43.0006305952985));
#236705=CARTESIAN_POINT('Ctrl Pts',(46.4112771461008,32.2058257980606,-42.9861365540135));
#236706=CARTESIAN_POINT('Ctrl Pts',(46.1786137650572,32.6713828596358,-42.958979058755));
#236707=CARTESIAN_POINT('Ctrl Pts',(46.0143711622087,32.8824162231044,-42.9452442068107));
#236708=CARTESIAN_POINT('Ctrl Pts',(45.6150407712465,33.2266213567624,-42.9150314583995));
#236709=CARTESIAN_POINT('Ctrl Pts',(45.3845803766436,33.3571348728264,-42.8995823817306));
#236710=CARTESIAN_POINT('Ctrl Pts',(44.8949905975828,33.5189286620772,-42.8701302270217));
#236711=CARTESIAN_POINT('Ctrl Pts',(44.6416231755321,33.5519820788101,-42.8570390783313));
#236712=CARTESIAN_POINT('Ctrl Pts',(44.1241290834013,33.5211110601426,-42.829995830198));
#236713=CARTESIAN_POINT('Ctrl Pts',(43.8652150613394,33.4528260772934,-42.8149243278356));
#236714=CARTESIAN_POINT('Ctrl Pts',(43.3944144468747,33.221897208872,-42.7844049271258));
#236715=CARTESIAN_POINT('Ctrl Pts',(43.1860250669658,33.0635256619809,-42.7692583113568));
#236716=CARTESIAN_POINT('Ctrl Pts',(42.8439847575439,32.6790416055694,-42.7407649498819));
#236717=CARTESIAN_POINT('Ctrl Pts',(42.7124082776733,32.4576181754678,-42.7284513346686));
#236718=CARTESIAN_POINT('Ctrl Pts',(42.5358196918728,31.9666908278183,-42.6998139060558));
#236719=CARTESIAN_POINT('Ctrl Pts',(42.4966476923776,31.7004968805927,-42.6842859258009));
#236720=CARTESIAN_POINT('Ctrl Pts',(42.524340301447,31.178564329912,-42.6538398603445));
#236721=CARTESIAN_POINT('Ctrl Pts',(42.5869861387273,30.9275852584862,-42.6391994145114));
#236722=CARTESIAN_POINT('Ctrl Pts',(42.8062031762079,30.4574517210543,-42.6117749581612));
#236723=CARTESIAN_POINT('Ctrl Pts',(42.9627882462913,30.2437875024397,-42.5985227745748));
#236724=CARTESIAN_POINT('Ctrl Pts',(43.3501233460486,29.8885876489612,-42.5685953267386));
#236725=CARTESIAN_POINT('Ctrl Pts',(43.5772339468994,29.7507639672093,-42.5531022622821));
#236726=CARTESIAN_POINT('Ctrl Pts',(44.0437613891552,29.5811257564053,-42.5245863785012));
#236727=CARTESIAN_POINT('Ctrl Pts',(44.2750608700149,29.5404524382925,-42.511715251855));
#236728=CARTESIAN_POINT('Ctrl Pts',(44.5079524583208,29.5404524382925,-42.49995));
#236729=CARTESIAN_POINT('Ctrl Pts',(44.5079524583211,29.5404524382925,-42.3412));
#236730=CARTESIAN_POINT('Ctrl Pts',(44.3067852482428,29.5404524382925,-42.3513625950029));
#236731=CARTESIAN_POINT('Ctrl Pts',(44.1064975352776,29.5707947521519,-42.3623657435942));
#236732=CARTESIAN_POINT('Ctrl Pts',(43.6637830034297,29.7085277257708,-42.3887480738117));
#236733=CARTESIAN_POINT('Ctrl Pts',(43.4314436034151,29.8346697873297,-42.4041645735987));
#236734=CARTESIAN_POINT('Ctrl Pts',(43.02504561223,30.1722454089543,-42.4345410033202));
#236735=CARTESIAN_POINT('Ctrl Pts',(42.8562112397984,30.3817086260739,-42.4486066109538));
#236736=CARTESIAN_POINT('Ctrl Pts',(42.6156402274143,30.8445243871565,-42.4756041970169));
#236737=CARTESIAN_POINT('Ctrl Pts',(42.5423722700094,31.091439238053,-42.4900075633192));
#236738=CARTESIAN_POINT('Ctrl Pts',(42.4916260697972,31.6093081936101,-42.5202165857267));
#236739=CARTESIAN_POINT('Ctrl Pts',(42.5185044057893,31.8757541979105,-42.5357592693109));
#236740=CARTESIAN_POINT('Ctrl Pts',(42.6723278910724,32.3751426374909,-42.5648902616198));
#236741=CARTESIAN_POINT('Ctrl Pts',(42.7948106555084,32.6041089980684,-42.5773452309046));
#236742=CARTESIAN_POINT('Ctrl Pts',(43.120414414186,33.0038070068886,-42.6054519885459));
#236743=CARTESIAN_POINT('Ctrl Pts',(43.3207062234586,33.1705099476173,-42.6204325290254));
#236744=CARTESIAN_POINT('Ctrl Pts',(43.7796827487293,33.4219256547043,-42.6509521314353));
#236745=CARTESIAN_POINT('Ctrl Pts',(44.0353147676662,33.5018217336608,-42.666196490046));
#236746=CARTESIAN_POINT('Ctrl Pts',(44.5511784166266,33.5559845339382,-42.6938367148393));
#236747=CARTESIAN_POINT('Ctrl Pts',(44.8059645593044,33.5343048854853,-42.7064343232118));
#236748=CARTESIAN_POINT('Ctrl Pts',(45.3013478971403,33.3948318195729,-42.7355281366863));
#236749=CARTESIAN_POINT('Ctrl Pts',(45.5364369445363,33.2755056929497,-42.7508847454659));
#236750=CARTESIAN_POINT('Ctrl Pts',(45.9506404016502,32.9507645573285,-42.7812811536996));
#236751=CARTESIAN_POINT('Ctrl Pts',(46.1246470852223,32.7473180417129,-42.795799506467));
#236752=CARTESIAN_POINT('Ctrl Pts',(46.3780443384741,32.2937985562453,-42.822254809786));
#236753=CARTESIAN_POINT('Ctrl Pts',(46.4586171008651,32.0499961352609,-42.8364766176767));
#236754=CARTESIAN_POINT('Ctrl Pts',(46.5253375612345,31.5355664158354,-42.8664850179766));
#236755=CARTESIAN_POINT('Ctrl Pts',(46.5070368788851,31.2692699282744,-42.8820189797509));
#236756=CARTESIAN_POINT('Ctrl Pts',(46.3692941445005,30.764191883341,-42.9114818657054));
#236757=CARTESIAN_POINT('Ctrl Pts',(46.2531756622305,30.5298303795275,-42.9241776983054));
#236758=CARTESIAN_POINT('Ctrl Pts',(45.9389970183727,30.1197526296116,-42.9520100227475));
#236759=CARTESIAN_POINT('Ctrl Pts',(45.7444537874955,29.9475590727496,-42.9668602986604));
#236760=CARTESIAN_POINT('Ctrl Pts',(45.2920419459663,29.6811989986307,-42.9974841427735));
#236761=CARTESIAN_POINT('Ctrl Pts',(45.0364736653742,29.5930647429175,-43.0129655615965));
#236762=CARTESIAN_POINT('Ctrl Pts',(44.6836956983711,29.5462378354539,-43.0321530361411));
#236763=CARTESIAN_POINT('Ctrl Pts',(44.5957863231696,29.5404524382925,-43.0367627957675));
#236764=CARTESIAN_POINT('Ctrl Pts',(44.507952458321,29.5404524382925,-43.0412));
#236765=CARTESIAN_POINT('Origin',(44.5079524583208,31.5404524382925,235.35105));
#236766=CARTESIAN_POINT('',(44.5079524583208,29.5404524382925,-41.6412));
#236767=CARTESIAN_POINT('',(44.5079524583208,29.5404524382925,-41.79995));
#236768=CARTESIAN_POINT('',(44.5079524583208,29.5404524382925,235.35105));
#236769=CARTESIAN_POINT('Ctrl Pts',(44.5079524583208,29.5404524382925,-42.49995));
#236770=CARTESIAN_POINT('Ctrl Pts',(44.5281915482536,29.5404524382925,-42.4989275586482));
#236771=CARTESIAN_POINT('Ctrl Pts',(44.5484417718872,29.540759652605,-42.497895594425));
#236772=CARTESIAN_POINT('Ctrl Pts',(44.8337286956703,29.5494283529019,-42.4832305901368));
#236773=CARTESIAN_POINT('Ctrl Pts',(45.0944824477049,29.610105155334,-42.4682880532845));
#236774=CARTESIAN_POINT('Ctrl Pts',(45.5724645023405,29.8274378483818,-42.4378024146283));
#236775=CARTESIAN_POINT('Ctrl Pts',(45.7859274646337,29.9801957566941,-42.422563221996));
#236776=CARTESIAN_POINT('Ctrl Pts',(46.1385233715512,30.354731520291,-42.3938267698192));
#236777=CARTESIAN_POINT('Ctrl Pts',(46.2759191572335,30.5714415107971,-42.3814756374373));
#236778=CARTESIAN_POINT('Ctrl Pts',(46.4669005030961,31.0567856226139,-42.3531638975813));
#236779=CARTESIAN_POINT('Ctrl Pts',(46.5139163692276,31.3225329220241,-42.3376619717824));
#236780=CARTESIAN_POINT('Ctrl Pts',(46.5010299700797,31.8465280017547,-42.3070955921314));
#236781=CARTESIAN_POINT('Ctrl Pts',(46.4452548083671,32.0998571912959,-42.2923180560748));
#236782=CARTESIAN_POINT('Ctrl Pts',(46.23956736931,32.5744893336426,-42.2646311811046));
#236783=CARTESIAN_POINT('Ctrl Pts',(46.0904999084609,32.7907659112026,-42.2517632242203));
#236784=CARTESIAN_POINT('Ctrl Pts',(45.7151930054219,33.1566867337951,-42.2221307236802));
#236785=CARTESIAN_POINT('Ctrl Pts',(45.4916386210013,33.3017007381006,-42.2066075949526));
#236786=CARTESIAN_POINT('Ctrl Pts',(45.0101917985323,33.4929784639923,-42.1767068591824));
#236787=CARTESIAN_POINT('Ctrl Pts',(44.7583465761211,33.5409006655415,-42.162612520535));
#236788=CARTESIAN_POINT('Ctrl Pts',(44.2392900816279,33.5399780585633,-42.136363838068));
#236789=CARTESIAN_POINT('Ctrl Pts',(43.9769576015324,33.486801213419,-42.1215602955512));
#236790=CARTESIAN_POINT('Ctrl Pts',(43.4923247293002,33.2830028017046,-42.0911334197759));
#236791=CARTESIAN_POINT('Ctrl Pts',(43.2740359223536,33.1358969078494,-42.0758152848281));
#236792=CARTESIAN_POINT('Ctrl Pts',(42.9111780813867,32.7711782445811,-42.0468467508355));
#236793=CARTESIAN_POINT('Ctrl Pts',(42.7681190298049,32.5589509546727,-42.0343624134556));
#236794=CARTESIAN_POINT('Ctrl Pts',(42.5643848417266,32.081662414282,-42.0065205819328));
#236795=CARTESIAN_POINT('Ctrl Pts',(42.5098289559704,31.8194338258323,-41.9912239142732));
#236796=CARTESIAN_POINT('Ctrl Pts',(42.5062223419112,31.2964890670197,-41.9607188033425));
#236797=CARTESIAN_POINT('Ctrl Pts',(42.5542911162574,31.0407740716014,-41.9458020952764));
#236798=CARTESIAN_POINT('Ctrl Pts',(42.7450244417216,30.5612921769914,-41.9178323180909));
#236799=CARTESIAN_POINT('Ctrl Pts',(42.8859943698823,30.3421493374886,-41.9052711458869));
#236800=CARTESIAN_POINT('Ctrl Pts',(43.2480710190736,29.9647613371827,-41.8759725539261));
#236801=CARTESIAN_POINT('Ctrl Pts',(43.467493951482,29.8120037073267,-41.8604322827597));
#236802=CARTESIAN_POINT('Ctrl Pts',(43.9439239948383,29.6047886635623,-41.830320146944));
#236803=CARTESIAN_POINT('Ctrl Pts',(44.1949022099252,29.5487278530391,-41.8160060852168));
#236804=CARTESIAN_POINT('Ctrl Pts',(44.4691115548922,29.5407351434851,-41.8019204160975));
#236805=CARTESIAN_POINT('Ctrl Pts',(44.4885374707127,29.5404524382925,-41.8009308092281));
#236806=CARTESIAN_POINT('Ctrl Pts',(44.5079524583208,29.5404524382925,-41.79995));
#236807=CARTESIAN_POINT('Ctrl Pts',(44.5079524583208,29.5404524382925,-41.6412));
#236808=CARTESIAN_POINT('Ctrl Pts',(44.2672514934039,29.5404524382925,-41.6533597671028));
#236809=CARTESIAN_POINT('Ctrl Pts',(44.0283515184313,29.5839018714322,-41.6666958266611));
#236810=CARTESIAN_POINT('Ctrl Pts',(43.5562868000569,29.7617686632792,-41.69573144366));
#236811=CARTESIAN_POINT('Ctrl Pts',(43.3305491677514,29.9024320466283,-41.7112379729174));
#236812=CARTESIAN_POINT('Ctrl Pts',(42.9479362256659,30.2618758672077,-41.7410506484646));
#236813=CARTESIAN_POINT('Ctrl Pts',(42.7943210334294,30.4765676682521,-41.7541400550808));
#236814=CARTESIAN_POINT('Ctrl Pts',(42.5804091612362,30.9484777886012,-41.7816681454345));
#236815=CARTESIAN_POINT('Ctrl Pts',(42.5204451959738,31.2003996722857,-41.7963635886494));
#236816=CARTESIAN_POINT('Ctrl Pts',(42.4985416134286,31.7231890228391,-41.8268596340984));
#236817=CARTESIAN_POINT('Ctrl Pts',(42.5407852138562,31.9892345588435,-41.842378957032));
#236818=CARTESIAN_POINT('Ctrl Pts',(42.7230203528376,32.4779932068023,-41.8708898781629));
#236819=CARTESIAN_POINT('Ctrl Pts',(42.8568716981678,32.6975615073306,-41.8832061380639));
#236820=CARTESIAN_POINT('Ctrl Pts',(43.2030381015716,33.0781745372596,-41.9117950372284));
#236821=CARTESIAN_POINT('Ctrl Pts',(43.4134232315287,33.2343761643763,-41.9269791852681));
#236822=CARTESIAN_POINT('Ctrl Pts',(43.8870707998596,33.4600306290821,-41.9574885720412));
#236823=CARTESIAN_POINT('Ctrl Pts',(44.1467295085273,33.5253551614776,-41.9725113481206));
#236824=CARTESIAN_POINT('Ctrl Pts',(44.664577292091,33.5503314990797,-41.9994005358924));
#236825=CARTESIAN_POINT('Ctrl Pts',(44.9176184749323,33.5143764221844,-42.0126561191544));
#236826=CARTESIAN_POINT('Ctrl Pts',(45.4056701495064,33.3468502962067,-42.0421977648269));
#236827=CARTESIAN_POINT('Ctrl Pts',(45.634857478873,33.2134903728229,-42.0576655488106));
#236828=CARTESIAN_POINT('Ctrl Pts',(46.029544062124,32.8649914031207,-42.0877689375386));
#236829=CARTESIAN_POINT('Ctrl Pts',(46.1908023739995,32.6529352518331,-42.10130516921));
#236830=CARTESIAN_POINT('Ctrl Pts',(46.4182646419594,32.1855953946261,-42.1285666608804));
#236831=CARTESIAN_POINT('Ctrl Pts',(46.4850456536318,31.9361351339568,-42.1431185094195));
#236832=CARTESIAN_POINT('Ctrl Pts',(46.5216889813397,31.4156558332057,-42.1734798019633));
#236833=CARTESIAN_POINT('Ctrl Pts',(46.4872782951218,31.1492992840176,-42.1890172673326));
#236834=CARTESIAN_POINT('Ctrl Pts',(46.31947278005,30.6550538068162,-42.2178482535027));
#236835=CARTESIAN_POINT('Ctrl Pts',(46.1914177283946,30.4307314959853,-42.2301879788846));
#236836=CARTESIAN_POINT('Ctrl Pts',(45.8557565048388,30.0403046812106,-42.2585324112043));
#236837=CARTESIAN_POINT('Ctrl Pts',(45.6504828371936,29.8786401490778,-42.2736176723612));
#236838=CARTESIAN_POINT('Ctrl Pts',(45.1841813937079,29.6396597414361,-42.3041446198437));
#236839=CARTESIAN_POINT('Ctrl Pts',(44.9264820266832,29.5668330656511,-42.3192872261264));
#236840=CARTESIAN_POINT('Ctrl Pts',(44.6107093301824,29.5424301869479,-42.3359512287464));
#236841=CARTESIAN_POINT('Ctrl Pts',(44.5593051412479,29.5404524382925,-42.3386057575353));
#236842=CARTESIAN_POINT('Ctrl Pts',(44.5079524583211,29.5404524382925,-42.3412));
#236843=CARTESIAN_POINT('Origin',(44.5079524583208,31.5404524382925,235.35105));
#236844=CARTESIAN_POINT('',(44.5079524583208,29.5404524382925,-40.9412));
#236845=CARTESIAN_POINT('',(44.5079524583206,29.5404524382925,-41.09995));
#236846=CARTESIAN_POINT('',(44.5079524583208,29.5404524382925,235.35105));
#236847=CARTESIAN_POINT('Ctrl Pts',(44.5079524583208,29.5404524382925,-41.79995));
#236848=CARTESIAN_POINT('Ctrl Pts',(44.753283869434,29.5404524382925,-41.7875563113284));
#236849=CARTESIAN_POINT('Ctrl Pts',(44.9967396162526,29.58558799845,-41.7739409239064));
#236850=CARTESIAN_POINT('Ctrl Pts',(45.4701984701951,29.7677506117743,-41.7447095829667));
#236851=CARTESIAN_POINT('Ctrl Pts',(45.693504501057,29.908624585447,-41.7293197514945));
#236852=CARTESIAN_POINT('Ctrl Pts',(46.0673014950109,30.2627124837551,-41.7001086557242));
#236853=CARTESIAN_POINT('Ctrl Pts',(46.2164182255828,30.4702627635807,-41.6873777310249));
#236854=CARTESIAN_POINT('Ctrl Pts',(46.4342882217952,30.9408037405067,-41.6599295073709));
#236855=CARTESIAN_POINT('Ctrl Pts',(46.4967302934578,31.2012315980501,-41.6447378823475));
#236856=CARTESIAN_POINT('Ctrl Pts',(46.5161707857634,31.7245417365144,-41.6142114576038));
#236857=CARTESIAN_POINT('Ctrl Pts',(46.4755905046121,31.9823295990548,-41.5991738322889));
#236858=CARTESIAN_POINT('Ctrl Pts',(46.2991994999433,32.4663423599117,-41.5709397545723));
#236859=CARTESIAN_POINT('Ctrl Pts',(46.1657958992151,32.6882311279318,-41.5585576361121));
#236860=CARTESIAN_POINT('Ctrl Pts',(45.8163303102628,33.0762557531885,-41.5295858966716));
#236861=CARTESIAN_POINT('Ctrl Pts',(45.6010513151848,33.2362292669554,-41.5140445062661));
#236862=CARTESIAN_POINT('Ctrl Pts',(45.1297039593719,33.4584532284062,-41.4837513783156));
#236863=CARTESIAN_POINT('Ctrl Pts',(44.8797674055392,33.5221428655078,-41.4692674319445));
#236864=CARTESIAN_POINT('Ctrl Pts',(44.3600710535679,33.5524997240187,-41.4421279260594));
#236865=CARTESIAN_POINT('Ctrl Pts',(44.095084372802,33.5152425638956,-41.4283573807194));
#236866=CARTESIAN_POINT('Ctrl Pts',(43.5975734914173,33.340450392492,-41.3981259471071));
#236867=CARTESIAN_POINT('Ctrl Pts',(43.369633415828,33.2056893646584,-41.3826803065285));
#236868=CARTESIAN_POINT('Ctrl Pts',(42.9854456376923,32.8618668253909,-41.3532436938847));
#236869=CARTESIAN_POINT('Ctrl Pts',(42.8305419303208,32.6586702709936,-41.3401793735744));
#236870=CARTESIAN_POINT('Ctrl Pts',(42.5994453267602,32.1946166682982,-41.3131095800838));
#236871=CARTESIAN_POINT('Ctrl Pts',(42.5296341191085,31.9361069541665,-41.2980298467594));
#236872=CARTESIAN_POINT('Ctrl Pts',(42.495261037926,31.412894521579,-41.2675091215251));
#236873=CARTESIAN_POINT('Ctrl Pts',(42.5287171011554,31.1533528012335,-41.2523691878383));
#236874=CARTESIAN_POINT('Ctrl Pts',(42.6916071169511,30.6651803505833,-41.2238924615504));
#236875=CARTESIAN_POINT('Ctrl Pts',(42.8180545809363,30.4407001078993,-41.2115777357079));
#236876=CARTESIAN_POINT('Ctrl Pts',(43.1557309418803,30.042969513371,-41.1829184754688));
#236877=CARTESIAN_POINT('Ctrl Pts',(43.3669616425938,29.8763993374101,-41.1673891947521));
#236878=CARTESIAN_POINT('Ctrl Pts',(43.8331823775542,29.6403626770763,-41.1369521838113));
#236879=CARTESIAN_POINT('Ctrl Pts',(44.0819474833038,29.5696116631542,-41.1223214600046));
#236880=CARTESIAN_POINT('Ctrl Pts',(44.3941587347587,29.5428775963385,-41.1057693820078));
#236881=CARTESIAN_POINT('Ctrl Pts',(44.4510868615659,29.5404524382925,-41.1028227446645));
#236882=CARTESIAN_POINT('Ctrl Pts',(44.5079524583204,29.5404524382924,-41.09995));
#236883=CARTESIAN_POINT('Ctrl Pts',(44.5079524583207,29.5404524382925,-40.9412));
#236884=CARTESIAN_POINT('Ctrl Pts',(44.4816990227574,29.5404524382925,-40.9425262749579));
#236885=CARTESIAN_POINT('Ctrl Pts',(44.4554265546438,29.5409693663035,-40.9438685884719));
#236886=CARTESIAN_POINT('Ctrl Pts',(44.1742025575873,29.5520585347067,-40.9583989382106));
#236887=CARTESIAN_POINT('Ctrl Pts',(43.9235644051612,29.6108031890804,-40.9727740993808));
#236888=CARTESIAN_POINT('Ctrl Pts',(43.448868722049,29.8233085901873,-41.0029529206172));
#236889=CARTESIAN_POINT('Ctrl Pts',(43.230876575762,29.978615301625,-41.0184952593305));
#236890=CARTESIAN_POINT('Ctrl Pts',(42.8732223925083,30.3597649017264,-41.0476801498274));
#236891=CARTESIAN_POINT('Ctrl Pts',(42.7349219704941,30.5798681249784,-41.0601659150567));
#236892=CARTESIAN_POINT('Ctrl Pts',(42.5492075747699,31.0609489748742,-41.0882289646339));
#236893=CARTESIAN_POINT('Ctrl Pts',(42.5037491863373,31.3174136321222,-41.1031894029734));
#236894=CARTESIAN_POINT('Ctrl Pts',(42.5128914807453,31.8405411036034,-41.1337051721431));
#236895=CARTESIAN_POINT('Ctrl Pts',(42.5702129101642,32.1021675131214,-41.1489667126983));
#236896=CARTESIAN_POINT('Ctrl Pts',(42.7789038315715,32.5771121942379,-41.1766718190968));
#236897=CARTESIAN_POINT('Ctrl Pts',(42.9240730637951,32.7876963277406,-41.1892299588978));
#236898=CARTESIAN_POINT('Ctrl Pts',(43.2907472347089,33.148726136872,-41.2182836952346));
#236899=CARTESIAN_POINT('Ctrl Pts',(43.5108018640736,33.2936819270355,-41.233628324904));
#236900=CARTESIAN_POINT('Ctrl Pts',(43.9980058766551,33.4924456941335,-41.2640382461281));
#236901=CARTESIAN_POINT('Ctrl Pts',(44.260932027402,33.5427496462346,-41.2786539832764));
#236902=CARTESIAN_POINT('Ctrl Pts',(44.7802678792263,33.5380892918405,-41.3050257959915));
#236903=CARTESIAN_POINT('Ctrl Pts',(45.0318308817501,33.4872993287206,-41.3192156670481));
#236904=CARTESIAN_POINT('Ctrl Pts',(45.5114979339958,33.2905061605134,-41.3491873591893));
#236905=CARTESIAN_POINT('Ctrl Pts',(45.7336456823359,33.1427878180178,-41.364718303797));
#236906=CARTESIAN_POINT('Ctrl Pts',(46.1043659850929,32.7728543315175,-41.3942361338133));
#236907=CARTESIAN_POINT('Ctrl Pts',(46.2506066901437,32.5555843884028,-41.4069839695767));
#236908=CARTESIAN_POINT('Ctrl Pts',(46.4511194586139,32.0792595436652,-41.4347695855198));
#236909=CARTESIAN_POINT('Ctrl Pts',(46.5042405839542,31.82507926019,-41.4495967687225));
#236910=CARTESIAN_POINT('Ctrl Pts',(46.5114289970589,31.3004026013653,-41.4802029071539));
#236911=CARTESIAN_POINT('Ctrl Pts',(46.4614050940075,31.0348855798487,-41.4956914000758));
#236912=CARTESIAN_POINT('Ctrl Pts',(46.2649253314838,30.5517220087559,-41.5238759417228));
#236913=CARTESIAN_POINT('Ctrl Pts',(46.1252870630233,30.3367996096282,-41.5362684576805));
#236914=CARTESIAN_POINT('Ctrl Pts',(45.7686251759153,29.9661360534585,-41.5650973762653));
#236915=CARTESIAN_POINT('Ctrl Pts',(45.5532369682635,29.8155948501023,-41.5803691748342));
#236916=CARTESIAN_POINT('Ctrl Pts',(45.0725796557155,29.6035881876034,-41.6108346200093));
#236917=CARTESIAN_POINT('Ctrl Pts',(44.8111752277478,29.545871382327,-41.6257236945546));
#236918=CARTESIAN_POINT('Ctrl Pts',(44.533371567733,29.5405735432228,-41.6399123414273));
#236919=CARTESIAN_POINT('Ctrl Pts',(44.5206596789984,29.5404524382925,-41.6405580547381));
#236920=CARTESIAN_POINT('Ctrl Pts',(44.5079524583208,29.5404524382925,-41.6412));
#236921=CARTESIAN_POINT('Origin',(44.5079524583208,31.5404524382925,235.35105));
#236922=CARTESIAN_POINT('',(44.5079524583206,29.5404524382925,-40.2412));
#236923=CARTESIAN_POINT('',(44.5079524583207,29.5404524382925,-40.39995));
#236924=CARTESIAN_POINT('',(44.5079524583208,29.5404524382925,235.35105));
#236925=CARTESIAN_POINT('Ctrl Pts',(44.5079524583204,29.5404524382925,-41.09995));
#236926=CARTESIAN_POINT('Ctrl Pts',(44.7127884447251,29.5404524382924,-41.0896020652096));
#236927=CARTESIAN_POINT('Ctrl Pts',(44.9167205496817,29.5719115854782,-41.078382234377));
#236928=CARTESIAN_POINT('Ctrl Pts',(45.3633783085636,29.7135852641125,-41.0516857624007));
#236929=CARTESIAN_POINT('Ctrl Pts',(45.5959805326658,29.8418092860262,-41.0361952613837));
#236930=CARTESIAN_POINT('Ctrl Pts',(45.9909489883467,30.1747975453953,-41.0065300287005));
#236931=CARTESIAN_POINT('Ctrl Pts',(46.1519040618263,30.3735580889598,-40.9930188370445));
#236932=CARTESIAN_POINT('Ctrl Pts',(46.3965269748775,30.8308081927069,-40.9663459143259));
#236933=CARTESIAN_POINT('Ctrl Pts',(46.473849762942,31.0871228318008,-40.9513942270455));
#236934=CARTESIAN_POINT('Ctrl Pts',(46.5235842739099,31.6097873306858,-40.9209054646105));
#236935=CARTESIAN_POINT('Ctrl Pts',(46.4975203039116,31.8709296573216,-40.9056721622234));
#236936=CARTESIAN_POINT('Ctrl Pts',(46.3485189858338,32.363275640451,-40.8769519798742));
#236937=CARTESIAN_POINT('Ctrl Pts',(46.2290714930095,32.5904360952347,-40.8646065570797));
#236938=CARTESIAN_POINT('Ctrl Pts',(45.9034293848198,32.9978564570087,-40.8362726267976));
#236939=CARTESIAN_POINT('Ctrl Pts',(45.6964973846956,33.1710083951975,-40.8207685404109));
#236940=CARTESIAN_POINT('Ctrl Pts',(45.2358707299797,33.4209180536095,-40.7902095029363));
#236941=CARTESIAN_POINT('Ctrl Pts',(44.9884931356865,33.4988014136315,-40.7754408468782));
#236942=CARTESIAN_POINT('Ctrl Pts',(44.4744103511585,33.557050459181,-40.7477714059051));
#236943=CARTESIAN_POINT('Ctrl Pts',(44.212477323953,33.5355728713584,-40.7348808225659));
#236944=CARTESIAN_POINT('Ctrl Pts',(43.7081385544689,33.3924547954086,-40.7052282844723));
#236945=CARTESIAN_POINT('Ctrl Pts',(43.4710669440809,33.2709075220833,-40.6897067368354));
#236946=CARTESIAN_POINT('Ctrl Pts',(43.0654031441697,32.9488661305975,-40.6598204788102));
#236947=CARTESIAN_POINT('Ctrl Pts',(42.8983842260015,32.7544370551136,-40.6457657693148));
#236948=CARTESIAN_POINT('Ctrl Pts',(42.64052838135,32.30400417371,-40.6194905178995));
#236949=CARTESIAN_POINT('Ctrl Pts',(42.5558954333463,32.0500645319282,-40.6046773721289));
#236950=CARTESIAN_POINT('Ctrl Pts',(42.4910710393704,31.5283806464918,-40.5742458121451));
#236951=CARTESIAN_POINT('Ctrl Pts',(42.5098104533401,31.2658675908542,-40.5589325505662));
#236952=CARTESIAN_POINT('Ctrl Pts',(42.645142236704,30.7695248525269,-40.5299792241638));
#236953=CARTESIAN_POINT('Ctrl Pts',(42.7578483998159,30.539696308703,-40.5175066296998));
#236954=CARTESIAN_POINT('Ctrl Pts',(43.0717451965258,30.1230227740392,-40.4894961665986));
#236955=CARTESIAN_POINT('Ctrl Pts',(43.2743287784446,29.9436007811549,-40.4740288776534));
#236956=CARTESIAN_POINT('Ctrl Pts',(43.7291590812721,29.6803859546179,-40.4433745937409));
#236957=CARTESIAN_POINT('Ctrl Pts',(43.9750015604766,29.5956233620597,-40.4284828445726));
#236958=CARTESIAN_POINT('Ctrl Pts',(44.3224079897582,29.5469011967279,-40.409511451814));
#236959=CARTESIAN_POINT('Ctrl Pts',(44.4152191380681,29.5404524382925,-40.4046347156484));
#236960=CARTESIAN_POINT('Ctrl Pts',(44.5079524583206,29.5404524382925,-40.39995));
#236961=CARTESIAN_POINT('Ctrl Pts',(44.5079524583204,29.5404524382925,-40.2412));
#236962=CARTESIAN_POINT('Ctrl Pts',(44.4461937530077,29.5404524382925,-40.2443199354495));
#236963=CARTESIAN_POINT('Ctrl Pts',(44.3843665227043,29.5433128801535,-40.2475267622089));
#236964=CARTESIAN_POINT('Ctrl Pts',(44.0672753494251,29.5728160956729,-40.2644061316585));
#236965=CARTESIAN_POINT('Ctrl Pts',(43.818862770905,29.6454834042868,-40.2790749383708));
#236966=CARTESIAN_POINT('Ctrl Pts',(43.3541037750594,29.885255197537,-40.3095470463346));
#236967=CARTESIAN_POINT('Ctrl Pts',(43.1440072234425,30.0536017892691,-40.3250708440654));
#236968=CARTESIAN_POINT('Ctrl Pts',(42.8095507615993,30.4539465413159,-40.3536436872243));
#236969=CARTESIAN_POINT('Ctrl Pts',(42.6849862659914,30.679139208081,-40.3659567282376));
#236970=CARTESIAN_POINT('Ctrl Pts',(42.5258014009256,31.1684360756242,-40.394499045511));
#236971=CARTESIAN_POINT('Ctrl Pts',(42.4943116988828,31.4284251490941,-40.4096650747967));
#236972=CARTESIAN_POINT('Ctrl Pts',(42.5327841504894,31.9515357506962,-40.4401798598902));
#236973=CARTESIAN_POINT('Ctrl Pts',(42.6046067820175,32.2094816692934,-40.4552267051417));
#236974=CARTESIAN_POINT('Ctrl Pts',(42.8393199349264,32.6717327757373,-40.4821913530176));
#236975=CARTESIAN_POINT('Ctrl Pts',(42.995827829265,32.8737419397183,-40.4953645404819));
#236976=CARTESIAN_POINT('Ctrl Pts',(43.3828828207437,33.2147017651451,-40.524862503615));
#236977=CARTESIAN_POINT('Ctrl Pts',(43.612077751551,33.3477433963758,-40.5403213880883));
#236978=CARTESIAN_POINT('Ctrl Pts',(44.1105508779273,33.5183219887893,-40.5704785364822));
#236979=CARTESIAN_POINT('Ctrl Pts',(44.3751222469798,33.5534614761425,-40.5841102333803));
#236980=CARTESIAN_POINT('Ctrl Pts',(44.8941011422762,33.5194230807133,-40.6113208728427));
#236981=CARTESIAN_POINT('Ctrl Pts',(45.143747689986,33.4538681268884,-40.6258445737125));
#236982=CARTESIAN_POINT('Ctrl Pts',(45.6137803908419,33.227987954367,-40.6561779272182));
#236983=CARTESIAN_POINT('Ctrl Pts',(45.8280099452777,33.0662641489134,-40.6717173519996));
#236984=CARTESIAN_POINT('Ctrl Pts',(46.1743724328927,32.6756638086287,-40.7006074535274));
#236985=CARTESIAN_POINT('Ctrl Pts',(46.3059352902341,32.4530950791237,-40.7129625126182));
#236986=CARTESIAN_POINT('Ctrl Pts',(46.4787821253612,31.9679809190841,-40.7412608386205));
#236987=CARTESIAN_POINT('Ctrl Pts',(46.5174988314685,31.7097139650406,-40.7563264109397));
#236988=CARTESIAN_POINT('Ctrl Pts',(46.4941399869417,31.186387959989,-40.7868537612344));
#236989=CARTESIAN_POINT('Ctrl Pts',(46.4297578284954,30.926442816073,-40.8020172279628));
#236990=CARTESIAN_POINT('Ctrl Pts',(46.2084083392178,30.4575923617246,-40.8293668377998));
#236991=CARTESIAN_POINT('Ctrl Pts',(46.0577809710145,30.2511892981575,-40.842175707883));
#236992=CARTESIAN_POINT('Ctrl Pts',(45.6812650408056,29.8997713426122,-40.8714462859484));
#236993=CARTESIAN_POINT('Ctrl Pts',(45.4567336356385,29.7604789049286,-40.8868518929288));
#236994=CARTESIAN_POINT('Ctrl Pts',(44.9865042082021,29.5836942426894,-40.9157632323138));
#236995=CARTESIAN_POINT('Ctrl Pts',(44.74808715979,29.5404524382924,-40.9290688394782));
#236996=CARTESIAN_POINT('Ctrl Pts',(44.5079524583207,29.5404524382925,-40.9412));
#236997=CARTESIAN_POINT('Origin',(44.5079524583208,31.5404524382925,235.35105));
#236998=CARTESIAN_POINT('',(44.5079524583208,29.5404524382925,-39.5412));
#236999=CARTESIAN_POINT('',(44.5079524583208,29.5404524382925,-39.69995));
#237000=CARTESIAN_POINT('',(44.5079524583208,29.5404524382925,235.35105));
#237001=CARTESIAN_POINT('',(45.8699699536314,30.0759011606612,-39.4567768040287));
#237002=CARTESIAN_POINT('Ctrl Pts',(45.8699695685728,30.075901520304,-39.4567761523991));
#237003=CARTESIAN_POINT('Ctrl Pts',(45.7701107830075,29.9830338890879,-39.4645294726065));
#237004=CARTESIAN_POINT('Ctrl Pts',(45.6610194473437,29.9006263473464,-39.4724441182083));
#237005=CARTESIAN_POINT('Ctrl Pts',(45.4275260895439,29.7591440756338,-39.4883663366023));
#237006=CARTESIAN_POINT('Ctrl Pts',(45.3036963603113,29.7004880778269,-39.4963327851952));
#237007=CARTESIAN_POINT('Ctrl Pts',(44.9604389072844,29.5790802543851,-39.5172145777165));
#237008=CARTESIAN_POINT('Ctrl Pts',(44.7349169043735,29.5404524382924,-39.5297341763978));
#237009=CARTESIAN_POINT('Ctrl Pts',(44.5079524583207,29.5404524382925,-39.5412));
#237010=CARTESIAN_POINT('',(46.1726017293051,30.4318753540615,-39.5898550790525));
#237011=CARTESIAN_POINT('Ctrl Pts',(45.8699698689079,30.0759017996126,-39.4567779390767));
#237012=CARTESIAN_POINT('Ctrl Pts',(45.9271083068064,30.129039973996,-39.4791532819239));
#237013=CARTESIAN_POINT('Ctrl Pts',(45.981085284682,30.1854725512665,-39.5015086752499));
#237014=CARTESIAN_POINT('Ctrl Pts',(46.0821973535923,30.3043921848593,-39.5459690352455));
#237015=CARTESIAN_POINT('Ctrl Pts',(46.129270885215,30.3668095284313,-39.5680428991861));
#237016=CARTESIAN_POINT('Ctrl Pts',(46.1726016483627,30.4318753890564,-39.5898550650905));
#237017=CARTESIAN_POINT('Ctrl Pts',(44.5079524583208,29.5404524382925,-39.69995));
#237018=CARTESIAN_POINT('Ctrl Pts',(44.6319808972993,29.5404524382925,-39.6936843128947));
#237019=CARTESIAN_POINT('Ctrl Pts',(44.7560060404353,29.5519873437279,-39.6870823575476));
#237020=CARTESIAN_POINT('Ctrl Pts',(45.1400567254562,29.6243843292702,-39.6655692492444));
#237021=CARTESIAN_POINT('Ctrl Pts',(45.3891835300754,29.7254372108916,-39.6500364486059));
#237022=CARTESIAN_POINT('Ctrl Pts',(45.8337542537958,30.019451126976,-39.6190021528564));
#237023=CARTESIAN_POINT('Ctrl Pts',(46.024657531644,30.2097211747746,-39.6038085296457));
#237024=CARTESIAN_POINT('Ctrl Pts',(46.1726016676276,30.4318754179848,-39.5898551670461));
#237025=CARTESIAN_POINT('Origin',(-44.5079524583208,31.5404524382925,235.35105));
#237026=CARTESIAN_POINT('',(-44.5079524583208,29.5404524382925,-52.3162000000004));
#237027=CARTESIAN_POINT('',(-44.5079524583208,29.5404524382925,-52.4749499999996));
#237028=CARTESIAN_POINT('',(-44.5079524583208,29.5404524382925,235.35105));
#237029=CARTESIAN_POINT('',(-46.5079524583208,31.5404524382925,-52.64995));
#237030=CARTESIAN_POINT('Ctrl Pts',(-46.5079524583208,31.5404524382925,
-52.6499499999996));
#237031=CARTESIAN_POINT('Ctrl Pts',(-46.5079524583208,31.2923954725884,
-52.6374186213562));
#237032=CARTESIAN_POINT('Ctrl Pts',(-46.4618041379609,31.0465391623049,
-52.6236524230731));
#237033=CARTESIAN_POINT('Ctrl Pts',(-46.2794036058753,30.577598336436,-52.5946423852496));
#237034=CARTESIAN_POINT('Ctrl Pts',(-46.1422160174819,30.3596409234275,
-52.5796302756193));
#237035=CARTESIAN_POINT('Ctrl Pts',(-45.7889072840913,29.9823693960786,
-52.5502663784982));
#237036=CARTESIAN_POINT('Ctrl Pts',(-45.5743499468127,29.8283664394868,
-52.5371565201615));
#237037=CARTESIAN_POINT('Ctrl Pts',(-45.1026718366126,29.6137589726646,
-52.5096419637332));
#237038=CARTESIAN_POINT('Ctrl Pts',(-44.8508720180615,29.5534424514737,
-52.4949536409844));
#237039=CARTESIAN_POINT('Ctrl Pts',(-44.5657020983325,29.5410772302566,
-52.4783187290003));
#237040=CARTESIAN_POINT('Ctrl Pts',(-44.5368153039993,29.5404524382925,
-52.4766336659975));
#237041=CARTESIAN_POINT('Ctrl Pts',(-44.5079524583208,29.5404524382925,
-52.4749499999996));
#237042=CARTESIAN_POINT('',(-44.7865238868864,33.5209569091754,-52.64995));
#237043=CARTESIAN_POINT('Origin',(-44.5079524583208,31.5404524382925,-52.64995));
#237044=CARTESIAN_POINT('Ctrl Pts',(-44.5079524583208,29.5404524382925,
-52.3162000000005));
#237045=CARTESIAN_POINT('Ctrl Pts',(-44.7127351905467,29.5404524382925,
-52.3281456593803));
#237046=CARTESIAN_POINT('Ctrl Pts',(-44.9166514162594,29.5719068831819,
-52.3400407725471));
#237047=CARTESIAN_POINT('Ctrl Pts',(-45.3553832799493,29.7110280003146,
-52.3656334645957));
#237048=CARTESIAN_POINT('Ctrl Pts',(-45.581284963268,29.8337345445251,-52.3779519699644));
#237049=CARTESIAN_POINT('Ctrl Pts',(-45.9842037250954,30.1650012258081,
-52.4064387466005));
#237050=CARTESIAN_POINT('Ctrl Pts',(-46.1542990722659,30.3739626070849,
-52.4219562029942));
#237051=CARTESIAN_POINT('Ctrl Pts',(-46.3977544226486,30.8372481514485,
-52.4524613120001));
#237052=CARTESIAN_POINT('Ctrl Pts',(-46.4723144406481,31.0852979527207,
-52.4671669959012));
#237053=CARTESIAN_POINT('Ctrl Pts',(-46.5240542552125,31.6007273814734,
-52.4947146142767));
#237054=CARTESIAN_POINT('Ctrl Pts',(-46.4989470904135,31.8633519585254,
-52.5077749424954));
#237055=CARTESIAN_POINT('Ctrl Pts',(-46.3484897234824,32.3661902348615,
-52.5375657411067));
#237056=CARTESIAN_POINT('Ctrl Pts',(-46.2238224665166,32.6012088871632,
-52.5530745766248));
#237057=CARTESIAN_POINT('Ctrl Pts',(-45.899615045655,32.9983157068768,-52.5825917277099));
#237058=CARTESIAN_POINT('Ctrl Pts',(-45.707401438058,33.1601177057035,-52.5962321428486));
#237059=CARTESIAN_POINT('Ctrl Pts',(-45.2727931896581,33.405262303546,-52.6215842906718));
#237060=CARTESIAN_POINT('Ctrl Pts',(-45.0339917549731,33.4861488698347,
-52.6355143743617));
#237061=CARTESIAN_POINT('Ctrl Pts',(-44.7865238868852,33.5209569091755,
-52.6499500000001));
#237062=CARTESIAN_POINT('Origin',(-44.5079524583208,31.5404524382925,235.35105));
#237063=CARTESIAN_POINT('',(-44.5079524583208,29.5404524382925,-51.6162000000004));
#237064=CARTESIAN_POINT('',(-44.5079524583208,29.5404524382925,-51.7749499999997));
#237065=CARTESIAN_POINT('',(-44.5079524583208,29.5404524382925,235.35105));
#237066=CARTESIAN_POINT('Ctrl Pts',(-44.5079524583208,29.5404524382925,
-52.4749499999996));
#237067=CARTESIAN_POINT('Ctrl Pts',(-44.2706710647853,29.5404524382925,
-52.4611085853768));
#237068=CARTESIAN_POINT('Ctrl Pts',(-44.0350082364426,29.5826825426037,
-52.4473615870568));
#237069=CARTESIAN_POINT('Ctrl Pts',(-43.5730800140031,29.754114096945,-52.4204157740813));
#237070=CARTESIAN_POINT('Ctrl Pts',(-43.3532689868484,29.8876666859978,
-52.4081007415779));
#237071=CARTESIAN_POINT('Ctrl Pts',(-42.9721462304376,30.233291144132,-52.3795243534628));
#237072=CARTESIAN_POINT('Ctrl Pts',(-42.8156577993954,30.443415036027,-52.3643450375719));
#237073=CARTESIAN_POINT('Ctrl Pts',(-42.5893075901103,30.916691541608,-52.3338341036518));
#237074=CARTESIAN_POINT('Ctrl Pts',(-42.5235932041223,31.176254293647,-52.3188048043939));
#237075=CARTESIAN_POINT('Ctrl Pts',(-42.4978414783645,31.6940568751854,
-52.2918952846569));
#237076=CARTESIAN_POINT('Ctrl Pts',(-42.5334142479843,31.9471402165956,
-52.2786622508692));
#237077=CARTESIAN_POINT('Ctrl Pts',(-42.7001843791251,32.4353959452518,
-52.2491323466117));
#237078=CARTESIAN_POINT('Ctrl Pts',(-42.8331696097481,32.6647531256922,
-52.2336669106051));
#237079=CARTESIAN_POINT('Ctrl Pts',(-43.1811043150024,33.0600529371203,
-52.203549000438));
#237080=CARTESIAN_POINT('Ctrl Pts',(-43.3930257525339,33.2217038791566,
-52.1899873911714));
#237081=CARTESIAN_POINT('Ctrl Pts',(-43.8601310007166,33.4498532621196,
-52.1627395850274));
#237082=CARTESIAN_POINT('Ctrl Pts',(-44.1094617907247,33.5169770097097,
-52.1481952889435));
#237083=CARTESIAN_POINT('Ctrl Pts',(-44.6298133586672,33.5543635583677,
-52.1178414474801));
#237084=CARTESIAN_POINT('Ctrl Pts',(-44.8961797354773,33.5203488950871,
-52.1023034088328));
#237085=CARTESIAN_POINT('Ctrl Pts',(-45.3906990097786,33.3532756557018,
-52.0734564511651));
#237086=CARTESIAN_POINT('Ctrl Pts',(-45.615263401957,33.2255135713542,-52.0611129327868));
#237087=CARTESIAN_POINT('Ctrl Pts',(-46.006181641077,32.8903819778783,-52.0327809231879));
#237088=CARTESIAN_POINT('Ctrl Pts',(-46.1681162515263,32.6853686448247,
-52.0177009363683));
#237089=CARTESIAN_POINT('Ctrl Pts',(-46.407759615724,32.2194460560125,-51.9871737916894));
#237090=CARTESIAN_POINT('Ctrl Pts',(-46.4809614792731,31.9618509727281,
-51.9720255106516));
#237091=CARTESIAN_POINT('Ctrl Pts',(-46.5216593348524,31.4449987360713,
-51.9447280717919));
#237092=CARTESIAN_POINT('Ctrl Pts',(-46.493420758581,31.1910579788034,-51.9318753975487));
#237093=CARTESIAN_POINT('Ctrl Pts',(-46.3411075770592,30.6989699950747,
-51.9025735558905));
#237094=CARTESIAN_POINT('Ctrl Pts',(-46.2153268957618,30.4664793382221,
-51.8871599551457));
#237095=CARTESIAN_POINT('Ctrl Pts',(-45.8783013478925,30.0595004846572,
-51.8567702251501));
#237096=CARTESIAN_POINT('Ctrl Pts',(-45.6689680127052,29.8902859884014,
-51.8426759073385));
#237097=CARTESIAN_POINT('Ctrl Pts',(-45.2063790954135,29.6490654181459,
-51.8156915538299));
#237098=CARTESIAN_POINT('Ctrl Pts',(-44.9595944554625,29.5754789339219,
-51.8012957831661));
#237099=CARTESIAN_POINT('Ctrl Pts',(-44.6398630971928,29.5437110434508,
-51.7826447872671));
#237100=CARTESIAN_POINT('Ctrl Pts',(-44.5738684804503,29.5404524382925,
-51.7787951012905));
#237101=CARTESIAN_POINT('Ctrl Pts',(-44.5079524583208,29.5404524382925,
-51.7749499999997));
#237102=CARTESIAN_POINT('Ctrl Pts',(-44.5079524583208,29.5404524382925,
-51.6162000000004));
#237103=CARTESIAN_POINT('Ctrl Pts',(-44.7495896327406,29.5404524382925,
-51.6302955018416));
#237104=CARTESIAN_POINT('Ctrl Pts',(-44.9894048430363,29.5842459600337,
-51.6442847224424));
#237105=CARTESIAN_POINT('Ctrl Pts',(-45.456284003817,29.7608924187297,-51.6715193401547));
#237106=CARTESIAN_POINT('Ctrl Pts',(-45.6770188246547,29.897450543898,-51.6839630219098));
#237107=CARTESIAN_POINT('Ctrl Pts',(-46.0606183380932,30.2522024107171,
-51.7130727485595));
#237108=CARTESIAN_POINT('Ctrl Pts',(-46.2175870475827,30.4692423383284,
-51.7286154578915));
#237109=CARTESIAN_POINT('Ctrl Pts',(-46.433548589117,30.9427714748038,-51.7588361514474));
#237110=CARTESIAN_POINT('Ctrl Pts',(-46.4940496040989,31.1931715890985,
-51.7732505145562));
#237111=CARTESIAN_POINT('Ctrl Pts',(-46.5180988052615,31.7140804531209,
-51.8002673009658));
#237112=CARTESIAN_POINT('Ctrl Pts',(-46.4771874157357,31.9797855580725,
-51.8142916095523));
#237113=CARTESIAN_POINT('Ctrl Pts',(-46.2951539687465,32.4756025332761,
-51.8446486740316));
#237114=CARTESIAN_POINT('Ctrl Pts',(-46.1574664721582,32.7013583560729,
-51.8600693255417));
#237115=CARTESIAN_POINT('Ctrl Pts',(-45.8087475736808,33.0806111959291,
-51.8893994447173));
#237116=CARTESIAN_POINT('Ctrl Pts',(-45.6034934894683,33.2327616514278,
-51.9022934398498));
#237117=CARTESIAN_POINT('Ctrl Pts',(-45.1363498331127,33.4576002820923,
-51.9295434864704));
#237118=CARTESIAN_POINT('Ctrl Pts',(-44.8769044300919,33.5239269792106,
-51.9446778016465));
#237119=CARTESIAN_POINT('Ctrl Pts',(-44.3535922286762,33.551222433402,-51.975204346729));
#237120=CARTESIAN_POINT('Ctrl Pts',(-44.0948574742939,33.5143821643818,
-51.9902972074012));
#237121=CARTESIAN_POINT('Ctrl Pts',(-43.6086444486617,33.3450948666379,
-52.0186596338964));
#237122=CARTESIAN_POINT('Ctrl Pts',(-43.3853918009882,33.2153695035301,
-52.0309943100544));
#237123=CARTESIAN_POINT('Ctrl Pts',(-42.9922251533322,32.8721179323723,
-52.0598021044742));
#237124=CARTESIAN_POINT('Ctrl Pts',(-42.8287568054832,32.6589519911188,
-52.0753386799734));
#237125=CARTESIAN_POINT('Ctrl Pts',(-42.599226214873,32.1902621614667,-52.1057106646397));
#237126=CARTESIAN_POINT('Ctrl Pts',(-42.5318061633352,31.9409195204642,
-52.1202734113886));
#237127=CARTESIAN_POINT('Ctrl Pts',(-42.4940923139192,31.4226640461013,
-52.1475547057062));
#237128=CARTESIAN_POINT('Ctrl Pts',(-42.527128561288,31.1585040368843,-52.1610546290855));
#237129=CARTESIAN_POINT('Ctrl Pts',(-42.6935102234801,30.6590892925398,
-52.1911369358111));
#237130=CARTESIAN_POINT('Ctrl Pts',(-42.8248272762757,30.4286564703355,
-52.2066080560616));
#237131=CARTESIAN_POINT('Ctrl Pts',(-43.1629254864012,30.0387487135716,
-52.2361666718356));
#237132=CARTESIAN_POINT('Ctrl Pts',(-43.3637588445647,29.8806411062191,
-52.2494553725313));
#237133=CARTESIAN_POINT('Ctrl Pts',(-43.8242114769924,29.6423435096061,
-52.276315109423));
#237134=CARTESIAN_POINT('Ctrl Pts',(-44.0815819548725,29.5685293338514,
-52.2913283872994));
#237135=CARTESIAN_POINT('Ctrl Pts',(-44.3998220308925,29.5426422323627,
-52.309892391734));
#237136=CARTESIAN_POINT('Ctrl Pts',(-44.4539174098103,29.5404524382925,
-52.313047955504));
#237137=CARTESIAN_POINT('Ctrl Pts',(-44.5079524583208,29.5404524382925,
-52.3162000000005));
#237138=CARTESIAN_POINT('Origin',(-44.5079524583208,31.5404524382925,235.35105));
#237139=CARTESIAN_POINT('',(-44.5079524583208,29.5404524382925,-50.9162000000005));
#237140=CARTESIAN_POINT('',(-44.5079524583208,29.5404524382925,-51.0749499999997));
#237141=CARTESIAN_POINT('',(-44.5079524583208,29.5404524382925,235.35105));
#237142=CARTESIAN_POINT('Ctrl Pts',(-44.5079524583208,29.5404524382925,
-51.7749499999996));
#237143=CARTESIAN_POINT('Ctrl Pts',(-44.3097004477224,29.5404524382925,
-51.7633852993815));
#237144=CARTESIAN_POINT('Ctrl Pts',(-44.1121593984864,29.5699326646355,
-51.7518620715094));
#237145=CARTESIAN_POINT('Ctrl Pts',(-43.675780382826,29.7036747192049,-51.7264066289293));
#237146=CARTESIAN_POINT('Ctrl Pts',(-43.4465825171116,29.8258821762405,
-51.7139436252528));
#237147=CARTESIAN_POINT('Ctrl Pts',(-43.0464307373388,30.1509901224479,
-51.6858486801536));
#237148=CARTESIAN_POINT('Ctrl Pts',(-42.8794843611898,30.3510343371154,
-51.6708735474952));
#237149=CARTESIAN_POINT('Ctrl Pts',(-42.6274641193755,30.8096427930648,
-51.6403549070032));
#237150=CARTESIAN_POINT('Ctrl Pts',(-42.5472226233,31.0651682126213,-51.6251058589299));
#237151=CARTESIAN_POINT('Ctrl Pts',(-42.4923620277257,31.5809771092096,
-51.5974480477624));
#237152=CARTESIAN_POINT('Ctrl Pts',(-42.5137028025219,31.8358089353058,
-51.5848614182352));
#237153=CARTESIAN_POINT('Ctrl Pts',(-42.6525151090392,32.3313591732875,
-51.5557784454235));
#237154=CARTESIAN_POINT('Ctrl Pts',(-42.7715078345278,32.5665771817518,
-51.5404250459692));
#237155=CARTESIAN_POINT('Ctrl Pts',(-43.0956557171075,32.9811970848786,
-51.5100249028677));
#237156=CARTESIAN_POINT('Ctrl Pts',(-43.2988594490325,33.1554808273183,
-51.4954804255421));
#237157=CARTESIAN_POINT('Ctrl Pts',(-43.7519921956795,33.4094843772839,
-51.4690476819877));
#237158=CARTESIAN_POINT('Ctrl Pts',(-43.995646870312,33.4903889620451,-51.4548344926341));
#237159=CARTESIAN_POINT('Ctrl Pts',(-44.5099074369239,33.5578374719646,
-51.4248359595817));
#237160=CARTESIAN_POINT('Ctrl Pts',(-44.776190663482,33.539928907508,-51.4093027713657));
#237161=CARTESIAN_POINT('Ctrl Pts',(-45.2815245090258,33.4029258337993,
-51.3798249637089));
#237162=CARTESIAN_POINT('Ctrl Pts',(-45.5161354722425,33.2870992589641,
-51.3671153589855));
#237163=CARTESIAN_POINT('Ctrl Pts',(-45.9266836109983,32.9734425472894,
-51.3392956819162));
#237164=CARTESIAN_POINT('Ctrl Pts',(-46.0991220374941,32.7791639643163,
-51.3244516334945));
#237165=CARTESIAN_POINT('Ctrl Pts',(-46.366080736808,32.3271912353577,-51.2938325126338));
#237166=CARTESIAN_POINT('Ctrl Pts',(-46.4545686056881,32.0717882815627,
-51.2783491320971));
#237167=CARTESIAN_POINT('Ctrl Pts',(-46.5239606482487,31.5548230770405,
-51.2502090725229));
#237168=CARTESIAN_POINT('Ctrl Pts',(-46.5095061620318,31.2990209657207,
-51.2377986453606));
#237169=CARTESIAN_POINT('Ctrl Pts',(-46.3840578706243,30.8001501121403,
-51.2089377049707));
#237170=CARTESIAN_POINT('Ctrl Pts',(-46.2718308375706,30.5624246444881,
-51.1936549660167));
#237171=CARTESIAN_POINT('Ctrl Pts',(-45.9598446851843,30.1396483898485,
-51.1631974962684));
#237172=CARTESIAN_POINT('Ctrl Pts',(-45.7616139336562,29.959747807885,-51.1483275216909));
#237173=CARTESIAN_POINT('Ctrl Pts',(-45.3162899010547,29.6935789602594,
-51.1218925466886));
#237174=CARTESIAN_POINT('Ctrl Pts',(-45.0756792469387,29.6059936984791,
-51.1080673960021));
#237175=CARTESIAN_POINT('Ctrl Pts',(-44.7199342861136,29.5488717075795,
-51.0873156066207));
#237176=CARTESIAN_POINT('Ctrl Pts',(-44.6139049131048,29.5404524382925,
-51.081130559862));
#237177=CARTESIAN_POINT('Ctrl Pts',(-44.5079524583208,29.5404524382925,
-51.0749499999997));
#237178=CARTESIAN_POINT('Ctrl Pts',(-44.5079524583208,29.5404524382925,
-50.9162000000005));
#237179=CARTESIAN_POINT('Ctrl Pts',(-44.5308414227161,29.5404524382925,
-50.9175351895902));
#237180=CARTESIAN_POINT('Ctrl Pts',(-44.5537463650632,29.5408453642649,
-50.9188713112273));
#237181=CARTESIAN_POINT('Ctrl Pts',(-44.8332472937377,29.5504525720521,
-50.9351755320667));
#237182=CARTESIAN_POINT('Ctrl Pts',(-45.0857893570274,29.6085994744155,
-50.9499071524252));
#237183=CARTESIAN_POINT('Ctrl Pts',(-45.5588880169674,29.8189347221883,
-50.9775045742551));
#237184=CARTESIAN_POINT('Ctrl Pts',(-45.7742700740383,29.9705638419848,
-50.9904930651375));
#237185=CARTESIAN_POINT('Ctrl Pts',(-46.1365457455234,30.3499972378686,
-51.0202277115488));
#237186=CARTESIAN_POINT('Ctrl Pts',(-46.2791089307299,30.5747934763861,
-51.0357420942224));
#237187=CARTESIAN_POINT('Ctrl Pts',(-46.4653506019942,31.0576728823897,
-51.0655683165337));
#237188=CARTESIAN_POINT('Ctrl Pts',(-46.510741168321,31.3097515187281,-51.0794640792994));
#237189=CARTESIAN_POINT('Ctrl Pts',(-46.5047676255909,31.8285847441161,
-51.1058488015839));
#237190=CARTESIAN_POINT('Ctrl Pts',(-46.4490325421369,32.0904046450506,
-51.1207010648344));
#237191=CARTESIAN_POINT('Ctrl Pts',(-46.2406029881886,32.5728162555197,
-51.1511508015596));
#237192=CARTESIAN_POINT('Ctrl Pts',(-46.0915560582926,32.7894783483111,
-51.1664433714712));
#237193=CARTESIAN_POINT('Ctrl Pts',(-45.723486432103,33.1488506286628,-51.1953335578133));
#237194=CARTESIAN_POINT('Ctrl Pts',(-45.5097472355858,33.2899846489231,
-51.2077619713262));
#237195=CARTESIAN_POINT('Ctrl Pts',(-45.0280460202198,33.4901158075745,
-51.2358612088891));
#237196=CARTESIAN_POINT('Ctrl Pts',(-44.7627002581642,33.5421402081724,
-51.2513397116756));
#237197=CARTESIAN_POINT('Ctrl Pts',(-44.2376038870666,33.5387473638364,
-51.2819703333228));
#237198=CARTESIAN_POINT('Ctrl Pts',(-43.982872978989,33.4873971949234,-51.296829636294));
#237199=CARTESIAN_POINT('Ctrl Pts',(-43.5054319540045,33.2903226125284,
-51.3246803627514));
#237200=CARTESIAN_POINT('Ctrl Pts',(-43.2875030771622,33.1459455249636,
-51.3373565686951));
#237201=CARTESIAN_POINT('Ctrl Pts',(-42.9149297381558,32.7782678865303,
-51.3667976846411));
#237202=CARTESIAN_POINT('Ctrl Pts',(-42.7654289473987,32.55706837429,-51.382332714191));
#237203=CARTESIAN_POINT('Ctrl Pts',(-42.5649549535069,32.0785175276322,
-51.4123553751084));
#237204=CARTESIAN_POINT('Ctrl Pts',(-42.5123058678244,31.8271482438344,
-51.4265896842617));
#237205=CARTESIAN_POINT('Ctrl Pts',(-42.5039484084957,31.3076457237372,
-51.4530777489767));
#237206=CARTESIAN_POINT('Ctrl Pts',(-42.5523930990478,31.0443489439623,
-51.4675584153792));
#237207=CARTESIAN_POINT('Ctrl Pts',(-42.7477755310645,30.5555697799855,
-51.4979492880624));
#237208=CARTESIAN_POINT('Ctrl Pts',(-42.8912996606656,30.3343599251892,
-51.5133105208154));
#237209=CARTESIAN_POINT('Ctrl Pts',(-43.2498858906573,29.965169694845,-51.5424200927582));
#237210=CARTESIAN_POINT('Ctrl Pts',(-43.459393533305,29.8186075358262,-51.5550340627078));
#237211=CARTESIAN_POINT('Ctrl Pts',(-43.9327868878355,29.60666355077,-51.5826486750555));
#237212=CARTESIAN_POINT('Ctrl Pts',(-44.1940009390038,29.5475271107708,
-51.5978861613737));
#237213=CARTESIAN_POINT('Ctrl Pts',(-44.4753868222998,29.5406511842867,
-51.6143003378994));
#237214=CARTESIAN_POINT('Ctrl Pts',(-44.4916737747902,29.5404524382925,
-51.6152504101278));
#237215=CARTESIAN_POINT('Ctrl Pts',(-44.5079524583208,29.5404524382925,
-51.6162000000005));
#237216=CARTESIAN_POINT('Origin',(-44.5079524583208,31.5404524382925,235.35105));
#237217=CARTESIAN_POINT('',(-44.5079524583208,29.5404524382925,-50.2162000000005));
#237218=CARTESIAN_POINT('',(-44.5079524583208,29.5404524382925,-50.3749499999996));
#237219=CARTESIAN_POINT('',(-44.5079524583208,29.5404524382925,235.35105));
#237220=CARTESIAN_POINT('Ctrl Pts',(-44.5079524583208,29.5404524382925,
-51.0749499999997));
#237221=CARTESIAN_POINT('Ctrl Pts',(-44.3516039912595,29.5404524382925,
-51.0658296727544));
#237222=CARTESIAN_POINT('Ctrl Pts',(-44.1954230163498,29.5587866319509,
-51.0567191158846));
#237223=CARTESIAN_POINT('Ctrl Pts',(-43.788571375697,29.6561109667705,-51.0329861035133));
#237224=CARTESIAN_POINT('Ctrl Pts',(-43.5489082807268,29.7660616018213,
-51.0199501513565));
#237225=CARTESIAN_POINT('Ctrl Pts',(-43.1290035764768,30.0692603440578,
-50.9923858917143));
#237226=CARTESIAN_POINT('Ctrl Pts',(-42.9517689545595,30.2582030606817,
-50.9776715123485));
#237227=CARTESIAN_POINT('Ctrl Pts',(-42.6730273018941,30.7012671538275,
-50.9471587698027));
#237228=CARTESIAN_POINT('Ctrl Pts',(-42.5775540444165,30.9532789509942,
-50.9316429637197));
#237229=CARTESIAN_POINT('Ctrl Pts',(-42.493095495297,31.4679999066779,-50.9031768396673));
#237230=CARTESIAN_POINT('Ctrl Pts',(-42.5002483396806,31.7249154109233,
-50.8908559756066));
#237231=CARTESIAN_POINT('Ctrl Pts',(-42.6116732973496,32.2271604777061,
-50.8622335901137));
#237232=CARTESIAN_POINT('Ctrl Pts',(-42.7167625248647,32.4673089076121,
-50.8470366335875));
#237233=CARTESIAN_POINT('Ctrl Pts',(-43.0159187736098,32.8984312146818,
-50.8165317422456));
#237234=CARTESIAN_POINT('Ctrl Pts',(-43.2088712752572,33.0840540472864,
-50.8015266391149));
#237235=CARTESIAN_POINT('Ctrl Pts',(-43.6459960586556,33.3628659269626,
-50.7746921063096));
#237236=CARTESIAN_POINT('Ctrl Pts',(-43.8835300958586,33.4573032823413,
-50.7613746378106));
#237237=CARTESIAN_POINT('Ctrl Pts',(-44.3904975881245,33.5542128545749,
-50.7318015340951));
#237238=CARTESIAN_POINT('Ctrl Pts',(-44.6557646955364,33.5522127365159,
-50.716327619496));
#237239=CARTESIAN_POINT('Ctrl Pts',(-45.1711513253888,33.4456120628235,
-50.6862633994211));
#237240=CARTESIAN_POINT('Ctrl Pts',(-45.4161016075001,33.3417550836486,
-50.6727941244446));
#237241=CARTESIAN_POINT('Ctrl Pts',(-45.8454739110283,33.0492886426713,
-50.6454959024792));
#237242=CARTESIAN_POINT('Ctrl Pts',(-46.0274114976107,32.8658788848522,
-50.6309238681454));
#237243=CARTESIAN_POINT('Ctrl Pts',(-46.3178214003599,32.4321584913588,
-50.6005428280456));
#237244=CARTESIAN_POINT('Ctrl Pts',(-46.4202614959123,32.1837740555559,
-50.5850070700988));
#237245=CARTESIAN_POINT('Ctrl Pts',(-46.5199855615089,31.6714972722088,
-50.5562191768769));
#237246=CARTESIAN_POINT('Ctrl Pts',(-46.5202396738285,31.4133698957995,
-50.5438884023581));
#237247=CARTESIAN_POINT('Ctrl Pts',(-46.4228646160598,30.9078541416314,
-50.515510576541));
#237248=CARTESIAN_POINT('Ctrl Pts',(-46.3249538074677,30.6654938288931,
-50.5004112503412));
#237249=CARTESIAN_POINT('Ctrl Pts',(-46.0388405005334,30.2264215419042,
-50.4698851598688));
#237250=CARTESIAN_POINT('Ctrl Pts',(-45.8513328786031,30.0352391567394,
-50.4547580074278));
#237251=CARTESIAN_POINT('Ctrl Pts',(-45.422523382229,29.7438783769635,-50.4275320566281));
#237252=CARTESIAN_POINT('Ctrl Pts',(-45.1879495468724,29.6426221565203,
-50.4146164968316));
#237253=CARTESIAN_POINT('Ctrl Pts',(-44.798241208485,29.5562621223149,-50.3918835104257));
#237254=CARTESIAN_POINT('Ctrl Pts',(-44.6531392944108,29.5404524382925,
-50.3834192321049));
#237255=CARTESIAN_POINT('Ctrl Pts',(-44.5079524583208,29.5404524382925,
-50.3749499999996));
#237256=CARTESIAN_POINT('Ctrl Pts',(-44.5079524583208,29.5404524382925,
-50.2162000000005));
#237257=CARTESIAN_POINT('Ctrl Pts',(-44.5682680746908,29.5404524382925,
-50.2197184109554));
#237258=CARTESIAN_POINT('Ctrl Pts',(-44.6286552888035,29.543180850818,-50.2232409984454));
#237259=CARTESIAN_POINT('Ctrl Pts',(-44.9432382652611,29.5717642544572,
-50.2415916720722));
#237260=CARTESIAN_POINT('Ctrl Pts',(-45.1908258060872,29.6433670029181,
-50.2560342786204));
#237261=CARTESIAN_POINT('Ctrl Pts',(-45.6548201389246,29.8805514677881,
-50.2831006147026));
#237262=CARTESIAN_POINT('Ctrl Pts',(-45.864958208498,30.0474112649116,-50.2970203252533));
#237263=CARTESIAN_POINT('Ctrl Pts',(-46.2053881098655,30.4507815490265,
-50.3273270506451));
#237264=CARTESIAN_POINT('Ctrl Pts',(-46.3334086716835,30.68232470417,-50.3427581152063));
#237265=CARTESIAN_POINT('Ctrl Pts',(-46.4902011678538,31.1732393682324,
-50.3721313296043));
#237266=CARTESIAN_POINT('Ctrl Pts',(-46.5207172683144,31.426903935316,-50.3850914329009));
#237267=CARTESIAN_POINT('Ctrl Pts',(-46.4846744327701,31.9440684483801,
-50.4122688759687));
#237268=CARTESIAN_POINT('Ctrl Pts',(-46.4137986858253,32.2023003552664,
-50.427381483088));
#237269=CARTESIAN_POINT('Ctrl Pts',(-46.1782709362098,32.6705540875203,
-50.4579063540587));
#237270=CARTESIAN_POINT('Ctrl Pts',(-46.0180155913664,32.8771741937101,
-50.4730185335019));
#237271=CARTESIAN_POINT('Ctrl Pts',(-45.6301427936608,33.2155827944716,
-50.5014272660668));
#237272=CARTESIAN_POINT('Ctrl Pts',(-45.4070728232207,33.345156025004,-50.5137513120474));
#237273=CARTESIAN_POINT('Ctrl Pts',(-44.9142518287101,33.5167525737318,
-50.5424992033937));
#237274=CARTESIAN_POINT('Ctrl Pts',(-44.647955317031,33.5532158781841,-50.558033166575));
#237275=CARTESIAN_POINT('Ctrl Pts',(-44.1268308510684,33.520427817413,-50.588432093756));
#237276=CARTESIAN_POINT('Ctrl Pts',(-43.8767072715789,33.4554262072406,
-50.6030226358928));
#237277=CARTESIAN_POINT('Ctrl Pts',(-43.4081569945764,33.2315219641398,
-50.6303547353846));
#237278=CARTESIAN_POINT('Ctrl Pts',(-43.1954050869066,33.0722889103156,
-50.6437637558782));
#237279=CARTESIAN_POINT('Ctrl Pts',(-42.8439986947426,32.6807763605484,
-50.673791598133));
#237280=CARTESIAN_POINT('Ctrl Pts',(-42.7087051457558,32.452476521955,-50.6892709451393));
#237281=CARTESIAN_POINT('Ctrl Pts',(-42.5372706610271,31.9654857010376,
-50.7188729922463));
#237282=CARTESIAN_POINT('Ctrl Pts',(-42.4993407797864,31.7126583229252,
-50.7322493035807));
#237283=CARTESIAN_POINT('Ctrl Pts',(-42.5203182212263,31.194583721686,-50.7590333152903));
#237284=CARTESIAN_POINT('Ctrl Pts',(-42.5836301971647,30.9344397801151,
-50.7740219048743));
#237285=CARTESIAN_POINT('Ctrl Pts',(-42.8056873490928,30.4588951271366,
-50.804522207229));
#237286=CARTESIAN_POINT('Ctrl Pts',(-42.9604033279121,30.2471689693533,
-50.819730770103));
#237287=CARTESIAN_POINT('Ctrl Pts',(-43.3383849810633,29.8982114541963,
-50.8483839225765));
#237288=CARTESIAN_POINT('Ctrl Pts',(-43.5567076480399,29.7628215150986,
-50.8607107194007));
#237289=CARTESIAN_POINT('Ctrl Pts',(-44.0225681142928,29.584960108793,-50.8878859132655));
#237290=CARTESIAN_POINT('Ctrl Pts',(-44.2643554233246,29.5404524382925,
-50.901990172959));
#237291=CARTESIAN_POINT('Ctrl Pts',(-44.5079524583208,29.5404524382925,
-50.9162000000005));
#237292=CARTESIAN_POINT('Origin',(-44.5079524583208,31.5404524382925,235.35105));
#237293=CARTESIAN_POINT('',(-44.5079524583208,29.5404524382925,-49.5162000000005));
#237294=CARTESIAN_POINT('',(-44.5079524583208,29.5404524382925,-49.6749499999997));
#237295=CARTESIAN_POINT('',(-44.5079524583208,29.5404524382925,235.35105));
#237296=CARTESIAN_POINT('Ctrl Pts',(-44.5079524583208,29.5404524382925,
-50.3749499999996));
#237297=CARTESIAN_POINT('Ctrl Pts',(-44.3924091245316,29.5404524382925,
-50.3682099721953));
#237298=CARTESIAN_POINT('Ctrl Pts',(-44.2768120064326,29.5504650026777,
-50.3614668069728));
#237299=CARTESIAN_POINT('Ctrl Pts',(-43.9003665379152,29.6164848585984,
-50.339507487976));
#237300=CARTESIAN_POINT('Ctrl Pts',(-43.6501321722007,29.7142834763753,
-50.3255182498909));
#237301=CARTESIAN_POINT('Ctrl Pts',(-43.2115972335477,29.9962147682009,
-50.2984850006312));
#237302=CARTESIAN_POINT('Ctrl Pts',(-43.0252592255953,30.1741490453239,
-50.2840612318214));
#237303=CARTESIAN_POINT('Ctrl Pts',(-42.723818163838,30.5985232252024,-50.253830602992));
#237304=CARTESIAN_POINT('Ctrl Pts',(-42.614742881212,30.843213893845,-50.2382879210339));
#237305=CARTESIAN_POINT('Ctrl Pts',(-42.5002245589074,31.3529575529645,
-50.2091964974042));
#237306=CARTESIAN_POINT('Ctrl Pts',(-42.4927710519953,31.6123206435822,
-50.196762142347));
#237307=CARTESIAN_POINT('Ctrl Pts',(-42.5766779131083,32.1208776863805,
-50.1686234986617));
#237308=CARTESIAN_POINT('Ctrl Pts',(-42.6676932477752,32.3651548635337,
-50.1536284540101));
#237309=CARTESIAN_POINT('Ctrl Pts',(-42.9411486631884,32.8114526906639,
-50.1231065311302));
#237310=CARTESIAN_POINT('Ctrl Pts',(-43.1232997004361,33.0077938297902,
-50.1078750017102));
#237311=CARTESIAN_POINT('Ctrl Pts',(-43.5440398982312,33.3110704390746,
-50.080282439807));
#237312=CARTESIAN_POINT('Ctrl Pts',(-43.7758833547215,33.4188327572136,
-50.0676540310437));
#237313=CARTESIAN_POINT('Ctrl Pts',(-44.2751366816049,33.5439605610322,
-50.0385309203087));
#237314=CARTESIAN_POINT('Ctrl Pts',(-44.5385395304028,33.5572082346637,
-50.0231657541288));
#237315=CARTESIAN_POINT('Ctrl Pts',(-45.0594426530212,33.4811202826094,
-49.9927797386426));
#237316=CARTESIAN_POINT('Ctrl Pts',(-45.3115366621747,33.3909896609665,
-49.978331175041));
#237317=CARTESIAN_POINT('Ctrl Pts',(-45.7568417506746,33.1232024289028,
-49.9518149947893));
#237318=CARTESIAN_POINT('Ctrl Pts',(-45.9479404421206,32.9515549679649,
-49.9375699710248));
#237319=CARTESIAN_POINT('Ctrl Pts',(-46.2614539645297,32.5380265596496,
-49.9075351370584));
#237320=CARTESIAN_POINT('Ctrl Pts',(-46.3778496296041,32.2976967025486,
-49.8919992440707));
#237321=CARTESIAN_POINT('Ctrl Pts',(-46.5090182683512,31.7910157173607,
-49.8625769068278));
#237322=CARTESIAN_POINT('Ctrl Pts',(-46.5246154445457,31.5301825592137,
-49.8499171884875));
#237323=CARTESIAN_POINT('Ctrl Pts',(-46.4557043772846,31.0183536933514,
-49.822050635679));
#237324=CARTESIAN_POINT('Ctrl Pts',(-46.372368230767,30.7721768865771,-49.8071836015771));
#237325=CARTESIAN_POINT('Ctrl Pts',(-46.1119061688116,30.3161120727555,
-49.7765472414218));
#237326=CARTESIAN_POINT('Ctrl Pts',(-45.9337779549868,30.1126103578477,
-49.7610713053205));
#237327=CARTESIAN_POINT('Ctrl Pts',(-45.5190165437163,29.7962661962156,
-49.7329929761403));
#237328=CARTESIAN_POINT('Ctrl Pts',(-45.2897486819327,29.6821620200328,
-49.7205547797102));
#237329=CARTESIAN_POINT('Ctrl Pts',(-44.8699416127025,29.565085884589,-49.6960660340051));
#237330=CARTESIAN_POINT('Ctrl Pts',(-44.6891776833351,29.5404524382925,
-49.6855214714588));
#237331=CARTESIAN_POINT('Ctrl Pts',(-44.5079524583208,29.5404524382925,
-49.6749499999997));
#237332=CARTESIAN_POINT('Ctrl Pts',(-44.5079524583208,29.5404524382925,
-49.5162000000005));
#237333=CARTESIAN_POINT('Ctrl Pts',(-44.6075826695198,29.5404524382925,
-49.5220117623204));
#237334=CARTESIAN_POINT('Ctrl Pts',(-44.7072983762974,29.5478968952994,
-49.5278285118826));
#237335=CARTESIAN_POINT('Ctrl Pts',(-45.0574846297731,29.600719504041,-49.5482560433354));
#237336=CARTESIAN_POINT('Ctrl Pts',(-45.29909581334,29.6861235028605,-49.5622644165605));
#237337=CARTESIAN_POINT('Ctrl Pts',(-45.7469953257586,29.9482656497159,
-49.5885710882564));
#237338=CARTESIAN_POINT('Ctrl Pts',(-45.9468628369225,30.1263200493847,
-49.6033955359452));
#237339=CARTESIAN_POINT('Ctrl Pts',(-46.2628676237101,30.5463702077689,
-49.6338324985279));
#237340=CARTESIAN_POINT('Ctrl Pts',(-46.3773467568928,30.783284056148,-49.6491399222326));
#237341=CARTESIAN_POINT('Ctrl Pts',(-46.5072346558957,31.2810633104478,
-49.6780752056027));
#237342=CARTESIAN_POINT('Ctrl Pts',(-46.5239839945915,31.5365332692116,
-49.6905344243601));
#237343=CARTESIAN_POINT('Ctrl Pts',(-46.459326200111,32.0541703938326,-49.7185703458577));
#237344=CARTESIAN_POINT('Ctrl Pts',(-46.3730540890751,32.3105994108117,
-49.7340409349361));
#237345=CARTESIAN_POINT('Ctrl Pts',(-46.1098497512395,32.765305155933,-49.7646886205033));
#237346=CARTESIAN_POINT('Ctrl Pts',(-45.9389489246245,32.9612335178118,
-49.7795711660375));
#237347=CARTESIAN_POINT('Ctrl Pts',(-45.5313434501067,33.2781493688681,
-49.807469661087));
#237348=CARTESIAN_POINT('Ctrl Pts',(-45.2982859569776,33.3957968842558,
-49.8200972125782));
#237349=CARTESIAN_POINT('Ctrl Pts',(-44.7945554557703,33.5374114466433,
-49.8494814918152));
#237350=CARTESIAN_POINT('Ctrl Pts',(-44.5281986460667,33.55776831581,-49.8650189723812));
#237351=CARTESIAN_POINT('Ctrl Pts',(-44.0128990377119,33.4948687514879,
-49.8950781162018));
#237352=CARTESIAN_POINT('Ctrl Pts',(-43.7683297027054,33.4160390242073,
-49.9093446607438));
#237353=CARTESIAN_POINT('Ctrl Pts',(-43.3127967774858,33.1658285001609,
-49.935917414715));
#237354=CARTESIAN_POINT('Ctrl Pts',(-43.1080838362608,32.9932790555579,
-49.9503020572687));
#237355=CARTESIAN_POINT('Ctrl Pts',(-42.7802422051094,32.5812708563266,
-49.9806779962582));
#237356=CARTESIAN_POINT('Ctrl Pts',(-42.6591711818348,32.3468651094646,
-49.996050978779));
#237357=CARTESIAN_POINT('Ctrl Pts',(-42.5162361847141,31.8523604660051,
-50.025201375234));
#237358=CARTESIAN_POINT('Ctrl Pts',(-42.4927833343748,31.5978101679999,
-50.0378599609079));
#237359=CARTESIAN_POINT('Ctrl Pts',(-42.5432979860439,31.0816659714257,
-50.0654079541129));
#237360=CARTESIAN_POINT('Ctrl Pts',(-42.6213856920525,30.8254844179476,
-50.0806273299803));
#237361=CARTESIAN_POINT('Ctrl Pts',(-42.8696317804171,30.3645964810192,
-50.1111510461556));
#237362=CARTESIAN_POINT('Ctrl Pts',(-43.0350560656012,30.1630148227299,
-50.1261594532995));
#237363=CARTESIAN_POINT('Ctrl Pts',(-43.4323797711602,29.8348222084344,
-50.1543277446218));
#237364=CARTESIAN_POINT('Ctrl Pts',(-43.660141244683,29.7109029976232,-50.1667443458715));
#237365=CARTESIAN_POINT('Ctrl Pts',(-44.1005015496996,29.5717085211214,
-50.1924320303309));
#237366=CARTESIAN_POINT('Ctrl Pts',(-44.3038169444646,29.5404524382925,
-50.2042920950255));
#237367=CARTESIAN_POINT('Ctrl Pts',(-44.5079524583208,29.5404524382925,
-50.2162000000005));
#237368=CARTESIAN_POINT('Origin',(-44.5079524583208,31.5404524382925,235.35105));
#237369=CARTESIAN_POINT('',(-44.5079524583208,29.5404524382925,-48.8162000000004));
#237370=CARTESIAN_POINT('',(-44.5079524583208,29.5404524382925,-48.9749499999996));
#237371=CARTESIAN_POINT('',(-44.5079524583208,29.5404524382925,235.35105));
#237372=CARTESIAN_POINT('Ctrl Pts',(-44.5079524583208,29.5404524382925,
-49.6749499999997));
#237373=CARTESIAN_POINT('Ctrl Pts',(-44.4296713573153,29.5404524382925,
-49.670383602441));
#237374=CARTESIAN_POINT('Ctrl Pts',(-44.3513041854955,29.5450482640994,
-49.6658121840848));
#237375=CARTESIAN_POINT('Ctrl Pts',(-44.0100641429768,29.5853706921466,
-49.645906514938));
#237376=CARTESIAN_POINT('Ctrl Pts',(-43.755610585112,29.6684825954307,-49.6310633907293));
#237377=CARTESIAN_POINT('Ctrl Pts',(-43.3037426519632,29.9235780366005,
-49.6047044279624));
#237378=CARTESIAN_POINT('Ctrl Pts',(-43.108410266594,30.0893196633568,-49.5907718938373));
#237379=CARTESIAN_POINT('Ctrl Pts',(-42.7840560257168,30.4927404792281,
-49.5609314891058));
#237380=CARTESIAN_POINT('Ctrl Pts',(-42.6610929378257,30.7288880785963,
-49.5454153262035));
#237381=CARTESIAN_POINT('Ctrl Pts',(-42.5146543172607,31.2325538999191,
-49.5156999349872));
#237382=CARTESIAN_POINT('Ctrl Pts',(-42.4915363829144,31.4947984047003,
-49.5027351594508));
#237383=CARTESIAN_POINT('Ctrl Pts',(-42.5468368096406,32.0094939633745,
-49.4751207636448));
#237384=CARTESIAN_POINT('Ctrl Pts',(-42.623214093632,32.2571817619078,-49.4603803638605));
#237385=CARTESIAN_POINT('Ctrl Pts',(-42.8702009197475,32.7190247217399,
-49.4298451301786));
#237386=CARTESIAN_POINT('Ctrl Pts',(-43.0419698811053,32.9268821241792,
-49.4143346310045));
#237387=CARTESIAN_POINT('Ctrl Pts',(-43.4473529517607,33.2550770068072,
-49.3859311602751));
#237388=CARTESIAN_POINT('Ctrl Pts',(-43.6739406933817,33.3760010232055,
-49.3736006862886));
#237389=CARTESIAN_POINT('Ctrl Pts',(-44.1654079682929,33.5279579915564,
-49.3449317619187));
#237390=CARTESIAN_POINT('Ctrl Pts',(-44.4262271418543,33.5555997274517,
-49.3297173101275));
#237391=CARTESIAN_POINT('Ctrl Pts',(-44.9490461965395,33.509132724569,-49.2992195319375));
#237392=CARTESIAN_POINT('Ctrl Pts',(-45.2058465600757,33.4334018254037,
-49.2842395107311));
#237393=CARTESIAN_POINT('Ctrl Pts',(-45.6645551224534,33.191650543762,-49.257481511259));
#237394=CARTESIAN_POINT('Ctrl Pts',(-45.8642564135317,33.0319921369332,
-49.2440742920432));
#237395=CARTESIAN_POINT('Ctrl Pts',(-46.1995741557137,32.639325372177,-49.2144573932752));
#237396=CARTESIAN_POINT('Ctrl Pts',(-46.3292102598113,32.4077055769673,
-49.1989753370165));
#237397=CARTESIAN_POINT('Ctrl Pts',(-46.491528560328,31.9073949943738,-49.1689662889167));
#237398=CARTESIAN_POINT('Ctrl Pts',(-46.5225340672254,31.6436308176897,
-49.1555876776239));
#237399=CARTESIAN_POINT('Ctrl Pts',(-46.4812535020921,31.1260841753774,
-49.1282381629808));
#237400=CARTESIAN_POINT('Ctrl Pts',(-46.4120209946098,30.8770502457702,
-49.1136381484616));
#237401=CARTESIAN_POINT('Ctrl Pts',(-46.178948166395,30.4096926314201,-49.0832301495823));
#237402=CARTESIAN_POINT('Ctrl Pts',(-46.0137898376405,30.1975740153553,
-49.0676971919029));
#237403=CARTESIAN_POINT('Ctrl Pts',(-45.6181367783471,29.8573528393903,
-49.0389699670982));
#237404=CARTESIAN_POINT('Ctrl Pts',(-45.3942174077798,29.7294116890116,
-49.0266487887179));
#237405=CARTESIAN_POINT('Ctrl Pts',(-44.9445050686823,29.5763822844598,
-49.0004155689373));
#237406=CARTESIAN_POINT('Ctrl Pts',(-44.7268193952234,29.5404524382925,
-48.9877172379856));
#237407=CARTESIAN_POINT('Ctrl Pts',(-44.5079524583208,29.5404524382925,
-48.9749499999996));
#237408=CARTESIAN_POINT('Ctrl Pts',(-44.5079524583208,29.5404524382925,
-48.8162000000004));
#237409=CARTESIAN_POINT('Ctrl Pts',(-44.6469069524102,29.5404524382925,
-48.8243056788223));
#237410=CARTESIAN_POINT('Ctrl Pts',(-44.7858169909055,29.5549338421087,
-48.8324087644013));
#237411=CARTESIAN_POINT('Ctrl Pts',(-45.1702021228419,29.6363555489129,
-48.854831230431));
#237412=CARTESIAN_POINT('Ctrl Pts',(-45.405715723631,29.7354215086392,-48.8678646079231));
#237413=CARTESIAN_POINT('Ctrl Pts',(-45.8372124491951,30.0227568965869,
-48.8949655808986));
#237414=CARTESIAN_POINT('Ctrl Pts',(-46.0264887799817,30.212169595963,-48.9100549194317));
#237415=CARTESIAN_POINT('Ctrl Pts',(-46.3168186695098,30.648729018531,-48.9405770483049));
#237416=CARTESIAN_POINT('Ctrl Pts',(-46.4170418320557,30.890401137655,-48.9557090518944));
#237417=CARTESIAN_POINT('Ctrl Pts',(-46.5189384190221,31.3948760227152,
-48.9841661728661));
#237418=CARTESIAN_POINT('Ctrl Pts',(-46.5210788733626,31.6526032984413,
-48.9964828000418));
#237419=CARTESIAN_POINT('Ctrl Pts',(-46.4262861046215,32.1656887343397,
-49.0251677154016));
#237420=CARTESIAN_POINT('Ctrl Pts',(-46.3260837074216,32.4152656781251,
-49.0406984504417));
#237421=CARTESIAN_POINT('Ctrl Pts',(-46.0394122132731,32.8520385101669,
-49.0711246571677));
#237422=CARTESIAN_POINT('Ctrl Pts',(-45.8589761702092,33.0372490386676,
-49.0857438680829));
#237423=CARTESIAN_POINT('Ctrl Pts',(-45.4326608595628,33.3331976238984,
-49.1131288392364));
#237424=CARTESIAN_POINT('Ctrl Pts',(-45.189437010449,33.4390396738555,-49.126446734459));
#237425=CARTESIAN_POINT('Ctrl Pts',(-44.6756555075747,33.550686055685,-49.1564173221266));
#237426=CARTESIAN_POINT('Ctrl Pts',(-44.4101572833061,33.5552965078418,
-49.1719047185422));
#237427=CARTESIAN_POINT('Ctrl Pts',(-43.9019216507782,33.4632115008325,
-49.2015517971062));
#237428=CARTESIAN_POINT('Ctrl Pts',(-43.6633961901834,33.3710070719332,
-49.2150233269016));
#237429=CARTESIAN_POINT('Ctrl Pts',(-43.2235817281476,33.0963130838346,
-49.2417282804086));
#237430=CARTESIAN_POINT('Ctrl Pts',(-43.0288870275621,32.9125412104799,
-49.2566906906406));
#237431=CARTESIAN_POINT('Ctrl Pts',(-42.7255171362445,32.4841010351062,
-49.2871829835634));
#237432=CARTESIAN_POINT('Ctrl Pts',(-42.6180922873079,32.2447206477794,
-49.302409262292));
#237433=CARTESIAN_POINT('Ctrl Pts',(-42.5020856709242,31.7435657778012,
-49.3311102047735));
#237434=CARTESIAN_POINT('Ctrl Pts',(-42.4925379086377,31.4870247470635,
-49.3434494770097));
#237435=CARTESIAN_POINT('Ctrl Pts',(-42.5720552127493,30.9715497267348,
-49.371809575366));
#237436=CARTESIAN_POINT('Ctrl Pts',(-42.6652490010032,30.718404833557,-49.3873161388427));
#237437=CARTESIAN_POINT('Ctrl Pts',(-42.9401546415722,30.2723841156141,
-49.4178663609134));
#237438=CARTESIAN_POINT('Ctrl Pts',(-43.1158328585487,30.0816773705056,
-49.4326244605883));
#237439=CARTESIAN_POINT('Ctrl Pts',(-43.5326703382316,29.7750342823307,
-49.460273261494));
#237440=CARTESIAN_POINT('Ctrl Pts',(-43.7706583326269,29.6631423424877,
-49.4731911760016));
#237441=CARTESIAN_POINT('Ctrl Pts',(-44.1822860790587,29.5603671423784,
-49.4972027945435));
#237442=CARTESIAN_POINT('Ctrl Pts',(-44.3450049210616,29.5404524382925,
-49.5066947269937));
#237443=CARTESIAN_POINT('Ctrl Pts',(-44.5079524583208,29.5404524382925,
-49.5162000000005));
#237444=CARTESIAN_POINT('Origin',(-44.5079524583208,31.5404524382925,235.35105));
#237445=CARTESIAN_POINT('',(-44.5079524583208,29.5404524382925,-48.1162000000004));
#237446=CARTESIAN_POINT('',(-44.5079524583208,29.5404524382925,-48.2749499999996));
#237447=CARTESIAN_POINT('',(-44.5079524583208,29.5404524382925,235.35105));
#237448=CARTESIAN_POINT('Ctrl Pts',(-44.5079524583208,29.5404524382925,
-48.9749499999996));
#237449=CARTESIAN_POINT('Ctrl Pts',(-44.4683714928986,29.5404524382925,
-48.97264111035));
#237450=CARTESIAN_POINT('Ctrl Pts',(-44.4287518944074,29.5416274112108,
-48.9703299671047));
#237451=CARTESIAN_POINT('Ctrl Pts',(-44.1244892411486,29.5597336396126,
-48.9525813123313));
#237452=CARTESIAN_POINT('Ctrl Pts',(-43.8655460451714,29.6279544839446,
-48.9374762925661));
#237453=CARTESIAN_POINT('Ctrl Pts',(-43.400077042296,29.8561938741588,-48.9103239340652));
#237454=CARTESIAN_POINT('Ctrl Pts',(-43.1959415636786,30.0098370335365,
-48.8973402053029));
#237455=CARTESIAN_POINT('Ctrl Pts',(-42.8498745701799,30.3917675000002,
-48.8679521646172));
#237456=CARTESIAN_POINT('Ctrl Pts',(-42.7137697510356,30.61871226316,-48.8525176114667));
#237457=CARTESIAN_POINT('Ctrl Pts',(-42.5356635853209,31.1154542836193,
-48.8222283611175));
#237458=CARTESIAN_POINT('Ctrl Pts',(-42.496736437211,31.3807690747112,-48.8083440418324));
#237459=CARTESIAN_POINT('Ctrl Pts',(-42.524203596213,31.9010235360147,-48.7812606241996));
#237460=CARTESIAN_POINT('Ctrl Pts',(-42.5864312605022,32.1511776656024,
-48.7668083271779));
#237461=CARTESIAN_POINT('Ctrl Pts',(-42.8057858625377,32.6235356115091,
-48.7365478357366));
#237462=CARTESIAN_POINT('Ctrl Pts',(-42.9643836875725,32.8396271517157,
-48.7210055213103));
#237463=CARTESIAN_POINT('Ctrl Pts',(-43.350382955504,33.1915192885072,-48.6919702700874));
#237464=CARTESIAN_POINT('Ctrl Pts',(-43.5717413988538,33.326367924112,-48.6795623118027));
#237465=CARTESIAN_POINT('Ctrl Pts',(-44.0548892019584,33.5055260564065,
-48.6513786899549));
#237466=CARTESIAN_POINT('Ctrl Pts',(-44.3122938236924,33.5475578917467,
-48.6363634203537));
#237467=CARTESIAN_POINT('Ctrl Pts',(-44.8355710464731,33.5311754888667,
-48.6058389156914));
#237468=CARTESIAN_POINT('Ctrl Pts',(-45.0963654311893,33.4702507280505,
-48.5906259099162));
#237469=CARTESIAN_POINT('Ctrl Pts',(-45.5682200277731,33.2551011217427,
-48.5631010584487));
#237470=CARTESIAN_POINT('Ctrl Pts',(-45.7766682854539,33.1071598903678,
-48.5504262815134));
#237471=CARTESIAN_POINT('Ctrl Pts',(-46.132828773842,32.7354814161378,-48.5212617588931));
#237472=CARTESIAN_POINT('Ctrl Pts',(-46.2749260998083,32.5131362704431,
-48.5058847884518));
#237473=CARTESIAN_POINT('Ctrl Pts',(-46.4669477216483,32.0228186329689,
-48.4755142185661));
#237474=CARTESIAN_POINT('Ctrl Pts',(-46.5135478681275,31.7591670652899,
-48.4611622574699));
#237475=CARTESIAN_POINT('Ctrl Pts',(-46.5015253869323,31.2395253140083,
-48.4345602625822));
#237476=CARTESIAN_POINT('Ctrl Pts',(-46.4470347162938,30.9883613969714,
-48.4202826152829));
#237477=CARTESIAN_POINT('Ctrl Pts',(-46.242919821103,30.5109436639625,-48.3902110042146));
#237478=CARTESIAN_POINT('Ctrl Pts',(-46.0916587682423,30.2906972496676,
-48.3746727824303));
#237479=CARTESIAN_POINT('Ctrl Pts',(-45.7164818762461,29.9260400811427,
-48.3453083180696));
#237480=CARTESIAN_POINT('Ctrl Pts',(-45.4978985777791,29.7835041007128,
-48.3326968569679));
#237481=CARTESIAN_POINT('Ctrl Pts',(-45.0198102819191,29.59003151068,-48.3048083730428));
#237482=CARTESIAN_POINT('Ctrl Pts',(-44.7650619789425,29.5404524382925,
-48.2899480553692));
#237483=CARTESIAN_POINT('Ctrl Pts',(-44.5079524583208,29.5404524382925,
-48.2749499999996));
#237484=CARTESIAN_POINT('Ctrl Pts',(-44.5079524583208,29.5404524382925,
-48.1162000000004));
#237485=CARTESIAN_POINT('Ctrl Pts',(-44.6829574575485,29.5404524382925,
-48.1264086249554));
#237486=CARTESIAN_POINT('Ctrl Pts',(-44.8575854482278,29.5634237494144,
-48.1365952577451));
#237487=CARTESIAN_POINT('Ctrl Pts',(-45.2722893575364,29.6749367761027,
-48.1607863191215));
#237488=CARTESIAN_POINT('Ctrl Pts',(-45.5024584683471,29.786798548748,-48.1732817442552));
#237489=CARTESIAN_POINT('Ctrl Pts',(-45.9180503088427,30.0975433635833,
-48.2011014256546));
#237490=CARTESIAN_POINT('Ctrl Pts',(-46.0967531377997,30.2970540722592,
-48.2163925031182));
#237491=CARTESIAN_POINT('Ctrl Pts',(-46.3621447032057,30.7477137033057,
-48.246899580631));
#237492=CARTESIAN_POINT('Ctrl Pts',(-46.4488020510829,30.99309905767,-48.2618235003955));
#237493=CARTESIAN_POINT('Ctrl Pts',(-46.5242001097123,31.5035272387935,
-48.2898084971189));
#237494=CARTESIAN_POINT('Ctrl Pts',(-46.5121432671305,31.7637128885449,
-48.3023564726688));
#237495=CARTESIAN_POINT('Ctrl Pts',(-46.3882000551431,32.271751121424,-48.3316366339381));
#237496=CARTESIAN_POINT('Ctrl Pts',(-46.2749612510384,32.5139993733863,
-48.3471773655706));
#237497=CARTESIAN_POINT('Ctrl Pts',(-45.9666409067441,32.9322757248042,
-48.3773005891367));
#237498=CARTESIAN_POINT('Ctrl Pts',(-45.7775827427436,33.1066668926727,
-48.3916247045115));
#237499=CARTESIAN_POINT('Ctrl Pts',(-45.3332167323945,33.381814914463,-48.4184853484524));
#237500=CARTESIAN_POINT('Ctrl Pts',(-45.0795347991248,33.4756664295537,
-48.4328576967862));
#237501=CARTESIAN_POINT('Ctrl Pts',(-44.5564675923915,33.5568862540778,
-48.4633699505122));
#237502=CARTESIAN_POINT('Ctrl Pts',(-44.2927243429971,33.5459555958065,
-48.4787549733934));
#237503=CARTESIAN_POINT('Ctrl Pts',(-43.7922644434613,33.4251241785786,
-48.507948467533));
#237504=CARTESIAN_POINT('Ctrl Pts',(-43.5595661090824,33.3194223032443,
-48.5206576712748));
#237505=CARTESIAN_POINT('Ctrl Pts',(-43.1362566519627,33.0199117609383,
-48.5481349151771));
#237506=CARTESIAN_POINT('Ctrl Pts',(-42.9523932251493,32.825187863206,-48.5633346892518));
#237507=CARTESIAN_POINT('Ctrl Pts',(-42.6749091578537,32.381138797746,-48.5938605112022));
#237508=CARTESIAN_POINT('Ctrl Pts',(-42.5817065529211,32.1374478458307,
-48.6088897362229));
#237509=CARTESIAN_POINT('Ctrl Pts',(-42.4935289496987,31.6298445702235,
-48.6371047606673));
#237510=CARTESIAN_POINT('Ctrl Pts',(-42.4986884027967,31.3708823477966,
-48.6494961654023));
#237511=CARTESIAN_POINT('Ctrl Pts',(-42.6084989238686,30.860313793874,-48.6784919503211));
#237512=CARTESIAN_POINT('Ctrl Pts',(-42.7154756982118,30.6144289468359,
-48.6940337534694));
#237513=CARTESIAN_POINT('Ctrl Pts',(-43.0134368174215,30.1870502854352,
-48.7243146648186));
#237514=CARTESIAN_POINT('Ctrl Pts',(-43.1983916540592,30.0073619324355,
-48.7387867037976));
#237515=CARTESIAN_POINT('Ctrl Pts',(-43.634012144625,29.7220634423569,-48.7659050529433));
#237516=CARTESIAN_POINT('Ctrl Pts',(-43.8825480054977,29.6223194049305,
-48.7797180735857));
#237517=CARTESIAN_POINT('Ctrl Pts',(-44.2639012978467,29.5516168955097,
-48.8019636823061));
#237518=CARTESIAN_POINT('Ctrl Pts',(-44.385944014934,29.5404524382925,-48.8090828408029));
#237519=CARTESIAN_POINT('Ctrl Pts',(-44.5079524583208,29.5404524382925,
-48.8162000000004));
#237520=CARTESIAN_POINT('Origin',(-44.5079524583208,31.5404524382925,235.35105));
#237521=CARTESIAN_POINT('',(-44.5079524583208,29.5404524382925,-47.4162000000004));
#237522=CARTESIAN_POINT('',(-44.5079524583208,29.5404524382925,-47.5749499999997));
#237523=CARTESIAN_POINT('',(-44.5079524583208,29.5404524382925,235.35105));
#237524=CARTESIAN_POINT('Ctrl Pts',(-44.5079524583208,29.5404524382925,
-48.2749499999996));
#237525=CARTESIAN_POINT('Ctrl Pts',(-44.5074611740721,29.5404524382925,
-48.2749213417518));
#237526=CARTESIAN_POINT('Ctrl Pts',(-44.5069698812021,29.5404526193126,
-48.2748926830011));
#237527=CARTESIAN_POINT('Ctrl Pts',(-44.2386011496059,29.5406503908197,
-48.2592378403247));
#237528=CARTESIAN_POINT('Ctrl Pts',(-43.9734400904005,29.5946645805173,
-48.2437701118711));
#237529=CARTESIAN_POINT('Ctrl Pts',(-43.4932031097656,29.798423853582,-48.2157562880009));
#237530=CARTESIAN_POINT('Ctrl Pts',(-43.2806365401203,29.9410495527583,
-48.2032854916218));
#237531=CARTESIAN_POINT('Ctrl Pts',(-42.9151623196074,30.3031230496922,
-48.1743345441514));
#237532=CARTESIAN_POINT('Ctrl Pts',(-42.7676177442234,30.5210469482816,
-48.1590220488203));
#237533=CARTESIAN_POINT('Ctrl Pts',(-42.5627741871192,31.0051834192762,
-48.1285897669094));
#237534=CARTESIAN_POINT('Ctrl Pts',(-42.50902073151,31.2674026979878,-48.1137751253118));
#237535=CARTESIAN_POINT('Ctrl Pts',(-42.5069602194121,31.7864102811206,
-48.0874957248569));
#237536=CARTESIAN_POINT('Ctrl Pts',(-42.5543111330295,32.0383072839409,
-48.0734471669374));
#237537=CARTESIAN_POINT('Ctrl Pts',(-42.7444520332751,32.5200790493857,
-48.0435631730643));
#237538=CARTESIAN_POINT('Ctrl Pts',(-42.8889138044954,32.743915970668,-48.0280418778959));
#237539=CARTESIAN_POINT('Ctrl Pts',(-43.2540140322781,33.1201551487533,
-47.9983862145619));
#237540=CARTESIAN_POINT('Ctrl Pts',(-43.4700886114566,33.2697998012266,
-47.9854920577344));
#237541=CARTESIAN_POINT('Ctrl Pts',(-43.9443751863956,33.4765379120186,
-47.9578253408628));
#237542=CARTESIAN_POINT('Ctrl Pts',(-44.1975283092354,33.5328502398106,
-47.9430580753638));
#237543=CARTESIAN_POINT('Ctrl Pts',(-44.7213777085793,33.5468913257583,
-47.9125001937353));
#237544=CARTESIAN_POINT('Ctrl Pts',(-44.9871677370191,33.5004857452827,
-47.8969957754096));
#237545=CARTESIAN_POINT('Ctrl Pts',(-45.4729515719845,33.3106212295625,
-47.8686583850365));
#237546=CARTESIAN_POINT('Ctrl Pts',(-45.6900255288811,33.1736795453411,
-47.8563138117252));
#237547=CARTESIAN_POINT('Ctrl Pts',(-46.0653428964289,32.821907248863,-47.8275961700409));
#237548=CARTESIAN_POINT('Ctrl Pts',(-46.2185461635087,32.6088362993964,
-47.8123637915399));
#237549=CARTESIAN_POINT('Ctrl Pts',(-46.4369517705266,32.1314024279935,
-47.7818745527615));
#237550=CARTESIAN_POINT('Ctrl Pts',(-46.4982262257139,31.8707844500243,
-47.7669214434249));
#237551=CARTESIAN_POINT('Ctrl Pts',(-46.5151614667972,31.3524912152932,
-47.7402442842664));
#237552=CARTESIAN_POINT('Ctrl Pts',(-46.4752298333033,31.0998738211168,
-47.7267383740709));
#237553=CARTESIAN_POINT('Ctrl Pts',(-46.2998284515804,30.6139700091309,
-47.6970755394804));
#237554=CARTESIAN_POINT('Ctrl Pts',(-46.1625784307328,30.3865869735557,
-47.6815854439025));
#237555=CARTESIAN_POINT('Ctrl Pts',(-45.808237634687,29.9983022717098,-47.6516350797687));
#237556=CARTESIAN_POINT('Ctrl Pts',(-45.5947804975627,29.8411169979924,
-47.6383483022886));
#237557=CARTESIAN_POINT('Ctrl Pts',(-45.1250058936745,29.620834015134,-47.6109447837285));
#237558=CARTESIAN_POINT('Ctrl Pts',(-44.874219530905,29.5576512913066,-47.5963155792336));
#237559=CARTESIAN_POINT('Ctrl Pts',(-44.5815654461517,29.5414674752469,
-47.5792440909564));
#237560=CARTESIAN_POINT('Ctrl Pts',(-44.5447410599504,29.5404524382925,
-47.5770960017614));
#237561=CARTESIAN_POINT('Ctrl Pts',(-44.5079524583208,29.5404524382925,
-47.5749499999996));
#237562=CARTESIAN_POINT('Ctrl Pts',(-44.5079524583208,29.5404524382925,
-47.4162000000004));
#237563=CARTESIAN_POINT('Ctrl Pts',(-44.7203615317488,29.5404524382925,
-47.4285905292838));
#237564=CARTESIAN_POINT('Ctrl Pts',(-44.9317409055993,29.5742933371907,
-47.4409209927584));
#237565=CARTESIAN_POINT('Ctrl Pts',(-45.3764514988243,29.7208785666382,
-47.4668624440298));
#237566=CARTESIAN_POINT('Ctrl Pts',(-45.6012773747708,29.8464104982827,
-47.4791754476813));
#237567=CARTESIAN_POINT('Ctrl Pts',(-46.000279698641,30.182522922248,-47.5077927928256));
#237568=CARTESIAN_POINT('Ctrl Pts',(-46.1677140915721,30.3932042385524,
-47.5233195259874));
#237569=CARTESIAN_POINT('Ctrl Pts',(-46.4055670380206,30.8587182248351,
-47.5537738083052));
#237570=CARTESIAN_POINT('Ctrl Pts',(-46.4772495247028,31.1073138275644,
-47.5684231370886));
#237571=CARTESIAN_POINT('Ctrl Pts',(-46.5233442630961,31.6238931033201,
-47.5958641955509));
#237572=CARTESIAN_POINT('Ctrl Pts',(-46.4950640003346,31.8871286464186,
-47.6090893535405));
#237573=CARTESIAN_POINT('Ctrl Pts',(-46.33821528632,32.3886208514487,-47.6389985654116));
#237574=CARTESIAN_POINT('Ctrl Pts',(-46.2108591253111,32.6218203074811,
-47.6544939248702));
#237575=CARTESIAN_POINT('Ctrl Pts',(-45.8792998736936,33.0181962783179,
-47.6841885832202));
#237576=CARTESIAN_POINT('Ctrl Pts',(-45.6811130217757,33.1799456474558,
-47.6977656337983));
#237577=CARTESIAN_POINT('Ctrl Pts',(-45.2247563204773,33.4263203586885,
-47.724386441374));
#237578=CARTESIAN_POINT('Ctrl Pts',(-44.9687431979571,33.5046133828753,
-47.7393205401875));
#237579=CARTESIAN_POINT('Ctrl Pts',(-44.44618315351,33.5563426158039,-47.7698032094469));
#237580=CARTESIAN_POINT('Ctrl Pts',(-44.1848481544729,33.5312432690995,
-47.7850477510573));
#237581=CARTESIAN_POINT('Ctrl Pts',(-43.6919680971685,33.3840468816324,
-47.8137990877334));
#237582=CARTESIAN_POINT('Ctrl Pts',(-43.4644572149029,33.26549767212,-47.8261558532141));
#237583=CARTESIAN_POINT('Ctrl Pts',(-43.0557992144319,32.9414122120539,
-47.8544472423104));
#237584=CARTESIAN_POINT('Ctrl Pts',(-42.8818074731782,32.7350480172083,
-47.8699471384817));
#237585=CARTESIAN_POINT('Ctrl Pts',(-42.630120881441,32.2751707661802,-47.9005201446915));
#237586=CARTESIAN_POINT('Ctrl Pts',(-42.5513210079441,32.0279864772773,
-47.9153057669622));
#237587=CARTESIAN_POINT('Ctrl Pts',(-42.4912785014281,31.514278639586,-47.9430085755936));
#237588=CARTESIAN_POINT('Ctrl Pts',(-42.5117614109264,31.2525335670707,
-47.9558562227586));
#237589=CARTESIAN_POINT('Ctrl Pts',(-42.6528631438635,30.7477908955022,
-47.9854703552333));
#237590=CARTESIAN_POINT('Ctrl Pts',(-42.7735473128218,30.5101621105732,
-48.0009948764191));
#237591=CARTESIAN_POINT('Ctrl Pts',(-43.0941807328986,30.1031372910013,
-48.0309088248051));
#237592=CARTESIAN_POINT('Ctrl Pts',(-43.2880628865459,29.9353417761717,
-48.04503977498));
#237593=CARTESIAN_POINT('Ctrl Pts',(-43.7376236282077,29.6758146575417,
-48.071264151577));
#237594=CARTESIAN_POINT('Ctrl Pts',(-43.9912474034753,29.5902619044792,
-48.086058871801));
#237595=CARTESIAN_POINT('Ctrl Pts',(-44.3384685866399,29.5458325820639,
-48.106313440819));
#237596=CARTESIAN_POINT('Ctrl Pts',(-44.4232546759027,29.5404524382925,
-48.1112592960261));
#237597=CARTESIAN_POINT('Ctrl Pts',(-44.5079524583208,29.5404524382925,
-48.1162000000005));
#237598=CARTESIAN_POINT('Origin',(-44.5079524583208,31.5404524382925,235.35105));
#237599=CARTESIAN_POINT('',(-44.5079524583208,29.5404524382925,-46.7162000000005));
#237600=CARTESIAN_POINT('',(-44.5079524583208,29.5404524382925,-46.8749499999997));
#237601=CARTESIAN_POINT('',(-44.5079524583208,29.5404524382925,235.35105));
#237602=CARTESIAN_POINT('Ctrl Pts',(-44.5079524583208,29.5404524382925,
-47.5749499999996));
#237603=CARTESIAN_POINT('Ctrl Pts',(-44.2790401916845,29.5404524382925,
-47.5615967844459));
#237604=CARTESIAN_POINT('Ctrl Pts',(-44.0515134278049,29.5797563843007,
-47.5483243898863));
#237605=CARTESIAN_POINT('Ctrl Pts',(-43.5948870817519,29.7428074112483,
-47.5216878530334));
#237606=CARTESIAN_POINT('Ctrl Pts',(-43.3730898217265,29.8739277980452,
-47.5093729124444));
#237607=CARTESIAN_POINT('Ctrl Pts',(-42.9878325441943,30.2151410676517,
-47.4808987792072));
#237608=CARTESIAN_POINT('Ctrl Pts',(-42.8290298482996,30.4231285580667,
-47.4657598909722));
#237609=CARTESIAN_POINT('Ctrl Pts',(-42.5970500796493,30.893352521703,-47.435238970338));
#237610=CARTESIAN_POINT('Ctrl Pts',(-42.5281738590795,31.1521133878894,
-47.4201579606935));
#237611=CARTESIAN_POINT('Ctrl Pts',(-42.4961237146183,31.6695339342438,
-47.3930840367877));
#237612=CARTESIAN_POINT('Ctrl Pts',(-42.5285979724327,31.9229682037961,
-47.3800238509062));
#237613=CARTESIAN_POINT('Ctrl Pts',(-42.6892492137716,32.412862045555,-47.3505896598269));
#237614=CARTESIAN_POINT('Ctrl Pts',(-42.8191939761698,32.6435720986671,
-47.3351445595209));
#237615=CARTESIAN_POINT('Ctrl Pts',(-43.1625390471162,33.0438263860826,
-47.3049102227339));
#237616=CARTESIAN_POINT('Ctrl Pts',(-43.3733681478899,33.2086657806137,
-47.2911340847757));
#237617=CARTESIAN_POINT('Ctrl Pts',(-43.8471273660993,33.4466628425882,
-47.2634981303801));
#237618=CARTESIAN_POINT('Ctrl Pts',(-44.1053866322545,33.5173752418216,
-47.248433006521));
#237619=CARTESIAN_POINT('Ctrl Pts',(-44.6285574664938,33.553583731792,-47.2179147078569));
#237620=CARTESIAN_POINT('Ctrl Pts',(-44.8883012981081,33.5210075007997,
-47.202762984346));
#237621=CARTESIAN_POINT('Ctrl Pts',(-45.3769781595273,33.3597763480789,
-47.1742568340965));
#237622=CARTESIAN_POINT('Ctrl Pts',(-45.6017771569532,33.2341733546916,
-47.1619437578205));
#237623=CARTESIAN_POINT('Ctrl Pts',(-46.0006808176217,32.8979394298809,
-47.133323152355));
#237624=CARTESIAN_POINT('Ctrl Pts',(-46.1680481645495,32.6872153317937,
-47.1177962134451));
#237625=CARTESIAN_POINT('Ctrl Pts',(-46.4057601468361,32.2216462196778,
-47.0873432577269));
#237626=CARTESIAN_POINT('Ctrl Pts',(-46.4773703160619,31.9730373316473,
-47.0726953670536));
#237627=CARTESIAN_POINT('Ctrl Pts',(-46.5233230608925,31.4564293490652,
-47.0452569998543));
#237628=CARTESIAN_POINT('Ctrl Pts',(-46.4949626727678,31.1931783110856,
-47.0320274853069));
#237629=CARTESIAN_POINT('Ctrl Pts',(-46.3379528821531,30.691720510442,-47.0021153134141));
#237630=CARTESIAN_POINT('Ctrl Pts',(-46.2105292972496,30.4585672754571,
-46.9866203224269));
#237631=CARTESIAN_POINT('Ctrl Pts',(-45.8788590973917,30.0623004629269,
-46.9569279425619));
#237632=CARTESIAN_POINT('Ctrl Pts',(-45.6806277956508,29.900612732495,-46.9433560613437));
#237633=CARTESIAN_POINT('Ctrl Pts',(-45.2242017661382,29.6543737657247,
-46.9167312096222));
#237634=CARTESIAN_POINT('Ctrl Pts',(-44.9681651385769,29.5761558991475,
-46.9017957396811));
#237635=CARTESIAN_POINT('Ctrl Pts',(-44.6389915185149,29.5436682735582,
-46.8825939451776));
#237636=CARTESIAN_POINT('Ctrl Pts',(-44.5734344131156,29.5404524382925,
-46.878769780696));
#237637=CARTESIAN_POINT('Ctrl Pts',(-44.5079524583208,29.5404524382925,
-46.8749499999997));
#237638=CARTESIAN_POINT('Ctrl Pts',(-44.5079524583208,29.5404524382925,
-46.7162000000005));
#237639=CARTESIAN_POINT('Ctrl Pts',(-44.7564402632578,29.5404524382925,
-46.7306951219552));
#237640=CARTESIAN_POINT('Ctrl Pts',(-45.0028783481848,29.586763517434,-46.7450706769092));
#237641=CARTESIAN_POINT('Ctrl Pts',(-45.4747682115069,29.770783442715,-46.7725975856031));
#237642=CARTESIAN_POINT('Ctrl Pts',(-45.6945496843684,29.9099755438604,
-46.78510707846));
#237643=CARTESIAN_POINT('Ctrl Pts',(-46.0744438759381,30.2691102378815,
-46.8143301455376));
#237644=CARTESIAN_POINT('Ctrl Pts',(-46.2288994520815,30.4875840958792,
-46.8298719946552));
#237645=CARTESIAN_POINT('Ctrl Pts',(-46.4396370053616,30.9628662222822,
-46.8600288796926));
#237646=CARTESIAN_POINT('Ctrl Pts',(-46.4974841926455,31.2136212729569,
-46.8743837702223));
#237647=CARTESIAN_POINT('Ctrl Pts',(-46.5162685102811,31.7355259471015,
-46.9012973040128));
#237648=CARTESIAN_POINT('Ctrl Pts',(-46.4722813752727,32.0018365091121,
-46.9155486756193));
#237649=CARTESIAN_POINT('Ctrl Pts',(-46.2841830000069,32.4961949103054,
-46.9460089493815));
#237650=CARTESIAN_POINT('Ctrl Pts',(-46.1440724337216,32.7200947827809,
-46.9614065145837));
#237651=CARTESIAN_POINT('Ctrl Pts',(-45.7912746217199,33.0952069681266,
-46.9906464238707));
#237652=CARTESIAN_POINT('Ctrl Pts',(-45.5842799981298,33.2450541268618,
-47.0034142268443));
#237653=CARTESIAN_POINT('Ctrl Pts',(-45.1145561139262,33.4646088685245,
-47.030814786756));
#237654=CARTESIAN_POINT('Ctrl Pts',(-44.8543600324493,33.5279904158309,
-47.0459928915088));
#237655=CARTESIAN_POINT('Ctrl Pts',(-44.3310385260286,33.5493271984139,
-47.0765199793832));
#237656=CARTESIAN_POINT('Ctrl Pts',(-44.0730171296042,33.5096482784744,
-47.091571227508));
#237657=CARTESIAN_POINT('Ctrl Pts',(-43.588470387443,33.3349726475461,-47.119836454134));
#237658=CARTESIAN_POINT('Ctrl Pts',(-43.3662526306331,33.2024613684762,
-47.1322046309404));
#237659=CARTESIAN_POINT('Ctrl Pts',(-42.9769787956073,32.8544983659666,
-47.1611368977808));
#237660=CARTESIAN_POINT('Ctrl Pts',(-42.8161564949552,32.6397260889244,
-47.1766774460134));
#237661=CARTESIAN_POINT('Ctrl Pts',(-42.5921602652309,32.1690122033702,
-47.2069902633773));
#237662=CARTESIAN_POINT('Ctrl Pts',(-42.5275667981423,31.9192144321939,
-47.2214935604135));
#237663=CARTESIAN_POINT('Ctrl Pts',(-42.4954253358138,31.3998649668793,
-47.2486675931718));
#237664=CARTESIAN_POINT('Ctrl Pts',(-42.5316545863151,31.1350799987585,
-47.2623699771863));
#237665=CARTESIAN_POINT('Ctrl Pts',(-42.7044030484733,30.6371002695444,
-47.2925654879368));
#237666=CARTESIAN_POINT('Ctrl Pts',(-42.8383316269604,30.4085500582092,
-47.308017671671));
#237667=CARTESIAN_POINT('Ctrl Pts',(-43.1807669366193,30.0229712011951,
-47.3374840981808));
#237668=CARTESIAN_POINT('Ctrl Pts',(-43.3833866896859,29.8672896342856,
-47.3506003301631));
#237669=CARTESIAN_POINT('Ctrl Pts',(-43.8465664256208,29.6344366411589,
-47.3776191480928));
#237670=CARTESIAN_POINT('Ctrl Pts',(-44.1048044388238,29.5636483406197,
-47.3926830321964));
#237671=CARTESIAN_POINT('Ctrl Pts',(-44.4154946330336,29.5420535557601,
-47.4108066268586));
#237672=CARTESIAN_POINT('Ctrl Pts',(-44.4617479071714,29.5404524382925,
-47.4135047345167));
#237673=CARTESIAN_POINT('Ctrl Pts',(-44.5079524583208,29.5404524382925,
-47.4162000000004));
#237674=CARTESIAN_POINT('Origin',(-44.5079524583208,31.5404524382925,235.35105));
#237675=CARTESIAN_POINT('',(-44.5079524583208,29.5404524382925,-46.0162000000005));
#237676=CARTESIAN_POINT('',(-44.5079524583208,29.5404524382925,-46.1749499999996));
#237677=CARTESIAN_POINT('',(-44.5079524583208,29.5404524382925,235.35105));
#237678=CARTESIAN_POINT('Ctrl Pts',(-44.5079524583208,29.5404524382925,
-46.8749499999997));
#237679=CARTESIAN_POINT('Ctrl Pts',(-44.3143021702569,29.5404524382925,
-46.863653733196));
#237680=CARTESIAN_POINT('Ctrl Pts',(-44.1213091244848,29.5685798054682,
-46.852395805526));
#237681=CARTESIAN_POINT('Ctrl Pts',(-43.6914378076858,29.6970917220659,
-46.8273199787128));
#237682=CARTESIAN_POINT('Ctrl Pts',(-43.4639541085933,29.8157104726805,
-46.8149641523025));
#237683=CARTESIAN_POINT('Ctrl Pts',(-43.0553918712656,30.1399165374395,
-46.7866694635722));
#237684=CARTESIAN_POINT('Ctrl Pts',(-42.8814651000635,30.3463248186168,
-46.771169235201));
#237685=CARTESIAN_POINT('Ctrl Pts',(-42.6299160339596,30.8062603392753,
-46.7405972964818));
#237686=CARTESIAN_POINT('Ctrl Pts',(-42.5511871182224,31.0534597168105,
-46.7258129815627));
#237687=CARTESIAN_POINT('Ctrl Pts',(-42.4912834411294,31.567196639013,-46.6981127528274));
#237688=CARTESIAN_POINT('Ctrl Pts',(-42.5118432659359,31.8289562196735,
-46.6852618412255));
#237689=CARTESIAN_POINT('Ctrl Pts',(-42.653100990733,32.3336677708646,-46.6556447311323));
#237690=CARTESIAN_POINT('Ctrl Pts',(-42.7738520231998,32.5712535567185,
-46.6401204319946));
#237691=CARTESIAN_POINT('Ctrl Pts',(-43.0945944652074,32.9781731096842,
-46.6102086216764));
#237692=CARTESIAN_POINT('Ctrl Pts',(-43.2885188885881,33.1459085169591,
-46.5960836249017));
#237693=CARTESIAN_POINT('Ctrl Pts',(-43.738147121595,33.4053064718327,-46.5698553113095));
#237694=CARTESIAN_POINT('Ctrl Pts',(-43.9917954352067,33.4907881687241,
-46.5550591596821));
#237695=CARTESIAN_POINT('Ctrl Pts',(-44.5133362311153,33.557373773589,-46.5246359465874));
#237696=CARTESIAN_POINT('Ctrl Pts',(-44.7759962087206,33.5394933565031,
-46.5093141145603));
#237697=CARTESIAN_POINT('Ctrl Pts',(-45.2727989878659,33.4057598484895,
-46.4803339524434));
#237698=CARTESIAN_POINT('Ctrl Pts',(-45.5029417480266,33.2938328714309,
-46.4678403455768));
#237699=CARTESIAN_POINT('Ctrl Pts',(-45.9184513158687,32.9829695593626,
-46.4400170775355));
#237700=CARTESIAN_POINT('Ctrl Pts',(-46.0970988735073,32.7834089690963,
-46.4247250922264));
#237701=CARTESIAN_POINT('Ctrl Pts',(-46.3623616986635,32.3326811878688,
-46.3942183268163));
#237702=CARTESIAN_POINT('Ctrl Pts',(-46.448949684947,32.0872788365525,-46.3792955714436));
#237703=CARTESIAN_POINT('Ctrl Pts',(-46.5242122990237,31.5768211820417,
-46.3513130362452));
#237704=CARTESIAN_POINT('Ctrl Pts',(-46.5120818147021,31.3166221890583,
-46.3387629497789));
#237705=CARTESIAN_POINT('Ctrl Pts',(-46.3879880918281,30.8086117835772,
-46.3094798043972));
#237706=CARTESIAN_POINT('Ctrl Pts',(-46.2746832139355,30.5664030893519,
-46.293939143996));
#237707=CARTESIAN_POINT('Ctrl Pts',(-45.9662539710802,30.1482250005864,
-46.2638177082691));
#237708=CARTESIAN_POINT('Ctrl Pts',(-45.7771529020937,29.9738907471899,
-46.2494952167125));
#237709=CARTESIAN_POINT('Ctrl Pts',(-45.3326938112695,29.6988515142441,
-46.2226373537353));
#237710=CARTESIAN_POINT('Ctrl Pts',(-45.0789563152446,29.6050636206244,
-46.20825855832));
#237711=CARTESIAN_POINT('Ctrl Pts',(-44.7126485077894,29.5483025272819,
-46.1868906028852));
#237712=CARTESIAN_POINT('Ctrl Pts',(-44.6102608596984,29.5404524382925,
-46.18091799008));
#237713=CARTESIAN_POINT('Ctrl Pts',(-44.5079524583208,29.5404524382925,
-46.1749499999996));
#237714=CARTESIAN_POINT('Ctrl Pts',(-44.5079524583208,29.5404524382925,
-46.0162000000005));
#237715=CARTESIAN_POINT('Ctrl Pts',(-44.5383536771069,29.5404524382925,
-46.0179734044297));
#237716=CARTESIAN_POINT('Ctrl Pts',(-44.5687810503939,29.5411456067265,
-46.0197483345381));
#237717=CARTESIAN_POINT('Ctrl Pts',(-44.8554070412256,29.5542378028698,
-46.0364681840033));
#237718=CARTESIAN_POINT('Ctrl Pts',(-45.1070127036482,29.6151117604346,
-46.051145180978));
#237719=CARTESIAN_POINT('Ctrl Pts',(-45.5783230337682,29.8308201602911,
-46.0786382835683));
#237720=CARTESIAN_POINT('Ctrl Pts',(-45.7926673939301,29.9854378464794,
-46.0917810608028));
#237721=CARTESIAN_POINT('Ctrl Pts',(-46.15067990082,30.3696491201322,-46.1216327344523));
#237722=CARTESIAN_POINT('Ctrl Pts',(-46.2903845425981,30.5958548497405,
-46.137134947823));
#237723=CARTESIAN_POINT('Ctrl Pts',(-46.470781347776,31.0803748758474,-46.1668735759635));
#237724=CARTESIAN_POINT('Ctrl Pts',(-46.5132304133134,31.3327377152465,
-46.1805526964107));
#237725=CARTESIAN_POINT('Ctrl Pts',(-46.5013618106744,31.8512900681338,
-46.2070951687838));
#237726=CARTESIAN_POINT('Ctrl Pts',(-46.4426453630262,32.1124787945741,
-46.2220025027231));
#237727=CARTESIAN_POINT('Ctrl Pts',(-46.2288377388442,32.5922400048864,
-46.2524752065213));
#237728=CARTESIAN_POINT('Ctrl Pts',(-46.0775458753399,32.8069810465109,
-46.2677362057149));
#237729=CARTESIAN_POINT('Ctrl Pts',(-45.705574354989,33.162272184137,-46.2965340255289));
#237730=CARTESIAN_POINT('Ctrl Pts',(-45.4900510161627,33.3011542993969,
-46.308910917459));
#237731=CARTESIAN_POINT('Ctrl Pts',(-45.0061505371029,33.4957832007704,
-46.337138445404));
#237732=CARTESIAN_POINT('Ctrl Pts',(-44.7405522996734,33.5447939295987,
-46.3526316759207));
#237733=CARTESIAN_POINT('Ctrl Pts',(-44.2160984402956,33.5356850725764,
-46.3832248177176));
#237734=CARTESIAN_POINT('Ctrl Pts',(-43.9622017190187,33.4816688204458,
-46.3980354597921));
#237735=CARTESIAN_POINT('Ctrl Pts',(-43.4864450689416,33.2794138062905,
-46.4257879310466));
#237736=CARTESIAN_POINT('Ctrl Pts',(-43.26950932895,33.1322243219307,-46.4385745561242));
#237737=CARTESIAN_POINT('Ctrl Pts',(-42.9009215232177,32.7599607115152,
-46.4681311021637));
#237738=CARTESIAN_POINT('Ctrl Pts',(-42.754110809741,32.5373365857783,-46.4836596399625));
#237739=CARTESIAN_POINT('Ctrl Pts',(-42.5591896442861,32.0571131135749,
-46.5136048413296));
#237740=CARTESIAN_POINT('Ctrl Pts',(-42.509344177805,31.8054569258723,-46.5277718721102));
#237741=CARTESIAN_POINT('Ctrl Pts',(-42.5065609942799,31.2862157253844,
-46.5540841523981));
#237742=CARTESIAN_POINT('Ctrl Pts',(-42.5578084465479,31.0234825992861,
-46.5687704921146));
#237743=CARTESIAN_POINT('Ctrl Pts',(-42.7582857197508,30.5370872462227,
-46.5991895386185));
#237744=CARTESIAN_POINT('Ctrl Pts',(-42.9039655063881,30.3176230386802,
-46.6145254578345));
#237745=CARTESIAN_POINT('Ctrl Pts',(-43.2662348402282,29.9522288050545,
-46.6435506869134));
#237746=CARTESIAN_POINT('Ctrl Pts',(-43.477368658903,29.8077676195006,-46.6560826117008));
#237747=CARTESIAN_POINT('Ctrl Pts',(-43.9531006830822,29.6007360692539,
-46.6838336464447));
#237748=CARTESIAN_POINT('Ctrl Pts',(-44.2149321958984,29.5443404907937,
-46.6991071513591));
#237749=CARTESIAN_POINT('Ctrl Pts',(-44.4893817598351,29.5405170815757,
-46.7151167092554));
#237750=CARTESIAN_POINT('Ctrl Pts',(-44.4986685396741,29.5404524382925,
-46.7156584380794));
#237751=CARTESIAN_POINT('Ctrl Pts',(-44.5079524583208,29.5404524382925,
-46.7162000000005));
#237752=CARTESIAN_POINT('Origin',(-44.5079524583208,31.5404524382925,235.35105));
#237753=CARTESIAN_POINT('',(-44.5079524583208,29.5404524382925,-45.3162000000005));
#237754=CARTESIAN_POINT('',(-44.5079524583208,29.5404524382925,-45.4749499999996));
#237755=CARTESIAN_POINT('',(-44.5079524583208,29.5404524382925,235.35105));
#237756=CARTESIAN_POINT('Ctrl Pts',(-44.5079524583208,29.5404524382925,
-46.1749499999996));
#237757=CARTESIAN_POINT('Ctrl Pts',(-44.3499883457847,29.5404524382925,
-46.1657354267684));
#237758=CARTESIAN_POINT('Ctrl Pts',(-44.1922131522001,29.5591675560845,
-46.1565318738093));
#237759=CARTESIAN_POINT('Ctrl Pts',(-43.7916928277782,29.6559975471492,
-46.1331681882181));
#237760=CARTESIAN_POINT('Ctrl Pts',(-43.5590243839374,29.7617710997056,
-46.1204619525901));
#237761=CARTESIAN_POINT('Ctrl Pts',(-43.1358040936022,30.0614127809282,
-46.0929806844905));
#237762=CARTESIAN_POINT('Ctrl Pts',(-42.9519999941258,30.2561932014292,
-46.0777797853709));
#237763=CARTESIAN_POINT('Ctrl Pts',(-42.6746557778512,30.7003211188648,
-46.047254058953));
#237764=CARTESIAN_POINT('Ctrl Pts',(-42.5815292159222,30.9440327901853,
-46.0322260051473));
#237765=CARTESIAN_POINT('Ctrl Pts',(-42.4935001036119,31.4516693923597,
-46.0040136280915));
#237766=CARTESIAN_POINT('Ctrl Pts',(-42.4987391411722,31.7106454145308,
-45.9916208876941));
#237767=CARTESIAN_POINT('Ctrl Pts',(-42.6087130924422,32.2211856295038,
-45.9626217676926));
#237768=CARTESIAN_POINT('Ctrl Pts',(-42.71576292151,32.46702931215,-45.9470799133305));
#237769=CARTESIAN_POINT('Ctrl Pts',(-43.0138453266327,32.8943041431967,
-45.9168007097928));
#237770=CARTESIAN_POINT('Ctrl Pts',(-43.1988484496968,33.0739317835504,
-45.9023303295503));
#237771=CARTESIAN_POINT('Ctrl Pts',(-43.6345701344869,33.3591136145181,
-45.8752149223088));
#237772=CARTESIAN_POINT('Ctrl Pts',(-43.8831646935248,33.4587903990257,
-45.8613959529469));
#237773=CARTESIAN_POINT('Ctrl Pts',(-44.4018450959186,33.5547728555338,
-45.8311395961405));
#237774=CARTESIAN_POINT('Ctrl Pts',(-44.6665470282396,33.5513217783439,
-45.8156986500884));
#237775=CARTESIAN_POINT('Ctrl Pts',(-45.1708172757467,33.4443351603151,
-45.7862828856504));
#237776=CARTESIAN_POINT('Ctrl Pts',(-45.4062982186259,33.3451934933126,
-45.7732537587104));
#237777=CARTESIAN_POINT('Ctrl Pts',(-45.8377023124348,33.0577188693083,
-45.7461484535465));
#237778=CARTESIAN_POINT('Ctrl Pts',(-46.0269178118715,32.8682447374916,
-45.7310577858079));
#237779=CARTESIAN_POINT('Ctrl Pts',(-46.3171023630338,32.4315978014306,
-45.7005354749506));
#237780=CARTESIAN_POINT('Ctrl Pts',(-46.4172456921539,32.189901539422,-45.6854045801821));
#237781=CARTESIAN_POINT('Ctrl Pts',(-46.5189861151194,31.6853905271185,
-45.656950188912));
#237782=CARTESIAN_POINT('Ctrl Pts',(-46.5210440443298,31.4276495789899,
-45.6446332463212));
#237783=CARTESIAN_POINT('Ctrl Pts',(-46.4260812542442,30.9145917233784,
-45.6159447653103));
#237784=CARTESIAN_POINT('Ctrl Pts',(-46.3258014972443,30.6650555678543,
-45.6004138344901));
#237785=CARTESIAN_POINT('Ctrl Pts',(-46.0390006125387,30.2283874424556,
-45.5699891434584));
#237786=CARTESIAN_POINT('Ctrl Pts',(-45.8585125153081,30.0432387913122,
-45.5553715402261));
#237787=CARTESIAN_POINT('Ctrl Pts',(-45.4320917831814,29.7474100204124,
-45.5279895470776));
#237788=CARTESIAN_POINT('Ctrl Pts',(-45.1888087028346,29.6416361403906,
-45.5146666142627));
#237789=CARTESIAN_POINT('Ctrl Pts',(-44.7923251502757,29.5556220098947,
-45.4915384070302));
#237790=CARTESIAN_POINT('Ctrl Pts',(-44.6501700009571,29.5404524382925,
-45.4832460233201));
#237791=CARTESIAN_POINT('Ctrl Pts',(-44.5079524583208,29.5404524382925,
-45.4749499999996));
#237792=CARTESIAN_POINT('Ctrl Pts',(-44.5079524583208,29.5404524382925,
-45.3162000000005));
#237793=CARTESIAN_POINT('Ctrl Pts',(-44.5752886867944,29.5404524382925,
-45.3201279466614));
#237794=CARTESIAN_POINT('Ctrl Pts',(-44.6427020885513,29.5438529784239,
-45.324060395097));
#237795=CARTESIAN_POINT('Ctrl Pts',(-44.9637283423644,29.5764404651513,
-45.3427869265695));
#237796=CARTESIAN_POINT('Ctrl Pts',(-45.2103073144421,29.6505276104354,
-45.357170699941));
#237797=CARTESIAN_POINT('Ctrl Pts',(-45.6725387562852,29.8927703223525,
-45.3841342007152));
#237798=CARTESIAN_POINT('Ctrl Pts',(-45.8816674111162,30.0625838873391,
-45.3982741697899));
#237799=CARTESIAN_POINT('Ctrl Pts',(-46.2178256572483,30.4704768600807,
-45.4286847830932));
#237800=CARTESIAN_POINT('Ctrl Pts',(-46.3430369784634,30.7032045710331,
-45.4440937530365));
#237801=CARTESIAN_POINT('Ctrl Pts',(-46.4942135996953,31.1955882923935,
-45.473377385137));
#237802=CARTESIAN_POINT('Ctrl Pts',(-46.5218734780736,31.4496006556456,
-45.4862043064054));
#237803=CARTESIAN_POINT('Ctrl Pts',(-46.4799910133021,31.9663710348521,
-45.5135321610796));
#237804=CARTESIAN_POINT('Ctrl Pts',(-46.4061981185894,32.2238006132641,
-45.5286893195264));
#237805=CARTESIAN_POINT('Ctrl Pts',(-46.1655110794876,32.6891241595004,
-45.5592166422012));
#237806=CARTESIAN_POINT('Ctrl Pts',(-46.0031516230724,32.8937264714402,
-45.5742882563357));
#237807=CARTESIAN_POINT('Ctrl Pts',(-45.61145913328,33.2280228330628,-45.6026006538787));
#237808=CARTESIAN_POINT('Ctrl Pts',(-45.3865124168643,33.3553228205668,
-45.6149506690847));
#237809=CARTESIAN_POINT('Ctrl Pts',(-44.8915620166817,33.5212403492853,
-45.6438227757619));
#237810=CARTESIAN_POINT('Ctrl Pts',(-44.625181292559,33.5546303190202,-45.6593616513357));
#237811=CARTESIAN_POINT('Ctrl Pts',(-44.1050333555753,33.5160717933918,
-45.6897036143263));
#237812=CARTESIAN_POINT('Ctrl Pts',(-43.8559077769371,33.4484077857242,
-45.7042359397469));
#237813=CARTESIAN_POINT('Ctrl Pts',(-43.3891733207894,33.2191740955852,
-45.7314621163555));
#237814=CARTESIAN_POINT('Ctrl Pts',(-43.1774647128587,33.0569025576557,
-45.7450643068372));
#237815=CARTESIAN_POINT('Ctrl Pts',(-42.8304222957157,32.6606348682511,
-45.7752050873378));
#237816=CARTESIAN_POINT('Ctrl Pts',(-42.6980291883871,32.4310106793887,
-45.7906667418528));
#237817=CARTESIAN_POINT('Ctrl Pts',(-42.5324528658392,31.9424334735313,
-45.8201780671262));
#237818=CARTESIAN_POINT('Ctrl Pts',(-42.4974840288384,31.6892830248564,
-45.8333760251249));
#237819=CARTESIAN_POINT('Ctrl Pts',(-42.5244614333995,31.1715527096957,
-45.8603176430636));
#237820=CARTESIAN_POINT('Ctrl Pts',(-42.5907918097007,30.9121428759785,
-45.8753571835553));
#237821=CARTESIAN_POINT('Ctrl Pts',(-42.8182406097052,30.439455042982,-45.9058704210559));
#237822=CARTESIAN_POINT('Ctrl Pts',(-42.9751815563657,30.2297448947546,
-45.9210420337551));
#237823=CARTESIAN_POINT('Ctrl Pts',(-43.3571097235158,29.8849776008381,
-45.9495986106678));
#237824=CARTESIAN_POINT('Ctrl Pts',(-43.5773052343559,29.7518975545269,
-45.9619122452689));
#237825=CARTESIAN_POINT('Ctrl Pts',(-44.0382118459221,29.5821060668551,
-45.9887984642771));
#237826=CARTESIAN_POINT('Ctrl Pts',(-44.2722963888769,29.5404524382925,
-46.0024533959495));
#237827=CARTESIAN_POINT('Ctrl Pts',(-44.5079524583208,29.5404524382925,
-46.0162000000005));
#237828=CARTESIAN_POINT('Origin',(-44.5079524583208,31.5404524382925,235.35105));
#237829=CARTESIAN_POINT('',(-44.5079524583208,29.5404524382925,-44.6162000000005));
#237830=CARTESIAN_POINT('',(-44.5079524583208,29.5404524382925,-44.7749499999996));
#237831=CARTESIAN_POINT('',(-44.5079524583208,29.5404524382925,235.35105));
#237832=CARTESIAN_POINT('Ctrl Pts',(-44.5079524583208,29.5404524382925,
-45.4749499999996));
#237833=CARTESIAN_POINT('Ctrl Pts',(-44.3884404302508,29.5404524382925,
-45.4679784650289));
#237834=CARTESIAN_POINT('Ctrl Pts',(-44.2688843411178,29.5511646694685,
-45.4610043598295));
#237835=CARTESIAN_POINT('Ctrl Pts',(-43.9012887286443,29.6178935469937,
-45.4395612824353));
#237836=CARTESIAN_POINT('Ctrl Pts',(-43.6627974894879,29.7101746456848,
-45.4260952254977));
#237837=CARTESIAN_POINT('Ctrl Pts',(-43.2230751000556,29.9850100727128,
-45.3993858122089));
#237838=CARTESIAN_POINT('Ctrl Pts',(-43.0284398716923,30.1688457313581,
-45.3844219142687));
#237839=CARTESIAN_POINT('Ctrl Pts',(-42.7252141543255,30.5973786185983,
-45.3539291427878));
#237840=CARTESIAN_POINT('Ctrl Pts',(-42.6178693581101,30.8367857273349,
-45.3387038490141));
#237841=CARTESIAN_POINT('Ctrl Pts',(-42.5020198797053,31.3379781831177,
-45.3100055909587));
#237842=CARTESIAN_POINT('Ctrl Pts',(-42.4925541004512,31.5945318855494,
-45.2976671252213));
#237843=CARTESIAN_POINT('Ctrl Pts',(-42.5722405742376,32.1099813837036,
-45.2693033820827));
#237844=CARTESIAN_POINT('Ctrl Pts',(-42.6655125922908,32.3630878196491,
-45.2537964796918));
#237845=CARTESIAN_POINT('Ctrl Pts',(-42.9405500282181,32.8090078723666,
-45.2232474990108));
#237846=CARTESIAN_POINT('Ctrl Pts',(-43.1162818009553,32.9996544475994,
-45.2084908769637));
#237847=CARTESIAN_POINT('Ctrl Pts',(-43.533224312882,33.3061798501348,-45.1808449578783));
#237848=CARTESIAN_POINT('Ctrl Pts',(-43.7712693626966,33.4180055638395,
-45.1679231805785));
#237849=CARTESIAN_POINT('Ctrl Pts',(-44.28006033097,33.544858196687,-45.1382437074292));
#237850=CARTESIAN_POINT('Ctrl Pts',(-44.5461058074549,33.5574089118735,
-45.1227243879675));
#237851=CARTESIAN_POINT('Ctrl Pts',(-45.0581062113836,33.4800081747317,
-45.0928576977382));
#237852=CARTESIAN_POINT('Ctrl Pts',(-45.2996831041404,33.3945297789453,
-45.078855744023));
#237853=CARTESIAN_POINT('Ctrl Pts',(-45.7474950569434,33.132250299015,-45.0525446883363));
#237854=CARTESIAN_POINT('Ctrl Pts',(-45.9473071006096,32.9541327539777,
-45.0377186684623));
#237855=CARTESIAN_POINT('Ctrl Pts',(-46.2631753763515,32.5339890935242,
-45.0072809639001));
#237856=CARTESIAN_POINT('Ctrl Pts',(-46.377577875197,32.2970472517023,-44.9919743611866));
#237857=CARTESIAN_POINT('Ctrl Pts',(-46.5073145669426,31.7992306316387,
-44.9630416003788));
#237858=CARTESIAN_POINT('Ctrl Pts',(-46.5239858684761,31.5437495211416,
-44.9505842036502));
#237859=CARTESIAN_POINT('Ctrl Pts',(-46.4591671137971,31.0261349851744,
-44.9225447286169));
#237860=CARTESIAN_POINT('Ctrl Pts',(-46.3728195132755,30.7697405399738,
-44.9070736842639));
#237861=CARTESIAN_POINT('Ctrl Pts',(-46.1094871362041,30.3151271858606,
-44.8764269316416));
#237862=CARTESIAN_POINT('Ctrl Pts',(-45.9385337983681,30.1192546985941,
-44.861545677212));
#237863=CARTESIAN_POINT('Ctrl Pts',(-45.530828254992,29.8024494454341,-44.8336498506883));
#237864=CARTESIAN_POINT('Ctrl Pts',(-45.2977182116059,29.6848636532952,
-44.8210196689411));
#237865=CARTESIAN_POINT('Ctrl Pts',(-44.8722812568097,29.5654047678576,
-44.7962025132447));
#237866=CARTESIAN_POINT('Ctrl Pts',(-44.6903467166921,29.5404524382925,
-44.7855896650713));
#237867=CARTESIAN_POINT('Ctrl Pts',(-44.5079524583208,29.5404524382925,
-44.7749499999996));
#237868=CARTESIAN_POINT('Ctrl Pts',(-44.5079524583208,29.5404524382925,
-44.6162000000005));
#237869=CARTESIAN_POINT('Ctrl Pts',(-44.6122192188551,29.5404524382925,
-44.6222822276983));
#237870=CARTESIAN_POINT('Ctrl Pts',(-44.716562581159,29.5486059400025,-44.6283689238327));
#237871=CARTESIAN_POINT('Ctrl Pts',(-45.0843777019556,29.6067092957952,
-44.6498248058792));
#237872=CARTESIAN_POINT('Ctrl Pts',(-45.3375946885842,29.7010931643449,
-44.6641435400043));
#237873=CARTESIAN_POINT('Ctrl Pts',(-45.7811807138443,29.9771521689784,
-44.6910274555468));
#237874=CARTESIAN_POINT('Ctrl Pts',(-45.9698787058019,30.15201982734,-44.7053651373213));
#237875=CARTESIAN_POINT('Ctrl Pts',(-46.2772853751844,30.5711184567403,
-44.7355032519971));
#237876=CARTESIAN_POINT('Ctrl Pts',(-46.389970016758,30.8136974900051,-44.7510445310149));
#237877=CARTESIAN_POINT('Ctrl Pts',(-46.5126520729056,31.3219681554154,
-44.7802996506334));
#237878=CARTESIAN_POINT('Ctrl Pts',(-46.5240920270596,31.5820422493856,
-44.7928303028339));
#237879=CARTESIAN_POINT('Ctrl Pts',(-46.4475585219114,32.0922229686962,
-44.8208359154349));
#237880=CARTESIAN_POINT('Ctrl Pts',(-46.3603196882749,32.3374650435143,
-44.8357695569832));
#237881=CARTESIAN_POINT('Ctrl Pts',(-46.0938493289167,32.7875517806148,
-44.8662791577781));
#237882=CARTESIAN_POINT('Ctrl Pts',(-45.9146836175038,32.9866436168496,
-44.8815625753197));
#237883=CARTESIAN_POINT('Ctrl Pts',(-45.4984024727998,33.2963945808861,
-44.9093521539228));
#237884=CARTESIAN_POINT('Ctrl Pts',(-45.268012095978,33.4077096809596,-44.9218631878031));
#237885=CARTESIAN_POINT('Ctrl Pts',(-44.7708483802375,33.5401854738332,
-44.9508644045545));
#237886=CARTESIAN_POINT('Ctrl Pts',(-44.5080747570903,33.5573895966803,
-44.9661928659047));
#237887=CARTESIAN_POINT('Ctrl Pts',(-43.9864789169903,33.4893962270578,
-44.9966192899104));
#237888=CARTESIAN_POINT('Ctrl Pts',(-43.7330682428071,33.4031791871255,
-45.0113659496721));
#237889=CARTESIAN_POINT('Ctrl Pts',(-43.2840691961485,33.1425552376921,
-45.0376279945938));
#237890=CARTESIAN_POINT('Ctrl Pts',(-43.0905893083135,32.974208798702,-45.0517757084025));
#237891=CARTESIAN_POINT('Ctrl Pts',(-42.7709778104767,32.5664218049919,
-45.0816983543494));
#237892=CARTESIAN_POINT('Ctrl Pts',(-42.6508593773377,32.3284303032967,
-45.0972246986866));
#237893=CARTESIAN_POINT('Ctrl Pts',(-42.5110760907483,31.8234254495933,
-45.1268136214321));
#237894=CARTESIAN_POINT('Ctrl Pts',(-42.4912430285492,31.5618027775643,
-45.1396340620203));
#237895=CARTESIAN_POINT('Ctrl Pts',(-42.5524594664912,31.048341281544,-45.1673586655931));
#237896=CARTESIAN_POINT('Ctrl Pts',(-42.6318594285012,30.8012854209585,
-45.1821553024847));
#237897=CARTESIAN_POINT('Ctrl Pts',(-42.8847087561168,30.3419026329704,
-45.2127372424671));
#237898=CARTESIAN_POINT('Ctrl Pts',(-43.0592496209379,30.1359121223225,
-45.2282342769088));
#237899=CARTESIAN_POINT('Ctrl Pts',(-43.4687171145355,29.8128472013648,
-45.2564977204751));
#237900=CARTESIAN_POINT('Ctrl Pts',(-43.6964582419797,29.6948860705821,
-45.2688628373804));
#237901=CARTESIAN_POINT('Ctrl Pts',(-44.1248814272467,29.5680588587409,
-45.2938541898544));
#237902=CARTESIAN_POINT('Ctrl Pts',(-44.3161037171375,29.5404524382925,
-45.3050088234314));
#237903=CARTESIAN_POINT('Ctrl Pts',(-44.5079524583208,29.5404524382925,
-45.3162000000005));
#237904=CARTESIAN_POINT('Origin',(-44.5079524583208,31.5404524382925,235.35105));
#237905=CARTESIAN_POINT('',(-44.5079524583208,29.5404524382925,-43.9162000000005));
#237906=CARTESIAN_POINT('',(-44.5079524583208,29.5404524382925,-44.0749499999996));
#237907=CARTESIAN_POINT('',(-44.5079524583208,29.5404524382925,235.35105));
#237908=CARTESIAN_POINT('Ctrl Pts',(-44.5079524583208,29.5404524382925,
-44.7749499999996));
#237909=CARTESIAN_POINT('Ctrl Pts',(-44.4269158891708,29.5404524382925,
-44.7702228667993));
#237910=CARTESIAN_POINT('Ctrl Pts',(-44.3457885731801,29.5453774932786,
-44.7654904400331));
#237911=CARTESIAN_POINT('Ctrl Pts',(-44.0123133744175,29.5861855354304,
-44.7460377201053));
#237912=CARTESIAN_POINT('Ctrl Pts',(-43.7677747684345,29.6650857813368,
-44.7317729680897));
#237913=CARTESIAN_POINT('Ctrl Pts',(-43.3123227136843,29.9154252946429,
-44.7052049315628));
#237914=CARTESIAN_POINT('Ctrl Pts',(-43.1076607188679,30.0880337573836,
-44.6908149936175));
#237915=CARTESIAN_POINT('Ctrl Pts',(-42.7799440122894,30.5001310234453,
-44.6604381987701));
#237916=CARTESIAN_POINT('Ctrl Pts',(-42.658943374774,30.7345646059895,-44.6450658629603));
#237917=CARTESIAN_POINT('Ctrl Pts',(-42.5161481504766,31.2291048648655,
-44.6159177439879));
#237918=CARTESIAN_POINT('Ctrl Pts',(-42.4927668196029,31.4836645710956,
-44.6032617323741));
#237919=CARTESIAN_POINT('Ctrl Pts',(-42.5434285080603,31.9997976447559,
-44.5757100125053));
#237920=CARTESIAN_POINT('Ctrl Pts',(-42.6215891793797,32.2559573025136,
-44.5604896146143));
#237921=CARTESIAN_POINT('Ctrl Pts',(-42.8699633092896,32.7167686211005,
-44.5299660345109));
#237922=CARTESIAN_POINT('Ctrl Pts',(-43.035439322463,32.9182984430415,-44.5149587373105));
#237923=CARTESIAN_POINT('Ctrl Pts',(-43.4328587864362,33.2463868218929,
-44.4867929188162));
#237924=CARTESIAN_POINT('Ctrl Pts',(-43.6606686457498,33.3702482293867,
-44.4743748890671));
#237925=CARTESIAN_POINT('Ctrl Pts',(-44.1587978262492,33.5275409238952,
-44.4453173535379));
#237926=CARTESIAN_POINT('Ctrl Pts',(-44.4252408746356,33.5562821846605,
-44.429774842382));
#237927=CARTESIAN_POINT('Ctrl Pts',(-44.9437910037961,33.5090174220985,
-44.3995260848475));
#237928=CARTESIAN_POINT('Ctrl Pts',(-45.1913516937128,33.4373475623424,
-44.3850850446023));
#237929=CARTESIAN_POINT('Ctrl Pts',(-45.6552987634885,33.2000269091421,
-44.3580214655319));
#237930=CARTESIAN_POINT('Ctrl Pts',(-45.8654097666201,33.0330879397658,
-44.3440960105084));
#237931=CARTESIAN_POINT('Ctrl Pts',(-46.2057253231842,32.6295959221004,
-44.3137864704197));
#237932=CARTESIAN_POINT('Ctrl Pts',(-46.3336705246337,32.3980205000053,
-44.2983559738024));
#237933=CARTESIAN_POINT('Ctrl Pts',(-46.4903121008032,31.9070661004001,
-44.2689851538715));
#237934=CARTESIAN_POINT('Ctrl Pts',(-46.520751545409,31.6533923832289,-44.2560288236222));
#237935=CARTESIAN_POINT('Ctrl Pts',(-46.4845522240017,31.1362381260368,
-44.2288473344909));
#237936=CARTESIAN_POINT('Ctrl Pts',(-46.4135981899322,30.8780272756441,
-44.2137335077321));
#237937=CARTESIAN_POINT('Ctrl Pts',(-46.1779317184528,30.4098513143393,
-44.1832085195513));
#237938=CARTESIAN_POINT('Ctrl Pts',(-46.0176196702392,30.2032850039629,
-44.1680974039245));
#237939=CARTESIAN_POINT('Ctrl Pts',(-45.6296444473373,29.8649864588488,
-44.1396912437655));
#237940=CARTESIAN_POINT('Ctrl Pts',(-45.4065243784234,29.7354739554711,
-44.1273666953388));
#237941=CARTESIAN_POINT('Ctrl Pts',(-44.9534608432788,29.5778783047637,
-44.1009379891221));
#237942=CARTESIAN_POINT('Ctrl Pts',(-44.7313283970238,29.5404524382925,
-44.0879802630906));
#237943=CARTESIAN_POINT('Ctrl Pts',(-44.5079524583208,29.5404524382925,
-44.0749499999997));
#237944=CARTESIAN_POINT('Ctrl Pts',(-44.5079524583208,29.5404524382925,
-43.9162000000005));
#237945=CARTESIAN_POINT('Ctrl Pts',(-44.6523156556797,29.5404524382925,
-43.9246211865131));
#237946=CARTESIAN_POINT('Ctrl Pts',(-44.7966026468966,29.5560832331624,
-43.9330379276674));
#237947=CARTESIAN_POINT('Ctrl Pts',(-45.1946723394097,29.6437828286242,
-43.9562586597307));
#237948=CARTESIAN_POINT('Ctrl Pts',(-45.4374028973042,29.7501928106054,
-43.9695350359824));
#237949=CARTESIAN_POINT('Ctrl Pts',(-45.8628387194137,30.0471402137679,
-43.9969448138196));
#237950=CARTESIAN_POINT('Ctrl Pts',(-46.042839741025,30.2328663342062,-44.0115773833593));
#237951=CARTESIAN_POINT('Ctrl Pts',(-46.3284304855397,30.6705111297737,
-44.042016118204));
#237952=CARTESIAN_POINT('Ctrl Pts',(-46.4279869739964,30.9204274153687,
-44.057545157159));
#237953=CARTESIAN_POINT('Ctrl Pts',(-46.5213614199234,31.4337420706773,
-44.0862002845104));
#237954=CARTESIAN_POINT('Ctrl Pts',(-46.5185326280804,31.6913556855195,
-44.0985147643764));
#237955=CARTESIAN_POINT('Ctrl Pts',(-46.4153325676931,32.1955284989266,
-44.1269946432222));
#237956=CARTESIAN_POINT('Ctrl Pts',(-46.3144431403658,32.4369980572508,
-44.1421358465379));
#237957=CARTESIAN_POINT('Ctrl Pts',(-46.0229009685275,32.8728250015037,
-44.1726563301967));
#237958=CARTESIAN_POINT('Ctrl Pts',(-45.8331176096775,33.0617240701592,
-44.1877345093751));
#237959=CARTESIAN_POINT('Ctrl Pts',(-45.4008481988035,33.3478966983426,
-44.2147992785349));
#237960=CARTESIAN_POINT('Ctrl Pts',(-45.1650614423334,33.4463305633755,
-44.227868642599));
#237961=CARTESIAN_POINT('Ctrl Pts',(-44.6603833204181,33.551808762868,-44.2573081997106));
#237962=CARTESIAN_POINT('Ctrl Pts',(-44.3955896792146,33.5544440813145,
-44.2727544954474));
#237963=CARTESIAN_POINT('Ctrl Pts',(-43.8773970976013,33.456865381138,-44.3029823960414));
#237964=CARTESIAN_POINT('Ctrl Pts',(-43.6293512739145,33.3565598115926,
-44.3167461524701));
#237965=CARTESIAN_POINT('Ctrl Pts',(-43.1945769409543,33.0702865657418,
-44.3438890648757));
#237966=CARTESIAN_POINT('Ctrl Pts',(-43.0100265915509,32.890091094939,-44.3583749249628));
#237967=CARTESIAN_POINT('Ctrl Pts',(-42.7130809076758,32.4618456208354,
-44.3886700092209));
#237968=CARTESIAN_POINT('Ctrl Pts',(-42.6067155290989,32.2156174147622,
-44.4042113258553));
#237969=CARTESIAN_POINT('Ctrl Pts',(-42.498271475132,31.7048127455013,-44.4331791835933));
#237970=CARTESIAN_POINT('Ctrl Pts',(-42.4937772998067,31.4459655722021,
-44.4455598594139));
#237971=CARTESIAN_POINT('Ctrl Pts',(-42.583197121164,30.9386415599925,-44.4737970073508));
#237972=CARTESIAN_POINT('Ctrl Pts',(-42.6770358458382,30.6951248891461,
-44.4888359815071));
#237973=CARTESIAN_POINT('Ctrl Pts',(-42.955689210157,30.2517373390094,-44.5193624894247));
#237974=CARTESIAN_POINT('Ctrl Pts',(-43.1400483434228,30.0574871098765,
-44.5345527927437));
#237975=CARTESIAN_POINT('Ctrl Pts',(-43.5641032727125,29.7590741737154,
-44.5619963305543));
#237976=CARTESIAN_POINT('Ctrl Pts',(-43.7970521365803,29.6539720334572,
-44.5747308145655));
#237977=CARTESIAN_POINT('Ctrl Pts',(-44.1959803359963,29.5587218245104,
-44.5980016261982));
#237978=CARTESIAN_POINT('Ctrl Pts',(-44.3518805815372,29.5404524382925,
-44.6070958071881));
#237979=CARTESIAN_POINT('Ctrl Pts',(-44.5079524583208,29.5404524382925,
-44.6162000000005));
#237980=CARTESIAN_POINT('Origin',(-44.5079524583208,31.5404524382925,235.35105));
#237981=CARTESIAN_POINT('',(-44.5079524583208,29.5404524382925,-43.2162000000004));
#237982=CARTESIAN_POINT('',(-44.5079524583208,29.5404524382925,-43.3749499999997));
#237983=CARTESIAN_POINT('',(-44.5079524583208,29.5404524382925,235.35105));
#237984=CARTESIAN_POINT('Ctrl Pts',(-44.5079524583208,29.5404524382925,
-44.0749499999997));
#237985=CARTESIAN_POINT('Ctrl Pts',(-44.4659149033209,29.5404524382925,
-44.0724978092913));
#237986=CARTESIAN_POINT('Ctrl Pts',(-44.4238333085281,29.5417777833755,
-44.070043049595));
#237987=CARTESIAN_POINT('Ctrl Pts',(-44.1262478307761,29.5605903219429,
-44.0526838967262));
#237988=CARTESIAN_POINT('Ctrl Pts',(-43.8761505507025,29.6256632463176,
-44.038094888722));
#237989=CARTESIAN_POINT('Ctrl Pts',(-43.4076485412583,29.8497097904113,
-44.0107656048379));
#237990=CARTESIAN_POINT('Ctrl Pts',(-43.1949244037257,30.009023590732,-43.997351631762));
#237991=CARTESIAN_POINT('Ctrl Pts',(-42.8436338287753,30.4006630372635,
-43.9673207569199));
#237992=CARTESIAN_POINT('Ctrl Pts',(-42.708417399813,30.6289986251821,-43.9518418532579));
#237993=CARTESIAN_POINT('Ctrl Pts',(-42.5371390233473,31.1160320104332,
-43.9222422090375));
#237994=CARTESIAN_POINT('Ctrl Pts',(-42.4992879688712,31.368867795911,-43.9088708527294));
#237995=CARTESIAN_POINT('Ctrl Pts',(-42.5204248231154,31.8869335563989,
-43.8820826380982));
#237996=CARTESIAN_POINT('Ctrl Pts',(-42.5838170893789,32.1470584640277,
-43.8670926682727));
#237997=CARTESIAN_POINT('Ctrl Pts',(-42.8060179358639,32.6225280247556,
-43.8365919683484));
#237998=CARTESIAN_POINT('Ctrl Pts',(-42.9607933466564,32.8342009250777,
-43.8213843625103));
#237999=CARTESIAN_POINT('Ctrl Pts',(-43.3388799803566,33.1830472982667,
-43.7927337627908));
#238000=CARTESIAN_POINT('Ctrl Pts',(-43.5572521065149,33.318375970392,-43.7804075205225));
#238001=CARTESIAN_POINT('Ctrl Pts',(-44.0445925985247,33.504264475221,-43.7519793251552));
#238002=CARTESIAN_POINT('Ctrl Pts',(-44.3105236922181,33.5484994715933,
-43.736466678023));
#238003=CARTESIAN_POINT('Ctrl Pts',(-44.8338347314534,33.5303552378897,
-43.7059402007342));
#238004=CARTESIAN_POINT('Ctrl Pts',(-45.0863523706445,33.4721359389528,
-43.6912100051146));
#238005=CARTESIAN_POINT('Ctrl Pts',(-45.5594039056671,33.2616584557708,
-43.6636153322382));
#238006=CARTESIAN_POINT('Ctrl Pts',(-45.7747585466089,33.1099506004804,
-43.6506229637377));
#238007=CARTESIAN_POINT('Ctrl Pts',(-46.1369220480862,32.7303908260498,
-43.6208852045413));
#238008=CARTESIAN_POINT('Ctrl Pts',(-46.2794099100104,32.5055569114119,
-43.6053711154687));
#238009=CARTESIAN_POINT('Ctrl Pts',(-46.4654971743976,32.0226338617521,
-43.5755471918944));
#238010=CARTESIAN_POINT('Ctrl Pts',(-46.5108100821409,31.7705479030538,
-43.5616573442314));
#238011=CARTESIAN_POINT('Ctrl Pts',(-46.5046812629471,31.251721794336,-43.5352684525709));
#238012=CARTESIAN_POINT('Ctrl Pts',(-46.4488675860034,30.9899180640861,
-43.5204147139232));
#238013=CARTESIAN_POINT('Ctrl Pts',(-46.2402959941818,30.5075754677912,
-43.4899643208948));
#238014=CARTESIAN_POINT('Ctrl Pts',(-46.0911896472629,30.2909636669984,
-43.4746725586453));
#238015=CARTESIAN_POINT('Ctrl Pts',(-45.7230171197802,29.9316987040934,
-43.4457847924941));
#238016=CARTESIAN_POINT('Ctrl Pts',(-45.5092312008947,29.7906239252334,
-43.4333579266496));
#238017=CARTESIAN_POINT('Ctrl Pts',(-45.0316282768101,29.5923624973419,
-43.405497756078));
#238018=CARTESIAN_POINT('Ctrl Pts',(-44.7710344880029,29.5404524382925,
-43.3902964517311));
#238019=CARTESIAN_POINT('Ctrl Pts',(-44.5079524583208,29.5404524382925,
-43.3749499999997));
#238020=CARTESIAN_POINT('Ctrl Pts',(-44.5079524583208,29.5404524382925,
-43.2162000000004));
#238021=CARTESIAN_POINT('Ctrl Pts',(-44.6923124819427,29.5404524382925,
-43.2269543347117));
#238022=CARTESIAN_POINT('Ctrl Pts',(-44.8761848820962,29.5659455735621,
-43.2376802247207));
#238023=CARTESIAN_POINT('Ctrl Pts',(-45.3029944073813,29.6871421391465,
-43.2625774470291));
#238024=CARTESIAN_POINT('Ctrl Pts',(-45.5356162731434,29.8053016743605,
-43.2751835905435));
#238025=CARTESIAN_POINT('Ctrl Pts',(-45.9423907698327,30.1231353045488,
-43.3031042132423));
#238026=CARTESIAN_POINT('Ctrl Pts',(-46.1128549381114,30.3195270278415,
-43.3179974310691));
#238027=CARTESIAN_POINT('Ctrl Pts',(-46.3749950428255,30.7749984950565,
-43.3486527593662));
#238028=CARTESIAN_POINT('Ctrl Pts',(-46.4606399108811,31.0317137236471,
-43.3641195127385));
#238029=CARTESIAN_POINT('Ctrl Pts',(-46.5239611741609,31.549537721084,-43.3921258925448));
#238030=CARTESIAN_POINT('Ctrl Pts',(-46.5065638074057,31.804915466823,-43.404600684881));
#238031=CARTESIAN_POINT('Ctrl Pts',(-46.3754196378857,32.3023837632647,
-43.4335569004592));
#238032=CARTESIAN_POINT('Ctrl Pts',(-46.2603040023265,32.5390640797171,
-43.4488710912159));
#238033=CARTESIAN_POINT('Ctrl Pts',(-45.9431660366353,32.9583356198413,
-43.4793017704969));
#238034=CARTESIAN_POINT('Ctrl Pts',(-45.7428384517924,33.1358646692272,
-43.4941130972777));
#238035=CARTESIAN_POINT('Ctrl Pts',(-45.2942118987344,33.3968653020267,
-43.5203833071489));
#238036=CARTESIAN_POINT('Ctrl Pts',(-45.0523152307769,33.4816508919774,
-43.5344455049398));
#238037=CARTESIAN_POINT('Ctrl Pts',(-44.5399322360448,33.5575267826389,
-43.5643345129657));
#238038=CARTESIAN_POINT('Ctrl Pts',(-44.2738433379105,33.5441523280242,
-43.5798563653568));
#238039=CARTESIAN_POINT('Ctrl Pts',(-43.7655792376963,33.4157336424454,
-43.6095051045359));
#238040=CARTESIAN_POINT('Ctrl Pts',(-43.5280652801099,33.303291173352,-43.6223913602693));
#238041=CARTESIAN_POINT('Ctrl Pts',(-43.1121019935912,32.9956692908682,
-43.6500641107506));
#238042=CARTESIAN_POINT('Ctrl Pts',(-42.936870233636,32.8044624020852,-43.6648344550947));
#238043=CARTESIAN_POINT('Ctrl Pts',(-42.6630627278422,32.3576054412223,
-43.6953948936784));
#238044=CARTESIAN_POINT('Ctrl Pts',(-42.570520521925,32.1041414138609,-43.7108985747384));
#238045=CARTESIAN_POINT('Ctrl Pts',(-42.4924111348435,31.5884547885678,
-43.7392282987389));
#238046=CARTESIAN_POINT('Ctrl Pts',(-42.5026411845677,31.3320188059258,
-43.7515747690521));
#238047=CARTESIAN_POINT('Ctrl Pts',(-42.619956356439,30.8311774693128,-43.7802980386102));
#238048=CARTESIAN_POINT('Ctrl Pts',(-42.7280476853849,30.5920206489724,
-43.7955324621489));
#238049=CARTESIAN_POINT('Ctrl Pts',(-43.0326172146599,30.164354510323,-43.8260206416101));
#238050=CARTESIAN_POINT('Ctrl Pts',(-43.227806385461,29.981114633024,-43.8409705984343));
#238051=CARTESIAN_POINT('Ctrl Pts',(-43.6683870931636,29.7075990362631,
-43.8676383706248));
#238052=CARTESIAN_POINT('Ctrl Pts',(-43.9071981376441,29.616033318842,-43.8811559979609));
#238053=CARTESIAN_POINT('Ctrl Pts',(-44.2729995134149,29.5507984087063,
-43.9024944115476));
#238054=CARTESIAN_POINT('Ctrl Pts',(-44.3905012068673,29.5404524382925,
-43.909348676999));
#238055=CARTESIAN_POINT('Ctrl Pts',(-44.5079524583208,29.5404524382925,
-43.9162000000005));
#238056=CARTESIAN_POINT('Origin',(-44.5079524583208,31.5404524382925,235.35105));
#238057=CARTESIAN_POINT('',(-44.5079524583208,29.5404524382925,-42.5162000000004));
#238058=CARTESIAN_POINT('',(-44.5079524583208,29.5404524382925,-42.6749499999997));
#238059=CARTESIAN_POINT('',(-44.5079524583208,29.5404524382925,235.35105));
#238060=CARTESIAN_POINT('Ctrl Pts',(-44.5079524583208,29.5404524382925,
-43.3749499999997));
#238061=CARTESIAN_POINT('Ctrl Pts',(-44.5034547997409,29.5404524382925,
-43.3746876365825));
#238062=CARTESIAN_POINT('Ctrl Pts',(-44.4989564139122,29.5404676099871,
-43.3744252307424));
#238063=CARTESIAN_POINT('Ctrl Pts',(-44.2370388629623,29.5422349497112,
-43.359146706937));
#238064=CARTESIAN_POINT('Ctrl Pts',(-43.9823295026895,29.593655263083,-43.3442886609212));
#238065=CARTESIAN_POINT('Ctrl Pts',(-43.5049324886095,29.7908658093173,
-43.3164405017666));
#238066=CARTESIAN_POINT('Ctrl Pts',(-43.2870296568381,29.9353163752196,
-43.3037615870405));
#238067=CARTESIAN_POINT('Ctrl Pts',(-42.9145603165496,30.3031142607244,
-43.2743174297311));
#238068=CARTESIAN_POINT('Ctrl Pts',(-42.7651297928638,30.5243514743431,
-43.2587825450337));
#238069=CARTESIAN_POINT('Ctrl Pts',(-42.564801016483,31.0029469157913,-43.228761866781));
#238070=CARTESIAN_POINT('Ctrl Pts',(-42.5122253282156,31.2543241065678,
-43.2145292989398));
#238071=CARTESIAN_POINT('Ctrl Pts',(-42.5040138827789,31.7738205426458,
-43.1880458003169));
#238072=CARTESIAN_POINT('Ctrl Pts',(-42.5525320299186,32.0371029262524,
-43.1735598993653));
#238073=CARTESIAN_POINT('Ctrl Pts',(-42.7480481725244,32.5258203225073,
-43.143168247181));
#238074=CARTESIAN_POINT('Ctrl Pts',(-42.891628989319,32.746984743603,-43.1278076562781));
#238075=CARTESIAN_POINT('Ctrl Pts',(-43.2503117884441,33.1160757216122,
-43.0987002817799));
#238076=CARTESIAN_POINT('Ctrl Pts',(-43.4598617949897,33.2625829045186,
-43.0860886220281));
#238077=CARTESIAN_POINT('Ctrl Pts',(-43.9333164345857,33.4743987861099,
-43.0584704347183));
#238078=CARTESIAN_POINT('Ctrl Pts',(-44.1945469816096,33.5334637551795,
-43.0432319861418));
#238079=CARTESIAN_POINT('Ctrl Pts',(-44.717759448349,33.5461054116061,-43.0127112589153));
#238080=CARTESIAN_POINT('Ctrl Pts',(-44.9746841494797,33.5023014180199,
-42.9977239846826));
#238081=CARTESIAN_POINT('Ctrl Pts',(-45.4567674143157,33.3197568490683,
-42.9696024609003));
#238082=CARTESIAN_POINT('Ctrl Pts',(-45.6774773406108,33.1831302570668,
-42.9571572330085));
#238083=CARTESIAN_POINT('Ctrl Pts',(-46.0609806578878,32.8282641030214,
-42.9280445385009));
#238084=CARTESIAN_POINT('Ctrl Pts',(-46.2178840852463,32.6111864822102,
-42.9125018290403));
#238085=CARTESIAN_POINT('Ctrl Pts',(-46.4337097693197,32.1376109875537,
-42.8822827560641));
#238086=CARTESIAN_POINT('Ctrl Pts',(-46.4941416980732,31.8872012781276,
-42.8678699232418));
#238087=CARTESIAN_POINT('Ctrl Pts',(-46.5180540212289,31.3662663370907,
-42.8408558117447));
#238088=CARTESIAN_POINT('Ctrl Pts',(-46.4770629652323,31.1005455540052,
-42.8268257751206));
#238089=CARTESIAN_POINT('Ctrl Pts',(-46.2948720769304,30.6047659797364,
-42.7964660080287));
#238090=CARTESIAN_POINT('Ctrl Pts',(-46.1571213548608,30.3790580324543,
-42.7810459310244));
#238091=CARTESIAN_POINT('Ctrl Pts',(-45.8082963202166,29.9999125950756,
-42.7517181419849));
#238092=CARTESIAN_POINT('Ctrl Pts',(-45.6029972554696,29.8478219583038,
-42.7388276131664));
#238093=CARTESIAN_POINT('Ctrl Pts',(-45.1357865257117,29.6231199988592,
-42.7115736539305));
#238094=CARTESIAN_POINT('Ctrl Pts',(-44.8763212518798,29.5568694496022,
-42.6964381796237));
#238095=CARTESIAN_POINT('Ctrl Pts',(-44.5770034733222,29.5413456320306,
-42.6789779758746));
#238096=CARTESIAN_POINT('Ctrl Pts',(-44.5424624403491,29.5404524382925,
-42.6769630822846));
#238097=CARTESIAN_POINT('Ctrl Pts',(-44.5079524583208,29.5404524382925,
-42.6749499999997));
#238098=CARTESIAN_POINT('Ctrl Pts',(-44.5079524583208,29.5404524382925,
-42.5162000000004));
#238099=CARTESIAN_POINT('Ctrl Pts',(-44.7332666959702,29.5404524382925,
-42.52934333053));
#238100=CARTESIAN_POINT('Ctrl Pts',(-44.957288796902,29.5785306087671,-42.5424112864178));
#238101=CARTESIAN_POINT('Ctrl Pts',(-45.4116046387501,29.7380281571039,
-42.568913043859));
#238102=CARTESIAN_POINT('Ctrl Pts',(-45.6342607733475,29.868103521915,-42.5812333548637));
#238103=CARTESIAN_POINT('Ctrl Pts',(-46.0212859603873,30.2074222321539,
-42.6096633424967));
#238104=CARTESIAN_POINT('Ctrl Pts',(-46.1810715288083,30.4144868042626,
-42.6247842737231));
#238105=CARTESIAN_POINT('Ctrl Pts',(-46.4154506575917,30.8833823440739,
-42.6553080661824));
#238106=CARTESIAN_POINT('Ctrl Pts',(-46.4856784980985,31.141787512218,-42.6704105288686));
#238107=CARTESIAN_POINT('Ctrl Pts',(-46.5204267239946,31.6590362307413,
-42.6975544663922));
#238108=CARTESIAN_POINT('Ctrl Pts',(-46.4892761910751,31.9126254579149,
-42.7105462163547));
#238109=CARTESIAN_POINT('Ctrl Pts',(-46.3312342187149,32.4032106010717,
-42.7399392270222));
#238110=CARTESIAN_POINT('Ctrl Pts',(-46.2025900374275,32.6344856994316,
-42.7553749387522));
#238111=CARTESIAN_POINT('Ctrl Pts',(-45.8612144213161,33.0368477454997,
-42.7856583131711));
#238112=CARTESIAN_POINT('Ctrl Pts',(-45.65085238483,33.2030525098178,-42.7995308376202));
#238113=CARTESIAN_POINT('Ctrl Pts',(-45.1864669965252,33.4391089222736,
-42.8266199852712));
#238114=CARTESIAN_POINT('Ctrl Pts',(-44.9386576993136,33.5101553199242,
-42.8410755276084));
#238115=CARTESIAN_POINT('Ctrl Pts',(-44.4198486332464,33.5560631483164,
-42.8713393897956));
#238116=CARTESIAN_POINT('Ctrl Pts',(-44.1534101472401,33.5265964113438,
-42.8868816348126));
#238117=CARTESIAN_POINT('Ctrl Pts',(-43.6557736215184,33.3679547677738,
-42.9159104321463));
#238118=CARTESIAN_POINT('Ctrl Pts',(-43.4284127082079,33.2435566432759,
-42.9283155714807));
#238119=CARTESIAN_POINT('Ctrl Pts',(-43.031883069797,32.9145002366682,-42.9565043396993));
#238120=CARTESIAN_POINT('Ctrl Pts',(-42.8668882421245,32.7124893320118,
-42.9715219057308));
#238121=CARTESIAN_POINT('Ctrl Pts',(-42.6197045856503,32.2509675743979,
-43.0020466537567));
#238122=CARTESIAN_POINT('Ctrl Pts',(-42.5422220334332,31.9946053198465,
-43.0172575079889));
#238123=CARTESIAN_POINT('Ctrl Pts',(-42.492926353371,31.4783695051474,-43.0447745762333));
#238124=CARTESIAN_POINT('Ctrl Pts',(-42.5169722905291,31.2238968880538,
-43.0574548787517));
#238125=CARTESIAN_POINT('Ctrl Pts',(-42.6610668231682,30.7296881573348,
-43.086624146029));
#238126=CARTESIAN_POINT('Ctrl Pts',(-42.7827215470223,30.4955141344456,
-43.102002446884));
#238127=CARTESIAN_POINT('Ctrl Pts',(-43.1115986924766,30.0842462329312,
-43.1323711899042));
#238128=CARTESIAN_POINT('Ctrl Pts',(-43.3167336698099,29.9121869880077,
-43.146712237337));
#238129=CARTESIAN_POINT('Ctrl Pts',(-43.7729361058758,29.6630475933886,
-43.1733240461077));
#238130=CARTESIAN_POINT('Ctrl Pts',(-44.0177595996246,29.5848033418876,
-43.1876054165764));
#238131=CARTESIAN_POINT('Ctrl Pts',(-44.3495422509698,29.5451520527569,
-43.2069594045716));
#238132=CARTESIAN_POINT('Ctrl Pts',(-44.4287923051265,29.5404524382925,
-43.2115823243974));
#238133=CARTESIAN_POINT('Ctrl Pts',(-44.5079524583208,29.5404524382925,
-43.2162000000004));
#238134=CARTESIAN_POINT('Origin',(-44.5079524583208,31.5404524382925,235.35105));
#238135=CARTESIAN_POINT('',(-44.5079524583208,29.5404524382925,-41.8162000000004));
#238136=CARTESIAN_POINT('',(-44.5079524583208,29.5404524382925,-41.9749499999997));
#238137=CARTESIAN_POINT('',(-44.5079524583208,29.5404524382925,235.35105));
#238138=CARTESIAN_POINT('Ctrl Pts',(-44.5079524583208,29.5404524382925,
-42.6749499999997));
#238139=CARTESIAN_POINT('Ctrl Pts',(-44.2841370889279,29.5404524382925,
-42.6618941034518));
#238140=CARTESIAN_POINT('Ctrl Pts',(-44.0616277856587,29.5780252361848,
-42.6489143940944));
#238141=CARTESIAN_POINT('Ctrl Pts',(-43.608121189646,29.7360690715554,-42.6224598426604));
#238142=CARTESIAN_POINT('Ctrl Pts',(-43.3848953730774,29.8658662543444,
-42.6101244952876));
#238143=CARTESIAN_POINT('Ctrl Pts',(-42.9918289387129,30.2092396644597,
-42.581313468677));
#238144=CARTESIAN_POINT('Ctrl Pts',(-42.8284287235735,30.4224474775894,
-42.5657767650923));
#238145=CARTESIAN_POINT('Ctrl Pts',(-42.5990408165836,30.8911903670437,
-42.5354062615487));
#238146=CARTESIAN_POINT('Ctrl Pts',(-42.5316937175442,31.1405451574942,
-42.5208450288135));
#238147=CARTESIAN_POINT('Ctrl Pts',(-42.4941235311099,31.6588290422461,
-42.4935664894262));
#238148=CARTESIAN_POINT('Ctrl Pts',(-42.5272417851303,31.9230050659609,
-42.4800615441608));
#238149=CARTESIAN_POINT('Ctrl Pts',(-42.6937873095637,32.4223833588244,
-42.4499762995813));
#238150=CARTESIAN_POINT('Ctrl Pts',(-42.8251719183327,32.6527680759523,
-42.4345056391277));
#238151=CARTESIAN_POINT('Ctrl Pts',(-43.1633820494583,33.0425645094426,
-42.404949382837));
#238152=CARTESIAN_POINT('Ctrl Pts',(-43.3642611890508,33.2006096207479,
-42.3916653240412));
#238153=CARTESIAN_POINT('Ctrl Pts',(-43.8247840964883,33.4387675987847,
-42.364801487774));
#238154=CARTESIAN_POINT('Ctrl Pts',(-44.082177298587,33.5125042425652,-42.3497868843181));
#238155=CARTESIAN_POINT('Ctrl Pts',(-44.6051606547095,33.5548870328411,
-42.3192795218776));
#238156=CARTESIAN_POINT('Ctrl Pts',(-44.8655627452052,33.5252772867362,
-42.3040893999319));
#238157=CARTESIAN_POINT('Ctrl Pts',(-45.3559248803719,33.3696272638332,
-42.2754849420471));
#238158=CARTESIAN_POINT('Ctrl Pts',(-45.5817988901373,33.2468485025364,
-42.2631667822709));
#238159=CARTESIAN_POINT('Ctrl Pts',(-45.9846177047329,32.9154576062036,
-42.234676645648));
#238160=CARTESIAN_POINT('Ctrl Pts',(-46.1546451592276,32.7064518049151,
-42.2191589254403));
#238161=CARTESIAN_POINT('Ctrl Pts',(-46.3979573784054,32.2431084125083,
-42.1886550687183));
#238162=CARTESIAN_POINT('Ctrl Pts',(-46.4724437982236,31.995044233128,-42.1739508050754));
#238163=CARTESIAN_POINT('Ctrl Pts',(-46.5240393417302,31.4795852093357,
-42.1464058995188));
#238164=CARTESIAN_POINT('Ctrl Pts',(-46.498851379292,31.2169451438094,-42.1333415623));
#238165=CARTESIAN_POINT('Ctrl Pts',(-46.3482309719834,30.7141407460003,
-42.1035477198246));
#238166=CARTESIAN_POINT('Ctrl Pts',(-46.2234947946519,30.4791681395843,
-42.088039200282));
#238167=CARTESIAN_POINT('Ctrl Pts',(-45.8962379917397,30.0785749281764,
-42.0582569828334));
#238168=CARTESIAN_POINT('Ctrl Pts',(-45.6997631742947,29.9144391357236,
-42.0444722917645));
#238169=CARTESIAN_POINT('Ctrl Pts',(-45.2460901769229,29.6628345948263,
-42.0180080335845));
#238170=CARTESIAN_POINT('Ctrl Pts',(-44.9910006366204,29.5816493308882,
-42.0031278104002));
#238171=CARTESIAN_POINT('Ctrl Pts',(-44.654499455299,29.5444745450108,-41.9834985748232));
#238172=CARTESIAN_POINT('Ctrl Pts',(-44.5811846202044,29.5404524382925,
-41.9792218761095));
#238173=CARTESIAN_POINT('Ctrl Pts',(-44.5079524583208,29.5404524382925,
-41.9749499999997));
#238174=CARTESIAN_POINT('Ctrl Pts',(-44.5079524583208,29.5404524382925,
-41.8162000000004));
#238175=CARTESIAN_POINT('Ctrl Pts',(-44.7729039134369,29.5404524382925,
-41.8316555015489));
#238176=CARTESIAN_POINT('Ctrl Pts',(-45.0352945948459,29.5931024916833,
-41.8469616246312));
#238177=CARTESIAN_POINT('Ctrl Pts',(-45.5139921448838,29.7933651489333,
-41.8748856483834));
#238178=CARTESIAN_POINT('Ctrl Pts',(-45.7273470393406,29.9349870020374,
-41.8873272005398));
#238179=CARTESIAN_POINT('Ctrl Pts',(-46.0945687985833,30.2952428951762,
-41.9162372959115));
#238180=CARTESIAN_POINT('Ctrl Pts',(-46.2431257236584,30.5123186077162,
-41.9315364693197));
#238181=CARTESIAN_POINT('Ctrl Pts',(-46.4503845331156,30.995297046345,-41.9619806944399));
#238182=CARTESIAN_POINT('Ctrl Pts',(-46.5054721111779,31.257249210245,-41.9768207537966));
#238183=CARTESIAN_POINT('Ctrl Pts',(-46.5101666263359,31.7761404805287,
-42.0031711034309));
#238184=CARTESIAN_POINT('Ctrl Pts',(-46.4641359997729,32.0281591361894,
-42.0171160194564));
#238185=CARTESIAN_POINT('Ctrl Pts',(-46.2766215298312,32.5106781500049,
-42.0469611587164));
#238186=CARTESIAN_POINT('Ctrl Pts',(-46.1334378488472,32.7351629111486,
-42.0624779039232));
#238187=CARTESIAN_POINT('Ctrl Pts',(-45.7702384727176,33.1135542276122,
-42.0921868477969));
#238188=CARTESIAN_POINT('Ctrl Pts',(-45.5546304034682,33.2645347610461,
-42.1051437865329));
#238189=CARTESIAN_POINT('Ctrl Pts',(-45.0811435304602,33.4736969370716,
-42.1327638541249));
#238190=CARTESIAN_POINT('Ctrl Pts',(-44.8284007905841,33.531246333344,-42.1475071806176));
#238191=CARTESIAN_POINT('Ctrl Pts',(-44.3048968527452,33.5479484634135,
-42.1780449103248));
#238192=CARTESIAN_POINT('Ctrl Pts',(-44.0390134197966,33.5029502399948,
-42.1935547772468));
#238193=CARTESIAN_POINT('Ctrl Pts',(-43.5522189874468,33.3156629807161,
-42.2219511191338));
#238194=CARTESIAN_POINT('Ctrl Pts',(-43.3343039869024,33.1797674883365,
-42.2342829191908));
#238195=CARTESIAN_POINT('Ctrl Pts',(-42.9571892165043,32.8298928830521,
-42.2629571172791));
#238196=CARTESIAN_POINT('Ctrl Pts',(-42.8029645057999,32.6177277261712,
-42.2781735289213));
#238197=CARTESIAN_POINT('Ctrl Pts',(-42.5820944686412,32.141564881733,-42.3086704369831));
#238198=CARTESIAN_POINT('Ctrl Pts',(-42.5194454807074,31.8812647971072,
-42.323647577475));
#238199=CARTESIAN_POINT('Ctrl Pts',(-42.4997839987105,31.3631178499939,
-42.3503968618138));
#238200=CARTESIAN_POINT('Ctrl Pts',(-42.5383649321693,31.1103595086761,
-42.3638145289975));
#238201=CARTESIAN_POINT('Ctrl Pts',(-42.7110890663376,30.6237209358429,
-42.3934363959587));
#238202=CARTESIAN_POINT('Ctrl Pts',(-42.8470193569132,30.3957173869416,
-42.4089193465882));
#238203=CARTESIAN_POINT('Ctrl Pts',(-43.1993815561311,30.0052535364079,
-42.4389220882051));
#238204=CARTESIAN_POINT('Ctrl Pts',(-43.412362825029,29.8466870834928,-42.4522906047249));
#238205=CARTESIAN_POINT('Ctrl Pts',(-43.8813116004633,29.6239590185105,
-42.4796459499587));
#238206=CARTESIAN_POINT('Ctrl Pts',(-44.1316518199665,29.559547318394,-42.4942491294297));
#238207=CARTESIAN_POINT('Ctrl Pts',(-44.4275126620251,29.5416644091701,
-42.5115076785499));
#238208=CARTESIAN_POINT('Ctrl Pts',(-44.4677531256547,29.5404524382925,
-42.5138550389283));
#238209=CARTESIAN_POINT('Ctrl Pts',(-44.5079524583208,29.5404524382925,
-42.5162000000005));
#238210=CARTESIAN_POINT('Origin',(-44.5079524583208,31.5404524382925,235.35105));
#238211=CARTESIAN_POINT('',(-44.5079524583208,29.5404524382925,-41.1162000000004));
#238212=CARTESIAN_POINT('',(-44.5079524583208,29.5404524382925,-41.2749499999996));
#238213=CARTESIAN_POINT('',(-44.5079524583208,29.5404524382925,235.35105));
#238214=CARTESIAN_POINT('Ctrl Pts',(-44.5079524583208,29.5404524382925,
-41.9749499999997));
#238215=CARTESIAN_POINT('Ctrl Pts',(-44.3218286908714,29.5404524382925,
-41.9640927802318));
#238216=CARTESIAN_POINT('Ctrl Pts',(-44.1362389523276,29.5664357012366,
-41.95326671215));
#238217=CARTESIAN_POINT('Ctrl Pts',(-43.7124429497979,29.6879690440001,
-41.9285452786692));
#238218=CARTESIAN_POINT('Ctrl Pts',(-43.4838809667533,29.8038473029044,
-41.9161446577051));
#238219=CARTESIAN_POINT('Ctrl Pts',(-43.0715512709672,30.123288631754,-41.8879807904063));
#238220=CARTESIAN_POINT('Ctrl Pts',(-42.8950699812305,30.3279432472202,
-41.8724946471893));
#238221=CARTESIAN_POINT('Ctrl Pts',(-42.6381064955435,30.7855503339349,
-41.8418824160708));
#238222=CARTESIAN_POINT('Ctrl Pts',(-42.5565808648473,31.0321393902305,
-41.8270473625978));
#238223=CARTESIAN_POINT('Ctrl Pts',(-42.4912079870856,31.5447228561652,
-41.7992458859848));
#238224=CARTESIAN_POINT('Ctrl Pts',(-42.5087479068552,31.805916250814,-41.7865160591014));
#238225=CARTESIAN_POINT('Ctrl Pts',(-42.6438718891428,32.3118355648619,
-41.7570168358879));
#238226=CARTESIAN_POINT('Ctrl Pts',(-42.7619824534228,32.5510986273815,
-41.7414848174939));
#238227=CARTESIAN_POINT('Ctrl Pts',(-43.078308585955,32.9620016550282,-41.7115005784364));
#238228=CARTESIAN_POINT('Ctrl Pts',(-43.2705076063607,33.1321374223604,
-41.6972998297061));
#238229=CARTESIAN_POINT('Ctrl Pts',(-43.7175229558531,33.3966417541728,
-41.6708996128849));
#238230=CARTESIAN_POINT('Ctrl Pts',(-43.9702286576964,33.484977612375,-41.6563172217035));
#238231=CARTESIAN_POINT('Ctrl Pts',(-44.4914644076179,33.5573495307964,
-41.6259118029579));
#238232=CARTESIAN_POINT('Ctrl Pts',(-44.7545856011578,33.5422834627067,
-41.610563066668));
#238233=CARTESIAN_POINT('Ctrl Pts',(-45.2528831641334,33.4137804886457,
-41.5814957088276));
#238234=CARTESIAN_POINT('Ctrl Pts',(-45.484057791781,33.304390870872,-41.568924498218));
#238235=CARTESIAN_POINT('Ctrl Pts',(-45.9027600729807,32.9981455705253,
-41.5412414027726));
#238236=CARTESIAN_POINT('Ctrl Pts',(-46.0835487375013,32.8005384566929,
-41.5259856545255));
#238237=CARTESIAN_POINT('Ctrl Pts',(-46.3538105203188,32.3524911214934,
-41.4954684973543));
#238238=CARTESIAN_POINT('Ctrl Pts',(-46.4430967263761,32.1077647451806,
-41.4805011929106));
#238239=CARTESIAN_POINT('Ctrl Pts',(-46.5236276705724,31.5984606951186,
-41.4524232760445));
#238240=CARTESIAN_POINT('Ctrl Pts',(-46.5143530940854,31.3387749910143,
-41.4399483139675));
#238241=CARTESIAN_POINT('Ctrl Pts',(-46.3961025789716,30.8296979833545,
-41.4107817127116));
#238242=CARTESIAN_POINT('Ctrl Pts',(-46.2853724928991,30.5859662992026,
-41.3952392117738));
#238243=CARTESIAN_POINT('Ctrl Pts',(-45.9811932080273,30.1639937114167,
-41.3650500420895));
#238244=CARTESIAN_POINT('Ctrl Pts',(-45.7937701872473,29.9874575277945,
-41.3506652561674));
#238245=CARTESIAN_POINT('Ctrl Pts',(-45.3529256117621,29.7082055742254,
-41.323699997708));
#238246=CARTESIAN_POINT('Ctrl Pts',(-45.1013335290938,29.6119614386068,
-41.3095638957945));
#238247=CARTESIAN_POINT('Ctrl Pts',(-44.7288150439468,29.5495931329844,
-41.2878336508276));
#238248=CARTESIAN_POINT('Ctrl Pts',(-44.6183508181325,29.5404524382925,
-41.281389904322));
#238249=CARTESIAN_POINT('Ctrl Pts',(-44.5079524583208,29.5404524382925,
-41.2749499999996));
#238250=CARTESIAN_POINT('Ctrl Pts',(-44.5079524583208,29.5404524382925,
-41.1162000000005));
#238251=CARTESIAN_POINT('Ctrl Pts',(-44.5442641855471,29.5404524382925,
-41.1183181840887));
#238252=CARTESIAN_POINT('Ctrl Pts',(-44.5806096277852,29.5414413320196,
-41.120438334886));
#238253=CARTESIAN_POINT('Ctrl Pts',(-44.8816866451562,29.5578738957329,
-41.1380011608993));
#238254=CARTESIAN_POINT('Ctrl Pts',(-45.1409681939803,29.6248249502642,
-41.1531259179141));
#238255=CARTESIAN_POINT('Ctrl Pts',(-45.6075611689831,29.8507843113607,
-41.1803438414559));
#238256=CARTESIAN_POINT('Ctrl Pts',(-45.8124464798734,30.0034257864677,
-41.1932666682341));
#238257=CARTESIAN_POINT('Ctrl Pts',(-46.1602937634056,30.3835599514533,
-41.222615888221));
#238258=CARTESIAN_POINT('Ctrl Pts',(-46.2974616923732,30.6097080927158,
-41.2380412048781));
#238259=CARTESIAN_POINT('Ctrl Pts',(-46.4782029531163,31.1058311080966,
-41.2683760411751));
#238260=CARTESIAN_POINT('Ctrl Pts',(-46.5184608384878,31.3714076229008,
-41.2823536744827));
#238261=CARTESIAN_POINT('Ctrl Pts',(-46.4932878027219,31.8921020041553,
-41.3093924041292));
#238262=CARTESIAN_POINT('Ctrl Pts',(-46.4322193782992,32.1424225938883,
-41.3238192992464));
#238263=CARTESIAN_POINT('Ctrl Pts',(-46.2151423082367,32.6155695235688,
-41.3540532206713));
#238264=CARTESIAN_POINT('Ctrl Pts',(-46.0576377189352,32.8322991372114,
-41.3695958833439));
#238265=CARTESIAN_POINT('Ctrl Pts',(-45.6732486620862,33.1861119639656,
-41.3986811997775));
#238266=CARTESIAN_POINT('Ctrl Pts',(-45.4523092165156,33.3221079656183,
-41.4111125224385));
#238267=CARTESIAN_POINT('Ctrl Pts',(-44.969848357842,33.5034537564664,-41.4392560725276));
#238268=CARTESIAN_POINT('Ctrl Pts',(-44.7127523988259,33.546630964103,-41.4542533368035));
#238269=CARTESIAN_POINT('Ctrl Pts',(-44.1895139304819,33.5326653521654,
-41.4847755807901));
#238270=CARTESIAN_POINT('Ctrl Pts',(-43.9284362195246,33.4729416759115,
-41.5000051139293));
#238271=CARTESIAN_POINT('Ctrl Pts',(-43.4555470252595,33.2599451113419,
-41.5275903169281));
#238272=CARTESIAN_POINT('Ctrl Pts',(-43.2463873872433,33.1129308446866,
-41.5402236168403));
#238273=CARTESIAN_POINT('Ctrl Pts',(-42.8885957004252,32.7429245610463,
-41.5693512401087));
#238274=CARTESIAN_POINT('Ctrl Pts',(-42.7455383109935,32.5213415806022,
-41.5847177092236));
#238275=CARTESIAN_POINT('Ctrl Pts',(-42.5512562589388,32.0320557203347,
-41.6151020848497));
#238276=CARTESIAN_POINT('Ctrl Pts',(-42.5034158782804,31.7686412814615,
-41.6295400052042));
#238277=CARTESIAN_POINT('Ctrl Pts',(-42.5129743893263,31.2490902760617,
-41.656065549982));
#238278=CARTESIAN_POINT('Ctrl Pts',(-42.5662271284927,30.9977868310396,
-41.6703141396422));
#238279=CARTESIAN_POINT('Ctrl Pts',(-42.7678951447684,30.5196043976839,
-41.7003530146546));
#238280=CARTESIAN_POINT('Ctrl Pts',(-42.9179735214712,30.2987157867033,
-41.7158891843053));
#238281=CARTESIAN_POINT('Ctrl Pts',(-43.2914015115809,29.9320275058476,
-41.7453052470623));
#238282=CARTESIAN_POINT('Ctrl Pts',(-43.5095446989283,29.7882544431415,
-41.757959547369));
#238283=CARTESIAN_POINT('Ctrl Pts',(-43.9873475189462,29.592298804994,-41.7858313785369));
#238284=CARTESIAN_POINT('Ctrl Pts',(-44.2422550479135,29.5415262495077,
-41.8007009843933));
#238285=CARTESIAN_POINT('Ctrl Pts',(-44.5024795660782,29.5404580538342,
-41.815880747953));
#238286=CARTESIAN_POINT('Ctrl Pts',(-44.5052161487644,29.5404524382925,
-41.816040381943));
#238287=CARTESIAN_POINT('Ctrl Pts',(-44.5079524583208,29.5404524382925,
-41.8162000000004));
#238288=CARTESIAN_POINT('Origin',(-44.5079524583208,31.5404524382925,235.35105));
#238289=CARTESIAN_POINT('',(-44.5079524583208,29.5404524382925,-40.4162000000004));
#238290=CARTESIAN_POINT('',(-44.5079524583208,29.5404524382925,-40.5749499999997));
#238291=CARTESIAN_POINT('',(-44.5079524583208,29.5404524382925,235.35105));
#238292=CARTESIAN_POINT('Ctrl Pts',(-44.5079524583208,29.5404524382925,
-41.2749499999996));
#238293=CARTESIAN_POINT('Ctrl Pts',(-44.3578015660496,29.5404524382925,
-41.2661911979505));
#238294=CARTESIAN_POINT('Ctrl Pts',(-44.2077725143422,29.557361800295,-41.2574395032674));
#238295=CARTESIAN_POINT('Ctrl Pts',(-43.8138468828723,29.6477343665768,
-41.2344605080985));
#238296=CARTESIAN_POINT('Ctrl Pts',(-43.5800166448313,29.7507411266094,
-41.2216314406855));
#238297=CARTESIAN_POINT('Ctrl Pts',(-43.1533656622638,30.0453145822135,
-41.1943061481038));
#238298=CARTESIAN_POINT('Ctrl Pts',(-42.9672845218358,30.2378997606675,
-41.1791497348536));
#238299=CARTESIAN_POINT('Ctrl Pts',(-42.684558257388,30.6789517759641,-41.1486224209118));
#238300=CARTESIAN_POINT('Ctrl Pts',(-42.5884992636513,30.9218467048739,
-41.1335500981595));
#238301=CARTESIAN_POINT('Ctrl Pts',(-42.4947427452761,31.4281892360414,
-41.1052360458316));
#238302=CARTESIAN_POINT('Ctrl Pts',(-42.4969211982232,31.6866403428544,
-41.092886602807));
#238303=CARTESIAN_POINT('Ctrl Pts',(-42.6006050062832,32.1982560191603,
-41.0640166150004));
#238304=CARTESIAN_POINT('Ctrl Pts',(-42.7048326024362,32.4456688198682,
-41.0484778068256));
#238305=CARTESIAN_POINT('Ctrl Pts',(-42.9982222886613,32.8769152557054,
-41.018134836135));
#238306=CARTESIAN_POINT('Ctrl Pts',(-43.1813530602796,33.0588701330176,
-41.0036014984407));
#238307=CARTESIAN_POINT('Ctrl Pts',(-43.6131789265666,33.348530028927,-40.9763734956889));
#238308=CARTESIAN_POINT('Ctrl Pts',(-43.8595281088582,33.4507810501543,
-40.962774753719));
#238309=CARTESIAN_POINT('Ctrl Pts',(-44.3761941666342,33.5533008432308,
-40.9326359003487));
#238310=CARTESIAN_POINT('Ctrl Pts',(-44.6412566326515,33.5531990720144,
-40.9171739231643));
#238311=CARTESIAN_POINT('Ctrl Pts',(-45.1471919732393,33.4524045635475,
-40.8876610282965));
#238312=CARTESIAN_POINT('Ctrl Pts',(-45.3839316726719,33.3561602304872,
-40.8744601355583));
#238313=CARTESIAN_POINT('Ctrl Pts',(-45.8188676392155,33.0740185112342,
-40.8475212259141));
#238314=CARTESIAN_POINT('Ctrl Pts',(-46.0103951893242,32.886908350919,-40.8324825468278));
#238315=CARTESIAN_POINT('Ctrl Pts',(-46.3061199456251,32.4536433767286,
-40.8019694971061));
#238316=CARTESIAN_POINT('Ctrl Pts',(-46.4093131594905,32.2128890246153,
-40.7867972309098));
#238317=CARTESIAN_POINT('Ctrl Pts',(-46.5170230053301,31.7097685641752,
-40.7582389795783));
#238318=CARTESIAN_POINT('Ctrl Pts',(-46.5222267679748,31.4525418257785,
-40.7459252526485));
#238319=CARTESIAN_POINT('Ctrl Pts',(-46.4337482063667,30.9384475986097,
-40.7173735393959));
#238320=CARTESIAN_POINT('Ctrl Pts',(-46.3364290625623,30.6873725516868,
-40.7018512178498));
#238321=CARTESIAN_POINT('Ctrl Pts',(-46.0545875790311,30.2467385831459,
-40.6713708289661));
#238322=CARTESIAN_POINT('Ctrl Pts',(-45.8760988962231,30.0592408825443,
-40.6566928723583));
#238323=CARTESIAN_POINT('Ctrl Pts',(-45.4536997868605,29.7588549154494,
-40.629197955426));
#238324=CARTESIAN_POINT('Ctrl Pts',(-45.2126607854844,29.6504945112309,
-40.6160579857508));
#238325=CARTESIAN_POINT('Ctrl Pts',(-44.8097429655949,29.5575438432581,
-40.5925544462573));
#238326=CARTESIAN_POINT('Ctrl Pts',(-44.6589093996137,29.5404524382925,
-40.583755821575));
#238327=CARTESIAN_POINT('Ctrl Pts',(-44.5079524583208,29.5404524382925,
-40.5749499999997));
#238328=CARTESIAN_POINT('Ctrl Pts',(-44.5079524583208,29.5404524382925,
-40.4162000000005));
#238329=CARTESIAN_POINT('Ctrl Pts',(-44.5829923762501,29.5404524382925,
-40.4205773285463));
#238330=CARTESIAN_POINT('Ctrl Pts',(-44.6581163348707,29.5446755687294,
-40.424959559466));
#238331=CARTESIAN_POINT('Ctrl Pts',(-44.9963174757759,29.5829688449569,
-40.4446879593522));
#238332=CARTESIAN_POINT('Ctrl Pts',(-45.2511810225848,29.6648445373245,
-40.4595549995827));
#238333=CARTESIAN_POINT('Ctrl Pts',(-45.7042087706374,29.9176993849155,
-40.4859816182191));
#238334=CARTESIAN_POINT('Ctrl Pts',(-45.900274393063,30.0824091221457,-40.4998184075873));
#238335=CARTESIAN_POINT('Ctrl Pts',(-46.2264944584649,30.4840139191428,
-40.5296214902895));
#238336=CARTESIAN_POINT('Ctrl Pts',(-46.3505978161064,30.7194081747423,
-40.5451328535272));
#238337=CARTESIAN_POINT('Ctrl Pts',(-46.4997227128501,31.2225224340371,
-40.5748987305729));
#238338=CARTESIAN_POINT('Ctrl Pts',(-46.5241698272145,31.4850206280497,
-40.5879266809833));
#238339=CARTESIAN_POINT('Ctrl Pts',(-46.47125040528,32.000207668004,-40.6154964595404));
#238340=CARTESIAN_POINT('Ctrl Pts',(-46.3960885197321,32.2481390631782,
-40.6302137162548));
#238341=CARTESIAN_POINT('Ctrl Pts',(-46.1514629950418,32.7109498599051,
-40.660728971973));
#238342=CARTESIAN_POINT('Ctrl Pts',(-45.9808127663973,32.9195471375113,
-40.6762442185664));
#238343=CARTESIAN_POINT('Ctrl Pts',(-45.5770770869542,33.2497974648976,
-40.704703477649));
#238344=CARTESIAN_POINT('Ctrl Pts',(-45.3509487745718,33.3719135158588,
-40.7170252148852));
#238345=CARTESIAN_POINT('Ctrl Pts',(-44.8601916059309,33.5262465147202,
-40.7456527163891));
#238346=CARTESIAN_POINT('Ctrl Pts',(-44.5996390813612,33.5551548713799,
-40.7608516136556));
#238347=CARTESIAN_POINT('Ctrl Pts',(-44.0767106440532,33.5113154004804,
-40.7913557724985));
#238348=CARTESIAN_POINT('Ctrl Pts',(-43.8195270625652,33.4368669124925,
-40.8063581480853));
#238349=CARTESIAN_POINT('Ctrl Pts',(-43.3596501657047,33.1974268160417,
-40.8331843004021));
#238350=CARTESIAN_POINT('Ctrl Pts',(-43.1591913872011,33.0388072324325,
-40.8465114211634));
#238351=CARTESIAN_POINT('Ctrl Pts',(-42.8220104306781,32.6479878959408,
-40.8760893350274));
#238352=CARTESIAN_POINT('Ctrl Pts',(-42.6912473505325,32.4171617775238,
-40.8915641663387));
#238353=CARTESIAN_POINT('Ctrl Pts',(-42.526207751472,31.9174494400805,-40.9216223634086));
#238354=CARTESIAN_POINT('Ctrl Pts',(-42.4938428204949,31.6534204444785,
-40.9350815343781));
#238355=CARTESIAN_POINT('Ctrl Pts',(-42.5327337940736,31.1353981648866,
-40.9623853809157));
#238356=CARTESIAN_POINT('Ctrl Pts',(-42.6007517442998,30.8861559029383,
-40.9769604954124));
#238357=CARTESIAN_POINT('Ctrl Pts',(-42.8314514208811,30.4179025768849,
-41.007344527066));
#238358=CARTESIAN_POINT('Ctrl Pts',(-42.9954778454,30.2050806326366,-41.0228800017097));
#238359=CARTESIAN_POINT('Ctrl Pts',(-43.3894653112581,29.8628281077271,
-41.0516612666937));
#238360=CARTESIAN_POINT('Ctrl Pts',(-43.6129381130091,29.7336912042102,
-41.0639908298572));
#238361=CARTESIAN_POINT('Ctrl Pts',(-44.0650998168327,29.5774371450193,
-41.090366929247));
#238362=CARTESIAN_POINT('Ctrl Pts',(-44.2858957213049,29.5404524382925,
-41.1032466903412));
#238363=CARTESIAN_POINT('Ctrl Pts',(-44.5079524583208,29.5404524382925,
-41.1162000000004));
#238364=CARTESIAN_POINT('Origin',(-44.5079524583208,31.5404524382925,235.35105));
#238365=CARTESIAN_POINT('',(-44.5079524583208,29.5404524382925,-39.7162000000004));
#238366=CARTESIAN_POINT('',(-44.5079524583208,29.5404524382925,-39.8749499999996));
#238367=CARTESIAN_POINT('',(-44.5079524583208,29.5404524382925,235.35105));
#238368=CARTESIAN_POINT('',(-43.0434008745115,32.9024688233232,-39.4567761906824));
#238369=CARTESIAN_POINT('Ctrl Pts',(-44.5079524583208,29.5404524382925,
-39.7162000000005));
#238370=CARTESIAN_POINT('Ctrl Pts',(-44.2727838454877,29.5404524382925,
-39.7024818309185));
#238371=CARTESIAN_POINT('Ctrl Pts',(-44.0391728207237,29.5819339445239,
-39.6888545211407));
#238372=CARTESIAN_POINT('Ctrl Pts',(-43.5769885436395,29.7518172548108,
-39.661893771644));
#238373=CARTESIAN_POINT('Ctrl Pts',(-43.3553604175783,29.8859300422344,
-39.6494994736688));
#238374=CARTESIAN_POINT('Ctrl Pts',(-42.9683294219119,30.2365875679526,
-39.6204965006525));
#238375=CARTESIAN_POINT('Ctrl Pts',(-42.8090308900948,30.4522665828854,
-39.6049545889581));
#238376=CARTESIAN_POINT('Ctrl Pts',(-42.5882152549613,30.9241122679227,
-39.5746773625219));
#238377=CARTESIAN_POINT('Ctrl Pts',(-42.5252433861803,31.1741567088814,
-39.5602089008022));
#238378=CARTESIAN_POINT('Ctrl Pts',(-42.4963483862349,31.6933438391783,
-39.5331377573946));
#238379=CARTESIAN_POINT('Ctrl Pts',(-42.5341552917939,31.9577132499568,
-39.5193565070205));
#238380=CARTESIAN_POINT('Ctrl Pts',(-42.6679048358913,32.3360106662249,
-39.4963445935783));
#238381=CARTESIAN_POINT('Ctrl Pts',(-42.7265667691374,32.4598822126121,
-39.4883758593432));
#238382=CARTESIAN_POINT('Ctrl Pts',(-42.8680765464176,32.6934533978673,
-39.4724489070045));
#238383=CARTESIAN_POINT('Ctrl Pts',(-42.9505054915165,32.802580106633,-39.4645318501545));
#238384=CARTESIAN_POINT('Ctrl Pts',(-43.0434008641317,32.9024688214384,
-39.4567762088531));
#238385=CARTESIAN_POINT('',(-43.3993761328101,33.2051021117905,-39.5898551227246));
#238386=CARTESIAN_POINT('Ctrl Pts',(-43.3993761338312,33.2051021109807,
-39.5898551212222));
#238387=CARTESIAN_POINT('Ctrl Pts',(-43.3343112356562,33.1617720296696,
-39.5680449019351));
#238388=CARTESIAN_POINT('Ctrl Pts',(-43.2718932132572,33.1146982543088,
-39.5459701333695));
#238389=CARTESIAN_POINT('Ctrl Pts',(-43.1529636864307,33.0135776982464,
-39.5015049864959));
#238390=CARTESIAN_POINT('Ctrl Pts',(-43.0965305096728,32.959598167928,-39.4791495394364));
#238391=CARTESIAN_POINT('Ctrl Pts',(-43.043400874595,32.9024688326895,-39.4567761622585));
#238392=CARTESIAN_POINT('Ctrl Pts',(-44.5079524583208,29.5404524382925,
-39.8749499999996));
#238393=CARTESIAN_POINT('Ctrl Pts',(-44.4373589931104,29.5404524382925,
-39.8708320478624));
#238394=CARTESIAN_POINT('Ctrl Pts',(-44.3666819864989,29.5441899135023,
-39.8667092224767));
#238395=CARTESIAN_POINT('Ctrl Pts',(-44.0426740209612,29.5786855502815,
-39.8478087578204));
#238396=CARTESIAN_POINT('Ctrl Pts',(-43.7965720231925,29.6539224734034,
-39.8334528079507));
#238397=CARTESIAN_POINT('Ctrl Pts',(-43.3351658396914,29.8985180124527,
-39.8065374472466));
#238398=CARTESIAN_POINT('Ctrl Pts',(-43.1265097586977,30.06971477229,-39.7922901984896));
#238399=CARTESIAN_POINT('Ctrl Pts',(-42.792355887439,30.4797122390129,-39.7618317309806));
#238400=CARTESIAN_POINT('Ctrl Pts',(-42.6684583528071,30.712981114929,-39.7464337411607));
#238401=CARTESIAN_POINT('Ctrl Pts',(-42.5199012825829,31.2060434353122,
-39.7171922310651));
#238402=CARTESIAN_POINT('Ctrl Pts',(-42.4935765041893,31.4602232063242,
-39.7044223309215));
#238403=CARTESIAN_POINT('Ctrl Pts',(-42.5381946201159,31.9768008141531,
-39.6770244248751));
#238404=CARTESIAN_POINT('Ctrl Pts',(-42.613350918841,32.2338428608599,-39.6618470778621));
#238405=CARTESIAN_POINT('Ctrl Pts',(-42.8150006258135,32.6186840080726,
-39.6365241658308));
#238406=CARTESIAN_POINT('Ctrl Pts',(-42.912317892686,32.7580827818824,-39.6266435775835));
#238407=CARTESIAN_POINT('Ctrl Pts',(-43.1367390871144,33.0056999129204,
-39.6075888004023));
#238408=CARTESIAN_POINT('Ctrl Pts',(-43.2621306492484,33.1137032434628,
-39.5984754182101));
#238409=CARTESIAN_POINT('Ctrl Pts',(-43.3993761335977,33.2051021108252,
-39.5898551233574));
#238410=CARTESIAN_POINT('Origin',(44.5079524583205,-57.4754524783491,-52.920575));
#238411=CARTESIAN_POINT('',(42.839207175268,-57.4754524783491,-40.04995));
#238412=CARTESIAN_POINT('',(42.839207175268,-57.4754524783491,-39.8912));
#238413=CARTESIAN_POINT('',(42.839207175268,-57.4754524783491,-52.920575));
#238414=CARTESIAN_POINT('',(43.0534153750531,-58.2933966653875,-39.8341885847849));
#238415=CARTESIAN_POINT('Ctrl Pts',(42.839207175268,-57.4754524783491,-39.8912));
#238416=CARTESIAN_POINT('Ctrl Pts',(42.839207175268,-57.9124736451316,-39.8647399998442));
#238417=CARTESIAN_POINT('Ctrl Pts',(43.0534153750531,-58.2933966653875,
-39.8341885847849));
#238418=CARTESIAN_POINT('',(43.3633213057583,-58.68975488891,-39.9581073773015));
#238419=CARTESIAN_POINT('Ctrl Pts',(43.3633213057583,-58.68975488891,-39.9581073773016));
#238420=CARTESIAN_POINT('Ctrl Pts',(43.3039463283678,-58.6337865829816,
-39.9376450972415));
#238421=CARTESIAN_POINT('Ctrl Pts',(43.2487306042849,-58.5735157107134,
-39.9172507770231));
#238422=CARTESIAN_POINT('Ctrl Pts',(43.1444016679814,-58.4413495448207,
-39.875725104448));
#238423=CARTESIAN_POINT('Ctrl Pts',(43.0960118137051,-58.3691452318743,
-39.8546807358163));
#238424=CARTESIAN_POINT('Ctrl Pts',(43.0534153750531,-58.2933966653875,
-39.8341885847849));
#238425=CARTESIAN_POINT('Ctrl Pts',(42.839207175268,-57.4754524783491,-40.04995));
#238426=CARTESIAN_POINT('Ctrl Pts',(42.839207175268,-58.1957120903124,-40.0063409693778));
#238427=CARTESIAN_POINT('Ctrl Pts',(43.3633213057583,-58.68975488891,-39.9581073773015));
#238428=CARTESIAN_POINT('Origin',(44.5079524583205,-57.4754524783491,-52.920575));
#238429=CARTESIAN_POINT('',(42.839207175268,-57.4754524783491,-40.74995));
#238430=CARTESIAN_POINT('',(42.839207175268,-57.4754524783491,-40.5912));
#238431=CARTESIAN_POINT('',(42.839207175268,-57.4754524783491,-52.920575));
#238432=CARTESIAN_POINT('',(45.3466064770396,-58.918147961324,-40.3575668307237));
#238433=CARTESIAN_POINT('Ctrl Pts',(42.839207175268,-57.4754524783491,-40.5912));
#238434=CARTESIAN_POINT('Ctrl Pts',(42.839207175268,-58.4389030167283,-40.5328666666667));
#238435=CARTESIAN_POINT('Ctrl Pts',(43.6735798167943,-58.920628285918,-40.4745333333334));
#238436=CARTESIAN_POINT('Ctrl Pts',(44.5079524583205,-59.4023535551075,
-40.4162));
#238437=CARTESIAN_POINT('Ctrl Pts',(45.3423250998467,-58.920628285918,-40.3578666666667));
#238438=CARTESIAN_POINT('Ctrl Pts',(45.3444676270302,-58.9193912972719,
-40.3577168765775));
#238439=CARTESIAN_POINT('Ctrl Pts',(45.3466064770396,-58.918147961324,-40.3575668307237));
#238440=CARTESIAN_POINT('',(46.1762417771239,-57.4364451908711,-40.2388223154955));
#238441=CARTESIAN_POINT('Ctrl Pts',(46.1762417771238,-57.4364451908711,
-40.2388223154955));
#238442=CARTESIAN_POINT('Ctrl Pts',(46.179661059212,-57.5826832954551,-40.2660212994017));
#238443=CARTESIAN_POINT('Ctrl Pts',(46.1638510938788,-57.7293501220844,
-40.2898469846044));
#238444=CARTESIAN_POINT('Ctrl Pts',(46.0933221577362,-58.0171833460811,
-40.3294337826712));
#238445=CARTESIAN_POINT('Ctrl Pts',(46.0386075282205,-58.15680126839,-40.3449195577534));
#238446=CARTESIAN_POINT('Ctrl Pts',(45.8931630193347,-58.417855944105,-40.36600443659));
#238447=CARTESIAN_POINT('Ctrl Pts',(45.8033935488223,-58.5379373447246,
-40.3715360596572));
#238448=CARTESIAN_POINT('Ctrl Pts',(45.6856994285344,-58.6578091204824,
-40.3719332463563));
#238449=CARTESIAN_POINT('Ctrl Pts',(45.6724768224328,-58.6708344909785,
-40.3718974824544));
#238450=CARTESIAN_POINT('Ctrl Pts',(45.5643373887037,-58.7738638224284,
-40.3709688119876));
#238451=CARTESIAN_POINT('Ctrl Pts',(45.4594840399648,-58.8525310498637,
-40.3661880411365));
#238452=CARTESIAN_POINT('Ctrl Pts',(45.3466064770396,-58.918147961324,-40.3575668307237));
#238453=CARTESIAN_POINT('Ctrl Pts',(46.1762417771239,-57.4364451908711,
-40.2388223154955));
#238454=CARTESIAN_POINT('Ctrl Pts',(46.1543247861016,-56.4990849082214,
-40.181302510566));
#238455=CARTESIAN_POINT('Ctrl Pts',(45.3423250998467,-56.0302766707802,
-40.1245333333334));
#238456=CARTESIAN_POINT('Ctrl Pts',(44.5079524583205,-55.5485514015906,
-40.0662));
#238457=CARTESIAN_POINT('Ctrl Pts',(43.6735798167943,-56.0302766707802,
-40.0078666666667));
#238458=CARTESIAN_POINT('Ctrl Pts',(42.839207175268,-56.5120019399698,-39.9495333333333));
#238459=CARTESIAN_POINT('Ctrl Pts',(42.839207175268,-57.4754524783491,-39.8912));
#238460=CARTESIAN_POINT('Ctrl Pts',(42.839207175268,-57.4754524783491,-40.74995));
#238461=CARTESIAN_POINT('Ctrl Pts',(42.839207175268,-58.4389030167283,-40.6916166666667));
#238462=CARTESIAN_POINT('Ctrl Pts',(43.6735798167943,-58.920628285918,-40.6332833333334));
#238463=CARTESIAN_POINT('Ctrl Pts',(44.5079524583205,-59.4023535551075,
-40.57495));
#238464=CARTESIAN_POINT('Ctrl Pts',(45.3423250998467,-58.920628285918,-40.5166166666667));
#238465=CARTESIAN_POINT('Ctrl Pts',(46.1766977413729,-58.4389030167283,
-40.4582833333333));
#238466=CARTESIAN_POINT('Ctrl Pts',(46.1766977413729,-57.4754524783491,
-40.39995));
#238467=CARTESIAN_POINT('Ctrl Pts',(46.1766977413729,-56.5120019399699,
-40.3416166666667));
#238468=CARTESIAN_POINT('Ctrl Pts',(45.3423250998467,-56.0302766707802,
-40.2832833333334));
#238469=CARTESIAN_POINT('Ctrl Pts',(44.5079524583205,-55.5485514015906,
-40.22495));
#238470=CARTESIAN_POINT('Ctrl Pts',(43.6735798167943,-56.0302766707802,
-40.1666166666667));
#238471=CARTESIAN_POINT('Ctrl Pts',(42.839207175268,-56.5120019399698,-40.1082833333334));
#238472=CARTESIAN_POINT('Ctrl Pts',(42.839207175268,-57.4754524783491,-40.04995));
#238473=CARTESIAN_POINT('Origin',(44.5079524583205,-57.4754524783491,-52.920575));
#238474=CARTESIAN_POINT('',(42.839207175268,-57.4754524783491,-41.44995));
#238475=CARTESIAN_POINT('',(42.839207175268,-57.4754524783491,-41.2912));
#238476=CARTESIAN_POINT('',(42.839207175268,-57.4754524783491,-52.920575));
#238477=CARTESIAN_POINT('Ctrl Pts',(42.839207175268,-57.4754524783491,-41.2912));
#238478=CARTESIAN_POINT('Ctrl Pts',(42.839207175268,-58.4389030167283,-41.2328666666667));
#238479=CARTESIAN_POINT('Ctrl Pts',(43.6735798167943,-58.920628285918,-41.1745333333334));
#238480=CARTESIAN_POINT('Ctrl Pts',(44.5079524583205,-59.4023535551075,
-41.1162));
#238481=CARTESIAN_POINT('Ctrl Pts',(45.3423250998467,-58.920628285918,-41.0578666666667));
#238482=CARTESIAN_POINT('Ctrl Pts',(46.1766977413729,-58.4389030167283,
-40.9995333333333));
#238483=CARTESIAN_POINT('Ctrl Pts',(46.1766977413729,-57.4754524783491,
-40.9412));
#238484=CARTESIAN_POINT('Ctrl Pts',(46.1766977413729,-56.5120019399699,
-40.8828666666667));
#238485=CARTESIAN_POINT('Ctrl Pts',(45.3423250998467,-56.0302766707802,
-40.8245333333333));
#238486=CARTESIAN_POINT('Ctrl Pts',(44.5079524583205,-55.5485514015906,
-40.7662));
#238487=CARTESIAN_POINT('Ctrl Pts',(43.6735798167943,-56.0302766707802,
-40.7078666666667));
#238488=CARTESIAN_POINT('Ctrl Pts',(42.839207175268,-56.5120019399698,-40.6495333333334));
#238489=CARTESIAN_POINT('Ctrl Pts',(42.839207175268,-57.4754524783491,-40.5912));
#238490=CARTESIAN_POINT('Ctrl Pts',(42.839207175268,-57.4754524783491,-41.44995));
#238491=CARTESIAN_POINT('Ctrl Pts',(42.839207175268,-58.4389030167283,-41.3916166666667));
#238492=CARTESIAN_POINT('Ctrl Pts',(43.6735798167943,-58.920628285918,-41.3332833333334));
#238493=CARTESIAN_POINT('Ctrl Pts',(44.5079524583205,-59.4023535551075,
-41.27495));
#238494=CARTESIAN_POINT('Ctrl Pts',(45.3423250998467,-58.920628285918,-41.2166166666667));
#238495=CARTESIAN_POINT('Ctrl Pts',(46.1766977413729,-58.4389030167283,
-41.1582833333333));
#238496=CARTESIAN_POINT('Ctrl Pts',(46.1766977413729,-57.4754524783491,
-41.09995));
#238497=CARTESIAN_POINT('Ctrl Pts',(46.1766977413729,-56.5120019399699,
-41.0416166666667));
#238498=CARTESIAN_POINT('Ctrl Pts',(45.3423250998467,-56.0302766707802,
-40.9832833333333));
#238499=CARTESIAN_POINT('Ctrl Pts',(44.5079524583205,-55.5485514015906,
-40.92495));
#238500=CARTESIAN_POINT('Ctrl Pts',(43.6735798167943,-56.0302766707802,
-40.8666166666667));
#238501=CARTESIAN_POINT('Ctrl Pts',(42.839207175268,-56.5120019399698,-40.8082833333334));
#238502=CARTESIAN_POINT('Ctrl Pts',(42.839207175268,-57.4754524783491,-40.74995));
#238503=CARTESIAN_POINT('Origin',(44.5079524583205,-57.4754524783491,-52.920575));
#238504=CARTESIAN_POINT('',(42.839207175268,-57.4754524783491,-42.14995));
#238505=CARTESIAN_POINT('',(42.839207175268,-57.4754524783491,-41.9912));
#238506=CARTESIAN_POINT('',(42.839207175268,-57.4754524783491,-52.920575));
#238507=CARTESIAN_POINT('Ctrl Pts',(42.839207175268,-57.4754524783491,-41.9912));
#238508=CARTESIAN_POINT('Ctrl Pts',(42.839207175268,-58.4389030167283,-41.9328666666667));
#238509=CARTESIAN_POINT('Ctrl Pts',(43.6735798167943,-58.920628285918,-41.8745333333334));
#238510=CARTESIAN_POINT('Ctrl Pts',(44.5079524583205,-59.4023535551075,
-41.8162));
#238511=CARTESIAN_POINT('Ctrl Pts',(45.3423250998467,-58.920628285918,-41.7578666666667));
#238512=CARTESIAN_POINT('Ctrl Pts',(46.1766977413729,-58.4389030167283,
-41.6995333333334));
#238513=CARTESIAN_POINT('Ctrl Pts',(46.1766977413729,-57.4754524783491,
-41.6412));
#238514=CARTESIAN_POINT('Ctrl Pts',(46.1766977413729,-56.5120019399699,
-41.5828666666667));
#238515=CARTESIAN_POINT('Ctrl Pts',(45.3423250998467,-56.0302766707802,
-41.5245333333334));
#238516=CARTESIAN_POINT('Ctrl Pts',(44.5079524583205,-55.5485514015906,
-41.4662));
#238517=CARTESIAN_POINT('Ctrl Pts',(43.6735798167943,-56.0302766707802,
-41.4078666666667));
#238518=CARTESIAN_POINT('Ctrl Pts',(42.839207175268,-56.5120019399698,-41.3495333333333));
#238519=CARTESIAN_POINT('Ctrl Pts',(42.839207175268,-57.4754524783491,-41.2912));
#238520=CARTESIAN_POINT('Ctrl Pts',(42.839207175268,-57.4754524783491,-42.14995));
#238521=CARTESIAN_POINT('Ctrl Pts',(42.839207175268,-58.4389030167283,-42.0916166666667));
#238522=CARTESIAN_POINT('Ctrl Pts',(43.6735798167943,-58.920628285918,-42.0332833333334));
#238523=CARTESIAN_POINT('Ctrl Pts',(44.5079524583205,-59.4023535551075,
-41.97495));
#238524=CARTESIAN_POINT('Ctrl Pts',(45.3423250998467,-58.920628285918,-41.9166166666667));
#238525=CARTESIAN_POINT('Ctrl Pts',(46.1766977413729,-58.4389030167283,
-41.8582833333333));
#238526=CARTESIAN_POINT('Ctrl Pts',(46.1766977413729,-57.4754524783491,
-41.79995));
#238527=CARTESIAN_POINT('Ctrl Pts',(46.1766977413729,-56.5120019399699,
-41.7416166666666));
#238528=CARTESIAN_POINT('Ctrl Pts',(45.3423250998467,-56.0302766707802,
-41.6832833333333));
#238529=CARTESIAN_POINT('Ctrl Pts',(44.5079524583205,-55.5485514015906,
-41.62495));
#238530=CARTESIAN_POINT('Ctrl Pts',(43.6735798167943,-56.0302766707802,
-41.5666166666667));
#238531=CARTESIAN_POINT('Ctrl Pts',(42.839207175268,-56.5120019399698,-41.5082833333334));
#238532=CARTESIAN_POINT('Ctrl Pts',(42.839207175268,-57.4754524783491,-41.44995));
#238533=CARTESIAN_POINT('Origin',(44.5079524583205,-57.4754524783491,-52.920575));
#238534=CARTESIAN_POINT('',(42.839207175268,-57.4754524783491,-42.84995));
#238535=CARTESIAN_POINT('',(42.839207175268,-57.4754524783491,-42.6912));
#238536=CARTESIAN_POINT('',(42.839207175268,-57.4754524783491,-52.920575));
#238537=CARTESIAN_POINT('Ctrl Pts',(42.839207175268,-57.4754524783491,-42.6912));
#238538=CARTESIAN_POINT('Ctrl Pts',(42.839207175268,-58.4389030167283,-42.6328666666667));
#238539=CARTESIAN_POINT('Ctrl Pts',(43.6735798167943,-58.920628285918,-42.5745333333333));
#238540=CARTESIAN_POINT('Ctrl Pts',(44.5079524583205,-59.4023535551075,
-42.5162));
#238541=CARTESIAN_POINT('Ctrl Pts',(45.3423250998467,-58.920628285918,-42.4578666666667));
#238542=CARTESIAN_POINT('Ctrl Pts',(46.1766977413729,-58.4389030167283,
-42.3995333333334));
#238543=CARTESIAN_POINT('Ctrl Pts',(46.1766977413729,-57.4754524783491,
-42.3412));
#238544=CARTESIAN_POINT('Ctrl Pts',(46.1766977413729,-56.5120019399699,
-42.2828666666667));
#238545=CARTESIAN_POINT('Ctrl Pts',(45.3423250998467,-56.0302766707802,
-42.2245333333333));
#238546=CARTESIAN_POINT('Ctrl Pts',(44.5079524583205,-55.5485514015906,
-42.1662));
#238547=CARTESIAN_POINT('Ctrl Pts',(43.6735798167943,-56.0302766707802,
-42.1078666666667));
#238548=CARTESIAN_POINT('Ctrl Pts',(42.839207175268,-56.5120019399698,-42.0495333333334));
#238549=CARTESIAN_POINT('Ctrl Pts',(42.839207175268,-57.4754524783491,-41.9912));
#238550=CARTESIAN_POINT('Ctrl Pts',(42.839207175268,-57.4754524783491,-42.84995));
#238551=CARTESIAN_POINT('Ctrl Pts',(42.839207175268,-58.4389030167283,-42.7916166666667));
#238552=CARTESIAN_POINT('Ctrl Pts',(43.6735798167943,-58.920628285918,-42.7332833333334));
#238553=CARTESIAN_POINT('Ctrl Pts',(44.5079524583205,-59.4023535551075,
-42.67495));
#238554=CARTESIAN_POINT('Ctrl Pts',(45.3423250998467,-58.920628285918,-42.6166166666667));
#238555=CARTESIAN_POINT('Ctrl Pts',(46.1766977413729,-58.4389030167283,
-42.5582833333333));
#238556=CARTESIAN_POINT('Ctrl Pts',(46.1766977413729,-57.4754524783491,
-42.49995));
#238557=CARTESIAN_POINT('Ctrl Pts',(46.1766977413729,-56.5120019399699,
-42.4416166666667));
#238558=CARTESIAN_POINT('Ctrl Pts',(45.3423250998467,-56.0302766707802,
-42.3832833333333));
#238559=CARTESIAN_POINT('Ctrl Pts',(44.5079524583205,-55.5485514015906,
-42.32495));
#238560=CARTESIAN_POINT('Ctrl Pts',(43.6735798167943,-56.0302766707802,
-42.2666166666667));
#238561=CARTESIAN_POINT('Ctrl Pts',(42.839207175268,-56.5120019399698,-42.2082833333333));
#238562=CARTESIAN_POINT('Ctrl Pts',(42.839207175268,-57.4754524783491,-42.14995));
#238563=CARTESIAN_POINT('Origin',(44.5079524583205,-57.4754524783491,-52.920575));
#238564=CARTESIAN_POINT('',(42.839207175268,-57.4754524783491,-43.54995));
#238565=CARTESIAN_POINT('',(42.839207175268,-57.4754524783491,-43.3912));
#238566=CARTESIAN_POINT('',(42.839207175268,-57.4754524783491,-52.920575));
#238567=CARTESIAN_POINT('Ctrl Pts',(42.839207175268,-57.4754524783491,-43.3912));
#238568=CARTESIAN_POINT('Ctrl Pts',(42.839207175268,-58.4389030167283,-43.3328666666667));
#238569=CARTESIAN_POINT('Ctrl Pts',(43.6735798167943,-58.920628285918,-43.2745333333334));
#238570=CARTESIAN_POINT('Ctrl Pts',(44.5079524583205,-59.4023535551075,
-43.2162));
#238571=CARTESIAN_POINT('Ctrl Pts',(45.3423250998467,-58.920628285918,-43.1578666666667));
#238572=CARTESIAN_POINT('Ctrl Pts',(46.1766977413729,-58.4389030167283,
-43.0995333333334));
#238573=CARTESIAN_POINT('Ctrl Pts',(46.1766977413729,-57.4754524783491,
-43.0412));
#238574=CARTESIAN_POINT('Ctrl Pts',(46.1766977413729,-56.5120019399699,
-42.9828666666667));
#238575=CARTESIAN_POINT('Ctrl Pts',(45.3423250998467,-56.0302766707802,
-42.9245333333334));
#238576=CARTESIAN_POINT('Ctrl Pts',(44.5079524583205,-55.5485514015906,
-42.8662));
#238577=CARTESIAN_POINT('Ctrl Pts',(43.6735798167943,-56.0302766707802,
-42.8078666666667));
#238578=CARTESIAN_POINT('Ctrl Pts',(42.839207175268,-56.5120019399698,-42.7495333333334));
#238579=CARTESIAN_POINT('Ctrl Pts',(42.839207175268,-57.4754524783491,-42.6912));
#238580=CARTESIAN_POINT('Ctrl Pts',(42.839207175268,-57.4754524783491,-43.54995));
#238581=CARTESIAN_POINT('Ctrl Pts',(42.839207175268,-58.4389030167283,-43.4916166666667));
#238582=CARTESIAN_POINT('Ctrl Pts',(43.6735798167943,-58.920628285918,-43.4332833333333));
#238583=CARTESIAN_POINT('Ctrl Pts',(44.5079524583205,-59.4023535551075,
-43.37495));
#238584=CARTESIAN_POINT('Ctrl Pts',(45.3423250998467,-58.920628285918,-43.3166166666667));
#238585=CARTESIAN_POINT('Ctrl Pts',(46.1766977413729,-58.4389030167283,
-43.2582833333333));
#238586=CARTESIAN_POINT('Ctrl Pts',(46.1766977413729,-57.4754524783491,
-43.19995));
#238587=CARTESIAN_POINT('Ctrl Pts',(46.1766977413729,-56.5120019399699,
-43.1416166666667));
#238588=CARTESIAN_POINT('Ctrl Pts',(45.3423250998467,-56.0302766707802,
-43.0832833333333));
#238589=CARTESIAN_POINT('Ctrl Pts',(44.5079524583205,-55.5485514015906,
-43.02495));
#238590=CARTESIAN_POINT('Ctrl Pts',(43.6735798167943,-56.0302766707802,
-42.9666166666667));
#238591=CARTESIAN_POINT('Ctrl Pts',(42.839207175268,-56.5120019399698,-42.9082833333333));
#238592=CARTESIAN_POINT('Ctrl Pts',(42.839207175268,-57.4754524783491,-42.84995));
#238593=CARTESIAN_POINT('Origin',(44.5079524583205,-57.4754524783491,-52.920575));
#238594=CARTESIAN_POINT('',(42.839207175268,-57.4754524783491,-44.24995));
#238595=CARTESIAN_POINT('',(42.839207175268,-57.4754524783491,-44.0912));
#238596=CARTESIAN_POINT('',(42.839207175268,-57.4754524783491,-52.920575));
#238597=CARTESIAN_POINT('Ctrl Pts',(42.839207175268,-57.4754524783491,-44.0912));
#238598=CARTESIAN_POINT('Ctrl Pts',(42.839207175268,-58.4389030167283,-44.0328666666667));
#238599=CARTESIAN_POINT('Ctrl Pts',(43.6735798167943,-58.920628285918,-43.9745333333333));
#238600=CARTESIAN_POINT('Ctrl Pts',(44.5079524583205,-59.4023535551075,
-43.9162));
#238601=CARTESIAN_POINT('Ctrl Pts',(45.3423250998467,-58.920628285918,-43.8578666666667));
#238602=CARTESIAN_POINT('Ctrl Pts',(46.1766977413729,-58.4389030167283,
-43.7995333333334));
#238603=CARTESIAN_POINT('Ctrl Pts',(46.1766977413729,-57.4754524783491,
-43.7412));
#238604=CARTESIAN_POINT('Ctrl Pts',(46.1766977413729,-56.5120019399699,
-43.6828666666667));
#238605=CARTESIAN_POINT('Ctrl Pts',(45.3423250998467,-56.0302766707802,
-43.6245333333333));
#238606=CARTESIAN_POINT('Ctrl Pts',(44.5079524583205,-55.5485514015906,
-43.5662));
#238607=CARTESIAN_POINT('Ctrl Pts',(43.6735798167943,-56.0302766707802,
-43.5078666666667));
#238608=CARTESIAN_POINT('Ctrl Pts',(42.839207175268,-56.5120019399698,-43.4495333333334));
#238609=CARTESIAN_POINT('Ctrl Pts',(42.839207175268,-57.4754524783491,-43.3912));
#238610=CARTESIAN_POINT('Ctrl Pts',(42.839207175268,-57.4754524783491,-44.24995));
#238611=CARTESIAN_POINT('Ctrl Pts',(42.839207175268,-58.4389030167283,-44.1916166666667));
#238612=CARTESIAN_POINT('Ctrl Pts',(43.6735798167943,-58.920628285918,-44.1332833333334));
#238613=CARTESIAN_POINT('Ctrl Pts',(44.5079524583205,-59.4023535551075,
-44.07495));
#238614=CARTESIAN_POINT('Ctrl Pts',(45.3423250998467,-58.920628285918,-44.0166166666667));
#238615=CARTESIAN_POINT('Ctrl Pts',(46.1766977413729,-58.4389030167283,
-43.9582833333334));
#238616=CARTESIAN_POINT('Ctrl Pts',(46.1766977413729,-57.4754524783491,
-43.89995));
#238617=CARTESIAN_POINT('Ctrl Pts',(46.1766977413729,-56.5120019399699,
-43.8416166666667));
#238618=CARTESIAN_POINT('Ctrl Pts',(45.3423250998467,-56.0302766707802,
-43.7832833333334));
#238619=CARTESIAN_POINT('Ctrl Pts',(44.5079524583205,-55.5485514015906,
-43.72495));
#238620=CARTESIAN_POINT('Ctrl Pts',(43.6735798167943,-56.0302766707802,
-43.6666166666667));
#238621=CARTESIAN_POINT('Ctrl Pts',(42.839207175268,-56.5120019399698,-43.6082833333334));
#238622=CARTESIAN_POINT('Ctrl Pts',(42.839207175268,-57.4754524783491,-43.54995));
#238623=CARTESIAN_POINT('Origin',(44.5079524583205,-57.4754524783491,-52.920575));
#238624=CARTESIAN_POINT('',(42.839207175268,-57.4754524783491,-44.94995));
#238625=CARTESIAN_POINT('',(42.839207175268,-57.4754524783491,-44.7912));
#238626=CARTESIAN_POINT('',(42.839207175268,-57.4754524783491,-52.920575));
#238627=CARTESIAN_POINT('Ctrl Pts',(42.839207175268,-57.4754524783491,-44.7912));
#238628=CARTESIAN_POINT('Ctrl Pts',(42.839207175268,-58.4389030167283,-44.7328666666667));
#238629=CARTESIAN_POINT('Ctrl Pts',(43.6735798167943,-58.920628285918,-44.6745333333334));
#238630=CARTESIAN_POINT('Ctrl Pts',(44.5079524583205,-59.4023535551075,
-44.6162));
#238631=CARTESIAN_POINT('Ctrl Pts',(45.3423250998467,-58.920628285918,-44.5578666666667));
#238632=CARTESIAN_POINT('Ctrl Pts',(46.1766977413729,-58.4389030167283,
-44.4995333333333));
#238633=CARTESIAN_POINT('Ctrl Pts',(46.1766977413729,-57.4754524783491,
-44.4412));
#238634=CARTESIAN_POINT('Ctrl Pts',(46.1766977413729,-56.5120019399699,
-44.3828666666667));
#238635=CARTESIAN_POINT('Ctrl Pts',(45.3423250998467,-56.0302766707802,
-44.3245333333334));
#238636=CARTESIAN_POINT('Ctrl Pts',(44.5079524583205,-55.5485514015906,
-44.2662));
#238637=CARTESIAN_POINT('Ctrl Pts',(43.6735798167943,-56.0302766707802,
-44.2078666666667));
#238638=CARTESIAN_POINT('Ctrl Pts',(42.839207175268,-56.5120019399698,-44.1495333333334));
#238639=CARTESIAN_POINT('Ctrl Pts',(42.839207175268,-57.4754524783491,-44.0912));
#238640=CARTESIAN_POINT('Ctrl Pts',(42.839207175268,-57.4754524783491,-44.94995));
#238641=CARTESIAN_POINT('Ctrl Pts',(42.839207175268,-58.4389030167283,-44.8916166666667));
#238642=CARTESIAN_POINT('Ctrl Pts',(43.6735798167943,-58.920628285918,-44.8332833333334));
#238643=CARTESIAN_POINT('Ctrl Pts',(44.5079524583205,-59.4023535551075,
-44.77495));
#238644=CARTESIAN_POINT('Ctrl Pts',(45.3423250998467,-58.920628285918,-44.7166166666667));
#238645=CARTESIAN_POINT('Ctrl Pts',(46.1766977413729,-58.4389030167283,
-44.6582833333334));
#238646=CARTESIAN_POINT('Ctrl Pts',(46.1766977413729,-57.4754524783491,
-44.59995));
#238647=CARTESIAN_POINT('Ctrl Pts',(46.1766977413729,-56.5120019399699,
-44.5416166666667));
#238648=CARTESIAN_POINT('Ctrl Pts',(45.3423250998467,-56.0302766707802,
-44.4832833333334));
#238649=CARTESIAN_POINT('Ctrl Pts',(44.5079524583205,-55.5485514015906,
-44.42495));
#238650=CARTESIAN_POINT('Ctrl Pts',(43.6735798167943,-56.0302766707802,
-44.3666166666667));
#238651=CARTESIAN_POINT('Ctrl Pts',(42.839207175268,-56.5120019399698,-44.3082833333334));
#238652=CARTESIAN_POINT('Ctrl Pts',(42.839207175268,-57.4754524783491,-44.24995));
#238653=CARTESIAN_POINT('Origin',(44.5079524583205,-57.4754524783491,-52.920575));
#238654=CARTESIAN_POINT('',(42.839207175268,-57.4754524783491,-45.64995));
#238655=CARTESIAN_POINT('',(42.839207175268,-57.4754524783491,-45.4912));
#238656=CARTESIAN_POINT('',(42.839207175268,-57.4754524783491,-52.920575));
#238657=CARTESIAN_POINT('Ctrl Pts',(42.839207175268,-57.4754524783491,-45.4912));
#238658=CARTESIAN_POINT('Ctrl Pts',(42.839207175268,-58.4389030167283,-45.4328666666666));
#238659=CARTESIAN_POINT('Ctrl Pts',(43.6735798167943,-58.920628285918,-45.3745333333334));
#238660=CARTESIAN_POINT('Ctrl Pts',(44.5079524583205,-59.4023535551075,
-45.3162));
#238661=CARTESIAN_POINT('Ctrl Pts',(45.3423250998467,-58.920628285918,-45.2578666666667));
#238662=CARTESIAN_POINT('Ctrl Pts',(46.1766977413729,-58.4389030167283,
-45.1995333333333));
#238663=CARTESIAN_POINT('Ctrl Pts',(46.1766977413729,-57.4754524783491,
-45.1412));
#238664=CARTESIAN_POINT('Ctrl Pts',(46.1766977413729,-56.5120019399699,
-45.0828666666667));
#238665=CARTESIAN_POINT('Ctrl Pts',(45.3423250998467,-56.0302766707802,
-45.0245333333334));
#238666=CARTESIAN_POINT('Ctrl Pts',(44.5079524583205,-55.5485514015906,
-44.9662));
#238667=CARTESIAN_POINT('Ctrl Pts',(43.6735798167943,-56.0302766707802,
-44.9078666666667));
#238668=CARTESIAN_POINT('Ctrl Pts',(42.839207175268,-56.5120019399698,-44.8495333333333));
#238669=CARTESIAN_POINT('Ctrl Pts',(42.839207175268,-57.4754524783491,-44.7912));
#238670=CARTESIAN_POINT('Ctrl Pts',(42.839207175268,-57.4754524783491,-45.64995));
#238671=CARTESIAN_POINT('Ctrl Pts',(42.839207175268,-58.4389030167283,-45.5916166666667));
#238672=CARTESIAN_POINT('Ctrl Pts',(43.6735798167943,-58.920628285918,-45.5332833333333));
#238673=CARTESIAN_POINT('Ctrl Pts',(44.5079524583205,-59.4023535551075,
-45.47495));
#238674=CARTESIAN_POINT('Ctrl Pts',(45.3423250998467,-58.920628285918,-45.4166166666667));
#238675=CARTESIAN_POINT('Ctrl Pts',(46.1766977413729,-58.4389030167283,
-45.3582833333334));
#238676=CARTESIAN_POINT('Ctrl Pts',(46.1766977413729,-57.4754524783491,
-45.29995));
#238677=CARTESIAN_POINT('Ctrl Pts',(46.1766977413729,-56.5120019399699,
-45.2416166666667));
#238678=CARTESIAN_POINT('Ctrl Pts',(45.3423250998467,-56.0302766707802,
-45.1832833333334));
#238679=CARTESIAN_POINT('Ctrl Pts',(44.5079524583205,-55.5485514015906,
-45.12495));
#238680=CARTESIAN_POINT('Ctrl Pts',(43.6735798167943,-56.0302766707802,
-45.0666166666667));
#238681=CARTESIAN_POINT('Ctrl Pts',(42.839207175268,-56.5120019399698,-45.0082833333334));
#238682=CARTESIAN_POINT('Ctrl Pts',(42.839207175268,-57.4754524783491,-44.94995));
#238683=CARTESIAN_POINT('Origin',(44.5079524583205,-57.4754524783491,-52.920575));
#238684=CARTESIAN_POINT('',(42.839207175268,-57.4754524783491,-46.34995));
#238685=CARTESIAN_POINT('',(42.839207175268,-57.4754524783491,-46.1912));
#238686=CARTESIAN_POINT('',(42.839207175268,-57.4754524783491,-52.920575));
#238687=CARTESIAN_POINT('Ctrl Pts',(42.839207175268,-57.4754524783491,-46.1912));
#238688=CARTESIAN_POINT('Ctrl Pts',(42.839207175268,-58.4389030167283,-46.1328666666667));
#238689=CARTESIAN_POINT('Ctrl Pts',(43.6735798167943,-58.920628285918,-46.0745333333334));
#238690=CARTESIAN_POINT('Ctrl Pts',(44.5079524583205,-59.4023535551075,
-46.0162));
#238691=CARTESIAN_POINT('Ctrl Pts',(45.3423250998467,-58.920628285918,-45.9578666666667));
#238692=CARTESIAN_POINT('Ctrl Pts',(46.1766977413729,-58.4389030167283,
-45.8995333333333));
#238693=CARTESIAN_POINT('Ctrl Pts',(46.1766977413729,-57.4754524783491,
-45.8412));
#238694=CARTESIAN_POINT('Ctrl Pts',(46.1766977413729,-56.5120019399699,
-45.7828666666667));
#238695=CARTESIAN_POINT('Ctrl Pts',(45.3423250998467,-56.0302766707802,
-45.7245333333333));
#238696=CARTESIAN_POINT('Ctrl Pts',(44.5079524583205,-55.5485514015906,
-45.6662));
#238697=CARTESIAN_POINT('Ctrl Pts',(43.6735798167943,-56.0302766707802,
-45.6078666666667));
#238698=CARTESIAN_POINT('Ctrl Pts',(42.839207175268,-56.5120019399698,-45.5495333333333));
#238699=CARTESIAN_POINT('Ctrl Pts',(42.839207175268,-57.4754524783491,-45.4912));
#238700=CARTESIAN_POINT('Ctrl Pts',(42.839207175268,-57.4754524783491,-46.34995));
#238701=CARTESIAN_POINT('Ctrl Pts',(42.839207175268,-58.4389030167283,-46.2916166666667));
#238702=CARTESIAN_POINT('Ctrl Pts',(43.6735798167943,-58.920628285918,-46.2332833333334));
#238703=CARTESIAN_POINT('Ctrl Pts',(44.5079524583205,-59.4023535551075,
-46.17495));
#238704=CARTESIAN_POINT('Ctrl Pts',(45.3423250998467,-58.920628285918,-46.1166166666667));
#238705=CARTESIAN_POINT('Ctrl Pts',(46.1766977413729,-58.4389030167283,
-46.0582833333333));
#238706=CARTESIAN_POINT('Ctrl Pts',(46.1766977413729,-57.4754524783491,
-45.99995));
#238707=CARTESIAN_POINT('Ctrl Pts',(46.1766977413729,-56.5120019399699,
-45.9416166666667));
#238708=CARTESIAN_POINT('Ctrl Pts',(45.3423250998467,-56.0302766707802,
-45.8832833333333));
#238709=CARTESIAN_POINT('Ctrl Pts',(44.5079524583205,-55.5485514015906,
-45.82495));
#238710=CARTESIAN_POINT('Ctrl Pts',(43.6735798167943,-56.0302766707802,
-45.7666166666667));
#238711=CARTESIAN_POINT('Ctrl Pts',(42.839207175268,-56.5120019399698,-45.7082833333333));
#238712=CARTESIAN_POINT('Ctrl Pts',(42.839207175268,-57.4754524783491,-45.64995));
#238713=CARTESIAN_POINT('Origin',(44.5079524583205,-57.4754524783491,-52.920575));
#238714=CARTESIAN_POINT('',(42.839207175268,-57.4754524783491,-47.04995));
#238715=CARTESIAN_POINT('',(42.839207175268,-57.4754524783491,-46.8912));
#238716=CARTESIAN_POINT('',(42.839207175268,-57.4754524783491,-52.920575));
#238717=CARTESIAN_POINT('Ctrl Pts',(42.839207175268,-57.4754524783491,-46.8912));
#238718=CARTESIAN_POINT('Ctrl Pts',(42.839207175268,-58.4389030167283,-46.8328666666667));
#238719=CARTESIAN_POINT('Ctrl Pts',(43.6735798167943,-58.920628285918,-46.7745333333334));
#238720=CARTESIAN_POINT('Ctrl Pts',(44.5079524583205,-59.4023535551075,
-46.7162));
#238721=CARTESIAN_POINT('Ctrl Pts',(45.3423250998467,-58.920628285918,-46.6578666666667));
#238722=CARTESIAN_POINT('Ctrl Pts',(46.1766977413729,-58.4389030167283,
-46.5995333333334));
#238723=CARTESIAN_POINT('Ctrl Pts',(46.1766977413729,-57.4754524783491,
-46.5412));
#238724=CARTESIAN_POINT('Ctrl Pts',(46.1766977413729,-56.5120019399699,
-46.4828666666667));
#238725=CARTESIAN_POINT('Ctrl Pts',(45.3423250998467,-56.0302766707802,
-46.4245333333334));
#238726=CARTESIAN_POINT('Ctrl Pts',(44.5079524583205,-55.5485514015906,
-46.3662));
#238727=CARTESIAN_POINT('Ctrl Pts',(43.6735798167943,-56.0302766707802,
-46.3078666666667));
#238728=CARTESIAN_POINT('Ctrl Pts',(42.839207175268,-56.5120019399698,-46.2495333333334));
#238729=CARTESIAN_POINT('Ctrl Pts',(42.839207175268,-57.4754524783491,-46.1912));
#238730=CARTESIAN_POINT('Ctrl Pts',(42.839207175268,-57.4754524783491,-47.04995));
#238731=CARTESIAN_POINT('Ctrl Pts',(42.839207175268,-58.4389030167283,-46.9916166666667));
#238732=CARTESIAN_POINT('Ctrl Pts',(43.6735798167943,-58.920628285918,-46.9332833333334));
#238733=CARTESIAN_POINT('Ctrl Pts',(44.5079524583205,-59.4023535551075,
-46.87495));
#238734=CARTESIAN_POINT('Ctrl Pts',(45.3423250998467,-58.920628285918,-46.8166166666667));
#238735=CARTESIAN_POINT('Ctrl Pts',(46.1766977413729,-58.4389030167283,
-46.7582833333333));
#238736=CARTESIAN_POINT('Ctrl Pts',(46.1766977413729,-57.4754524783491,
-46.69995));
#238737=CARTESIAN_POINT('Ctrl Pts',(46.1766977413729,-56.5120019399699,
-46.6416166666666));
#238738=CARTESIAN_POINT('Ctrl Pts',(45.3423250998467,-56.0302766707802,
-46.5832833333334));
#238739=CARTESIAN_POINT('Ctrl Pts',(44.5079524583205,-55.5485514015906,
-46.52495));
#238740=CARTESIAN_POINT('Ctrl Pts',(43.6735798167943,-56.0302766707802,
-46.4666166666667));
#238741=CARTESIAN_POINT('Ctrl Pts',(42.839207175268,-56.5120019399698,-46.4082833333333));
#238742=CARTESIAN_POINT('Ctrl Pts',(42.839207175268,-57.4754524783491,-46.34995));
#238743=CARTESIAN_POINT('Origin',(44.5079524583205,-57.4754524783491,-52.920575));
#238744=CARTESIAN_POINT('',(42.839207175268,-57.4754524783491,-47.74995));
#238745=CARTESIAN_POINT('',(42.839207175268,-57.4754524783491,-47.5912));
#238746=CARTESIAN_POINT('',(42.839207175268,-57.4754524783491,-52.920575));
#238747=CARTESIAN_POINT('Ctrl Pts',(42.839207175268,-57.4754524783491,-47.5912));
#238748=CARTESIAN_POINT('Ctrl Pts',(42.839207175268,-58.4389030167283,-47.5328666666667));
#238749=CARTESIAN_POINT('Ctrl Pts',(43.6735798167943,-58.920628285918,-47.4745333333334));
#238750=CARTESIAN_POINT('Ctrl Pts',(44.5079524583205,-59.4023535551075,
-47.4162));
#238751=CARTESIAN_POINT('Ctrl Pts',(45.3423250998467,-58.920628285918,-47.3578666666667));
#238752=CARTESIAN_POINT('Ctrl Pts',(46.1766977413729,-58.4389030167283,
-47.2995333333334));
#238753=CARTESIAN_POINT('Ctrl Pts',(46.1766977413729,-57.4754524783491,
-47.2412));
#238754=CARTESIAN_POINT('Ctrl Pts',(46.1766977413729,-56.5120019399699,
-47.1828666666667));
#238755=CARTESIAN_POINT('Ctrl Pts',(45.3423250998467,-56.0302766707802,
-47.1245333333333));
#238756=CARTESIAN_POINT('Ctrl Pts',(44.5079524583205,-55.5485514015906,
-47.0662));
#238757=CARTESIAN_POINT('Ctrl Pts',(43.6735798167943,-56.0302766707802,
-47.0078666666667));
#238758=CARTESIAN_POINT('Ctrl Pts',(42.839207175268,-56.5120019399698,-46.9495333333334));
#238759=CARTESIAN_POINT('Ctrl Pts',(42.839207175268,-57.4754524783491,-46.8912));
#238760=CARTESIAN_POINT('Ctrl Pts',(42.839207175268,-57.4754524783491,-47.74995));
#238761=CARTESIAN_POINT('Ctrl Pts',(42.839207175268,-58.4389030167283,-47.6916166666667));
#238762=CARTESIAN_POINT('Ctrl Pts',(43.6735798167943,-58.920628285918,-47.6332833333333));
#238763=CARTESIAN_POINT('Ctrl Pts',(44.5079524583205,-59.4023535551075,
-47.57495));
#238764=CARTESIAN_POINT('Ctrl Pts',(45.3423250998467,-58.920628285918,-47.5166166666667));
#238765=CARTESIAN_POINT('Ctrl Pts',(46.1766977413729,-58.4389030167283,
-47.4582833333333));
#238766=CARTESIAN_POINT('Ctrl Pts',(46.1766977413729,-57.4754524783491,
-47.39995));
#238767=CARTESIAN_POINT('Ctrl Pts',(46.1766977413729,-56.5120019399699,
-47.3416166666667));
#238768=CARTESIAN_POINT('Ctrl Pts',(45.3423250998467,-56.0302766707802,
-47.2832833333333));
#238769=CARTESIAN_POINT('Ctrl Pts',(44.5079524583205,-55.5485514015906,
-47.22495));
#238770=CARTESIAN_POINT('Ctrl Pts',(43.6735798167943,-56.0302766707802,
-47.1666166666667));
#238771=CARTESIAN_POINT('Ctrl Pts',(42.839207175268,-56.5120019399698,-47.1082833333333));
#238772=CARTESIAN_POINT('Ctrl Pts',(42.839207175268,-57.4754524783491,-47.04995));
#238773=CARTESIAN_POINT('Origin',(44.5079524583205,-57.4754524783491,-52.920575));
#238774=CARTESIAN_POINT('',(42.839207175268,-57.4754524783491,-48.44995));
#238775=CARTESIAN_POINT('',(42.839207175268,-57.4754524783491,-48.2912));
#238776=CARTESIAN_POINT('',(42.839207175268,-57.4754524783491,-52.920575));
#238777=CARTESIAN_POINT('Ctrl Pts',(42.839207175268,-57.4754524783491,-48.2912));
#238778=CARTESIAN_POINT('Ctrl Pts',(42.839207175268,-58.4389030167283,-48.2328666666667));
#238779=CARTESIAN_POINT('Ctrl Pts',(43.6735798167943,-58.920628285918,-48.1745333333334));
#238780=CARTESIAN_POINT('Ctrl Pts',(44.5079524583205,-59.4023535551075,
-48.1162));
#238781=CARTESIAN_POINT('Ctrl Pts',(45.3423250998467,-58.920628285918,-48.0578666666667));
#238782=CARTESIAN_POINT('Ctrl Pts',(46.1766977413729,-58.4389030167283,
-47.9995333333334));
#238783=CARTESIAN_POINT('Ctrl Pts',(46.1766977413729,-57.4754524783491,
-47.9412));
#238784=CARTESIAN_POINT('Ctrl Pts',(46.1766977413729,-56.5120019399699,
-47.8828666666667));
#238785=CARTESIAN_POINT('Ctrl Pts',(45.3423250998467,-56.0302766707802,
-47.8245333333333));
#238786=CARTESIAN_POINT('Ctrl Pts',(44.5079524583205,-55.5485514015906,
-47.7662));
#238787=CARTESIAN_POINT('Ctrl Pts',(43.6735798167943,-56.0302766707802,
-47.7078666666667));
#238788=CARTESIAN_POINT('Ctrl Pts',(42.839207175268,-56.5120019399698,-47.6495333333334));
#238789=CARTESIAN_POINT('Ctrl Pts',(42.839207175268,-57.4754524783491,-47.5912));
#238790=CARTESIAN_POINT('Ctrl Pts',(42.839207175268,-57.4754524783491,-48.44995));
#238791=CARTESIAN_POINT('Ctrl Pts',(42.839207175268,-58.4389030167283,-48.3916166666667));
#238792=CARTESIAN_POINT('Ctrl Pts',(43.6735798167943,-58.920628285918,-48.3332833333334));
#238793=CARTESIAN_POINT('Ctrl Pts',(44.5079524583205,-59.4023535551075,
-48.27495));
#238794=CARTESIAN_POINT('Ctrl Pts',(45.3423250998467,-58.920628285918,-48.2166166666667));
#238795=CARTESIAN_POINT('Ctrl Pts',(46.1766977413729,-58.4389030167283,
-48.1582833333334));
#238796=CARTESIAN_POINT('Ctrl Pts',(46.1766977413729,-57.4754524783491,
-48.09995));
#238797=CARTESIAN_POINT('Ctrl Pts',(46.1766977413729,-56.5120019399699,
-48.0416166666667));
#238798=CARTESIAN_POINT('Ctrl Pts',(45.3423250998467,-56.0302766707802,
-47.9832833333334));
#238799=CARTESIAN_POINT('Ctrl Pts',(44.5079524583205,-55.5485514015906,
-47.92495));
#238800=CARTESIAN_POINT('Ctrl Pts',(43.6735798167943,-56.0302766707802,
-47.8666166666667));
#238801=CARTESIAN_POINT('Ctrl Pts',(42.839207175268,-56.5120019399698,-47.8082833333333));
#238802=CARTESIAN_POINT('Ctrl Pts',(42.839207175268,-57.4754524783491,-47.74995));
#238803=CARTESIAN_POINT('Origin',(44.5079524583205,-57.4754524783491,-52.920575));
#238804=CARTESIAN_POINT('',(42.839207175268,-57.4754524783491,-49.14995));
#238805=CARTESIAN_POINT('',(42.839207175268,-57.4754524783491,-48.9912));
#238806=CARTESIAN_POINT('',(42.839207175268,-57.4754524783491,-52.920575));
#238807=CARTESIAN_POINT('Ctrl Pts',(42.839207175268,-57.4754524783491,-48.9912));
#238808=CARTESIAN_POINT('Ctrl Pts',(42.839207175268,-58.4389030167283,-48.9328666666667));
#238809=CARTESIAN_POINT('Ctrl Pts',(43.6735798167943,-58.920628285918,-48.8745333333334));
#238810=CARTESIAN_POINT('Ctrl Pts',(44.5079524583205,-59.4023535551075,
-48.8162));
#238811=CARTESIAN_POINT('Ctrl Pts',(45.3423250998467,-58.920628285918,-48.7578666666667));
#238812=CARTESIAN_POINT('Ctrl Pts',(46.1766977413729,-58.4389030167283,
-48.6995333333333));
#238813=CARTESIAN_POINT('Ctrl Pts',(46.1766977413729,-57.4754524783491,
-48.6412));
#238814=CARTESIAN_POINT('Ctrl Pts',(46.1766977413729,-56.5120019399699,
-48.5828666666667));
#238815=CARTESIAN_POINT('Ctrl Pts',(45.3423250998467,-56.0302766707802,
-48.5245333333334));
#238816=CARTESIAN_POINT('Ctrl Pts',(44.5079524583205,-55.5485514015906,
-48.4662));
#238817=CARTESIAN_POINT('Ctrl Pts',(43.6735798167943,-56.0302766707802,
-48.4078666666667));
#238818=CARTESIAN_POINT('Ctrl Pts',(42.839207175268,-56.5120019399698,-48.3495333333333));
#238819=CARTESIAN_POINT('Ctrl Pts',(42.839207175268,-57.4754524783491,-48.2912));
#238820=CARTESIAN_POINT('Ctrl Pts',(42.839207175268,-57.4754524783491,-49.14995));
#238821=CARTESIAN_POINT('Ctrl Pts',(42.839207175268,-58.4389030167283,-49.0916166666667));
#238822=CARTESIAN_POINT('Ctrl Pts',(43.6735798167943,-58.920628285918,-49.0332833333333));
#238823=CARTESIAN_POINT('Ctrl Pts',(44.5079524583205,-59.4023535551075,
-48.97495));
#238824=CARTESIAN_POINT('Ctrl Pts',(45.3423250998467,-58.920628285918,-48.9166166666667));
#238825=CARTESIAN_POINT('Ctrl Pts',(46.1766977413729,-58.4389030167283,
-48.8582833333333));
#238826=CARTESIAN_POINT('Ctrl Pts',(46.1766977413729,-57.4754524783491,
-48.79995));
#238827=CARTESIAN_POINT('Ctrl Pts',(46.1766977413729,-56.5120019399699,
-48.7416166666667));
#238828=CARTESIAN_POINT('Ctrl Pts',(45.3423250998467,-56.0302766707802,
-48.6832833333334));
#238829=CARTESIAN_POINT('Ctrl Pts',(44.5079524583205,-55.5485514015906,
-48.62495));
#238830=CARTESIAN_POINT('Ctrl Pts',(43.6735798167943,-56.0302766707802,
-48.5666166666667));
#238831=CARTESIAN_POINT('Ctrl Pts',(42.839207175268,-56.5120019399698,-48.5082833333334));
#238832=CARTESIAN_POINT('Ctrl Pts',(42.839207175268,-57.4754524783491,-48.44995));
#238833=CARTESIAN_POINT('Origin',(44.5079524583205,-57.4754524783491,-52.920575));
#238834=CARTESIAN_POINT('',(42.839207175268,-57.4754524783491,-49.84995));
#238835=CARTESIAN_POINT('',(42.839207175268,-57.4754524783491,-49.6912));
#238836=CARTESIAN_POINT('',(42.839207175268,-57.4754524783491,-52.920575));
#238837=CARTESIAN_POINT('Ctrl Pts',(42.839207175268,-57.4754524783491,-49.6912));
#238838=CARTESIAN_POINT('Ctrl Pts',(42.839207175268,-58.4389030167283,-49.6328666666667));
#238839=CARTESIAN_POINT('Ctrl Pts',(43.6735798167943,-58.920628285918,-49.5745333333334));
#238840=CARTESIAN_POINT('Ctrl Pts',(44.5079524583205,-59.4023535551075,
-49.5162));
#238841=CARTESIAN_POINT('Ctrl Pts',(45.3423250998467,-58.920628285918,-49.4578666666667));
#238842=CARTESIAN_POINT('Ctrl Pts',(46.1766977413729,-58.4389030167283,
-49.3995333333333));
#238843=CARTESIAN_POINT('Ctrl Pts',(46.1766977413729,-57.4754524783491,
-49.3412));
#238844=CARTESIAN_POINT('Ctrl Pts',(46.1766977413729,-56.5120019399699,
-49.2828666666667));
#238845=CARTESIAN_POINT('Ctrl Pts',(45.3423250998467,-56.0302766707802,
-49.2245333333334));
#238846=CARTESIAN_POINT('Ctrl Pts',(44.5079524583205,-55.5485514015906,
-49.1662));
#238847=CARTESIAN_POINT('Ctrl Pts',(43.6735798167943,-56.0302766707802,
-49.1078666666667));
#238848=CARTESIAN_POINT('Ctrl Pts',(42.839207175268,-56.5120019399698,-49.0495333333334));
#238849=CARTESIAN_POINT('Ctrl Pts',(42.839207175268,-57.4754524783491,-48.9912));
#238850=CARTESIAN_POINT('Ctrl Pts',(42.839207175268,-57.4754524783491,-49.84995));
#238851=CARTESIAN_POINT('Ctrl Pts',(42.839207175268,-58.4389030167283,-49.7916166666667));
#238852=CARTESIAN_POINT('Ctrl Pts',(43.6735798167943,-58.920628285918,-49.7332833333334));
#238853=CARTESIAN_POINT('Ctrl Pts',(44.5079524583205,-59.4023535551075,
-49.67495));
#238854=CARTESIAN_POINT('Ctrl Pts',(45.3423250998467,-58.920628285918,-49.6166166666667));
#238855=CARTESIAN_POINT('Ctrl Pts',(46.1766977413729,-58.4389030167283,
-49.5582833333334));
#238856=CARTESIAN_POINT('Ctrl Pts',(46.1766977413729,-57.4754524783491,
-49.49995));
#238857=CARTESIAN_POINT('Ctrl Pts',(46.1766977413729,-56.5120019399699,
-49.4416166666667));
#238858=CARTESIAN_POINT('Ctrl Pts',(45.3423250998467,-56.0302766707802,
-49.3832833333334));
#238859=CARTESIAN_POINT('Ctrl Pts',(44.5079524583205,-55.5485514015906,
-49.32495));
#238860=CARTESIAN_POINT('Ctrl Pts',(43.6735798167943,-56.0302766707802,
-49.2666166666667));
#238861=CARTESIAN_POINT('Ctrl Pts',(42.839207175268,-56.5120019399698,-49.2082833333334));
#238862=CARTESIAN_POINT('Ctrl Pts',(42.839207175268,-57.4754524783491,-49.14995));
#238863=CARTESIAN_POINT('Origin',(44.5079524583205,-57.4754524783491,-52.920575));
#238864=CARTESIAN_POINT('',(42.839207175268,-57.4754524783491,-50.54995));
#238865=CARTESIAN_POINT('',(42.839207175268,-57.4754524783491,-50.3912));
#238866=CARTESIAN_POINT('',(42.839207175268,-57.4754524783491,-52.920575));
#238867=CARTESIAN_POINT('Ctrl Pts',(42.839207175268,-57.4754524783491,-50.3912));
#238868=CARTESIAN_POINT('Ctrl Pts',(42.839207175268,-58.4389030167283,-50.3328666666667));
#238869=CARTESIAN_POINT('Ctrl Pts',(43.6735798167943,-58.920628285918,-50.2745333333334));
#238870=CARTESIAN_POINT('Ctrl Pts',(44.5079524583205,-59.4023535551075,
-50.2162));
#238871=CARTESIAN_POINT('Ctrl Pts',(45.3423250998467,-58.920628285918,-50.1578666666667));
#238872=CARTESIAN_POINT('Ctrl Pts',(46.1766977413729,-58.4389030167283,
-50.0995333333333));
#238873=CARTESIAN_POINT('Ctrl Pts',(46.1766977413729,-57.4754524783491,
-50.0412));
#238874=CARTESIAN_POINT('Ctrl Pts',(46.1766977413729,-56.5120019399699,
-49.9828666666667));
#238875=CARTESIAN_POINT('Ctrl Pts',(45.3423250998467,-56.0302766707802,
-49.9245333333334));
#238876=CARTESIAN_POINT('Ctrl Pts',(44.5079524583205,-55.5485514015906,
-49.8662));
#238877=CARTESIAN_POINT('Ctrl Pts',(43.6735798167943,-56.0302766707802,
-49.8078666666667));
#238878=CARTESIAN_POINT('Ctrl Pts',(42.839207175268,-56.5120019399698,-49.7495333333333));
#238879=CARTESIAN_POINT('Ctrl Pts',(42.839207175268,-57.4754524783491,-49.6912));
#238880=CARTESIAN_POINT('Ctrl Pts',(42.839207175268,-57.4754524783491,-50.54995));
#238881=CARTESIAN_POINT('Ctrl Pts',(42.839207175268,-58.4389030167283,-50.4916166666667));
#238882=CARTESIAN_POINT('Ctrl Pts',(43.6735798167943,-58.920628285918,-50.4332833333333));
#238883=CARTESIAN_POINT('Ctrl Pts',(44.5079524583205,-59.4023535551075,
-50.37495));
#238884=CARTESIAN_POINT('Ctrl Pts',(45.3423250998467,-58.920628285918,-50.3166166666667));
#238885=CARTESIAN_POINT('Ctrl Pts',(46.1766977413729,-58.4389030167283,
-50.2582833333334));
#238886=CARTESIAN_POINT('Ctrl Pts',(46.1766977413729,-57.4754524783491,
-50.19995));
#238887=CARTESIAN_POINT('Ctrl Pts',(46.1766977413729,-56.5120019399699,
-50.1416166666667));
#238888=CARTESIAN_POINT('Ctrl Pts',(45.3423250998467,-56.0302766707802,
-50.0832833333334));
#238889=CARTESIAN_POINT('Ctrl Pts',(44.5079524583205,-55.5485514015906,
-50.02495));
#238890=CARTESIAN_POINT('Ctrl Pts',(43.6735798167943,-56.0302766707802,
-49.9666166666667));
#238891=CARTESIAN_POINT('Ctrl Pts',(42.839207175268,-56.5120019399698,-49.9082833333334));
#238892=CARTESIAN_POINT('Ctrl Pts',(42.839207175268,-57.4754524783491,-49.84995));
#238893=CARTESIAN_POINT('Origin',(44.5079524583205,-57.4754524783491,-52.920575));
#238894=CARTESIAN_POINT('',(42.839207175268,-57.4754524783491,-51.24995));
#238895=CARTESIAN_POINT('',(42.839207175268,-57.4754524783491,-51.0912));
#238896=CARTESIAN_POINT('',(42.839207175268,-57.4754524783491,-52.920575));
#238897=CARTESIAN_POINT('Ctrl Pts',(42.839207175268,-57.4754524783491,-51.0912));
#238898=CARTESIAN_POINT('Ctrl Pts',(42.839207175268,-58.4389030167283,-51.0328666666667));
#238899=CARTESIAN_POINT('Ctrl Pts',(43.6735798167943,-58.920628285918,-50.9745333333333));
#238900=CARTESIAN_POINT('Ctrl Pts',(44.5079524583205,-59.4023535551075,
-50.9162));
#238901=CARTESIAN_POINT('Ctrl Pts',(45.3423250998467,-58.920628285918,-50.8578666666667));
#238902=CARTESIAN_POINT('Ctrl Pts',(46.1766977413729,-58.4389030167283,
-50.7995333333334));
#238903=CARTESIAN_POINT('Ctrl Pts',(46.1766977413729,-57.4754524783491,
-50.7412));
#238904=CARTESIAN_POINT('Ctrl Pts',(46.1766977413729,-56.5120019399699,
-50.6828666666667));
#238905=CARTESIAN_POINT('Ctrl Pts',(45.3423250998467,-56.0302766707802,
-50.6245333333333));
#238906=CARTESIAN_POINT('Ctrl Pts',(44.5079524583205,-55.5485514015906,
-50.5662));
#238907=CARTESIAN_POINT('Ctrl Pts',(43.6735798167943,-56.0302766707802,
-50.5078666666667));
#238908=CARTESIAN_POINT('Ctrl Pts',(42.839207175268,-56.5120019399698,-50.4495333333333));
#238909=CARTESIAN_POINT('Ctrl Pts',(42.839207175268,-57.4754524783491,-50.3912));
#238910=CARTESIAN_POINT('Ctrl Pts',(42.839207175268,-57.4754524783491,-51.24995));
#238911=CARTESIAN_POINT('Ctrl Pts',(42.839207175268,-58.4389030167283,-51.1916166666667));
#238912=CARTESIAN_POINT('Ctrl Pts',(43.6735798167943,-58.920628285918,-51.1332833333334));
#238913=CARTESIAN_POINT('Ctrl Pts',(44.5079524583205,-59.4023535551075,
-51.07495));
#238914=CARTESIAN_POINT('Ctrl Pts',(45.3423250998467,-58.920628285918,-51.0166166666667));
#238915=CARTESIAN_POINT('Ctrl Pts',(46.1766977413729,-58.4389030167283,
-50.9582833333334));
#238916=CARTESIAN_POINT('Ctrl Pts',(46.1766977413729,-57.4754524783491,
-50.89995));
#238917=CARTESIAN_POINT('Ctrl Pts',(46.1766977413729,-56.5120019399699,
-50.8416166666667));
#238918=CARTESIAN_POINT('Ctrl Pts',(45.3423250998467,-56.0302766707802,
-50.7832833333333));
#238919=CARTESIAN_POINT('Ctrl Pts',(44.5079524583205,-55.5485514015906,
-50.72495));
#238920=CARTESIAN_POINT('Ctrl Pts',(43.6735798167943,-56.0302766707802,
-50.6666166666667));
#238921=CARTESIAN_POINT('Ctrl Pts',(42.839207175268,-56.5120019399698,-50.6082833333334));
#238922=CARTESIAN_POINT('Ctrl Pts',(42.839207175268,-57.4754524783491,-50.54995));
#238923=CARTESIAN_POINT('Origin',(44.5079524583205,-57.4754524783491,-52.920575));
#238924=CARTESIAN_POINT('',(42.839207175268,-57.4754524783491,-51.94995));
#238925=CARTESIAN_POINT('',(42.839207175268,-57.4754524783491,-51.7912));
#238926=CARTESIAN_POINT('',(42.839207175268,-57.4754524783491,-52.920575));
#238927=CARTESIAN_POINT('Ctrl Pts',(42.839207175268,-57.4754524783491,-51.7912));
#238928=CARTESIAN_POINT('Ctrl Pts',(42.839207175268,-58.4389030167283,-51.7328666666667));
#238929=CARTESIAN_POINT('Ctrl Pts',(43.6735798167943,-58.920628285918,-51.6745333333334));
#238930=CARTESIAN_POINT('Ctrl Pts',(44.5079524583205,-59.4023535551075,
-51.6162));
#238931=CARTESIAN_POINT('Ctrl Pts',(45.3423250998467,-58.920628285918,-51.5578666666667));
#238932=CARTESIAN_POINT('Ctrl Pts',(46.1766977413729,-58.4389030167283,
-51.4995333333334));
#238933=CARTESIAN_POINT('Ctrl Pts',(46.1766977413729,-57.4754524783491,
-51.4412));
#238934=CARTESIAN_POINT('Ctrl Pts',(46.1766977413729,-56.5120019399699,
-51.3828666666667));
#238935=CARTESIAN_POINT('Ctrl Pts',(45.3423250998467,-56.0302766707802,
-51.3245333333334));
#238936=CARTESIAN_POINT('Ctrl Pts',(44.5079524583205,-55.5485514015906,
-51.2662));
#238937=CARTESIAN_POINT('Ctrl Pts',(43.6735798167943,-56.0302766707802,
-51.2078666666667));
#238938=CARTESIAN_POINT('Ctrl Pts',(42.839207175268,-56.5120019399698,-51.1495333333334));
#238939=CARTESIAN_POINT('Ctrl Pts',(42.839207175268,-57.4754524783491,-51.0912));
#238940=CARTESIAN_POINT('Ctrl Pts',(42.839207175268,-57.4754524783491,-51.94995));
#238941=CARTESIAN_POINT('Ctrl Pts',(42.839207175268,-58.4389030167283,-51.8916166666667));
#238942=CARTESIAN_POINT('Ctrl Pts',(43.6735798167943,-58.920628285918,-51.8332833333334));
#238943=CARTESIAN_POINT('Ctrl Pts',(44.5079524583205,-59.4023535551075,
-51.77495));
#238944=CARTESIAN_POINT('Ctrl Pts',(45.3423250998467,-58.920628285918,-51.7166166666667));
#238945=CARTESIAN_POINT('Ctrl Pts',(46.1766977413729,-58.4389030167283,
-51.6582833333333));
#238946=CARTESIAN_POINT('Ctrl Pts',(46.1766977413729,-57.4754524783491,
-51.59995));
#238947=CARTESIAN_POINT('Ctrl Pts',(46.1766977413729,-56.5120019399699,
-51.5416166666667));
#238948=CARTESIAN_POINT('Ctrl Pts',(45.3423250998467,-56.0302766707802,
-51.4832833333334));
#238949=CARTESIAN_POINT('Ctrl Pts',(44.5079524583205,-55.5485514015906,
-51.42495));
#238950=CARTESIAN_POINT('Ctrl Pts',(43.6735798167943,-56.0302766707802,
-51.3666166666667));
#238951=CARTESIAN_POINT('Ctrl Pts',(42.839207175268,-56.5120019399698,-51.3082833333333));
#238952=CARTESIAN_POINT('Ctrl Pts',(42.839207175268,-57.4754524783491,-51.24995));
#238953=CARTESIAN_POINT('Origin',(44.5079524583205,-57.4754524783491,-52.920575));
#238954=CARTESIAN_POINT('',(42.839207175268,-57.4754524783491,-52.64995));
#238955=CARTESIAN_POINT('',(42.839207175268,-57.4754524783491,-52.4912));
#238956=CARTESIAN_POINT('',(42.839207175268,-57.4754524783491,-52.920575));
#238957=CARTESIAN_POINT('',(44.2755200796093,-55.8229737314248,-52.64995));
#238958=CARTESIAN_POINT('Origin',(44.5079524583205,-57.4754524783491,-52.64995));
#238959=CARTESIAN_POINT('Ctrl Pts',(44.2755200796093,-55.8229737314248,
-52.64995));
#238960=CARTESIAN_POINT('Ctrl Pts',(43.9544082597716,-55.8681402936311,
-52.6275001713604));
#238961=CARTESIAN_POINT('Ctrl Pts',(43.6735798167943,-56.0302766707802,
-52.6078666666667));
#238962=CARTESIAN_POINT('Ctrl Pts',(42.839207175268,-56.5120019399698,-52.5495333333333));
#238963=CARTESIAN_POINT('Ctrl Pts',(42.839207175268,-57.4754524783491,-52.4912));
#238964=CARTESIAN_POINT('Origin',(44.5079524583206,-57.475452478349,235.35105));
#238965=CARTESIAN_POINT('',(44.5079524583206,-59.475452478349,-51.9662));
#238966=CARTESIAN_POINT('',(44.5079524583206,-59.475452478349,-52.1249500000001));
#238967=CARTESIAN_POINT('',(44.5079524583206,-59.475452478349,235.35105));
#238968=CARTESIAN_POINT('',(46.5079524583206,-57.4754524783491,-52.64995));
#238969=CARTESIAN_POINT('Ctrl Pts',(44.5079524583206,-59.475452478349,-52.1249500000001));
#238970=CARTESIAN_POINT('Ctrl Pts',(44.4513597608212,-59.475452478349,-52.1282512406875));
#238971=CARTESIAN_POINT('Ctrl Pts',(44.3947006314118,-59.4730504845328,
-52.1315563565699));
#238972=CARTESIAN_POINT('Ctrl Pts',(44.08355625845,-59.4465346697816,-52.1497064449927));
#238973=CARTESIAN_POINT('Ctrl Pts',(43.8354437380825,-59.3762551365555,
-52.1641796753474));
#238974=CARTESIAN_POINT('Ctrl Pts',(43.3705215162246,-59.1417508717089,
-52.1913001382892));
#238975=CARTESIAN_POINT('Ctrl Pts',(43.1598519544925,-58.9764452064066,
-52.2051088910806));
#238976=CARTESIAN_POINT('Ctrl Pts',(42.817179172053,-58.5754701885061,-52.2353600294226));
#238977=CARTESIAN_POINT('Ctrl Pts',(42.6876786575065,-58.3445662146524,
-52.2508019690164));
#238978=CARTESIAN_POINT('Ctrl Pts',(42.5279192111384,-57.8544356169778,
-52.2802221098797));
#238979=CARTESIAN_POINT('Ctrl Pts',(42.4958972035575,-57.6009487460923,
-52.2932585493062));
#238980=CARTESIAN_POINT('Ctrl Pts',(42.5288686707642,-57.0835863192722,
-52.3203564090341));
#238981=CARTESIAN_POINT('Ctrl Pts',(42.5982066316955,-56.8249460940721,
-52.3354447915466));
#238982=CARTESIAN_POINT('Ctrl Pts',(42.831006553102,-56.3551743566381,-52.3659667876725));
#238983=CARTESIAN_POINT('Ctrl Pts',(42.9901454516923,-56.1475015012174,
-52.3810995870422));
#238984=CARTESIAN_POINT('Ctrl Pts',(43.3760066384796,-55.8069348406429,
-52.4095586688083));
#238985=CARTESIAN_POINT('Ctrl Pts',(43.5980966363497,-55.6761710812624,
-52.4218750770519));
#238986=CARTESIAN_POINT('Ctrl Pts',(44.0897941185096,-55.5016056305671,
-52.4505574301779));
#238987=CARTESIAN_POINT('Ctrl Pts',(44.3560328624495,-55.4635321991934,
-52.4660880235743));
#238988=CARTESIAN_POINT('Ctrl Pts',(44.8776436126168,-55.493292462122,-52.4965153173341));
#238989=CARTESIAN_POINT('Ctrl Pts',(45.1282784417565,-55.5568947771729,
-52.5111356823672));
#238990=CARTESIAN_POINT('Ctrl Pts',(45.5977717555248,-55.7780117532505,
-52.538522792337));
#238991=CARTESIAN_POINT('Ctrl Pts',(45.8110667164859,-55.9356674403983,
-52.5518370765746));
#238992=CARTESIAN_POINT('Ctrl Pts',(46.1561721894381,-56.31527754973,-52.5810798527649));
#238993=CARTESIAN_POINT('Ctrl Pts',(46.288274338177,-56.530421203333,-52.5958014911562));
#238994=CARTESIAN_POINT('Ctrl Pts',(46.4636467216999,-56.9914153174137,
-52.6242050881466));
#238995=CARTESIAN_POINT('Ctrl Pts',(46.5079524583206,-57.2323982040817,
-52.6376713480658));
#238996=CARTESIAN_POINT('Ctrl Pts',(46.5079524583206,-57.4754524783491,
-52.6499499999999));
#238997=CARTESIAN_POINT('',(44.7865238868913,-59.4559569492311,-52.64995));
#238998=CARTESIAN_POINT('Origin',(44.5079524583206,-57.4754524783489,-52.64995));
#238999=CARTESIAN_POINT('Ctrl Pts',(44.7865238868906,-59.4559569492312,
-52.6499500000001));
#239000=CARTESIAN_POINT('Ctrl Pts',(44.9389460862256,-59.4345177298612,
-52.6410587050389));
#239001=CARTESIAN_POINT('Ctrl Pts',(45.0883897049096,-59.3955549779547,
-52.6323411606156));
#239002=CARTESIAN_POINT('Ctrl Pts',(45.3702837264581,-59.2860937769035,
-52.615897342692));
#239003=CARTESIAN_POINT('Ctrl Pts',(45.5021972948078,-59.217147964577,-52.6085217569117));
#239004=CARTESIAN_POINT('Ctrl Pts',(45.8375272388861,-58.9912737652174,
-52.5873305538517));
#239005=CARTESIAN_POINT('Ctrl Pts',(46.0203348377673,-58.8089227056349,
-52.572786627634));
#239006=CARTESIAN_POINT('Ctrl Pts',(46.3129166430222,-58.3770018942788,
-52.5424331519357));
#239007=CARTESIAN_POINT('Ctrl Pts',(46.4166592650751,-58.1293237884958,
-52.5268950861176));
#239008=CARTESIAN_POINT('Ctrl Pts',(46.5192669221118,-57.6175272330474,
-52.4980473483698));
#239009=CARTESIAN_POINT('Ctrl Pts',(46.5209222271569,-57.3591646298644,
-52.4857036381197));
#239010=CARTESIAN_POINT('Ctrl Pts',(46.4261832933532,-56.8530458580145,
-52.4573722359148));
#239011=CARTESIAN_POINT('Ctrl Pts',(46.3296214606361,-56.6102946503741,
-52.442292507558));
#239012=CARTESIAN_POINT('Ctrl Pts',(46.0459745854273,-56.1697773429461,
-52.4117653549204));
#239013=CARTESIAN_POINT('Ctrl Pts',(45.8595052204716,-55.9775718101498,
-52.3966167974505));
#239014=CARTESIAN_POINT('Ctrl Pts',(45.4322675281872,-55.6838697728091,
-52.3693184149391));
#239015=CARTESIAN_POINT('Ctrl Pts',(45.198236150389,-55.5813380716029,-52.3564665487041));
#239016=CARTESIAN_POINT('Ctrl Pts',(44.69592853734,-55.4671660403481,-52.3271652712762));
#239017=CARTESIAN_POINT('Ctrl Pts',(44.4316978233376,-55.4598310010966,
-52.3117518129594));
#239018=CARTESIAN_POINT('Ctrl Pts',(43.9107199000999,-55.5481767987879,
-52.2813614341039));
#239019=CARTESIAN_POINT('Ctrl Pts',(43.6594962686467,-55.6448427549355,
-52.2672657084199));
#239020=CARTESIAN_POINT('Ctrl Pts',(43.2192767418188,-55.9248207668429,
-52.2402820014233));
#239021=CARTESIAN_POINT('Ctrl Pts',(43.032146377683,-56.1017360044494,-52.2258866022144));
#239022=CARTESIAN_POINT('Ctrl Pts',(42.7287064066549,-56.5243603120291,
-52.1956860721732));
#239023=CARTESIAN_POINT('Ctrl Pts',(42.6184234279488,-56.7683526193353,
-52.1801434456677));
#239024=CARTESIAN_POINT('Ctrl Pts',(42.501183061899,-57.2776111785268,-52.1509971354455));
#239025=CARTESIAN_POINT('Ctrl Pts',(42.492401597098,-57.5372091531185,-52.1385337339152));
#239026=CARTESIAN_POINT('Ctrl Pts',(42.5738454144996,-58.0463118080004,
-52.1104393656924));
#239027=CARTESIAN_POINT('Ctrl Pts',(42.6635991909277,-58.2909179537301,
-52.095464497606));
#239028=CARTESIAN_POINT('Ctrl Pts',(42.9347253230964,-58.7384946609519,
-52.0649459054996));
#239029=CARTESIAN_POINT('Ctrl Pts',(43.1158831362097,-58.9357605337373,
-52.0496966292845));
#239030=CARTESIAN_POINT('Ctrl Pts',(43.5351370959696,-59.241203804816,-52.0220379602483));
#239031=CARTESIAN_POINT('Ctrl Pts',(43.7664919850463,-59.3501535032036,
-52.0094518609408));
#239032=CARTESIAN_POINT('Ctrl Pts',(44.1744699518852,-59.4545645545293,
-51.9856531462085));
#239033=CARTESIAN_POINT('Ctrl Pts',(44.3410712893685,-59.475452478349,-51.9759347348555));
#239034=CARTESIAN_POINT('Ctrl Pts',(44.5079524583206,-59.475452478349,-51.9662));
#239035=CARTESIAN_POINT('Origin',(44.5079524583206,-57.475452478349,235.35105));
#239036=CARTESIAN_POINT('',(44.5079524583206,-59.475452478349,-51.2662));
#239037=CARTESIAN_POINT('',(44.5079524583206,-59.475452478349,-51.4249500000001));
#239038=CARTESIAN_POINT('',(44.5079524583206,-59.475452478349,235.35105));
#239039=CARTESIAN_POINT('Ctrl Pts',(44.5079524583206,-59.475452478349,-51.4249500000001));
#239040=CARTESIAN_POINT('Ctrl Pts',(44.4125121220936,-59.475452478349,-51.4305173529467));
#239041=CARTESIAN_POINT('Ctrl Pts',(44.3169826779063,-59.4686210091442,
-51.4360899038576));
#239042=CARTESIAN_POINT('Ctrl Pts',(43.9706471848928,-59.4186073047783,
-51.4562928076168));
#239043=CARTESIAN_POINT('Ctrl Pts',(43.7283528405609,-59.3347051059968,
-51.4704266443695));
#239044=CARTESIAN_POINT('Ctrl Pts',(43.2787639257411,-59.0752295338068,
-51.4966526644006));
#239045=CARTESIAN_POINT('Ctrl Pts',(43.0777780687277,-58.8984478296677,
-51.5114429958136));
#239046=CARTESIAN_POINT('Ctrl Pts',(42.759033675885,-58.4800868047618,-51.541874531677));
#239047=CARTESIAN_POINT('Ctrl Pts',(42.6430709224838,-58.2437201427654,
-51.5571975847951));
#239048=CARTESIAN_POINT('Ctrl Pts',(42.5102536931264,-57.7466673953907,
-51.5861816051825));
#239049=CARTESIAN_POINT('Ctrl Pts',(42.4919941938421,-57.4914112410099,
-51.5986783434767));
#239050=CARTESIAN_POINT('Ctrl Pts',(42.5532078057466,-56.9761171215888,
-51.6264954453646));
#239051=CARTESIAN_POINT('Ctrl Pts',(42.6365867942621,-56.7215841050276,
-51.6417858692722));
#239052=CARTESIAN_POINT('Ctrl Pts',(42.8940849597355,-56.2663628040766,
-51.6722931697382));
#239053=CARTESIAN_POINT('Ctrl Pts',(43.0632307042696,-56.0685855867604,
-51.6872179261321));
#239054=CARTESIAN_POINT('Ctrl Pts',(43.4675083927591,-55.7480011186832,
-51.7152046924955));
#239055=CARTESIAN_POINT('Ctrl Pts',(43.6988294193687,-55.6283087693928,
-51.7277511560613));
#239056=CARTESIAN_POINT('Ctrl Pts',(44.2007382506901,-55.481523908706,-51.7570291712216));
#239057=CARTESIAN_POINT('Ctrl Pts',(44.4671516575844,-55.4584121001176,
-51.7725699532905));
#239058=CARTESIAN_POINT('Ctrl Pts',(44.9835717875786,-55.5161840363474,
-51.8026944608734));
#239059=CARTESIAN_POINT('Ctrl Pts',(45.2291480546249,-55.592670444065,-51.8170197431178));
#239060=CARTESIAN_POINT('Ctrl Pts',(45.6896505047163,-55.8398316248472,
-51.8438823860397));
#239061=CARTESIAN_POINT('Ctrl Pts',(45.8977889023861,-56.0125434124774,
-51.8582501054411));
#239062=CARTESIAN_POINT('Ctrl Pts',(46.2297443679366,-56.4248361486605,
-51.8887604055473));
#239063=CARTESIAN_POINT('Ctrl Pts',(46.3522042551334,-56.6586879284254,
-51.904145911207));
#239064=CARTESIAN_POINT('Ctrl Pts',(46.497899504113,-57.1524868272325,-51.9333411620947));
#239065=CARTESIAN_POINT('Ctrl Pts',(46.522763526501,-57.4068532858747,-51.9460525063153));
#239066=CARTESIAN_POINT('Ctrl Pts',(46.4751481959428,-57.9232136644451,
-51.973526857102));
#239067=CARTESIAN_POINT('Ctrl Pts',(46.3985005787866,-58.1798226132569,
-51.9887258215988));
#239068=CARTESIAN_POINT('Ctrl Pts',(46.1527842050746,-58.6422140890608,
-52.0192517104303));
#239069=CARTESIAN_POINT('Ctrl Pts',(45.9883831911795,-58.8448152691331,
-52.0342817765143));
#239070=CARTESIAN_POINT('Ctrl Pts',(45.5929487775531,-59.1750614020357,
-52.0624987034466));
#239071=CARTESIAN_POINT('Ctrl Pts',(45.3661383698148,-59.3001188717699,
-52.074889155163));
#239072=CARTESIAN_POINT('Ctrl Pts',(44.923153957511,-59.4429862119282,-52.1007299125474));
#239073=CARTESIAN_POINT('Ctrl Pts',(44.7160021186349,-59.475452478349,-52.1128137698151));
#239074=CARTESIAN_POINT('Ctrl Pts',(44.5079524583206,-59.475452478349,-52.1249500000001));
#239075=CARTESIAN_POINT('Ctrl Pts',(44.5079524583206,-59.475452478349,-51.9662));
#239076=CARTESIAN_POINT('Ctrl Pts',(44.6010399043629,-59.475452478349,-51.9607698989808));
#239077=CARTESIAN_POINT('Ctrl Pts',(44.6942144195173,-59.4689536852591,
-51.95533471893));
#239078=CARTESIAN_POINT('Ctrl Pts',(45.0493950081076,-59.4189460111751,
-51.9346158512622));
#239079=CARTESIAN_POINT('Ctrl Pts',(45.3019367943206,-59.3301253082591,
-51.9200700944071));
#239080=CARTESIAN_POINT('Ctrl Pts',(45.7484928539025,-59.064733753287,-51.8936384526703));
#239081=CARTESIAN_POINT('Ctrl Pts',(45.9403960211653,-58.8941892509691,
-51.8794256844553));
#239082=CARTESIAN_POINT('Ctrl Pts',(46.255965041182,-58.4825757154018,-51.8494276343015));
#239083=CARTESIAN_POINT('Ctrl Pts',(46.3736136173997,-58.2430235310882,
-51.8338944846615));
#239084=CARTESIAN_POINT('Ctrl Pts',(46.5076698892025,-57.7368972946749,
-51.804415949669));
#239085=CARTESIAN_POINT('Ctrl Pts',(46.5246850365527,-57.4758015300995,
-51.7917056669799));
#239086=CARTESIAN_POINT('Ctrl Pts',(46.4583579434643,-56.9634209222726,
-51.7638866071024));
#239087=CARTESIAN_POINT('Ctrl Pts',(46.3763441180367,-56.7169416968142,
-51.7490428630669));
#239088=CARTESIAN_POINT('Ctrl Pts',(46.118436752915,-56.2597477670313,-51.7184239740547));
#239089=CARTESIAN_POINT('Ctrl Pts',(45.9415108526329,-56.0554026569323,
-51.7029404986682));
#239090=CARTESIAN_POINT('Ctrl Pts',(45.5285249192671,-55.7367954676129,
-51.6747996302913));
#239091=CARTESIAN_POINT('Ctrl Pts',(45.2997732220664,-55.6213955602625,
-51.6623895445518));
#239092=CARTESIAN_POINT('Ctrl Pts',(44.8050242006444,-55.4805673939303,
-51.6335291849689));
#239093=CARTESIAN_POINT('Ctrl Pts',(44.5430377637212,-55.458877813189,-51.618246642815));
#239094=CARTESIAN_POINT('Ctrl Pts',(44.0209071528755,-55.5176399327209,
-51.5877890238489));
#239095=CARTESIAN_POINT('Ctrl Pts',(43.7659873176074,-55.5993442682777,
-51.572918700125));
#239096=CARTESIAN_POINT('Ctrl Pts',(43.3127992584962,-55.8518887331076,
-51.5464827300101));
#239097=CARTESIAN_POINT('Ctrl Pts',(43.1166320578916,-56.0164558665738,
-51.5326589625609));
#239098=CARTESIAN_POINT('Ctrl Pts',(42.7901543316252,-56.4178094217715,
-51.5028610570206));
#239099=CARTESIAN_POINT('Ctrl Pts',(42.6658936469586,-56.6530990885663,
-51.4873503887108));
#239100=CARTESIAN_POINT('Ctrl Pts',(42.5163972629145,-57.156136564909,-51.4575775555513));
#239101=CARTESIAN_POINT('Ctrl Pts',(42.491766179016,-57.4186699581944,-51.4445406476013));
#239102=CARTESIAN_POINT('Ctrl Pts',(42.5443566356938,-57.9339246682677,
-51.4169770452948));
#239103=CARTESIAN_POINT('Ctrl Pts',(42.6193506557171,-58.1818892358007,
-51.402263008852));
#239104=CARTESIAN_POINT('Ctrl Pts',(42.8636498665352,-58.6448327446183,
-51.3717505662526));
#239105=CARTESIAN_POINT('Ctrl Pts',(43.0341453932076,-58.8535317255553,
-51.3562346939359));
#239106=CARTESIAN_POINT('Ctrl Pts',(43.4376533039693,-59.1840656215097,
-51.3277677527474));
#239107=CARTESIAN_POINT('Ctrl Pts',(43.6637183498251,-59.3063463516232,
-51.3154469896621));
#239108=CARTESIAN_POINT('Ctrl Pts',(44.1015387374648,-59.4443516292416,
-51.2899074670498));
#239109=CARTESIAN_POINT('Ctrl Pts',(44.3043239750094,-59.475452478349,-51.2780783281931));
#239110=CARTESIAN_POINT('Ctrl Pts',(44.5079524583206,-59.475452478349,-51.2662));
#239111=CARTESIAN_POINT('Origin',(44.5079524583206,-57.475452478349,235.35105));
#239112=CARTESIAN_POINT('',(44.5079524583206,-59.475452478349,-50.5661999999999));
#239113=CARTESIAN_POINT('',(44.5079524583206,-59.475452478349,-50.7249500000001));
#239114=CARTESIAN_POINT('',(44.5079524583206,-59.475452478349,235.35105));
#239115=CARTESIAN_POINT('Ctrl Pts',(44.5079524583206,-59.475452478349,-50.7249500000001));
#239116=CARTESIAN_POINT('Ctrl Pts',(44.3732303097234,-59.475452478349,-50.7328087920016));
#239117=CARTESIAN_POINT('Ctrl Pts',(44.2385286748256,-59.4618398691135,
-50.7406663873707));
#239118=CARTESIAN_POINT('Ctrl Pts',(43.8577756421695,-59.3837085760508,
-50.7628769809423));
#239119=CARTESIAN_POINT('Ctrl Pts',(43.6216198460632,-59.2861254963707,
-50.775996186017));
#239120=CARTESIAN_POINT('Ctrl Pts',(43.1883124452698,-59.0015185944403,
-50.8030121322914));
#239121=CARTESIAN_POINT('Ctrl Pts',(42.9978490958847,-58.8133128673102,
-50.818075118197));
#239122=CARTESIAN_POINT('Ctrl Pts',(42.7046785832125,-58.37847689791,-50.8485930329154));
#239123=CARTESIAN_POINT('Ctrl Pts',(42.6028931943792,-58.1372827567734,
-50.8637464548754));
#239124=CARTESIAN_POINT('Ctrl Pts',(42.4979397582136,-57.6335177550656,
-50.8922568719562));
#239125=CARTESIAN_POINT('Ctrl Pts',(42.4941863971064,-57.3760557321509,
-50.9045698294716));
#239126=CARTESIAN_POINT('Ctrl Pts',(42.5856552766182,-56.8624355105712,
-50.9331848144449));
#239127=CARTESIAN_POINT('Ctrl Pts',(42.6843423686,-56.6120658856088,-50.9487113978683));
#239128=CARTESIAN_POINT('Ctrl Pts',(42.9684772538217,-56.173253814368,-50.9791666387562));
#239129=CARTESIAN_POINT('Ctrl Pts',(43.1478916112811,-55.9868366474121,
-50.9938170076487));
#239130=CARTESIAN_POINT('Ctrl Pts',(43.5721456417778,-55.6885491944948,
-51.0212600133965));
#239131=CARTESIAN_POINT('Ctrl Pts',(43.8142157450224,-55.581378245293,-51.0344820250577));
#239132=CARTESIAN_POINT('Ctrl Pts',(44.3269083595648,-55.4663537302885,
-51.0643890942393));
#239133=CARTESIAN_POINT('Ctrl Pts',(44.5925476488824,-55.4599886933024,
-51.0798847194495));
#239134=CARTESIAN_POINT('Ctrl Pts',(45.1016271919251,-55.5488304120265,
-51.109581026127));
#239135=CARTESIAN_POINT('Ctrl Pts',(45.3408222305017,-55.6395404222803,
-51.123161823708));
#239136=CARTESIAN_POINT('Ctrl Pts',(45.7824273092984,-55.911477008505,-51.1497797046997));
#239137=CARTESIAN_POINT('Ctrl Pts',(45.9782761977746,-56.0940024364279,
-51.1647128106296));
#239138=CARTESIAN_POINT('Ctrl Pts',(46.2844488827478,-56.520626893157,-51.1951951249564));
#239139=CARTESIAN_POINT('Ctrl Pts',(46.3934319368649,-56.7594815185977,
-51.210440290819));
#239140=CARTESIAN_POINT('Ctrl Pts',(46.5124987741093,-57.2599016385867,
-51.2391933715331));
#239141=CARTESIAN_POINT('Ctrl Pts',(46.523640990306,-57.5161983286478,-51.2515508227354));
#239142=CARTESIAN_POINT('Ctrl Pts',(46.4474139510621,-58.0321656305446,
-51.2798398241863));
#239143=CARTESIAN_POINT('Ctrl Pts',(46.3557443156348,-58.2860537421219,
-51.2953394792231));
#239144=CARTESIAN_POINT('Ctrl Pts',(46.0834084997015,-58.7340244154266,
-51.3259132562097));
#239145=CARTESIAN_POINT('Ctrl Pts',(45.9087756930046,-58.9258982429212,
-51.3406998235928));
#239146=CARTESIAN_POINT('Ctrl Pts',(45.4939813497915,-59.2348269490163,
-51.3684044982037));
#239147=CARTESIAN_POINT('Ctrl Pts',(45.2570989143405,-59.3480036986934,
-51.3812497900656));
#239148=CARTESIAN_POINT('Ctrl Pts',(44.8423276786983,-59.4544534084242,
-51.4054447788114));
#239149=CARTESIAN_POINT('Ctrl Pts',(44.6752770121716,-59.475452478349,-51.4151894010254));
#239150=CARTESIAN_POINT('Ctrl Pts',(44.5079524583206,-59.475452478349,-51.4249500000001));
#239151=CARTESIAN_POINT('Ctrl Pts',(44.5079524583206,-59.475452478349,-51.2662));
#239152=CARTESIAN_POINT('Ctrl Pts',(44.5631734525969,-59.475452478349,-51.2629787753339));
#239153=CARTESIAN_POINT('Ctrl Pts',(44.6184564602758,-59.4731655085845,
-51.2597539332191));
#239154=CARTESIAN_POINT('Ctrl Pts',(44.9378351352537,-59.446612498114,-51.2411235105121));
#239155=CARTESIAN_POINT('Ctrl Pts',(45.1950710343904,-59.3723409740258,
-51.2261180830625));
#239156=CARTESIAN_POINT('Ctrl Pts',(45.6551086957666,-59.1332196616792,
-51.1992825528155));
#239157=CARTESIAN_POINT('Ctrl Pts',(45.8556719818888,-58.9747430339204,
-51.1859662302413));
#239158=CARTESIAN_POINT('Ctrl Pts',(46.1931091254407,-58.5841781606304,
-51.1563936992655));
#239159=CARTESIAN_POINT('Ctrl Pts',(46.3240269851495,-58.3534617183551,
-51.1409198941859));
#239160=CARTESIAN_POINT('Ctrl Pts',(46.489441262139,-57.8538322926681,-51.1108549575582));
#239161=CARTESIAN_POINT('Ctrl Pts',(46.5219935519418,-57.5897667474203,
-51.097384477124));
#239162=CARTESIAN_POINT('Ctrl Pts',(46.4834312978279,-57.071679273164,-51.0700869247239));
#239163=CARTESIAN_POINT('Ctrl Pts',(46.4155803416157,-56.8224088306493,
-51.055515257256));
#239164=CARTESIAN_POINT('Ctrl Pts',(46.1852071369206,-56.3540332941882,
-51.0251345738557));
#239165=CARTESIAN_POINT('Ctrl Pts',(46.0213365265818,-56.1411151227246,
-51.0095987825716));
#239166=CARTESIAN_POINT('Ctrl Pts',(45.6275782266816,-55.7985834749711,
-50.9808101008255));
#239167=CARTESIAN_POINT('Ctrl Pts',(45.404166960123,-55.6692822412727,-50.9684791792718));
#239168=CARTESIAN_POINT('Ctrl Pts',(44.9177003933257,-55.5008196290297,
-50.9401019628753));
#239169=CARTESIAN_POINT('Ctrl Pts',(44.6588591761761,-55.4644147596997,
-50.9250028918749));
#239170=CARTESIAN_POINT('Ctrl Pts',(44.1355544264234,-55.4926223906537,
-50.8944767814726));
#239171=CARTESIAN_POINT('Ctrl Pts',(43.8762269335403,-55.5593990126897,
-50.8793493443878));
#239172=CARTESIAN_POINT('Ctrl Pts',(43.4094799788231,-55.7850452420739,
-50.8521224386959));
#239173=CARTESIAN_POINT('Ctrl Pts',(43.2044916462832,-55.9375494374975,
-50.839207740595));
#239174=CARTESIAN_POINT('Ctrl Pts',(42.8564006042176,-56.3174372521513,
-50.8098638561468));
#239175=CARTESIAN_POINT('Ctrl Pts',(42.7190873096172,-56.5434758284824,
-50.7944398346762));
#239176=CARTESIAN_POINT('Ctrl Pts',(42.537984808442,-57.0395134538714,-50.7640987759441));
#239177=CARTESIAN_POINT('Ctrl Pts',(42.4975442940095,-57.3051259012254,
-50.7501081547847));
#239178=CARTESIAN_POINT('Ctrl Pts',(42.5224030777523,-57.8258803250107,
-50.7230755575846));
#239179=CARTESIAN_POINT('Ctrl Pts',(42.5833128086047,-58.0762232854203,
-50.7086521609046));
#239180=CARTESIAN_POINT('Ctrl Pts',(42.8000779364503,-58.5494773740377,
-50.6784219243232));
#239181=CARTESIAN_POINT('Ctrl Pts',(42.9574327018484,-58.7662939090198,
-50.6628792404092));
#239182=CARTESIAN_POINT('Ctrl Pts',(43.3416010318863,-59.1203694379146,
-50.633787090615));
#239183=CARTESIAN_POINT('Ctrl Pts',(43.5624832180562,-59.2565226192977,
-50.6213523723485));
#239184=CARTESIAN_POINT('Ctrl Pts',(44.0285820716791,-59.4320414521156,
-50.5941632725539));
#239185=CARTESIAN_POINT('Ctrl Pts',(44.2673731131723,-59.475452478349,-50.5802337951336));
#239186=CARTESIAN_POINT('Ctrl Pts',(44.5079524583206,-59.475452478349,-50.5661999999999));
#239187=CARTESIAN_POINT('Origin',(44.5079524583206,-57.475452478349,235.35105));
#239188=CARTESIAN_POINT('',(44.5079524583206,-59.475452478349,-49.8662));
#239189=CARTESIAN_POINT('',(44.5079524583206,-59.475452478349,-50.02495));
#239190=CARTESIAN_POINT('',(44.5079524583206,-59.475452478349,235.35105));
#239191=CARTESIAN_POINT('Ctrl Pts',(44.5079524583206,-59.475452478349,-50.02495));
#239192=CARTESIAN_POINT('Ctrl Pts',(44.3365369173601,-59.475452478349,-50.0349492398894));
#239193=CARTESIAN_POINT('Ctrl Pts',(44.165453694393,-59.4534139082329,-50.0449290945625));
#239194=CARTESIAN_POINT('Ctrl Pts',(43.7537132796872,-59.3450617430205,
-50.0689472854204));
#239195=CARTESIAN_POINT('Ctrl Pts',(43.5230214878811,-59.2344889054372,
-50.0814805564355));
#239196=CARTESIAN_POINT('Ctrl Pts',(43.1058057632521,-58.9260884222208,
-50.1092291698292));
#239197=CARTESIAN_POINT('Ctrl Pts',(42.9260130342561,-58.7275672179406,
-50.1245020481139));
#239198=CARTESIAN_POINT('Ctrl Pts',(42.6580795457638,-58.2782626921982,
-50.1550148076391));
#239199=CARTESIAN_POINT('Ctrl Pts',(42.5700513130442,-58.0332173811712,
-50.169961533185));
#239200=CARTESIAN_POINT('Ctrl Pts',(42.4919764703888,-57.5233736810765,
-50.1979950758765));
#239201=CARTESIAN_POINT('Ctrl Pts',(42.5025803167883,-57.2634501512911,
-50.2105032775909));
#239202=CARTESIAN_POINT('Ctrl Pts',(42.623552088484,-56.7548663782633,-50.23972433153));
#239203=CARTESIAN_POINT('Ctrl Pts',(42.7354837407372,-56.5118407088338,
-50.2552662115914));
#239204=CARTESIAN_POINT('Ctrl Pts',(43.0416479502191,-56.0916300652184,
-50.2854242647528));
#239205=CARTESIAN_POINT('Ctrl Pts',(43.2298556124923,-55.9161173897087,
-50.2997802303169));
#239206=CARTESIAN_POINT('Ctrl Pts',(43.6723837433044,-55.6388246208237,
-50.3266956180905));
#239207=CARTESIAN_POINT('Ctrl Pts',(43.9249719861093,-55.5437209148654,
-50.3409428057877));
#239208=CARTESIAN_POINT('Ctrl Pts',(44.4471166845182,-55.45933233961,-50.3714012465282));
#239209=CARTESIAN_POINT('Ctrl Pts',(44.7110823320703,-55.4686675746012,
-50.3867992426354));
#239210=CARTESIAN_POINT('Ctrl Pts',(45.212365768875,-55.5865430738959,-50.416040776449));
#239211=CARTESIAN_POINT('Ctrl Pts',(45.4456545898622,-55.6908343352178,
-50.4288107077029));
#239212=CARTESIAN_POINT('Ctrl Pts',(45.8707157277807,-55.987762283461,-50.4562085744247));
#239213=CARTESIAN_POINT('Ctrl Pts',(46.055743094387,-56.1813700172138,-50.4713859102056));
#239214=CARTESIAN_POINT('Ctrl Pts',(46.3359749373623,-56.6238582150205,
-50.5019130234693));
#239215=CARTESIAN_POINT('Ctrl Pts',(46.4306733023535,-56.8671366434277,
-50.5169650349012));
#239216=CARTESIAN_POINT('Ctrl Pts',(46.5217720057947,-57.3740819004816,
-50.5452320162229));
#239217=CARTESIAN_POINT('Ctrl Pts',(46.5181755725226,-57.6327747083439,
-50.5575994536215));
#239218=CARTESIAN_POINT('Ctrl Pts',(46.4115762574803,-58.1438957866815,
-50.5865294908748));
#239219=CARTESIAN_POINT('Ctrl Pts',(46.3060378820656,-58.3905851910932,
-50.6020699854699));
#239220=CARTESIAN_POINT('Ctrl Pts',(46.010466834972,-58.8199970849343,-50.6323839015208));
#239221=CARTESIAN_POINT('Ctrl Pts',(45.8264646834458,-59.0008757128014,
-50.6468882843332));
#239222=CARTESIAN_POINT('Ctrl Pts',(45.3928328266298,-59.2884630472197,
-50.6740642598394));
#239223=CARTESIAN_POINT('Ctrl Pts',(45.1454464338896,-59.3895244960639,
-50.6877628514252));
#239224=CARTESIAN_POINT('Ctrl Pts',(44.7607754026071,-59.463469340792,-50.7102019949167));
#239225=CARTESIAN_POINT('Ctrl Pts',(44.6343549013126,-59.475452478349,-50.7175765241589));
#239226=CARTESIAN_POINT('Ctrl Pts',(44.5079524583206,-59.475452478349,-50.7249500000001));
#239227=CARTESIAN_POINT('Ctrl Pts',(44.5079524583206,-59.475452478349,-50.5661999999999));
#239228=CARTESIAN_POINT('Ctrl Pts',(44.525311884392,-59.475452478349,-50.5651873668124));
#239229=CARTESIAN_POINT('Ctrl Pts',(44.5426806214417,-59.475226466934,-50.5641741904845));
#239230=CARTESIAN_POINT('Ctrl Pts',(44.8251356375188,-59.4678657513322,
-50.54769764788));
#239231=CARTESIAN_POINT('Ctrl Pts',(45.0862516346071,-59.4083063571444,
-50.5324658813832));
#239232=CARTESIAN_POINT('Ctrl Pts',(45.5592819807103,-59.1956042615348,
-50.5048724445272));
#239233=CARTESIAN_POINT('Ctrl Pts',(45.7685389612303,-59.0487165462796,
-50.492244614897));
#239234=CARTESIAN_POINT('Ctrl Pts',(46.1265531213234,-58.678938656933,-50.4631220408816));
#239235=CARTESIAN_POINT('Ctrl Pts',(46.2697412585774,-58.4574600281666,
-50.4477570299421));
#239236=CARTESIAN_POINT('Ctrl Pts',(46.4643314628618,-57.9683157718007,
-50.4173708201097));
#239237=CARTESIAN_POINT('Ctrl Pts',(46.5123410384248,-57.7049341357576,
-50.4029209887124));
#239238=CARTESIAN_POINT('Ctrl Pts',(46.5031187675918,-57.1853964236243,
-50.3764059224922));
#239239=CARTESIAN_POINT('Ctrl Pts',(46.4500350089897,-56.9340744031033,
-50.362161323032));
#239240=CARTESIAN_POINT('Ctrl Pts',(46.2487011790163,-56.4557885441269,
-50.3321269702494));
#239241=CARTESIAN_POINT('Ctrl Pts',(46.098784427892,-56.2348127537926,-50.3165911105387));
#239242=CARTESIAN_POINT('Ctrl Pts',(45.7255955579612,-55.8678474518023,
-50.2871680275256));
#239243=CARTESIAN_POINT('Ctrl Pts',(45.5075123815212,-55.7239053571838,
-50.2745076621868));
#239244=CARTESIAN_POINT('Ctrl Pts',(45.0298108081354,-55.5276363640678,
-50.2466417370726));
#239245=CARTESIAN_POINT('Ctrl Pts',(44.774952613007,-55.47670198901,-50.2317750090234));
#239246=CARTESIAN_POINT('Ctrl Pts',(44.24976174175,-55.4741995360601,-50.2011388748668));
#239247=CARTESIAN_POINT('Ctrl Pts',(43.9844582170926,-55.5266928550564,
-50.1856628359284));
#239248=CARTESIAN_POINT('Ctrl Pts',(43.5031011930694,-55.727679343834,-50.1575836761937));
#239249=CARTESIAN_POINT('Ctrl Pts',(43.2896387143397,-55.8691645288258,
-50.1451458757219));
#239250=CARTESIAN_POINT('Ctrl Pts',(42.9221793307712,-56.2291728948758,
-50.1162413542509));
#239251=CARTESIAN_POINT('Ctrl Pts',(42.7734849989007,-56.4461328238379,
-50.1009440223164));
#239252=CARTESIAN_POINT('Ctrl Pts',(42.5658980022833,-56.9289527302484,
-50.0704982338248));
#239253=CARTESIAN_POINT('Ctrl Pts',(42.5106289671819,-57.1908680016921,
-50.0556547457096));
#239254=CARTESIAN_POINT('Ctrl Pts',(42.5055760603303,-57.7097431108916,
-50.0292947594122));
#239255=CARTESIAN_POINT('Ctrl Pts',(42.5514272695259,-57.9617785134588,
-50.0153636937856));
#239256=CARTESIAN_POINT('Ctrl Pts',(42.7385849251039,-58.4443986727495,
-49.9855238519291));
#239257=CARTESIAN_POINT('Ctrl Pts',(42.8815947303821,-58.6689709161487,
-49.9700077586553));
#239258=CARTESIAN_POINT('Ctrl Pts',(43.2445353236585,-59.0476544253552,
-49.9402916015783));
#239259=CARTESIAN_POINT('Ctrl Pts',(43.4600800296516,-59.1988167030237,
-49.9273258916723));
#239260=CARTESIAN_POINT('Ctrl Pts',(43.9334581156285,-59.4083078449751,
-49.8997121699903));
#239261=CARTESIAN_POINT('Ctrl Pts',(44.1861447161658,-59.4660248765132,
-49.8849721182923));
#239262=CARTESIAN_POINT('Ctrl Pts',(44.4645221691663,-59.4750990564982,
-49.8687334335339));
#239263=CARTESIAN_POINT('Ctrl Pts',(44.4862445813218,-59.475452478349,-49.8674662928249));
#239264=CARTESIAN_POINT('Ctrl Pts',(44.5079524583206,-59.475452478349,-49.8662));
#239265=CARTESIAN_POINT('Origin',(44.5079524583206,-57.475452478349,235.35105));
#239266=CARTESIAN_POINT('',(44.5079524583206,-59.475452478349,-49.1662));
#239267=CARTESIAN_POINT('',(44.5079524583206,-59.475452478349,-49.3249500000001));
#239268=CARTESIAN_POINT('',(44.5079524583206,-59.475452478349,235.35105));
#239269=CARTESIAN_POINT('Ctrl Pts',(44.5079524583206,-59.475452478349,-49.3249500000001));
#239270=CARTESIAN_POINT('Ctrl Pts',(44.2993850363199,-59.475452478349,-49.3371164329501));
#239271=CARTESIAN_POINT('Ctrl Pts',(44.0917630202625,-59.4428246129822,
-49.3492277172203));
#239272=CARTESIAN_POINT('Ctrl Pts',(43.6500545683669,-59.300019158842,-49.3749940435809));
#239273=CARTESIAN_POINT('Ctrl Pts',(43.4246875255532,-59.1759130933234,
-49.387307771915));
#239274=CARTESIAN_POINT('Ctrl Pts',(43.0237071573202,-58.8422425206466,
-49.4158594522137));
#239275=CARTESIAN_POINT('Ctrl Pts',(42.8549286887907,-58.6324245804788,
-49.4313817714165));
#239276=CARTESIAN_POINT('Ctrl Pts',(42.6142478061451,-58.1680262740998,
-49.4618621731236));
#239277=CARTESIAN_POINT('Ctrl Pts',(42.5411136494647,-57.9197018279802,
-49.4765401439522));
#239278=CARTESIAN_POINT('Ctrl Pts',(42.4921699010616,-57.4037007753935,
-49.5040350877759));
#239279=CARTESIAN_POINT('Ctrl Pts',(42.518845738177,-57.1407748289753,-49.5171750158715));
#239280=CARTESIAN_POINT('Ctrl Pts',(42.6724657743842,-56.6385980063255,
-49.547024643588));
#239281=CARTESIAN_POINT('Ctrl Pts',(42.7984669024605,-56.4044759374015,
-49.5625270899479));
#239282=CARTESIAN_POINT('Ctrl Pts',(43.1277988610394,-56.0059129337578,
-49.5922672704326));
#239283=CARTESIAN_POINT('Ctrl Pts',(43.3250966049773,-55.842927230864,-49.6059500752218));
#239284=CARTESIAN_POINT('Ctrl Pts',(43.7800628312528,-55.5938368428163,
-49.6324897717545));
#239285=CARTESIAN_POINT('Ctrl Pts',(44.0356007460214,-55.5140411370886,
-49.6473961501161));
#239286=CARTESIAN_POINT('Ctrl Pts',(44.5579835976218,-55.45921768084,-49.6778684831261));
#239287=CARTESIAN_POINT('Ctrl Pts',(44.8196105601658,-55.4828185316031,
-49.6931300559411));
#239288=CARTESIAN_POINT('Ctrl Pts',(45.3133155785361,-55.6272140610877,
-49.7219295153461));
#239289=CARTESIAN_POINT('Ctrl Pts',(45.5413713246016,-55.7443743383945,
-49.7343071876337));
#239290=CARTESIAN_POINT('Ctrl Pts',(45.9519402281426,-56.0660476571897,
-49.7625324544917));
#239291=CARTESIAN_POINT('Ctrl Pts',(46.1272280173218,-56.2715267988392,
-49.7780254408121));
#239292=CARTESIAN_POINT('Ctrl Pts',(46.3816599958988,-56.7302313335169,
-49.8086192773458));
#239293=CARTESIAN_POINT('Ctrl Pts',(46.4618772342432,-56.9771099115252,
-49.8234307954762));
#239294=CARTESIAN_POINT('Ctrl Pts',(46.5246920778563,-57.4902348273388,
-49.8511850158054));
#239295=CARTESIAN_POINT('Ctrl Pts',(46.5057422852615,-57.7516916526499,
-49.8639695550248));
#239296=CARTESIAN_POINT('Ctrl Pts',(46.3677524162161,-58.2570507134512,
-49.8935240636454));
#239297=CARTESIAN_POINT('Ctrl Pts',(46.2484052535005,-58.4955335504917,
-49.9090527339471));
#239298=CARTESIAN_POINT('Ctrl Pts',(45.9300547456721,-58.9045229115213,
-49.9389993423897));
#239299=CARTESIAN_POINT('Ctrl Pts',(45.7370659118431,-59.0735591688394,
-49.9531675821346));
#239300=CARTESIAN_POINT('Ctrl Pts',(45.2888264544129,-59.3356783731931,
-49.9794830098808));
#239301=CARTESIAN_POINT('Ctrl Pts',(45.0356851522591,-59.4227115455241,
-49.9941655928536));
#239302=CARTESIAN_POINT('Ctrl Pts',(44.6848476516991,-59.4695912588368,
-50.0146311137196));
#239303=CARTESIAN_POINT('Ctrl Pts',(44.5963558612004,-59.475452478349,-50.0197931348321));
#239304=CARTESIAN_POINT('Ctrl Pts',(44.5079524583206,-59.475452478349,-50.0249500000001));
#239305=CARTESIAN_POINT('Ctrl Pts',(44.5079524583206,-59.475452478349,-49.8662));
#239306=CARTESIAN_POINT('Ctrl Pts',(44.7527989264331,-59.475452478349,-49.8519172893601));
#239307=CARTESIAN_POINT('Ctrl Pts',(44.99579624215,-59.4304871657721,-49.8377424459432));
#239308=CARTESIAN_POINT('Ctrl Pts',(45.4624274771203,-59.2513430521657,
-49.81052229057));
#239309=CARTESIAN_POINT('Ctrl Pts',(45.6804567563558,-59.1155893798232,
-49.798191970945));
#239310=CARTESIAN_POINT('Ctrl Pts',(46.0578148199063,-58.765972037735,-49.7695236732668));
#239311=CARTESIAN_POINT('Ctrl Pts',(46.2121774971817,-58.5539299471189,
-49.7543094546795));
#239312=CARTESIAN_POINT('Ctrl Pts',(46.4333807998448,-58.0779402599982,
-49.723811573961));
#239313=CARTESIAN_POINT('Ctrl Pts',(46.4962158545024,-57.8176838117814,
-49.7088312109536));
#239314=CARTESIAN_POINT('Ctrl Pts',(46.516246592131,-57.2995570505814,-49.682072176414));
#239315=CARTESIAN_POINT('Ctrl Pts',(46.4778484030692,-57.0467794036011,
-49.668666194984));
#239316=CARTESIAN_POINT('Ctrl Pts',(46.3054863165889,-56.5600418323204,
-49.6390498865289));
#239317=CARTESIAN_POINT('Ctrl Pts',(46.1697347144584,-56.3319549329881,
-49.6235679369362));
#239318=CARTESIAN_POINT('Ctrl Pts',(45.8176406644073,-55.9411966105091,
-49.5935581401593));
#239319=CARTESIAN_POINT('Ctrl Pts',(45.604723775311,-55.7824431043697,-49.5801783268244));
#239320=CARTESIAN_POINT('Ctrl Pts',(45.1358868263273,-55.5593847398029,
-49.5528295048004));
#239321=CARTESIAN_POINT('Ctrl Pts',(44.8856073119475,-55.4948072943955,
-49.5382298664615));
#239322=CARTESIAN_POINT('Ctrl Pts',(44.3643334885523,-55.4629374060242,
-49.5078222267634));
#239323=CARTESIAN_POINT('Ctrl Pts',(44.0980535099889,-55.4998891566375,
-49.4922892280139));
#239324=CARTESIAN_POINT('Ctrl Pts',(43.6055726841607,-55.6723868202004,
-49.4635611798405));
#239325=CARTESIAN_POINT('Ctrl Pts',(43.3828003792474,-55.8023211373756,
-49.4512398953274));
#239326=CARTESIAN_POINT('Ctrl Pts',(42.9955369778988,-56.1413841849868,
-49.4228158753796));
#239327=CARTESIAN_POINT('Ctrl Pts',(42.8356192866904,-56.3483239727476,
-49.4076973944461));
#239328=CARTESIAN_POINT('Ctrl Pts',(42.6009172321237,-56.8170394584344,
-49.3771732793191));
#239329=CARTESIAN_POINT('Ctrl Pts',(42.5305072941766,-57.0753961113057,
-49.3620679563592));
#239330=CARTESIAN_POINT('Ctrl Pts',(42.4953952961135,-57.5926212844573,
-49.3349145982825));
#239331=CARTESIAN_POINT('Ctrl Pts',(42.5263675132484,-57.8462316166951,
-49.3219318186393));
#239332=CARTESIAN_POINT('Ctrl Pts',(42.6840582308023,-58.336909494207,-49.2925443681356));
#239333=CARTESIAN_POINT('Ctrl Pts',(42.8125271523483,-58.5682601143377,
-49.277109952928));
#239334=CARTESIAN_POINT('Ctrl Pts',(43.1536370793267,-58.9709056695457,
-49.2468200054185));
#239335=CARTESIAN_POINT('Ctrl Pts',(43.3639361748342,-59.1372944985489,
-49.2329342832032));
#239336=CARTESIAN_POINT('Ctrl Pts',(43.8282116719572,-59.3736681285028,
-49.205851545871));
#239337=CARTESIAN_POINT('Ctrl Pts',(44.075958726924,-59.4448710603739,-49.1913996343313));
#239338=CARTESIAN_POINT('Ctrl Pts',(44.3895030689671,-59.4728249807475,
-49.1731095477121));
#239339=CARTESIAN_POINT('Ctrl Pts',(44.4487628003175,-59.475452478349,-49.1696527300501));
#239340=CARTESIAN_POINT('Ctrl Pts',(44.5079524583206,-59.475452478349,-49.1662));
#239341=CARTESIAN_POINT('Origin',(44.5079524583206,-57.475452478349,235.35105));
#239342=CARTESIAN_POINT('',(44.5079524583206,-59.475452478349,-48.4662));
#239343=CARTESIAN_POINT('',(44.5079524583206,-59.475452478349,-48.6249500000001));
#239344=CARTESIAN_POINT('',(44.5079524583206,-59.475452478349,235.35105));
#239345=CARTESIAN_POINT('Ctrl Pts',(44.5079524583206,-59.475452478349,-48.6249500000001));
#239346=CARTESIAN_POINT('Ctrl Pts',(44.2628858061291,-59.475452478349,-48.6392455547112));
#239347=CARTESIAN_POINT('Ctrl Pts',(44.0197530000773,-59.4304074108024,
-48.653428301731));
#239348=CARTESIAN_POINT('Ctrl Pts',(43.5503561414569,-59.250085042783,-48.6808097851505));
#239349=CARTESIAN_POINT('Ctrl Pts',(43.3300987723401,-59.1122108366676,
-48.6932847306152));
#239350=CARTESIAN_POINT('Ctrl Pts',(42.9483494736007,-58.7552654889186,
-48.7224513032651));
#239351=CARTESIAN_POINT('Ctrl Pts',(42.7926360521606,-58.53750494125,-48.7379938044201));
#239352=CARTESIAN_POINT('Ctrl Pts',(42.5792853953837,-58.0630921017883,
-48.7681829902094));
#239353=CARTESIAN_POINT('Ctrl Pts',(42.5201114162669,-57.8125110023086,
-48.782567791142));
#239354=CARTESIAN_POINT('Ctrl Pts',(42.4986930893646,-57.2911026753661,
-48.8095330756611));
#239355=CARTESIAN_POINT('Ctrl Pts',(42.5411384880099,-57.025095625394,-48.8236691202661));
#239356=CARTESIAN_POINT('Ctrl Pts',(42.7262002695061,-56.5300023567024,
-48.8540779508556));
#239357=CARTESIAN_POINT('Ctrl Pts',(42.8651008634393,-56.3051702510185,
-48.8694873198933));
#239358=CARTESIAN_POINT('Ctrl Pts',(43.2158589037499,-55.9279840651222,
-48.8987725105074));
#239359=CARTESIAN_POINT('Ctrl Pts',(43.421980054436,-55.7769839375025,-48.9116016097736));
#239360=CARTESIAN_POINT('Ctrl Pts',(43.8904129903254,-55.5547787422683,
-48.938926864367));
#239361=CARTESIAN_POINT('Ctrl Pts',(44.1502370279982,-55.4899195933945,
-48.9540832665646));
#239362=CARTESIAN_POINT('Ctrl Pts',(44.673562407491,-55.4655959698017,-48.9846105803683));
#239363=CARTESIAN_POINT('Ctrl Pts',(44.9319452632814,-55.5038531889676,
-48.9996829136228));
#239364=CARTESIAN_POINT('Ctrl Pts',(45.4173294380215,-55.6758275679205,
-49.0279969904826));
#239365=CARTESIAN_POINT('Ctrl Pts',(45.6400656968707,-55.8069390138041,
-49.040346425058));
#239366=CARTESIAN_POINT('Ctrl Pts',(46.0312969479705,-56.15253847459,-49.0692163814486));
#239367=CARTESIAN_POINT('Ctrl Pts',(46.1934495883523,-56.3665082155528,
-49.0847551886198));
#239368=CARTESIAN_POINT('Ctrl Pts',(46.4202265107652,-56.836213844073,-49.1150981742418));
#239369=CARTESIAN_POINT('Ctrl Pts',(46.4862393844462,-57.0857870682806,
-49.1296315269398));
#239370=CARTESIAN_POINT('Ctrl Pts',(46.5211806859975,-57.6045889103354,
-49.1568595567621));
#239371=CARTESIAN_POINT('Ctrl Pts',(46.4865588826382,-57.8690589132808,
-49.1704582476425));
#239372=CARTESIAN_POINT('Ctrl Pts',(46.3170122058166,-58.367765103258,-49.20059707244));
#239373=CARTESIAN_POINT('Ctrl Pts',(46.1843934954698,-58.597265521946,-49.216059054403));
#239374=CARTESIAN_POINT('Ctrl Pts',(45.8441363149027,-58.9850222178621,
-49.2455719725367));
#239375=CARTESIAN_POINT('Ctrl Pts',(45.6424168786208,-59.1419232574092,
-49.258772908816));
#239376=CARTESIAN_POINT('Ctrl Pts',(45.1806076872912,-59.3775193679133,
-49.2857117783102));
#239377=CARTESIAN_POINT('Ctrl Pts',(44.9228019790787,-59.449832775337,-49.3007504446226));
#239378=CARTESIAN_POINT('Ctrl Pts',(44.6083029113298,-59.473566405843,-49.3190962235747));
#239379=CARTESIAN_POINT('Ctrl Pts',(44.5581003572643,-59.475452478349,-49.322024705895));
#239380=CARTESIAN_POINT('Ctrl Pts',(44.5079524583206,-59.475452478349,-49.3249500000001));
#239381=CARTESIAN_POINT('Ctrl Pts',(44.5079524583206,-59.475452478349,-49.1662));
#239382=CARTESIAN_POINT('Ctrl Pts',(44.7132715088587,-59.475452478349,-49.1542230553852));
#239383=CARTESIAN_POINT('Ctrl Pts',(44.9177473805613,-59.4438328899582,
-49.1422952962024));
#239384=CARTESIAN_POINT('Ctrl Pts',(45.358903240101,-59.3035316594213,-49.116561204396));
#239385=CARTESIAN_POINT('Ctrl Pts',(45.5863767543091,-59.1792682324807,
-49.1041529087429));
#239386=CARTESIAN_POINT('Ctrl Pts',(45.9831298528174,-58.8504548046765,
-49.0759698977774));
#239387=CARTESIAN_POINT('Ctrl Pts',(46.1482456265836,-58.6485645864941,
-49.0609549010088));
#239388=CARTESIAN_POINT('Ctrl Pts',(46.3957283829482,-58.1872209175729,
-49.0304304259471));
#239389=CARTESIAN_POINT('Ctrl Pts',(46.4733812498941,-57.9309093580201,
-49.0152171652196));
#239390=CARTESIAN_POINT('Ctrl Pts',(46.5230199061657,-57.4146992144779,
-48.9876913903617));
#239391=CARTESIAN_POINT('Ctrl Pts',(46.4991408743921,-57.1602047976489,
-48.9750172663038));
#239392=CARTESIAN_POINT('Ctrl Pts',(46.3553727362881,-56.6659126895361,
-48.9458533067957));
#239393=CARTESIAN_POINT('Ctrl Pts',(46.2338822787049,-56.4316732943863,
-48.9304764945548));
#239394=CARTESIAN_POINT('Ctrl Pts',(45.9052964648732,-56.0201967535934,
-48.9001057086371));
#239395=CARTESIAN_POINT('Ctrl Pts',(45.7002801752457,-55.8479994165806,
-48.885752450154));
#239396=CARTESIAN_POINT('Ctrl Pts',(45.2442659485269,-55.5985583229646,
-48.8591516202621));
#239397=CARTESIAN_POINT('Ctrl Pts',(44.9995138590369,-55.5201491841072,
-48.8448744150418));
#239398=CARTESIAN_POINT('Ctrl Pts',(44.484009019507,-55.4581707161369,-48.8148032994025));
#239399=CARTESIAN_POINT('Ctrl Pts',(44.217639991574,-55.4790228412861,-48.7992651061064));
#239400=CARTESIAN_POINT('Ctrl Pts',(43.7142356080425,-55.6215683034491,
-48.7698998504004));
#239401=CARTESIAN_POINT('Ctrl Pts',(43.4814911769751,-55.7395837163142,
-48.7572877552849));
#239402=CARTESIAN_POINT('Ctrl Pts',(43.0744826223804,-56.0571589538179,
-48.7293733594172));
#239403=CARTESIAN_POINT('Ctrl Pts',(42.9038953539184,-56.2534202770791,
-48.7144831387365));
#239404=CARTESIAN_POINT('Ctrl Pts',(42.6414553133673,-56.7086763374907,
-48.6838299442637));
#239405=CARTESIAN_POINT('Ctrl Pts',(42.5556337052545,-56.9653111080983,
-48.6683621005613));
#239406=CARTESIAN_POINT('Ctrl Pts',(42.4919360036821,-57.4830825969925,
-48.6403473939391));
#239407=CARTESIAN_POINT('Ctrl Pts',(42.5091508424181,-57.7384862452087,
-48.6278770682213));
#239408=CARTESIAN_POINT('Ctrl Pts',(42.6399410486995,-58.2360422490106,
-48.5989267457574));
#239409=CARTESIAN_POINT('Ctrl Pts',(42.7548773808458,-58.472788537187,-48.5836144519141));
#239410=CARTESIAN_POINT('Ctrl Pts',(43.0716962448171,-58.8922797794919,
-48.553181980819));
#239411=CARTESIAN_POINT('Ctrl Pts',(43.2718943390135,-59.0699569802348,
-48.5383669465165));
#239412=CARTESIAN_POINT('Ctrl Pts',(43.720316120413,-59.3312793356208,-48.5120864563225));
#239413=CARTESIAN_POINT('Ctrl Pts',(43.9621322449313,-59.4162392210301,
-48.4980395124476));
#239414=CARTESIAN_POINT('Ctrl Pts',(44.3111829714994,-59.4681993883674,
-48.4776782200645));
#239415=CARTESIAN_POINT('Ctrl Pts',(44.409611102366,-59.475452478349,-48.4719365790973));
#239416=CARTESIAN_POINT('Ctrl Pts',(44.5079524583206,-59.475452478349,-48.4662));
#239417=CARTESIAN_POINT('Origin',(44.5079524583206,-57.475452478349,235.35105));
#239418=CARTESIAN_POINT('',(44.5079524583206,-59.475452478349,-47.7662));
#239419=CARTESIAN_POINT('',(44.5079524583206,-59.475452478349,-47.9249500000001));
#239420=CARTESIAN_POINT('',(44.5079524583206,-59.475452478349,235.35105));
#239421=CARTESIAN_POINT('Ctrl Pts',(44.5079524583206,-59.475452478349,-47.9249500000001));
#239422=CARTESIAN_POINT('Ctrl Pts',(44.4812735172686,-59.475452478349,-47.9265062715615));
#239423=CARTESIAN_POINT('Ctrl Pts',(44.4545736600142,-59.4749186583905,
-47.9280637632347));
#239424=CARTESIAN_POINT('Ctrl Pts',(44.1714735144825,-59.4635736950934,
-47.9445779383907));
#239425=CARTESIAN_POINT('Ctrl Pts',(43.9194001871073,-59.4040494254147,
-47.9592822158209));
#239426=CARTESIAN_POINT('Ctrl Pts',(43.4472013548033,-59.1910043209327,
-47.9868271477054));
#239427=CARTESIAN_POINT('Ctrl Pts',(43.2323421053487,-59.0378716270781,
-47.9998914459693));
#239428=CARTESIAN_POINT('Ctrl Pts',(42.872209851426,-58.6560295349205,-48.0296852589112));
#239429=CARTESIAN_POINT('Ctrl Pts',(42.7310849722988,-58.4305188890606,
-48.0451937815271));
#239430=CARTESIAN_POINT('Ctrl Pts',(42.5477880010018,-57.946809992494,-48.0749760210836));
#239431=CARTESIAN_POINT('Ctrl Pts',(42.5038789014379,-57.6945899848913,
-48.0887607668151));
#239432=CARTESIAN_POINT('Ctrl Pts',(42.5128179882102,-57.1758953028072,
-48.115224985183));
#239433=CARTESIAN_POINT('Ctrl Pts',(42.57005350494,-56.914388489372,-48.13010519447));
#239434=CARTESIAN_POINT('Ctrl Pts',(42.7811922510803,-56.4333024154484,
-48.1605669856489));
#239435=CARTESIAN_POINT('Ctrl Pts',(42.9313712997834,-56.217603719075,-48.175843906689));
#239436=CARTESIAN_POINT('Ctrl Pts',(43.3014050122175,-55.8602827251107,
-48.2046877516896));
#239437=CARTESIAN_POINT('Ctrl Pts',(43.5160390694056,-55.7202808025766,
-48.2170883856467));
#239438=CARTESIAN_POINT('Ctrl Pts',(43.9988476680525,-55.5229120870323,
-48.2452522205677));
#239439=CARTESIAN_POINT('Ctrl Pts',(44.264324345215,-55.472401353952,-48.2607383600689));
#239440=CARTESIAN_POINT('Ctrl Pts',(44.7891056123032,-55.4786665482241,
-48.291350600649));
#239441=CARTESIAN_POINT('Ctrl Pts',(45.0434210252528,-55.5313571362534,
-48.3061856664044));
#239442=CARTESIAN_POINT('Ctrl Pts',(45.520018192311,-55.7310329889019,-48.3339871678161));
#239443=CARTESIAN_POINT('Ctrl Pts',(45.7374485981369,-55.8768189925122,
-48.3467169668236));
#239444=CARTESIAN_POINT('Ctrl Pts',(46.1080265911284,-56.2467982934191,
-48.3762161609043));
#239445=CARTESIAN_POINT('Ctrl Pts',(46.2561798782702,-56.4687162142566,
-48.3917481809377));
#239446=CARTESIAN_POINT('Ctrl Pts',(46.4538706739191,-56.9481137726077,
-48.4217324395466));
#239447=CARTESIAN_POINT('Ctrl Pts',(46.5051137679225,-57.1996308181294,
-48.4359332052579));
#239448=CARTESIAN_POINT('Ctrl Pts',(46.5106749708228,-57.719009698564,-48.4623334664469));
#239449=CARTESIAN_POINT('Ctrl Pts',(46.4608239245511,-57.9820273274215,
-48.4769158057141));
#239450=CARTESIAN_POINT('Ctrl Pts',(46.2628832553274,-58.4696172890998,
-48.5073212173507));
#239451=CARTESIAN_POINT('Ctrl Pts',(46.118275604911,-58.6899543335241,-48.5226699600301));
#239452=CARTESIAN_POINT('Ctrl Pts',(45.7578409129819,-59.057242152736,-48.5517373391578));
#239453=CARTESIAN_POINT('Ctrl Pts',(45.5475198216822,-59.2027509743537,
-48.5643085704707));
#239454=CARTESIAN_POINT('Ctrl Pts',(45.0729530614444,-59.4122363761628,
-48.5919916314846));
#239455=CARTESIAN_POINT('Ctrl Pts',(44.8114261044714,-59.4700010872062,
-48.6072473706413));
#239456=CARTESIAN_POINT('Ctrl Pts',(44.5335099733831,-59.4753300564951,
-48.6234591449548));
#239457=CARTESIAN_POINT('Ctrl Pts',(44.5207285878716,-59.475452478349,-48.6242047257763));
#239458=CARTESIAN_POINT('Ctrl Pts',(44.5079524583206,-59.475452478349,-48.6249500000001));
#239459=CARTESIAN_POINT('Ctrl Pts',(44.5079524583206,-59.475452478349,-48.4662));
#239460=CARTESIAN_POINT('Ctrl Pts',(44.6722461043367,-59.475452478349,-48.4566162039824));
#239461=CARTESIAN_POINT('Ctrl Pts',(44.8362975563793,-59.4552073494373,
-48.4470465359465));
#239462=CARTESIAN_POINT('Ctrl Pts',(45.2488941590956,-59.3513070975787,
-48.422978400788));
#239463=CARTESIAN_POINT('Ctrl Pts',(45.486541680707,-59.2390197994558,-48.4100833035931));
#239464=CARTESIAN_POINT('Ctrl Pts',(45.9027515590896,-58.9316738856167,
-48.3824173022742));
#239465=CARTESIAN_POINT('Ctrl Pts',(46.0781093830703,-58.7406079583137,
-48.3676504021756));
#239466=CARTESIAN_POINT('Ctrl Pts',(46.3522268646779,-58.2939865942306,
-48.3370928245439));
#239467=CARTESIAN_POINT('Ctrl Pts',(46.4449529529653,-58.0406124163855,
-48.3215883192794));
#239468=CARTESIAN_POINT('Ctrl Pts',(46.5234594666808,-57.5249853327108,
-48.2932500203511));
#239469=CARTESIAN_POINT('Ctrl Pts',(46.5134218647486,-57.2685197941095,
-48.2809056682711));
#239470=CARTESIAN_POINT('Ctrl Pts',(46.3964759327107,-56.767589888895,-48.2521886938865));
#239471=CARTESIAN_POINT('Ctrl Pts',(46.2885726388101,-56.5283697946779,
-48.2369565582243));
#239472=CARTESIAN_POINT('Ctrl Pts',(45.9843414414616,-56.1004848845509,
-48.2064671948478));
#239473=CARTESIAN_POINT('Ctrl Pts',(45.7892916557144,-55.9170947423855,
-48.1915137123182));
#239474=CARTESIAN_POINT('Ctrl Pts',(45.348927075157,-55.6432465319262,-48.164835440808));
#239475=CARTESIAN_POINT('Ctrl Pts',(45.1101967248856,-55.5515005415793,
-48.1513309155497));
#239476=CARTESIAN_POINT('Ctrl Pts',(44.6017017858425,-55.4604092580464,
-48.1216687107721));
#239477=CARTESIAN_POINT('Ctrl Pts',(44.336159119653,-55.4655573311246,-48.1061787219111));
#239478=CARTESIAN_POINT('Ctrl Pts',(43.8227104150117,-55.5782399321306,
-48.0762275474736));
#239479=CARTESIAN_POINT('Ctrl Pts',(43.5798406550112,-55.684489612824,-48.0629395338322));
#239480=CARTESIAN_POINT('Ctrl Pts',(43.154156374964,-55.9811549817676,-48.0355367571517));
#239481=CARTESIAN_POINT('Ctrl Pts',(42.9740323221626,-56.16673555949,-48.0209079517508));
#239482=CARTESIAN_POINT('Ctrl Pts',(42.6881360285851,-56.6041343058631,
-47.9904727350081));
#239483=CARTESIAN_POINT('Ctrl Pts',(42.5883969739102,-56.8539548963596,
-47.9749432055442));
#239484=CARTESIAN_POINT('Ctrl Pts',(42.4946218652844,-57.3672049541195,
-47.9462796555459));
#239485=CARTESIAN_POINT('Ctrl Pts',(42.4972562241896,-57.6248506055178,
-47.9339646567133));
#239486=CARTESIAN_POINT('Ctrl Pts',(42.6000879300122,-58.1291088776438,
-47.9054912043259));
#239487=CARTESIAN_POINT('Ctrl Pts',(42.7007890912238,-58.3706358676202,
-47.8903525907645));
#239488=CARTESIAN_POINT('Ctrl Pts',(42.9919888297182,-58.8066701715437,
-47.8598316193181));
#239489=CARTESIAN_POINT('Ctrl Pts',(43.1816290358722,-58.995714545876,-47.8447502748528));
#239490=CARTESIAN_POINT('Ctrl Pts',(43.6136801796984,-59.2822158687836,
-47.8176752667663));
#239491=CARTESIAN_POINT('Ctrl Pts',(43.8493896412147,-59.3808283931455,
-47.8046161643311));
#239492=CARTESIAN_POINT('Ctrl Pts',(44.2326665036937,-59.4612393661861,
-47.7822583473531));
#239493=CARTESIAN_POINT('Ctrl Pts',(44.3702910583955,-59.475452478349,-47.7742302483289));
#239494=CARTESIAN_POINT('Ctrl Pts',(44.5079524583206,-59.475452478349,-47.7662));
#239495=CARTESIAN_POINT('Origin',(44.5079524583206,-57.475452478349,235.35105));
#239496=CARTESIAN_POINT('',(44.5079524583206,-59.475452478349,-47.0662));
#239497=CARTESIAN_POINT('',(44.5079524583206,-59.475452478349,-47.2249500000001));
#239498=CARTESIAN_POINT('',(44.5079524583206,-59.475452478349,235.35105));
#239499=CARTESIAN_POINT('Ctrl Pts',(44.5079524583206,-59.475452478349,-47.2249500000001));
#239500=CARTESIAN_POINT('Ctrl Pts',(44.4440657053146,-59.475452478349,-47.2286767272588));
#239501=CARTESIAN_POINT('Ctrl Pts',(44.3801027710404,-59.4723914198285,
-47.2324078984249));
#239502=CARTESIAN_POINT('Ctrl Pts',(44.0622334462755,-59.4417876861605,
-47.2509502757029));
#239503=CARTESIAN_POINT('Ctrl Pts',(43.8151560576545,-59.3689190437521,
-47.2653631233725));
#239504=CARTESIAN_POINT('Ctrl Pts',(43.3520565585926,-59.1291615287946,
-47.2923772608178));
#239505=CARTESIAN_POINT('Ctrl Pts',(43.1424308834313,-58.9608025867536,
-47.3064072418367));
#239506=CARTESIAN_POINT('Ctrl Pts',(42.804167543703,-58.5551320031449,-47.3367669827188));
#239507=CARTESIAN_POINT('Ctrl Pts',(42.6775733797043,-58.3229827036197,
-47.3521870653023));
#239508=CARTESIAN_POINT('Ctrl Pts',(42.5236348995407,-57.8313190140775,
-47.3815148769473));
#239509=CARTESIAN_POINT('Ctrl Pts',(42.4945693561079,-57.577479578032,-47.3944054393407));
#239510=CARTESIAN_POINT('Ctrl Pts',(42.5335756423137,-57.0605121379261,
-47.4216593606253));
#239511=CARTESIAN_POINT('Ctrl Pts',(42.6059328844838,-56.8026831422405,
-47.4367948236942));
#239512=CARTESIAN_POINT('Ctrl Pts',(42.8440833337503,-56.3359092265583,
-47.4673214324781));
#239513=CARTESIAN_POINT('Ctrl Pts',(43.0054095238479,-56.1303104652254,
-47.4824132484568));
#239514=CARTESIAN_POINT('Ctrl Pts',(43.3952215439451,-55.7939871960042,
-47.5107731945863));
#239515=CARTESIAN_POINT('Ctrl Pts',(43.6192416365683,-55.6655659856764,
-47.523108535398));
#239516=CARTESIAN_POINT('Ctrl Pts',(44.1131444124268,-55.4968457401887,
-47.5519195306564));
#239517=CARTESIAN_POINT('Ctrl Pts',(44.3794878812615,-55.4619401339279,
-47.567456233005));
#239518=CARTESIAN_POINT('Ctrl Pts',(44.9001253313971,-55.4976543677708,
-47.5978267509296));
#239519=CARTESIAN_POINT('Ctrl Pts',(45.1497467158906,-55.5640067925415,
-47.6123879983584));
#239520=CARTESIAN_POINT('Ctrl Pts',(45.6173792779121,-55.7906106541898,
-47.6396665644763));
#239521=CARTESIAN_POINT('Ctrl Pts',(45.8296035617798,-55.9513791485695,
-47.6531714609698));
#239522=CARTESIAN_POINT('Ctrl Pts',(46.1788061885846,-56.3452997501013,
-47.6832566770517));
#239523=CARTESIAN_POINT('Ctrl Pts',(46.3126336338315,-56.5742741833758,
-47.6987273419733));
#239524=CARTESIAN_POINT('Ctrl Pts',(46.481103660285,-57.0620705652085,-47.7282836211598));
#239525=CARTESIAN_POINT('Ctrl Pts',(46.5175359190433,-57.3150594772912,
-47.7415677249412));
#239526=CARTESIAN_POINT('Ctrl Pts',(46.4935268385644,-57.8329630900862,
-47.7684315214364));
#239527=CARTESIAN_POINT('Ctrl Pts',(46.4286888059395,-58.092740649065,-47.7834461120366));
#239528=CARTESIAN_POINT('Ctrl Pts',(46.2039030615399,-58.566849637401,-47.8139534712186));
#239529=CARTESIAN_POINT('Ctrl Pts',(46.048059785429,-58.7775600987125,-47.8291436024916));
#239530=CARTESIAN_POINT('Ctrl Pts',(45.6680828398364,-59.1244022108298,
-47.8577480847495));
#239531=CARTESIAN_POINT('Ctrl Pts',(45.448816781282,-59.2586260436173,-47.8700662478273));
#239532=CARTESIAN_POINT('Ctrl Pts',(44.9854445467154,-59.4323969429685,
-47.8970962948437));
#239533=CARTESIAN_POINT('Ctrl Pts',(44.7475419366017,-59.475452478349,-47.9109739471004));
#239534=CARTESIAN_POINT('Ctrl Pts',(44.5079524583206,-59.475452478349,-47.9249500000001));
#239535=CARTESIAN_POINT('Ctrl Pts',(44.5079524583206,-59.475452478349,-47.7662));
#239536=CARTESIAN_POINT('Ctrl Pts',(44.6313030775092,-59.475452478349,-47.759004547214));
#239537=CARTESIAN_POINT('Ctrl Pts',(44.7546832795126,-59.4640410230751,
-47.7518073687637));
#239538=CARTESIAN_POINT('Ctrl Pts',(45.1370515644779,-59.3923532492405,
-47.7295025521408));
#239539=CARTESIAN_POINT('Ctrl Pts',(45.3852358868118,-59.2922063992075,
-47.7157249444625));
#239540=CARTESIAN_POINT('Ctrl Pts',(45.820249612569,-59.0062087994247,-47.688588974896));
#239541=CARTESIAN_POINT('Ctrl Pts',(46.0049145305874,-58.8261567023458,
-47.6741070161994));
#239542=CARTESIAN_POINT('Ctrl Pts',(46.3021477299,-58.3981562130439,-47.643815922253));
#239543=CARTESIAN_POINT('Ctrl Pts',(46.4086861793783,-58.1520249958447,
-47.6282744574157));
#239544=CARTESIAN_POINT('Ctrl Pts',(46.5175168144668,-57.6412869744509,
-47.5992986913219));
#239545=CARTESIAN_POINT('Ctrl Pts',(46.522199175265,-57.3824073136085,-47.5869150597897));
#239546=CARTESIAN_POINT('Ctrl Pts',(46.4331309042178,-56.8750041847558,
-47.5586841685773));
#239547=CARTESIAN_POINT('Ctrl Pts',(46.3394721976225,-56.6314380197376,
-47.5436479445944));
#239548=CARTESIAN_POINT('Ctrl Pts',(46.0611496297214,-56.1878629206276,
-47.5131216102789));
#239549=CARTESIAN_POINT('Ctrl Pts',(45.8769306728218,-55.993478493689,-47.4979286160126));
#239550=CARTESIAN_POINT('Ctrl Pts',(45.4530866298438,-55.6947548334533,
-47.470475531848));
#239551=CARTESIAN_POINT('Ctrl Pts',(45.2202087529216,-55.5894829466028,
-47.4577482838518));
#239552=CARTESIAN_POINT('Ctrl Pts',(44.719497596083,-55.469551318773,-47.4285401330362));
#239553=CARTESIAN_POINT('Ctrl Pts',(44.4556856297394,-55.4591062061042,
-47.4131511016661));
#239554=CARTESIAN_POINT('Ctrl Pts',(43.9353429727177,-55.5409072719665,
-47.3827977800065));
#239555=CARTESIAN_POINT('Ctrl Pts',(43.6842138557186,-55.6337907462551,
-47.3685449650591));
#239556=CARTESIAN_POINT('Ctrl Pts',(43.2415863401375,-55.906606008996,-47.3418528738837));
#239557=CARTESIAN_POINT('Ctrl Pts',(43.0522030195489,-56.0805650309788,
-47.327541105985));
#239558=CARTESIAN_POINT('Ctrl Pts',(42.7430570731635,-56.4980950413809,
-47.2974315061241));
#239559=CARTESIAN_POINT('Ctrl Pts',(42.629317206933,-56.7400426823803,-47.2818913464887));
#239560=CARTESIAN_POINT('Ctrl Pts',(42.5042318600095,-57.2478692796583,
-47.2525885643891));
#239561=CARTESIAN_POINT('Ctrl Pts',(42.4916160868242,-57.5081563403832,
-47.2400243389413));
#239562=CARTESIAN_POINT('Ctrl Pts',(42.5659866783359,-58.018807860116,-47.2120580273557));
#239563=CARTESIAN_POINT('Ctrl Pts',(42.6521178711617,-58.2643216483869,
-47.1971429655331));
#239564=CARTESIAN_POINT('Ctrl Pts',(42.9126065722437,-58.7087982931983,
-47.1670912412467));
#239565=CARTESIAN_POINT('Ctrl Pts',(43.0844502985395,-58.9037183457706,
-47.1522321323951));
#239566=CARTESIAN_POINT('Ctrl Pts',(43.4938571975499,-59.2186407206989,
-47.124381802521));
#239567=CARTESIAN_POINT('Ctrl Pts',(43.7278636795627,-59.335174960608,-47.1117051787608));
#239568=CARTESIAN_POINT('Ctrl Pts',(44.1507753466232,-59.4514755926062,
-47.0870353315156));
#239569=CARTESIAN_POINT('Ctrl Pts',(44.3291584670778,-59.475452478349,-47.0766296494891));
#239570=CARTESIAN_POINT('Ctrl Pts',(44.5079524583206,-59.475452478349,-47.0662));
#239571=CARTESIAN_POINT('Origin',(44.5079524583206,-57.475452478349,235.35105));
#239572=CARTESIAN_POINT('',(44.5079524583206,-59.475452478349,-46.3662));
#239573=CARTESIAN_POINT('',(44.5079524583206,-59.475452478349,-46.5249500000001));
#239574=CARTESIAN_POINT('',(44.5079524583206,-59.475452478349,235.35105));
#239575=CARTESIAN_POINT('Ctrl Pts',(44.5079524583206,-59.475452478349,-46.5249500000001));
#239576=CARTESIAN_POINT('Ctrl Pts',(44.4042739832461,-59.475452478349,-46.5309979110461));
#239577=CARTESIAN_POINT('Ctrl Pts',(44.3005150510559,-59.4673907344713,
-46.537050515424));
#239578=CARTESIAN_POINT('Ctrl Pts',(43.9467671950224,-59.4118283130573,
-46.5576858070259));
#239579=CARTESIAN_POINT('Ctrl Pts',(43.7057975820276,-59.3250281505324,
-46.5715757119894));
#239580=CARTESIAN_POINT('Ctrl Pts',(43.2595445886996,-59.0603086524142,
-46.5979645632259));
#239581=CARTESIAN_POINT('Ctrl Pts',(43.0607222290518,-58.8810713066766,
-46.612818287574));
#239582=CARTESIAN_POINT('Ctrl Pts',(42.74728581496,-58.4592725694533,-46.643268674252));
#239583=CARTESIAN_POINT('Ctrl Pts',(42.634246955762,-58.2218370397722,-46.6585604443391));
#239584=CARTESIAN_POINT('Ctrl Pts',(42.5071992348591,-57.7233581402891,
-46.6874482339606));
#239585=CARTESIAN_POINT('Ctrl Pts',(42.4919171279419,-57.4676768193125,
-46.6998751147625));
#239586=CARTESIAN_POINT('Ctrl Pts',(42.5596016163837,-56.9504674630264,
-46.7279777047698));
#239587=CARTESIAN_POINT('Ctrl Pts',(42.6472914041524,-56.6946922299341,
-46.7434566148015));
#239588=CARTESIAN_POINT('Ctrl Pts',(42.9128987581068,-56.2417300473847,
-46.7740863067859));
#239589=CARTESIAN_POINT('Ctrl Pts',(43.0847842513759,-56.0468549063726,
-46.7889443649961));
#239590=CARTESIAN_POINT('Ctrl Pts',(43.4942711729337,-55.7320212087172,
-46.8167925490495));
#239591=CARTESIAN_POINT('Ctrl Pts',(43.7283199576162,-55.6155365287536,
-46.8294714374591));
#239592=CARTESIAN_POINT('Ctrl Pts',(44.2330764345255,-55.4768661041142,
-46.8589155652787));
#239593=CARTESIAN_POINT('Ctrl Pts',(44.4993887678175,-55.4580733083678,
-46.8744504513874));
#239594=CARTESIAN_POINT('Ctrl Pts',(45.0140292962556,-55.5238797838391,
-46.9044711488796));
#239595=CARTESIAN_POINT('Ctrl Pts',(45.2580164631152,-55.6040358428384,
-46.9187037336131));
#239596=CARTESIAN_POINT('Ctrl Pts',(45.7120200559247,-55.8566715438271,
-46.9451872765269));
#239597=CARTESIAN_POINT('Ctrl Pts',(45.9157706920935,-56.0303301365342,
-46.9596731266758));
#239598=CARTESIAN_POINT('Ctrl Pts',(46.2412554684407,-56.4440099576876,
-46.9900647713114));
#239599=CARTESIAN_POINT('Ctrl Pts',(46.3609997236072,-56.6789365473775,
-47.0054253684444));
#239600=CARTESIAN_POINT('Ctrl Pts',(46.5013017891596,-57.1741101225957,
-47.0345327642559));
#239601=CARTESIAN_POINT('Ctrl Pts',(46.5234063952971,-57.4288392538153,
-47.04714444637));
#239602=CARTESIAN_POINT('Ctrl Pts',(46.470118383048,-57.9447710465749,-47.074762599011));
#239603=CARTESIAN_POINT('Ctrl Pts',(46.3906555534907,-58.2005360292035,
-47.0900010382605));
#239604=CARTESIAN_POINT('Ctrl Pts',(46.1399985072978,-58.6599728667733,
-47.120521767186));
#239605=CARTESIAN_POINT('Ctrl Pts',(45.97360126581,-58.8605746742798,-47.1355090519746));
#239606=CARTESIAN_POINT('Ctrl Pts',(45.5744722927262,-59.1867997188816,
-47.1636305989549));
#239607=CARTESIAN_POINT('Ctrl Pts',(45.3457956844884,-59.3096273670682,
-47.1760758118071));
#239608=CARTESIAN_POINT('Ctrl Pts',(44.9079694493998,-59.445334969169,-47.2016156755206));
#239609=CARTESIAN_POINT('Ctrl Pts',(44.7083356845824,-59.475452478349,-47.2132609784681));
#239610=CARTESIAN_POINT('Ctrl Pts',(44.5079524583206,-59.475452478349,-47.2249500000001));
#239611=CARTESIAN_POINT('Ctrl Pts',(44.5079524583206,-59.475452478349,-47.0662));
#239612=CARTESIAN_POINT('Ctrl Pts',(44.5924271409675,-59.475452478349,-47.0612723101789));
#239613=CARTESIAN_POINT('Ctrl Pts',(44.6769935411895,-59.4701006492632,
-47.0563392701659));
#239614=CARTESIAN_POINT('Ctrl Pts',(45.0135599292962,-59.4271476052498,
-47.0367062308597));
#239615=CARTESIAN_POINT('Ctrl Pts',(45.2575720473973,-59.3470479781173,
-47.0224721906372));
#239616=CARTESIAN_POINT('Ctrl Pts',(45.711641066771,-59.0945154240205,-46.9959848311737));
#239617=CARTESIAN_POINT('Ctrl Pts',(45.9154328226276,-58.9209039851203,
-46.9815033566545));
#239618=CARTESIAN_POINT('Ctrl Pts',(46.2410181893005,-58.5072951339138,
-46.9511123634047));
#239619=CARTESIAN_POINT('Ctrl Pts',(46.3608190217601,-58.2723905884207,
-46.9357512297327));
#239620=CARTESIAN_POINT('Ctrl Pts',(46.5012332875956,-57.7772454347755,
-46.9066419972182));
#239621=CARTESIAN_POINT('Ctrl Pts',(46.5233953924273,-57.5225239937747,
-46.8940283847204));
#239622=CARTESIAN_POINT('Ctrl Pts',(46.4702257197404,-57.0065830249847,
-46.8664132200939));
#239623=CARTESIAN_POINT('Ctrl Pts',(46.3908215178601,-56.75080011293,-46.851175585057));
#239624=CARTESIAN_POINT('Ctrl Pts',(46.140267168965,-56.2913011007345,-46.8206547105223));
#239625=CARTESIAN_POINT('Ctrl Pts',(45.9739113259972,-56.0906573913506,
-46.8056665163854));
#239626=CARTESIAN_POINT('Ctrl Pts',(45.5748593452836,-55.7643483249545,
-46.7775429703905));
#239627=CARTESIAN_POINT('Ctrl Pts',(45.3462218937679,-55.6414740431258,
-46.7650990504012));
#239628=CARTESIAN_POINT('Ctrl Pts',(44.8471901486515,-55.4866647470764,
-46.7359888652694));
#239629=CARTESIAN_POINT('Ctrl Pts',(44.5807437012705,-55.459257464827,-46.7204461558388));
#239630=CARTESIAN_POINT('Ctrl Pts',(44.0626789576252,-55.5090156063934,
-46.6902257124594));
#239631=CARTESIAN_POINT('Ctrl Pts',(43.8155796410498,-55.5818302308093,
-46.6758115856592));
#239632=CARTESIAN_POINT('Ctrl Pts',(43.352441813358,-55.8214777672794,-46.6487952123772));
#239633=CARTESIAN_POINT('Ctrl Pts',(43.1427941923756,-55.9897724887097,
-46.6347700196637));
#239634=CARTESIAN_POINT('Ctrl Pts',(42.8044379796576,-56.3953447375082,
-46.6044125376785));
#239635=CARTESIAN_POINT('Ctrl Pts',(42.677782736474,-56.6274682800165,-46.5889919748156));
#239636=CARTESIAN_POINT('Ctrl Pts',(42.523722154733,-57.1191000281729,-46.5596622154942));
#239637=CARTESIAN_POINT('Ctrl Pts',(42.4945945119314,-57.3729319034361,
-46.5467687564028));
#239638=CARTESIAN_POINT('Ctrl Pts',(42.5334738337986,-57.8899079106368,
-46.519518105451));
#239639=CARTESIAN_POINT('Ctrl Pts',(42.6057676504509,-58.1477543480952,
-46.504383611167));
#239640=CARTESIAN_POINT('Ctrl Pts',(42.8438059234446,-58.6145919678895,
-46.4738570559773));
#239641=CARTESIAN_POINT('Ctrl Pts',(43.0050863640377,-58.8202345987045,
-46.4587643581541));
#239642=CARTESIAN_POINT('Ctrl Pts',(43.3948153248215,-59.1566472643482,
-46.4304023184461));
#239643=CARTESIAN_POINT('Ctrl Pts',(43.6187946416987,-59.2851179128159,
-46.4180675393028));
#239644=CARTESIAN_POINT('Ctrl Pts',(44.0695283912006,-59.4392184739542,
-46.3917747372486));
#239645=CARTESIAN_POINT('Ctrl Pts',(44.2881621760599,-59.475452478349,-46.3790210997985));
#239646=CARTESIAN_POINT('Ctrl Pts',(44.5079524583206,-59.475452478349,-46.3662));
#239647=CARTESIAN_POINT('Origin',(44.5079524583206,-57.475452478349,235.35105));
#239648=CARTESIAN_POINT('',(44.5079524583206,-59.475452478349,-45.6662));
#239649=CARTESIAN_POINT('',(44.5079524583206,-59.475452478349,-45.8249500000001));
#239650=CARTESIAN_POINT('',(44.5079524583206,-59.475452478349,235.35105));
#239651=CARTESIAN_POINT('Ctrl Pts',(44.5079524583206,-59.475452478349,-45.8249500000001));
#239652=CARTESIAN_POINT('Ctrl Pts',(44.3649863637798,-59.475452478349,-45.8332896888483));
#239653=CARTESIAN_POINT('Ctrl Pts',(44.2220900392258,-59.4601227788311,
-45.8416253077807));
#239654=CARTESIAN_POINT('Ctrl Pts',(43.8342749498873,-59.375535093521,-45.8642478546587));
#239655=CARTESIAN_POINT('Ctrl Pts',(43.5993670496297,-59.275060254976,-45.8772042214215));
#239656=CARTESIAN_POINT('Ctrl Pts',(43.1695971414633,-58.9851348581437,
-45.9043856713432));
#239657=CARTESIAN_POINT('Ctrl Pts',(42.9814564463317,-58.7945819919116,
-45.9194994862883));
#239658=CARTESIAN_POINT('Ctrl Pts',(42.6938360810368,-58.3564016474037,
-45.9500244733467));
#239659=CARTESIAN_POINT('Ctrl Pts',(42.5950997064634,-58.1142844010626,
-45.9651355992899));
#239660=CARTESIAN_POINT('Ctrl Pts',(42.4961107636773,-57.6091390557547,
-45.9935417843835));
#239661=CARTESIAN_POINT('Ctrl Pts',(42.4955089275564,-57.3511552825602,
-46.0058663278879));
#239662=CARTESIAN_POINT('Ctrl Pts',(42.5934707759449,-56.8385875537474,
-46.0346175211341));
#239663=CARTESIAN_POINT('Ctrl Pts',(42.6951126763407,-56.5897747239274,
-46.0501516400613));
#239664=CARTESIAN_POINT('Ctrl Pts',(42.9841901064911,-56.1549598604126,
-46.0805491069759));
#239665=CARTESIAN_POINT('Ctrl Pts',(43.1655930810649,-55.9709051582107,
-46.0951381298556));
#239666=CARTESIAN_POINT('Ctrl Pts',(43.593873124054,-55.6771926934943,-46.1224674410341));
#239667=CARTESIAN_POINT('Ctrl Pts',(43.8382044477795,-55.5726244620485,
-46.1358813660518));
#239668=CARTESIAN_POINT('Ctrl Pts',(44.3530189412511,-55.4642160359475,
-46.1659122115043));
#239669=CARTESIAN_POINT('Ctrl Pts',(44.6183716492554,-55.4612821467786,
-46.1813911194712));
#239670=CARTESIAN_POINT('Ctrl Pts',(45.1257945209625,-55.5564658975393,
-46.2109907869875));
#239671=CARTESIAN_POINT('Ctrl Pts',(45.3636825728427,-55.6501031130295,
-46.2243621912732));
#239672=CARTESIAN_POINT('Ctrl Pts',(45.8017731021026,-55.9274397505774,
-46.2511503651651));
#239673=CARTESIAN_POINT('Ctrl Pts',(45.995352296195,-56.1124009356582,-46.2661403216174));
#239674=CARTESIAN_POINT('Ctrl Pts',(46.2960219183106,-56.5425664516416,
-46.2966410177018));
#239675=CARTESIAN_POINT('Ctrl Pts',(46.4019490570959,-56.782442098733,-46.311848632824));
#239676=CARTESIAN_POINT('Ctrl Pts',(46.5150170033861,-57.2842975723613,
-46.3404992572935));
#239677=CARTESIAN_POINT('Ctrl Pts',(46.5230297623749,-57.541077598839,-46.3528255048842));
#239678=CARTESIAN_POINT('Ctrl Pts',(46.4403452397433,-58.0560713358598,
-46.3812536669056));
#239679=CARTESIAN_POINT('Ctrl Pts',(46.3456890407522,-58.3084922745376,
-46.3967663111878));
#239680=CARTESIAN_POINT('Ctrl Pts',(46.0683213604673,-58.7526217442415,
-46.4272928003906));
#239681=CARTESIAN_POINT('Ctrl Pts',(45.8916436383633,-58.9421993412834,
-46.4420230098285));
#239682=CARTESIAN_POINT('Ctrl Pts',(45.472839989253,-59.2466363315248,-46.4696177093593));
#239683=CARTESIAN_POINT('Ctrl Pts',(45.2337803403992,-59.3572856056787,
-46.4826100402123));
#239684=CARTESIAN_POINT('Ctrl Pts',(44.8252063906043,-59.4565575163686,
-46.506443520617));
#239685=CARTESIAN_POINT('Ctrl Pts',(44.6666737061617,-59.475452478349,-46.5156912605427));
#239686=CARTESIAN_POINT('Ctrl Pts',(44.5079524583206,-59.475452478349,-46.5249500000001));
#239687=CARTESIAN_POINT('Ctrl Pts',(44.5079524583206,-59.475452478349,-46.3662));
#239688=CARTESIAN_POINT('Ctrl Pts',(44.5533920533117,-59.475452478349,-46.3635493569588));
#239689=CARTESIAN_POINT('Ctrl Pts',(44.5988810789836,-59.4739039391127,
-46.3608958304612));
#239690=CARTESIAN_POINT('Ctrl Pts',(44.899651414889,-59.453345274133,-46.3433508942001));
#239691=CARTESIAN_POINT('Ctrl Pts',(45.1492944950089,-59.3870507353323,
-46.3287883811931));
#239692=CARTESIAN_POINT('Ctrl Pts',(45.616966533528,-59.16056274243,-46.3015075122795));
#239693=CARTESIAN_POINT('Ctrl Pts',(45.8292134984025,-58.9998603054208,
-46.2880068140626));
#239694=CARTESIAN_POINT('Ctrl Pts',(46.1785109975564,-58.6060430867782,
-46.2579240535827));
#239695=CARTESIAN_POINT('Ctrl Pts',(46.3124015001476,-58.3770974501211,
-46.2424530042404));
#239696=CARTESIAN_POINT('Ctrl Pts',(46.4809988880742,-57.8893355595287,
-46.2128947527779));
#239697=CARTESIAN_POINT('Ctrl Pts',(46.5174955209621,-57.6363536693044,
-46.1996067695942));
#239698=CARTESIAN_POINT('Ctrl Pts',(46.4936168806862,-57.1184425749291,
-46.1727463996494));
#239699=CARTESIAN_POINT('Ctrl Pts',(46.4288444702513,-56.8586490605961,
-46.1577329169946));
#239700=CARTESIAN_POINT('Ctrl Pts',(46.2041759466876,-56.3844779714447,
-46.1272258395355));
#239701=CARTESIAN_POINT('Ctrl Pts',(46.0483810452414,-56.173723684135,-46.112034905182));
#239702=CARTESIAN_POINT('Ctrl Pts',(45.6684898985691,-55.8267904777021,
-46.0834283234764));
#239703=CARTESIAN_POINT('Ctrl Pts',(45.4492645527083,-55.6925164292725,
-46.0711098721726));
#239704=CARTESIAN_POINT('Ctrl Pts',(44.9609109157122,-55.5092348402656,
-46.0426225766812));
#239705=CARTESIAN_POINT('Ctrl Pts',(44.6948966776886,-55.466421146957,-46.0271050794631));
#239706=CARTESIAN_POINT('Ctrl Pts',(44.1719552637017,-55.4872490067109,
-45.9966001636472));
#239707=CARTESIAN_POINT('Ctrl Pts',(43.9198615833972,-55.5467139895591,
-45.9818946989627));
#239708=CARTESIAN_POINT('Ctrl Pts',(43.4476238767116,-55.7596422861188,
-45.9543474994061));
#239709=CARTESIAN_POINT('Ctrl Pts',(43.2327420701107,-55.9127100154752,
-45.9412865529017));
#239710=CARTESIAN_POINT('Ctrl Pts',(42.8725171468024,-56.2944482407933,
-45.9114952842631));
#239711=CARTESIAN_POINT('Ctrl Pts',(42.7313301285655,-56.5199282406862,
-45.8959864974339));
#239712=CARTESIAN_POINT('Ctrl Pts',(42.5479060980174,-57.0036014693219,
-45.8662023538604));
#239713=CARTESIAN_POINT('Ctrl Pts',(42.5039330557245,-57.2558153013869,
-45.8524128961093));
#239714=CARTESIAN_POINT('Ctrl Pts',(42.5127439979152,-57.7745160849174,
-45.8259521070579));
#239715=CARTESIAN_POINT('Ctrl Pts',(42.5699147052662,-58.0360366126589,
-45.8110730952231));
#239716=CARTESIAN_POINT('Ctrl Pts',(42.7809365385862,-58.5171802899984,
-45.7806118039836));
#239717=CARTESIAN_POINT('Ctrl Pts',(42.931066783459,-58.7329207418088,-45.7653341969811));
#239718=CARTESIAN_POINT('Ctrl Pts',(43.3010156764702,-59.0903304477651,
-45.7364883443148));
#239719=CARTESIAN_POINT('Ctrl Pts',(43.5156109547163,-59.2303813196796,
-45.7240865877101));
#239720=CARTESIAN_POINT('Ctrl Pts',(43.9911480609499,-59.4249145608405,
-45.6963469231798));
#239721=CARTESIAN_POINT('Ctrl Pts',(44.2483722690796,-59.475452478349,-45.6813421777057));
#239722=CARTESIAN_POINT('Ctrl Pts',(44.5079524583206,-59.475452478349,-45.6662));
#239723=CARTESIAN_POINT('Origin',(44.5079524583206,-57.475452478349,235.35105));
#239724=CARTESIAN_POINT('',(44.5079524583206,-59.475452478349,-44.9662));
#239725=CARTESIAN_POINT('',(44.5079524583206,-59.475452478349,-45.1249500000001));
#239726=CARTESIAN_POINT('',(44.5079524583206,-59.475452478349,235.35105));
#239727=CARTESIAN_POINT('Ctrl Pts',(44.5079524583206,-59.475452478349,-45.1249500000001));
#239728=CARTESIAN_POINT('Ctrl Pts',(44.3289485674432,-59.475452478349,-45.1353918936346));
#239729=CARTESIAN_POINT('Ctrl Pts',(44.1503748551903,-59.4514192683433,
-45.1458086935161));
#239730=CARTESIAN_POINT('Ctrl Pts',(43.732385405699,-59.3363422420862,-45.1701914114031));
#239731=CARTESIAN_POINT('Ctrl Pts',(43.5027963386504,-59.2230401662548,
-45.1826488257283));
#239732=CARTESIAN_POINT('Ctrl Pts',(43.0869374091872,-58.9080994510816,
-45.2106882663391));
#239733=CARTESIAN_POINT('Ctrl Pts',(42.9080664507182,-58.7051234786716,
-45.2261593062883));
#239734=CARTESIAN_POINT('Ctrl Pts',(42.6460245302134,-58.249764899943,-45.2568060679619));
#239735=CARTESIAN_POINT('Ctrl Pts',(42.5618699260756,-58.0037788926928,
-45.2716873349057));
#239736=CARTESIAN_POINT('Ctrl Pts',(42.4913598877592,-57.4922932120912,
-45.2995831872859));
#239737=CARTESIAN_POINT('Ctrl Pts',(42.5060818538212,-57.2316212385311,
-45.3122133434975));
#239738=CARTESIAN_POINT('Ctrl Pts',(42.6354663213177,-56.7246010300115,
-45.3416007793467));
#239739=CARTESIAN_POINT('Ctrl Pts',(42.7510853474001,-56.4837937980965,
-45.3571381364555));
#239740=CARTESIAN_POINT('Ctrl Pts',(43.0633231251013,-56.0690871789363,
-45.3871952822316));
#239741=CARTESIAN_POINT('Ctrl Pts',(43.2539216026626,-55.8967600573789,
-45.4014600516205));
#239742=CARTESIAN_POINT('Ctrl Pts',(43.6984473177722,-55.627495460869,-45.4280281338647));
#239743=CARTESIAN_POINT('Ctrl Pts',(43.9502613805181,-55.5365564921131,
-45.4424180204615));
#239744=CARTESIAN_POINT('Ctrl Pts',(44.4710062930961,-55.4587926522892,
-45.4727948070285));
#239745=CARTESIAN_POINT('Ctrl Pts',(44.7345321573533,-55.4712190921781,
-45.4881671491102));
#239746=CARTESIAN_POINT('Ctrl Pts',(45.2342145752133,-55.5948235845074,
-45.517315290152));
#239747=CARTESIAN_POINT('Ctrl Pts',(45.4663606805312,-55.7018539653741,
-45.5299713266606));
#239748=CARTESIAN_POINT('Ctrl Pts',(45.8880149955959,-56.0037936314747,
-45.5575230104231));
#239749=CARTESIAN_POINT('Ctrl Pts',(46.0707759682939,-56.1995620811647,
-45.5727433984171));
#239750=CARTESIAN_POINT('Ctrl Pts',(46.3456644749568,-56.6450653435323,
-45.6032669798511));
#239751=CARTESIAN_POINT('Ctrl Pts',(46.4374570994028,-56.8891365027887,
-45.6182742878118));
#239752=CARTESIAN_POINT('Ctrl Pts',(46.5228815768366,-57.3973557454645,
-45.6464401302699));
#239753=CARTESIAN_POINT('Ctrl Pts',(46.5162444921619,-57.6565754485845,
-45.6588581461298));
#239754=CARTESIAN_POINT('Ctrl Pts',(46.4034008475248,-58.166614580002,-45.6879156517078));
#239755=CARTESIAN_POINT('Ctrl Pts',(46.295070642816,-58.4117320342241,-45.7034581626441));
#239756=CARTESIAN_POINT('Ctrl Pts',(45.9948641831446,-58.8371781813898,
-45.7337069360488));
#239757=CARTESIAN_POINT('Ctrl Pts',(45.8090163519768,-59.0157376485121,
-45.748147991477));
#239758=CARTESIAN_POINT('Ctrl Pts',(45.3715180164748,-59.29886832691,-45.7752115972674));
#239759=CARTESIAN_POINT('Ctrl Pts',(45.1218896599051,-59.3973609193807,
-45.7891369965743));
#239760=CARTESIAN_POINT('Ctrl Pts',(44.7436924583087,-59.4650367847731,
-45.8111985000008));
#239761=CARTESIAN_POINT('Ctrl Pts',(44.6257987552545,-59.475452478349,-45.8180756326789));
#239762=CARTESIAN_POINT('Ctrl Pts',(44.5079524583206,-59.475452478349,-45.8249500000001));
#239763=CARTESIAN_POINT('Ctrl Pts',(44.5079524583206,-59.475452478349,-45.6662));
#239764=CARTESIAN_POINT('Ctrl Pts',(44.5157509961426,-59.475452478349,-45.6657450852937));
#239765=CARTESIAN_POINT('Ctrl Pts',(44.5235516604141,-59.4754068654962,
-45.6652900465444));
#239766=CARTESIAN_POINT('Ctrl Pts',(44.7886381494436,-59.472304928927,-45.6498266680177));
#239767=CARTESIAN_POINT('Ctrl Pts',(45.0429716896782,-59.4196722948256,
-45.6349905448373));
#239768=CARTESIAN_POINT('Ctrl Pts',(45.5196054658849,-59.2201090456352,
-45.6071869078919));
#239769=CARTESIAN_POINT('Ctrl Pts',(45.7370574577538,-59.0743841677975,
-45.5944595061318));
#239770=CARTESIAN_POINT('Ctrl Pts',(46.1077220718494,-58.7045045479164,
-45.5649628213031));
#239771=CARTESIAN_POINT('Ctrl Pts',(46.2559338267876,-58.4826175982597,
-45.5494306605658));
#239772=CARTESIAN_POINT('Ctrl Pts',(46.4537453137754,-58.0032564081277,
-45.5194447190478));
#239773=CARTESIAN_POINT('Ctrl Pts',(46.5050493459787,-57.7517456048985,
-45.5052424913214));
#239774=CARTESIAN_POINT('Ctrl Pts',(46.5107317100971,-57.2323610559215,
-45.4788384098993));
#239775=CARTESIAN_POINT('Ctrl Pts',(46.4609415843893,-56.9693311808515,
-45.4642605386169));
#239776=CARTESIAN_POINT('Ctrl Pts',(46.2631116586593,-56.4816894154821,
-45.4338557399724));
#239777=CARTESIAN_POINT('Ctrl Pts',(46.1185508664246,-56.2613144328984,
-45.4185064474244));
#239778=CARTESIAN_POINT('Ctrl Pts',(45.75819622982,-55.8939441087259,-45.3894372352459));
#239779=CARTESIAN_POINT('Ctrl Pts',(45.5479104800947,-55.7483896228915,
-45.3768642179368));
#239780=CARTESIAN_POINT('Ctrl Pts',(45.0733945528864,-55.5387974566262,
-45.349184122183));
#239781=CARTESIAN_POINT('Ctrl Pts',(44.8118810224575,-55.4809731764661,
-45.3339291662413));
#239782=CARTESIAN_POINT('Ctrl Pts',(44.2887266335646,-55.4708223858735,
-45.3034118268891));
#239783=CARTESIAN_POINT('Ctrl Pts',(44.0321282941721,-55.5158043248852,
-45.2884435904246));
#239784=CARTESIAN_POINT('Ctrl Pts',(43.5507578965307,-55.7006049862007,
-45.2603636505621));
#239785=CARTESIAN_POINT('Ctrl Pts',(43.3304798078508,-55.8384219509829,
-45.2478901323969));
#239786=CARTESIAN_POINT('Ctrl Pts',(42.9486499874786,-56.1952720441168,
-45.2187260232862));
#239787=CARTESIAN_POINT('Ctrl Pts',(42.7928819508842,-56.4130014215983,
-45.2031835038493));
#239788=CARTESIAN_POINT('Ctrl Pts',(42.5794177640479,-56.8873761501774,
-45.1729929320579));
#239789=CARTESIAN_POINT('Ctrl Pts',(42.5201861094759,-57.1379495293302,
-45.1586068389411));
#239790=CARTESIAN_POINT('Ctrl Pts',(42.4986533657732,-57.6593362115786,
-45.1316393107151));
#239791=CARTESIAN_POINT('Ctrl Pts',(42.5410319282442,-57.9253301041547,
-45.1175081973955));
#239792=CARTESIAN_POINT('Ctrl Pts',(42.7259619103225,-58.4204550598936,
-45.0871016101847));
#239793=CARTESIAN_POINT('Ctrl Pts',(42.8648098408148,-58.6453274923437,
-45.0716917399305));
#239794=CARTESIAN_POINT('Ctrl Pts',(43.2154792362735,-59.0226036586122,
-45.0424045891495));
#239795=CARTESIAN_POINT('Ctrl Pts',(43.4215625673015,-59.1736538398396,
-45.0295727436427));
#239796=CARTESIAN_POINT('Ctrl Pts',(43.8899394289875,-59.395973850698,-45.0022507600444));
#239797=CARTESIAN_POINT('Ctrl Pts',(44.1497471451407,-59.4608969960235,
-44.9870953099354));
#239798=CARTESIAN_POINT('Ctrl Pts',(44.4457278897632,-59.4747271146837,
-44.9698297664991));
#239799=CARTESIAN_POINT('Ctrl Pts',(44.4768532435007,-59.475452478349,-44.9680141208644));
#239800=CARTESIAN_POINT('Ctrl Pts',(44.5079524583206,-59.475452478349,-44.9662));
#239801=CARTESIAN_POINT('Origin',(44.5079524583206,-57.475452478349,235.35105));
#239802=CARTESIAN_POINT('',(44.5079524583206,-59.475452478349,-44.2662));
#239803=CARTESIAN_POINT('',(44.5079524583206,-59.475452478349,-44.4249500000001));
#239804=CARTESIAN_POINT('',(44.5079524583206,-59.475452478349,235.35105));
#239805=CARTESIAN_POINT('Ctrl Pts',(44.5079524583206,-59.475452478349,-44.4249500000001));
#239806=CARTESIAN_POINT('Ctrl Pts',(44.283285075366,-59.475452478349,-44.4380555973391));
#239807=CARTESIAN_POINT('Ctrl Pts',(44.059893467904,-59.4375926222143,-44.4510867744411));
#239808=CARTESIAN_POINT('Ctrl Pts',(43.6059949604271,-59.2787307478272,
-44.4775641873773));
#239809=CARTESIAN_POINT('Ctrl Pts',(43.383184097842,-59.1488432296001,-44.4898858079534));
#239810=CARTESIAN_POINT('Ctrl Pts',(42.995841679397,-58.8098650069049,-44.5183078473687));
#239811=CARTESIAN_POINT('Ctrl Pts',(42.8358801787966,-58.6029666331937,
-44.533425513915));
#239812=CARTESIAN_POINT('Ctrl Pts',(42.601071027619,-58.1343109279424,-44.5639497326963));
#239813=CARTESIAN_POINT('Ctrl Pts',(42.5306006882951,-57.8759703986851,
-44.5790560028278));
#239814=CARTESIAN_POINT('Ctrl Pts',(42.4953680131583,-57.3587530563562,
-44.6062124850538));
#239815=CARTESIAN_POINT('Ctrl Pts',(42.5262810842606,-57.1051357115976,
-44.6191923023582));
#239816=CARTESIAN_POINT('Ctrl Pts',(42.6838553056735,-56.6144270951757,
-44.6485779079306));
#239817=CARTESIAN_POINT('Ctrl Pts',(42.8122660918713,-56.3830514562381,
-44.6640118914276));
#239818=CARTESIAN_POINT('Ctrl Pts',(43.1532878715183,-55.9803118855556,
-44.694304017461));
#239819=CARTESIAN_POINT('Ctrl Pts',(43.3635660886199,-55.8138619965146,
-44.7081941284342));
#239820=CARTESIAN_POINT('Ctrl Pts',(43.827805132134,-55.577383175988,-44.7352747393058));
#239821=CARTESIAN_POINT('Ctrl Pts',(44.0755315270225,-55.5061283512199,
-44.7497254456743));
#239822=CARTESIAN_POINT('Ctrl Pts',(44.594254452503,-55.4597669706736,-44.779984282994));
#239823=CARTESIAN_POINT('Ctrl Pts',(44.8606946758697,-55.4889912576162,
-44.795526629357));
#239824=CARTESIAN_POINT('Ctrl Pts',(45.3584959850637,-55.6471822161361,
-44.82456503906));
#239825=CARTESIAN_POINT('Ctrl Pts',(45.5860068450698,-55.7714009808656,
-44.8369743929198));
#239826=CARTESIAN_POINT('Ctrl Pts',(45.9828340158242,-56.1001338486245,
-44.8651554945815));
#239827=CARTESIAN_POINT('Ctrl Pts',(46.147989864832,-56.3019840430269,-44.880169638284));
#239828=CARTESIAN_POINT('Ctrl Pts',(46.3955717459517,-56.7632686316113,
-44.9106940198552));
#239829=CARTESIAN_POINT('Ctrl Pts',(46.4732810656571,-57.01956335981,-44.9259080768327));
#239830=CARTESIAN_POINT('Ctrl Pts',(46.5230334210941,-57.5357649746953,
-44.9534367370643));
#239831=CARTESIAN_POINT('Ctrl Pts',(46.4992097142434,-57.7902666281475,
-44.9661088246886));
#239832=CARTESIAN_POINT('Ctrl Pts',(46.3555497542076,-58.2845863549509,
-44.9952710242482));
#239833=CARTESIAN_POINT('Ctrl Pts',(46.2341137483518,-58.5188473904699,
-45.0106473413109));
#239834=CARTESIAN_POINT('Ctrl Pts',(45.9125846210923,-58.9216731144069,
-45.0403752844146));
#239835=CARTESIAN_POINT('Ctrl Pts',(45.717770169913,-59.0881462927263,-45.0543773001572));
#239836=CARTESIAN_POINT('Ctrl Pts',(45.266724227889,-59.3448244804227,-45.0806883134419));
#239837=CARTESIAN_POINT('Ctrl Pts',(45.0125641481616,-59.4288087849436,
-45.0955143180927));
#239838=CARTESIAN_POINT('Ctrl Pts',(44.6691833888416,-59.4705837361307,
-45.1155448623864));
#239839=CARTESIAN_POINT('Ctrl Pts',(44.5885243462159,-59.475452478349,-45.1202499732062));
#239840=CARTESIAN_POINT('Ctrl Pts',(44.5079524583206,-59.475452478349,-45.1249500000001));
#239841=CARTESIAN_POINT('Ctrl Pts',(44.5079524583206,-59.475452478349,-44.9662));
#239842=CARTESIAN_POINT('Ctrl Pts',(44.7350982804284,-59.475452478349,-44.9529498270437));
#239843=CARTESIAN_POINT('Ctrl Pts',(44.9608496675886,-59.436753282891,-44.939780996126));
#239844=CARTESIAN_POINT('Ctrl Pts',(45.4168910322583,-59.2752972816714,
-44.913178583187));
#239845=CARTESIAN_POINT('Ctrl Pts',(45.6396497792772,-59.1442463664141,
-44.9008298723489));
#239846=CARTESIAN_POINT('Ctrl Pts',(46.0309656080461,-58.7987492821338,
-44.8719626209811));
#239847=CARTESIAN_POINT('Ctrl Pts',(46.1931757392732,-58.5848144534829,
-44.856423900699));
#239848=CARTESIAN_POINT('Ctrl Pts',(46.4200729111258,-58.1151528227274,
-44.8260796304873));
#239849=CARTESIAN_POINT('Ctrl Pts',(46.4861472020093,-57.8655894967344,
-44.8115449864937));
#239850=CARTESIAN_POINT('Ctrl Pts',(46.5212095777296,-57.346811429197,-44.7843146263861));
#239851=CARTESIAN_POINT('Ctrl Pts',(46.4866571426256,-57.0823550036448,
-44.7707203300023));
#239852=CARTESIAN_POINT('Ctrl Pts',(46.317248794841,-56.5836176484322,-44.7405839653918));
#239853=CARTESIAN_POINT('Ctrl Pts',(46.184686832037,-56.3540763338423,-44.7251215725803));
#239854=CARTESIAN_POINT('Ctrl Pts',(45.8445238885936,-55.966225588339,-44.6956066518184));
#239855=CARTESIAN_POINT('Ctrl Pts',(45.6428432591009,-55.8092718386522,
-44.6824019633789));
#239856=CARTESIAN_POINT('Ctrl Pts',(45.1810933209143,-55.5735574485446,
-44.655466550318));
#239857=CARTESIAN_POINT('Ctrl Pts',(44.9233064714477,-55.5011783070721,
-44.6404289840991));
#239858=CARTESIAN_POINT('Ctrl Pts',(44.4002298059176,-55.4615698607251,
-44.6099161786099));
#239859=CARTESIAN_POINT('Ctrl Pts',(44.1401193669863,-55.4925138456731,
-44.5947430696722));
#239860=CARTESIAN_POINT('Ctrl Pts',(43.6505122983323,-55.6506718760281,
-44.566182657334));
#239861=CARTESIAN_POINT('Ctrl Pts',(43.4251218828497,-55.774716568916,-44.5538688042061));
#239862=CARTESIAN_POINT('Ctrl Pts',(43.024056446069,-56.1082818723179,-44.5253199607502));
#239863=CARTESIAN_POINT('Ctrl Pts',(42.855220178695,-56.3180624394509,-44.5097978437643));
#239864=CARTESIAN_POINT('Ctrl Pts',(42.614417600695,-56.78241231548,-44.4793163392209));
#239865=CARTESIAN_POINT('Ctrl Pts',(42.5412209361295,-57.030724894256,-44.464637144762));
#239866=CARTESIAN_POINT('Ctrl Pts',(42.4921545656837,-57.5467009642602,
-44.4371398865358));
#239867=CARTESIAN_POINT('Ctrl Pts',(42.5187614856851,-57.8096136419463,
-44.4240035333981));
#239868=CARTESIAN_POINT('Ctrl Pts',(42.6722426971373,-58.3118196887116,
-44.3941564783888));
#239869=CARTESIAN_POINT('Ctrl Pts',(42.7981854105964,-58.5459812622667,
-44.3786537400878));
#239870=CARTESIAN_POINT('Ctrl Pts',(43.1274214550792,-58.9446382608674,
-44.3489116086462));
#239871=CARTESIAN_POINT('Ctrl Pts',(43.3246810481936,-59.1076771589167,
-44.3352241655906));
#239872=CARTESIAN_POINT('Ctrl Pts',(43.7795874523815,-59.3568840913519,
-44.3086879586797));
#239873=CARTESIAN_POINT('Ctrl Pts',(44.0351047616619,-59.4367442456094,
-44.293782782305));
#239874=CARTESIAN_POINT('Ctrl Pts',(44.3683379691323,-59.4718019510095,
-44.2743441785359));
#239875=CARTESIAN_POINT('Ctrl Pts',(44.4381850249233,-59.475452478349,-44.2702697669481));
#239876=CARTESIAN_POINT('Ctrl Pts',(44.5079524583206,-59.475452478349,-44.2662));
#239877=CARTESIAN_POINT('Origin',(44.5079524583206,-57.475452478349,235.35105));
#239878=CARTESIAN_POINT('',(44.5079524583206,-59.475452478349,-43.5662));
#239879=CARTESIAN_POINT('',(44.5079524583206,-59.475452478349,-43.7249500000001));
#239880=CARTESIAN_POINT('',(44.5079524583206,-59.475452478349,235.35105));
#239881=CARTESIAN_POINT('Ctrl Pts',(44.5079524583206,-59.475452478349,-43.7249500000001));
#239882=CARTESIAN_POINT('Ctrl Pts',(44.2436230538572,-59.475452478349,-43.7403692152604));
#239883=CARTESIAN_POINT('Ctrl Pts',(43.9818301375788,-59.4230492364018,
-43.7556404687101));
#239884=CARTESIAN_POINT('Ctrl Pts',(43.5034961874671,-59.2234533329351,
-43.7835432824667));
#239885=CARTESIAN_POINT('Ctrl Pts',(43.2899979499798,-59.0820135561926,
-43.7959798486351));
#239886=CARTESIAN_POINT('Ctrl Pts',(42.9224596309662,-58.7220874350348,
-43.8248825175301));
#239887=CARTESIAN_POINT('Ctrl Pts',(42.7737196678051,-58.5051659915419,
-43.8401792361626));
#239888=CARTESIAN_POINT('Ctrl Pts',(42.5660236645173,-58.0223988037884,
-43.8706255407665));
#239889=CARTESIAN_POINT('Ctrl Pts',(42.5106943495575,-57.7604958177748,
-43.885470166407));
#239890=CARTESIAN_POINT('Ctrl Pts',(42.5055223779315,-57.2416260954196,
-43.9118333532936));
#239891=CARTESIAN_POINT('Ctrl Pts',(42.5513139929662,-56.9895851188607,
-43.9257598308716));
#239892=CARTESIAN_POINT('Ctrl Pts',(42.7383531367516,-56.5069313848787,
-43.9555979122654));
#239893=CARTESIAN_POINT('Ctrl Pts',(42.8813051785868,-56.2823301133647,
-43.9711137872188));
#239894=CARTESIAN_POINT('Ctrl Pts',(43.2441597913404,-55.9035495656452,
-44.0008323387365));
#239895=CARTESIAN_POINT('Ctrl Pts',(43.459683452574,-55.7523269100348,-44.0138009746649));
#239896=CARTESIAN_POINT('Ctrl Pts',(43.9330253986036,-55.5427265246074,
-44.0414125881832));
#239897=CARTESIAN_POINT('Ctrl Pts',(44.1856933327387,-55.484953837572,-44.0561515510078));
#239898=CARTESIAN_POINT('Ctrl Pts',(44.7091334295394,-55.4677711128755,
-44.0866855566545));
#239899=CARTESIAN_POINT('Ctrl Pts',(44.9750329771393,-55.5125150255964,
-44.1021963635978));
#239900=CARTESIAN_POINT('Ctrl Pts',(45.4620095151533,-55.69933629957,-44.1306033283153));
#239901=CARTESIAN_POINT('Ctrl Pts',(45.6800767517487,-55.8350428842699,
-44.1429331696617));
#239902=CARTESIAN_POINT('Ctrl Pts',(46.0575155752788,-56.1845748082541,
-44.1715995076749));
#239903=CARTESIAN_POINT('Ctrl Pts',(46.2119240342626,-56.3965760234397,
-44.186812996611));
#239904=CARTESIAN_POINT('Ctrl Pts',(46.4332379459014,-56.8725081731857,
-44.217311196743));
#239905=CARTESIAN_POINT('Ctrl Pts',(46.4961347650193,-57.1327501044986,
-44.2322926278467));
#239906=CARTESIAN_POINT('Ctrl Pts',(46.5162880877179,-57.650870144721,-44.2590548982529));
#239907=CARTESIAN_POINT('Ctrl Pts',(46.4779505554758,-57.903654212139,-44.2724570142984));
#239908=CARTESIAN_POINT('Ctrl Pts',(46.3057086310559,-58.3904246214665,
-44.3020714769441));
#239909=CARTESIAN_POINT('Ctrl Pts',(46.1700163462968,-58.6185391547815,
-44.3175530924643));
#239910=CARTESIAN_POINT('Ctrl Pts',(45.818011324453,-59.0093951996859,-44.3475652293412));
#239911=CARTESIAN_POINT('Ctrl Pts',(45.6051158043426,-59.1682108024561,
-44.3609488048155));
#239912=CARTESIAN_POINT('Ctrl Pts',(45.1363159779013,-59.3913787735358,
-44.3882954613579));
#239913=CARTESIAN_POINT('Ctrl Pts',(44.886056630806,-59.4560112053162,-44.4028939232718));
#239914=CARTESIAN_POINT('Ctrl Pts',(44.5896200096801,-59.4742032392965,
-44.4201860595041));
#239915=CARTESIAN_POINT('Ctrl Pts',(44.5487651838402,-59.475452478349,-44.4225692576781));
#239916=CARTESIAN_POINT('Ctrl Pts',(44.5079524583206,-59.475452478349,-44.4249500000001));
#239917=CARTESIAN_POINT('Ctrl Pts',(44.5079524583206,-59.475452478349,-44.2662));
#239918=CARTESIAN_POINT('Ctrl Pts',(44.6974398807997,-59.475452478349,-44.255146567022));
#239919=CARTESIAN_POINT('Ctrl Pts',(44.8863399620151,-59.4485215007381,
-44.2441273956178));
#239920=CARTESIAN_POINT('Ctrl Pts',(45.3128592425604,-59.3238888304483,
-44.2192471042526));
#239921=CARTESIAN_POINT('Ctrl Pts',(45.5409384166266,-59.2067880626703,
-44.2068684444618));
#239922=CARTESIAN_POINT('Ctrl Pts',(45.9515891183784,-58.8852182334852,
-44.1786460199261));
#239923=CARTESIAN_POINT('Ctrl Pts',(46.1269323684712,-58.6797772042736,
-44.1631533413656));
#239924=CARTESIAN_POINT('Ctrl Pts',(46.3814819126568,-58.2211232935122,
-44.1325586332614));
#239925=CARTESIAN_POINT('Ctrl Pts',(46.4617598831783,-57.9742579987788,
-44.1177460148224));
#239926=CARTESIAN_POINT('Ctrl Pts',(46.5246934873947,-57.4611581443313,
-44.089989596696));
#239927=CARTESIAN_POINT('Ctrl Pts',(46.5058092502291,-57.1997136035875,
-44.0772076723267));
#239928=CARTESIAN_POINT('Ctrl Pts',(46.3679525499589,-56.6943283526042,
-44.047655724716));
#239929=CARTESIAN_POINT('Ctrl Pts',(46.2486627364475,-56.4558091263641,
-44.0321268887843));
#239930=CARTESIAN_POINT('Ctrl Pts',(45.9304060416829,-56.046730632363,-44.0021785137235));
#239931=CARTESIAN_POINT('Ctrl Pts',(45.7374537689556,-55.8776432070875,
-43.9880087554335));
#239932=CARTESIAN_POINT('Ctrl Pts',(45.2892709116404,-55.6154130555524,
-43.9616893736779));
#239933=CARTESIAN_POINT('Ctrl Pts',(45.0361497099667,-55.5283193103871,
-43.947011506346));
#239934=CARTESIAN_POINT('Ctrl Pts',(44.514698625747,-55.4585153078826,-43.9165935264332));
#239935=CARTESIAN_POINT('Ctrl Pts',(44.2517792160158,-55.4748358885902,
-43.9012565608655));
#239936=CARTESIAN_POINT('Ctrl Pts',(43.7541456155875,-55.6056693303521,
-43.8722279341739));
#239937=CARTESIAN_POINT('Ctrl Pts',(43.5234314201282,-55.7161871084399,
-43.8596929656892));
#239938=CARTESIAN_POINT('Ctrl Pts',(43.1061464323116,-56.0244873685016,
-43.8319473952074));
#239939=CARTESIAN_POINT('Ctrl Pts',(42.9263072608162,-56.2229661580715,
-43.8166753050625));
#239940=CARTESIAN_POINT('Ctrl Pts',(42.6582653170492,-56.6722124621946,
-43.7861623235068));
#239941=CARTESIAN_POINT('Ctrl Pts',(42.5701785351436,-56.9172430758713,
-43.7712146327592));
#239942=CARTESIAN_POINT('Ctrl Pts',(42.49198937607,-57.4270617299001,-43.7431790211196));
#239943=CARTESIAN_POINT('Ctrl Pts',(42.5025312701276,-57.6869741329687,
-43.7306724356183));
#239944=CARTESIAN_POINT('Ctrl Pts',(42.6233762732508,-58.1955810180198,
-43.7014539115192));
#239945=CARTESIAN_POINT('Ctrl Pts',(42.7352520455834,-58.4386397034046,
-43.6859119933839));
#239946=CARTESIAN_POINT('Ctrl Pts',(43.0413240068088,-58.8589326285793,
-43.6557524740846));
#239947=CARTESIAN_POINT('Ctrl Pts',(43.2294952386905,-59.0344930600324,
-43.6413951585317));
#239948=CARTESIAN_POINT('Ctrl Pts',(43.6719449506611,-59.3118772021662,
-43.614477441967));
#239949=CARTESIAN_POINT('Ctrl Pts',(43.9244866719363,-59.4070341679364,
-43.6002355042056));
#239950=CARTESIAN_POINT('Ctrl Pts',(44.2942567973847,-59.4668961143992,
-43.5786655802211));
#239951=CARTESIAN_POINT('Ctrl Pts',(44.4011409321713,-59.475452478349,-43.5724306723587));
#239952=CARTESIAN_POINT('Ctrl Pts',(44.5079524583206,-59.475452478349,-43.5662));
#239953=CARTESIAN_POINT('Origin',(44.5079524583206,-57.475452478349,235.35105));
#239954=CARTESIAN_POINT('',(44.5079524583206,-59.475452478349,-42.8662));
#239955=CARTESIAN_POINT('',(44.5079524583206,-59.475452478349,-43.0249500000001));
#239956=CARTESIAN_POINT('',(44.5079524583206,-59.475452478349,235.35105));
#239957=CARTESIAN_POINT('Ctrl Pts',(44.5079524583206,-59.475452478349,-43.0249500000001));
#239958=CARTESIAN_POINT('Ctrl Pts',(44.4722388018602,-59.475452478349,-43.0270332966269));
#239959=CARTESIAN_POINT('Ctrl Pts',(44.4364923191056,-59.4744958911332,
-43.0291185081211));
#239960=CARTESIAN_POINT('Ctrl Pts',(44.1359989856678,-59.4583660521796,
-43.046647285905));
#239961=CARTESIAN_POINT('Ctrl Pts',(43.8766562345333,-59.3916474688325,
-43.0617756130545));
#239962=CARTESIAN_POINT('Ctrl Pts',(43.4098580688571,-59.1661054233476,
-43.0890055060523));
#239963=CARTESIAN_POINT('Ctrl Pts',(43.2048354570692,-59.0136468877318,
-43.1019175121918));
#239964=CARTESIAN_POINT('Ctrl Pts',(42.8566633521768,-58.6338410191185,
-43.1312596212102));
#239965=CARTESIAN_POINT('Ctrl Pts',(42.7193017262729,-58.4078389051919,
-43.1466832103306));
#239966=CARTESIAN_POINT('Ctrl Pts',(42.5380790697365,-57.9118297106231,
-43.1770263373216));
#239967=CARTESIAN_POINT('Ctrl Pts',(42.4975777986357,-57.6462053086828,
-43.1910212889106));
#239968=CARTESIAN_POINT('Ctrl Pts',(42.5223320692649,-57.1254309277759,
-43.2180518460084));
#239969=CARTESIAN_POINT('Ctrl Pts',(42.5831890276793,-56.8750805503825,
-43.2324740781846));
#239970=CARTESIAN_POINT('Ctrl Pts',(42.7998504127542,-56.4017908720666,
-43.2627030868609));
#239971=CARTESIAN_POINT('Ctrl Pts',(42.9571553464097,-56.1849454547931,
-43.2782457764289));
#239972=CARTESIAN_POINT('Ctrl Pts',(43.341250259259,-55.8307825783057,-43.3073401975271));
#239973=CARTESIAN_POINT('Ctrl Pts',(43.5621134093721,-55.6945771218292,
-43.3197760554782));
#239974=CARTESIAN_POINT('Ctrl Pts',(44.0444488513265,-55.5128328693985,
-43.3479122895921));
#239975=CARTESIAN_POINT('Ctrl Pts',(44.3014880521876,-55.4694472573116,
-43.3629062429757));
#239976=CARTESIAN_POINT('Ctrl Pts',(44.8247182520767,-55.4829727685835,
-43.3934280046359));
#239977=CARTESIAN_POINT('Ctrl Pts',(45.0858469543679,-55.5424775393722,
-43.4086605122695));
#239978=CARTESIAN_POINT('Ctrl Pts',(45.5589242140665,-55.7550817256449,
-43.4362566857519));
#239979=CARTESIAN_POINT('Ctrl Pts',(45.7682135630241,-55.9019273753259,
-43.4488827073125));
#239980=CARTESIAN_POINT('Ctrl Pts',(46.1263016611398,-56.2716293412843,
-43.4780036023445));
#239981=CARTESIAN_POINT('Ctrl Pts',(46.2695332415759,-56.4930732678543,
-43.4933681272861));
#239982=CARTESIAN_POINT('Ctrl Pts',(46.4642258513371,-56.9821704159436,
-43.523754944122));
#239983=CARTESIAN_POINT('Ctrl Pts',(46.5122916603142,-57.2455411256538,
-43.5382087440721));
#239984=CARTESIAN_POINT('Ctrl Pts',(46.5031811471748,-57.7650743711394,
-43.5647203250463));
#239985=CARTESIAN_POINT('Ctrl Pts',(46.4501535560201,-58.0164025409574,
-43.5789635969404));
#239986=CARTESIAN_POINT('Ctrl Pts',(46.2489308158815,-58.4947227266461,
-43.6089964437248));
#239987=CARTESIAN_POINT('Ctrl Pts',(46.0990677974513,-58.7157274688955,
-43.6245321988292));
#239988=CARTESIAN_POINT('Ctrl Pts',(45.7259584296462,-59.0827848377704,
-43.6539576140789));
#239989=CARTESIAN_POINT('Ctrl Pts',(45.5078951969149,-59.2267831259288,
-43.6666200069155));
#239990=CARTESIAN_POINT('Ctrl Pts',(45.0302272821456,-59.4231562527943,
-43.6944839686103));
#239991=CARTESIAN_POINT('Ctrl Pts',(44.7753855036338,-59.4741443929355,
-43.7093497390236));
#239992=CARTESIAN_POINT('Ctrl Pts',(44.5145975316104,-59.4754441999115,
-43.7245623707249));
#239993=CARTESIAN_POINT('Ctrl Pts',(44.511274794611,-59.475452478349,-43.7247561970498));
#239994=CARTESIAN_POINT('Ctrl Pts',(44.5079524583206,-59.475452478349,-43.7249500000001));
#239995=CARTESIAN_POINT('Ctrl Pts',(44.5079524583206,-59.475452478349,-43.5662));
#239996=CARTESIAN_POINT('Ctrl Pts',(44.6615663204189,-59.475452478349,-43.5572391913776));
#239997=CARTESIAN_POINT('Ctrl Pts',(44.815030002254,-59.4577540742531,-43.5482871432704));
#239998=CARTESIAN_POINT('Ctrl Pts',(45.2118852073288,-59.3645408368662,
-43.5251372563077));
#239999=CARTESIAN_POINT('Ctrl Pts',(45.4451992360649,-59.2603095681955,
-43.512364644595));
#240000=CARTESIAN_POINT('Ctrl Pts',(45.8703347392719,-58.9634915289442,
-43.4849701612844));
#240001=CARTESIAN_POINT('Ctrl Pts',(46.0554114531177,-58.7699314236281,
-43.4697937923094));
#240002=CARTESIAN_POINT('Ctrl Pts',(46.335759964064,-58.3275099888803,-43.4392666489761));
#240003=CARTESIAN_POINT('Ctrl Pts',(46.4305219085137,-58.0842493054552,
-43.424213679587));
#240004=CARTESIAN_POINT('Ctrl Pts',(46.5217447918344,-57.5773321239347,
-43.3959444946762));
#240005=CARTESIAN_POINT('Ctrl Pts',(46.51821469771,-57.3186506821524,-43.3835779788817));
#240006=CARTESIAN_POINT('Ctrl Pts',(46.4117517357226,-56.8075063233078,
-43.3546507425044));
#240007=CARTESIAN_POINT('Ctrl Pts',(46.3062745611358,-56.5607829365096,
-43.3391103162062));
#240008=CARTESIAN_POINT('Ctrl Pts',(46.0108052920072,-56.1312850003737,
-43.3087950219819));
#240009=CARTESIAN_POINT('Ctrl Pts',(45.8268437575018,-55.9503559439615,
-43.2942892762759));
#240010=CARTESIAN_POINT('Ctrl Pts',(45.393296353515,-55.6626715628225,-43.2671108613565));
#240011=CARTESIAN_POINT('Ctrl Pts',(45.1459586054206,-55.5615543425804,
-43.2534170252475));
#240012=CARTESIAN_POINT('Ctrl Pts',(44.6283997479283,-55.4619145925842,
-43.2232260918937));
#240013=CARTESIAN_POINT('Ctrl Pts',(44.3634911982133,-55.463494642993,-43.2077730931604));
#240014=CARTESIAN_POINT('Ctrl Pts',(43.8582876714391,-55.567021828036,-43.1783028874318));
#240015=CARTESIAN_POINT('Ctrl Pts',(43.6221045851968,-55.664542137411,-43.1651799413221));
#240016=CARTESIAN_POINT('Ctrl Pts',(43.1887206949131,-55.9490334918029,
-43.138167601352));
#240017=CARTESIAN_POINT('Ctrl Pts',(42.9982072889421,-56.1371879745595,
-43.1231057442334));
#240018=CARTESIAN_POINT('Ctrl Pts',(42.7049167935935,-56.5719506013494,
-43.0925880351531));
#240019=CARTESIAN_POINT('Ctrl Pts',(42.6030653396854,-56.8131242966944,
-43.0774337191787));
#240020=CARTESIAN_POINT('Ctrl Pts',(42.4979825906407,-57.3168591547252,
-43.048921053275));
#240021=CARTESIAN_POINT('Ctrl Pts',(42.4941611025798,-57.5743100567886,
-43.0366081460423));
#240022=CARTESIAN_POINT('Ctrl Pts',(42.5854895496084,-58.0879526889787,
-43.0079961248739));
#240023=CARTESIAN_POINT('Ctrl Pts',(42.6841124987043,-58.3383556059968,
-42.9924697304316));
#240024=CARTESIAN_POINT('Ctrl Pts',(42.9681399198854,-58.7772535078167,
-42.9620132879096));
#240025=CARTESIAN_POINT('Ctrl Pts',(43.1475109432184,-58.9637215259788,
-42.9473616140203));
#240026=CARTESIAN_POINT('Ctrl Pts',(43.5716778728517,-59.26210764927,-42.9199161640698));
#240027=CARTESIAN_POINT('Ctrl Pts',(43.8136994076378,-59.3693345857257,
-42.9066980946229));
#240028=CARTESIAN_POINT('Ctrl Pts',(44.213802706673,-59.4592184173348,-42.8833587355126));
#240029=CARTESIAN_POINT('Ctrl Pts',(44.3608300508606,-59.475452478349,-42.8747821404351));
#240030=CARTESIAN_POINT('Ctrl Pts',(44.5079524583206,-59.475452478349,-42.8662));
#240031=CARTESIAN_POINT('Origin',(44.5079524583206,-57.475452478349,235.35105));
#240032=CARTESIAN_POINT('',(44.5079524583206,-59.475452478349,-42.1661999999999));
#240033=CARTESIAN_POINT('',(44.5079524583206,-59.475452478349,-42.3249500000001));
#240034=CARTESIAN_POINT('',(44.5079524583206,-59.475452478349,235.35105));
#240035=CARTESIAN_POINT('Ctrl Pts',(44.5079524583206,-59.475452478349,-42.3249500000001));
#240036=CARTESIAN_POINT('Ctrl Pts',(44.4335108999353,-59.475452478349,-42.3292924242392));
#240037=CARTESIAN_POINT('Ctrl Pts',(44.3589857355706,-59.4712964286506,
-42.3336397254938));
#240038=CARTESIAN_POINT('Ctrl Pts',(44.0213468793765,-59.433374420538,-42.3533353254385));
#240039=CARTESIAN_POINT('Ctrl Pts',(43.7664083172945,-59.3517271833582,
-42.3682067415599));
#240040=CARTESIAN_POINT('Ctrl Pts',(43.3131668649557,-59.0992861318309,
-42.3946458262797));
#240041=CARTESIAN_POINT('Ctrl Pts',(43.1169658201907,-58.9347664927564,
-42.408465268112));
#240042=CARTESIAN_POINT('Ctrl Pts',(42.7904022899136,-58.533496628627,-42.4382614483514));
#240043=CARTESIAN_POINT('Ctrl Pts',(42.6660892211492,-58.2982418210313,
-42.4537718835088));
#240044=CARTESIAN_POINT('Ctrl Pts',(42.5164690992943,-57.7952299475756,
-42.4835470322772));
#240045=CARTESIAN_POINT('Ctrl Pts',(42.4917767288961,-57.5326848236753,
-42.4965869357688));
#240046=CARTESIAN_POINT('Ctrl Pts',(42.5442576277417,-57.0174075895169,
-42.5241484805135));
#240047=CARTESIAN_POINT('Ctrl Pts',(42.6191957453779,-56.7694320003765,
-42.5388614432612));
#240048=CARTESIAN_POINT('Ctrl Pts',(42.8633862777626,-56.3064443476726,
-42.5693729461404));
#240049=CARTESIAN_POINT('Ctrl Pts',(43.033830275666,-56.0977115237113,-42.5848890252216));
#240050=CARTESIAN_POINT('Ctrl Pts',(43.4372623221583,-55.7670832112067,
-42.6133585234516));
#240051=CARTESIAN_POINT('Ctrl Pts',(43.6633063090487,-55.6447476374709,
-42.625678974626));
#240052=CARTESIAN_POINT('Ctrl Pts',(44.1539326420176,-55.4899780632874,
-42.6542988440492));
#240053=CARTESIAN_POINT('Ctrl Pts',(44.4144355075536,-55.4608371500119,
-42.6694948445387));
#240054=CARTESIAN_POINT('Ctrl Pts',(44.9373826012068,-55.5041937692303,
-42.7000000916685));
#240055=CARTESIAN_POINT('Ctrl Pts',(45.1946358903184,-55.5784063694658,
-42.7150065335333));
#240056=CARTESIAN_POINT('Ctrl Pts',(45.654727057096,-55.8174215434278,-42.7418451849287));
#240057=CARTESIAN_POINT('Ctrl Pts',(45.8553251402743,-55.9758505920282,
-42.7551579256919));
#240058=CARTESIAN_POINT('Ctrl Pts',(46.1928475373647,-56.366330761512,-42.7847286641498));
#240059=CARTESIAN_POINT('Ctrl Pts',(46.3238168947725,-56.5970106765827,
-42.8002021259589));
#240060=CARTESIAN_POINT('Ctrl Pts',(46.4893558836183,-57.0966124757606,
-42.8302693043756));
#240061=CARTESIAN_POINT('Ctrl Pts',(46.5219705461844,-57.3606901912239,
-42.8437435608347));
#240062=CARTESIAN_POINT('Ctrl Pts',(46.4835176912486,-57.8787993498951,
-42.871039017882));
#240063=CARTESIAN_POINT('Ctrl Pts',(46.4157223067143,-58.1280791453904,
-42.8856095370046));
#240064=CARTESIAN_POINT('Ctrl Pts',(46.1854577537387,-58.5964953000075,
-42.9159891033505));
#240065=CARTESIAN_POINT('Ctrl Pts',(46.0216390045741,-58.8094454681241,
-42.9315249984287));
#240066=CARTESIAN_POINT('Ctrl Pts',(45.627956981107,-59.1520699862854,-42.9603161470866));
#240067=CARTESIAN_POINT('Ctrl Pts',(45.4045661840963,-59.2814259098854,
-42.9726475326633));
#240068=CARTESIAN_POINT('Ctrl Pts',(44.9519576094212,-59.4382730917703,
-42.9990496995194));
#240069=CARTESIAN_POINT('Ctrl Pts',(44.7305929026539,-59.475452478349,-43.0119626407473));
#240070=CARTESIAN_POINT('Ctrl Pts',(44.5079524583206,-59.475452478349,-43.0249500000001));
#240071=CARTESIAN_POINT('Ctrl Pts',(44.5079524583206,-59.475452478349,-42.8662));
#240072=CARTESIAN_POINT('Ctrl Pts',(44.6227546351814,-59.475452478349,-42.8595032063498));
#240073=CARTESIAN_POINT('Ctrl Pts',(44.737614695619,-59.4655679660078,-42.8528030361574));
#240074=CARTESIAN_POINT('Ctrl Pts',(45.1011058928316,-59.4022356541609,
-42.8315993829867));
#240075=CARTESIAN_POINT('Ctrl Pts',(45.3403292438796,-59.3115885970665,
-42.8180138742986));
#240076=CARTESIAN_POINT('Ctrl Pts',(45.7820095842752,-59.0397681873013,
-42.7913996671966));
#240077=CARTESIAN_POINT('Ctrl Pts',(45.9779068823429,-58.8572953967276,
-42.7764678084617));
#240078=CARTESIAN_POINT('Ctrl Pts',(46.2841973240556,-58.4307477847042,
-42.7459859416155));
#240079=CARTESIAN_POINT('Ctrl Pts',(46.393245926337,-58.1919155116682,-42.7307399931335));
#240080=CARTESIAN_POINT('Ctrl Pts',(46.5124415638417,-57.6915264323124,
-42.7019847238606));
#240081=CARTESIAN_POINT('Ctrl Pts',(46.5236508000073,-57.4352399244353,
-42.6896264045268));
#240082=CARTESIAN_POINT('Ctrl Pts',(46.4475620650062,-56.9192521004401,
-42.6613404002113));
#240083=CARTESIAN_POINT('Ctrl Pts',(46.3559566047958,-56.6653329466362,
-42.6458410487559));
#240084=CARTESIAN_POINT('Ctrl Pts',(46.0837290779512,-56.2172806396749,
-42.6152663062198));
#240085=CARTESIAN_POINT('Ctrl Pts',(45.9091403711885,-56.0253578881873,
-42.6004785535353));
#240086=CARTESIAN_POINT('Ctrl Pts',(45.4944319230012,-55.7163332450967,
-42.5727715376367));
#240087=CARTESIAN_POINT('Ctrl Pts',(45.2575957865996,-55.6031026233215,
-42.5599291941495));
#240088=CARTESIAN_POINT('Ctrl Pts',(44.750008238189,-55.4726832794671,-42.5303199204922));
#240089=CARTESIAN_POINT('Ctrl Pts',(44.4838674301552,-55.4582549240482,
-42.5147950400236));
#240090=CARTESIAN_POINT('Ctrl Pts',(43.9711540783505,-55.5321567162246,
-42.4848867611683));
#240091=CARTESIAN_POINT('Ctrl Pts',(43.7288317395534,-55.6159982417038,
-42.4707512914051));
#240092=CARTESIAN_POINT('Ctrl Pts',(43.2791701979494,-55.8753631474548,
-42.4445210348116));
#240093=CARTESIAN_POINT('Ctrl Pts',(43.078139009641,-56.0520943766476,-42.4297358571075));
#240094=CARTESIAN_POINT('Ctrl Pts',(42.7592844524011,-56.4703800500612,
-42.3993049147337));
#240095=CARTESIAN_POINT('Ctrl Pts',(42.6432600435373,-56.7067237562461,
-42.3839812230163));
#240096=CARTESIAN_POINT('Ctrl Pts',(42.5103209946102,-57.2037461827188,
-42.354995181314));
#240097=CARTESIAN_POINT('Ctrl Pts',(42.491998760499,-57.4589935379043,-42.3424967913847));
#240098=CARTESIAN_POINT('Ctrl Pts',(42.5530828863182,-57.9742984445225,
-42.3146829212251));
#240099=CARTESIAN_POINT('Ctrl Pts',(42.6363980620258,-58.2288520804956,
-42.2993933168699));
#240100=CARTESIAN_POINT('Ctrl Pts',(42.8937850504995,-58.6841430634323,
-42.2688857388614));
#240101=CARTESIAN_POINT('Ctrl Pts',(43.06288627497,-58.8819667140344,-42.2539599352457));
#240102=CARTESIAN_POINT('Ctrl Pts',(43.4670799663806,-59.2026435486667,
-42.2259709526097));
#240103=CARTESIAN_POINT('Ctrl Pts',(43.698357440717,-59.3223873201503,-42.2134263760266));
#240104=CARTESIAN_POINT('Ctrl Pts',(44.1289367369284,-59.4484346369407,
-42.1883092504143));
#240105=CARTESIAN_POINT('Ctrl Pts',(44.3181598941138,-59.475452478349,-42.177271232912));
#240106=CARTESIAN_POINT('Ctrl Pts',(44.5079524583206,-59.475452478349,-42.1662));
#240107=CARTESIAN_POINT('Origin',(44.5079524583206,-57.475452478349,235.35105));
#240108=CARTESIAN_POINT('',(44.5079524583206,-59.475452478349,-41.4662));
#240109=CARTESIAN_POINT('',(44.5079524583206,-59.475452478349,-41.6249500000001));
#240110=CARTESIAN_POINT('',(44.5079524583206,-59.475452478349,235.35105));
#240111=CARTESIAN_POINT('Ctrl Pts',(44.5079524583206,-59.475452478349,-41.6249500000001));
#240112=CARTESIAN_POINT('Ctrl Pts',(44.3963129281412,-59.475452478349,-41.6314623059272));
#240113=CARTESIAN_POINT('Ctrl Pts',(44.284610180426,-59.4661050893039,-41.637978299544));
#240114=CARTESIAN_POINT('Ctrl Pts',(43.911142678792,-59.4028619686822,-41.659763903806));
#240115=CARTESIAN_POINT('Ctrl Pts',(43.6598786140261,-59.3062423031846,
-41.6738640414497));
#240116=CARTESIAN_POINT('Ctrl Pts',(43.2195904327178,-59.0263440056424,
-41.7008457238465));
#240117=CARTESIAN_POINT('Ctrl Pts',(43.0324278880756,-58.8494703777636,
-41.715239959607));
#240118=CARTESIAN_POINT('Ctrl Pts',(42.728906649178,-58.4269175895807,-41.7454392469336));
#240119=CARTESIAN_POINT('Ctrl Pts',(42.6185745343544,-58.1829538690468,
-41.760981862425));
#240120=CARTESIAN_POINT('Ctrl Pts',(42.5012232192591,-57.6737152098165,
-41.7901304033518));
#240121=CARTESIAN_POINT('Ctrl Pts',(42.4923876021727,-57.4141076143141,
-41.8025950539835));
#240122=CARTESIAN_POINT('Ctrl Pts',(42.5737311241404,-56.9049828108047,
-41.8306876158305));
#240123=CARTESIAN_POINT('Ctrl Pts',(42.6634335294862,-56.6603634107947,
-41.8456616551753));
#240124=CARTESIAN_POINT('Ctrl Pts',(42.9344647249112,-56.2127349077193,
-41.8761800949239));
#240125=CARTESIAN_POINT('Ctrl Pts',(43.1155820075873,-56.0154315039811,
-41.8914300849956));
#240126=CARTESIAN_POINT('Ctrl Pts',(43.5347753777698,-55.709900089237,-41.9190914396905));
#240127=CARTESIAN_POINT('Ctrl Pts',(43.7661104404675,-55.6009020538235,
-41.9316758822919));
#240128=CARTESIAN_POINT('Ctrl Pts',(44.2646382087956,-55.4732097928478,
-41.9607566687777));
#240129=CARTESIAN_POINT('Ctrl Pts',(44.5278281986985,-55.4585803441233,
-41.9761094181887));
#240130=CARTESIAN_POINT('Ctrl Pts',(45.0489862984194,-55.5318451887435,
-42.0065103073391));
#240131=CARTESIAN_POINT('Ctrl Pts',(45.3015461474302,-55.6206126054169,
-42.0210600730208));
#240132=CARTESIAN_POINT('Ctrl Pts',(45.7481527830709,-55.885906664465,-42.0474882645792));
#240133=CARTESIAN_POINT('Ctrl Pts',(45.9400885160742,-56.0564062583027,
-42.061699713935));
#240134=CARTESIAN_POINT('Ctrl Pts',(46.2557408430406,-56.4679417525677,
-42.0916962513727));
#240135=CARTESIAN_POINT('Ctrl Pts',(46.3734402397765,-56.7074621950644,
-42.10722927974));
#240136=CARTESIAN_POINT('Ctrl Pts',(46.5076138855837,-57.2135657321372,
-42.1367100914123));
#240137=CARTESIAN_POINT('Ctrl Pts',(46.5246867087515,-57.4746722153939,
-42.1494225002558));
#240138=CARTESIAN_POINT('Ctrl Pts',(46.4584645450735,-57.9870751538133,
-42.1772396277924));
#240139=CARTESIAN_POINT('Ctrl Pts',(46.3765044067399,-58.2335665054474,
-42.1920824185463));
#240140=CARTESIAN_POINT('Ctrl Pts',(46.1187008222665,-58.6908059681195,
-42.2227005808602));
#240141=CARTESIAN_POINT('Ctrl Pts',(45.9418237970571,-58.8951851640859,
-42.2381843526787));
#240142=CARTESIAN_POINT('Ctrl Pts',(45.5289100107533,-59.2138841198949,
-42.2663277526395));
#240143=CARTESIAN_POINT('Ctrl Pts',(45.3001791987696,-59.3293366322367,
-42.2787367734739));
#240144=CARTESIAN_POINT('Ctrl Pts',(44.8773365012054,-59.4497959150024,
-42.3034025974984));
#240145=CARTESIAN_POINT('Ctrl Pts',(44.6929025187842,-59.475452478349,-42.314161246473));
#240146=CARTESIAN_POINT('Ctrl Pts',(44.5079524583206,-59.475452478349,-42.3249500000001));
#240147=CARTESIAN_POINT('Ctrl Pts',(44.5079524583206,-59.475452478349,-42.1661999999999));
#240148=CARTESIAN_POINT('Ctrl Pts',(44.5819299860625,-59.475452478349,-42.161884644215));
#240149=CARTESIAN_POINT('Ctrl Pts',(44.6559940233556,-59.4713480872461,
-42.1575642420394));
#240150=CARTESIAN_POINT('Ctrl Pts',(44.9830823256217,-59.4348404808826,
-42.1384840910739));
#240151=CARTESIAN_POINT('Ctrl Pts',(45.2286836340998,-59.3584131739,-42.1241573480794));
#240152=CARTESIAN_POINT('Ctrl Pts',(45.6892289950069,-59.1113735572966,
-42.0972922020265));
#240153=CARTESIAN_POINT('Ctrl Pts',(45.8973919788335,-58.9387337125747,
-42.0829302727521));
#240154=CARTESIAN_POINT('Ctrl Pts',(46.2294519095304,-58.5265497382248,
-42.0524224201923));
#240155=CARTESIAN_POINT('Ctrl Pts',(46.3519800320567,-58.2927254065234,
-42.0370363109609));
#240156=CARTESIAN_POINT('Ctrl Pts',(46.497811004372,-57.7989613281489,-42.0078388605397));
#240157=CARTESIAN_POINT('Ctrl Pts',(46.5227443568654,-57.5446038131605,
-41.995124827779));
#240158=CARTESIAN_POINT('Ctrl Pts',(46.4752713728182,-57.0282329744125,
-41.9676541003368));
#240159=CARTESIAN_POINT('Ctrl Pts',(46.3986945235629,-56.7716032555838,
-41.952456150641));
#240160=CARTESIAN_POINT('Ctrl Pts',(46.1531025911945,-56.3091383174921,
-41.92193018017));
#240161=CARTESIAN_POINT('Ctrl Pts',(45.9887519767006,-56.1064872107599,
-41.9068990618661));
#240162=CARTESIAN_POINT('Ctrl Pts',(45.5934103745848,-55.7761403469175,
-41.8786797531957));
#240163=CARTESIAN_POINT('Ctrl Pts',(45.3666465129243,-55.6510270662813,
-41.8662904865186));
#240164=CARTESIAN_POINT('Ctrl Pts',(44.8696684889806,-55.4905895017291,
-41.8373001017886));
#240165=CARTESIAN_POINT('Ctrl Pts',(44.6032390529754,-55.4601559654108,
-41.8217583846883));
#240166=CARTESIAN_POINT('Ctrl Pts',(44.0840904291311,-55.5042544757982,
-41.791474714964));
#240167=CARTESIAN_POINT('Ctrl Pts',(43.8359523532419,-55.5744690499767,
-41.7769999938704));
#240168=CARTESIAN_POINT('Ctrl Pts',(43.3709847734867,-55.8088419811641,
-41.7498768850514));
#240169=CARTESIAN_POINT('Ctrl Pts',(43.1602892241647,-55.9740716865162,
-41.7360734668819));
#240170=CARTESIAN_POINT('Ctrl Pts',(42.817506900039,-56.3749293567097,-41.705825061763));
#240171=CARTESIAN_POINT('Ctrl Pts',(42.6879340204009,-56.6058018069247,
-41.6903826040365));
#240172=CARTESIAN_POINT('Ctrl Pts',(42.5280293442433,-57.0958938829126,
-41.6609601733486));
#240173=CARTESIAN_POINT('Ctrl Pts',(42.495933675203,-57.3493721621776,-41.647919891983));
#240174=CARTESIAN_POINT('Ctrl Pts',(42.5287550455231,-57.8667440966951,
-41.6208259297696));
#240175=CARTESIAN_POINT('Ctrl Pts',(42.5980177961076,-58.1254040341162,
-41.6057387450673));
#240176=CARTESIAN_POINT('Ctrl Pts',(42.830684161527,-58.5952495445704,-41.5752169174479));
#240177=CARTESIAN_POINT('Ctrl Pts',(42.9897683285869,-58.8029736952618,
-41.5600831230724));
#240178=CARTESIAN_POINT('Ctrl Pts',(43.3755311450215,-59.1436457213512,
-41.5316215875709));
#240179=CARTESIAN_POINT('Ctrl Pts',(43.597573413174,-59.2744675958978,-41.5193054443001));
#240180=CARTESIAN_POINT('Ctrl Pts',(44.0535417110567,-59.4365006200257,
-41.4927072935903));
#240181=CARTESIAN_POINT('Ctrl Pts',(44.2800678724856,-59.475452478349,-41.479493267507));
#240182=CARTESIAN_POINT('Ctrl Pts',(44.5079524583206,-59.475452478349,-41.4662));
#240183=CARTESIAN_POINT('Origin',(44.5079524583206,-57.475452478349,235.35105));
#240184=CARTESIAN_POINT('',(44.5079524583206,-59.475452478349,-40.7662));
#240185=CARTESIAN_POINT('',(44.5079524583206,-59.475452478349,-40.9249500000001));
#240186=CARTESIAN_POINT('',(44.5079524583206,-59.475452478349,235.35105));
#240187=CARTESIAN_POINT('Ctrl Pts',(44.5079524583206,-59.475452478349,-40.9249500000001));
#240188=CARTESIAN_POINT('Ctrl Pts',(44.3556832620905,-59.475452478349,-40.9338323697802));
#240189=CARTESIAN_POINT('Ctrl Pts',(44.2035477074772,-59.4580626051099,
-40.9427069437994));
#240190=CARTESIAN_POINT('Ctrl Pts',(43.7996698653827,-59.364054039355,-40.9662664845882));
#240191=CARTESIAN_POINT('Ctrl Pts',(43.5589663513918,-59.2553062210328,
-40.9793805123415));
#240192=CARTESIAN_POINT('Ctrl Pts',(43.1371734125507,-58.9542357473873,
-41.0068923293039));
#240193=CARTESIAN_POINT('Ctrl Pts',(42.9589885091226,-58.7663860387722,
-41.0215792084729));
#240194=CARTESIAN_POINT('Ctrl Pts',(42.6778986677055,-58.3251594171462,
-41.0520676141982));
#240195=CARTESIAN_POINT('Ctrl Pts',(42.5810274339302,-58.0738554741762,
-41.0675884351065));
#240196=CARTESIAN_POINT('Ctrl Pts',(42.4935259126035,-57.5596078215576,
-41.0961194021204));
#240197=CARTESIAN_POINT('Ctrl Pts',(42.4992034595432,-57.3024572643112,
-41.1084342187911));
#240198=CARTESIAN_POINT('Ctrl Pts',(42.607815229616,-56.7995486188924,-41.1370080757433));
#240199=CARTESIAN_POINT('Ctrl Pts',(42.7114689037048,-56.5589399783078,
-41.1521864109526));
#240200=CARTESIAN_POINT('Ctrl Pts',(43.0080279189641,-56.1261925223017,
-41.1826976491666));
#240201=CARTESIAN_POINT('Ctrl Pts',(43.1999024039458,-55.9394423174307,
-41.1977282629041));
#240202=CARTESIAN_POINT('Ctrl Pts',(43.6353704033976,-55.6581082265016,
-41.224641890287));
#240203=CARTESIAN_POINT('Ctrl Pts',(43.8723021658698,-55.5623022940588,
-41.2378703996071));
#240204=CARTESIAN_POINT('Ctrl Pts',(44.3784883874681,-55.4624487207122,
-41.2673979292003));
#240205=CARTESIAN_POINT('Ctrl Pts',(44.6436019396349,-55.462856007272,-41.2828628864101));
#240206=CARTESIAN_POINT('Ctrl Pts',(45.1599592078587,-55.5663656558035,
-41.3129837270564));
#240207=CARTESIAN_POINT('Ctrl Pts',(45.4059688703599,-55.6690062719493,
-41.326550494208));
#240208=CARTESIAN_POINT('Ctrl Pts',(45.837201140743,-55.9593461274327,-41.3537955340446));
#240209=CARTESIAN_POINT('Ctrl Pts',(46.0200442270936,-56.1416537602683,
-41.3683383014746));
#240210=CARTESIAN_POINT('Ctrl Pts',(46.3127147158099,-56.5735006762076,
-41.3986906307142));
#240211=CARTESIAN_POINT('Ctrl Pts',(46.4165105622606,-56.8211497271544,
-41.414228781114));
#240212=CARTESIAN_POINT('Ctrl Pts',(46.5192362568492,-57.3329264870405,
-41.4430789615887));
#240213=CARTESIAN_POINT('Ctrl Pts',(46.5209489371288,-57.591298778833,-41.455423276652));
#240214=CARTESIAN_POINT('Ctrl Pts',(46.4263177960313,-58.0974421277088,
-41.4837527764889));
#240215=CARTESIAN_POINT('Ctrl Pts',(46.3298111331428,-58.3402091566098,
-41.4988316949865));
#240216=CARTESIAN_POINT('Ctrl Pts',(46.0462652316372,-58.7807852345967,
-41.5293588715376));
#240217=CARTESIAN_POINT('Ctrl Pts',(45.8598384293943,-58.9730324669386,
-41.5445082941789));
#240218=CARTESIAN_POINT('Ctrl Pts',(45.4326650871948,-59.2668301475951,
-41.571809631536));
#240219=CARTESIAN_POINT('Ctrl Pts',(45.1986558057962,-59.3694139804964,
-41.5846589713973));
#240220=CARTESIAN_POINT('Ctrl Pts',(44.8057459523781,-59.4588118646948,
-41.6075787128467));
#240221=CARTESIAN_POINT('Ctrl Pts',(44.6569054744755,-59.475452478349,-41.6162610740577));
#240222=CARTESIAN_POINT('Ctrl Pts',(44.5079524583206,-59.475452478349,-41.6249500000001));
#240223=CARTESIAN_POINT('Ctrl Pts',(44.5079524583206,-59.475452478349,-41.4662));
#240224=CARTESIAN_POINT('Ctrl Pts',(44.5457150412834,-59.475452478349,-41.4639971826605));
#240225=CARTESIAN_POINT('Ctrl Pts',(44.5835149259749,-59.474382984109,-41.4617921893868));
#240226=CARTESIAN_POINT('Ctrl Pts',(44.8770856294728,-59.4577173897901,
-41.4446672316827));
#240227=CARTESIAN_POINT('Ctrl Pts',(45.1277452030424,-59.394183437444,-41.4300454232245));
#240228=CARTESIAN_POINT('Ctrl Pts',(45.5972843930366,-59.1732023971889,
-41.4026556371415));
#240229=CARTESIAN_POINT('Ctrl Pts',(45.8106057972645,-59.015623433461,-41.3893458627232));
#240230=CARTESIAN_POINT('Ctrl Pts',(46.1643828643518,-58.6267167277128,
-41.3593805181985));
#240231=CARTESIAN_POINT('Ctrl Pts',(46.3012566561433,-58.3991559118811,
-41.3438924148386));
#240232=CARTESIAN_POINT('Ctrl Pts',(46.475894211567,-57.9130419854652,-41.3142412439232));
#240233=CARTESIAN_POINT('Ctrl Pts',(46.515440600153,-57.6603847032348,-41.300760837746));
#240234=CARTESIAN_POINT('Ctrl Pts',(46.4977283275787,-57.1421326714575,
-41.2740630966662));
#240235=CARTESIAN_POINT('Ctrl Pts',(46.4360619646601,-56.8816045311775,
-41.2591030951212));
#240236=CARTESIAN_POINT('Ctrl Pts',(46.2169532500797,-56.4045315959542,
-41.2286115828665));
#240237=CARTESIAN_POINT('Ctrl Pts',(46.0634583460397,-56.1917183083876,
-41.2133837148898));
#240238=CARTESIAN_POINT('Ctrl Pts',(45.6876284766909,-55.840486585305,-41.1846784340035));
#240239=CARTESIAN_POINT('Ctrl Pts',(45.470315286488,-55.7038429311988,-41.1723378316431));
#240240=CARTESIAN_POINT('Ctrl Pts',(44.9842432072125,-55.5147120063731,
-41.1439836270187));
#240241=CARTESIAN_POINT('Ctrl Pts',(44.7184258538704,-55.4687071560742,
-41.1284776147404));
#240242=CARTESIAN_POINT('Ctrl Pts',(44.1946734695817,-55.4835061931311,
-41.0979253923236));
#240243=CARTESIAN_POINT('Ctrl Pts',(43.9416365793137,-55.5401710005153,
-41.0831649070579));
#240244=CARTESIAN_POINT('Ctrl Pts',(43.4675773117692,-55.7475991719258,
-41.0555114497845));
#240245=CARTESIAN_POINT('Ctrl Pts',(43.251635465688,-55.8976235119033,-41.0425997525014));
#240246=CARTESIAN_POINT('Ctrl Pts',(42.8870752719029,-56.2744751676231,
-41.0129288989228));
#240247=CARTESIAN_POINT('Ctrl Pts',(42.742976768466,-56.4984970825621,-40.9974088535276));
#240248=CARTESIAN_POINT('Ctrl Pts',(42.5535830260601,-56.9804819149329,
-40.9675358880115));
#240249=CARTESIAN_POINT('Ctrl Pts',(42.5066076402285,-57.232413236575,-40.9535171163813));
#240250=CARTESIAN_POINT('Ctrl Pts',(42.5094167419912,-57.751388203542,-40.9272175297695));
#240251=CARTESIAN_POINT('Ctrl Pts',(42.5635494460456,-58.0135322888619,
-40.9123956253898));
#240252=CARTESIAN_POINT('Ctrl Pts',(42.7690799993602,-58.4973409176244,
-40.8819598680719));
#240253=CARTESIAN_POINT('Ctrl Pts',(42.9169127288896,-58.7150242563767,
-40.8666511208824));
#240254=CARTESIAN_POINT('Ctrl Pts',(43.2828838041862,-59.076581472659,-40.8377117633567));
#240255=CARTESIAN_POINT('Ctrl Pts',(43.4956739950599,-59.2189219816486,
-40.8252495770234));
#240256=CARTESIAN_POINT('Ctrl Pts',(43.9757997011733,-59.421823142488,-40.7972422441668));
#240257=CARTESIAN_POINT('Ctrl Pts',(44.2405470537739,-59.475452478349,-40.7817986485985));
#240258=CARTESIAN_POINT('Ctrl Pts',(44.5079524583207,-59.475452478349,-40.7661999999999));
#240259=CARTESIAN_POINT('Origin',(44.5079524583206,-57.475452478349,235.35105));
#240260=CARTESIAN_POINT('',(44.5079524583206,-59.475452478349,-40.0662));
#240261=CARTESIAN_POINT('',(44.5079524583206,-59.475452478349,-40.22495));
#240262=CARTESIAN_POINT('',(44.5079524583206,-59.475452478349,235.35105));
#240263=CARTESIAN_POINT('',(45.4139072126472,-59.2584969021125,-40.0133531362322));
#240264=CARTESIAN_POINT('Ctrl Pts',(44.5079524583206,-59.475452478349,-40.0662));
#240265=CARTESIAN_POINT('Ctrl Pts',(44.6477540810448,-59.475452478349,-40.058044905341));
#240266=CARTESIAN_POINT('Ctrl Pts',(44.7872831379324,-59.4607938517436,
-40.0499057103559));
#240267=CARTESIAN_POINT('Ctrl Pts',(45.0942698010449,-59.3954660374654,
-40.0319981550077));
#240268=CARTESIAN_POINT('Ctrl Pts',(45.2588837491004,-59.3372630397163,
-40.0223956747045));
#240269=CARTESIAN_POINT('Ctrl Pts',(45.4139070277165,-59.2584965939532,
-40.0133526501186));
#240270=CARTESIAN_POINT('',(46.5057019923328,-57.5702877145999,-39.8960552477251));
#240271=CARTESIAN_POINT('Ctrl Pts',(45.4139070626845,-59.2584965761862,
-40.0133533627948));
#240272=CARTESIAN_POINT('Ctrl Pts',(45.5708274797814,-59.178766201284,-40.0284745705566));
#240273=CARTESIAN_POINT('Ctrl Pts',(45.7167913486008,-59.0785403908483,
-40.0374253375929));
#240274=CARTESIAN_POINT('Ctrl Pts',(45.9789089800695,-58.8419935930646,
-40.0424294628079));
#240275=CARTESIAN_POINT('Ctrl Pts',(46.0936204899094,-58.7070030684609,
-40.0384624535326));
#240276=CARTESIAN_POINT('Ctrl Pts',(46.2846200996576,-58.4106275181728,
-40.0178326575726));
#240277=CARTESIAN_POINT('Ctrl Pts',(46.3598125890322,-58.2509288938826,
-40.0012757421132));
#240278=CARTESIAN_POINT('Ctrl Pts',(46.4665664629444,-57.9166464805059,
-39.9566009687345));
#240279=CARTESIAN_POINT('Ctrl Pts',(46.4974588687898,-57.7439490347554,
-39.9287059824097));
#240280=CARTESIAN_POINT('Ctrl Pts',(46.5057027546467,-57.5702878806477,
-39.8960539311642));
#240281=CARTESIAN_POINT('',(43.0434015151427,-58.8374706322701,-39.4567770164569));
#240282=CARTESIAN_POINT('Ctrl Pts',(43.0434024600225,-58.8374705775258,
-39.456776075616));
#240283=CARTESIAN_POINT('Ctrl Pts',(42.9505070828511,-58.7375820925191,
-39.4645317054413));
#240284=CARTESIAN_POINT('Ctrl Pts',(42.8680780966169,-58.6284556232212,
-39.4724487513936));
#240285=CARTESIAN_POINT('Ctrl Pts',(42.7265681044559,-58.3948848309218,
-39.4883756901483));
#240286=CARTESIAN_POINT('Ctrl Pts',(42.6679060158213,-58.2710134250182,
-39.4963444218185));
#240287=CARTESIAN_POINT('Ctrl Pts',(42.5341559488002,-57.8927163453032,
-39.5193563335106));
#240288=CARTESIAN_POINT('Ctrl Pts',(42.4963486406859,-57.6283470788705,
-39.5331376031768));
#240289=CARTESIAN_POINT('Ctrl Pts',(42.5252427856916,-57.1091600280751,
-39.5602087176322));
#240290=CARTESIAN_POINT('Ctrl Pts',(42.5882142281025,-56.8591155236405,
-39.5746771701227));
#240291=CARTESIAN_POINT('Ctrl Pts',(42.8090290264238,-56.3872695438299,
-39.6049543870431));
#240292=CARTESIAN_POINT('Ctrl Pts',(42.9683271570434,-56.1715902919037,
-39.6204962990084));
#240293=CARTESIAN_POINT('Ctrl Pts',(43.3553575620516,-55.8209320584954,
-39.6494992905482));
#240294=CARTESIAN_POINT('Ctrl Pts',(43.5769855334451,-55.6868188496488,
-39.661893596049));
#240295=CARTESIAN_POINT('Ctrl Pts',(44.0682014711997,-55.506263568743,-39.6905478590847));
#240296=CARTESIAN_POINT('Ctrl Pts',(44.3343106141816,-55.4652516279505,
-39.7060708924254));
#240297=CARTESIAN_POINT('Ctrl Pts',(44.8567640004058,-55.4894779008722,
-39.7365473399551));
#240298=CARTESIAN_POINT('Ctrl Pts',(45.1083113153773,-55.5505185872555,
-39.7512209333284));
#240299=CARTESIAN_POINT('Ctrl Pts',(45.5795114174102,-55.7665565411676,
-39.778707605947));
#240300=CARTESIAN_POINT('Ctrl Pts',(45.7937919860029,-55.9213584811786,
-39.7918603681415));
#240301=CARTESIAN_POINT('Ctrl Pts',(46.1515412850048,-56.3058630393379,
-39.8217191810845));
#240302=CARTESIAN_POINT('Ctrl Pts',(46.2910697333296,-56.5321542872952,
-39.8372205757081));
#240303=CARTESIAN_POINT('Ctrl Pts',(46.4304078182913,-56.9072207565103,
-39.8602322667956));
#240304=CARTESIAN_POINT('Ctrl Pts',(46.4647739918623,-57.0400469563788,
-39.8679447472216));
#240305=CARTESIAN_POINT('Ctrl Pts',(46.5051437473397,-57.3060403765032,
-39.8825596935352));
#240306=CARTESIAN_POINT('Ctrl Pts',(46.5119682426376,-57.4383022409662,
-39.8892061117466));
#240307=CARTESIAN_POINT('Ctrl Pts',(46.5057027656803,-57.5702876482191,
-39.8960565132351));
#240308=CARTESIAN_POINT('',(43.3993759211742,-59.1401020382204,-39.589855096412));
#240309=CARTESIAN_POINT('Origin',(44.6251460650309,-57.3664988654425,-39.4575809488933));
#240310=CARTESIAN_POINT('Ctrl Pts',(43.3993759361741,-59.1401020194073,
-39.589855135757));
#240311=CARTESIAN_POINT('Ctrl Pts',(43.2536892830903,-59.0430817162051,
-39.5990056158952));
#240312=CARTESIAN_POINT('Ctrl Pts',(43.1213873644818,-58.9273679902937,
-39.60871006505));
#240313=CARTESIAN_POINT('Ctrl Pts',(42.8872222066712,-58.6609972317884,
-39.6289964397015));
#240314=CARTESIAN_POINT('Ctrl Pts',(42.7873202434622,-58.5106839058266,
-39.6395037978923));
#240315=CARTESIAN_POINT('Ctrl Pts',(42.5930417605153,-58.1105886447152,
-39.6653823254816));
#240316=CARTESIAN_POINT('Ctrl Pts',(42.5257866956149,-57.8514113611987,
-39.6804370880517));
#240317=CARTESIAN_POINT('Ctrl Pts',(42.4969681427887,-57.3337914820228,
-39.7074268271265));
#240318=CARTESIAN_POINT('Ctrl Pts',(42.5310306699669,-57.0805391543703,
-39.7205734044732));
#240319=CARTESIAN_POINT('Ctrl Pts',(42.6948165101306,-56.5914815004161,
-39.7500567786919));
#240320=CARTESIAN_POINT('Ctrl Pts',(42.8263205480509,-56.3614596380144,
-39.7655125917468));
#240321=CARTESIAN_POINT('Ctrl Pts',(43.1720218424975,-55.9637414363319,
-39.7956875333634));
#240322=CARTESIAN_POINT('Ctrl Pts',(43.3834109997795,-55.8005377803727,
-39.8093517482518));
#240323=CARTESIAN_POINT('Ctrl Pts',(43.8495886138448,-55.5696795120759,
-39.8365454424056));
#240324=CARTESIAN_POINT('Ctrl Pts',(44.0984046783535,-55.5012074295454,
-39.8510597128353));
#240325=CARTESIAN_POINT('Ctrl Pts',(44.6182428099406,-55.4608949849634,
-39.8813836038445));
#240326=CARTESIAN_POINT('Ctrl Pts',(44.8846423726718,-55.4933495918306,
-39.8969235783371));
#240327=CARTESIAN_POINT('Ctrl Pts',(45.380236549904,-55.657535245913,-39.9258332386757));
#240328=CARTESIAN_POINT('Ctrl Pts',(45.6057567875752,-55.7841433844684,
-39.9381941555478));
#240329=CARTESIAN_POINT('Ctrl Pts',(45.9986064673138,-56.1171896181519,
-39.9664771503155));
#240330=CARTESIAN_POINT('Ctrl Pts',(46.1615993591797,-56.3211756711888,
-39.9815361073918));
#240331=CARTESIAN_POINT('Ctrl Pts',(46.4038443510521,-56.7855990008045,
-40.0120633930789));
#240332=CARTESIAN_POINT('Ctrl Pts',(46.4785203864252,-57.0427784721124,
-40.0272336748473));
#240333=CARTESIAN_POINT('Ctrl Pts',(46.5221743812755,-57.5594246147262,
-40.0546069229462));
#240334=CARTESIAN_POINT('Ctrl Pts',(46.4953792794438,-57.8135450608098,
-40.0673965290231));
#240335=CARTESIAN_POINT('Ctrl Pts',(46.3458998218777,-58.306368914152,-40.0966528951696));
#240336=CARTESIAN_POINT('Ctrl Pts',(46.2215394421076,-58.5394480650177,
-40.1120548000812));
#240337=CARTESIAN_POINT('Ctrl Pts',(45.8866789349324,-58.948704885331,-40.1424964617192));
#240338=CARTESIAN_POINT('Ctrl Pts',(45.6778563177999,-59.1194142087351,
-40.1567056081972));
#240339=CARTESIAN_POINT('Ctrl Pts',(45.2161593327308,-59.3631817568321,
-40.1836379323262));
#240340=CARTESIAN_POINT('Ctrl Pts',(44.9698889176337,-59.4380144849026,
-40.1980037065402));
#240341=CARTESIAN_POINT('Ctrl Pts',(44.6469276953965,-59.4718354739981,
-40.2168431111707));
#240342=CARTESIAN_POINT('Ctrl Pts',(44.5773988698809,-59.475452478349,-40.2208989593257));
#240343=CARTESIAN_POINT('Ctrl Pts',(44.5079524583206,-59.475452478349,-40.2249500000001));
#240344=CARTESIAN_POINT('Origin',(-44.5079524583207,-57.4754524783487,-52.920575));
#240345=CARTESIAN_POINT('',(-44.5079524583207,-55.8067071952963,-40.04995));
#240346=CARTESIAN_POINT('',(-44.5079524583207,-55.8067071952963,-39.8912));
#240347=CARTESIAN_POINT('',(-44.5079524583207,-55.8067071952962,-52.920575));
#240348=CARTESIAN_POINT('',(-45.3258935545055,-56.0209136569754,-39.8341888326825));
#240349=CARTESIAN_POINT('Ctrl Pts',(-44.5079524583208,-55.8067071952963,
-39.8912));
#240350=CARTESIAN_POINT('Ctrl Pts',(-44.9449717304834,-55.8067071952963,
-39.8647401145564));
#240351=CARTESIAN_POINT('Ctrl Pts',(-45.3258935545055,-56.0209136569754,
-39.8341888326825));
#240352=CARTESIAN_POINT('',(-45.7222549758842,-56.3308214393021,-39.9581073668549));
#240353=CARTESIAN_POINT('Ctrl Pts',(-45.7222549758842,-56.3308214393021,
-39.9581073668549));
#240354=CARTESIAN_POINT('Ctrl Pts',(-45.7045762341998,-56.3120666267883,
-39.9516436713479));
#240355=CARTESIAN_POINT('Ctrl Pts',(-45.686660871375,-56.2939315400474,
-39.9452586862569));
#240356=CARTESIAN_POINT('Ctrl Pts',(-45.6685147272012,-56.2763687588793,
-39.9389426841664));
#240357=CARTESIAN_POINT('Ctrl Pts',(-45.648505858845,-56.2570031364642,
-39.9319783366359));
#240358=CARTESIAN_POINT('Ctrl Pts',(-45.6282239848617,-56.238342887266,
-39.9251019846523));
#240359=CARTESIAN_POINT('Ctrl Pts',(-45.6076972509794,-56.2203564794336,
-39.9183131959778));
#240360=CARTESIAN_POINT('Ctrl Pts',(-45.5657790231701,-56.1836259237927,
-39.9044496172986));
#240361=CARTESIAN_POINT('Ctrl Pts',(-45.5228400189614,-56.1497051629388,
-39.8909512030947));
#240362=CARTESIAN_POINT('Ctrl Pts',(-45.4790691672601,-56.118382182885,
-39.8778157637598));
#240363=CARTESIAN_POINT('Ctrl Pts',(-45.4340050705677,-56.086133740212,
-39.864292227313));
#240364=CARTESIAN_POINT('Ctrl Pts',(-45.3880438891079,-56.0566341670122,
-39.8511484168624));
#240365=CARTESIAN_POINT('Ctrl Pts',(-45.3413791392512,-56.0297312061481,
-39.8383987109864));
#240366=CARTESIAN_POINT('Ctrl Pts',(-45.3362271142298,-56.0267609828437,
-39.8369910788038));
#240367=CARTESIAN_POINT('Ctrl Pts',(-45.3310650292783,-56.0238217689367,
-39.8355877210878));
#240368=CARTESIAN_POINT('Ctrl Pts',(-45.3258935545055,-56.0209136569754,
-39.8341888326825));
#240369=CARTESIAN_POINT('Ctrl Pts',(-44.5079524583208,-55.8067071952963,
-40.04995));
#240370=CARTESIAN_POINT('Ctrl Pts',(-45.2282121628138,-55.8067071952963,
-40.0063409637755));
#240371=CARTESIAN_POINT('Ctrl Pts',(-45.7222549758842,-56.3308214393021,
-39.9581073668549));
#240372=CARTESIAN_POINT('Origin',(-44.5079524583207,-57.4754524783487,-52.920575));
#240373=CARTESIAN_POINT('',(-44.5079524583207,-55.8067071952963,-40.74995));
#240374=CARTESIAN_POINT('',(-44.5079524583207,-55.8067071952963,-40.5912));
#240375=CARTESIAN_POINT('',(-44.5079524583207,-55.8067071952962,-52.920575));
#240376=CARTESIAN_POINT('',(-45.9506478428458,-58.3141066664263,-40.3575668188428));
#240377=CARTESIAN_POINT('Ctrl Pts',(-44.5079524583208,-55.8067071952963,
-40.5912));
#240378=CARTESIAN_POINT('Ctrl Pts',(-45.4714029967,-55.8067071952963,-40.5328666666667));
#240379=CARTESIAN_POINT('Ctrl Pts',(-45.9531282658897,-56.6410798368225,
-40.4745333333334));
#240380=CARTESIAN_POINT('Ctrl Pts',(-46.4348535350793,-57.4754524783487,
-40.4162));
#240381=CARTESIAN_POINT('Ctrl Pts',(-45.9531282658897,-58.309825119875,
-40.3578666666667));
#240382=CARTESIAN_POINT('Ctrl Pts',(-45.9518912282699,-58.3119677318833,
-40.3577168706472));
#240383=CARTESIAN_POINT('Ctrl Pts',(-45.9506478428458,-58.3141066664263,
-40.3575668188428));
#240384=CARTESIAN_POINT('',(-44.4689492302737,-59.1437418920632,-40.2388225645966));
#240385=CARTESIAN_POINT('Ctrl Pts',(-44.4689492302736,-59.1437418920632,
-40.2388225645967));
#240386=CARTESIAN_POINT('Ctrl Pts',(-44.6151980966235,-59.1471610697185,
-40.266024559964));
#240387=CARTESIAN_POINT('Ctrl Pts',(-44.7618474420247,-59.1313541404608,
-40.2898435667392));
#240388=CARTESIAN_POINT('Ctrl Pts',(-45.0497620148851,-59.0608004987189,
-40.3294471928174));
#240389=CARTESIAN_POINT('Ctrl Pts',(-45.1893227978148,-59.0060957201154,
-40.3449203569677));
#240390=CARTESIAN_POINT('Ctrl Pts',(-45.4502212571483,-58.8607378909715,
-40.365994271027));
#240391=CARTESIAN_POINT('Ctrl Pts',(-45.5702107742475,-58.771067079493,
-40.3715288199669));
#240392=CARTESIAN_POINT('Ctrl Pts',(-45.6900411584965,-58.6534685340575,
-40.3719332763248));
#240393=CARTESIAN_POINT('Ctrl Pts',(-45.7030763481267,-58.6402419523344,
-40.3718986213114));
#240394=CARTESIAN_POINT('Ctrl Pts',(-45.8062133726342,-58.5320358540091,
-40.3709726646665));
#240395=CARTESIAN_POINT('Ctrl Pts',(-45.8849732379958,-58.4270834459435,
-40.3661946462488));
#240396=CARTESIAN_POINT('Ctrl Pts',(-45.9506478428458,-58.3141066664263,
-40.3575668188428));
#240397=CARTESIAN_POINT('Ctrl Pts',(-44.4689492302737,-59.1437418920632,
-40.2388225645966));
#240398=CARTESIAN_POINT('Ctrl Pts',(-43.5315862238041,-59.121827119476,
-40.1813026722985));
#240399=CARTESIAN_POINT('Ctrl Pts',(-43.0627766507519,-58.309825119875,
-40.1245333333334));
#240400=CARTESIAN_POINT('Ctrl Pts',(-42.5810513815623,-57.4754524783487,
-40.0662));
#240401=CARTESIAN_POINT('Ctrl Pts',(-43.0627766507519,-56.6410798368225,
-40.0078666666667));
#240402=CARTESIAN_POINT('Ctrl Pts',(-43.5445019199415,-55.8067071952963,
-39.9495333333333));
#240403=CARTESIAN_POINT('Ctrl Pts',(-44.5079524583208,-55.8067071952963,
-39.8912));
#240404=CARTESIAN_POINT('Ctrl Pts',(-44.5079524583208,-55.8067071952963,
-40.74995));
#240405=CARTESIAN_POINT('Ctrl Pts',(-45.4714029967,-55.8067071952963,-40.6916166666667));
#240406=CARTESIAN_POINT('Ctrl Pts',(-45.9531282658897,-56.6410798368225,
-40.6332833333334));
#240407=CARTESIAN_POINT('Ctrl Pts',(-46.4348535350793,-57.4754524783487,
-40.57495));
#240408=CARTESIAN_POINT('Ctrl Pts',(-45.9531282658897,-58.309825119875,
-40.5166166666667));
#240409=CARTESIAN_POINT('Ctrl Pts',(-45.4714029967,-59.1441977614012,-40.4582833333333));
#240410=CARTESIAN_POINT('Ctrl Pts',(-44.5079524583208,-59.1441977614012,
-40.39995));
#240411=CARTESIAN_POINT('Ctrl Pts',(-43.5445019199415,-59.1441977614012,
-40.3416166666667));
#240412=CARTESIAN_POINT('Ctrl Pts',(-43.0627766507519,-58.309825119875,
-40.2832833333334));
#240413=CARTESIAN_POINT('Ctrl Pts',(-42.5810513815623,-57.4754524783487,
-40.22495));
#240414=CARTESIAN_POINT('Ctrl Pts',(-43.0627766507519,-56.6410798368225,
-40.1666166666667));
#240415=CARTESIAN_POINT('Ctrl Pts',(-43.5445019199415,-55.8067071952963,
-40.1082833333334));
#240416=CARTESIAN_POINT('Ctrl Pts',(-44.5079524583208,-55.8067071952963,
-40.04995));
#240417=CARTESIAN_POINT('Origin',(-44.5079524583207,-57.4754524783487,-52.920575));
#240418=CARTESIAN_POINT('',(-44.5079524583207,-55.8067071952963,-41.44995));
#240419=CARTESIAN_POINT('',(-44.5079524583207,-55.8067071952963,-41.2912));
#240420=CARTESIAN_POINT('',(-44.5079524583207,-55.8067071952962,-52.920575));
#240421=CARTESIAN_POINT('Ctrl Pts',(-44.5079524583208,-55.8067071952963,
-41.2912));
#240422=CARTESIAN_POINT('Ctrl Pts',(-45.4714029967,-55.8067071952963,-41.2328666666667));
#240423=CARTESIAN_POINT('Ctrl Pts',(-45.9531282658897,-56.6410798368225,
-41.1745333333334));
#240424=CARTESIAN_POINT('Ctrl Pts',(-46.4348535350793,-57.4754524783487,
-41.1162));
#240425=CARTESIAN_POINT('Ctrl Pts',(-45.9531282658897,-58.309825119875,
-41.0578666666667));
#240426=CARTESIAN_POINT('Ctrl Pts',(-45.4714029967,-59.1441977614012,-40.9995333333333));
#240427=CARTESIAN_POINT('Ctrl Pts',(-44.5079524583208,-59.1441977614012,
-40.9412));
#240428=CARTESIAN_POINT('Ctrl Pts',(-43.5445019199415,-59.1441977614012,
-40.8828666666667));
#240429=CARTESIAN_POINT('Ctrl Pts',(-43.0627766507519,-58.309825119875,
-40.8245333333333));
#240430=CARTESIAN_POINT('Ctrl Pts',(-42.5810513815623,-57.4754524783487,
-40.7662));
#240431=CARTESIAN_POINT('Ctrl Pts',(-43.0627766507519,-56.6410798368225,
-40.7078666666667));
#240432=CARTESIAN_POINT('Ctrl Pts',(-43.5445019199415,-55.8067071952963,
-40.6495333333334));
#240433=CARTESIAN_POINT('Ctrl Pts',(-44.5079524583208,-55.8067071952963,
-40.5912));
#240434=CARTESIAN_POINT('Ctrl Pts',(-44.5079524583208,-55.8067071952963,
-41.44995));
#240435=CARTESIAN_POINT('Ctrl Pts',(-45.4714029967,-55.8067071952963,-41.3916166666667));
#240436=CARTESIAN_POINT('Ctrl Pts',(-45.9531282658897,-56.6410798368225,
-41.3332833333334));
#240437=CARTESIAN_POINT('Ctrl Pts',(-46.4348535350793,-57.4754524783487,
-41.27495));
#240438=CARTESIAN_POINT('Ctrl Pts',(-45.9531282658897,-58.309825119875,
-41.2166166666667));
#240439=CARTESIAN_POINT('Ctrl Pts',(-45.4714029967,-59.1441977614012,-41.1582833333333));
#240440=CARTESIAN_POINT('Ctrl Pts',(-44.5079524583208,-59.1441977614012,
-41.09995));
#240441=CARTESIAN_POINT('Ctrl Pts',(-43.5445019199415,-59.1441977614012,
-41.0416166666667));
#240442=CARTESIAN_POINT('Ctrl Pts',(-43.0627766507519,-58.309825119875,
-40.9832833333333));
#240443=CARTESIAN_POINT('Ctrl Pts',(-42.5810513815623,-57.4754524783487,
-40.92495));
#240444=CARTESIAN_POINT('Ctrl Pts',(-43.0627766507519,-56.6410798368225,
-40.8666166666667));
#240445=CARTESIAN_POINT('Ctrl Pts',(-43.5445019199415,-55.8067071952963,
-40.8082833333334));
#240446=CARTESIAN_POINT('Ctrl Pts',(-44.5079524583208,-55.8067071952963,
-40.74995));
#240447=CARTESIAN_POINT('Origin',(-44.5079524583207,-57.4754524783487,-52.920575));
#240448=CARTESIAN_POINT('',(-44.5079524583207,-55.8067071952963,-42.14995));
#240449=CARTESIAN_POINT('',(-44.5079524583207,-55.8067071952963,-41.9912));
#240450=CARTESIAN_POINT('',(-44.5079524583207,-55.8067071952962,-52.920575));
#240451=CARTESIAN_POINT('Ctrl Pts',(-44.5079524583208,-55.8067071952963,
-41.9912));
#240452=CARTESIAN_POINT('Ctrl Pts',(-45.4714029967,-55.8067071952963,-41.9328666666667));
#240453=CARTESIAN_POINT('Ctrl Pts',(-45.9531282658897,-56.6410798368225,
-41.8745333333334));
#240454=CARTESIAN_POINT('Ctrl Pts',(-46.4348535350793,-57.4754524783487,
-41.8162));
#240455=CARTESIAN_POINT('Ctrl Pts',(-45.9531282658897,-58.309825119875,
-41.7578666666667));
#240456=CARTESIAN_POINT('Ctrl Pts',(-45.4714029967,-59.1441977614012,-41.6995333333334));
#240457=CARTESIAN_POINT('Ctrl Pts',(-44.5079524583208,-59.1441977614012,
-41.6412));
#240458=CARTESIAN_POINT('Ctrl Pts',(-43.5445019199415,-59.1441977614012,
-41.5828666666667));
#240459=CARTESIAN_POINT('Ctrl Pts',(-43.0627766507519,-58.309825119875,
-41.5245333333334));
#240460=CARTESIAN_POINT('Ctrl Pts',(-42.5810513815623,-57.4754524783487,
-41.4662));
#240461=CARTESIAN_POINT('Ctrl Pts',(-43.0627766507519,-56.6410798368225,
-41.4078666666667));
#240462=CARTESIAN_POINT('Ctrl Pts',(-43.5445019199415,-55.8067071952963,
-41.3495333333333));
#240463=CARTESIAN_POINT('Ctrl Pts',(-44.5079524583208,-55.8067071952963,
-41.2912));
#240464=CARTESIAN_POINT('Ctrl Pts',(-44.5079524583208,-55.8067071952963,
-42.14995));
#240465=CARTESIAN_POINT('Ctrl Pts',(-45.4714029967,-55.8067071952963,-42.0916166666667));
#240466=CARTESIAN_POINT('Ctrl Pts',(-45.9531282658897,-56.6410798368225,
-42.0332833333334));
#240467=CARTESIAN_POINT('Ctrl Pts',(-46.4348535350793,-57.4754524783487,
-41.97495));
#240468=CARTESIAN_POINT('Ctrl Pts',(-45.9531282658897,-58.309825119875,
-41.9166166666667));
#240469=CARTESIAN_POINT('Ctrl Pts',(-45.4714029967,-59.1441977614012,-41.8582833333333));
#240470=CARTESIAN_POINT('Ctrl Pts',(-44.5079524583208,-59.1441977614012,
-41.79995));
#240471=CARTESIAN_POINT('Ctrl Pts',(-43.5445019199415,-59.1441977614012,
-41.7416166666666));
#240472=CARTESIAN_POINT('Ctrl Pts',(-43.0627766507519,-58.309825119875,
-41.6832833333333));
#240473=CARTESIAN_POINT('Ctrl Pts',(-42.5810513815623,-57.4754524783487,
-41.62495));
#240474=CARTESIAN_POINT('Ctrl Pts',(-43.0627766507519,-56.6410798368225,
-41.5666166666667));
#240475=CARTESIAN_POINT('Ctrl Pts',(-43.5445019199415,-55.8067071952963,
-41.5082833333334));
#240476=CARTESIAN_POINT('Ctrl Pts',(-44.5079524583208,-55.8067071952963,
-41.44995));
#240477=CARTESIAN_POINT('Origin',(-44.5079524583207,-57.4754524783487,-52.920575));
#240478=CARTESIAN_POINT('',(-44.5079524583207,-55.8067071952963,-42.84995));
#240479=CARTESIAN_POINT('',(-44.5079524583207,-55.8067071952963,-42.6912));
#240480=CARTESIAN_POINT('',(-44.5079524583207,-55.8067071952962,-52.920575));
#240481=CARTESIAN_POINT('Ctrl Pts',(-44.5079524583208,-55.8067071952963,
-42.6912));
#240482=CARTESIAN_POINT('Ctrl Pts',(-45.4714029967,-55.8067071952963,-42.6328666666667));
#240483=CARTESIAN_POINT('Ctrl Pts',(-45.9531282658897,-56.6410798368225,
-42.5745333333333));
#240484=CARTESIAN_POINT('Ctrl Pts',(-46.4348535350793,-57.4754524783487,
-42.5162));
#240485=CARTESIAN_POINT('Ctrl Pts',(-45.9531282658897,-58.309825119875,
-42.4578666666667));
#240486=CARTESIAN_POINT('Ctrl Pts',(-45.4714029967,-59.1441977614012,-42.3995333333334));
#240487=CARTESIAN_POINT('Ctrl Pts',(-44.5079524583208,-59.1441977614012,
-42.3412));
#240488=CARTESIAN_POINT('Ctrl Pts',(-43.5445019199415,-59.1441977614012,
-42.2828666666667));
#240489=CARTESIAN_POINT('Ctrl Pts',(-43.0627766507519,-58.309825119875,
-42.2245333333333));
#240490=CARTESIAN_POINT('Ctrl Pts',(-42.5810513815623,-57.4754524783487,
-42.1662));
#240491=CARTESIAN_POINT('Ctrl Pts',(-43.0627766507519,-56.6410798368225,
-42.1078666666667));
#240492=CARTESIAN_POINT('Ctrl Pts',(-43.5445019199415,-55.8067071952963,
-42.0495333333334));
#240493=CARTESIAN_POINT('Ctrl Pts',(-44.5079524583208,-55.8067071952963,
-41.9912));
#240494=CARTESIAN_POINT('Ctrl Pts',(-44.5079524583208,-55.8067071952963,
-42.84995));
#240495=CARTESIAN_POINT('Ctrl Pts',(-45.4714029967,-55.8067071952963,-42.7916166666667));
#240496=CARTESIAN_POINT('Ctrl Pts',(-45.9531282658897,-56.6410798368225,
-42.7332833333334));
#240497=CARTESIAN_POINT('Ctrl Pts',(-46.4348535350793,-57.4754524783487,
-42.67495));
#240498=CARTESIAN_POINT('Ctrl Pts',(-45.9531282658897,-58.309825119875,
-42.6166166666667));
#240499=CARTESIAN_POINT('Ctrl Pts',(-45.4714029967,-59.1441977614012,-42.5582833333333));
#240500=CARTESIAN_POINT('Ctrl Pts',(-44.5079524583208,-59.1441977614012,
-42.49995));
#240501=CARTESIAN_POINT('Ctrl Pts',(-43.5445019199415,-59.1441977614012,
-42.4416166666667));
#240502=CARTESIAN_POINT('Ctrl Pts',(-43.0627766507519,-58.309825119875,
-42.3832833333333));
#240503=CARTESIAN_POINT('Ctrl Pts',(-42.5810513815623,-57.4754524783487,
-42.32495));
#240504=CARTESIAN_POINT('Ctrl Pts',(-43.0627766507519,-56.6410798368225,
-42.2666166666667));
#240505=CARTESIAN_POINT('Ctrl Pts',(-43.5445019199415,-55.8067071952963,
-42.2082833333333));
#240506=CARTESIAN_POINT('Ctrl Pts',(-44.5079524583208,-55.8067071952963,
-42.14995));
#240507=CARTESIAN_POINT('Origin',(-44.5079524583207,-57.4754524783487,-52.920575));
#240508=CARTESIAN_POINT('',(-44.5079524583207,-55.8067071952963,-43.54995));
#240509=CARTESIAN_POINT('',(-44.5079524583207,-55.8067071952963,-43.3912));
#240510=CARTESIAN_POINT('',(-44.5079524583207,-55.8067071952962,-52.920575));
#240511=CARTESIAN_POINT('Ctrl Pts',(-44.5079524583208,-55.8067071952963,
-43.3912));
#240512=CARTESIAN_POINT('Ctrl Pts',(-45.4714029967,-55.8067071952963,-43.3328666666667));
#240513=CARTESIAN_POINT('Ctrl Pts',(-45.9531282658897,-56.6410798368225,
-43.2745333333334));
#240514=CARTESIAN_POINT('Ctrl Pts',(-46.4348535350793,-57.4754524783487,
-43.2162));
#240515=CARTESIAN_POINT('Ctrl Pts',(-45.9531282658897,-58.309825119875,
-43.1578666666667));
#240516=CARTESIAN_POINT('Ctrl Pts',(-45.4714029967,-59.1441977614012,-43.0995333333334));
#240517=CARTESIAN_POINT('Ctrl Pts',(-44.5079524583208,-59.1441977614012,
-43.0412));
#240518=CARTESIAN_POINT('Ctrl Pts',(-43.5445019199415,-59.1441977614012,
-42.9828666666667));
#240519=CARTESIAN_POINT('Ctrl Pts',(-43.0627766507519,-58.309825119875,
-42.9245333333334));
#240520=CARTESIAN_POINT('Ctrl Pts',(-42.5810513815623,-57.4754524783487,
-42.8662));
#240521=CARTESIAN_POINT('Ctrl Pts',(-43.0627766507519,-56.6410798368225,
-42.8078666666667));
#240522=CARTESIAN_POINT('Ctrl Pts',(-43.5445019199415,-55.8067071952963,
-42.7495333333334));
#240523=CARTESIAN_POINT('Ctrl Pts',(-44.5079524583208,-55.8067071952963,
-42.6912));
#240524=CARTESIAN_POINT('Ctrl Pts',(-44.5079524583208,-55.8067071952963,
-43.54995));
#240525=CARTESIAN_POINT('Ctrl Pts',(-45.4714029967,-55.8067071952963,-43.4916166666667));
#240526=CARTESIAN_POINT('Ctrl Pts',(-45.9531282658897,-56.6410798368225,
-43.4332833333333));
#240527=CARTESIAN_POINT('Ctrl Pts',(-46.4348535350793,-57.4754524783487,
-43.37495));
#240528=CARTESIAN_POINT('Ctrl Pts',(-45.9531282658897,-58.309825119875,
-43.3166166666667));
#240529=CARTESIAN_POINT('Ctrl Pts',(-45.4714029967,-59.1441977614012,-43.2582833333333));
#240530=CARTESIAN_POINT('Ctrl Pts',(-44.5079524583208,-59.1441977614012,
-43.19995));
#240531=CARTESIAN_POINT('Ctrl Pts',(-43.5445019199415,-59.1441977614012,
-43.1416166666667));
#240532=CARTESIAN_POINT('Ctrl Pts',(-43.0627766507519,-58.309825119875,
-43.0832833333333));
#240533=CARTESIAN_POINT('Ctrl Pts',(-42.5810513815623,-57.4754524783487,
-43.02495));
#240534=CARTESIAN_POINT('Ctrl Pts',(-43.0627766507519,-56.6410798368225,
-42.9666166666667));
#240535=CARTESIAN_POINT('Ctrl Pts',(-43.5445019199415,-55.8067071952963,
-42.9082833333333));
#240536=CARTESIAN_POINT('Ctrl Pts',(-44.5079524583208,-55.8067071952963,
-42.84995));
#240537=CARTESIAN_POINT('Origin',(-44.5079524583207,-57.4754524783487,-52.920575));
#240538=CARTESIAN_POINT('',(-44.5079524583207,-55.8067071952963,-44.24995));
#240539=CARTESIAN_POINT('',(-44.5079524583207,-55.8067071952963,-44.0912));
#240540=CARTESIAN_POINT('',(-44.5079524583207,-55.8067071952962,-52.920575));
#240541=CARTESIAN_POINT('Ctrl Pts',(-44.5079524583208,-55.8067071952963,
-44.0912));
#240542=CARTESIAN_POINT('Ctrl Pts',(-45.4714029967,-55.8067071952963,-44.0328666666667));
#240543=CARTESIAN_POINT('Ctrl Pts',(-45.9531282658897,-56.6410798368225,
-43.9745333333333));
#240544=CARTESIAN_POINT('Ctrl Pts',(-46.4348535350793,-57.4754524783487,
-43.9162));
#240545=CARTESIAN_POINT('Ctrl Pts',(-45.9531282658897,-58.309825119875,
-43.8578666666667));
#240546=CARTESIAN_POINT('Ctrl Pts',(-45.4714029967,-59.1441977614012,-43.7995333333334));
#240547=CARTESIAN_POINT('Ctrl Pts',(-44.5079524583208,-59.1441977614012,
-43.7412));
#240548=CARTESIAN_POINT('Ctrl Pts',(-43.5445019199415,-59.1441977614012,
-43.6828666666667));
#240549=CARTESIAN_POINT('Ctrl Pts',(-43.0627766507519,-58.309825119875,
-43.6245333333333));
#240550=CARTESIAN_POINT('Ctrl Pts',(-42.5810513815623,-57.4754524783487,
-43.5662));
#240551=CARTESIAN_POINT('Ctrl Pts',(-43.0627766507519,-56.6410798368225,
-43.5078666666667));
#240552=CARTESIAN_POINT('Ctrl Pts',(-43.5445019199415,-55.8067071952963,
-43.4495333333334));
#240553=CARTESIAN_POINT('Ctrl Pts',(-44.5079524583208,-55.8067071952963,
-43.3912));
#240554=CARTESIAN_POINT('Ctrl Pts',(-44.5079524583208,-55.8067071952963,
-44.24995));
#240555=CARTESIAN_POINT('Ctrl Pts',(-45.4714029967,-55.8067071952963,-44.1916166666667));
#240556=CARTESIAN_POINT('Ctrl Pts',(-45.9531282658897,-56.6410798368225,
-44.1332833333334));
#240557=CARTESIAN_POINT('Ctrl Pts',(-46.4348535350793,-57.4754524783487,
-44.07495));
#240558=CARTESIAN_POINT('Ctrl Pts',(-45.9531282658897,-58.309825119875,
-44.0166166666667));
#240559=CARTESIAN_POINT('Ctrl Pts',(-45.4714029967,-59.1441977614012,-43.9582833333334));
#240560=CARTESIAN_POINT('Ctrl Pts',(-44.5079524583208,-59.1441977614012,
-43.89995));
#240561=CARTESIAN_POINT('Ctrl Pts',(-43.5445019199415,-59.1441977614012,
-43.8416166666667));
#240562=CARTESIAN_POINT('Ctrl Pts',(-43.0627766507519,-58.309825119875,
-43.7832833333334));
#240563=CARTESIAN_POINT('Ctrl Pts',(-42.5810513815623,-57.4754524783487,
-43.72495));
#240564=CARTESIAN_POINT('Ctrl Pts',(-43.0627766507519,-56.6410798368225,
-43.6666166666667));
#240565=CARTESIAN_POINT('Ctrl Pts',(-43.5445019199415,-55.8067071952963,
-43.6082833333334));
#240566=CARTESIAN_POINT('Ctrl Pts',(-44.5079524583208,-55.8067071952963,
-43.54995));
#240567=CARTESIAN_POINT('Origin',(-44.5079524583207,-57.4754524783487,-52.920575));
#240568=CARTESIAN_POINT('',(-44.5079524583207,-55.8067071952963,-44.94995));
#240569=CARTESIAN_POINT('',(-44.5079524583207,-55.8067071952963,-44.7912));
#240570=CARTESIAN_POINT('',(-44.5079524583207,-55.8067071952962,-52.920575));
#240571=CARTESIAN_POINT('Ctrl Pts',(-44.5079524583208,-55.8067071952963,
-44.7912));
#240572=CARTESIAN_POINT('Ctrl Pts',(-45.4714029967,-55.8067071952963,-44.7328666666667));
#240573=CARTESIAN_POINT('Ctrl Pts',(-45.9531282658897,-56.6410798368225,
-44.6745333333334));
#240574=CARTESIAN_POINT('Ctrl Pts',(-46.4348535350793,-57.4754524783487,
-44.6162));
#240575=CARTESIAN_POINT('Ctrl Pts',(-45.9531282658897,-58.309825119875,
-44.5578666666667));
#240576=CARTESIAN_POINT('Ctrl Pts',(-45.4714029967,-59.1441977614012,-44.4995333333333));
#240577=CARTESIAN_POINT('Ctrl Pts',(-44.5079524583208,-59.1441977614012,
-44.4412));
#240578=CARTESIAN_POINT('Ctrl Pts',(-43.5445019199415,-59.1441977614012,
-44.3828666666667));
#240579=CARTESIAN_POINT('Ctrl Pts',(-43.0627766507519,-58.309825119875,
-44.3245333333334));
#240580=CARTESIAN_POINT('Ctrl Pts',(-42.5810513815623,-57.4754524783487,
-44.2662));
#240581=CARTESIAN_POINT('Ctrl Pts',(-43.0627766507519,-56.6410798368225,
-44.2078666666667));
#240582=CARTESIAN_POINT('Ctrl Pts',(-43.5445019199415,-55.8067071952963,
-44.1495333333334));
#240583=CARTESIAN_POINT('Ctrl Pts',(-44.5079524583208,-55.8067071952963,
-44.0912));
#240584=CARTESIAN_POINT('Ctrl Pts',(-44.5079524583208,-55.8067071952963,
-44.94995));
#240585=CARTESIAN_POINT('Ctrl Pts',(-45.4714029967,-55.8067071952963,-44.8916166666667));
#240586=CARTESIAN_POINT('Ctrl Pts',(-45.9531282658897,-56.6410798368225,
-44.8332833333334));
#240587=CARTESIAN_POINT('Ctrl Pts',(-46.4348535350793,-57.4754524783487,
-44.77495));
#240588=CARTESIAN_POINT('Ctrl Pts',(-45.9531282658897,-58.309825119875,
-44.7166166666667));
#240589=CARTESIAN_POINT('Ctrl Pts',(-45.4714029967,-59.1441977614012,-44.6582833333334));
#240590=CARTESIAN_POINT('Ctrl Pts',(-44.5079524583208,-59.1441977614012,
-44.59995));
#240591=CARTESIAN_POINT('Ctrl Pts',(-43.5445019199415,-59.1441977614012,
-44.5416166666667));
#240592=CARTESIAN_POINT('Ctrl Pts',(-43.0627766507519,-58.309825119875,
-44.4832833333334));
#240593=CARTESIAN_POINT('Ctrl Pts',(-42.5810513815623,-57.4754524783487,
-44.42495));
#240594=CARTESIAN_POINT('Ctrl Pts',(-43.0627766507519,-56.6410798368225,
-44.3666166666667));
#240595=CARTESIAN_POINT('Ctrl Pts',(-43.5445019199415,-55.8067071952963,
-44.3082833333334));
#240596=CARTESIAN_POINT('Ctrl Pts',(-44.5079524583208,-55.8067071952963,
-44.24995));
#240597=CARTESIAN_POINT('Origin',(-44.5079524583207,-57.4754524783487,-52.920575));
#240598=CARTESIAN_POINT('',(-44.5079524583207,-55.8067071952963,-45.64995));
#240599=CARTESIAN_POINT('',(-44.5079524583207,-55.8067071952963,-45.4912));
#240600=CARTESIAN_POINT('',(-44.5079524583207,-55.8067071952962,-52.920575));
#240601=CARTESIAN_POINT('Ctrl Pts',(-44.5079524583208,-55.8067071952963,
-45.4912));
#240602=CARTESIAN_POINT('Ctrl Pts',(-45.4714029967,-55.8067071952963,-45.4328666666666));
#240603=CARTESIAN_POINT('Ctrl Pts',(-45.9531282658897,-56.6410798368225,
-45.3745333333334));
#240604=CARTESIAN_POINT('Ctrl Pts',(-46.4348535350793,-57.4754524783487,
-45.3162));
#240605=CARTESIAN_POINT('Ctrl Pts',(-45.9531282658897,-58.309825119875,
-45.2578666666667));
#240606=CARTESIAN_POINT('Ctrl Pts',(-45.4714029967,-59.1441977614012,-45.1995333333333));
#240607=CARTESIAN_POINT('Ctrl Pts',(-44.5079524583208,-59.1441977614012,
-45.1412));
#240608=CARTESIAN_POINT('Ctrl Pts',(-43.5445019199415,-59.1441977614012,
-45.0828666666667));
#240609=CARTESIAN_POINT('Ctrl Pts',(-43.0627766507519,-58.309825119875,
-45.0245333333334));
#240610=CARTESIAN_POINT('Ctrl Pts',(-42.5810513815623,-57.4754524783487,
-44.9662));
#240611=CARTESIAN_POINT('Ctrl Pts',(-43.0627766507519,-56.6410798368225,
-44.9078666666667));
#240612=CARTESIAN_POINT('Ctrl Pts',(-43.5445019199415,-55.8067071952963,
-44.8495333333333));
#240613=CARTESIAN_POINT('Ctrl Pts',(-44.5079524583208,-55.8067071952963,
-44.7912));
#240614=CARTESIAN_POINT('Ctrl Pts',(-44.5079524583208,-55.8067071952963,
-45.64995));
#240615=CARTESIAN_POINT('Ctrl Pts',(-45.4714029967,-55.8067071952963,-45.5916166666667));
#240616=CARTESIAN_POINT('Ctrl Pts',(-45.9531282658897,-56.6410798368225,
-45.5332833333333));
#240617=CARTESIAN_POINT('Ctrl Pts',(-46.4348535350793,-57.4754524783487,
-45.47495));
#240618=CARTESIAN_POINT('Ctrl Pts',(-45.9531282658897,-58.309825119875,
-45.4166166666667));
#240619=CARTESIAN_POINT('Ctrl Pts',(-45.4714029967,-59.1441977614012,-45.3582833333334));
#240620=CARTESIAN_POINT('Ctrl Pts',(-44.5079524583208,-59.1441977614012,
-45.29995));
#240621=CARTESIAN_POINT('Ctrl Pts',(-43.5445019199415,-59.1441977614012,
-45.2416166666667));
#240622=CARTESIAN_POINT('Ctrl Pts',(-43.0627766507519,-58.309825119875,
-45.1832833333334));
#240623=CARTESIAN_POINT('Ctrl Pts',(-42.5810513815623,-57.4754524783487,
-45.12495));
#240624=CARTESIAN_POINT('Ctrl Pts',(-43.0627766507519,-56.6410798368225,
-45.0666166666667));
#240625=CARTESIAN_POINT('Ctrl Pts',(-43.5445019199415,-55.8067071952963,
-45.0082833333334));
#240626=CARTESIAN_POINT('Ctrl Pts',(-44.5079524583208,-55.8067071952963,
-44.94995));
#240627=CARTESIAN_POINT('Origin',(-44.5079524583207,-57.4754524783487,-52.920575));
#240628=CARTESIAN_POINT('',(-44.5079524583207,-55.8067071952963,-46.34995));
#240629=CARTESIAN_POINT('',(-44.5079524583207,-55.8067071952963,-46.1912));
#240630=CARTESIAN_POINT('',(-44.5079524583207,-55.8067071952962,-52.920575));
#240631=CARTESIAN_POINT('Ctrl Pts',(-44.5079524583208,-55.8067071952963,
-46.1912));
#240632=CARTESIAN_POINT('Ctrl Pts',(-45.4714029967,-55.8067071952963,-46.1328666666667));
#240633=CARTESIAN_POINT('Ctrl Pts',(-45.9531282658897,-56.6410798368225,
-46.0745333333334));
#240634=CARTESIAN_POINT('Ctrl Pts',(-46.4348535350793,-57.4754524783487,
-46.0162));
#240635=CARTESIAN_POINT('Ctrl Pts',(-45.9531282658897,-58.309825119875,
-45.9578666666667));
#240636=CARTESIAN_POINT('Ctrl Pts',(-45.4714029967,-59.1441977614012,-45.8995333333333));
#240637=CARTESIAN_POINT('Ctrl Pts',(-44.5079524583208,-59.1441977614012,
-45.8412));
#240638=CARTESIAN_POINT('Ctrl Pts',(-43.5445019199415,-59.1441977614012,
-45.7828666666667));
#240639=CARTESIAN_POINT('Ctrl Pts',(-43.0627766507519,-58.309825119875,
-45.7245333333333));
#240640=CARTESIAN_POINT('Ctrl Pts',(-42.5810513815623,-57.4754524783487,
-45.6662));
#240641=CARTESIAN_POINT('Ctrl Pts',(-43.0627766507519,-56.6410798368225,
-45.6078666666667));
#240642=CARTESIAN_POINT('Ctrl Pts',(-43.5445019199415,-55.8067071952963,
-45.5495333333333));
#240643=CARTESIAN_POINT('Ctrl Pts',(-44.5079524583208,-55.8067071952963,
-45.4912));
#240644=CARTESIAN_POINT('Ctrl Pts',(-44.5079524583208,-55.8067071952963,
-46.34995));
#240645=CARTESIAN_POINT('Ctrl Pts',(-45.4714029967,-55.8067071952963,-46.2916166666667));
#240646=CARTESIAN_POINT('Ctrl Pts',(-45.9531282658897,-56.6410798368225,
-46.2332833333334));
#240647=CARTESIAN_POINT('Ctrl Pts',(-46.4348535350793,-57.4754524783487,
-46.17495));
#240648=CARTESIAN_POINT('Ctrl Pts',(-45.9531282658897,-58.309825119875,
-46.1166166666667));
#240649=CARTESIAN_POINT('Ctrl Pts',(-45.4714029967,-59.1441977614012,-46.0582833333333));
#240650=CARTESIAN_POINT('Ctrl Pts',(-44.5079524583208,-59.1441977614012,
-45.99995));
#240651=CARTESIAN_POINT('Ctrl Pts',(-43.5445019199415,-59.1441977614012,
-45.9416166666667));
#240652=CARTESIAN_POINT('Ctrl Pts',(-43.0627766507519,-58.309825119875,
-45.8832833333333));
#240653=CARTESIAN_POINT('Ctrl Pts',(-42.5810513815623,-57.4754524783487,
-45.82495));
#240654=CARTESIAN_POINT('Ctrl Pts',(-43.0627766507519,-56.6410798368225,
-45.7666166666667));
#240655=CARTESIAN_POINT('Ctrl Pts',(-43.5445019199415,-55.8067071952963,
-45.7082833333333));
#240656=CARTESIAN_POINT('Ctrl Pts',(-44.5079524583208,-55.8067071952963,
-45.64995));
#240657=CARTESIAN_POINT('Origin',(-44.5079524583207,-57.4754524783487,-52.920575));
#240658=CARTESIAN_POINT('',(-44.5079524583207,-55.8067071952963,-47.04995));
#240659=CARTESIAN_POINT('',(-44.5079524583207,-55.8067071952963,-46.8912));
#240660=CARTESIAN_POINT('',(-44.5079524583207,-55.8067071952962,-52.920575));
#240661=CARTESIAN_POINT('Ctrl Pts',(-44.5079524583208,-55.8067071952963,
-46.8912));
#240662=CARTESIAN_POINT('Ctrl Pts',(-45.4714029967,-55.8067071952963,-46.8328666666667));
#240663=CARTESIAN_POINT('Ctrl Pts',(-45.9531282658897,-56.6410798368225,
-46.7745333333334));
#240664=CARTESIAN_POINT('Ctrl Pts',(-46.4348535350793,-57.4754524783487,
-46.7162));
#240665=CARTESIAN_POINT('Ctrl Pts',(-45.9531282658897,-58.309825119875,
-46.6578666666667));
#240666=CARTESIAN_POINT('Ctrl Pts',(-45.4714029967,-59.1441977614012,-46.5995333333334));
#240667=CARTESIAN_POINT('Ctrl Pts',(-44.5079524583208,-59.1441977614012,
-46.5412));
#240668=CARTESIAN_POINT('Ctrl Pts',(-43.5445019199415,-59.1441977614012,
-46.4828666666667));
#240669=CARTESIAN_POINT('Ctrl Pts',(-43.0627766507519,-58.309825119875,
-46.4245333333334));
#240670=CARTESIAN_POINT('Ctrl Pts',(-42.5810513815623,-57.4754524783487,
-46.3662));
#240671=CARTESIAN_POINT('Ctrl Pts',(-43.0627766507519,-56.6410798368225,
-46.3078666666667));
#240672=CARTESIAN_POINT('Ctrl Pts',(-43.5445019199415,-55.8067071952963,
-46.2495333333334));
#240673=CARTESIAN_POINT('Ctrl Pts',(-44.5079524583208,-55.8067071952963,
-46.1912));
#240674=CARTESIAN_POINT('Ctrl Pts',(-44.5079524583208,-55.8067071952963,
-47.04995));
#240675=CARTESIAN_POINT('Ctrl Pts',(-45.4714029967,-55.8067071952963,-46.9916166666667));
#240676=CARTESIAN_POINT('Ctrl Pts',(-45.9531282658897,-56.6410798368225,
-46.9332833333334));
#240677=CARTESIAN_POINT('Ctrl Pts',(-46.4348535350793,-57.4754524783487,
-46.87495));
#240678=CARTESIAN_POINT('Ctrl Pts',(-45.9531282658897,-58.309825119875,
-46.8166166666667));
#240679=CARTESIAN_POINT('Ctrl Pts',(-45.4714029967,-59.1441977614012,-46.7582833333333));
#240680=CARTESIAN_POINT('Ctrl Pts',(-44.5079524583208,-59.1441977614012,
-46.69995));
#240681=CARTESIAN_POINT('Ctrl Pts',(-43.5445019199415,-59.1441977614012,
-46.6416166666666));
#240682=CARTESIAN_POINT('Ctrl Pts',(-43.0627766507519,-58.309825119875,
-46.5832833333334));
#240683=CARTESIAN_POINT('Ctrl Pts',(-42.5810513815623,-57.4754524783487,
-46.52495));
#240684=CARTESIAN_POINT('Ctrl Pts',(-43.0627766507519,-56.6410798368225,
-46.4666166666667));
#240685=CARTESIAN_POINT('Ctrl Pts',(-43.5445019199415,-55.8067071952963,
-46.4082833333333));
#240686=CARTESIAN_POINT('Ctrl Pts',(-44.5079524583208,-55.8067071952963,
-46.34995));
#240687=CARTESIAN_POINT('Origin',(-44.5079524583207,-57.4754524783487,-52.920575));
#240688=CARTESIAN_POINT('',(-44.5079524583207,-55.8067071952963,-47.74995));
#240689=CARTESIAN_POINT('',(-44.5079524583207,-55.8067071952963,-47.5912));
#240690=CARTESIAN_POINT('',(-44.5079524583207,-55.8067071952962,-52.920575));
#240691=CARTESIAN_POINT('Ctrl Pts',(-44.5079524583208,-55.8067071952963,
-47.5912));
#240692=CARTESIAN_POINT('Ctrl Pts',(-45.4714029967,-55.8067071952963,-47.5328666666667));
#240693=CARTESIAN_POINT('Ctrl Pts',(-45.9531282658897,-56.6410798368225,
-47.4745333333334));
#240694=CARTESIAN_POINT('Ctrl Pts',(-46.4348535350793,-57.4754524783487,
-47.4162));
#240695=CARTESIAN_POINT('Ctrl Pts',(-45.9531282658897,-58.309825119875,
-47.3578666666667));
#240696=CARTESIAN_POINT('Ctrl Pts',(-45.4714029967,-59.1441977614012,-47.2995333333334));
#240697=CARTESIAN_POINT('Ctrl Pts',(-44.5079524583208,-59.1441977614012,
-47.2412));
#240698=CARTESIAN_POINT('Ctrl Pts',(-43.5445019199415,-59.1441977614012,
-47.1828666666667));
#240699=CARTESIAN_POINT('Ctrl Pts',(-43.0627766507519,-58.309825119875,
-47.1245333333333));
#240700=CARTESIAN_POINT('Ctrl Pts',(-42.5810513815623,-57.4754524783487,
-47.0662));
#240701=CARTESIAN_POINT('Ctrl Pts',(-43.0627766507519,-56.6410798368225,
-47.0078666666667));
#240702=CARTESIAN_POINT('Ctrl Pts',(-43.5445019199415,-55.8067071952963,
-46.9495333333334));
#240703=CARTESIAN_POINT('Ctrl Pts',(-44.5079524583208,-55.8067071952963,
-46.8912));
#240704=CARTESIAN_POINT('Ctrl Pts',(-44.5079524583208,-55.8067071952963,
-47.74995));
#240705=CARTESIAN_POINT('Ctrl Pts',(-45.4714029967,-55.8067071952963,-47.6916166666667));
#240706=CARTESIAN_POINT('Ctrl Pts',(-45.9531282658897,-56.6410798368225,
-47.6332833333333));
#240707=CARTESIAN_POINT('Ctrl Pts',(-46.4348535350793,-57.4754524783487,
-47.57495));
#240708=CARTESIAN_POINT('Ctrl Pts',(-45.9531282658897,-58.309825119875,
-47.5166166666667));
#240709=CARTESIAN_POINT('Ctrl Pts',(-45.4714029967,-59.1441977614012,-47.4582833333333));
#240710=CARTESIAN_POINT('Ctrl Pts',(-44.5079524583208,-59.1441977614012,
-47.39995));
#240711=CARTESIAN_POINT('Ctrl Pts',(-43.5445019199415,-59.1441977614012,
-47.3416166666667));
#240712=CARTESIAN_POINT('Ctrl Pts',(-43.0627766507519,-58.309825119875,
-47.2832833333333));
#240713=CARTESIAN_POINT('Ctrl Pts',(-42.5810513815623,-57.4754524783487,
-47.22495));
#240714=CARTESIAN_POINT('Ctrl Pts',(-43.0627766507519,-56.6410798368225,
-47.1666166666667));
#240715=CARTESIAN_POINT('Ctrl Pts',(-43.5445019199415,-55.8067071952963,
-47.1082833333333));
#240716=CARTESIAN_POINT('Ctrl Pts',(-44.5079524583208,-55.8067071952963,
-47.04995));
#240717=CARTESIAN_POINT('Origin',(-44.5079524583207,-57.4754524783487,-52.920575));
#240718=CARTESIAN_POINT('',(-44.5079524583207,-55.8067071952963,-48.44995));
#240719=CARTESIAN_POINT('',(-44.5079524583207,-55.8067071952963,-48.2912));
#240720=CARTESIAN_POINT('',(-44.5079524583207,-55.8067071952962,-52.920575));
#240721=CARTESIAN_POINT('Ctrl Pts',(-44.5079524583208,-55.8067071952963,
-48.2912));
#240722=CARTESIAN_POINT('Ctrl Pts',(-45.4714029967,-55.8067071952963,-48.2328666666667));
#240723=CARTESIAN_POINT('Ctrl Pts',(-45.9531282658897,-56.6410798368225,
-48.1745333333334));
#240724=CARTESIAN_POINT('Ctrl Pts',(-46.4348535350793,-57.4754524783487,
-48.1162));
#240725=CARTESIAN_POINT('Ctrl Pts',(-45.9531282658897,-58.309825119875,
-48.0578666666667));
#240726=CARTESIAN_POINT('Ctrl Pts',(-45.4714029967,-59.1441977614012,-47.9995333333334));
#240727=CARTESIAN_POINT('Ctrl Pts',(-44.5079524583208,-59.1441977614012,
-47.9412));
#240728=CARTESIAN_POINT('Ctrl Pts',(-43.5445019199415,-59.1441977614012,
-47.8828666666667));
#240729=CARTESIAN_POINT('Ctrl Pts',(-43.0627766507519,-58.309825119875,
-47.8245333333333));
#240730=CARTESIAN_POINT('Ctrl Pts',(-42.5810513815623,-57.4754524783487,
-47.7662));
#240731=CARTESIAN_POINT('Ctrl Pts',(-43.0627766507519,-56.6410798368225,
-47.7078666666667));
#240732=CARTESIAN_POINT('Ctrl Pts',(-43.5445019199415,-55.8067071952963,
-47.6495333333334));
#240733=CARTESIAN_POINT('Ctrl Pts',(-44.5079524583208,-55.8067071952963,
-47.5912));
#240734=CARTESIAN_POINT('Ctrl Pts',(-44.5079524583208,-55.8067071952963,
-48.44995));
#240735=CARTESIAN_POINT('Ctrl Pts',(-45.4714029967,-55.8067071952963,-48.3916166666667));
#240736=CARTESIAN_POINT('Ctrl Pts',(-45.9531282658897,-56.6410798368225,
-48.3332833333334));
#240737=CARTESIAN_POINT('Ctrl Pts',(-46.4348535350793,-57.4754524783487,
-48.27495));
#240738=CARTESIAN_POINT('Ctrl Pts',(-45.9531282658897,-58.309825119875,
-48.2166166666667));
#240739=CARTESIAN_POINT('Ctrl Pts',(-45.4714029967,-59.1441977614012,-48.1582833333334));
#240740=CARTESIAN_POINT('Ctrl Pts',(-44.5079524583208,-59.1441977614012,
-48.09995));
#240741=CARTESIAN_POINT('Ctrl Pts',(-43.5445019199415,-59.1441977614012,
-48.0416166666667));
#240742=CARTESIAN_POINT('Ctrl Pts',(-43.0627766507519,-58.309825119875,
-47.9832833333334));
#240743=CARTESIAN_POINT('Ctrl Pts',(-42.5810513815623,-57.4754524783487,
-47.92495));
#240744=CARTESIAN_POINT('Ctrl Pts',(-43.0627766507519,-56.6410798368225,
-47.8666166666667));
#240745=CARTESIAN_POINT('Ctrl Pts',(-43.5445019199415,-55.8067071952963,
-47.8082833333333));
#240746=CARTESIAN_POINT('Ctrl Pts',(-44.5079524583208,-55.8067071952963,
-47.74995));
#240747=CARTESIAN_POINT('Origin',(-44.5079524583207,-57.4754524783487,-52.920575));
#240748=CARTESIAN_POINT('',(-44.5079524583207,-55.8067071952963,-49.14995));
#240749=CARTESIAN_POINT('',(-44.5079524583207,-55.8067071952963,-48.9912));
#240750=CARTESIAN_POINT('',(-44.5079524583207,-55.8067071952962,-52.920575));
#240751=CARTESIAN_POINT('Ctrl Pts',(-44.5079524583208,-55.8067071952963,
-48.9912));
#240752=CARTESIAN_POINT('Ctrl Pts',(-45.4714029967,-55.8067071952963,-48.9328666666667));
#240753=CARTESIAN_POINT('Ctrl Pts',(-45.9531282658897,-56.6410798368225,
-48.8745333333334));
#240754=CARTESIAN_POINT('Ctrl Pts',(-46.4348535350793,-57.4754524783487,
-48.8162));
#240755=CARTESIAN_POINT('Ctrl Pts',(-45.9531282658897,-58.309825119875,
-48.7578666666667));
#240756=CARTESIAN_POINT('Ctrl Pts',(-45.4714029967,-59.1441977614012,-48.6995333333333));
#240757=CARTESIAN_POINT('Ctrl Pts',(-44.5079524583208,-59.1441977614012,
-48.6412));
#240758=CARTESIAN_POINT('Ctrl Pts',(-43.5445019199415,-59.1441977614012,
-48.5828666666667));
#240759=CARTESIAN_POINT('Ctrl Pts',(-43.0627766507519,-58.309825119875,
-48.5245333333334));
#240760=CARTESIAN_POINT('Ctrl Pts',(-42.5810513815623,-57.4754524783487,
-48.4662));
#240761=CARTESIAN_POINT('Ctrl Pts',(-43.0627766507519,-56.6410798368225,
-48.4078666666667));
#240762=CARTESIAN_POINT('Ctrl Pts',(-43.5445019199415,-55.8067071952963,
-48.3495333333333));
#240763=CARTESIAN_POINT('Ctrl Pts',(-44.5079524583208,-55.8067071952963,
-48.2912));
#240764=CARTESIAN_POINT('Ctrl Pts',(-44.5079524583208,-55.8067071952963,
-49.14995));
#240765=CARTESIAN_POINT('Ctrl Pts',(-45.4714029967,-55.8067071952963,-49.0916166666667));
#240766=CARTESIAN_POINT('Ctrl Pts',(-45.9531282658897,-56.6410798368225,
-49.0332833333333));
#240767=CARTESIAN_POINT('Ctrl Pts',(-46.4348535350793,-57.4754524783487,
-48.97495));
#240768=CARTESIAN_POINT('Ctrl Pts',(-45.9531282658897,-58.309825119875,
-48.9166166666667));
#240769=CARTESIAN_POINT('Ctrl Pts',(-45.4714029967,-59.1441977614012,-48.8582833333333));
#240770=CARTESIAN_POINT('Ctrl Pts',(-44.5079524583208,-59.1441977614012,
-48.79995));
#240771=CARTESIAN_POINT('Ctrl Pts',(-43.5445019199415,-59.1441977614012,
-48.7416166666667));
#240772=CARTESIAN_POINT('Ctrl Pts',(-43.0627766507519,-58.309825119875,
-48.6832833333334));
#240773=CARTESIAN_POINT('Ctrl Pts',(-42.5810513815623,-57.4754524783487,
-48.62495));
#240774=CARTESIAN_POINT('Ctrl Pts',(-43.0627766507519,-56.6410798368225,
-48.5666166666667));
#240775=CARTESIAN_POINT('Ctrl Pts',(-43.5445019199415,-55.8067071952963,
-48.5082833333334));
#240776=CARTESIAN_POINT('Ctrl Pts',(-44.5079524583208,-55.8067071952963,
-48.44995));
#240777=CARTESIAN_POINT('Origin',(-44.5079524583207,-57.4754524783487,-52.920575));
#240778=CARTESIAN_POINT('',(-44.5079524583207,-55.8067071952963,-49.84995));
#240779=CARTESIAN_POINT('',(-44.5079524583207,-55.8067071952963,-49.6912));
#240780=CARTESIAN_POINT('',(-44.5079524583207,-55.8067071952962,-52.920575));
#240781=CARTESIAN_POINT('Ctrl Pts',(-44.5079524583208,-55.8067071952963,
-49.6912));
#240782=CARTESIAN_POINT('Ctrl Pts',(-45.4714029967,-55.8067071952963,-49.6328666666667));
#240783=CARTESIAN_POINT('Ctrl Pts',(-45.9531282658897,-56.6410798368225,
-49.5745333333334));
#240784=CARTESIAN_POINT('Ctrl Pts',(-46.4348535350793,-57.4754524783487,
-49.5162));
#240785=CARTESIAN_POINT('Ctrl Pts',(-45.9531282658897,-58.309825119875,
-49.4578666666667));
#240786=CARTESIAN_POINT('Ctrl Pts',(-45.4714029967,-59.1441977614012,-49.3995333333333));
#240787=CARTESIAN_POINT('Ctrl Pts',(-44.5079524583208,-59.1441977614012,
-49.3412));
#240788=CARTESIAN_POINT('Ctrl Pts',(-43.5445019199415,-59.1441977614012,
-49.2828666666667));
#240789=CARTESIAN_POINT('Ctrl Pts',(-43.0627766507519,-58.309825119875,
-49.2245333333334));
#240790=CARTESIAN_POINT('Ctrl Pts',(-42.5810513815623,-57.4754524783487,
-49.1662));
#240791=CARTESIAN_POINT('Ctrl Pts',(-43.0627766507519,-56.6410798368225,
-49.1078666666667));
#240792=CARTESIAN_POINT('Ctrl Pts',(-43.5445019199415,-55.8067071952963,
-49.0495333333334));
#240793=CARTESIAN_POINT('Ctrl Pts',(-44.5079524583208,-55.8067071952963,
-48.9912));
#240794=CARTESIAN_POINT('Ctrl Pts',(-44.5079524583208,-55.8067071952963,
-49.84995));
#240795=CARTESIAN_POINT('Ctrl Pts',(-45.4714029967,-55.8067071952963,-49.7916166666667));
#240796=CARTESIAN_POINT('Ctrl Pts',(-45.9531282658897,-56.6410798368225,
-49.7332833333334));
#240797=CARTESIAN_POINT('Ctrl Pts',(-46.4348535350793,-57.4754524783487,
-49.67495));
#240798=CARTESIAN_POINT('Ctrl Pts',(-45.9531282658897,-58.309825119875,
-49.6166166666667));
#240799=CARTESIAN_POINT('Ctrl Pts',(-45.4714029967,-59.1441977614012,-49.5582833333334));
#240800=CARTESIAN_POINT('Ctrl Pts',(-44.5079524583208,-59.1441977614012,
-49.49995));
#240801=CARTESIAN_POINT('Ctrl Pts',(-43.5445019199415,-59.1441977614012,
-49.4416166666667));
#240802=CARTESIAN_POINT('Ctrl Pts',(-43.0627766507519,-58.309825119875,
-49.3832833333334));
#240803=CARTESIAN_POINT('Ctrl Pts',(-42.5810513815623,-57.4754524783487,
-49.32495));
#240804=CARTESIAN_POINT('Ctrl Pts',(-43.0627766507519,-56.6410798368225,
-49.2666166666667));
#240805=CARTESIAN_POINT('Ctrl Pts',(-43.5445019199415,-55.8067071952963,
-49.2082833333334));
#240806=CARTESIAN_POINT('Ctrl Pts',(-44.5079524583208,-55.8067071952963,
-49.14995));
#240807=CARTESIAN_POINT('Origin',(-44.5079524583207,-57.4754524783487,-52.920575));
#240808=CARTESIAN_POINT('',(-44.5079524583207,-55.8067071952963,-50.54995));
#240809=CARTESIAN_POINT('',(-44.5079524583207,-55.8067071952963,-50.3912));
#240810=CARTESIAN_POINT('',(-44.5079524583207,-55.8067071952962,-52.920575));
#240811=CARTESIAN_POINT('Ctrl Pts',(-44.5079524583208,-55.8067071952963,
-50.3912));
#240812=CARTESIAN_POINT('Ctrl Pts',(-45.4714029967,-55.8067071952963,-50.3328666666667));
#240813=CARTESIAN_POINT('Ctrl Pts',(-45.9531282658897,-56.6410798368225,
-50.2745333333334));
#240814=CARTESIAN_POINT('Ctrl Pts',(-46.4348535350793,-57.4754524783487,
-50.2162));
#240815=CARTESIAN_POINT('Ctrl Pts',(-45.9531282658897,-58.309825119875,
-50.1578666666667));
#240816=CARTESIAN_POINT('Ctrl Pts',(-45.4714029967,-59.1441977614012,-50.0995333333333));
#240817=CARTESIAN_POINT('Ctrl Pts',(-44.5079524583208,-59.1441977614012,
-50.0412));
#240818=CARTESIAN_POINT('Ctrl Pts',(-43.5445019199415,-59.1441977614012,
-49.9828666666667));
#240819=CARTESIAN_POINT('Ctrl Pts',(-43.0627766507519,-58.309825119875,
-49.9245333333334));
#240820=CARTESIAN_POINT('Ctrl Pts',(-42.5810513815623,-57.4754524783487,
-49.8662));
#240821=CARTESIAN_POINT('Ctrl Pts',(-43.0627766507519,-56.6410798368225,
-49.8078666666667));
#240822=CARTESIAN_POINT('Ctrl Pts',(-43.5445019199415,-55.8067071952963,
-49.7495333333333));
#240823=CARTESIAN_POINT('Ctrl Pts',(-44.5079524583208,-55.8067071952963,
-49.6912));
#240824=CARTESIAN_POINT('Ctrl Pts',(-44.5079524583208,-55.8067071952963,
-50.54995));
#240825=CARTESIAN_POINT('Ctrl Pts',(-45.4714029967,-55.8067071952963,-50.4916166666667));
#240826=CARTESIAN_POINT('Ctrl Pts',(-45.9531282658897,-56.6410798368225,
-50.4332833333333));
#240827=CARTESIAN_POINT('Ctrl Pts',(-46.4348535350793,-57.4754524783487,
-50.37495));
#240828=CARTESIAN_POINT('Ctrl Pts',(-45.9531282658897,-58.309825119875,
-50.3166166666667));
#240829=CARTESIAN_POINT('Ctrl Pts',(-45.4714029967,-59.1441977614012,-50.2582833333334));
#240830=CARTESIAN_POINT('Ctrl Pts',(-44.5079524583208,-59.1441977614012,
-50.19995));
#240831=CARTESIAN_POINT('Ctrl Pts',(-43.5445019199415,-59.1441977614012,
-50.1416166666667));
#240832=CARTESIAN_POINT('Ctrl Pts',(-43.0627766507519,-58.309825119875,
-50.0832833333334));
#240833=CARTESIAN_POINT('Ctrl Pts',(-42.5810513815623,-57.4754524783487,
-50.02495));
#240834=CARTESIAN_POINT('Ctrl Pts',(-43.0627766507519,-56.6410798368225,
-49.9666166666667));
#240835=CARTESIAN_POINT('Ctrl Pts',(-43.5445019199415,-55.8067071952963,
-49.9082833333334));
#240836=CARTESIAN_POINT('Ctrl Pts',(-44.5079524583208,-55.8067071952963,
-49.84995));
#240837=CARTESIAN_POINT('Origin',(-44.5079524583207,-57.4754524783487,-52.920575));
#240838=CARTESIAN_POINT('',(-44.5079524583207,-55.8067071952963,-51.24995));
#240839=CARTESIAN_POINT('',(-44.5079524583207,-55.8067071952963,-51.0912));
#240840=CARTESIAN_POINT('',(-44.5079524583207,-55.8067071952962,-52.920575));
#240841=CARTESIAN_POINT('Ctrl Pts',(-44.5079524583208,-55.8067071952963,
-51.0912));
#240842=CARTESIAN_POINT('Ctrl Pts',(-45.4714029967,-55.8067071952963,-51.0328666666667));
#240843=CARTESIAN_POINT('Ctrl Pts',(-45.9531282658897,-56.6410798368225,
-50.9745333333333));
#240844=CARTESIAN_POINT('Ctrl Pts',(-46.4348535350793,-57.4754524783487,
-50.9162));
#240845=CARTESIAN_POINT('Ctrl Pts',(-45.9531282658897,-58.309825119875,
-50.8578666666667));
#240846=CARTESIAN_POINT('Ctrl Pts',(-45.4714029967,-59.1441977614012,-50.7995333333334));
#240847=CARTESIAN_POINT('Ctrl Pts',(-44.5079524583208,-59.1441977614012,
-50.7412));
#240848=CARTESIAN_POINT('Ctrl Pts',(-43.5445019199415,-59.1441977614012,
-50.6828666666667));
#240849=CARTESIAN_POINT('Ctrl Pts',(-43.0627766507519,-58.309825119875,
-50.6245333333333));
#240850=CARTESIAN_POINT('Ctrl Pts',(-42.5810513815623,-57.4754524783487,
-50.5662));
#240851=CARTESIAN_POINT('Ctrl Pts',(-43.0627766507519,-56.6410798368225,
-50.5078666666667));
#240852=CARTESIAN_POINT('Ctrl Pts',(-43.5445019199415,-55.8067071952963,
-50.4495333333333));
#240853=CARTESIAN_POINT('Ctrl Pts',(-44.5079524583208,-55.8067071952963,
-50.3912));
#240854=CARTESIAN_POINT('Ctrl Pts',(-44.5079524583208,-55.8067071952963,
-51.24995));
#240855=CARTESIAN_POINT('Ctrl Pts',(-45.4714029967,-55.8067071952963,-51.1916166666667));
#240856=CARTESIAN_POINT('Ctrl Pts',(-45.9531282658897,-56.6410798368225,
-51.1332833333334));
#240857=CARTESIAN_POINT('Ctrl Pts',(-46.4348535350793,-57.4754524783487,
-51.07495));
#240858=CARTESIAN_POINT('Ctrl Pts',(-45.9531282658897,-58.309825119875,
-51.0166166666667));
#240859=CARTESIAN_POINT('Ctrl Pts',(-45.4714029967,-59.1441977614012,-50.9582833333334));
#240860=CARTESIAN_POINT('Ctrl Pts',(-44.5079524583208,-59.1441977614012,
-50.89995));
#240861=CARTESIAN_POINT('Ctrl Pts',(-43.5445019199415,-59.1441977614012,
-50.8416166666667));
#240862=CARTESIAN_POINT('Ctrl Pts',(-43.0627766507519,-58.309825119875,
-50.7832833333333));
#240863=CARTESIAN_POINT('Ctrl Pts',(-42.5810513815623,-57.4754524783487,
-50.72495));
#240864=CARTESIAN_POINT('Ctrl Pts',(-43.0627766507519,-56.6410798368225,
-50.6666166666667));
#240865=CARTESIAN_POINT('Ctrl Pts',(-43.5445019199415,-55.8067071952963,
-50.6082833333334));
#240866=CARTESIAN_POINT('Ctrl Pts',(-44.5079524583208,-55.8067071952963,
-50.54995));
#240867=CARTESIAN_POINT('Origin',(-44.5079524583207,-57.4754524783487,-52.920575));
#240868=CARTESIAN_POINT('',(-44.5079524583207,-55.8067071952963,-51.94995));
#240869=CARTESIAN_POINT('',(-44.5079524583207,-55.8067071952963,-51.7912));
#240870=CARTESIAN_POINT('',(-44.5079524583207,-55.8067071952962,-52.920575));
#240871=CARTESIAN_POINT('Ctrl Pts',(-44.5079524583208,-55.8067071952963,
-51.7912));
#240872=CARTESIAN_POINT('Ctrl Pts',(-45.4714029967,-55.8067071952963,-51.7328666666667));
#240873=CARTESIAN_POINT('Ctrl Pts',(-45.9531282658897,-56.6410798368225,
-51.6745333333334));
#240874=CARTESIAN_POINT('Ctrl Pts',(-46.4348535350793,-57.4754524783487,
-51.6162));
#240875=CARTESIAN_POINT('Ctrl Pts',(-45.9531282658897,-58.309825119875,
-51.5578666666667));
#240876=CARTESIAN_POINT('Ctrl Pts',(-45.4714029967,-59.1441977614012,-51.4995333333334));
#240877=CARTESIAN_POINT('Ctrl Pts',(-44.5079524583208,-59.1441977614012,
-51.4412));
#240878=CARTESIAN_POINT('Ctrl Pts',(-43.5445019199415,-59.1441977614012,
-51.3828666666667));
#240879=CARTESIAN_POINT('Ctrl Pts',(-43.0627766507519,-58.309825119875,
-51.3245333333334));
#240880=CARTESIAN_POINT('Ctrl Pts',(-42.5810513815623,-57.4754524783487,
-51.2662));
#240881=CARTESIAN_POINT('Ctrl Pts',(-43.0627766507519,-56.6410798368225,
-51.2078666666667));
#240882=CARTESIAN_POINT('Ctrl Pts',(-43.5445019199415,-55.8067071952963,
-51.1495333333334));
#240883=CARTESIAN_POINT('Ctrl Pts',(-44.5079524583208,-55.8067071952963,
-51.0912));
#240884=CARTESIAN_POINT('Ctrl Pts',(-44.5079524583208,-55.8067071952963,
-51.94995));
#240885=CARTESIAN_POINT('Ctrl Pts',(-45.4714029967,-55.8067071952963,-51.8916166666667));
#240886=CARTESIAN_POINT('Ctrl Pts',(-45.9531282658897,-56.6410798368225,
-51.8332833333334));
#240887=CARTESIAN_POINT('Ctrl Pts',(-46.4348535350793,-57.4754524783487,
-51.77495));
#240888=CARTESIAN_POINT('Ctrl Pts',(-45.9531282658897,-58.309825119875,
-51.7166166666667));
#240889=CARTESIAN_POINT('Ctrl Pts',(-45.4714029967,-59.1441977614012,-51.6582833333333));
#240890=CARTESIAN_POINT('Ctrl Pts',(-44.5079524583208,-59.1441977614012,
-51.59995));
#240891=CARTESIAN_POINT('Ctrl Pts',(-43.5445019199415,-59.1441977614012,
-51.5416166666667));
#240892=CARTESIAN_POINT('Ctrl Pts',(-43.0627766507519,-58.309825119875,
-51.4832833333334));
#240893=CARTESIAN_POINT('Ctrl Pts',(-42.5810513815623,-57.4754524783487,
-51.42495));
#240894=CARTESIAN_POINT('Ctrl Pts',(-43.0627766507519,-56.6410798368225,
-51.3666166666667));
#240895=CARTESIAN_POINT('Ctrl Pts',(-43.5445019199415,-55.8067071952963,
-51.3082833333333));
#240896=CARTESIAN_POINT('Ctrl Pts',(-44.5079524583208,-55.8067071952963,
-51.24995));
#240897=CARTESIAN_POINT('Origin',(-44.5079524583207,-57.4754524783487,-52.920575));
#240898=CARTESIAN_POINT('',(-44.5079524583208,-55.8067071952963,-52.64995));
#240899=CARTESIAN_POINT('',(-44.5079524583207,-55.8067071952963,-52.4912));
#240900=CARTESIAN_POINT('',(-44.5079524583207,-55.8067071952962,-52.920575));
#240901=CARTESIAN_POINT('',(-42.8554737113965,-57.2430200996376,-52.64995));
#240902=CARTESIAN_POINT('Origin',(-44.5079524583207,-57.4754524783487,-52.64995));
#240903=CARTESIAN_POINT('Ctrl Pts',(-42.8554737113965,-57.2430200996376,
-52.64995));
#240904=CARTESIAN_POINT('Ctrl Pts',(-42.9006402736028,-56.9219082798,-52.6275001713604));
#240905=CARTESIAN_POINT('Ctrl Pts',(-43.0627766507519,-56.6410798368225,
-52.6078666666667));
#240906=CARTESIAN_POINT('Ctrl Pts',(-43.5445019199415,-55.8067071952963,
-52.5495333333333));
#240907=CARTESIAN_POINT('Ctrl Pts',(-44.5079524583208,-55.8067071952963,
-52.4912));
#240908=CARTESIAN_POINT('Origin',(-44.5079524583206,-57.475452478349,235.35105));
#240909=CARTESIAN_POINT('',(-44.5079524583206,-59.475452478349,-52.4912000000001));
#240910=CARTESIAN_POINT('',(-44.5079524583208,-59.4754524783489,-52.64995));
#240911=CARTESIAN_POINT('',(-44.5079524583206,-59.475452478349,235.35105));
#240912=CARTESIAN_POINT('',(-46.4884569292071,-57.7540239068883,-52.64995));
#240913=CARTESIAN_POINT('Origin',(-44.5079524583206,-57.4754524783489,-52.64995));
#240914=CARTESIAN_POINT('Ctrl Pts',(-46.4884569292073,-57.7540239068874,
-52.6499500000019));
#240915=CARTESIAN_POINT('Ctrl Pts',(-46.4571755210013,-57.9764191795565,
-52.6369769424295));
#240916=CARTESIAN_POINT('Ctrl Pts',(-46.3886551524865,-58.1919907826354,
-52.62440193225));
#240917=CARTESIAN_POINT('Ctrl Pts',(-46.1844788607781,-58.5881583563758,
-52.6012921571151));
#240918=CARTESIAN_POINT('Ctrl Pts',(-46.0513419995026,-58.7665170353615,
-52.5898464658721));
#240919=CARTESIAN_POINT('Ctrl Pts',(-45.7029579949069,-59.1003460934955,
-52.5625100701119));
#240920=CARTESIAN_POINT('Ctrl Pts',(-45.4806104593203,-59.2424403948135,
-52.5471330671567));
#240921=CARTESIAN_POINT('Ctrl Pts',(-45.0046748918109,-59.4288214762729,
-52.5176535685792));
#240922=CARTESIAN_POINT('Ctrl Pts',(-44.757311248525,-59.475452478349,-52.5037971444069));
#240923=CARTESIAN_POINT('Ctrl Pts',(-44.5079524583206,-59.475452478349,
-52.4912000000001));
#240924=CARTESIAN_POINT('Origin',(-44.5079524583206,-57.475452478349,235.35105));
#240925=CARTESIAN_POINT('',(-44.5079524583206,-59.475452478349,-51.7912000000001));
#240926=CARTESIAN_POINT('',(-44.5079524583207,-59.475452478349,-51.9499499999999));
#240927=CARTESIAN_POINT('',(-44.5079524583206,-59.475452478349,235.35105));
#240928=CARTESIAN_POINT('Ctrl Pts',(-44.5079524583208,-59.475452478349,
-51.9499499999999));
#240929=CARTESIAN_POINT('Ctrl Pts',(-44.5462530077334,-59.475452478349,
-51.9518848728448));
#240930=CARTESIAN_POINT('Ctrl Pts',(-44.5845870500328,-59.4743523002202,
-51.9538535262171));
#240931=CARTESIAN_POINT('Ctrl Pts',(-44.8876628879482,-59.4569033381397,
-51.9696732844808));
#240932=CARTESIAN_POINT('Ctrl Pts',(-45.1467151397867,-59.389156943588,
-51.9847360611302));
#240933=CARTESIAN_POINT('Ctrl Pts',(-45.618038707975,-59.159186107665,-52.0152539378795));
#240934=CARTESIAN_POINT('Ctrl Pts',(-45.8267932266755,-59.0012079574294,
-52.0304075257151));
#240935=CARTESIAN_POINT('Ctrl Pts',(-46.1695860436834,-58.6174282183136,
-52.0589183598922));
#240936=CARTESIAN_POINT('Ctrl Pts',(-46.3015774721523,-58.3963443508154,
-52.0712313074395));
#240937=CARTESIAN_POINT('Ctrl Pts',(-46.47919784431,-57.9058111734347,-52.0998457427868));
#240938=CARTESIAN_POINT('Ctrl Pts',(-46.5189305178084,-57.6396417713126,
-52.1153722912439));
#240939=CARTESIAN_POINT('Ctrl Pts',(-46.4922937440839,-57.1175481044096,
-52.1458277551466));
#240940=CARTESIAN_POINT('Ctrl Pts',(-46.4301366114906,-56.8663947730836,
-52.1604783661406));
#240941=CARTESIAN_POINT('Ctrl Pts',(-46.2118887101475,-56.3959354740626,
-52.1879218252502));
#240942=CARTESIAN_POINT('Ctrl Pts',(-46.0558483200505,-56.1820831689376,
-52.2011431051022));
#240943=CARTESIAN_POINT('Ctrl Pts',(-45.669376355768,-55.8261041251902,
-52.2310496753152));
#240944=CARTESIAN_POINT('Ctrl Pts',(-45.4425144507322,-55.687759774618,
-52.2465453622934));
#240945=CARTESIAN_POINT('Ctrl Pts',(-44.9572247708576,-55.5101339142034,
-52.2762420526951));
#240946=CARTESIAN_POINT('Ctrl Pts',(-44.7047220768785,-55.4690808303961,
-52.289823723447));
#240947=CARTESIAN_POINT('Ctrl Pts',(-44.1863112510203,-55.4837566408039,
-52.3164409230299));
#240948=CARTESIAN_POINT('Ctrl Pts',(-43.9254355283081,-55.5438909091359,
-52.3313737977038));
#240949=CARTESIAN_POINT('Ctrl Pts',(-43.446958185133,-55.7602489202191,
-52.3618560291959));
#240950=CARTESIAN_POINT('Ctrl Pts',(-43.2331403216415,-55.9126018978207,
-52.3771013403007));
#240951=CARTESIAN_POINT('Ctrl Pts',(-42.8797975441431,-56.2864280845043,
-52.4058548270031));
#240952=CARTESIAN_POINT('Ctrl Pts',(-42.7419899350815,-56.5028085687393,
-52.4182124386061));
#240953=CARTESIAN_POINT('Ctrl Pts',(-42.5499967148387,-56.9877533495184,
-52.4465008841515));
#240954=CARTESIAN_POINT('Ctrl Pts',(-42.5024277035354,-57.2534607575844,
-52.4620004829554));
#240955=CARTESIAN_POINT('Ctrl Pts',(-42.5142671348049,-57.7775857217385,
-52.4925744391976));
#240956=CARTESIAN_POINT('Ctrl Pts',(-42.5695550463785,-58.0310735043884,
-52.5073612265188));
#240957=CARTESIAN_POINT('Ctrl Pts',(-42.7742904349951,-58.5060182293466,
-52.5350663354747));
#240958=CARTESIAN_POINT('Ctrl Pts',(-42.922835831421,-58.7224777476931,
-52.5479110797891));
#240959=CARTESIAN_POINT('Ctrl Pts',(-43.2963567570324,-59.0882185387781,
-52.5774481051372));
#240960=CARTESIAN_POINT('Ctrl Pts',(-43.5183762271097,-59.23320900112,-52.5928930061934));
#240961=CARTESIAN_POINT('Ctrl Pts',(-43.9991306930556,-59.4264496379907,
-52.6228160169642));
#240962=CARTESIAN_POINT('Ctrl Pts',(-44.2523385936067,-59.475452478349,
-52.6370368608098));
#240963=CARTESIAN_POINT('Ctrl Pts',(-44.5079524583208,-59.475452478349,
-52.6499499999999));
#240964=CARTESIAN_POINT('Ctrl Pts',(-44.5079524583206,-59.475452478349,
-52.4912000000001));
#240965=CARTESIAN_POINT('Ctrl Pts',(-44.4925286932249,-59.475452478349,
-52.4904208199437));
#240966=CARTESIAN_POINT('Ctrl Pts',(-44.477097811945,-59.4752740593648,
-52.4896360765039));
#240967=CARTESIAN_POINT('Ctrl Pts',(-44.2069952709762,-59.4690209166747,
-52.475808612886));
#240968=CARTESIAN_POINT('Ctrl Pts',(-43.9558318021867,-59.4145263539375,
-52.4615308747119));
#240969=CARTESIAN_POINT('Ctrl Pts',(-43.4784164929003,-59.2104037693686,
-52.4314591618121));
#240970=CARTESIAN_POINT('Ctrl Pts',(-43.2581721074967,-59.0591390019468,
-52.4159209341823));
#240971=CARTESIAN_POINT('Ctrl Pts',(-42.8935213295786,-58.6839566192263,
-52.3865566325171));
#240972=CARTESIAN_POINT('Ctrl Pts',(-42.7509892352242,-58.4653719356495,
-52.3739453016761));
#240973=CARTESIAN_POINT('Ctrl Pts',(-42.5573395383357,-57.9868257843532,
-52.3460301095172));
#240974=CARTESIAN_POINT('Ctrl Pts',(-42.5077592542388,-57.7315582833632,
-52.3311395052927));
#240975=CARTESIAN_POINT('Ctrl Pts',(-42.5081545171318,-57.2060702590284,
-52.3004860372065));
#240976=CARTESIAN_POINT('Ctrl Pts',(-42.5621729208094,-56.9409096061898,
-52.2850183324575));
#240977=CARTESIAN_POINT('Ctrl Pts',(-42.7659398738441,-56.4606757368225,
-52.2570046900777));
#240978=CARTESIAN_POINT('Ctrl Pts',(-42.9085687365412,-56.248111646219,
-52.2445337968481));
#240979=CARTESIAN_POINT('Ctrl Pts',(-43.2706479599599,-55.8826429388458,
-52.215582720886));
#240980=CARTESIAN_POINT('Ctrl Pts',(-43.4885745251695,-55.7351015622851,
-52.2002701841412));
#240981=CARTESIAN_POINT('Ctrl Pts',(-43.9727146276586,-55.5302656294541,
-52.1698379411483));
#240982=CARTESIAN_POINT('Ctrl Pts',(-44.2349347373735,-55.4765163817129,
-52.1550233802994));
#240983=CARTESIAN_POINT('Ctrl Pts',(-44.7539426804031,-55.4744641746777,
-52.1287442038941));
#240984=CARTESIAN_POINT('Ctrl Pts',(-45.005839303614,-55.5218192558505,
-52.1146953140424));
#240985=CARTESIAN_POINT('Ctrl Pts',(-45.4876087021152,-55.7119684484848,
-52.0848111978816));
#240986=CARTESIAN_POINT('Ctrl Pts',(-45.7114435671204,-55.8564342500284,
-52.0692898890414));
#240987=CARTESIAN_POINT('Ctrl Pts',(-46.0876759464907,-56.2215404682432,
-52.0396343944449));
#240988=CARTESIAN_POINT('Ctrl Pts',(-46.2373163864829,-56.4376165206826,
-52.0267404308638));
#240989=CARTESIAN_POINT('Ctrl Pts',(-46.4440468364767,-56.9119056175668,
-51.9990735668789));
#240990=CARTESIAN_POINT('Ctrl Pts',(-46.50035524974,-57.1650600281304,-51.9843062262627));
#240991=CARTESIAN_POINT('Ctrl Pts',(-46.5143879192962,-57.688910498562,
-51.9537482821542));
#240992=CARTESIAN_POINT('Ctrl Pts',(-46.4679778896413,-57.9547002203644,
-51.9382438817157));
#240993=CARTESIAN_POINT('Ctrl Pts',(-46.2781052302168,-58.440480852866,
-51.9099066781532));
#240994=CARTESIAN_POINT('Ctrl Pts',(-46.1411602364249,-58.6575521547172,
-51.8975620592599));
#240995=CARTESIAN_POINT('Ctrl Pts',(-45.7893819371086,-59.0328638289246,
-51.8688442803793));
#240996=CARTESIAN_POINT('Ctrl Pts',(-45.5763081280395,-59.1860638545062,
-51.8536118519604));
#240997=CARTESIAN_POINT('Ctrl Pts',(-45.0988702536503,-59.404461648935,
-51.8231226388258));
#240998=CARTESIAN_POINT('Ctrl Pts',(-44.8382512812852,-59.4657317505508,
-51.8081696062334));
#240999=CARTESIAN_POINT('Ctrl Pts',(-44.5514667254131,-59.4750976575076,
-51.7934086091506));
#241000=CARTESIAN_POINT('Ctrl Pts',(-44.5297032459204,-59.475452478349,
-51.7922988095192));
#241001=CARTESIAN_POINT('Ctrl Pts',(-44.5079524583207,-59.475452478349,
-51.7912000000001));
#241002=CARTESIAN_POINT('Origin',(-44.5079524583206,-57.475452478349,235.35105));
#241003=CARTESIAN_POINT('',(-44.5079524583208,-59.475452478349,-51.0912000000001));
#241004=CARTESIAN_POINT('',(-44.5079524583208,-59.475452478349,-51.2499499999999));
#241005=CARTESIAN_POINT('',(-44.5079524583206,-59.475452478349,235.35105));
#241006=CARTESIAN_POINT('Ctrl Pts',(-44.5079524583209,-59.475452478349,
-51.2499499999999));
#241007=CARTESIAN_POINT('Ctrl Pts',(-44.5831034040224,-59.475452478349,
-51.2537464866388));
#241008=CARTESIAN_POINT('Ctrl Pts',(-44.6583291409112,-59.4712171014566,
-51.2576702834159));
#241009=CARTESIAN_POINT('Ctrl Pts',(-44.9968439360842,-59.432834683858,
-51.2758909113062));
#241010=CARTESIAN_POINT('Ctrl Pts',(-45.2518131349861,-59.3508177570532,
-51.2911636435384));
#241011=CARTESIAN_POINT('Ctrl Pts',(-45.7085146235329,-59.0956947682382,
-51.3216764443555));
#241012=CARTESIAN_POINT('Ctrl Pts',(-45.9072800035909,-58.9275012065103,
-51.3366233489031));
#241013=CARTESIAN_POINT('Ctrl Pts',(-46.2298326839446,-58.5250156496126,
-51.364657275202));
#241014=CARTESIAN_POINT('Ctrl Pts',(-46.3506201644387,-58.2946208767058,
-51.3771651767626));
#241015=CARTESIAN_POINT('Ctrl Pts',(-46.5001699212596,-57.7936965633861,
-51.4063857617063));
#241016=CARTESIAN_POINT('Ctrl Pts',(-46.5247591345641,-57.5272642115913,
-51.4219276488944));
#241017=CARTESIAN_POINT('Ctrl Pts',(-46.469740912205,-57.0102643525022,
-51.4520859740079));
#241018=CARTESIAN_POINT('Ctrl Pts',(-46.3945149093217,-56.7641577939788,
-51.4664421899218));
#241019=CARTESIAN_POINT('Ctrl Pts',(-46.1499417528502,-56.3027437439466,
-51.493358009507));
#241020=CARTESIAN_POINT('Ctrl Pts',(-45.9787581791892,-56.0940831577275,
-51.5076042232839));
#241021=CARTESIAN_POINT('Ctrl Pts',(-45.5687807345382,-55.7599101662309,
-51.5380622369886));
#241022=CARTESIAN_POINT('Ctrl Pts',(-45.3355169770568,-55.6360001125875,
-51.5534603333726));
#241023=CARTESIAN_POINT('Ctrl Pts',(-44.8424610981469,-55.4874181004114,
-51.5827022455307));
#241024=CARTESIAN_POINT('Ctrl Pts',(-44.5882829367332,-55.4610806010797,
-51.5954726732046));
#241025=CARTESIAN_POINT('Ctrl Pts',(-44.071703466241,-55.5056726343423,
-51.6228699126051));
#241026=CARTESIAN_POINT('Ctrl Pts',(-43.8146576896166,-55.5808159438177,
-51.6380470691935));
#241027=CARTESIAN_POINT('Ctrl Pts',(-43.3507131484704,-55.8238845064,-51.6685741881859));
#241028=CARTESIAN_POINT('Ctrl Pts',(-43.1470541791173,-55.9872118799288,
-51.6836263773153));
#241029=CARTESIAN_POINT('Ctrl Pts',(-42.8146704204402,-56.3806739780254,
-51.7118937672742));
#241030=CARTESIAN_POINT('Ctrl Pts',(-42.688429019529,-56.6064987614925,
-51.7242610331834));
#241031=CARTESIAN_POINT('Ctrl Pts',(-42.5251621390899,-57.1024333545853,
-51.7531905511137));
#241032=CARTESIAN_POINT('Ctrl Pts',(-42.4932033721177,-57.3688416175935,
-51.7687310331225));
#241033=CARTESIAN_POINT('Ctrl Pts',(-42.5344451390283,-57.8885131333919,
-51.7990452048774));
#241034=CARTESIAN_POINT('Ctrl Pts',(-42.6033451648736,-58.1371640294665,
-51.8135498404817));
#241035=CARTESIAN_POINT('Ctrl Pts',(-42.8350651409272,-58.6030456506682,
-51.8407262683851));
#241036=CARTESIAN_POINT('Ctrl Pts',(-42.9987643329247,-58.814265075649,
-51.8544239775063));
#241037=CARTESIAN_POINT('Ctrl Pts',(-43.3972520846828,-59.1592529371033,
-51.8846169869057));
#241038=CARTESIAN_POINT('Ctrl Pts',(-43.6274837288687,-59.2902844759237,
-51.9000696165241));
#241039=CARTESIAN_POINT('Ctrl Pts',(-44.0803611280474,-59.4409948871493,
-51.92734386458));
#241040=CARTESIAN_POINT('Ctrl Pts',(-44.293581933249,-59.475452478349,-51.9391203979687));
#241041=CARTESIAN_POINT('Ctrl Pts',(-44.5079524583208,-59.475452478349,
-51.9499499999999));
#241042=CARTESIAN_POINT('Ctrl Pts',(-44.5079524583207,-59.475452478349,
-51.7912000000001));
#241043=CARTESIAN_POINT('Ctrl Pts',(-44.2766221791823,-59.475452478349,
-51.7795136225936));
#241044=CARTESIAN_POINT('Ctrl Pts',(-44.0468438420911,-59.4353231275902,
-51.7667352070288));
#241045=CARTESIAN_POINT('Ctrl Pts',(-43.5814391635927,-59.2673125783722,
-51.7383235166572));
#241046=CARTESIAN_POINT('Ctrl Pts',(-43.3540581067742,-59.1300583783617,
-51.7228333991501));
#241047=CARTESIAN_POINT('Ctrl Pts',(-42.9657803176365,-58.7757113218568,
-51.6928832016369));
#241048=CARTESIAN_POINT('Ctrl Pts',(-42.8085994167965,-58.5622526766641,
-51.6795966782353));
#241049=CARTESIAN_POINT('Ctrl Pts',(-42.5883241925499,-58.0924754578454,
-51.6521930071375));
#241050=CARTESIAN_POINT('Ctrl Pts',(-42.5251453740978,-57.841687688488,
-51.6375637205917));
#241051=CARTESIAN_POINT('Ctrl Pts',(-42.4963007968343,-57.319933397626,
-51.6071280536247));
#241052=CARTESIAN_POINT('Ctrl Pts',(-42.5348608396013,-57.053713957869,
-51.5915985863055));
#241053=CARTESIAN_POINT('Ctrl Pts',(-42.7103226845749,-56.5623572492977,
-51.5629361116388));
#241054=CARTESIAN_POINT('Ctrl Pts',(-42.8414463899597,-56.340562711555,
-51.5506211829297));
#241055=CARTESIAN_POINT('Ctrl Pts',(-43.1826656768646,-55.955311056523,
-51.5221469096991));
#241056=CARTESIAN_POINT('Ctrl Pts',(-43.3906560935106,-55.7965114929554,
-51.5070079649958));
#241057=CARTESIAN_POINT('Ctrl Pts',(-43.8608842598543,-55.5645393626881,
-51.4764870548346));
#241058=CARTESIAN_POINT('Ctrl Pts',(-44.1196462450192,-55.4956674411495,
-51.4614061140497));
#241059=CARTESIAN_POINT('Ctrl Pts',(-44.6370673296782,-55.4636258727586,
-51.4343324130851));
#241060=CARTESIAN_POINT('Ctrl Pts',(-44.8905011111168,-55.4961043414681,
-51.4212720043211));
#241061=CARTESIAN_POINT('Ctrl Pts',(-45.3803927456486,-55.6567638879207,
-51.3918376825142));
#241062=CARTESIAN_POINT('Ctrl Pts',(-45.6111009889157,-55.7867127862103,
-51.3763925530081));
#241063=CARTESIAN_POINT('Ctrl Pts',(-46.0113485626539,-56.1300641139995,
-51.3461583728924));
#241064=CARTESIAN_POINT('Ctrl Pts',(-46.1761836167742,-56.3408947000873,
-51.3323825370652));
#241065=CARTESIAN_POINT('Ctrl Pts',(-46.4098736954516,-56.8060979471342,
-51.3052456809875));
#241066=CARTESIAN_POINT('Ctrl Pts',(-46.4797503444935,-57.0543686399577,
-51.2907632239061));
#241067=CARTESIAN_POINT('Ctrl Pts',(-46.5231141856447,-57.5736532824897,
-51.2604716197584));
#241068=CARTESIAN_POINT('Ctrl Pts',(-46.4922882589103,-57.8400780776405,
-51.2449301733746));
#241069=CARTESIAN_POINT('Ctrl Pts',(-46.3311223508435,-58.3367881966841,
-51.2159554164305));
#241070=CARTESIAN_POINT('Ctrl Pts',(-46.2057188345087,-58.5633101349482,
-51.203572165685));
#241071=CARTESIAN_POINT('Ctrl Pts',(-45.8748480738052,-58.9581688225288,
-51.1753404757225));
#241072=CARTESIAN_POINT('Ctrl Pts',(-45.6719374286852,-59.1222570032394,
-51.1603039003384));
#241073=CARTESIAN_POINT('Ctrl Pts',(-45.2090908576926,-59.3672011933224,
-51.1297775429632));
#241074=CARTESIAN_POINT('Ctrl Pts',(-44.9523534101276,-59.4434097910955,
-51.1145848916794));
#241075=CARTESIAN_POINT('Ctrl Pts',(-44.6281752479175,-59.4727453981219,
-51.0973523892512));
#241076=CARTESIAN_POINT('Ctrl Pts',(-44.5680326999524,-59.475452478349,
-51.094235142572));
#241077=CARTESIAN_POINT('Ctrl Pts',(-44.507952458321,-59.475452478349,-51.0912000000001));
#241078=CARTESIAN_POINT('Origin',(-44.5079524583206,-57.475452478349,235.35105));
#241079=CARTESIAN_POINT('',(-44.5079524583207,-59.475452478349,-50.3912000000001));
#241080=CARTESIAN_POINT('',(-44.5079524583206,-59.475452478349,-50.5499499999999));
#241081=CARTESIAN_POINT('',(-44.5079524583206,-59.475452478349,235.35105));
#241082=CARTESIAN_POINT('Ctrl Pts',(-44.5079524583206,-59.475452478349,
-50.5499499999999));
#241083=CARTESIAN_POINT('Ctrl Pts',(-44.6213616955837,-59.475452478349,
-50.5556792246953));
#241084=CARTESIAN_POINT('Ctrl Pts',(-44.7348059108359,-59.4658080199635,
-50.5616915131168));
#241085=CARTESIAN_POINT('Ctrl Pts',(-45.1098602422553,-59.4012787529964,
-50.5825206671672));
#241086=CARTESIAN_POINT('Ctrl Pts',(-45.3609414688666,-59.3039716755222,
-50.5980429489653));
#241087=CARTESIAN_POINT('Ctrl Pts',(-45.8015914280971,-59.0221504360446,
-50.6285235552176));
#241088=CARTESIAN_POINT('Ctrl Pts',(-45.9890986230645,-58.8436699323974,
-50.6432017529043));
#241089=CARTESIAN_POINT('Ctrl Pts',(-46.2895030469822,-58.4212871603916,
-50.670697125735));
#241090=CARTESIAN_POINT('Ctrl Pts',(-46.3978739009398,-58.1802572104635,
-50.6838363906266));
#241091=CARTESIAN_POINT('Ctrl Pts',(-46.5159484522013,-57.6685574805219,
-50.7136855415399));
#241092=CARTESIAN_POINT('Ctrl Pts',(-46.5239023467295,-57.4028003281862,
-50.7291880420928));
#241093=CARTESIAN_POINT('Ctrl Pts',(-46.4379981133226,-56.8929624627827,
-50.7589285842414));
#241094=CARTESIAN_POINT('Ctrl Pts',(-46.3486371608918,-56.6531588287568,
-50.7726122482007));
#241095=CARTESIAN_POINT('Ctrl Pts',(-46.0791904496544,-56.209943946477,
-50.7991512979196));
#241096=CARTESIAN_POINT('Ctrl Pts',(-45.8977952569553,-56.0130614435529,
-50.8140574535467));
#241097=CARTESIAN_POINT('Ctrl Pts',(-45.4728237624427,-55.7043709288116,
-50.8445296999843));
#241098=CARTESIAN_POINT('Ctrl Pts',(-45.2344517260874,-55.593984902286,
-50.8597914063684));
#241099=CARTESIAN_POINT('Ctrl Pts',(-44.734698350124,-55.4721600076459,
-50.8885912477494));
#241100=CARTESIAN_POINT('Ctrl Pts',(-44.4786178970573,-55.4595841859626,
-50.9009691025291));
#241101=CARTESIAN_POINT('Ctrl Pts',(-43.9622145966234,-55.5328528041225,
-50.9291938425372));
#241102=CARTESIAN_POINT('Ctrl Pts',(-43.7076659751875,-55.6231478076247,
-50.9446867718779));
#241103=CARTESIAN_POINT('Ctrl Pts',(-43.2579549673169,-55.8931625756044,
-50.9752807701127));
#241104=CARTESIAN_POINT('Ctrl Pts',(-43.0650369926213,-56.0668493158641,
-50.9900924922746));
#241105=CARTESIAN_POINT('Ctrl Pts',(-42.7540585407624,-56.4798060755593,
-51.0178471200605));
#241106=CARTESIAN_POINT('Ctrl Pts',(-42.6397317435719,-56.7157011752985,
-51.0306311739886));
#241107=CARTESIAN_POINT('Ctrl Pts',(-42.5065311368032,-57.2223417564747,
-51.0601852078905));
#241108=CARTESIAN_POINT('Ctrl Pts',(-42.4906348128566,-57.4885480607252,
-51.0757139089717));
#241109=CARTESIAN_POINT('Ctrl Pts',(-42.5618164365921,-58.0019241078571,
-51.1056608450544));
#241110=CARTESIAN_POINT('Ctrl Pts',(-42.644420928482,-58.244813044795,-51.1198293663758));
#241111=CARTESIAN_POINT('Ctrl Pts',(-42.9015287135843,-58.6959472311451,
-51.1461455272462));
#241112=CARTESIAN_POINT('Ctrl Pts',(-43.0772300847524,-58.8978986829694,
-51.1608272355602));
#241113=CARTESIAN_POINT('Ctrl Pts',(-43.4939761355689,-59.218992128493,
-51.1912456999591));
#241114=CARTESIAN_POINT('Ctrl Pts',(-43.7298491568058,-59.3362706282669,
-51.2065821911959));
#241115=CARTESIAN_POINT('Ctrl Pts',(-44.1534726225493,-59.4518347281563,
-51.2313534839495));
#241116=CARTESIAN_POINT('Ctrl Pts',(-44.3304689495412,-59.475452478349,
-51.2409838617374));
#241117=CARTESIAN_POINT('Ctrl Pts',(-44.5079524583209,-59.475452478349,
-51.2499499999999));
#241118=CARTESIAN_POINT('Ctrl Pts',(-44.507952458321,-59.475452478349,-51.0912000000001));
#241119=CARTESIAN_POINT('Ctrl Pts',(-44.3155292379269,-59.475452478349,
-51.081479135167));
#241120=CARTESIAN_POINT('Ctrl Pts',(-44.1238270035994,-59.4476910747681,
-51.0709849856108));
#241121=CARTESIAN_POINT('Ctrl Pts',(-43.6880346010131,-59.3183107915699,
-51.0451959686849));
#241122=CARTESIAN_POINT('Ctrl Pts',(-43.4543534409762,-59.19542761922,-51.029806736601));
#241123=CARTESIAN_POINT('Ctrl Pts',(-43.0427356756326,-58.8628243208416,
-50.9993116396479));
#241124=CARTESIAN_POINT('Ctrl Pts',(-42.8704701156885,-58.6545334333459,
-50.9849797223751));
#241125=CARTESIAN_POINT('Ctrl Pts',(-42.6240633703296,-58.1937648214756,
-50.9581015533493));
#241126=CARTESIAN_POINT('Ctrl Pts',(-42.5479439098418,-57.9480333564835,
-50.9437672178914));
#241127=CARTESIAN_POINT('Ctrl Pts',(-42.4909739825197,-57.4314427985909,
-50.913632768681));
#241128=CARTESIAN_POINT('Ctrl Pts',(-42.5145162301838,-57.1650230507651,
-50.8980916167245));
#241129=CARTESIAN_POINT('Ctrl Pts',(-42.6621071878323,-56.6634005101717,
-50.8688303018565));
#241130=CARTESIAN_POINT('Ctrl Pts',(-42.78211869464,-56.4323497013107,-50.8562954287898));
#241131=CARTESIAN_POINT('Ctrl Pts',(-43.1032765292122,-56.0285935944511,
-50.8282949098101));
#241132=CARTESIAN_POINT('Ctrl Pts',(-43.3013418874345,-55.8597244716109,
-50.8133636652038));
#241133=CARTESIAN_POINT('Ctrl Pts',(-43.7569953943809,-55.6029168978137,
-50.7828546727482));
#241134=CARTESIAN_POINT('Ctrl Pts',(-44.0116561683845,-55.5199341998579,
-50.7675693532458));
#241135=CARTESIAN_POINT('Ctrl Pts',(-44.5270170631809,-55.45952453514,-50.7397723264492));
#241136=CARTESIAN_POINT('Ctrl Pts',(-44.7822186864924,-55.4781735824444,
-50.7272652124056));
#241137=CARTESIAN_POINT('Ctrl Pts',(-45.2790829766877,-55.6117474079419,
-50.6982686451386));
#241138=CARTESIAN_POINT('Ctrl Pts',(-45.5153068061894,-55.7280930343386,
-50.6829416405246));
#241139=CARTESIAN_POINT('Ctrl Pts',(-45.9331993908207,-56.0475213946705,
-50.6525138203448));
#241140=CARTESIAN_POINT('Ctrl Pts',(-46.1096674151591,-56.2487886211153,
-50.6377553916718));
#241141=CARTESIAN_POINT('Ctrl Pts',(-46.3684553054871,-56.6988281977221,
-50.6115030830364));
#241142=CARTESIAN_POINT('Ctrl Pts',(-46.4519805126622,-56.9412961747351,
-50.5973591177107));
#241143=CARTESIAN_POINT('Ctrl Pts',(-46.5251864516007,-57.4541805161915,
-50.5674408644591));
#241144=CARTESIAN_POINT('Ctrl Pts',(-46.5103824320334,-57.7203388394583,
-50.5519149622686));
#241145=CARTESIAN_POINT('Ctrl Pts',(-46.3792507450676,-58.2276845613751,
-50.5223197951568));
#241146=CARTESIAN_POINT('Ctrl Pts',(-46.2657394275693,-58.4642795373728,
-50.5094926873508));
#241147=CARTESIAN_POINT('Ctrl Pts',(-45.9562147847162,-58.8785401443913,
-50.481773474424));
#241148=CARTESIAN_POINT('Ctrl Pts',(-45.7640371376476,-59.0528987269253,
-50.4669795568434));
#241149=CARTESIAN_POINT('Ctrl Pts',(-45.3155596585774,-59.3245613274818,
-50.4363998124163));
#241150=CARTESIAN_POINT('Ctrl Pts',(-45.0614789223731,-59.4158320621292,
-50.4209020609462));
#241151=CARTESIAN_POINT('Ctrl Pts',(-44.7010492059048,-59.4684672724759,
-50.4011586253512));
#241152=CARTESIAN_POINT('Ctrl Pts',(-44.6044663788676,-59.475452478349,
-50.3960757045758));
#241153=CARTESIAN_POINT('Ctrl Pts',(-44.5079524583207,-59.475452478349,
-50.3912000000001));
#241154=CARTESIAN_POINT('Origin',(-44.5079524583206,-57.475452478349,235.35105));
#241155=CARTESIAN_POINT('',(-44.5079524583206,-59.475452478349,-49.6912000000001));
#241156=CARTESIAN_POINT('',(-44.5079524583206,-59.475452478349,-49.8499499999999));
#241157=CARTESIAN_POINT('',(-44.5079524583206,-59.475452478349,235.35105));
#241158=CARTESIAN_POINT('Ctrl Pts',(-44.5079524583205,-59.475452478349,
-49.8499499999999));
#241159=CARTESIAN_POINT('Ctrl Pts',(-44.6599129559212,-59.475452478349,
-49.857626762992));
#241160=CARTESIAN_POINT('Ctrl Pts',(-44.8116920785691,-59.4581383328145,
-49.8657993591687));
#241161=CARTESIAN_POINT('Ctrl Pts',(-45.21861949929,-59.363635675348,-49.8891129065688));
#241162=CARTESIAN_POINT('Ctrl Pts',(-45.4623574287261,-59.2529162806659,
-49.9046554111746));
#241163=CARTESIAN_POINT('Ctrl Pts',(-45.8843456253122,-58.9487546700144,
-49.9348448538885));
#241164=CARTESIAN_POINT('Ctrl Pts',(-46.0608908843471,-58.7613386430007,
-49.9492298942989));
#241165=CARTESIAN_POINT('Ctrl Pts',(-46.3401602182985,-58.3205090227498,
-49.9761955945888));
#241166=CARTESIAN_POINT('Ctrl Pts',(-46.4364144565539,-58.0689257646349,
-49.9903307249666));
#241167=CARTESIAN_POINT('Ctrl Pts',(-46.5237169735492,-57.5476386510155,
-50.0207391399278));
#241168=CARTESIAN_POINT('Ctrl Pts',(-46.515853770386,-57.2834764456064,
-50.03614860191));
#241169=CARTESIAN_POINT('Ctrl Pts',(-46.40070405108,-56.7814383793904,-50.0654341557726));
#241170=CARTESIAN_POINT('Ctrl Pts',(-46.2977086690653,-56.547603329606,
-50.078263763375));
#241171=CARTESIAN_POINT('Ctrl Pts',(-46.0031560806814,-56.1209382868014,
-50.1055884118738));
#241172=CARTESIAN_POINT('Ctrl Pts',(-45.810579985855,-55.9348478385497,
-50.1207446377143));
#241173=CARTESIAN_POINT('Ctrl Pts',(-45.3695407548981,-55.6520995124664,
-50.1512719492794));
#241174=CARTESIAN_POINT('Ctrl Pts',(-45.1266492563282,-55.5560284728997,
-50.166344450074));
#241175=CARTESIAN_POINT('Ctrl Pts',(-44.6203120790311,-55.4622484213822,
-50.1946589183177));
#241176=CARTESIAN_POINT('Ctrl Pts',(-44.3618630975721,-55.4644143364923,
-50.2070082182243));
#241177=CARTESIAN_POINT('Ctrl Pts',(-43.8502430762259,-55.568072356457,
-50.2358776733816));
#241178=CARTESIAN_POINT('Ctrl Pts',(-43.6028239071385,-55.6722883382533,
-50.251416464523));
#241179=CARTESIAN_POINT('Ctrl Pts',(-43.1715612934929,-55.9656586820565,
-50.2817596883325));
#241180=CARTESIAN_POINT('Ctrl Pts',(-42.9895969155478,-56.1487817190571,
-50.2962932803883));
#241181=CARTESIAN_POINT('Ctrl Pts',(-42.6999187108287,-56.580591609061,
-50.3235217420922));
#241182=CARTESIAN_POINT('Ctrl Pts',(-42.5976571949136,-56.826931644352,
-50.3371196180167));
#241183=CARTESIAN_POINT('Ctrl Pts',(-42.4951107390491,-57.3435893973861,
-50.3672579869436));
#241184=CARTESIAN_POINT('Ctrl Pts',(-42.4951988047948,-57.608653251943,
-50.3827200451261));
#241185=CARTESIAN_POINT('Ctrl Pts',(-42.5959679797622,-58.1145953544506,
-50.412233334439));
#241186=CARTESIAN_POINT('Ctrl Pts',(-42.6922005031069,-58.3513402222056,
-50.425434965518));
#241187=CARTESIAN_POINT('Ctrl Pts',(-42.9743204684951,-58.7862905290305,
-50.4523731944552));
#241188=CARTESIAN_POINT('Ctrl Pts',(-43.1614209398734,-58.9778274350877,
-50.4674116569562));
#241189=CARTESIAN_POINT('Ctrl Pts',(-43.5946719927533,-59.2735746790815,
-50.49792465929));
#241190=CARTESIAN_POINT('Ctrl Pts',(-43.8354224305791,-59.3767803006319,
-50.5130970896344));
#241191=CARTESIAN_POINT('Ctrl Pts',(-44.227140195886,-59.4606605256588,
-50.5353324524567));
#241192=CARTESIAN_POINT('Ctrl Pts',(-44.3674974673574,-59.475452478349,
-50.5428544739012));
#241193=CARTESIAN_POINT('Ctrl Pts',(-44.5079524583206,-59.475452478349,
-50.5499499999999));
#241194=CARTESIAN_POINT('Ctrl Pts',(-44.5079524583207,-59.475452478349,
-50.3912000000001));
#241195=CARTESIAN_POINT('Ctrl Pts',(-44.3513025812242,-59.475452478349,
-50.383286338238));
#241196=CARTESIAN_POINT('Ctrl Pts',(-44.1948889936747,-59.4570535088991,
-50.3748479767774));
#241197=CARTESIAN_POINT('Ctrl Pts',(-43.788923747471,-59.3597737085898,
-50.3515020366529));
#241198=CARTESIAN_POINT('Ctrl Pts',(-43.5502083419417,-59.250383299058,
-50.3362520227229));
#241199=CARTESIAN_POINT('Ctrl Pts',(-43.1240620521067,-58.9434789960096,
-50.3057725256417));
#241200=CARTESIAN_POINT('Ctrl Pts',(-42.9418640111444,-58.7473294489174,
-50.2908471894852));
#241201=CARTESIAN_POINT('Ctrl Pts',(-42.6706496560568,-58.3052567302801,
-50.264252154778));
#241202=CARTESIAN_POINT('Ctrl Pts',(-42.5803309933147,-58.0658855487501,
-50.250641929107));
#241203=CARTESIAN_POINT('Ctrl Pts',(-42.4923404721843,-57.5565856752963,
-50.2209327698221));
#241204=CARTESIAN_POINT('Ctrl Pts',(-42.4991659477739,-57.2909112651402,
-50.2054350958963));
#241205=CARTESIAN_POINT('Ctrl Pts',(-42.6150752109583,-56.7785057137568,
-50.1755447720656));
#241206=CARTESIAN_POINT('Ctrl Pts',(-42.7225942132042,-56.5367374890622,
-50.162347139195));
#241207=CARTESIAN_POINT('Ctrl Pts',(-43.0214952362546,-56.1130252706333,
-50.134888939872));
#241208=CARTESIAN_POINT('Ctrl Pts',(-43.2082285435438,-55.9338806860874,
-50.1202304685317));
#241209=CARTESIAN_POINT('Ctrl Pts',(-43.6475740771907,-55.6504146457762,
-50.0897677860873));
#241210=CARTESIAN_POINT('Ctrl Pts',(-43.8981505276236,-55.5521267023332,
-50.0742423960563));
#241211=CARTESIAN_POINT('Ctrl Pts',(-44.4119099094751,-55.4615313574422,
-50.0456458590569));
#241212=CARTESIAN_POINT('Ctrl Pts',(-44.6693028709624,-55.4657084686857,
-50.0333330761666));
#241213=CARTESIAN_POINT('Ctrl Pts',(-45.172880169066,-55.5714664870943,
-50.0048086745423));
#241214=CARTESIAN_POINT('Ctrl Pts',(-45.4139467989259,-55.6736629018997,
-49.9896497059584));
#241215=CARTESIAN_POINT('Ctrl Pts',(-45.84832585836,-55.967579699605,-49.9591331068387));
#241216=CARTESIAN_POINT('Ctrl Pts',(-46.036212499502,-56.1583542910206,
-49.9440771626739));
#241217=CARTESIAN_POINT('Ctrl Pts',(-46.320100302134,-56.5921374674081,
-49.9170836671766));
#241218=CARTESIAN_POINT('Ctrl Pts',(-46.417292771059,-56.8284632261593,
-49.903941039711));
#241219=CARTESIAN_POINT('Ctrl Pts',(-46.5201186902985,-57.3338550090348,
-49.8744598523766));
#241220=CARTESIAN_POINT('Ctrl Pts',(-46.521319403242,-57.5988038392898,
-49.859004503945));
#241221=CARTESIAN_POINT('Ctrl Pts',(-46.4209398179983,-58.1161341573481,
-49.8288269020583));
#241222=CARTESIAN_POINT('Ctrl Pts',(-46.3195313044318,-58.363217860143,
-49.8151577856296));
#241223=CARTESIAN_POINT('Ctrl Pts',(-46.0313398527511,-58.7963238182018,
-49.7879666299516));
#241224=CARTESIAN_POINT('Ctrl Pts',(-45.850147359489,-58.9800728327082,
-49.7734537744037));
#241225=CARTESIAN_POINT('Ctrl Pts',(-45.4202000744181,-59.2750097298543,
-49.7431313074193));
#241226=CARTESIAN_POINT('Ctrl Pts',(-45.1732993036512,-59.3801668480655,
-49.7275912549891));
#241227=CARTESIAN_POINT('Ctrl Pts',(-44.7794705425607,-59.4616264148727,
-49.7053198510996));
#241228=CARTESIAN_POINT('Ctrl Pts',(-44.6437432571755,-59.475452478349,
-49.6980598997489));
#241229=CARTESIAN_POINT('Ctrl Pts',(-44.5079524583206,-59.475452478349,
-49.6912000000001));
#241230=CARTESIAN_POINT('Origin',(-44.5079524583206,-57.475452478349,235.35105));
#241231=CARTESIAN_POINT('',(-44.5079524583205,-59.475452478349,-48.9912000000001));
#241232=CARTESIAN_POINT('',(-44.5079524583204,-59.475452478349,-49.1499499999999));
#241233=CARTESIAN_POINT('',(-44.5079524583206,-59.475452478349,235.35105));
#241234=CARTESIAN_POINT('Ctrl Pts',(-44.5079524583202,-59.475452478349,
-49.1499499999999));
#241235=CARTESIAN_POINT('Ctrl Pts',(-44.7019516755273,-59.475452478349,
-49.1597504812741));
#241236=CARTESIAN_POINT('Ctrl Pts',(-44.8952411044441,-59.4472344414536,
-49.1703381314341));
#241237=CARTESIAN_POINT('Ctrl Pts',(-45.3341697230981,-59.3157735812064,
-49.1963462676865));
#241238=CARTESIAN_POINT('Ctrl Pts',(-45.5691499075924,-59.1910487434321,
-49.2118548393225));
#241239=CARTESIAN_POINT('Ctrl Pts',(-45.9697612694271,-58.8638105260088,
-49.2416374316203));
#241240=CARTESIAN_POINT('Ctrl Pts',(-46.1339073546182,-58.667343055432,
-49.2554230496701));
#241241=CARTESIAN_POINT('Ctrl Pts',(-46.3855343432818,-58.213681630364,
-49.2818866327991));
#241242=CARTESIAN_POINT('Ctrl Pts',(-46.4667320066789,-57.9585961298683,
-49.296766620328));
#241243=CARTESIAN_POINT('Ctrl Pts',(-46.5244476178428,-57.4363955805834,
-49.3272283190364));
#241244=CARTESIAN_POINT('Ctrl Pts',(-46.5022497916875,-57.1745033260573,
-49.3425053672171));
#241245=CARTESIAN_POINT('Ctrl Pts',(-46.3604735179476,-56.6800310354043,
-49.3713495841718));
#241246=CARTESIAN_POINT('Ctrl Pts',(-46.2446066891854,-56.4514645244218,
-49.3837504255677));
#241247=CARTESIAN_POINT('Ctrl Pts',(-45.925185283618,-56.0391191431053,
-49.4119137438739));
#241248=CARTESIAN_POINT('Ctrl Pts',(-45.7205380520192,-55.8626272248705,
-49.4273998240695));
#241249=CARTESIAN_POINT('Ctrl Pts',(-45.2629408143957,-55.6056411808176,
-49.4580122155826));
#241250=CARTESIAN_POINT('Ctrl Pts',(-45.0163543710696,-55.5241038847157,
-49.4728474772943));
#241251=CARTESIAN_POINT('Ctrl Pts',(-44.503775747153,-55.4587082044725,
-49.50064937437));
#241252=CARTESIAN_POINT('Ctrl Pts',(-44.2425846895981,-55.4762355767426,
-49.5133787287316));
#241253=CARTESIAN_POINT('Ctrl Pts',(-43.7366604177638,-55.6113340358778,
-49.542877457978));
#241254=CARTESIAN_POINT('Ctrl Pts',(-43.4973904340246,-55.7294335646316,
-49.5584095041497));
#241255=CARTESIAN_POINT('Ctrl Pts',(-43.086470406459,-56.0457416171329,
-49.5883940746774));
#241256=CARTESIAN_POINT('Ctrl Pts',(-42.916324862786,-56.2379335754247,
-49.602595111312));
#241257=CARTESIAN_POINT('Ctrl Pts',(-42.6517993134929,-56.6849379663124,
-49.628996080375));
#241258=CARTESIAN_POINT('Ctrl Pts',(-42.5634518622002,-56.937639760177,
-49.6435775914398));
#241259=CARTESIAN_POINT('Ctrl Pts',(-42.4910559618037,-57.4588734433419,
-49.6739828896244));
#241260=CARTESIAN_POINT('Ctrl Pts',(-42.5061103059526,-57.7219964938289,
-49.6893317342361));
#241261=CARTESIAN_POINT('Ctrl Pts',(-42.6345915085431,-58.2203002441122,
-49.7183994530026));
#241262=CARTESIAN_POINT('Ctrl Pts',(-42.7439706046001,-58.4514791784199,
-49.7309710147522));
#241263=CARTESIAN_POINT('Ctrl Pts',(-43.0501967270924,-58.8701946608091,
-49.7586535264024));
#241264=CARTESIAN_POINT('Ctrl Pts',(-43.2477956880408,-59.0509921616579,
-49.7739091205071));
#241265=CARTESIAN_POINT('Ctrl Pts',(-43.6958317872822,-59.3212746258446,
-49.804426313265));
#241266=CARTESIAN_POINT('Ctrl Pts',(-43.9405552984306,-59.4105720159264,
-49.8193937991665));
#241267=CARTESIAN_POINT('Ctrl Pts',(-44.2990888000906,-59.4672790910993,
-49.8391602042242));
#241268=CARTESIAN_POINT('Ctrl Pts',(-44.4035512640085,-59.475452478349,
-49.8446758449564));
#241269=CARTESIAN_POINT('Ctrl Pts',(-44.5079524583205,-59.475452478349,
-49.8499499999999));
#241270=CARTESIAN_POINT('Ctrl Pts',(-44.5079524583206,-59.475452478349,
-49.6912000000001));
#241271=CARTESIAN_POINT('Ctrl Pts',(-44.3885780724371,-59.475452478349,
-49.6851694270405));
#241272=CARTESIAN_POINT('Ctrl Pts',(-44.269186440873,-59.4647669035076,
-49.6788263202615));
#241273=CARTESIAN_POINT('Ctrl Pts',(-43.8966411141707,-59.397228324263,
-49.6580361448761));
#241274=CARTESIAN_POINT('Ctrl Pts',(-43.6534734865964,-59.3021339659884,
-49.6429781810931));
#241275=CARTESIAN_POINT('Ctrl Pts',(-43.2114016638356,-59.0211756506772,
-49.6124509135494));
#241276=CARTESIAN_POINT('Ctrl Pts',(-43.0180908202016,-58.8358411034676,
-49.5972796166733));
#241277=CARTESIAN_POINT('Ctrl Pts',(-42.7218475977894,-58.4103169154255,
-49.5699028354042));
#241278=CARTESIAN_POINT('Ctrl Pts',(-42.6179300357161,-58.1768709471206,
-49.5571160773453));
#241279=CARTESIAN_POINT('Ctrl Pts',(-42.5008395774885,-57.6753697000545,
-49.527861837933));
#241280=CARTESIAN_POINT('Ctrl Pts',(-42.4919282202469,-57.4113466039644,
-49.5124604906611));
#241281=CARTESIAN_POINT('Ctrl Pts',(-42.5771568260949,-56.889448221801,
-49.4820164183682));
#241282=CARTESIAN_POINT('Ctrl Pts',(-42.6725922982354,-56.6371497732339,
-49.467801834985));
#241283=CARTESIAN_POINT('Ctrl Pts',(-42.9504544477179,-56.1951104579857,
-49.4408719402785));
#241284=CARTESIAN_POINT('Ctrl Pts',(-43.1262646751023,-56.0071300685192,
-49.4265075717347));
#241285=CARTESIAN_POINT('Ctrl Pts',(-43.5469878758011,-55.7015412112566,
-49.3963404062447));
#241286=CARTESIAN_POINT('Ctrl Pts',(-43.7902191393219,-55.5899580215752,
-49.3807983034421));
#241287=CARTESIAN_POINT('Ctrl Pts',(-44.2989467591262,-55.4697764255278,
-49.3515930294198));
#241288=CARTESIAN_POINT('Ctrl Pts',(-44.5588010092762,-55.4595586946896,
-49.339094794039));
#241289=CARTESIAN_POINT('Ctrl Pts',(-45.0684884434839,-55.5383462550722,
-49.3110483580103));
#241290=CARTESIAN_POINT('Ctrl Pts',(-45.3134418880181,-55.6267395221787,
-49.2960956265532));
#241291=CARTESIAN_POINT('Ctrl Pts',(-45.7623829581058,-55.895349048267,
-49.2655815103716));
#241292=CARTESIAN_POINT('Ctrl Pts',(-45.9606395150753,-56.0754311885403,
-49.2503135604168));
#241293=CARTESIAN_POINT('Ctrl Pts',(-46.2684150070898,-56.4930786251726,
-49.2225839288215));
#241294=CARTESIAN_POINT('Ctrl Pts',(-46.3786445516313,-56.7239102050038,
-49.210039965945));
#241295=CARTESIAN_POINT('Ctrl Pts',(-46.5088833214484,-57.2217135426928,
-49.1810014379132));
#241296=CARTESIAN_POINT('Ctrl Pts',(-46.5248838699055,-57.484685009209,
-49.1656614356997));
#241297=CARTESIAN_POINT('Ctrl Pts',(-46.4544244517634,-58.0060822547599,
-49.135246596376));
#241298=CARTESIAN_POINT('Ctrl Pts',(-46.3670135365742,-58.259097962154,
-49.1205933304447));
#241299=CARTESIAN_POINT('Ctrl Pts',(-46.1042025134809,-58.706983944617,
-49.0942532629833));
#241300=CARTESIAN_POINT('Ctrl Pts',(-45.9348472313648,-58.8997445162226,
-49.0800755643444));
#241301=CARTESIAN_POINT('Ctrl Pts',(-45.5253022608469,-59.2175094848837,
-49.050117965765));
#241302=CARTESIAN_POINT('Ctrl Pts',(-45.2865926692342,-59.3364987682916,
-49.0345882783886));
#241303=CARTESIAN_POINT('Ctrl Pts',(-44.8605785192526,-59.452085760637,
-49.0096955449969));
#241304=CARTESIAN_POINT('Ctrl Pts',(-44.6844897702049,-59.475452478349,
-49.0001183381472));
#241305=CARTESIAN_POINT('Ctrl Pts',(-44.5079524583203,-59.475452478349,
-48.9912000000001));
#241306=CARTESIAN_POINT('Origin',(-44.5079524583206,-57.475452478349,235.35105));
#241307=CARTESIAN_POINT('',(-44.5079524583205,-59.475452478349,-48.2912000000001));
#241308=CARTESIAN_POINT('',(-44.5079524583205,-59.475452478349,-48.4499499999999));
#241309=CARTESIAN_POINT('',(-44.5079524583206,-59.475452478349,235.35105));
#241310=CARTESIAN_POINT('Ctrl Pts',(-44.5079524583205,-59.475452478349,
-48.4499499999999));
#241311=CARTESIAN_POINT('Ctrl Pts',(-44.7430370280651,-59.475452478349,
-48.461826037217));
#241312=CARTESIAN_POINT('Ctrl Pts',(-44.9765380902944,-59.434011449719,
-48.4748307752346));
#241313=CARTESIAN_POINT('Ctrl Pts',(-45.4435506997623,-59.262418474562,
-48.5034281827251));
#241314=CARTESIAN_POINT('Ctrl Pts',(-45.6692665229574,-59.1246781509403,
-48.518848354318));
#241315=CARTESIAN_POINT('Ctrl Pts',(-46.0484296267242,-58.7758705731551,
-48.5481765266724));
#241316=CARTESIAN_POINT('Ctrl Pts',(-46.2005301026568,-58.5705789077536,
-48.5610676249514));
#241317=CARTESIAN_POINT('Ctrl Pts',(-46.4252545442384,-58.1033792102185,
-48.588320940641));
#241318=CARTESIAN_POINT('Ctrl Pts',(-46.4915176197873,-57.8439172034373,
-48.6034562243699));
#241319=CARTESIAN_POINT('Ctrl Pts',(-46.5186841281559,-57.3206040777301,
-48.6339828233695));
#241320=CARTESIAN_POINT('Ctrl Pts',(-46.4817823289692,-57.0618844316932,
-48.6490748027217));
#241321=CARTESIAN_POINT('Ctrl Pts',(-46.3123784502638,-56.5757072795242,
-48.6774351365982));
#241322=CARTESIAN_POINT('Ctrl Pts',(-46.1825930825342,-56.3524770495347,
-48.6897703728452));
#241323=CARTESIAN_POINT('Ctrl Pts',(-45.83923971478,-55.9593941285552,-48.7185808678125));
#241324=CARTESIAN_POINT('Ctrl Pts',(-45.6260387883208,-55.7959827045881,
-48.7341175504196));
#241325=CARTESIAN_POINT('Ctrl Pts',(-45.1573046245358,-55.5665713247126,
-48.7644882977844));
#241326=CARTESIAN_POINT('Ctrl Pts',(-44.9079518312746,-55.4992122245449,
-48.7790497796583));
#241327=CARTESIAN_POINT('Ctrl Pts',(-44.3896726195646,-55.4616184041298,
-48.8063287722967));
#241328=CARTESIAN_POINT('Ctrl Pts',(-44.1254992307615,-55.4947231661162,
-48.8198328906914));
#241329=CARTESIAN_POINT('Ctrl Pts',(-43.6261149392988,-55.6612417325591,
-48.8499176520344));
#241330=CARTESIAN_POINT('Ctrl Pts',(-43.3957223068424,-55.7926152285137,
-48.8653883882319));
#241331=CARTESIAN_POINT('Ctrl Pts',(-43.0059075585446,-56.1308069479149,
-48.8949450327441));
#241332=CARTESIAN_POINT('Ctrl Pts',(-42.8478521658473,-56.3316785550261,
-48.9082298544728));
#241333=CARTESIAN_POINT('Ctrl Pts',(-42.6096712164602,-56.7921899013986,
-48.9350930163445));
#241334=CARTESIAN_POINT('Ctrl Pts',(-42.5359218161572,-57.0495793664238,
-48.9501074018042));
#241335=CARTESIAN_POINT('Ctrl Pts',(-42.4935129329832,-57.5725617747053,
-48.9806147089539));
#241336=CARTESIAN_POINT('Ctrl Pts',(-42.5231101205008,-57.8329665762101,
-48.9958049890417));
#241337=CARTESIAN_POINT('Ctrl Pts',(-42.6787365533554,-58.3233357959971,
-49.0244098601959));
#241338=CARTESIAN_POINT('Ctrl Pts',(-42.8015034319804,-58.5492143585533,
-49.0367280760931));
#241339=CARTESIAN_POINT('Ctrl Pts',(-43.1328738911161,-58.9520496191419,
-49.0652176599413));
#241340=CARTESIAN_POINT('Ctrl Pts',(-43.3418723851366,-59.1220882452236,
-49.0807353368372));
#241341=CARTESIAN_POINT('Ctrl Pts',(-43.8052062623671,-59.365424015634,
-49.1112393997809));
#241342=CARTESIAN_POINT('Ctrl Pts',(-44.0532680775006,-59.4399225452165,
-49.1259438971879));
#241343=CARTESIAN_POINT('Ctrl Pts',(-44.3750039639929,-59.4721422398772,
-49.1431371395912));
#241344=CARTESIAN_POINT('Ctrl Pts',(-44.4415149442898,-59.475452478349,
-49.1465936997965));
#241345=CARTESIAN_POINT('Ctrl Pts',(-44.5079524583202,-59.475452478349,
-49.1499499999999));
#241346=CARTESIAN_POINT('Ctrl Pts',(-44.5079524583203,-59.475452478349,
-48.9912000000001));
#241347=CARTESIAN_POINT('Ctrl Pts',(-44.4259098953645,-59.475452478349,
-48.987055361617));
#241348=CARTESIAN_POINT('Ctrl Pts',(-44.3437854394165,-59.4704047613634,
-48.9827593610728));
#241349=CARTESIAN_POINT('Ctrl Pts',(-44.0067217856789,-59.4286432605234,
-48.9645134855666));
#241350=CARTESIAN_POINT('Ctrl Pts',(-43.7599263287128,-59.3480471172143,
-48.9496951151626));
#241351=CARTESIAN_POINT('Ctrl Pts',(-43.3015381377503,-59.09288174759,-48.9190958691554));
#241352=CARTESIAN_POINT('Ctrl Pts',(-43.0962970319428,-58.9172480387275,
-48.903604818641));
#241353=CARTESIAN_POINT('Ctrl Pts',(-42.7752695593589,-58.5061689076375,
-48.875397297101));
#241354=CARTESIAN_POINT('Ctrl Pts',(-42.6584805553404,-58.277966884615,
-48.8630133403658));
#241355=CARTESIAN_POINT('Ctrl Pts',(-42.5148357827412,-57.7840415274964,
-48.8342010278671));
#241356=CARTESIAN_POINT('Ctrl Pts',(-42.491636918027,-57.5223377588128,
-48.8189349746939));
#241357=CARTESIAN_POINT('Ctrl Pts',(-42.5472895037159,-57.0000055215278,
-48.7884655941856));
#241358=CARTESIAN_POINT('Ctrl Pts',(-42.6274873819553,-56.7445964917713,
-48.7735667341164));
#241359=CARTESIAN_POINT('Ctrl Pts',(-42.8773051311541,-56.2900038195635,
-48.7470488282376));
#241360=CARTESIAN_POINT('Ctrl Pts',(-43.0406230148019,-56.0929441708537,
-48.7333369411703));
#241361=CARTESIAN_POINT('Ctrl Pts',(-43.4397728318041,-55.7642112632147,
-48.7035845882801));
#241362=CARTESIAN_POINT('Ctrl Pts',(-43.6741413291616,-55.6385750584568,
-48.6880803364087));
#241363=CARTESIAN_POINT('Ctrl Pts',(-44.1765003305804,-55.4858217928749,
-48.658246786168));
#241364=CARTESIAN_POINT('Ctrl Pts',(-44.4393434915333,-55.4595761570491,
-48.6451290573474));
#241365=CARTESIAN_POINT('Ctrl Pts',(-44.9551883989394,-55.5092856781278,
-48.6176196666527));
#241366=CARTESIAN_POINT('Ctrl Pts',(-45.203438467538,-55.5828102316503,
-48.6029340666643));
#241367=CARTESIAN_POINT('Ctrl Pts',(-45.6675337712541,-55.824251070524,
-48.5724468067007));
#241368=CARTESIAN_POINT('Ctrl Pts',(-45.8771180295607,-55.9933904222787,
-48.5569257669122));
#241369=CARTESIAN_POINT('Ctrl Pts',(-46.2101309659608,-56.3949019520463,
-48.5283918169692));
#241370=CARTESIAN_POINT('Ctrl Pts',(-46.3338537554103,-56.6204150673259,
-48.5160771823096));
#241371=CARTESIAN_POINT('Ctrl Pts',(-46.4913750186542,-57.1102141906313,
-48.4875055667834));
#241372=CARTESIAN_POINT('Ctrl Pts',(-46.5219804278959,-57.3703993207582,
-48.4723281008594));
#241373=CARTESIAN_POINT('Ctrl Pts',(-46.4816675517556,-57.8934536961542,
-48.441816595628));
#241374=CARTESIAN_POINT('Ctrl Pts',(-46.40894351168,-58.1511412894893,-48.4267848193501));
#241375=CARTESIAN_POINT('Ctrl Pts',(-46.1726084551324,-58.6125800873386,
-48.3998675561423));
#241376=CARTESIAN_POINT('Ctrl Pts',(-46.0153779364691,-58.8140570978205,
-48.3866430428381));
#241377=CARTESIAN_POINT('Ctrl Pts',(-45.6270334709081,-59.1537251060519,
-48.3571176158634));
#241378=CARTESIAN_POINT('Ctrl Pts',(-45.3972776717518,-59.2859889199384,
-48.3416530836987));
#241379=CARTESIAN_POINT('Ctrl Pts',(-44.9418533362197,-59.4399713428427,
-48.3141547354598));
#241380=CARTESIAN_POINT('Ctrl Pts',(-44.7254848228503,-59.475452478349,
-48.3021893323067));
#241381=CARTESIAN_POINT('Ctrl Pts',(-44.5079524583203,-59.475452478349,
-48.2912000000001));
#241382=CARTESIAN_POINT('Origin',(-44.5079524583206,-57.475452478349,235.35105));
#241383=CARTESIAN_POINT('',(-44.5079524583206,-59.475452478349,-47.5912000000001));
#241384=CARTESIAN_POINT('',(-44.5079524583206,-59.475452478349,-47.7499499999999));
#241385=CARTESIAN_POINT('',(-44.5079524583206,-59.475452478349,235.35105));
#241386=CARTESIAN_POINT('Ctrl Pts',(-44.5079524583206,-59.475452478349,
-47.7499499999999));
#241387=CARTESIAN_POINT('Ctrl Pts',(-44.5157926193897,-59.475452478349,
-47.7503460704215));
#241388=CARTESIAN_POINT('Ctrl Pts',(-44.5236346243393,-59.475406377275,
-47.7507435786071));
#241389=CARTESIAN_POINT('Ctrl Pts',(-44.7965847178638,-59.4721954961175,
-47.7646261626801));
#241390=CARTESIAN_POINT('Ctrl Pts',(-45.0583911087667,-59.4163947421566,
-47.7794796588187));
#241391=CARTESIAN_POINT('Ctrl Pts',(-45.5407450561074,-59.2078465043819,
-47.8099299441212));
#241392=CARTESIAN_POINT('Ctrl Pts',(-45.7573651276197,-59.0587499264138,
-47.8252218392644));
#241393=CARTESIAN_POINT('Ctrl Pts',(-46.1166477375133,-58.6905943186293,
-47.8541100034177));
#241394=CARTESIAN_POINT('Ctrl Pts',(-46.2577322577609,-58.4768160833543,
-47.8665371230414));
#241395=CARTESIAN_POINT('Ctrl Pts',(-46.4577427899821,-57.9950663769071,
-47.8946391892509));
#241396=CARTESIAN_POINT('Ctrl Pts',(-46.5097010685008,-57.7297147229521,
-47.9101180357316));
#241397=CARTESIAN_POINT('Ctrl Pts',(-46.506182691861,-57.2046317958789,
-47.9407478731442));
#241398=CARTESIAN_POINT('Ctrl Pts',(-46.4547739127248,-56.9499188909053,
-47.9556061259344));
#241399=CARTESIAN_POINT('Ctrl Pts',(-46.2575857249768,-56.4725146387524,
-47.98345470731));
#241400=CARTESIAN_POINT('Ctrl Pts',(-46.1131472434065,-56.2546075239529,
-47.9961331758922));
#241401=CARTESIAN_POINT('Ctrl Pts',(-45.7453691322896,-55.8821210794356,
-48.0255768331097));
#241402=CARTESIAN_POINT('Ctrl Pts',(-45.5241381173083,-55.7326789994757,
-48.0411117417214));
#241403=CARTESIAN_POINT('Ctrl Pts',(-45.0455500066651,-55.5323263409505,
-48.0711327461981));
#241404=CARTESIAN_POINT('Ctrl Pts',(-44.7941741147582,-55.4797385821954,
-48.0853656004787));
#241405=CARTESIAN_POINT('Ctrl Pts',(-44.2746766753311,-55.4715031245149,
-48.1118498501461));
#241406=CARTESIAN_POINT('Ctrl Pts',(-44.0113919228789,-55.5200091917417,
-48.1263348897029));
#241407=CARTESIAN_POINT('Ctrl Pts',(-43.5226643663141,-55.7155033463606,
-48.156726413851));
#241408=CARTESIAN_POINT('Ctrl Pts',(-43.3014924724896,-55.859074841667,
-48.1720871103856));
#241409=CARTESIAN_POINT('Ctrl Pts',(-42.9323851716076,-56.2177417601912,
-48.2011948463009));
#241410=CARTESIAN_POINT('Ctrl Pts',(-42.7858689475892,-56.427284799075,
-48.2138068853757));
#241411=CARTESIAN_POINT('Ctrl Pts',(-42.5740319970683,-56.90072936033,-48.2414244847822));
#241412=CARTESIAN_POINT('Ctrl Pts',(-42.5149552732893,-57.1619571957634,
-48.2566627751824));
#241413=CARTESIAN_POINT('Ctrl Pts',(-42.5022899998702,-57.6851701559193,
-48.2871835311915));
#241414=CARTESIAN_POINT('Ctrl Pts',(-42.5460828168514,-57.9420979254273,
-48.3021709844128));
#241415=CARTESIAN_POINT('Ctrl Pts',(-42.7286059994751,-58.4241879338099,
-48.3302929015684));
#241416=CARTESIAN_POINT('Ctrl Pts',(-42.8652213300627,-58.6449019543281,
-48.3427378745441));
#241417=CARTESIAN_POINT('Ctrl Pts',(-43.2200686874805,-59.028421094374,
-48.3718500809782));
#241418=CARTESIAN_POINT('Ctrl Pts',(-43.4371401100596,-59.1853352594998,
-48.3873927905004));
#241419=CARTESIAN_POINT('Ctrl Pts',(-43.9107079826349,-59.4011832891677,
-48.4176121301696));
#241420=CARTESIAN_POINT('Ctrl Pts',(-44.1611161152121,-59.4616265808456,
-48.4320252147509));
#241421=CARTESIAN_POINT('Ctrl Pts',(-44.4467642018672,-59.4747510539149,
-48.4468384243579));
#241422=CARTESIAN_POINT('Ctrl Pts',(-44.4773707112758,-59.475452478349,
-48.4484050667596));
#241423=CARTESIAN_POINT('Ctrl Pts',(-44.5079524583205,-59.475452478349,
-48.4499499999999));
#241424=CARTESIAN_POINT('Ctrl Pts',(-44.5079524583203,-59.475452478349,
-48.2912000000001));
#241425=CARTESIAN_POINT('Ctrl Pts',(-44.4621954116032,-59.475452478349,
-48.2888884387167));
#241426=CARTESIAN_POINT('Ctrl Pts',(-44.4163914604066,-59.4738822430967,
-48.2865287093776));
#241427=CARTESIAN_POINT('Ctrl Pts',(-44.1153387113921,-59.4531611952842,
-48.2707157179857));
#241428=CARTESIAN_POINT('Ctrl Pts',(-43.8658276208728,-59.3867643302114,
-48.2561743044177));
#241429=CARTESIAN_POINT('Ctrl Pts',(-43.3963975797605,-59.1592356822322,
-48.2258233156324));
#241430=CARTESIAN_POINT('Ctrl Pts',(-43.1826463715709,-58.9967236975126,
-48.2102850674558));
#241431=CARTESIAN_POINT('Ctrl Pts',(-42.8376871341619,-58.604963811654,
-48.1814320354511));
#241432=CARTESIAN_POINT('Ctrl Pts',(-42.7069540844508,-58.3820868789375,
-48.1690870067012));
#241433=CARTESIAN_POINT('Ctrl Pts',(-42.5357120482107,-57.8964763928939,
-48.1407597283487));
#241434=CARTESIAN_POINT('Ctrl Pts',(-42.4978407438657,-57.6379968708878,
-48.1256817562316));
#241435=CARTESIAN_POINT('Ctrl Pts',(-42.5229742600458,-57.1146733989098,
-48.0951545536995));
#241436=CARTESIAN_POINT('Ctrl Pts',(-42.5882336096158,-56.8549517116878,
-48.0800041219449));
#241437=CARTESIAN_POINT('Ctrl Pts',(-42.8111568346108,-56.3868696565536,
-48.0526993353954));
#241438=CARTESIAN_POINT('Ctrl Pts',(-42.9624701342427,-56.1809849963628,
-48.039852937411));
#241439=CARTESIAN_POINT('Ctrl Pts',(-43.3402192219354,-55.8307817084993,
-48.01055549032));
#241440=CARTESIAN_POINT('Ctrl Pts',(-43.5653034425167,-55.6922107984702,
-47.9951430006849));
#241441=CARTESIAN_POINT('Ctrl Pts',(-44.0605946738937,-55.5079736091455,
-47.964748219992));
#241442=CARTESIAN_POINT('Ctrl Pts',(-44.3265194290946,-55.4659462558285,
-47.9506429255464));
#241443=CARTESIAN_POINT('Ctrl Pts',(-44.8477921988355,-55.4880805475756,
-47.9236636068181));
#241444=CARTESIAN_POINT('Ctrl Pts',(-45.0983247630082,-55.547615488173,
-47.9092707297562));
#241445=CARTESIAN_POINT('Ctrl Pts',(-45.5724986425265,-55.7616765882054,
-47.8790728945193));
#241446=CARTESIAN_POINT('Ctrl Pts',(-45.7900638885917,-55.9177317315564,
-47.8635302927506));
#241447=CARTESIAN_POINT('Ctrl Pts',(-46.1464129696538,-56.2999848121768,
-47.8343791487517));
#241448=CARTESIAN_POINT('Ctrl Pts',(-46.2839289948305,-56.520371900573,
-47.8219130337035));
#241449=CARTESIAN_POINT('Ctrl Pts',(-46.4681601359308,-57.0019225276565,
-47.7938225804569));
#241450=CARTESIAN_POINT('Ctrl Pts',(-46.5128449253758,-57.2586037516272,
-47.7788495090587));
#241451=CARTESIAN_POINT('Ctrl Pts',(-46.502065453837,-57.7817739277742,
-47.7483312487834));
#241452=CARTESIAN_POINT('Ctrl Pts',(-46.4439278569422,-58.0432165967563,
-47.7330804264262));
#241453=CARTESIAN_POINT('Ctrl Pts',(-46.2337741368597,-58.5174649721109,
-47.7054159378638));
#241454=CARTESIAN_POINT('Ctrl Pts',(-46.087979354215,-58.7275648603756,
-47.6928334223038));
#241455=CARTESIAN_POINT('Ctrl Pts',(-45.7201749141811,-59.0874981065514,
-47.6637545699499));
#241456=CARTESIAN_POINT('Ctrl Pts',(-45.4996004399675,-59.2318121470762,
-47.6484023963791));
#241457=CARTESIAN_POINT('Ctrl Pts',(-45.0192141980181,-59.4260158553972,
-47.6184698980189));
#241458=CARTESIAN_POINT('Ctrl Pts',(-44.7646955321978,-59.475452478349,
-47.6041701847465));
#241459=CARTESIAN_POINT('Ctrl Pts',(-44.5079524583206,-59.475452478349,
-47.5912000000001));
#241460=CARTESIAN_POINT('Origin',(-44.5079524583206,-57.475452478349,235.35105));
#241461=CARTESIAN_POINT('',(-44.5079524583207,-59.475452478349,-46.8912000000001));
#241462=CARTESIAN_POINT('',(-44.5079524583207,-59.475452478349,-47.0499499999999));
#241463=CARTESIAN_POINT('',(-44.5079524583206,-59.475452478349,235.35105));
#241464=CARTESIAN_POINT('Ctrl Pts',(-44.5079524583209,-59.475452478349,
-47.0499499999999));
#241465=CARTESIAN_POINT('Ctrl Pts',(-44.554453134705,-59.475452478349,-47.0522991280773));
#241466=CARTESIAN_POINT('Ctrl Pts',(-44.6009987273649,-59.4738307924441,
-47.0546978244141));
#241467=CARTESIAN_POINT('Ctrl Pts',(-44.912068432154,-59.4520723435267,
-47.0710471113981));
#241468=CARTESIAN_POINT('Ctrl Pts',(-45.1702827452092,-59.3811311768095,
-47.0861607377864));
#241469=CARTESIAN_POINT('Ctrl Pts',(-45.6384714922981,-59.1454875048052,
-47.1166857068967));
#241470=CARTESIAN_POINT('Ctrl Pts',(-45.845046645952,-58.985184775525,-47.1317969974673));
#241471=CARTESIAN_POINT('Ctrl Pts',(-46.1833632812087,-58.5972263874509,
-47.160203580491));
#241472=CARTESIAN_POINT('Ctrl Pts',(-46.3128857665671,-58.3741145541745,
-47.1725280455769));
#241473=CARTESIAN_POINT('Ctrl Pts',(-46.4843556329206,-57.8812457960168,
-47.2012787231362));
#241474=CARTESIAN_POINT('Ctrl Pts',(-46.5207502878101,-57.6149470298648,
-47.2168128178284));
#241475=CARTESIAN_POINT('Ctrl Pts',(-46.4878332043256,-57.0938436840021,
-47.2472105130038));
#241476=CARTESIAN_POINT('Ctrl Pts',(-46.4227720017422,-56.8437420795107,
-47.2617997732658));
#241477=CARTESIAN_POINT('Ctrl Pts',(-46.1987488490944,-56.3752321350285,
-47.2891295200273));
#241478=CARTESIAN_POINT('Ctrl Pts',(-46.0394483233293,-56.1625034323286,
-47.302542678224));
#241479=CARTESIAN_POINT('Ctrl Pts',(-45.6478297363726,-55.8111938166951,
-47.3325730546324));
#241480=CARTESIAN_POINT('Ctrl Pts',(-45.4195000234809,-55.6759647095067,
-47.3480520312806));
#241481=CARTESIAN_POINT('Ctrl Pts',(-44.9324736341766,-55.5046606707868,
-47.3776520705612));
#241482=CARTESIAN_POINT('Ctrl Pts',(-44.6796392315179,-55.4667966578895,
-47.3910242406569));
#241483=CARTESIAN_POINT('Ctrl Pts',(-44.1615720164789,-55.487907304876,
-47.417811764391));
#241484=CARTESIAN_POINT('Ctrl Pts',(-43.901443977928,-55.5512863718557,
-47.4328015074059));
#241485=CARTESIAN_POINT('Ctrl Pts',(-43.4259620690812,-55.7734635967845,
-47.4633021421722));
#241486=CARTESIAN_POINT('Ctrl Pts',(-43.2142804121466,-55.9282292382173,
-47.4785099054385));
#241487=CARTESIAN_POINT('Ctrl Pts',(-42.8654157666587,-56.3062986137255,
-47.5071609248768));
#241488=CARTESIAN_POINT('Ctrl Pts',(-42.730077021945,-56.5246626077399,
-47.5194872575478));
#241489=CARTESIAN_POINT('Ctrl Pts',(-42.5441636461992,-57.011993405316,
-47.5479148874064));
#241490=CARTESIAN_POINT('Ctrl Pts',(-42.4999150827817,-57.2779236701761,
-47.5634274861899));
#241491=CARTESIAN_POINT('Ctrl Pts',(-42.5180336880231,-57.8012381724356,
-47.5939541654883));
#241492=CARTESIAN_POINT('Ctrl Pts',(-42.5762410848256,-58.0537598286179,
-47.6086845954322));
#241493=CARTESIAN_POINT('Ctrl Pts',(-42.7866951827343,-58.5268191123656,
-47.6362797203175));
#241494=CARTESIAN_POINT('Ctrl Pts',(-42.9383900915285,-58.7421782610436,
-47.6492714505179));
#241495=CARTESIAN_POINT('Ctrl Pts',(-43.3179290873681,-59.1043602072032,
-47.6790086979881));
#241496=CARTESIAN_POINT('Ctrl Pts',(-43.542756808932,-59.2468604545175,
-47.6945228354385));
#241497=CARTESIAN_POINT('Ctrl Pts',(-44.018347888704,-59.4301501778751,
-47.723894766522));
#241498=CARTESIAN_POINT('Ctrl Pts',(-44.2621782516623,-59.475452478349,
-47.7375339421171));
#241499=CARTESIAN_POINT('Ctrl Pts',(-44.5079524583206,-59.475452478349,
-47.7499499999999));
#241500=CARTESIAN_POINT('Ctrl Pts',(-44.5079524583206,-59.475452478349,
-47.5912000000001));
#241501=CARTESIAN_POINT('Ctrl Pts',(-44.4998432267422,-59.475452478349,
-47.5907903366346));
#241502=CARTESIAN_POINT('Ctrl Pts',(-44.4917319195567,-59.475403158648,
-47.5903791299219));
#241503=CARTESIAN_POINT('Ctrl Pts',(-44.2291784192164,-59.4722085024506,
-47.577022235716));
#241504=CARTESIAN_POINT('Ctrl Pts',(-43.9777007086603,-59.4205837749565,
-47.5628123261575));
#241505=CARTESIAN_POINT('Ctrl Pts',(-43.4985314033797,-59.2221372272902,
-47.5328175557038));
#241506=CARTESIAN_POINT('Ctrl Pts',(-43.2768076913432,-59.0736178742876,
-47.5172846698186));
#241507=CARTESIAN_POINT('Ctrl Pts',(-42.907452770555,-58.7024976143473,
-47.4878012021461));
#241508=CARTESIAN_POINT('Ctrl Pts',(-42.7620494834633,-58.4849319964058,
-47.4750863052201));
#241509=CARTESIAN_POINT('Ctrl Pts',(-42.5630790326398,-58.0081056120536,
-47.4472714327996));
#241510=CARTESIAN_POINT('Ctrl Pts',(-42.5107516006776,-57.7536768518206,
-47.4324297551193));
#241511=CARTESIAN_POINT('Ctrl Pts',(-42.5052648978142,-57.2288086346005,
-47.4018124424481));
#241512=CARTESIAN_POINT('Ctrl Pts',(-42.5561860249955,-56.9633666331564,
-47.3863283256972));
#241513=CARTESIAN_POINT('Ctrl Pts',(-42.7543039331701,-56.4808577221684,
-47.3581819725562));
#241514=CARTESIAN_POINT('Ctrl Pts',(-42.8946125818443,-56.2664665314353,
-47.3457741867631));
#241515=CARTESIAN_POINT('Ctrl Pts',(-43.2524894351964,-55.8969644685894,
-47.3169177672217));
#241516=CARTESIAN_POINT('Ctrl Pts',(-43.4684496307538,-55.7470914534659,
-47.301636561692));
#241517=CARTESIAN_POINT('Ctrl Pts',(-43.9405559987394,-55.540767590807,
-47.2717688427325));
#241518=CARTESIAN_POINT('Ctrl Pts',(-44.1914799958216,-55.4842633210659,
-47.2574445857863));
#241519=CARTESIAN_POINT('Ctrl Pts',(-44.7138839733911,-55.468148873538,
-47.2305836993226));
#241520=CARTESIAN_POINT('Ctrl Pts',(-44.980503307442,-55.5137048163344,
-47.2162119128134));
#241521=CARTESIAN_POINT('Ctrl Pts',(-45.4741062072976,-55.7048858038013,
-47.1856998960573));
#241522=CARTESIAN_POINT('Ctrl Pts',(-45.6970536289956,-55.8462180502047,
-47.1703148145681));
#241523=CARTESIAN_POINT('Ctrl Pts',(-46.070058607397,-56.2010815829189,
-47.141121107287));
#241524=CARTESIAN_POINT('Ctrl Pts',(-46.2187357219036,-56.4089671497174,
-47.1284116441701));
#241525=CARTESIAN_POINT('Ctrl Pts',(-46.4355896459721,-56.8799995998964,
-47.100934751243));
#241526=CARTESIAN_POINT('Ctrl Pts',(-46.4974650403638,-57.1405654723828,
-47.085735075348));
#241527=CARTESIAN_POINT('Ctrl Pts',(-46.5157627592656,-57.6638654177115,
-47.0552092452038));
#241528=CARTESIAN_POINT('Ctrl Pts',(-46.4746397536553,-57.9215110250732,
-47.0401799181078));
#241529=CARTESIAN_POINT('Ctrl Pts',(-46.2972148278118,-58.4052011155574,
-47.0119646628295));
#241530=CARTESIAN_POINT('Ctrl Pts',(-46.1632721103581,-58.6268916802298,
-46.9995733740313));
#241531=CARTESIAN_POINT('Ctrl Pts',(-45.812900239099,-59.0141610223658,
-46.9705778799776));
#241532=CARTESIAN_POINT('Ctrl Pts',(-45.597316934554,-59.1736214523215,
-46.9550360813658));
#241533=CARTESIAN_POINT('Ctrl Pts',(-45.1255903396062,-59.3947747987772,
-46.924755021227));
#241534=CARTESIAN_POINT('Ctrl Pts',(-44.875571576505,-59.4579187488746,
-46.9102828376669));
#241535=CARTESIAN_POINT('Ctrl Pts',(-44.5829155271721,-59.4743998206703,
-46.8950176979641));
#241536=CARTESIAN_POINT('Ctrl Pts',(-44.5454166966125,-59.475452478349,
-46.8930926239556));
#241537=CARTESIAN_POINT('Ctrl Pts',(-44.5079524583208,-59.475452478349,
-46.8912000000001));
#241538=CARTESIAN_POINT('Origin',(-44.5079524583206,-57.475452478349,235.35105));
#241539=CARTESIAN_POINT('',(-44.5079524583208,-59.475452478349,-46.1912000000001));
#241540=CARTESIAN_POINT('',(-44.5079524583207,-59.475452478349,-46.3499499999999));
#241541=CARTESIAN_POINT('',(-44.5079524583206,-59.475452478349,235.35105));
#241542=CARTESIAN_POINT('Ctrl Pts',(-44.5079524583208,-59.475452478349,
-46.3499499999999));
#241543=CARTESIAN_POINT('Ctrl Pts',(-44.5908361851837,-59.475452478349,
-46.3541371324263));
#241544=CARTESIAN_POINT('Ctrl Pts',(-44.6737964586255,-59.4703007458636,
-46.3584783907082));
#241545=CARTESIAN_POINT('Ctrl Pts',(-45.0221714091031,-59.4266932865337,
-46.3773495324395));
#241546=CARTESIAN_POINT('Ctrl Pts',(-45.2785715363833,-59.340358089104,
-46.3928205020837));
#241547=CARTESIAN_POINT('Ctrl Pts',(-45.7332000740234,-59.0770467485376,
-46.4234674081851));
#241548=CARTESIAN_POINT('Ctrl Pts',(-45.9290817432164,-58.906102037805,
-46.4383488748448));
#241549=CARTESIAN_POINT('Ctrl Pts',(-46.2459051699612,-58.4984129368513,
-46.4662451398937));
#241550=CARTESIAN_POINT('Ctrl Pts',(-46.3635011048669,-58.2653115293938,
-46.4788748886891));
#241551=CARTESIAN_POINT('Ctrl Pts',(-46.5049851294361,-57.761535363337,
-46.5082618317092));
#241552=CARTESIAN_POINT('Ctrl Pts',(-46.5252725773139,-57.4951803379431,
-46.5237992081905));
#241553=CARTESIAN_POINT('Ctrl Pts',(-46.4622439250661,-56.9799096304069,
-46.5538566661302));
#241554=CARTESIAN_POINT('Ctrl Pts',(-46.3833552663526,-56.735365973496,
-46.5681217127833));
#241555=CARTESIAN_POINT('Ctrl Pts',(-46.133036947415,-56.279900627202,-46.5946905246505));
#241556=CARTESIAN_POINT('Ctrl Pts',(-45.9604381818125,-56.075230259504,
-46.6090795918312));
#241557=CARTESIAN_POINT('Ctrl Pts',(-45.5483555492046,-55.7474930231164,
-46.6394562462098));
#241558=CARTESIAN_POINT('Ctrl Pts',(-45.313926539347,-55.6264808190422,
-46.654828688374));
#241559=CARTESIAN_POINT('Ctrl Pts',(-44.8193921321944,-55.4836626264803,
-46.683977181636));
#241560=CARTESIAN_POINT('Ctrl Pts',(-44.5648339726336,-55.4602695427118,
-46.6966336155873));
#241561=CARTESIAN_POINT('Ctrl Pts',(-44.0486990700218,-55.5109070677797,
-46.7241847230859));
#241562=CARTESIAN_POINT('Ctrl Pts',(-43.792535812555,-55.5890557487495,
-46.739404953109));
#241563=CARTESIAN_POINT('Ctrl Pts',(-43.3317119004113,-55.837408838538,
-46.7699285557454));
#241564=CARTESIAN_POINT('Ctrl Pts',(-43.1301735590373,-56.0028763520636,
-46.7849360354254));
#241565=CARTESIAN_POINT('Ctrl Pts',(-42.8020680499677,-56.4002800798801,
-46.8131022603353));
#241566=CARTESIAN_POINT('Ctrl Pts',(-42.6781971428059,-56.6280819866651,
-46.8255200546518));
#241567=CARTESIAN_POINT('Ctrl Pts',(-42.5208805642364,-57.1262024590094,
-46.8545770822051));
#241568=CARTESIAN_POINT('Ctrl Pts',(-42.492126463739,-57.3926454432649,
-46.87011958962));
#241569=CARTESIAN_POINT('Ctrl Pts',(-42.5393672164669,-57.9112001860202,
-46.9003686162807));
#241570=CARTESIAN_POINT('Ctrl Pts',(-42.6110260474126,-58.1587652900053,
-46.9148099140131));
#241571=CARTESIAN_POINT('Ctrl Pts',(-42.8483243182583,-58.6227201281582,
-46.9418739462387));
#241572=CARTESIAN_POINT('Ctrl Pts',(-43.0152502744431,-58.8328355800266,
-46.9557984564599));
#241573=CARTESIAN_POINT('Ctrl Pts',(-43.4187222852275,-59.1731699315095,
-46.9861075340231));
#241574=CARTESIAN_POINT('Ctrl Pts',(-43.6502924057069,-59.301127519383,
-47.0015381240831));
#241575=CARTESIAN_POINT('Ctrl Pts',(-44.0968123151278,-59.4436164931208,
-47.0282514116003));
#241576=CARTESIAN_POINT('Ctrl Pts',(-44.3018947694972,-59.475452478349,
-47.0395403470652));
#241577=CARTESIAN_POINT('Ctrl Pts',(-44.5079524583209,-59.475452478349,
-47.0499499999999));
#241578=CARTESIAN_POINT('Ctrl Pts',(-44.5079524583208,-59.475452478349,
-46.8912000000001));
#241579=CARTESIAN_POINT('Ctrl Pts',(-44.2808580754121,-59.475452478349,
-46.8797276122286));
#241580=CARTESIAN_POINT('Ctrl Pts',(-44.0551473047433,-59.4367820789147,
-46.8671972353355));
#241581=CARTESIAN_POINT('Ctrl Pts',(-43.5933321620571,-59.2732901054593,
-46.8390986734603));
#241582=CARTESIAN_POINT('Ctrl Pts',(-43.3657623743608,-59.1380271069426,
-46.823657098329));
#241583=CARTESIAN_POINT('Ctrl Pts',(-42.9824160998001,-58.793366905255,
-46.7942385650673));
#241584=CARTESIAN_POINT('Ctrl Pts',(-42.8279825519172,-58.5898207593303,
-46.7812048163908));
#241585=CARTESIAN_POINT('Ctrl Pts',(-42.59795005691,-58.1252391266868,-46.7541042211533));
#241586=CARTESIAN_POINT('Ctrl Pts',(-42.5287310253326,-57.8665667397225,
-46.7390149985803));
#241587=CARTESIAN_POINT('Ctrl Pts',(-42.4955628885015,-57.343330519362,
-46.7084928857259));
#241588=CARTESIAN_POINT('Ctrl Pts',(-42.5295960628064,-57.0839230875256,
-46.6933607855354));
#241589=CARTESIAN_POINT('Ctrl Pts',(-42.6935751068041,-56.5960826489329,
-46.6649034266175));
#241590=CARTESIAN_POINT('Ctrl Pts',(-42.8205782309082,-56.3718114885146,
-46.65258682635));
#241591=CARTESIAN_POINT('Ctrl Pts',(-43.1592022603968,-55.9748533589649,
-46.6239022218791));
#241592=CARTESIAN_POINT('Ctrl Pts',(-43.3707644901368,-55.8088081333853,
-46.6083715039825));
#241593=CARTESIAN_POINT('Ctrl Pts',(-43.8374104957225,-55.5738739682217,
-46.5779451652662));
#241594=CARTESIAN_POINT('Ctrl Pts',(-44.0862767230464,-55.5036880267608,
-46.5633258142649));
#241595=CARTESIAN_POINT('Ctrl Pts',(-44.6034481677545,-55.4605330491705,
-46.5359405835467));
#241596=CARTESIAN_POINT('Ctrl Pts',(-44.8670057249247,-55.4904753426572,
-46.5226231268631));
#241597=CARTESIAN_POINT('Ctrl Pts',(-45.3677801070811,-55.6506619888066,
-46.4926528217206));
#241598=CARTESIAN_POINT('Ctrl Pts',(-45.6000180238917,-55.7794118764381,
-46.4771653870833));
#241599=CARTESIAN_POINT('Ctrl Pts',(-45.9941310039061,-56.1132670012756,
-46.4475180878708));
#241600=CARTESIAN_POINT('Ctrl Pts',(-46.1546038227961,-56.3123768136984,
-46.4340460804379));
#241601=CARTESIAN_POINT('Ctrl Pts',(-46.3981604390762,-56.7701693522984,
-46.4073415156862));
#241602=CARTESIAN_POINT('Ctrl Pts',(-46.4748923274485,-57.0266655892397,
-46.392379235198));
#241603=CARTESIAN_POINT('Ctrl Pts',(-46.5234131951804,-57.5493898930644,
-46.3618869841416));
#241604=CARTESIAN_POINT('Ctrl Pts',(-46.4967628570803,-57.8104132845754,
-46.3466606196368));
#241605=CARTESIAN_POINT('Ctrl Pts',(-46.346663598018,-58.3024334517028,
-46.3179594432211));
#241606=CARTESIAN_POINT('Ctrl Pts',(-46.2266684269433,-58.5293809990701,
-46.3056201001042));
#241607=CARTESIAN_POINT('Ctrl Pts',(-45.9000785678642,-58.9360461067693,
-46.2772603194458));
#241608=CARTESIAN_POINT('Ctrl Pts',(-45.6928021629035,-59.1086854318011,
-46.2617537855815));
#241609=CARTESIAN_POINT('Ctrl Pts',(-45.2317220985817,-59.3575112238338,
-46.2312034554625));
#241610=CARTESIAN_POINT('Ctrl Pts',(-44.9842283485895,-59.4348358761522,
-46.2164452270749));
#241611=CARTESIAN_POINT('Ctrl Pts',(-44.6553612302489,-59.471382934638,
-46.1987655132635));
#241612=CARTESIAN_POINT('Ctrl Pts',(-44.5816172779389,-59.475452478349,
-46.1949214103008));
#241613=CARTESIAN_POINT('Ctrl Pts',(-44.507952458321,-59.475452478349,-46.1912000000001));
#241614=CARTESIAN_POINT('Origin',(-44.5079524583206,-57.475452478349,235.35105));
#241615=CARTESIAN_POINT('',(-44.5079524583206,-59.475452478349,-45.4912000000001));
#241616=CARTESIAN_POINT('',(-44.5079524583206,-59.475452478349,-45.6499499999999));
#241617=CARTESIAN_POINT('',(-44.5079524583206,-59.475452478349,235.35105));
#241618=CARTESIAN_POINT('Ctrl Pts',(-44.5079524583206,-59.475452478349,
-45.6499499999999));
#241619=CARTESIAN_POINT('Ctrl Pts',(-44.6297441139361,-59.475452478349,
-45.6561026889509));
#241620=CARTESIAN_POINT('Ctrl Pts',(-44.7515417358596,-59.4643298262064,
-45.6625800899963));
#241621=CARTESIAN_POINT('Ctrl Pts',(-45.1337106204023,-59.3936149337826,
-45.6839490721741));
#241622=CARTESIAN_POINT('Ctrl Pts',(-45.3832534767605,-59.2933478816507,
-45.6994799709494));
#241623=CARTESIAN_POINT('Ctrl Pts',(-45.8199388022307,-59.0065682461395,
-45.7299049111287));
#241624=CARTESIAN_POINT('Ctrl Pts',(-46.005097617392,-58.8260886971062,
-45.7445227785059));
#241625=CARTESIAN_POINT('Ctrl Pts',(-46.3009460682604,-58.3996852797117,
-45.7719052608371));
#241626=CARTESIAN_POINT('Ctrl Pts',(-46.406731146095,-58.1564119291741,
-45.7852273653686));
#241627=CARTESIAN_POINT('Ctrl Pts',(-46.5182327027892,-57.6425839989162,
-45.8152006613004));
#241628=CARTESIAN_POINT('Ctrl Pts',(-46.5227680569918,-57.3770920683106,
-45.8306876905857));
#241629=CARTESIAN_POINT('Ctrl Pts',(-46.4305442437757,-56.8688927081907,
-45.8603326532594));
#241630=CARTESIAN_POINT('Ctrl Pts',(-46.3382757391706,-56.6303958485609,
-45.8737996082983));
#241631=CARTESIAN_POINT('Ctrl Pts',(-46.0634635452641,-56.1906583335379,
-45.9005082890561));
#241632=CARTESIAN_POINT('Ctrl Pts',(-45.8796383631409,-55.9960133343155,
-45.9154719427252));
#241633=CARTESIAN_POINT('Ctrl Pts',(-45.4511207021371,-55.6927639318498,
-45.9459646358205));
#241634=CARTESIAN_POINT('Ctrl Pts',(-45.2117179810681,-55.5854059851322,
-45.9611900914936));
#241635=CARTESIAN_POINT('Ctrl Pts',(-44.7105316985395,-55.4695306937223,
-45.9898887905671));
#241636=CARTESIAN_POINT('Ctrl Pts',(-44.4539800785212,-55.4600514463944,
-46.0022273879353));
#241637=CARTESIAN_POINT('Ctrl Pts',(-43.9385263862013,-55.5397101292635,
-46.0305905323871));
#241638=CARTESIAN_POINT('Ctrl Pts',(-43.6854136309263,-55.6329692967654,
-46.0460973792111));
#241639=CARTESIAN_POINT('Ctrl Pts',(-43.2394770383604,-55.9079850838125,
-46.0766465640289));
#241640=CARTESIAN_POINT('Ctrl Pts',(-43.0488205774223,-56.0837080598058,
-46.0914034289118));
#241641=CARTESIAN_POINT('Ctrl Pts',(-42.7422758405384,-56.5006333173148,
-46.1190498214788));
#241642=CARTESIAN_POINT('Ctrl Pts',(-42.6304392461764,-56.7386689927291,
-46.1319709633388));
#241643=CARTESIAN_POINT('Ctrl Pts',(-42.5035589820785,-57.2474506857119,
-46.1616498954294));
#241644=CARTESIAN_POINT('Ctrl Pts',(-42.4909937423021,-57.5134969494907,
-46.1771692608165));
#241645=CARTESIAN_POINT('Ctrl Pts',(-42.5683675957886,-58.025504112438,
-46.2070363453217));
#241646=CARTESIAN_POINT('Ctrl Pts',(-42.6538337684111,-58.2670866382577,
-46.2210393529167));
#241647=CARTESIAN_POINT('Ctrl Pts',(-42.9160906849344,-58.7149129781829,
-46.2473496883661));
#241648=CARTESIAN_POINT('Ctrl Pts',(-43.0941978562435,-58.9147341367152,
-46.2621754500287));
#241649=CARTESIAN_POINT('Ctrl Pts',(-43.5143261571294,-59.2306248434691,
-46.2926130328917));
#241650=CARTESIAN_POINT('Ctrl Pts',(-43.7512634012235,-59.3450399339582,
-46.3079197705927));
#241651=CARTESIAN_POINT('Ctrl Pts',(-44.1685463803989,-59.4538108059516,
-46.3321726178903));
#241652=CARTESIAN_POINT('Ctrl Pts',(-44.3380564620073,-59.475452478349,
-46.3413671688194));
#241653=CARTESIAN_POINT('Ctrl Pts',(-44.5079524583208,-59.475452478349,
-46.3499499999999));
#241654=CARTESIAN_POINT('Ctrl Pts',(-44.507952458321,-59.475452478349,-46.1912000000001));
#241655=CARTESIAN_POINT('Ctrl Pts',(-44.3220721510077,-59.475452478349,
-46.181809671022));
#241656=CARTESIAN_POINT('Ctrl Pts',(-44.1367724407075,-59.4495470295496,
-46.1716930971401));
#241657=CARTESIAN_POINT('Ctrl Pts',(-43.7037790848822,-59.3255571982284,
-46.1462027043874));
#241658=CARTESIAN_POINT('Ctrl Pts',(-43.4670490297897,-59.203484337701,
-46.130683081865));
#241659=CARTESIAN_POINT('Ctrl Pts',(-43.0622163648016,-58.8805848381541,
-46.1008137830855));
#241660=CARTESIAN_POINT('Ctrl Pts',(-42.8956711117532,-58.6858213338311,
-46.0868048499034));
#241661=CARTESIAN_POINT('Ctrl Pts',(-42.6388372387598,-58.2348563683312,
-46.0604985602492));
#241662=CARTESIAN_POINT('Ctrl Pts',(-42.5547671602554,-57.9807253290289,
-46.0456742496232));
#241663=CARTESIAN_POINT('Ctrl Pts',(-42.4911096915645,-57.4589499384175,
-46.0152373518375));
#241664=CARTESIAN_POINT('Ctrl Pts',(-42.5104177753976,-57.1965357354181,
-45.9999298566625));
#241665=CARTESIAN_POINT('Ctrl Pts',(-42.6468081439976,-56.7004985387426,
-45.9709943535231));
#241666=CARTESIAN_POINT('Ctrl Pts',(-42.7600313966352,-56.4708778366039,
-45.9585349754709));
#241667=CARTESIAN_POINT('Ctrl Pts',(-43.0748340898635,-56.0549111182015,
-45.9304993636291));
#241668=CARTESIAN_POINT('Ctrl Pts',(-43.2777582471938,-55.8759672341481,
-45.9150288142856));
#241669=CARTESIAN_POINT('Ctrl Pts',(-43.733047124395,-55.6137701281319,
-45.8843810475599));
#241670=CARTESIAN_POINT('Ctrl Pts',(-43.979014233557,-55.5295350993375,
-45.8694983895933));
#241671=CARTESIAN_POINT('Ctrl Pts',(-44.4904661217093,-55.4588679546952,
-45.8415996620773));
#241672=CARTESIAN_POINT('Ctrl Pts',(-44.7511223131829,-55.4735040185731,
-45.8289723392249));
#241673=CARTESIAN_POINT('Ctrl Pts',(-45.2581756857081,-55.6027132949404,
-45.7995883377328));
#241674=CARTESIAN_POINT('Ctrl Pts',(-45.4990296628474,-55.7182559587453,
-45.7840508463748));
#241675=CARTESIAN_POINT('Ctrl Pts',(-45.9138517687926,-56.0303682340407,
-45.7539915269071));
#241676=CARTESIAN_POINT('Ctrl Pts',(-46.0862455518917,-56.2209174650915,
-45.739724826257));
#241677=CARTESIAN_POINT('Ctrl Pts',(-46.3556550946895,-56.6653663866578,
-45.7131516614064));
#241678=CARTESIAN_POINT('Ctrl Pts',(-46.4466733942451,-56.9171528251501,
-45.6987674797699));
#241679=CARTESIAN_POINT('Ctrl Pts',(-46.5246017804916,-57.4378819276168,
-45.6683916154593));
#241680=CARTESIAN_POINT('Ctrl Pts',(-46.5122560120561,-57.7014197356871,
-45.6530185766552));
#241681=CARTESIAN_POINT('Ctrl Pts',(-46.3888011260386,-58.2011442186326,
-45.6238679818168));
#241682=CARTESIAN_POINT('Ctrl Pts',(-46.2818425465019,-58.4333200741879,
-45.6112091714481));
#241683=CARTESIAN_POINT('Ctrl Pts',(-45.9800340851223,-58.8550639774218,
-45.583661502917));
#241684=CARTESIAN_POINT('Ctrl Pts',(-45.7843219229271,-59.0378846869053,
-45.5684422161401));
#241685=CARTESIAN_POINT('Ctrl Pts',(-45.3388968597982,-59.3129136606705,
-45.5379184882298));
#241686=CARTESIAN_POINT('Ctrl Pts',(-45.0948460428784,-59.4047825186084,
-45.5229099844494));
#241687=CARTESIAN_POINT('Ctrl Pts',(-44.7300666440941,-59.4662076315768,
-45.5026904387972));
#241688=CARTESIAN_POINT('Ctrl Pts',(-44.6189869517897,-59.475452478349,
-45.4968092570358));
#241689=CARTESIAN_POINT('Ctrl Pts',(-44.5079524583207,-59.475452478349,
-45.4912000000001));
#241690=CARTESIAN_POINT('Origin',(-44.5079524583206,-57.475452478349,235.35105));
#241691=CARTESIAN_POINT('',(-44.5079524583206,-59.475452478349,-44.7912000000002));
#241692=CARTESIAN_POINT('',(-44.5079524583205,-59.475452478349,-44.9499499999999));
#241693=CARTESIAN_POINT('',(-44.5079524583206,-59.475452478349,235.35105));
#241694=CARTESIAN_POINT('Ctrl Pts',(-44.5079524583205,-59.475452478349,
-44.9499499999999));
#241695=CARTESIAN_POINT('Ctrl Pts',(-44.6703684237631,-59.475452478349,
-44.9581549538697));
#241696=CARTESIAN_POINT('Ctrl Pts',(-44.8325030142928,-59.4556741995973,
-44.9669225596634));
#241697=CARTESIAN_POINT('Ctrl Pts',(-45.247675743369,-59.3523848442981,
-44.9909089234627));
#241698=CARTESIAN_POINT('Ctrl Pts',(-45.4893066193448,-59.2381195950336,
-45.0064484043874));
#241699=CARTESIAN_POINT('Ctrl Pts',(-45.9060511378812,-58.9281085094198,
-45.0365435558811));
#241700=CARTESIAN_POINT('Ctrl Pts',(-46.0795556928749,-58.7383847653617,
-45.0508422939668));
#241701=CARTESIAN_POINT('Ctrl Pts',(-46.3513816465344,-58.2952247764233,
-45.0774999375521));
#241702=CARTESIAN_POINT('Ctrl Pts',(-46.4437230807142,-58.0439030757439,
-45.0917903818188));
#241703=CARTESIAN_POINT('Ctrl Pts',(-46.5243979108967,-57.5234451878826,
-45.1221504252774));
#241704=CARTESIAN_POINT('Ctrl Pts',(-46.513399658897,-57.2597115764675,
-45.1375348859433));
#241705=CARTESIAN_POINT('Ctrl Pts',(-46.3924429660938,-56.759286698404,
-45.1667263371637));
#241706=CARTESIAN_POINT('Ctrl Pts',(-46.2866811829253,-56.5266133472947,
-45.1794330593757));
#241707=CARTESIAN_POINT('Ctrl Pts',(-45.9870610340795,-56.1033784147385,
-45.2069136667644));
#241708=CARTESIAN_POINT('Ctrl Pts',(-45.7922898933191,-55.9195645725112,
-45.2221143812524));
#241709=CARTESIAN_POINT('Ctrl Pts',(-45.348174920298,-55.642197391229,-45.2526401235552));
#241710=CARTESIAN_POINT('Ctrl Pts',(-45.1044666494907,-55.5490583428045,
-45.2676683697628));
#241711=CARTESIAN_POINT('Ctrl Pts',(-44.5968355188062,-55.461004847915,
-45.2958811815676));
#241712=CARTESIAN_POINT('Ctrl Pts',(-44.3378617632765,-55.4662308166362,
-45.3082737018668));
#241713=CARTESIAN_POINT('Ctrl Pts',(-43.8273168932962,-55.5761779309857,
-45.3372722742871));
#241714=CARTESIAN_POINT('Ctrl Pts',(-43.5814664495911,-55.683215764723,
-45.3528141203417));
#241715=CARTESIAN_POINT('Ctrl Pts',(-43.154174566203,-55.9812782558104,
-45.383093604506));
#241716=CARTESIAN_POINT('Ctrl Pts',(-42.9745369553145,-56.1662734510742,
-45.3975642572139));
#241717=CARTESIAN_POINT('Ctrl Pts',(-42.6893359665779,-56.601978518829,
-45.4246801476068));
#241718=CARTESIAN_POINT('Ctrl Pts',(-42.5896481370744,-56.8505634377133,
-45.4384981392962));
#241719=CARTESIAN_POINT('Ctrl Pts',(-42.4936376452033,-57.3692352948812,
-45.468753997631));
#241720=CARTESIAN_POINT('Ctrl Pts',(-42.4970744065062,-57.6339388582957,
-45.4841950388301));
#241721=CARTESIAN_POINT('Ctrl Pts',(-42.6040345512156,-58.1382162765997,
-45.5136112215644));
#241722=CARTESIAN_POINT('Ctrl Pts',(-42.7031637847086,-58.3737025820734,
-45.5266410457028));
#241723=CARTESIAN_POINT('Ctrl Pts',(-42.9906155422345,-58.8051218901766,
-45.5537456394447));
#241724=CARTESIAN_POINT('Ctrl Pts',(-43.1800795861886,-58.994347381544,
-45.5688360889943));
#241725=CARTESIAN_POINT('Ctrl Pts',(-43.6167121529827,-59.2845558038791,
-45.5993583701853));
#241726=CARTESIAN_POINT('Ctrl Pts',(-43.8584044517106,-59.3847122446367,
-45.6144894471589));
#241727=CARTESIAN_POINT('Ctrl Pts',(-44.2429768168709,-59.4622861285099,
-45.6361799026449));
#241728=CARTESIAN_POINT('Ctrl Pts',(-44.3754414902991,-59.475452478349,
-45.6432557912323));
#241729=CARTESIAN_POINT('Ctrl Pts',(-44.5079524583206,-59.475452478349,
-45.6499499999999));
#241730=CARTESIAN_POINT('Ctrl Pts',(-44.5079524583207,-59.475452478349,
-45.4912000000001));
#241731=CARTESIAN_POINT('Ctrl Pts',(-44.3631837356181,-59.475452478349,
-45.4838865521606));
#241732=CARTESIAN_POINT('Ctrl Pts',(-44.2185386657933,-59.4597381216607,
-45.4761210156323));
#241733=CARTESIAN_POINT('Ctrl Pts',(-43.8173863312277,-59.3711192579799,
-45.4532708255445));
#241734=CARTESIAN_POINT('Ctrl Pts',(-43.5722271629013,-59.2628621673636,
-45.4377283397833));
#241735=CARTESIAN_POINT('Ctrl Pts',(-43.1466761350244,-58.9627769154267,
-45.4074778032249));
#241736=CARTESIAN_POINT('Ctrl Pts',(-42.9680554613902,-58.7769772398011,
-45.3930350602937));
#241737=CARTESIAN_POINT('Ctrl Pts',(-42.6848073184084,-58.3395805164596,
-45.3659684840981));
#241738=CARTESIAN_POINT('Ctrl Pts',(-42.5862468213381,-58.0900114512799,
-45.3520492734212));
#241739=CARTESIAN_POINT('Ctrl Pts',(-42.4930970950562,-57.5704717910895,
-45.3217427932434));
#241740=CARTESIAN_POINT('Ctrl Pts',(-42.497992524066,-57.3059384089094,
-45.3063116792829));
#241741=CARTESIAN_POINT('Ctrl Pts',(-42.6076504567339,-56.8023940160349,
-45.2769382563651));
#241742=CARTESIAN_POINT('Ctrl Pts',(-42.7080488419627,-56.5674533582485,
-45.2639778239381));
#241743=CARTESIAN_POINT('Ctrl Pts',(-42.9978337533079,-56.1375895827023,
-45.2368007332845));
#241744=CARTESIAN_POINT('Ctrl Pts',(-43.1883249155673,-55.949387068423,
-45.2216882324514));
#241745=CARTESIAN_POINT('Ctrl Pts',(-43.6264177179127,-55.6616194103928,
-45.1911633718228));
#241746=CARTESIAN_POINT('Ctrl Pts',(-43.8685110354901,-55.5628022955403,
-45.1760510997916));
#241747=CARTESIAN_POINT('Ctrl Pts',(-44.3736200988442,-55.4636554886945,
-45.1476421432267));
#241748=CARTESIAN_POINT('Ctrl Pts',(-44.6315898416643,-55.4629700035312,
-45.1353181404835));
#241749=CARTESIAN_POINT('Ctrl Pts',(-45.144185906275,-55.5607596082545,
-45.1065705395388));
#241750=CARTESIAN_POINT('Ctrl Pts',(-45.3930404753725,-55.66232340238,-45.0910365901201));
#241751=CARTESIAN_POINT('Ctrl Pts',(-45.8279620987918,-55.9512703836321,
-45.0606375346524));
#241752=CARTESIAN_POINT('Ctrl Pts',(-46.0120797555593,-56.132620985077,
-45.0460468589742));
#241753=CARTESIAN_POINT('Ctrl Pts',(-46.3059139123148,-56.5607942558644,
-45.0187145143283));
#241754=CARTESIAN_POINT('Ctrl Pts',(-46.4105515514957,-56.8050651998506,
-45.005305924579));
#241755=CARTESIAN_POINT('Ctrl Pts',(-46.5191363970842,-57.319823682072,
-44.9752783464494));
#241756=CARTESIAN_POINT('Ctrl Pts',(-46.5221615004682,-57.585184577012,
-44.9597989609113));
#241757=CARTESIAN_POINT('Ctrl Pts',(-46.4271463345645,-58.0926518279142,
-44.9301967046087));
#241758=CARTESIAN_POINT('Ctrl Pts',(-46.333587196176,-58.3305744990687,
-44.9168199612882));
#241759=CARTESIAN_POINT('Ctrl Pts',(-46.0563945341639,-58.768759149932,
-44.8900363155604));
#241760=CARTESIAN_POINT('Ctrl Pts',(-45.8714980102073,-58.96239935367,-44.8750478462204));
#241761=CARTESIAN_POINT('Ctrl Pts',(-45.4414261170752,-59.2632164444138,
-44.8445475786209));
#241762=CARTESIAN_POINT('Ctrl Pts',(-45.2015772341122,-59.3692252891307,
-44.8293389324833));
#241763=CARTESIAN_POINT('Ctrl Pts',(-44.8033600491983,-59.459077523037,
-44.8066010474234));
#241764=CARTESIAN_POINT('Ctrl Pts',(-44.6557335545469,-59.475452478349,
-44.7986656273728));
#241765=CARTESIAN_POINT('Ctrl Pts',(-44.5079524583206,-59.475452478349,
-44.7912000000001));
#241766=CARTESIAN_POINT('Origin',(-44.5079524583206,-57.475452478349,235.35105));
#241767=CARTESIAN_POINT('',(-44.5079524583204,-59.475452478349,-44.0912000000001));
#241768=CARTESIAN_POINT('',(-44.5079524583204,-59.475452478349,-44.2499499999999));
#241769=CARTESIAN_POINT('',(-44.5079524583206,-59.475452478349,235.35105));
#241770=CARTESIAN_POINT('Ctrl Pts',(-44.5079524583202,-59.475452478349,
-44.2499499999999));
#241771=CARTESIAN_POINT('Ctrl Pts',(-44.7020823833798,-59.475452478349,
-44.2597570843928));
#241772=CARTESIAN_POINT('Ctrl Pts',(-44.895461652298,-59.4471963517014,
-44.2703503840545));
#241773=CARTESIAN_POINT('Ctrl Pts',(-45.3326169478005,-59.3162010396124,
-44.2962553568166));
#241774=CARTESIAN_POINT('Ctrl Pts',(-45.5660396176025,-59.1926805068228,
-44.3116501201319));
#241775=CARTESIAN_POINT('Ctrl Pts',(-45.9766397528035,-58.8591026172973,
-44.3421222338695));
#241776=CARTESIAN_POINT('Ctrl Pts',(-46.148233658917,-58.6505822291728,
-44.3564007645353));
#241777=CARTESIAN_POINT('Ctrl Pts',(-46.3935029008547,-58.1894129661638,
-44.3833023048775));
#241778=CARTESIAN_POINT('Ctrl Pts',(-46.4690683573656,-57.9434484530477,
-44.3976502348093));
#241779=CARTESIAN_POINT('Ctrl Pts',(-46.5248279196195,-57.4266031567635,
-44.4277995437592));
#241780=CARTESIAN_POINT('Ctrl Pts',(-46.500636301891,-57.1601751210114,
-44.4433411791781));
#241781=CARTESIAN_POINT('Ctrl Pts',(-46.3518301060207,-56.6589853359418,
-44.4725772499739));
#241782=CARTESIAN_POINT('Ctrl Pts',(-46.2313372582583,-56.4283416300066,
-44.4850951904043));
#241783=CARTESIAN_POINT('Ctrl Pts',(-45.9093143253537,-56.0253732506028,
-44.5131164371659));
#241784=CARTESIAN_POINT('Ctrl Pts',(-45.710814646849,-55.8569226816391,
-44.5280574150073));
#241785=CARTESIAN_POINT('Ctrl Pts',(-45.2545105909144,-55.6011591450698,
-44.5585688209075));
#241786=CARTESIAN_POINT('Ctrl Pts',(-44.9996581311869,-55.5187751452991,
-44.5738463619873));
#241787=CARTESIAN_POINT('Ctrl Pts',(-44.4841973251914,-55.4595792055189,
-44.601613035802));
#241788=CARTESIAN_POINT('Ctrl Pts',(-44.2290775712395,-55.4788165537459,
-44.6141363618394));
#241789=CARTESIAN_POINT('Ctrl Pts',(-43.7324987118838,-55.6135337419647,
-44.6431518577482));
#241790=CARTESIAN_POINT('Ctrl Pts',(-43.4964918993264,-55.7304577057381,
-44.6584847672415));
#241791=CARTESIAN_POINT('Ctrl Pts',(-43.0793092444697,-56.0509185764088,
-44.6889068379682));
#241792=CARTESIAN_POINT('Ctrl Pts',(-42.9033161117682,-56.2526102145332,
-44.7036175346107));
#241793=CARTESIAN_POINT('Ctrl Pts',(-42.6455690443934,-56.703328973278,
-44.7299094622041));
#241794=CARTESIAN_POINT('Ctrl Pts',(-42.5626142744282,-56.9460582767092,
-44.7440686715709));
#241795=CARTESIAN_POINT('Ctrl Pts',(-42.4906627140526,-57.4592483089433,
-44.7740047567846));
#241796=CARTESIAN_POINT('Ctrl Pts',(-42.5061436817519,-57.7254368847256,
-44.7895324237052));
#241797=CARTESIAN_POINT('Ctrl Pts',(-42.6385579739842,-58.2323459492272,
-44.8191021191344));
#241798=CARTESIAN_POINT('Ctrl Pts',(-42.7525747976378,-58.4685069477834,
-44.8319023259275));
#241799=CARTESIAN_POINT('Ctrl Pts',(-43.0630004304665,-58.8819598003333,
-44.8596434956944));
#241800=CARTESIAN_POINT('Ctrl Pts',(-43.2556370349585,-59.0559024907331,
-44.8744484687671));
#241801=CARTESIAN_POINT('Ctrl Pts',(-43.7048794642206,-59.3265447748553,
-44.9050370978322));
#241802=CARTESIAN_POINT('Ctrl Pts',(-43.9592505100791,-59.4172112392399,
-44.920531890674));
#241803=CARTESIAN_POINT('Ctrl Pts',(-44.3182135068885,-59.468708630863,
-44.9401680439288));
#241804=CARTESIAN_POINT('Ctrl Pts',(-44.4131209121855,-59.475452478349,
-44.9451592858646));
#241805=CARTESIAN_POINT('Ctrl Pts',(-44.5079524583205,-59.475452478349,
-44.9499499999999));
#241806=CARTESIAN_POINT('Ctrl Pts',(-44.5079524583205,-59.475452478349,
-44.7912000000001));
#241807=CARTESIAN_POINT('Ctrl Pts',(-44.4022180531919,-59.475452478349,
-44.7858584936146));
#241808=CARTESIAN_POINT('Ctrl Pts',(-44.2964294722225,-59.467069050198,
-44.7802697337115));
#241809=CARTESIAN_POINT('Ctrl Pts',(-43.9279727565971,-59.4080384353609,
-44.7599342563497));
#241810=CARTESIAN_POINT('Ctrl Pts',(-43.6755120802264,-59.3134619513892,
-44.7444219296143));
#241811=CARTESIAN_POINT('Ctrl Pts',(-43.2312790046323,-59.0362283816049,
-44.7138941179901));
#241812=CARTESIAN_POINT('Ctrl Pts',(-43.0416396211848,-58.8596050514797,
-44.69916237365));
#241813=CARTESIAN_POINT('Ctrl Pts',(-42.7370820431139,-58.4409087264589,
-44.6715647125313));
#241814=CARTESIAN_POINT('Ctrl Pts',(-42.626364776298,-58.2019077703289,
-44.6585765586991));
#241815=CARTESIAN_POINT('Ctrl Pts',(-42.5023275829223,-57.6921756209946,
-44.6288421833212));
#241816=CARTESIAN_POINT('Ctrl Pts',(-42.4912550434187,-57.4262143382321,
-44.61332777516));
#241817=CARTESIAN_POINT('Ctrl Pts',(-42.5713911869543,-56.9149042401955,
-44.5835013527745));
#241818=CARTESIAN_POINT('Ctrl Pts',(-42.6581149484718,-56.6738996256653,
-44.569605074587));
#241819=CARTESIAN_POINT('Ctrl Pts',(-42.9226934049082,-56.2275563495412,
-44.5432207152669));
#241820=CARTESIAN_POINT('Ctrl Pts',(-43.1018661319024,-56.0286765671277,
-44.5283685805073));
#241821=CARTESIAN_POINT('Ctrl Pts',(-43.5235695202026,-55.7150992511455,
-44.4979189010419));
#241822=CARTESIAN_POINT('Ctrl Pts',(-43.7609767029779,-55.6019814627906,
-44.4826262608876));
#241823=CARTESIAN_POINT('Ctrl Pts',(-44.2594174029405,-55.4747781833009,
-44.4537358639097));
#241824=CARTESIAN_POINT('Ctrl Pts',(-44.5150870437871,-55.4594156358102,
-44.4413073151922));
#241825=CARTESIAN_POINT('Ctrl Pts',(-45.0323200202224,-55.5269341683579,
-44.4132083723189));
#241826=CARTESIAN_POINT('Ctrl Pts',(-45.2881313028365,-55.6145463245205,
-44.3977299053872));
#241827=CARTESIAN_POINT('Ctrl Pts',(-45.7411894271921,-55.8800221740483,
-44.3670992021461));
#241828=CARTESIAN_POINT('Ctrl Pts',(-45.9361224564827,-56.0518538285405,
-44.352239789825));
#241829=CARTESIAN_POINT('Ctrl Pts',(-46.2510704556164,-56.4612376024201,
-44.3243888399465));
#241830=CARTESIAN_POINT('Ctrl Pts',(-46.3676190157825,-56.6952318620315,
-44.3117128692851));
#241831=CARTESIAN_POINT('Ctrl Pts',(-46.5064512434471,-57.1999321684089,
-44.2822720180798));
#241832=CARTESIAN_POINT('Ctrl Pts',(-46.5253299068317,-57.46624717571,-44.2667369759872));
#241833=CARTESIAN_POINT('Ctrl Pts',(-46.4596829413825,-57.9809243189306,
-44.2367141426327));
#241834=CARTESIAN_POINT('Ctrl Pts',(-46.3795996217551,-58.2249436443509,
-44.2224796819832));
#241835=CARTESIAN_POINT('Ctrl Pts',(-46.1270968753499,-58.6790315645635,
-44.1959912199709));
#241836=CARTESIAN_POINT('Ctrl Pts',(-45.9534990634237,-58.8828352001413,
-44.1815110087529));
#241837=CARTESIAN_POINT('Ctrl Pts',(-45.5399107234176,-59.2084496299062,
-44.1511202040175));
#241838=CARTESIAN_POINT('Ctrl Pts',(-45.3050125501161,-59.328266809786,
-44.1357589154571));
#241839=CARTESIAN_POINT('Ctrl Pts',(-44.8758366402836,-59.4500035041743,
-44.110527089502));
#241840=CARTESIAN_POINT('Ctrl Pts',(-44.6921881144964,-59.475452478349,
-44.1005072442478));
#241841=CARTESIAN_POINT('Ctrl Pts',(-44.5079524583202,-59.475452478349,
-44.0912000000001));
#241842=CARTESIAN_POINT('Origin',(-44.5079524583206,-57.475452478349,235.35105));
#241843=CARTESIAN_POINT('',(-44.5079524583205,-59.475452478349,-43.3912000000001));
#241844=CARTESIAN_POINT('',(-44.5079524583206,-59.475452478349,-43.5499499999999));
#241845=CARTESIAN_POINT('',(-44.5079524583206,-59.475452478349,235.35105));
#241846=CARTESIAN_POINT('Ctrl Pts',(-44.5079524583206,-59.475452478349,
-43.5499499999999));
#241847=CARTESIAN_POINT('Ctrl Pts',(-44.7411427905853,-59.475452478349,
-43.5617303438466));
#241848=CARTESIAN_POINT('Ctrl Pts',(-44.9727332695675,-59.4346746567168,
-43.5746192191985));
#241849=CARTESIAN_POINT('Ctrl Pts',(-45.4394749499459,-59.2647243400995,
-43.6031550289789));
#241850=CARTESIAN_POINT('Ctrl Pts',(-45.6665336475973,-59.1267917585162,
-43.6186486476269));
#241851=CARTESIAN_POINT('Ctrl Pts',(-46.0536883181991,-58.7714288945144,
-43.6485717349899));
#241852=CARTESIAN_POINT('Ctrl Pts',(-46.2101594603455,-58.5577253477594,
-43.6618174159511));
#241853=CARTESIAN_POINT('Ctrl Pts',(-46.4291739303611,-58.087523674963,
-43.6892458468642));
#241854=CARTESIAN_POINT('Ctrl Pts',(-46.4917176646714,-57.8365081053396,
-43.7038884217589));
#241855=CARTESIAN_POINT('Ctrl Pts',(-46.5191896482408,-57.3145417089397,
-43.734336461549));
#241856=CARTESIAN_POINT('Ctrl Pts',(-46.4799004743569,-57.0483527973918,
-43.7498641480559));
#241857=CARTESIAN_POINT('Ctrl Pts',(-46.3030962153959,-56.5575077643044,
-43.7784967749861));
#241858=CARTESIAN_POINT('Ctrl Pts',(-46.171433025635,-56.3361553339704,
-43.7908102082948));
#241859=CARTESIAN_POINT('Ctrl Pts',(-45.8292354738008,-55.9518183888728,
-43.8193072226185));
#241860=CARTESIAN_POINT('Ctrl Pts',(-45.6207697531512,-55.7935289585522,
-43.8344552999138));
#241861=CARTESIAN_POINT('Ctrl Pts',(-45.1498597268732,-55.5628001339988,
-43.864974393293));
#241862=CARTESIAN_POINT('Ctrl Pts',(-44.8909167319963,-55.4946276437662,
-43.8800440782737));
#241863=CARTESIAN_POINT('Ctrl Pts',(-44.3734087572596,-55.4639808994358,
-43.9070814863956));
#241864=CARTESIAN_POINT('Ctrl Pts',(-44.1200539898213,-55.4971445208707,
-43.9201785970292));
#241865=CARTESIAN_POINT('Ctrl Pts',(-43.6305221796573,-55.6591557814902,
-43.9496341661717));
#241866=CARTESIAN_POINT('Ctrl Pts',(-43.400109458794,-55.7897775013242,
-43.9650839903949));
#241867=CARTESIAN_POINT('Ctrl Pts',(-43.0009549861012,-56.1341461785003,
-43.99529262176));
#241868=CARTESIAN_POINT('Ctrl Pts',(-42.8368259016293,-56.3452184044869,
-44.0090196790247));
#241869=CARTESIAN_POINT('Ctrl Pts',(-42.6043594635739,-56.810843263918,
-44.0361811291582));
#241870=CARTESIAN_POINT('Ctrl Pts',(-42.5350891087905,-57.0593505250132,
-44.0506773860554));
#241871=CARTESIAN_POINT('Ctrl Pts',(-42.4930428685444,-57.578876428523,
-44.0809830637601));
#241872=CARTESIAN_POINT('Ctrl Pts',(-42.5245722780062,-57.8452915051078,
-44.0965239432275));
#241873=CARTESIAN_POINT('Ctrl Pts',(-42.687043176314,-58.341520393353,-44.1254706283751));
#241874=CARTESIAN_POINT('Ctrl Pts',(-42.812967013659,-58.5676091816501,
-44.137843710689));
#241875=CARTESIAN_POINT('Ctrl Pts',(-43.1447772426943,-58.9616010236369,
-44.1660975778558));
#241876=CARTESIAN_POINT('Ctrl Pts',(-43.3481527596839,-59.1252173029631,
-44.1811438739157));
#241877=CARTESIAN_POINT('Ctrl Pts',(-43.8116818273377,-59.3689977237109,
-44.2116707664864));
#241878=CARTESIAN_POINT('Ctrl Pts',(-44.0686112146914,-59.4445451620155,
-44.2268538303952));
#241879=CARTESIAN_POINT('Ctrl Pts',(-44.3911492849965,-59.4728971911007,
-44.2439747907269));
#241880=CARTESIAN_POINT('Ctrl Pts',(-44.4495810412991,-59.475452478349,
-44.2470011840835));
#241881=CARTESIAN_POINT('Ctrl Pts',(-44.5079524583202,-59.475452478349,
-44.2499499999999));
#241882=CARTESIAN_POINT('Ctrl Pts',(-44.5079524583202,-59.475452478349,
-44.0912000000001));
#241883=CARTESIAN_POINT('Ctrl Pts',(-44.4396380533254,-59.475452478349,
-44.0877488827402));
#241884=CARTESIAN_POINT('Ctrl Pts',(-44.3712532747759,-59.4719525857611,
-44.0841921301382));
#241885=CARTESIAN_POINT('Ctrl Pts',(-44.0392127721053,-59.4377567333654,
-44.0664206796701));
#241886=CARTESIAN_POINT('Ctrl Pts',(-43.78342468228,-59.3583694715361,-44.0511832771466));
#241887=CARTESIAN_POINT('Ctrl Pts',(-43.3239077102798,-59.1078447978339,
-44.0206623608423));
#241888=CARTESIAN_POINT('Ctrl Pts',(-43.1232518957464,-58.941500918052,
-44.0056739041018));
#241889=CARTESIAN_POINT('Ctrl Pts',(-42.7969185541133,-58.5424711832971,
-43.9775497806073));
#241890=CARTESIAN_POINT('Ctrl Pts',(-42.6740307994288,-58.3138450434982,
-43.9651062329672));
#241891=CARTESIAN_POINT('Ctrl Pts',(-42.5191875880454,-57.8148255859975,
-43.935996764613));
#241892=CARTESIAN_POINT('Ctrl Pts',(-42.4917621021746,-57.5483791414746,
-43.9204540553491));
#241893=CARTESIAN_POINT('Ctrl Pts',(-42.5414862336479,-57.0303076934156,
-43.890233220879));
#241894=CARTESIAN_POINT('Ctrl Pts',(-42.6142852507321,-56.7832020438742,
-43.8758187246558));
#241895=CARTESIAN_POINT('Ctrl Pts',(-42.8539010143348,-56.3200531443656,
-43.8488017055177));
#241896=CARTESIAN_POINT('Ctrl Pts',(-43.0221771847699,-56.110399183978,
-43.8347778949015));
#241897=CARTESIAN_POINT('Ctrl Pts',(-43.4277210247951,-55.7720161446635,
-43.8044210656325));
#241898=CARTESIAN_POINT('Ctrl Pts',(-43.6598371235613,-55.6453432575024,
-43.7890003641977));
#241899=CARTESIAN_POINT('Ctrl Pts',(-44.1514596426019,-55.4912474024193,
-43.7596700423083));
#241900=CARTESIAN_POINT('Ctrl Pts',(-44.4052893349927,-55.4621018207231,
-43.746775745096));
#241901=CARTESIAN_POINT('Ctrl Pts',(-44.9222678148284,-55.5009444674812,
-43.7195260389219));
#241902=CARTESIAN_POINT('Ctrl Pts',(-45.1801192875519,-55.5732199621532,
-43.7043918246567));
#241903=CARTESIAN_POINT('Ctrl Pts',(-45.6469753039607,-55.8112258285714,
-43.6738652852958));
#241904=CARTESIAN_POINT('Ctrl Pts',(-45.8526306051278,-55.9724930517351,
-43.6587723328983));
#241905=CARTESIAN_POINT('Ctrl Pts',(-46.1890690927262,-56.3621980191077,
-43.6304096885208));
#241906=CARTESIAN_POINT('Ctrl Pts',(-46.3175540210956,-56.5861655594622,
-43.6180750702683));
#241907=CARTESIAN_POINT('Ctrl Pts',(-46.4864333897417,-57.0800086426784,
-43.5892675570807));
#241908=CARTESIAN_POINT('Ctrl Pts',(-46.5214251156315,-57.3463497448326,
-43.5737309927884));
#241909=CARTESIAN_POINT('Ctrl Pts',(-46.4858725815761,-57.8670145459856,
-43.5433588793878));
#241910=CARTESIAN_POINT('Ctrl Pts',(-46.4195947636065,-58.1166638901354,
-43.5287960009791));
#241911=CARTESIAN_POINT('Ctrl Pts',(-46.193140237254,-58.5843473292451,
-43.5015144670311));
#241912=CARTESIAN_POINT('Ctrl Pts',(-46.0324568770958,-58.7966008445079,
-43.4880149800194));
#241913=CARTESIAN_POINT('Ctrl Pts',(-45.6386695182338,-59.1459257410061,
-43.4579329289112));
#241914=CARTESIAN_POINT('Ctrl Pts',(-45.4097322015845,-59.2798344543604,
-43.442461768733));
#241915=CARTESIAN_POINT('Ctrl Pts',(-44.9510044081974,-59.4384338924148,
-43.4146618729776));
#241916=CARTESIAN_POINT('Ctrl Pts',(-44.7301421454,-59.475452478349,-43.4024246116192));
#241917=CARTESIAN_POINT('Ctrl Pts',(-44.5079524583205,-59.475452478349,
-43.3912000000001));
#241918=CARTESIAN_POINT('Origin',(-44.5079524583206,-57.475452478349,235.35105));
#241919=CARTESIAN_POINT('',(-44.5079524583206,-59.475452478349,-42.6912000000002));
#241920=CARTESIAN_POINT('',(-44.5079524583206,-59.475452478349,-42.8499499999999));
#241921=CARTESIAN_POINT('',(-44.5079524583206,-59.475452478349,235.35105));
#241922=CARTESIAN_POINT('Ctrl Pts',(-44.5079524583206,-59.475452478349,
-42.8499499999999));
#241923=CARTESIAN_POINT('Ctrl Pts',(-44.5276346988284,-59.475452478349,
-42.8509443103497));
#241924=CARTESIAN_POINT('Ctrl Pts',(-44.5473281463706,-59.4751619365887,
-42.8519476609929));
#241925=CARTESIAN_POINT('Ctrl Pts',(-44.8218121533896,-59.4670509640143,
-42.8660506548686));
#241926=CARTESIAN_POINT('Ctrl Pts',(-45.0727776159488,-59.410885272387,
-42.8803671313939));
#241927=CARTESIAN_POINT('Ctrl Pts',(-45.5491409754711,-59.2034632813881,
-42.9104819344268));
#241928=CARTESIAN_POINT('Ctrl Pts',(-45.7685085447205,-59.0506058229546,
-42.9260223204158));
#241929=CARTESIAN_POINT('Ctrl Pts',(-46.1304126464785,-58.6730704055913,
-42.9553164952639));
#241930=CARTESIAN_POINT('Ctrl Pts',(-46.2712780829291,-58.4538901331987,
-42.9678744701338));
#241931=CARTESIAN_POINT('Ctrl Pts',(-46.4618157928791,-57.9743456480368,
-42.9958478984349));
#241932=CARTESIAN_POINT('Ctrl Pts',(-46.5097830405982,-57.7186009486152,
-43.0107663392346));
#241933=CARTESIAN_POINT('Ctrl Pts',(-46.5059607988654,-57.1956479648935,
-43.0412719299517));
#241934=CARTESIAN_POINT('Ctrl Pts',(-46.4512970185361,-56.9334422805496,
-43.0565672615384));
#241935=CARTESIAN_POINT('Ctrl Pts',(-46.2473694361858,-56.4562447360175,
-43.0844037849695));
#241936=CARTESIAN_POINT('Ctrl Pts',(-46.1042283225714,-56.244081623675,
-43.0968907486846));
#241937=CARTESIAN_POINT('Ctrl Pts',(-45.7412219755972,-55.8795061147239,
-43.1258626095916));
#241938=CARTESIAN_POINT('Ctrl Pts',(-45.5228641533644,-55.7324834035986,
-43.1411818049009));
#241939=CARTESIAN_POINT('Ctrl Pts',(-45.038137520016,-55.5288830734955,
-43.1716076399338));
#241940=CARTESIAN_POINT('Ctrl Pts',(-44.7757837472277,-55.4758154631358,
-43.1864090721034));
#241941=CARTESIAN_POINT('Ctrl Pts',(-44.256718078785,-55.4751083907211,
-43.2126519315965));
#241942=CARTESIAN_POINT('Ctrl Pts',(-44.0048826118991,-55.5231388650409,
-43.2267550101799));
#241943=CARTESIAN_POINT('Ctrl Pts',(-43.5234974835783,-55.7146320702014,
-43.256658914088));
#241944=CARTESIAN_POINT('Ctrl Pts',(-43.2999967969317,-55.859750680214,
-43.2721823811033));
#241945=CARTESIAN_POINT('Ctrl Pts',(-42.9248666517407,-56.2258268948668,
-43.3018104844325));
#241946=CARTESIAN_POINT('Ctrl Pts',(-42.7759085245037,-56.4421417661968,
-43.3146735417911));
#241947=CARTESIAN_POINT('Ctrl Pts',(-42.5704203330931,-56.9168393697716,
-43.342364235333));
#241948=CARTESIAN_POINT('Ctrl Pts',(-42.514747104781,-57.1702018246777,
-43.3571437118691));
#241949=CARTESIAN_POINT('Ctrl Pts',(-42.5020797657798,-57.694224253965,
-43.3877116869108));
#241950=CARTESIAN_POINT('Ctrl Pts',(-42.5492113844385,-57.9599632971108,
-43.4032131310943));
#241951=CARTESIAN_POINT('Ctrl Pts',(-42.7404045078387,-58.4452239052171,
-43.4315199999005));
#241952=CARTESIAN_POINT('Ctrl Pts',(-42.8778864535938,-58.6618649124905,
-43.4438724460826));
#241953=CARTESIAN_POINT('Ctrl Pts',(-43.2306386228494,-59.0362522793755,
-43.4726124641059));
#241954=CARTESIAN_POINT('Ctrl Pts',(-43.4441758847969,-59.1889255509586,
-43.487852941648));
#241955=CARTESIAN_POINT('Ctrl Pts',(-43.9222617083629,-59.406054454791,
-43.5183378786663));
#241956=CARTESIAN_POINT('Ctrl Pts',(-44.1830410702355,-59.4666177912531,
-43.533278399856));
#241957=CARTESIAN_POINT('Ctrl Pts',(-44.4680414873419,-59.4751539757667,
-43.5479250653137));
#241958=CARTESIAN_POINT('Ctrl Pts',(-44.4880023952141,-59.475452478349,
-43.5489421597482));
#241959=CARTESIAN_POINT('Ctrl Pts',(-44.5079524583206,-59.475452478349,
-43.5499499999999));
#241960=CARTESIAN_POINT('Ctrl Pts',(-44.5079524583205,-59.475452478349,
-43.3912000000001));
#241961=CARTESIAN_POINT('Ctrl Pts',(-44.4773116517654,-59.475452478349,
-43.3896520831827));
#241962=CARTESIAN_POINT('Ctrl Pts',(-44.4466476465931,-59.4747483419293,
-43.388082457102));
#241963=CARTESIAN_POINT('Ctrl Pts',(-44.1510871580738,-59.4611428803614,
-43.3727544624739));
#241964=CARTESIAN_POINT('Ctrl Pts',(-43.8912890391863,-59.3963894216387,
-43.3577412999638));
#241965=CARTESIAN_POINT('Ctrl Pts',(-43.4171000214185,-59.171754753365,
-43.3272343042302));
#241966=CARTESIAN_POINT('Ctrl Pts',(-43.206333079655,-59.0159738242197,
-43.3120431381224));
#241967=CARTESIAN_POINT('Ctrl Pts',(-42.8593735673371,-58.636107456305,
-43.2834359502061));
#241968=CARTESIAN_POINT('Ctrl Pts',(-42.7250850178345,-58.4168938658302,
-43.2711174142699));
#241969=CARTESIAN_POINT('Ctrl Pts',(-42.541767545564,-57.9285541339348,
-43.2426309299094));
#241970=CARTESIAN_POINT('Ctrl Pts',(-42.4989342989933,-57.6625409902181,
-43.2271134965259));
#241971=CARTESIAN_POINT('Ctrl Pts',(-42.5197252561373,-57.1395943993428,
-43.1966082787248));
#241972=CARTESIAN_POINT('Ctrl Pts',(-42.5791731179057,-56.8874948444075,
-43.1819024713535));
#241973=CARTESIAN_POINT('Ctrl Pts',(-42.7920676850265,-56.4152459138284,
-43.1543546170697));
#241974=CARTESIAN_POINT('Ctrl Pts',(-42.9451166578166,-56.2003575940057,
-43.1412946370089));
#241975=CARTESIAN_POINT('Ctrl Pts',(-43.3268248912264,-55.8401059161665,
-43.1115041031655));
#241976=CARTESIAN_POINT('Ctrl Pts',(-43.5522960392943,-55.6989009570075,
-43.0959952402373));
#241977=CARTESIAN_POINT('Ctrl Pts',(-44.0359589670054,-55.5154402389995,
-43.0662105469964));
#241978=CARTESIAN_POINT('Ctrl Pts',(-44.2881710172024,-55.4714487340392,
-43.0524197273675));
#241979=CARTESIAN_POINT('Ctrl Pts',(-44.8068735603992,-55.4802226785142,
-43.025959928521));
#241980=CARTESIAN_POINT('Ctrl Pts',(-45.0683980446005,-55.5373746737467,
-43.0110812625833));
#241981=CARTESIAN_POINT('Ctrl Pts',(-45.5495583476536,-55.7483627495522,
-42.9806201160377));
#241982=CARTESIAN_POINT('Ctrl Pts',(-45.7653108529225,-55.8984789018917,
-42.965342311149));
#241983=CARTESIAN_POINT('Ctrl Pts',(-46.12274617044,-56.2684033051083,-42.9364958789197));
#241984=CARTESIAN_POINT('Ctrl Pts',(-46.2628111744314,-56.4829873890269,
-42.924093796877));
#241985=CARTESIAN_POINT('Ctrl Pts',(-46.4603340143122,-56.9657343748614,
-42.8959335560367));
#241986=CARTESIAN_POINT('Ctrl Pts',(-46.5109291662741,-57.2312039689145,
-42.880447829717));
#241987=CARTESIAN_POINT('Ctrl Pts',(-46.5048240924326,-57.7560032140316,
-42.8498345404185));
#241988=CARTESIAN_POINT('Ctrl Pts',(-46.4522081901623,-58.0103419850332,
-42.8349981121101));
#241989=CARTESIAN_POINT('Ctrl Pts',(-46.2526774483189,-58.4869863285353,
-42.8071938587392));
#241990=CARTESIAN_POINT('Ctrl Pts',(-46.1069702144933,-58.7044445518999,
-42.7944671477351));
#241991=CARTESIAN_POINT('Ctrl Pts',(-45.7371193706181,-59.0751341683654,
-42.7649711873811));
#241992=CARTESIAN_POINT('Ctrl Pts',(-45.5152413641435,-59.2233627999929,
-42.7494389862001));
#241993=CARTESIAN_POINT('Ctrl Pts',(-45.0358906779062,-59.4212091256449,
-42.7194525591918));
#241994=CARTESIAN_POINT('Ctrl Pts',(-44.7843816793554,-59.4725307487516,
-42.7052499095664));
#241995=CARTESIAN_POINT('Ctrl Pts',(-44.5226272522411,-59.4754121097202,
-42.6919425208378));
#241996=CARTESIAN_POINT('Ctrl Pts',(-44.5152890012201,-59.475452478349,
-42.6915706285642));
#241997=CARTESIAN_POINT('Ctrl Pts',(-44.5079524583206,-59.475452478349,
-42.6912000000002));
#241998=CARTESIAN_POINT('Origin',(-44.5079524583206,-57.475452478349,235.35105));
#241999=CARTESIAN_POINT('',(-44.5079524583208,-59.475452478349,-41.9912000000002));
#242000=CARTESIAN_POINT('',(-44.5079524583208,-59.475452478349,-42.1499499999999));
#242001=CARTESIAN_POINT('',(-44.5079524583206,-59.475452478349,235.35105));
#242002=CARTESIAN_POINT('Ctrl Pts',(-44.507952458321,-59.475452478349,-42.1499499999999));
#242003=CARTESIAN_POINT('Ctrl Pts',(-44.5650747796958,-59.475452478349,
-42.1528357139169));
#242004=CARTESIAN_POINT('Ctrl Pts',(-44.6222599632747,-59.4730053748643,
-42.1557959773676));
#242005=CARTESIAN_POINT('Ctrl Pts',(-44.9347278022592,-59.4461278479024,
-42.1723652019455));
#242006=CARTESIAN_POINT('Ctrl Pts',(-45.1834747757773,-59.3752762646862,
-42.1869979430166));
#242007=CARTESIAN_POINT('Ctrl Pts',(-45.649619547893,-59.1390434386582,
-42.2174368379546));
#242008=CARTESIAN_POINT('Ctrl Pts',(-45.8607911058115,-58.9723798878383,
-42.2329658543202));
#242009=CARTESIAN_POINT('Ctrl Pts',(-46.1982987190847,-58.5745118910737,
-42.2616205973047));
#242010=CARTESIAN_POINT('Ctrl Pts',(-46.3246473098617,-58.3499943901759,
-42.2739350551434));
#242011=CARTESIAN_POINT('Ctrl Pts',(-46.4873433377963,-57.8617628708698,
-42.302415227103));
#242012=CARTESIAN_POINT('Ctrl Pts',(-46.5206965595169,-57.6021973631596,
-42.3175565483861));
#242013=CARTESIAN_POINT('Ctrl Pts',(-46.4861088430538,-57.0789894607449,
-42.3480770093603));
#242014=CARTESIAN_POINT('Ctrl Pts',(-46.4161921970786,-56.820508868563,
-42.3631550439043));
#242015=CARTESIAN_POINT('Ctrl Pts',(-46.1849060981301,-56.3565494080106,
-42.3902193457699));
#242016=CARTESIAN_POINT('Ctrl Pts',(-46.0299185779906,-56.1534150975443,
-42.4032891797458));
#242017=CARTESIAN_POINT('Ctrl Pts',(-45.6455808442644,-55.8097419487664,
-42.4327290106458));
#242018=CARTESIAN_POINT('Ctrl Pts',(-45.4175748781868,-55.675070498779,
-42.4481753672027));
#242019=CARTESIAN_POINT('Ctrl Pts',(-44.9200132742906,-55.500498582363,
-42.4784029391186));
#242020=CARTESIAN_POINT('Ctrl Pts',(-44.6550483564574,-55.4633522733737,
-42.4921660649213));
#242021=CARTESIAN_POINT('Ctrl Pts',(-44.1353892897578,-55.4939013682113,
-42.5193092941163));
#242022=CARTESIAN_POINT('Ctrl Pts',(-43.8854675233247,-55.5576883309377,
-42.5337953321194));
#242023=CARTESIAN_POINT('Ctrl Pts',(-43.4141880609877,-55.7801031930307,
-42.5640905981526));
#242024=CARTESIAN_POINT('Ctrl Pts',(-43.1989634690461,-55.9401681677463,
-42.5796319078233));
#242025=CARTESIAN_POINT('Ctrl Pts',(-42.8496595906262,-56.328327415621,
-42.6085994044402));
#242026=CARTESIAN_POINT('Ctrl Pts',(-42.7163521133916,-56.5502515671372,
-42.620979946846));
#242027=CARTESIAN_POINT('Ctrl Pts',(-42.5401456495728,-57.0343218554623,
-42.6492173803316));
#242028=CARTESIAN_POINT('Ctrl Pts',(-42.4996622819459,-57.2921349904168,
-42.6642564798706));
#242029=CARTESIAN_POINT('Ctrl Pts',(-42.5193067596286,-57.8154466839436,
-42.6947829953263));
#242030=CARTESIAN_POINT('Ctrl Pts',(-42.5818499425991,-58.0758497743081,
-42.7099731755975));
#242031=CARTESIAN_POINT('Ctrl Pts',(-42.7999012454534,-58.5463029491167,
-42.7374162774613));
#242032=CARTESIAN_POINT('Ctrl Pts',(-42.9490964919264,-58.7537934143169,
-42.7501510933475));
#242033=CARTESIAN_POINT('Ctrl Pts',(-43.3230349053399,-59.107742718469,
-42.7793652910375));
#242034=CARTESIAN_POINT('Ctrl Pts',(-43.5464048897313,-59.2485347493895,
-42.7947559633267));
#242035=CARTESIAN_POINT('Ctrl Pts',(-44.019696696047,-59.4304161605894,
-42.8239706636009));
#242036=CARTESIAN_POINT('Ctrl Pts',(-44.2628906747684,-59.475452478349,
-42.8375699324134));
#242037=CARTESIAN_POINT('Ctrl Pts',(-44.5079524583206,-59.475452478349,
-42.8499499999999));
#242038=CARTESIAN_POINT('Ctrl Pts',(-44.5079524583206,-59.475452478349,
-42.6912000000002));
#242039=CARTESIAN_POINT('Ctrl Pts',(-44.2504290540854,-59.475452478349,
-42.6781903944089));
#242040=CARTESIAN_POINT('Ctrl Pts',(-43.9951550570802,-59.4257145549608,
-42.663843735274));
#242041=CARTESIAN_POINT('Ctrl Pts',(-43.514305376544,-59.2306775940827,
-42.6338635216549));
#242042=CARTESIAN_POINT('Ctrl Pts',(-43.2939194442701,-59.0861303300434,
-42.6185140705213));
#242043=CARTESIAN_POINT('Ctrl Pts',(-42.9265253044388,-58.7257988038404,
-42.5894443292731));
#242044=CARTESIAN_POINT('Ctrl Pts',(-42.7809576370071,-58.5155232546435,
-42.576870795284));
#242045=CARTESIAN_POINT('Ctrl Pts',(-42.5713346547531,-58.0410220017098,
-42.5491915555295));
#242046=CARTESIAN_POINT('Ctrl Pts',(-42.5134931808606,-57.7795123493802,
-42.5339368258103));
#242047=CARTESIAN_POINT('Ctrl Pts',(-42.5033078965441,-57.2563570745263,
-42.5034194347771));
#242048=CARTESIAN_POINT('Ctrl Pts',(-42.5482735346596,-56.9997541785442,
-42.4884509325115));
#242049=CARTESIAN_POINT('Ctrl Pts',(-42.7330429464916,-56.5183738869157,
-42.4603704154998));
#242050=CARTESIAN_POINT('Ctrl Pts',(-42.8708433909339,-56.298089817614,
-42.4478973081275));
#242051=CARTESIAN_POINT('Ctrl Pts',(-43.2276659902567,-55.9162367588301,
-42.4187339101662));
#242052=CARTESIAN_POINT('Ctrl Pts',(-43.4453863688403,-55.7604529601252,
-42.4031913856087));
#242053=CARTESIAN_POINT('Ctrl Pts',(-43.9197500928027,-55.5469560070576,
-42.3730004140684));
#242054=CARTESIAN_POINT('Ctrl Pts',(-44.1703212412459,-55.4877077061276,
-42.3586139481242));
#242055=CARTESIAN_POINT('Ctrl Pts',(-44.6917016753155,-55.4661419405827,
-42.3316457724076));
#242056=CARTESIAN_POINT('Ctrl Pts',(-44.9576917709601,-55.5085012155312,
-42.3175160810923));
#242057=CARTESIAN_POINT('Ctrl Pts',(-45.4528258682846,-55.6933931606017,
-42.2871101414782));
#242058=CARTESIAN_POINT('Ctrl Pts',(-45.677709936842,-55.8322258902904,
-42.2717001267461));
#242059=CARTESIAN_POINT('Ctrl Pts',(-46.0550120706384,-56.1828697013188,
-42.2424124103462));
#242060=CARTESIAN_POINT('Ctrl Pts',(-46.2060766973967,-56.3889421190976,
-42.2295797709562));
#242061=CARTESIAN_POINT('Ctrl Pts',(-46.4284298403303,-56.8573027972508,
-42.2022587313973));
#242062=CARTESIAN_POINT('Ctrl Pts',(-46.4933714527608,-57.1171058003779,
-42.1871035562149));
#242063=CARTESIAN_POINT('Ctrl Pts',(-46.5178619269603,-57.6404308900813,
-42.1565762593156));
#242064=CARTESIAN_POINT('Ctrl Pts',(-46.4796841978071,-57.8988337075529,
-42.1415027616298));
#242065=CARTESIAN_POINT('Ctrl Pts',(-46.3078606964485,-58.3842645324407,
-42.1131859635114));
#242066=CARTESIAN_POINT('Ctrl Pts',(-46.1768272466949,-58.6070297692475,
-42.1008374601594));
#242067=CARTESIAN_POINT('Ctrl Pts',(-45.8313597047937,-58.9983700010671,
-42.0719709894624));
#242068=CARTESIAN_POINT('Ctrl Pts',(-45.617434952966,-59.1605967201461,
-42.0564322944304));
#242069=CARTESIAN_POINT('Ctrl Pts',(-45.1477860234778,-59.3875285888647,
-42.0260876538713));
#242070=CARTESIAN_POINT('Ctrl Pts',(-44.8982255564231,-59.4536206016677,
-42.0115526374167));
#242071=CARTESIAN_POINT('Ctrl Pts',(-44.5979575875366,-59.4739351411411,
-41.9957911481571));
#242072=CARTESIAN_POINT('Ctrl Pts',(-44.5529321463451,-59.475452478349,
-41.9934722905617));
#242073=CARTESIAN_POINT('Ctrl Pts',(-44.5079524583209,-59.475452478349,
-41.9912000000002));
#242074=CARTESIAN_POINT('Origin',(-44.5079524583206,-57.475452478349,235.35105));
#242075=CARTESIAN_POINT('',(-44.5079524583208,-59.475452478349,-41.2912000000002));
#242076=CARTESIAN_POINT('',(-44.5079524583207,-59.475452478349,-41.4499499999999));
#242077=CARTESIAN_POINT('',(-44.5079524583206,-59.475452478349,235.35105));
#242078=CARTESIAN_POINT('Ctrl Pts',(-44.5079524583208,-59.475452478349,
-41.4499499999999));
#242079=CARTESIAN_POINT('Ctrl Pts',(-44.6009259794205,-59.475452478349,
-41.4546468501504));
#242080=CARTESIAN_POINT('Ctrl Pts',(-44.6939771241189,-59.4689702732022,
-41.4595366860181));
#242081=CARTESIAN_POINT('Ctrl Pts',(-45.0416143584034,-59.4200877927684,
-41.4785244144753));
#242082=CARTESIAN_POINT('Ctrl Pts',(-45.2874346307486,-59.3352317064797,
-41.4934177686947));
#242083=CARTESIAN_POINT('Ctrl Pts',(-45.7421834212317,-59.0718365676755,
-41.5240731938623));
#242084=CARTESIAN_POINT('Ctrl Pts',(-45.9447065234524,-58.8923298930035,
-41.5395398973705));
#242085=CARTESIAN_POINT('Ctrl Pts',(-46.2584426863796,-58.4755311426912,
-41.5675458976735));
#242086=CARTESIAN_POINT('Ctrl Pts',(-46.3710572059469,-58.2456657066199,
-41.5800208950175));
#242087=CARTESIAN_POINT('Ctrl Pts',(-46.5062012038549,-57.749268837484,
-41.6089773790505));
#242088=CARTESIAN_POINT('Ctrl Pts',(-46.5248397171714,-57.4867383743764,
-41.6242916560651));
#242089=CARTESIAN_POINT('Ctrl Pts',(-46.4598083536196,-56.9650709933012,
-41.6547222532945));
#242090=CARTESIAN_POINT('Ctrl Pts',(-46.37507561606,-56.7111654338419,-41.6695334109297));
#242091=CARTESIAN_POINT('Ctrl Pts',(-46.1170385297601,-56.2608270119092,
-41.6958031522091));
#242092=CARTESIAN_POINT('Ctrl Pts',(-45.9499355131943,-56.0664572462705,
-41.7098660467572));
#242093=CARTESIAN_POINT('Ctrl Pts',(-45.5441242268398,-55.7445682618479,
-41.7397553103185));
#242094=CARTESIAN_POINT('Ctrl Pts',(-45.3069921100196,-55.6231143727148,
-41.7552771909227));
#242095=CARTESIAN_POINT('Ctrl Pts',(-44.8026094104671,-55.4802147431357,
-41.7849255769294));
#242096=CARTESIAN_POINT('Ctrl Pts',(-44.5406967898439,-55.4588449667596,
-41.7978114312412));
#242097=CARTESIAN_POINT('Ctrl Pts',(-44.0266545219183,-55.5172882033606,
-41.8254844892962));
#242098=CARTESIAN_POINT('Ctrl Pts',(-43.779297689101,-55.5952707848365,
-41.8402549904821));
#242099=CARTESIAN_POINT('Ctrl Pts',(-43.3187518271973,-55.8453728770303,
-41.8708155591053));
#242100=CARTESIAN_POINT('Ctrl Pts',(-43.1118811272099,-56.0186157977966,
-41.8863192023811));
#242101=CARTESIAN_POINT('Ctrl Pts',(-42.7864074243799,-56.4261702229759,
-41.9146485353188));
#242102=CARTESIAN_POINT('Ctrl Pts',(-42.6670571871209,-56.6533685443121,
-41.9269951038478));
#242103=CARTESIAN_POINT('Ctrl Pts',(-42.5182510384644,-57.1457723700787,
-41.9557186603508));
#242104=CARTESIAN_POINT('Ctrl Pts',(-42.4922913340079,-57.406935701447,
-41.970953188014));
#242105=CARTESIAN_POINT('Ctrl Pts',(-42.5422415623305,-57.9295892736244,
-42.0014413130576));
#242106=CARTESIAN_POINT('Ctrl Pts',(-42.6196693330092,-58.1858714881189,
-42.0163911089031));
#242107=CARTESIAN_POINT('Ctrl Pts',(-42.864481736838,-58.6430250877798,
-42.0430584022166));
#242108=CARTESIAN_POINT('Ctrl Pts',(-43.0255226079038,-58.8417235688324,
-42.0565766287346));
#242109=CARTESIAN_POINT('Ctrl Pts',(-43.4206431894206,-59.1745575448617,
-42.0862450466026));
#242110=CARTESIAN_POINT('Ctrl Pts',(-43.6533100929671,-59.3026879263632,
-42.1017360839267));
#242111=CARTESIAN_POINT('Ctrl Pts',(-44.0997626031168,-59.4440829473174,
-42.1284140596013));
#242112=CARTESIAN_POINT('Ctrl Pts',(-44.3034083695787,-59.4754524783491,
-42.1396168113389));
#242113=CARTESIAN_POINT('Ctrl Pts',(-44.507952458321,-59.475452478349,-42.1499499999999));
#242114=CARTESIAN_POINT('Ctrl Pts',(-44.5079524583209,-59.475452478349,
-41.9912000000002));
#242115=CARTESIAN_POINT('Ctrl Pts',(-44.2895268033131,-59.4754524783491,
-41.9801655403125));
#242116=CARTESIAN_POINT('Ctrl Pts',(-44.072284646167,-59.4396792295317,
-41.9681474823218));
#242117=CARTESIAN_POINT('Ctrl Pts',(-43.6162554978214,-59.2848170542454,
-41.9405929206148));
#242118=CARTESIAN_POINT('Ctrl Pts',(-43.3867023861031,-59.1522714670058,
-41.9251304094548));
#242119=CARTESIAN_POINT('Ctrl Pts',(-42.9988245054448,-58.8121357155321,
-41.8956149109742));
#242120=CARTESIAN_POINT('Ctrl Pts',(-42.8418555471031,-58.6104662814462,
-41.8824091385142));
#242121=CARTESIAN_POINT('Ctrl Pts',(-42.6061070337851,-58.1487334399722,
-41.8554747227616));
#242122=CARTESIAN_POINT('Ctrl Pts',(-42.5337089287158,-57.8909520345353,
-41.8404374741111));
#242123=CARTESIAN_POINT('Ctrl Pts',(-42.494061758467,-57.3678765695541,
-41.8099247386538));
#242124=CARTESIAN_POINT('Ctrl Pts',(-42.5249871347537,-57.1077620134154,
-41.7947513895457));
#242125=CARTESIAN_POINT('Ctrl Pts',(-42.6831101613391,-56.6181443811625,
-41.7661903609976));
#242126=CARTESIAN_POINT('Ctrl Pts',(-42.8071371501217,-56.3927472221573,
-41.7538764704305));
#242127=CARTESIAN_POINT('Ctrl Pts',(-43.1406720840627,-55.991657246832,
-41.725328445476));
#242128=CARTESIAN_POINT('Ctrl Pts',(-43.3504418669979,-55.8228043071185,
-41.7098063870112));
#242129=CARTESIAN_POINT('Ctrl Pts',(-43.8147777661047,-55.5819666242096,
-41.6793245646629));
#242130=CARTESIAN_POINT('Ctrl Pts',(-44.0630869185102,-55.5087519276968,
-41.664645017366));
#242131=CARTESIAN_POINT('Ctrl Pts',(-44.5790557803663,-55.4596501846947,
-41.6371470915826));
#242132=CARTESIAN_POINT('Ctrl Pts',(-44.8419646313228,-55.4862372264034,
-41.6240117682738));
#242133=CARTESIAN_POINT('Ctrl Pts',(-45.3441791046204,-55.6396783934614,
-41.5941654555332));
#242134=CARTESIAN_POINT('Ctrl Pts',(-45.5783520708578,-55.7656042547414,
-41.5786626332168));
#242135=CARTESIAN_POINT('Ctrl Pts',(-45.9770361819292,-56.0948126302783,
-41.5489199391143));
#242136=CARTESIAN_POINT('Ctrl Pts',(-46.1400904248351,-56.2920612198681,
-41.5352311567446));
#242137=CARTESIAN_POINT('Ctrl Pts',(-46.3893309714318,-56.7469503676705,
-41.5086959564562));
#242138=CARTESIAN_POINT('Ctrl Pts',(-46.4692097135499,-57.0024617306042,
-41.4937911269517));
#242139=CARTESIAN_POINT('Ctrl Pts',(-46.5242043250541,-57.5248342425204,
-41.46331939709));
#242140=CARTESIAN_POINT('Ctrl Pts',(-46.5006864397953,-57.7864771094481,
-41.4480568965192));
#242141=CARTESIAN_POINT('Ctrl Pts',(-46.3564458786342,-58.2802276366138,
-41.4192547824346));
#242142=CARTESIAN_POINT('Ctrl Pts',(-46.2393622733395,-58.5083135685649,
-41.4068758364452));
#242143=CARTESIAN_POINT('Ctrl Pts',(-45.9178222925651,-58.9189878596702,
-41.3786542317732));
#242144=CARTESIAN_POINT('Ctrl Pts',(-45.7123922578584,-59.0943471035571,
-41.3631616421491));
#242145=CARTESIAN_POINT('Ctrl Pts',(-45.2537529527428,-59.3489305525486,
-41.332566683005));
#242146=CARTESIAN_POINT('Ctrl Pts',(-45.0068914917131,-59.4292260382104,
-41.3177537473793));
#242147=CARTESIAN_POINT('Ctrl Pts',(-44.6705784160196,-59.4704991177613,
-41.2995600353072));
#242148=CARTESIAN_POINT('Ctrl Pts',(-44.5892245188092,-59.475452478349,
-41.2953057140252));
#242149=CARTESIAN_POINT('Ctrl Pts',(-44.5079524583209,-59.475452478349,
-41.2912000000002));
#242150=CARTESIAN_POINT('Origin',(-44.5079524583206,-57.475452478349,235.35105));
#242151=CARTESIAN_POINT('',(-44.5079524583206,-59.475452478349,-40.5912000000001));
#242152=CARTESIAN_POINT('',(-44.5079524583206,-59.475452478349,-40.7499499999999));
#242153=CARTESIAN_POINT('',(-44.5079524583206,-59.475452478349,235.35105));
#242154=CARTESIAN_POINT('Ctrl Pts',(-44.5079524583206,-59.475452478349,
-40.7499499999999));
#242155=CARTESIAN_POINT('Ctrl Pts',(-44.6385960929674,-59.475452478349,
-40.7565498745426));
#242156=CARTESIAN_POINT('Ctrl Pts',(-44.769204040552,-59.4626545153701,
-40.7635212201612));
#242157=CARTESIAN_POINT('Ctrl Pts',(-45.1520824190208,-59.3865372026326,
-40.785083615251));
#242158=CARTESIAN_POINT('Ctrl Pts',(-45.3939906952831,-59.2870988818203,
-40.8002046578447));
#242159=CARTESIAN_POINT('Ctrl Pts',(-45.8314081075506,-58.9981985528729,
-40.8307284352522));
#242160=CARTESIAN_POINT('Ctrl Pts',(-46.0214237092286,-58.8095209785697,
-40.8458307675625));
#242161=CARTESIAN_POINT('Ctrl Pts',(-46.3101271098484,-58.37893535582,-40.8729742761734));
#242162=CARTESIAN_POINT('Ctrl Pts',(-46.4099370609394,-58.1437421486912,
-40.8859664358967));
#242163=CARTESIAN_POINT('Ctrl Pts',(-46.5183453086989,-57.6398576279405,
-40.9153596996072));
#242164=CARTESIAN_POINT('Ctrl Pts',(-46.5225650990151,-57.3752444181325,
-40.9307954701794));
#242165=CARTESIAN_POINT('Ctrl Pts',(-46.4280892393463,-56.8561059894309,
-40.961078545187));
#242166=CARTESIAN_POINT('Ctrl Pts',(-46.3290060834648,-56.6069932463964,
-40.9749504700387));
#242167=CARTESIAN_POINT('Ctrl Pts',(-46.044853192413,-56.1703797098378,
-41.0020399094839));
#242168=CARTESIAN_POINT('Ctrl Pts',(-45.8657612276326,-55.9849518339394,
-41.0164956170126));
#242169=CARTESIAN_POINT('Ctrl Pts',(-45.4394030099877,-55.6858019193976,
-41.0467596506296));
#242170=CARTESIAN_POINT('Ctrl Pts',(-45.1939230531916,-55.5781088311712,
-41.0623018919607));
#242171=CARTESIAN_POINT('Ctrl Pts',(-44.6836335356126,-55.4666944261493,
-41.0913303604284));
#242172=CARTESIAN_POINT('Ctrl Pts',(-44.4245355192991,-55.4607537804227,
-41.1037353572947));
#242173=CARTESIAN_POINT('Ctrl Pts',(-43.9166058575354,-55.547474839854,
-41.1319243876361));
#242174=CARTESIAN_POINT('Ctrl Pts',(-43.6727127176413,-55.6399315150409,
-41.1469420705348));
#242175=CARTESIAN_POINT('Ctrl Pts',(-43.2278922594853,-55.9160430858539,
-41.1774668306685));
#242176=CARTESIAN_POINT('Ctrl Pts',(-43.0326148387811,-56.099323910573,
-41.1926775751379));
#242177=CARTESIAN_POINT('Ctrl Pts',(-42.7318185640421,-56.5217582212481,
-41.2201942467576));
#242178=CARTESIAN_POINT('Ctrl Pts',(-42.6254137272816,-56.7541638828771,
-41.2328748319307));
#242179=CARTESIAN_POINT('Ctrl Pts',(-42.5031136631561,-57.2542126081442,
-41.2620443409046));
#242180=CARTESIAN_POINT('Ctrl Pts',(-42.4913907026965,-57.5178417825212,
-41.2774227094099));
#242181=CARTESIAN_POINT('Ctrl Pts',(-42.5705889589166,-58.0384472049299,
-41.3077913590504));
#242182=CARTESIAN_POINT('Ctrl Pts',(-42.6622192643798,-58.2900196235696,
-41.322131851386));
#242183=CARTESIAN_POINT('Ctrl Pts',(-42.9327467595647,-58.7338742660884,
-41.3487441599825));
#242184=CARTESIAN_POINT('Ctrl Pts',(-43.105654569544,-58.9240426415747,
-41.3630257200316));
#242185=CARTESIAN_POINT('Ctrl Pts',(-43.5213667545882,-59.2351848995639,
-41.3931017124761));
#242186=CARTESIAN_POINT('Ctrl Pts',(-43.7625807260854,-59.350137595176,
-41.4086401826768));
#242187=CARTESIAN_POINT('Ctrl Pts',(-44.1793416823659,-59.4551740438799,
-41.432757737665));
#242188=CARTESIAN_POINT('Ctrl Pts',(-44.3434954665592,-59.475452478349,
-41.4416419372593));
#242189=CARTESIAN_POINT('Ctrl Pts',(-44.5079524583208,-59.475452478349,
-41.4499499999999));
#242190=CARTESIAN_POINT('Ctrl Pts',(-44.5079524583209,-59.475452478349,
-41.2912000000002));
#242191=CARTESIAN_POINT('Ctrl Pts',(-44.3305589288781,-59.475452478349,
-41.2822384073272));
#242192=CARTESIAN_POINT('Ctrl Pts',(-44.1536253369592,-59.4518585597956,
-41.2726118938888));
#242193=CARTESIAN_POINT('Ctrl Pts',(-43.7269650664756,-59.3355102624255,
-41.2476643149557));
#242194=CARTESIAN_POINT('Ctrl Pts',(-43.4884353487384,-59.2162369893224,
-41.2321354314417));
#242195=CARTESIAN_POINT('Ctrl Pts',(-43.0793311543506,-58.8980073529936,
-41.2021865472492));
#242196=CARTESIAN_POINT('Ctrl Pts',(-42.9102289746349,-58.7050656262889,
-41.1880163511847));
#242197=CARTESIAN_POINT('Ctrl Pts',(-42.6479668302325,-58.2568990964046,
-41.1616958294253));
#242198=CARTESIAN_POINT('Ctrl Pts',(-42.560855617791,-58.003783693849,-41.1470193209044));
#242199=CARTESIAN_POINT('Ctrl Pts',(-42.4910155252582,-57.4823355542716,
-41.1166015127624));
#242200=CARTESIAN_POINT('Ctrl Pts',(-42.5073184864561,-57.2194132681746,
-41.1012643794067));
#242201=CARTESIAN_POINT('Ctrl Pts',(-42.6381191854166,-56.7217703164105,
-41.0722352072204));
#242202=CARTESIAN_POINT('Ctrl Pts',(-42.7486210868745,-56.4910496596015,
-41.059699748032));
#242203=CARTESIAN_POINT('Ctrl Pts',(-43.0568924459804,-56.0737447010577,
-41.0319550550934));
#242204=CARTESIAN_POINT('Ctrl Pts',(-43.255359002887,-55.8938921394422,
-41.0166831923748));
#242205=CARTESIAN_POINT('Ctrl Pts',(-43.7045885134784,-55.6258189241425,
-40.9861701471109));
#242206=CARTESIAN_POINT('Ctrl Pts',(-43.9496148865039,-55.5377152595265,
-40.9712221781807));
#242207=CARTESIAN_POINT('Ctrl Pts',(-44.4594263172017,-55.4594931372893,
-40.9431859700249));
#242208=CARTESIAN_POINT('Ctrl Pts',(-44.7193355129139,-55.4700171688899,
-40.9306798493055));
#242209=CARTESIAN_POINT('Ctrl Pts',(-45.2279490595016,-55.5908256202746,
-40.9014620547703));
#242210=CARTESIAN_POINT('Ctrl Pts',(-45.4710172622289,-55.7026852787828,
-40.8859201258229));
#242211=CARTESIAN_POINT('Ctrl Pts',(-45.891333908348,-56.0087306376859,
-40.8557601840865));
#242212=CARTESIAN_POINT('Ctrl Pts',(-46.0669081081037,-56.1968913632185,
-40.8414024794196));
#242213=CARTESIAN_POINT('Ctrl Pts',(-46.344318594368,-56.6393184641795,
-40.8144840914861));
#242214=CARTESIAN_POINT('Ctrl Pts',(-46.4394909143367,-56.8918467737974,
-40.8002436660988));
#242215=CARTESIAN_POINT('Ctrl Pts',(-46.5240532042183,-57.4139405955126,
-40.7697881931655));
#242216=CARTESIAN_POINT('Ctrl Pts',(-46.5148055933205,-57.6779181751886,
-40.7543895010177));
#242217=CARTESIAN_POINT('Ctrl Pts',(-46.3970923876378,-58.1792466717677,
-40.7251453387173));
#242218=CARTESIAN_POINT('Ctrl Pts',(-46.292878414085,-58.4125679690147,
-40.7123719527804));
#242219=CARTESIAN_POINT('Ctrl Pts',(-45.9960920612698,-58.8377249087666,
-40.6849784449773));
#242220=CARTESIAN_POINT('Ctrl Pts',(-45.8025456890086,-59.022815846432,
-40.6698023549094));
#242221=CARTESIAN_POINT('Ctrl Pts',(-45.3601435069346,-59.30319798829,-40.6392752032839));
#242222=CARTESIAN_POINT('Ctrl Pts',(-45.1168879421948,-59.397978261341,
-40.6242219578971));
#242223=CARTESIAN_POINT('Ctrl Pts',(-44.7450953866053,-59.4649119571554,
-40.603487453548));
#242224=CARTESIAN_POINT('Ctrl Pts',(-44.6265137360848,-59.475452478349,
-40.597189496243));
#242225=CARTESIAN_POINT('Ctrl Pts',(-44.5079524583206,-59.475452478349,
-40.5912000000001));
#242226=CARTESIAN_POINT('Origin',(-44.5079524583206,-57.475452478349,235.35105));
#242227=CARTESIAN_POINT('',(-44.5079524583206,-59.475452478349,-39.8912000000002));
#242228=CARTESIAN_POINT('',(-44.5079524583205,-59.475452478349,-40.0499499999999));
#242229=CARTESIAN_POINT('',(-44.5079524583206,-59.475452478349,235.35105));
#242230=CARTESIAN_POINT('',(-45.8699702267784,-56.010901219983,-39.4567770046169));
#242231=CARTESIAN_POINT('Ctrl Pts',(-44.5079524583206,-59.475452478349,
-39.8912000000001));
#242232=CARTESIAN_POINT('Ctrl Pts',(-44.4030527700808,-59.475452478349,
-39.8859006619664));
#242233=CARTESIAN_POINT('Ctrl Pts',(-44.2982740085944,-59.4672023132265,
-39.8803668031122));
#242234=CARTESIAN_POINT('Ctrl Pts',(-44.0546664311063,-59.428549470864,
-39.8669328247549));
#242235=CARTESIAN_POINT('Ctrl Pts',(-43.917561197412,-59.3915650040988,
-39.8589278085776));
#242236=CARTESIAN_POINT('Ctrl Pts',(-43.539674380705,-59.2451842460787,
-39.835568227459));
#242237=CARTESIAN_POINT('Ctrl Pts',(-43.3150565229897,-59.1022652247094,
-39.8200524776984));
#242238=CARTESIAN_POINT('Ctrl Pts',(-42.9362205101898,-58.7394597649563,
-39.7903325578167));
#242239=CARTESIAN_POINT('Ctrl Pts',(-42.7849633394211,-58.5239481327958,
-39.7773622465096));
#242240=CARTESIAN_POINT('Ctrl Pts',(-42.5753005145157,-58.0506268460953,
-39.7497518381187));
#242241=CARTESIAN_POINT('Ctrl Pts',(-42.5174960198121,-57.7979695862523,
-39.7350134979612));
#242242=CARTESIAN_POINT('Ctrl Pts',(-42.5002448277343,-57.2745386206229,
-39.7044800249661));
#242243=CARTESIAN_POINT('Ctrl Pts',(-42.5449525069551,-57.0086367960749,
-39.6889690852008));
#242244=CARTESIAN_POINT('Ctrl Pts',(-42.7317073816525,-56.5216343248397,
-39.660560607712));
#242245=CARTESIAN_POINT('Ctrl Pts',(-42.8673870546418,-56.3035453915529,
-39.6482310367443));
#242246=CARTESIAN_POINT('Ctrl Pts',(-43.2168701600232,-55.9260604160653,
-39.6195658188577));
#242247=CARTESIAN_POINT('Ctrl Pts',(-43.4288480106903,-55.7716257976807,
-39.6043527472713));
#242248=CARTESIAN_POINT('Ctrl Pts',(-43.9047472663919,-55.5502486800498,
-39.5738543653773));
#242249=CARTESIAN_POINT('Ctrl Pts',(-44.1649808945557,-55.4873165642459,
-39.5588723242467));
#242250=CARTESIAN_POINT('Ctrl Pts',(-44.6830970893764,-55.4670931849909,
-39.5321082047868));
#242251=CARTESIAN_POINT('Ctrl Pts',(-44.935884828577,-55.5053960545974,
-39.5187082946409));
#242252=CARTESIAN_POINT('Ctrl Pts',(-45.3036945482771,-55.6354872771797,
-39.4963329012561));
#242253=CARTESIAN_POINT('Ctrl Pts',(-45.4275250240718,-55.6941435067538,
-39.4883664081885));
#242254=CARTESIAN_POINT('Ctrl Pts',(-45.661019427692,-55.8356263389039,
-39.4724441206155));
#242255=CARTESIAN_POINT('Ctrl Pts',(-45.7701110912147,-55.9180341425543,
-39.4645294508118));
#242256=CARTESIAN_POINT('Ctrl Pts',(-45.8699701444046,-56.0109020958785,
-39.4567761076897));
#242257=CARTESIAN_POINT('',(-46.1726021450474,-56.3668761778516,-39.5898551203275));
#242258=CARTESIAN_POINT('Ctrl Pts',(-46.1726021471674,-56.3668761781232,
-39.5898551143304));
#242259=CARTESIAN_POINT('Ctrl Pts',(-46.1292686891332,-56.3018062073701,
-39.5680429301834));
#242260=CARTESIAN_POINT('Ctrl Pts',(-46.0821985274757,-56.239393519002,
-39.5459682234167));
#242261=CARTESIAN_POINT('Ctrl Pts',(-45.9810865903201,-56.1204740032778,
-39.5015108791791));
#242262=CARTESIAN_POINT('Ctrl Pts',(-45.927110977529,-56.0640425168199,
-39.4791550503913));
#242263=CARTESIAN_POINT('Ctrl Pts',(-45.8699701303408,-56.0109020827993,
-39.456778435228));
#242264=CARTESIAN_POINT('Ctrl Pts',(-46.1726021464359,-56.3668761770248,
-39.5898551218874));
#242265=CARTESIAN_POINT('Ctrl Pts',(-46.0838141022853,-56.2335511277457,
-39.5982291767623));
#242266=CARTESIAN_POINT('Ctrl Pts',(-45.9793476562866,-56.111398861529,
-39.6070694026315));
#242267=CARTESIAN_POINT('Ctrl Pts',(-45.7403294976802,-55.8916874465253,
-39.6255524070794));
#242268=CARTESIAN_POINT('Ctrl Pts',(-45.605941082968,-55.7957258336973,
-39.6351403413518));
#242269=CARTESIAN_POINT('Ctrl Pts',(-45.2282291009047,-55.5909056020896,
-39.6601955747942));
#242270=CARTESIAN_POINT('Ctrl Pts',(-44.9722651093681,-55.5120963029165,
-39.6754250063023));
#242271=CARTESIAN_POINT('Ctrl Pts',(-44.4562316377863,-55.4601269365062,
-39.7030098350655));
#242272=CARTESIAN_POINT('Ctrl Pts',(-44.2015878989259,-55.4828723992968,
-39.7156433846842));
#242273=CARTESIAN_POINT('Ctrl Pts',(-43.7067316346864,-55.6244254417704,
-39.7447712373595));
#242274=CARTESIAN_POINT('Ctrl Pts',(-43.4720515882353,-55.744800314759,
-39.7601377726042));
#242275=CARTESIAN_POINT('Ctrl Pts',(-43.0591643804455,-56.0714058466317,
-39.790522064583));
#242276=CARTESIAN_POINT('Ctrl Pts',(-42.8860320916942,-56.2756143860978,
-39.8049594446186));
#242277=CARTESIAN_POINT('Ctrl Pts',(-42.6345474374558,-56.7303461705793,
-39.83148546538));
#242278=CARTESIAN_POINT('Ctrl Pts',(-42.5550210142441,-56.9746108140771,
-39.8457342362507));
#242279=CARTESIAN_POINT('Ctrl Pts',(-42.4905949281106,-57.4895664751933,
-39.8757733164824));
#242280=CARTESIAN_POINT('Ctrl Pts',(-42.5101306523353,-57.7559010506206,
-39.891309500049));
#242281=CARTESIAN_POINT('Ctrl Pts',(-42.6502003430826,-58.2601709403834,
-39.9207252436185));
#242282=CARTESIAN_POINT('Ctrl Pts',(-42.7672375565043,-58.4937483705101,
-39.9333792695209));
#242283=CARTESIAN_POINT('Ctrl Pts',(-43.0830602239057,-58.9023423061901,
-39.9612513690734));
#242284=CARTESIAN_POINT('Ctrl Pts',(-43.2784359602378,-59.0737611424876,
-39.976121105604));
#242285=CARTESIAN_POINT('Ctrl Pts',(-43.7322273873726,-59.3382290998623,
-40.0067594570893));
#242286=CARTESIAN_POINT('Ctrl Pts',(-43.9883139194582,-59.4252464536864,
-40.0222344807131));
#242287=CARTESIAN_POINT('Ctrl Pts',(-44.338359511837,-59.4700651055624,
-40.0412253466293));
#242288=CARTESIAN_POINT('Ctrl Pts',(-44.4231941692624,-59.475452478349,
-40.045668168162));
#242289=CARTESIAN_POINT('Ctrl Pts',(-44.5079524583204,-59.475452478349,
-40.0499499999999));
#242290=CARTESIAN_POINT('Origin',(-44.5079524583202,31.5404524382932,-52.920575));
#242291=CARTESIAN_POINT('',(-42.8392071752677,31.5404524382931,-40.04995));
#242292=CARTESIAN_POINT('',(-42.8392071752677,31.5404524382931,-39.8912));
#242293=CARTESIAN_POINT('',(-42.8392071752678,31.5404524382932,-52.920575));
#242294=CARTESIAN_POINT('',(-43.0534148594279,32.3583957084033,-39.8341886583259));
#242295=CARTESIAN_POINT('Ctrl Pts',(-42.8392071752677,31.5404524382931,
-39.8912));
#242296=CARTESIAN_POINT('Ctrl Pts',(-42.8392071752677,31.97747304302,-39.8647400338745));
#242297=CARTESIAN_POINT('Ctrl Pts',(-43.0534148594279,32.3583957084033,
-39.8341886583259));
#242298=CARTESIAN_POINT('',(-43.3633208282253,32.7547543987198,-39.9581074212484));
#242299=CARTESIAN_POINT('Ctrl Pts',(-43.3633208282253,32.7547543987198,
-39.9581074212484));
#242300=CARTESIAN_POINT('Ctrl Pts',(-43.3034586305286,32.6983267825555,
-39.9374768681555));
#242301=CARTESIAN_POINT('Ctrl Pts',(-43.247828429449,32.6375299746023,-39.916915604885));
#242302=CARTESIAN_POINT('Ctrl Pts',(-43.1436618117789,32.5052440677468,
-39.8754008689186));
#242303=CARTESIAN_POINT('Ctrl Pts',(-43.0956858178016,32.4335655894238,
-39.8545232151814));
#242304=CARTESIAN_POINT('Ctrl Pts',(-43.0534148594279,32.3583957084032,
-39.834188658326));
#242305=CARTESIAN_POINT('Ctrl Pts',(-42.8392071752677,31.5404524382931,
-40.04995));
#242306=CARTESIAN_POINT('Ctrl Pts',(-42.8392071752677,32.2607116610065,
-40.0063409929454));
#242307=CARTESIAN_POINT('Ctrl Pts',(-43.3633208282253,32.7547543987198,
-39.9581074212484));
#242308=CARTESIAN_POINT('Origin',(-44.5079524583202,31.5404524382932,-52.920575));
#242309=CARTESIAN_POINT('',(-42.8392071752677,31.5404524382931,-40.74995));
#242310=CARTESIAN_POINT('',(-42.8392071752677,31.5404524382931,-40.5912));
#242311=CARTESIAN_POINT('',(-42.8392071752678,31.5404524382932,-52.920575));
#242312=CARTESIAN_POINT('',(-45.3466072487201,32.9831474726816,-40.3575667765883));
#242313=CARTESIAN_POINT('Ctrl Pts',(-42.8392071752677,31.5404524382931,
-40.5912));
#242314=CARTESIAN_POINT('Ctrl Pts',(-42.8392071752677,32.5039029766724,
-40.5328666666667));
#242315=CARTESIAN_POINT('Ctrl Pts',(-43.6735798167939,32.985628245862,-40.4745333333334));
#242316=CARTESIAN_POINT('Ctrl Pts',(-44.5079524583201,33.4673535150516,
-40.4162));
#242317=CARTESIAN_POINT('Ctrl Pts',(-45.3423250998464,32.985628245862,-40.3578666666667));
#242318=CARTESIAN_POINT('Ctrl Pts',(-45.3444680135345,32.9843910340674,
-40.3577168495559));
#242319=CARTESIAN_POINT('Ctrl Pts',(-45.3466072487201,32.9831474726816,
-40.3575667765883));
#242320=CARTESIAN_POINT('',(-46.1762418209585,31.5014470256211,-40.2388224305403));
#242321=CARTESIAN_POINT('Ctrl Pts',(-46.1762415911269,31.5014371968004,
-40.2388206025736));
#242322=CARTESIAN_POINT('Ctrl Pts',(-46.1796538231586,31.6473807982463,
-40.2659631539464));
#242323=CARTESIAN_POINT('Ctrl Pts',(-46.1639045822899,31.7938643599,-40.2897732731299));
#242324=CARTESIAN_POINT('Ctrl Pts',(-46.0934988211157,32.0817317952749,
-40.3293811885115));
#242325=CARTESIAN_POINT('Ctrl Pts',(-46.0387181149382,32.221603202291,-40.3449011256526));
#242326=CARTESIAN_POINT('Ctrl Pts',(-45.8931721207653,32.482839107779,-40.3660091204542));
#242327=CARTESIAN_POINT('Ctrl Pts',(-45.8033957445043,32.6029396495541,
-40.371534813758));
#242328=CARTESIAN_POINT('Ctrl Pts',(-45.6856456418945,32.7228632916643,
-40.3719334317363));
#242329=CARTESIAN_POINT('Ctrl Pts',(-45.6723922330737,32.7359175307787,
-40.3718982162907));
#242330=CARTESIAN_POINT('Ctrl Pts',(-45.5642589075492,32.8389209808004,
-40.3709686031484));
#242331=CARTESIAN_POINT('Ctrl Pts',(-45.4594610512511,32.9175442926251,
-40.3661892700017));
#242332=CARTESIAN_POINT('Ctrl Pts',(-45.3466072487201,32.9831474726816,
-40.3575667765883));
#242333=CARTESIAN_POINT('Ctrl Pts',(-46.1762418209585,31.501447025621,-40.2388224305402));
#242334=CARTESIAN_POINT('Ctrl Pts',(-46.1543258544958,30.5640854850033,
-40.1813025852605));
#242335=CARTESIAN_POINT('Ctrl Pts',(-45.3423250998464,30.0952766307242,
-40.1245333333334));
#242336=CARTESIAN_POINT('Ctrl Pts',(-44.5079524583202,29.6135513615346,
-40.0662));
#242337=CARTESIAN_POINT('Ctrl Pts',(-43.6735798167939,30.0952766307242,
-40.0078666666667));
#242338=CARTESIAN_POINT('Ctrl Pts',(-42.8392071752677,30.5770018999139,
-39.9495333333333));
#242339=CARTESIAN_POINT('Ctrl Pts',(-42.8392071752677,31.5404524382931,
-39.8912));
#242340=CARTESIAN_POINT('Ctrl Pts',(-42.8392071752677,31.5404524382931,
-40.74995));
#242341=CARTESIAN_POINT('Ctrl Pts',(-42.8392071752677,32.5039029766724,
-40.6916166666667));
#242342=CARTESIAN_POINT('Ctrl Pts',(-43.6735798167939,32.985628245862,-40.6332833333334));
#242343=CARTESIAN_POINT('Ctrl Pts',(-44.5079524583201,33.4673535150516,
-40.57495));
#242344=CARTESIAN_POINT('Ctrl Pts',(-45.3423250998464,32.985628245862,-40.5166166666666));
#242345=CARTESIAN_POINT('Ctrl Pts',(-46.1766977413726,32.5039029766724,
-40.4582833333333));
#242346=CARTESIAN_POINT('Ctrl Pts',(-46.1766977413726,31.5404524382932,
-40.39995));
#242347=CARTESIAN_POINT('Ctrl Pts',(-46.1766977413726,30.5770018999139,
-40.3416166666667));
#242348=CARTESIAN_POINT('Ctrl Pts',(-45.3423250998464,30.0952766307242,
-40.2832833333334));
#242349=CARTESIAN_POINT('Ctrl Pts',(-44.5079524583202,29.6135513615346,
-40.22495));
#242350=CARTESIAN_POINT('Ctrl Pts',(-43.6735798167939,30.0952766307242,
-40.1666166666667));
#242351=CARTESIAN_POINT('Ctrl Pts',(-42.8392071752677,30.5770018999139,
-40.1082833333334));
#242352=CARTESIAN_POINT('Ctrl Pts',(-42.8392071752677,31.5404524382931,
-40.04995));
#242353=CARTESIAN_POINT('Origin',(-44.5079524583202,31.5404524382932,-52.920575));
#242354=CARTESIAN_POINT('',(-42.8392071752677,31.5404524382931,-41.44995));
#242355=CARTESIAN_POINT('',(-42.8392071752677,31.5404524382931,-41.2912));
#242356=CARTESIAN_POINT('',(-42.8392071752678,31.5404524382932,-52.920575));
#242357=CARTESIAN_POINT('Ctrl Pts',(-42.8392071752677,31.5404524382931,
-41.2912));
#242358=CARTESIAN_POINT('Ctrl Pts',(-42.8392071752677,32.5039029766724,
-41.2328666666667));
#242359=CARTESIAN_POINT('Ctrl Pts',(-43.6735798167939,32.985628245862,-41.1745333333334));
#242360=CARTESIAN_POINT('Ctrl Pts',(-44.5079524583201,33.4673535150516,
-41.1162));
#242361=CARTESIAN_POINT('Ctrl Pts',(-45.3423250998464,32.985628245862,-41.0578666666667));
#242362=CARTESIAN_POINT('Ctrl Pts',(-46.1766977413726,32.5039029766724,
-40.9995333333333));
#242363=CARTESIAN_POINT('Ctrl Pts',(-46.1766977413726,31.5404524382932,
-40.9412));
#242364=CARTESIAN_POINT('Ctrl Pts',(-46.1766977413726,30.5770018999139,
-40.8828666666667));
#242365=CARTESIAN_POINT('Ctrl Pts',(-45.3423250998464,30.0952766307242,
-40.8245333333333));
#242366=CARTESIAN_POINT('Ctrl Pts',(-44.5079524583202,29.6135513615346,
-40.7662));
#242367=CARTESIAN_POINT('Ctrl Pts',(-43.6735798167939,30.0952766307242,
-40.7078666666667));
#242368=CARTESIAN_POINT('Ctrl Pts',(-42.8392071752677,30.5770018999139,
-40.6495333333333));
#242369=CARTESIAN_POINT('Ctrl Pts',(-42.8392071752677,31.5404524382931,
-40.5912));
#242370=CARTESIAN_POINT('Ctrl Pts',(-42.8392071752677,31.5404524382931,
-41.44995));
#242371=CARTESIAN_POINT('Ctrl Pts',(-42.8392071752677,32.5039029766724,
-41.3916166666667));
#242372=CARTESIAN_POINT('Ctrl Pts',(-43.6735798167939,32.985628245862,-41.3332833333334));
#242373=CARTESIAN_POINT('Ctrl Pts',(-44.5079524583201,33.4673535150516,
-41.27495));
#242374=CARTESIAN_POINT('Ctrl Pts',(-45.3423250998464,32.985628245862,-41.2166166666667));
#242375=CARTESIAN_POINT('Ctrl Pts',(-46.1766977413726,32.5039029766724,
-41.1582833333333));
#242376=CARTESIAN_POINT('Ctrl Pts',(-46.1766977413726,31.5404524382932,
-41.09995));
#242377=CARTESIAN_POINT('Ctrl Pts',(-46.1766977413726,30.5770018999139,
-41.0416166666667));
#242378=CARTESIAN_POINT('Ctrl Pts',(-45.3423250998464,30.0952766307242,
-40.9832833333333));
#242379=CARTESIAN_POINT('Ctrl Pts',(-44.5079524583202,29.6135513615346,
-40.92495));
#242380=CARTESIAN_POINT('Ctrl Pts',(-43.6735798167939,30.0952766307242,
-40.8666166666667));
#242381=CARTESIAN_POINT('Ctrl Pts',(-42.8392071752677,30.5770018999139,
-40.8082833333334));
#242382=CARTESIAN_POINT('Ctrl Pts',(-42.8392071752677,31.5404524382931,
-40.74995));
#242383=CARTESIAN_POINT('Origin',(-44.5079524583202,31.5404524382932,-52.920575));
#242384=CARTESIAN_POINT('',(-42.8392071752677,31.5404524382931,-42.14995));
#242385=CARTESIAN_POINT('',(-42.8392071752677,31.5404524382931,-41.9912));
#242386=CARTESIAN_POINT('',(-42.8392071752678,31.5404524382932,-52.920575));
#242387=CARTESIAN_POINT('Ctrl Pts',(-42.8392071752677,31.5404524382931,
-41.9912));
#242388=CARTESIAN_POINT('Ctrl Pts',(-42.8392071752677,32.5039029766724,
-41.9328666666667));
#242389=CARTESIAN_POINT('Ctrl Pts',(-43.6735798167939,32.985628245862,-41.8745333333334));
#242390=CARTESIAN_POINT('Ctrl Pts',(-44.5079524583201,33.4673535150516,
-41.8162));
#242391=CARTESIAN_POINT('Ctrl Pts',(-45.3423250998464,32.985628245862,-41.7578666666667));
#242392=CARTESIAN_POINT('Ctrl Pts',(-46.1766977413726,32.5039029766724,
-41.6995333333334));
#242393=CARTESIAN_POINT('Ctrl Pts',(-46.1766977413726,31.5404524382932,
-41.6412));
#242394=CARTESIAN_POINT('Ctrl Pts',(-46.1766977413726,30.5770018999139,
-41.5828666666667));
#242395=CARTESIAN_POINT('Ctrl Pts',(-45.3423250998464,30.0952766307242,
-41.5245333333334));
#242396=CARTESIAN_POINT('Ctrl Pts',(-44.5079524583202,29.6135513615346,
-41.4662));
#242397=CARTESIAN_POINT('Ctrl Pts',(-43.6735798167939,30.0952766307242,
-41.4078666666667));
#242398=CARTESIAN_POINT('Ctrl Pts',(-42.8392071752677,30.5770018999139,
-41.3495333333333));
#242399=CARTESIAN_POINT('Ctrl Pts',(-42.8392071752677,31.5404524382931,
-41.2912));
#242400=CARTESIAN_POINT('Ctrl Pts',(-42.8392071752677,31.5404524382931,
-42.14995));
#242401=CARTESIAN_POINT('Ctrl Pts',(-42.8392071752677,32.5039029766724,
-42.0916166666667));
#242402=CARTESIAN_POINT('Ctrl Pts',(-43.6735798167939,32.985628245862,-42.0332833333334));
#242403=CARTESIAN_POINT('Ctrl Pts',(-44.5079524583201,33.4673535150516,
-41.97495));
#242404=CARTESIAN_POINT('Ctrl Pts',(-45.3423250998464,32.985628245862,-41.9166166666666));
#242405=CARTESIAN_POINT('Ctrl Pts',(-46.1766977413726,32.5039029766724,
-41.8582833333333));
#242406=CARTESIAN_POINT('Ctrl Pts',(-46.1766977413726,31.5404524382932,
-41.79995));
#242407=CARTESIAN_POINT('Ctrl Pts',(-46.1766977413726,30.5770018999139,
-41.7416166666666));
#242408=CARTESIAN_POINT('Ctrl Pts',(-45.3423250998464,30.0952766307242,
-41.6832833333333));
#242409=CARTESIAN_POINT('Ctrl Pts',(-44.5079524583202,29.6135513615346,
-41.62495));
#242410=CARTESIAN_POINT('Ctrl Pts',(-43.6735798167939,30.0952766307242,
-41.5666166666667));
#242411=CARTESIAN_POINT('Ctrl Pts',(-42.8392071752677,30.5770018999139,
-41.5082833333334));
#242412=CARTESIAN_POINT('Ctrl Pts',(-42.8392071752677,31.5404524382931,
-41.44995));
#242413=CARTESIAN_POINT('Origin',(-44.5079524583202,31.5404524382932,-52.920575));
#242414=CARTESIAN_POINT('',(-42.8392071752677,31.5404524382931,-42.84995));
#242415=CARTESIAN_POINT('',(-42.8392071752677,31.5404524382931,-42.6912));
#242416=CARTESIAN_POINT('',(-42.8392071752678,31.5404524382932,-52.920575));
#242417=CARTESIAN_POINT('Ctrl Pts',(-42.8392071752677,31.5404524382931,
-42.6912));
#242418=CARTESIAN_POINT('Ctrl Pts',(-42.8392071752677,32.5039029766724,
-42.6328666666667));
#242419=CARTESIAN_POINT('Ctrl Pts',(-43.6735798167939,32.985628245862,-42.5745333333333));
#242420=CARTESIAN_POINT('Ctrl Pts',(-44.5079524583201,33.4673535150516,
-42.5162));
#242421=CARTESIAN_POINT('Ctrl Pts',(-45.3423250998464,32.985628245862,-42.4578666666667));
#242422=CARTESIAN_POINT('Ctrl Pts',(-46.1766977413726,32.5039029766724,
-42.3995333333334));
#242423=CARTESIAN_POINT('Ctrl Pts',(-46.1766977413726,31.5404524382932,
-42.3412));
#242424=CARTESIAN_POINT('Ctrl Pts',(-46.1766977413726,30.5770018999139,
-42.2828666666667));
#242425=CARTESIAN_POINT('Ctrl Pts',(-45.3423250998464,30.0952766307242,
-42.2245333333333));
#242426=CARTESIAN_POINT('Ctrl Pts',(-44.5079524583202,29.6135513615346,
-42.1662));
#242427=CARTESIAN_POINT('Ctrl Pts',(-43.6735798167939,30.0952766307242,
-42.1078666666667));
#242428=CARTESIAN_POINT('Ctrl Pts',(-42.8392071752677,30.5770018999139,
-42.0495333333334));
#242429=CARTESIAN_POINT('Ctrl Pts',(-42.8392071752677,31.5404524382931,
-41.9912));
#242430=CARTESIAN_POINT('Ctrl Pts',(-42.8392071752677,31.5404524382931,
-42.84995));
#242431=CARTESIAN_POINT('Ctrl Pts',(-42.8392071752677,32.5039029766724,
-42.7916166666667));
#242432=CARTESIAN_POINT('Ctrl Pts',(-43.6735798167939,32.985628245862,-42.7332833333334));
#242433=CARTESIAN_POINT('Ctrl Pts',(-44.5079524583201,33.4673535150516,
-42.67495));
#242434=CARTESIAN_POINT('Ctrl Pts',(-45.3423250998464,32.985628245862,-42.6166166666667));
#242435=CARTESIAN_POINT('Ctrl Pts',(-46.1766977413726,32.5039029766724,
-42.5582833333333));
#242436=CARTESIAN_POINT('Ctrl Pts',(-46.1766977413726,31.5404524382932,
-42.49995));
#242437=CARTESIAN_POINT('Ctrl Pts',(-46.1766977413726,30.5770018999139,
-42.4416166666666));
#242438=CARTESIAN_POINT('Ctrl Pts',(-45.3423250998464,30.0952766307242,
-42.3832833333333));
#242439=CARTESIAN_POINT('Ctrl Pts',(-44.5079524583202,29.6135513615346,
-42.32495));
#242440=CARTESIAN_POINT('Ctrl Pts',(-43.6735798167939,30.0952766307242,
-42.2666166666667));
#242441=CARTESIAN_POINT('Ctrl Pts',(-42.8392071752677,30.5770018999139,
-42.2082833333333));
#242442=CARTESIAN_POINT('Ctrl Pts',(-42.8392071752677,31.5404524382931,
-42.14995));
#242443=CARTESIAN_POINT('Origin',(-44.5079524583202,31.5404524382932,-52.920575));
#242444=CARTESIAN_POINT('',(-42.8392071752677,31.5404524382931,-43.54995));
#242445=CARTESIAN_POINT('',(-42.8392071752677,31.5404524382931,-43.3912));
#242446=CARTESIAN_POINT('',(-42.8392071752678,31.5404524382932,-52.920575));
#242447=CARTESIAN_POINT('Ctrl Pts',(-42.8392071752677,31.5404524382931,
-43.3912));
#242448=CARTESIAN_POINT('Ctrl Pts',(-42.8392071752677,32.5039029766724,
-43.3328666666667));
#242449=CARTESIAN_POINT('Ctrl Pts',(-43.6735798167939,32.985628245862,-43.2745333333334));
#242450=CARTESIAN_POINT('Ctrl Pts',(-44.5079524583201,33.4673535150516,
-43.2162));
#242451=CARTESIAN_POINT('Ctrl Pts',(-45.3423250998464,32.985628245862,-43.1578666666667));
#242452=CARTESIAN_POINT('Ctrl Pts',(-46.1766977413726,32.5039029766724,
-43.0995333333334));
#242453=CARTESIAN_POINT('Ctrl Pts',(-46.1766977413726,31.5404524382932,
-43.0412));
#242454=CARTESIAN_POINT('Ctrl Pts',(-46.1766977413726,30.5770018999139,
-42.9828666666667));
#242455=CARTESIAN_POINT('Ctrl Pts',(-45.3423250998464,30.0952766307242,
-42.9245333333334));
#242456=CARTESIAN_POINT('Ctrl Pts',(-44.5079524583202,29.6135513615346,
-42.8662));
#242457=CARTESIAN_POINT('Ctrl Pts',(-43.6735798167939,30.0952766307242,
-42.8078666666667));
#242458=CARTESIAN_POINT('Ctrl Pts',(-42.8392071752677,30.5770018999139,
-42.7495333333334));
#242459=CARTESIAN_POINT('Ctrl Pts',(-42.8392071752677,31.5404524382931,
-42.6912));
#242460=CARTESIAN_POINT('Ctrl Pts',(-42.8392071752677,31.5404524382931,
-43.54995));
#242461=CARTESIAN_POINT('Ctrl Pts',(-42.8392071752677,32.5039029766724,
-43.4916166666667));
#242462=CARTESIAN_POINT('Ctrl Pts',(-43.6735798167939,32.985628245862,-43.4332833333333));
#242463=CARTESIAN_POINT('Ctrl Pts',(-44.5079524583201,33.4673535150516,
-43.37495));
#242464=CARTESIAN_POINT('Ctrl Pts',(-45.3423250998464,32.985628245862,-43.3166166666667));
#242465=CARTESIAN_POINT('Ctrl Pts',(-46.1766977413726,32.5039029766724,
-43.2582833333333));
#242466=CARTESIAN_POINT('Ctrl Pts',(-46.1766977413726,31.5404524382932,
-43.19995));
#242467=CARTESIAN_POINT('Ctrl Pts',(-46.1766977413726,30.5770018999139,
-43.1416166666666));
#242468=CARTESIAN_POINT('Ctrl Pts',(-45.3423250998464,30.0952766307242,
-43.0832833333333));
#242469=CARTESIAN_POINT('Ctrl Pts',(-44.5079524583202,29.6135513615346,
-43.02495));
#242470=CARTESIAN_POINT('Ctrl Pts',(-43.6735798167939,30.0952766307242,
-42.9666166666667));
#242471=CARTESIAN_POINT('Ctrl Pts',(-42.8392071752677,30.5770018999139,
-42.9082833333333));
#242472=CARTESIAN_POINT('Ctrl Pts',(-42.8392071752677,31.5404524382931,
-42.84995));
#242473=CARTESIAN_POINT('Origin',(-44.5079524583202,31.5404524382932,-52.920575));
#242474=CARTESIAN_POINT('',(-42.8392071752677,31.5404524382931,-44.24995));
#242475=CARTESIAN_POINT('',(-42.8392071752677,31.5404524382931,-44.0912));
#242476=CARTESIAN_POINT('',(-42.8392071752678,31.5404524382932,-52.920575));
#242477=CARTESIAN_POINT('Ctrl Pts',(-42.8392071752677,31.5404524382931,
-44.0912));
#242478=CARTESIAN_POINT('Ctrl Pts',(-42.8392071752677,32.5039029766724,
-44.0328666666667));
#242479=CARTESIAN_POINT('Ctrl Pts',(-43.6735798167939,32.985628245862,-43.9745333333333));
#242480=CARTESIAN_POINT('Ctrl Pts',(-44.5079524583201,33.4673535150516,
-43.9162));
#242481=CARTESIAN_POINT('Ctrl Pts',(-45.3423250998464,32.985628245862,-43.8578666666667));
#242482=CARTESIAN_POINT('Ctrl Pts',(-46.1766977413726,32.5039029766724,
-43.7995333333334));
#242483=CARTESIAN_POINT('Ctrl Pts',(-46.1766977413726,31.5404524382932,
-43.7412));
#242484=CARTESIAN_POINT('Ctrl Pts',(-46.1766977413726,30.5770018999139,
-43.6828666666667));
#242485=CARTESIAN_POINT('Ctrl Pts',(-45.3423250998464,30.0952766307242,
-43.6245333333333));
#242486=CARTESIAN_POINT('Ctrl Pts',(-44.5079524583202,29.6135513615346,
-43.5662));
#242487=CARTESIAN_POINT('Ctrl Pts',(-43.6735798167939,30.0952766307242,
-43.5078666666667));
#242488=CARTESIAN_POINT('Ctrl Pts',(-42.8392071752677,30.5770018999139,
-43.4495333333334));
#242489=CARTESIAN_POINT('Ctrl Pts',(-42.8392071752677,31.5404524382931,
-43.3912));
#242490=CARTESIAN_POINT('Ctrl Pts',(-42.8392071752677,31.5404524382931,
-44.24995));
#242491=CARTESIAN_POINT('Ctrl Pts',(-42.8392071752677,32.5039029766724,
-44.1916166666667));
#242492=CARTESIAN_POINT('Ctrl Pts',(-43.6735798167939,32.985628245862,-44.1332833333334));
#242493=CARTESIAN_POINT('Ctrl Pts',(-44.5079524583201,33.4673535150516,
-44.07495));
#242494=CARTESIAN_POINT('Ctrl Pts',(-45.3423250998464,32.985628245862,-44.0166166666667));
#242495=CARTESIAN_POINT('Ctrl Pts',(-46.1766977413726,32.5039029766724,
-43.9582833333334));
#242496=CARTESIAN_POINT('Ctrl Pts',(-46.1766977413726,31.5404524382932,
-43.89995));
#242497=CARTESIAN_POINT('Ctrl Pts',(-46.1766977413726,30.5770018999139,
-43.8416166666667));
#242498=CARTESIAN_POINT('Ctrl Pts',(-45.3423250998464,30.0952766307242,
-43.7832833333334));
#242499=CARTESIAN_POINT('Ctrl Pts',(-44.5079524583202,29.6135513615346,
-43.72495));
#242500=CARTESIAN_POINT('Ctrl Pts',(-43.6735798167939,30.0952766307242,
-43.6666166666667));
#242501=CARTESIAN_POINT('Ctrl Pts',(-42.8392071752677,30.5770018999139,
-43.6082833333333));
#242502=CARTESIAN_POINT('Ctrl Pts',(-42.8392071752677,31.5404524382931,
-43.54995));
#242503=CARTESIAN_POINT('Origin',(-44.5079524583202,31.5404524382932,-52.920575));
#242504=CARTESIAN_POINT('',(-42.8392071752677,31.5404524382931,-44.94995));
#242505=CARTESIAN_POINT('',(-42.8392071752677,31.5404524382931,-44.7912));
#242506=CARTESIAN_POINT('',(-42.8392071752678,31.5404524382932,-52.920575));
#242507=CARTESIAN_POINT('Ctrl Pts',(-42.8392071752677,31.5404524382931,
-44.7912));
#242508=CARTESIAN_POINT('Ctrl Pts',(-42.8392071752677,32.5039029766724,
-44.7328666666667));
#242509=CARTESIAN_POINT('Ctrl Pts',(-43.6735798167939,32.985628245862,-44.6745333333334));
#242510=CARTESIAN_POINT('Ctrl Pts',(-44.5079524583201,33.4673535150516,
-44.6162));
#242511=CARTESIAN_POINT('Ctrl Pts',(-45.3423250998464,32.985628245862,-44.5578666666667));
#242512=CARTESIAN_POINT('Ctrl Pts',(-46.1766977413726,32.5039029766724,
-44.4995333333333));
#242513=CARTESIAN_POINT('Ctrl Pts',(-46.1766977413726,31.5404524382932,
-44.4412));
#242514=CARTESIAN_POINT('Ctrl Pts',(-46.1766977413726,30.5770018999139,
-44.3828666666667));
#242515=CARTESIAN_POINT('Ctrl Pts',(-45.3423250998464,30.0952766307242,
-44.3245333333334));
#242516=CARTESIAN_POINT('Ctrl Pts',(-44.5079524583202,29.6135513615346,
-44.2662));
#242517=CARTESIAN_POINT('Ctrl Pts',(-43.6735798167939,30.0952766307242,
-44.2078666666667));
#242518=CARTESIAN_POINT('Ctrl Pts',(-42.8392071752677,30.5770018999139,
-44.1495333333334));
#242519=CARTESIAN_POINT('Ctrl Pts',(-42.8392071752677,31.5404524382931,
-44.0912));
#242520=CARTESIAN_POINT('Ctrl Pts',(-42.8392071752677,31.5404524382931,
-44.94995));
#242521=CARTESIAN_POINT('Ctrl Pts',(-42.8392071752677,32.5039029766724,
-44.8916166666667));
#242522=CARTESIAN_POINT('Ctrl Pts',(-43.6735798167939,32.985628245862,-44.8332833333334));
#242523=CARTESIAN_POINT('Ctrl Pts',(-44.5079524583201,33.4673535150516,
-44.77495));
#242524=CARTESIAN_POINT('Ctrl Pts',(-45.3423250998464,32.985628245862,-44.7166166666667));
#242525=CARTESIAN_POINT('Ctrl Pts',(-46.1766977413726,32.5039029766724,
-44.6582833333333));
#242526=CARTESIAN_POINT('Ctrl Pts',(-46.1766977413726,31.5404524382932,
-44.59995));
#242527=CARTESIAN_POINT('Ctrl Pts',(-46.1766977413726,30.5770018999139,
-44.5416166666667));
#242528=CARTESIAN_POINT('Ctrl Pts',(-45.3423250998464,30.0952766307242,
-44.4832833333334));
#242529=CARTESIAN_POINT('Ctrl Pts',(-44.5079524583202,29.6135513615346,
-44.42495));
#242530=CARTESIAN_POINT('Ctrl Pts',(-43.6735798167939,30.0952766307242,
-44.3666166666667));
#242531=CARTESIAN_POINT('Ctrl Pts',(-42.8392071752677,30.5770018999139,
-44.3082833333334));
#242532=CARTESIAN_POINT('Ctrl Pts',(-42.8392071752677,31.5404524382931,
-44.24995));
#242533=CARTESIAN_POINT('Origin',(-44.5079524583202,31.5404524382932,-52.920575));
#242534=CARTESIAN_POINT('',(-42.8392071752677,31.5404524382931,-45.64995));
#242535=CARTESIAN_POINT('',(-42.8392071752677,31.5404524382931,-45.4912));
#242536=CARTESIAN_POINT('',(-42.8392071752678,31.5404524382932,-52.920575));
#242537=CARTESIAN_POINT('Ctrl Pts',(-42.8392071752677,31.5404524382931,
-45.4912));
#242538=CARTESIAN_POINT('Ctrl Pts',(-42.8392071752677,32.5039029766724,
-45.4328666666666));
#242539=CARTESIAN_POINT('Ctrl Pts',(-43.6735798167939,32.985628245862,-45.3745333333333));
#242540=CARTESIAN_POINT('Ctrl Pts',(-44.5079524583201,33.4673535150516,
-45.3162));
#242541=CARTESIAN_POINT('Ctrl Pts',(-45.3423250998464,32.985628245862,-45.2578666666667));
#242542=CARTESIAN_POINT('Ctrl Pts',(-46.1766977413726,32.5039029766724,
-45.1995333333333));
#242543=CARTESIAN_POINT('Ctrl Pts',(-46.1766977413726,31.5404524382932,
-45.1412));
#242544=CARTESIAN_POINT('Ctrl Pts',(-46.1766977413726,30.5770018999139,
-45.0828666666667));
#242545=CARTESIAN_POINT('Ctrl Pts',(-45.3423250998464,30.0952766307242,
-45.0245333333333));
#242546=CARTESIAN_POINT('Ctrl Pts',(-44.5079524583202,29.6135513615346,
-44.9662));
#242547=CARTESIAN_POINT('Ctrl Pts',(-43.6735798167939,30.0952766307242,
-44.9078666666666));
#242548=CARTESIAN_POINT('Ctrl Pts',(-42.8392071752677,30.5770018999139,
-44.8495333333333));
#242549=CARTESIAN_POINT('Ctrl Pts',(-42.8392071752677,31.5404524382931,
-44.7912));
#242550=CARTESIAN_POINT('Ctrl Pts',(-42.8392071752677,31.5404524382931,
-45.64995));
#242551=CARTESIAN_POINT('Ctrl Pts',(-42.8392071752677,32.5039029766724,
-45.5916166666667));
#242552=CARTESIAN_POINT('Ctrl Pts',(-43.6735798167939,32.985628245862,-45.5332833333333));
#242553=CARTESIAN_POINT('Ctrl Pts',(-44.5079524583201,33.4673535150516,
-45.47495));
#242554=CARTESIAN_POINT('Ctrl Pts',(-45.3423250998464,32.985628245862,-45.4166166666667));
#242555=CARTESIAN_POINT('Ctrl Pts',(-46.1766977413726,32.5039029766724,
-45.3582833333334));
#242556=CARTESIAN_POINT('Ctrl Pts',(-46.1766977413726,31.5404524382932,
-45.29995));
#242557=CARTESIAN_POINT('Ctrl Pts',(-46.1766977413726,30.5770018999139,
-45.2416166666667));
#242558=CARTESIAN_POINT('Ctrl Pts',(-45.3423250998464,30.0952766307242,
-45.1832833333333));
#242559=CARTESIAN_POINT('Ctrl Pts',(-44.5079524583202,29.6135513615346,
-45.12495));
#242560=CARTESIAN_POINT('Ctrl Pts',(-43.6735798167939,30.0952766307242,
-45.0666166666667));
#242561=CARTESIAN_POINT('Ctrl Pts',(-42.8392071752677,30.5770018999139,
-45.0082833333334));
#242562=CARTESIAN_POINT('Ctrl Pts',(-42.8392071752677,31.5404524382931,
-44.94995));
#242563=CARTESIAN_POINT('Origin',(-44.5079524583202,31.5404524382932,-52.920575));
#242564=CARTESIAN_POINT('',(-42.8392071752677,31.5404524382931,-46.34995));
#242565=CARTESIAN_POINT('',(-42.8392071752677,31.5404524382931,-46.1912));
#242566=CARTESIAN_POINT('',(-42.8392071752678,31.5404524382932,-52.920575));
#242567=CARTESIAN_POINT('Ctrl Pts',(-42.8392071752677,31.5404524382931,
-46.1912));
#242568=CARTESIAN_POINT('Ctrl Pts',(-42.8392071752677,32.5039029766724,
-46.1328666666667));
#242569=CARTESIAN_POINT('Ctrl Pts',(-43.6735798167939,32.985628245862,-46.0745333333334));
#242570=CARTESIAN_POINT('Ctrl Pts',(-44.5079524583201,33.4673535150516,
-46.0162));
#242571=CARTESIAN_POINT('Ctrl Pts',(-45.3423250998464,32.985628245862,-45.9578666666667));
#242572=CARTESIAN_POINT('Ctrl Pts',(-46.1766977413726,32.5039029766724,
-45.8995333333333));
#242573=CARTESIAN_POINT('Ctrl Pts',(-46.1766977413726,31.5404524382932,
-45.8412));
#242574=CARTESIAN_POINT('Ctrl Pts',(-46.1766977413726,30.5770018999139,
-45.7828666666667));
#242575=CARTESIAN_POINT('Ctrl Pts',(-45.3423250998464,30.0952766307242,
-45.7245333333333));
#242576=CARTESIAN_POINT('Ctrl Pts',(-44.5079524583202,29.6135513615346,
-45.6662));
#242577=CARTESIAN_POINT('Ctrl Pts',(-43.6735798167939,30.0952766307242,
-45.6078666666667));
#242578=CARTESIAN_POINT('Ctrl Pts',(-42.8392071752677,30.5770018999139,
-45.5495333333333));
#242579=CARTESIAN_POINT('Ctrl Pts',(-42.8392071752677,31.5404524382931,
-45.4912));
#242580=CARTESIAN_POINT('Ctrl Pts',(-42.8392071752677,31.5404524382931,
-46.34995));
#242581=CARTESIAN_POINT('Ctrl Pts',(-42.8392071752677,32.5039029766724,
-46.2916166666667));
#242582=CARTESIAN_POINT('Ctrl Pts',(-43.6735798167939,32.985628245862,-46.2332833333334));
#242583=CARTESIAN_POINT('Ctrl Pts',(-44.5079524583201,33.4673535150516,
-46.17495));
#242584=CARTESIAN_POINT('Ctrl Pts',(-45.3423250998464,32.985628245862,-46.1166166666667));
#242585=CARTESIAN_POINT('Ctrl Pts',(-46.1766977413726,32.5039029766724,
-46.0582833333333));
#242586=CARTESIAN_POINT('Ctrl Pts',(-46.1766977413726,31.5404524382932,
-45.99995));
#242587=CARTESIAN_POINT('Ctrl Pts',(-46.1766977413726,30.5770018999139,
-45.9416166666667));
#242588=CARTESIAN_POINT('Ctrl Pts',(-45.3423250998464,30.0952766307242,
-45.8832833333333));
#242589=CARTESIAN_POINT('Ctrl Pts',(-44.5079524583202,29.6135513615346,
-45.82495));
#242590=CARTESIAN_POINT('Ctrl Pts',(-43.6735798167939,30.0952766307242,
-45.7666166666667));
#242591=CARTESIAN_POINT('Ctrl Pts',(-42.8392071752677,30.5770018999139,
-45.7082833333333));
#242592=CARTESIAN_POINT('Ctrl Pts',(-42.8392071752677,31.5404524382931,
-45.64995));
#242593=CARTESIAN_POINT('Origin',(-44.5079524583202,31.5404524382932,-52.920575));
#242594=CARTESIAN_POINT('',(-42.8392071752677,31.5404524382931,-47.04995));
#242595=CARTESIAN_POINT('',(-42.8392071752677,31.5404524382931,-46.8912));
#242596=CARTESIAN_POINT('',(-42.8392071752678,31.5404524382932,-52.920575));
#242597=CARTESIAN_POINT('Ctrl Pts',(-42.8392071752677,31.5404524382931,
-46.8912));
#242598=CARTESIAN_POINT('Ctrl Pts',(-42.8392071752677,32.5039029766724,
-46.8328666666667));
#242599=CARTESIAN_POINT('Ctrl Pts',(-43.6735798167939,32.985628245862,-46.7745333333333));
#242600=CARTESIAN_POINT('Ctrl Pts',(-44.5079524583201,33.4673535150516,
-46.7162));
#242601=CARTESIAN_POINT('Ctrl Pts',(-45.3423250998464,32.985628245862,-46.6578666666667));
#242602=CARTESIAN_POINT('Ctrl Pts',(-46.1766977413726,32.5039029766724,
-46.5995333333333));
#242603=CARTESIAN_POINT('Ctrl Pts',(-46.1766977413726,31.5404524382932,
-46.5412));
#242604=CARTESIAN_POINT('Ctrl Pts',(-46.1766977413726,30.5770018999139,
-46.4828666666667));
#242605=CARTESIAN_POINT('Ctrl Pts',(-45.3423250998464,30.0952766307242,
-46.4245333333333));
#242606=CARTESIAN_POINT('Ctrl Pts',(-44.5079524583202,29.6135513615346,
-46.3662));
#242607=CARTESIAN_POINT('Ctrl Pts',(-43.6735798167939,30.0952766307242,
-46.3078666666667));
#242608=CARTESIAN_POINT('Ctrl Pts',(-42.8392071752677,30.5770018999139,
-46.2495333333334));
#242609=CARTESIAN_POINT('Ctrl Pts',(-42.8392071752677,31.5404524382931,
-46.1912));
#242610=CARTESIAN_POINT('Ctrl Pts',(-42.8392071752677,31.5404524382931,
-47.04995));
#242611=CARTESIAN_POINT('Ctrl Pts',(-42.8392071752677,32.5039029766724,
-46.9916166666667));
#242612=CARTESIAN_POINT('Ctrl Pts',(-43.6735798167939,32.985628245862,-46.9332833333333));
#242613=CARTESIAN_POINT('Ctrl Pts',(-44.5079524583201,33.4673535150516,
-46.87495));
#242614=CARTESIAN_POINT('Ctrl Pts',(-45.3423250998464,32.985628245862,-46.8166166666667));
#242615=CARTESIAN_POINT('Ctrl Pts',(-46.1766977413726,32.5039029766724,
-46.7582833333333));
#242616=CARTESIAN_POINT('Ctrl Pts',(-46.1766977413726,31.5404524382932,
-46.69995));
#242617=CARTESIAN_POINT('Ctrl Pts',(-46.1766977413726,30.5770018999139,
-46.6416166666666));
#242618=CARTESIAN_POINT('Ctrl Pts',(-45.3423250998464,30.0952766307242,
-46.5832833333334));
#242619=CARTESIAN_POINT('Ctrl Pts',(-44.5079524583202,29.6135513615346,
-46.52495));
#242620=CARTESIAN_POINT('Ctrl Pts',(-43.6735798167939,30.0952766307242,
-46.4666166666667));
#242621=CARTESIAN_POINT('Ctrl Pts',(-42.8392071752677,30.5770018999139,
-46.4082833333333));
#242622=CARTESIAN_POINT('Ctrl Pts',(-42.8392071752677,31.5404524382931,
-46.34995));
#242623=CARTESIAN_POINT('Origin',(-44.5079524583202,31.5404524382932,-52.920575));
#242624=CARTESIAN_POINT('',(-42.8392071752677,31.5404524382931,-47.74995));
#242625=CARTESIAN_POINT('',(-42.8392071752677,31.5404524382931,-47.5912));
#242626=CARTESIAN_POINT('',(-42.8392071752678,31.5404524382932,-52.920575));
#242627=CARTESIAN_POINT('Ctrl Pts',(-42.8392071752677,31.5404524382931,
-47.5912));
#242628=CARTESIAN_POINT('Ctrl Pts',(-42.8392071752677,32.5039029766724,
-47.5328666666667));
#242629=CARTESIAN_POINT('Ctrl Pts',(-43.6735798167939,32.985628245862,-47.4745333333334));
#242630=CARTESIAN_POINT('Ctrl Pts',(-44.5079524583201,33.4673535150516,
-47.4162));
#242631=CARTESIAN_POINT('Ctrl Pts',(-45.3423250998464,32.985628245862,-47.3578666666667));
#242632=CARTESIAN_POINT('Ctrl Pts',(-46.1766977413726,32.5039029766724,
-47.2995333333334));
#242633=CARTESIAN_POINT('Ctrl Pts',(-46.1766977413726,31.5404524382932,
-47.2412));
#242634=CARTESIAN_POINT('Ctrl Pts',(-46.1766977413726,30.5770018999139,
-47.1828666666667));
#242635=CARTESIAN_POINT('Ctrl Pts',(-45.3423250998464,30.0952766307242,
-47.1245333333333));
#242636=CARTESIAN_POINT('Ctrl Pts',(-44.5079524583202,29.6135513615346,
-47.0662));
#242637=CARTESIAN_POINT('Ctrl Pts',(-43.6735798167939,30.0952766307242,
-47.0078666666667));
#242638=CARTESIAN_POINT('Ctrl Pts',(-42.8392071752677,30.5770018999139,
-46.9495333333334));
#242639=CARTESIAN_POINT('Ctrl Pts',(-42.8392071752677,31.5404524382931,
-46.8912));
#242640=CARTESIAN_POINT('Ctrl Pts',(-42.8392071752677,31.5404524382931,
-47.74995));
#242641=CARTESIAN_POINT('Ctrl Pts',(-42.8392071752677,32.5039029766724,
-47.6916166666667));
#242642=CARTESIAN_POINT('Ctrl Pts',(-43.6735798167939,32.985628245862,-47.6332833333333));
#242643=CARTESIAN_POINT('Ctrl Pts',(-44.5079524583201,33.4673535150516,
-47.57495));
#242644=CARTESIAN_POINT('Ctrl Pts',(-45.3423250998464,32.985628245862,-47.5166166666667));
#242645=CARTESIAN_POINT('Ctrl Pts',(-46.1766977413726,32.5039029766724,
-47.4582833333333));
#242646=CARTESIAN_POINT('Ctrl Pts',(-46.1766977413726,31.5404524382932,
-47.39995));
#242647=CARTESIAN_POINT('Ctrl Pts',(-46.1766977413726,30.5770018999139,
-47.3416166666666));
#242648=CARTESIAN_POINT('Ctrl Pts',(-45.3423250998464,30.0952766307242,
-47.2832833333333));
#242649=CARTESIAN_POINT('Ctrl Pts',(-44.5079524583202,29.6135513615346,
-47.22495));
#242650=CARTESIAN_POINT('Ctrl Pts',(-43.6735798167939,30.0952766307242,
-47.1666166666667));
#242651=CARTESIAN_POINT('Ctrl Pts',(-42.8392071752677,30.5770018999139,
-47.1082833333333));
#242652=CARTESIAN_POINT('Ctrl Pts',(-42.8392071752677,31.5404524382931,
-47.04995));
#242653=CARTESIAN_POINT('Origin',(-44.5079524583202,31.5404524382932,-52.920575));
#242654=CARTESIAN_POINT('',(-42.8392071752677,31.5404524382931,-48.44995));
#242655=CARTESIAN_POINT('',(-42.8392071752677,31.5404524382931,-48.2912));
#242656=CARTESIAN_POINT('',(-42.8392071752678,31.5404524382932,-52.920575));
#242657=CARTESIAN_POINT('Ctrl Pts',(-42.8392071752677,31.5404524382931,
-48.2912));
#242658=CARTESIAN_POINT('Ctrl Pts',(-42.8392071752677,32.5039029766724,
-48.2328666666667));
#242659=CARTESIAN_POINT('Ctrl Pts',(-43.6735798167939,32.985628245862,-48.1745333333334));
#242660=CARTESIAN_POINT('Ctrl Pts',(-44.5079524583201,33.4673535150516,
-48.1162));
#242661=CARTESIAN_POINT('Ctrl Pts',(-45.3423250998464,32.985628245862,-48.0578666666667));
#242662=CARTESIAN_POINT('Ctrl Pts',(-46.1766977413726,32.5039029766724,
-47.9995333333334));
#242663=CARTESIAN_POINT('Ctrl Pts',(-46.1766977413726,31.5404524382932,
-47.9412));
#242664=CARTESIAN_POINT('Ctrl Pts',(-46.1766977413726,30.5770018999139,
-47.8828666666667));
#242665=CARTESIAN_POINT('Ctrl Pts',(-45.3423250998464,30.0952766307242,
-47.8245333333333));
#242666=CARTESIAN_POINT('Ctrl Pts',(-44.5079524583202,29.6135513615346,
-47.7662));
#242667=CARTESIAN_POINT('Ctrl Pts',(-43.6735798167939,30.0952766307242,
-47.7078666666667));
#242668=CARTESIAN_POINT('Ctrl Pts',(-42.8392071752677,30.5770018999139,
-47.6495333333334));
#242669=CARTESIAN_POINT('Ctrl Pts',(-42.8392071752677,31.5404524382931,
-47.5912));
#242670=CARTESIAN_POINT('Ctrl Pts',(-42.8392071752677,31.5404524382931,
-48.44995));
#242671=CARTESIAN_POINT('Ctrl Pts',(-42.8392071752677,32.5039029766724,
-48.3916166666667));
#242672=CARTESIAN_POINT('Ctrl Pts',(-43.6735798167939,32.985628245862,-48.3332833333333));
#242673=CARTESIAN_POINT('Ctrl Pts',(-44.5079524583201,33.4673535150516,
-48.27495));
#242674=CARTESIAN_POINT('Ctrl Pts',(-45.3423250998464,32.985628245862,-48.2166166666667));
#242675=CARTESIAN_POINT('Ctrl Pts',(-46.1766977413726,32.5039029766724,
-48.1582833333333));
#242676=CARTESIAN_POINT('Ctrl Pts',(-46.1766977413726,31.5404524382932,
-48.09995));
#242677=CARTESIAN_POINT('Ctrl Pts',(-46.1766977413726,30.5770018999139,
-48.0416166666667));
#242678=CARTESIAN_POINT('Ctrl Pts',(-45.3423250998464,30.0952766307242,
-47.9832833333334));
#242679=CARTESIAN_POINT('Ctrl Pts',(-44.5079524583202,29.6135513615346,
-47.92495));
#242680=CARTESIAN_POINT('Ctrl Pts',(-43.6735798167939,30.0952766307242,
-47.8666166666667));
#242681=CARTESIAN_POINT('Ctrl Pts',(-42.8392071752677,30.5770018999139,
-47.8082833333333));
#242682=CARTESIAN_POINT('Ctrl Pts',(-42.8392071752677,31.5404524382931,
-47.74995));
#242683=CARTESIAN_POINT('Origin',(-44.5079524583202,31.5404524382932,-52.920575));
#242684=CARTESIAN_POINT('',(-42.8392071752677,31.5404524382931,-49.14995));
#242685=CARTESIAN_POINT('',(-42.8392071752677,31.5404524382931,-48.9912));
#242686=CARTESIAN_POINT('',(-42.8392071752678,31.5404524382932,-52.920575));
#242687=CARTESIAN_POINT('Ctrl Pts',(-42.8392071752677,31.5404524382931,
-48.9912));
#242688=CARTESIAN_POINT('Ctrl Pts',(-42.8392071752677,32.5039029766724,
-48.9328666666667));
#242689=CARTESIAN_POINT('Ctrl Pts',(-43.6735798167939,32.985628245862,-48.8745333333333));
#242690=CARTESIAN_POINT('Ctrl Pts',(-44.5079524583201,33.4673535150516,
-48.8162));
#242691=CARTESIAN_POINT('Ctrl Pts',(-45.3423250998464,32.985628245862,-48.7578666666667));
#242692=CARTESIAN_POINT('Ctrl Pts',(-46.1766977413726,32.5039029766724,
-48.6995333333333));
#242693=CARTESIAN_POINT('Ctrl Pts',(-46.1766977413726,31.5404524382932,
-48.6412));
#242694=CARTESIAN_POINT('Ctrl Pts',(-46.1766977413726,30.5770018999139,
-48.5828666666667));
#242695=CARTESIAN_POINT('Ctrl Pts',(-45.3423250998464,30.0952766307242,
-48.5245333333333));
#242696=CARTESIAN_POINT('Ctrl Pts',(-44.5079524583202,29.6135513615346,
-48.4662));
#242697=CARTESIAN_POINT('Ctrl Pts',(-43.6735798167939,30.0952766307242,
-48.4078666666667));
#242698=CARTESIAN_POINT('Ctrl Pts',(-42.8392071752677,30.5770018999139,
-48.3495333333333));
#242699=CARTESIAN_POINT('Ctrl Pts',(-42.8392071752677,31.5404524382931,
-48.2912));
#242700=CARTESIAN_POINT('Ctrl Pts',(-42.8392071752677,31.5404524382931,
-49.14995));
#242701=CARTESIAN_POINT('Ctrl Pts',(-42.8392071752677,32.5039029766724,
-49.0916166666667));
#242702=CARTESIAN_POINT('Ctrl Pts',(-43.6735798167939,32.985628245862,-49.0332833333333));
#242703=CARTESIAN_POINT('Ctrl Pts',(-44.5079524583201,33.4673535150516,
-48.97495));
#242704=CARTESIAN_POINT('Ctrl Pts',(-45.3423250998464,32.985628245862,-48.9166166666667));
#242705=CARTESIAN_POINT('Ctrl Pts',(-46.1766977413726,32.5039029766724,
-48.8582833333333));
#242706=CARTESIAN_POINT('Ctrl Pts',(-46.1766977413726,31.5404524382932,
-48.79995));
#242707=CARTESIAN_POINT('Ctrl Pts',(-46.1766977413726,30.5770018999139,
-48.7416166666667));
#242708=CARTESIAN_POINT('Ctrl Pts',(-45.3423250998464,30.0952766307242,
-48.6832833333333));
#242709=CARTESIAN_POINT('Ctrl Pts',(-44.5079524583202,29.6135513615346,
-48.62495));
#242710=CARTESIAN_POINT('Ctrl Pts',(-43.6735798167939,30.0952766307242,
-48.5666166666667));
#242711=CARTESIAN_POINT('Ctrl Pts',(-42.8392071752677,30.5770018999139,
-48.5082833333334));
#242712=CARTESIAN_POINT('Ctrl Pts',(-42.8392071752677,31.5404524382931,
-48.44995));
#242713=CARTESIAN_POINT('Origin',(-44.5079524583202,31.5404524382932,-52.920575));
#242714=CARTESIAN_POINT('',(-42.8392071752677,31.5404524382931,-49.84995));
#242715=CARTESIAN_POINT('',(-42.8392071752677,31.5404524382931,-49.6912));
#242716=CARTESIAN_POINT('',(-42.8392071752678,31.5404524382932,-52.920575));
#242717=CARTESIAN_POINT('Ctrl Pts',(-42.8392071752677,31.5404524382931,
-49.6912));
#242718=CARTESIAN_POINT('Ctrl Pts',(-42.8392071752677,32.5039029766724,
-49.6328666666667));
#242719=CARTESIAN_POINT('Ctrl Pts',(-43.6735798167939,32.985628245862,-49.5745333333333));
#242720=CARTESIAN_POINT('Ctrl Pts',(-44.5079524583201,33.4673535150516,
-49.5162));
#242721=CARTESIAN_POINT('Ctrl Pts',(-45.3423250998464,32.985628245862,-49.4578666666667));
#242722=CARTESIAN_POINT('Ctrl Pts',(-46.1766977413726,32.5039029766724,
-49.3995333333333));
#242723=CARTESIAN_POINT('Ctrl Pts',(-46.1766977413726,31.5404524382932,
-49.3412));
#242724=CARTESIAN_POINT('Ctrl Pts',(-46.1766977413726,30.5770018999139,
-49.2828666666667));
#242725=CARTESIAN_POINT('Ctrl Pts',(-45.3423250998464,30.0952766307242,
-49.2245333333333));
#242726=CARTESIAN_POINT('Ctrl Pts',(-44.5079524583202,29.6135513615346,
-49.1662));
#242727=CARTESIAN_POINT('Ctrl Pts',(-43.6735798167939,30.0952766307242,
-49.1078666666667));
#242728=CARTESIAN_POINT('Ctrl Pts',(-42.8392071752677,30.5770018999139,
-49.0495333333334));
#242729=CARTESIAN_POINT('Ctrl Pts',(-42.8392071752677,31.5404524382931,
-48.9912));
#242730=CARTESIAN_POINT('Ctrl Pts',(-42.8392071752677,31.5404524382931,
-49.84995));
#242731=CARTESIAN_POINT('Ctrl Pts',(-42.8392071752677,32.5039029766724,
-49.7916166666667));
#242732=CARTESIAN_POINT('Ctrl Pts',(-43.6735798167939,32.985628245862,-49.7332833333333));
#242733=CARTESIAN_POINT('Ctrl Pts',(-44.5079524583201,33.4673535150516,
-49.67495));
#242734=CARTESIAN_POINT('Ctrl Pts',(-45.3423250998464,32.985628245862,-49.6166166666667));
#242735=CARTESIAN_POINT('Ctrl Pts',(-46.1766977413726,32.5039029766724,
-49.5582833333334));
#242736=CARTESIAN_POINT('Ctrl Pts',(-46.1766977413726,31.5404524382932,
-49.49995));
#242737=CARTESIAN_POINT('Ctrl Pts',(-46.1766977413726,30.5770018999139,
-49.4416166666667));
#242738=CARTESIAN_POINT('Ctrl Pts',(-45.3423250998464,30.0952766307242,
-49.3832833333334));
#242739=CARTESIAN_POINT('Ctrl Pts',(-44.5079524583202,29.6135513615346,
-49.32495));
#242740=CARTESIAN_POINT('Ctrl Pts',(-43.6735798167939,30.0952766307242,
-49.2666166666667));
#242741=CARTESIAN_POINT('Ctrl Pts',(-42.8392071752677,30.5770018999139,
-49.2082833333334));
#242742=CARTESIAN_POINT('Ctrl Pts',(-42.8392071752677,31.5404524382931,
-49.14995));
#242743=CARTESIAN_POINT('Origin',(-44.5079524583202,31.5404524382932,-52.920575));
#242744=CARTESIAN_POINT('',(-42.8392071752677,31.5404524382931,-50.54995));
#242745=CARTESIAN_POINT('',(-42.8392071752677,31.5404524382931,-50.3912));
#242746=CARTESIAN_POINT('',(-42.8392071752678,31.5404524382932,-52.920575));
#242747=CARTESIAN_POINT('Ctrl Pts',(-42.8392071752677,31.5404524382931,
-50.3912));
#242748=CARTESIAN_POINT('Ctrl Pts',(-42.8392071752677,32.5039029766724,
-50.3328666666666));
#242749=CARTESIAN_POINT('Ctrl Pts',(-43.6735798167939,32.985628245862,-50.2745333333333));
#242750=CARTESIAN_POINT('Ctrl Pts',(-44.5079524583201,33.4673535150516,
-50.2162));
#242751=CARTESIAN_POINT('Ctrl Pts',(-45.3423250998464,32.985628245862,-50.1578666666667));
#242752=CARTESIAN_POINT('Ctrl Pts',(-46.1766977413726,32.5039029766724,
-50.0995333333333));
#242753=CARTESIAN_POINT('Ctrl Pts',(-46.1766977413726,31.5404524382932,
-50.0412));
#242754=CARTESIAN_POINT('Ctrl Pts',(-46.1766977413726,30.5770018999139,
-49.9828666666667));
#242755=CARTESIAN_POINT('Ctrl Pts',(-45.3423250998464,30.0952766307242,
-49.9245333333334));
#242756=CARTESIAN_POINT('Ctrl Pts',(-44.5079524583202,29.6135513615346,
-49.8662));
#242757=CARTESIAN_POINT('Ctrl Pts',(-43.6735798167939,30.0952766307242,
-49.8078666666667));
#242758=CARTESIAN_POINT('Ctrl Pts',(-42.8392071752677,30.5770018999139,
-49.7495333333333));
#242759=CARTESIAN_POINT('Ctrl Pts',(-42.8392071752677,31.5404524382931,
-49.6912));
#242760=CARTESIAN_POINT('Ctrl Pts',(-42.8392071752677,31.5404524382931,
-50.54995));
#242761=CARTESIAN_POINT('Ctrl Pts',(-42.8392071752677,32.5039029766724,
-50.4916166666667));
#242762=CARTESIAN_POINT('Ctrl Pts',(-43.6735798167939,32.985628245862,-50.4332833333333));
#242763=CARTESIAN_POINT('Ctrl Pts',(-44.5079524583201,33.4673535150516,
-50.37495));
#242764=CARTESIAN_POINT('Ctrl Pts',(-45.3423250998464,32.985628245862,-50.3166166666667));
#242765=CARTESIAN_POINT('Ctrl Pts',(-46.1766977413726,32.5039029766724,
-50.2582833333334));
#242766=CARTESIAN_POINT('Ctrl Pts',(-46.1766977413726,31.5404524382932,
-50.19995));
#242767=CARTESIAN_POINT('Ctrl Pts',(-46.1766977413726,30.5770018999139,
-50.1416166666667));
#242768=CARTESIAN_POINT('Ctrl Pts',(-45.3423250998464,30.0952766307242,
-50.0832833333333));
#242769=CARTESIAN_POINT('Ctrl Pts',(-44.5079524583202,29.6135513615346,
-50.02495));
#242770=CARTESIAN_POINT('Ctrl Pts',(-43.6735798167939,30.0952766307242,
-49.9666166666667));
#242771=CARTESIAN_POINT('Ctrl Pts',(-42.8392071752677,30.5770018999139,
-49.9082833333334));
#242772=CARTESIAN_POINT('Ctrl Pts',(-42.8392071752677,31.5404524382931,
-49.84995));
#242773=CARTESIAN_POINT('Origin',(-44.5079524583202,31.5404524382932,-52.920575));
#242774=CARTESIAN_POINT('',(-42.8392071752677,31.5404524382931,-51.24995));
#242775=CARTESIAN_POINT('',(-42.8392071752677,31.5404524382931,-51.0912));
#242776=CARTESIAN_POINT('',(-42.8392071752678,31.5404524382932,-52.920575));
#242777=CARTESIAN_POINT('Ctrl Pts',(-42.8392071752677,31.5404524382931,
-51.0912));
#242778=CARTESIAN_POINT('Ctrl Pts',(-42.8392071752677,32.5039029766724,
-51.0328666666667));
#242779=CARTESIAN_POINT('Ctrl Pts',(-43.6735798167939,32.985628245862,-50.9745333333333));
#242780=CARTESIAN_POINT('Ctrl Pts',(-44.5079524583201,33.4673535150516,
-50.9162));
#242781=CARTESIAN_POINT('Ctrl Pts',(-45.3423250998464,32.985628245862,-50.8578666666667));
#242782=CARTESIAN_POINT('Ctrl Pts',(-46.1766977413726,32.5039029766724,
-50.7995333333333));
#242783=CARTESIAN_POINT('Ctrl Pts',(-46.1766977413726,31.5404524382932,
-50.7412));
#242784=CARTESIAN_POINT('Ctrl Pts',(-46.1766977413726,30.5770018999139,
-50.6828666666667));
#242785=CARTESIAN_POINT('Ctrl Pts',(-45.3423250998464,30.0952766307242,
-50.6245333333333));
#242786=CARTESIAN_POINT('Ctrl Pts',(-44.5079524583202,29.6135513615346,
-50.5662));
#242787=CARTESIAN_POINT('Ctrl Pts',(-43.6735798167939,30.0952766307242,
-50.5078666666667));
#242788=CARTESIAN_POINT('Ctrl Pts',(-42.8392071752677,30.5770018999139,
-50.4495333333333));
#242789=CARTESIAN_POINT('Ctrl Pts',(-42.8392071752677,31.5404524382931,
-50.3912));
#242790=CARTESIAN_POINT('Ctrl Pts',(-42.8392071752677,31.5404524382931,
-51.24995));
#242791=CARTESIAN_POINT('Ctrl Pts',(-42.8392071752677,32.5039029766724,
-51.1916166666667));
#242792=CARTESIAN_POINT('Ctrl Pts',(-43.6735798167939,32.985628245862,-51.1332833333333));
#242793=CARTESIAN_POINT('Ctrl Pts',(-44.5079524583201,33.4673535150516,
-51.07495));
#242794=CARTESIAN_POINT('Ctrl Pts',(-45.3423250998464,32.985628245862,-51.0166166666667));
#242795=CARTESIAN_POINT('Ctrl Pts',(-46.1766977413726,32.5039029766724,
-50.9582833333334));
#242796=CARTESIAN_POINT('Ctrl Pts',(-46.1766977413726,31.5404524382932,
-50.89995));
#242797=CARTESIAN_POINT('Ctrl Pts',(-46.1766977413726,30.5770018999139,
-50.8416166666667));
#242798=CARTESIAN_POINT('Ctrl Pts',(-45.3423250998464,30.0952766307242,
-50.7832833333333));
#242799=CARTESIAN_POINT('Ctrl Pts',(-44.5079524583202,29.6135513615346,
-50.72495));
#242800=CARTESIAN_POINT('Ctrl Pts',(-43.6735798167939,30.0952766307242,
-50.6666166666667));
#242801=CARTESIAN_POINT('Ctrl Pts',(-42.8392071752677,30.5770018999139,
-50.6082833333334));
#242802=CARTESIAN_POINT('Ctrl Pts',(-42.8392071752677,31.5404524382931,
-50.54995));
#242803=CARTESIAN_POINT('Origin',(-44.5079524583202,31.5404524382932,-52.920575));
#242804=CARTESIAN_POINT('',(-42.8392071752677,31.5404524382931,-51.94995));
#242805=CARTESIAN_POINT('',(-42.8392071752677,31.5404524382931,-51.7912));
#242806=CARTESIAN_POINT('',(-42.8392071752678,31.5404524382932,-52.920575));
#242807=CARTESIAN_POINT('Ctrl Pts',(-42.8392071752677,31.5404524382931,
-51.7912));
#242808=CARTESIAN_POINT('Ctrl Pts',(-42.8392071752677,32.5039029766724,
-51.7328666666667));
#242809=CARTESIAN_POINT('Ctrl Pts',(-43.6735798167939,32.985628245862,-51.6745333333333));
#242810=CARTESIAN_POINT('Ctrl Pts',(-44.5079524583201,33.4673535150516,
-51.6162));
#242811=CARTESIAN_POINT('Ctrl Pts',(-45.3423250998464,32.985628245862,-51.5578666666667));
#242812=CARTESIAN_POINT('Ctrl Pts',(-46.1766977413726,32.5039029766724,
-51.4995333333333));
#242813=CARTESIAN_POINT('Ctrl Pts',(-46.1766977413726,31.5404524382932,
-51.4412));
#242814=CARTESIAN_POINT('Ctrl Pts',(-46.1766977413726,30.5770018999139,
-51.3828666666667));
#242815=CARTESIAN_POINT('Ctrl Pts',(-45.3423250998464,30.0952766307242,
-51.3245333333334));
#242816=CARTESIAN_POINT('Ctrl Pts',(-44.5079524583202,29.6135513615346,
-51.2662));
#242817=CARTESIAN_POINT('Ctrl Pts',(-43.6735798167939,30.0952766307242,
-51.2078666666667));
#242818=CARTESIAN_POINT('Ctrl Pts',(-42.8392071752677,30.5770018999139,
-51.1495333333333));
#242819=CARTESIAN_POINT('Ctrl Pts',(-42.8392071752677,31.5404524382931,
-51.0912));
#242820=CARTESIAN_POINT('Ctrl Pts',(-42.8392071752677,31.5404524382931,
-51.94995));
#242821=CARTESIAN_POINT('Ctrl Pts',(-42.8392071752677,32.5039029766724,
-51.8916166666666));
#242822=CARTESIAN_POINT('Ctrl Pts',(-43.6735798167939,32.985628245862,-51.8332833333333));
#242823=CARTESIAN_POINT('Ctrl Pts',(-44.5079524583201,33.4673535150516,
-51.77495));
#242824=CARTESIAN_POINT('Ctrl Pts',(-45.3423250998464,32.985628245862,-51.7166166666667));
#242825=CARTESIAN_POINT('Ctrl Pts',(-46.1766977413726,32.5039029766724,
-51.6582833333333));
#242826=CARTESIAN_POINT('Ctrl Pts',(-46.1766977413726,31.5404524382932,
-51.59995));
#242827=CARTESIAN_POINT('Ctrl Pts',(-46.1766977413726,30.5770018999139,
-51.5416166666667));
#242828=CARTESIAN_POINT('Ctrl Pts',(-45.3423250998464,30.0952766307242,
-51.4832833333333));
#242829=CARTESIAN_POINT('Ctrl Pts',(-44.5079524583202,29.6135513615346,
-51.42495));
#242830=CARTESIAN_POINT('Ctrl Pts',(-43.6735798167939,30.0952766307242,
-51.3666166666667));
#242831=CARTESIAN_POINT('Ctrl Pts',(-42.8392071752677,30.5770018999139,
-51.3082833333333));
#242832=CARTESIAN_POINT('Ctrl Pts',(-42.8392071752677,31.5404524382931,
-51.24995));
#242833=CARTESIAN_POINT('Origin',(-44.5079524583202,31.5404524382932,-52.920575));
#242834=CARTESIAN_POINT('',(-42.8392071752677,31.5404524382931,-52.64995));
#242835=CARTESIAN_POINT('',(-42.8392071752677,31.5404524382931,-52.4912));
#242836=CARTESIAN_POINT('',(-42.8392071752678,31.5404524382932,-52.920575));
#242837=CARTESIAN_POINT('',(-44.2755200796091,29.8879736913688,-52.64995));
#242838=CARTESIAN_POINT('Origin',(-44.5079524583202,31.5404524382932,-52.64995));
#242839=CARTESIAN_POINT('Ctrl Pts',(-44.2755200796091,29.8879736913688,
-52.64995));
#242840=CARTESIAN_POINT('Ctrl Pts',(-43.9544082597714,29.9331402535751,
-52.6275001713604));
#242841=CARTESIAN_POINT('Ctrl Pts',(-43.6735798167939,30.0952766307242,
-52.6078666666667));
#242842=CARTESIAN_POINT('Ctrl Pts',(-42.8392071752677,30.5770018999139,
-52.5495333333333));
#242843=CARTESIAN_POINT('Ctrl Pts',(-42.8392071752677,31.5404524382931,
-52.4912));
#242844=CARTESIAN_POINT('Origin',(44.5079524583208,31.5404524382925,-52.920575));
#242845=CARTESIAN_POINT('',(44.5079524583208,29.87170715524,-40.04995));
#242846=CARTESIAN_POINT('',(44.5079524583208,29.87170715524,-39.8912));
#242847=CARTESIAN_POINT('',(44.5079524583209,29.8717071552401,-52.920575));
#242848=CARTESIAN_POINT('',(45.3258959266108,30.0859149508445,-39.8341886424312));
#242849=CARTESIAN_POINT('Ctrl Pts',(44.5079524583208,29.87170715524,-39.8912));
#242850=CARTESIAN_POINT('Ctrl Pts',(44.9449731845273,29.87170715524,-39.8647400265194));
#242851=CARTESIAN_POINT('Ctrl Pts',(45.3258959266108,30.0859149508445,-39.8341886424312));
#242852=CARTESIAN_POINT('',(45.7222548898542,30.3958213079794,-39.958107375254));
#242853=CARTESIAN_POINT('Ctrl Pts',(45.7222548898542,30.3958213079794,-39.9581073752541));
#242854=CARTESIAN_POINT('Ctrl Pts',(45.6645243102482,30.3345767888213,-39.937000346169));
#242855=CARTESIAN_POINT('Ctrl Pts',(45.6022203991058,30.2777619587592,-39.9159679625448));
#242856=CARTESIAN_POINT('Ctrl Pts',(45.4695708655712,30.1740414353458,-39.8744792788644));
#242857=CARTESIAN_POINT('Ctrl Pts',(45.3994027590463,30.1272507252637,-39.8540736326231));
#242858=CARTESIAN_POINT('Ctrl Pts',(45.3258959266108,30.0859149508445,-39.8341886424312));
#242859=CARTESIAN_POINT('Ctrl Pts',(44.5079524583208,29.87170715524,-40.04995));
#242860=CARTESIAN_POINT('Ctrl Pts',(45.22821208842,29.87170715524,-40.0063409682797));
#242861=CARTESIAN_POINT('Ctrl Pts',(45.7222548898542,30.3958213079794,-39.958107375254));
#242862=CARTESIAN_POINT('Origin',(44.5079524583208,31.5404524382925,-52.920575));
#242863=CARTESIAN_POINT('',(44.5079524583208,29.87170715524,-40.74995));
#242864=CARTESIAN_POINT('',(44.5079524583208,29.87170715524,-40.5912));
#242865=CARTESIAN_POINT('',(44.5079524583209,29.8717071552401,-52.920575));
#242866=CARTESIAN_POINT('',(45.9506566843147,32.3790914166432,-40.3575678858381));
#242867=CARTESIAN_POINT('Ctrl Pts',(44.5079524583208,29.87170715524,-40.5912));
#242868=CARTESIAN_POINT('Ctrl Pts',(45.4714029967,29.87170715524,-40.5328666666667));
#242869=CARTESIAN_POINT('Ctrl Pts',(45.9531282658897,30.7060797967663,-40.4745333333334));
#242870=CARTESIAN_POINT('Ctrl Pts',(46.4348535350793,31.5404524382925,-40.4162));
#242871=CARTESIAN_POINT('Ctrl Pts',(45.9531282658897,32.3748250798187,-40.3578666666667));
#242872=CARTESIAN_POINT('Ctrl Pts',(45.9518956264848,32.3769600738953,-40.3577174032382));
#242873=CARTESIAN_POINT('Ctrl Pts',(45.9506566843147,32.3790914166432,-40.3575678858381));
#242874=CARTESIAN_POINT('',(44.4689444465313,33.2087417401602,-40.2388222710491));
#242875=CARTESIAN_POINT('Ctrl Pts',(44.4689444465313,33.2087417401601,-40.2388222710491));
#242876=CARTESIAN_POINT('Ctrl Pts',(44.6155079330583,33.2121686938689,-40.2660845126688));
#242877=CARTESIAN_POINT('Ctrl Pts',(44.762424616678,33.1962849161559,-40.2899383159198));
#242878=CARTESIAN_POINT('Ctrl Pts',(45.0501580461342,33.1256303733612,-40.3294880310719));
#242879=CARTESIAN_POINT('Ctrl Pts',(45.1895314514539,33.0709802808554,-40.3449374316991));
#242880=CARTESIAN_POINT('Ctrl Pts',(45.450238361729,32.9257274737428,-40.3659945174197));
#242881=CARTESIAN_POINT('Ctrl Pts',(45.5702035368922,32.8360707980695,-40.3715333771918));
#242882=CARTESIAN_POINT('Ctrl Pts',(45.6900480373997,32.7184621594941,-40.3719335667203));
#242883=CARTESIAN_POINT('Ctrl Pts',(45.703109839145,32.7052081033347,-40.3718982256622));
#242884=CARTESIAN_POINT('Ctrl Pts',(45.8062679295088,32.596969205699,-40.3709718752492));
#242885=CARTESIAN_POINT('Ctrl Pts',(45.8850264885628,32.4919945408818,-40.3661895545283));
#242886=CARTESIAN_POINT('Ctrl Pts',(45.9506566843147,32.3790914166432,-40.357567885838));
#242887=CARTESIAN_POINT('Ctrl Pts',(44.4689444465313,33.2087417401602,-40.2388222710491));
#242888=CARTESIAN_POINT('Ctrl Pts',(43.5315846498844,33.1868243533108,-40.1813024817086));
#242889=CARTESIAN_POINT('Ctrl Pts',(43.0627766507519,32.3748250798187,-40.1245333333334));
#242890=CARTESIAN_POINT('Ctrl Pts',(42.5810513815623,31.5404524382925,-40.0662));
#242891=CARTESIAN_POINT('Ctrl Pts',(43.0627766507519,30.7060797967663,-40.0078666666667));
#242892=CARTESIAN_POINT('Ctrl Pts',(43.5445019199415,29.87170715524,-39.9495333333333));
#242893=CARTESIAN_POINT('Ctrl Pts',(44.5079524583208,29.87170715524,-39.8912));
#242894=CARTESIAN_POINT('Ctrl Pts',(44.5079524583208,29.87170715524,-40.74995));
#242895=CARTESIAN_POINT('Ctrl Pts',(45.4714029967,29.87170715524,-40.6916166666667));
#242896=CARTESIAN_POINT('Ctrl Pts',(45.9531282658897,30.7060797967663,-40.6332833333334));
#242897=CARTESIAN_POINT('Ctrl Pts',(46.4348535350793,31.5404524382925,-40.57495));
#242898=CARTESIAN_POINT('Ctrl Pts',(45.9531282658897,32.3748250798187,-40.5166166666666));
#242899=CARTESIAN_POINT('Ctrl Pts',(45.4714029967,33.2091977213449,-40.4582833333333));
#242900=CARTESIAN_POINT('Ctrl Pts',(44.5079524583208,33.2091977213449,-40.39995));
#242901=CARTESIAN_POINT('Ctrl Pts',(43.5445019199415,33.2091977213449,-40.3416166666667));
#242902=CARTESIAN_POINT('Ctrl Pts',(43.0627766507519,32.3748250798187,-40.2832833333334));
#242903=CARTESIAN_POINT('Ctrl Pts',(42.5810513815623,31.5404524382925,-40.22495));
#242904=CARTESIAN_POINT('Ctrl Pts',(43.0627766507519,30.7060797967663,-40.1666166666667));
#242905=CARTESIAN_POINT('Ctrl Pts',(43.5445019199415,29.87170715524,-40.1082833333334));
#242906=CARTESIAN_POINT('Ctrl Pts',(44.5079524583208,29.87170715524,-40.04995));
#242907=CARTESIAN_POINT('Origin',(44.5079524583208,31.5404524382925,-52.920575));
#242908=CARTESIAN_POINT('',(44.5079524583208,29.87170715524,-41.44995));
#242909=CARTESIAN_POINT('',(44.5079524583208,29.87170715524,-41.2912));
#242910=CARTESIAN_POINT('',(44.5079524583209,29.8717071552401,-52.920575));
#242911=CARTESIAN_POINT('Ctrl Pts',(44.5079524583208,29.87170715524,-41.2912));
#242912=CARTESIAN_POINT('Ctrl Pts',(45.4714029967,29.87170715524,-41.2328666666667));
#242913=CARTESIAN_POINT('Ctrl Pts',(45.9531282658897,30.7060797967663,-41.1745333333334));
#242914=CARTESIAN_POINT('Ctrl Pts',(46.4348535350793,31.5404524382925,-41.1162));
#242915=CARTESIAN_POINT('Ctrl Pts',(45.9531282658897,32.3748250798187,-41.0578666666667));
#242916=CARTESIAN_POINT('Ctrl Pts',(45.4714029967,33.2091977213449,-40.9995333333333));
#242917=CARTESIAN_POINT('Ctrl Pts',(44.5079524583208,33.2091977213449,-40.9412));
#242918=CARTESIAN_POINT('Ctrl Pts',(43.5445019199415,33.2091977213449,-40.8828666666667));
#242919=CARTESIAN_POINT('Ctrl Pts',(43.0627766507519,32.3748250798187,-40.8245333333333));
#242920=CARTESIAN_POINT('Ctrl Pts',(42.5810513815623,31.5404524382925,-40.7662));
#242921=CARTESIAN_POINT('Ctrl Pts',(43.0627766507519,30.7060797967663,-40.7078666666667));
#242922=CARTESIAN_POINT('Ctrl Pts',(43.5445019199415,29.87170715524,-40.6495333333333));
#242923=CARTESIAN_POINT('Ctrl Pts',(44.5079524583208,29.87170715524,-40.5912));
#242924=CARTESIAN_POINT('Ctrl Pts',(44.5079524583208,29.87170715524,-41.44995));
#242925=CARTESIAN_POINT('Ctrl Pts',(45.4714029967,29.87170715524,-41.3916166666667));
#242926=CARTESIAN_POINT('Ctrl Pts',(45.9531282658897,30.7060797967663,-41.3332833333334));
#242927=CARTESIAN_POINT('Ctrl Pts',(46.4348535350793,31.5404524382925,-41.27495));
#242928=CARTESIAN_POINT('Ctrl Pts',(45.9531282658897,32.3748250798187,-41.2166166666667));
#242929=CARTESIAN_POINT('Ctrl Pts',(45.4714029967,33.2091977213449,-41.1582833333333));
#242930=CARTESIAN_POINT('Ctrl Pts',(44.5079524583208,33.2091977213449,-41.09995));
#242931=CARTESIAN_POINT('Ctrl Pts',(43.5445019199415,33.2091977213449,-41.0416166666667));
#242932=CARTESIAN_POINT('Ctrl Pts',(43.0627766507519,32.3748250798187,-40.9832833333333));
#242933=CARTESIAN_POINT('Ctrl Pts',(42.5810513815623,31.5404524382925,-40.92495));
#242934=CARTESIAN_POINT('Ctrl Pts',(43.0627766507519,30.7060797967663,-40.8666166666667));
#242935=CARTESIAN_POINT('Ctrl Pts',(43.5445019199415,29.87170715524,-40.8082833333334));
#242936=CARTESIAN_POINT('Ctrl Pts',(44.5079524583208,29.87170715524,-40.74995));
#242937=CARTESIAN_POINT('Origin',(44.5079524583208,31.5404524382925,-52.920575));
#242938=CARTESIAN_POINT('',(44.5079524583208,29.87170715524,-42.14995));
#242939=CARTESIAN_POINT('',(44.5079524583208,29.87170715524,-41.9912));
#242940=CARTESIAN_POINT('',(44.5079524583209,29.8717071552401,-52.920575));
#242941=CARTESIAN_POINT('Ctrl Pts',(44.5079524583208,29.87170715524,-41.9912));
#242942=CARTESIAN_POINT('Ctrl Pts',(45.4714029967,29.87170715524,-41.9328666666667));
#242943=CARTESIAN_POINT('Ctrl Pts',(45.9531282658897,30.7060797967663,-41.8745333333334));
#242944=CARTESIAN_POINT('Ctrl Pts',(46.4348535350793,31.5404524382925,-41.8162));
#242945=CARTESIAN_POINT('Ctrl Pts',(45.9531282658897,32.3748250798187,-41.7578666666667));
#242946=CARTESIAN_POINT('Ctrl Pts',(45.4714029967,33.2091977213449,-41.6995333333334));
#242947=CARTESIAN_POINT('Ctrl Pts',(44.5079524583208,33.2091977213449,-41.6412));
#242948=CARTESIAN_POINT('Ctrl Pts',(43.5445019199415,33.2091977213449,-41.5828666666667));
#242949=CARTESIAN_POINT('Ctrl Pts',(43.0627766507519,32.3748250798187,-41.5245333333334));
#242950=CARTESIAN_POINT('Ctrl Pts',(42.5810513815623,31.5404524382925,-41.4662));
#242951=CARTESIAN_POINT('Ctrl Pts',(43.0627766507519,30.7060797967663,-41.4078666666667));
#242952=CARTESIAN_POINT('Ctrl Pts',(43.5445019199415,29.87170715524,-41.3495333333333));
#242953=CARTESIAN_POINT('Ctrl Pts',(44.5079524583208,29.87170715524,-41.2912));
#242954=CARTESIAN_POINT('Ctrl Pts',(44.5079524583208,29.87170715524,-42.14995));
#242955=CARTESIAN_POINT('Ctrl Pts',(45.4714029967,29.87170715524,-42.0916166666667));
#242956=CARTESIAN_POINT('Ctrl Pts',(45.9531282658897,30.7060797967663,-42.0332833333334));
#242957=CARTESIAN_POINT('Ctrl Pts',(46.4348535350793,31.5404524382925,-41.97495));
#242958=CARTESIAN_POINT('Ctrl Pts',(45.9531282658897,32.3748250798187,-41.9166166666666));
#242959=CARTESIAN_POINT('Ctrl Pts',(45.4714029967,33.2091977213449,-41.8582833333333));
#242960=CARTESIAN_POINT('Ctrl Pts',(44.5079524583208,33.2091977213449,-41.79995));
#242961=CARTESIAN_POINT('Ctrl Pts',(43.5445019199415,33.2091977213449,-41.7416166666666));
#242962=CARTESIAN_POINT('Ctrl Pts',(43.0627766507519,32.3748250798187,-41.6832833333333));
#242963=CARTESIAN_POINT('Ctrl Pts',(42.5810513815623,31.5404524382925,-41.62495));
#242964=CARTESIAN_POINT('Ctrl Pts',(43.0627766507519,30.7060797967663,-41.5666166666667));
#242965=CARTESIAN_POINT('Ctrl Pts',(43.5445019199415,29.87170715524,-41.5082833333334));
#242966=CARTESIAN_POINT('Ctrl Pts',(44.5079524583208,29.87170715524,-41.44995));
#242967=CARTESIAN_POINT('Origin',(44.5079524583208,31.5404524382925,-52.920575));
#242968=CARTESIAN_POINT('',(44.5079524583208,29.87170715524,-42.84995));
#242969=CARTESIAN_POINT('',(44.5079524583208,29.87170715524,-42.6912));
#242970=CARTESIAN_POINT('',(44.5079524583209,29.8717071552401,-52.920575));
#242971=CARTESIAN_POINT('Ctrl Pts',(44.5079524583208,29.87170715524,-42.6912));
#242972=CARTESIAN_POINT('Ctrl Pts',(45.4714029967,29.87170715524,-42.6328666666667));
#242973=CARTESIAN_POINT('Ctrl Pts',(45.9531282658897,30.7060797967663,-42.5745333333333));
#242974=CARTESIAN_POINT('Ctrl Pts',(46.4348535350793,31.5404524382925,-42.5162));
#242975=CARTESIAN_POINT('Ctrl Pts',(45.9531282658897,32.3748250798187,-42.4578666666667));
#242976=CARTESIAN_POINT('Ctrl Pts',(45.4714029967,33.2091977213449,-42.3995333333334));
#242977=CARTESIAN_POINT('Ctrl Pts',(44.5079524583208,33.2091977213449,-42.3412));
#242978=CARTESIAN_POINT('Ctrl Pts',(43.5445019199415,33.2091977213449,-42.2828666666667));
#242979=CARTESIAN_POINT('Ctrl Pts',(43.0627766507519,32.3748250798187,-42.2245333333333));
#242980=CARTESIAN_POINT('Ctrl Pts',(42.5810513815623,31.5404524382925,-42.1662));
#242981=CARTESIAN_POINT('Ctrl Pts',(43.0627766507519,30.7060797967663,-42.1078666666667));
#242982=CARTESIAN_POINT('Ctrl Pts',(43.5445019199415,29.87170715524,-42.0495333333334));
#242983=CARTESIAN_POINT('Ctrl Pts',(44.5079524583208,29.87170715524,-41.9912));
#242984=CARTESIAN_POINT('Ctrl Pts',(44.5079524583208,29.87170715524,-42.84995));
#242985=CARTESIAN_POINT('Ctrl Pts',(45.4714029967,29.87170715524,-42.7916166666667));
#242986=CARTESIAN_POINT('Ctrl Pts',(45.9531282658897,30.7060797967663,-42.7332833333334));
#242987=CARTESIAN_POINT('Ctrl Pts',(46.4348535350793,31.5404524382925,-42.67495));
#242988=CARTESIAN_POINT('Ctrl Pts',(45.9531282658897,32.3748250798187,-42.6166166666667));
#242989=CARTESIAN_POINT('Ctrl Pts',(45.4714029967,33.2091977213449,-42.5582833333333));
#242990=CARTESIAN_POINT('Ctrl Pts',(44.5079524583208,33.2091977213449,-42.49995));
#242991=CARTESIAN_POINT('Ctrl Pts',(43.5445019199415,33.2091977213449,-42.4416166666666));
#242992=CARTESIAN_POINT('Ctrl Pts',(43.0627766507519,32.3748250798187,-42.3832833333333));
#242993=CARTESIAN_POINT('Ctrl Pts',(42.5810513815623,31.5404524382925,-42.32495));
#242994=CARTESIAN_POINT('Ctrl Pts',(43.0627766507519,30.7060797967663,-42.2666166666667));
#242995=CARTESIAN_POINT('Ctrl Pts',(43.5445019199415,29.87170715524,-42.2082833333333));
#242996=CARTESIAN_POINT('Ctrl Pts',(44.5079524583208,29.87170715524,-42.14995));
#242997=CARTESIAN_POINT('Origin',(44.5079524583208,31.5404524382925,-52.920575));
#242998=CARTESIAN_POINT('',(44.5079524583208,29.87170715524,-43.54995));
#242999=CARTESIAN_POINT('',(44.5079524583208,29.87170715524,-43.3912));
#243000=CARTESIAN_POINT('',(44.5079524583209,29.8717071552401,-52.920575));
#243001=CARTESIAN_POINT('Ctrl Pts',(44.5079524583208,29.87170715524,-43.3912));
#243002=CARTESIAN_POINT('Ctrl Pts',(45.4714029967,29.87170715524,-43.3328666666667));
#243003=CARTESIAN_POINT('Ctrl Pts',(45.9531282658897,30.7060797967663,-43.2745333333334));
#243004=CARTESIAN_POINT('Ctrl Pts',(46.4348535350793,31.5404524382925,-43.2162));
#243005=CARTESIAN_POINT('Ctrl Pts',(45.9531282658897,32.3748250798187,-43.1578666666667));
#243006=CARTESIAN_POINT('Ctrl Pts',(45.4714029967,33.2091977213449,-43.0995333333334));
#243007=CARTESIAN_POINT('Ctrl Pts',(44.5079524583208,33.2091977213449,-43.0412));
#243008=CARTESIAN_POINT('Ctrl Pts',(43.5445019199415,33.2091977213449,-42.9828666666667));
#243009=CARTESIAN_POINT('Ctrl Pts',(43.0627766507519,32.3748250798187,-42.9245333333334));
#243010=CARTESIAN_POINT('Ctrl Pts',(42.5810513815623,31.5404524382925,-42.8662));
#243011=CARTESIAN_POINT('Ctrl Pts',(43.0627766507519,30.7060797967663,-42.8078666666667));
#243012=CARTESIAN_POINT('Ctrl Pts',(43.5445019199415,29.87170715524,-42.7495333333334));
#243013=CARTESIAN_POINT('Ctrl Pts',(44.5079524583208,29.87170715524,-42.6912));
#243014=CARTESIAN_POINT('Ctrl Pts',(44.5079524583208,29.87170715524,-43.54995));
#243015=CARTESIAN_POINT('Ctrl Pts',(45.4714029967,29.87170715524,-43.4916166666667));
#243016=CARTESIAN_POINT('Ctrl Pts',(45.9531282658897,30.7060797967663,-43.4332833333333));
#243017=CARTESIAN_POINT('Ctrl Pts',(46.4348535350793,31.5404524382925,-43.37495));
#243018=CARTESIAN_POINT('Ctrl Pts',(45.9531282658897,32.3748250798187,-43.3166166666667));
#243019=CARTESIAN_POINT('Ctrl Pts',(45.4714029967,33.2091977213449,-43.2582833333333));
#243020=CARTESIAN_POINT('Ctrl Pts',(44.5079524583208,33.2091977213449,-43.19995));
#243021=CARTESIAN_POINT('Ctrl Pts',(43.5445019199415,33.2091977213449,-43.1416166666666));
#243022=CARTESIAN_POINT('Ctrl Pts',(43.0627766507519,32.3748250798187,-43.0832833333333));
#243023=CARTESIAN_POINT('Ctrl Pts',(42.5810513815623,31.5404524382925,-43.02495));
#243024=CARTESIAN_POINT('Ctrl Pts',(43.0627766507519,30.7060797967663,-42.9666166666667));
#243025=CARTESIAN_POINT('Ctrl Pts',(43.5445019199415,29.87170715524,-42.9082833333333));
#243026=CARTESIAN_POINT('Ctrl Pts',(44.5079524583208,29.87170715524,-42.84995));
#243027=CARTESIAN_POINT('Origin',(44.5079524583208,31.5404524382925,-52.920575));
#243028=CARTESIAN_POINT('',(44.5079524583208,29.87170715524,-44.24995));
#243029=CARTESIAN_POINT('',(44.5079524583208,29.87170715524,-44.0912));
#243030=CARTESIAN_POINT('',(44.5079524583209,29.8717071552401,-52.920575));
#243031=CARTESIAN_POINT('Ctrl Pts',(44.5079524583208,29.87170715524,-44.0912));
#243032=CARTESIAN_POINT('Ctrl Pts',(45.4714029967,29.87170715524,-44.0328666666667));
#243033=CARTESIAN_POINT('Ctrl Pts',(45.9531282658897,30.7060797967663,-43.9745333333333));
#243034=CARTESIAN_POINT('Ctrl Pts',(46.4348535350793,31.5404524382925,-43.9162));
#243035=CARTESIAN_POINT('Ctrl Pts',(45.9531282658897,32.3748250798187,-43.8578666666667));
#243036=CARTESIAN_POINT('Ctrl Pts',(45.4714029967,33.2091977213449,-43.7995333333334));
#243037=CARTESIAN_POINT('Ctrl Pts',(44.5079524583208,33.2091977213449,-43.7412));
#243038=CARTESIAN_POINT('Ctrl Pts',(43.5445019199415,33.2091977213449,-43.6828666666667));
#243039=CARTESIAN_POINT('Ctrl Pts',(43.0627766507519,32.3748250798187,-43.6245333333333));
#243040=CARTESIAN_POINT('Ctrl Pts',(42.5810513815623,31.5404524382925,-43.5662));
#243041=CARTESIAN_POINT('Ctrl Pts',(43.0627766507519,30.7060797967663,-43.5078666666667));
#243042=CARTESIAN_POINT('Ctrl Pts',(43.5445019199415,29.87170715524,-43.4495333333334));
#243043=CARTESIAN_POINT('Ctrl Pts',(44.5079524583208,29.87170715524,-43.3912));
#243044=CARTESIAN_POINT('Ctrl Pts',(44.5079524583208,29.87170715524,-44.24995));
#243045=CARTESIAN_POINT('Ctrl Pts',(45.4714029967,29.87170715524,-44.1916166666667));
#243046=CARTESIAN_POINT('Ctrl Pts',(45.9531282658897,30.7060797967663,-44.1332833333334));
#243047=CARTESIAN_POINT('Ctrl Pts',(46.4348535350793,31.5404524382925,-44.07495));
#243048=CARTESIAN_POINT('Ctrl Pts',(45.9531282658897,32.3748250798187,-44.0166166666667));
#243049=CARTESIAN_POINT('Ctrl Pts',(45.4714029967,33.2091977213449,-43.9582833333334));
#243050=CARTESIAN_POINT('Ctrl Pts',(44.5079524583208,33.2091977213449,-43.89995));
#243051=CARTESIAN_POINT('Ctrl Pts',(43.5445019199415,33.2091977213449,-43.8416166666667));
#243052=CARTESIAN_POINT('Ctrl Pts',(43.0627766507519,32.3748250798187,-43.7832833333334));
#243053=CARTESIAN_POINT('Ctrl Pts',(42.5810513815623,31.5404524382925,-43.72495));
#243054=CARTESIAN_POINT('Ctrl Pts',(43.0627766507519,30.7060797967663,-43.6666166666667));
#243055=CARTESIAN_POINT('Ctrl Pts',(43.5445019199415,29.87170715524,-43.6082833333333));
#243056=CARTESIAN_POINT('Ctrl Pts',(44.5079524583208,29.87170715524,-43.54995));
#243057=CARTESIAN_POINT('Origin',(44.5079524583208,31.5404524382925,-52.920575));
#243058=CARTESIAN_POINT('',(44.5079524583208,29.87170715524,-44.94995));
#243059=CARTESIAN_POINT('',(44.5079524583208,29.87170715524,-44.7912));
#243060=CARTESIAN_POINT('',(44.5079524583209,29.8717071552401,-52.920575));
#243061=CARTESIAN_POINT('Ctrl Pts',(44.5079524583208,29.87170715524,-44.7912));
#243062=CARTESIAN_POINT('Ctrl Pts',(45.4714029967,29.87170715524,-44.7328666666667));
#243063=CARTESIAN_POINT('Ctrl Pts',(45.9531282658897,30.7060797967663,-44.6745333333334));
#243064=CARTESIAN_POINT('Ctrl Pts',(46.4348535350793,31.5404524382925,-44.6162));
#243065=CARTESIAN_POINT('Ctrl Pts',(45.9531282658897,32.3748250798187,-44.5578666666667));
#243066=CARTESIAN_POINT('Ctrl Pts',(45.4714029967,33.2091977213449,-44.4995333333333));
#243067=CARTESIAN_POINT('Ctrl Pts',(44.5079524583208,33.2091977213449,-44.4412));
#243068=CARTESIAN_POINT('Ctrl Pts',(43.5445019199415,33.2091977213449,-44.3828666666667));
#243069=CARTESIAN_POINT('Ctrl Pts',(43.0627766507519,32.3748250798187,-44.3245333333334));
#243070=CARTESIAN_POINT('Ctrl Pts',(42.5810513815623,31.5404524382925,-44.2662));
#243071=CARTESIAN_POINT('Ctrl Pts',(43.0627766507519,30.7060797967663,-44.2078666666667));
#243072=CARTESIAN_POINT('Ctrl Pts',(43.5445019199415,29.87170715524,-44.1495333333334));
#243073=CARTESIAN_POINT('Ctrl Pts',(44.5079524583208,29.87170715524,-44.0912));
#243074=CARTESIAN_POINT('Ctrl Pts',(44.5079524583208,29.87170715524,-44.94995));
#243075=CARTESIAN_POINT('Ctrl Pts',(45.4714029967,29.87170715524,-44.8916166666667));
#243076=CARTESIAN_POINT('Ctrl Pts',(45.9531282658897,30.7060797967663,-44.8332833333334));
#243077=CARTESIAN_POINT('Ctrl Pts',(46.4348535350793,31.5404524382925,-44.77495));
#243078=CARTESIAN_POINT('Ctrl Pts',(45.9531282658897,32.3748250798187,-44.7166166666667));
#243079=CARTESIAN_POINT('Ctrl Pts',(45.4714029967,33.2091977213449,-44.6582833333333));
#243080=CARTESIAN_POINT('Ctrl Pts',(44.5079524583208,33.2091977213449,-44.59995));
#243081=CARTESIAN_POINT('Ctrl Pts',(43.5445019199415,33.2091977213449,-44.5416166666667));
#243082=CARTESIAN_POINT('Ctrl Pts',(43.0627766507519,32.3748250798187,-44.4832833333334));
#243083=CARTESIAN_POINT('Ctrl Pts',(42.5810513815623,31.5404524382925,-44.42495));
#243084=CARTESIAN_POINT('Ctrl Pts',(43.0627766507519,30.7060797967663,-44.3666166666667));
#243085=CARTESIAN_POINT('Ctrl Pts',(43.5445019199415,29.87170715524,-44.3082833333334));
#243086=CARTESIAN_POINT('Ctrl Pts',(44.5079524583208,29.87170715524,-44.24995));
#243087=CARTESIAN_POINT('Origin',(44.5079524583208,31.5404524382925,-52.920575));
#243088=CARTESIAN_POINT('',(44.5079524583208,29.87170715524,-45.64995));
#243089=CARTESIAN_POINT('',(44.5079524583208,29.87170715524,-45.4912));
#243090=CARTESIAN_POINT('',(44.5079524583209,29.8717071552401,-52.920575));
#243091=CARTESIAN_POINT('Ctrl Pts',(44.5079524583208,29.87170715524,-45.4912));
#243092=CARTESIAN_POINT('Ctrl Pts',(45.4714029967,29.87170715524,-45.4328666666666));
#243093=CARTESIAN_POINT('Ctrl Pts',(45.9531282658897,30.7060797967663,-45.3745333333333));
#243094=CARTESIAN_POINT('Ctrl Pts',(46.4348535350793,31.5404524382925,-45.3162));
#243095=CARTESIAN_POINT('Ctrl Pts',(45.9531282658897,32.3748250798187,-45.2578666666667));
#243096=CARTESIAN_POINT('Ctrl Pts',(45.4714029967,33.2091977213449,-45.1995333333333));
#243097=CARTESIAN_POINT('Ctrl Pts',(44.5079524583208,33.2091977213449,-45.1412));
#243098=CARTESIAN_POINT('Ctrl Pts',(43.5445019199415,33.2091977213449,-45.0828666666667));
#243099=CARTESIAN_POINT('Ctrl Pts',(43.0627766507519,32.3748250798187,-45.0245333333333));
#243100=CARTESIAN_POINT('Ctrl Pts',(42.5810513815623,31.5404524382925,-44.9662));
#243101=CARTESIAN_POINT('Ctrl Pts',(43.0627766507519,30.7060797967663,-44.9078666666666));
#243102=CARTESIAN_POINT('Ctrl Pts',(43.5445019199415,29.87170715524,-44.8495333333333));
#243103=CARTESIAN_POINT('Ctrl Pts',(44.5079524583208,29.87170715524,-44.7912));
#243104=CARTESIAN_POINT('Ctrl Pts',(44.5079524583208,29.87170715524,-45.64995));
#243105=CARTESIAN_POINT('Ctrl Pts',(45.4714029967,29.87170715524,-45.5916166666667));
#243106=CARTESIAN_POINT('Ctrl Pts',(45.9531282658897,30.7060797967663,-45.5332833333333));
#243107=CARTESIAN_POINT('Ctrl Pts',(46.4348535350793,31.5404524382925,-45.47495));
#243108=CARTESIAN_POINT('Ctrl Pts',(45.9531282658897,32.3748250798187,-45.4166166666667));
#243109=CARTESIAN_POINT('Ctrl Pts',(45.4714029967,33.2091977213449,-45.3582833333334));
#243110=CARTESIAN_POINT('Ctrl Pts',(44.5079524583208,33.2091977213449,-45.29995));
#243111=CARTESIAN_POINT('Ctrl Pts',(43.5445019199415,33.2091977213449,-45.2416166666667));
#243112=CARTESIAN_POINT('Ctrl Pts',(43.0627766507519,32.3748250798187,-45.1832833333333));
#243113=CARTESIAN_POINT('Ctrl Pts',(42.5810513815623,31.5404524382925,-45.12495));
#243114=CARTESIAN_POINT('Ctrl Pts',(43.0627766507519,30.7060797967663,-45.0666166666667));
#243115=CARTESIAN_POINT('Ctrl Pts',(43.5445019199415,29.87170715524,-45.0082833333334));
#243116=CARTESIAN_POINT('Ctrl Pts',(44.5079524583208,29.87170715524,-44.94995));
#243117=CARTESIAN_POINT('Origin',(44.5079524583208,31.5404524382925,-52.920575));
#243118=CARTESIAN_POINT('',(44.5079524583208,29.87170715524,-46.34995));
#243119=CARTESIAN_POINT('',(44.5079524583208,29.87170715524,-46.1912));
#243120=CARTESIAN_POINT('',(44.5079524583209,29.8717071552401,-52.920575));
#243121=CARTESIAN_POINT('Ctrl Pts',(44.5079524583208,29.87170715524,-46.1912));
#243122=CARTESIAN_POINT('Ctrl Pts',(45.4714029967,29.87170715524,-46.1328666666667));
#243123=CARTESIAN_POINT('Ctrl Pts',(45.9531282658897,30.7060797967663,-46.0745333333334));
#243124=CARTESIAN_POINT('Ctrl Pts',(46.4348535350793,31.5404524382925,-46.0162));
#243125=CARTESIAN_POINT('Ctrl Pts',(45.9531282658897,32.3748250798187,-45.9578666666667));
#243126=CARTESIAN_POINT('Ctrl Pts',(45.4714029967,33.2091977213449,-45.8995333333333));
#243127=CARTESIAN_POINT('Ctrl Pts',(44.5079524583208,33.2091977213449,-45.8412));
#243128=CARTESIAN_POINT('Ctrl Pts',(43.5445019199415,33.2091977213449,-45.7828666666667));
#243129=CARTESIAN_POINT('Ctrl Pts',(43.0627766507519,32.3748250798187,-45.7245333333333));
#243130=CARTESIAN_POINT('Ctrl Pts',(42.5810513815623,31.5404524382925,-45.6662));
#243131=CARTESIAN_POINT('Ctrl Pts',(43.0627766507519,30.7060797967663,-45.6078666666667));
#243132=CARTESIAN_POINT('Ctrl Pts',(43.5445019199415,29.87170715524,-45.5495333333333));
#243133=CARTESIAN_POINT('Ctrl Pts',(44.5079524583208,29.87170715524,-45.4912));
#243134=CARTESIAN_POINT('Ctrl Pts',(44.5079524583208,29.87170715524,-46.34995));
#243135=CARTESIAN_POINT('Ctrl Pts',(45.4714029967,29.87170715524,-46.2916166666667));
#243136=CARTESIAN_POINT('Ctrl Pts',(45.9531282658897,30.7060797967663,-46.2332833333334));
#243137=CARTESIAN_POINT('Ctrl Pts',(46.4348535350793,31.5404524382925,-46.17495));
#243138=CARTESIAN_POINT('Ctrl Pts',(45.9531282658897,32.3748250798187,-46.1166166666667));
#243139=CARTESIAN_POINT('Ctrl Pts',(45.4714029967,33.2091977213449,-46.0582833333333));
#243140=CARTESIAN_POINT('Ctrl Pts',(44.5079524583208,33.2091977213449,-45.99995));
#243141=CARTESIAN_POINT('Ctrl Pts',(43.5445019199415,33.2091977213449,-45.9416166666667));
#243142=CARTESIAN_POINT('Ctrl Pts',(43.0627766507519,32.3748250798187,-45.8832833333333));
#243143=CARTESIAN_POINT('Ctrl Pts',(42.5810513815623,31.5404524382925,-45.82495));
#243144=CARTESIAN_POINT('Ctrl Pts',(43.0627766507519,30.7060797967663,-45.7666166666667));
#243145=CARTESIAN_POINT('Ctrl Pts',(43.5445019199415,29.87170715524,-45.7082833333333));
#243146=CARTESIAN_POINT('Ctrl Pts',(44.5079524583208,29.87170715524,-45.64995));
#243147=CARTESIAN_POINT('Origin',(44.5079524583208,31.5404524382925,-52.920575));
#243148=CARTESIAN_POINT('',(44.5079524583208,29.87170715524,-47.04995));
#243149=CARTESIAN_POINT('',(44.5079524583208,29.87170715524,-46.8912));
#243150=CARTESIAN_POINT('',(44.5079524583209,29.8717071552401,-52.920575));
#243151=CARTESIAN_POINT('Ctrl Pts',(44.5079524583208,29.87170715524,-46.8912));
#243152=CARTESIAN_POINT('Ctrl Pts',(45.4714029967,29.87170715524,-46.8328666666667));
#243153=CARTESIAN_POINT('Ctrl Pts',(45.9531282658897,30.7060797967663,-46.7745333333333));
#243154=CARTESIAN_POINT('Ctrl Pts',(46.4348535350793,31.5404524382925,-46.7162));
#243155=CARTESIAN_POINT('Ctrl Pts',(45.9531282658897,32.3748250798187,-46.6578666666667));
#243156=CARTESIAN_POINT('Ctrl Pts',(45.4714029967,33.2091977213449,-46.5995333333333));
#243157=CARTESIAN_POINT('Ctrl Pts',(44.5079524583208,33.2091977213449,-46.5412));
#243158=CARTESIAN_POINT('Ctrl Pts',(43.5445019199415,33.2091977213449,-46.4828666666667));
#243159=CARTESIAN_POINT('Ctrl Pts',(43.0627766507519,32.3748250798187,-46.4245333333333));
#243160=CARTESIAN_POINT('Ctrl Pts',(42.5810513815623,31.5404524382925,-46.3662));
#243161=CARTESIAN_POINT('Ctrl Pts',(43.0627766507519,30.7060797967663,-46.3078666666667));
#243162=CARTESIAN_POINT('Ctrl Pts',(43.5445019199415,29.87170715524,-46.2495333333334));
#243163=CARTESIAN_POINT('Ctrl Pts',(44.5079524583208,29.87170715524,-46.1912));
#243164=CARTESIAN_POINT('Ctrl Pts',(44.5079524583208,29.87170715524,-47.04995));
#243165=CARTESIAN_POINT('Ctrl Pts',(45.4714029967,29.87170715524,-46.9916166666667));
#243166=CARTESIAN_POINT('Ctrl Pts',(45.9531282658897,30.7060797967663,-46.9332833333333));
#243167=CARTESIAN_POINT('Ctrl Pts',(46.4348535350793,31.5404524382925,-46.87495));
#243168=CARTESIAN_POINT('Ctrl Pts',(45.9531282658897,32.3748250798187,-46.8166166666667));
#243169=CARTESIAN_POINT('Ctrl Pts',(45.4714029967,33.2091977213449,-46.7582833333333));
#243170=CARTESIAN_POINT('Ctrl Pts',(44.5079524583208,33.2091977213449,-46.69995));
#243171=CARTESIAN_POINT('Ctrl Pts',(43.5445019199415,33.2091977213449,-46.6416166666666));
#243172=CARTESIAN_POINT('Ctrl Pts',(43.0627766507519,32.3748250798187,-46.5832833333334));
#243173=CARTESIAN_POINT('Ctrl Pts',(42.5810513815623,31.5404524382925,-46.52495));
#243174=CARTESIAN_POINT('Ctrl Pts',(43.0627766507519,30.7060797967663,-46.4666166666667));
#243175=CARTESIAN_POINT('Ctrl Pts',(43.5445019199415,29.87170715524,-46.4082833333333));
#243176=CARTESIAN_POINT('Ctrl Pts',(44.5079524583208,29.87170715524,-46.34995));
#243177=CARTESIAN_POINT('Origin',(44.5079524583208,31.5404524382925,-52.920575));
#243178=CARTESIAN_POINT('',(44.5079524583208,29.87170715524,-47.74995));
#243179=CARTESIAN_POINT('',(44.5079524583208,29.87170715524,-47.5912));
#243180=CARTESIAN_POINT('',(44.5079524583209,29.8717071552401,-52.920575));
#243181=CARTESIAN_POINT('Ctrl Pts',(44.5079524583208,29.87170715524,-47.5912));
#243182=CARTESIAN_POINT('Ctrl Pts',(45.4714029967,29.87170715524,-47.5328666666667));
#243183=CARTESIAN_POINT('Ctrl Pts',(45.9531282658897,30.7060797967663,-47.4745333333334));
#243184=CARTESIAN_POINT('Ctrl Pts',(46.4348535350793,31.5404524382925,-47.4162));
#243185=CARTESIAN_POINT('Ctrl Pts',(45.9531282658897,32.3748250798187,-47.3578666666667));
#243186=CARTESIAN_POINT('Ctrl Pts',(45.4714029967,33.2091977213449,-47.2995333333334));
#243187=CARTESIAN_POINT('Ctrl Pts',(44.5079524583208,33.2091977213449,-47.2412));
#243188=CARTESIAN_POINT('Ctrl Pts',(43.5445019199415,33.2091977213449,-47.1828666666667));
#243189=CARTESIAN_POINT('Ctrl Pts',(43.0627766507519,32.3748250798187,-47.1245333333333));
#243190=CARTESIAN_POINT('Ctrl Pts',(42.5810513815623,31.5404524382925,-47.0662));
#243191=CARTESIAN_POINT('Ctrl Pts',(43.0627766507519,30.7060797967663,-47.0078666666667));
#243192=CARTESIAN_POINT('Ctrl Pts',(43.5445019199415,29.87170715524,-46.9495333333334));
#243193=CARTESIAN_POINT('Ctrl Pts',(44.5079524583208,29.87170715524,-46.8912));
#243194=CARTESIAN_POINT('Ctrl Pts',(44.5079524583208,29.87170715524,-47.74995));
#243195=CARTESIAN_POINT('Ctrl Pts',(45.4714029967,29.87170715524,-47.6916166666667));
#243196=CARTESIAN_POINT('Ctrl Pts',(45.9531282658897,30.7060797967663,-47.6332833333333));
#243197=CARTESIAN_POINT('Ctrl Pts',(46.4348535350793,31.5404524382925,-47.57495));
#243198=CARTESIAN_POINT('Ctrl Pts',(45.9531282658897,32.3748250798187,-47.5166166666667));
#243199=CARTESIAN_POINT('Ctrl Pts',(45.4714029967,33.2091977213449,-47.4582833333333));
#243200=CARTESIAN_POINT('Ctrl Pts',(44.5079524583208,33.2091977213449,-47.39995));
#243201=CARTESIAN_POINT('Ctrl Pts',(43.5445019199415,33.2091977213449,-47.3416166666666));
#243202=CARTESIAN_POINT('Ctrl Pts',(43.0627766507519,32.3748250798187,-47.2832833333333));
#243203=CARTESIAN_POINT('Ctrl Pts',(42.5810513815623,31.5404524382925,-47.22495));
#243204=CARTESIAN_POINT('Ctrl Pts',(43.0627766507519,30.7060797967663,-47.1666166666667));
#243205=CARTESIAN_POINT('Ctrl Pts',(43.5445019199415,29.87170715524,-47.1082833333333));
#243206=CARTESIAN_POINT('Ctrl Pts',(44.5079524583208,29.87170715524,-47.04995));
#243207=CARTESIAN_POINT('Origin',(44.5079524583208,31.5404524382925,-52.920575));
#243208=CARTESIAN_POINT('',(44.5079524583208,29.87170715524,-48.44995));
#243209=CARTESIAN_POINT('',(44.5079524583208,29.87170715524,-48.2912));
#243210=CARTESIAN_POINT('',(44.5079524583209,29.8717071552401,-52.920575));
#243211=CARTESIAN_POINT('Ctrl Pts',(44.5079524583208,29.87170715524,-48.2912));
#243212=CARTESIAN_POINT('Ctrl Pts',(45.4714029967,29.87170715524,-48.2328666666667));
#243213=CARTESIAN_POINT('Ctrl Pts',(45.9531282658897,30.7060797967663,-48.1745333333334));
#243214=CARTESIAN_POINT('Ctrl Pts',(46.4348535350793,31.5404524382925,-48.1162));
#243215=CARTESIAN_POINT('Ctrl Pts',(45.9531282658897,32.3748250798187,-48.0578666666667));
#243216=CARTESIAN_POINT('Ctrl Pts',(45.4714029967,33.2091977213449,-47.9995333333334));
#243217=CARTESIAN_POINT('Ctrl Pts',(44.5079524583208,33.2091977213449,-47.9412));
#243218=CARTESIAN_POINT('Ctrl Pts',(43.5445019199415,33.2091977213449,-47.8828666666667));
#243219=CARTESIAN_POINT('Ctrl Pts',(43.0627766507519,32.3748250798187,-47.8245333333333));
#243220=CARTESIAN_POINT('Ctrl Pts',(42.5810513815623,31.5404524382925,-47.7662));
#243221=CARTESIAN_POINT('Ctrl Pts',(43.0627766507519,30.7060797967663,-47.7078666666667));
#243222=CARTESIAN_POINT('Ctrl Pts',(43.5445019199415,29.87170715524,-47.6495333333334));
#243223=CARTESIAN_POINT('Ctrl Pts',(44.5079524583208,29.87170715524,-47.5912));
#243224=CARTESIAN_POINT('Ctrl Pts',(44.5079524583208,29.87170715524,-48.44995));
#243225=CARTESIAN_POINT('Ctrl Pts',(45.4714029967,29.87170715524,-48.3916166666667));
#243226=CARTESIAN_POINT('Ctrl Pts',(45.9531282658897,30.7060797967663,-48.3332833333333));
#243227=CARTESIAN_POINT('Ctrl Pts',(46.4348535350793,31.5404524382925,-48.27495));
#243228=CARTESIAN_POINT('Ctrl Pts',(45.9531282658897,32.3748250798187,-48.2166166666667));
#243229=CARTESIAN_POINT('Ctrl Pts',(45.4714029967,33.2091977213449,-48.1582833333333));
#243230=CARTESIAN_POINT('Ctrl Pts',(44.5079524583208,33.2091977213449,-48.09995));
#243231=CARTESIAN_POINT('Ctrl Pts',(43.5445019199415,33.2091977213449,-48.0416166666667));
#243232=CARTESIAN_POINT('Ctrl Pts',(43.0627766507519,32.3748250798187,-47.9832833333334));
#243233=CARTESIAN_POINT('Ctrl Pts',(42.5810513815623,31.5404524382925,-47.92495));
#243234=CARTESIAN_POINT('Ctrl Pts',(43.0627766507519,30.7060797967663,-47.8666166666667));
#243235=CARTESIAN_POINT('Ctrl Pts',(43.5445019199415,29.87170715524,-47.8082833333333));
#243236=CARTESIAN_POINT('Ctrl Pts',(44.5079524583208,29.87170715524,-47.74995));
#243237=CARTESIAN_POINT('Origin',(44.5079524583208,31.5404524382925,-52.920575));
#243238=CARTESIAN_POINT('',(44.5079524583208,29.87170715524,-49.14995));
#243239=CARTESIAN_POINT('',(44.5079524583208,29.87170715524,-48.9912));
#243240=CARTESIAN_POINT('',(44.5079524583209,29.8717071552401,-52.920575));
#243241=CARTESIAN_POINT('Ctrl Pts',(44.5079524583208,29.87170715524,-48.9912));
#243242=CARTESIAN_POINT('Ctrl Pts',(45.4714029967,29.87170715524,-48.9328666666667));
#243243=CARTESIAN_POINT('Ctrl Pts',(45.9531282658897,30.7060797967663,-48.8745333333333));
#243244=CARTESIAN_POINT('Ctrl Pts',(46.4348535350793,31.5404524382925,-48.8162));
#243245=CARTESIAN_POINT('Ctrl Pts',(45.9531282658897,32.3748250798187,-48.7578666666667));
#243246=CARTESIAN_POINT('Ctrl Pts',(45.4714029967,33.2091977213449,-48.6995333333333));
#243247=CARTESIAN_POINT('Ctrl Pts',(44.5079524583208,33.2091977213449,-48.6412));
#243248=CARTESIAN_POINT('Ctrl Pts',(43.5445019199415,33.2091977213449,-48.5828666666667));
#243249=CARTESIAN_POINT('Ctrl Pts',(43.0627766507519,32.3748250798187,-48.5245333333333));
#243250=CARTESIAN_POINT('Ctrl Pts',(42.5810513815623,31.5404524382925,-48.4662));
#243251=CARTESIAN_POINT('Ctrl Pts',(43.0627766507519,30.7060797967663,-48.4078666666667));
#243252=CARTESIAN_POINT('Ctrl Pts',(43.5445019199415,29.87170715524,-48.3495333333333));
#243253=CARTESIAN_POINT('Ctrl Pts',(44.5079524583208,29.87170715524,-48.2912));
#243254=CARTESIAN_POINT('Ctrl Pts',(44.5079524583208,29.87170715524,-49.14995));
#243255=CARTESIAN_POINT('Ctrl Pts',(45.4714029967,29.87170715524,-49.0916166666667));
#243256=CARTESIAN_POINT('Ctrl Pts',(45.9531282658897,30.7060797967663,-49.0332833333333));
#243257=CARTESIAN_POINT('Ctrl Pts',(46.4348535350793,31.5404524382925,-48.97495));
#243258=CARTESIAN_POINT('Ctrl Pts',(45.9531282658897,32.3748250798187,-48.9166166666667));
#243259=CARTESIAN_POINT('Ctrl Pts',(45.4714029967,33.2091977213449,-48.8582833333333));
#243260=CARTESIAN_POINT('Ctrl Pts',(44.5079524583208,33.2091977213449,-48.79995));
#243261=CARTESIAN_POINT('Ctrl Pts',(43.5445019199415,33.2091977213449,-48.7416166666667));
#243262=CARTESIAN_POINT('Ctrl Pts',(43.0627766507519,32.3748250798187,-48.6832833333333));
#243263=CARTESIAN_POINT('Ctrl Pts',(42.5810513815623,31.5404524382925,-48.62495));
#243264=CARTESIAN_POINT('Ctrl Pts',(43.0627766507519,30.7060797967663,-48.5666166666667));
#243265=CARTESIAN_POINT('Ctrl Pts',(43.5445019199415,29.87170715524,-48.5082833333334));
#243266=CARTESIAN_POINT('Ctrl Pts',(44.5079524583208,29.87170715524,-48.44995));
#243267=CARTESIAN_POINT('Origin',(44.5079524583208,31.5404524382925,-52.920575));
#243268=CARTESIAN_POINT('',(44.5079524583208,29.87170715524,-49.84995));
#243269=CARTESIAN_POINT('',(44.5079524583208,29.87170715524,-49.6912));
#243270=CARTESIAN_POINT('',(44.5079524583209,29.8717071552401,-52.920575));
#243271=CARTESIAN_POINT('Ctrl Pts',(44.5079524583208,29.87170715524,-49.6912));
#243272=CARTESIAN_POINT('Ctrl Pts',(45.4714029967,29.87170715524,-49.6328666666667));
#243273=CARTESIAN_POINT('Ctrl Pts',(45.9531282658897,30.7060797967663,-49.5745333333333));
#243274=CARTESIAN_POINT('Ctrl Pts',(46.4348535350793,31.5404524382925,-49.5162));
#243275=CARTESIAN_POINT('Ctrl Pts',(45.9531282658897,32.3748250798187,-49.4578666666667));
#243276=CARTESIAN_POINT('Ctrl Pts',(45.4714029967,33.2091977213449,-49.3995333333333));
#243277=CARTESIAN_POINT('Ctrl Pts',(44.5079524583208,33.2091977213449,-49.3412));
#243278=CARTESIAN_POINT('Ctrl Pts',(43.5445019199415,33.2091977213449,-49.2828666666667));
#243279=CARTESIAN_POINT('Ctrl Pts',(43.0627766507519,32.3748250798187,-49.2245333333333));
#243280=CARTESIAN_POINT('Ctrl Pts',(42.5810513815623,31.5404524382925,-49.1662));
#243281=CARTESIAN_POINT('Ctrl Pts',(43.0627766507519,30.7060797967663,-49.1078666666667));
#243282=CARTESIAN_POINT('Ctrl Pts',(43.5445019199415,29.87170715524,-49.0495333333334));
#243283=CARTESIAN_POINT('Ctrl Pts',(44.5079524583208,29.87170715524,-48.9912));
#243284=CARTESIAN_POINT('Ctrl Pts',(44.5079524583208,29.87170715524,-49.84995));
#243285=CARTESIAN_POINT('Ctrl Pts',(45.4714029967,29.87170715524,-49.7916166666667));
#243286=CARTESIAN_POINT('Ctrl Pts',(45.9531282658897,30.7060797967663,-49.7332833333333));
#243287=CARTESIAN_POINT('Ctrl Pts',(46.4348535350793,31.5404524382925,-49.67495));
#243288=CARTESIAN_POINT('Ctrl Pts',(45.9531282658897,32.3748250798187,-49.6166166666667));
#243289=CARTESIAN_POINT('Ctrl Pts',(45.4714029967,33.2091977213449,-49.5582833333334));
#243290=CARTESIAN_POINT('Ctrl Pts',(44.5079524583208,33.2091977213449,-49.49995));
#243291=CARTESIAN_POINT('Ctrl Pts',(43.5445019199415,33.2091977213449,-49.4416166666667));
#243292=CARTESIAN_POINT('Ctrl Pts',(43.0627766507519,32.3748250798187,-49.3832833333334));
#243293=CARTESIAN_POINT('Ctrl Pts',(42.5810513815623,31.5404524382925,-49.32495));
#243294=CARTESIAN_POINT('Ctrl Pts',(43.0627766507519,30.7060797967663,-49.2666166666667));
#243295=CARTESIAN_POINT('Ctrl Pts',(43.5445019199415,29.87170715524,-49.2082833333334));
#243296=CARTESIAN_POINT('Ctrl Pts',(44.5079524583208,29.87170715524,-49.14995));
#243297=CARTESIAN_POINT('Origin',(44.5079524583208,31.5404524382925,-52.920575));
#243298=CARTESIAN_POINT('',(44.5079524583208,29.87170715524,-50.54995));
#243299=CARTESIAN_POINT('',(44.5079524583208,29.87170715524,-50.3912));
#243300=CARTESIAN_POINT('',(44.5079524583209,29.8717071552401,-52.920575));
#243301=CARTESIAN_POINT('Ctrl Pts',(44.5079524583208,29.87170715524,-50.3912));
#243302=CARTESIAN_POINT('Ctrl Pts',(45.4714029967,29.87170715524,-50.3328666666666));
#243303=CARTESIAN_POINT('Ctrl Pts',(45.9531282658897,30.7060797967663,-50.2745333333333));
#243304=CARTESIAN_POINT('Ctrl Pts',(46.4348535350793,31.5404524382925,-50.2162));
#243305=CARTESIAN_POINT('Ctrl Pts',(45.9531282658897,32.3748250798187,-50.1578666666667));
#243306=CARTESIAN_POINT('Ctrl Pts',(45.4714029967,33.2091977213449,-50.0995333333333));
#243307=CARTESIAN_POINT('Ctrl Pts',(44.5079524583208,33.2091977213449,-50.0412));
#243308=CARTESIAN_POINT('Ctrl Pts',(43.5445019199415,33.2091977213449,-49.9828666666667));
#243309=CARTESIAN_POINT('Ctrl Pts',(43.0627766507519,32.3748250798187,-49.9245333333334));
#243310=CARTESIAN_POINT('Ctrl Pts',(42.5810513815623,31.5404524382925,-49.8662));
#243311=CARTESIAN_POINT('Ctrl Pts',(43.0627766507519,30.7060797967663,-49.8078666666667));
#243312=CARTESIAN_POINT('Ctrl Pts',(43.5445019199415,29.87170715524,-49.7495333333333));
#243313=CARTESIAN_POINT('Ctrl Pts',(44.5079524583208,29.87170715524,-49.6912));
#243314=CARTESIAN_POINT('Ctrl Pts',(44.5079524583208,29.87170715524,-50.54995));
#243315=CARTESIAN_POINT('Ctrl Pts',(45.4714029967,29.87170715524,-50.4916166666667));
#243316=CARTESIAN_POINT('Ctrl Pts',(45.9531282658897,30.7060797967663,-50.4332833333333));
#243317=CARTESIAN_POINT('Ctrl Pts',(46.4348535350793,31.5404524382925,-50.37495));
#243318=CARTESIAN_POINT('Ctrl Pts',(45.9531282658897,32.3748250798187,-50.3166166666667));
#243319=CARTESIAN_POINT('Ctrl Pts',(45.4714029967,33.2091977213449,-50.2582833333334));
#243320=CARTESIAN_POINT('Ctrl Pts',(44.5079524583208,33.2091977213449,-50.19995));
#243321=CARTESIAN_POINT('Ctrl Pts',(43.5445019199415,33.2091977213449,-50.1416166666667));
#243322=CARTESIAN_POINT('Ctrl Pts',(43.0627766507519,32.3748250798187,-50.0832833333333));
#243323=CARTESIAN_POINT('Ctrl Pts',(42.5810513815623,31.5404524382925,-50.02495));
#243324=CARTESIAN_POINT('Ctrl Pts',(43.0627766507519,30.7060797967663,-49.9666166666667));
#243325=CARTESIAN_POINT('Ctrl Pts',(43.5445019199415,29.87170715524,-49.9082833333334));
#243326=CARTESIAN_POINT('Ctrl Pts',(44.5079524583208,29.87170715524,-49.84995));
#243327=CARTESIAN_POINT('Origin',(44.5079524583208,31.5404524382925,-52.920575));
#243328=CARTESIAN_POINT('',(44.5079524583208,29.87170715524,-51.24995));
#243329=CARTESIAN_POINT('',(44.5079524583208,29.87170715524,-51.0912));
#243330=CARTESIAN_POINT('',(44.5079524583209,29.8717071552401,-52.920575));
#243331=CARTESIAN_POINT('Ctrl Pts',(44.5079524583208,29.87170715524,-51.0912));
#243332=CARTESIAN_POINT('Ctrl Pts',(45.4714029967,29.87170715524,-51.0328666666667));
#243333=CARTESIAN_POINT('Ctrl Pts',(45.9531282658897,30.7060797967663,-50.9745333333333));
#243334=CARTESIAN_POINT('Ctrl Pts',(46.4348535350793,31.5404524382925,-50.9162));
#243335=CARTESIAN_POINT('Ctrl Pts',(45.9531282658897,32.3748250798187,-50.8578666666667));
#243336=CARTESIAN_POINT('Ctrl Pts',(45.4714029967,33.2091977213449,-50.7995333333333));
#243337=CARTESIAN_POINT('Ctrl Pts',(44.5079524583208,33.2091977213449,-50.7412));
#243338=CARTESIAN_POINT('Ctrl Pts',(43.5445019199415,33.2091977213449,-50.6828666666667));
#243339=CARTESIAN_POINT('Ctrl Pts',(43.0627766507519,32.3748250798187,-50.6245333333333));
#243340=CARTESIAN_POINT('Ctrl Pts',(42.5810513815623,31.5404524382925,-50.5662));
#243341=CARTESIAN_POINT('Ctrl Pts',(43.0627766507519,30.7060797967663,-50.5078666666667));
#243342=CARTESIAN_POINT('Ctrl Pts',(43.5445019199415,29.87170715524,-50.4495333333333));
#243343=CARTESIAN_POINT('Ctrl Pts',(44.5079524583208,29.87170715524,-50.3912));
#243344=CARTESIAN_POINT('Ctrl Pts',(44.5079524583208,29.87170715524,-51.24995));
#243345=CARTESIAN_POINT('Ctrl Pts',(45.4714029967,29.87170715524,-51.1916166666667));
#243346=CARTESIAN_POINT('Ctrl Pts',(45.9531282658897,30.7060797967663,-51.1332833333333));
#243347=CARTESIAN_POINT('Ctrl Pts',(46.4348535350793,31.5404524382925,-51.07495));
#243348=CARTESIAN_POINT('Ctrl Pts',(45.9531282658897,32.3748250798187,-51.0166166666667));
#243349=CARTESIAN_POINT('Ctrl Pts',(45.4714029967,33.2091977213449,-50.9582833333334));
#243350=CARTESIAN_POINT('Ctrl Pts',(44.5079524583208,33.2091977213449,-50.89995));
#243351=CARTESIAN_POINT('Ctrl Pts',(43.5445019199415,33.2091977213449,-50.8416166666667));
#243352=CARTESIAN_POINT('Ctrl Pts',(43.0627766507519,32.3748250798187,-50.7832833333333));
#243353=CARTESIAN_POINT('Ctrl Pts',(42.5810513815623,31.5404524382925,-50.72495));
#243354=CARTESIAN_POINT('Ctrl Pts',(43.0627766507519,30.7060797967663,-50.6666166666667));
#243355=CARTESIAN_POINT('Ctrl Pts',(43.5445019199415,29.87170715524,-50.6082833333334));
#243356=CARTESIAN_POINT('Ctrl Pts',(44.5079524583208,29.87170715524,-50.54995));
#243357=CARTESIAN_POINT('Origin',(44.5079524583208,31.5404524382925,-52.920575));
#243358=CARTESIAN_POINT('',(44.5079524583208,29.87170715524,-51.94995));
#243359=CARTESIAN_POINT('',(44.5079524583208,29.87170715524,-51.7912));
#243360=CARTESIAN_POINT('',(44.5079524583209,29.8717071552401,-52.920575));
#243361=CARTESIAN_POINT('Ctrl Pts',(44.5079524583208,29.87170715524,-51.7912));
#243362=CARTESIAN_POINT('Ctrl Pts',(45.4714029967,29.87170715524,-51.7328666666667));
#243363=CARTESIAN_POINT('Ctrl Pts',(45.9531282658897,30.7060797967663,-51.6745333333333));
#243364=CARTESIAN_POINT('Ctrl Pts',(46.4348535350793,31.5404524382925,-51.6162));
#243365=CARTESIAN_POINT('Ctrl Pts',(45.9531282658897,32.3748250798187,-51.5578666666667));
#243366=CARTESIAN_POINT('Ctrl Pts',(45.4714029967,33.2091977213449,-51.4995333333333));
#243367=CARTESIAN_POINT('Ctrl Pts',(44.5079524583208,33.2091977213449,-51.4412));
#243368=CARTESIAN_POINT('Ctrl Pts',(43.5445019199415,33.2091977213449,-51.3828666666667));
#243369=CARTESIAN_POINT('Ctrl Pts',(43.0627766507519,32.3748250798187,-51.3245333333334));
#243370=CARTESIAN_POINT('Ctrl Pts',(42.5810513815623,31.5404524382925,-51.2662));
#243371=CARTESIAN_POINT('Ctrl Pts',(43.0627766507519,30.7060797967663,-51.2078666666667));
#243372=CARTESIAN_POINT('Ctrl Pts',(43.5445019199415,29.87170715524,-51.1495333333333));
#243373=CARTESIAN_POINT('Ctrl Pts',(44.5079524583208,29.87170715524,-51.0912));
#243374=CARTESIAN_POINT('Ctrl Pts',(44.5079524583208,29.87170715524,-51.94995));
#243375=CARTESIAN_POINT('Ctrl Pts',(45.4714029967,29.87170715524,-51.8916166666666));
#243376=CARTESIAN_POINT('Ctrl Pts',(45.9531282658897,30.7060797967663,-51.8332833333333));
#243377=CARTESIAN_POINT('Ctrl Pts',(46.4348535350793,31.5404524382925,-51.77495));
#243378=CARTESIAN_POINT('Ctrl Pts',(45.9531282658897,32.3748250798187,-51.7166166666667));
#243379=CARTESIAN_POINT('Ctrl Pts',(45.4714029967,33.2091977213449,-51.6582833333333));
#243380=CARTESIAN_POINT('Ctrl Pts',(44.5079524583208,33.2091977213449,-51.59995));
#243381=CARTESIAN_POINT('Ctrl Pts',(43.5445019199415,33.2091977213449,-51.5416166666667));
#243382=CARTESIAN_POINT('Ctrl Pts',(43.0627766507519,32.3748250798187,-51.4832833333333));
#243383=CARTESIAN_POINT('Ctrl Pts',(42.5810513815623,31.5404524382925,-51.42495));
#243384=CARTESIAN_POINT('Ctrl Pts',(43.0627766507519,30.7060797967663,-51.3666166666667));
#243385=CARTESIAN_POINT('Ctrl Pts',(43.5445019199415,29.87170715524,-51.3082833333333));
#243386=CARTESIAN_POINT('Ctrl Pts',(44.5079524583208,29.87170715524,-51.24995));
#243387=CARTESIAN_POINT('Origin',(44.5079524583208,31.5404524382925,-52.920575));
#243388=CARTESIAN_POINT('',(44.5079524583208,29.87170715524,-52.64995));
#243389=CARTESIAN_POINT('',(44.5079524583208,29.87170715524,-52.4912));
#243390=CARTESIAN_POINT('',(44.5079524583209,29.8717071552401,-52.920575));
#243391=CARTESIAN_POINT('',(42.8554737113965,31.3080200595814,-52.64995));
#243392=CARTESIAN_POINT('Origin',(44.5079524583208,31.5404524382925,-52.64995));
#243393=CARTESIAN_POINT('Ctrl Pts',(42.8554737113965,31.3080200595814,-52.64995));
#243394=CARTESIAN_POINT('Ctrl Pts',(42.9006402736027,30.9869082397437,-52.6275001713604));
#243395=CARTESIAN_POINT('Ctrl Pts',(43.0627766507519,30.7060797967663,-52.6078666666667));
#243396=CARTESIAN_POINT('Ctrl Pts',(43.5445019199415,29.87170715524,-52.5495333333333));
#243397=CARTESIAN_POINT('Ctrl Pts',(44.5079524583208,29.87170715524,-52.4912));
#243398=CARTESIAN_POINT('Origin',(-73.0894692252869,64.3905251417593,178.93805));
#243399=CARTESIAN_POINT('',(73.0894692252869,64.3905251417593,-27.14995));
#243400=CARTESIAN_POINT('',(-63.0894692252869,64.3905251417593,-27.14995));
#243401=CARTESIAN_POINT('',(-73.0894692252869,64.3905251417593,-27.14995));
#243402=CARTESIAN_POINT('',(-63.0894692252869,64.3905251417593,153.53805));
#243403=CARTESIAN_POINT('',(-63.0894692252869,64.3905251417593,178.93805));
#243404=CARTESIAN_POINT('',(-52.7694692252869,64.3905251417593,153.53805));
#243405=CARTESIAN_POINT('',(-52.7694692252869,64.3905251417593,153.53805));
#243406=CARTESIAN_POINT('',(-52.7694692252869,64.3905251417593,10.95005));
#243407=CARTESIAN_POINT('',(-52.7694692252869,64.3905251417593,10.95005));
#243408=CARTESIAN_POINT('',(52.7165405689488,64.3905251417593,10.95005));
#243409=CARTESIAN_POINT('',(-52.7694692252869,64.3905251417593,10.95005));
#243410=CARTESIAN_POINT('',(52.7165405689488,64.3905251417593,153.53805));
#243411=CARTESIAN_POINT('',(52.7165405689488,64.3905251417593,10.95005));
#243412=CARTESIAN_POINT('',(73.0894692252869,64.3905251417593,153.53805));
#243413=CARTESIAN_POINT('',(73.0894692252869,64.3905251417593,153.53805));
#243414=CARTESIAN_POINT('',(73.0894692252869,64.3905251417593,178.93805));
#243415=CARTESIAN_POINT('Origin',(73.0894692252869,-92.5030998968147,178.93805));
#243416=CARTESIAN_POINT('',(73.0894692252869,-92.5030998968147,143.53805));
#243417=CARTESIAN_POINT('',(73.0894692252869,-92.5030998968147,-17.1499499999999));
#243418=CARTESIAN_POINT('',(73.0894692252869,-92.5030998968147,178.93805));
#243419=CARTESIAN_POINT('',(73.0894692252869,-82.5030998968147,-27.14995));
#243420=CARTESIAN_POINT('Origin',(73.0894692252869,-82.5030998968147,-17.14995));
#243421=CARTESIAN_POINT('',(73.0894692252869,-92.5030998968147,-27.14995));
#243422=CARTESIAN_POINT('',(73.0894692252869,-82.5030998968147,153.53805));
#243423=CARTESIAN_POINT('',(73.0894692252869,-92.5030998968147,153.53805));
#243424=CARTESIAN_POINT('Origin',(73.0894692252869,-82.5030998968147,143.53805));
#243425=CARTESIAN_POINT('Origin',(-73.0894692252869,-92.5030998968147,178.93805));
#243426=CARTESIAN_POINT('',(1.41042477341199E-15,-92.5030998968147,-17.7284445206843));
#243427=CARTESIAN_POINT('',(5.38401031719611,-92.5030998968147,-17.14995));
#243428=CARTESIAN_POINT('Ctrl Pts',(2.91433543964104E-16,-92.5030998968147,
-17.7284445206843));
#243429=CARTESIAN_POINT('Ctrl Pts',(0.147229163500497,-92.5030998968147,
-17.7284445207334));
#243430=CARTESIAN_POINT('Ctrl Pts',(0.293871405581726,-92.5030998968147,
-17.7239593344788));
#243431=CARTESIAN_POINT('Ctrl Pts',(0.44004554522873,-92.5030998968147,
-17.7155634484342));
#243432=CARTESIAN_POINT('Ctrl Pts',(0.517553206202418,-92.5030998968147,
-17.7111115974386));
#243433=CARTESIAN_POINT('Ctrl Pts',(0.594929276459816,-92.5030998968147,
-17.7055592859653));
#243434=CARTESIAN_POINT('Ctrl Pts',(0.672191588762477,-92.5030998968147,
-17.6989863163936));
#243435=CARTESIAN_POINT('Ctrl Pts',(0.817842223176104,-92.5030998968147,
-17.686595317994));
#243436=CARTESIAN_POINT('Ctrl Pts',(0.963088078591146,-92.5030998968147,
-17.6706470841864));
#243437=CARTESIAN_POINT('Ctrl Pts',(1.10803994708469,-92.5030998968147,
-17.6522190746586));
#243438=CARTESIAN_POINT('Ctrl Pts',(1.1872147971738,-92.5030998968147,-17.6421534238535));
#243439=CARTESIAN_POINT('Ctrl Pts',(1.26630195606147,-92.5030998968147,
-17.6313468742016));
#243440=CARTESIAN_POINT('Ctrl Pts',(1.34531959863512,-92.5030998968147,
-17.6199686692659));
#243441=CARTESIAN_POINT('Ctrl Pts',(1.52436111987836,-92.5030998968147,
-17.5941874506121));
#243442=CARTESIAN_POINT('Ctrl Pts',(1.70304430645085,-92.5030998968147,
-17.5655472846095));
#243443=CARTESIAN_POINT('Ctrl Pts',(1.88158201618799,-92.5030998968147,
-17.5359412079341));
#243444=CARTESIAN_POINT('Ctrl Pts',(1.92738834388522,-92.5030998968147,
-17.5283453580041));
#243445=CARTESIAN_POINT('Ctrl Pts',(1.97318510093253,-92.5030998968147,
-17.5206856425068));
#243446=CARTESIAN_POINT('Ctrl Pts',(2.0189758909695,-92.5030998968147,-17.5129935633713));
#243447=CARTESIAN_POINT('Ctrl Pts',(2.2426386144668,-92.5030998968147,-17.475422004387));
#243448=CARTESIAN_POINT('Ctrl Pts',(2.46615860930815,-92.5030998968147,
-17.4370978585973));
#243449=CARTESIAN_POINT('Ctrl Pts',(2.68997472098224,-92.5030998968146,
-17.4006914213871));
#243450=CARTESIAN_POINT('Ctrl Pts',(2.69089693821404,-92.5030998968146,
-17.400541411437));
#243451=CARTESIAN_POINT('Ctrl Pts',(2.6918191587813,-92.5030998968146,-17.4003914343617));
#243452=CARTESIAN_POINT('Ctrl Pts',(2.69274138269184,-92.5030998968146,
-17.4002414903531));
#243453=CARTESIAN_POINT('Ctrl Pts',(2.91701904908716,-92.5030998968146,
-17.3637762762437));
#243454=CARTESIAN_POINT('Ctrl Pts',(3.14149484510243,-92.5030998968146,
-17.3292456165492));
#243455=CARTESIAN_POINT('Ctrl Pts',(3.36629960048568,-92.5030998968147,
-17.2984515031681));
#243456=CARTESIAN_POINT('Ctrl Pts',(3.58776424796595,-92.5030998968147,
-17.2681149230864));
#243457=CARTESIAN_POINT('Ctrl Pts',(3.8095485406857,-92.5030998968147,-17.2413843839963));
#243458=CARTESIAN_POINT('Ctrl Pts',(4.03178888983265,-92.5030998968147,
-17.2193800201178));
#243459=CARTESIAN_POINT('Ctrl Pts',(4.0343401623378,-92.5030998968147,-17.2191274146447));
#243460=CARTESIAN_POINT('Ctrl Pts',(4.03689149329264,-92.5030998968147,
-17.218875432595));
#243461=CARTESIAN_POINT('Ctrl Pts',(4.03944288277982,-92.5030998968147,
-17.2186240757152));
#243462=CARTESIAN_POINT('Ctrl Pts',(4.28517101203901,-92.5030998968146,
-17.1944155194854));
#243463=CARTESIAN_POINT('Ctrl Pts',(4.53144181435921,-92.5030998968146,
-17.176053999827));
#243464=CARTESIAN_POINT('Ctrl Pts',(4.77834069452045,-92.5030998968147,
-17.1644308424862));
#243465=CARTESIAN_POINT('Ctrl Pts',(4.97979715780893,-92.5030998968147,
-17.1549469591708));
#243466=CARTESIAN_POINT('Ctrl Pts',(5.18167176193193,-92.5030998968147,
-17.14995000057));
#243467=CARTESIAN_POINT('Ctrl Pts',(5.38401031719608,-92.5030998968147,
-17.14995));
#243468=CARTESIAN_POINT('',(73.0894692252869,-92.5030998968147,-17.14995));
#243469=CARTESIAN_POINT('',(-63.0894692252869,-92.5030998968147,143.53805));
#243470=CARTESIAN_POINT('',(-73.0894692252869,-92.5030998968147,143.53805));
#243471=CARTESIAN_POINT('',(-63.0894692252869,-92.5030998968147,-17.14995));
#243472=CARTESIAN_POINT('',(-63.0894692252869,-92.5030998968147,178.93805));
#243473=CARTESIAN_POINT('',(-5.38401031719611,-92.5030998968147,-17.14995));
#243474=CARTESIAN_POINT('',(73.0894692252869,-92.5030998968147,-17.14995));
#243475=CARTESIAN_POINT('Ctrl Pts',(-5.38401031719611,-92.5030998968147,
-17.14995));
#243476=CARTESIAN_POINT('Ctrl Pts',(-5.17485934008524,-92.5030998968147,
-17.1499500004992));
#243477=CARTESIAN_POINT('Ctrl Pts',(-4.96574937219036,-92.5030998968147,
-17.1553183575515));
#243478=CARTESIAN_POINT('Ctrl Pts',(-4.75693472932383,-92.5030998968147,
-17.165480868006));
#243479=CARTESIAN_POINT('Ctrl Pts',(-4.53691595770484,-92.5030998968146,
-17.1761886566749));
#243480=CARTESIAN_POINT('Ctrl Pts',(-4.31722468835889,-92.5030998968146,
-17.1922190450184));
#243481=CARTESIAN_POINT('Ctrl Pts',(-4.09814106884925,-92.5030998968147,
-17.2129547281307));
#243482=CARTESIAN_POINT('Ctrl Pts',(-4.0782215499176,-92.5030998968147,
-17.2148400577288));
#243483=CARTESIAN_POINT('Ctrl Pts',(-4.05830704542795,-92.5030998968147,
-17.2167643191585));
#243484=CARTESIAN_POINT('Ctrl Pts',(-4.0383977610556,-92.5030998968147,
-17.2187270683337));
#243485=CARTESIAN_POINT('Ctrl Pts',(-4.03578258234885,-92.5030998968146,
-17.218984884725));
#243486=CARTESIAN_POINT('Ctrl Pts',(-4.03316747486925,-92.5030998968147,
-17.2192433566002));
#243487=CARTESIAN_POINT('Ctrl Pts',(-4.03055243826174,-92.5030998968147,
-17.2195024821027));
#243488=CARTESIAN_POINT('Ctrl Pts',(-3.80825137721949,-92.5030998968147,
-17.2415304238898));
#243489=CARTESIAN_POINT('Ctrl Pts',(-3.58653411126924,-92.5030998968147,
-17.2682720627626));
#243490=CARTESIAN_POINT('Ctrl Pts',(-3.36523550080909,-92.5030998968146,
-17.2985975766844));
#243491=CARTESIAN_POINT('Ctrl Pts',(-3.14061523848556,-92.5030998968146,
-17.3293782710504));
#243492=CARTESIAN_POINT('Ctrl Pts',(-2.91642667300228,-92.5030998968146,
-17.3638716676672));
#243493=CARTESIAN_POINT('Ctrl Pts',(-2.69248545255446,-92.5030998968146,
-17.4002835179756));
#243494=CARTESIAN_POINT('Ctrl Pts',(-2.69114305863619,-92.5030998968146,
-17.4005017852795));
#243495=CARTESIAN_POINT('Ctrl Pts',(-2.68980067362,-92.5030998968146,-17.4007201222748));
#243496=CARTESIAN_POINT('Ctrl Pts',(-2.68845829746235,-92.5030998968146,
-17.4009385283737));
#243497=CARTESIAN_POINT('Ctrl Pts',(-2.46547921905367,-92.5030998968146,
-17.4372174732668));
#243498=CARTESIAN_POINT('Ctrl Pts',(-2.2427730556341,-92.5030998968147,
-17.4753971680139));
#243499=CARTESIAN_POINT('Ctrl Pts',(-2.01994046127722,-92.5030998968147,
-17.512831695184));
#243500=CARTESIAN_POINT('Ctrl Pts',(-1.82567729605443,-92.5030998968147,
-17.5454667311745));
#243501=CARTESIAN_POINT('Ctrl Pts',(-1.63131786476234,-92.5030998968147,
-17.5775261019158));
#243502=CARTESIAN_POINT('Ctrl Pts',(-1.43658485311307,-92.5030998968147,
-17.606583833856));
#243503=CARTESIAN_POINT('Ctrl Pts',(-1.40682826463025,-92.5030998968147,
-17.6110240618598));
#243504=CARTESIAN_POINT('Ctrl Pts',(-1.37706295113733,-92.5030998968147,
-17.6153941011427));
#243505=CARTESIAN_POINT('Ctrl Pts',(-1.34728792074641,-92.5030998968147,
-17.6196851681245));
#243506=CARTESIAN_POINT('Ctrl Pts',(-1.19021355623138,-92.5030998968147,
-17.6423221431472));
#243507=CARTESIAN_POINT('Ctrl Pts',(-1.03286783750708,-92.5030998968147,
-17.6627117449257));
#243508=CARTESIAN_POINT('Ctrl Pts',(-0.875104001456876,-92.5030998968147,
-17.6795039821736));
#243509=CARTESIAN_POINT('Ctrl Pts',(-0.80818557225273,-92.5030998968147,
-17.686626718078));
#243510=CARTESIAN_POINT('Ctrl Pts',(-0.741191904926731,-92.5030998968147,
-17.6931016412339));
#243511=CARTESIAN_POINT('Ctrl Pts',(-0.674111743118813,-92.5030998968147,
-17.6988227621603));
#243512=CARTESIAN_POINT('Ctrl Pts',(-0.516701310019878,-92.5030998968147,
-17.7122479552213));
#243513=CARTESIAN_POINT('Ctrl Pts',(-0.358814095941945,-92.5030998968147,
-17.7214461823106));
#243514=CARTESIAN_POINT('Ctrl Pts',(-0.200315373111298,-92.5030998968147,
-17.7257206232356));
#243515=CARTESIAN_POINT('Ctrl Pts',(-0.133655118857088,-92.5030998968147,
-17.7275183368939));
#243516=CARTESIAN_POINT('Ctrl Pts',(-0.0668866878046401,-92.5030998968147,
-17.7284445206844));
#243517=CARTESIAN_POINT('Ctrl Pts',(-2.77555756156289E-14,-92.5030998968147,
-17.7284445206844));
#243518=CARTESIAN_POINT('Origin',(-73.0894692252869,-64.3905251417593,178.93805));
#243519=CARTESIAN_POINT('',(-73.0894692252869,-82.5030998968147,143.53805));
#243520=CARTESIAN_POINT('',(-73.0894692252869,54.3905251417593,143.53805));
#243521=CARTESIAN_POINT('',(-73.0894692252869,64.3905251417593,143.53805));
#243522=CARTESIAN_POINT('',(-73.0894692252869,54.3905251417593,-17.14995));
#243523=CARTESIAN_POINT('',(-73.0894692252869,54.3905251417593,178.93805));
#243524=CARTESIAN_POINT('',(-73.0894692252869,-82.5030998968147,-17.14995));
#243525=CARTESIAN_POINT('',(-73.0894692252869,-92.5030998968147,-17.14995));
#243526=CARTESIAN_POINT('',(-73.0894692252869,-82.5030998968147,178.93805));
#243527=CARTESIAN_POINT('Origin',(-52.7694692252869,296.281453912738,10.95005));
#243528=CARTESIAN_POINT('',(-52.7694692252869,97.9199999800001,153.53805));
#243529=CARTESIAN_POINT('',(-52.7694692252869,97.9199999800001,153.53805));
#243530=CARTESIAN_POINT('',(-52.7694692252869,97.9199999800001,10.95005));
#243531=CARTESIAN_POINT('',(-52.7694692252869,97.9199999800001,10.95005));
#243532=CARTESIAN_POINT('',(-52.7694692252869,296.281453912738,10.95005));
#243533=CARTESIAN_POINT('Origin',(52.7165405689488,296.281453912738,10.95005));
#243534=CARTESIAN_POINT('',(52.7165405689488,97.9199999800001,153.53805));
#243535=CARTESIAN_POINT('',(52.7165405689488,64.3905251417593,153.53805));
#243536=CARTESIAN_POINT('',(52.7165405689488,97.9199999800001,10.95005));
#243537=CARTESIAN_POINT('',(52.7165405689488,296.281453912738,10.95005));
#243538=CARTESIAN_POINT('',(52.7165405689488,97.9199999800001,10.95005));
#243539=CARTESIAN_POINT('Origin',(45.,97.9199999800001,-179.84995));
#243540=CARTESIAN_POINT('',(52.7165405689488,97.9199999800001,153.53805));
#243541=CARTESIAN_POINT('',(-52.7694692252869,97.9199999800001,10.95005));
#243542=CARTESIAN_POINT('Origin',(0.,0.,-27.14995));
#243543=CARTESIAN_POINT('',(5.38401031719611,-82.5030998968147,-27.14995));
#243544=CARTESIAN_POINT('',(-73.0894692252869,-82.5030998968147,-27.14995));
#243545=CARTESIAN_POINT('',(-5.38401031719611,-82.5030998968147,-27.14995));
#243546=CARTESIAN_POINT('Origin',(1.73472347597681E-15,-79.8550000300563,
-27.14995));
#243547=CARTESIAN_POINT('',(-63.0894692252869,-82.5030998968147,-27.14995));
#243548=CARTESIAN_POINT('',(-73.0894692252869,-82.5030998968147,-27.14995));
#243549=CARTESIAN_POINT('',(-63.0894692252869,-17.612385611532,-27.14995));
#243550=CARTESIAN_POINT('',(-63.0894692252869,64.3905251417593,-27.14995));
#243551=CARTESIAN_POINT('',(-63.0894692252869,-8.3226144285248,-27.14995));
#243552=CARTESIAN_POINT('Origin',(-66.8875000100282,-12.9675000200284,-27.14995));
#243553=CARTESIAN_POINT('',(-63.0894692252869,64.3905251417593,-27.14995));
#243554=CARTESIAN_POINT('',(72.8875000100282,-12.9675000200274,-27.14995));
#243555=CARTESIAN_POINT('Origin',(66.8875000100282,-12.9675000200274,-27.14995));
#243556=CARTESIAN_POINT('',(-2.46951155546522E-15,59.91999999,-27.14995));
#243557=CARTESIAN_POINT('Origin',(-1.73472347597681E-15,53.91999999,-27.14995));
#243558=CARTESIAN_POINT('',(-55.8761336488114,-39.4730326646711,-27.14995));
#243559=CARTESIAN_POINT('',(-55.7820023947001,-39.0050779822088,-27.14995));
#243560=CARTESIAN_POINT('Ctrl Pts',(-55.8761336488114,-39.4730326646711,
-27.14995));
#243561=CARTESIAN_POINT('Ctrl Pts',(-55.857436348509,-39.4770567377031,
-27.14995));
#243562=CARTESIAN_POINT('Ctrl Pts',(-55.8345450449543,-39.478704339892,
-27.14995));
#243563=CARTESIAN_POINT('Ctrl Pts',(-55.8010467908434,-39.4734293400209,
-27.14995));
#243564=CARTESIAN_POINT('Ctrl Pts',(-55.7843587662846,-39.4674032100666,
-27.14995));
#243565=CARTESIAN_POINT('Ctrl Pts',(-55.7594408254806,-39.4513001221049,
-27.14995));
#243566=CARTESIAN_POINT('Ctrl Pts',(-55.74702264916,-39.4384648268173,-27.14995));
#243567=CARTESIAN_POINT('Ctrl Pts',(-55.7281173639228,-39.4097003595277,
-27.14995));
#243568=CARTESIAN_POINT('Ctrl Pts',(-55.7199815038304,-39.3877113716395,
-27.14995));
#243569=CARTESIAN_POINT('Ctrl Pts',(-55.7068870219065,-39.3286173033286,
-27.14995));
#243570=CARTESIAN_POINT('Ctrl Pts',(-55.7084166181688,-39.2794539793635,
-27.14995));
#243571=CARTESIAN_POINT('Ctrl Pts',(-55.7242400077265,-39.1630314139732,
-27.14995));
#243572=CARTESIAN_POINT('Ctrl Pts',(-55.7527257002045,-39.0757581751218,
-27.14995));
#243573=CARTESIAN_POINT('Ctrl Pts',(-55.7820023947002,-39.0050779822088,
-27.14995));
#243574=CARTESIAN_POINT('',(-53.5626016629799,-44.3631853290296,-27.149950000041));
#243575=CARTESIAN_POINT('',(-60.2627421407299,-28.1876153178796,-27.14995));
#243576=CARTESIAN_POINT('',(-53.5586640602543,-44.3727771923847,-27.14995));
#243577=CARTESIAN_POINT('Ctrl Pts',(-53.5586640602543,-44.3727771923846,
-27.14995));
#243578=CARTESIAN_POINT('Ctrl Pts',(-53.5593152758377,-44.3711764813904,
-27.14995));
#243579=CARTESIAN_POINT('Ctrl Pts',(-53.5599690168506,-44.3695767986133,
-27.1499500000007));
#243580=CARTESIAN_POINT('Ctrl Pts',(-53.5612815516416,-44.3663795033483,
-27.1499500000007));
#243581=CARTESIAN_POINT('Ctrl Pts',(-53.5619403445691,-44.3647818929451,
-27.14995));
#243582=CARTESIAN_POINT('Ctrl Pts',(-53.5626016635193,-44.3631853277664,
-27.14995));
#243583=CARTESIAN_POINT('',(-53.2522037718306,-45.0092559826887,-27.1499499611498));
#243584=CARTESIAN_POINT('Ctrl Pts',(-53.2522036547411,-45.0092557774118,
-27.14995));
#243585=CARTESIAN_POINT('Ctrl Pts',(-53.3294790538135,-44.9004089637583,
-27.14995));
#243586=CARTESIAN_POINT('Ctrl Pts',(-53.3831793339603,-44.793525414087,
-27.14995));
#243587=CARTESIAN_POINT('Ctrl Pts',(-53.4750626849387,-44.5886297190003,
-27.14995));
#243588=CARTESIAN_POINT('Ctrl Pts',(-53.513383785808,-44.4840786455929,
-27.14995));
#243589=CARTESIAN_POINT('Ctrl Pts',(-53.5586640602543,-44.3727771923846,
-27.14995));
#243590=CARTESIAN_POINT('',(-52.345151028036,-45.4735034267004,-27.1499501536531));
#243591=CARTESIAN_POINT('Ctrl Pts',(-52.3451484065213,-45.4735122149407,
-27.1499499998352));
#243592=CARTESIAN_POINT('Ctrl Pts',(-52.3459275035447,-45.4737446180718,
-27.1499500014364));
#243593=CARTESIAN_POINT('Ctrl Pts',(-52.346637838916,-45.4739531739643,
-27.1499500089096));
#243594=CARTESIAN_POINT('Ctrl Pts',(-52.3473191716821,-45.4741281319922,
-27.1499500260981));
#243595=CARTESIAN_POINT('Ctrl Pts',(-52.3482254969746,-45.4743608653843,
-27.1499500489628));
#243596=CARTESIAN_POINT('Ctrl Pts',(-52.3490793422263,-45.47453678322,-27.1499500935485));
#243597=CARTESIAN_POINT('Ctrl Pts',(-52.3499379336497,-45.4747048986454,
-27.1499501664179));
#243598=CARTESIAN_POINT('Ctrl Pts',(-52.3508910661715,-45.474891525573,
-27.149950247311));
#243599=CARTESIAN_POINT('Ctrl Pts',(-52.3518546868251,-45.4750614608143,
-27.1499503632212));
#243600=CARTESIAN_POINT('Ctrl Pts',(-52.3529246660297,-45.4752419002879,
-27.1499505368206));
#243601=CARTESIAN_POINT('Ctrl Pts',(-52.3535486204709,-45.4753471229038,
-27.1499506380545));
#243602=CARTESIAN_POINT('Ctrl Pts',(-52.3543069993715,-45.475480515556,
-27.1499507672218));
#243603=CARTESIAN_POINT('Ctrl Pts',(-52.3551332277138,-45.4756238142328,
-27.1499509263529));
#243604=CARTESIAN_POINT('Ctrl Pts',(-52.3567068551066,-45.4758967396599,
-27.1499512294326));
#243605=CARTESIAN_POINT('Ctrl Pts',(-52.3585273930797,-45.4762015051856,
-27.1499516548711));
#243606=CARTESIAN_POINT('Ctrl Pts',(-52.3601264666894,-45.4764605215105,
-27.1499520866353));
#243607=CARTESIAN_POINT('Ctrl Pts',(-52.3614001841934,-45.4766668369827,
-27.1499524305505));
#243608=CARTESIAN_POINT('Ctrl Pts',(-52.3625330431393,-45.4768463573693,
-27.1499527703999));
#243609=CARTESIAN_POINT('Ctrl Pts',(-52.3632870358042,-45.4769745988415,
-27.149952977261));
#243610=CARTESIAN_POINT('Ctrl Pts',(-52.3639857420081,-45.4770934370165,
-27.1499531689539));
#243611=CARTESIAN_POINT('Ctrl Pts',(-52.3647126753518,-45.4772172193922,
-27.1499533707677));
#243612=CARTESIAN_POINT('Ctrl Pts',(-52.3654678294564,-45.4773457555014,
-27.1499535811654));
#243613=CARTESIAN_POINT('Ctrl Pts',(-52.367087805466,-45.4776214944691,
-27.1499540325159));
#243614=CARTESIAN_POINT('Ctrl Pts',(-52.3688375340627,-45.4779190999074,
-27.14995452436));
#243615=CARTESIAN_POINT('Ctrl Pts',(-52.3707158918108,-45.4782384677742,
-27.1499550323686));
#243616=CARTESIAN_POINT('Ctrl Pts',(-52.3725442373027,-45.4785493323048,
-27.1499555268512));
#243617=CARTESIAN_POINT('Ctrl Pts',(-52.3750453259033,-45.4789803305049,
-27.1499561520407));
#243618=CARTESIAN_POINT('Ctrl Pts',(-52.3771208085955,-45.4793308918207,
-27.149956637901));
#243619=CARTESIAN_POINT('Ctrl Pts',(-52.3781715347264,-45.4795083656856,
-27.1499568838708));
#243620=CARTESIAN_POINT('Ctrl Pts',(-52.3791131815617,-45.4796663726659,
-27.1499570932415));
#243621=CARTESIAN_POINT('Ctrl Pts',(-52.37980339475,-45.4797837664548,-27.1499572335388));
#243622=CARTESIAN_POINT('Ctrl Pts',(-52.3816853956202,-45.4801038635155,
-27.1499576160867));
#243623=CARTESIAN_POINT('Ctrl Pts',(-52.3837163183772,-45.4804481688642,
-27.1499579779973));
#243624=CARTESIAN_POINT('Ctrl Pts',(-52.3858957243288,-45.4808133331965,
-27.1499582713809));
#243625=CARTESIAN_POINT('Ctrl Pts',(-52.3884725173317,-45.4812450806164,
-27.1499586182592));
#243626=CARTESIAN_POINT('Ctrl Pts',(-52.3912547089599,-45.4817150874301,
-27.1499588202072));
#243627=CARTESIAN_POINT('Ctrl Pts',(-52.3942399854462,-45.4822229778649,
-27.1499587218464));
#243628=CARTESIAN_POINT('Ctrl Pts',(-52.3982047554552,-45.4828975112869,
-27.1499585912127));
#243629=CARTESIAN_POINT('Ctrl Pts',(-52.4032077802452,-45.4837599356511,
-27.1499577375115));
#243630=CARTESIAN_POINT('Ctrl Pts',(-52.4077765937205,-45.4845400810146,
-27.1499560472647));
#243631=CARTESIAN_POINT('Ctrl Pts',(-52.4095574402195,-45.4848441685303,
-27.1499553884349));
#243632=CARTESIAN_POINT('Ctrl Pts',(-52.411272670905,-45.4851361374688,
-27.149954621023));
#243633=CARTESIAN_POINT('Ctrl Pts',(-52.4128361264391,-45.4854020484429,
-27.1499538159014));
#243634=CARTESIAN_POINT('Ctrl Pts',(-52.4173474081285,-45.48616932278,-27.1499514927587));
#243635=CARTESIAN_POINT('Ctrl Pts',(-52.4217963551763,-45.4866586938774,
-27.1499500079827));
#243636=CARTESIAN_POINT('Ctrl Pts',(-52.4262642309366,-45.4869505480063,
-27.1499494127242));
#243637=CARTESIAN_POINT('Ctrl Pts',(-52.4312521526722,-45.4872763729915,
-27.1499487481797));
#243638=CARTESIAN_POINT('Ctrl Pts',(-52.4362563424152,-45.4873670236692,
-27.1499492753577));
#243639=CARTESIAN_POINT('Ctrl Pts',(-52.4413789434443,-45.4874163648212,
-27.1499497332176));
#243640=CARTESIAN_POINT('Ctrl Pts',(-52.4430077900509,-45.487432053954,
-27.1499498788045));
#243641=CARTESIAN_POINT('Ctrl Pts',(-52.4446486005821,-45.487443961417,
-27.14995));
#243642=CARTESIAN_POINT('Ctrl Pts',(-52.4463046574406,-45.4874594061206,
-27.14995));
#243643=CARTESIAN_POINT('Ctrl Pts',(-52.4511323504925,-45.4875044301112,
-27.14995));
#243644=CARTESIAN_POINT('Ctrl Pts',(-52.4562630265793,-45.4874833394179,
-27.149949981182));
#243645=CARTESIAN_POINT('Ctrl Pts',(-52.4612401260371,-45.487394572175,
-27.1499499742965));
#243646=CARTESIAN_POINT('Ctrl Pts',(-52.4667587388206,-45.4872961469686,
-27.1499499666618));
#243647=CARTESIAN_POINT('Ctrl Pts',(-52.4720883220187,-45.4871148353533,
-27.1499499814094));
#243648=CARTESIAN_POINT('Ctrl Pts',(-52.4766216320627,-45.4869142695831,
-27.1499499942742));
#243649=CARTESIAN_POINT('Ctrl Pts',(-52.4777638653127,-45.4868637341268,
-27.1499499975157));
#243650=CARTESIAN_POINT('Ctrl Pts',(-52.4788556174783,-45.4868122411815,
-27.14995));
#243651=CARTESIAN_POINT('Ctrl Pts',(-52.4798872980886,-45.486761251452,
-27.14995));
#243652=CARTESIAN_POINT('Ctrl Pts',(-52.4856274379354,-45.4864775510753,
-27.14995));
#243653=CARTESIAN_POINT('Ctrl Pts',(-52.4924152853978,-45.4860650982164,
-27.1499498564486));
#243654=CARTESIAN_POINT('Ctrl Pts',(-52.4997470974223,-45.4854718698351,
-27.1499498264905));
#243655=CARTESIAN_POINT('Ctrl Pts',(-52.5020014705864,-45.4852894649755,
-27.149949817279));
#243656=CARTESIAN_POINT('Ctrl Pts',(-52.5043073701312,-45.4850903128208,
-27.1499498205136));
#243657=CARTESIAN_POINT('Ctrl Pts',(-52.5066504691328,-45.4848739122105,
-27.1499498482367));
#243658=CARTESIAN_POINT('Ctrl Pts',(-52.5138001026149,-45.4842135965139,
-27.1499499328297));
#243659=CARTESIAN_POINT('Ctrl Pts',(-52.5212928305955,-45.4834010173043,
-27.1499499622158));
#243660=CARTESIAN_POINT('Ctrl Pts',(-52.5287234875121,-45.4824712805355,
-27.1499499765901));
#243661=CARTESIAN_POINT('Ctrl Pts',(-52.5352735769052,-45.4816517219129,
-27.1499499892609));
#243662=CARTESIAN_POINT('Ctrl Pts',(-52.5417754929017,-45.4807422838156,
-27.1499499937208));
#243663=CARTESIAN_POINT('Ctrl Pts',(-52.5479631027218,-45.4797987114518,
-27.1499499898166));
#243664=CARTESIAN_POINT('Ctrl Pts',(-52.5566877067233,-45.4784682631107,
-27.1499499843116));
#243665=CARTESIAN_POINT('Ctrl Pts',(-52.5649219427036,-45.4770557430141,
-27.1499500428287));
#243666=CARTESIAN_POINT('Ctrl Pts',(-52.572986092149,-45.4755497840266,
-27.1499500764828));
#243667=CARTESIAN_POINT('Ctrl Pts',(-52.5813327839574,-45.4739910609858,
-27.1499501113161));
#243668=CARTESIAN_POINT('Ctrl Pts',(-52.5894975461691,-45.4723317537798,
-27.1499501069544));
#243669=CARTESIAN_POINT('Ctrl Pts',(-52.5978166954089,-45.4705078966956,
-27.1499500626457));
#243670=CARTESIAN_POINT('Ctrl Pts',(-52.6026387135951,-45.4694507366693,
-27.1499500369632));
#243671=CARTESIAN_POINT('Ctrl Pts',(-52.6075122389011,-45.4683374225039,
-27.14995));
#243672=CARTESIAN_POINT('Ctrl Pts',(-52.6124993356304,-45.4671482695449,
-27.14995));
#243673=CARTESIAN_POINT('Ctrl Pts',(-52.627793731053,-45.4635013830774,
-27.14995));
#243674=CARTESIAN_POINT('Ctrl Pts',(-52.6429619515309,-45.4594379777908,
-27.1499496611238));
#243675=CARTESIAN_POINT('Ctrl Pts',(-52.6579886217047,-45.4549557198868,
-27.1499498084471));
#243676=CARTESIAN_POINT('Ctrl Pts',(-52.6860026011899,-45.4465995185783,
-27.1499500830997));
#243677=CARTESIAN_POINT('Ctrl Pts',(-52.7135780856693,-45.4368490997121,
-27.1499486186568));
#243678=CARTESIAN_POINT('Ctrl Pts',(-52.7405840158337,-45.4259326684973,
-27.1499479502485));
#243679=CARTESIAN_POINT('Ctrl Pts',(-52.7613299576862,-45.4175466715759,
-27.1499474367776));
#243680=CARTESIAN_POINT('Ctrl Pts',(-52.7817402072434,-45.408472118313,
-27.1499474429761));
#243681=CARTESIAN_POINT('Ctrl Pts',(-52.8017665864966,-45.3987978865569,
-27.1499480642926));
#243682=CARTESIAN_POINT('Ctrl Pts',(-52.8108546681608,-45.3944076666811,
-27.1499483462494));
#243683=CARTESIAN_POINT('Ctrl Pts',(-52.8196245960772,-45.3900100214443,
-27.1499490848697));
#243684=CARTESIAN_POINT('Ctrl Pts',(-52.8284043464921,-45.385459859022,
-27.1499495201295));
#243685=CARTESIAN_POINT('Ctrl Pts',(-52.837148245319,-45.3809282769169,
-27.1499499536118));
#243686=CARTESIAN_POINT('Ctrl Pts',(-52.8459020777059,-45.3762451854422,
-27.149950050525));
#243687=CARTESIAN_POINT('Ctrl Pts',(-52.8549538192956,-45.3712314506474,
-27.1499500157449));
#243688=CARTESIAN_POINT('Ctrl Pts',(-52.8568413065408,-45.3701859766486,
-27.1499500084925));
#243689=CARTESIAN_POINT('Ctrl Pts',(-52.8587416139914,-45.3691260055679,
-27.14995));
#243690=CARTESIAN_POINT('Ctrl Pts',(-52.860657134334,-45.3680497216908,
-27.14995));
#243691=CARTESIAN_POINT('Ctrl Pts',(-52.8790418427447,-45.3577198051622,
-27.14995));
#243692=CARTESIAN_POINT('Ctrl Pts',(-52.8969351392667,-45.346949593182,
-27.1499512477437));
#243693=CARTESIAN_POINT('Ctrl Pts',(-52.9143346753781,-45.3357995458469,
-27.1499502874174));
#243694=CARTESIAN_POINT('Ctrl Pts',(-52.9354078751652,-45.3222953251814,
-27.149949124332));
#243695=CARTESIAN_POINT('Ctrl Pts',(-52.9557647883118,-45.3082165069823,
-27.1499463866147));
#243696=CARTESIAN_POINT('Ctrl Pts',(-52.9754070241005,-45.293686770453,
-27.1499452341524));
#243697=CARTESIAN_POINT('Ctrl Pts',(-52.9895115081847,-45.2832534145036,
-27.1499444066047));
#243698=CARTESIAN_POINT('Ctrl Pts',(-53.0030953312206,-45.2726984482425,
-27.1499455008849));
#243699=CARTESIAN_POINT('Ctrl Pts',(-53.016353957345,-45.2619395866555,
-27.1499467204705));
#243700=CARTESIAN_POINT('Ctrl Pts',(-53.0300370747147,-45.2508362668637,
-27.1499479791026));
#243701=CARTESIAN_POINT('Ctrl Pts',(-53.0433739841894,-45.2395153060101,
-27.1499492614315));
#243702=CARTESIAN_POINT('Ctrl Pts',(-53.0565343570519,-45.2278539896112,
-27.1499497201218));
#243703=CARTESIAN_POINT('Ctrl Pts',(-53.0630437485743,-45.2220860622963,
-27.1499499469995));
#243704=CARTESIAN_POINT('Ctrl Pts',(-53.069509252334,-45.216234425568,-27.14995));
#243705=CARTESIAN_POINT('Ctrl Pts',(-53.0759473313773,-45.2102819476699,
-27.14995));
#243706=CARTESIAN_POINT('Ctrl Pts',(-53.0919806669554,-45.1954579489247,
-27.14995));
#243707=CARTESIAN_POINT('Ctrl Pts',(-53.1078101056455,-45.1800393974224,
-27.1499491809342));
#243708=CARTESIAN_POINT('Ctrl Pts',(-53.1233647837272,-45.1640567641704,
-27.1499491278329));
#243709=CARTESIAN_POINT('Ctrl Pts',(-53.1297654807438,-45.1574799650599,
-27.1499491059819));
#243710=CARTESIAN_POINT('Ctrl Pts',(-53.136356763247,-45.1505658263301,
-27.1499477144818));
#243711=CARTESIAN_POINT('Ctrl Pts',(-53.1428321977,-45.143611524022,-27.149947486813));
#243712=CARTESIAN_POINT('Ctrl Pts',(-53.1495450082546,-45.1364022913024,
-27.1499472507983));
#243713=CARTESIAN_POINT('Ctrl Pts',(-53.1561332556085,-45.1291501133495,
-27.1499483370776));
#243714=CARTESIAN_POINT('Ctrl Pts',(-53.1623094714303,-45.1222061453175,
-27.1499493180657));
#243715=CARTESIAN_POINT('Ctrl Pts',(-53.1646538467079,-45.1195703457515,
-27.1499496904302));
#243716=CARTESIAN_POINT('Ctrl Pts',(-53.1669393916557,-45.1169791342172,
-27.14995));
#243717=CARTESIAN_POINT('Ctrl Pts',(-53.1691521892031,-45.1144522908955,
-27.14995));
#243718=CARTESIAN_POINT('Ctrl Pts',(-53.1832815234621,-45.0983176861041,
-27.14995));
#243719=CARTESIAN_POINT('Ctrl Pts',(-53.1976035909501,-45.0811624281401,
-27.1499475469042));
#243720=CARTESIAN_POINT('Ctrl Pts',(-53.2119604318319,-45.0629713614228,
-27.1499474781223));
#243721=CARTESIAN_POINT('Ctrl Pts',(-53.22537529149,-45.0459738472028,-27.1499474138532));
#243722=CARTESIAN_POINT('Ctrl Pts',(-53.2388193211434,-45.0280729758151,
-27.14995));
#243723=CARTESIAN_POINT('Ctrl Pts',(-53.2522038624528,-45.0092562151227,
-27.14995));
#243724=CARTESIAN_POINT('',(-46.5036191527319,-43.0538517754469,-27.14995));
#243725=CARTESIAN_POINT('',(3.82683432365091,-22.2062953451411,-27.14995));
#243726=CARTESIAN_POINT('',(-54.1572878000337,-24.5762611252214,-27.14995));
#243727=CARTESIAN_POINT('Origin',(0.,-12.9675000200281,-27.14995));
#243728=CARTESIAN_POINT('',(-59.9987583592935,-26.9958774300648,-27.1499499915518));
#243729=CARTESIAN_POINT('',(-60.645425573095,-27.2637357853684,-27.14995));
#243730=CARTESIAN_POINT('',(-60.3119373224971,-27.9655514979169,-27.1499499611521));
#243731=CARTESIAN_POINT('Ctrl Pts',(-60.3119375509452,-27.9655513976194,
-27.14995));
#243732=CARTESIAN_POINT('Ctrl Pts',(-60.315915240292,-27.9419723101595,
-27.14995));
#243733=CARTESIAN_POINT('Ctrl Pts',(-60.319153179389,-27.9190421520094,
-27.14995));
#243734=CARTESIAN_POINT('Ctrl Pts',(-60.3217313771192,-27.8968214356441,
-27.14995));
#243735=CARTESIAN_POINT('Ctrl Pts',(-60.3243095748493,-27.8746007192789,
-27.14995));
#243736=CARTESIAN_POINT('Ctrl Pts',(-60.3261016152477,-27.855008293032,
-27.14995));
#243737=CARTESIAN_POINT('Ctrl Pts',(-60.3275996320819,-27.8323854269183,
-27.14995));
#243738=CARTESIAN_POINT('Ctrl Pts',(-60.3305956657503,-27.7871396946909,
-27.14995));
#243739=CARTESIAN_POINT('Ctrl Pts',(-60.3311172816358,-27.7413426078692,
-27.14995));
#243740=CARTESIAN_POINT('Ctrl Pts',(-60.3294555661254,-27.6988630851455,
-27.14995));
#243741=CARTESIAN_POINT('Ctrl Pts',(-60.3277938506151,-27.6563835624219,
-27.14995));
#243742=CARTESIAN_POINT('Ctrl Pts',(-60.3239443539489,-27.6128971630214,
-27.14995));
#243743=CARTESIAN_POINT('Ctrl Pts',(-60.3173464366114,-27.5687770367428,
-27.14995));
#243744=CARTESIAN_POINT('Ctrl Pts',(-60.3140474779426,-27.5467169736035,
-27.14995));
#243745=CARTESIAN_POINT('Ctrl Pts',(-60.3100616489501,-27.5245016407786,
-27.14995));
#243746=CARTESIAN_POINT('Ctrl Pts',(-60.30532142818,-27.5021961390353,-27.14995));
#243747=CARTESIAN_POINT('Ctrl Pts',(-60.3005812074099,-27.4798906372921,
-27.14995));
#243748=CARTESIAN_POINT('Ctrl Pts',(-60.2947466238143,-27.4562643586996,
-27.14995));
#243749=CARTESIAN_POINT('Ctrl Pts',(-60.2887929107262,-27.435035580692,
-27.14995));
#243750=CARTESIAN_POINT('Ctrl Pts',(-60.27688548455,-27.3925780246767,-27.14995));
#243751=CARTESIAN_POINT('Ctrl Pts',(-60.2623025201996,-27.3504009664825,
-27.14995));
#243752=CARTESIAN_POINT('Ctrl Pts',(-60.2448262721408,-27.3092030144389,
-27.14995));
#243753=CARTESIAN_POINT('Ctrl Pts',(-60.2360881481114,-27.2886040384171,
-27.14995));
#243754=CARTESIAN_POINT('Ctrl Pts',(-60.226625880273,-27.268254849865,-27.14995));
#243755=CARTESIAN_POINT('Ctrl Pts',(-60.2164086170247,-27.24826843343,-27.14995));
#243756=CARTESIAN_POINT('Ctrl Pts',(-60.2061913537764,-27.2282820169949,
-27.14995));
#243757=CARTESIAN_POINT('Ctrl Pts',(-60.1944578757994,-27.2074570444496,
-27.14995));
#243758=CARTESIAN_POINT('Ctrl Pts',(-60.1834132478005,-27.1894928213111,
-27.14995));
#243759=CARTESIAN_POINT('Ctrl Pts',(-60.177890933801,-27.1805107097419,
-27.14995));
#243760=CARTESIAN_POINT('Ctrl Pts',(-60.1720349812705,-27.1713636479865,
-27.14995));
#243761=CARTESIAN_POINT('Ctrl Pts',(-60.1658052523223,-27.1620782693979,
-27.14995));
#243762=CARTESIAN_POINT('Ctrl Pts',(-60.1595755233741,-27.1527928908093,
-27.14995));
#243763=CARTESIAN_POINT('Ctrl Pts',(-60.1541727712369,-27.1449958026448,
-27.14995));
#243764=CARTESIAN_POINT('Ctrl Pts',(-60.14594718448,-27.1338491692113,-27.14995));
#243765=CARTESIAN_POINT('Ctrl Pts',(-60.1377215977232,-27.1227025357779,
-27.14995));
#243766=CARTESIAN_POINT('Ctrl Pts',(-60.1299471689708,-27.1128327042649,
-27.14995));
#243767=CARTESIAN_POINT('Ctrl Pts',(-60.1228187178762,-27.1041813790389,
-27.14995));
#243768=CARTESIAN_POINT('Ctrl Pts',(-60.1192544923289,-27.0998557164259,
-27.14995));
#243769=CARTESIAN_POINT('Ctrl Pts',(-60.1158492999601,-27.0958373343259,
-27.14995));
#243770=CARTESIAN_POINT('Ctrl Pts',(-60.1126231807877,-27.0921164159072,
-27.14995));
#243771=CARTESIAN_POINT('Ctrl Pts',(-60.1093970616152,-27.0883954974885,
-27.14995));
#243772=CARTESIAN_POINT('Ctrl Pts',(-60.1071557123175,-27.0858589013014,
-27.14995));
#243773=CARTESIAN_POINT('Ctrl Pts',(-60.1035059146068,-27.0818289508923,
-27.14995));
#243774=CARTESIAN_POINT('Ctrl Pts',(-60.0962063191852,-27.0737690500741,
-27.14995));
#243775=CARTESIAN_POINT('Ctrl Pts',(-60.0881358252403,-27.0653231937789,
-27.14995));
#243776=CARTESIAN_POINT('Ctrl Pts',(-60.0802510129,-27.0575828777573,-27.14995));
#243777=CARTESIAN_POINT('Ctrl Pts',(-60.0763086067298,-27.0537127197465,
-27.14995));
#243778=CARTESIAN_POINT('Ctrl Pts',(-60.0726275116169,-27.0501964597785,
-27.14995));
#243779=CARTESIAN_POINT('Ctrl Pts',(-60.068073229236,-27.0460154954056,
-27.14995));
#243780=CARTESIAN_POINT('Ctrl Pts',(-60.0635189468552,-27.0418345310327,
-27.14995));
#243781=CARTESIAN_POINT('Ctrl Pts',(-60.0608270167709,-27.0394009294251,
-27.14995));
#243782=CARTESIAN_POINT('Ctrl Pts',(-60.0551300882665,-27.0353595333066,
-27.14995));
#243783=CARTESIAN_POINT('Ctrl Pts',(-60.049433159762,-27.0313181371882,
-27.14995));
#243784=CARTESIAN_POINT('Ctrl Pts',(-60.0442902943263,-27.0276890843295,
-27.14995));
#243785=CARTESIAN_POINT('Ctrl Pts',(-60.0397289987587,-27.0244536454528,
-27.14995));
#243786=CARTESIAN_POINT('Ctrl Pts',(-60.0374483509749,-27.0228359260145,
-27.14995));
#243787=CARTESIAN_POINT('Ctrl Pts',(-60.0353125919848,-27.0213175666086,
-27.14995));
#243788=CARTESIAN_POINT('Ctrl Pts',(-60.0333232381725,-27.0198996133675,
-27.14995));
#243789=CARTESIAN_POINT('Ctrl Pts',(-60.0313338843601,-27.0184816601264,
-27.14995));
#243790=CARTESIAN_POINT('Ctrl Pts',(-60.0305214001357,-27.0179021513849,
-27.14995));
#243791=CARTESIAN_POINT('Ctrl Pts',(-60.0277868739454,-27.0159622808878,
-27.14995));
#243792=CARTESIAN_POINT('Ctrl Pts',(-60.0250523477551,-27.0140224103907,
-27.14995));
#243793=CARTESIAN_POINT('Ctrl Pts',(-60.0225438971918,-27.0122427021784,
-27.14995));
#243794=CARTESIAN_POINT('Ctrl Pts',(-60.0202643910877,-27.010625425684,
-27.14995));
#243795=CARTESIAN_POINT('Ctrl Pts',(-60.0179848849835,-27.0090081491896,
-27.14995));
#243796=CARTESIAN_POINT('Ctrl Pts',(-60.0175503464132,-27.0087004971746,
-27.14995));
#243797=CARTESIAN_POINT('Ctrl Pts',(-60.0141152667846,-27.0062636546787,
-27.14995));
#243798=CARTESIAN_POINT('Ctrl Pts',(-60.0072451122419,-27.0013899730315,
-27.14995));
#243799=CARTESIAN_POINT('Ctrl Pts',(-60.0026514387729,-26.9981429986844,
-27.14995));
#243800=CARTESIAN_POINT('Ctrl Pts',(-59.9987583829376,-26.9958773894365,
-27.14995));
#243801=CARTESIAN_POINT('',(-60.0785790019143,-28.6323101147099,-27.14995));
#243802=CARTESIAN_POINT('Ctrl Pts',(-60.0785790019143,-28.6323101147099,
-27.14995));
#243803=CARTESIAN_POINT('Ctrl Pts',(-60.1258286923341,-28.5202492179071,
-27.14995));
#243804=CARTESIAN_POINT('Ctrl Pts',(-60.1730775948717,-28.4178603385288,
-27.1499499999982));
#243805=CARTESIAN_POINT('Ctrl Pts',(-60.2584466045542,-28.193908983491,
-27.1499499999982));
#243806=CARTESIAN_POINT('Ctrl Pts',(-60.2916736659582,-28.0851185333452,
-27.14995));
#243807=CARTESIAN_POINT('Ctrl Pts',(-60.3119370945392,-27.9655515603093,
-27.14995));
#243808=CARTESIAN_POINT('',(-60.0745809370706,-28.6418766476167,-27.1499500000522));
#243809=CARTESIAN_POINT('Ctrl Pts',(-60.0745809362347,-28.6418766496844,
-27.14995));
#243810=CARTESIAN_POINT('Ctrl Pts',(-60.0752422385998,-28.6402801245457,
-27.14995));
#243811=CARTESIAN_POINT('Ctrl Pts',(-60.0759060662479,-28.638684646748,
-27.1499500000006));
#243812=CARTESIAN_POINT('Ctrl Pts',(-60.0772387597021,-28.6354957964475,
-27.1499500000006));
#243813=CARTESIAN_POINT('Ctrl Pts',(-60.0779076244668,-28.6339024264159,
-27.14995));
#243814=CARTESIAN_POINT('Ctrl Pts',(-60.0785790019143,-28.6323101147099,
-27.14995));
#243815=CARTESIAN_POINT('',(-57.855180104188,-33.9999842387537,-27.14995));
#243816=CARTESIAN_POINT('',(-60.2627421407299,-28.1876153178796,-27.14995));
#243817=CARTESIAN_POINT('',(-58.2526348815488,-33.7356511576002,-27.14995));
#243818=CARTESIAN_POINT('Ctrl Pts',(-57.8551801041881,-33.9999842387536,
-27.14995));
#243819=CARTESIAN_POINT('Ctrl Pts',(-57.8844567986838,-33.9293040458406,
-27.14995));
#243820=CARTESIAN_POINT('Ctrl Pts',(-57.9260258713737,-33.8474501205147,
-27.14995));
#243821=CARTESIAN_POINT('Ctrl Pts',(-57.9971602307868,-33.7539381089864,
-27.14995));
#243822=CARTESIAN_POINT('Ctrl Pts',(-58.0308423626586,-33.7180928013356,
-27.14995));
#243823=CARTESIAN_POINT('Ctrl Pts',(-58.0818873760537,-33.6855661818695,
-27.14995));
#243824=CARTESIAN_POINT('Ctrl Pts',(-58.1031888603429,-33.6757705412644,
-27.14995));
#243825=CARTESIAN_POINT('Ctrl Pts',(-58.1368964656122,-33.6687990467782,
-27.14995));
#243826=CARTESIAN_POINT('Ctrl Pts',(-58.1547533666348,-33.6685040991281,
-27.14995));
#243827=CARTESIAN_POINT('Ctrl Pts',(-58.1837596142463,-33.674737141348,
-27.14995));
#243828=CARTESIAN_POINT('Ctrl Pts',(-58.1998209469314,-33.6822762393232,
-27.14995));
#243829=CARTESIAN_POINT('Ctrl Pts',(-58.2272377777507,-33.7022330937833,
-27.14995));
#243830=CARTESIAN_POINT('Ctrl Pts',(-58.242259343044,-33.7195847204375,
-27.14995));
#243831=CARTESIAN_POINT('Ctrl Pts',(-58.2526348815488,-33.7356511576002,
-27.14995));
#243832=CARTESIAN_POINT('Origin',(-40.1177331105385,-29.5848091660776,-27.14995));
#243833=CARTESIAN_POINT('Origin',(0.,2.17747716649809E-16,-28.54995));
#243834=CARTESIAN_POINT('',(-2.46951155546522E-15,59.91999999,-28.54995));
#243835=CARTESIAN_POINT('Origin',(-1.73472347597681E-15,53.91999999,-28.54995));
#243836=CARTESIAN_POINT('',(-2.10211751572101E-15,56.91999999,-28.54995));
#243837=CARTESIAN_POINT('Origin',(-1.73472347597681E-15,53.91999999,-28.54995));
#243838=CARTESIAN_POINT('Origin',(-1.73472347597681E-15,53.91999999,-45.5205127484771));
#243839=CARTESIAN_POINT('',(-2.10211751572101E-15,56.91999999,-27.14995));
#243840=CARTESIAN_POINT('',(-2.10211751572101E-15,56.91999999,-45.5205127484771));
#243841=CARTESIAN_POINT('Origin',(-1.73472347597681E-15,53.91999999,-27.14995));
#243842=CARTESIAN_POINT('Origin',(-1.73472347597681E-15,53.91999999,-45.5205127484771));
#243843=CARTESIAN_POINT('',(-2.46951155546522E-15,59.91999999,-45.5205127484771));
#243844=CARTESIAN_POINT('Origin',(0.,0.,-27.14995));
#243845=CARTESIAN_POINT('Origin',(12.9675000200281,-12.967500020028,-28.54995));
#243846=CARTESIAN_POINT('',(72.8875000100282,-12.9675000200274,-28.54995));
#243847=CARTESIAN_POINT('Origin',(66.8875000100282,-12.9675000200274,-28.54995));
#243848=CARTESIAN_POINT('',(69.8875000100282,-12.9675000200274,-28.54995));
#243849=CARTESIAN_POINT('Origin',(66.8875000100282,-12.9675000200274,-28.54995));
#243850=CARTESIAN_POINT('Origin',(66.8875000100282,-12.9675000200274,-45.5205127484772));
#243851=CARTESIAN_POINT('',(69.8875000100282,-12.9675000200274,-27.14995));
#243852=CARTESIAN_POINT('',(69.8875000100282,-12.9675000200274,-45.5205127484772));
#243853=CARTESIAN_POINT('Origin',(66.8875000100282,-12.9675000200274,-27.14995));
#243854=CARTESIAN_POINT('Origin',(66.8875000100282,-12.9675000200274,-45.5205127484772));
#243855=CARTESIAN_POINT('',(72.8875000100282,-12.9675000200274,-45.5205127484772));
#243856=CARTESIAN_POINT('Origin',(0.,0.,-27.14995));
#243857=CARTESIAN_POINT('Origin',(-12.9675000200281,-12.9675000200282,-28.54995));
#243858=CARTESIAN_POINT('',(-72.8875000100282,-12.9675000200284,-28.54995));
#243859=CARTESIAN_POINT('Origin',(-66.8875000100282,-12.9675000200284,-28.54995));
#243860=CARTESIAN_POINT('',(-69.8875000100282,-12.9675000200284,-28.54995));
#243861=CARTESIAN_POINT('Origin',(-66.8875000100282,-12.9675000200284,-28.54995));
#243862=CARTESIAN_POINT('Origin',(-66.8875000100282,-12.9675000200284,-45.5205127484772));
#243863=CARTESIAN_POINT('',(-69.8875000100282,-12.9675000200284,-27.14995));
#243864=CARTESIAN_POINT('',(-69.8875000100282,-12.9675000200284,-45.5205127484772));
#243865=CARTESIAN_POINT('Origin',(-66.8875000100282,-12.9675000200284,-27.14995));
#243866=CARTESIAN_POINT('Origin',(-66.8875000100282,-12.9675000200284,-45.5205127484772));
#243867=CARTESIAN_POINT('',(-72.8875000100282,-12.9675000200284,-19.1495981543667));
#243868=CARTESIAN_POINT('Ctrl Pts',(-63.0894692252869,-17.612385611532,
-27.14995));
#243869=CARTESIAN_POINT('Ctrl Pts',(-63.5471016769306,-17.9865825869362,
-27.14995));
#243870=CARTESIAN_POINT('Ctrl Pts',(-64.0759568113924,-18.3017783306405,
-27.1170384642544));
#243871=CARTESIAN_POINT('Ctrl Pts',(-65.3769931585463,-18.8297394406605,
-26.9140019035161));
#243872=CARTESIAN_POINT('Ctrl Pts',(-66.1724941403793,-18.9675000200284,
-26.6941821528334));
#243873=CARTESIAN_POINT('Ctrl Pts',(-67.7431470572572,-18.9675000200284,
-26.0493222880549));
#243874=CARTESIAN_POINT('Ctrl Pts',(-68.5842584032391,-18.7773839207075,
-25.5566509641909));
#243875=CARTESIAN_POINT('Ctrl Pts',(-70.0405902601868,-18.1339073024589,
-24.3988971850764));
#243876=CARTESIAN_POINT('Ctrl Pts',(-70.6574511542138,-17.6828302500813,
-23.7346108572202));
#243877=CARTESIAN_POINT('Ctrl Pts',(-71.6953344410442,-16.644946963251,
-22.3309543073884));
#243878=CARTESIAN_POINT('Ctrl Pts',(-72.1391640112646,-15.965192613364,
-21.4806501260797));
#243879=CARTESIAN_POINT('Ctrl Pts',(-72.5723511030316,-14.9230055464081,
-20.3496274930716));
#243880=CARTESIAN_POINT('Ctrl Pts',(-72.6783812619408,-14.5802499618463,
-20.0034708627134));
#243881=CARTESIAN_POINT('Ctrl Pts',(-72.7936053444643,-14.0406964652972,
-19.5690738680634));
#243882=CARTESIAN_POINT('Ctrl Pts',(-72.8242996686683,-13.8590796780428,
-19.4400001816203));
#243883=CARTESIAN_POINT('Ctrl Pts',(-72.8706981898791,-13.4592683047818,
-19.2329336835229));
#243884=CARTESIAN_POINT('Ctrl Pts',(-72.8875000100282,-13.2439920760961,
-19.1495981543667));
#243885=CARTESIAN_POINT('Ctrl Pts',(-72.8875000100282,-12.9675000200284,
-19.1495981543667));
#243886=CARTESIAN_POINT('',(-72.8875000100282,-12.9675000200284,-45.5205127484772));
#243887=CARTESIAN_POINT('Ctrl Pts',(-72.8875000100282,-12.9675000200284,
-19.1495981543667));
#243888=CARTESIAN_POINT('Ctrl Pts',(-72.8875000100282,-12.7143686770247,
-19.1495981543667));
#243889=CARTESIAN_POINT('Ctrl Pts',(-72.8731254021373,-12.5111144844339,
-19.220932038759));
#243890=CARTESIAN_POINT('Ctrl Pts',(-72.8323299217736,-12.1338327493845,
-19.4050676822193));
#243891=CARTESIAN_POINT('Ctrl Pts',(-72.8051266450376,-11.9616848910719,
-19.5215236887874));
#243892=CARTESIAN_POINT('Ctrl Pts',(-72.7033687071041,-11.4523905224552,
-19.9151662946502));
#243893=CARTESIAN_POINT('Ctrl Pts',(-72.609889943601,-11.1300135832241,
-20.2316301675614));
#243894=CARTESIAN_POINT('Ctrl Pts',(-72.2319065968022,-10.1522326657623,
-21.2677761539189));
#243895=CARTESIAN_POINT('Ctrl Pts',(-71.8480681919679,-9.51569868903438,
-22.0510777895308));
#243896=CARTESIAN_POINT('Ctrl Pts',(-70.8903178012519,-8.44072115508987,
-23.4642017994411));
#243897=CARTESIAN_POINT('Ctrl Pts',(-70.2528967393358,-7.92767447817741,
-24.1985795660467));
#243898=CARTESIAN_POINT('Ctrl Pts',(-68.7170274778242,-7.19008180081177,
-25.4763223240037));
#243899=CARTESIAN_POINT('Ctrl Pts',(-67.8170490374015,-6.96750002002839,
-26.018980498083));
#243900=CARTESIAN_POINT('Ctrl Pts',(-66.1804258126876,-6.96750002002839,
-26.6909256618053));
#243901=CARTESIAN_POINT('Ctrl Pts',(-65.3934975758082,-7.10219196742949,
-26.9096248240429));
#243902=CARTESIAN_POINT('Ctrl Pts',(-64.0901992025078,-7.6247696746572,
-27.1161425394507));
#243903=CARTESIAN_POINT('Ctrl Pts',(-63.5528101105262,-7.94374978023574,
-27.14995));
#243904=CARTESIAN_POINT('Ctrl Pts',(-63.0894692252869,-8.3226144285248,
-27.14995));
#243905=CARTESIAN_POINT('Origin',(0.,0.,-27.14995));
#243906=CARTESIAN_POINT('Origin',(0.,-25.9350000400563,-28.54995));
#243907=CARTESIAN_POINT('',(2.46951155546522E-15,-85.8550000300563,-28.54995));
#243908=CARTESIAN_POINT('Origin',(1.73472347597681E-15,-79.8550000300563,
-28.54995));
#243909=CARTESIAN_POINT('',(2.10211751572101E-15,-82.8550000300563,-28.54995));
#243910=CARTESIAN_POINT('Origin',(1.73472347597681E-15,-79.8550000300563,
-28.54995));
#243911=CARTESIAN_POINT('Origin',(1.73472347597681E-15,-79.8550000300563,
-45.5205127484772));
#243912=CARTESIAN_POINT('',(2.10211751572101E-15,-82.8550000300563,-27.14995));
#243913=CARTESIAN_POINT('',(2.10211751572101E-15,-82.8550000300563,-45.5205127484772));
#243914=CARTESIAN_POINT('Origin',(1.73472347597681E-15,-79.8550000300563,
-27.14995));
#243915=CARTESIAN_POINT('Origin',(1.73472347597681E-15,-79.8550000300563,
-45.5205127484772));
#243916=CARTESIAN_POINT('',(9.99935396488397E-16,-85.8550000300563,-27.14995));
#243917=CARTESIAN_POINT('Origin',(1.73472347597681E-15,-79.8550000300563,
-27.14995));
#243918=CARTESIAN_POINT('',(2.46951155546522E-15,-85.8550000300563,-45.5205127484772));
#243919=CARTESIAN_POINT('Origin',(1.73472347597681E-15,-79.8550000300563,
-27.14995));
#243920=CARTESIAN_POINT('Origin',(0.,0.,-27.14995));
#243921=CARTESIAN_POINT('Origin',(-55.0820026611041,-35.7832125649284,-33.0452518248346));
#243922=CARTESIAN_POINT('',(-52.4032186345485,-42.2503692925074,-33.0452518248346));
#243923=CARTESIAN_POINT('Origin',(-55.0820026611041,-35.7832125649284,-33.0452518248346));
#243924=CARTESIAN_POINT('Origin',(-55.0820026611041,-35.7832125649284,-33.0452518248346));
#243925=CARTESIAN_POINT('Origin',(-54.8649619663051,-35.6933113655558,-32.9597467890032));
#243926=CARTESIAN_POINT('Origin',(-58.1205723882901,-37.0418293561452,-34.2423223264744));
#243927=CARTESIAN_POINT('',(-60.5940855103344,-31.6841242185413,-34.3278273623058));
#243928=CARTESIAN_POINT('Origin',(-58.3376130830891,-37.1317305555178,-34.3278273623058));
#243929=CARTESIAN_POINT('',(-60.5981652751394,-31.4944723962724,-34.3027835171364));
#243930=CARTESIAN_POINT('Origin',(-60.3770448155354,-31.5942230191687,-34.2423223264744));
#243931=CARTESIAN_POINT('',(-55.9499213956124,-42.7163258114444,-34.3027835171364));
#243932=CARTESIAN_POINT('Origin',(-58.2740433353759,-37.1053991038583,-34.3027835171364));
#243933=CARTESIAN_POINT('Origin',(-58.2740433353759,-37.1053991038583,-34.3027835171364));
#243934=CARTESIAN_POINT('Origin',(-57.3795491045205,-36.7348874619736,-33.9503898734876));
#243935=CARTESIAN_POINT('',(-54.8822573706237,-43.1979644247475,-34.0108510641496));
#243936=CARTESIAN_POINT('',(-60.183782732589,-30.398949994626,-34.0108510641496));
#243937=CARTESIAN_POINT('Origin',(-57.5330200516063,-36.7984572096868,-34.0108510641496));
#243938=CARTESIAN_POINT('Origin',(-57.5330200516063,-36.7984572096868,-34.0108510641496));
#243939=CARTESIAN_POINT('',(-60.0583331310761,-30.2677307343945,-33.9503898734876));
#243940=CARTESIAN_POINT('Origin',(-59.9626622729849,-30.4987006175224,-33.9503898734876));
#243941=CARTESIAN_POINT('',(-54.7007650779648,-43.2020441895526,-33.9503898734876));
#243942=CARTESIAN_POINT('Origin',(-57.3795491045205,-36.7348874619736,-33.9503898734876));
#243943=CARTESIAN_POINT('Origin',(-57.3795491045205,-36.7348874619736,-33.9503898734876));
#243944=CARTESIAN_POINT('Origin',(-56.4399049639283,-34.7833755446169,-30.7021592582377));
#243945=CARTESIAN_POINT('',(-57.886842929255,-35.3827168737675,-31.2721928304471));
#243946=CARTESIAN_POINT('',(-59.679932565128,-36.125438919497,-31.9785958103411));
#243947=CARTESIAN_POINT('',(-56.4399049639283,-34.7833755446169,-30.7021592582377));
#243948=CARTESIAN_POINT('',(-59.4423249965411,-34.4647200715469,-34.3278273623058));
#243949=CARTESIAN_POINT('Ctrl Pts',(-59.6799325651279,-36.125438919497,
-31.9785958103412));
#243950=CARTESIAN_POINT('Ctrl Pts',(-58.934586262998,-35.0355570872307,
-32.9063798090518));
#243951=CARTESIAN_POINT('Ctrl Pts',(-59.442324996541,-34.464720071547,-34.3278273623057));
#243952=CARTESIAN_POINT('',(-57.6492353606681,-33.7219980258176,-33.6214243824119));
#243953=CARTESIAN_POINT('',(-56.2022973953414,-33.1226566966669,-33.0513908102024));
#243954=CARTESIAN_POINT('Ctrl Pts',(-57.649235360668,-33.7219980258177,
-33.6214243824119));
#243955=CARTESIAN_POINT('Ctrl Pts',(-57.4063046536298,-34.402522117505,
-32.3043002133772));
#243956=CARTESIAN_POINT('Ctrl Pts',(-57.8868429292549,-35.3827168737677,
-31.2721928304472));
#243957=CARTESIAN_POINT('Origin',(-55.3351930504764,-37.4503860285879,-30.7021592582377));
#243958=CARTESIAN_POINT('',(-56.782131015803,-38.0497273577386,-31.2721928304472));
#243959=CARTESIAN_POINT('',(-58.575220651676,-38.7924494034679,-31.9785958103411));
#243960=CARTESIAN_POINT('',(-55.3351930504764,-37.4503860285879,-30.7021592582377));
#243961=CARTESIAN_POINT('Ctrl Pts',(-58.575220651676,-38.7924494034677,
-31.978595810341));
#243962=CARTESIAN_POINT('Ctrl Pts',(-58.5010340905656,-37.1994217531912,
-31.7317640330694));
#243963=CARTESIAN_POINT('Ctrl Pts',(-59.6799325651279,-36.1254389194971,
-31.978595810341));
#243964=CARTESIAN_POINT('Ctrl Pts',(-57.8868429292551,-35.3827168737676,
-31.2721928304471));
#243965=CARTESIAN_POINT('Ctrl Pts',(-56.9727524811973,-36.5663867834655,
-31.1296844373948));
#243966=CARTESIAN_POINT('Ctrl Pts',(-56.782131015803,-38.0497273577387,
-31.2721928304471));
#243967=CARTESIAN_POINT('Origin',(-53.9928735684375,-38.4566776646086,-33.0513908102024));
#243968=CARTESIAN_POINT('',(-55.4398115337641,-39.0560189937595,-33.6214243824119));
#243969=CARTESIAN_POINT('',(-57.2329011696371,-39.7987410394886,-34.3278273623058));
#243970=CARTESIAN_POINT('',(-53.9928735684375,-38.4566776646086,-33.0513908102024));
#243971=CARTESIAN_POINT('Ctrl Pts',(-57.2329011696371,-39.7987410394885,
-34.3278273623054));
#243972=CARTESIAN_POINT('Ctrl Pts',(-57.2775183928202,-39.0360728131871,
-32.9063798090518));
#243973=CARTESIAN_POINT('Ctrl Pts',(-58.5752206516756,-38.792449403468,
-31.9785958103413));
#243974=CARTESIAN_POINT('Ctrl Pts',(-56.782131015803,-38.0497273577387,
-31.2721928304471));
#243975=CARTESIAN_POINT('Ctrl Pts',(-55.7492367834519,-38.4030378434613,
-32.3043002133771));
#243976=CARTESIAN_POINT('Ctrl Pts',(-55.4398115337641,-39.0560189937594,
-33.6214243824119));
#243977=CARTESIAN_POINT('Origin',(-53.7552659998506,-36.7959588166585,-35.4006223621673));
#243978=CARTESIAN_POINT('',(-55.2022039651772,-37.3953001458094,-35.9706559343767));
#243979=CARTESIAN_POINT('',(-56.9952936010502,-38.1380221915386,-36.6770589142706));
#243980=CARTESIAN_POINT('',(-53.7552659998506,-36.7959588166585,-35.4006223621673));
#243981=CARTESIAN_POINT('Ctrl Pts',(-56.9952936010502,-38.1380221915386,
-36.6770589142705));
#243982=CARTESIAN_POINT('Ctrl Pts',(-56.4875548675072,-38.7088592072223,
-35.2556113610166));
#243983=CARTESIAN_POINT('Ctrl Pts',(-57.2329011696371,-39.7987410394886,
-34.3278273623059));
#243984=CARTESIAN_POINT('Ctrl Pts',(-55.4398115337641,-39.0560189937594,
-33.6214243824119));
#243985=CARTESIAN_POINT('Ctrl Pts',(-54.959273258139,-38.0758242374967,
-34.6535317653419));
#243986=CARTESIAN_POINT('Ctrl Pts',(-55.2022039651772,-37.3953001458093,
-35.9706559343767));
#243987=CARTESIAN_POINT('Origin',(-54.8599779133025,-34.1289483326876,-35.4006223621673));
#243988=CARTESIAN_POINT('',(-56.3069158786292,-34.7282896618384,-35.9706559343767));
#243989=CARTESIAN_POINT('',(-58.1000055145022,-35.4710117075677,-36.6770589142706));
#243990=CARTESIAN_POINT('',(-54.8599779133025,-34.1289483326876,-35.4006223621673));
#243991=CARTESIAN_POINT('Ctrl Pts',(-58.100005514502,-35.4710117075679,
-36.6770589142706));
#243992=CARTESIAN_POINT('Ctrl Pts',(-56.9211070399398,-36.5449945412619,
-36.430227136999));
#243993=CARTESIAN_POINT('Ctrl Pts',(-56.9952936010502,-38.1380221915383,
-36.6770589142706));
#243994=CARTESIAN_POINT('Ctrl Pts',(-55.2022039651772,-37.3953001458093,
-35.9706559343767));
#243995=CARTESIAN_POINT('Ctrl Pts',(-55.3928254305715,-35.9119595715362,
-35.8281475413243));
#243996=CARTESIAN_POINT('Ctrl Pts',(-56.3069158786292,-34.7282896618384,
-35.9706559343767));
#243997=CARTESIAN_POINT('Origin',(-56.2022973953414,-33.1226566966669,-33.0513908102024));
#243998=CARTESIAN_POINT('Ctrl Pts',(-59.4423249965407,-34.464720071547,
-34.3278273623061));
#243999=CARTESIAN_POINT('Ctrl Pts',(-58.1446227376852,-34.7083434812661,
-35.2556113610166));
#244000=CARTESIAN_POINT('Ctrl Pts',(-58.1000055145022,-35.4710117075675,
-36.6770589142702));
#244001=CARTESIAN_POINT('Ctrl Pts',(-56.3069158786292,-34.7282896618385,
-35.9706559343767));
#244002=CARTESIAN_POINT('Ctrl Pts',(-56.6163411283169,-34.0753085115404,
-34.6535317653419));
#244003=CARTESIAN_POINT('Ctrl Pts',(-57.6492353606681,-33.7219980258177,
-33.6214243824118));
#244004=CARTESIAN_POINT('Origin',(-56.6012875246971,-36.4125209605368,-33.6437870756545));
#244005=CARTESIAN_POINT('',(-55.0975854818894,-35.7896671806377,-33.0513908102024));
#244006=CARTESIAN_POINT('',(-57.7493378217924,-33.6408823630029,-33.6437870756545));
#244007=CARTESIAN_POINT('Origin',(-58.3376130830891,-37.1317305555178,-34.3278273623058));
#244008=CARTESIAN_POINT('Origin',(-58.3376130830891,-37.1317305555178,-34.3278273623058));
#244009=CARTESIAN_POINT('Origin',(-58.3376130830891,-37.1317305555178,-34.3278273623058));
#244010=CARTESIAN_POINT('Origin',(-58.3376130830891,-37.1317305555178,-34.3278273623058));
#244011=CARTESIAN_POINT('Origin',(-58.3376130830891,-37.1317305555178,-34.3278273623058));
#244012=CARTESIAN_POINT('Origin',(-58.3376130830891,-37.1317305555178,-34.3278273623058));
#244013=CARTESIAN_POINT('Origin',(-58.3376130830891,-37.1317305555178,-34.3278273623058));
#244014=CARTESIAN_POINT('Origin',(-58.3376130830891,-37.1317305555178,-34.3278273623058));
#244015=CARTESIAN_POINT('Origin',(-58.3376130830891,-37.1317305555178,-34.3278273623058));
#244016=CARTESIAN_POINT('Origin',(-58.3376130830891,-37.1317305555178,-34.3278273623058));
#244017=CARTESIAN_POINT('Origin',(-58.3376130830891,-37.1317305555178,-34.3278273623058));
#244018=CARTESIAN_POINT('Origin',(-58.3376130830891,-37.1317305555178,-34.3278273623058));
#244019=CARTESIAN_POINT('Origin',(-58.3376130830891,-37.1317305555178,-34.3278273623058));
#244020=CARTESIAN_POINT('',(-56.0415124888986,-42.6750077505855,-34.3278273623058));
#244021=CARTESIAN_POINT('Origin',(-58.3376130830891,-37.1317305555178,-34.3278273623058));
#244022=CARTESIAN_POINT('Origin',(-58.3376130830891,-37.1317305555178,-34.3278273623058));
#244023=CARTESIAN_POINT('',(-55.6588290565335,-43.5988872830968,-34.3278273623058));
#244024=CARTESIAN_POINT('Ctrl Pts',(-43.4805771074156,-59.5712767529309,
-39.2399080357013));
#244025=CARTESIAN_POINT('Ctrl Pts',(-43.4150727209207,-59.5358440364426,
-39.2223070534893));
#244026=CARTESIAN_POINT('Ctrl Pts',(-43.2883193276586,-59.4590682572254,
-39.1867578392588));
#244027=CARTESIAN_POINT('Ctrl Pts',(-43.1106712693135,-59.32658002426,-39.1324031814995));
#244028=CARTESIAN_POINT('Ctrl Pts',(-43.0005921597408,-59.2266373021163,
-39.0954660506179));
#244029=CARTESIAN_POINT('Ctrl Pts',(-42.8948534568781,-59.1207134074407,
-39.0581733199915));
#244030=CARTESIAN_POINT('Ctrl Pts',(-42.7951360401793,-59.0104958554849,
-39.0211184761739));
#244031=CARTESIAN_POINT('Ctrl Pts',(-42.6850011896347,-58.8622904152127,
-38.9753582681256));
#244032=CARTESIAN_POINT('Ctrl Pts',(-42.6055727997797,-58.7375004045667,
-38.939089851323));
#244033=CARTESIAN_POINT('Ctrl Pts',(-42.5503788594446,-58.6407591922129,
-38.9120596161462));
#244034=CARTESIAN_POINT('Ctrl Pts',(-42.5165536369311,-58.5741539171446,
-38.8941613358138));
#244035=CARTESIAN_POINT('Ctrl Pts',(-42.4842288567228,-58.5064298632496,
-38.8763157156907));
#244036=CARTESIAN_POINT('Ctrl Pts',(-42.4689425396028,-58.4722695523732,
-38.8674882509199));
#244037=CARTESIAN_POINT('Ctrl Pts',(-42.4257123024776,-58.3690064948315,
-38.8413136266604));
#244038=CARTESIAN_POINT('Ctrl Pts',(-42.3750272156063,-58.229152189777,
-38.8072100415055));
#244039=CARTESIAN_POINT('Ctrl Pts',(-42.3380647902547,-58.0850119200902,
-38.7746901633276));
#244040=CARTESIAN_POINT('Ctrl Pts',(-42.3155659796374,-57.9752818499468,
-38.7509105250088));
#244041=CARTESIAN_POINT('Ctrl Pts',(-42.3089374211558,-57.9384266221928,
-38.7430843922672));
#244042=CARTESIAN_POINT('Ctrl Pts',(-42.297458012674,-57.864178756387,-38.7276438637217));
#244043=CARTESIAN_POINT('Ctrl Pts',(-42.292601515188,-57.8267325312259,
-38.720018782004));
#244044=CARTESIAN_POINT('Ctrl Pts',(-42.2847289916893,-57.7514526301959,
-38.7050196673963));
#244045=CARTESIAN_POINT('Ctrl Pts',(-42.2817363521424,-57.7138759968928,
-38.6976962453237));
#244046=CARTESIAN_POINT('Ctrl Pts',(-42.277596992864,-57.6387184974263,
-38.6833720377019));
#244047=CARTESIAN_POINT('Ctrl Pts',(-42.2741651307842,-57.5260409596698,
-38.6623829091612));
#244048=CARTESIAN_POINT('Ctrl Pts',(-42.2805893100654,-57.3760354719141,
-38.6363740800325));
#244049=CARTESIAN_POINT('Ctrl Pts',(-42.2937061680812,-57.2637038035873,
-38.618370061439));
#244050=CARTESIAN_POINT('Ctrl Pts',(-42.3043247017591,-57.1888547452426,
-38.6067079534822));
#244051=CARTESIAN_POINT('Ctrl Pts',(-42.3105743117123,-57.1514345461221,
-38.6010450635964));
#244052=CARTESIAN_POINT('Ctrl Pts',(-42.3249704170347,-57.0766935209607,
-38.590076215021));
#244053=CARTESIAN_POINT('Ctrl Pts',(-42.3331592025312,-57.0392159768686,
-38.5847494243559));
#244054=CARTESIAN_POINT('Ctrl Pts',(-42.3512949844302,-56.9651221381903,
-38.5745673038812));
#244055=CARTESIAN_POINT('Ctrl Pts',(-42.3712216906218,-56.8916587034686,
-38.564820665347));
#244056=CARTESIAN_POINT('Ctrl Pts',(-42.4063979707918,-56.7834465224234,
-38.5515118436));
#244057=CARTESIAN_POINT('Ctrl Pts',(-42.4468320479729,-56.6771725078319,
-38.5395042677724));
#244058=CARTESIAN_POINT('Ctrl Pts',(-42.4925290654744,-56.5728473165674,
-38.5288039137004));
#244059=CARTESIAN_POINT('Ctrl Pts',(-42.5265325119253,-56.5046058456765,
-38.5225509073062));
#244060=CARTESIAN_POINT('Ctrl Pts',(-42.5623338475306,-56.4370293947697,
-38.5167461666044));
#244061=CARTESIAN_POINT('Ctrl Pts',(-42.5811223641794,-56.4035923099625,
-38.5140693065785));
#244062=CARTESIAN_POINT('Ctrl Pts',(-42.620584523009,-56.3373241998654,
-38.5091697400817));
#244063=CARTESIAN_POINT('Ctrl Pts',(-42.6411082254821,-56.3047465904101,
-38.5069659500128));
#244064=CARTESIAN_POINT('Ctrl Pts',(-42.7048067991197,-56.2090283357163,
-38.501110858935));
#244065=CARTESIAN_POINT('Ctrl Pts',(-42.7502234543428,-56.1476408662828,
-38.4981890389281));
#244066=CARTESIAN_POINT('Ctrl Pts',(-42.8467942323831,-56.0297655581676,
-38.4942910511033));
#244067=CARTESIAN_POINT('Ctrl Pts',(-42.8979715413934,-55.9732420482176,
-38.4933125989996));
#244068=CARTESIAN_POINT('Ctrl Pts',(-42.9790570553347,-55.8921695883033,
-38.4933149859729));
#244069=CARTESIAN_POINT('Ctrl Pts',(-43.0068374106561,-55.8657400908868,
-38.4935622007431));
#244070=CARTESIAN_POINT('Ctrl Pts',(-43.0495800649421,-55.8270637749536,
-38.4943063068789));
#244071=CARTESIAN_POINT('Ctrl Pts',(-43.0640222060113,-55.8143203511958,
-38.494617152342));
#244072=CARTESIAN_POINT('Ctrl Pts',(-43.0932714774893,-55.7891564261061,
-38.4953646906773));
#244073=CARTESIAN_POINT('Ctrl Pts',(-43.1080901283632,-55.7767277938553,
-38.4958020036096));
#244074=CARTESIAN_POINT('Ctrl Pts',(-43.1528523310046,-55.7401327167866,
-38.4972962980169));
#244075=CARTESIAN_POINT('Ctrl Pts',(-43.2134913856688,-55.6930468850421,
-38.4997758707861));
#244076=CARTESIAN_POINT('Ctrl Pts',(-43.3385569247743,-55.6055389451161,
-38.5066450244003));
#244077=CARTESIAN_POINT('Ctrl Pts',(-43.4691986576013,-55.5278792007279,
-38.5163302992824));
#244078=CARTESIAN_POINT('Ctrl Pts',(-43.5713395927684,-55.4769743237494,
-38.5256877381308));
#244079=CARTESIAN_POINT('Ctrl Pts',(-43.6403672861995,-55.4446857735354,
-38.5323951500278));
#244080=CARTESIAN_POINT('Ctrl Pts',(-43.6753577685123,-55.4293620157832,
-38.5359845633874));
#244081=CARTESIAN_POINT('Ctrl Pts',(-43.7462462065788,-55.4003985583156,
-38.5436333065981));
#244082=CARTESIAN_POINT('Ctrl Pts',(-43.7822717759725,-55.3867204456352,
-38.5477088862383));
#244083=CARTESIAN_POINT('Ctrl Pts',(-43.8543821738219,-55.3613797848081,
-38.5562346427694));
#244084=CARTESIAN_POINT('Ctrl Pts',(-43.890622407919,-55.349649082917,-38.5607007444526));
#244085=CARTESIAN_POINT('Ctrl Pts',(-43.9997560709039,-55.3172704656441,
-38.5746802407103));
#244086=CARTESIAN_POINT('Ctrl Pts',(-44.1098017310836,-55.290468361793,
-38.5898286859852));
#244087=CARTESIAN_POINT('Ctrl Pts',(-44.2583166685835,-55.2656490138239,
-38.612301023075));
#244088=CARTESIAN_POINT('Ctrl Pts',(-44.3705972700495,-55.2524997368729,
-38.6302900391873));
#244089=CARTESIAN_POINT('Ctrl Pts',(-44.446056048267,-55.2474029004138,
-38.6430428201589));
#244090=CARTESIAN_POINT('Ctrl Pts',(-44.5218128020516,-55.2441636366351,
-38.65617756452));
#244091=CARTESIAN_POINT('Ctrl Pts',(-44.5599089424743,-55.2434808562086,
-38.6629497802385));
#244092=CARTESIAN_POINT('Ctrl Pts',(-44.6354869543582,-55.2439911084578,
-38.6767130108817));
#244093=CARTESIAN_POINT('Ctrl Pts',(-44.6731456892459,-55.2451740103824,
-38.6837342374529));
#244094=CARTESIAN_POINT('Ctrl Pts',(-44.7481014788608,-55.2493620066237,
-38.6980304684339));
#244095=CARTESIAN_POINT('Ctrl Pts',(-44.860046548974,-55.2583760573225,
-38.7198650218829));
#244096=CARTESIAN_POINT('Ctrl Pts',(-45.0073845433675,-55.2811507310277,
-38.7505067688753));
#244097=CARTESIAN_POINT('Ctrl Pts',(-45.1528189888476,-55.3146135839333,
-38.7826550300594));
#244098=CARTESIAN_POINT('Ctrl Pts',(-45.2248832056965,-55.3349380951144,
-38.7992310848652));
#244099=CARTESIAN_POINT('Ctrl Pts',(-45.2966462681613,-55.3570913336823,
-38.8160672125853));
#244100=CARTESIAN_POINT('Ctrl Pts',(-45.3323638946335,-55.3690863290504,
-38.8246135819642));
#244101=CARTESIAN_POINT('Ctrl Pts',(-45.4027951436545,-55.3946744461232,
-38.841798196801));
#244102=CARTESIAN_POINT('Ctrl Pts',(-45.4376370321487,-55.4083060218429,
-38.85046633842));
#244103=CARTESIAN_POINT('Ctrl Pts',(-45.5409345111852,-55.4516493275196,
-38.8766665754573));
#244104=CARTESIAN_POINT('Ctrl Pts',(-45.6082182891413,-55.4838201174091,
-38.8944064774514));
#244105=CARTESIAN_POINT('Ctrl Pts',(-45.7067749877369,-55.5369855856676,
-38.9214216121435));
#244106=CARTESIAN_POINT('Ctrl Pts',(-45.7392219877795,-55.5555212114618,
-38.9304915704334));
#244107=CARTESIAN_POINT('Ctrl Pts',(-45.8033556832395,-55.5942722159849,
-38.9487787872477));
#244108=CARTESIAN_POINT('Ctrl Pts',(-45.8348443691401,-55.6143675312756,
-38.9579395118015));
#244109=CARTESIAN_POINT('Ctrl Pts',(-45.9274099842789,-55.6766589025306,
-38.9854159162723));
#244110=CARTESIAN_POINT('Ctrl Pts',(-45.9867610865919,-55.7209353156014,
-39.0037703637879));
#244111=CARTESIAN_POINT('Ctrl Pts',(-46.1007337830098,-55.8148102393793,
-39.0405190865864));
#244112=CARTESIAN_POINT('Ctrl Pts',(-46.1826971388658,-55.889219933262,
-39.0681181728269));
#244113=CARTESIAN_POINT('Ctrl Pts',(-46.259356574729,-55.9696687352924,
-39.0957737179551));
#244114=CARTESIAN_POINT('Ctrl Pts',(-46.309266807939,-56.024663053365,-39.1142236413887));
#244115=CARTESIAN_POINT('Ctrl Pts',(-46.3336138177017,-56.0528284109483,
-39.1234510495426));
#244116=CARTESIAN_POINT('Ctrl Pts',(-46.3692509284248,-56.0961546965833,
-39.1373141736981));
#244117=CARTESIAN_POINT('Ctrl Pts',(-46.3809719555493,-56.1107655250657,
-39.14193505412));
#244118=CARTESIAN_POINT('Ctrl Pts',(-46.4039850968433,-56.1401806715041,
-39.1511314768264));
#244119=CARTESIAN_POINT('Ctrl Pts',(-46.4153001903629,-56.1550126624776,
-39.1557159133813));
#244120=CARTESIAN_POINT('Ctrl Pts',(-46.4486370096885,-56.1998310060263,
-39.1694131182659));
#244121=CARTESIAN_POINT('Ctrl Pts',(-46.4700835091466,-56.2301795317326,
-39.1784826054425));
#244122=CARTESIAN_POINT('Ctrl Pts',(-46.532071913686,-56.3225583984772,
-39.2054898733524));
#244123=CARTESIAN_POINT('Ctrl Pts',(-46.5894197348374,-56.4176636744323,
-39.23211607576));
#244124=CARTESIAN_POINT('Ctrl Pts',(-46.6566074362748,-56.5498680842415,
-39.2668544229849));
#244125=CARTESIAN_POINT('Ctrl Pts',(-46.6870820302515,-56.617790568625,
-39.2839693714534));
#244126=CARTESIAN_POINT('Ctrl Pts',(-46.7159729830272,-56.6866360545619,
-39.3009558869148));
#244127=CARTESIAN_POINT('Ctrl Pts',(-46.7296188023799,-56.7214992889704,
-39.3093799218186));
#244128=CARTESIAN_POINT('Ctrl Pts',(-46.7553216997643,-56.7922546384013,
-39.3261176641085));
#244129=CARTESIAN_POINT('Ctrl Pts',(-46.7672996943011,-56.8279354881579,
-39.3343809787628));
#244130=CARTESIAN_POINT('Ctrl Pts',(-46.8004530502947,-56.9353633959568,
-39.358737163018));
#244131=CARTESIAN_POINT('Ctrl Pts',(-46.8189795501832,-57.0077635587999,
-39.3744658121213));
#244132=CARTESIAN_POINT('Ctrl Pts',(-46.848916211803,-57.1540080946302,
-39.4048998290393));
#244133=CARTESIAN_POINT('Ctrl Pts',(-46.866048617508,-57.2647966217996,
-39.4269646939479));
#244134=CARTESIAN_POINT('Ctrl Pts',(-46.875074749658,-57.3772756893033,
-39.4478819384746));
#244135=CARTESIAN_POINT('Ctrl Pts',(-46.8792542953452,-57.4526370309597,
-39.4615663943076));
#244136=CARTESIAN_POINT('Ctrl Pts',(-46.8804258736835,-57.4905390832845,
-39.4682843608713));
#244137=CARTESIAN_POINT('Ctrl Pts',(-46.8808837743635,-57.566610437341,
-39.4814341960201));
#244138=CARTESIAN_POINT('Ctrl Pts',(-46.8801708637706,-57.604491394965,
-39.4878166677226));
#244139=CARTESIAN_POINT('Ctrl Pts',(-46.8768913879562,-57.6800597985945,
-39.5002231148134));
#244140=CARTESIAN_POINT('Ctrl Pts',(-46.8691896925243,-57.7930657109158,
-39.5182849936093));
#244141=CARTESIAN_POINT('Ctrl Pts',(-46.8479069711518,-57.9423669591112,
-39.540205996752));
#244142=CARTESIAN_POINT('Ctrl Pts',(-46.8236459543104,-58.053306681129,
-39.5550278422771));
#244143=CARTESIAN_POINT('Ctrl Pts',(-46.8055990109883,-58.1270324939452,
-39.5645447403379));
#244144=CARTESIAN_POINT('Ctrl Pts',(-46.7956339676918,-58.1637938532181,
-39.5691227921436));
#244145=CARTESIAN_POINT('Ctrl Pts',(-46.7738161327052,-58.2370162077019,
-39.5779016468881));
#244146=CARTESIAN_POINT('Ctrl Pts',(-46.7619036278491,-58.2736352268715,
-39.5821192203466));
#244147=CARTESIAN_POINT('Ctrl Pts',(-46.7364059718256,-58.3458255995332,
-39.5900871854462));
#244148=CARTESIAN_POINT('Ctrl Pts',(-46.7091836493705,-58.4171862986019,
-39.5976163356366));
#244149=CARTESIAN_POINT('Ctrl Pts',(-46.663274408039,-58.5216699086648,
-39.6076014242402));
#244150=CARTESIAN_POINT('Ctrl Pts',(-46.6123207377325,-58.6236436013082,
-39.616293729045));
#244151=CARTESIAN_POINT('Ctrl Pts',(-46.5563244858032,-58.7230996041114,
-39.6236943138341));
#244152=CARTESIAN_POINT('Ctrl Pts',(-46.515607032986,-58.7877140896312,
-39.6277619492082));
#244153=CARTESIAN_POINT('Ctrl Pts',(-46.4731710833873,-58.8514710047945,
-39.6313905635194));
#244154=CARTESIAN_POINT('Ctrl Pts',(-46.4511086137465,-58.8829006319494,
-39.6329844599904));
#244155=CARTESIAN_POINT('Ctrl Pts',(-46.4051673201274,-58.9449633016888,
-39.6357273485653));
#244156=CARTESIAN_POINT('Ctrl Pts',(-46.381447994276,-58.975377588932,-39.6368662598532));
#244157=CARTESIAN_POINT('Ctrl Pts',(-46.3084068909562,-59.0643493136614,
-39.6395761233691));
#244158=CARTESIAN_POINT('Ctrl Pts',(-46.2570407846102,-59.1209150453974,
-39.6404603784325));
#244159=CARTESIAN_POINT('Ctrl Pts',(-46.1491379755941,-59.228544463199,
-39.6404138814247));
#244160=CARTESIAN_POINT('Ctrl Pts',(-46.0925836555155,-59.2796343044913,
-39.6394845811684));
#244161=CARTESIAN_POINT('Ctrl Pts',(-46.0038529437629,-59.3521266125547,
-39.6367223387528));
#244162=CARTESIAN_POINT('Ctrl Pts',(-45.9736068078661,-59.3756113554055,
-39.6355721163029));
#244163=CARTESIAN_POINT('Ctrl Pts',(-45.9272656961273,-59.4097723546528,
-39.6334997725088));
#244164=CARTESIAN_POINT('Ctrl Pts',(-45.9116419215573,-59.4209912820171,
-39.6327502808957));
#244165=CARTESIAN_POINT('Ctrl Pts',(-45.8800804794677,-59.4430610802669,
-39.6311351339295));
#244166=CARTESIAN_POINT('Ctrl Pts',(-45.8321587971618,-59.4756823489919,
-39.628531354857));
#244167=CARTESIAN_POINT('Ctrl Pts',(-45.7834097108732,-59.5062438963941,
-39.6254355071979));
#244168=CARTESIAN_POINT('Ctrl Pts',(-45.717633106262,-59.5452481912826,
-39.6208773262667));
#244169=CARTESIAN_POINT('Ctrl Pts',(-45.6178307490054,-59.601113548897,
-39.6133952897297));
#244170=CARTESIAN_POINT('Ctrl Pts',(-45.4802897643185,-59.6652183443042,
-39.6008811885904));
#244171=CARTESIAN_POINT('Ctrl Pts',(-45.3738098009101,-59.7055766782111,
-39.5896017905935));
#244172=CARTESIAN_POINT('Ctrl Pts',(-45.3020778813705,-59.7307512119865,
-39.5816566825671));
#244173=CARTESIAN_POINT('Ctrl Pts',(-45.2658207311094,-59.7424779859237,
-39.5774690651077));
#244174=CARTESIAN_POINT('Ctrl Pts',(-45.1926264675053,-59.7641596016776,
-39.5686715125846));
#244175=CARTESIAN_POINT('Ctrl Pts',(-45.1555073907618,-59.7741562512684,
-39.5640376159893));
#244176=CARTESIAN_POINT('Ctrl Pts',(-45.0441315765335,-59.8011904590316,
-39.5496210468413));
#244177=CARTESIAN_POINT('Ctrl Pts',(-44.9324484012679,-59.8224577850013,
-39.5341534065747));
#244178=CARTESIAN_POINT('Ctrl Pts',(-44.8203079610257,-59.8353953605365,
-39.5171556909205));
#244179=CARTESIAN_POINT('Ctrl Pts',(-44.7080184564226,-59.8455760612675,
-39.4996502778008));
#244180=CARTESIAN_POINT('Ctrl Pts',(-44.6329372249224,-59.8486931621852,
-39.4873001861445));
#244181=CARTESIAN_POINT('Ctrl Pts',(-44.5200834441659,-59.8478515133141,
-39.4677634802869));
#244182=CARTESIAN_POINT('Ctrl Pts',(-44.4823810871712,-59.8466449718289,
-39.4610736497974));
#244183=CARTESIAN_POINT('Ctrl Pts',(-44.4258051079382,-59.8434394706745,
-39.4507883432074));
#244184=CARTESIAN_POINT('Ctrl Pts',(-44.4069254589855,-59.8421361346926,
-39.4473147915973));
#244185=CARTESIAN_POINT('Ctrl Pts',(-44.3691376542581,-59.8390581625153,
-39.4402793331445));
#244186=CARTESIAN_POINT('Ctrl Pts',(-44.3502459350849,-59.8372838734483,
-39.4367203104461));
#244187=CARTESIAN_POINT('Ctrl Pts',(-44.2562487381671,-59.8272835659938,
-39.4188041728073));
#244188=CARTESIAN_POINT('Ctrl Pts',(-44.1080045765469,-59.8040393501646,
-39.3892226636159));
#244189=CARTESIAN_POINT('Ctrl Pts',(-43.9639303529155,-59.7668593120831,
-39.3578670379715));
#244190=CARTESIAN_POINT('Ctrl Pts',(-43.8219159040518,-59.7227861654643,
-39.3256251231267));
#244191=CARTESIAN_POINT('Ctrl Pts',(-43.7519290534068,-59.6972943066161,
-39.3090578287531));
#244192=CARTESIAN_POINT('Ctrl Pts',(-43.665783177736,-59.6610675807531,
-39.2877890488175));
#244193=CARTESIAN_POINT('Ctrl Pts',(-43.6486106666635,-59.653596197985,
-39.2835041280971));
#244194=CARTESIAN_POINT('Ctrl Pts',(-43.6144193015916,-59.6382222359849,
-39.2748825183767));
#244195=CARTESIAN_POINT('Ctrl Pts',(-43.597366582891,-59.6303022352814,
-39.2705368924251));
#244196=CARTESIAN_POINT('Ctrl Pts',(-43.5465994182959,-59.605961903298,
-39.2574616452183));
#244197=CARTESIAN_POINT('Ctrl Pts',(-43.513329300663,-59.588993111175,-39.2487085268073));
#244198=CARTESIAN_POINT('Ctrl Pts',(-43.4805771074156,-59.5712767529309,
-39.2399080357013));
#244199=CARTESIAN_POINT('Ctrl Pts',(-43.8341420587998,-57.9817357678076,
-41.1268248734572));
#244200=CARTESIAN_POINT('Ctrl Pts',(-43.8090823387197,-57.9680163597508,
-41.1092238912453));
#244201=CARTESIAN_POINT('Ctrl Pts',(-43.7605654269547,-57.9383371077444,
-41.0736746770147));
#244202=CARTESIAN_POINT('Ctrl Pts',(-43.6924895655639,-57.8872515755908,
-41.019320019256));
#244203=CARTESIAN_POINT('Ctrl Pts',(-43.6502497090231,-57.8487916199066,
-40.9823828883729));
#244204=CARTESIAN_POINT('Ctrl Pts',(-43.6096433745973,-57.8080652293815,
-40.945090157748));
#244205=CARTESIAN_POINT('Ctrl Pts',(-43.5713160673933,-57.7657212262301,
-40.9080353139296));
#244206=CARTESIAN_POINT('Ctrl Pts',(-43.5288984657655,-57.7088609123343,
-40.8622751058818));
#244207=CARTESIAN_POINT('Ctrl Pts',(-43.4982484100127,-57.6610280687967,
-40.826006689079));
#244208=CARTESIAN_POINT('Ctrl Pts',(-43.4769169762936,-57.6239677344727,
-40.798976453902));
#244209=CARTESIAN_POINT('Ctrl Pts',(-43.4638199758968,-57.5984660781933,
-40.7810781735695));
#244210=CARTESIAN_POINT('Ctrl Pts',(-43.4512904535732,-57.5725430453748,
-40.7632325534464));
#244211=CARTESIAN_POINT('Ctrl Pts',(-43.4453582046716,-57.5594707895743,
-40.7544050886758));
#244212=CARTESIAN_POINT('Ctrl Pts',(-43.4285595200757,-57.5199648485381,
-40.7282304644163));
#244213=CARTESIAN_POINT('Ctrl Pts',(-43.4088016745783,-57.4664867157472,
-40.6941268792613));
#244214=CARTESIAN_POINT('Ctrl Pts',(-43.3942530508608,-57.4114223976644,
-40.6616070010832));
#244215=CARTESIAN_POINT('Ctrl Pts',(-43.3853242538269,-57.3695231591805,
-40.6378273627645));
#244216=CARTESIAN_POINT('Ctrl Pts',(-43.3826786150667,-57.3554536366825,
-40.630001230023));
#244217=CARTESIAN_POINT('Ctrl Pts',(-43.378062215599,-57.3271160344971,
-40.6145607014775));
#244218=CARTESIAN_POINT('Ctrl Pts',(-43.3760891270041,-57.3128275119467,
-40.60693561976));
#244219=CARTESIAN_POINT('Ctrl Pts',(-43.3728422231051,-57.2841093232557,
-40.5919365051523));
#244220=CARTESIAN_POINT('Ctrl Pts',(-43.3715781643254,-57.2697777029377,
-40.5846130830795));
#244221=CARTESIAN_POINT('Ctrl Pts',(-43.3697526802575,-57.2411194243864,
-40.5702888754578));
#244222=CARTESIAN_POINT('Ctrl Pts',(-43.3680717796799,-57.1981642741791,
-40.5492997469169));
#244223=CARTESIAN_POINT('Ctrl Pts',(-43.3700185838812,-57.1410182421193,
-40.5232909177883));
#244224=CARTESIAN_POINT('Ctrl Pts',(-43.3746384661022,-57.0982543712987,
-40.505286899195));
#244225=CARTESIAN_POINT('Ctrl Pts',(-43.3784319419536,-57.0697666559562,
-40.4936247912381));
#244226=CARTESIAN_POINT('Ctrl Pts',(-43.3806866868643,-57.0555278483981,
-40.4879619013523));
#244227=CARTESIAN_POINT('Ctrl Pts',(-43.3859186984709,-57.0270949764048,
-40.476993052777));
#244228=CARTESIAN_POINT('Ctrl Pts',(-43.3889115442249,-57.0128413374093,
-40.4716662621118));
#244229=CARTESIAN_POINT('Ctrl Pts',(-43.3955695423488,-56.984668670318,
-40.4614841416371));
#244230=CARTESIAN_POINT('Ctrl Pts',(-43.4029115329907,-56.9567427536229,
-40.4517375031029));
#244231=CARTESIAN_POINT('Ctrl Pts',(-43.4159439893498,-56.915628788467,
-40.4384286813559));
#244232=CARTESIAN_POINT('Ctrl Pts',(-43.4309850942545,-56.8752725380991,
-40.4264211055283));
#244233=CARTESIAN_POINT('Ctrl Pts',(-43.4480370013178,-56.8356780486645,
-40.4157207514563));
#244234=CARTESIAN_POINT('Ctrl Pts',(-43.4607570961379,-56.8097932355363,
-40.409467745062));
#244235=CARTESIAN_POINT('Ctrl Pts',(-43.4741642201056,-56.7841683331057,
-40.4036630043601));
#244236=CARTESIAN_POINT('Ctrl Pts',(-43.4812071336048,-56.7714928975767,
-40.4009861443346));
#244237=CARTESIAN_POINT('Ctrl Pts',(-43.4960130774609,-56.7463797512019,
-40.3960865778375));
#244238=CARTESIAN_POINT('Ctrl Pts',(-43.5037198572985,-56.7340380787953,
-40.3938827877695));
#244239=CARTESIAN_POINT('Ctrl Pts',(-43.527657505214,-56.6977883833479,
-40.3880276966888));
#244240=CARTESIAN_POINT('Ctrl Pts',(-43.5447483375558,-56.6745564757614,
-40.3851058766842));
#244241=CARTESIAN_POINT('Ctrl Pts',(-43.5811328114983,-56.629979998045,
-40.3812078888591));
#244242=CARTESIAN_POINT('Ctrl Pts',(-43.6004351631962,-56.6086219171049,
-40.3802294367552));
#244243=CARTESIAN_POINT('Ctrl Pts',(-43.6310475296952,-56.578014570072,
-40.3802318237287));
#244244=CARTESIAN_POINT('Ctrl Pts',(-43.6415402048873,-56.5680413281089,
-40.3804790384992));
#244245=CARTESIAN_POINT('Ctrl Pts',(-43.6576911458811,-56.5534539772523,
-40.3812231446347));
#244246=CARTESIAN_POINT('Ctrl Pts',(-43.6631494628181,-56.5486488515781,
-40.3815339900979));
#244247=CARTESIAN_POINT('Ctrl Pts',(-43.6742063152013,-56.5391628964206,
-40.3822815284329));
#244248=CARTESIAN_POINT('Ctrl Pts',(-43.6798092119243,-56.534479009001,
-40.3827188413654));
#244249=CARTESIAN_POINT('Ctrl Pts',(-43.6967370434146,-56.5206915949946,
-40.3842131357726));
#244250=CARTESIAN_POINT('Ctrl Pts',(-43.7196778600618,-56.5029622466235,
-40.386692708542));
#244251=CARTESIAN_POINT('Ctrl Pts',(-43.7670264629127,-56.4700551612604,
-40.3935618621563));
#244252=CARTESIAN_POINT('Ctrl Pts',(-43.8165352419067,-56.4409186299576,
-40.4032471370382));
#244253=CARTESIAN_POINT('Ctrl Pts',(-43.8552784957563,-56.4218759376155,
-40.4126045758866));
#244254=CARTESIAN_POINT('Ctrl Pts',(-43.8814691350842,-56.4098116142502,
-40.4193119877837));
#244255=CARTESIAN_POINT('Ctrl Pts',(-43.8947490665381,-56.4040935548973,
-40.4229014011429));
#244256=CARTESIAN_POINT('Ctrl Pts',(-43.9216608718689,-56.3933018151258,
-40.430550144354));
#244257=CARTESIAN_POINT('Ctrl Pts',(-43.9353412421961,-56.3882139347518,
-40.434625723994));
#244258=CARTESIAN_POINT('Ctrl Pts',(-43.9627318697344,-56.3788058930362,
-40.4431514805252));
#244259=CARTESIAN_POINT('Ctrl Pts',(-43.9765011076412,-56.3744602994329,
-40.4476175822086));
#244260=CARTESIAN_POINT('Ctrl Pts',(-44.0179764085085,-56.3624961934912,
-40.4615970784657));
#244261=CARTESIAN_POINT('Ctrl Pts',(-44.0598195105868,-56.3526585058303,
-40.4767455237411));
#244262=CARTESIAN_POINT('Ctrl Pts',(-44.1163310625808,-56.3437038269143,
-40.4992178608308));
#244263=CARTESIAN_POINT('Ctrl Pts',(-44.1590753545772,-56.3390714325247,
-40.5172068769433));
#244264=CARTESIAN_POINT('Ctrl Pts',(-44.1878153726385,-56.337382052278,
-40.5299596579145));
#244265=CARTESIAN_POINT('Ctrl Pts',(-44.2166756293141,-56.3364007867548,
-40.5430944022758));
#244266=CARTESIAN_POINT('Ctrl Pts',(-44.2311921171808,-56.3362675100036,
-40.5498666179945));
#244267=CARTESIAN_POINT('Ctrl Pts',(-44.2599977007373,-56.3367129587916,
-40.5636298486377));
#244268=CARTESIAN_POINT('Ctrl Pts',(-44.2743541649932,-56.3372884158027,
-40.5706510752088));
#244269=CARTESIAN_POINT('Ctrl Pts',(-44.3029357424357,-56.3391317429585,
-40.5849473061899));
#244270=CARTESIAN_POINT('Ctrl Pts',(-44.3456316213443,-56.3429350642169,
-40.6067818596389));
#244271=CARTESIAN_POINT('Ctrl Pts',(-44.4018650235691,-56.3520939287388,
-40.6374236066311));
#244272=CARTESIAN_POINT('Ctrl Pts',(-44.4574103376146,-56.3653147883305,
-40.6695718678152));
#244273=CARTESIAN_POINT('Ctrl Pts',(-44.4849466005937,-56.3732907222196,
-40.686147922621));
#244274=CARTESIAN_POINT('Ctrl Pts',(-44.512374392093,-56.3819617528141,
-40.7029840503412));
#244275=CARTESIAN_POINT('Ctrl Pts',(-44.5260289861432,-56.3866462995878,
-40.7115304197201));
#244276=CARTESIAN_POINT('Ctrl Pts',(-44.5529609776699,-56.3966203919845,
-40.7287150345567));
#244277=CARTESIAN_POINT('Ctrl Pts',(-44.5662873943758,-56.4019250012471,
-40.737383176176));
#244278=CARTESIAN_POINT('Ctrl Pts',(-44.6058068395674,-56.4187668411382,
-40.7635834132132));
#244279=CARTESIAN_POINT('Ctrl Pts',(-44.6315615859976,-56.4312362585519,
-40.7813233152079));
#244280=CARTESIAN_POINT('Ctrl Pts',(-44.6693071486035,-56.4518014713652,
-40.8083384498991));
#244281=CARTESIAN_POINT('Ctrl Pts',(-44.6817372625133,-56.458965010373,
-40.8174084081892));
#244282=CARTESIAN_POINT('Ctrl Pts',(-44.7063132537473,-56.473929075182,
-40.8356956250034));
#244283=CARTESIAN_POINT('Ctrl Pts',(-44.7183832523531,-56.4816832398284,
-40.8448563495594));
#244284=CARTESIAN_POINT('Ctrl Pts',(-44.7538754102704,-56.505703003501,
-40.8723327540241));
#244285=CARTESIAN_POINT('Ctrl Pts',(-44.7766465418209,-56.5227549736834,
-40.8906872015444));
#244286=CARTESIAN_POINT('Ctrl Pts',(-44.8204030914552,-56.5588699415109,
-40.9274359243417));
#244287=CARTESIAN_POINT('Ctrl Pts',(-44.851893062885,-56.5874690797881,
-40.9550350105826));
#244288=CARTESIAN_POINT('Ctrl Pts',(-44.8813802932551,-56.6183507815631,
-40.982690555711));
#244289=CARTESIAN_POINT('Ctrl Pts',(-44.9005867815582,-56.6394533348067,
-41.0011404791447));
#244290=CARTESIAN_POINT('Ctrl Pts',(-44.9099603095753,-56.6502571213647,
-41.0103678872986));
#244291=CARTESIAN_POINT('Ctrl Pts',(-44.9236872082217,-56.6668706184025,
-41.0242310114538));
#244292=CARTESIAN_POINT('Ctrl Pts',(-44.9282031316495,-56.6724722064122,
-41.0288518918758));
#244293=CARTESIAN_POINT('Ctrl Pts',(-44.9370720489983,-56.6837477093971,
-41.038048314582));
#244294=CARTESIAN_POINT('Ctrl Pts',(-44.9414338933841,-56.6894322363092,
-41.0426327511372));
#244295=CARTESIAN_POINT('Ctrl Pts',(-44.9542884395491,-56.7066066663578,
-41.0563299560217));
#244296=CARTESIAN_POINT('Ctrl Pts',(-44.9625629539304,-56.7182326826763,
-41.0653994431984));
#244297=CARTESIAN_POINT('Ctrl Pts',(-44.9864941991718,-56.7536111473724,
-41.0924067111081));
#244298=CARTESIAN_POINT('Ctrl Pts',(-45.0086645271567,-56.7900134244028,
-41.1190329135161));
#244299=CARTESIAN_POINT('Ctrl Pts',(-45.034704630644,-56.8405768845403,
-41.1537712607408));
#244300=CARTESIAN_POINT('Ctrl Pts',(-45.0465408860903,-56.8665423758261,
-41.1708862092094));
#244301=CARTESIAN_POINT('Ctrl Pts',(-45.0577761134165,-56.8928546179869,
-41.1878727246706));
#244302=CARTESIAN_POINT('Ctrl Pts',(-45.0630901582258,-56.906176087846,
-41.1962967595746));
#244303=CARTESIAN_POINT('Ctrl Pts',(-45.0731156002939,-56.9332061371524,
-41.2130345018643));
#244304=CARTESIAN_POINT('Ctrl Pts',(-45.0777961712447,-56.9468340019015,
-41.2212978165198));
#244305=CARTESIAN_POINT('Ctrl Pts',(-45.0907786540592,-56.9878560258786,
-41.2456540007716));
#244306=CARTESIAN_POINT('Ctrl Pts',(-45.0980724298404,-57.0154910056487,
-41.2613826498774));
#244307=CARTESIAN_POINT('Ctrl Pts',(-45.1099506000897,-57.0712899900431,
-41.2918166667949));
#244308=CARTESIAN_POINT('Ctrl Pts',(-45.1168338059478,-57.11354441615,-41.3138815317038));
#244309=CARTESIAN_POINT('Ctrl Pts',(-45.1206309792415,-57.1564190282566,
-41.3347987762303));
#244310=CARTESIAN_POINT('Ctrl Pts',(-45.1224627479043,-57.1851396939165,
-41.3484832320635));
#244311=CARTESIAN_POINT('Ctrl Pts',(-45.1230291819396,-57.199581674993,
-41.3552011986272));
#244312=CARTESIAN_POINT('Ctrl Pts',(-45.1234439819388,-57.2285619504273,
-41.3683510337761));
#244313=CARTESIAN_POINT('Ctrl Pts',(-45.1232917301137,-57.2429904040975,
-41.3747335054784));
#244314=CARTESIAN_POINT('Ctrl Pts',(-45.122279779691,-57.2717682086368,
-41.3871399525693));
#244315=CARTESIAN_POINT('Ctrl Pts',(-45.1196997436484,-57.3147947598186,
-41.4052018313649));
#244316=CARTESIAN_POINT('Ctrl Pts',(-45.1120557453653,-57.3716084168758,
-41.4271228345082));
#244317=CARTESIAN_POINT('Ctrl Pts',(-45.1031553338884,-57.4137999065974,
-41.4419446800329));
#244318=CARTESIAN_POINT('Ctrl Pts',(-45.09650693546,-57.4418330021969,-41.4514615780937));
#244319=CARTESIAN_POINT('Ctrl Pts',(-45.092823442876,-57.4558081403435,
-41.4560396298995));
#244320=CARTESIAN_POINT('Ctrl Pts',(-45.08473584999,-57.4836385233421,-41.464818484644));
#244321=CARTESIAN_POINT('Ctrl Pts',(-45.0803094818206,-57.4975537933777,
-41.4690360581021));
#244322=CARTESIAN_POINT('Ctrl Pts',(-45.0708158371377,-57.5249803724867,
-41.4770040232021));
#244323=CARTESIAN_POINT('Ctrl Pts',(-45.060662137239,-57.5520858826269,
-41.4845331733926));
#244324=CARTESIAN_POINT('Ctrl Pts',(-45.0434887903859,-57.591755117417,
-41.4945182619959));
#244325=CARTESIAN_POINT('Ctrl Pts',(-45.0243848727922,-57.6304534586566,
-41.5032105668009));
#244326=CARTESIAN_POINT('Ctrl Pts',(-45.0033512023575,-57.6681778817651,
-41.51061115159));
#244327=CARTESIAN_POINT('Ctrl Pts',(-44.9880328234845,-57.692673879575,
-41.5146787869643));
#244328=CARTESIAN_POINT('Ctrl Pts',(-44.9720568870916,-57.7168380825906,
-41.5183074012753));
#244329=CARTESIAN_POINT('Ctrl Pts',(-44.9637457009402,-57.7287466936453,
-41.5199012977462));
#244330=CARTESIAN_POINT('Ctrl Pts',(-44.9464287138105,-57.7522550306847,
-41.5226441863212));
#244331=CARTESIAN_POINT('Ctrl Pts',(-44.9374830238235,-57.7637718882179,
-41.5237830976086));
#244332=CARTESIAN_POINT('Ctrl Pts',(-44.9099214446927,-57.7974515399035,
-41.5264929611258));
#244333=CARTESIAN_POINT('Ctrl Pts',(-44.8905204729439,-57.8188493934961,
-41.5273772161885));
#244334=CARTESIAN_POINT('Ctrl Pts',(-44.8497318000032,-57.8595330722204,
-41.5273307191807));
#244335=CARTESIAN_POINT('Ctrl Pts',(-44.8283374647208,-57.878828810327,
-41.5264014189239));
#244336=CARTESIAN_POINT('Ctrl Pts',(-44.7947479986672,-57.9061820008563,
-41.5236391765087));
#244337=CARTESIAN_POINT('Ctrl Pts',(-44.7832945060713,-57.9150388128137,
-41.5224889540588));
#244338=CARTESIAN_POINT('Ctrl Pts',(-44.7657408175914,-57.9279147771907,
-41.5204166102647));
#244339=CARTESIAN_POINT('Ctrl Pts',(-44.7598217545323,-57.9321421746299,
-41.5196671186517));
#244340=CARTESIAN_POINT('Ctrl Pts',(-44.7478629508254,-57.9404557426351,
-41.5180519716851));
#244341=CARTESIAN_POINT('Ctrl Pts',(-44.7297025277655,-57.9527400844071,
-41.5154481926132));
#244342=CARTESIAN_POINT('Ctrl Pts',(-44.711220794734,-57.9642369190977,
-41.5123523449538));
#244343=CARTESIAN_POINT('Ctrl Pts',(-44.6862770262529,-57.9788987855805,
-41.5077941640223));
#244344=CARTESIAN_POINT('Ctrl Pts',(-44.6484202704456,-57.9998814948776,
-41.5003121274858));
#244345=CARTESIAN_POINT('Ctrl Pts',(-44.5962108390282,-58.0238874022289,
-41.4877980263462));
#244346=CARTESIAN_POINT('Ctrl Pts',(-44.5557649369164,-58.0389385823793,
-41.4765186283493));
#244347=CARTESIAN_POINT('Ctrl Pts',(-44.5285120653069,-58.048310487242,
-41.4685735203231));
#244348=CARTESIAN_POINT('Ctrl Pts',(-44.5147341086114,-58.0526671867402,
-41.4643859028639));
#244349=CARTESIAN_POINT('Ctrl Pts',(-44.4869140318333,-58.0607029371288,
-41.4555883503401));
#244350=CARTESIAN_POINT('Ctrl Pts',(-44.4728027150897,-58.0643973546439,
-41.4509544537452));
#244351=CARTESIAN_POINT('Ctrl Pts',(-44.4304531283686,-58.0743536715507,
-41.4365378845966));
#244352=CARTESIAN_POINT('Ctrl Pts',(-44.3879697631396,-58.0821103913619,
-41.4210702443308));
#244353=CARTESIAN_POINT('Ctrl Pts',(-44.3452880889881,-58.0866896268435,
-41.4040725286766));
#244354=CARTESIAN_POINT('Ctrl Pts',(-44.3025416355467,-58.090217180745,
-41.3865671155567));
#244355=CARTESIAN_POINT('Ctrl Pts',(-44.2739489581488,-58.0911687787978,
-41.3742170239002));
#244356=CARTESIAN_POINT('Ctrl Pts',(-44.2309555122234,-58.090491506171,
-41.3546803180427));
#244357=CARTESIAN_POINT('Ctrl Pts',(-44.2165895018292,-58.0899123697243,
-41.347990487553));
#244358=CARTESIAN_POINT('Ctrl Pts',(-44.1950278537333,-58.0885113544661,
-41.337705180963));
#244359=CARTESIAN_POINT('Ctrl Pts',(-44.1878319550126,-58.0879547296283,
-41.3342316293533));
#244360=CARTESIAN_POINT('Ctrl Pts',(-44.1734279164018,-58.0866616594573,
-41.3271961709002));
#244361=CARTESIAN_POINT('Ctrl Pts',(-44.1662260389348,-58.0859253983809,
-41.3236371482021));
#244362=CARTESIAN_POINT('Ctrl Pts',(-44.130389101081,-58.0818150523559,
-41.3057210105631));
#244363=CARTESIAN_POINT('Ctrl Pts',(-44.073848260417,-58.0724828543971,
-41.2761395013722));
#244364=CARTESIAN_POINT('Ctrl Pts',(-44.0188545174212,-58.0578491440998,
-41.2447838757269));
#244365=CARTESIAN_POINT('Ctrl Pts',(-43.9646246641704,-58.0405931079736,
-41.2125419608827));
#244366=CARTESIAN_POINT('Ctrl Pts',(-43.9378880325505,-58.0306505669816,
-41.1959746665064));
#244367=CARTESIAN_POINT('Ctrl Pts',(-43.9049634769563,-58.0165631445999,
-41.174705886574));
#244368=CARTESIAN_POINT('Ctrl Pts',(-43.898399460067,-58.0136596367661,
-41.1704209658528));
#244369=CARTESIAN_POINT('Ctrl Pts',(-43.8853286348063,-58.0076886655405,
-41.1617993561325));
#244370=CARTESIAN_POINT('Ctrl Pts',(-43.8788088737381,-58.0046144513738,
-41.157453730181));
#244371=CARTESIAN_POINT('Ctrl Pts',(-43.8593967360427,-57.9951717320096,
-41.1443784829743));
#244372=CARTESIAN_POINT('Ctrl Pts',(-43.8466719188398,-57.9885954718361,
-41.1356253645631));
#244373=CARTESIAN_POINT('Ctrl Pts',(-43.8341420587998,-57.9817357678076,
-41.1268248734572));
#244374=CARTESIAN_POINT('',(-43.4124018854943,-55.8022015878058,-38.9060745433569));
#244375=CARTESIAN_POINT('',(-42.5465470395476,-57.084443392074,-38.9933901058265));
#244376=CARTESIAN_POINT('Ctrl Pts',(-43.412401749244,-55.8022014449206,
-38.9060739147518));
#244377=CARTESIAN_POINT('Ctrl Pts',(-43.4091603539247,-55.8043237908914,
-38.905838575256));
#244378=CARTESIAN_POINT('Ctrl Pts',(-43.405924519186,-55.8064559313723,
-38.9056064596797));
#244379=CARTESIAN_POINT('Ctrl Pts',(-43.4026942423849,-55.8085978727799,
-38.9053775693585));
#244380=CARTESIAN_POINT('Ctrl Pts',(-43.37514439206,-55.8268657082684,-38.9034254474569));
#244381=CARTESIAN_POINT('Ctrl Pts',(-43.3479995130707,-55.8458475490097,
-38.9017082880385));
#244382=CARTESIAN_POINT('Ctrl Pts',(-43.3212654553579,-55.8655537371234,
-38.9002297378292));
#244383=CARTESIAN_POINT('Ctrl Pts',(-43.2945313976451,-55.8852599252372,
-38.89875118762));
#244384=CARTESIAN_POINT('Ctrl Pts',(-43.2682103054482,-55.9056892935197,
-38.8975114527738));
#244385=CARTESIAN_POINT('Ctrl Pts',(-43.2423046180206,-55.9268610072553,
-38.8965152565023));
#244386=CARTESIAN_POINT('Ctrl Pts',(-43.2293517743068,-55.9374468641231,
-38.8960171583666));
#244387=CARTESIAN_POINT('Ctrl Pts',(-43.2164877853448,-55.9482328356115,
-38.8955798454342));
#244388=CARTESIAN_POINT('Ctrl Pts',(-43.2037924561014,-55.9591521490568,
-38.8952060762666));
#244389=CARTESIAN_POINT('Ctrl Pts',(-43.191097126858,-55.9700714625021,
-38.894832307099));
#244390=CARTESIAN_POINT('Ctrl Pts',(-43.1785604553322,-55.9811311728431,
-38.8945214616358));
#244391=CARTESIAN_POINT('Ctrl Pts',(-43.1661929384724,-55.9923201879255,
-38.8942734262572));
#244392=CARTESIAN_POINT('Ctrl Pts',(-43.1414579047527,-56.0146982180903,
-38.8937773555001));
#244393=CARTESIAN_POINT('Ctrl Pts',(-43.117344267243,-56.0376373429099,
-38.8935301407298));
#244394=CARTESIAN_POINT('Ctrl Pts',(-43.0938842149535,-56.0610936119007,
-38.893529345072));
#244395=CARTESIAN_POINT('Ctrl Pts',(-43.0469641103745,-56.1080061498824,
-38.8935277537564));
#244396=CARTESIAN_POINT('Ctrl Pts',(-43.0025474813891,-56.1570710705973,
-38.8945062058602));
#244397=CARTESIAN_POINT('Ctrl Pts',(-42.9606448514092,-56.2082353818757,
-38.8964551997726));
#244398=CARTESIAN_POINT('Ctrl Pts',(-42.9187422214293,-56.2593996931541,
-38.8984041936851));
#244399=CARTESIAN_POINT('Ctrl Pts',(-42.8793334746424,-56.3126943660298,
-38.9013260136914));
#244400=CARTESIAN_POINT('Ctrl Pts',(-42.8424899550942,-56.3680976795844,
-38.9052294077438));
#244401=CARTESIAN_POINT('Ctrl Pts',(-42.8240681953201,-56.3957993363617,
-38.9071811047699));
#244402=CARTESIAN_POINT('Ctrl Pts',(-42.8062629627728,-56.4240849025666,
-38.9093848948387));
#244403=CARTESIAN_POINT('Ctrl Pts',(-42.7891466755666,-56.452854472693,
-38.9118346780871));
#244404=CARTESIAN_POINT('Ctrl Pts',(-42.7720303883604,-56.4816240428195,
-38.9142844613354));
#244405=CARTESIAN_POINT('Ctrl Pts',(-42.7557331147215,-56.5106575807864,
-38.9169613213614));
#244406=CARTESIAN_POINT('Ctrl Pts',(-42.7402073536177,-56.5399968434848,
-38.9198636917123));
#244407=CARTESIAN_POINT('Ctrl Pts',(-42.7246815925139,-56.5693361061833,
-38.9227660620632));
#244408=CARTESIAN_POINT('Ctrl Pts',(-42.7099369818181,-56.5989648901808,
-38.9258925623446));
#244409=CARTESIAN_POINT('Ctrl Pts',(-42.6959610908403,-56.6288786279515,
-38.9292392096901));
#244410=CARTESIAN_POINT('Ctrl Pts',(-42.6819851998625,-56.6587923657221,
-38.9325858570355));
#244411=CARTESIAN_POINT('Ctrl Pts',(-42.6687780682593,-56.6889910719312,
-38.9361526631523));
#244412=CARTESIAN_POINT('Ctrl Pts',(-42.6563331490266,-56.719472363895,
-38.9399372898988));
#244413=CARTESIAN_POINT('Ctrl Pts',(-42.643888229794,-56.7499536558588,
-38.9437219166453));
#244414=CARTESIAN_POINT('Ctrl Pts',(-42.6322055381297,-56.7807175391602,
-38.9477243688907));
#244415=CARTESIAN_POINT('Ctrl Pts',(-42.6212841673493,-56.8117637261138,
-38.9519438796553));
#244416=CARTESIAN_POINT('Ctrl Pts',(-42.6103627965688,-56.8428099130675,
-38.9561633904199));
#244417=CARTESIAN_POINT('Ctrl Pts',(-42.6002027387397,-56.8741384006643,
-38.9605999581383));
#244418=CARTESIAN_POINT('Ctrl Pts',(-42.5908086952621,-56.9057509847877,
-38.9652543723165));
#244419=CARTESIAN_POINT('Ctrl Pts',(-42.5814146517845,-56.9373635689111,
-38.9699087864947));
#244420=CARTESIAN_POINT('Ctrl Pts',(-42.5727856698931,-56.9692679586228,
-38.9747824586382));
#244421=CARTESIAN_POINT('Ctrl Pts',(-42.5649349981973,-57.0014449365778,
-38.9798735188755));
#244422=CARTESIAN_POINT('Ctrl Pts',(-42.5582279477202,-57.0289346372945,
-38.9842229553717));
#244423=CARTESIAN_POINT('Ctrl Pts',(-42.5520784846546,-57.0566978718422,
-38.9887444451878));
#244424=CARTESIAN_POINT('Ctrl Pts',(-42.5465468336536,-57.0844434303275,
-38.9933892883181));
#244425=CARTESIAN_POINT('Ctrl Pts',(-43.4124020554461,-55.8022017898837,
-38.9060751583925));
#244426=CARTESIAN_POINT('Ctrl Pts',(-43.3061848450385,-55.8790363393388,
-38.9101809968017));
#244427=CARTESIAN_POINT('Ctrl Pts',(-43.2069727235914,-55.9648033290264,
-38.9151474711616));
#244428=CARTESIAN_POINT('Ctrl Pts',(-43.031358609741,-56.1455355255316,
-38.9261117869001));
#244429=CARTESIAN_POINT('Ctrl Pts',(-42.9541369537678,-56.2389770816702,
-38.9319838163158));
#244430=CARTESIAN_POINT('Ctrl Pts',(-42.8824499129319,-56.3415276713087,
-38.9385899207548));
#244431=CARTESIAN_POINT('Ctrl Pts',(-42.880249864589,-56.3446921073219,
-38.9387939270245));
#244432=CARTESIAN_POINT('Ctrl Pts',(-42.8735245664188,-56.3544183519727,
-38.93942145924));
#244433=CARTESIAN_POINT('Ctrl Pts',(-42.8690260301994,-56.3609982673211,
-38.9398466822262));
#244434=CARTESIAN_POINT('Ctrl Pts',(-42.7971306143081,-56.4673582778772,
-38.9467316408428));
#244435=CARTESIAN_POINT('Ctrl Pts',(-42.7376562988331,-56.5724855808993,
-38.9536292675083));
#244436=CARTESIAN_POINT('Ctrl Pts',(-42.6273438404767,-56.8117291221827,
-38.971053016757));
#244437=CARTESIAN_POINT('Ctrl Pts',(-42.5803525009342,-56.9465451572024,
-38.9817005915576));
#244438=CARTESIAN_POINT('Ctrl Pts',(-42.5465476043924,-57.084443479682,
-38.9933907057792));
#244439=CARTESIAN_POINT('Ctrl Pts',(-44.5079524583208,-59.1441977614012,
-52.99995));
#244440=CARTESIAN_POINT('Ctrl Pts',(-43.5445019199415,-59.1441977614012,
-52.9416166666667));
#244441=CARTESIAN_POINT('Ctrl Pts',(-43.0627766507519,-58.309825119875,
-52.8832833333334));
#244442=CARTESIAN_POINT('Ctrl Pts',(-42.5810513815623,-57.4754524783487,
-52.82495));
#244443=CARTESIAN_POINT('Ctrl Pts',(-43.0627766507519,-56.6410798368225,
-52.7666166666667));
#244444=CARTESIAN_POINT('Ctrl Pts',(-43.5445019199415,-55.8067071952963,
-52.7082833333333));
#244445=CARTESIAN_POINT('Ctrl Pts',(-44.5079524583208,-55.8067071952963,
-52.64995));
#244446=CARTESIAN_POINT('Ctrl Pts',(-45.4714029967,-55.8067071952963,-52.5916166666666));
#244447=CARTESIAN_POINT('Ctrl Pts',(-45.9531282658897,-56.6410798368225,
-52.5332833333334));
#244448=CARTESIAN_POINT('Ctrl Pts',(-46.4348535350793,-57.4754524783487,
-52.4749500000001));
#244449=CARTESIAN_POINT('Ctrl Pts',(-45.9531282658897,-58.309825119875,
-52.4166166666667));
#244450=CARTESIAN_POINT('Ctrl Pts',(-45.4714029967,-59.1441977614012,-52.3582833333334));
#244451=CARTESIAN_POINT('Ctrl Pts',(-44.5079524583208,-59.1441977614012,
-52.29995));
#244452=CARTESIAN_POINT('Ctrl Pts',(-43.5445019199415,-59.1441977614012,
-52.2416166666667));
#244453=CARTESIAN_POINT('Ctrl Pts',(-43.0627766507519,-58.309825119875,
-52.1832833333333));
#244454=CARTESIAN_POINT('Ctrl Pts',(-42.5810513815623,-57.4754524783487,
-52.12495));
#244455=CARTESIAN_POINT('Ctrl Pts',(-43.0627766507519,-56.6410798368225,
-52.0666166666667));
#244456=CARTESIAN_POINT('Ctrl Pts',(-43.5445019199415,-55.8067071952963,
-52.0082833333333));
#244457=CARTESIAN_POINT('Ctrl Pts',(-44.5079524583208,-55.8067071952963,
-51.94995));
#244458=CARTESIAN_POINT('Ctrl Pts',(-45.4714029967,-55.8067071952963,-51.8916166666667));
#244459=CARTESIAN_POINT('Ctrl Pts',(-45.9531282658897,-56.6410798368225,
-51.8332833333334));
#244460=CARTESIAN_POINT('Ctrl Pts',(-46.4348535350793,-57.4754524783487,
-51.77495));
#244461=CARTESIAN_POINT('Ctrl Pts',(-45.9531282658897,-58.309825119875,
-51.7166166666667));
#244462=CARTESIAN_POINT('Ctrl Pts',(-45.4714029967,-59.1441977614012,-51.6582833333333));
#244463=CARTESIAN_POINT('Ctrl Pts',(-44.5079524583208,-59.1441977614012,
-51.59995));
#244464=CARTESIAN_POINT('Ctrl Pts',(-43.5445019199415,-59.1441977614012,
-51.5416166666667));
#244465=CARTESIAN_POINT('Ctrl Pts',(-43.0627766507519,-58.309825119875,
-51.4832833333334));
#244466=CARTESIAN_POINT('Ctrl Pts',(-42.5810513815623,-57.4754524783487,
-51.42495));
#244467=CARTESIAN_POINT('Ctrl Pts',(-43.0627766507519,-56.6410798368225,
-51.3666166666667));
#244468=CARTESIAN_POINT('Ctrl Pts',(-43.5445019199415,-55.8067071952963,
-51.3082833333333));
#244469=CARTESIAN_POINT('Ctrl Pts',(-44.5079524583208,-55.8067071952963,
-51.24995));
#244470=CARTESIAN_POINT('Ctrl Pts',(-45.4714029967,-55.8067071952963,-51.1916166666667));
#244471=CARTESIAN_POINT('Ctrl Pts',(-45.9531282658897,-56.6410798368225,
-51.1332833333334));
#244472=CARTESIAN_POINT('Ctrl Pts',(-46.4348535350793,-57.4754524783487,
-51.07495));
#244473=CARTESIAN_POINT('Ctrl Pts',(-45.9531282658897,-58.309825119875,
-51.0166166666667));
#244474=CARTESIAN_POINT('Ctrl Pts',(-45.4714029967,-59.1441977614012,-50.9582833333334));
#244475=CARTESIAN_POINT('Ctrl Pts',(-44.5079524583208,-59.1441977614012,
-50.89995));
#244476=CARTESIAN_POINT('Ctrl Pts',(-43.5445019199415,-59.1441977614012,
-50.8416166666667));
#244477=CARTESIAN_POINT('Ctrl Pts',(-43.0627766507519,-58.309825119875,
-50.7832833333333));
#244478=CARTESIAN_POINT('Ctrl Pts',(-42.5810513815623,-57.4754524783487,
-50.72495));
#244479=CARTESIAN_POINT('Ctrl Pts',(-43.0627766507519,-56.6410798368225,
-50.6666166666667));
#244480=CARTESIAN_POINT('Ctrl Pts',(-43.5445019199415,-55.8067071952963,
-50.6082833333334));
#244481=CARTESIAN_POINT('Ctrl Pts',(-44.5079524583208,-55.8067071952963,
-50.54995));
#244482=CARTESIAN_POINT('Ctrl Pts',(-45.4714029967,-55.8067071952963,-50.4916166666667));
#244483=CARTESIAN_POINT('Ctrl Pts',(-45.9531282658897,-56.6410798368225,
-50.4332833333333));
#244484=CARTESIAN_POINT('Ctrl Pts',(-46.4348535350793,-57.4754524783487,
-50.37495));
#244485=CARTESIAN_POINT('Ctrl Pts',(-45.9531282658897,-58.309825119875,
-50.3166166666667));
#244486=CARTESIAN_POINT('Ctrl Pts',(-45.4714029967,-59.1441977614012,-50.2582833333334));
#244487=CARTESIAN_POINT('Ctrl Pts',(-44.5079524583208,-59.1441977614012,
-50.19995));
#244488=CARTESIAN_POINT('Ctrl Pts',(-43.5445019199415,-59.1441977614012,
-50.1416166666667));
#244489=CARTESIAN_POINT('Ctrl Pts',(-43.0627766507519,-58.309825119875,
-50.0832833333334));
#244490=CARTESIAN_POINT('Ctrl Pts',(-42.5810513815623,-57.4754524783487,
-50.02495));
#244491=CARTESIAN_POINT('Ctrl Pts',(-43.0627766507519,-56.6410798368225,
-49.9666166666667));
#244492=CARTESIAN_POINT('Ctrl Pts',(-43.5445019199415,-55.8067071952963,
-49.9082833333334));
#244493=CARTESIAN_POINT('Ctrl Pts',(-44.5079524583208,-55.8067071952963,
-49.84995));
#244494=CARTESIAN_POINT('Ctrl Pts',(-45.4714029967,-55.8067071952963,-49.7916166666667));
#244495=CARTESIAN_POINT('Ctrl Pts',(-45.9531282658897,-56.6410798368225,
-49.7332833333334));
#244496=CARTESIAN_POINT('Ctrl Pts',(-46.4348535350793,-57.4754524783487,
-49.67495));
#244497=CARTESIAN_POINT('Ctrl Pts',(-45.9531282658897,-58.309825119875,
-49.6166166666667));
#244498=CARTESIAN_POINT('Ctrl Pts',(-45.4714029967,-59.1441977614012,-49.5582833333334));
#244499=CARTESIAN_POINT('Ctrl Pts',(-44.5079524583208,-59.1441977614012,
-49.49995));
#244500=CARTESIAN_POINT('Ctrl Pts',(-43.5445019199415,-59.1441977614012,
-49.4416166666667));
#244501=CARTESIAN_POINT('Ctrl Pts',(-43.0627766507519,-58.309825119875,
-49.3832833333334));
#244502=CARTESIAN_POINT('Ctrl Pts',(-42.5810513815623,-57.4754524783487,
-49.32495));
#244503=CARTESIAN_POINT('Ctrl Pts',(-43.0627766507519,-56.6410798368225,
-49.2666166666667));
#244504=CARTESIAN_POINT('Ctrl Pts',(-43.5445019199415,-55.8067071952963,
-49.2082833333334));
#244505=CARTESIAN_POINT('Ctrl Pts',(-44.5079524583208,-55.8067071952963,
-49.14995));
#244506=CARTESIAN_POINT('Ctrl Pts',(-45.4714029967,-55.8067071952963,-49.0916166666667));
#244507=CARTESIAN_POINT('Ctrl Pts',(-45.9531282658897,-56.6410798368225,
-49.0332833333333));
#244508=CARTESIAN_POINT('Ctrl Pts',(-46.4348535350793,-57.4754524783487,
-48.97495));
#244509=CARTESIAN_POINT('Ctrl Pts',(-45.9531282658897,-58.309825119875,
-48.9166166666667));
#244510=CARTESIAN_POINT('Ctrl Pts',(-45.4714029967,-59.1441977614012,-48.8582833333333));
#244511=CARTESIAN_POINT('Ctrl Pts',(-44.5079524583208,-59.1441977614012,
-48.79995));
#244512=CARTESIAN_POINT('Ctrl Pts',(-43.5445019199415,-59.1441977614012,
-48.7416166666667));
#244513=CARTESIAN_POINT('Ctrl Pts',(-43.0627766507519,-58.309825119875,
-48.6832833333334));
#244514=CARTESIAN_POINT('Ctrl Pts',(-42.5810513815623,-57.4754524783487,
-48.62495));
#244515=CARTESIAN_POINT('Ctrl Pts',(-43.0627766507519,-56.6410798368225,
-48.5666166666667));
#244516=CARTESIAN_POINT('Ctrl Pts',(-43.5445019199415,-55.8067071952963,
-48.5082833333334));
#244517=CARTESIAN_POINT('Ctrl Pts',(-44.5079524583208,-55.8067071952963,
-48.44995));
#244518=CARTESIAN_POINT('Ctrl Pts',(-45.4714029967,-55.8067071952963,-48.3916166666667));
#244519=CARTESIAN_POINT('Ctrl Pts',(-45.9531282658897,-56.6410798368225,
-48.3332833333334));
#244520=CARTESIAN_POINT('Ctrl Pts',(-46.4348535350793,-57.4754524783487,
-48.27495));
#244521=CARTESIAN_POINT('Ctrl Pts',(-45.9531282658897,-58.309825119875,
-48.2166166666667));
#244522=CARTESIAN_POINT('Ctrl Pts',(-45.4714029967,-59.1441977614012,-48.1582833333334));
#244523=CARTESIAN_POINT('Ctrl Pts',(-44.5079524583208,-59.1441977614012,
-48.09995));
#244524=CARTESIAN_POINT('Ctrl Pts',(-43.5445019199415,-59.1441977614012,
-48.0416166666667));
#244525=CARTESIAN_POINT('Ctrl Pts',(-43.0627766507519,-58.309825119875,
-47.9832833333334));
#244526=CARTESIAN_POINT('Ctrl Pts',(-42.5810513815623,-57.4754524783487,
-47.92495));
#244527=CARTESIAN_POINT('Ctrl Pts',(-43.0627766507519,-56.6410798368225,
-47.8666166666667));
#244528=CARTESIAN_POINT('Ctrl Pts',(-43.5445019199415,-55.8067071952963,
-47.8082833333333));
#244529=CARTESIAN_POINT('Ctrl Pts',(-44.5079524583208,-55.8067071952963,
-47.74995));
#244530=CARTESIAN_POINT('Ctrl Pts',(-45.4714029967,-55.8067071952963,-47.6916166666667));
#244531=CARTESIAN_POINT('Ctrl Pts',(-45.9531282658897,-56.6410798368225,
-47.6332833333333));
#244532=CARTESIAN_POINT('Ctrl Pts',(-46.4348535350793,-57.4754524783487,
-47.57495));
#244533=CARTESIAN_POINT('Ctrl Pts',(-45.9531282658897,-58.309825119875,
-47.5166166666667));
#244534=CARTESIAN_POINT('Ctrl Pts',(-45.4714029967,-59.1441977614012,-47.4582833333333));
#244535=CARTESIAN_POINT('Ctrl Pts',(-44.5079524583208,-59.1441977614012,
-47.39995));
#244536=CARTESIAN_POINT('Ctrl Pts',(-43.5445019199415,-59.1441977614012,
-47.3416166666666));
#244537=CARTESIAN_POINT('Ctrl Pts',(-43.0627766507519,-58.309825119875,
-47.2832833333333));
#244538=CARTESIAN_POINT('Ctrl Pts',(-42.5810513815623,-57.4754524783487,
-47.22495));
#244539=CARTESIAN_POINT('Ctrl Pts',(-43.0627766507519,-56.6410798368225,
-47.1666166666667));
#244540=CARTESIAN_POINT('Ctrl Pts',(-43.5445019199415,-55.8067071952963,
-47.1082833333333));
#244541=CARTESIAN_POINT('Ctrl Pts',(-44.5079524583208,-55.8067071952963,
-47.04995));
#244542=CARTESIAN_POINT('Ctrl Pts',(-45.4714029967,-55.8067071952963,-46.9916166666667));
#244543=CARTESIAN_POINT('Ctrl Pts',(-45.9531282658897,-56.6410798368225,
-46.9332833333334));
#244544=CARTESIAN_POINT('Ctrl Pts',(-46.4348535350793,-57.4754524783487,
-46.87495));
#244545=CARTESIAN_POINT('Ctrl Pts',(-45.9531282658897,-58.309825119875,
-46.8166166666667));
#244546=CARTESIAN_POINT('Ctrl Pts',(-45.4714029967,-59.1441977614012,-46.7582833333333));
#244547=CARTESIAN_POINT('Ctrl Pts',(-44.5079524583208,-59.1441977614012,
-46.69995));
#244548=CARTESIAN_POINT('Ctrl Pts',(-43.5445019199415,-59.1441977614012,
-46.6416166666666));
#244549=CARTESIAN_POINT('Ctrl Pts',(-43.0627766507519,-58.309825119875,
-46.5832833333334));
#244550=CARTESIAN_POINT('Ctrl Pts',(-42.5810513815623,-57.4754524783487,
-46.52495));
#244551=CARTESIAN_POINT('Ctrl Pts',(-43.0627766507519,-56.6410798368225,
-46.4666166666667));
#244552=CARTESIAN_POINT('Ctrl Pts',(-43.5445019199415,-55.8067071952963,
-46.4082833333333));
#244553=CARTESIAN_POINT('Ctrl Pts',(-44.5079524583208,-55.8067071952963,
-46.34995));
#244554=CARTESIAN_POINT('Ctrl Pts',(-45.4714029967,-55.8067071952963,-46.2916166666667));
#244555=CARTESIAN_POINT('Ctrl Pts',(-45.9531282658897,-56.6410798368225,
-46.2332833333334));
#244556=CARTESIAN_POINT('Ctrl Pts',(-46.4348535350793,-57.4754524783487,
-46.17495));
#244557=CARTESIAN_POINT('Ctrl Pts',(-45.9531282658897,-58.309825119875,
-46.1166166666667));
#244558=CARTESIAN_POINT('Ctrl Pts',(-45.4714029967,-59.1441977614012,-46.0582833333333));
#244559=CARTESIAN_POINT('Ctrl Pts',(-44.5079524583208,-59.1441977614012,
-45.99995));
#244560=CARTESIAN_POINT('Ctrl Pts',(-43.5445019199415,-59.1441977614012,
-45.9416166666667));
#244561=CARTESIAN_POINT('Ctrl Pts',(-43.0627766507519,-58.309825119875,
-45.8832833333333));
#244562=CARTESIAN_POINT('Ctrl Pts',(-42.5810513815623,-57.4754524783487,
-45.82495));
#244563=CARTESIAN_POINT('Ctrl Pts',(-43.0627766507519,-56.6410798368225,
-45.7666166666667));
#244564=CARTESIAN_POINT('Ctrl Pts',(-43.5445019199415,-55.8067071952963,
-45.7082833333333));
#244565=CARTESIAN_POINT('Ctrl Pts',(-44.5079524583208,-55.8067071952963,
-45.64995));
#244566=CARTESIAN_POINT('Ctrl Pts',(-45.4714029967,-55.8067071952963,-45.5916166666667));
#244567=CARTESIAN_POINT('Ctrl Pts',(-45.9531282658897,-56.6410798368225,
-45.5332833333333));
#244568=CARTESIAN_POINT('Ctrl Pts',(-46.4348535350793,-57.4754524783487,
-45.47495));
#244569=CARTESIAN_POINT('Ctrl Pts',(-45.9531282658897,-58.309825119875,
-45.4166166666667));
#244570=CARTESIAN_POINT('Ctrl Pts',(-45.4714029967,-59.1441977614012,-45.3582833333333));
#244571=CARTESIAN_POINT('Ctrl Pts',(-44.5079524583208,-59.1441977614012,
-45.29995));
#244572=CARTESIAN_POINT('Ctrl Pts',(-43.5445019199415,-59.1441977614012,
-45.2416166666667));
#244573=CARTESIAN_POINT('Ctrl Pts',(-43.0627766507519,-58.309825119875,
-45.1832833333334));
#244574=CARTESIAN_POINT('Ctrl Pts',(-42.5810513815623,-57.4754524783487,
-45.12495));
#244575=CARTESIAN_POINT('Ctrl Pts',(-43.0627766507519,-56.6410798368225,
-45.0666166666667));
#244576=CARTESIAN_POINT('Ctrl Pts',(-43.5445019199415,-55.8067071952963,
-45.0082833333334));
#244577=CARTESIAN_POINT('Ctrl Pts',(-44.5079524583208,-55.8067071952963,
-44.94995));
#244578=CARTESIAN_POINT('Ctrl Pts',(-45.4714029967,-55.8067071952963,-44.8916166666667));
#244579=CARTESIAN_POINT('Ctrl Pts',(-45.9531282658897,-56.6410798368225,
-44.8332833333334));
#244580=CARTESIAN_POINT('Ctrl Pts',(-46.4348535350793,-57.4754524783487,
-44.77495));
#244581=CARTESIAN_POINT('Ctrl Pts',(-45.9531282658897,-58.309825119875,
-44.7166166666667));
#244582=CARTESIAN_POINT('Ctrl Pts',(-45.4714029967,-59.1441977614012,-44.6582833333334));
#244583=CARTESIAN_POINT('Ctrl Pts',(-44.5079524583208,-59.1441977614012,
-44.59995));
#244584=CARTESIAN_POINT('Ctrl Pts',(-43.5445019199415,-59.1441977614012,
-44.5416166666667));
#244585=CARTESIAN_POINT('Ctrl Pts',(-43.0627766507519,-58.309825119875,
-44.4832833333334));
#244586=CARTESIAN_POINT('Ctrl Pts',(-42.5810513815623,-57.4754524783487,
-44.42495));
#244587=CARTESIAN_POINT('Ctrl Pts',(-43.0627766507519,-56.6410798368225,
-44.3666166666667));
#244588=CARTESIAN_POINT('Ctrl Pts',(-43.5445019199415,-55.8067071952963,
-44.3082833333334));
#244589=CARTESIAN_POINT('Ctrl Pts',(-44.5079524583208,-55.8067071952963,
-44.24995));
#244590=CARTESIAN_POINT('Ctrl Pts',(-45.4714029967,-55.8067071952963,-44.1916166666667));
#244591=CARTESIAN_POINT('Ctrl Pts',(-45.9531282658897,-56.6410798368225,
-44.1332833333334));
#244592=CARTESIAN_POINT('Ctrl Pts',(-46.4348535350793,-57.4754524783487,
-44.07495));
#244593=CARTESIAN_POINT('Ctrl Pts',(-45.9531282658897,-58.309825119875,
-44.0166166666667));
#244594=CARTESIAN_POINT('Ctrl Pts',(-45.4714029967,-59.1441977614012,-43.9582833333334));
#244595=CARTESIAN_POINT('Ctrl Pts',(-44.5079524583208,-59.1441977614012,
-43.89995));
#244596=CARTESIAN_POINT('Ctrl Pts',(-43.5445019199415,-59.1441977614012,
-43.8416166666667));
#244597=CARTESIAN_POINT('Ctrl Pts',(-43.0627766507519,-58.309825119875,
-43.7832833333334));
#244598=CARTESIAN_POINT('Ctrl Pts',(-42.5810513815623,-57.4754524783487,
-43.72495));
#244599=CARTESIAN_POINT('Ctrl Pts',(-43.0627766507519,-56.6410798368225,
-43.6666166666667));
#244600=CARTESIAN_POINT('Ctrl Pts',(-43.5445019199415,-55.8067071952963,
-43.6082833333333));
#244601=CARTESIAN_POINT('Ctrl Pts',(-44.5079524583208,-55.8067071952963,
-43.54995));
#244602=CARTESIAN_POINT('Ctrl Pts',(-45.4714029967,-55.8067071952963,-43.4916166666667));
#244603=CARTESIAN_POINT('Ctrl Pts',(-45.9531282658897,-56.6410798368225,
-43.4332833333333));
#244604=CARTESIAN_POINT('Ctrl Pts',(-46.4348535350793,-57.4754524783487,
-43.37495));
#244605=CARTESIAN_POINT('Ctrl Pts',(-45.9531282658897,-58.309825119875,
-43.3166166666667));
#244606=CARTESIAN_POINT('Ctrl Pts',(-45.4714029967,-59.1441977614012,-43.2582833333333));
#244607=CARTESIAN_POINT('Ctrl Pts',(-44.5079524583208,-59.1441977614012,
-43.19995));
#244608=CARTESIAN_POINT('Ctrl Pts',(-43.5445019199415,-59.1441977614012,
-43.1416166666667));
#244609=CARTESIAN_POINT('Ctrl Pts',(-43.0627766507519,-58.309825119875,
-43.0832833333333));
#244610=CARTESIAN_POINT('Ctrl Pts',(-42.5810513815623,-57.4754524783487,
-43.02495));
#244611=CARTESIAN_POINT('Ctrl Pts',(-43.0627766507519,-56.6410798368225,
-42.9666166666667));
#244612=CARTESIAN_POINT('Ctrl Pts',(-43.5445019199415,-55.8067071952963,
-42.9082833333333));
#244613=CARTESIAN_POINT('Ctrl Pts',(-44.5079524583208,-55.8067071952963,
-42.84995));
#244614=CARTESIAN_POINT('Ctrl Pts',(-45.4714029967,-55.8067071952963,-42.7916166666667));
#244615=CARTESIAN_POINT('Ctrl Pts',(-45.9531282658897,-56.6410798368225,
-42.7332833333334));
#244616=CARTESIAN_POINT('Ctrl Pts',(-46.4348535350793,-57.4754524783487,
-42.67495));
#244617=CARTESIAN_POINT('Ctrl Pts',(-45.9531282658897,-58.309825119875,
-42.6166166666667));
#244618=CARTESIAN_POINT('Ctrl Pts',(-45.4714029967,-59.1441977614012,-42.5582833333333));
#244619=CARTESIAN_POINT('Ctrl Pts',(-44.5079524583208,-59.1441977614012,
-42.49995));
#244620=CARTESIAN_POINT('Ctrl Pts',(-43.5445019199415,-59.1441977614012,
-42.4416166666667));
#244621=CARTESIAN_POINT('Ctrl Pts',(-43.0627766507519,-58.309825119875,
-42.3832833333333));
#244622=CARTESIAN_POINT('Ctrl Pts',(-42.5810513815623,-57.4754524783487,
-42.32495));
#244623=CARTESIAN_POINT('Ctrl Pts',(-43.0627766507519,-56.6410798368225,
-42.2666166666667));
#244624=CARTESIAN_POINT('Ctrl Pts',(-43.5445019199415,-55.8067071952963,
-42.2082833333333));
#244625=CARTESIAN_POINT('Ctrl Pts',(-44.5079524583208,-55.8067071952963,
-42.14995));
#244626=CARTESIAN_POINT('Ctrl Pts',(-45.4714029967,-55.8067071952963,-42.0916166666667));
#244627=CARTESIAN_POINT('Ctrl Pts',(-45.9531282658897,-56.6410798368225,
-42.0332833333334));
#244628=CARTESIAN_POINT('Ctrl Pts',(-46.4348535350793,-57.4754524783487,
-41.97495));
#244629=CARTESIAN_POINT('Ctrl Pts',(-45.9531282658897,-58.309825119875,
-41.9166166666667));
#244630=CARTESIAN_POINT('Ctrl Pts',(-45.4714029967,-59.1441977614012,-41.8582833333333));
#244631=CARTESIAN_POINT('Ctrl Pts',(-44.5079524583208,-59.1441977614012,
-41.79995));
#244632=CARTESIAN_POINT('Ctrl Pts',(-43.5445019199415,-59.1441977614012,
-41.7416166666667));
#244633=CARTESIAN_POINT('Ctrl Pts',(-43.0627766507519,-58.309825119875,
-41.6832833333333));
#244634=CARTESIAN_POINT('Ctrl Pts',(-42.5810513815623,-57.4754524783487,
-41.62495));
#244635=CARTESIAN_POINT('Ctrl Pts',(-43.0627766507519,-56.6410798368225,
-41.5666166666667));
#244636=CARTESIAN_POINT('Ctrl Pts',(-43.5445019199415,-55.8067071952963,
-41.5082833333334));
#244637=CARTESIAN_POINT('Ctrl Pts',(-44.5079524583208,-55.8067071952963,
-41.44995));
#244638=CARTESIAN_POINT('Ctrl Pts',(-45.4714029967,-55.8067071952963,-41.3916166666667));
#244639=CARTESIAN_POINT('Ctrl Pts',(-45.9531282658897,-56.6410798368225,
-41.3332833333334));
#244640=CARTESIAN_POINT('Ctrl Pts',(-46.4348535350793,-57.4754524783487,
-41.27495));
#244641=CARTESIAN_POINT('Ctrl Pts',(-45.9531282658897,-58.309825119875,
-41.2166166666667));
#244642=CARTESIAN_POINT('Ctrl Pts',(-45.4714029967,-59.1441977614012,-41.1582833333333));
#244643=CARTESIAN_POINT('Ctrl Pts',(-44.5079524583208,-59.1441977614012,
-41.09995));
#244644=CARTESIAN_POINT('Ctrl Pts',(-43.5445019199415,-59.1441977614012,
-41.0416166666667));
#244645=CARTESIAN_POINT('Ctrl Pts',(-43.0627766507519,-58.309825119875,
-40.9832833333333));
#244646=CARTESIAN_POINT('Ctrl Pts',(-42.5810513815623,-57.4754524783487,
-40.92495));
#244647=CARTESIAN_POINT('Ctrl Pts',(-43.0627766507519,-56.6410798368225,
-40.8666166666667));
#244648=CARTESIAN_POINT('Ctrl Pts',(-43.5445019199415,-55.8067071952963,
-40.8082833333334));
#244649=CARTESIAN_POINT('Ctrl Pts',(-44.5079524583208,-55.8067071952963,
-40.74995));
#244650=CARTESIAN_POINT('Ctrl Pts',(-45.4714029967,-55.8067071952963,-40.6916166666667));
#244651=CARTESIAN_POINT('Ctrl Pts',(-45.9531282658897,-56.6410798368225,
-40.6332833333334));
#244652=CARTESIAN_POINT('Ctrl Pts',(-46.4348535350793,-57.4754524783487,
-40.57495));
#244653=CARTESIAN_POINT('Ctrl Pts',(-45.9531282658897,-58.309825119875,
-40.5166166666667));
#244654=CARTESIAN_POINT('Ctrl Pts',(-45.4714029967,-59.1441977614012,-40.4582833333333));
#244655=CARTESIAN_POINT('Ctrl Pts',(-44.5079524583208,-59.1441977614012,
-40.39995));
#244656=CARTESIAN_POINT('Ctrl Pts',(-43.5445019199415,-59.1441977614012,
-40.3416166666667));
#244657=CARTESIAN_POINT('Ctrl Pts',(-43.0627766507519,-58.309825119875,
-40.2832833333334));
#244658=CARTESIAN_POINT('Ctrl Pts',(-42.5810513815623,-57.4754524783487,
-40.22495));
#244659=CARTESIAN_POINT('Ctrl Pts',(-43.0627766507519,-56.6410798368225,
-40.1666166666667));
#244660=CARTESIAN_POINT('Ctrl Pts',(-43.5445019199415,-55.8067071952963,
-40.1082833333334));
#244661=CARTESIAN_POINT('Ctrl Pts',(-44.5079524583208,-55.8067071952963,
-40.04995));
#244662=CARTESIAN_POINT('Ctrl Pts',(-45.4714029967,-55.8067071952963,-39.9916166666667));
#244663=CARTESIAN_POINT('Ctrl Pts',(-45.9531282658897,-56.6410798368225,
-39.9332833333333));
#244664=CARTESIAN_POINT('Ctrl Pts',(-46.4348535350793,-57.4754524783487,
-39.87495));
#244665=CARTESIAN_POINT('Ctrl Pts',(-45.9531282658897,-58.309825119875,
-39.8166166666667));
#244666=CARTESIAN_POINT('Ctrl Pts',(-45.4714029967,-59.1441977614012,-39.7582833333334));
#244667=CARTESIAN_POINT('Ctrl Pts',(-44.5079524583208,-59.1441977614012,
-39.69995));
#244668=CARTESIAN_POINT('Ctrl Pts',(-43.5445019199415,-59.1441977614012,
-39.6416166666667));
#244669=CARTESIAN_POINT('Ctrl Pts',(-43.0627766507519,-58.309825119875,
-39.5832833333333));
#244670=CARTESIAN_POINT('Ctrl Pts',(-42.5810513815623,-57.4754524783487,
-39.52495));
#244671=CARTESIAN_POINT('Ctrl Pts',(-43.0627766507519,-56.6410798368225,
-39.4666166666667));
#244672=CARTESIAN_POINT('Ctrl Pts',(-43.5445019199415,-55.8067071952963,
-39.4082833333334));
#244673=CARTESIAN_POINT('Ctrl Pts',(-44.5079524583208,-55.8067071952963,
-39.34995));
#244674=CARTESIAN_POINT('Ctrl Pts',(-45.4714029967,-55.8067071952963,-39.2916166666667));
#244675=CARTESIAN_POINT('Ctrl Pts',(-45.9531282658897,-56.6410798368225,
-39.2332833333333));
#244676=CARTESIAN_POINT('Ctrl Pts',(-46.4348535350793,-57.4754524783487,
-39.17495));
#244677=CARTESIAN_POINT('Ctrl Pts',(-45.9531282658897,-58.309825119875,
-39.1166166666667));
#244678=CARTESIAN_POINT('Ctrl Pts',(-45.4714029967,-59.1441977614012,-39.0582833333334));
#244679=CARTESIAN_POINT('Ctrl Pts',(-44.5079524583208,-59.1441977614012,
-38.99995));
#244680=CARTESIAN_POINT('Ctrl Pts',(-43.5445019199415,-59.1441977614012,
-38.9416166666667));
#244681=CARTESIAN_POINT('Ctrl Pts',(-43.0627766507519,-58.309825119875,
-38.8832833333334));
#244682=CARTESIAN_POINT('Ctrl Pts',(-42.5810513815623,-57.4754524783487,
-38.82495));
#244683=CARTESIAN_POINT('Ctrl Pts',(-43.0627766507519,-56.6410798368225,
-38.7666166666667));
#244684=CARTESIAN_POINT('Ctrl Pts',(-43.5445019199415,-55.8067071952963,
-38.7082833333334));
#244685=CARTESIAN_POINT('Ctrl Pts',(-44.5079524583208,-55.8067071952963,
-38.64995));
#244686=CARTESIAN_POINT('Ctrl Pts',(-45.4714029967,-55.8067071952963,-38.5916166666667));
#244687=CARTESIAN_POINT('Ctrl Pts',(-45.9531282658897,-56.6410798368225,
-38.5332833333334));
#244688=CARTESIAN_POINT('Ctrl Pts',(-46.4348535350793,-57.4754524783487,
-38.47495));
#244689=CARTESIAN_POINT('Ctrl Pts',(-45.9531282658897,-58.309825119875,
-38.4166166666667));
#244690=CARTESIAN_POINT('Ctrl Pts',(-45.4714029967,-59.1441977614012,-38.3582833333333));
#244691=CARTESIAN_POINT('Ctrl Pts',(-44.5079524583208,-59.1441977614012,
-38.29995));
#244692=CARTESIAN_POINT('Ctrl Pts',(-43.5445019199415,-59.1441977614012,
-38.2416166666667));
#244693=CARTESIAN_POINT('Ctrl Pts',(-43.0627766507519,-58.309825119875,
-38.1832833333333));
#244694=CARTESIAN_POINT('Ctrl Pts',(-42.5810513815623,-57.4754524783487,
-38.12495));
#244695=CARTESIAN_POINT('Ctrl Pts',(-43.0627766507519,-56.6410798368225,
-38.0666166666667));
#244696=CARTESIAN_POINT('Ctrl Pts',(-43.5445019199415,-55.8067071952963,
-38.0082833333333));
#244697=CARTESIAN_POINT('Ctrl Pts',(-44.5079524583208,-55.8067071952963,
-37.94995));
#244698=CARTESIAN_POINT('Ctrl Pts',(-45.4714029967,-55.8067071952963,-37.8916166666667));
#244699=CARTESIAN_POINT('Ctrl Pts',(-45.9531282658897,-56.6410798368225,
-37.8332833333334));
#244700=CARTESIAN_POINT('Ctrl Pts',(-46.4348535350793,-57.4754524783487,
-37.77495));
#244701=CARTESIAN_POINT('Ctrl Pts',(-45.9531282658897,-58.309825119875,
-37.7166166666667));
#244702=CARTESIAN_POINT('Ctrl Pts',(-45.4714029967,-59.1441977614012,-37.6582833333333));
#244703=CARTESIAN_POINT('Ctrl Pts',(-44.5079524583208,-59.1441977614012,
-37.59995));
#244704=CARTESIAN_POINT('Ctrl Pts',(-43.5445019199415,-59.1441977614012,
-37.5416166666667));
#244705=CARTESIAN_POINT('Ctrl Pts',(-43.0627766507519,-58.309825119875,
-37.4832833333334));
#244706=CARTESIAN_POINT('Ctrl Pts',(-42.5810513815623,-57.4754524783487,
-37.42495));
#244707=CARTESIAN_POINT('Ctrl Pts',(-43.0627766507519,-56.6410798368225,
-37.3666166666667));
#244708=CARTESIAN_POINT('Ctrl Pts',(-43.5445019199415,-55.8067071952963,
-37.3082833333333));
#244709=CARTESIAN_POINT('Ctrl Pts',(-44.5079524583208,-55.8067071952963,
-37.24995));
#244710=CARTESIAN_POINT('Ctrl Pts',(-45.4714029967,-55.8067071952963,-37.1916166666667));
#244711=CARTESIAN_POINT('Ctrl Pts',(-45.9531282658897,-56.6410798368225,
-37.1332833333334));
#244712=CARTESIAN_POINT('Ctrl Pts',(-46.4348535350793,-57.4754524783487,
-37.07495));
#244713=CARTESIAN_POINT('Ctrl Pts',(-45.9531282658897,-58.309825119875,
-37.0166166666667));
#244714=CARTESIAN_POINT('Ctrl Pts',(-45.8905850977848,-58.418153064699,
-37.0090431559831));
#244715=CARTESIAN_POINT('Ctrl Pts',(-45.8125914103809,-58.5159466035015,
-37.0009024189827));
#244716=CARTESIAN_POINT('Ctrl Pts',(-44.5079524583208,-59.5441932447742,
-53.2308875));
#244717=CARTESIAN_POINT('Ctrl Pts',(-43.3135644199415,-59.5441932447742,
-53.1725541666667));
#244718=CARTESIAN_POINT('Ctrl Pts',(-42.7163704007519,-58.5098228615615,
-53.1142208333334));
#244719=CARTESIAN_POINT('Ctrl Pts',(-42.1191763815623,-57.4754524783487,
-53.0558875000001));
#244720=CARTESIAN_POINT('Ctrl Pts',(-42.7163704007519,-56.4410820951361,
-52.9975541666667));
#244721=CARTESIAN_POINT('Ctrl Pts',(-43.3135644199415,-55.4067117119233,
-52.9392208333334));
#244722=CARTESIAN_POINT('Ctrl Pts',(-44.5079524583208,-55.4067117119234,
-52.8808875));
#244723=CARTESIAN_POINT('Ctrl Pts',(-45.7023404967,-55.4067117119233,-52.8225541666667));
#244724=CARTESIAN_POINT('Ctrl Pts',(-46.2995345158897,-56.4410820951361,
-52.7642208333334));
#244725=CARTESIAN_POINT('Ctrl Pts',(-46.8967285350793,-57.4754524783487,
-52.7058875));
#244726=CARTESIAN_POINT('Ctrl Pts',(-46.2995345158897,-58.5098228615615,
-52.6475541666667));
#244727=CARTESIAN_POINT('Ctrl Pts',(-45.7023404967,-59.5441932447742,-52.5892208333333));
#244728=CARTESIAN_POINT('Ctrl Pts',(-44.5079524583208,-59.5441932447742,
-52.5308875));
#244729=CARTESIAN_POINT('Ctrl Pts',(-43.3135644199415,-59.5441932447742,
-52.4725541666667));
#244730=CARTESIAN_POINT('Ctrl Pts',(-42.7163704007519,-58.5098228615615,
-52.4142208333334));
#244731=CARTESIAN_POINT('Ctrl Pts',(-42.1191763815623,-57.4754524783487,
-52.3558875000001));
#244732=CARTESIAN_POINT('Ctrl Pts',(-42.7163704007519,-56.4410820951361,
-52.2975541666667));
#244733=CARTESIAN_POINT('Ctrl Pts',(-43.3135644199415,-55.4067117119233,
-52.2392208333334));
#244734=CARTESIAN_POINT('Ctrl Pts',(-44.5079524583208,-55.4067117119234,
-52.1808875));
#244735=CARTESIAN_POINT('Ctrl Pts',(-45.7023404967,-55.4067117119233,-52.1225541666667));
#244736=CARTESIAN_POINT('Ctrl Pts',(-46.2995345158897,-56.4410820951361,
-52.0642208333334));
#244737=CARTESIAN_POINT('Ctrl Pts',(-46.8967285350793,-57.4754524783487,
-52.0058875));
#244738=CARTESIAN_POINT('Ctrl Pts',(-46.2995345158897,-58.5098228615615,
-51.9475541666667));
#244739=CARTESIAN_POINT('Ctrl Pts',(-45.7023404967,-59.5441932447742,-51.8892208333334));
#244740=CARTESIAN_POINT('Ctrl Pts',(-44.5079524583208,-59.5441932447742,
-51.8308875));
#244741=CARTESIAN_POINT('Ctrl Pts',(-43.3135644199415,-59.5441932447742,
-51.7725541666667));
#244742=CARTESIAN_POINT('Ctrl Pts',(-42.7163704007519,-58.5098228615615,
-51.7142208333334));
#244743=CARTESIAN_POINT('Ctrl Pts',(-42.1191763815623,-57.4754524783487,
-51.6558875));
#244744=CARTESIAN_POINT('Ctrl Pts',(-42.7163704007519,-56.4410820951361,
-51.5975541666667));
#244745=CARTESIAN_POINT('Ctrl Pts',(-43.3135644199415,-55.4067117119233,
-51.5392208333333));
#244746=CARTESIAN_POINT('Ctrl Pts',(-44.5079524583208,-55.4067117119234,
-51.4808875));
#244747=CARTESIAN_POINT('Ctrl Pts',(-45.7023404967,-55.4067117119233,-51.4225541666667));
#244748=CARTESIAN_POINT('Ctrl Pts',(-46.2995345158897,-56.4410820951361,
-51.3642208333334));
#244749=CARTESIAN_POINT('Ctrl Pts',(-46.8967285350793,-57.4754524783487,
-51.3058875));
#244750=CARTESIAN_POINT('Ctrl Pts',(-46.2995345158897,-58.5098228615615,
-51.2475541666667));
#244751=CARTESIAN_POINT('Ctrl Pts',(-45.7023404967,-59.5441932447742,-51.1892208333334));
#244752=CARTESIAN_POINT('Ctrl Pts',(-44.5079524583208,-59.5441932447742,
-51.1308875));
#244753=CARTESIAN_POINT('Ctrl Pts',(-43.3135644199415,-59.5441932447742,
-51.0725541666667));
#244754=CARTESIAN_POINT('Ctrl Pts',(-42.7163704007519,-58.5098228615615,
-51.0142208333334));
#244755=CARTESIAN_POINT('Ctrl Pts',(-42.1191763815623,-57.4754524783487,
-50.9558875));
#244756=CARTESIAN_POINT('Ctrl Pts',(-42.7163704007519,-56.4410820951361,
-50.8975541666667));
#244757=CARTESIAN_POINT('Ctrl Pts',(-43.3135644199415,-55.4067117119233,
-50.8392208333333));
#244758=CARTESIAN_POINT('Ctrl Pts',(-44.5079524583208,-55.4067117119234,
-50.7808875));
#244759=CARTESIAN_POINT('Ctrl Pts',(-45.7023404967,-55.4067117119233,-50.7225541666667));
#244760=CARTESIAN_POINT('Ctrl Pts',(-46.2995345158897,-56.4410820951361,
-50.6642208333333));
#244761=CARTESIAN_POINT('Ctrl Pts',(-46.8967285350793,-57.4754524783487,
-50.6058875));
#244762=CARTESIAN_POINT('Ctrl Pts',(-46.2995345158897,-58.5098228615615,
-50.5475541666667));
#244763=CARTESIAN_POINT('Ctrl Pts',(-45.7023404967,-59.5441932447742,-50.4892208333333));
#244764=CARTESIAN_POINT('Ctrl Pts',(-44.5079524583208,-59.5441932447742,
-50.4308875));
#244765=CARTESIAN_POINT('Ctrl Pts',(-43.3135644199415,-59.5441932447742,
-50.3725541666667));
#244766=CARTESIAN_POINT('Ctrl Pts',(-42.7163704007519,-58.5098228615615,
-50.3142208333334));
#244767=CARTESIAN_POINT('Ctrl Pts',(-42.1191763815623,-57.4754524783487,
-50.2558875));
#244768=CARTESIAN_POINT('Ctrl Pts',(-42.7163704007519,-56.4410820951361,
-50.1975541666667));
#244769=CARTESIAN_POINT('Ctrl Pts',(-43.3135644199415,-55.4067117119233,
-50.1392208333333));
#244770=CARTESIAN_POINT('Ctrl Pts',(-44.5079524583208,-55.4067117119234,
-50.0808875));
#244771=CARTESIAN_POINT('Ctrl Pts',(-45.7023404967,-55.4067117119233,-50.0225541666667));
#244772=CARTESIAN_POINT('Ctrl Pts',(-46.2995345158897,-56.4410820951361,
-49.9642208333334));
#244773=CARTESIAN_POINT('Ctrl Pts',(-46.8967285350793,-57.4754524783487,
-49.9058875));
#244774=CARTESIAN_POINT('Ctrl Pts',(-46.2995345158897,-58.5098228615615,
-49.8475541666667));
#244775=CARTESIAN_POINT('Ctrl Pts',(-45.7023404967,-59.5441932447742,-49.7892208333333));
#244776=CARTESIAN_POINT('Ctrl Pts',(-44.5079524583208,-59.5441932447742,
-49.7308875));
#244777=CARTESIAN_POINT('Ctrl Pts',(-43.3135644199415,-59.5441932447742,
-49.6725541666667));
#244778=CARTESIAN_POINT('Ctrl Pts',(-42.7163704007519,-58.5098228615615,
-49.6142208333334));
#244779=CARTESIAN_POINT('Ctrl Pts',(-42.1191763815623,-57.4754524783487,
-49.5558875));
#244780=CARTESIAN_POINT('Ctrl Pts',(-42.7163704007519,-56.4410820951361,
-49.4975541666667));
#244781=CARTESIAN_POINT('Ctrl Pts',(-43.3135644199415,-55.4067117119233,
-49.4392208333333));
#244782=CARTESIAN_POINT('Ctrl Pts',(-44.5079524583208,-55.4067117119234,
-49.3808875));
#244783=CARTESIAN_POINT('Ctrl Pts',(-45.7023404967,-55.4067117119233,-49.3225541666667));
#244784=CARTESIAN_POINT('Ctrl Pts',(-46.2995345158897,-56.4410820951361,
-49.2642208333334));
#244785=CARTESIAN_POINT('Ctrl Pts',(-46.8967285350793,-57.4754524783487,
-49.2058875));
#244786=CARTESIAN_POINT('Ctrl Pts',(-46.2995345158897,-58.5098228615615,
-49.1475541666667));
#244787=CARTESIAN_POINT('Ctrl Pts',(-45.7023404967,-59.5441932447742,-49.0892208333333));
#244788=CARTESIAN_POINT('Ctrl Pts',(-44.5079524583208,-59.5441932447742,
-49.0308875));
#244789=CARTESIAN_POINT('Ctrl Pts',(-43.3135644199415,-59.5441932447742,
-48.9725541666667));
#244790=CARTESIAN_POINT('Ctrl Pts',(-42.7163704007519,-58.5098228615615,
-48.9142208333334));
#244791=CARTESIAN_POINT('Ctrl Pts',(-42.1191763815623,-57.4754524783487,
-48.8558875));
#244792=CARTESIAN_POINT('Ctrl Pts',(-42.7163704007519,-56.4410820951361,
-48.7975541666667));
#244793=CARTESIAN_POINT('Ctrl Pts',(-43.3135644199415,-55.4067117119233,
-48.7392208333334));
#244794=CARTESIAN_POINT('Ctrl Pts',(-44.5079524583208,-55.4067117119234,
-48.6808875));
#244795=CARTESIAN_POINT('Ctrl Pts',(-45.7023404967,-55.4067117119233,-48.6225541666667));
#244796=CARTESIAN_POINT('Ctrl Pts',(-46.2995345158897,-56.4410820951361,
-48.5642208333334));
#244797=CARTESIAN_POINT('Ctrl Pts',(-46.8967285350793,-57.4754524783487,
-48.5058875));
#244798=CARTESIAN_POINT('Ctrl Pts',(-46.2995345158897,-58.5098228615615,
-48.4475541666667));
#244799=CARTESIAN_POINT('Ctrl Pts',(-45.7023404967,-59.5441932447742,-48.3892208333334));
#244800=CARTESIAN_POINT('Ctrl Pts',(-44.5079524583208,-59.5441932447742,
-48.3308875));
#244801=CARTESIAN_POINT('Ctrl Pts',(-43.3135644199415,-59.5441932447742,
-48.2725541666667));
#244802=CARTESIAN_POINT('Ctrl Pts',(-42.7163704007519,-58.5098228615615,
-48.2142208333334));
#244803=CARTESIAN_POINT('Ctrl Pts',(-42.1191763815623,-57.4754524783487,
-48.1558875));
#244804=CARTESIAN_POINT('Ctrl Pts',(-42.7163704007519,-56.4410820951361,
-48.0975541666667));
#244805=CARTESIAN_POINT('Ctrl Pts',(-43.3135644199415,-55.4067117119233,
-48.0392208333334));
#244806=CARTESIAN_POINT('Ctrl Pts',(-44.5079524583208,-55.4067117119234,
-47.9808875));
#244807=CARTESIAN_POINT('Ctrl Pts',(-45.7023404967,-55.4067117119233,-47.9225541666667));
#244808=CARTESIAN_POINT('Ctrl Pts',(-46.2995345158897,-56.4410820951361,
-47.8642208333334));
#244809=CARTESIAN_POINT('Ctrl Pts',(-46.8967285350793,-57.4754524783487,
-47.8058875000001));
#244810=CARTESIAN_POINT('Ctrl Pts',(-46.2995345158897,-58.5098228615615,
-47.7475541666667));
#244811=CARTESIAN_POINT('Ctrl Pts',(-45.7023404967,-59.5441932447742,-47.6892208333334));
#244812=CARTESIAN_POINT('Ctrl Pts',(-44.5079524583208,-59.5441932447742,
-47.6308875));
#244813=CARTESIAN_POINT('Ctrl Pts',(-43.3135644199415,-59.5441932447742,
-47.5725541666667));
#244814=CARTESIAN_POINT('Ctrl Pts',(-42.7163704007519,-58.5098228615615,
-47.5142208333333));
#244815=CARTESIAN_POINT('Ctrl Pts',(-42.1191763815623,-57.4754524783487,
-47.4558875));
#244816=CARTESIAN_POINT('Ctrl Pts',(-42.7163704007519,-56.4410820951361,
-47.3975541666667));
#244817=CARTESIAN_POINT('Ctrl Pts',(-43.3135644199415,-55.4067117119233,
-47.3392208333334));
#244818=CARTESIAN_POINT('Ctrl Pts',(-44.5079524583208,-55.4067117119234,
-47.2808875));
#244819=CARTESIAN_POINT('Ctrl Pts',(-45.7023404967,-55.4067117119233,-47.2225541666667));
#244820=CARTESIAN_POINT('Ctrl Pts',(-46.2995345158897,-56.4410820951361,
-47.1642208333334));
#244821=CARTESIAN_POINT('Ctrl Pts',(-46.8967285350793,-57.4754524783487,
-47.1058875));
#244822=CARTESIAN_POINT('Ctrl Pts',(-46.2995345158897,-58.5098228615615,
-47.0475541666667));
#244823=CARTESIAN_POINT('Ctrl Pts',(-45.7023404967,-59.5441932447742,-46.9892208333334));
#244824=CARTESIAN_POINT('Ctrl Pts',(-44.5079524583208,-59.5441932447742,
-46.9308875));
#244825=CARTESIAN_POINT('Ctrl Pts',(-43.3135644199415,-59.5441932447742,
-46.8725541666667));
#244826=CARTESIAN_POINT('Ctrl Pts',(-42.7163704007519,-58.5098228615615,
-46.8142208333334));
#244827=CARTESIAN_POINT('Ctrl Pts',(-42.1191763815623,-57.4754524783487,
-46.7558875));
#244828=CARTESIAN_POINT('Ctrl Pts',(-42.7163704007519,-56.4410820951361,
-46.6975541666667));
#244829=CARTESIAN_POINT('Ctrl Pts',(-43.3135644199415,-55.4067117119233,
-46.6392208333334));
#244830=CARTESIAN_POINT('Ctrl Pts',(-44.5079524583208,-55.4067117119234,
-46.5808875));
#244831=CARTESIAN_POINT('Ctrl Pts',(-45.7023404967,-55.4067117119233,-46.5225541666667));
#244832=CARTESIAN_POINT('Ctrl Pts',(-46.2995345158897,-56.4410820951361,
-46.4642208333334));
#244833=CARTESIAN_POINT('Ctrl Pts',(-46.8967285350793,-57.4754524783487,
-46.4058875));
#244834=CARTESIAN_POINT('Ctrl Pts',(-46.2995345158897,-58.5098228615615,
-46.3475541666667));
#244835=CARTESIAN_POINT('Ctrl Pts',(-45.7023404967,-59.5441932447742,-46.2892208333334));
#244836=CARTESIAN_POINT('Ctrl Pts',(-44.5079524583208,-59.5441932447742,
-46.2308875));
#244837=CARTESIAN_POINT('Ctrl Pts',(-43.3135644199415,-59.5441932447742,
-46.1725541666667));
#244838=CARTESIAN_POINT('Ctrl Pts',(-42.7163704007519,-58.5098228615615,
-46.1142208333334));
#244839=CARTESIAN_POINT('Ctrl Pts',(-42.1191763815623,-57.4754524783487,
-46.0558875));
#244840=CARTESIAN_POINT('Ctrl Pts',(-42.7163704007519,-56.4410820951361,
-45.9975541666667));
#244841=CARTESIAN_POINT('Ctrl Pts',(-43.3135644199415,-55.4067117119233,
-45.9392208333333));
#244842=CARTESIAN_POINT('Ctrl Pts',(-44.5079524583208,-55.4067117119234,
-45.8808875));
#244843=CARTESIAN_POINT('Ctrl Pts',(-45.7023404967,-55.4067117119233,-45.8225541666667));
#244844=CARTESIAN_POINT('Ctrl Pts',(-46.2995345158897,-56.4410820951361,
-45.7642208333334));
#244845=CARTESIAN_POINT('Ctrl Pts',(-46.8967285350793,-57.4754524783487,
-45.7058875));
#244846=CARTESIAN_POINT('Ctrl Pts',(-46.2995345158897,-58.5098228615615,
-45.6475541666667));
#244847=CARTESIAN_POINT('Ctrl Pts',(-45.7023404967,-59.5441932447742,-45.5892208333334));
#244848=CARTESIAN_POINT('Ctrl Pts',(-44.5079524583208,-59.5441932447742,
-45.5308875));
#244849=CARTESIAN_POINT('Ctrl Pts',(-43.3135644199415,-59.5441932447742,
-45.4725541666667));
#244850=CARTESIAN_POINT('Ctrl Pts',(-42.7163704007519,-58.5098228615615,
-45.4142208333334));
#244851=CARTESIAN_POINT('Ctrl Pts',(-42.1191763815623,-57.4754524783487,
-45.3558875));
#244852=CARTESIAN_POINT('Ctrl Pts',(-42.7163704007519,-56.4410820951361,
-45.2975541666667));
#244853=CARTESIAN_POINT('Ctrl Pts',(-43.3135644199415,-55.4067117119233,
-45.2392208333333));
#244854=CARTESIAN_POINT('Ctrl Pts',(-44.5079524583208,-55.4067117119234,
-45.1808875));
#244855=CARTESIAN_POINT('Ctrl Pts',(-45.7023404967,-55.4067117119233,-45.1225541666667));
#244856=CARTESIAN_POINT('Ctrl Pts',(-46.2995345158897,-56.4410820951361,
-45.0642208333334));
#244857=CARTESIAN_POINT('Ctrl Pts',(-46.8967285350793,-57.4754524783487,
-45.0058875));
#244858=CARTESIAN_POINT('Ctrl Pts',(-46.2995345158897,-58.5098228615615,
-44.9475541666667));
#244859=CARTESIAN_POINT('Ctrl Pts',(-45.7023404967,-59.5441932447742,-44.8892208333333));
#244860=CARTESIAN_POINT('Ctrl Pts',(-44.5079524583208,-59.5441932447742,
-44.8308875));
#244861=CARTESIAN_POINT('Ctrl Pts',(-43.3135644199415,-59.5441932447742,
-44.7725541666667));
#244862=CARTESIAN_POINT('Ctrl Pts',(-42.7163704007519,-58.5098228615615,
-44.7142208333334));
#244863=CARTESIAN_POINT('Ctrl Pts',(-42.1191763815623,-57.4754524783487,
-44.6558875));
#244864=CARTESIAN_POINT('Ctrl Pts',(-42.7163704007519,-56.4410820951361,
-44.5975541666667));
#244865=CARTESIAN_POINT('Ctrl Pts',(-43.3135644199415,-55.4067117119233,
-44.5392208333333));
#244866=CARTESIAN_POINT('Ctrl Pts',(-44.5079524583208,-55.4067117119234,
-44.4808875000001));
#244867=CARTESIAN_POINT('Ctrl Pts',(-45.7023404967,-55.4067117119233,-44.4225541666667));
#244868=CARTESIAN_POINT('Ctrl Pts',(-46.2995345158897,-56.4410820951361,
-44.3642208333333));
#244869=CARTESIAN_POINT('Ctrl Pts',(-46.8967285350793,-57.4754524783487,
-44.3058875));
#244870=CARTESIAN_POINT('Ctrl Pts',(-46.2995345158897,-58.5098228615615,
-44.2475541666667));
#244871=CARTESIAN_POINT('Ctrl Pts',(-45.7023404967,-59.5441932447742,-44.1892208333334));
#244872=CARTESIAN_POINT('Ctrl Pts',(-44.5079524583208,-59.5441932447742,
-44.1308875000001));
#244873=CARTESIAN_POINT('Ctrl Pts',(-43.3135644199415,-59.5441932447742,
-44.0725541666667));
#244874=CARTESIAN_POINT('Ctrl Pts',(-42.7163704007519,-58.5098228615615,
-44.0142208333334));
#244875=CARTESIAN_POINT('Ctrl Pts',(-42.1191763815623,-57.4754524783487,
-43.9558875));
#244876=CARTESIAN_POINT('Ctrl Pts',(-42.7163704007519,-56.4410820951361,
-43.8975541666667));
#244877=CARTESIAN_POINT('Ctrl Pts',(-43.3135644199415,-55.4067117119233,
-43.8392208333333));
#244878=CARTESIAN_POINT('Ctrl Pts',(-44.5079524583208,-55.4067117119234,
-43.7808875));
#244879=CARTESIAN_POINT('Ctrl Pts',(-45.7023404967,-55.4067117119233,-43.7225541666667));
#244880=CARTESIAN_POINT('Ctrl Pts',(-46.2995345158897,-56.4410820951361,
-43.6642208333334));
#244881=CARTESIAN_POINT('Ctrl Pts',(-46.8967285350793,-57.4754524783487,
-43.6058875));
#244882=CARTESIAN_POINT('Ctrl Pts',(-46.2995345158897,-58.5098228615615,
-43.5475541666667));
#244883=CARTESIAN_POINT('Ctrl Pts',(-45.7023404967,-59.5441932447742,-43.4892208333333));
#244884=CARTESIAN_POINT('Ctrl Pts',(-44.5079524583208,-59.5441932447742,
-43.4308875));
#244885=CARTESIAN_POINT('Ctrl Pts',(-43.3135644199415,-59.5441932447742,
-43.3725541666667));
#244886=CARTESIAN_POINT('Ctrl Pts',(-42.7163704007519,-58.5098228615615,
-43.3142208333334));
#244887=CARTESIAN_POINT('Ctrl Pts',(-42.1191763815623,-57.4754524783487,
-43.2558875));
#244888=CARTESIAN_POINT('Ctrl Pts',(-42.7163704007519,-56.4410820951361,
-43.1975541666667));
#244889=CARTESIAN_POINT('Ctrl Pts',(-43.3135644199415,-55.4067117119233,
-43.1392208333334));
#244890=CARTESIAN_POINT('Ctrl Pts',(-44.5079524583208,-55.4067117119234,
-43.0808875));
#244891=CARTESIAN_POINT('Ctrl Pts',(-45.7023404967,-55.4067117119233,-43.0225541666667));
#244892=CARTESIAN_POINT('Ctrl Pts',(-46.2995345158897,-56.4410820951361,
-42.9642208333334));
#244893=CARTESIAN_POINT('Ctrl Pts',(-46.8967285350793,-57.4754524783487,
-42.9058875));
#244894=CARTESIAN_POINT('Ctrl Pts',(-46.2995345158897,-58.5098228615615,
-42.8475541666667));
#244895=CARTESIAN_POINT('Ctrl Pts',(-45.7023404967,-59.5441932447742,-42.7892208333334));
#244896=CARTESIAN_POINT('Ctrl Pts',(-44.5079524583208,-59.5441932447742,
-42.7308875000001));
#244897=CARTESIAN_POINT('Ctrl Pts',(-43.3135644199415,-59.5441932447742,
-42.6725541666667));
#244898=CARTESIAN_POINT('Ctrl Pts',(-42.7163704007519,-58.5098228615615,
-42.6142208333334));
#244899=CARTESIAN_POINT('Ctrl Pts',(-42.1191763815623,-57.4754524783487,
-42.5558875));
#244900=CARTESIAN_POINT('Ctrl Pts',(-42.7163704007519,-56.4410820951361,
-42.4975541666667));
#244901=CARTESIAN_POINT('Ctrl Pts',(-43.3135644199415,-55.4067117119233,
-42.4392208333334));
#244902=CARTESIAN_POINT('Ctrl Pts',(-44.5079524583208,-55.4067117119234,
-42.3808875000001));
#244903=CARTESIAN_POINT('Ctrl Pts',(-45.7023404967,-55.4067117119233,-42.3225541666667));
#244904=CARTESIAN_POINT('Ctrl Pts',(-46.2995345158897,-56.4410820951361,
-42.2642208333334));
#244905=CARTESIAN_POINT('Ctrl Pts',(-46.8967285350793,-57.4754524783487,
-42.2058875));
#244906=CARTESIAN_POINT('Ctrl Pts',(-46.2995345158897,-58.5098228615615,
-42.1475541666667));
#244907=CARTESIAN_POINT('Ctrl Pts',(-45.7023404967,-59.5441932447742,-42.0892208333334));
#244908=CARTESIAN_POINT('Ctrl Pts',(-44.5079524583208,-59.5441932447742,
-42.0308875000001));
#244909=CARTESIAN_POINT('Ctrl Pts',(-43.3135644199415,-59.5441932447742,
-41.9725541666667));
#244910=CARTESIAN_POINT('Ctrl Pts',(-42.7163704007519,-58.5098228615615,
-41.9142208333334));
#244911=CARTESIAN_POINT('Ctrl Pts',(-42.1191763815623,-57.4754524783487,
-41.8558875));
#244912=CARTESIAN_POINT('Ctrl Pts',(-42.7163704007519,-56.4410820951361,
-41.7975541666667));
#244913=CARTESIAN_POINT('Ctrl Pts',(-43.3135644199415,-55.4067117119233,
-41.7392208333334));
#244914=CARTESIAN_POINT('Ctrl Pts',(-44.5079524583208,-55.4067117119234,
-41.6808875000001));
#244915=CARTESIAN_POINT('Ctrl Pts',(-45.7023404967,-55.4067117119233,-41.6225541666667));
#244916=CARTESIAN_POINT('Ctrl Pts',(-46.2995345158897,-56.4410820951361,
-41.5642208333334));
#244917=CARTESIAN_POINT('Ctrl Pts',(-46.8967285350793,-57.4754524783487,
-41.5058875));
#244918=CARTESIAN_POINT('Ctrl Pts',(-46.2995345158897,-58.5098228615615,
-41.4475541666667));
#244919=CARTESIAN_POINT('Ctrl Pts',(-45.7023404967,-59.5441932447742,-41.3892208333334));
#244920=CARTESIAN_POINT('Ctrl Pts',(-44.5079524583208,-59.5441932447742,
-41.3308875000001));
#244921=CARTESIAN_POINT('Ctrl Pts',(-43.3135644199415,-59.5441932447742,
-41.2725541666667));
#244922=CARTESIAN_POINT('Ctrl Pts',(-42.7163704007519,-58.5098228615615,
-41.2142208333333));
#244923=CARTESIAN_POINT('Ctrl Pts',(-42.1191763815623,-57.4754524783487,
-41.1558875));
#244924=CARTESIAN_POINT('Ctrl Pts',(-42.7163704007519,-56.4410820951361,
-41.0975541666667));
#244925=CARTESIAN_POINT('Ctrl Pts',(-43.3135644199415,-55.4067117119233,
-41.0392208333333));
#244926=CARTESIAN_POINT('Ctrl Pts',(-44.5079524583208,-55.4067117119234,
-40.9808875000001));
#244927=CARTESIAN_POINT('Ctrl Pts',(-45.7023404967,-55.4067117119233,-40.9225541666667));
#244928=CARTESIAN_POINT('Ctrl Pts',(-46.2995345158897,-56.4410820951361,
-40.8642208333334));
#244929=CARTESIAN_POINT('Ctrl Pts',(-46.8967285350793,-57.4754524783487,
-40.8058875));
#244930=CARTESIAN_POINT('Ctrl Pts',(-46.2995345158897,-58.5098228615615,
-40.7475541666667));
#244931=CARTESIAN_POINT('Ctrl Pts',(-45.7023404967,-59.5441932447742,-40.6892208333333));
#244932=CARTESIAN_POINT('Ctrl Pts',(-44.5079524583208,-59.5441932447742,
-40.6308875));
#244933=CARTESIAN_POINT('Ctrl Pts',(-43.3135644199415,-59.5441932447742,
-40.5725541666667));
#244934=CARTESIAN_POINT('Ctrl Pts',(-42.7163704007519,-58.5098228615615,
-40.5142208333333));
#244935=CARTESIAN_POINT('Ctrl Pts',(-42.1191763815623,-57.4754524783487,
-40.4558875));
#244936=CARTESIAN_POINT('Ctrl Pts',(-42.7163704007519,-56.4410820951361,
-40.3975541666667));
#244937=CARTESIAN_POINT('Ctrl Pts',(-43.3135644199415,-55.4067117119233,
-40.3392208333333));
#244938=CARTESIAN_POINT('Ctrl Pts',(-44.5079524583208,-55.4067117119234,
-40.2808875));
#244939=CARTESIAN_POINT('Ctrl Pts',(-45.7023404967,-55.4067117119233,-40.2225541666667));
#244940=CARTESIAN_POINT('Ctrl Pts',(-46.2995345158897,-56.4410820951361,
-40.1642208333333));
#244941=CARTESIAN_POINT('Ctrl Pts',(-46.8967285350793,-57.4754524783487,
-40.1058875));
#244942=CARTESIAN_POINT('Ctrl Pts',(-46.2995345158897,-58.5098228615615,
-40.0475541666667));
#244943=CARTESIAN_POINT('Ctrl Pts',(-45.7023404967,-59.5441932447742,-39.9892208333333));
#244944=CARTESIAN_POINT('Ctrl Pts',(-44.5079524583208,-59.5441932447742,
-39.9308875));
#244945=CARTESIAN_POINT('Ctrl Pts',(-43.3135644199415,-59.5441932447742,
-39.8725541666667));
#244946=CARTESIAN_POINT('Ctrl Pts',(-42.7163704007519,-58.5098228615615,
-39.8142208333334));
#244947=CARTESIAN_POINT('Ctrl Pts',(-42.1191763815623,-57.4754524783487,
-39.7558875));
#244948=CARTESIAN_POINT('Ctrl Pts',(-42.7163704007519,-56.4410820951361,
-39.6975541666667));
#244949=CARTESIAN_POINT('Ctrl Pts',(-43.3135644199415,-55.4067117119233,
-39.6392208333334));
#244950=CARTESIAN_POINT('Ctrl Pts',(-44.5079524583208,-55.4067117119234,
-39.5808875000001));
#244951=CARTESIAN_POINT('Ctrl Pts',(-45.7023404967,-55.4067117119233,-39.5225541666667));
#244952=CARTESIAN_POINT('Ctrl Pts',(-46.2995345158897,-56.4410820951361,
-39.4642208333333));
#244953=CARTESIAN_POINT('Ctrl Pts',(-46.8967285350793,-57.4754524783487,
-39.4058875));
#244954=CARTESIAN_POINT('Ctrl Pts',(-46.2995345158897,-58.5098228615615,
-39.3475541666667));
#244955=CARTESIAN_POINT('Ctrl Pts',(-45.7023404967,-59.5441932447742,-39.2892208333334));
#244956=CARTESIAN_POINT('Ctrl Pts',(-44.5079524583208,-59.5441932447742,
-39.2308875));
#244957=CARTESIAN_POINT('Ctrl Pts',(-43.3135644199415,-59.5441932447742,
-39.1725541666667));
#244958=CARTESIAN_POINT('Ctrl Pts',(-42.7163704007519,-58.5098228615615,
-39.1142208333333));
#244959=CARTESIAN_POINT('Ctrl Pts',(-42.1191763815623,-57.4754524783487,
-39.0558875));
#244960=CARTESIAN_POINT('Ctrl Pts',(-42.7163704007519,-56.4410820951361,
-38.9975541666667));
#244961=CARTESIAN_POINT('Ctrl Pts',(-43.3135644199415,-55.4067117119233,
-38.9392208333334));
#244962=CARTESIAN_POINT('Ctrl Pts',(-44.5079524583208,-55.4067117119234,
-38.8808875));
#244963=CARTESIAN_POINT('Ctrl Pts',(-45.7023404967,-55.4067117119233,-38.8225541666667));
#244964=CARTESIAN_POINT('Ctrl Pts',(-46.2995345158897,-56.4410820951361,
-38.7642208333333));
#244965=CARTESIAN_POINT('Ctrl Pts',(-46.8967285350793,-57.4754524783487,
-38.7058875));
#244966=CARTESIAN_POINT('Ctrl Pts',(-46.2995345158897,-58.5098228615615,
-38.6475541666667));
#244967=CARTESIAN_POINT('Ctrl Pts',(-45.7023404967,-59.5441932447742,-38.5892208333334));
#244968=CARTESIAN_POINT('Ctrl Pts',(-44.5079524583208,-59.5441932447742,
-38.5308875));
#244969=CARTESIAN_POINT('Ctrl Pts',(-43.3135644199415,-59.5441932447742,
-38.4725541666667));
#244970=CARTESIAN_POINT('Ctrl Pts',(-42.7163704007519,-58.5098228615615,
-38.4142208333334));
#244971=CARTESIAN_POINT('Ctrl Pts',(-42.1191763815623,-57.4754524783487,
-38.3558875));
#244972=CARTESIAN_POINT('Ctrl Pts',(-42.7163704007519,-56.4410820951361,
-38.2975541666667));
#244973=CARTESIAN_POINT('Ctrl Pts',(-43.3135644199415,-55.4067117119233,
-38.2392208333333));
#244974=CARTESIAN_POINT('Ctrl Pts',(-44.5079524583208,-55.4067117119234,
-38.1808875000001));
#244975=CARTESIAN_POINT('Ctrl Pts',(-45.7023404967,-55.4067117119233,-38.1225541666667));
#244976=CARTESIAN_POINT('Ctrl Pts',(-46.2995345158897,-56.4410820951361,
-38.0642208333334));
#244977=CARTESIAN_POINT('Ctrl Pts',(-46.8967285350793,-57.4754524783487,
-38.0058875));
#244978=CARTESIAN_POINT('Ctrl Pts',(-46.2995345158897,-58.5098228615615,
-37.9475541666667));
#244979=CARTESIAN_POINT('Ctrl Pts',(-45.7023404967,-59.5441932447742,-37.8892208333334));
#244980=CARTESIAN_POINT('Ctrl Pts',(-44.5079524583208,-59.5441932447742,
-37.8308875));
#244981=CARTESIAN_POINT('Ctrl Pts',(-43.3135644199415,-59.5441932447742,
-37.7725541666667));
#244982=CARTESIAN_POINT('Ctrl Pts',(-42.7163704007519,-58.5098228615615,
-37.7142208333333));
#244983=CARTESIAN_POINT('Ctrl Pts',(-42.1191763815623,-57.4754524783487,
-37.6558875));
#244984=CARTESIAN_POINT('Ctrl Pts',(-42.7163704007519,-56.4410820951361,
-37.5975541666667));
#244985=CARTESIAN_POINT('Ctrl Pts',(-43.3135644199415,-55.4067117119233,
-37.5392208333334));
#244986=CARTESIAN_POINT('Ctrl Pts',(-44.5079524583208,-55.4067117119234,
-37.4808875));
#244987=CARTESIAN_POINT('Ctrl Pts',(-45.7023404967,-55.4067117119233,-37.4225541666667));
#244988=CARTESIAN_POINT('Ctrl Pts',(-46.2995345158897,-56.4410820951361,
-37.3642208333333));
#244989=CARTESIAN_POINT('Ctrl Pts',(-46.8967285350793,-57.4754524783487,
-37.3058875));
#244990=CARTESIAN_POINT('Ctrl Pts',(-46.2995345158897,-58.5098228615615,
-37.2475541666667));
#244991=CARTESIAN_POINT('Ctrl Pts',(-46.2219998538691,-58.6441168355289,
-37.239980655983));
#244992=CARTESIAN_POINT('Ctrl Pts',(-46.1253112086366,-58.7653513237809,
-37.2318399189827));
#244993=CARTESIAN_POINT('Ctrl Pts',(-43.4124017072694,-55.802201528474,
-38.9060754033995));
#244994=CARTESIAN_POINT('Ctrl Pts',(-43.3649158658203,-55.8332929240044,
-38.9093809723611));
#244995=CARTESIAN_POINT('Ctrl Pts',(-43.3188133243802,-55.8663716512136,
-38.9126746807634));
#244996=CARTESIAN_POINT('Ctrl Pts',(-43.2743250866905,-55.9012347622251,
-38.9159389233579));
#244997=CARTESIAN_POINT('Ctrl Pts',(-43.2296908678756,-55.9362122710289,
-38.9192138770489));
#244998=CARTESIAN_POINT('Ctrl Pts',(-43.1866820205791,-55.972985308453,
-38.9224591311364));
#244999=CARTESIAN_POINT('Ctrl Pts',(-43.1454915293058,-56.0113153370374,
-38.925657963383));
#245000=CARTESIAN_POINT('Ctrl Pts',(-43.1039234831771,-56.0499967012809,
-38.9288861163445));
#245001=CARTESIAN_POINT('Ctrl Pts',(-43.064207623636,-56.0902630655489,
-38.9320669558098));
#245002=CARTESIAN_POINT('Ctrl Pts',(-43.0264951685045,-56.1318445720534,
-38.9351849561294));
#245003=CARTESIAN_POINT('Ctrl Pts',(-42.9885545942382,-56.1736776012247,
-38.9383218169429));
#245004=CARTESIAN_POINT('Ctrl Pts',(-42.9526418729829,-56.2168409968285,
-38.9413950476852));
#245005=CARTESIAN_POINT('Ctrl Pts',(-42.9188598747448,-56.2610457456956,
-38.9443910067074));
#245006=CARTESIAN_POINT('Ctrl Pts',(-42.8846518529637,-56.3058079590324,
-38.9474247476591));
#245007=CARTESIAN_POINT('Ctrl Pts',(-42.852628641587,-56.3516372104306,
-38.9503792335294));
#245008=CARTESIAN_POINT('Ctrl Pts',(-42.8228435979642,-56.3982301413591,
-38.9532429054736));
#245009=CARTESIAN_POINT('Ctrl Pts',(-42.8065246134638,-56.4237580313726,
-38.9548118881705));
#245010=CARTESIAN_POINT('Ctrl Pts',(-42.7908765577231,-56.4495151786358,
-38.9563536575169));
#245011=CARTESIAN_POINT('Ctrl Pts',(-42.7759016507518,-56.4754524783487,
-38.9578666666668));
#245012=CARTESIAN_POINT('Ctrl Pts',(-42.7486194549309,-56.5227066276525,
-38.9606231587095));
#245013=CARTESIAN_POINT('Ctrl Pts',(-42.7229732223034,-56.571599774412,
-38.9634751990818));
#245014=CARTESIAN_POINT('Ctrl Pts',(-42.699209382297,-56.6219610565873,
-38.9664128682174));
#245015=CARTESIAN_POINT('Ctrl Pts',(-42.6756509453961,-56.6718870402692,
-38.9693251455661));
#245016=CARTESIAN_POINT('Ctrl Pts',(-42.6539431678017,-56.7232556458407,
-38.9723215636153));
#245017=CARTESIAN_POINT('Ctrl Pts',(-42.6343032293951,-56.7758552387935,
-38.9753898218966));
#245018=CARTESIAN_POINT('Ctrl Pts',(-42.6148606751112,-56.827926198494,
-38.9784272437538));
#245019=CARTESIAN_POINT('Ctrl Pts',(-42.5974451867678,-56.881203113289,
-38.9815350449805));
#245020=CARTESIAN_POINT('Ctrl Pts',(-42.582235617094,-56.93544112293,-38.9846989841965));
#245021=CARTESIAN_POINT('Ctrl Pts',(-42.5685080995495,-56.9843940680093,
-38.9875546225892));
#245022=CARTESIAN_POINT('Ctrl Pts',(-42.5565774230983,-57.0341291617399,
-38.9904559466857));
#245023=CARTESIAN_POINT('Ctrl Pts',(-42.5465468989916,-57.0844431661648,
-38.9933911308716));
#245024=CARTESIAN_POINT('Ctrl Pts',(43.4805771074156,-59.5712767529309,
-39.2399080357013));
#245025=CARTESIAN_POINT('Ctrl Pts',(43.4150727209207,-59.5358440364426,
-39.2223070534893));
#245026=CARTESIAN_POINT('Ctrl Pts',(43.2883193276586,-59.4590682572254,
-39.1867578392588));
#245027=CARTESIAN_POINT('Ctrl Pts',(43.1106712693135,-59.32658002426,-39.1324031814995));
#245028=CARTESIAN_POINT('Ctrl Pts',(43.0005921597408,-59.2266373021163,
-39.0954660506179));
#245029=CARTESIAN_POINT('Ctrl Pts',(42.8948534568781,-59.1207134074407,
-39.0581733199915));
#245030=CARTESIAN_POINT('Ctrl Pts',(42.7951360401793,-59.0104958554849,
-39.0211184761739));
#245031=CARTESIAN_POINT('Ctrl Pts',(42.6850011896347,-58.8622904152127,
-38.9753582681256));
#245032=CARTESIAN_POINT('Ctrl Pts',(42.6055727997797,-58.7375004045667,
-38.939089851323));
#245033=CARTESIAN_POINT('Ctrl Pts',(42.5503788594446,-58.6407591922129,
-38.9120596161462));
#245034=CARTESIAN_POINT('Ctrl Pts',(42.5165536369311,-58.5741539171446,
-38.8941613358138));
#245035=CARTESIAN_POINT('Ctrl Pts',(42.4842288567228,-58.5064298632496,
-38.8763157156907));
#245036=CARTESIAN_POINT('Ctrl Pts',(42.4689425396028,-58.4722695523732,
-38.8674882509199));
#245037=CARTESIAN_POINT('Ctrl Pts',(42.4257123024776,-58.3690064948315,
-38.8413136266604));
#245038=CARTESIAN_POINT('Ctrl Pts',(42.3750272156063,-58.229152189777,-38.8072100415055));
#245039=CARTESIAN_POINT('Ctrl Pts',(42.3380647902547,-58.0850119200902,
-38.7746901633276));
#245040=CARTESIAN_POINT('Ctrl Pts',(42.3155659796374,-57.9752818499468,
-38.7509105250088));
#245041=CARTESIAN_POINT('Ctrl Pts',(42.3089374211558,-57.9384266221928,
-38.7430843922672));
#245042=CARTESIAN_POINT('Ctrl Pts',(42.297458012674,-57.864178756387,-38.7276438637217));
#245043=CARTESIAN_POINT('Ctrl Pts',(42.292601515188,-57.8267325312259,-38.720018782004));
#245044=CARTESIAN_POINT('Ctrl Pts',(42.2847289916893,-57.7514526301959,
-38.7050196673963));
#245045=CARTESIAN_POINT('Ctrl Pts',(42.2817363521424,-57.7138759968928,
-38.6976962453237));
#245046=CARTESIAN_POINT('Ctrl Pts',(42.277596992864,-57.6387184974263,-38.6833720377019));
#245047=CARTESIAN_POINT('Ctrl Pts',(42.2741651307842,-57.5260409596698,
-38.6623829091612));
#245048=CARTESIAN_POINT('Ctrl Pts',(42.2805893100654,-57.3760354719141,
-38.6363740800325));
#245049=CARTESIAN_POINT('Ctrl Pts',(42.2937061680812,-57.2637038035873,
-38.618370061439));
#245050=CARTESIAN_POINT('Ctrl Pts',(42.3043247017591,-57.1888547452426,
-38.6067079534822));
#245051=CARTESIAN_POINT('Ctrl Pts',(42.3105743117123,-57.1514345461221,
-38.6010450635964));
#245052=CARTESIAN_POINT('Ctrl Pts',(42.3249704170347,-57.0766935209607,
-38.590076215021));
#245053=CARTESIAN_POINT('Ctrl Pts',(42.3331592025312,-57.0392159768686,
-38.5847494243559));
#245054=CARTESIAN_POINT('Ctrl Pts',(42.3512949844302,-56.9651221381903,
-38.5745673038812));
#245055=CARTESIAN_POINT('Ctrl Pts',(42.3712216906218,-56.8916587034686,
-38.564820665347));
#245056=CARTESIAN_POINT('Ctrl Pts',(42.4063979707918,-56.7834465224234,
-38.5515118436));
#245057=CARTESIAN_POINT('Ctrl Pts',(42.4468320479729,-56.6771725078319,
-38.5395042677724));
#245058=CARTESIAN_POINT('Ctrl Pts',(42.4925290654744,-56.5728473165674,
-38.5288039137004));
#245059=CARTESIAN_POINT('Ctrl Pts',(42.5265325119253,-56.5046058456765,
-38.5225509073062));
#245060=CARTESIAN_POINT('Ctrl Pts',(42.5623338475306,-56.4370293947697,
-38.5167461666044));
#245061=CARTESIAN_POINT('Ctrl Pts',(42.5811223641794,-56.4035923099625,
-38.5140693065785));
#245062=CARTESIAN_POINT('Ctrl Pts',(42.620584523009,-56.3373241998654,-38.5091697400817));
#245063=CARTESIAN_POINT('Ctrl Pts',(42.6411082254821,-56.3047465904101,
-38.5069659500128));
#245064=CARTESIAN_POINT('Ctrl Pts',(42.7048067991197,-56.2090283357163,
-38.501110858935));
#245065=CARTESIAN_POINT('Ctrl Pts',(42.7502234543428,-56.1476408662828,
-38.4981890389281));
#245066=CARTESIAN_POINT('Ctrl Pts',(42.8467942323831,-56.0297655581676,
-38.4942910511033));
#245067=CARTESIAN_POINT('Ctrl Pts',(42.8979715413934,-55.9732420482176,
-38.4933125989996));
#245068=CARTESIAN_POINT('Ctrl Pts',(42.9790570553347,-55.8921695883033,
-38.4933149859729));
#245069=CARTESIAN_POINT('Ctrl Pts',(43.0068374106561,-55.8657400908868,
-38.4935622007431));
#245070=CARTESIAN_POINT('Ctrl Pts',(43.0495800649421,-55.8270637749536,
-38.4943063068789));
#245071=CARTESIAN_POINT('Ctrl Pts',(43.0640222060113,-55.8143203511958,
-38.494617152342));
#245072=CARTESIAN_POINT('Ctrl Pts',(43.0932714774893,-55.7891564261061,
-38.4953646906773));
#245073=CARTESIAN_POINT('Ctrl Pts',(43.1080901283632,-55.7767277938553,
-38.4958020036096));
#245074=CARTESIAN_POINT('Ctrl Pts',(43.1528523310046,-55.7401327167866,
-38.4972962980169));
#245075=CARTESIAN_POINT('Ctrl Pts',(43.2134913856688,-55.6930468850421,
-38.4997758707861));
#245076=CARTESIAN_POINT('Ctrl Pts',(43.3385569247743,-55.6055389451161,
-38.5066450244003));
#245077=CARTESIAN_POINT('Ctrl Pts',(43.4691986576013,-55.5278792007279,
-38.5163302992824));
#245078=CARTESIAN_POINT('Ctrl Pts',(43.5713395927684,-55.4769743237494,
-38.5256877381308));
#245079=CARTESIAN_POINT('Ctrl Pts',(43.6403672861995,-55.4446857735354,
-38.5323951500278));
#245080=CARTESIAN_POINT('Ctrl Pts',(43.6753577685123,-55.4293620157832,
-38.5359845633874));
#245081=CARTESIAN_POINT('Ctrl Pts',(43.7462462065788,-55.4003985583156,
-38.5436333065981));
#245082=CARTESIAN_POINT('Ctrl Pts',(43.7822717759725,-55.3867204456352,
-38.5477088862383));
#245083=CARTESIAN_POINT('Ctrl Pts',(43.8543821738219,-55.3613797848081,
-38.5562346427694));
#245084=CARTESIAN_POINT('Ctrl Pts',(43.890622407919,-55.349649082917,-38.5607007444526));
#245085=CARTESIAN_POINT('Ctrl Pts',(43.9997560709039,-55.3172704656441,
-38.5746802407103));
#245086=CARTESIAN_POINT('Ctrl Pts',(44.1098017310836,-55.290468361793,-38.5898286859852));
#245087=CARTESIAN_POINT('Ctrl Pts',(44.2583166685835,-55.2656490138239,
-38.612301023075));
#245088=CARTESIAN_POINT('Ctrl Pts',(44.3705972700495,-55.2524997368729,
-38.6302900391873));
#245089=CARTESIAN_POINT('Ctrl Pts',(44.446056048267,-55.2474029004138,-38.6430428201589));
#245090=CARTESIAN_POINT('Ctrl Pts',(44.5218128020516,-55.2441636366351,
-38.65617756452));
#245091=CARTESIAN_POINT('Ctrl Pts',(44.5599089424743,-55.2434808562086,
-38.6629497802385));
#245092=CARTESIAN_POINT('Ctrl Pts',(44.6354869543582,-55.2439911084578,
-38.6767130108817));
#245093=CARTESIAN_POINT('Ctrl Pts',(44.6731456892459,-55.2451740103824,
-38.6837342374529));
#245094=CARTESIAN_POINT('Ctrl Pts',(44.7481014788608,-55.2493620066237,
-38.6980304684339));
#245095=CARTESIAN_POINT('Ctrl Pts',(44.860046548974,-55.2583760573225,-38.7198650218829));
#245096=CARTESIAN_POINT('Ctrl Pts',(45.0073845433675,-55.2811507310277,
-38.7505067688753));
#245097=CARTESIAN_POINT('Ctrl Pts',(45.1528189888476,-55.3146135839333,
-38.7826550300594));
#245098=CARTESIAN_POINT('Ctrl Pts',(45.2248832056965,-55.3349380951144,
-38.7992310848652));
#245099=CARTESIAN_POINT('Ctrl Pts',(45.2966462681613,-55.3570913336823,
-38.8160672125853));
#245100=CARTESIAN_POINT('Ctrl Pts',(45.3323638946335,-55.3690863290504,
-38.8246135819642));
#245101=CARTESIAN_POINT('Ctrl Pts',(45.4027951436545,-55.3946744461232,
-38.841798196801));
#245102=CARTESIAN_POINT('Ctrl Pts',(45.4376370321487,-55.4083060218429,
-38.85046633842));
#245103=CARTESIAN_POINT('Ctrl Pts',(45.5409345111852,-55.4516493275196,
-38.8766665754573));
#245104=CARTESIAN_POINT('Ctrl Pts',(45.6082182891413,-55.4838201174091,
-38.8944064774514));
#245105=CARTESIAN_POINT('Ctrl Pts',(45.7067749877369,-55.5369855856676,
-38.9214216121435));
#245106=CARTESIAN_POINT('Ctrl Pts',(45.7392219877795,-55.5555212114618,
-38.9304915704334));
#245107=CARTESIAN_POINT('Ctrl Pts',(45.8033556832395,-55.5942722159849,
-38.9487787872477));
#245108=CARTESIAN_POINT('Ctrl Pts',(45.8348443691401,-55.6143675312756,
-38.9579395118015));
#245109=CARTESIAN_POINT('Ctrl Pts',(45.9274099842789,-55.6766589025306,
-38.9854159162723));
#245110=CARTESIAN_POINT('Ctrl Pts',(45.9867610865919,-55.7209353156014,
-39.0037703637879));
#245111=CARTESIAN_POINT('Ctrl Pts',(46.1007337830098,-55.8148102393793,
-39.0405190865864));
#245112=CARTESIAN_POINT('Ctrl Pts',(46.1826971388658,-55.889219933262,-39.0681181728269));
#245113=CARTESIAN_POINT('Ctrl Pts',(46.259356574729,-55.9696687352924,-39.0957737179551));
#245114=CARTESIAN_POINT('Ctrl Pts',(46.309266807939,-56.024663053365,-39.1142236413887));
#245115=CARTESIAN_POINT('Ctrl Pts',(46.3336138177017,-56.0528284109483,
-39.1234510495426));
#245116=CARTESIAN_POINT('Ctrl Pts',(46.3692509284248,-56.0961546965833,
-39.1373141736981));
#245117=CARTESIAN_POINT('Ctrl Pts',(46.3809719555493,-56.1107655250657,
-39.14193505412));
#245118=CARTESIAN_POINT('Ctrl Pts',(46.4039850968433,-56.1401806715041,
-39.1511314768264));
#245119=CARTESIAN_POINT('Ctrl Pts',(46.4153001903629,-56.1550126624776,
-39.1557159133813));
#245120=CARTESIAN_POINT('Ctrl Pts',(46.4486370096885,-56.1998310060263,
-39.1694131182659));
#245121=CARTESIAN_POINT('Ctrl Pts',(46.4700835091466,-56.2301795317326,
-39.1784826054425));
#245122=CARTESIAN_POINT('Ctrl Pts',(46.532071913686,-56.3225583984772,-39.2054898733524));
#245123=CARTESIAN_POINT('Ctrl Pts',(46.5894197348374,-56.4176636744323,
-39.23211607576));
#245124=CARTESIAN_POINT('Ctrl Pts',(46.6566074362748,-56.5498680842415,
-39.2668544229849));
#245125=CARTESIAN_POINT('Ctrl Pts',(46.6870820302515,-56.617790568625,-39.2839693714534));
#245126=CARTESIAN_POINT('Ctrl Pts',(46.7159729830272,-56.6866360545619,
-39.3009558869148));
#245127=CARTESIAN_POINT('Ctrl Pts',(46.7296188023799,-56.7214992889704,
-39.3093799218186));
#245128=CARTESIAN_POINT('Ctrl Pts',(46.7553216997643,-56.7922546384013,
-39.3261176641085));
#245129=CARTESIAN_POINT('Ctrl Pts',(46.7672996943011,-56.8279354881579,
-39.3343809787628));
#245130=CARTESIAN_POINT('Ctrl Pts',(46.8004530502947,-56.9353633959568,
-39.358737163018));
#245131=CARTESIAN_POINT('Ctrl Pts',(46.8189795501832,-57.0077635587999,
-39.3744658121213));
#245132=CARTESIAN_POINT('Ctrl Pts',(46.848916211803,-57.1540080946302,-39.4048998290393));
#245133=CARTESIAN_POINT('Ctrl Pts',(46.866048617508,-57.2647966217996,-39.4269646939479));
#245134=CARTESIAN_POINT('Ctrl Pts',(46.875074749658,-57.3772756893033,-39.4478819384746));
#245135=CARTESIAN_POINT('Ctrl Pts',(46.8792542953452,-57.4526370309597,
-39.4615663943076));
#245136=CARTESIAN_POINT('Ctrl Pts',(46.8804258736835,-57.4905390832845,
-39.4682843608713));
#245137=CARTESIAN_POINT('Ctrl Pts',(46.8808837743635,-57.566610437341,-39.4814341960201));
#245138=CARTESIAN_POINT('Ctrl Pts',(46.8801708637706,-57.604491394965,-39.4878166677226));
#245139=CARTESIAN_POINT('Ctrl Pts',(46.8768913879562,-57.6800597985945,
-39.5002231148134));
#245140=CARTESIAN_POINT('Ctrl Pts',(46.8691896925243,-57.7930657109158,
-39.5182849936093));
#245141=CARTESIAN_POINT('Ctrl Pts',(46.8479069711518,-57.9423669591112,
-39.540205996752));
#245142=CARTESIAN_POINT('Ctrl Pts',(46.8236459543104,-58.053306681129,-39.5550278422771));
#245143=CARTESIAN_POINT('Ctrl Pts',(46.8055990109883,-58.1270324939452,
-39.5645447403379));
#245144=CARTESIAN_POINT('Ctrl Pts',(46.7956339676918,-58.1637938532181,
-39.5691227921436));
#245145=CARTESIAN_POINT('Ctrl Pts',(46.7738161327052,-58.2370162077019,
-39.5779016468881));
#245146=CARTESIAN_POINT('Ctrl Pts',(46.7619036278491,-58.2736352268715,
-39.5821192203466));
#245147=CARTESIAN_POINT('Ctrl Pts',(46.7364059718256,-58.3458255995332,
-39.5900871854462));
#245148=CARTESIAN_POINT('Ctrl Pts',(46.7091836493705,-58.4171862986019,
-39.5976163356366));
#245149=CARTESIAN_POINT('Ctrl Pts',(46.663274408039,-58.5216699086648,-39.6076014242402));
#245150=CARTESIAN_POINT('Ctrl Pts',(46.6123207377325,-58.6236436013082,
-39.616293729045));
#245151=CARTESIAN_POINT('Ctrl Pts',(46.5563244858032,-58.7230996041114,
-39.6236943138341));
#245152=CARTESIAN_POINT('Ctrl Pts',(46.515607032986,-58.7877140896312,-39.6277619492082));
#245153=CARTESIAN_POINT('Ctrl Pts',(46.4731710833873,-58.8514710047945,
-39.6313905635194));
#245154=CARTESIAN_POINT('Ctrl Pts',(46.4511086137465,-58.8829006319494,
-39.6329844599904));
#245155=CARTESIAN_POINT('Ctrl Pts',(46.4051673201274,-58.9449633016888,
-39.6357273485653));
#245156=CARTESIAN_POINT('Ctrl Pts',(46.381447994276,-58.975377588932,-39.6368662598532));
#245157=CARTESIAN_POINT('Ctrl Pts',(46.3084068909562,-59.0643493136614,
-39.6395761233691));
#245158=CARTESIAN_POINT('Ctrl Pts',(46.2570407846102,-59.1209150453974,
-39.6404603784325));
#245159=CARTESIAN_POINT('Ctrl Pts',(46.1491379755941,-59.228544463199,-39.6404138814247));
#245160=CARTESIAN_POINT('Ctrl Pts',(46.0925836555155,-59.2796343044913,
-39.6394845811684));
#245161=CARTESIAN_POINT('Ctrl Pts',(46.0038529437629,-59.3521266125547,
-39.6367223387528));
#245162=CARTESIAN_POINT('Ctrl Pts',(45.9736068078661,-59.3756113554055,
-39.6355721163029));
#245163=CARTESIAN_POINT('Ctrl Pts',(45.9272656961273,-59.4097723546528,
-39.6334997725088));
#245164=CARTESIAN_POINT('Ctrl Pts',(45.9116419215573,-59.4209912820171,
-39.6327502808957));
#245165=CARTESIAN_POINT('Ctrl Pts',(45.8800804794677,-59.4430610802669,
-39.6311351339295));
#245166=CARTESIAN_POINT('Ctrl Pts',(45.8321587971618,-59.4756823489919,
-39.628531354857));
#245167=CARTESIAN_POINT('Ctrl Pts',(45.7834097108732,-59.5062438963941,
-39.6254355071979));
#245168=CARTESIAN_POINT('Ctrl Pts',(45.717633106262,-59.5452481912826,-39.6208773262667));
#245169=CARTESIAN_POINT('Ctrl Pts',(45.6178307490054,-59.601113548897,-39.6133952897297));
#245170=CARTESIAN_POINT('Ctrl Pts',(45.4802897643185,-59.6652183443042,
-39.6008811885904));
#245171=CARTESIAN_POINT('Ctrl Pts',(45.3738098009101,-59.7055766782111,
-39.5896017905935));
#245172=CARTESIAN_POINT('Ctrl Pts',(45.3020778813705,-59.7307512119865,
-39.5816566825671));
#245173=CARTESIAN_POINT('Ctrl Pts',(45.2658207311094,-59.7424779859237,
-39.5774690651077));
#245174=CARTESIAN_POINT('Ctrl Pts',(45.1926264675053,-59.7641596016776,
-39.5686715125846));
#245175=CARTESIAN_POINT('Ctrl Pts',(45.1555073907618,-59.7741562512684,
-39.5640376159893));
#245176=CARTESIAN_POINT('Ctrl Pts',(45.0441315765335,-59.8011904590316,
-39.5496210468413));
#245177=CARTESIAN_POINT('Ctrl Pts',(44.9324484012679,-59.8224577850013,
-39.5341534065747));
#245178=CARTESIAN_POINT('Ctrl Pts',(44.8203079610257,-59.8353953605365,
-39.5171556909205));
#245179=CARTESIAN_POINT('Ctrl Pts',(44.7080184564226,-59.8455760612675,
-39.4996502778008));
#245180=CARTESIAN_POINT('Ctrl Pts',(44.6329372249224,-59.8486931621852,
-39.4873001861445));
#245181=CARTESIAN_POINT('Ctrl Pts',(44.5200834441659,-59.8478515133141,
-39.4677634802869));
#245182=CARTESIAN_POINT('Ctrl Pts',(44.4823810871712,-59.8466449718289,
-39.4610736497974));
#245183=CARTESIAN_POINT('Ctrl Pts',(44.4258051079382,-59.8434394706745,
-39.4507883432074));
#245184=CARTESIAN_POINT('Ctrl Pts',(44.4069254589855,-59.8421361346926,
-39.4473147915973));
#245185=CARTESIAN_POINT('Ctrl Pts',(44.3691376542581,-59.8390581625153,
-39.4402793331445));
#245186=CARTESIAN_POINT('Ctrl Pts',(44.3502459350849,-59.8372838734483,
-39.4367203104461));
#245187=CARTESIAN_POINT('Ctrl Pts',(44.2562487381671,-59.8272835659938,
-39.4188041728073));
#245188=CARTESIAN_POINT('Ctrl Pts',(44.1080045765469,-59.8040393501646,
-39.3892226636159));
#245189=CARTESIAN_POINT('Ctrl Pts',(43.9639303529155,-59.7668593120831,
-39.3578670379715));
#245190=CARTESIAN_POINT('Ctrl Pts',(43.8219159040518,-59.7227861654643,
-39.3256251231267));
#245191=CARTESIAN_POINT('Ctrl Pts',(43.7519290534068,-59.6972943066161,
-39.3090578287531));
#245192=CARTESIAN_POINT('Ctrl Pts',(43.665783177736,-59.6610675807531,-39.2877890488175));
#245193=CARTESIAN_POINT('Ctrl Pts',(43.6486106666635,-59.653596197985,-39.2835041280971));
#245194=CARTESIAN_POINT('Ctrl Pts',(43.6144193015916,-59.6382222359849,
-39.2748825183767));
#245195=CARTESIAN_POINT('Ctrl Pts',(43.597366582891,-59.6303022352814,-39.2705368924251));
#245196=CARTESIAN_POINT('Ctrl Pts',(43.5465994182959,-59.605961903298,-39.2574616452183));
#245197=CARTESIAN_POINT('Ctrl Pts',(43.513329300663,-59.588993111175,-39.2487085268073));
#245198=CARTESIAN_POINT('Ctrl Pts',(43.4805771074156,-59.5712767529309,
-39.2399080357013));
#245199=CARTESIAN_POINT('Ctrl Pts',(43.8903154257419,-57.7291941381088,
-41.4266127101804));
#245200=CARTESIAN_POINT('Ctrl Pts',(43.8716814361492,-57.7189244770852,
-41.4090117279687));
#245201=CARTESIAN_POINT('Ctrl Pts',(43.8355945080866,-57.6967277837834,
-41.3734625137379));
#245202=CARTESIAN_POINT('Ctrl Pts',(43.7849271573585,-57.6585752750105,
-41.3191078559793));
#245203=CARTESIAN_POINT('Ctrl Pts',(43.753465403225,-57.62988352171,-41.2821707250961));
#245204=CARTESIAN_POINT('Ctrl Pts',(43.7232071092872,-57.5995155202448,
-41.2448779944712));
#245205=CARTESIAN_POINT('Ctrl Pts',(43.694633283399,-57.5679550683129,-41.2078231506529));
#245206=CARTESIAN_POINT('Ctrl Pts',(43.6629744005209,-57.5256074013359,
-41.162062942605));
#245207=CARTESIAN_POINT('Ctrl Pts',(43.6400741040405,-57.4900012877665,
-41.1257945258022));
#245208=CARTESIAN_POINT('Ctrl Pts',(43.624122646482,-57.4624228770549,-41.0987642906252));
#245209=CARTESIAN_POINT('Ctrl Pts',(43.6143188854815,-57.4434516436916,
-41.0808660102928));
#245210=CARTESIAN_POINT('Ctrl Pts',(43.6049343759216,-57.4241698350281,
-41.0630203901697));
#245211=CARTESIAN_POINT('Ctrl Pts',(43.6004882740613,-57.4144479878336,
-41.054192925399));
#245212=CARTESIAN_POINT('Ctrl Pts',(43.5878889573419,-57.3850715912746,
-41.0280183011396));
#245213=CARTESIAN_POINT('Ctrl Pts',(43.5730447416356,-57.3453166524842,
-40.9939147159844));
#245214=CARTESIAN_POINT('Ctrl Pts',(43.5620571572655,-57.3044044614592,
-40.9613948378065));
#245215=CARTESIAN_POINT('Ctrl Pts',(43.5552843243605,-57.2732819874194,
-40.9376151994878));
#245216=CARTESIAN_POINT('Ctrl Pts',(43.5532714802541,-57.2628325912303,
-40.9297890667463));
#245217=CARTESIAN_POINT('Ctrl Pts',(43.5497454556161,-57.2417890776549,
-40.9143485382007));
#245218=CARTESIAN_POINT('Ctrl Pts',(43.5482304746054,-57.2311797832666,
-40.9067234564832));
#245219=CARTESIAN_POINT('Ctrl Pts',(43.5457184756399,-57.2098591834555,
-40.8917243418755));
#245220=CARTESIAN_POINT('Ctrl Pts',(43.5447290487245,-57.199220662917,-40.8844009198028));
#245221=CARTESIAN_POINT('Ctrl Pts',(43.5432711863927,-57.1779500447907,
-40.8700767121812));
#245222=CARTESIAN_POINT('Ctrl Pts',(43.5418684734652,-57.1460721839032,
-40.8490875836402));
#245223=CARTESIAN_POINT('Ctrl Pts',(43.5431039253892,-57.1036793909824,
-40.8230787545116));
#245224=CARTESIAN_POINT('Ctrl Pts',(43.5463738329101,-57.0719682486671,
-40.8050747359183));
#245225=CARTESIAN_POINT('Ctrl Pts',(43.5490829635055,-57.0508462881094,
-40.7934126279614));
#245226=CARTESIAN_POINT('Ctrl Pts',(43.5507030159248,-57.0402904723448,
-40.7877497380755));
#245227=CARTESIAN_POINT('Ctrl Pts',(43.5544790630841,-57.019214904491,-40.7767808895002));
#245228=CARTESIAN_POINT('Ctrl Pts',(43.5566463931059,-57.0086510117152,
-40.7714540988351));
#245229=CARTESIAN_POINT('Ctrl Pts',(43.5614808344627,-56.9877741662596,
-40.7612719783604));
#245230=CARTESIAN_POINT('Ctrl Pts',(43.5668234022498,-56.9670831174431,
-40.7515253398262));
#245231=CARTESIAN_POINT('Ctrl Pts',(43.5763377125496,-56.9366295208774,
-40.7382165180791));
#245232=CARTESIAN_POINT('Ctrl Pts',(43.5873444561754,-56.9067460923864,
-40.7262089422516));
#245233=CARTESIAN_POINT('Ctrl Pts',(43.5998453117462,-56.8774358278222,
-40.7155085881795));
#245234=CARTESIAN_POINT('Ctrl Pts',(43.6091839698139,-56.8582805167828,
-40.7092555817853));
#245235=CARTESIAN_POINT('Ctrl Pts',(43.6190331668358,-56.8393207538612,
-40.7034508410834));
#245236=CARTESIAN_POINT('Ctrl Pts',(43.6242099732076,-56.8299438685379,
-40.7007739810578));
#245237=CARTESIAN_POINT('Ctrl Pts',(43.6350986096338,-56.8113693026126,
-40.6958744145609));
#245238=CARTESIAN_POINT('Ctrl Pts',(43.6407690742328,-56.8022426567881,
-40.6936706244929));
#245239=CARTESIAN_POINT('Ctrl Pts',(43.6583896223854,-56.7754411523649,
-40.6878155334118));
#245240=CARTESIAN_POINT('Ctrl Pts',(43.6709801307092,-56.7582712890167,
-40.6848937134075));
#245241=CARTESIAN_POINT('Ctrl Pts',(43.6978023804218,-56.725340315416,-40.6809957255822));
#245242=CARTESIAN_POINT('Ctrl Pts',(43.7120405319879,-56.7095692151415,
-40.6800172734785));
#245243=CARTESIAN_POINT('Ctrl Pts',(43.7346338722206,-56.6869796178674,
-40.680019660452));
#245244=CARTESIAN_POINT('Ctrl Pts',(43.7423799312797,-56.6796208977126,
-40.6802668752224));
#245245=CARTESIAN_POINT('Ctrl Pts',(43.7543060585229,-56.6688607312791,
-40.681010981358));
#245246=CARTESIAN_POINT('Ctrl Pts',(43.7583370517177,-56.6653168192219,
-40.6813218268212));
#245247=CARTESIAN_POINT('Ctrl Pts',(43.7665035456834,-56.6583217341419,
-40.6820693651562));
#245248=CARTESIAN_POINT('Ctrl Pts',(43.7706422703,-56.6548683091639,-40.6825066780886));
#245249=CARTESIAN_POINT('Ctrl Pts',(43.7831478581881,-56.6447045100584,
-40.6840009724959));
#245250=CARTESIAN_POINT('Ctrl Pts',(43.8000992888712,-56.6316392340345,
-40.6864805452653));
#245251=CARTESIAN_POINT('Ctrl Pts',(43.8351004518507,-56.6074069729907,
-40.6933496988796));
#245252=CARTESIAN_POINT('Ctrl Pts',(43.8717190640765,-56.5859796680779,
-40.7030349737613));
#245253=CARTESIAN_POINT('Ctrl Pts',(43.9003898794618,-56.5719991465823,
-40.7123924126099));
#245254=CARTESIAN_POINT('Ctrl Pts',(43.919774692733,-56.5631479893168,-40.719099824507));
#245255=CARTESIAN_POINT('Ctrl Pts',(43.9296053152689,-56.5589560552736,
-40.722689237866));
#245256=CARTESIAN_POINT('Ctrl Pts',(43.9495302416178,-56.551051384942,-40.7303379810773));
#245257=CARTESIAN_POINT('Ctrl Pts',(43.959660471973,-56.5473282955902,-40.7344135607172));
#245258=CARTESIAN_POINT('Ctrl Pts',(43.9799461530017,-56.5404515818703,
-40.7429393172485));
#245259=CARTESIAN_POINT('Ctrl Pts',(43.9901452646573,-56.5372793127045,
-40.7474054189318));
#245260=CARTESIAN_POINT('Ctrl Pts',(44.0208712025373,-56.5285586047056,
-40.7613849151889));
#245261=CARTESIAN_POINT('Ctrl Pts',(44.0518784813599,-56.521416173947,-40.7765333604643));
#245262=CARTESIAN_POINT('Ctrl Pts',(44.0937728041468,-56.5149820273198,
-40.799005697554));
#245263=CARTESIAN_POINT('Ctrl Pts',(44.1254693703652,-56.5117027703592,
-40.8169947136667));
#245264=CARTESIAN_POINT('Ctrl Pts',(44.1467868482481,-56.5105547568045,
-40.8297474946377));
#245265=CARTESIAN_POINT('Ctrl Pts',(44.1681963264173,-56.50993223545,-40.842882238999));
#245266=CARTESIAN_POINT('Ctrl Pts',(44.1789665479467,-56.509886262238,-40.8496544547178));
#245267=CARTESIAN_POINT('Ctrl Pts',(44.2003410646824,-56.5103214152413,
-40.8634176853611));
#245268=CARTESIAN_POINT('Ctrl Pts',(44.2109953322312,-56.5108003631786,
-40.8704389119319));
#245269=CARTESIAN_POINT('Ctrl Pts',(44.2322091102727,-56.5122711761573,
-40.8847351429132));
#245270=CARTESIAN_POINT('Ctrl Pts',(44.2639028799147,-56.5152466319394,
-40.9065696963621));
#245271=CARTESIAN_POINT('Ctrl Pts',(44.305661850593,-56.5222422564611,-40.9372114433545));
#245272=CARTESIAN_POINT('Ctrl Pts',(44.346925841944,-56.532247127269,-40.9693597045385));
#245273=CARTESIAN_POINT('Ctrl Pts',(44.3673876336497,-56.53826115526,-40.9859357593442));
#245274=CARTESIAN_POINT('Ctrl Pts',(44.3877715667723,-56.5447901720246,
-41.0027718870644));
#245275=CARTESIAN_POINT('Ctrl Pts',(44.3979208506631,-56.5483132560745,
-41.0113182564434));
#245276=CARTESIAN_POINT('Ctrl Pts',(44.4179418071922,-56.5558066378292,
-41.02850287128));
#245277=CARTESIAN_POINT('Ctrl Pts',(44.4278499085732,-56.5597882829787,
-41.0371710128992));
#245278=CARTESIAN_POINT('Ctrl Pts',(44.4572364860018,-56.5724196473794,
-41.0633712499365));
#245279=CARTESIAN_POINT('Ctrl Pts',(44.4763932211824,-56.581758968269,-41.0811111519311));
#245280=CARTESIAN_POINT('Ctrl Pts',(44.5044772880921,-56.5971447477014,
-41.1081262866225));
#245281=CARTESIAN_POINT('Ctrl Pts',(44.5137271775895,-56.6025015227711,
-41.1171962449124));
#245282=CARTESIAN_POINT('Ctrl Pts',(44.5320183562985,-56.6136863880645,
-41.1354834617267));
#245283=CARTESIAN_POINT('Ctrl Pts',(44.5410031705763,-56.6194798267371,
-41.144644186283));
#245284=CARTESIAN_POINT('Ctrl Pts',(44.5674276642847,-56.6374191091633,
-41.1721205907467));
#245285=CARTESIAN_POINT('Ctrl Pts',(44.5843870769067,-56.6501457393646,
-41.1904750382678));
#245286=CARTESIAN_POINT('Ctrl Pts',(44.616987890196,-56.6770839740703,-41.2272237610649));
#245287=CARTESIAN_POINT('Ctrl Pts',(44.640458797708,-56.6984048650555,-41.2548228473058));
#245288=CARTESIAN_POINT('Ctrl Pts',(44.6624514458289,-56.7214114906953,
-41.2824783924342));
#245289=CARTESIAN_POINT('Ctrl Pts',(44.6767798128067,-56.7371294193188,
-41.3009283158679));
#245290=CARTESIAN_POINT('Ctrl Pts',(44.683774397772,-56.7451748501741,-41.3101557240219));
#245291=CARTESIAN_POINT('Ctrl Pts',(44.6940202659092,-56.7575442973705,
-41.324018848177));
#245292=CARTESIAN_POINT('Ctrl Pts',(44.6973914635031,-56.7617145235639,
-41.328639728599));
#245293=CARTESIAN_POINT('Ctrl Pts',(44.7040131878578,-56.770108052971,-41.3378361513053));
#245294=CARTESIAN_POINT('Ctrl Pts',(44.7072703203268,-56.7743392575068,
-41.3424205878605));
#245295=CARTESIAN_POINT('Ctrl Pts',(44.7168707027477,-56.7871217033085,
-41.3561177927451));
#245296=CARTESIAN_POINT('Ctrl Pts',(44.7230524906066,-56.7957731420119,
-41.3651872799216));
#245297=CARTESIAN_POINT('Ctrl Pts',(44.7409373255192,-56.8220955492914,
-41.3921945478314));
#245298=CARTESIAN_POINT('Ctrl Pts',(44.7575187561203,-56.8491712652862,
-41.4188207502394));
#245299=CARTESIAN_POINT('Ctrl Pts',(44.7770214494108,-56.88676384976,-41.453559097464));
#245300=CARTESIAN_POINT('Ctrl Pts',(44.7858965000619,-56.9060633365117,
-41.4706740459328));
#245301=CARTESIAN_POINT('Ctrl Pts',(44.7943266372896,-56.9256180211132,
-41.4876605613939));
#245302=CARTESIAN_POINT('Ctrl Pts',(44.7983169540911,-56.9355169983302,
-41.4960845962979));
#245303=CARTESIAN_POINT('Ctrl Pts',(44.8058516078422,-56.9556000996462,
-41.5128223385875));
#245304=CARTESIAN_POINT('Ctrl Pts',(44.8093727854448,-56.9657242505397,
-41.5210856532432));
#245305=CARTESIAN_POINT('Ctrl Pts',(44.8191505788346,-56.9961959016236,
-41.5454418374945));
#245306=CARTESIAN_POINT('Ctrl Pts',(44.8246597322132,-57.0167187198372,
-41.5611704866007));
#245307=CARTESIAN_POINT('Ctrl Pts',(44.8336688220904,-57.0581479791523,
-41.5916045035181));
#245308=CARTESIAN_POINT('Ctrl Pts',(44.8389236650083,-57.0895139074259,
-41.613669368427));
#245309=CARTESIAN_POINT('Ctrl Pts',(44.8418900765893,-57.1213299669285,
-41.6345866129535));
#245310=CARTESIAN_POINT('Ctrl Pts',(44.8433488372948,-57.142640498193,-41.6482710687869));
#245311=CARTESIAN_POINT('Ctrl Pts',(44.8438191277705,-57.1533552116615,
-41.6549890353504));
#245312=CARTESIAN_POINT('Ctrl Pts',(44.8442270800594,-57.1748537940466,
-41.6681388704993));
#245313=CARTESIAN_POINT('Ctrl Pts',(44.8441639040618,-57.1855561823783,
-41.6745213422017));
#245314=CARTESIAN_POINT('Ctrl Pts',(44.8435122114514,-57.2069000331791,
-41.6869277892926));
#245315=CARTESIAN_POINT('Ctrl Pts',(44.8417458896958,-57.2388084678274,
-41.7049896680882));
#245316=CARTESIAN_POINT('Ctrl Pts',(44.8362687719071,-57.2809279665006,
-41.7269106712316));
#245317=CARTESIAN_POINT('Ctrl Pts',(44.8298088085522,-57.3121969378441,
-41.7417325167562));
#245318=CARTESIAN_POINT('Ctrl Pts',(44.8249713776488,-57.3329705079708,
-41.751249414817));
#245319=CARTESIAN_POINT('Ctrl Pts',(44.8222858794974,-57.3433254378487,
-41.7558274666229));
#245320=CARTESIAN_POINT('Ctrl Pts',(44.8163797073795,-57.3639440769784,
-41.7646063213672));
#245321=CARTESIAN_POINT('Ctrl Pts',(44.8131427147447,-57.3742522416544,
-41.7688238948253));
#245322=CARTESIAN_POINT('Ctrl Pts',(44.8061917406462,-57.3945668799698,
-41.7767918599254));
#245323=CARTESIAN_POINT('Ctrl Pts',(44.7987498536529,-57.4146412549335,
-41.7843210101159));
#245324=CARTESIAN_POINT('Ctrl Pts',(44.7861419817956,-57.4440129710611,
-41.7943060987191));
#245325=CARTESIAN_POINT('Ctrl Pts',(44.7720982599006,-57.4726583092559,
-41.8029984035242));
#245326=CARTESIAN_POINT('Ctrl Pts',(44.7566193423106,-57.5005749992605,
-41.8103989883131));
#245327=CARTESIAN_POINT('Ctrl Pts',(44.7453362941317,-57.518697088903,-41.8144666236875));
#245328=CARTESIAN_POINT('Ctrl Pts',(44.7335642473644,-57.5365709174371,
-41.8180952379985));
#245329=CARTESIAN_POINT('Ctrl Pts',(44.7274378249752,-57.5453780864623,
-41.8196891344695));
#245330=CARTESIAN_POINT('Ctrl Pts',(44.7146685840676,-57.5627610237142,
-41.8224320230444));
#245331=CARTESIAN_POINT('Ctrl Pts',(44.7080700862024,-57.5712755128024,
-41.8235709343319));
#245332=CARTESIAN_POINT('Ctrl Pts',(44.6877341610586,-57.5961705213949,
-41.8262807978491));
#245333=CARTESIAN_POINT('Ctrl Pts',(44.6734117165454,-57.6119810052107,
-41.8271650529119));
#245334=CARTESIAN_POINT('Ctrl Pts',(44.6432859415473,-57.6420285404153,
-41.827118555904));
#245335=CARTESIAN_POINT('Ctrl Pts',(44.6274777219699,-57.6562729242579,
-41.8261892556471));
#245336=CARTESIAN_POINT('Ctrl Pts',(44.6026489360012,-57.6764545436153,
-41.823427013232));
#245337=CARTESIAN_POINT('Ctrl Pts',(44.5941811636919,-57.6829873126311,
-41.8222767907821));
#245338=CARTESIAN_POINT('Ctrl Pts',(44.5812011369499,-57.6924815728277,
-41.820204446988));
#245339=CARTESIAN_POINT('Ctrl Pts',(44.5768239301145,-57.6955981764101,
-41.8194549553751));
#245340=CARTESIAN_POINT('Ctrl Pts',(44.5679795363474,-57.7017261947271,
-41.8178398084084));
#245341=CARTESIAN_POINT('Ctrl Pts',(44.554547495243,-57.7107794649358,-41.8152360293365));
#245342=CARTESIAN_POINT('Ctrl Pts',(44.5408745509057,-57.7192473537464,
-41.812140181677));
#245343=CARTESIAN_POINT('Ctrl Pts',(44.5224181841827,-57.7300417662926,
-41.8075820007456));
#245344=CARTESIAN_POINT('Ctrl Pts',(44.494403164631,-57.7454824222945,-41.8000999642091));
#245345=CARTESIAN_POINT('Ctrl Pts',(44.4557509611988,-57.7631175354143,
-41.7875858630695));
#245346=CARTESIAN_POINT('Ctrl Pts',(44.4257963579031,-57.7741479888816,
-41.7763064650726));
#245347=CARTESIAN_POINT('Ctrl Pts',(44.4056101875344,-57.781009218212,-41.7683613570464));
#245348=CARTESIAN_POINT('Ctrl Pts',(44.3954036594654,-57.7841949818065,
-41.7641737395871));
#245349=CARTESIAN_POINT('Ctrl Pts',(44.3747925009816,-57.7900627169564,
-41.7553761870634));
#245350=CARTESIAN_POINT('Ctrl Pts',(44.3643365899562,-57.7927558542442,
-41.7507422904685));
#245351=CARTESIAN_POINT('Ctrl Pts',(44.3329536886806,-57.7999988857253,
-41.7363257213199));
#245352=CARTESIAN_POINT('Ctrl Pts',(44.3014645871824,-57.8056090798854,
-41.7208580810542));
#245353=CARTESIAN_POINT('Ctrl Pts',(44.2698183189435,-57.8088603667088,
-41.7038603653999));
#245354=CARTESIAN_POINT('Ctrl Pts',(44.2381206623806,-57.8113308880715,
-41.6863549522799));
#245355=CARTESIAN_POINT('Ctrl Pts',(44.2169139506954,-57.8119384373532,
-41.6740048606234));
#245356=CARTESIAN_POINT('Ctrl Pts',(44.1850197107514,-57.811287280344,-41.6544681547659));
#245357=CARTESIAN_POINT('Ctrl Pts',(44.1743613109546,-57.8108078241776,
-41.6477783242763));
#245358=CARTESIAN_POINT('Ctrl Pts',(44.1583626375358,-57.8096935003687,
-41.6374930176863));
#245359=CARTESIAN_POINT('Ctrl Pts',(44.1530230189312,-57.809255510817,-41.6340194660765));
#245360=CARTESIAN_POINT('Ctrl Pts',(44.1423341247923,-57.8082460206643,
-41.6269840076234));
#245361=CARTESIAN_POINT('Ctrl Pts',(44.1369894952372,-57.8076746784434,
-41.6234249849254));
#245362=CARTESIAN_POINT('Ctrl Pts',(44.1103928894951,-57.8045001122898,
-41.6055088472864));
#245363=CARTESIAN_POINT('Ctrl Pts',(44.0684216046586,-57.7973782151022,
-41.5759273380954));
#245364=CARTESIAN_POINT('Ctrl Pts',(44.0275807082801,-57.78632659952,-41.5445717124501));
#245365=CARTESIAN_POINT('Ctrl Pts',(43.9872978152183,-57.7733311875938,
-41.5123297976061));
#245366=CARTESIAN_POINT('Ctrl Pts',(43.9674326520914,-57.7658590768128,
-41.4957625032292));
#245367=CARTESIAN_POINT('Ctrl Pts',(43.942963744406,-57.7552890823142,-41.4744937232973));
#245368=CARTESIAN_POINT('Ctrl Pts',(43.938085174092,-57.7531113051098,-41.4702088025761));
#245369=CARTESIAN_POINT('Ctrl Pts',(43.9283699185172,-57.7486342535987,
-41.4615871928557));
#245370=CARTESIAN_POINT('Ctrl Pts',(43.9235236029976,-57.7463299238453,
-41.4572415669043));
#245371=CARTESIAN_POINT('Ctrl Pts',(43.9090930604083,-57.739254093668,-41.4441663196977));
#245372=CARTESIAN_POINT('Ctrl Pts',(43.8996324205383,-57.7343289686206,
-41.4354132012863));
#245373=CARTESIAN_POINT('Ctrl Pts',(43.8903154257419,-57.7291941381088,
-41.4266127101804));
#245374=CARTESIAN_POINT('',(44.1169604895359,-55.514043408345,-38.9933921916852));
#245375=CARTESIAN_POINT('',(42.8346996263142,-56.3799038065431,-38.9060746154351));
#245376=CARTESIAN_POINT('Ctrl Pts',(44.1169605045695,-55.5140434467185,
-38.9933921503467));
#245377=CARTESIAN_POINT('Ctrl Pts',(44.0897504669453,-55.5194672282592,
-38.9888363220206));
#245378=CARTESIAN_POINT('Ctrl Pts',(44.0626342052293,-55.5254611820674,
-38.9844176545342));
#245379=CARTESIAN_POINT('Ctrl Pts',(44.035612307405,-55.5320287845437,-38.9801370974184));
#245380=CARTESIAN_POINT('Ctrl Pts',(44.0037536535162,-55.5397719480894,
-38.9750903465021));
#245381=CARTESIAN_POINT('Ctrl Pts',(43.9720261635144,-55.5483124608923,
-38.9702355631519));
#245382=CARTESIAN_POINT('Ctrl Pts',(43.9404317247268,-55.5576620265682,
-38.9655757312954));
#245383=CARTESIAN_POINT('Ctrl Pts',(43.9088372843841,-55.5670115927043,
-38.9609158992096));
#245384=CARTESIAN_POINT('Ctrl Pts',(43.8773631496921,-55.5771759127617,
-38.9564497975263));
#245385=CARTESIAN_POINT('Ctrl Pts',(43.8460504835165,-55.5881565885239,
-38.9521869192607));
#245386=CARTESIAN_POINT('Ctrl Pts',(43.8147378173409,-55.5991372642861,
-38.9479240409952));
#245387=CARTESIAN_POINT('Ctrl Pts',(43.783451665776,-55.6109933882688,-38.943848461355));
#245388=CARTESIAN_POINT('Ctrl Pts',(43.7526711697336,-55.6235480058908,
-38.9400240897496));
#245389=CARTESIAN_POINT('Ctrl Pts',(43.7218906736911,-55.6361026235129,
-38.9361997181442));
#245390=CARTESIAN_POINT('Ctrl Pts',(43.6915050002909,-55.6493890121587,
-38.9326103047847));
#245391=CARTESIAN_POINT('Ctrl Pts',(43.661534024224,-55.6633885075075,-38.9292565988362));
#245392=CARTESIAN_POINT('Ctrl Pts',(43.6315630481571,-55.6773880028563,
-38.9259028928876));
#245393=CARTESIAN_POINT('Ctrl Pts',(43.6019980471442,-55.692103160754,-38.9227836007446));
#245394=CARTESIAN_POINT('Ctrl Pts',(43.5728356374758,-55.7075279772239,
-38.9198969730841));
#245395=CARTESIAN_POINT('Ctrl Pts',(43.5145108357497,-55.738377600849,-38.9141237195064));
#245396=CARTESIAN_POINT('Ctrl Pts',(43.4577942192328,-55.7720615501898,
-38.9092810747706));
#245397=CARTESIAN_POINT('Ctrl Pts',(43.4026941814562,-55.8085977570299,
-38.9053773125136));
#245398=CARTESIAN_POINT('Ctrl Pts',(43.3751441635105,-55.826865859825,-38.9034254314518));
#245399=CARTESIAN_POINT('Ctrl Pts',(43.3479989433793,-55.8458479689402,
-38.9017082565312));
#245400=CARTESIAN_POINT('Ctrl Pts',(43.3212654553579,-55.8655537371234,
-38.9002297378292));
#245401=CARTESIAN_POINT('Ctrl Pts',(43.2945319332195,-55.885259530455,-38.8987512172404));
#245402=CARTESIAN_POINT('Ctrl Pts',(43.2682103298005,-55.9056892736175,
-38.8975114537103));
#245403=CARTESIAN_POINT('Ctrl Pts',(43.2423046180206,-55.9268610072553,
-38.8965152565023));
#245404=CARTESIAN_POINT('Ctrl Pts',(43.2293517743067,-55.9374468641231,
-38.8960171583666));
#245405=CARTESIAN_POINT('Ctrl Pts',(43.2164877853448,-55.9482328356115,
-38.8955798454342));
#245406=CARTESIAN_POINT('Ctrl Pts',(43.2037924561014,-55.9591521490568,
-38.8952060762666));
#245407=CARTESIAN_POINT('Ctrl Pts',(43.191097126858,-55.9700714625021,-38.8948323070989));
#245408=CARTESIAN_POINT('Ctrl Pts',(43.1785604553322,-55.9811311728431,
-38.8945214616358));
#245409=CARTESIAN_POINT('Ctrl Pts',(43.1661929384724,-55.9923201879255,
-38.8942734262572));
#245410=CARTESIAN_POINT('Ctrl Pts',(43.1414579047527,-56.0146982180904,
-38.8937773555001));
#245411=CARTESIAN_POINT('Ctrl Pts',(43.117344267243,-56.0376373429098,-38.8935301407297));
#245412=CARTESIAN_POINT('Ctrl Pts',(43.0938842149535,-56.0610936119007,
-38.8935293450719));
#245413=CARTESIAN_POINT('Ctrl Pts',(43.0469641103745,-56.1080061498823,
-38.8935277537563));
#245414=CARTESIAN_POINT('Ctrl Pts',(43.0025474813891,-56.1570710705974,
-38.8945062058602));
#245415=CARTESIAN_POINT('Ctrl Pts',(42.9606448514092,-56.2082353818758,
-38.8964551997727));
#245416=CARTESIAN_POINT('Ctrl Pts',(42.9187422214293,-56.2593996931541,
-38.8984041936851));
#245417=CARTESIAN_POINT('Ctrl Pts',(42.8793334746424,-56.3126943660299,
-38.9013260136915));
#245418=CARTESIAN_POINT('Ctrl Pts',(42.8424899550942,-56.3680976795844,
-38.9052294077438));
#245419=CARTESIAN_POINT('Ctrl Pts',(42.8398779414905,-56.372025485898,-38.9055061380478));
#245420=CARTESIAN_POINT('Ctrl Pts',(42.8372783432785,-56.3759650434577,
-38.9057879244666));
#245421=CARTESIAN_POINT('Ctrl Pts',(42.8346994073709,-56.3799036571657,
-38.906073887373));
#245422=CARTESIAN_POINT('Ctrl Pts',(42.8346999571654,-56.3799040703247,
-38.9060752480495));
#245423=CARTESIAN_POINT('Ctrl Pts',(42.9101948352659,-56.2755386802039,
-38.9101094563356));
#245424=CARTESIAN_POINT('Ctrl Pts',(42.9944552171636,-56.1777247440651,
-38.9149819711245));
#245425=CARTESIAN_POINT('Ctrl Pts',(43.1750149383427,-56.0013540627946,
-38.9259216140551));
#245426=CARTESIAN_POINT('Ctrl Pts',(43.2698921661549,-55.922757935853,-38.931882518117));
#245427=CARTESIAN_POINT('Ctrl Pts',(43.3738733865066,-55.8500563343114,
-38.9385804803669));
#245428=CARTESIAN_POINT('Ctrl Pts',(43.3770600568266,-55.847840486669,-38.9387859039925));
#245429=CARTESIAN_POINT('Ctrl Pts',(43.3868444233345,-55.8410742771104,
-38.9394171105667));
#245430=CARTESIAN_POINT('Ctrl Pts',(43.393460399576,-55.8365509664054,-38.9398445749671));
#245431=CARTESIAN_POINT('Ctrl Pts',(43.4984963686718,-55.7655548257614,
-38.9466415987992));
#245432=CARTESIAN_POINT('Ctrl Pts',(43.6024979667475,-55.7065542689109,
-38.9534619752777));
#245433=CARTESIAN_POINT('Ctrl Pts',(43.8415689376835,-55.5957793032466,
-38.9708427154357));
#245434=CARTESIAN_POINT('Ctrl Pts',(43.9774091399379,-55.5482478649706,
-38.9815644662213));
#245435=CARTESIAN_POINT('Ctrl Pts',(44.1169604613867,-55.5140433046816,
-38.9933922348093));
#245436=CARTESIAN_POINT('Ctrl Pts',(46.1766977413729,-57.4754524783491,
-52.99995));
#245437=CARTESIAN_POINT('Ctrl Pts',(46.1766977413729,-56.5120019399699,
-52.9416166666667));
#245438=CARTESIAN_POINT('Ctrl Pts',(45.3423250998467,-56.0302766707802,
-52.8832833333334));
#245439=CARTESIAN_POINT('Ctrl Pts',(44.5079524583205,-55.5485514015906,
-52.82495));
#245440=CARTESIAN_POINT('Ctrl Pts',(43.6735798167943,-56.0302766707802,
-52.7666166666667));
#245441=CARTESIAN_POINT('Ctrl Pts',(42.839207175268,-56.5120019399698,-52.7082833333333));
#245442=CARTESIAN_POINT('Ctrl Pts',(42.839207175268,-57.4754524783491,-52.64995));
#245443=CARTESIAN_POINT('Ctrl Pts',(42.839207175268,-58.4389030167283,-52.5916166666666));
#245444=CARTESIAN_POINT('Ctrl Pts',(43.6735798167943,-58.920628285918,-52.5332833333334));
#245445=CARTESIAN_POINT('Ctrl Pts',(44.5079524583205,-59.4023535551075,
-52.4749500000001));
#245446=CARTESIAN_POINT('Ctrl Pts',(45.3423250998467,-58.920628285918,-52.4166166666667));
#245447=CARTESIAN_POINT('Ctrl Pts',(46.1766977413729,-58.4389030167283,
-52.3582833333334));
#245448=CARTESIAN_POINT('Ctrl Pts',(46.1766977413729,-57.4754524783491,
-52.29995));
#245449=CARTESIAN_POINT('Ctrl Pts',(46.1766977413729,-56.5120019399699,
-52.2416166666667));
#245450=CARTESIAN_POINT('Ctrl Pts',(45.3423250998467,-56.0302766707802,
-52.1832833333333));
#245451=CARTESIAN_POINT('Ctrl Pts',(44.5079524583205,-55.5485514015906,
-52.12495));
#245452=CARTESIAN_POINT('Ctrl Pts',(43.6735798167943,-56.0302766707802,
-52.0666166666667));
#245453=CARTESIAN_POINT('Ctrl Pts',(42.839207175268,-56.5120019399698,-52.0082833333333));
#245454=CARTESIAN_POINT('Ctrl Pts',(42.839207175268,-57.4754524783491,-51.94995));
#245455=CARTESIAN_POINT('Ctrl Pts',(42.839207175268,-58.4389030167283,-51.8916166666667));
#245456=CARTESIAN_POINT('Ctrl Pts',(43.6735798167943,-58.920628285918,-51.8332833333334));
#245457=CARTESIAN_POINT('Ctrl Pts',(44.5079524583205,-59.4023535551075,
-51.77495));
#245458=CARTESIAN_POINT('Ctrl Pts',(45.3423250998467,-58.920628285918,-51.7166166666667));
#245459=CARTESIAN_POINT('Ctrl Pts',(46.1766977413729,-58.4389030167283,
-51.6582833333333));
#245460=CARTESIAN_POINT('Ctrl Pts',(46.1766977413729,-57.4754524783491,
-51.59995));
#245461=CARTESIAN_POINT('Ctrl Pts',(46.1766977413729,-56.5120019399699,
-51.5416166666667));
#245462=CARTESIAN_POINT('Ctrl Pts',(45.3423250998467,-56.0302766707802,
-51.4832833333334));
#245463=CARTESIAN_POINT('Ctrl Pts',(44.5079524583205,-55.5485514015906,
-51.42495));
#245464=CARTESIAN_POINT('Ctrl Pts',(43.6735798167943,-56.0302766707802,
-51.3666166666667));
#245465=CARTESIAN_POINT('Ctrl Pts',(42.839207175268,-56.5120019399698,-51.3082833333333));
#245466=CARTESIAN_POINT('Ctrl Pts',(42.839207175268,-57.4754524783491,-51.24995));
#245467=CARTESIAN_POINT('Ctrl Pts',(42.839207175268,-58.4389030167283,-51.1916166666667));
#245468=CARTESIAN_POINT('Ctrl Pts',(43.6735798167943,-58.920628285918,-51.1332833333334));
#245469=CARTESIAN_POINT('Ctrl Pts',(44.5079524583205,-59.4023535551075,
-51.07495));
#245470=CARTESIAN_POINT('Ctrl Pts',(45.3423250998467,-58.920628285918,-51.0166166666667));
#245471=CARTESIAN_POINT('Ctrl Pts',(46.1766977413729,-58.4389030167283,
-50.9582833333334));
#245472=CARTESIAN_POINT('Ctrl Pts',(46.1766977413729,-57.4754524783491,
-50.89995));
#245473=CARTESIAN_POINT('Ctrl Pts',(46.1766977413729,-56.5120019399699,
-50.8416166666667));
#245474=CARTESIAN_POINT('Ctrl Pts',(45.3423250998467,-56.0302766707802,
-50.7832833333333));
#245475=CARTESIAN_POINT('Ctrl Pts',(44.5079524583205,-55.5485514015906,
-50.72495));
#245476=CARTESIAN_POINT('Ctrl Pts',(43.6735798167943,-56.0302766707802,
-50.6666166666667));
#245477=CARTESIAN_POINT('Ctrl Pts',(42.839207175268,-56.5120019399698,-50.6082833333334));
#245478=CARTESIAN_POINT('Ctrl Pts',(42.839207175268,-57.4754524783491,-50.54995));
#245479=CARTESIAN_POINT('Ctrl Pts',(42.839207175268,-58.4389030167283,-50.4916166666667));
#245480=CARTESIAN_POINT('Ctrl Pts',(43.6735798167943,-58.920628285918,-50.4332833333333));
#245481=CARTESIAN_POINT('Ctrl Pts',(44.5079524583205,-59.4023535551075,
-50.37495));
#245482=CARTESIAN_POINT('Ctrl Pts',(45.3423250998467,-58.920628285918,-50.3166166666667));
#245483=CARTESIAN_POINT('Ctrl Pts',(46.1766977413729,-58.4389030167283,
-50.2582833333334));
#245484=CARTESIAN_POINT('Ctrl Pts',(46.1766977413729,-57.4754524783491,
-50.19995));
#245485=CARTESIAN_POINT('Ctrl Pts',(46.1766977413729,-56.5120019399699,
-50.1416166666667));
#245486=CARTESIAN_POINT('Ctrl Pts',(45.3423250998467,-56.0302766707802,
-50.0832833333334));
#245487=CARTESIAN_POINT('Ctrl Pts',(44.5079524583205,-55.5485514015906,
-50.02495));
#245488=CARTESIAN_POINT('Ctrl Pts',(43.6735798167943,-56.0302766707802,
-49.9666166666667));
#245489=CARTESIAN_POINT('Ctrl Pts',(42.839207175268,-56.5120019399698,-49.9082833333334));
#245490=CARTESIAN_POINT('Ctrl Pts',(42.839207175268,-57.4754524783491,-49.84995));
#245491=CARTESIAN_POINT('Ctrl Pts',(42.839207175268,-58.4389030167283,-49.7916166666667));
#245492=CARTESIAN_POINT('Ctrl Pts',(43.6735798167943,-58.920628285918,-49.7332833333334));
#245493=CARTESIAN_POINT('Ctrl Pts',(44.5079524583205,-59.4023535551075,
-49.67495));
#245494=CARTESIAN_POINT('Ctrl Pts',(45.3423250998467,-58.920628285918,-49.6166166666667));
#245495=CARTESIAN_POINT('Ctrl Pts',(46.1766977413729,-58.4389030167283,
-49.5582833333334));
#245496=CARTESIAN_POINT('Ctrl Pts',(46.1766977413729,-57.4754524783491,
-49.49995));
#245497=CARTESIAN_POINT('Ctrl Pts',(46.1766977413729,-56.5120019399699,
-49.4416166666667));
#245498=CARTESIAN_POINT('Ctrl Pts',(45.3423250998467,-56.0302766707802,
-49.3832833333334));
#245499=CARTESIAN_POINT('Ctrl Pts',(44.5079524583205,-55.5485514015906,
-49.32495));
#245500=CARTESIAN_POINT('Ctrl Pts',(43.6735798167943,-56.0302766707802,
-49.2666166666667));
#245501=CARTESIAN_POINT('Ctrl Pts',(42.839207175268,-56.5120019399698,-49.2082833333334));
#245502=CARTESIAN_POINT('Ctrl Pts',(42.839207175268,-57.4754524783491,-49.14995));
#245503=CARTESIAN_POINT('Ctrl Pts',(42.839207175268,-58.4389030167283,-49.0916166666667));
#245504=CARTESIAN_POINT('Ctrl Pts',(43.6735798167943,-58.920628285918,-49.0332833333333));
#245505=CARTESIAN_POINT('Ctrl Pts',(44.5079524583205,-59.4023535551075,
-48.97495));
#245506=CARTESIAN_POINT('Ctrl Pts',(45.3423250998467,-58.920628285918,-48.9166166666667));
#245507=CARTESIAN_POINT('Ctrl Pts',(46.1766977413729,-58.4389030167283,
-48.8582833333333));
#245508=CARTESIAN_POINT('Ctrl Pts',(46.1766977413729,-57.4754524783491,
-48.79995));
#245509=CARTESIAN_POINT('Ctrl Pts',(46.1766977413729,-56.5120019399699,
-48.7416166666667));
#245510=CARTESIAN_POINT('Ctrl Pts',(45.3423250998467,-56.0302766707802,
-48.6832833333334));
#245511=CARTESIAN_POINT('Ctrl Pts',(44.5079524583205,-55.5485514015906,
-48.62495));
#245512=CARTESIAN_POINT('Ctrl Pts',(43.6735798167943,-56.0302766707802,
-48.5666166666667));
#245513=CARTESIAN_POINT('Ctrl Pts',(42.839207175268,-56.5120019399698,-48.5082833333334));
#245514=CARTESIAN_POINT('Ctrl Pts',(42.839207175268,-57.4754524783491,-48.44995));
#245515=CARTESIAN_POINT('Ctrl Pts',(42.839207175268,-58.4389030167283,-48.3916166666667));
#245516=CARTESIAN_POINT('Ctrl Pts',(43.6735798167943,-58.920628285918,-48.3332833333334));
#245517=CARTESIAN_POINT('Ctrl Pts',(44.5079524583205,-59.4023535551075,
-48.27495));
#245518=CARTESIAN_POINT('Ctrl Pts',(45.3423250998467,-58.920628285918,-48.2166166666667));
#245519=CARTESIAN_POINT('Ctrl Pts',(46.1766977413729,-58.4389030167283,
-48.1582833333334));
#245520=CARTESIAN_POINT('Ctrl Pts',(46.1766977413729,-57.4754524783491,
-48.09995));
#245521=CARTESIAN_POINT('Ctrl Pts',(46.1766977413729,-56.5120019399699,
-48.0416166666667));
#245522=CARTESIAN_POINT('Ctrl Pts',(45.3423250998467,-56.0302766707802,
-47.9832833333334));
#245523=CARTESIAN_POINT('Ctrl Pts',(44.5079524583205,-55.5485514015906,
-47.92495));
#245524=CARTESIAN_POINT('Ctrl Pts',(43.6735798167943,-56.0302766707802,
-47.8666166666667));
#245525=CARTESIAN_POINT('Ctrl Pts',(42.839207175268,-56.5120019399698,-47.8082833333333));
#245526=CARTESIAN_POINT('Ctrl Pts',(42.839207175268,-57.4754524783491,-47.74995));
#245527=CARTESIAN_POINT('Ctrl Pts',(42.839207175268,-58.4389030167283,-47.6916166666667));
#245528=CARTESIAN_POINT('Ctrl Pts',(43.6735798167943,-58.920628285918,-47.6332833333333));
#245529=CARTESIAN_POINT('Ctrl Pts',(44.5079524583205,-59.4023535551075,
-47.57495));
#245530=CARTESIAN_POINT('Ctrl Pts',(45.3423250998467,-58.920628285918,-47.5166166666667));
#245531=CARTESIAN_POINT('Ctrl Pts',(46.1766977413729,-58.4389030167283,
-47.4582833333333));
#245532=CARTESIAN_POINT('Ctrl Pts',(46.1766977413729,-57.4754524783491,
-47.39995));
#245533=CARTESIAN_POINT('Ctrl Pts',(46.1766977413729,-56.5120019399699,
-47.3416166666666));
#245534=CARTESIAN_POINT('Ctrl Pts',(45.3423250998467,-56.0302766707802,
-47.2832833333333));
#245535=CARTESIAN_POINT('Ctrl Pts',(44.5079524583205,-55.5485514015906,
-47.22495));
#245536=CARTESIAN_POINT('Ctrl Pts',(43.6735798167943,-56.0302766707802,
-47.1666166666667));
#245537=CARTESIAN_POINT('Ctrl Pts',(42.839207175268,-56.5120019399698,-47.1082833333333));
#245538=CARTESIAN_POINT('Ctrl Pts',(42.839207175268,-57.4754524783491,-47.04995));
#245539=CARTESIAN_POINT('Ctrl Pts',(42.839207175268,-58.4389030167283,-46.9916166666667));
#245540=CARTESIAN_POINT('Ctrl Pts',(43.6735798167943,-58.920628285918,-46.9332833333334));
#245541=CARTESIAN_POINT('Ctrl Pts',(44.5079524583205,-59.4023535551075,
-46.87495));
#245542=CARTESIAN_POINT('Ctrl Pts',(45.3423250998467,-58.920628285918,-46.8166166666667));
#245543=CARTESIAN_POINT('Ctrl Pts',(46.1766977413729,-58.4389030167283,
-46.7582833333333));
#245544=CARTESIAN_POINT('Ctrl Pts',(46.1766977413729,-57.4754524783491,
-46.69995));
#245545=CARTESIAN_POINT('Ctrl Pts',(46.1766977413729,-56.5120019399699,
-46.6416166666666));
#245546=CARTESIAN_POINT('Ctrl Pts',(45.3423250998467,-56.0302766707802,
-46.5832833333334));
#245547=CARTESIAN_POINT('Ctrl Pts',(44.5079524583205,-55.5485514015906,
-46.52495));
#245548=CARTESIAN_POINT('Ctrl Pts',(43.6735798167943,-56.0302766707802,
-46.4666166666667));
#245549=CARTESIAN_POINT('Ctrl Pts',(42.839207175268,-56.5120019399698,-46.4082833333333));
#245550=CARTESIAN_POINT('Ctrl Pts',(42.839207175268,-57.4754524783491,-46.34995));
#245551=CARTESIAN_POINT('Ctrl Pts',(42.839207175268,-58.4389030167283,-46.2916166666667));
#245552=CARTESIAN_POINT('Ctrl Pts',(43.6735798167943,-58.920628285918,-46.2332833333334));
#245553=CARTESIAN_POINT('Ctrl Pts',(44.5079524583205,-59.4023535551075,
-46.17495));
#245554=CARTESIAN_POINT('Ctrl Pts',(45.3423250998467,-58.920628285918,-46.1166166666667));
#245555=CARTESIAN_POINT('Ctrl Pts',(46.1766977413729,-58.4389030167283,
-46.0582833333333));
#245556=CARTESIAN_POINT('Ctrl Pts',(46.1766977413729,-57.4754524783491,
-45.99995));
#245557=CARTESIAN_POINT('Ctrl Pts',(46.1766977413729,-56.5120019399699,
-45.9416166666667));
#245558=CARTESIAN_POINT('Ctrl Pts',(45.3423250998467,-56.0302766707802,
-45.8832833333333));
#245559=CARTESIAN_POINT('Ctrl Pts',(44.5079524583205,-55.5485514015906,
-45.82495));
#245560=CARTESIAN_POINT('Ctrl Pts',(43.6735798167943,-56.0302766707802,
-45.7666166666667));
#245561=CARTESIAN_POINT('Ctrl Pts',(42.839207175268,-56.5120019399698,-45.7082833333333));
#245562=CARTESIAN_POINT('Ctrl Pts',(42.839207175268,-57.4754524783491,-45.64995));
#245563=CARTESIAN_POINT('Ctrl Pts',(42.839207175268,-58.4389030167283,-45.5916166666667));
#245564=CARTESIAN_POINT('Ctrl Pts',(43.6735798167943,-58.920628285918,-45.5332833333333));
#245565=CARTESIAN_POINT('Ctrl Pts',(44.5079524583205,-59.4023535551075,
-45.47495));
#245566=CARTESIAN_POINT('Ctrl Pts',(45.3423250998467,-58.920628285918,-45.4166166666667));
#245567=CARTESIAN_POINT('Ctrl Pts',(46.1766977413729,-58.4389030167283,
-45.3582833333333));
#245568=CARTESIAN_POINT('Ctrl Pts',(46.1766977413729,-57.4754524783491,
-45.29995));
#245569=CARTESIAN_POINT('Ctrl Pts',(46.1766977413729,-56.5120019399699,
-45.2416166666667));
#245570=CARTESIAN_POINT('Ctrl Pts',(45.3423250998467,-56.0302766707802,
-45.1832833333334));
#245571=CARTESIAN_POINT('Ctrl Pts',(44.5079524583205,-55.5485514015906,
-45.12495));
#245572=CARTESIAN_POINT('Ctrl Pts',(43.6735798167943,-56.0302766707802,
-45.0666166666667));
#245573=CARTESIAN_POINT('Ctrl Pts',(42.839207175268,-56.5120019399698,-45.0082833333334));
#245574=CARTESIAN_POINT('Ctrl Pts',(42.839207175268,-57.4754524783491,-44.94995));
#245575=CARTESIAN_POINT('Ctrl Pts',(42.839207175268,-58.4389030167283,-44.8916166666667));
#245576=CARTESIAN_POINT('Ctrl Pts',(43.6735798167943,-58.920628285918,-44.8332833333334));
#245577=CARTESIAN_POINT('Ctrl Pts',(44.5079524583205,-59.4023535551075,
-44.77495));
#245578=CARTESIAN_POINT('Ctrl Pts',(45.3423250998467,-58.920628285918,-44.7166166666667));
#245579=CARTESIAN_POINT('Ctrl Pts',(46.1766977413729,-58.4389030167283,
-44.6582833333334));
#245580=CARTESIAN_POINT('Ctrl Pts',(46.1766977413729,-57.4754524783491,
-44.59995));
#245581=CARTESIAN_POINT('Ctrl Pts',(46.1766977413729,-56.5120019399699,
-44.5416166666667));
#245582=CARTESIAN_POINT('Ctrl Pts',(45.3423250998467,-56.0302766707802,
-44.4832833333334));
#245583=CARTESIAN_POINT('Ctrl Pts',(44.5079524583205,-55.5485514015906,
-44.42495));
#245584=CARTESIAN_POINT('Ctrl Pts',(43.6735798167943,-56.0302766707802,
-44.3666166666667));
#245585=CARTESIAN_POINT('Ctrl Pts',(42.839207175268,-56.5120019399698,-44.3082833333334));
#245586=CARTESIAN_POINT('Ctrl Pts',(42.839207175268,-57.4754524783491,-44.24995));
#245587=CARTESIAN_POINT('Ctrl Pts',(42.839207175268,-58.4389030167283,-44.1916166666667));
#245588=CARTESIAN_POINT('Ctrl Pts',(43.6735798167943,-58.920628285918,-44.1332833333334));
#245589=CARTESIAN_POINT('Ctrl Pts',(44.5079524583205,-59.4023535551075,
-44.07495));
#245590=CARTESIAN_POINT('Ctrl Pts',(45.3423250998467,-58.920628285918,-44.0166166666667));
#245591=CARTESIAN_POINT('Ctrl Pts',(46.1766977413729,-58.4389030167283,
-43.9582833333334));
#245592=CARTESIAN_POINT('Ctrl Pts',(46.1766977413729,-57.4754524783491,
-43.89995));
#245593=CARTESIAN_POINT('Ctrl Pts',(46.1766977413729,-56.5120019399699,
-43.8416166666667));
#245594=CARTESIAN_POINT('Ctrl Pts',(45.3423250998467,-56.0302766707802,
-43.7832833333334));
#245595=CARTESIAN_POINT('Ctrl Pts',(44.5079524583205,-55.5485514015906,
-43.72495));
#245596=CARTESIAN_POINT('Ctrl Pts',(43.6735798167943,-56.0302766707802,
-43.6666166666667));
#245597=CARTESIAN_POINT('Ctrl Pts',(42.839207175268,-56.5120019399698,-43.6082833333333));
#245598=CARTESIAN_POINT('Ctrl Pts',(42.839207175268,-57.4754524783491,-43.54995));
#245599=CARTESIAN_POINT('Ctrl Pts',(42.839207175268,-58.4389030167283,-43.4916166666667));
#245600=CARTESIAN_POINT('Ctrl Pts',(43.6735798167943,-58.920628285918,-43.4332833333333));
#245601=CARTESIAN_POINT('Ctrl Pts',(44.5079524583205,-59.4023535551075,
-43.37495));
#245602=CARTESIAN_POINT('Ctrl Pts',(45.3423250998467,-58.920628285918,-43.3166166666667));
#245603=CARTESIAN_POINT('Ctrl Pts',(46.1766977413729,-58.4389030167283,
-43.2582833333333));
#245604=CARTESIAN_POINT('Ctrl Pts',(46.1766977413729,-57.4754524783491,
-43.19995));
#245605=CARTESIAN_POINT('Ctrl Pts',(46.1766977413729,-56.5120019399699,
-43.1416166666667));
#245606=CARTESIAN_POINT('Ctrl Pts',(45.3423250998467,-56.0302766707802,
-43.0832833333333));
#245607=CARTESIAN_POINT('Ctrl Pts',(44.5079524583205,-55.5485514015906,
-43.02495));
#245608=CARTESIAN_POINT('Ctrl Pts',(43.6735798167943,-56.0302766707802,
-42.9666166666667));
#245609=CARTESIAN_POINT('Ctrl Pts',(42.839207175268,-56.5120019399698,-42.9082833333333));
#245610=CARTESIAN_POINT('Ctrl Pts',(42.839207175268,-57.4754524783491,-42.84995));
#245611=CARTESIAN_POINT('Ctrl Pts',(42.839207175268,-58.4389030167283,-42.7916166666667));
#245612=CARTESIAN_POINT('Ctrl Pts',(43.6735798167943,-58.920628285918,-42.7332833333334));
#245613=CARTESIAN_POINT('Ctrl Pts',(44.5079524583205,-59.4023535551075,
-42.67495));
#245614=CARTESIAN_POINT('Ctrl Pts',(45.3423250998467,-58.920628285918,-42.6166166666667));
#245615=CARTESIAN_POINT('Ctrl Pts',(46.1766977413729,-58.4389030167283,
-42.5582833333333));
#245616=CARTESIAN_POINT('Ctrl Pts',(46.1766977413729,-57.4754524783491,
-42.49995));
#245617=CARTESIAN_POINT('Ctrl Pts',(46.1766977413729,-56.5120019399699,
-42.4416166666667));
#245618=CARTESIAN_POINT('Ctrl Pts',(45.3423250998467,-56.0302766707802,
-42.3832833333333));
#245619=CARTESIAN_POINT('Ctrl Pts',(44.5079524583205,-55.5485514015906,
-42.32495));
#245620=CARTESIAN_POINT('Ctrl Pts',(43.6735798167943,-56.0302766707802,
-42.2666166666667));
#245621=CARTESIAN_POINT('Ctrl Pts',(42.839207175268,-56.5120019399698,-42.2082833333333));
#245622=CARTESIAN_POINT('Ctrl Pts',(42.839207175268,-57.4754524783491,-42.14995));
#245623=CARTESIAN_POINT('Ctrl Pts',(42.839207175268,-58.4389030167283,-42.0916166666667));
#245624=CARTESIAN_POINT('Ctrl Pts',(43.6735798167943,-58.920628285918,-42.0332833333334));
#245625=CARTESIAN_POINT('Ctrl Pts',(44.5079524583205,-59.4023535551075,
-41.97495));
#245626=CARTESIAN_POINT('Ctrl Pts',(45.3423250998467,-58.920628285918,-41.9166166666667));
#245627=CARTESIAN_POINT('Ctrl Pts',(46.1766977413729,-58.4389030167283,
-41.8582833333333));
#245628=CARTESIAN_POINT('Ctrl Pts',(46.1766977413729,-57.4754524783491,
-41.79995));
#245629=CARTESIAN_POINT('Ctrl Pts',(46.1766977413729,-56.5120019399699,
-41.7416166666667));
#245630=CARTESIAN_POINT('Ctrl Pts',(45.3423250998467,-56.0302766707802,
-41.6832833333333));
#245631=CARTESIAN_POINT('Ctrl Pts',(44.5079524583205,-55.5485514015906,
-41.62495));
#245632=CARTESIAN_POINT('Ctrl Pts',(43.6735798167943,-56.0302766707802,
-41.5666166666667));
#245633=CARTESIAN_POINT('Ctrl Pts',(42.839207175268,-56.5120019399698,-41.5082833333334));
#245634=CARTESIAN_POINT('Ctrl Pts',(42.839207175268,-57.4754524783491,-41.44995));
#245635=CARTESIAN_POINT('Ctrl Pts',(42.839207175268,-58.4389030167283,-41.3916166666667));
#245636=CARTESIAN_POINT('Ctrl Pts',(43.6735798167943,-58.920628285918,-41.3332833333334));
#245637=CARTESIAN_POINT('Ctrl Pts',(44.5079524583205,-59.4023535551075,
-41.27495));
#245638=CARTESIAN_POINT('Ctrl Pts',(45.3423250998467,-58.920628285918,-41.2166166666667));
#245639=CARTESIAN_POINT('Ctrl Pts',(46.1766977413729,-58.4389030167283,
-41.1582833333333));
#245640=CARTESIAN_POINT('Ctrl Pts',(46.1766977413729,-57.4754524783491,
-41.09995));
#245641=CARTESIAN_POINT('Ctrl Pts',(46.1766977413729,-56.5120019399699,
-41.0416166666667));
#245642=CARTESIAN_POINT('Ctrl Pts',(45.3423250998467,-56.0302766707802,
-40.9832833333333));
#245643=CARTESIAN_POINT('Ctrl Pts',(44.5079524583205,-55.5485514015906,
-40.92495));
#245644=CARTESIAN_POINT('Ctrl Pts',(43.6735798167943,-56.0302766707802,
-40.8666166666667));
#245645=CARTESIAN_POINT('Ctrl Pts',(42.839207175268,-56.5120019399698,-40.8082833333334));
#245646=CARTESIAN_POINT('Ctrl Pts',(42.839207175268,-57.4754524783491,-40.74995));
#245647=CARTESIAN_POINT('Ctrl Pts',(42.839207175268,-58.4389030167283,-40.6916166666667));
#245648=CARTESIAN_POINT('Ctrl Pts',(43.6735798167943,-58.920628285918,-40.6332833333334));
#245649=CARTESIAN_POINT('Ctrl Pts',(44.5079524583205,-59.4023535551075,
-40.57495));
#245650=CARTESIAN_POINT('Ctrl Pts',(45.3423250998467,-58.920628285918,-40.5166166666667));
#245651=CARTESIAN_POINT('Ctrl Pts',(46.1766977413729,-58.4389030167283,
-40.4582833333333));
#245652=CARTESIAN_POINT('Ctrl Pts',(46.1766977413729,-57.4754524783491,
-40.39995));
#245653=CARTESIAN_POINT('Ctrl Pts',(46.1766977413729,-56.5120019399699,
-40.3416166666667));
#245654=CARTESIAN_POINT('Ctrl Pts',(45.3423250998467,-56.0302766707802,
-40.2832833333334));
#245655=CARTESIAN_POINT('Ctrl Pts',(44.5079524583205,-55.5485514015906,
-40.22495));
#245656=CARTESIAN_POINT('Ctrl Pts',(43.6735798167943,-56.0302766707802,
-40.1666166666667));
#245657=CARTESIAN_POINT('Ctrl Pts',(42.839207175268,-56.5120019399698,-40.1082833333334));
#245658=CARTESIAN_POINT('Ctrl Pts',(42.839207175268,-57.4754524783491,-40.04995));
#245659=CARTESIAN_POINT('Ctrl Pts',(42.839207175268,-58.4389030167283,-39.9916166666667));
#245660=CARTESIAN_POINT('Ctrl Pts',(43.6735798167943,-58.920628285918,-39.9332833333333));
#245661=CARTESIAN_POINT('Ctrl Pts',(44.5079524583205,-59.4023535551075,
-39.87495));
#245662=CARTESIAN_POINT('Ctrl Pts',(45.3423250998467,-58.920628285918,-39.8166166666667));
#245663=CARTESIAN_POINT('Ctrl Pts',(46.1766977413729,-58.4389030167283,
-39.7582833333334));
#245664=CARTESIAN_POINT('Ctrl Pts',(46.1766977413729,-57.4754524783491,
-39.69995));
#245665=CARTESIAN_POINT('Ctrl Pts',(46.1766977413729,-56.5120019399699,
-39.6416166666667));
#245666=CARTESIAN_POINT('Ctrl Pts',(45.3423250998467,-56.0302766707802,
-39.5832833333333));
#245667=CARTESIAN_POINT('Ctrl Pts',(44.5079524583205,-55.5485514015906,
-39.52495));
#245668=CARTESIAN_POINT('Ctrl Pts',(43.6735798167943,-56.0302766707802,
-39.4666166666667));
#245669=CARTESIAN_POINT('Ctrl Pts',(42.839207175268,-56.5120019399698,-39.4082833333334));
#245670=CARTESIAN_POINT('Ctrl Pts',(42.839207175268,-57.4754524783491,-39.34995));
#245671=CARTESIAN_POINT('Ctrl Pts',(42.839207175268,-58.4389030167283,-39.2916166666667));
#245672=CARTESIAN_POINT('Ctrl Pts',(43.6735798167943,-58.920628285918,-39.2332833333333));
#245673=CARTESIAN_POINT('Ctrl Pts',(44.5079524583205,-59.4023535551075,
-39.17495));
#245674=CARTESIAN_POINT('Ctrl Pts',(45.3423250998467,-58.920628285918,-39.1166166666667));
#245675=CARTESIAN_POINT('Ctrl Pts',(46.1766977413729,-58.4389030167283,
-39.0582833333334));
#245676=CARTESIAN_POINT('Ctrl Pts',(46.1766977413729,-57.4754524783491,
-38.99995));
#245677=CARTESIAN_POINT('Ctrl Pts',(46.1766977413729,-56.5120019399699,
-38.9416166666667));
#245678=CARTESIAN_POINT('Ctrl Pts',(45.3423250998467,-56.0302766707802,
-38.8832833333334));
#245679=CARTESIAN_POINT('Ctrl Pts',(44.5079524583205,-55.5485514015906,
-38.82495));
#245680=CARTESIAN_POINT('Ctrl Pts',(43.6735798167943,-56.0302766707802,
-38.7666166666667));
#245681=CARTESIAN_POINT('Ctrl Pts',(42.839207175268,-56.5120019399698,-38.7082833333334));
#245682=CARTESIAN_POINT('Ctrl Pts',(42.839207175268,-57.4754524783491,-38.64995));
#245683=CARTESIAN_POINT('Ctrl Pts',(42.839207175268,-58.4389030167283,-38.5916166666667));
#245684=CARTESIAN_POINT('Ctrl Pts',(43.6735798167943,-58.920628285918,-38.5332833333334));
#245685=CARTESIAN_POINT('Ctrl Pts',(44.5079524583205,-59.4023535551075,
-38.47495));
#245686=CARTESIAN_POINT('Ctrl Pts',(45.3423250998467,-58.920628285918,-38.4166166666667));
#245687=CARTESIAN_POINT('Ctrl Pts',(46.1766977413729,-58.4389030167283,
-38.3582833333333));
#245688=CARTESIAN_POINT('Ctrl Pts',(46.1766977413729,-57.4754524783491,
-38.29995));
#245689=CARTESIAN_POINT('Ctrl Pts',(46.1766977413729,-56.5120019399699,
-38.2416166666667));
#245690=CARTESIAN_POINT('Ctrl Pts',(45.3423250998467,-56.0302766707802,
-38.1832833333333));
#245691=CARTESIAN_POINT('Ctrl Pts',(44.5079524583205,-55.5485514015906,
-38.12495));
#245692=CARTESIAN_POINT('Ctrl Pts',(43.6735798167943,-56.0302766707802,
-38.0666166666667));
#245693=CARTESIAN_POINT('Ctrl Pts',(42.839207175268,-56.5120019399698,-38.0082833333333));
#245694=CARTESIAN_POINT('Ctrl Pts',(42.839207175268,-57.4754524783491,-37.94995));
#245695=CARTESIAN_POINT('Ctrl Pts',(42.839207175268,-58.4389030167283,-37.8916166666667));
#245696=CARTESIAN_POINT('Ctrl Pts',(43.6735798167943,-58.920628285918,-37.8332833333334));
#245697=CARTESIAN_POINT('Ctrl Pts',(44.5079524583205,-59.4023535551075,
-37.77495));
#245698=CARTESIAN_POINT('Ctrl Pts',(45.3423250998467,-58.920628285918,-37.7166166666667));
#245699=CARTESIAN_POINT('Ctrl Pts',(46.1766977413729,-58.4389030167283,
-37.6582833333333));
#245700=CARTESIAN_POINT('Ctrl Pts',(46.1766977413729,-57.4754524783491,
-37.59995));
#245701=CARTESIAN_POINT('Ctrl Pts',(46.1766977413729,-56.5120019399699,
-37.5416166666667));
#245702=CARTESIAN_POINT('Ctrl Pts',(45.3423250998467,-56.0302766707802,
-37.4832833333334));
#245703=CARTESIAN_POINT('Ctrl Pts',(44.5079524583205,-55.5485514015906,
-37.42495));
#245704=CARTESIAN_POINT('Ctrl Pts',(43.6735798167943,-56.0302766707802,
-37.3666166666667));
#245705=CARTESIAN_POINT('Ctrl Pts',(42.839207175268,-56.5120019399698,-37.3082833333333));
#245706=CARTESIAN_POINT('Ctrl Pts',(42.839207175268,-57.4754524783491,-37.24995));
#245707=CARTESIAN_POINT('Ctrl Pts',(42.839207175268,-58.4389030167283,-37.1916166666667));
#245708=CARTESIAN_POINT('Ctrl Pts',(43.6735798167943,-58.920628285918,-37.1332833333334));
#245709=CARTESIAN_POINT('Ctrl Pts',(44.5079524583205,-59.4023535551075,
-37.07495));
#245710=CARTESIAN_POINT('Ctrl Pts',(45.3423250998467,-58.920628285918,-37.0166166666667));
#245711=CARTESIAN_POINT('Ctrl Pts',(45.4506530446707,-58.8580851178131,
-37.0090431559831));
#245712=CARTESIAN_POINT('Ctrl Pts',(45.5484465834733,-58.7800914304091,
-37.0009024189827));
#245713=CARTESIAN_POINT('Ctrl Pts',(46.5766932247459,-57.4754524783491,
-53.2308875));
#245714=CARTESIAN_POINT('Ctrl Pts',(46.5766932247459,-56.2810644399698,
-53.1725541666667));
#245715=CARTESIAN_POINT('Ctrl Pts',(45.5423228415332,-55.6838704207802,
-53.1142208333334));
#245716=CARTESIAN_POINT('Ctrl Pts',(44.5079524583205,-55.0866764015906,
-53.0558875000001));
#245717=CARTESIAN_POINT('Ctrl Pts',(43.4735820751078,-55.6838704207802,
-52.9975541666667));
#245718=CARTESIAN_POINT('Ctrl Pts',(42.4392116918951,-56.2810644399698,
-52.9392208333334));
#245719=CARTESIAN_POINT('Ctrl Pts',(42.439211691895,-57.4754524783491,-52.8808875));
#245720=CARTESIAN_POINT('Ctrl Pts',(42.4392116918951,-58.6698405167284,
-52.8225541666667));
#245721=CARTESIAN_POINT('Ctrl Pts',(43.4735820751078,-59.267034535918,-52.7642208333334));
#245722=CARTESIAN_POINT('Ctrl Pts',(44.5079524583205,-59.8642285551076,
-52.7058875));
#245723=CARTESIAN_POINT('Ctrl Pts',(45.5423228415332,-59.267034535918,-52.6475541666667));
#245724=CARTESIAN_POINT('Ctrl Pts',(46.5766932247459,-58.6698405167284,
-52.5892208333333));
#245725=CARTESIAN_POINT('Ctrl Pts',(46.5766932247459,-57.4754524783491,
-52.5308875));
#245726=CARTESIAN_POINT('Ctrl Pts',(46.5766932247459,-56.2810644399698,
-52.4725541666667));
#245727=CARTESIAN_POINT('Ctrl Pts',(45.5423228415332,-55.6838704207802,
-52.4142208333334));
#245728=CARTESIAN_POINT('Ctrl Pts',(44.5079524583205,-55.0866764015906,
-52.3558875000001));
#245729=CARTESIAN_POINT('Ctrl Pts',(43.4735820751078,-55.6838704207802,
-52.2975541666667));
#245730=CARTESIAN_POINT('Ctrl Pts',(42.4392116918951,-56.2810644399698,
-52.2392208333334));
#245731=CARTESIAN_POINT('Ctrl Pts',(42.439211691895,-57.4754524783491,-52.1808875));
#245732=CARTESIAN_POINT('Ctrl Pts',(42.4392116918951,-58.6698405167284,
-52.1225541666667));
#245733=CARTESIAN_POINT('Ctrl Pts',(43.4735820751078,-59.267034535918,-52.0642208333334));
#245734=CARTESIAN_POINT('Ctrl Pts',(44.5079524583205,-59.8642285551076,
-52.0058875));
#245735=CARTESIAN_POINT('Ctrl Pts',(45.5423228415332,-59.267034535918,-51.9475541666667));
#245736=CARTESIAN_POINT('Ctrl Pts',(46.5766932247459,-58.6698405167284,
-51.8892208333334));
#245737=CARTESIAN_POINT('Ctrl Pts',(46.5766932247459,-57.4754524783491,
-51.8308875));
#245738=CARTESIAN_POINT('Ctrl Pts',(46.5766932247459,-56.2810644399698,
-51.7725541666667));
#245739=CARTESIAN_POINT('Ctrl Pts',(45.5423228415332,-55.6838704207802,
-51.7142208333334));
#245740=CARTESIAN_POINT('Ctrl Pts',(44.5079524583205,-55.0866764015906,
-51.6558875));
#245741=CARTESIAN_POINT('Ctrl Pts',(43.4735820751078,-55.6838704207802,
-51.5975541666667));
#245742=CARTESIAN_POINT('Ctrl Pts',(42.4392116918951,-56.2810644399698,
-51.5392208333333));
#245743=CARTESIAN_POINT('Ctrl Pts',(42.439211691895,-57.4754524783491,-51.4808875));
#245744=CARTESIAN_POINT('Ctrl Pts',(42.4392116918951,-58.6698405167284,
-51.4225541666667));
#245745=CARTESIAN_POINT('Ctrl Pts',(43.4735820751078,-59.267034535918,-51.3642208333334));
#245746=CARTESIAN_POINT('Ctrl Pts',(44.5079524583205,-59.8642285551076,
-51.3058875));
#245747=CARTESIAN_POINT('Ctrl Pts',(45.5423228415332,-59.267034535918,-51.2475541666667));
#245748=CARTESIAN_POINT('Ctrl Pts',(46.5766932247459,-58.6698405167284,
-51.1892208333334));
#245749=CARTESIAN_POINT('Ctrl Pts',(46.5766932247459,-57.4754524783491,
-51.1308875));
#245750=CARTESIAN_POINT('Ctrl Pts',(46.5766932247459,-56.2810644399698,
-51.0725541666667));
#245751=CARTESIAN_POINT('Ctrl Pts',(45.5423228415332,-55.6838704207802,
-51.0142208333334));
#245752=CARTESIAN_POINT('Ctrl Pts',(44.5079524583205,-55.0866764015906,
-50.9558875));
#245753=CARTESIAN_POINT('Ctrl Pts',(43.4735820751078,-55.6838704207802,
-50.8975541666667));
#245754=CARTESIAN_POINT('Ctrl Pts',(42.4392116918951,-56.2810644399698,
-50.8392208333333));
#245755=CARTESIAN_POINT('Ctrl Pts',(42.439211691895,-57.4754524783491,-50.7808875));
#245756=CARTESIAN_POINT('Ctrl Pts',(42.4392116918951,-58.6698405167284,
-50.7225541666667));
#245757=CARTESIAN_POINT('Ctrl Pts',(43.4735820751078,-59.267034535918,-50.6642208333333));
#245758=CARTESIAN_POINT('Ctrl Pts',(44.5079524583205,-59.8642285551076,
-50.6058875));
#245759=CARTESIAN_POINT('Ctrl Pts',(45.5423228415332,-59.267034535918,-50.5475541666667));
#245760=CARTESIAN_POINT('Ctrl Pts',(46.5766932247459,-58.6698405167284,
-50.4892208333333));
#245761=CARTESIAN_POINT('Ctrl Pts',(46.5766932247459,-57.4754524783491,
-50.4308875));
#245762=CARTESIAN_POINT('Ctrl Pts',(46.5766932247459,-56.2810644399698,
-50.3725541666667));
#245763=CARTESIAN_POINT('Ctrl Pts',(45.5423228415332,-55.6838704207802,
-50.3142208333334));
#245764=CARTESIAN_POINT('Ctrl Pts',(44.5079524583205,-55.0866764015906,
-50.2558875));
#245765=CARTESIAN_POINT('Ctrl Pts',(43.4735820751078,-55.6838704207802,
-50.1975541666667));
#245766=CARTESIAN_POINT('Ctrl Pts',(42.4392116918951,-56.2810644399698,
-50.1392208333333));
#245767=CARTESIAN_POINT('Ctrl Pts',(42.439211691895,-57.4754524783491,-50.0808875));
#245768=CARTESIAN_POINT('Ctrl Pts',(42.4392116918951,-58.6698405167284,
-50.0225541666667));
#245769=CARTESIAN_POINT('Ctrl Pts',(43.4735820751078,-59.267034535918,-49.9642208333334));
#245770=CARTESIAN_POINT('Ctrl Pts',(44.5079524583205,-59.8642285551076,
-49.9058875));
#245771=CARTESIAN_POINT('Ctrl Pts',(45.5423228415332,-59.267034535918,-49.8475541666667));
#245772=CARTESIAN_POINT('Ctrl Pts',(46.5766932247459,-58.6698405167284,
-49.7892208333333));
#245773=CARTESIAN_POINT('Ctrl Pts',(46.5766932247459,-57.4754524783491,
-49.7308875));
#245774=CARTESIAN_POINT('Ctrl Pts',(46.5766932247459,-56.2810644399698,
-49.6725541666667));
#245775=CARTESIAN_POINT('Ctrl Pts',(45.5423228415332,-55.6838704207802,
-49.6142208333334));
#245776=CARTESIAN_POINT('Ctrl Pts',(44.5079524583205,-55.0866764015906,
-49.5558875));
#245777=CARTESIAN_POINT('Ctrl Pts',(43.4735820751078,-55.6838704207802,
-49.4975541666667));
#245778=CARTESIAN_POINT('Ctrl Pts',(42.4392116918951,-56.2810644399698,
-49.4392208333333));
#245779=CARTESIAN_POINT('Ctrl Pts',(42.439211691895,-57.4754524783491,-49.3808875));
#245780=CARTESIAN_POINT('Ctrl Pts',(42.4392116918951,-58.6698405167284,
-49.3225541666667));
#245781=CARTESIAN_POINT('Ctrl Pts',(43.4735820751078,-59.267034535918,-49.2642208333334));
#245782=CARTESIAN_POINT('Ctrl Pts',(44.5079524583205,-59.8642285551076,
-49.2058875));
#245783=CARTESIAN_POINT('Ctrl Pts',(45.5423228415332,-59.267034535918,-49.1475541666667));
#245784=CARTESIAN_POINT('Ctrl Pts',(46.5766932247459,-58.6698405167284,
-49.0892208333333));
#245785=CARTESIAN_POINT('Ctrl Pts',(46.5766932247459,-57.4754524783491,
-49.0308875));
#245786=CARTESIAN_POINT('Ctrl Pts',(46.5766932247459,-56.2810644399698,
-48.9725541666667));
#245787=CARTESIAN_POINT('Ctrl Pts',(45.5423228415332,-55.6838704207802,
-48.9142208333334));
#245788=CARTESIAN_POINT('Ctrl Pts',(44.5079524583205,-55.0866764015906,
-48.8558875));
#245789=CARTESIAN_POINT('Ctrl Pts',(43.4735820751078,-55.6838704207802,
-48.7975541666667));
#245790=CARTESIAN_POINT('Ctrl Pts',(42.4392116918951,-56.2810644399698,
-48.7392208333334));
#245791=CARTESIAN_POINT('Ctrl Pts',(42.439211691895,-57.4754524783491,-48.6808875));
#245792=CARTESIAN_POINT('Ctrl Pts',(42.4392116918951,-58.6698405167284,
-48.6225541666667));
#245793=CARTESIAN_POINT('Ctrl Pts',(43.4735820751078,-59.267034535918,-48.5642208333334));
#245794=CARTESIAN_POINT('Ctrl Pts',(44.5079524583205,-59.8642285551076,
-48.5058875));
#245795=CARTESIAN_POINT('Ctrl Pts',(45.5423228415332,-59.267034535918,-48.4475541666667));
#245796=CARTESIAN_POINT('Ctrl Pts',(46.5766932247459,-58.6698405167284,
-48.3892208333334));
#245797=CARTESIAN_POINT('Ctrl Pts',(46.5766932247459,-57.4754524783491,
-48.3308875));
#245798=CARTESIAN_POINT('Ctrl Pts',(46.5766932247459,-56.2810644399698,
-48.2725541666667));
#245799=CARTESIAN_POINT('Ctrl Pts',(45.5423228415332,-55.6838704207802,
-48.2142208333334));
#245800=CARTESIAN_POINT('Ctrl Pts',(44.5079524583205,-55.0866764015906,
-48.1558875));
#245801=CARTESIAN_POINT('Ctrl Pts',(43.4735820751078,-55.6838704207802,
-48.0975541666667));
#245802=CARTESIAN_POINT('Ctrl Pts',(42.4392116918951,-56.2810644399698,
-48.0392208333334));
#245803=CARTESIAN_POINT('Ctrl Pts',(42.439211691895,-57.4754524783491,-47.9808875));
#245804=CARTESIAN_POINT('Ctrl Pts',(42.4392116918951,-58.6698405167284,
-47.9225541666667));
#245805=CARTESIAN_POINT('Ctrl Pts',(43.4735820751078,-59.267034535918,-47.8642208333334));
#245806=CARTESIAN_POINT('Ctrl Pts',(44.5079524583205,-59.8642285551076,
-47.8058875000001));
#245807=CARTESIAN_POINT('Ctrl Pts',(45.5423228415332,-59.267034535918,-47.7475541666667));
#245808=CARTESIAN_POINT('Ctrl Pts',(46.5766932247459,-58.6698405167284,
-47.6892208333334));
#245809=CARTESIAN_POINT('Ctrl Pts',(46.5766932247459,-57.4754524783491,
-47.6308875));
#245810=CARTESIAN_POINT('Ctrl Pts',(46.5766932247459,-56.2810644399698,
-47.5725541666667));
#245811=CARTESIAN_POINT('Ctrl Pts',(45.5423228415332,-55.6838704207802,
-47.5142208333333));
#245812=CARTESIAN_POINT('Ctrl Pts',(44.5079524583205,-55.0866764015906,
-47.4558875));
#245813=CARTESIAN_POINT('Ctrl Pts',(43.4735820751078,-55.6838704207802,
-47.3975541666667));
#245814=CARTESIAN_POINT('Ctrl Pts',(42.4392116918951,-56.2810644399698,
-47.3392208333334));
#245815=CARTESIAN_POINT('Ctrl Pts',(42.439211691895,-57.4754524783491,-47.2808875));
#245816=CARTESIAN_POINT('Ctrl Pts',(42.4392116918951,-58.6698405167284,
-47.2225541666667));
#245817=CARTESIAN_POINT('Ctrl Pts',(43.4735820751078,-59.267034535918,-47.1642208333334));
#245818=CARTESIAN_POINT('Ctrl Pts',(44.5079524583205,-59.8642285551076,
-47.1058875));
#245819=CARTESIAN_POINT('Ctrl Pts',(45.5423228415332,-59.267034535918,-47.0475541666667));
#245820=CARTESIAN_POINT('Ctrl Pts',(46.5766932247459,-58.6698405167284,
-46.9892208333334));
#245821=CARTESIAN_POINT('Ctrl Pts',(46.5766932247459,-57.4754524783491,
-46.9308875));
#245822=CARTESIAN_POINT('Ctrl Pts',(46.5766932247459,-56.2810644399698,
-46.8725541666667));
#245823=CARTESIAN_POINT('Ctrl Pts',(45.5423228415332,-55.6838704207802,
-46.8142208333334));
#245824=CARTESIAN_POINT('Ctrl Pts',(44.5079524583205,-55.0866764015906,
-46.7558875));
#245825=CARTESIAN_POINT('Ctrl Pts',(43.4735820751078,-55.6838704207802,
-46.6975541666667));
#245826=CARTESIAN_POINT('Ctrl Pts',(42.4392116918951,-56.2810644399698,
-46.6392208333334));
#245827=CARTESIAN_POINT('Ctrl Pts',(42.439211691895,-57.4754524783491,-46.5808875));
#245828=CARTESIAN_POINT('Ctrl Pts',(42.4392116918951,-58.6698405167284,
-46.5225541666667));
#245829=CARTESIAN_POINT('Ctrl Pts',(43.4735820751078,-59.267034535918,-46.4642208333334));
#245830=CARTESIAN_POINT('Ctrl Pts',(44.5079524583205,-59.8642285551076,
-46.4058875));
#245831=CARTESIAN_POINT('Ctrl Pts',(45.5423228415332,-59.267034535918,-46.3475541666667));
#245832=CARTESIAN_POINT('Ctrl Pts',(46.5766932247459,-58.6698405167284,
-46.2892208333334));
#245833=CARTESIAN_POINT('Ctrl Pts',(46.5766932247459,-57.4754524783491,
-46.2308875));
#245834=CARTESIAN_POINT('Ctrl Pts',(46.5766932247459,-56.2810644399698,
-46.1725541666667));
#245835=CARTESIAN_POINT('Ctrl Pts',(45.5423228415332,-55.6838704207802,
-46.1142208333334));
#245836=CARTESIAN_POINT('Ctrl Pts',(44.5079524583205,-55.0866764015906,
-46.0558875));
#245837=CARTESIAN_POINT('Ctrl Pts',(43.4735820751078,-55.6838704207802,
-45.9975541666667));
#245838=CARTESIAN_POINT('Ctrl Pts',(42.4392116918951,-56.2810644399698,
-45.9392208333333));
#245839=CARTESIAN_POINT('Ctrl Pts',(42.439211691895,-57.4754524783491,-45.8808875));
#245840=CARTESIAN_POINT('Ctrl Pts',(42.4392116918951,-58.6698405167284,
-45.8225541666667));
#245841=CARTESIAN_POINT('Ctrl Pts',(43.4735820751078,-59.267034535918,-45.7642208333334));
#245842=CARTESIAN_POINT('Ctrl Pts',(44.5079524583205,-59.8642285551076,
-45.7058875));
#245843=CARTESIAN_POINT('Ctrl Pts',(45.5423228415332,-59.267034535918,-45.6475541666667));
#245844=CARTESIAN_POINT('Ctrl Pts',(46.5766932247459,-58.6698405167284,
-45.5892208333334));
#245845=CARTESIAN_POINT('Ctrl Pts',(46.5766932247459,-57.4754524783491,
-45.5308875));
#245846=CARTESIAN_POINT('Ctrl Pts',(46.5766932247459,-56.2810644399698,
-45.4725541666667));
#245847=CARTESIAN_POINT('Ctrl Pts',(45.5423228415332,-55.6838704207802,
-45.4142208333334));
#245848=CARTESIAN_POINT('Ctrl Pts',(44.5079524583205,-55.0866764015906,
-45.3558875));
#245849=CARTESIAN_POINT('Ctrl Pts',(43.4735820751078,-55.6838704207802,
-45.2975541666667));
#245850=CARTESIAN_POINT('Ctrl Pts',(42.4392116918951,-56.2810644399698,
-45.2392208333333));
#245851=CARTESIAN_POINT('Ctrl Pts',(42.439211691895,-57.4754524783491,-45.1808875));
#245852=CARTESIAN_POINT('Ctrl Pts',(42.4392116918951,-58.6698405167284,
-45.1225541666667));
#245853=CARTESIAN_POINT('Ctrl Pts',(43.4735820751078,-59.267034535918,-45.0642208333334));
#245854=CARTESIAN_POINT('Ctrl Pts',(44.5079524583205,-59.8642285551076,
-45.0058875));
#245855=CARTESIAN_POINT('Ctrl Pts',(45.5423228415332,-59.267034535918,-44.9475541666667));
#245856=CARTESIAN_POINT('Ctrl Pts',(46.5766932247459,-58.6698405167284,
-44.8892208333333));
#245857=CARTESIAN_POINT('Ctrl Pts',(46.5766932247459,-57.4754524783491,
-44.8308875));
#245858=CARTESIAN_POINT('Ctrl Pts',(46.5766932247459,-56.2810644399698,
-44.7725541666667));
#245859=CARTESIAN_POINT('Ctrl Pts',(45.5423228415332,-55.6838704207802,
-44.7142208333334));
#245860=CARTESIAN_POINT('Ctrl Pts',(44.5079524583205,-55.0866764015906,
-44.6558875));
#245861=CARTESIAN_POINT('Ctrl Pts',(43.4735820751078,-55.6838704207802,
-44.5975541666667));
#245862=CARTESIAN_POINT('Ctrl Pts',(42.4392116918951,-56.2810644399698,
-44.5392208333333));
#245863=CARTESIAN_POINT('Ctrl Pts',(42.439211691895,-57.4754524783491,-44.4808875000001));
#245864=CARTESIAN_POINT('Ctrl Pts',(42.4392116918951,-58.6698405167284,
-44.4225541666667));
#245865=CARTESIAN_POINT('Ctrl Pts',(43.4735820751078,-59.267034535918,-44.3642208333333));
#245866=CARTESIAN_POINT('Ctrl Pts',(44.5079524583205,-59.8642285551076,
-44.3058875));
#245867=CARTESIAN_POINT('Ctrl Pts',(45.5423228415332,-59.267034535918,-44.2475541666667));
#245868=CARTESIAN_POINT('Ctrl Pts',(46.5766932247459,-58.6698405167284,
-44.1892208333334));
#245869=CARTESIAN_POINT('Ctrl Pts',(46.5766932247459,-57.4754524783491,
-44.1308875000001));
#245870=CARTESIAN_POINT('Ctrl Pts',(46.5766932247459,-56.2810644399698,
-44.0725541666667));
#245871=CARTESIAN_POINT('Ctrl Pts',(45.5423228415332,-55.6838704207802,
-44.0142208333334));
#245872=CARTESIAN_POINT('Ctrl Pts',(44.5079524583205,-55.0866764015906,
-43.9558875));
#245873=CARTESIAN_POINT('Ctrl Pts',(43.4735820751078,-55.6838704207802,
-43.8975541666667));
#245874=CARTESIAN_POINT('Ctrl Pts',(42.4392116918951,-56.2810644399698,
-43.8392208333333));
#245875=CARTESIAN_POINT('Ctrl Pts',(42.439211691895,-57.4754524783491,-43.7808875));
#245876=CARTESIAN_POINT('Ctrl Pts',(42.4392116918951,-58.6698405167284,
-43.7225541666667));
#245877=CARTESIAN_POINT('Ctrl Pts',(43.4735820751078,-59.267034535918,-43.6642208333334));
#245878=CARTESIAN_POINT('Ctrl Pts',(44.5079524583205,-59.8642285551076,
-43.6058875));
#245879=CARTESIAN_POINT('Ctrl Pts',(45.5423228415332,-59.267034535918,-43.5475541666667));
#245880=CARTESIAN_POINT('Ctrl Pts',(46.5766932247459,-58.6698405167284,
-43.4892208333333));
#245881=CARTESIAN_POINT('Ctrl Pts',(46.5766932247459,-57.4754524783491,
-43.4308875));
#245882=CARTESIAN_POINT('Ctrl Pts',(46.5766932247459,-56.2810644399698,
-43.3725541666667));
#245883=CARTESIAN_POINT('Ctrl Pts',(45.5423228415332,-55.6838704207802,
-43.3142208333334));
#245884=CARTESIAN_POINT('Ctrl Pts',(44.5079524583205,-55.0866764015906,
-43.2558875));
#245885=CARTESIAN_POINT('Ctrl Pts',(43.4735820751078,-55.6838704207802,
-43.1975541666667));
#245886=CARTESIAN_POINT('Ctrl Pts',(42.4392116918951,-56.2810644399698,
-43.1392208333334));
#245887=CARTESIAN_POINT('Ctrl Pts',(42.439211691895,-57.4754524783491,-43.0808875));
#245888=CARTESIAN_POINT('Ctrl Pts',(42.4392116918951,-58.6698405167284,
-43.0225541666667));
#245889=CARTESIAN_POINT('Ctrl Pts',(43.4735820751078,-59.267034535918,-42.9642208333334));
#245890=CARTESIAN_POINT('Ctrl Pts',(44.5079524583205,-59.8642285551076,
-42.9058875));
#245891=CARTESIAN_POINT('Ctrl Pts',(45.5423228415332,-59.267034535918,-42.8475541666667));
#245892=CARTESIAN_POINT('Ctrl Pts',(46.5766932247459,-58.6698405167284,
-42.7892208333334));
#245893=CARTESIAN_POINT('Ctrl Pts',(46.5766932247459,-57.4754524783491,
-42.7308875000001));
#245894=CARTESIAN_POINT('Ctrl Pts',(46.5766932247459,-56.2810644399698,
-42.6725541666667));
#245895=CARTESIAN_POINT('Ctrl Pts',(45.5423228415332,-55.6838704207802,
-42.6142208333334));
#245896=CARTESIAN_POINT('Ctrl Pts',(44.5079524583205,-55.0866764015906,
-42.5558875));
#245897=CARTESIAN_POINT('Ctrl Pts',(43.4735820751078,-55.6838704207802,
-42.4975541666667));
#245898=CARTESIAN_POINT('Ctrl Pts',(42.4392116918951,-56.2810644399698,
-42.4392208333334));
#245899=CARTESIAN_POINT('Ctrl Pts',(42.439211691895,-57.4754524783491,-42.3808875000001));
#245900=CARTESIAN_POINT('Ctrl Pts',(42.4392116918951,-58.6698405167284,
-42.3225541666667));
#245901=CARTESIAN_POINT('Ctrl Pts',(43.4735820751078,-59.267034535918,-42.2642208333334));
#245902=CARTESIAN_POINT('Ctrl Pts',(44.5079524583205,-59.8642285551076,
-42.2058875));
#245903=CARTESIAN_POINT('Ctrl Pts',(45.5423228415332,-59.267034535918,-42.1475541666667));
#245904=CARTESIAN_POINT('Ctrl Pts',(46.5766932247459,-58.6698405167284,
-42.0892208333334));
#245905=CARTESIAN_POINT('Ctrl Pts',(46.5766932247459,-57.4754524783491,
-42.0308875000001));
#245906=CARTESIAN_POINT('Ctrl Pts',(46.5766932247459,-56.2810644399698,
-41.9725541666667));
#245907=CARTESIAN_POINT('Ctrl Pts',(45.5423228415332,-55.6838704207802,
-41.9142208333334));
#245908=CARTESIAN_POINT('Ctrl Pts',(44.5079524583205,-55.0866764015906,
-41.8558875));
#245909=CARTESIAN_POINT('Ctrl Pts',(43.4735820751078,-55.6838704207802,
-41.7975541666667));
#245910=CARTESIAN_POINT('Ctrl Pts',(42.4392116918951,-56.2810644399698,
-41.7392208333334));
#245911=CARTESIAN_POINT('Ctrl Pts',(42.439211691895,-57.4754524783491,-41.6808875000001));
#245912=CARTESIAN_POINT('Ctrl Pts',(42.4392116918951,-58.6698405167284,
-41.6225541666667));
#245913=CARTESIAN_POINT('Ctrl Pts',(43.4735820751078,-59.267034535918,-41.5642208333334));
#245914=CARTESIAN_POINT('Ctrl Pts',(44.5079524583205,-59.8642285551076,
-41.5058875));
#245915=CARTESIAN_POINT('Ctrl Pts',(45.5423228415332,-59.267034535918,-41.4475541666667));
#245916=CARTESIAN_POINT('Ctrl Pts',(46.5766932247459,-58.6698405167284,
-41.3892208333334));
#245917=CARTESIAN_POINT('Ctrl Pts',(46.5766932247459,-57.4754524783491,
-41.3308875000001));
#245918=CARTESIAN_POINT('Ctrl Pts',(46.5766932247459,-56.2810644399698,
-41.2725541666667));
#245919=CARTESIAN_POINT('Ctrl Pts',(45.5423228415332,-55.6838704207802,
-41.2142208333333));
#245920=CARTESIAN_POINT('Ctrl Pts',(44.5079524583205,-55.0866764015906,
-41.1558875));
#245921=CARTESIAN_POINT('Ctrl Pts',(43.4735820751078,-55.6838704207802,
-41.0975541666667));
#245922=CARTESIAN_POINT('Ctrl Pts',(42.4392116918951,-56.2810644399698,
-41.0392208333333));
#245923=CARTESIAN_POINT('Ctrl Pts',(42.439211691895,-57.4754524783491,-40.9808875000001));
#245924=CARTESIAN_POINT('Ctrl Pts',(42.4392116918951,-58.6698405167284,
-40.9225541666667));
#245925=CARTESIAN_POINT('Ctrl Pts',(43.4735820751078,-59.267034535918,-40.8642208333334));
#245926=CARTESIAN_POINT('Ctrl Pts',(44.5079524583205,-59.8642285551076,
-40.8058875));
#245927=CARTESIAN_POINT('Ctrl Pts',(45.5423228415332,-59.267034535918,-40.7475541666667));
#245928=CARTESIAN_POINT('Ctrl Pts',(46.5766932247459,-58.6698405167284,
-40.6892208333333));
#245929=CARTESIAN_POINT('Ctrl Pts',(46.5766932247459,-57.4754524783491,
-40.6308875));
#245930=CARTESIAN_POINT('Ctrl Pts',(46.5766932247459,-56.2810644399698,
-40.5725541666667));
#245931=CARTESIAN_POINT('Ctrl Pts',(45.5423228415332,-55.6838704207802,
-40.5142208333333));
#245932=CARTESIAN_POINT('Ctrl Pts',(44.5079524583205,-55.0866764015906,
-40.4558875));
#245933=CARTESIAN_POINT('Ctrl Pts',(43.4735820751078,-55.6838704207802,
-40.3975541666667));
#245934=CARTESIAN_POINT('Ctrl Pts',(42.4392116918951,-56.2810644399698,
-40.3392208333333));
#245935=CARTESIAN_POINT('Ctrl Pts',(42.439211691895,-57.4754524783491,-40.2808875));
#245936=CARTESIAN_POINT('Ctrl Pts',(42.4392116918951,-58.6698405167284,
-40.2225541666667));
#245937=CARTESIAN_POINT('Ctrl Pts',(43.4735820751078,-59.267034535918,-40.1642208333333));
#245938=CARTESIAN_POINT('Ctrl Pts',(44.5079524583205,-59.8642285551076,
-40.1058875));
#245939=CARTESIAN_POINT('Ctrl Pts',(45.5423228415332,-59.267034535918,-40.0475541666667));
#245940=CARTESIAN_POINT('Ctrl Pts',(46.5766932247459,-58.6698405167284,
-39.9892208333333));
#245941=CARTESIAN_POINT('Ctrl Pts',(46.5766932247459,-57.4754524783491,
-39.9308875));
#245942=CARTESIAN_POINT('Ctrl Pts',(46.5766932247459,-56.2810644399698,
-39.8725541666667));
#245943=CARTESIAN_POINT('Ctrl Pts',(45.5423228415332,-55.6838704207802,
-39.8142208333334));
#245944=CARTESIAN_POINT('Ctrl Pts',(44.5079524583205,-55.0866764015906,
-39.7558875));
#245945=CARTESIAN_POINT('Ctrl Pts',(43.4735820751078,-55.6838704207802,
-39.6975541666667));
#245946=CARTESIAN_POINT('Ctrl Pts',(42.4392116918951,-56.2810644399698,
-39.6392208333334));
#245947=CARTESIAN_POINT('Ctrl Pts',(42.439211691895,-57.4754524783491,-39.5808875000001));
#245948=CARTESIAN_POINT('Ctrl Pts',(42.4392116918951,-58.6698405167284,
-39.5225541666667));
#245949=CARTESIAN_POINT('Ctrl Pts',(43.4735820751078,-59.267034535918,-39.4642208333333));
#245950=CARTESIAN_POINT('Ctrl Pts',(44.5079524583205,-59.8642285551076,
-39.4058875));
#245951=CARTESIAN_POINT('Ctrl Pts',(45.5423228415332,-59.267034535918,-39.3475541666667));
#245952=CARTESIAN_POINT('Ctrl Pts',(46.5766932247459,-58.6698405167284,
-39.2892208333334));
#245953=CARTESIAN_POINT('Ctrl Pts',(46.5766932247459,-57.4754524783491,
-39.2308875));
#245954=CARTESIAN_POINT('Ctrl Pts',(46.5766932247459,-56.2810644399698,
-39.1725541666667));
#245955=CARTESIAN_POINT('Ctrl Pts',(45.5423228415332,-55.6838704207802,
-39.1142208333333));
#245956=CARTESIAN_POINT('Ctrl Pts',(44.5079524583205,-55.0866764015906,
-39.0558875));
#245957=CARTESIAN_POINT('Ctrl Pts',(43.4735820751078,-55.6838704207802,
-38.9975541666667));
#245958=CARTESIAN_POINT('Ctrl Pts',(42.4392116918951,-56.2810644399698,
-38.9392208333334));
#245959=CARTESIAN_POINT('Ctrl Pts',(42.439211691895,-57.4754524783491,-38.8808875));
#245960=CARTESIAN_POINT('Ctrl Pts',(42.4392116918951,-58.6698405167284,
-38.8225541666667));
#245961=CARTESIAN_POINT('Ctrl Pts',(43.4735820751078,-59.267034535918,-38.7642208333333));
#245962=CARTESIAN_POINT('Ctrl Pts',(44.5079524583205,-59.8642285551076,
-38.7058875));
#245963=CARTESIAN_POINT('Ctrl Pts',(45.5423228415332,-59.267034535918,-38.6475541666667));
#245964=CARTESIAN_POINT('Ctrl Pts',(46.5766932247459,-58.6698405167284,
-38.5892208333334));
#245965=CARTESIAN_POINT('Ctrl Pts',(46.5766932247459,-57.4754524783491,
-38.5308875));
#245966=CARTESIAN_POINT('Ctrl Pts',(46.5766932247459,-56.2810644399698,
-38.4725541666667));
#245967=CARTESIAN_POINT('Ctrl Pts',(45.5423228415332,-55.6838704207802,
-38.4142208333334));
#245968=CARTESIAN_POINT('Ctrl Pts',(44.5079524583205,-55.0866764015906,
-38.3558875));
#245969=CARTESIAN_POINT('Ctrl Pts',(43.4735820751078,-55.6838704207802,
-38.2975541666667));
#245970=CARTESIAN_POINT('Ctrl Pts',(42.4392116918951,-56.2810644399698,
-38.2392208333333));
#245971=CARTESIAN_POINT('Ctrl Pts',(42.439211691895,-57.4754524783491,-38.1808875000001));
#245972=CARTESIAN_POINT('Ctrl Pts',(42.4392116918951,-58.6698405167284,
-38.1225541666667));
#245973=CARTESIAN_POINT('Ctrl Pts',(43.4735820751078,-59.267034535918,-38.0642208333334));
#245974=CARTESIAN_POINT('Ctrl Pts',(44.5079524583205,-59.8642285551076,
-38.0058875));
#245975=CARTESIAN_POINT('Ctrl Pts',(45.5423228415332,-59.267034535918,-37.9475541666667));
#245976=CARTESIAN_POINT('Ctrl Pts',(46.5766932247459,-58.6698405167284,
-37.8892208333334));
#245977=CARTESIAN_POINT('Ctrl Pts',(46.5766932247459,-57.4754524783491,
-37.8308875));
#245978=CARTESIAN_POINT('Ctrl Pts',(46.5766932247459,-56.2810644399698,
-37.7725541666667));
#245979=CARTESIAN_POINT('Ctrl Pts',(45.5423228415332,-55.6838704207802,
-37.7142208333333));
#245980=CARTESIAN_POINT('Ctrl Pts',(44.5079524583205,-55.0866764015906,
-37.6558875));
#245981=CARTESIAN_POINT('Ctrl Pts',(43.4735820751078,-55.6838704207802,
-37.5975541666667));
#245982=CARTESIAN_POINT('Ctrl Pts',(42.4392116918951,-56.2810644399698,
-37.5392208333334));
#245983=CARTESIAN_POINT('Ctrl Pts',(42.439211691895,-57.4754524783491,-37.4808875));
#245984=CARTESIAN_POINT('Ctrl Pts',(42.4392116918951,-58.6698405167284,
-37.4225541666667));
#245985=CARTESIAN_POINT('Ctrl Pts',(43.4735820751078,-59.267034535918,-37.3642208333333));
#245986=CARTESIAN_POINT('Ctrl Pts',(44.5079524583205,-59.8642285551076,
-37.3058875));
#245987=CARTESIAN_POINT('Ctrl Pts',(45.5423228415332,-59.267034535918,-37.2475541666667));
#245988=CARTESIAN_POINT('Ctrl Pts',(45.6766168155006,-59.1894998738974,
-37.239980655983));
#245989=CARTESIAN_POINT('Ctrl Pts',(45.7978513037526,-59.0928112286649,
-37.2318399189827));
#245990=CARTESIAN_POINT('Ctrl Pts',(42.8346997657407,-56.3799037924606,
-38.9060754358215));
#245991=CARTESIAN_POINT('Ctrl Pts',(42.8657912775273,-56.3324177857128,
-38.9093809684272));
#245992=CARTESIAN_POINT('Ctrl Pts',(42.8988701072886,-56.2863150958481,
-38.9126746506026));
#245993=CARTESIAN_POINT('Ctrl Pts',(42.9337333069081,-56.2418267252429,
-38.9159388745174));
#245994=CARTESIAN_POINT('Ctrl Pts',(42.9687109169304,-56.1971923573553,
-38.9192138106209));
#245995=CARTESIAN_POINT('Ctrl Pts',(43.0054840427986,-56.1541833777436,
-38.9224590546962));
#245996=CARTESIAN_POINT('Ctrl Pts',(43.0438141464837,-56.1129927698216,
-38.9256578819596));
#245997=CARTESIAN_POINT('Ctrl Pts',(43.0824956090267,-56.0714245817847,
-38.9288860317707));
#245998=CARTESIAN_POINT('Ctrl Pts',(43.1227620598465,-56.0317085984475,
-38.9320668731519));
#245999=CARTESIAN_POINT('Ctrl Pts',(43.1643436400644,-55.9939960368214,
-38.9351848778962));
#246000=CARTESIAN_POINT('Ctrl Pts',(43.2061767575094,-55.9560553426152,
-38.9383217442196));
#246001=CARTESIAN_POINT('Ctrl Pts',(43.2493402292857,-55.9201425202975,
-38.9413949829685));
#246002=CARTESIAN_POINT('Ctrl Pts',(43.2935450408245,-55.8863604391545,
-38.944390949966));
#246003=CARTESIAN_POINT('Ctrl Pts',(43.3383073424745,-55.8521523144312,
-38.947424700678));
#246004=CARTESIAN_POINT('Ctrl Pts',(43.3841366695237,-55.8201290211542,
-38.9503791961889));
#246005=CARTESIAN_POINT('Ctrl Pts',(43.4307296615396,-55.7903439160353,
-38.953242875097));
#246006=CARTESIAN_POINT('Ctrl Pts',(43.4562577073261,-55.7740248196576,
-38.9548118691264));
#246007=CARTESIAN_POINT('Ctrl Pts',(43.4820150081877,-55.7583766645963,
-38.9563536487424));
#246008=CARTESIAN_POINT('Ctrl Pts',(43.5079524583204,-55.7434016707801,
-38.9578666666668));
#246009=CARTESIAN_POINT('Ctrl Pts',(43.5552055679399,-55.7161200752212,
-38.9606230980613));
#246010=CARTESIAN_POINT('Ctrl Pts',(43.6040973111767,-55.6904744504906,
-38.9634751033216));
#246011=CARTESIAN_POINT('Ctrl Pts',(43.6544568310304,-55.6667111967904,
-38.9664127263806));
#246012=CARTESIAN_POINT('Ctrl Pts',(43.7043813282697,-55.643153218136,-38.9693249732551));
#246013=CARTESIAN_POINT('Ctrl Pts',(43.7557481097746,-55.6214458968395,
-38.9723213509202));
#246014=CARTESIAN_POINT('Ctrl Pts',(43.8083455435853,-55.6018063857908,
-38.9753895242081));
#246015=CARTESIAN_POINT('Ctrl Pts',(43.8604147804534,-55.5823640997575,
-38.9784268861116));
#246016=CARTESIAN_POINT('Ctrl Pts',(43.9136896632225,-55.5649488835336,
-38.9815345847811));
#246017=CARTESIAN_POINT('Ctrl Pts',(43.9679253295305,-55.5497395667206,
-38.9846983459951));
#246018=CARTESIAN_POINT('Ctrl Pts',(44.0168892084326,-55.5360086181159,
-38.9875545849152));
#246019=CARTESIAN_POINT('Ctrl Pts',(44.0666354001336,-55.52407545424,-38.9904564724688));
#246020=CARTESIAN_POINT('Ctrl Pts',(44.1169605007733,-55.5140434474753,
-38.9933921501253));
#246021=CARTESIAN_POINT('Ctrl Pts',(-50.8662592829675,-43.9775643489266,
-38.2016959289287));
#246022=CARTESIAN_POINT('Ctrl Pts',(-50.9206074996482,-43.8969602231097,
-38.2028048079744));
#246023=CARTESIAN_POINT('Ctrl Pts',(-50.9634706458651,-43.817641350392,
-38.2391813181835));
#246024=CARTESIAN_POINT('Ctrl Pts',(-50.6165344156739,-43.8081147605988,
-38.1265410889715));
#246025=CARTESIAN_POINT('Ctrl Pts',(-50.6707175035488,-43.7281782205006,
-38.1277074258953));
#246026=CARTESIAN_POINT('Ctrl Pts',(-50.7134583474186,-43.6493859440548,
-38.1636515730652));
#246027=CARTESIAN_POINT('Ctrl Pts',(-50.367254897517,-43.6381237449266,
-38.0514121363637));
#246028=CARTESIAN_POINT('Ctrl Pts',(-50.4211897771984,-43.558806022001,
-38.0526121686946));
#246029=CARTESIAN_POINT('Ctrl Pts',(-50.4638460929301,-43.480574245264,
-38.0881367070155));
#246030=CARTESIAN_POINT('Ctrl Pts',(-50.1184449162637,-43.4675617326621,
-37.9763108762634));
#246031=CARTESIAN_POINT('Ctrl Pts',(-50.1720495177334,-43.3888135426178,
-37.9775209986779));
#246032=CARTESIAN_POINT('Ctrl Pts',(-50.2146583013983,-43.3111769590637,
-38.012638623582));
#246033=CARTESIAN_POINT('',(-50.1228968347622,-43.4706134770457,-37.9776546393185));
#246034=CARTESIAN_POINT('',(-50.8662598031175,-43.9775646659832,-38.2016934855357));
#246035=CARTESIAN_POINT('Origin',(-163.821120857268,123.708346813688,-40.9343427676646));
#246036=CARTESIAN_POINT('',(-50.9629628917746,-43.8185802311495,-38.2387520398483));
#246037=CARTESIAN_POINT('Origin',(-50.2413380988264,-43.5197615250917,-38.4894964491189));
#246038=CARTESIAN_POINT('Origin',(-50.7629779210076,-43.9145999846305,-38.6868437920595));
#246039=CARTESIAN_POINT('Ctrl Pts',(-52.1463598473653,-42.4957105173844,
-39.6163034956207));
#246040=CARTESIAN_POINT('Ctrl Pts',(-52.1778331585616,-42.407856341012,
-39.2820037515321));
#246041=CARTESIAN_POINT('Ctrl Pts',(-51.8651142120726,-42.3571081800691,
-39.1398680265747));
#246042=CARTESIAN_POINT('Ctrl Pts',(-52.138908792049,-42.7327637189233,
-39.5106313066209));
#246043=CARTESIAN_POINT('Ctrl Pts',(-52.1408096255332,-42.6362970896441,
-39.208392993337));
#246044=CARTESIAN_POINT('Ctrl Pts',(-51.8563466958888,-42.5839200186503,
-39.0796163834337));
#246045=CARTESIAN_POINT('Ctrl Pts',(-52.1182999697365,-42.9653720232436,
-39.3935075242519));
#246046=CARTESIAN_POINT('Ctrl Pts',(-52.0958067489885,-42.8676463321302,
-39.1251861092046));
#246047=CARTESIAN_POINT('Ctrl Pts',(-51.8388838770158,-42.8062228472946,
-39.0116982544704));
#246048=CARTESIAN_POINT('Ctrl Pts',(-52.0320114860966,-43.3497261830944,
-39.161530854536));
#246049=CARTESIAN_POINT('Ctrl Pts',(-51.9795767898205,-43.2501370823012,
-38.9567426032799));
#246050=CARTESIAN_POINT('Ctrl Pts',(-51.7752900045357,-43.1727371404884,
-38.8742643034118));
#246051=CARTESIAN_POINT('Ctrl Pts',(-51.9821559399578,-43.506114175996,
-39.0559812260102));
#246052=CARTESIAN_POINT('Ctrl Pts',(-51.9220107796067,-43.40483234188,-38.8805374882183));
#246053=CARTESIAN_POINT('Ctrl Pts',(-51.7396064271064,-43.3216378204905,
-38.8110241554243));
#246054=CARTESIAN_POINT('Ctrl Pts',(-51.8587029432334,-43.7273337947907,
-38.8735991626261));
#246055=CARTESIAN_POINT('Ctrl Pts',(-51.7966191070807,-43.6242584279089,
-38.7452143542829));
#246056=CARTESIAN_POINT('Ctrl Pts',(-51.6539357945151,-43.5318198667555,
-38.699791068918));
#246057=CARTESIAN_POINT('Ctrl Pts',(-51.8101033942497,-43.7971217698189,
-38.8100520149236));
#246058=CARTESIAN_POINT('Ctrl Pts',(-51.7496889766211,-43.6930275230314,
-38.6980706314006));
#246059=CARTESIAN_POINT('Ctrl Pts',(-51.6204903967813,-43.598045469751,
-38.6607426239999));
#246060=CARTESIAN_POINT('Ctrl Pts',(-51.6873370041662,-43.9236094312998,
-38.674885570098));
#246061=CARTESIAN_POINT('Ctrl Pts',(-51.6361098819405,-43.8172559764407,
-38.5963460304981));
#246062=CARTESIAN_POINT('Ctrl Pts',(-51.5368137528036,-43.7178768472947,
-38.5767876614047));
#246063=CARTESIAN_POINT('Ctrl Pts',(-51.6135281175597,-43.9798771251562,
-38.6036544036492));
#246064=CARTESIAN_POINT('Ctrl Pts',(-51.5698336784193,-43.8726832305444,
-38.541955894343));
#246065=CARTESIAN_POINT('Ctrl Pts',(-51.4868275908931,-43.7710708483964,
-38.5321195958186));
#246066=CARTESIAN_POINT('Ctrl Pts',(-51.4291465383277,-44.058604748282,
-38.459510380713));
#246067=CARTESIAN_POINT('Ctrl Pts',(-51.4095099680441,-43.9497005422073,
-38.4289632372181));
#246068=CARTESIAN_POINT('Ctrl Pts',(-51.3629645413757,-43.8451599264395,
-38.440265964053));
#246069=CARTESIAN_POINT('Ctrl Pts',(-51.319068965668,-44.078041978234,-38.388630302131));
#246070=CARTESIAN_POINT('Ctrl Pts',(-51.3156521245987,-43.9687081271715,
-38.3713923008305));
#246071=CARTESIAN_POINT('Ctrl Pts',(-51.2894661655026,-43.8631892410449,
-38.3942946312693));
#246072=CARTESIAN_POINT('Ctrl Pts',(-51.089300024305,-44.0616597869013,
-38.2737385514644));
#246073=CARTESIAN_POINT('Ctrl Pts',(-51.1234504711255,-43.9521135664641,
-38.2731895662586));
#246074=CARTESIAN_POINT('Ctrl Pts',(-51.1369785556538,-43.8467829646352,
-38.3177691970519));
#246075=CARTESIAN_POINT('Ctrl Pts',(-50.9704089609615,-44.0259726799371,
-38.2301338295288));
#246076=CARTESIAN_POINT('Ctrl Pts',(-51.0249939553012,-43.9165958222839,
-38.2325205502091));
#246077=CARTESIAN_POINT('Ctrl Pts',(-51.0586423830823,-43.8125622297662,
-38.2875269246531));
#246078=CARTESIAN_POINT('Ctrl Pts',(-50.8660311843248,-43.9777851953718,
-38.2016761331321));
#246079=CARTESIAN_POINT('Ctrl Pts',(-50.9393056690222,-43.8691613854929,
-38.2030936955718));
#246080=CARTESIAN_POINT('Ctrl Pts',(-50.9899108736213,-43.7663745378293,
-38.2666882799375));
#246081=CARTESIAN_POINT('',(-51.855727616252,-42.5504169941763,-39.0864710348602));
#246082=CARTESIAN_POINT('',(-52.1363779744195,-42.6975314190816,-39.5221562288903));
#246083=CARTESIAN_POINT('Origin',(-51.6375959493,-42.6626531820611,-39.5221562583896));
#246084=CARTESIAN_POINT('Ctrl Pts',(-50.8662613636147,-43.9775656172223,
-38.2016861553823));
#246085=CARTESIAN_POINT('Ctrl Pts',(-50.9078004219846,-43.9967461943322,
-38.2130183288712));
#246086=CARTESIAN_POINT('Ctrl Pts',(-50.949269083369,-44.0129893917626,
-38.2259372986406));
#246087=CARTESIAN_POINT('Ctrl Pts',(-50.9903956935496,-44.0262820941249,
-38.2403937622755));
#246088=CARTESIAN_POINT('Ctrl Pts',(-51.0314585596062,-44.0395541934843,
-38.2548278191376));
#246089=CARTESIAN_POINT('Ctrl Pts',(-51.0721796277597,-44.0498849023057,
-38.2707944285533));
#246090=CARTESIAN_POINT('Ctrl Pts',(-51.1123002988897,-44.0572683454116,
-38.2881944319024));
#246091=CARTESIAN_POINT('Ctrl Pts',(-51.1298439799964,-44.0604969247866,
-38.2958029813462));
#246092=CARTESIAN_POINT('Ctrl Pts',(-51.1472730853109,-44.0631620602905,
-38.3036849773209));
#246093=CARTESIAN_POINT('Ctrl Pts',(-51.1645672900365,-44.0652637097802,
-38.3118293100208));
#246094=CARTESIAN_POINT('Ctrl Pts',(-51.2041865851273,-44.0700783787768,
-38.3304871625023));
#246095=CARTESIAN_POINT('Ctrl Pts',(-51.2430955061505,-44.0719352464437,
-38.3505244284462));
#246096=CARTESIAN_POINT('Ctrl Pts',(-51.2810711000578,-44.0708391843286,
-38.3717770661348));
#246097=CARTESIAN_POINT('Ctrl Pts',(-51.2893225981018,-44.0706010273055,
-38.3763949293537));
#246098=CARTESIAN_POINT('Ctrl Pts',(-51.2975301585805,-44.0702234828254,
-38.381070026873));
#246099=CARTESIAN_POINT('Ctrl Pts',(-51.3056917160415,-44.0697066461471,
-38.385800442706));
#246100=CARTESIAN_POINT('Ctrl Pts',(-51.3285533264544,-44.0682589177148,
-38.3990509680356));
#246101=CARTESIAN_POINT('Ctrl Pts',(-51.3510535722672,-44.0657181870734,
-38.412735840956));
#246102=CARTESIAN_POINT('Ctrl Pts',(-51.373150782787,-44.0620871882793,
-38.4268099888037));
#246103=CARTESIAN_POINT('Ctrl Pts',(-51.3841993880469,-44.0602716888823,
-38.4338470627276));
#246104=CARTESIAN_POINT('Ctrl Pts',(-51.3951472928094,-44.058183636393,
-38.4409813696671));
#246105=CARTESIAN_POINT('Ctrl Pts',(-51.4059898777672,-44.0558234574321,
-38.4482069490058));
#246106=CARTESIAN_POINT('Ctrl Pts',(-51.4126979836034,-44.054363258566,
-38.4526772806766));
#246107=CARTESIAN_POINT('Ctrl Pts',(-51.4197316537442,-44.05270078671,-38.4574288435828));
#246108=CARTESIAN_POINT('Ctrl Pts',(-51.4264092843737,-44.0510178394573,
-38.462005765729));
#246109=CARTESIAN_POINT('Ctrl Pts',(-51.4305249803831,-44.0499805704503,
-38.4648267094525));
#246110=CARTESIAN_POINT('Ctrl Pts',(-51.4345059407379,-44.04893567481,-38.4675802974087));
#246111=CARTESIAN_POINT('Ctrl Pts',(-51.4381973259372,-44.047927018598,
-38.470151265276));
#246112=CARTESIAN_POINT('Ctrl Pts',(-51.4751679454563,-44.0378249449793,
-38.4959004812708));
#246113=CARTESIAN_POINT('Ctrl Pts',(-51.5113692337529,-44.0243189447717,
-38.523077931443));
#246114=CARTESIAN_POINT('Ctrl Pts',(-51.5465460185733,-44.0074090900157,
-38.5515565059206));
#246115=CARTESIAN_POINT('Ctrl Pts',(-51.5815815540112,-43.9905671353408,
-38.5799207271087));
#246116=CARTESIAN_POINT('Ctrl Pts',(-51.6156000740549,-43.9703486034704,
-38.6095753079235));
#246117=CARTESIAN_POINT('Ctrl Pts',(-51.6483730590436,-43.9467609115004,
-38.6403493423971));
#246118=CARTESIAN_POINT('Ctrl Pts',(-51.6810670486091,-43.9232300748858,
-38.6710491996824));
#246119=CARTESIAN_POINT('Ctrl Pts',(-51.7125208832909,-43.8963463259735,
-38.7028626106144));
#246120=CARTESIAN_POINT('Ctrl Pts',(-51.7425412958989,-43.8661241919007,
-38.7355810510177));
#246121=CARTESIAN_POINT('Ctrl Pts',(-51.7471512174186,-43.8614832941205,
-38.7406052805137));
#246122=CARTESIAN_POINT('Ctrl Pts',(-51.7517274126434,-43.8567636886518,
-38.7456507856083));
#246123=CARTESIAN_POINT('Ctrl Pts',(-51.7562692654992,-43.8519654422891,
-38.7507167429485));
#246124=CARTESIAN_POINT('Ctrl Pts',(-51.7718585546465,-43.8354961174734,
-38.7681049491038));
#246125=CARTESIAN_POINT('Ctrl Pts',(-51.7870429900321,-43.8181002779942,
-38.785734261531));
#246126=CARTESIAN_POINT('Ctrl Pts',(-51.8017998436459,-43.7997809435826,
-38.8035700068467));
#246127=CARTESIAN_POINT('Ctrl Pts',(-51.8091782704528,-43.7906212763769,
-38.8124878795046));
#246128=CARTESIAN_POINT('Ctrl Pts',(-51.8164498539091,-43.781230743038,
-38.821457325757));
#246129=CARTESIAN_POINT('Ctrl Pts',(-51.8236120869667,-43.7716097649364,
-38.8304738402603));
#246130=CARTESIAN_POINT('Ctrl Pts',(-51.8271932034955,-43.7667992758857,
-38.8349820975119));
#246131=CARTESIAN_POINT('Ctrl Pts',(-51.8307469855887,-43.7619311761192,
-38.8395021196075));
#246132=CARTESIAN_POINT('Ctrl Pts',(-51.8342731412247,-43.7570055208757,
-38.8440333338866));
#246133=CARTESIAN_POINT('Ctrl Pts',(-51.8368130664596,-43.7534575220512,
-38.8472972129322));
#246134=CARTESIAN_POINT('Ctrl Pts',(-51.8397709257302,-43.7492575266246,
-38.8511273425434));
#246135=CARTESIAN_POINT('Ctrl Pts',(-51.8422112091579,-43.745749784102,
-38.8543131150123));
#246136=CARTESIAN_POINT('Ctrl Pts',(-51.8431587495307,-43.7443877588472,
-38.855550122156));
#246137=CARTESIAN_POINT('Ctrl Pts',(-51.8440288232728,-43.7431301746906,
-38.8566896765824));
#246138=CARTESIAN_POINT('Ctrl Pts',(-51.8447684504413,-43.7420559457143,
-38.857659973624));
#246139=CARTESIAN_POINT('Ctrl Pts',(-51.869619022372,-43.7059631606182,
-38.8902607723163));
#246140=CARTESIAN_POINT('Ctrl Pts',(-51.8933616238456,-43.6664604414045,
-38.92383760287));
#246141=CARTESIAN_POINT('Ctrl Pts',(-51.9157806930845,-43.6235568924935,
-38.9582211922616));
#246142=CARTESIAN_POINT('Ctrl Pts',(-51.9315329386519,-43.5934116964125,
-38.9823800339073));
#246143=CARTESIAN_POINT('Ctrl Pts',(-51.9466321814526,-43.5615877106783,
-39.0069361696535));
#246144=CARTESIAN_POINT('Ctrl Pts',(-51.9610125958872,-43.528090184004,
-39.0318184615583));
#246145=CARTESIAN_POINT('Ctrl Pts',(-51.9784361220784,-43.4875040773932,
-39.0619662202806));
#246146=CARTESIAN_POINT('Ctrl Pts',(-51.9948036328542,-43.444461108997,
-39.0925930961632));
#246147=CARTESIAN_POINT('Ctrl Pts',(-52.0100167926752,-43.3989739076197,
-39.1235551946763));
#246148=CARTESIAN_POINT('Ctrl Pts',(-52.0176233725858,-43.376230306931,
-39.1390362439329));
#246149=CARTESIAN_POINT('Ctrl Pts',(-52.0249417103708,-43.3528757033714,
-39.1546008212855));
#246150=CARTESIAN_POINT('Ctrl Pts',(-52.031961741472,-43.3289119934329,
-39.1702294612548));
#246151=CARTESIAN_POINT('Ctrl Pts',(-52.0354717570227,-43.3169301384636,
-39.1780437812394));
#246152=CARTESIAN_POINT('Ctrl Pts',(-52.0389072222062,-43.304796009584,
-39.1858741093882));
#246153=CARTESIAN_POINT('Ctrl Pts',(-52.0422670274971,-43.2925098629238,
-39.1937179293146));
#246154=CARTESIAN_POINT('Ctrl Pts',(-52.0439469301426,-43.2863667895937,
-39.1976398392779));
#246155=CARTESIAN_POINT('Ctrl Pts',(-52.0456079194934,-43.2801857119935,
-39.201565121674));
#246156=CARTESIAN_POINT('Ctrl Pts',(-52.0472498669231,-43.2739666631534,
-39.2054934588666));
#246157=CARTESIAN_POINT('Ctrl Pts',(-52.0485785941713,-43.2689339687429,
-39.2086724209779));
#246158=CARTESIAN_POINT('Ctrl Pts',(-52.050139501498,-43.2629252013346,
-39.2124478593144));
#246159=CARTESIAN_POINT('Ctrl Pts',(-52.0513379881636,-43.2582496014946,
-39.215376408652));
#246160=CARTESIAN_POINT('Ctrl Pts',(-52.0516205068005,-43.2571474247819,
-39.2160667540606));
#246161=CARTESIAN_POINT('Ctrl Pts',(-52.0518831318285,-43.2561193454742,
-39.2167100295185));
#246162=CARTESIAN_POINT('Ctrl Pts',(-52.0521184614956,-43.2551956366398,
-39.2172873150054));
#246163=CARTESIAN_POINT('Ctrl Pts',(-52.0649863542751,-43.2046869762132,
-39.2488534487757));
#246164=CARTESIAN_POINT('Ctrl Pts',(-52.0768350792428,-43.1508768626302,
-39.281128278774));
#246165=CARTESIAN_POINT('Ctrl Pts',(-52.0874657593684,-43.0937769205883,
-39.3139294576404));
#246166=CARTESIAN_POINT('Ctrl Pts',(-52.098456883128,-43.0347409490196,
-39.347842792641));
#246167=CARTESIAN_POINT('Ctrl Pts',(-52.1081448988321,-42.9721882462489,
-39.3823185300744));
#246168=CARTESIAN_POINT('Ctrl Pts',(-52.1163489521921,-42.9061392731944,
-39.417111092746));
#246169=CARTESIAN_POINT('Ctrl Pts',(-52.1241330629832,-42.843471162526,
-39.4501227213469));
#246170=CARTESIAN_POINT('Ctrl Pts',(-52.1305810127062,-42.7776556479445,
-39.4834186547465));
#246171=CARTESIAN_POINT('Ctrl Pts',(-52.1355813145032,-42.708716260349,
-39.5167597484441));
#246172=CARTESIAN_POINT('Ctrl Pts',(-52.1358510742276,-42.704997070797,
-39.5185584567247));
#246173=CARTESIAN_POINT('Ctrl Pts',(-52.1361166319404,-42.7012687906537,
-39.5203572909574));
#246174=CARTESIAN_POINT('Ctrl Pts',(-52.1363779740716,-42.6975314240561,
-39.5221562118214));
#246175=CARTESIAN_POINT('',(-51.2551520560089,-43.9396089457538,-38.3574184111583));
#246176=CARTESIAN_POINT('Ctrl Pts',(-51.2549749806985,-43.9395355987587,
-38.3573338134652));
#246177=CARTESIAN_POINT('Ctrl Pts',(-51.2311912050884,-43.9296840363366,
-38.3459729646063));
#246178=CARTESIAN_POINT('Ctrl Pts',(-51.2072412883732,-43.9197636560154,
-38.3352762701445));
#246179=CARTESIAN_POINT('Ctrl Pts',(-51.1631138496503,-43.9014854724236,
-38.316377625375));
#246180=CARTESIAN_POINT('Ctrl Pts',(-51.1425648781377,-43.8929738097303,
-38.3078789583852));
#246181=CARTESIAN_POINT('Ctrl Pts',(-51.1120978131143,-43.8803539381919,
-38.2955513131889));
#246182=CARTESIAN_POINT('Ctrl Pts',(-51.1015315829945,-43.8759772623731,
-38.2913264303936));
#246183=CARTESIAN_POINT('Ctrl Pts',(-51.0866459456191,-43.8698114294876,
-38.2854361560059));
#246184=CARTESIAN_POINT('Ctrl Pts',(-51.0822429209912,-43.8679876369713,
-38.283701557845));
#246185=CARTESIAN_POINT('Ctrl Pts',(-51.0758876115541,-43.8653551816094,
-38.2812086804991));
#246186=CARTESIAN_POINT('Ctrl Pts',(-51.0739305078821,-43.8645445227255,
-38.2804424886344));
#246187=CARTESIAN_POINT('Ctrl Pts',(-51.0710119900097,-43.8633356330407,
-38.2793021155487));
#246188=CARTESIAN_POINT('Ctrl Pts',(-51.0700503307405,-43.8629373007292,
-38.27892671662));
#246189=CARTESIAN_POINT('Ctrl Pts',(-51.0686079713225,-43.8623398558964,
-38.2783642040776));
#246190=CARTESIAN_POINT('Ctrl Pts',(-51.0681272830895,-43.8621407483109,
-38.2781768273618));
#246191=CARTESIAN_POINT('Ctrl Pts',(-51.0674057880406,-43.8618418952765,
-38.2778957157717));
#246192=CARTESIAN_POINT('Ctrl Pts',(-51.0671649926649,-43.8617421545661,
-38.2778019185543));
#246193=CARTESIAN_POINT('Ctrl Pts',(-51.0668036221895,-43.8615924700141,
-38.2776611872062));
#246194=CARTESIAN_POINT('Ctrl Pts',(-51.0666830508817,-43.8615425277432,
-38.2776142377835));
#246195=CARTESIAN_POINT('Ctrl Pts',(-51.0575674890041,-43.8577667383849,
-38.2740651411923));
#246196=CARTESIAN_POINT('Ctrl Pts',(-51.0485165904603,-43.8540177334563,
-38.2705724504896));
#246197=CARTESIAN_POINT('Ctrl Pts',(-51.0245088795784,-43.8440734140075,
-38.2613952017063));
#246198=CARTESIAN_POINT('Ctrl Pts',(-51.0093159881586,-43.8377803123299,
-38.2556783811805));
#246199=CARTESIAN_POINT('Ctrl Pts',(-50.9838482215668,-43.8272312180042,
-38.2462842461313));
#246200=CARTESIAN_POINT('Ctrl Pts',(-50.9733963020293,-43.8229018911788,
-38.2424824569401));
#246201=CARTESIAN_POINT('Ctrl Pts',(-50.9629628917746,-43.8185802311496,
-38.2387520398482));
#246202=CARTESIAN_POINT('',(-51.3131709192528,-43.8514488225354,-38.4111555278088));
#246203=CARTESIAN_POINT('Ctrl Pts',(-51.3131706199324,-43.8514490160907,
-38.4111560835884));
#246204=CARTESIAN_POINT('Ctrl Pts',(-51.3069386016551,-43.8640094387329,
-38.4034254897557));
#246205=CARTESIAN_POINT('Ctrl Pts',(-51.3002063680618,-43.8760898419399,
-38.3960439531634));
#246206=CARTESIAN_POINT('Ctrl Pts',(-51.2930358474315,-43.887681591147,
-38.3889937580458));
#246207=CARTESIAN_POINT('Ctrl Pts',(-51.2857753960681,-43.8994187209419,
-38.3818551412852));
#246208=CARTESIAN_POINT('Ctrl Pts',(-51.2780655250384,-43.9106546759655,
-38.3750568369513));
#246209=CARTESIAN_POINT('Ctrl Pts',(-51.2699335264417,-43.9213447836983,
-38.3685638057529));
#246210=CARTESIAN_POINT('Ctrl Pts',(-51.2651534708457,-43.9276285168645,
-38.3647471486611));
#246211=CARTESIAN_POINT('Ctrl Pts',(-51.2602268679523,-43.9337229911979,
-38.3610355849099));
#246212=CARTESIAN_POINT('Ctrl Pts',(-51.2551536659444,-43.939613984762,
-38.357418527837));
#246213=CARTESIAN_POINT('Ctrl Pts',(-51.855727616252,-42.5504169941763,
-39.0864710348602));
#246214=CARTESIAN_POINT('Ctrl Pts',(-51.8458743174447,-42.7008613470123,
-39.042782114243));
#246215=CARTESIAN_POINT('Ctrl Pts',(-51.8311705584223,-42.8391342171477,
-38.9977676632627));
#246216=CARTESIAN_POINT('Ctrl Pts',(-51.8014482670023,-43.0284553089955,
-38.9290723862128));
#246217=CARTESIAN_POINT('Ctrl Pts',(-51.7846711206524,-43.1185939468382,
-38.8944295129609));
#246218=CARTESIAN_POINT('Ctrl Pts',(-51.7616665101479,-43.2158800024417,
-38.8536552611055));
#246219=CARTESIAN_POINT('Ctrl Pts',(-51.7492971647288,-43.262558791895,
-38.8331972272602));
#246220=CARTESIAN_POINT('Ctrl Pts',(-51.7428945957875,-43.2854077086099,
-38.8229527559164));
#246221=CARTESIAN_POINT('Ctrl Pts',(-51.7401038255464,-43.2950950611959,
-38.8185591959896));
#246222=CARTESIAN_POINT('Ctrl Pts',(-51.7382328961144,-43.3015299608571,
-38.8156294996974));
#246223=CARTESIAN_POINT('Ctrl Pts',(-51.7376125178611,-43.3036541572315,
-38.8146605651198));
#246224=CARTESIAN_POINT('Ctrl Pts',(-51.7160874290895,-43.3763411190383,
-38.7813111028424));
#246225=CARTESIAN_POINT('Ctrl Pts',(-51.6936601975632,-43.4385690812335,
-38.7501513027776));
#246226=CARTESIAN_POINT('Ctrl Pts',(-51.6566553067176,-43.5226975170906,
-38.7039720702541));
#246227=CARTESIAN_POINT('Ctrl Pts',(-51.6373120808315,-43.5624582890849,
-38.681022058614));
#246228=CARTESIAN_POINT('Ctrl Pts',(-51.6132516816768,-43.6048274098125,
-38.6545338045479));
#246229=CARTESIAN_POINT('Ctrl Pts',(-51.6008456012002,-43.6250088569449,
-38.6413662782202));
#246230=CARTESIAN_POINT('Ctrl Pts',(-51.595447894416,-43.6334432541016,
-38.6357399840156));
#246231=CARTESIAN_POINT('Ctrl Pts',(-51.5918314348969,-43.639018470814,
-38.63199294011));
#246232=CARTESIAN_POINT('Ctrl Pts',(-51.5906499275888,-43.6408284542711,
-38.6307721667191));
#246233=CARTESIAN_POINT('Ctrl Pts',(-51.5094055996291,-43.7627195584335,
-38.5475952000448));
#246234=CARTESIAN_POINT('Ctrl Pts',(-51.418063219401,-43.8314895829832,
-38.474608352185));
#246235=CARTESIAN_POINT('Ctrl Pts',(-51.3131710690959,-43.8514487256653,
-38.4111552499418));
#246236=CARTESIAN_POINT('Ctrl Pts',(-52.3762811131638,-39.2667566979623,
-40.1997763344591));
#246237=CARTESIAN_POINT('Ctrl Pts',(-52.3787524417377,-39.2314150528153,
-39.8684983696827));
#246238=CARTESIAN_POINT('Ctrl Pts',(-52.0729733445211,-39.1963583849098,
-39.7409428796644));
#246239=CARTESIAN_POINT('Ctrl Pts',(-52.2944317444485,-40.4372572032816,
-40.074293523619));
#246240=CARTESIAN_POINT('Ctrl Pts',(-52.298594212147,-40.3777311420296,
-39.7508319554676));
#246241=CARTESIAN_POINT('Ctrl Pts',(-51.9996196710719,-40.3410025908912,
-39.6210810788317));
#246242=CARTESIAN_POINT('Ctrl Pts',(-52.2140974212184,-41.5860915487537,
-39.8473838284864));
#246243=CARTESIAN_POINT('Ctrl Pts',(-52.2193926604804,-41.5103660993754,
-39.5325747394078));
#246244=CARTESIAN_POINT('Ctrl Pts',(-51.9268724548342,-41.4641473693466,
-39.4019228714579));
#246245=CARTESIAN_POINT('Ctrl Pts',(-52.1363779744299,-42.6975314189331,
-39.5221562583896));
#246246=CARTESIAN_POINT('Ctrl Pts',(-52.1426275598539,-42.6081581835409,
-39.2152367329798));
#246247=CARTESIAN_POINT('Ctrl Pts',(-51.855727616252,-42.5504169941763,
-39.0864710348602));
#246248=CARTESIAN_POINT('',(-52.0729733445211,-39.1963583849098,-39.7409428796644));
#246249=CARTESIAN_POINT('',(-52.3762811131638,-39.2667566979623,-40.1997763344591));
#246250=CARTESIAN_POINT('Origin',(-51.8774990880339,-39.2318784610903,-40.1997763344591));
#246251=CARTESIAN_POINT('Origin',(-52.5931625893807,-36.1652070894527,-23.5673415363821));
#246252=CARTESIAN_POINT('Origin',(-52.1460600630305,-36.065931493028,-23.2795421339938));
#246253=CARTESIAN_POINT('Ctrl Pts',(-52.0729733445211,-39.1963583849098,
-39.7409428796644));
#246254=CARTESIAN_POINT('Ctrl Pts',(-52.3787524417377,-39.2314150528153,
-39.8684983696827));
#246255=CARTESIAN_POINT('Ctrl Pts',(-52.3762811131638,-39.2667566979623,
-40.1997763344591));
#246256=CARTESIAN_POINT('Ctrl Pts',(-52.100888629852,-38.7607556577822,
-39.7865571684177));
#246257=CARTESIAN_POINT('Ctrl Pts',(-52.4109286028315,-38.8364874603624,
-39.9107687095326));
#246258=CARTESIAN_POINT('Ctrl Pts',(-52.4029815901681,-38.8849220874284,
-40.2475330828085));
#246259=CARTESIAN_POINT('Ctrl Pts',(-52.2102585591639,-38.3472834992403,
-39.8504420494694));
#246260=CARTESIAN_POINT('Ctrl Pts',(-52.5175719298667,-38.4659927236101,
-39.9706931604272));
#246261=CARTESIAN_POINT('Ctrl Pts',(-52.4996604569693,-38.5219332431804,
-40.3132835285224));
#246262=CARTESIAN_POINT('Ctrl Pts',(-52.3973403582525,-37.9591679226684,
-39.9296369918383));
#246263=CARTESIAN_POINT('Ctrl Pts',(-52.6906835816361,-38.1229388123735,
-40.0447034978031));
#246264=CARTESIAN_POINT('Ctrl Pts',(-52.6630979669894,-38.1805575254669,
-40.3940322392211));
#246265=CARTESIAN_POINT('',(-52.3973403582525,-37.9591679226684,-39.9296369918383));
#246266=CARTESIAN_POINT('',(-52.6630979669894,-38.1805575254669,-40.3940322392211));
#246267=CARTESIAN_POINT('Origin',(-52.2121187508304,-37.964646093179,-40.3940322392211));
#246268=CARTESIAN_POINT('Ctrl Pts',(-52.3762811131638,-39.2667566979623,
-40.1997763344591));
#246269=CARTESIAN_POINT('Ctrl Pts',(-52.3813348028011,-39.1944855690943,
-40.2088154151));
#246270=CARTESIAN_POINT('Ctrl Pts',(-52.3890106866762,-39.1212990642225,
-40.2186994462388));
#246271=CARTESIAN_POINT('Ctrl Pts',(-52.399580537506,-39.0474991337333,
-40.2294606094852));
#246272=CARTESIAN_POINT('Ctrl Pts',(-52.4098707578906,-38.975651615605,
-40.2399370810253));
#246273=CARTESIAN_POINT('Ctrl Pts',(-52.4229039093203,-38.9032227962493,
-40.251244856509));
#246274=CARTESIAN_POINT('Ctrl Pts',(-52.4388845253147,-38.8304840396482,
-40.263398639784));
#246275=CARTESIAN_POINT('Ctrl Pts',(-52.4546982516725,-38.7585049123794,
-40.2754254980096));
#246276=CARTESIAN_POINT('Ctrl Pts',(-52.4733983143613,-38.6862223928386,
-40.2882807703834));
#246277=CARTESIAN_POINT('Ctrl Pts',(-52.4951355715001,-38.6138907219804,
-40.3019641257189));
#246278=CARTESIAN_POINT('Ctrl Pts',(-52.5169079265806,-38.5414422611912,
-40.3156695748081));
#246279=CARTESIAN_POINT('Ctrl Pts',(-52.5417274476098,-38.4689446114306,
-40.3302057758585));
#246280=CARTESIAN_POINT('Ctrl Pts',(-52.5696958444338,-38.3966427428268,
-40.3455578235737));
#246281=CARTESIAN_POINT('Ctrl Pts',(-52.5976642412578,-38.3243408742229,
-40.3609098712888));
#246282=CARTESIAN_POINT('Ctrl Pts',(-52.6287816069157,-38.2522349026372,
-40.3770777354374));
#246283=CARTESIAN_POINT('Ctrl Pts',(-52.6630979669894,-38.1805575254669,
-40.3940322392211));
#246284=CARTESIAN_POINT('Ctrl Pts',(-52.3973403582525,-37.9591679226684,
-39.9296369918383));
#246285=CARTESIAN_POINT('Ctrl Pts',(-52.3381595240891,-38.0819431134417,
-39.9045847271404));
#246286=CARTESIAN_POINT('Ctrl Pts',(-52.2869524009769,-38.2068368043554,
-39.8811490804055));
#246287=CARTESIAN_POINT('Ctrl Pts',(-52.2436543900273,-38.3338051377694,
-39.859375557193));
#246288=CARTESIAN_POINT('Ctrl Pts',(-52.2004721855357,-38.4604338769931,
-39.8376602702492));
#246289=CARTESIAN_POINT('Ctrl Pts',(-52.1651567780144,-38.5891263087813,
-39.8175981380879));
#246290=CARTESIAN_POINT('Ctrl Pts',(-52.1376916733654,-38.7198578257722,
-39.7992419918224));
#246291=CARTESIAN_POINT('Ctrl Pts',(-52.1103657443256,-38.8499268789298,
-39.7809788627825));
#246292=CARTESIAN_POINT('Ctrl Pts',(-52.090810706346,-38.9820145333958,
-39.7644043901133));
#246293=CARTESIAN_POINT('Ctrl Pts',(-52.0790583244375,-39.1161133203773,
-39.7495795137018));
#246294=CARTESIAN_POINT('Ctrl Pts',(-52.0767210815741,-39.1427820787019,
-39.7466312316546));
#246295=CARTESIAN_POINT('Ctrl Pts',(-52.0746925946574,-39.169530428859,
-39.7437521782701));
#246296=CARTESIAN_POINT('Ctrl Pts',(-52.0729733445211,-39.1963583849098,
-39.7409428796644));
#246297=CARTESIAN_POINT('Ctrl Pts',(-52.3973403582526,-37.9591679226684,
-39.9296369918383));
#246298=CARTESIAN_POINT('Ctrl Pts',(-52.6906835816361,-38.1229388123734,
-40.0447034978031));
#246299=CARTESIAN_POINT('Ctrl Pts',(-52.6630979669894,-38.1805575254669,
-40.3940322392211));
#246300=CARTESIAN_POINT('Ctrl Pts',(-53.1457424766041,-36.406550234656,
-40.2464484764969));
#246301=CARTESIAN_POINT('Ctrl Pts',(-53.4384326164932,-36.5566079867106,
-40.3650991663767));
#246302=CARTESIAN_POINT('Ctrl Pts',(-53.4324663318346,-36.573559978192,
-40.7170573734051));
#246303=CARTESIAN_POINT('Ctrl Pts',(-53.8198487743995,-34.8177779595407,
-40.2933158502147));
#246304=CARTESIAN_POINT('Ctrl Pts',(-54.1268603779516,-34.9318568554821,
-40.4136350441051));
#246305=CARTESIAN_POINT('Ctrl Pts',(-54.1287347135875,-34.9307380700991,
-40.7648390575021));
#246306=CARTESIAN_POINT('Ctrl Pts',(-54.5679521612331,-32.7869698119953,
-40.01447771336));
#246307=CARTESIAN_POINT('Ctrl Pts',(-54.8877444086082,-32.8830970178215,
-40.1309118165611));
#246308=CARTESIAN_POINT('Ctrl Pts',(-54.9060208033569,-32.8327777738735,
-40.4805364040184));
#246309=CARTESIAN_POINT('Ctrl Pts',(-54.7126522107998,-32.3789049161325,
-39.9414701040553));
#246310=CARTESIAN_POINT('Ctrl Pts',(-55.0357525196778,-32.4702090184626,
-40.0565968968413));
#246311=CARTESIAN_POINT('Ctrl Pts',(-55.0566283970611,-32.4113164265585,
-40.4060976883517));
#246312=CARTESIAN_POINT('Ctrl Pts',(-54.9880779906355,-31.5720202326829,
-39.7641101894595));
#246313=CARTESIAN_POINT('Ctrl Pts',(-55.3180333651333,-31.6546255096238,
-39.8762742785657));
#246314=CARTESIAN_POINT('Ctrl Pts',(-55.3438236830459,-31.5781288928756,
-40.2252589174025));
#246315=CARTESIAN_POINT('Ctrl Pts',(-55.1194549413204,-31.1714661595765,
-39.6595567410297));
#246316=CARTESIAN_POINT('Ctrl Pts',(-55.4530870881607,-31.2497493955288,
-39.7698680960119));
#246317=CARTESIAN_POINT('Ctrl Pts',(-55.4810874242724,-31.1646108621852,
-40.1186537766862));
#246318=CARTESIAN_POINT('Ctrl Pts',(-55.4956573107256,-29.9783108281782,
-39.2999034309858));
#246319=CARTESIAN_POINT('Ctrl Pts',(-55.8415244394745,-30.042499694056,
-39.4035145580109));
#246320=CARTESIAN_POINT('Ctrl Pts',(-55.8749613596854,-29.9331076843543,
-39.7519370004083));
#246321=CARTESIAN_POINT('Ctrl Pts',(-55.7225896344932,-29.1941586468675,
-38.9989859405087));
#246322=CARTESIAN_POINT('Ctrl Pts',(-56.077077518843,-29.2501138114284,
-39.0964197551406));
#246323=CARTESIAN_POINT('Ctrl Pts',(-56.1136890638183,-29.1241139971889,
-39.4451035675999));
#246324=CARTESIAN_POINT('Ctrl Pts',(-55.9280282803564,-28.4214833957092,
-38.6389054336786));
#246325=CARTESIAN_POINT('Ctrl Pts',(-56.2902455608578,-28.4766057597396,
-38.7328054198089));
#246326=CARTESIAN_POINT('Ctrl Pts',(-56.3309570935689,-28.3272991455305,
-39.0779244525544));
#246327=CARTESIAN_POINT('',(-55.9280282803564,-28.4214833957092,-38.6389054336786));
#246328=CARTESIAN_POINT('',(-56.3309570935689,-28.3272991455305,-39.0779244525544));
#246329=CARTESIAN_POINT('Origin',(-55.8485682509781,-28.1957658625034,-39.0779244525544));
#246330=CARTESIAN_POINT('Ctrl Pts',(-52.6630979669894,-38.1805575254669,
-40.3940322392211));
#246331=CARTESIAN_POINT('Ctrl Pts',(-52.8760451560815,-37.7357697928196,
-40.4834397291488));
#246332=CARTESIAN_POINT('Ctrl Pts',(-53.0834983485661,-37.2880132084225,
-40.551761385336));
#246333=CARTESIAN_POINT('Ctrl Pts',(-53.2853549466339,-36.8374221904802,
-40.5989778505683));
#246334=CARTESIAN_POINT('Ctrl Pts',(-53.4478491683769,-36.4746971793296,
-40.6369870256205));
#246335=CARTESIAN_POINT('Ctrl Pts',(-53.6067170909194,-36.1101352784612,
-40.6613205359031));
#246336=CARTESIAN_POINT('Ctrl Pts',(-53.7619142086117,-35.7438031016591,
-40.6719908480972));
#246337=CARTESIAN_POINT('Ctrl Pts',(-53.9359086942521,-35.3331010240432,
-40.6839535411514));
#246338=CARTESIAN_POINT('Ctrl Pts',(-54.105287952085,-34.9201765391549,
-40.6787343711124));
#246339=CARTESIAN_POINT('Ctrl Pts',(-54.2699948688641,-34.5051333001102,
-40.6563333253597));
#246340=CARTESIAN_POINT('Ctrl Pts',(-54.3523483272536,-34.2976116805879,
-40.6451328024833));
#246341=CARTESIAN_POINT('Ctrl Pts',(-54.4335338407837,-34.089560425584,
-40.629636810339));
#246342=CARTESIAN_POINT('Ctrl Pts',(-54.5135451044598,-33.8809928709033,
-40.6098453486404));
#246343=CARTESIAN_POINT('Ctrl Pts',(-54.5555679147339,-33.7714508592289,
-40.5994506516715));
#246344=CARTESIAN_POINT('Ctrl Pts',(-54.5974060491286,-33.6614000385814,
-40.5878321906909));
#246345=CARTESIAN_POINT('Ctrl Pts',(-54.6388378415948,-33.5514189685314,
-40.5750457578139));
#246346=CARTESIAN_POINT('Ctrl Pts',(-54.6762920172485,-33.4519965184991,
-40.5634868733328));
#246347=CARTESIAN_POINT('Ctrl Pts',(-54.7134142984132,-33.3526311541021,
-40.5509741559631));
#246348=CARTESIAN_POINT('Ctrl Pts',(-54.7500504083475,-33.2537548873174,
-40.5375839610123));
#246349=CARTESIAN_POINT('Ctrl Pts',(-54.7502214650147,-33.2532932268219,
-40.5375214412162));
#246350=CARTESIAN_POINT('Ctrl Pts',(-54.7503925152058,-33.2528315659145,
-40.5374589009037));
#246351=CARTESIAN_POINT('Ctrl Pts',(-54.7505635589241,-33.2523699045864,
-40.5373963400742));
#246352=CARTESIAN_POINT('Ctrl Pts',(-54.8109190055075,-33.0894654968639,
-40.5153207745943));
#246353=CARTESIAN_POINT('Ctrl Pts',(-54.8704399382255,-32.9265623149063,
-40.4906380116614));
#246354=CARTESIAN_POINT('Ctrl Pts',(-54.9291455224067,-32.7636633303162,
-40.4633905681202));
#246355=CARTESIAN_POINT('Ctrl Pts',(-54.9873071697268,-32.6022736870193,
-40.4363955858928));
#246356=CARTESIAN_POINT('Ctrl Pts',(-55.0446688758138,-32.4408869522044,
-40.4068828775015));
#246357=CARTESIAN_POINT('Ctrl Pts',(-55.1012324203421,-32.2795110730784,
-40.3748470776743));
#246358=CARTESIAN_POINT('Ctrl Pts',(-55.1333863062824,-32.18777598727,-40.3566361352335));
#246359=CARTESIAN_POINT('Ctrl Pts',(-55.1652819353429,-32.0960445994109,
-40.3376090518113));
#246360=CARTESIAN_POINT('Ctrl Pts',(-55.19691646867,-32.0043213810441,-40.3177586380898));
#246361=CARTESIAN_POINT('Ctrl Pts',(-55.1980200095687,-32.0011217029651,
-40.3170661751041));
#246362=CARTESIAN_POINT('Ctrl Pts',(-55.1991232004239,-31.9979221280785,
-40.3163727298852));
#246363=CARTESIAN_POINT('Ctrl Pts',(-55.2002260400535,-31.994722659717,
-40.3156783028771));
#246364=CARTESIAN_POINT('Ctrl Pts',(-55.2636031512567,-31.8108581551368,
-40.2757715235684));
#246365=CARTESIAN_POINT('Ctrl Pts',(-55.325951793402,-31.6269964981267,
-40.2325819377435));
#246366=CARTESIAN_POINT('Ctrl Pts',(-55.3872684018359,-31.443178847248,
-40.1861063713614));
#246367=CARTESIAN_POINT('Ctrl Pts',(-55.429027236798,-31.3179923579394,
-40.1544548244822));
#246368=CARTESIAN_POINT('Ctrl Pts',(-55.4703078146834,-31.192825294027,
-40.1212791854428));
#246369=CARTESIAN_POINT('Ctrl Pts',(-55.5111134058755,-31.0676789074495,
-40.0865765609729));
#246370=CARTESIAN_POINT('Ctrl Pts',(-55.530477816035,-31.0082903313041,
-40.0701083311491));
#246371=CARTESIAN_POINT('Ctrl Pts',(-55.5499419887612,-30.9482684207738,
-40.0531149583656));
#246372=CARTESIAN_POINT('Ctrl Pts',(-55.5691505247735,-30.8887074115548,
-40.0359028676874));
#246373=CARTESIAN_POINT('Ctrl Pts',(-55.5835906458874,-30.843932099879,
-40.02296358518));
#246374=CARTESIAN_POINT('Ctrl Pts',(-55.5978866951893,-30.7994170631401,
-40.0099017258433));
#246375=CARTESIAN_POINT('Ctrl Pts',(-55.6118945080683,-30.7556237400288,
-39.9968653099877));
#246376=CARTESIAN_POINT('Ctrl Pts',(-55.6120559180998,-30.7551191158079,
-39.9967150932257));
#246377=CARTESIAN_POINT('Ctrl Pts',(-55.6122173197593,-30.7546144941026,
-39.9965648522302));
#246378=CARTESIAN_POINT('Ctrl Pts',(-55.6123787130472,-30.7541098749132,
-39.9964145870016));
#246379=CARTESIAN_POINT('Ctrl Pts',(-55.7548384822693,-30.3086890385658,
-39.8637774118964));
#246380=CARTESIAN_POINT('Ctrl Pts',(-55.8907835748029,-29.8652112734624,
-39.7123085185695));
#246381=CARTESIAN_POINT('Ctrl Pts',(-56.0204269822374,-29.4238800047714,
-39.5419882937266));
#246382=CARTESIAN_POINT('Ctrl Pts',(-56.1282497940572,-29.0568302698414,
-39.4003350780657));
#246383=CARTESIAN_POINT('Ctrl Pts',(-56.2317142317968,-28.6912651936965,
-39.2456431279436));
#246384=CARTESIAN_POINT('Ctrl Pts',(-56.3309570935689,-28.3272991455305,
-39.0779244525544));
#246385=CARTESIAN_POINT('Ctrl Pts',(-55.9280282803564,-28.4214833957092,
-38.6389054336786));
#246386=CARTESIAN_POINT('Ctrl Pts',(-55.8595025109934,-28.6792156535855,
-38.7590132822262));
#246387=CARTESIAN_POINT('Ctrl Pts',(-55.7888458358274,-28.9372393566178,
-38.8720750899543));
#246388=CARTESIAN_POINT('Ctrl Pts',(-55.7160933944967,-29.1952948017582,
-38.9780896749729));
#246389=CARTESIAN_POINT('Ctrl Pts',(-55.6418369701219,-29.4586849271757,
-39.08629585845));
#246390=CARTESIAN_POINT('Ctrl Pts',(-55.565397089092,-29.7221081267061,
-39.1871602619621));
#246391=CARTESIAN_POINT('Ctrl Pts',(-55.4868336072826,-29.9852798369313,
-39.2807323450087));
#246392=CARTESIAN_POINT('Ctrl Pts',(-55.4082701254731,-30.2484515471565,
-39.3743044280552));
#246393=CARTESIAN_POINT('Ctrl Pts',(-55.3275829838991,-30.5113717428164,
-39.4605842051981));
#246394=CARTESIAN_POINT('Ctrl Pts',(-55.2448557311221,-30.773747715777,
-39.5396723043484));
#246395=CARTESIAN_POINT('Ctrl Pts',(-55.2035971806928,-30.9046024456088,
-39.5791159002327));
#246396=CARTESIAN_POINT('Ctrl Pts',(-55.1618285510732,-31.0353297545122,
-39.6167686677692));
#246397=CARTESIAN_POINT('Ctrl Pts',(-55.1195602217546,-31.165894991039,
-39.6526370728405));
#246398=CARTESIAN_POINT('Ctrl Pts',(-55.0429685311297,-31.4024837648001,
-39.7176318769577));
#246399=CARTESIAN_POINT('Ctrl Pts',(-54.964737103265,-31.6385337089141,
-39.776762889674));
#246400=CARTESIAN_POINT('Ctrl Pts',(-54.8849569483814,-31.8737910274784,
-39.8300923327622));
#246401=CARTESIAN_POINT('Ctrl Pts',(-54.8734583654024,-31.9076982792613,
-39.8377786179977));
#246402=CARTESIAN_POINT('Ctrl Pts',(-54.8619276465711,-31.941589052632,
-39.8453444670309));
#246403=CARTESIAN_POINT('Ctrl Pts',(-54.8503651007177,-31.9754625744077,
-39.8527901467574));
#246404=CARTESIAN_POINT('Ctrl Pts',(-54.8385632459024,-32.0100371733883,
-39.8603899290412));
#246405=CARTESIAN_POINT('Ctrl Pts',(-54.8267234728141,-32.044606447891,
-39.8678659505221));
#246406=CARTESIAN_POINT('Ctrl Pts',(-54.814851167199,-32.0791552626038,
-39.8752157882416));
#246407=CARTESIAN_POINT('Ctrl Pts',(-54.7610765509181,-32.2356412320839,
-39.9085062640686));
#246408=CARTESIAN_POINT('Ctrl Pts',(-54.7066122033027,-32.391776105291,
-39.9392266524732));
#246409=CARTESIAN_POINT('Ctrl Pts',(-54.6514895234034,-32.547506073265,
-39.9674256651062));
#246410=CARTESIAN_POINT('Ctrl Pts',(-54.5925932920716,-32.7138968988899,
-39.9975551068242));
#246411=CARTESIAN_POINT('Ctrl Pts',(-54.5329450048582,-32.8798272445593,
-40.0248067697069));
#246412=CARTESIAN_POINT('Ctrl Pts',(-54.4725652945174,-33.045235666278,
-40.0491901836131));
#246413=CARTESIAN_POINT('Ctrl Pts',(-54.459998567761,-33.0796618406867,
-40.0542650622142));
#246414=CARTESIAN_POINT('Ctrl Pts',(-54.4476988874635,-33.1132505315278,
-40.0590994196371));
#246415=CARTESIAN_POINT('Ctrl Pts',(-54.4350351962782,-33.1477240550659,
-40.0639400649739));
#246416=CARTESIAN_POINT('Ctrl Pts',(-54.4297277455465,-33.1621721748955,
-40.0659688168014));
#246417=CARTESIAN_POINT('Ctrl Pts',(-54.4243561818974,-33.1767756701395,
-40.0679980885883));
#246418=CARTESIAN_POINT('Ctrl Pts',(-54.4188732977944,-33.1916610504326,
-40.0700434285701));
#246419=CARTESIAN_POINT('Ctrl Pts',(-54.4186927565832,-33.1921511984162,
-40.0701107778248));
#246420=CARTESIAN_POINT('Ctrl Pts',(-54.4185122071696,-33.192641346441,
-40.0701781023605));
#246421=CARTESIAN_POINT('Ctrl Pts',(-54.4183316495574,-33.193131494494,
-40.0702454021735));
#246422=CARTESIAN_POINT('Ctrl Pts',(-54.3216825238763,-33.455498614907,
-40.1062697381429));
#246423=CARTESIAN_POINT('Ctrl Pts',(-54.2227641565077,-33.7177318491769,
-40.1353601491472));
#246424=CARTESIAN_POINT('Ctrl Pts',(-54.1216389171421,-33.9795830238138,
-40.1573801871496));
#246425=CARTESIAN_POINT('Ctrl Pts',(-54.0207235880817,-34.2408906619379,
-40.1793545171475));
#246426=CARTESIAN_POINT('Ctrl Pts',(-53.9176105406912,-34.5018178209743,
-40.1942877778114));
#246427=CARTESIAN_POINT('Ctrl Pts',(-53.8123757322959,-34.7621244357644,
-40.202093896917));
#246428=CARTESIAN_POINT('Ctrl Pts',(-53.7030310371878,-35.0325971801243,
-40.2102048796478));
#246429=CARTESIAN_POINT('Ctrl Pts',(-53.5913955171586,-35.3023999113141,
-40.2106207756592));
#246430=CARTESIAN_POINT('Ctrl Pts',(-53.4775703714016,-35.571270916981,
-40.2033021049399));
#246431=CARTESIAN_POINT('Ctrl Pts',(-53.3681804343619,-35.8296653357723,
-40.1962686069911));
#246432=CARTESIAN_POINT('Ctrl Pts',(-53.2567682858326,-36.0871992674317,
-40.1820918925141));
#246433=CARTESIAN_POINT('Ctrl Pts',(-53.1434378897113,-36.3436472007061,
-40.160787752568));
#246434=CARTESIAN_POINT('Ctrl Pts',(-53.0300324555901,-36.6002649325572,
-40.1394695067853));
#246435=CARTESIAN_POINT('Ctrl Pts',(-52.9147062402528,-36.8557952264196,
-40.1110143971545));
#246436=CARTESIAN_POINT('Ctrl Pts',(-52.7975772000339,-37.1100188075254,
-40.075488166563));
#246437=CARTESIAN_POINT('Ctrl Pts',(-52.6802158407442,-37.3647466272557,
-40.0398914716284));
#246438=CARTESIAN_POINT('Ctrl Pts',(-52.5610445063604,-37.6181625450243,
-39.997195584507));
#246439=CARTESIAN_POINT('Ctrl Pts',(-52.4401955774352,-37.8700527012338,
-39.9475166832538));
#246440=CARTESIAN_POINT('Ctrl Pts',(-52.4259337762717,-37.8997791320335,
-39.9416539038482));
#246441=CARTESIAN_POINT('Ctrl Pts',(-52.411648626526,-37.9294843209584,
-39.9356939278134));
#246442=CARTESIAN_POINT('Ctrl Pts',(-52.3973403582526,-37.9591679226684,
-39.9296369918383));
#246443=CARTESIAN_POINT('Ctrl Pts',(-55.9280282803564,-28.4214833957092,
-38.6389054336786));
#246444=CARTESIAN_POINT('Ctrl Pts',(-56.2902455608578,-28.4766057597396,
-38.7328054198089));
#246445=CARTESIAN_POINT('Ctrl Pts',(-56.3309570935689,-28.3272991455305,
-39.0779244525544));
#246446=CARTESIAN_POINT('Ctrl Pts',(-55.9771522644365,-28.2367232142716,
-38.552803881023));
#246447=CARTESIAN_POINT('Ctrl Pts',(-56.3140818024757,-28.2791502561168,
-38.6345461846056));
#246448=CARTESIAN_POINT('Ctrl Pts',(-56.3829126567059,-28.1367558595196,
-38.9462184848765));
#246449=CARTESIAN_POINT('Ctrl Pts',(-56.0135219001012,-28.0528579818781,
-38.461315834925));
#246450=CARTESIAN_POINT('Ctrl Pts',(-56.3268630274838,-28.0775147348304,
-38.5284708636181));
#246451=CARTESIAN_POINT('Ctrl Pts',(-56.4167006885852,-27.9458326698372,
-38.8064076909433));
#246452=CARTESIAN_POINT('Ctrl Pts',(-56.0471103898057,-27.685962661452,
-38.2659355865592));
#246453=CARTESIAN_POINT('Ctrl Pts',(-56.3080000147378,-27.6770507033699,
-38.3033918191236));
#246454=CARTESIAN_POINT('Ctrl Pts',(-56.4275000344708,-27.560942607285,
-38.5081858145621));
#246455=CARTESIAN_POINT('Ctrl Pts',(-56.0452301422673,-27.5003069580262,
-38.1605763563824));
#246456=CARTESIAN_POINT('Ctrl Pts',(-56.2793394878168,-27.4741008831429,
-38.1827126614319));
#246457=CARTESIAN_POINT('Ctrl Pts',(-56.4055238530003,-27.3641600613333,
-38.3474070423507));
#246458=CARTESIAN_POINT('Ctrl Pts',(-56.0042558232646,-27.3241842272071,
-38.0522584541458));
#246459=CARTESIAN_POINT('Ctrl Pts',(-56.2039767728891,-27.2781673895146,
-38.0563752154928));
#246460=CARTESIAN_POINT('Ctrl Pts',(-56.3272010881867,-27.1739053137705,
-38.1827403312291));
#246461=CARTESIAN_POINT('',(-56.329970462594,-27.1806936516958,-38.1886113251078));
#246462=CARTESIAN_POINT('',(-56.3105671034289,-27.2343570385725,-38.1841758734895));
#246463=CARTESIAN_POINT('Ctrl Pts',(-56.3299705172648,-27.1806936804351,
-38.1886114231063));
#246464=CARTESIAN_POINT('Ctrl Pts',(-56.3269691615845,-27.189692744714,
-38.1876467081772));
#246465=CARTESIAN_POINT('Ctrl Pts',(-56.3238524112746,-27.1986710864456,
-38.186802403549));
#246466=CARTESIAN_POINT('Ctrl Pts',(-56.3173870154762,-27.2165616053026,
-38.1853313182445));
#246467=CARTESIAN_POINT('Ctrl Pts',(-56.3140355294396,-27.2254811086767,
-38.1847041131599));
#246468=CARTESIAN_POINT('Ctrl Pts',(-56.3105671034163,-27.2343570378499,
-38.1841758742811));
#246469=CARTESIAN_POINT('Ctrl Pts',(-56.3309570935689,-28.3272991455305,
-39.0779244525544));
#246470=CARTESIAN_POINT('Ctrl Pts',(-56.3461201068511,-28.2716898863449,
-39.039486617472));
#246471=CARTESIAN_POINT('Ctrl Pts',(-56.3593682732299,-28.2173779774047,
-39.0012762447384));
#246472=CARTESIAN_POINT('Ctrl Pts',(-56.3707008719059,-28.1643327425414,
-38.9633572404796));
#246473=CARTESIAN_POINT('Ctrl Pts',(-56.3824169834641,-28.1094923738794,
-38.9241549977484));
#246474=CARTESIAN_POINT('Ctrl Pts',(-56.3920860246955,-28.0560058960518,
-38.885264239361));
#246475=CARTESIAN_POINT('Ctrl Pts',(-56.399764516406,-28.0038471393053,
-38.8467574908829));
#246476=CARTESIAN_POINT('Ctrl Pts',(-56.4079112481125,-27.948507703726,
-38.805902572942));
#246477=CARTESIAN_POINT('Ctrl Pts',(-56.413817471714,-27.8946628690484,
-38.7654800016931));
#246478=CARTESIAN_POINT('Ctrl Pts',(-56.4176100874624,-27.8422896230681,
-38.7255774452514));
#246479=CARTESIAN_POINT('Ctrl Pts',(-56.4197909465699,-27.812173555936,
-38.7026323700314));
#246480=CARTESIAN_POINT('Ctrl Pts',(-56.4212739875461,-27.7825442284572,
-38.6798592538911));
#246481=CARTESIAN_POINT('Ctrl Pts',(-56.4220909106037,-27.753398352269,
-38.6572747578281));
#246482=CARTESIAN_POINT('Ctrl Pts',(-56.423134269861,-27.7161737697971,
-38.6284302506032));
#246483=CARTESIAN_POINT('Ctrl Pts',(-56.4231257094644,-27.679634330352,
-38.5998063072248));
#246484=CARTESIAN_POINT('Ctrl Pts',(-56.4220192345237,-27.6438642774849,
-38.5715055700834));
#246485=CARTESIAN_POINT('Ctrl Pts',(-56.420876952977,-27.6069366708922,
-38.5422889935433));
#246486=CARTESIAN_POINT('Ctrl Pts',(-56.4185647847815,-27.5708289824376,
-38.5134168402244));
#246487=CARTESIAN_POINT('Ctrl Pts',(-56.4150800085523,-27.5356115188146,
-38.4849833562604));
#246488=CARTESIAN_POINT('Ctrl Pts',(-56.4113982623776,-27.4984034591139,
-38.4549427269819));
#246489=CARTESIAN_POINT('Ctrl Pts',(-56.4064077337896,-27.4621890975008,
-38.4253917770801));
#246490=CARTESIAN_POINT('Ctrl Pts',(-56.4001551812337,-27.427027248806,
-38.3964211901481));
#246491=CARTESIAN_POINT('Ctrl Pts',(-56.3936726956335,-27.3905723488592,
-38.3663852310843));
#246492=CARTESIAN_POINT('Ctrl Pts',(-56.3858340302463,-27.3552486854546,
-38.336973041202));
#246493=CARTESIAN_POINT('Ctrl Pts',(-56.3767393875982,-27.3210976288266,
-38.3082647183813));
#246494=CARTESIAN_POINT('Ctrl Pts',(-56.3670679856636,-27.284780798367,
-38.2777357861724));
#246495=CARTESIAN_POINT('Ctrl Pts',(-56.3559765593455,-27.2497899684099,
-38.2480028279519));
#246496=CARTESIAN_POINT('Ctrl Pts',(-56.3436339365408,-27.2161491683113,
-38.2191392545631));
#246497=CARTESIAN_POINT('Ctrl Pts',(-56.3392349416417,-27.2041593578492,
-38.2088520802636));
#246498=CARTESIAN_POINT('Ctrl Pts',(-56.3346774134342,-27.1923408141125,
-38.1986751391635));
#246499=CARTESIAN_POINT('Ctrl Pts',(-56.3299702222398,-27.1806939286319,
-38.1886111170349));
#246500=CARTESIAN_POINT('',(-56.0373082460296,-27.7729550357457,-38.311656138237));
#246501=CARTESIAN_POINT('Ctrl Pts',(-56.0373052066298,-27.7730130613194,
-38.3116877705396));
#246502=CARTESIAN_POINT('Ctrl Pts',(-56.035646130788,-27.8046657328717,
-38.3289427060704));
#246503=CARTESIAN_POINT('Ctrl Pts',(-56.0333127894923,-27.8368271237374,
-38.3462766787704));
#246504=CARTESIAN_POINT('Ctrl Pts',(-56.0303381943686,-27.8694105448201,
-38.3636295168291));
#246505=CARTESIAN_POINT('Ctrl Pts',(-56.0286759911365,-27.8876181547931,
-38.3733262796857));
#246506=CARTESIAN_POINT('Ctrl Pts',(-56.0268051262239,-27.9059830603538,
-38.3830432285537));
#246507=CARTESIAN_POINT('Ctrl Pts',(-56.0247195628867,-27.9245020533413,
-38.3927754207108));
#246508=CARTESIAN_POINT('Ctrl Pts',(-56.0182865355039,-27.9816248397191,
-38.4227948679862));
#246509=CARTESIAN_POINT('Ctrl Pts',(-56.0098655697242,-28.0401765970223,
-38.4529489814088));
#246510=CARTESIAN_POINT('Ctrl Pts',(-55.9994204528404,-28.100180513741,
-38.4831776867009));
#246511=CARTESIAN_POINT('Ctrl Pts',(-55.9893894320084,-28.1578055786693,
-38.5122079767289));
#246512=CARTESIAN_POINT('Ctrl Pts',(-55.97749145665,-28.2167699428144,-38.54130703125));
#246513=CARTESIAN_POINT('Ctrl Pts',(-55.9637414575256,-28.2770983741972,
-38.5704249033626));
#246514=CARTESIAN_POINT('Ctrl Pts',(-55.9529641626647,-28.3243839985543,
-38.593247587978));
#246515=CARTESIAN_POINT('Ctrl Pts',(-55.9410499212476,-28.3725077114536,
-38.6160818879126));
#246516=CARTESIAN_POINT('Ctrl Pts',(-55.9280282803564,-28.4214833957092,
-38.6389054336786));
#246517=CARTESIAN_POINT('Ctrl Pts',(-56.3105671031579,-27.2343570385113,
-38.1841758742417));
#246518=CARTESIAN_POINT('Ctrl Pts',(-56.2731836457653,-27.3300237523219,
-38.1784823996949));
#246519=CARTESIAN_POINT('Ctrl Pts',(-56.22815914317,-27.425144703044,-38.1927583058393));
#246520=CARTESIAN_POINT('Ctrl Pts',(-56.1357812725437,-27.6032305524574,
-38.2400026082589));
#246521=CARTESIAN_POINT('Ctrl Pts',(-56.086002246048,-27.6908676735014,
-38.2742157055539));
#246522=CARTESIAN_POINT('Ctrl Pts',(-56.037313485634,-27.7728550057779,
-38.3116016074841));
#246523=CARTESIAN_POINT('Ctrl Pts',(-53.5049272332164,-45.5904441965002,
-27.0918908718704));
#246524=CARTESIAN_POINT('Ctrl Pts',(-53.2176708121394,-45.0562509145002,
-26.9551461919307));
#246525=CARTESIAN_POINT('Ctrl Pts',(-53.1622384417568,-44.6469455848382,
-27.4198764587519));
#246526=CARTESIAN_POINT('Ctrl Pts',(-53.3401376735643,-45.6078127141537,
-27.1200911635315));
#246527=CARTESIAN_POINT('Ctrl Pts',(-53.1337365804956,-45.0871086122264,
-27.0122080197638));
#246528=CARTESIAN_POINT('Ctrl Pts',(-53.063726008764,-44.7100871047333,
-27.4303518614045));
#246529=CARTESIAN_POINT('Ctrl Pts',(-53.1566042596039,-45.6113895454731,
-27.1349070389393));
#246530=CARTESIAN_POINT('Ctrl Pts',(-53.0245060734752,-45.1301223401293,
-27.0637831794719));
#246531=CARTESIAN_POINT('Ctrl Pts',(-52.9589297219542,-44.7746345958153,
-27.4136386124325));
#246532=CARTESIAN_POINT('Ctrl Pts',(-52.8631376063666,-45.5875376591559,
-27.1460905313543));
#246533=CARTESIAN_POINT('Ctrl Pts',(-52.8151221132255,-45.2071015764094,
-27.1155083247184));
#246534=CARTESIAN_POINT('Ctrl Pts',(-52.7848678380642,-44.9023469842384,
-27.3473769064844));
#246535=CARTESIAN_POINT('Ctrl Pts',(-52.762004727618,-45.5747306984873,
-27.1480089070401));
#246536=CARTESIAN_POINT('Ctrl Pts',(-52.73999642702,-45.2344272993809,-27.1285847238272));
#246537=CARTESIAN_POINT('Ctrl Pts',(-52.7241510212094,-44.9506058502004,
-27.317579614679));
#246538=CARTESIAN_POINT('Ctrl Pts',(-52.6073879775618,-45.5460939686536,
-27.1494556764823));
#246539=CARTESIAN_POINT('Ctrl Pts',(-52.6148381830911,-45.2827523418283,
-27.1414548626328));
#246540=CARTESIAN_POINT('Ctrl Pts',(-52.6220773103498,-45.0491834799539,
-27.263203350593));
#246541=CARTESIAN_POINT('Ctrl Pts',(-52.5551162511329,-45.5349159989873,
-27.1497020573719));
#246542=CARTESIAN_POINT('Ctrl Pts',(-52.5715747382081,-45.2994028420944,
-27.1446544886293));
#246543=CARTESIAN_POINT('Ctrl Pts',(-52.5864288471625,-45.0855251832409,
-27.243489825349));
#246544=CARTESIAN_POINT('Ctrl Pts',(-52.4764210340132,-45.5150283699019,
-27.1498873098043));
#246545=CARTESIAN_POINT('Ctrl Pts',(-52.5008596531919,-45.334079330316,
-27.1478520318169));
#246546=CARTESIAN_POINT('Ctrl Pts',(-52.5238148016628,-45.1638876910866,
-27.2098971119021));
#246547=CARTESIAN_POINT('Ctrl Pts',(-52.4501261696617,-45.5078812506388,
-27.149918608058));
#246548=CARTESIAN_POINT('Ctrl Pts',(-52.4766859109803,-45.3462185725822,
-27.1486382797322));
#246549=CARTESIAN_POINT('Ctrl Pts',(-52.5018689863788,-45.192276719095,
-27.198669824253));
#246550=CARTESIAN_POINT('Ctrl Pts',(-52.4105457516782,-45.4960245236483,
-27.1499421164755));
#246551=CARTESIAN_POINT('Ctrl Pts',(-52.4374156231595,-45.3700061187084,
-27.1494236542118));
#246552=CARTESIAN_POINT('Ctrl Pts',(-52.4634217751467,-45.2479034668112,
-27.1813235487131));
#246553=CARTESIAN_POINT('Ctrl Pts',(-52.397352190851,-45.4918856766869,
-27.1499460403929));
#246554=CARTESIAN_POINT('Ctrl Pts',(-52.4242270113872,-45.3778792225278,
-27.1496188303446));
#246555=CARTESIAN_POINT('Ctrl Pts',(-52.450381510263,-45.2667337504327,
-27.1756979157076));
#246556=CARTESIAN_POINT('Ctrl Pts',(-52.3776026724743,-45.4853183606142,
-27.1499490074433));
#246557=CARTESIAN_POINT('Ctrl Pts',(-52.4007513598026,-45.3991513814277,
-27.1498212851494));
#246558=CARTESIAN_POINT('Ctrl Pts',(-52.4235369397624,-45.3142904301389,
-27.1653223320967));
#246559=CARTESIAN_POINT('Ctrl Pts',(-52.3710211458483,-45.483069951052,
-27.1499495102509));
#246560=CARTESIAN_POINT('Ctrl Pts',(-52.392612848151,-45.4068824448819,
-27.1498709642282));
#246561=CARTESIAN_POINT('Ctrl Pts',(-52.4139394359862,-45.3315890395918,
-27.161969255845));
#246562=CARTESIAN_POINT('Ctrl Pts',(-52.3611723955272,-45.4795723115674,
-27.1499498834281));
#246563=CARTESIAN_POINT('Ctrl Pts',(-52.3791731661577,-45.4211953896253,
-27.1499196186609));
#246564=CARTESIAN_POINT('Ctrl Pts',(-52.3970410441707,-45.3632394127332,
-27.1572535611551));
#246565=CARTESIAN_POINT('Ctrl Pts',(-52.357893820504,-45.4783859538111,
-27.1499499446124));
#246566=CARTESIAN_POINT('Ctrl Pts',(-52.3744966404333,-45.4264035092904,
-27.1499315299618));
#246567=CARTESIAN_POINT('Ctrl Pts',(-52.3910025434165,-45.3747156667379,
-27.1557336710171));
#246568=CARTESIAN_POINT('Ctrl Pts',(-52.3529857957684,-45.4765600171004,
-27.1499499883959));
#246569=CARTESIAN_POINT('Ctrl Pts',(-52.3667871434141,-45.435788327086,
-27.1499431389266));
#246570=CARTESIAN_POINT('Ctrl Pts',(-52.3805378126143,-45.3951641548607,
-27.153605667294));
#246571=CARTESIAN_POINT('Ctrl Pts',(-52.3513512437753,-45.4759437807972,
-27.1499499950419));
#246572=CARTESIAN_POINT('Ctrl Pts',(-52.3640896356265,-45.439210366248,
-27.1499459628841));
#246573=CARTESIAN_POINT('Ctrl Pts',(-52.3767900903855,-45.4025844806719,
-27.1529187439664));
#246574=CARTESIAN_POINT('Ctrl Pts',(-52.3480894402565,-45.4746884282277,
-27.1499500007674));
#246575=CARTESIAN_POINT('Ctrl Pts',(-52.358361049002,-45.4467890388277,
-27.149949596787));
#246576=CARTESIAN_POINT('Ctrl Pts',(-52.3686148330815,-45.4189361333146,
-27.151673524296));
#246577=CARTESIAN_POINT('Ctrl Pts',(-52.3464615330207,-45.4740496677423,
-27.1499499999556));
#246578=CARTESIAN_POINT('Ctrl Pts',(-52.354091925022,-45.4531300726578,
-27.1499503254651));
#246579=CARTESIAN_POINT('Ctrl Pts',(-52.3621865654577,-45.4322306539423,
-27.1509264737703));
#246580=CARTESIAN_POINT('Ctrl Pts',(-52.34484211086,-45.473387463513,-27.149949999795));
#246581=CARTESIAN_POINT('Ctrl Pts',(-52.3544411585185,-45.4495909622675,
-27.1499505193682));
#246582=CARTESIAN_POINT('Ctrl Pts',(-52.3640275639789,-45.4258258009784,
-27.1512670021823));
#246583=CARTESIAN_POINT('',(-53.1622408850506,-44.6469488027857,-27.4198793594831));
#246584=CARTESIAN_POINT('Ctrl Pts',(-52.3451506921103,-45.473503287774,
-27.1499501432945));
#246585=CARTESIAN_POINT('Ctrl Pts',(-52.3820649490763,-45.3843464938679,
-27.1499647742885));
#246586=CARTESIAN_POINT('Ctrl Pts',(-52.4255740573844,-45.3010011843873,
-27.1640868107759));
#246587=CARTESIAN_POINT('Ctrl Pts',(-52.5068084427536,-45.1823953595046,
-27.2020720172523));
#246588=CARTESIAN_POINT('Ctrl Pts',(-52.53660370576,-45.1439054140081,-27.2175412386481));
#246589=CARTESIAN_POINT('Ctrl Pts',(-52.586580167937,-45.0869019409087,
-27.2442488546962));
#246590=CARTESIAN_POINT('Ctrl Pts',(-52.6041258972165,-45.0680161745429,
-27.2537272597621));
#246591=CARTESIAN_POINT('Ctrl Pts',(-52.631952259695,-45.0396571638826,
-27.2686754446952));
#246592=CARTESIAN_POINT('Ctrl Pts',(-52.6414789512766,-45.0301983315303,
-27.2737797996278));
#246593=CARTESIAN_POINT('Ctrl Pts',(-52.6610625104122,-45.0112249171893,
-27.2842080852999));
#246594=CARTESIAN_POINT('Ctrl Pts',(-52.6725722732524,-45.0003652292174,
-27.290294169548));
#246595=CARTESIAN_POINT('Ctrl Pts',(-52.7525080504857,-44.9263566788015,
-27.3322280681073));
#246596=CARTESIAN_POINT('Ctrl Pts',(-52.8274152663173,-44.8683372625527,
-27.3682550785334));
#246597=CARTESIAN_POINT('Ctrl Pts',(-52.9889951430861,-44.7566940244181,
-27.4166930620214));
#246598=CARTESIAN_POINT('Ctrl Pts',(-53.0756516339733,-44.7024568188154,
-27.4290805984111));
#246599=CARTESIAN_POINT('Ctrl Pts',(-53.1622384085562,-44.6469454777987,
-27.4198761157188));
#246600=CARTESIAN_POINT('Origin',(-53.6334240605191,-45.2802247659028,-28.0338316716305));
#246601=CARTESIAN_POINT('Ctrl Pts',(-54.1729863252367,-45.4155339669028,
-26.8184100191364));
#246602=CARTESIAN_POINT('Ctrl Pts',(-53.4948062719818,-45.0018366342789,
-26.6524889540493));
#246603=CARTESIAN_POINT('Ctrl Pts',(-53.5626783369365,-44.363661901133,
-27.1491860078999));
#246604=CARTESIAN_POINT('Ctrl Pts',(-54.0985832939867,-45.4543288404299,
-26.8878842623322));
#246605=CARTESIAN_POINT('Ctrl Pts',(-53.4663807315788,-44.9982803860136,
-26.6936892350566));
#246606=CARTESIAN_POINT('Ctrl Pts',(-53.5158499791776,-44.4021217230785,
-27.2295107442058));
#246607=CARTESIAN_POINT('Ctrl Pts',(-54.0039121656008,-45.4910386121189,
-26.9442182302923));
#246608=CARTESIAN_POINT('Ctrl Pts',(-53.4359975789415,-44.9961164351359,
-26.7410719889231));
#246609=CARTESIAN_POINT('Ctrl Pts',(-53.4577716218956,-44.446641152384,
-27.2926084953181));
#246610=CARTESIAN_POINT('Ctrl Pts',(-53.7733799776403,-45.5533648819636,
-27.0359103001593));
#246611=CARTESIAN_POINT('Ctrl Pts',(-53.3470483842575,-45.0123168742401,
-26.8487365913724));
#246612=CARTESIAN_POINT('Ctrl Pts',(-53.3195631540916,-44.544459526392,
-27.3849932634619));
#246613=CARTESIAN_POINT('Ctrl Pts',(-53.6402578408342,-45.5778984718822,
-27.0696657788991));
#246614=CARTESIAN_POINT('Ctrl Pts',(-53.2906043022484,-45.0299634766633,
-26.9058257418929));
#246615=CARTESIAN_POINT('Ctrl Pts',(-53.2410272830333,-44.5963709464781,
-27.4125980820349));
#246616=CARTESIAN_POINT('Ctrl Pts',(-53.4944417351013,-45.5914386672807,
-27.0936350023709));
#246617=CARTESIAN_POINT('Ctrl Pts',(-53.2121096349814,-45.0580990514851,
-26.9588617892535));
#246618=CARTESIAN_POINT('Ctrl Pts',(-53.1561130272964,-44.6507276720235,
-27.4206373946492));
#246619=CARTESIAN_POINT('',(-53.5592639447716,-44.3666367581605,-27.1547933762998));
#246620=CARTESIAN_POINT('Origin',(-54.427442714539,-44.7262215362818,-27.496793978795));
#246621=CARTESIAN_POINT('Ctrl Pts',(-53.1622457766273,-44.6469552539754,
-27.4198856202721));
#246622=CARTESIAN_POINT('Ctrl Pts',(-53.1829616413124,-44.6336777614326,
-27.4176857913189));
#246623=CARTESIAN_POINT('Ctrl Pts',(-53.203825483367,-44.620248346138,-27.4142375777492));
#246624=CARTESIAN_POINT('Ctrl Pts',(-53.2246773472487,-44.606676467706,
-27.4094115119876));
#246625=CARTESIAN_POINT('Ctrl Pts',(-53.2420734725691,-44.5953538301051,
-27.4053852606525));
#246626=CARTESIAN_POINT('Ctrl Pts',(-53.2594606276377,-44.5839326590593,
-27.4004000481084));
#246627=CARTESIAN_POINT('Ctrl Pts',(-53.276734970572,-44.5724432363545,
-27.3943871326634));
#246628=CARTESIAN_POINT('Ctrl Pts',(-53.2957250867575,-44.559812627312,
-27.3877769846915));
#246629=CARTESIAN_POINT('Ctrl Pts',(-53.3145785223172,-44.5470989704662,
-27.3799245457684));
#246630=CARTESIAN_POINT('Ctrl Pts',(-53.3331483702287,-44.5343766610789,
-27.3707499894093));
#246631=CARTESIAN_POINT('Ctrl Pts',(-53.3424332941844,-44.5280155063852,
-27.3661627112298));
#246632=CARTESIAN_POINT('Ctrl Pts',(-53.3516472121374,-44.5216527584649,
-27.361245110394));
#246633=CARTESIAN_POINT('Ctrl Pts',(-53.3607713708089,-44.5153011412843,
-27.3559885994396));
#246634=CARTESIAN_POINT('Ctrl Pts',(-53.3659497709643,-44.5116962921602,
-27.353005275922));
#246635=CARTESIAN_POINT('Ctrl Pts',(-53.3713666791296,-44.5079151244326,
-27.3497435082216));
#246636=CARTESIAN_POINT('Ctrl Pts',(-53.3765597693778,-44.504264785144,
-27.3464883543585));
#246637=CARTESIAN_POINT('Ctrl Pts',(-53.3805167212274,-44.5014833551844,
-27.3440080417733));
#246638=CARTESIAN_POINT('Ctrl Pts',(-53.3843446775867,-44.4987785077191,
-27.3415321022123));
#246639=CARTESIAN_POINT('Ctrl Pts',(-53.3878557727717,-44.4962946745248,
-27.339194797945));
#246640=CARTESIAN_POINT('Ctrl Pts',(-53.4040938620753,-44.4848074595393,
-27.3283852489511));
#246641=CARTESIAN_POINT('Ctrl Pts',(-53.4201817297529,-44.4732534524402,
-27.3162930153253));
#246642=CARTESIAN_POINT('Ctrl Pts',(-53.4359540056218,-44.4617216985649,
-27.3028611096342));
#246643=CARTESIAN_POINT('Ctrl Pts',(-53.4428340594993,-44.4566914106963,
-27.2970019529976));
#246644=CARTESIAN_POINT('Ctrl Pts',(-53.4498511634597,-44.4515321157807,
-27.2907002087151));
#246645=CARTESIAN_POINT('Ctrl Pts',(-53.4567248436233,-44.4464263008861,
-27.2841946017466));
#246646=CARTESIAN_POINT('Ctrl Pts',(-53.4636552526535,-44.4412783474158,
-27.2776353036402));
#246647=CARTESIAN_POINT('Ctrl Pts',(-53.4704396513325,-44.4361851635385,
-27.2708689417737));
#246648=CARTESIAN_POINT('Ctrl Pts',(-53.4768392779086,-44.4313447726754,
-27.2641606808037));
#246649=CARTESIAN_POINT('Ctrl Pts',(-53.4786432337058,-44.4299803413208,
-27.2622697257421));
#246650=CARTESIAN_POINT('Ctrl Pts',(-53.4804169154806,-44.428636041392,
-27.2603834997713));
#246651=CARTESIAN_POINT('Ctrl Pts',(-53.4821556626255,-44.4273163903631,
-27.2585081884501));
#246652=CARTESIAN_POINT('Ctrl Pts',(-53.4894649357621,-44.4217688960977,
-27.2506248324929));
#246653=CARTESIAN_POINT('Ctrl Pts',(-53.496801847095,-44.4161533979149,
-27.242244797274));
#246654=CARTESIAN_POINT('Ctrl Pts',(-53.5039434369036,-44.4106261624368,
-27.2335970890786));
#246655=CARTESIAN_POINT('Ctrl Pts',(-53.5105049481577,-44.4055478789221,
-27.2256517945201));
#246656=CARTESIAN_POINT('Ctrl Pts',(-53.5169020275297,-44.4005444852192,
-27.2174809284803));
#246657=CARTESIAN_POINT('Ctrl Pts',(-53.522998259727,-44.3957400324566,
-27.2092754392718));
#246658=CARTESIAN_POINT('Ctrl Pts',(-53.5256916414775,-44.393617372923,
-27.2056501648116));
#246659=CARTESIAN_POINT('Ctrl Pts',(-53.5282004467817,-44.3916302581029,
-27.2022014922256));
#246660=CARTESIAN_POINT('Ctrl Pts',(-53.5309532960349,-44.3894455369061,
-27.1983202529587));
#246661=CARTESIAN_POINT('Ctrl Pts',(-53.5333769026166,-44.387522109873,
-27.1949032125881));
#246662=CARTESIAN_POINT('Ctrl Pts',(-53.5359898668883,-44.3854453842273,
-27.191150857536));
#246663=CARTESIAN_POINT('Ctrl Pts',(-53.5390481116965,-44.3829894685758,
-27.1866366971472));
#246664=CARTESIAN_POINT('Ctrl Pts',(-53.5407261265692,-44.3816419430349,
-27.1841598423676));
#246665=CARTESIAN_POINT('Ctrl Pts',(-53.5425375417721,-44.3801802906758,
-27.1814534500025));
#246666=CARTESIAN_POINT('Ctrl Pts',(-53.5445179248843,-44.3785677202971,
-27.1784452999289));
#246667=CARTESIAN_POINT('Ctrl Pts',(-53.5486210827242,-44.3752266340442,
-27.1722127106478));
#246668=CARTESIAN_POINT('Ctrl Pts',(-53.5517998805691,-44.3725906371767,
-27.1671864609521));
#246669=CARTESIAN_POINT('Ctrl Pts',(-53.5541506530685,-44.3706553907933,
-27.1633939311691));
#246670=CARTESIAN_POINT('Ctrl Pts',(-53.556524588143,-44.3687010760866,
-27.1595640329225));
#246671=CARTESIAN_POINT('Ctrl Pts',(-53.5580541187007,-44.3674611371709,
-27.1569920294027));
#246672=CARTESIAN_POINT('Ctrl Pts',(-53.5587877855783,-44.3669315765437,
-27.1556906963517));
#246673=CARTESIAN_POINT('Ctrl Pts',(-53.5590432140006,-44.3667472083521,
-27.1552376331725));
#246674=CARTESIAN_POINT('Ctrl Pts',(-53.559201727648,-44.3666489657124,
-27.1549384692066));
#246675=CARTESIAN_POINT('Ctrl Pts',(-53.5592639447716,-44.3666367581605,
-27.1547933762998));
#246676=CARTESIAN_POINT('Ctrl Pts',(-53.559279935343,-44.3666167387913,
-27.1547738354693));
#246677=CARTESIAN_POINT('Ctrl Pts',(-53.4929150197559,-45.0016832826959,
-26.6555125209271));
#246678=CARTESIAN_POINT('Ctrl Pts',(-54.1676134446955,-45.4183137084154,
-26.8233719893975));
#246679=CARTESIAN_POINT('Ctrl Pts',(-53.759714509971,-44.159109532608,-26.8641791075324));
#246680=CARTESIAN_POINT('Ctrl Pts',(-53.6168204963237,-44.9093405275666,
-26.4380889960535));
#246681=CARTESIAN_POINT('Ctrl Pts',(-54.3266292023091,-45.3366816698438,
-26.6781230301639));
#246682=CARTESIAN_POINT('Ctrl Pts',(-53.9467562705573,-44.0476837299281,
-26.5065585291096));
#246683=CARTESIAN_POINT('Ctrl Pts',(-53.7163262343164,-44.9073871865944,
-26.1875635549992));
#246684=CARTESIAN_POINT('Ctrl Pts',(-54.4936741569865,-45.3076755243593,
-26.4992996221132));
#246685=CARTESIAN_POINT('Ctrl Pts',(-54.0990511533284,-44.0351983215918,
-26.1331099517669));
#246686=CARTESIAN_POINT('Ctrl Pts',(-53.7768128357869,-44.9677898415763,
-25.9705199042206));
#246687=CARTESIAN_POINT('Ctrl Pts',(-54.6449756149829,-45.3273946390668,
-26.3125400475463));
#246688=CARTESIAN_POINT('',(-53.559279935343,-44.3666167387913,-27.1547738354693));
#246689=CARTESIAN_POINT('Ctrl Pts',(-60.2219860711698,-29.2531258014113,
-26.1331099517669));
#246690=CARTESIAN_POINT('Ctrl Pts',(-60.6535709595361,-28.3658271140614,
-25.9705199042206));
#246691=CARTESIAN_POINT('Ctrl Pts',(-61.5217337387322,-28.7254319115519,
-26.3125400475463));
#246692=CARTESIAN_POINT('Ctrl Pts',(-60.1224375724058,-29.1357973637293,
-26.5091584767853));
#246693=CARTESIAN_POINT('Ctrl Pts',(-60.5674386476715,-28.3657673146916,
-26.1892157116101));
#246694=CARTESIAN_POINT('Ctrl Pts',(-61.3999932287862,-28.6317653934777,
-26.500551642367));
#246695=CARTESIAN_POINT('Ctrl Pts',(-60.0697340205019,-28.9211346043095,
-26.8686373631129));
#246696=CARTESIAN_POINT('Ctrl Pts',(-60.4987668584442,-28.2916785253826,
-26.4414259312258));
#246697=CARTESIAN_POINT('Ctrl Pts',(-61.3023268669242,-28.4910580092523,
-26.6804294767723));
#246698=CARTESIAN_POINT('Ctrl Pts',(-60.0746583928549,-28.6371017026725,
-27.1547738354693));
#246699=CARTESIAN_POINT('Ctrl Pts',(-60.4767911707101,-28.1411147611284,
-26.6555125209271));
#246700=CARTESIAN_POINT('Ctrl Pts',(-61.2484772015156,-28.3235963933842,
-26.8233719893975));
#246701=CARTESIAN_POINT('',(-60.0746608288527,-28.637079928768,-27.1547905454732));
#246702=CARTESIAN_POINT('',(-60.0745809376059,-28.6418766419159,-27.1499500046874));
#246703=CARTESIAN_POINT('Origin',(-60.9428211720509,-28.996706500163,-27.496793978795));
#246704=CARTESIAN_POINT('Ctrl Pts',(-60.844966001754,-27.666686296169,-27.1052376108796));
#246705=CARTESIAN_POINT('Ctrl Pts',(-60.2994052311052,-27.862800659529,
-26.9851894460117));
#246706=CARTESIAN_POINT('Ctrl Pts',(-59.9789660757281,-28.0995786058708,
-27.4232256967097));
#246707=CARTESIAN_POINT('Ctrl Pts',(-60.9625188062383,-27.8006555414775,
-27.0805352245546));
#246708=CARTESIAN_POINT('Ctrl Pts',(-60.3447014319684,-27.9607038681006,
-26.9244775354546));
#246709=CARTESIAN_POINT('Ctrl Pts',(-60.0056441485464,-28.2188680374461,
-27.4213854663284));
#246710=CARTESIAN_POINT('Ctrl Pts',(-61.0541543765889,-27.9302946525346,
-27.0441985004279));
#246711=CARTESIAN_POINT('Ctrl Pts',(-60.3764775334752,-28.0237347066717,
-26.858283774367));
#246712=CARTESIAN_POINT('Ctrl Pts',(-60.0281768266373,-28.3265373252776,
-27.3933984485104));
#246713=CARTESIAN_POINT('Ctrl Pts',(-61.1938025120114,-28.1730269430135,
-26.9370053822956));
#246714=CARTESIAN_POINT('Ctrl Pts',(-60.4367689858647,-28.1111042957933,
-26.7320775605175));
#246715=CARTESIAN_POINT('Ctrl Pts',(-60.0617095819124,-28.5222327395198,
-27.2855146773129));
#246716=CARTESIAN_POINT('Ctrl Pts',(-61.2391009664971,-28.2820540015562,
-26.8673782615866));
#246717=CARTESIAN_POINT('Ctrl Pts',(-60.4637526568036,-28.1314416114958,
-26.6767248536642));
#246718=CARTESIAN_POINT('Ctrl Pts',(-60.0722222978374,-28.6067470756235,
-27.2066250416898));
#246719=CARTESIAN_POINT('Ctrl Pts',(-61.2616496374058,-28.368733778436,
-26.7820215656129));
#246720=CARTESIAN_POINT('Ctrl Pts',(-60.4895512830636,-28.1510794068988,
-26.6321340393296));
#246721=CARTESIAN_POINT('Ctrl Pts',(-60.0775655158368,-28.6712003044384,
-27.1069552801944));
#246722=CARTESIAN_POINT('',(-59.9921334535065,-28.1581281070072,-27.4198788482142));
#246723=CARTESIAN_POINT('Origin',(-60.7731046378674,-28.043511085052,-28.0338316716305));
#246724=CARTESIAN_POINT('Ctrl Pts',(-60.0746608288527,-28.637079928768,
-27.1547905454732));
#246725=CARTESIAN_POINT('Ctrl Pts',(-60.0745597917545,-28.6368564728994,
-27.1552819564429));
#246726=CARTESIAN_POINT('Ctrl Pts',(-60.0743992696367,-28.635573735643,
-27.1570485778493));
#246727=CARTESIAN_POINT('Ctrl Pts',(-60.0741584639655,-28.6332063693261,
-27.1600818130461));
#246728=CARTESIAN_POINT('Ctrl Pts',(-60.0739199748378,-28.6308617770044,
-27.1630858686084));
#246729=CARTESIAN_POINT('Ctrl Pts',(-60.0736028577126,-28.6274531695012,
-27.1673324792244));
#246730=CARTESIAN_POINT('Ctrl Pts',(-60.0731533921911,-28.6229201453569,
-27.1727994271334));
#246731=CARTESIAN_POINT('Ctrl Pts',(-60.0729827771374,-28.6211994301504,
-27.1748746555242));
#246732=CARTESIAN_POINT('Ctrl Pts',(-60.0727927342046,-28.6193163369742,
-27.177125565431));
#246733=CARTESIAN_POINT('Ctrl Pts',(-60.072578963976,-28.6172662809877,
-27.1795502902216));
#246734=CARTESIAN_POINT('Ctrl Pts',(-60.0721368775343,-28.6130266730578,
-27.1845647300795));
#246735=CARTESIAN_POINT('Ctrl Pts',(-60.0717521348559,-28.6096020511089,
-27.188527632882));
#246736=CARTESIAN_POINT('Ctrl Pts',(-60.071415717113,-28.6066382940892,
-27.1919084760572));
#246737=CARTESIAN_POINT('Ctrl Pts',(-60.0710288730816,-28.603230293954,
-27.1957960801764));
#246738=CARTESIAN_POINT('Ctrl Pts',(-60.0707052101654,-28.6004306127975,
-27.1989138452128));
#246739=CARTESIAN_POINT('Ctrl Pts',(-60.0703847997515,-28.5976487042245,
-27.2019560952377));
#246740=CARTESIAN_POINT('Ctrl Pts',(-60.0701357660212,-28.5954865114892,
-27.2043206340894));
#246741=CARTESIAN_POINT('Ctrl Pts',(-60.0698879348767,-28.59333416891,-27.2066392349029));
#246742=CARTESIAN_POINT('Ctrl Pts',(-60.0695992250175,-28.5908999407258,
-27.2092316651229));
#246743=CARTESIAN_POINT('Ctrl Pts',(-60.0687200962936,-28.583487655174,
-27.2171256798202));
#246744=CARTESIAN_POINT('Ctrl Pts',(-60.0678153539134,-28.5761854144752,
-27.2245640965939));
#246745=CARTESIAN_POINT('Ctrl Pts',(-60.0668681916812,-28.568727145558,
-27.2318214504281));
#246746=CARTESIAN_POINT('Ctrl Pts',(-60.06592907555,-28.5613322343037,-27.2390171533641));
#246747=CARTESIAN_POINT('Ctrl Pts',(-60.0649484332206,-28.5537835801611,
-27.2460350541153));
#246748=CARTESIAN_POINT('Ctrl Pts',(-60.063873374386,-28.5457910961666,
-27.2531269287546));
#246749=CARTESIAN_POINT('Ctrl Pts',(-60.0636074376708,-28.543813999777,
-27.2548812419011));
#246750=CARTESIAN_POINT('Ctrl Pts',(-60.0633355367877,-28.5418096082398,
-27.2566399957809));
#246751=CARTESIAN_POINT('Ctrl Pts',(-60.0630564862275,-28.5397732639399,
-27.2584068206655));
#246752=CARTESIAN_POINT('Ctrl Pts',(-60.0605116265829,-28.5212023984059,
-27.2745197478142));
#246753=CARTESIAN_POINT('Ctrl Pts',(-60.0577294240748,-28.5021745059489,
-27.289270645353));
#246754=CARTESIAN_POINT('Ctrl Pts',(-60.054737528402,-28.4828917423689,
-27.3026952770944));
#246755=CARTESIAN_POINT('Ctrl Pts',(-60.0532415805655,-28.4732503605789,
-27.3094075929651));
#246756=CARTESIAN_POINT('Ctrl Pts',(-60.0516935979333,-28.4635449380373,
-27.3157886794781));
#246757=CARTESIAN_POINT('Ctrl Pts',(-60.0500992168557,-28.4537985636733,
-27.3218448706633));
#246758=CARTESIAN_POINT('Ctrl Pts',(-60.0491851062695,-28.4482106499004,
-27.3253170822642));
#246759=CARTESIAN_POINT('Ctrl Pts',(-60.0483032371289,-28.4429277771905,
-27.328501753937));
#246760=CARTESIAN_POINT('Ctrl Pts',(-60.0473767034212,-28.437407468587,
-27.3317127204619));
#246761=CARTESIAN_POINT('Ctrl Pts',(-60.0466871877869,-28.4332993189782,
-27.3341022844918));
#246762=CARTESIAN_POINT('Ctrl Pts',(-60.0459721797416,-28.4290592947978,
-27.3365060899411));
#246763=CARTESIAN_POINT('Ctrl Pts',(-60.0451838338097,-28.4244580371654,
-27.3390462004825));
#246764=CARTESIAN_POINT('Ctrl Pts',(-60.04122942221,-28.401377729628,-27.3517876153646));
#246765=CARTESIAN_POINT('Ctrl Pts',(-60.037005635401,-28.3778607369677,
-27.3629374174089));
#246766=CARTESIAN_POINT('Ctrl Pts',(-60.0325473374862,-28.3541327475903,
-27.372575464053));
#246767=CARTESIAN_POINT('Ctrl Pts',(-60.0280704554034,-28.330305849403,
-27.3822536863609));
#246768=CARTESIAN_POINT('Ctrl Pts',(-60.0233574971758,-28.3062666481107,
-27.3904078485879));
#246769=CARTESIAN_POINT('Ctrl Pts',(-60.018474744767,-28.2822058428692,
-27.3971390011105));
#246770=CARTESIAN_POINT('Ctrl Pts',(-60.0135217812117,-28.2577990572095,
-27.4039669437006));
#246771=CARTESIAN_POINT('Ctrl Pts',(-60.008394606897,-28.2333704035156,
-27.4093309698207));
#246772=CARTESIAN_POINT('Ctrl Pts',(-60.0031874462669,-28.2090737209063,
-27.4133524650949));
#246773=CARTESIAN_POINT('Ctrl Pts',(-59.9995313655727,-28.1920143984598,
-27.4161760598096));
#246774=CARTESIAN_POINT('Ctrl Pts',(-59.9958363978412,-28.1750191601907,
-27.4183381480339));
#246775=CARTESIAN_POINT('Ctrl Pts',(-59.992140178489,-28.1581271757,-27.4198841015071));
#246776=CARTESIAN_POINT('Ctrl Pts',(-59.9921300883295,-28.1581285421428,
-27.4198764587517));
#246777=CARTESIAN_POINT('Ctrl Pts',(-60.320749267504,-27.9079025729579,
-26.9551461919303));
#246778=CARTESIAN_POINT('Ctrl Pts',(-60.9016019229534,-27.7332918440739,
-27.0918908718699));
#246779=CARTESIAN_POINT('Ctrl Pts',(-59.9671190756674,-28.0438219358925,
-27.430351861608));
#246780=CARTESIAN_POINT('Ctrl Pts',(-60.2832184902842,-27.8267324213398,
-27.0122080197432));
#246781=CARTESIAN_POINT('Ctrl Pts',(-60.797359504462,-27.6044866323707,
-27.1200911635279));
#246782=CARTESIAN_POINT('Ctrl Pts',(-59.938658879413,-27.9240778021679,
-27.4136386124499));
#246783=CARTESIAN_POINT('Ctrl Pts',(-60.2363961568897,-27.7190794903775,
-27.0637831794859));
#246784=CARTESIAN_POINT('Ctrl Pts',(-60.6701109845517,-27.4721797090988,
-27.1349070389388));
#246785=CARTESIAN_POINT('Ctrl Pts',(-59.9058848368889,-27.7106911677997,
-27.3473769064724));
#246786=CARTESIAN_POINT('Ctrl Pts',(-60.1427718787375,-27.5165901322075,
-27.1155083247124));
#246787=CARTESIAN_POINT('Ctrl Pts',(-60.445732893452,-27.2815332790988,
-27.1460905313549));
#246788=CARTESIAN_POINT('Ctrl Pts',(-59.8970757353221,-27.633633723506,
-27.3175796146788));
#246789=CARTESIAN_POINT('Ctrl Pts',(-60.1089722005848,-27.4441460460438,
-27.1285847238195));
#246790=CARTESIAN_POINT('Ctrl Pts',(-60.3651652603529,-27.2190774234678,
-27.1480089070405));
#246791=CARTESIAN_POINT('Ctrl Pts',(-59.8946036326632,-27.4917517999077,
-27.2632033505944));
#246792=CARTESIAN_POINT('Ctrl Pts',(-60.0546429227938,-27.3214748378271,
-27.1414548626368));
#246793=CARTESIAN_POINT('Ctrl Pts',(-60.2355854820384,-27.1299960968794,
-27.1494556764824));
#246794=CARTESIAN_POINT('Ctrl Pts',(-59.8950938274304,-27.4408470650292,
-27.2434898253561));
#246795=CARTESIAN_POINT('Ctrl Pts',(-60.0358247291844,-27.2791092809321,
-27.1446544886278));
#246796=CARTESIAN_POINT('Ctrl Pts',(-60.1907197716695,-27.1009384228054,
-27.1497020573719));
#246797=CARTESIAN_POINT('Ctrl Pts',(-59.9062296719677,-27.3411615881386,
-27.2098971118952));
#246798=CARTESIAN_POINT('Ctrl Pts',(-60.0103415930171,-27.2045861847983,
-27.1478520318177));
#246799=CARTESIAN_POINT('Ctrl Pts',(-60.1210111726076,-27.0593551785227,
-27.1498873098043));
#246800=CARTESIAN_POINT('Ctrl Pts',(-59.9107857113893,-27.3055694790947,
-27.198669824241));
#246801=CARTESIAN_POINT('Ctrl Pts',(-60.001831916504,-27.1789090272168,
-27.148638279731));
#246802=CARTESIAN_POINT('Ctrl Pts',(-60.0973641192197,-27.0458156781241,
-27.149918608058));
#246803=CARTESIAN_POINT('Ctrl Pts',(-59.9229334781053,-27.2390491448428,
-27.1813235487183));
#246804=CARTESIAN_POINT('Ctrl Pts',(-59.9908839648439,-27.1343204052552,
-27.1494236542124));
#246805=CARTESIAN_POINT('Ctrl Pts',(-60.0609925652013,-27.0262120682258,
-27.1499421164754));
#246806=CARTESIAN_POINT('Ctrl Pts',(-59.9270276396052,-27.2165132639013,
-27.1756979157175));
#246807=CARTESIAN_POINT('Ctrl Pts',(-59.9871253331188,-27.1194275233503,
-27.1496188303448));
#246808=CARTESIAN_POINT('Ctrl Pts',(-60.0487367021204,-27.0198094186492,
-27.1499460403929));
#246809=CARTESIAN_POINT('Ctrl Pts',(-59.941673312503,-27.1639036353,-27.1653223320947));
#246810=CARTESIAN_POINT('Ctrl Pts',(-59.9855672285123,-27.0877860430869,
-27.1498212851493));
#246811=CARTESIAN_POINT('Ctrl Pts',(-60.030127890022,-27.0104881940086,
-27.1499490074433));
#246812=CARTESIAN_POINT('Ctrl Pts',(-59.9471188165433,-27.1448852112603,
-27.1619692558456));
#246813=CARTESIAN_POINT('Ctrl Pts',(-59.9852791191255,-27.0765645589215,
-27.1498709642282));
#246814=CARTESIAN_POINT('Ctrl Pts',(-60.0238841822655,-27.0074242175497,
-27.1499495102509));
#246815=CARTESIAN_POINT('Ctrl Pts',(-59.9575500425786,-27.1105560503329,
-27.1572535611545));
#246816=CARTESIAN_POINT('Ctrl Pts',(-59.98589660914,-27.0569404883559,-27.149919618661));
#246817=CARTESIAN_POINT('Ctrl Pts',(-60.0144468595299,-27.0029333040085,
-27.1499498834281));
#246818=CARTESIAN_POINT('Ctrl Pts',(-59.9613951148011,-27.0981712484174,
-27.1557336710108));
#246819=CARTESIAN_POINT('Ctrl Pts',(-59.9862725028326,-27.0499509885438,
-27.1499315299619));
#246820=CARTESIAN_POINT('Ctrl Pts',(-60.0112896752839,-27.0014538829912,
-27.1499499446124));
#246821=CARTESIAN_POINT('Ctrl Pts',(-59.9684546972765,-27.0763123017486,
-27.1536056672944));
#246822=CARTESIAN_POINT('Ctrl Pts',(-59.9874571335005,-27.0378634826494,
-27.1499431389266));
#246823=CARTESIAN_POINT('Ctrl Pts',(-60.0065280454809,-26.999274517649,
-27.1499499883959));
#246824=CARTESIAN_POINT('Ctrl Pts',(-59.9710516202097,-27.0684152991668,
-27.1529187439602));
#246825=CARTESIAN_POINT('Ctrl Pts',(-59.9879694545663,-27.0335363094633,
-27.149945962884));
#246826=CARTESIAN_POINT('Ctrl Pts',(-60.0049364978137,-26.9985544597188,
-27.1499499950418));
#246827=CARTESIAN_POINT('Ctrl Pts',(-59.9768332047617,-27.0510721549069,
-27.1516735242969));
#246828=CARTESIAN_POINT('Ctrl Pts',(-59.9892776628721,-27.0241266562837,
-27.149949596787));
#246829=CARTESIAN_POINT('Ctrl Pts',(-60.001742386112,-26.9971356846468,
-27.1499500007674));
#246830=CARTESIAN_POINT('Ctrl Pts',(-59.9816883788974,-27.0371260374492,
-27.1509264737607));
#246831=CARTESIAN_POINT('Ctrl Pts',(-59.9907427244201,-27.0166241416866,
-27.1499503254652));
#246832=CARTESIAN_POINT('Ctrl Pts',(-60.0001396099956,-26.9964362522719,
-27.1499499999556));
#246833=CARTESIAN_POINT('Ctrl Pts',(-59.9784612462896,-27.0429567353391,
-27.1512670021965));
#246834=CARTESIAN_POINT('Ctrl Pts',(-59.9884871407403,-27.0193736162006,
-27.1499505193683));
#246835=CARTESIAN_POINT('Ctrl Pts',(-59.998526256503,-26.9957593969819,
-27.149949999795));
#246836=CARTESIAN_POINT('Ctrl Pts',(-59.9921299933151,-28.1581286133368,
-27.4198761139792));
#246837=CARTESIAN_POINT('Ctrl Pts',(-59.9701579252025,-28.0576651497413,
-27.4290779346156));
#246838=CARTESIAN_POINT('Ctrl Pts',(-59.9472412910225,-27.9580348996117,
-27.4166918460736));
#246839=CARTESIAN_POINT('Ctrl Pts',(-59.9207601538973,-27.8131235425062,
-27.3803603832272));
#246840=CARTESIAN_POINT('Ctrl Pts',(-59.9132588707421,-27.7653999402845,
-27.365309683848));
#246841=CARTESIAN_POINT('Ctrl Pts',(-59.9047658007748,-27.6938927948674,
-27.3402656049488));
#246842=CARTESIAN_POINT('Ctrl Pts',(-59.9023893111735,-27.6700639391975,
-27.3315068947973));
#246843=CARTESIAN_POINT('Ctrl Pts',(-59.8995467614903,-27.6341899840966,
-27.3180027950516));
#246844=CARTESIAN_POINT('Ctrl Pts',(-59.8987191770273,-27.6222100030513,
-27.3134404804139));
#246845=CARTESIAN_POINT('Ctrl Pts',(-59.8973051909472,-27.5981804781832,
-27.3042363771492));
#246846=CARTESIAN_POINT('Ctrl Pts',(-59.8967949914569,-27.588104634047,
-27.3003548689801));
#246847=CARTESIAN_POINT('Ctrl Pts',(-59.8919058191163,-27.4614630196987,
-27.2515720110604));
#246848=CARTESIAN_POINT('Ctrl Pts',(-59.8984591636505,-27.363138339122,
-27.2147413151307));
#246849=CARTESIAN_POINT('Ctrl Pts',(-59.9337022752968,-27.1747284561612,
-27.1640852704678));
#246850=CARTESIAN_POINT('Ctrl Pts',(-59.9618895982155,-27.0850253725664,
-27.1499500046719));
#246851=CARTESIAN_POINT('Ctrl Pts',(-59.9987583566445,-26.9958774289692,
-27.1499500000015));
#246852=CARTESIAN_POINT('Ctrl Pts',(-51.0753935148582,-44.2778743810374,
-38.2852384570399));
#246853=CARTESIAN_POINT('Ctrl Pts',(-51.221272714641,-44.0620551258768,
-38.2881244881786));
#246854=CARTESIAN_POINT('Ctrl Pts',(-51.322393361958,-43.857597022718,-38.4139756691106));
#246855=CARTESIAN_POINT('Ctrl Pts',(-50.5589168178961,-43.9265466949758,
-38.1296723017668));
#246856=CARTESIAN_POINT('Ctrl Pts',(-50.70387613966,-43.7144228107189,-38.13287636152));
#246857=CARTESIAN_POINT('Ctrl Pts',(-50.804491208013,-43.5123432497905,
-38.2555902237865));
#246858=CARTESIAN_POINT('Ctrl Pts',(-50.0437957213916,-43.5725655138355,
-37.9740538460248));
#246859=CARTESIAN_POINT('Ctrl Pts',(-50.18735261211,-43.3638960195065,-37.9774448600074));
#246860=CARTESIAN_POINT('Ctrl Pts',(-50.2878807263347,-43.164578596265,
-38.0971582664596));
#246861=CARTESIAN_POINT('Ctrl Pts',(-49.530715885079,-43.2159674697984,
-37.8185383057006));
#246862=CARTESIAN_POINT('Ctrl Pts',(-49.6723958234993,-43.010504571894,
-37.8219861814962));
#246863=CARTESIAN_POINT('Ctrl Pts',(-49.7732408306752,-42.814351716493,
-37.9388383832698));
#246864=CARTESIAN_POINT('',(-49.8728085526386,-42.8820630203836,-37.9694624807979));
#246865=CARTESIAN_POINT('Ctrl Pts',(-51.3131710686973,-43.8514487258803,
-38.411155249868));
#246866=CARTESIAN_POINT('Ctrl Pts',(-50.8316561824108,-43.5304148924606,
-38.2638929263568));
#246867=CARTESIAN_POINT('Ctrl Pts',(-50.3514791746876,-43.2073574749185,
-38.1166580156441));
#246868=CARTESIAN_POINT('Ctrl Pts',(-49.8728085497775,-42.8820630221025,
-37.9694624863033));
#246869=CARTESIAN_POINT('',(-49.5640573010087,-43.2391345629747,-37.8286434305113));
#246870=CARTESIAN_POINT('Ctrl Pts',(-49.5640573010554,-43.2391345629941,
-37.8286434303062));
#246871=CARTESIAN_POINT('Ctrl Pts',(-49.8494633692686,-43.3573536272316,
-37.904735709135));
#246872=CARTESIAN_POINT('Ctrl Pts',(-50.135471903199,-43.4758222409351,
-37.9876583178626));
#246873=CARTESIAN_POINT('Ctrl Pts',(-50.6978706344543,-43.7087754228824,
-38.1635076732467));
#246874=CARTESIAN_POINT('Ctrl Pts',(-50.9785707207733,-43.8250452056,-38.257673825788));
#246875=CARTESIAN_POINT('Ctrl Pts',(-51.2549749806985,-43.9395355987587,
-38.3573338134652));
#246876=CARTESIAN_POINT('',(-49.5398530052707,-43.2223193698252,-37.8213061206858));
#246877=CARTESIAN_POINT('',(-49.5398418208422,-43.2223097035821,-37.82130434093));
#246878=CARTESIAN_POINT('Ctrl Pts',(-49.8728085512757,-42.8820630232987,
-37.969462486706));
#246879=CARTESIAN_POINT('Ctrl Pts',(-49.835317068268,-42.9487641223396,
-37.9279035533955));
#246880=CARTESIAN_POINT('Ctrl Pts',(-49.7850972385136,-43.010927571904,
-37.8943460529194));
#246881=CARTESIAN_POINT('Ctrl Pts',(-49.6691607843692,-43.1241681864113,
-37.8451396851236));
#246882=CARTESIAN_POINT('Ctrl Pts',(-49.6055190626502,-43.1745010780307,
-37.8290666430855));
#246883=CARTESIAN_POINT('Ctrl Pts',(-49.5398550048227,-43.2223190381248,
-37.8213083592913));
#246884=CARTESIAN_POINT('Ctrl Pts',(-56.0567428479854,-26.4451399126818,
-36.7328353710964));
#246885=CARTESIAN_POINT('Ctrl Pts',(-56.9256533237087,-26.804455625982,
-37.0750745754352));
#246886=CARTESIAN_POINT('Ctrl Pts',(-56.5501269894349,-27.7316757551251,
-37.0532039630469));
#246887=CARTESIAN_POINT('Ctrl Pts',(-56.0161159413416,-26.4316774197765,
-36.8592602097566));
#246888=CARTESIAN_POINT('Ctrl Pts',(-56.8812242910574,-26.792771568599,
-37.2001343692902));
#246889=CARTESIAN_POINT('Ctrl Pts',(-56.4634891944676,-27.7025207485233,
-37.3037739683117));
#246890=CARTESIAN_POINT('Ctrl Pts',(-55.9865950568036,-26.3938324397214,
-36.9856616450977));
#246891=CARTESIAN_POINT('Ctrl Pts',(-56.8463391109411,-26.7573474025772,
-37.3259290836403));
#246892=CARTESIAN_POINT('Ctrl Pts',(-56.3975727115578,-27.6239813543799,
-37.5536697174369));
#246893=CARTESIAN_POINT('Ctrl Pts',(-55.9639108205415,-26.3064676587972,
-37.1605584951606));
#246894=CARTESIAN_POINT('Ctrl Pts',(-56.8116611688153,-26.6724967553174,
-37.5031641308945));
#246895=CARTESIAN_POINT('Ctrl Pts',(-56.3372700934347,-27.4430605475982,
-37.8969608391351));
#246896=CARTESIAN_POINT('Ctrl Pts',(-55.9598677494703,-26.2742284930919,
-37.2140109224323));
#246897=CARTESIAN_POINT('Ctrl Pts',(-56.8032368383072,-26.6410057827481,
-37.5576570896612));
#246898=CARTESIAN_POINT('Ctrl Pts',(-56.3237384842937,-27.3763245447103,
-38.0014758126155));
#246899=CARTESIAN_POINT('Ctrl Pts',(-55.9584332691836,-26.2015366731774,
-37.3161182781239));
#246900=CARTESIAN_POINT('Ctrl Pts',(-56.7915392176745,-26.5690973896552,
-37.6629529996084));
#246901=CARTESIAN_POINT('Ctrl Pts',(-56.3079807609824,-27.2255973278124,
-38.1999509624373));
#246902=CARTESIAN_POINT('Ctrl Pts',(-55.9611416957481,-26.1605953720209,
-37.3652108762889));
#246903=CARTESIAN_POINT('Ctrl Pts',(-56.7882693648106,-26.5282588226261,
-37.7141900108042));
#246904=CARTESIAN_POINT('Ctrl Pts',(-56.3058507535083,-27.1405858754377,
-38.2947398804766));
#246905=CARTESIAN_POINT('Ctrl Pts',(-55.9735854550226,-26.0733128348902,
-37.4552148376231));
#246906=CARTESIAN_POINT('Ctrl Pts',(-56.787283226926,-26.4397664909511,
-37.8097324411522));
#246907=CARTESIAN_POINT('Ctrl Pts',(-56.3133653432169,-26.9588185181872,
-38.4667780711462));
#246908=CARTESIAN_POINT('Ctrl Pts',(-55.9832537988535,-26.0268975082167,
-37.4964217183786));
#246909=CARTESIAN_POINT('Ctrl Pts',(-56.7894489037504,-26.3921445172251,
-37.8543040547116));
#246910=CARTESIAN_POINT('Ctrl Pts',(-56.3228479854743,-26.8619028223475,
-38.5446064466135));
#246911=CARTESIAN_POINT('Ctrl Pts',(-56.0096187269497,-25.9285721559953,
-37.5713719240169));
#246912=CARTESIAN_POINT('Ctrl Pts',(-56.7994567234388,-26.2891407664831,
-37.93719686714));
#246913=CARTESIAN_POINT('Ctrl Pts',(-56.3532675293309,-26.6560036746519,
-38.6838766227473));
#246914=CARTESIAN_POINT('Ctrl Pts',(-56.0264911179296,-25.876428712841,
-37.6051403493443));
#246915=CARTESIAN_POINT('Ctrl Pts',(-56.8073578500169,-26.2335499771157,
-37.975588088565));
#246916=CARTESIAN_POINT('Ctrl Pts',(-56.3744282312934,-26.5465004149421,
-38.745296875714));
#246917=CARTESIAN_POINT('Ctrl Pts',(-56.0847411249187,-25.7176419731692,
-37.6904448613398));
#246918=CARTESIAN_POINT('Ctrl Pts',(-56.8397912948059,-26.061143575332,
-38.0745256106056));
#246919=CARTESIAN_POINT('Ctrl Pts',(-56.4527962216696,-26.2131202154147,
-38.896893054692));
#246920=CARTESIAN_POINT('Ctrl Pts',(-56.1352426205228,-25.6049974448028,
-37.7283114705867));
#246921=CARTESIAN_POINT('Ctrl Pts',(-56.8741681320632,-25.932461502415,
-38.1225595342041));
#246922=CARTESIAN_POINT('Ctrl Pts',(-56.5266192379674,-25.9765570154852,
-38.9582311572884));
#246923=CARTESIAN_POINT('Ctrl Pts',(-56.1839719359073,-25.4898819665406,
-37.7383677470617));
#246924=CARTESIAN_POINT('Ctrl Pts',(-56.9226955196534,-25.8032369518573,
-38.135248020605));
#246925=CARTESIAN_POINT('Ctrl Pts',(-56.6168337454475,-25.7433245796562,
-38.9744601000404));
#246926=CARTESIAN_POINT('',(-56.5352472331774,-27.7260285737871,-37.0969113483379));
#246927=CARTESIAN_POINT('',(-56.0497678863462,-26.4425442437853,-36.7548912050127));
#246928=CARTESIAN_POINT('Origin',(-55.6670844539814,-27.3664237762966,-36.7548912050122));
#246929=CARTESIAN_POINT('',(-56.1804995572509,-25.4980753298431,-37.7376053587295));
#246930=CARTESIAN_POINT('Ctrl Pts',(-56.1804996992808,-25.4980753614798,
-37.7376050690768));
#246931=CARTESIAN_POINT('Ctrl Pts',(-56.1721547081557,-25.517745210166,
-37.7356615392445));
#246932=CARTESIAN_POINT('Ctrl Pts',(-56.1633474000913,-25.5383093620459,
-37.7328132500983));
#246933=CARTESIAN_POINT('Ctrl Pts',(-56.1541372930473,-25.5597695621204,
-37.7288569014977));
#246934=CARTESIAN_POINT('Ctrl Pts',(-56.1514769713159,-25.5659682996971,
-37.7277141178026));
#246935=CARTESIAN_POINT('Ctrl Pts',(-56.1487833323961,-25.5722416757009,
-37.7264788095946));
#246936=CARTESIAN_POINT('Ctrl Pts',(-56.1460585738842,-25.5785894156077,
-37.725145914588));
#246937=CARTESIAN_POINT('Ctrl Pts',(-56.1399796001049,-25.5927513107933,
-37.7221722074649));
#246938=CARTESIAN_POINT('Ctrl Pts',(-56.133753323915,-25.6072872660305,
-37.7187172178508));
#246939=CARTESIAN_POINT('Ctrl Pts',(-56.127401266824,-25.6221863641009,
-37.7147184532386));
#246940=CARTESIAN_POINT('Ctrl Pts',(-56.1242252382785,-25.6296359131361,
-37.7127190709326));
#246941=CARTESIAN_POINT('Ctrl Pts',(-56.121017807697,-25.6371762469106,
-37.7105836624425));
#246942=CARTESIAN_POINT('Ctrl Pts',(-56.117782435604,-25.6448052112892,
-37.7083042395931));
#246943=CARTESIAN_POINT('Ctrl Pts',(-56.1161647495575,-25.6486196934784,
-37.7071645281684));
#246944=CARTESIAN_POINT('Ctrl Pts',(-56.1145400807257,-25.6524563334436,
-37.7059888081935));
#246945=CARTESIAN_POINT('Ctrl Pts',(-56.1129088768668,-25.6563148191995,
-37.704776053173));
#246946=CARTESIAN_POINT('Ctrl Pts',(-56.1119212824668,-25.6586508968786,
-37.7040418040107));
#246947=CARTESIAN_POINT('Ctrl Pts',(-56.1106283545974,-25.6617120181857,
-37.7030640373722));
#246948=CARTESIAN_POINT('Ctrl Pts',(-56.1095810891675,-25.6641951359811,
-37.7022571329218));
#246949=CARTESIAN_POINT('Ctrl Pts',(-56.1088985924495,-25.6658133692363,
-37.7017312780396));
#246950=CARTESIAN_POINT('Ctrl Pts',(-56.1083201206434,-25.667186413911,
-37.7012794811119));
#246951=CARTESIAN_POINT('Ctrl Pts',(-56.1079961185751,-25.6679554802017,
-37.7010256371487));
#246952=CARTESIAN_POINT('Ctrl Pts',(-56.1047114345681,-25.6757521580389,
-37.6984522054096));
#246953=CARTESIAN_POINT('Ctrl Pts',(-56.1008359754091,-25.6849538000702,
-37.6952903021413));
#246954=CARTESIAN_POINT('Ctrl Pts',(-56.0964078629411,-25.6955756054257,
-37.6913867676171));
#246955=CARTESIAN_POINT('Ctrl Pts',(-56.0919797504732,-25.7061974107812,
-37.687483233093));
#246956=CARTESIAN_POINT('Ctrl Pts',(-56.0869979055547,-25.7182397591171,
-37.6828377562645));
#246957=CARTESIAN_POINT('Ctrl Pts',(-56.0815361707356,-25.7316992647335,
-37.6772557977095));
#246958=CARTESIAN_POINT('Ctrl Pts',(-56.0767092572323,-25.7435943624561,
-37.6723226341605));
#246959=CARTESIAN_POINT('Ctrl Pts',(-56.0714975515571,-25.7565942408721,
-37.6666519605074));
#246960=CARTESIAN_POINT('Ctrl Pts',(-56.0659762650254,-25.7706842877089,
-37.6600785155475));
#246961=CARTESIAN_POINT('Ctrl Pts',(-56.0621264069709,-25.7805089327426,
-37.6554950131556));
#246962=CARTESIAN_POINT('Ctrl Pts',(-56.0581267025653,-25.7908632519376,
-37.6504721261128));
#246963=CARTESIAN_POINT('Ctrl Pts',(-56.0540156952128,-25.8017372274691,
-37.6449482157837));
#246964=CARTESIAN_POINT('Ctrl Pts',(-56.0523569770774,-25.8061246826281,
-37.6427194165004));
#246965=CARTESIAN_POINT('Ctrl Pts',(-56.0505076302188,-25.811057589218,
-37.6401707669867));
#246966=CARTESIAN_POINT('Ctrl Pts',(-56.0487318534611,-25.8158450653948,
-37.637648186208));
#246967=CARTESIAN_POINT('Ctrl Pts',(-56.0477552145813,-25.8184780739365,
-37.6362608212391));
#246968=CARTESIAN_POINT('Ctrl Pts',(-56.0468004020449,-25.8210673534648,
-37.6348821415423));
#246969=CARTESIAN_POINT('Ctrl Pts',(-56.0459080583341,-25.8234999233763,
-37.6335753185341));
#246970=CARTESIAN_POINT('Ctrl Pts',(-56.045160120874,-25.8255388352205,
-37.6324799761569));
#246971=CARTESIAN_POINT('Ctrl Pts',(-56.0444554474835,-25.8274690560493,
-37.6314343381085));
#246972=CARTESIAN_POINT('Ctrl Pts',(-56.0438170325454,-25.8292240855981,
-37.6304777193087));
#246973=CARTESIAN_POINT('Ctrl Pts',(-56.0362567591205,-25.8500075956098,
-37.6191491941467));
#246974=CARTESIAN_POINT('Ctrl Pts',(-56.02931845791,-25.8701426530822,-37.6073098766025));
#246975=CARTESIAN_POINT('Ctrl Pts',(-56.0229752198237,-25.8895467790827,
-37.5951388123388));
#246976=CARTESIAN_POINT('Ctrl Pts',(-56.0162785047191,-25.9100322002368,
-37.5822895153734));
#246977=CARTESIAN_POINT('Ctrl Pts',(-56.0102448833575,-25.9297031511995,
-37.5690703868155));
#246978=CARTESIAN_POINT('Ctrl Pts',(-56.0048282449515,-25.9484996069876,
-37.5556484966893));
#246979=CARTESIAN_POINT('Ctrl Pts',(-56.0019374570599,-25.9585310255028,
-37.5484854124016));
#246980=CARTESIAN_POINT('Ctrl Pts',(-55.9992221728258,-25.9683139641521,
-37.5412638620756));
#246981=CARTESIAN_POINT('Ctrl Pts',(-55.9966740556322,-25.9778429475711,
-37.534004721751));
#246982=CARTESIAN_POINT('Ctrl Pts',(-55.9951913800419,-25.9833875870214,
-37.5297808382527));
#246983=CARTESIAN_POINT('Ctrl Pts',(-55.9937630386758,-25.9888492806145,
-37.5255438327704));
#246984=CARTESIAN_POINT('Ctrl Pts',(-55.9923857319884,-25.9942300976549,
-37.5212950898624));
#246985=CARTESIAN_POINT('Ctrl Pts',(-55.9880037727898,-26.011349393555,
-37.5077775354653));
#246986=CARTESIAN_POINT('Ctrl Pts',(-55.9842072046152,-26.0274324169427,
-37.4943285285434));
#246987=CARTESIAN_POINT('Ctrl Pts',(-55.9808899258191,-26.0426836271918,
-37.4809469087161));
#246988=CARTESIAN_POINT('Ctrl Pts',(-55.9774338122668,-26.0585731311112,
-37.4670052413193));
#246989=CARTESIAN_POINT('Ctrl Pts',(-55.974498085135,-26.0735596866835,
-37.4531366392436));
#246990=CARTESIAN_POINT('Ctrl Pts',(-55.9719986222037,-26.087847946888,
-37.4393035224131));
#246991=CARTESIAN_POINT('Ctrl Pts',(-55.9702448851522,-26.0978732411258,
-37.4295975774998));
#246992=CARTESIAN_POINT('Ctrl Pts',(-55.9687066805805,-26.1075541977658,
-37.4199083357066));
#246993=CARTESIAN_POINT('Ctrl Pts',(-55.9673642825326,-26.1169544197451,
-37.4102131602444));
#246994=CARTESIAN_POINT('Ctrl Pts',(-55.9672678347631,-26.1176298009733,
-37.4095165873842));
#246995=CARTESIAN_POINT('Ctrl Pts',(-55.9671724168607,-26.1183037484222,
-37.4088199099095));
#246996=CARTESIAN_POINT('Ctrl Pts',(-55.9670780227245,-26.1189762775923,
-37.4081231265292));
#246997=CARTESIAN_POINT('Ctrl Pts',(-55.9648434489261,-26.1348969281966,
-37.3916283107813));
#246998=CARTESIAN_POINT('Ctrl Pts',(-55.9630287311143,-26.1509346460944,
-37.3741059408746));
#246999=CARTESIAN_POINT('Ctrl Pts',(-55.96170828606,-26.1668761819019,-37.3556204411724));
#247000=CARTESIAN_POINT('Ctrl Pts',(-55.9603820323537,-26.1828878446978,
-37.3370536235569));
#247001=CARTESIAN_POINT('Ctrl Pts',(-55.9595544937755,-26.1988023789265,
-37.3175151190445));
#247002=CARTESIAN_POINT('Ctrl Pts',(-55.9592940442026,-26.2143746264578,
-37.2971137790707));
#247003=CARTESIAN_POINT('Ctrl Pts',(-55.9591607998138,-26.222341291868,
-37.2866765798698));
#247004=CARTESIAN_POINT('Ctrl Pts',(-55.9591758576328,-26.230217912011,
-37.2760142599166));
#247005=CARTESIAN_POINT('Ctrl Pts',(-55.9593475633682,-26.2379689077822,
-37.2651458023614));
#247006=CARTESIAN_POINT('Ctrl Pts',(-55.9598305616365,-26.2597720090362,
-37.2345734620393));
#247007=CARTESIAN_POINT('Ctrl Pts',(-55.9615201312929,-26.2807531775857,
-37.2022137984117));
#247008=CARTESIAN_POINT('Ctrl Pts',(-55.964565507656,-26.3005184935725,
-37.1680104276273));
#247009=CARTESIAN_POINT('Ctrl Pts',(-55.9657901137843,-26.3084665184464,
-37.1542565750731));
#247010=CARTESIAN_POINT('Ctrl Pts',(-55.9672335016317,-26.3162182494181,
-37.1402047360869));
#247011=CARTESIAN_POINT('Ctrl Pts',(-55.9689034868341,-26.3237494563216,
-37.1258518969158));
#247012=CARTESIAN_POINT('Ctrl Pts',(-55.9697156062902,-26.3274119077281,
-37.1188720626497));
#247013=CARTESIAN_POINT('Ctrl Pts',(-55.9705815899045,-26.3310227930614,
-37.111820163739));
#247014=CARTESIAN_POINT('Ctrl Pts',(-55.9715024848901,-26.3345790848028,
-37.1046968313216));
#247015=CARTESIAN_POINT('Ctrl Pts',(-55.9751208331207,-26.3485523413963,
-37.0767080837981));
#247016=CARTESIAN_POINT('Ctrl Pts',(-55.9795661956742,-26.3615529551416,
-37.0478335973107));
#247017=CARTESIAN_POINT('Ctrl Pts',(-55.9848552614668,-26.3733867099384,
-37.0182655556123));
#247018=CARTESIAN_POINT('Ctrl Pts',(-55.9901546423669,-26.3852435437551,
-36.9886398482424));
#247019=CARTESIAN_POINT('Ctrl Pts',(-55.9963009301748,-26.3959285868322,
-36.9583183373182));
#247020=CARTESIAN_POINT('Ctrl Pts',(-56.0032806792625,-26.4052809700527,
-36.9275198794518));
#247021=CARTESIAN_POINT('Ctrl Pts',(-56.0102641509324,-26.4146383412771,
-36.8967049955237));
#247022=CARTESIAN_POINT('Ctrl Pts',(-56.0180818130719,-26.4226612919738,
-36.8654132065517));
#247023=CARTESIAN_POINT('Ctrl Pts',(-56.0266918657886,-26.4292285506241,
-36.8338816445531));
#247024=CARTESIAN_POINT('Ctrl Pts',(-56.0338493648503,-26.4346878839377,
-36.8076695953536));
#247025=CARTESIAN_POINT('Ctrl Pts',(-56.041553878962,-26.4391418905252,
-36.7812923423983));
#247026=CARTESIAN_POINT('Ctrl Pts',(-56.0497678863463,-26.4425442437853,
-36.7548912050128));
#247027=CARTESIAN_POINT('Ctrl Pts',(-56.3299706459847,-27.1806933304988,
-38.1886114270112));
#247028=CARTESIAN_POINT('Ctrl Pts',(-56.3437769035186,-27.1393066339906,
-38.193039662463));
#247029=CARTESIAN_POINT('Ctrl Pts',(-56.3564803637532,-27.0977146430855,
-38.1960409587767));
#247030=CARTESIAN_POINT('Ctrl Pts',(-56.3680979352093,-27.056004561509,
-38.1976404253347));
#247031=CARTESIAN_POINT('Ctrl Pts',(-56.3800510880585,-27.0130896560733,
-38.1992860935639));
#247032=CARTESIAN_POINT('Ctrl Pts',(-56.3908561640652,-26.9700488132131,
-38.1994477244899));
#247033=CARTESIAN_POINT('Ctrl Pts',(-56.4005166943456,-26.9269475570461,
-38.1981091053726));
#247034=CARTESIAN_POINT('Ctrl Pts',(-56.4040961557844,-26.9109774932987,
-38.1976131144309));
#247035=CARTESIAN_POINT('Ctrl Pts',(-56.4075182298872,-26.8949989247735,
-38.196910746293));
#247036=CARTESIAN_POINT('Ctrl Pts',(-56.4107820091105,-26.8790146182937,
-38.1959998501665));
#247037=CARTESIAN_POINT('Ctrl Pts',(-56.4197273242927,-26.8352050804409,
-38.1935032802724));
#247038=CARTESIAN_POINT('Ctrl Pts',(-56.4274760433765,-26.7913422802906,
-38.189480689052));
#247039=CARTESIAN_POINT('Ctrl Pts',(-56.4339768310141,-26.7474071238096,
-38.1839506306335));
#247040=CARTESIAN_POINT('Ctrl Pts',(-56.4344734020574,-26.7440510802489,
-38.1835282099929));
#247041=CARTESIAN_POINT('Ctrl Pts',(-56.4349626672844,-26.7406946136967,
-38.1830969864374));
#247042=CARTESIAN_POINT('Ctrl Pts',(-56.4354445914514,-26.7373377156824,
-38.1826569655605));
#247043=CARTESIAN_POINT('Ctrl Pts',(-56.4419501218732,-26.6920226979891,
-38.1767170907896));
#247044=CARTESIAN_POINT('Ctrl Pts',(-56.4470910724675,-26.6468479021783,
-38.1691966063775));
#247045=CARTESIAN_POINT('Ctrl Pts',(-56.450788998755,-26.6017985919294,
-38.1601708188183));
#247046=CARTESIAN_POINT('Ctrl Pts',(-56.4531572262878,-26.5729480934145,
-38.1543905200937));
#247047=CARTESIAN_POINT('Ctrl Pts',(-56.4549325771593,-26.5441489691068,
-38.1479926699768));
#247048=CARTESIAN_POINT('Ctrl Pts',(-56.4560836745012,-26.5153977768571,
-38.14100084909));
#247049=CARTESIAN_POINT('Ctrl Pts',(-56.4570386769814,-26.4915444858214,
-38.1352001178704));
#247050=CARTESIAN_POINT('Ctrl Pts',(-56.4575638982276,-26.4677219169545,
-38.1289906679363));
#247051=CARTESIAN_POINT('Ctrl Pts',(-56.4576378137927,-26.4439320606186,
-38.1223923804602));
#247052=CARTESIAN_POINT('Ctrl Pts',(-56.4576780029057,-26.4309971229861,
-38.1188047826295));
#247053=CARTESIAN_POINT('Ctrl Pts',(-56.4575863209636,-26.4180682023607,
-38.1151026029789));
#247054=CARTESIAN_POINT('Ctrl Pts',(-56.4573583944686,-26.4051487944763,
-38.1112876037085));
#247055=CARTESIAN_POINT('Ctrl Pts',(-56.4570348307297,-26.3868084434738,
-38.1058718426829));
#247056=CARTESIAN_POINT('Ctrl Pts',(-56.4564370919895,-26.3684842352767,
-38.1002302193718));
#247057=CARTESIAN_POINT('Ctrl Pts',(-56.4555535507852,-26.350174320246,
-38.0943733011292));
#247058=CARTESIAN_POINT('Ctrl Pts',(-56.4550955081205,-26.340682151426,
-38.0913369759125));
#247059=CARTESIAN_POINT('Ctrl Pts',(-56.4545387351896,-26.3308044692514,
-38.0881165337714));
#247060=CARTESIAN_POINT('Ctrl Pts',(-56.4539112632845,-26.321149637431,
-38.0849073026169));
#247061=CARTESIAN_POINT('Ctrl Pts',(-56.4533283735237,-26.312180785495,
-38.0819260886932));
#247062=CARTESIAN_POINT('Ctrl Pts',(-56.4526850619369,-26.3034039575018,
-38.0789551544803));
#247063=CARTESIAN_POINT('Ctrl Pts',(-56.4520336712243,-26.2952855196118,
-38.0761685452557));
#247064=CARTESIAN_POINT('Ctrl Pts',(-56.4489043128688,-26.2562835796778,
-38.0627813435463));
#247065=CARTESIAN_POINT('Ctrl Pts',(-56.444386387158,-26.217066609373,-38.0483345530097));
#247066=CARTESIAN_POINT('Ctrl Pts',(-56.4383206844836,-26.1776021530648,
-38.032981847176));
#247067=CARTESIAN_POINT('Ctrl Pts',(-56.4338992703069,-26.1488357073674,
-38.0217909473136));
#247068=CARTESIAN_POINT('Ctrl Pts',(-56.4286554571048,-26.1199385485611,
-38.0101193157026));
#247069=CARTESIAN_POINT('Ctrl Pts',(-56.4225389178063,-26.0909056213828,
-37.998038048118));
#247070=CARTESIAN_POINT('Ctrl Pts',(-56.4213234888835,-26.0851364343173,
-37.9956373569215));
#247071=CARTESIAN_POINT('Ctrl Pts',(-56.4200733065636,-26.0793629877505,
-37.9932198357306));
#247072=CARTESIAN_POINT('Ctrl Pts',(-56.4187877641046,-26.0735858933992,
-37.9907856426935));
#247073=CARTESIAN_POINT('Ctrl Pts',(-56.412400971856,-26.0448843120847,
-37.9786921602017));
#247074=CARTESIAN_POINT('Ctrl Pts',(-56.405165059693,-26.0160109209669,
-37.9662294042276));
#247075=CARTESIAN_POINT('Ctrl Pts',(-56.3970073796387,-25.9870111882494,
-37.9534493683309));
#247076=CARTESIAN_POINT('Ctrl Pts',(-56.3921075449972,-25.9695927685497,
-37.9457731586502));
#247077=CARTESIAN_POINT('Ctrl Pts',(-56.3868771908374,-25.9521216702897,
-37.9379863926414));
#247078=CARTESIAN_POINT('Ctrl Pts',(-56.3813044015347,-25.9345959421817,
-37.9301082422528));
#247079=CARTESIAN_POINT('Ctrl Pts',(-56.3785180068833,-25.9258330781278,
-37.9261691670585));
#247080=CARTESIAN_POINT('Ctrl Pts',(-56.3756459973473,-25.9170565567473,
-37.9222072490867));
#247081=CARTESIAN_POINT('Ctrl Pts',(-56.3726869268393,-25.9082661430612,
-37.9182250284407));
#247082=CARTESIAN_POINT('Ctrl Pts',(-56.3712073915853,-25.9038709362181,
-37.9162339181176));
#247083=CARTESIAN_POINT('Ctrl Pts',(-56.3697060905476,-25.8994722563214,
-37.9142377323202));
#247084=CARTESIAN_POINT('Ctrl Pts',(-56.3681828424972,-25.8950700745533,
-37.9122367943842));
#247085=CARTESIAN_POINT('Ctrl Pts',(-56.3669710243399,-25.8915679241342,
-37.9106449506121));
#247086=CARTESIAN_POINT('Ctrl Pts',(-56.3654774223584,-25.8873033214185,
-37.9087037044428));
#247087=CARTESIAN_POINT('Ctrl Pts',(-56.3643408295022,-25.8840911501479,
-37.9072401091671));
#247088=CARTESIAN_POINT('Ctrl Pts',(-56.3640487320537,-25.8832656416757,
-37.9068639740865));
#247089=CARTESIAN_POINT('Ctrl Pts',(-56.3637804176812,-25.8825094376191,
-37.9065193163851));
#247090=CARTESIAN_POINT('Ctrl Pts',(-56.3635470749447,-25.8818529950945,
-37.9062200511035));
#247091=CARTESIAN_POINT('Ctrl Pts',(-56.3559220562341,-25.8604022029829,
-37.8964408593217));
#247092=CARTESIAN_POINT('Ctrl Pts',(-56.3474085676981,-25.8377868512682,
-37.8860858805099));
#247093=CARTESIAN_POINT('Ctrl Pts',(-56.3378749583545,-25.8140733963192,
-37.8752267949122));
#247094=CARTESIAN_POINT('Ctrl Pts',(-56.328842437291,-25.7916063249726,
-37.8649384648732));
#247095=CARTESIAN_POINT('Ctrl Pts',(-56.3188936191063,-25.7681544980646,
-37.8541980336547));
#247096=CARTESIAN_POINT('Ctrl Pts',(-56.3079341570525,-25.7437537778324,
-37.8431049637893));
#247097=CARTESIAN_POINT('Ctrl Pts',(-56.2975795165837,-25.7206996640498,
-37.8326240889445));
#247098=CARTESIAN_POINT('Ctrl Pts',(-56.2863224087543,-25.6967991089898,
-37.8218290008965));
#247099=CARTESIAN_POINT('Ctrl Pts',(-56.274105561681,-25.6720524972858,
-37.8108317796241));
#247100=CARTESIAN_POINT('Ctrl Pts',(-56.2621445138239,-25.6478240359556,
-37.8000648207562));
#247101=CARTESIAN_POINT('Ctrl Pts',(-56.2492633010286,-25.622785034932,
-37.7891046168325));
#247102=CARTESIAN_POINT('Ctrl Pts',(-56.2354338835942,-25.5968983561643,
-37.7780764398159));
#247103=CARTESIAN_POINT('Ctrl Pts',(-56.2215469023249,-25.5709039261838,
-37.7670023589017));
#247104=CARTESIAN_POINT('Ctrl Pts',(-56.2067037293098,-25.544054901184,
-37.7558602365061));
#247105=CARTESIAN_POINT('Ctrl Pts',(-56.1909044158831,-25.5162703670661,
-37.7447898421755));
#247106=CARTESIAN_POINT('Ctrl Pts',(-56.1874809063733,-25.5102498132477,
-37.7423910290597));
#247107=CARTESIAN_POINT('Ctrl Pts',(-56.1840126093571,-25.5041851725429,
-37.7399956157948));
#247108=CARTESIAN_POINT('Ctrl Pts',(-56.1804996997125,-25.498075361193,
-37.7376050692572));
#247109=CARTESIAN_POINT('Origin',(-57.2992117475353,-25.881758760926,-37.0968023399421));
#247110=CARTESIAN_POINT('Origin',(-59.8906867066747,-29.1158971114318,-24.194539546945));
#247111=CARTESIAN_POINT('',(-59.5084684665646,-28.5649662692455,-28.4686772617213));
#247112=CARTESIAN_POINT('',(-58.9433054279041,-27.6410867367342,-28.14995));
#247113=CARTESIAN_POINT('Origin',(-58.560621995539,-28.5649662692455,-28.14995));
#247114=CARTESIAN_POINT('',(-59.0583147116521,-27.6887251418614,-27.8079298566744));
#247115=CARTESIAN_POINT('',(-59.428784774735,-28.924571066736,-28.4919701433257));
#247116=CARTESIAN_POINT('',(-56.4622101753633,-27.6957756338847,-37.3141124660878));
#247117=CARTESIAN_POINT('Origin',(-58.560621995539,-28.5649662692455,-28.14995));
#247118=CARTESIAN_POINT('Ctrl Pts',(-59.998518160033,-26.9957779612784,
-27.14995));
#247119=CARTESIAN_POINT('Ctrl Pts',(-60.6454255730951,-27.2637357853683,
-27.14995));
#247120=CARTESIAN_POINT('Ctrl Pts',(-60.8666809392289,-27.3553827587689,
-26.4919701433257));
#247121=CARTESIAN_POINT('Ctrl Pts',(-59.9484159856373,-27.1167353102034,
-27.14995));
#247122=CARTESIAN_POINT('Ctrl Pts',(-60.5825424694076,-27.4155490271209,
-27.1499500000068));
#247123=CARTESIAN_POINT('Ctrl Pts',(-60.7664765904384,-27.5972974566192,
-26.4919701433347));
#247124=CARTESIAN_POINT('Ctrl Pts',(-59.8808474404287,-27.230351027148,
-27.1759773253793));
#247125=CARTESIAN_POINT('Ctrl Pts',(-60.5059399274626,-27.5624213738311,
-27.189969500269));
#247126=CARTESIAN_POINT('Ctrl Pts',(-60.6488436389318,-27.8317793422431,
-26.5440247940841));
#247127=CARTESIAN_POINT('Ctrl Pts',(-59.720909171428,-27.4259018040837,
-27.2761636095982));
#247128=CARTESIAN_POINT('Ctrl Pts',(-60.3438449576235,-27.8117580695072,
-27.3392652319674));
#247129=CARTESIAN_POINT('Ctrl Pts',(-60.3963453125034,-28.2507898651562,
-26.7443973625222));
#247130=CARTESIAN_POINT('Ctrl Pts',(-59.6286113898652,-27.5077381405927,
-27.3502831612192));
#247131=CARTESIAN_POINT('Ctrl Pts',(-60.25750475067,-27.9147957782208,-27.4500905748289));
#247132=CARTESIAN_POINT('Ctrl Pts',(-60.2615973195289,-28.4351100777821,
-26.8926364657637));
#247133=CARTESIAN_POINT('Ctrl Pts',(-59.4332702873462,-27.6271977754378,
-27.5354032764078));
#247134=CARTESIAN_POINT('Ctrl Pts',(-60.0950932878165,-28.0555284666377,
-27.714377456199));
#247135=CARTESIAN_POINT('Ctrl Pts',(-59.9954138159282,-28.7255983981058,
-27.2628766961414));
#247136=CARTESIAN_POINT('Ctrl Pts',(-59.3303038024737,-27.6647740853107,
-27.6463310241559));
#247137=CARTESIAN_POINT('Ctrl Pts',(-60.018639255483,-28.0922015151602,
-27.8698850835747));
#247138=CARTESIAN_POINT('Ctrl Pts',(-59.8640830067033,-28.8316522445216,
-27.4847321916381));
#247139=CARTESIAN_POINT('Ctrl Pts',(-59.1292987784775,-27.6899559312547,
-27.888202111114));
#247140=CARTESIAN_POINT('Ctrl Pts',(-59.8921803917124,-28.0961466343177,
-28.1867324885194));
#247141=CARTESIAN_POINT('Ctrl Pts',(-59.6247383514533,-28.9493941482113,
-27.968474365553));
#247142=CARTESIAN_POINT('Ctrl Pts',(-59.0313551773641,-27.6775581371241,
-28.0190267086425));
#247143=CARTESIAN_POINT('Ctrl Pts',(-59.8428062390324,-28.0610797847622,
-28.3489305637492));
#247144=CARTESIAN_POINT('Ctrl Pts',(-59.5168345241973,-28.9610424671195,
-28.23012356061));
#247145=CARTESIAN_POINT('Ctrl Pts',(-58.9433054279041,-27.6410867367342,
-28.14995));
#247146=CARTESIAN_POINT('Ctrl Pts',(-59.8114682071001,-28.0006915342247,
-28.4919701433256));
#247147=CARTESIAN_POINT('Ctrl Pts',(-59.428784774735,-28.924571066736,-28.4919701433257));
#247148=CARTESIAN_POINT('Ctrl Pts',(-60.0746608288527,-28.637079928768,
-27.1547905454732));
#247149=CARTESIAN_POINT('Ctrl Pts',(-60.0444600479327,-28.667752613367,
-27.1992006472175));
#247150=CARTESIAN_POINT('Ctrl Pts',(-60.0141620017611,-28.6965907066387,
-27.2457865562304));
#247151=CARTESIAN_POINT('Ctrl Pts',(-59.9839608794947,-28.7233395120922,
-27.2943231462453));
#247152=CARTESIAN_POINT('Ctrl Pts',(-59.9534054378562,-28.750402134359,
-27.3434291672218));
#247153=CARTESIAN_POINT('Ctrl Pts',(-59.9229495475082,-28.7753257426137,
-27.3945314828291));
#247154=CARTESIAN_POINT('Ctrl Pts',(-59.8927990300297,-28.7978772501937,
-27.4473527189011));
#247155=CARTESIAN_POINT('Ctrl Pts',(-59.8623328067314,-28.8206648944234,
-27.5007270457002));
#247156=CARTESIAN_POINT('Ctrl Pts',(-59.832178773856,-28.8410300714376,
-27.5558559437987));
#247157=CARTESIAN_POINT('Ctrl Pts',(-59.8025485290152,-28.8587698654644,
-27.6124156554068));
#247158=CARTESIAN_POINT('Ctrl Pts',(-59.7829193828322,-28.8705219455461,
-27.6498847635154));
#247159=CARTESIAN_POINT('Ctrl Pts',(-59.7635200854943,-28.881122619247,
-27.6879810424222));
#247160=CARTESIAN_POINT('Ctrl Pts',(-59.7444106790783,-28.8905231963665,
-27.7266032785955));
#247161=CARTESIAN_POINT('Ctrl Pts',(-59.7141853858534,-28.9053920621874,
-27.7876919585852));
#247162=CARTESIAN_POINT('Ctrl Pts',(-59.6846932959222,-28.917253071195,
-27.8500820237121));
#247163=CARTESIAN_POINT('Ctrl Pts',(-59.6561316380727,-28.9260738700217,
-27.9133068574047));
#247164=CARTESIAN_POINT('Ctrl Pts',(-59.628803824998,-28.9345136161588,
-27.9738004199962));
#247165=CARTESIAN_POINT('Ctrl Pts',(-59.6023280103622,-28.9401705089795,
-28.035057253628));
#247166=CARTESIAN_POINT('Ctrl Pts',(-59.5768604082263,-28.9430655183748,
-28.0966587861506));
#247167=CARTESIAN_POINT('Ctrl Pts',(-59.551602297407,-28.9459367140114,
-28.1577535969929));
#247168=CARTESIAN_POINT('Ctrl Pts',(-59.5273361425688,-28.9460913671025,
-28.2191866992274));
#247169=CARTESIAN_POINT('Ctrl Pts',(-59.5041940479805,-28.9435966619134,
-28.2805521290657));
#247170=CARTESIAN_POINT('Ctrl Pts',(-59.4814573360743,-28.9411456567565,
-28.3408426137454));
#247171=CARTESIAN_POINT('Ctrl Pts',(-59.4598058222201,-28.9361374839187,
-28.4010671409335));
#247172=CARTESIAN_POINT('Ctrl Pts',(-59.439341970719,-28.9286789989135,
-28.4608532721926));
#247173=CARTESIAN_POINT('Ctrl Pts',(-59.4357869697836,-28.9273833033711,
-28.4712393792527));
#247174=CARTESIAN_POINT('Ctrl Pts',(-59.4322677512012,-28.9260137628254,
-28.4816123002776));
#247175=CARTESIAN_POINT('Ctrl Pts',(-59.428784774735,-28.924571066736,-28.4919701433257));
#247176=CARTESIAN_POINT('Ctrl Pts',(-58.9433054279041,-27.6410867367342,
-28.14995));
#247177=CARTESIAN_POINT('Ctrl Pts',(-58.9613748712486,-27.648571345232,
-28.1230821098565));
#247178=CARTESIAN_POINT('Ctrl Pts',(-58.9791315286144,-27.6547427046832,
-28.0973015822799));
#247179=CARTESIAN_POINT('Ctrl Pts',(-58.9964342459705,-27.6598302215434,
-28.0726669650116));
#247180=CARTESIAN_POINT('Ctrl Pts',(-59.0144311387734,-27.6651218467652,
-28.0470440205289));
#247181=CARTESIAN_POINT('Ctrl Pts',(-59.0319371483571,-27.6692410795885,
-28.0226604247913));
#247182=CARTESIAN_POINT('Ctrl Pts',(-59.0488314419348,-27.6724253459282,
-27.9995447185591));
#247183=CARTESIAN_POINT('Ctrl Pts',(-59.068041016188,-27.6760460004654,
-27.9732611173396));
#247184=CARTESIAN_POINT('Ctrl Pts',(-59.086460041634,-27.6784586319551,
-27.9486159224461));
#247185=CARTESIAN_POINT('Ctrl Pts',(-59.1039586602071,-27.6799782867226,
-27.9256083236474));
#247186=CARTESIAN_POINT('Ctrl Pts',(-59.1211642581416,-27.6814724943265,
-27.9029859953353));
#247187=CARTESIAN_POINT('Ctrl Pts',(-59.1374778388352,-27.6821028285425,
-27.881949932047));
#247188=CARTESIAN_POINT('Ctrl Pts',(-59.1528052574349,-27.6821364137596,
-27.8624791903457));
#247189=CARTESIAN_POINT('Ctrl Pts',(-59.1690851883618,-27.6821720861078,
-27.8417984522337));
#247190=CARTESIAN_POINT('Ctrl Pts',(-59.1842533698988,-27.6815349481643,
-27.8228824131788));
#247191=CARTESIAN_POINT('Ctrl Pts',(-59.1982293897907,-27.6805062024526,
-27.8056852997811));
#247192=CARTESIAN_POINT('Ctrl Pts',(-59.2028122682947,-27.6801688663122,
-27.8000461920859));
#247193=CARTESIAN_POINT('Ctrl Pts',(-59.2072672152542,-27.6797890985914,
-27.7945917577315));
#247194=CARTESIAN_POINT('Ctrl Pts',(-59.2115920807886,-27.679375851391,
-27.7893200190977));
#247195=CARTESIAN_POINT('Ctrl Pts',(-59.2126299161687,-27.6792766847089,
-27.7880549631497));
#247196=CARTESIAN_POINT('Ctrl Pts',(-59.2136602613722,-27.6791755879617,
-27.786800428185));
#247197=CARTESIAN_POINT('Ctrl Pts',(-59.2146831346899,-27.679072706751,
-27.7855564027394));
#247198=CARTESIAN_POINT('Ctrl Pts',(-59.2157060080076,-27.6789698255402,
-27.7843123772939));
#247199=CARTESIAN_POINT('Ctrl Pts',(-59.2159304130621,-27.6789487784925,
-27.7840390885988));
#247200=CARTESIAN_POINT('Ctrl Pts',(-59.217729308674,-27.6787588260363,
-27.7818558257232));
#247201=CARTESIAN_POINT('Ctrl Pts',(-59.2217623561684,-27.6783329607041,
-27.7769610431625));
#247202=CARTESIAN_POINT('Ctrl Pts',(-59.2257866159072,-27.6778681563496,
-27.7720978874654));
#247203=CARTESIAN_POINT('Ctrl Pts',(-59.2298015448288,-27.677365154145,
-27.7672666579805));
#247204=CARTESIAN_POINT('Ctrl Pts',(-59.2564471047789,-27.6740269193568,
-27.7352036209043));
#247205=CARTESIAN_POINT('Ctrl Pts',(-59.2826719347528,-27.6690086662134,
-27.7045578880862));
#247206=CARTESIAN_POINT('Ctrl Pts',(-59.3083322835412,-27.6625830507753,
-27.6753684982175));
#247207=CARTESIAN_POINT('Ctrl Pts',(-59.3339926323296,-27.6561574353372,
-27.6461791083489));
#247208=CARTESIAN_POINT('Ctrl Pts',(-59.3590887994654,-27.6483243303831,
-27.6184457481429));
#247209=CARTESIAN_POINT('Ctrl Pts',(-59.3835121576981,-27.6393314235105,
-27.5921760116137));
#247210=CARTESIAN_POINT('Ctrl Pts',(-59.4102021141836,-27.6295039341529,
-27.5634683245637));
#247211=CARTESIAN_POINT('Ctrl Pts',(-59.4360869695798,-27.6182918335755,
-27.5365103467925));
#247212=CARTESIAN_POINT('Ctrl Pts',(-59.461058297068,-27.6059926956016,
-27.51128325361));
#247213=CARTESIAN_POINT('Ctrl Pts',(-59.4790883909822,-27.5971123261924,
-27.4930684887171));
#247214=CARTESIAN_POINT('Ctrl Pts',(-59.4966429912841,-27.5876646717946,
-27.4757554313279));
#247215=CARTESIAN_POINT('Ctrl Pts',(-59.5136917085776,-27.5777545780401,
-27.459327532637));
#247216=CARTESIAN_POINT('Ctrl Pts',(-59.5171569791665,-27.5757402824289,
-27.455988447755));
#247217=CARTESIAN_POINT('Ctrl Pts',(-59.5202646758599,-27.5739061150911,
-27.4530084899692));
#247218=CARTESIAN_POINT('Ctrl Pts',(-59.523617795358,-27.5718989259609,
-27.4498080531444));
#247219=CARTESIAN_POINT('Ctrl Pts',(-59.5258853753984,-27.5705415445697,
-27.4476437262635));
#247220=CARTESIAN_POINT('Ctrl Pts',(-59.5282650669352,-27.5691043972,-27.4453790651482));
#247221=CARTESIAN_POINT('Ctrl Pts',(-59.5309409555251,-27.5674680334054,
-27.4428432437218));
#247222=CARTESIAN_POINT('Ctrl Pts',(-59.5623318535266,-27.5482718197956,
-27.4130954761778));
#247223=CARTESIAN_POINT('Ctrl Pts',(-59.5927659836345,-27.5270383018031,
-27.3856317423159));
#247224=CARTESIAN_POINT('Ctrl Pts',(-59.6220731179921,-27.5041279599908,
-27.3604797898221));
#247225=CARTESIAN_POINT('Ctrl Pts',(-59.6423059120638,-27.4883113256403,
-27.3431156125847));
#247226=CARTESIAN_POINT('Ctrl Pts',(-59.6620022705099,-27.4716947429332,
-27.3268527561149));
#247227=CARTESIAN_POINT('Ctrl Pts',(-59.6811150169812,-27.4543872636165,
-27.3116941131195));
#247228=CARTESIAN_POINT('Ctrl Pts',(-59.6966942407607,-27.4402795531553,
-27.2993379668287));
#247229=CARTESIAN_POINT('Ctrl Pts',(-59.7119961768362,-27.4256086581483,
-27.2876298176573));
#247230=CARTESIAN_POINT('Ctrl Pts',(-59.7268826337955,-27.4105236752065,
-27.2766669971972));
#247231=CARTESIAN_POINT('Ctrl Pts',(-59.74173904001,-27.3954691437667,-27.2657263069808));
#247232=CARTESIAN_POINT('Ctrl Pts',(-59.7561813657372,-27.3800025679289,
-27.2555280942016));
#247233=CARTESIAN_POINT('Ctrl Pts',(-59.7700924498725,-27.364298936964,
-27.2461293656728));
#247234=CARTESIAN_POINT('Ctrl Pts',(-59.7806770832468,-27.352350394723,
-27.2389780829479));
#247235=CARTESIAN_POINT('Ctrl Pts',(-59.7909545612152,-27.3402652046939,
-27.2322888317529));
#247236=CARTESIAN_POINT('Ctrl Pts',(-59.8008824303336,-27.328128780816,
-27.2260707188289));
#247237=CARTESIAN_POINT('Ctrl Pts',(-59.8041054693502,-27.3241887442165,
-27.2240520358341));
#247238=CARTESIAN_POINT('Ctrl Pts',(-59.8072916110025,-27.3202435181017,
-27.2220829617867));
#247239=CARTESIAN_POINT('Ctrl Pts',(-59.8104397189014,-27.3162962998181,
-27.2201632624574));
#247240=CARTESIAN_POINT('Ctrl Pts',(-59.8437952720307,-27.2744738294958,
-27.1998232248763));
#247241=CARTESIAN_POINT('Ctrl Pts',(-59.874727000118,-27.230098430282,-27.1838933969132));
#247242=CARTESIAN_POINT('Ctrl Pts',(-59.902952727294,-27.1838915675732,
-27.1723878666496));
#247243=CARTESIAN_POINT('Ctrl Pts',(-59.9311901022577,-27.1376656368799,
-27.160877588449));
#247244=CARTESIAN_POINT('Ctrl Pts',(-59.9567191564442,-27.0896067866201,
-27.1537949386769));
#247245=CARTESIAN_POINT('Ctrl Pts',(-59.9792844971738,-27.0403941998065,
-27.1511419396506));
#247246=CARTESIAN_POINT('Ctrl Pts',(-59.9860436278898,-27.0256532609866,
-27.1503472710736));
#247247=CARTESIAN_POINT('Ctrl Pts',(-59.9925370376024,-27.0108085114896,
-27.1499499750118));
#247248=CARTESIAN_POINT('Ctrl Pts',(-59.9987583477721,-26.9958774502974,
-27.1499499662059));
#247249=CARTESIAN_POINT('Ctrl Pts',(-50.4237575282656,-42.512871148214,
-37.0628442249021));
#247250=CARTESIAN_POINT('Ctrl Pts',(-50.0392469284306,-43.4351970348678,
-37.0691716931121));
#247251=CARTESIAN_POINT('Ctrl Pts',(-49.1714197666586,-43.0765237853397,
-36.7274049322981));
#247252=CARTESIAN_POINT('Ctrl Pts',(-50.3416577002277,-42.4769411182047,
-37.3090186906075));
#247253=CARTESIAN_POINT('Ctrl Pts',(-49.9919063191206,-43.4299470769918,
-37.1948592375177));
#247254=CARTESIAN_POINT('Ctrl Pts',(-49.1176720095218,-43.0532992273906,
-36.8471157789082));
#247255=CARTESIAN_POINT('Ctrl Pts',(-50.2401291906866,-42.4884206957375,
-37.5546625905171));
#247256=CARTESIAN_POINT('Ctrl Pts',(-49.936763884108,-43.4500767701373,
-37.3136659503387));
#247257=CARTESIAN_POINT('Ctrl Pts',(-49.0542361384641,-43.0537900902966,
-36.9665683337155));
#247258=CARTESIAN_POINT('Ctrl Pts',(-50.0695743278833,-42.5755840840409,
-37.8959436915621));
#247259=CARTESIAN_POINT('Ctrl Pts',(-49.8496587474524,-43.5105080802159,
-37.4712316264487));
#247260=CARTESIAN_POINT('Ctrl Pts',(-48.9513522923176,-43.0900782943884,
-37.1325273165808));
#247261=CARTESIAN_POINT('Ctrl Pts',(-50.0111449417175,-42.6150505005841,
-38.0027616853659));
#247262=CARTESIAN_POINT('Ctrl Pts',(-49.8204425668583,-43.5351648198003,
-37.5194682740609));
#247263=CARTESIAN_POINT('Ctrl Pts',(-48.9166267233427,-43.1075285409369,
-37.1844709706788));
#247264=CARTESIAN_POINT('Ctrl Pts',(-49.8898699570401,-42.7151860559833,
-38.2053146722979));
#247265=CARTESIAN_POINT('Ctrl Pts',(-49.7612063443368,-43.5929894582252,
-37.6090332432771));
#247266=CARTESIAN_POINT('Ctrl Pts',(-48.8455389394235,-43.1532669776793,
-37.2829687310632));
#247267=CARTESIAN_POINT('Ctrl Pts',(-49.8264028016164,-42.7766563905902,
-38.3017849985497));
#247268=CARTESIAN_POINT('Ctrl Pts',(-49.7309236615698,-43.626585368299,
-37.6505782223522));
#247269=CARTESIAN_POINT('Ctrl Pts',(-48.8088280035253,-43.1819400457003,
-37.3298804131014));
#247270=CARTESIAN_POINT('Ctrl Pts',(-49.6998636398414,-42.9166438821161,
-38.4757993599315));
#247271=CARTESIAN_POINT('Ctrl Pts',(-49.6717558147567,-43.6995260307251,
-37.7240763018152));
#247272=CARTESIAN_POINT('Ctrl Pts',(-48.7365799885116,-43.2482138864143,
-37.4145002189235));
#247273=CARTESIAN_POINT('Ctrl Pts',(-49.636377638708,-42.9953419367724,
-38.5542040553824));
#247274=CARTESIAN_POINT('Ctrl Pts',(-49.6426863188407,-43.7390132802502,
-37.7563474788299));
#247275=CARTESIAN_POINT('Ctrl Pts',(-48.7007915109969,-43.2858867144277,
-37.4526268655564));
#247276=CARTESIAN_POINT('Ctrl Pts',(-49.5089673406965,-43.1703662790524,
-38.6935914165869));
#247277=CARTESIAN_POINT('Ctrl Pts',(-49.5852286190754,-43.8240110418488,
-37.8128274533556));
#247278=CARTESIAN_POINT('Ctrl Pts',(-48.6298942465199,-43.3704186966852,
-37.5204081363966));
#247279=CARTESIAN_POINT('Ctrl Pts',(-49.4452086173444,-43.2667004006212,
-38.7541455640211));
#247280=CARTESIAN_POINT('Ctrl Pts',(-49.5569626986225,-43.8694639105835,
-37.8367864581829));
#247281=CARTESIAN_POINT('Ctrl Pts',(-48.5948903577209,-43.4172909280656,
-37.5498543766621));
#247282=CARTESIAN_POINT('Ctrl Pts',(-49.2615126569161,-43.5701125808966,
-38.9014161879009));
#247283=CARTESIAN_POINT('Ctrl Pts',(-49.4760987284841,-44.0097527471331,
-37.8945457008393));
#247284=CARTESIAN_POINT('Ctrl Pts',(-48.4954434049397,-43.5658475318205,
-37.6214690391308));
#247285=CARTESIAN_POINT('Ctrl Pts',(-49.1445110616521,-43.7995630731719,
-38.957158320864));
#247286=CARTESIAN_POINT('Ctrl Pts',(-49.4258287509964,-44.1113431434592,
-37.9153346356675));
#247287=CARTESIAN_POINT('Ctrl Pts',(-48.4340663781108,-43.6793802666741,
-37.6485752564667));
#247288=CARTESIAN_POINT('Ctrl Pts',(-49.0438717682238,-44.0349657503363,
-38.9651091877403));
#247289=CARTESIAN_POINT('Ctrl Pts',(-49.3817941333223,-44.2147893101095,
-37.9183446714817));
#247290=CARTESIAN_POINT('Ctrl Pts',(-48.3833370225155,-43.7969102160512,
-37.6524415864869));
#247291=CARTESIAN_POINT('',(-48.3869818477026,-43.7885141789011,-37.6521262739199));
#247292=CARTESIAN_POINT('Ctrl Pts',(-48.3869820185779,-43.7885142818768,
-37.6521255977635));
#247293=CARTESIAN_POINT('Ctrl Pts',(-48.3941923230744,-43.7855029913321,
-37.6532372055275));
#247294=CARTESIAN_POINT('Ctrl Pts',(-48.40472479657,-43.7811582841343,-37.6548675123769));
#247295=CARTESIAN_POINT('Ctrl Pts',(-48.4185542648403,-43.7754695476231,
-37.6570112368262));
#247296=CARTESIAN_POINT('Ctrl Pts',(-48.4332645964769,-43.7694184689384,
-37.6592915050889));
#247297=CARTESIAN_POINT('Ctrl Pts',(-48.4517063655238,-43.7618503879438,
-37.662153381686));
#247298=CARTESIAN_POINT('Ctrl Pts',(-48.4738977492675,-43.7527517588849,
-37.6656002137221));
#247299=CARTESIAN_POINT('Ctrl Pts',(-48.4777287835395,-43.7511810069139,
-37.6661952614132));
#247300=CARTESIAN_POINT('Ctrl Pts',(-48.4816716525774,-43.7495645474523,
-37.6668077446633));
#247301=CARTESIAN_POINT('Ctrl Pts',(-48.4857265410659,-43.7479021557398,
-37.6674376688176));
#247302=CARTESIAN_POINT('Ctrl Pts',(-48.5038894581431,-43.740455863959,
-37.6702592655672));
#247303=CARTESIAN_POINT('Ctrl Pts',(-48.5242907044421,-43.7320882445654,
-37.6734280242068));
#247304=CARTESIAN_POINT('Ctrl Pts',(-48.5469302210382,-43.7227990263846,
-37.6769467634094));
#247305=CARTESIAN_POINT('Ctrl Pts',(-48.5552184355614,-43.7193982897696,
-37.6782349563457));
#247306=CARTESIAN_POINT('Ctrl Pts',(-48.5638066266517,-43.7158735854635,
-37.6795699967092));
#247307=CARTESIAN_POINT('Ctrl Pts',(-48.5726946772116,-43.7122230706351,
-37.6809516127904));
#247308=CARTESIAN_POINT('Ctrl Pts',(-48.5892776962156,-43.7054120656387,
-37.68352938455));
#247309=CARTESIAN_POINT('Ctrl Pts',(-48.6069047406048,-43.6981667414177,
-37.6862702702229));
#247310=CARTESIAN_POINT('Ctrl Pts',(-48.6255745808139,-43.690481744612,
-37.6891773653139));
#247311=CARTESIAN_POINT('Ctrl Pts',(-48.6349095009184,-43.6866392462091,
-37.6906309128593));
#247312=CARTESIAN_POINT('Ctrl Pts',(-48.6445051011876,-43.6826868018733,
-37.6921260606455));
#247313=CARTESIAN_POINT('Ctrl Pts',(-48.6543610548145,-43.6786234447101,
-37.6936635574224));
#247314=CARTESIAN_POINT('Ctrl Pts',(-48.6592890316279,-43.6765917661285,
-37.6944323058108));
#247315=CARTESIAN_POINT('Ctrl Pts',(-48.6642820944631,-43.6745323555192,
-37.6952116459788));
#247316=CARTESIAN_POINT('Ctrl Pts',(-48.6693401861212,-43.6724450617448,
-37.6960017001812));
#247317=CARTESIAN_POINT('Ctrl Pts',(-48.6743982777794,-43.6703577679704,
-37.6967917543835));
#247318=CARTESIAN_POINT('Ctrl Pts',(-48.6809273732975,-43.6676617725024,
-37.6978124741394));
#247319=CARTESIAN_POINT('Ctrl Pts',(-48.6847094771468,-43.6660993562588,
-37.698404148648));
#247320=CARTESIAN_POINT('Ctrl Pts',(-48.7123065729498,-43.6546987833301,
-37.7027214542398));
#247321=CARTESIAN_POINT('Ctrl Pts',(-48.7387413992479,-43.6436924952179,
-37.7068525271263));
#247322=CARTESIAN_POINT('Ctrl Pts',(-48.7640030878273,-43.6330656769537,
-37.7107829608343));
#247323=CARTESIAN_POINT('Ctrl Pts',(-48.7909189728857,-43.6217429889221,
-37.7149707688498));
#247324=CARTESIAN_POINT('Ctrl Pts',(-48.8165033200792,-43.6108520387734,
-37.7189299873399));
#247325=CARTESIAN_POINT('Ctrl Pts',(-48.8407654011673,-43.6004175398603,
-37.7226755849429));
#247326=CARTESIAN_POINT('Ctrl Pts',(-48.8436635160472,-43.599171134968,
-37.7231229980113));
#247327=CARTESIAN_POINT('Ctrl Pts',(-48.8465427863071,-43.5979312796092,
-37.7235674059532));
#247328=CARTESIAN_POINT('Ctrl Pts',(-48.8494032448022,-43.5966980430636,
-37.7240088692827));
#247329=CARTESIAN_POINT('Ctrl Pts',(-48.8595586364947,-43.5923197239264,
-37.7255761820184));
#247330=CARTESIAN_POINT('Ctrl Pts',(-48.8694763091597,-43.5880221626812,
-37.727104110795));
#247331=CARTESIAN_POINT('Ctrl Pts',(-48.8791523850949,-43.583810866203,
-37.7285943817753));
#247332=CARTESIAN_POINT('Ctrl Pts',(-48.892954490905,-43.5778038071453,
-37.7307201275729));
#247333=CARTESIAN_POINT('Ctrl Pts',(-48.9062809742503,-43.571946621652,
-37.7327581161945));
#247334=CARTESIAN_POINT('Ctrl Pts',(-48.9191161911195,-43.5662657232329,
-37.7347219845827));
#247335=CARTESIAN_POINT('Ctrl Pts',(-48.9300329149347,-43.5614339545377,
-37.736392311545));
#247336=CARTESIAN_POINT('Ctrl Pts',(-48.9405984373613,-43.5567226003328,
-37.7380053451827));
#247337=CARTESIAN_POINT('Ctrl Pts',(-48.9508131358863,-43.552133008746,
-37.7395604493697));
#247338=CARTESIAN_POINT('Ctrl Pts',(-48.9559204851488,-43.5498382129526,
-37.7403380014632));
#247339=CARTESIAN_POINT('Ctrl Pts',(-48.9609401364647,-43.547573871151,
-37.7411010587111));
#247340=CARTESIAN_POINT('Ctrl Pts',(-48.9658721830952,-43.5453402239186,
-37.7418494793756));
#247341=CARTESIAN_POINT('Ctrl Pts',(-48.9683382064105,-43.5442234003024,
-37.7422236897079));
#247342=CARTESIAN_POINT('Ctrl Pts',(-48.9707823289942,-43.5431142510686,
-37.7425942403847));
#247343=CARTESIAN_POINT('Ctrl Pts',(-48.9732045651145,-43.5420128103547,
-37.742961110882));
#247344=CARTESIAN_POINT('Ctrl Pts',(-48.9756268012349,-43.5409113696408,
-37.7433279813792));
#247345=CARTESIAN_POINT('Ctrl Pts',(-48.9768890918041,-43.5403372625218,
-37.7435191631628));
#247346=CARTESIAN_POINT('Ctrl Pts',(-48.980405629973,-43.5387316505353,
-37.7440506597886));
#247347=CARTESIAN_POINT('Ctrl Pts',(-49.0162112906282,-43.5223831864575,
-37.749462399093));
#247348=CARTESIAN_POINT('Ctrl Pts',(-49.0511276808107,-43.5059828258899,
-37.7547048280429));
#247349=CARTESIAN_POINT('Ctrl Pts',(-49.0850703209528,-43.4895147250152,
-37.7597506223924));
#247350=CARTESIAN_POINT('Ctrl Pts',(-49.1076241559372,-43.4785721811212,
-37.763103396739));
#247351=CARTESIAN_POINT('Ctrl Pts',(-49.1297489180256,-43.4676007829305,
-37.766369148453));
#247352=CARTESIAN_POINT('Ctrl Pts',(-49.1514279942163,-43.4566051623532,
-37.7695413736243));
#247353=CARTESIAN_POINT('Ctrl Pts',(-49.1832043343191,-43.440488212718,
-37.7741910969354));
#247354=CARTESIAN_POINT('Ctrl Pts',(-49.2140118419065,-43.4243167890084,
-37.7786635108871));
#247355=CARTESIAN_POINT('Ctrl Pts',(-49.2438645278442,-43.4080568268287,
-37.7829115278891));
#247356=CARTESIAN_POINT('Ctrl Pts',(-49.275440482448,-43.3908582461476,
-37.7874047648558));
#247357=CARTESIAN_POINT('Ctrl Pts',(-49.3059481203,-43.3735617149496,-37.7916467356859));
#247358=CARTESIAN_POINT('Ctrl Pts',(-49.3354042005926,-43.3561704676905,
-37.7956243930565));
#247359=CARTESIAN_POINT('Ctrl Pts',(-49.3678131316066,-43.3370358195272,
-37.8000007941949));
#247360=CARTESIAN_POINT('Ctrl Pts',(-49.3989490230391,-43.3177876585055,
-37.8040571104969));
#247361=CARTESIAN_POINT('Ctrl Pts',(-49.4288357902375,-43.2984632285755,
-37.8078297319575));
#247362=CARTESIAN_POINT('Ctrl Pts',(-49.4364798994516,-43.2935206380335,
-37.8087946516584));
#247363=CARTESIAN_POINT('Ctrl Pts',(-49.4440423047,-43.2885731615757,-37.8097412644242));
#247364=CARTESIAN_POINT('Ctrl Pts',(-49.4515234297442,-43.2836215894803,
-37.810670665132));
#247365=CARTESIAN_POINT('Ctrl Pts',(-49.4823256120956,-43.2632343849215,
-37.8144973048295));
#247366=CARTESIAN_POINT('Ctrl Pts',(-49.5117715503363,-43.2427689466307,
-37.8179862888973));
#247367=CARTESIAN_POINT('Ctrl Pts',(-49.539850477956,-43.2223212301653,
-37.8213021121719));
#247368=CARTESIAN_POINT('',(-49.1686140212331,-43.0753365939135,-36.7336343834465));
#247369=CARTESIAN_POINT('Ctrl Pts',(-49.1686140214361,-43.0753365934265,
-36.7336343834471));
#247370=CARTESIAN_POINT('Ctrl Pts',(-49.1683337750584,-43.075220511576,
-36.7342546446349));
#247371=CARTESIAN_POINT('Ctrl Pts',(-49.1673315732913,-43.0748009644702,
-36.7364762491404));
#247372=CARTESIAN_POINT('Ctrl Pts',(-49.1655731415317,-43.0741060083359,
-36.7403419878483));
#247373=CARTESIAN_POINT('Ctrl Pts',(-49.1639046758595,-43.0734466080223,
-36.7440099449906));
#247374=CARTESIAN_POINT('Ctrl Pts',(-49.1615552406925,-43.0725394115718,
-36.749158251366));
#247375=CARTESIAN_POINT('Ctrl Pts',(-49.1584774905419,-43.0714549440963,
-36.7558211532992));
#247376=CARTESIAN_POINT('Ctrl Pts',(-49.1554493667226,-43.0703879628168,
-36.7623766211126));
#247377=CARTESIAN_POINT('Ctrl Pts',(-49.151716128663,-43.069149267846,-36.7703985066625));
#247378=CARTESIAN_POINT('Ctrl Pts',(-49.1472163071513,-43.0678524373069,
-36.7799140437103));
#247379=CARTESIAN_POINT('Ctrl Pts',(-49.1431401300286,-43.0666776993841,
-36.7885337221405));
#247380=CARTESIAN_POINT('Ctrl Pts',(-49.1384346443936,-43.0654556929127,
-36.7983792211052));
#247381=CARTESIAN_POINT('Ctrl Pts',(-49.1330435616248,-43.0643059188313,
-36.8094633528079));
#247382=CARTESIAN_POINT('Ctrl Pts',(-49.128280821557,-43.0632901534794,
-36.8192556042798));
#247383=CARTESIAN_POINT('Ctrl Pts',(-49.1229843241211,-43.0623311285456,
-36.8300117719329));
#247384=CARTESIAN_POINT('Ctrl Pts',(-49.1170958753251,-43.0615332342699,
-36.8417600935923));
#247385=CARTESIAN_POINT('Ctrl Pts',(-49.1101501782072,-43.0605920811474,
-36.8556177811971));
#247386=CARTESIAN_POINT('Ctrl Pts',(-49.1023827525068,-43.059874088312,
-36.8708531503353));
#247387=CARTESIAN_POINT('Ctrl Pts',(-49.0936988710649,-43.0595999877853,
-36.8874724047507));
#247388=CARTESIAN_POINT('Ctrl Pts',(-49.0858463594793,-43.0593521288554,
-36.9025005795036));
#247389=CARTESIAN_POINT('Ctrl Pts',(-49.0772442151559,-43.0594676696369,
-36.9186604878903));
#247390=CARTESIAN_POINT('Ctrl Pts',(-49.0678179136489,-43.0601492850026,
-36.9359343013193));
#247391=CARTESIAN_POINT('Ctrl Pts',(-49.0586745427887,-43.0608104416682,
-36.9526896408587));
#247392=CARTESIAN_POINT('Ctrl Pts',(-49.0487557305991,-43.0620042891318,
-36.9704929824581));
#247393=CARTESIAN_POINT('Ctrl Pts',(-49.0379957893748,-43.0639516440868,
-36.9892956075429));
#247394=CARTESIAN_POINT('Ctrl Pts',(-49.0305212063224,-43.0653044085713,
-37.0023571828686));
#247395=CARTESIAN_POINT('Ctrl Pts',(-49.0226405847877,-43.0670215909623,
-37.0159006128308));
#247396=CARTESIAN_POINT('Ctrl Pts',(-49.0143347106628,-43.0691871639097,
-37.029896478983));
#247397=CARTESIAN_POINT('Ctrl Pts',(-49.0101817736003,-43.0702699503835,
-37.036894412059));
#247398=CARTESIAN_POINT('Ctrl Pts',(-49.0059224867822,-43.0714649806154,
-37.0440054089939));
#247399=CARTESIAN_POINT('Ctrl Pts',(-49.0015548172672,-43.0727834636932,
-37.051224538183));
#247400=CARTESIAN_POINT('Ctrl Pts',(-48.9993709825097,-43.073442705232,
-37.0548341027775));
#247401=CARTESIAN_POINT('Ctrl Pts',(-48.9971600554548,-43.0741328172138,
-37.0584706883975));
#247402=CARTESIAN_POINT('Ctrl Pts',(-48.9949218013837,-43.0748552442512,
-37.0621336079249));
#247403=CARTESIAN_POINT('Ctrl Pts',(-48.9947516515637,-43.074910162427,
-37.0624120593779));
#247404=CARTESIAN_POINT('Ctrl Pts',(-48.9945823225945,-43.0749649498015,
-37.0626890625254));
#247405=CARTESIAN_POINT('Ctrl Pts',(-48.9944107145094,-43.0750206127534,
-37.0629696859303));
#247406=CARTESIAN_POINT('Ctrl Pts',(-48.9929547407522,-43.0754928737024,
-37.0653505779076));
#247407=CARTESIAN_POINT('Ctrl Pts',(-48.9910589517925,-43.0761221560178,
-37.0684394409689));
#247408=CARTESIAN_POINT('Ctrl Pts',(-48.9896342939045,-43.0766054080036,
-37.0707525726143));
#247409=CARTESIAN_POINT('Ctrl Pts',(-48.9890179860343,-43.0768144631071,
-37.0717532347733));
#247410=CARTESIAN_POINT('Ctrl Pts',(-48.9884900444376,-43.0769953611969,
-37.072608999683));
#247411=CARTESIAN_POINT('Ctrl Pts',(-48.988124835575,-43.0771209443097,
-37.0732006352929));
#247412=CARTESIAN_POINT('Ctrl Pts',(-48.9871657946507,-43.0774507264069,
-37.0747542743754));
#247413=CARTESIAN_POINT('Ctrl Pts',(-48.9862068882847,-43.0777847567456,
-37.0763044684413));
#247414=CARTESIAN_POINT('Ctrl Pts',(-48.9852481546861,-43.0781229928334,
-37.0778511718949));
#247415=CARTESIAN_POINT('Ctrl Pts',(-48.96949840413,-43.0836794206261,-37.1032598919126));
#247416=CARTESIAN_POINT('Ctrl Pts',(-48.9539049319844,-43.0903185138448,
-37.1275604547439));
#247417=CARTESIAN_POINT('Ctrl Pts',(-48.9385790570763,-43.0978238481727,
-37.150682142485));
#247418=CARTESIAN_POINT('Ctrl Pts',(-48.9223950612735,-43.1057494184902,
-37.1750984514786));
#247419=CARTESIAN_POINT('Ctrl Pts',(-48.9065095058817,-43.1146407285902,
-37.1982002688633));
#247420=CARTESIAN_POINT('Ctrl Pts',(-48.8910609812166,-43.1241913276533,
-37.2199301095669));
#247421=CARTESIAN_POINT('Ctrl Pts',(-48.8877410902348,-43.126243753266,
-37.224599856598));
#247422=CARTESIAN_POINT('Ctrl Pts',(-48.8844414069668,-43.1283264551359,
-37.2292063289032));
#247423=CARTESIAN_POINT('Ctrl Pts',(-48.8811633453352,-43.1304361250316,
-37.2337490904038));
#247424=CARTESIAN_POINT('Ctrl Pts',(-48.87925775696,-43.1316625090599,-37.2363898685463));
#247425=CARTESIAN_POINT('Ctrl Pts',(-48.8773584741306,-43.1328991103173,
-37.2390101440911));
#247426=CARTESIAN_POINT('Ctrl Pts',(-48.8754660681914,-43.134145042483,
-37.2416094617211));
#247427=CARTESIAN_POINT('Ctrl Pts',(-48.8633226216908,-43.1421401085966,
-37.2582891148152));
#247428=CARTESIAN_POINT('Ctrl Pts',(-48.8514789480032,-43.1505096699715,
-37.2740888990657));
#247429=CARTESIAN_POINT('Ctrl Pts',(-48.8399944210421,-43.159099822315,
-37.2890302768204));
#247430=CARTESIAN_POINT('Ctrl Pts',(-48.834685217634,-43.1630709798779,
-37.295937554235));
#247431=CARTESIAN_POINT('Ctrl Pts',(-48.8294523536931,-43.1670898452388,
-37.3026617223202));
#247432=CARTESIAN_POINT('Ctrl Pts',(-48.8242997622521,-43.1711439171208,
-37.309206443355));
#247433=CARTESIAN_POINT('Ctrl Pts',(-48.8161505895126,-43.1775557066917,
-37.3195573634414));
#247434=CARTESIAN_POINT('Ctrl Pts',(-48.8082033886358,-43.1840546475917,
-37.329458206654));
#247435=CARTESIAN_POINT('Ctrl Pts',(-48.8004734072819,-43.1905952224304,
-37.3389225331823));
#247436=CARTESIAN_POINT('Ctrl Pts',(-48.796608416605,-43.1938655098497,
-37.3436546964465));
#247437=CARTESIAN_POINT('Ctrl Pts',(-48.7927977248867,-43.1971462475385,
-37.3482776875658));
#247438=CARTESIAN_POINT('Ctrl Pts',(-48.7890429180782,-43.2004323433745,
-37.3527934738198));
#247439=CARTESIAN_POINT('Ctrl Pts',(-48.7869512675521,-43.2022628940351,
-37.3553090351191));
#247440=CARTESIAN_POINT('Ctrl Pts',(-48.7852402434882,-43.2037739309092,
-37.3573565500108));
#247441=CARTESIAN_POINT('Ctrl Pts',(-48.783302773363,-43.2054983650398,
-37.3596657888437));
#247442=CARTESIAN_POINT('Ctrl Pts',(-48.7817622121791,-43.2068695326521,
-37.3615019584258));
#247443=CARTESIAN_POINT('Ctrl Pts',(-48.7800784456113,-43.2083758932927,
-37.3635034554526));
#247444=CARTESIAN_POINT('Ctrl Pts',(-48.7779479513844,-43.2103018304306,
-37.3660211095965));
#247445=CARTESIAN_POINT('Ctrl Pts',(-48.7761984141342,-43.2118833877622,
-37.3680885780985));
#247446=CARTESIAN_POINT('Ctrl Pts',(-48.7744507032931,-43.2134753302845,
-37.370145189086));
#247447=CARTESIAN_POINT('Ctrl Pts',(-48.7727050281733,-43.215077463822,
-37.3721906661398));
#247448=CARTESIAN_POINT('Ctrl Pts',(-48.749680734094,-43.2362085398765,
-37.3991691483819));
#247449=CARTESIAN_POINT('Ctrl Pts',(-48.7269086677561,-43.2591448935121,
-37.4243779608413));
#247450=CARTESIAN_POINT('Ctrl Pts',(-48.7044148467678,-43.2837824910303,
-37.4477732221221));
#247451=CARTESIAN_POINT('Ctrl Pts',(-48.6913853473366,-43.2980537685965,
-37.4613248789841));
#247452=CARTESIAN_POINT('Ctrl Pts',(-48.6784491398924,-43.3128951477292,
-37.4742687062647));
#247453=CARTESIAN_POINT('Ctrl Pts',(-48.6656107043938,-43.3282806397202,
-37.4866016703672));
#247454=CARTESIAN_POINT('Ctrl Pts',(-48.6460866766756,-43.3516780990231,
-37.5053570033683));
#247455=CARTESIAN_POINT('Ctrl Pts',(-48.6268227356246,-43.3763363759805,
-37.5226335144684));
#247456=CARTESIAN_POINT('Ctrl Pts',(-48.6080585338523,-43.40181969179,-37.5382668320716));
#247457=CARTESIAN_POINT('Ctrl Pts',(-48.5924087617698,-43.4230733581684,
-37.5513053753761));
#247458=CARTESIAN_POINT('Ctrl Pts',(-48.577106383062,-43.4449007487233,
-37.5632014659455));
#247459=CARTESIAN_POINT('Ctrl Pts',(-48.5622752927423,-43.4670574296315,
-37.5738817239087));
#247460=CARTESIAN_POINT('Ctrl Pts',(-48.5609740374997,-43.4690014200306,
-37.5748187920114));
#247461=CARTESIAN_POINT('Ctrl Pts',(-48.5596754374432,-43.4709494581627,
-37.5757471545326));
#247462=CARTESIAN_POINT('Ctrl Pts',(-48.5583795328176,-43.4729014153975,
-37.5766668154231));
#247463=CARTESIAN_POINT('Ctrl Pts',(-48.5393600363684,-43.501549545024,
-37.5901643265022));
#247464=CARTESIAN_POINT('Ctrl Pts',(-48.5210197611396,-43.530904729223,
-37.6017244902742));
#247465=CARTESIAN_POINT('Ctrl Pts',(-48.5034701459434,-43.560633202674,
-37.611456384112));
#247466=CARTESIAN_POINT('Ctrl Pts',(-48.4857114947968,-43.59071577618,-37.6213041959147));
#247467=CARTESIAN_POINT('Ctrl Pts',(-48.4687624047102,-43.6211806953529,
-37.6292799395048));
#247468=CARTESIAN_POINT('Ctrl Pts',(-48.4527142239903,-43.6517295750421,
-37.6355052155685));
#247469=CARTESIAN_POINT('Ctrl Pts',(-48.4363750855775,-43.6828323138703,
-37.6418433575073));
#247470=CARTESIAN_POINT('Ctrl Pts',(-48.4209697936999,-43.7140221500743,
-37.6463669886134));
#247471=CARTESIAN_POINT('Ctrl Pts',(-48.4065704198427,-43.7450317991596,
-37.6492131468641));
#247472=CARTESIAN_POINT('Ctrl Pts',(-48.3998182147374,-43.7595729530278,
-37.6505477774155));
#247473=CARTESIAN_POINT('Ctrl Pts',(-48.3932868585182,-43.7740751531259,
-37.6515136723023));
#247474=CARTESIAN_POINT('Ctrl Pts',(-48.3869820185779,-43.7885142818768,
-37.6521255977635));
#247475=CARTESIAN_POINT('',(-50.4194602329978,-42.5110618584059,-37.075654526771));
#247476=CARTESIAN_POINT('Origin',(-49.5512974538022,-42.1514570609157,-36.7336343834439));
#247477=CARTESIAN_POINT('',(-49.9605657445604,-42.6569090739569,-38.0871380980686));
#247478=CARTESIAN_POINT('Origin',(-49.6622328036899,-44.3390837210073,-37.0757458603726));
#247479=CARTESIAN_POINT('Ctrl Pts',(-49.8728085593972,-42.8820630175426,
-37.969462470141));
#247480=CARTESIAN_POINT('Ctrl Pts',(-49.8921616460598,-42.8476319404765,
-37.9909151727652));
#247481=CARTESIAN_POINT('Ctrl Pts',(-49.9092258698084,-42.811480340848,
-38.0115509623024));
#247482=CARTESIAN_POINT('Ctrl Pts',(-49.9385737864525,-42.7361810737982,
-38.050911317004));
#247483=CARTESIAN_POINT('Ctrl Pts',(-49.9508224032009,-42.6971223001809,
-38.0695891203786));
#247484=CARTESIAN_POINT('Ctrl Pts',(-49.96056574456,-42.6569090739567,-38.0871380980685));
#247485=CARTESIAN_POINT('Origin',(-48.14917985945,-41.570680937293,-40.903319168463));
#247486=CARTESIAN_POINT('',(-52.0550036453325,-44.2709183219374,-28.14995));
#247487=CARTESIAN_POINT('',(-53.3058498568936,-43.7066435869166,-28.4919701433257));
#247488=CARTESIAN_POINT('Origin',(-52.4376870776976,-43.3470387894261,-28.14995));
#247489=CARTESIAN_POINT('',(-49.017342638646,-41.9302857347835,-41.2453393117887));
#247490=CARTESIAN_POINT('',(-53.3850683564681,-44.8218491641236,-24.194539546945));
#247491=CARTESIAN_POINT('Ctrl Pts',(-52.0550036453325,-44.2709183219374,
-28.14995));
#247492=CARTESIAN_POINT('Ctrl Pts',(-52.9231664245284,-44.6305231194279,
-28.4919701433257));
#247493=CARTESIAN_POINT('Ctrl Pts',(-53.3058498568936,-43.7066435869166,
-28.4919701433257));
#247494=CARTESIAN_POINT('Ctrl Pts',(-52.1435820782265,-44.3076087101758,
-28.0182405965214));
#247495=CARTESIAN_POINT('Ctrl Pts',(-52.9884077964684,-44.6098608177916,
-28.3480901147829));
#247496=CARTESIAN_POINT('Ctrl Pts',(-53.3944282897846,-43.743333975162,
-28.228551336368));
#247497=CARTESIAN_POINT('Ctrl Pts',(-52.2220105281705,-44.3686099077136,
-27.8866328738247));
#247498=CARTESIAN_POINT('Ctrl Pts',(-53.048435044978,-44.620231423514,-28.1848168586396));
#247499=CARTESIAN_POINT('Ctrl Pts',(-53.4627751400873,-43.8286743072844,
-27.9653358909753));
#247500=CARTESIAN_POINT('Ctrl Pts',(-52.3467027906606,-44.5299708800253,
-27.6435487102698));
#247501=CARTESIAN_POINT('Ctrl Pts',(-53.1352121592815,-44.7138087590227,
-27.8661586695385));
#247502=CARTESIAN_POINT('Ctrl Pts',(-53.5486784427678,-44.0836801124388,
-27.479167563865));
#247503=CARTESIAN_POINT('Ctrl Pts',(-52.3929000186986,-44.6302588784236,
-27.5321945097562));
#247504=CARTESIAN_POINT('Ctrl Pts',(-53.1631899467114,-44.794885409667,
-27.7098964514495));
#247505=CARTESIAN_POINT('Ctrl Pts',(-53.5661839363464,-44.2532360852968,
-27.2564591628373));
#247506=CARTESIAN_POINT('Ctrl Pts',(-52.4459516145522,-44.8547560303666,
-27.3468433305442));
#247507=CARTESIAN_POINT('Ctrl Pts',(-53.1776753975914,-45.0117760871578,
-27.4450855646671));
#247508=CARTESIAN_POINT('Ctrl Pts',(-53.5476330292888,-44.6505969708682,
-26.8857568044149));
#247509=CARTESIAN_POINT('Ctrl Pts',(-52.452784611166,-44.9788747485428,
-27.2729210180269));
#247510=CARTESIAN_POINT('Ctrl Pts',(-53.1651856643124,-45.1471482079303,
-27.3344565761127));
#247511=CARTESIAN_POINT('Ctrl Pts',(-53.5115841014411,-44.8782418126584,
-26.7379121793796));
#247512=CARTESIAN_POINT('Ctrl Pts',(-52.4260229733029,-45.2319244248767,
-27.1738560637643));
#247513=CARTESIAN_POINT('Ctrl Pts',(-53.1017995598561,-45.4406484702319,
-27.1867616325076));
#247514=CARTESIAN_POINT('Ctrl Pts',(-53.3914367413948,-45.356744566022,
-26.539782270854));
#247515=CARTESIAN_POINT('Ctrl Pts',(-52.3924488199414,-45.3607304740787,
-27.1487530935363));
#247516=CARTESIAN_POINT('Ctrl Pts',(-53.0510858309516,-45.5998124623687,
-27.1481429616664));
#247517=CARTESIAN_POINT('Ctrl Pts',(-53.3074055923412,-45.6073645701926,
-26.4895763391844));
#247518=CARTESIAN_POINT('Ctrl Pts',(-52.3412129907762,-45.4820634699211,
-27.1499944128911));
#247519=CARTESIAN_POINT('Ctrl Pts',(-52.9872085841078,-45.752243332221,
-27.1500170503128));
#247520=CARTESIAN_POINT('Ctrl Pts',(-53.2057691169878,-45.8503754979613,
-26.4920589691078));
#247521=CARTESIAN_POINT('Ctrl Pts',(-52.3451505088232,-45.4735032149087,
-27.1499504714879));
#247522=CARTESIAN_POINT('Ctrl Pts',(-52.3627366640159,-45.4303973965223,
-27.149955201081));
#247523=CARTESIAN_POINT('Ctrl Pts',(-52.3783532542793,-45.3862784926915,
-27.1532451336684));
#247524=CARTESIAN_POINT('Ctrl Pts',(-52.391705759617,-45.3414941638924,
-27.1598205284727));
#247525=CARTESIAN_POINT('Ctrl Pts',(-52.3961646350242,-45.3265390871288,
-27.162016286156));
#247526=CARTESIAN_POINT('Ctrl Pts',(-52.4003708846481,-45.3115102106125,
-27.1645784468541));
#247527=CARTESIAN_POINT('Ctrl Pts',(-52.4043130646239,-45.2964216897362,
-27.1675069834584));
#247528=CARTESIAN_POINT('Ctrl Pts',(-52.4096690785004,-45.275921781643,
-27.1714858182115));
#247529=CARTESIAN_POINT('Ctrl Pts',(-52.4144998716781,-45.2554681891212,
-27.1761072098123));
#247530=CARTESIAN_POINT('Ctrl Pts',(-52.4188376180112,-45.2349418246403,
-27.1813926878448));
#247531=CARTESIAN_POINT('Ctrl Pts',(-52.4231338832753,-45.2146117500013,
-27.1866276218246));
#247532=CARTESIAN_POINT('Ctrl Pts',(-52.4269465681568,-45.1942098686581,
-27.1925141192982));
#247533=CARTESIAN_POINT('Ctrl Pts',(-52.4302758447408,-45.1736199006748,
-27.199112847856));
#247534=CARTESIAN_POINT('Ctrl Pts',(-52.4334702013726,-45.1538643474436,
-27.20544416092));
#247535=CARTESIAN_POINT('Ctrl Pts',(-52.4362195192742,-45.1339352959373,
-27.2124313525265));
#247536=CARTESIAN_POINT('Ctrl Pts',(-52.438494965569,-45.1137349982039,
-27.220162175848));
#247537=CARTESIAN_POINT('Ctrl Pts',(-52.4388077184374,-45.1109585314193,
-27.2212247529671));
#247538=CARTESIAN_POINT('Ctrl Pts',(-52.4391111205152,-45.108180141414,
-27.2223002129721));
#247539=CARTESIAN_POINT('Ctrl Pts',(-52.4394050835699,-45.1053999392664,
-27.2233886092791));
#247540=CARTESIAN_POINT('Ctrl Pts',(-52.4434186911884,-45.0674406095399,
-27.2382489655034));
#247541=CARTESIAN_POINT('Ctrl Pts',(-52.4456709126751,-45.0291509483473,
-27.2555192111601));
#247542=CARTESIAN_POINT('Ctrl Pts',(-52.4460185726721,-44.9908310284022,
-27.2752228594763));
#247543=CARTESIAN_POINT('Ctrl Pts',(-52.4462187383754,-44.9687682837951,
-27.2865672610631));
#247544=CARTESIAN_POINT('Ctrl Pts',(-52.4457875494046,-44.9466963412302,
-27.298717887852));
#247545=CARTESIAN_POINT('Ctrl Pts',(-52.4446976007478,-44.9246794826073,
-27.3116756346609));
#247546=CARTESIAN_POINT('Ctrl Pts',(-52.4429172619991,-44.8887168101594,
-27.332841015796));
#247547=CARTESIAN_POINT('Ctrl Pts',(-52.4393794287248,-44.8528972178532,
-27.3561617363975));
#247548=CARTESIAN_POINT('Ctrl Pts',(-52.4339628625585,-44.8175267802565,
-27.3816307628944));
#247549=CARTESIAN_POINT('Ctrl Pts',(-52.431069078058,-44.79863022828,-27.3952375151907));
#247550=CARTESIAN_POINT('Ctrl Pts',(-52.4276390143528,-44.7798625814266,
-27.4094571301389));
#247551=CARTESIAN_POINT('Ctrl Pts',(-52.423654105959,-44.761276036307,-27.4242857303512));
#247552=CARTESIAN_POINT('Ctrl Pts',(-52.4227084790016,-44.7568654109244,
-27.4278045876786));
#247553=CARTESIAN_POINT('Ctrl Pts',(-52.4216502220477,-44.7521007131266,
-27.4316525297199));
#247554=CARTESIAN_POINT('Ctrl Pts',(-52.4206177053084,-44.7476164130445,
-27.4353204873094));
#247555=CARTESIAN_POINT('Ctrl Pts',(-52.4202128499573,-44.745858094932,
-27.4367587131523));
#247556=CARTESIAN_POINT('Ctrl Pts',(-52.4198123437877,-44.7441426586176,
-27.4381688899413));
#247557=CARTESIAN_POINT('Ctrl Pts',(-52.4194259738441,-44.7425074883477,
-27.4395189486769));
#247558=CARTESIAN_POINT('Ctrl Pts',(-52.4190941693375,-44.7411032464454,
-27.4406783441735));
#247559=CARTESIAN_POINT('Ctrl Pts',(-52.4187728116493,-44.7397582037023,
-27.4417933739563));
#247560=CARTESIAN_POINT('Ctrl Pts',(-52.4184684924213,-44.7384957856129,
-27.442843360707));
#247561=CARTESIAN_POINT('Ctrl Pts',(-52.4122187620994,-44.7125698108868,
-27.464406684453));
#247562=CARTESIAN_POINT('Ctrl Pts',(-52.404731444009,-44.6865268769795,
-27.4876002411829));
#247563=CARTESIAN_POINT('Ctrl Pts',(-52.3958714578284,-44.6606022207932,
-27.5124732459137));
#247564=CARTESIAN_POINT('Ctrl Pts',(-52.3870114716477,-44.6346775646069,
-27.5373462506445));
#247565=CARTESIAN_POINT('Ctrl Pts',(-52.3767786586423,-44.6088708924118,
-27.5638990563341));
#247566=CARTESIAN_POINT('Ctrl Pts',(-52.3650469817685,-44.5834604974678,
-27.5921469614712));
#247567=CARTESIAN_POINT('Ctrl Pts',(-52.3536937597227,-44.5588698222236,
-27.619483611023));
#247568=CARTESIAN_POINT('Ctrl Pts',(-52.3409355488873,-44.5346481494281,
-27.6484094417132));
#247569=CARTESIAN_POINT('Ctrl Pts',(-52.3266618289586,-44.5110837509137,
-27.6789131759605));
#247570=CARTESIAN_POINT('Ctrl Pts',(-52.3138131594986,-44.4898719596604,
-27.7063714980095));
#247571=CARTESIAN_POINT('Ctrl Pts',(-52.2997365041,-44.4691930457479,-27.7351082044668));
#247572=CARTESIAN_POINT('Ctrl Pts',(-52.2843566594156,-44.4492903938695,
-27.7650907920472));
#247573=CARTESIAN_POINT('Ctrl Pts',(-52.2837186874352,-44.4484648111348,
-27.7663345010161));
#247574=CARTESIAN_POINT('Ctrl Pts',(-52.2830784779469,-44.4476405726622,
-27.767580343073));
#247575=CARTESIAN_POINT('Ctrl Pts',(-52.2824360261253,-44.4468176910827,
-27.7688283177016));
#247576=CARTESIAN_POINT('Ctrl Pts',(-52.2813248295301,-44.4453944198295,
-27.7709868377828));
#247577=CARTESIAN_POINT('Ctrl Pts',(-52.2802069226367,-44.4439752050525,
-27.773151741833));
#247578=CARTESIAN_POINT('Ctrl Pts',(-52.2790823052009,-44.4425601308152,
-27.7753230093723));
#247579=CARTESIAN_POINT('Ctrl Pts',(-52.2780757844132,-44.4412936542423,
-27.7772662710044));
#247580=CARTESIAN_POINT('Ctrl Pts',(-52.2766634267718,-44.4395338119596,
-27.7799843776605));
#247581=CARTESIAN_POINT('Ctrl Pts',(-52.2759205732601,-44.4386144114997,
-27.7814106877139));
#247582=CARTESIAN_POINT('Ctrl Pts',(-52.2758334131032,-44.438506536815,
-27.7815780388889));
#247583=CARTESIAN_POINT('Ctrl Pts',(-52.2757555052074,-44.4384101877566,
-27.7817275847392));
#247584=CARTESIAN_POINT('Ctrl Pts',(-52.2756886070813,-44.4383274928831,
-27.7818559746203));
#247585=CARTESIAN_POINT('Ctrl Pts',(-52.2676800702558,-44.4284278891467,
-27.7972258384781));
#247586=CARTESIAN_POINT('Ctrl Pts',(-52.2586467068395,-44.4178780252673,
-27.8142376774287));
#247587=CARTESIAN_POINT('Ctrl Pts',(-52.2484496368236,-44.4068934908634,
-27.8329545686498));
#247588=CARTESIAN_POINT('Ctrl Pts',(-52.2386193771832,-44.39630409361,-27.8509981733398));
#247589=CARTESIAN_POINT('Ctrl Pts',(-52.2277071249877,-44.3853106597761,
-27.8706270447069));
#247590=CARTESIAN_POINT('Ctrl Pts',(-52.215582220397,-44.3741516473034,
-27.8918817944962));
#247591=CARTESIAN_POINT('Ctrl Pts',(-52.2042196016309,-44.3636941955698,
-27.911800270309));
#247592=CARTESIAN_POINT('Ctrl Pts',(-52.1917916195219,-44.3530914633972,
-27.9331470466369));
#247593=CARTESIAN_POINT('Ctrl Pts',(-52.1781914581759,-44.3425794767405,
-27.9559337338037));
#247594=CARTESIAN_POINT('Ctrl Pts',(-52.165085428788,-44.332449420005,-27.9778925167962));
#247595=CARTESIAN_POINT('Ctrl Pts',(-52.1508905243962,-44.3224035921207,
-28.0011889148053));
#247596=CARTESIAN_POINT('Ctrl Pts',(-52.1355169284213,-44.31269102401,-28.025806121144));
#247597=CARTESIAN_POINT('Ctrl Pts',(-52.120939443385,-44.3034814144607,
-28.0491485426324));
#247598=CARTESIAN_POINT('Ctrl Pts',(-52.1053019503684,-44.2945715114819,
-28.0736787774362));
#247599=CARTESIAN_POINT('Ctrl Pts',(-52.0885370500198,-44.2862079032681,
-28.0993528411084));
#247600=CARTESIAN_POINT('Ctrl Pts',(-52.0778243289322,-44.2808635826806,
-28.1157584908639));
#247601=CARTESIAN_POINT('Ctrl Pts',(-52.0666514599927,-44.2757430047416,
-28.1326305840812));
#247602=CARTESIAN_POINT('Ctrl Pts',(-52.0550036453325,-44.2709183219374,
-28.14995));
#247603=CARTESIAN_POINT('Ctrl Pts',(-53.3058498568936,-43.7066435869166,
-28.4919701433257));
#247604=CARTESIAN_POINT('Ctrl Pts',(-53.325878097415,-43.7149395557728,
-28.4324091977161));
#247605=CARTESIAN_POINT('Ctrl Pts',(-53.3450421162736,-43.7257975480542,
-28.3723481914006));
#247606=CARTESIAN_POINT('Ctrl Pts',(-53.3631923272661,-43.7392286476817,
-28.3121551709553));
#247607=CARTESIAN_POINT('Ctrl Pts',(-53.3817311398638,-43.7529473112873,
-28.2506733994109));
#247608=CARTESIAN_POINT('Ctrl Pts',(-53.3992119966698,-43.7693504901722,
-28.1890545402301));
#247609=CARTESIAN_POINT('Ctrl Pts',(-53.4154902120498,-43.7884000440542,
-28.1277059557092));
#247610=CARTESIAN_POINT('Ctrl Pts',(-53.4318778232817,-43.807577618246,
-28.0659450851662));
#247611=CARTESIAN_POINT('Ctrl Pts',(-53.4470463242961,-43.8294371266463,
-28.0044589051888));
#247612=CARTESIAN_POINT('Ctrl Pts',(-53.4608667701963,-43.8538903731411,
-27.9436674521647));
#247613=CARTESIAN_POINT('Ctrl Pts',(-53.4746634610095,-43.8783015885027,
-27.8829804897104));
#247614=CARTESIAN_POINT('Ctrl Pts',(-53.4871165121676,-43.9052973926726,
-27.8229866659694));
#247615=CARTESIAN_POINT('Ctrl Pts',(-53.4981196516723,-43.934743987147,
-27.7640964128422));
#247616=CARTESIAN_POINT('Ctrl Pts',(-53.5007377563813,-43.9417505571923,
-27.7500839713058));
#247617=CARTESIAN_POINT('Ctrl Pts',(-53.503273878774,-43.9488956857912,
-27.7361339461954));
#247618=CARTESIAN_POINT('Ctrl Pts',(-53.5057267914276,-43.9561772098616,
-27.7222517274201));
#247619=CARTESIAN_POINT('Ctrl Pts',(-53.516015172449,-43.98671849063,-27.6640248044291));
#247620=CARTESIAN_POINT('Ctrl Pts',(-53.524834739455,-44.0196559383853,
-27.607006864364));
#247621=CARTESIAN_POINT('Ctrl Pts',(-53.5321633779772,-44.0547175334498,
-27.5515400465457));
#247622=CARTESIAN_POINT('Ctrl Pts',(-53.539448489013,-44.0895708847729,
-27.4964026666108));
#247623=CARTESIAN_POINT('Ctrl Pts',(-53.5452603272204,-44.1265226675562,
-27.4427986309046));
#247624=CARTESIAN_POINT('Ctrl Pts',(-53.5496025507427,-44.1652740000725,
-27.3910329022814));
#247625=CARTESIAN_POINT('Ctrl Pts',(-53.5538697570887,-44.2033558563332,
-27.3401614893866));
#247626=CARTESIAN_POINT('Ctrl Pts',(-53.5567177527472,-44.2431750607486,
-27.2910658408008));
#247627=CARTESIAN_POINT('Ctrl Pts',(-53.5581740600656,-44.2844256199221,
-27.2439978212674));
#247628=CARTESIAN_POINT('Ctrl Pts',(-53.5591211928104,-44.3112535805061,
-27.2133863823412));
#247629=CARTESIAN_POINT('Ctrl Pts',(-53.5594801618893,-44.3386865381858,
-27.1836317992188));
#247630=CARTESIAN_POINT('Ctrl Pts',(-53.5592639447716,-44.3666367581605,
-27.1547933762998));
#247631=CARTESIAN_POINT('Ctrl Pts',(-55.7504626785233,-26.3185679674161,
-36.6521851368644));
#247632=CARTESIAN_POINT('Ctrl Pts',(-55.5392505223476,-26.2310810277901,
-37.5833004572826));
#247633=CARTESIAN_POINT('Ctrl Pts',(-55.8969434195062,-25.3423960630483,
-37.6224808631404));
#247634=CARTESIAN_POINT('Ctrl Pts',(-55.9208644997853,-26.3891507128358,
-36.6974706218906));
#247635=CARTESIAN_POINT('Ctrl Pts',(-55.6480848386771,-26.2761616776646,
-37.5999312032258));
#247636=CARTESIAN_POINT('Ctrl Pts',(-55.996440168022,-25.3971431190627,
-37.6496522218102));
#247637=CARTESIAN_POINT('Ctrl Pts',(-56.0836332067825,-26.456571718804,
-36.762150428292));
#247638=CARTESIAN_POINT('Ctrl Pts',(-55.7548998347942,-26.3204058977241,
-37.6301299838414));
#247639=CARTESIAN_POINT('Ctrl Pts',(-56.0914939922152,-25.4493175282016,
-37.6884594400956));
#247640=CARTESIAN_POINT('Ctrl Pts',(-56.2387979627755,-26.5208430651387,
-36.8455500552174));
#247641=CARTESIAN_POINT('Ctrl Pts',(-55.8586323634263,-26.3633733179405,
-37.6741999657538));
#247642=CARTESIAN_POINT('Ctrl Pts',(-56.182121826823,-25.498964054333,-37.7384998141522));
#247643=CARTESIAN_POINT('',(-55.8969434190161,-25.3423960644772,-37.6224808629378));
#247644=CARTESIAN_POINT('Origin',(-55.5095456070917,-25.1140012264302,-39.2553865411486));
#247645=CARTESIAN_POINT('',(-55.7504626788662,-26.3185679665883,-36.6521851368644));
#247646=CARTESIAN_POINT('Origin',(-55.1862083484817,-26.0848461712916,-39.1409509186699));
#247647=CARTESIAN_POINT('Origin',(-56.1331461108883,-25.3946884349048,-36.6521851368644));
#247648=CARTESIAN_POINT('Ctrl Pts',(-55.8969434195062,-25.3423960630483,
-37.6224808631404));
#247649=CARTESIAN_POINT('Ctrl Pts',(-55.5392505223476,-26.23108102779,-37.5833004572826));
#247650=CARTESIAN_POINT('Ctrl Pts',(-55.7504626785233,-26.3185679674161,
-36.6521851368644));
#247651=CARTESIAN_POINT('Ctrl Pts',(-55.0816420516339,-25.0053755109404,
-37.405845897407));
#247652=CARTESIAN_POINT('Ctrl Pts',(-54.7245658074498,-25.8936275698287,
-37.3661635279098));
#247653=CARTESIAN_POINT('Ctrl Pts',(-54.9353008930509,-25.9809169003452,
-36.4355501696994));
#247654=CARTESIAN_POINT('Ctrl Pts',(-54.2663041831515,-24.6683705249141,
-37.1893551119314));
#247655=CARTESIAN_POINT('Ctrl Pts',(-53.9096353215527,-25.5560723101748,
-37.1490863785069));
#247656=CARTESIAN_POINT('Ctrl Pts',(-54.1201064257051,-25.643252295999,
-36.2190593841676));
#247657=CARTESIAN_POINT('Ctrl Pts',(-53.45092477896,-24.3313834513715,-36.9730300997693));
#247658=CARTESIAN_POINT('Ctrl Pts',(-53.094385962218,-25.218384968819,-36.9320687979064));
#247659=CARTESIAN_POINT('Ctrl Pts',(-53.3048743824714,-25.3055721272105,
-36.0027343734933));
#247660=CARTESIAN_POINT('',(-53.3048743827289,-25.3055721265897,-36.0027343734921));
#247661=CARTESIAN_POINT('',(-53.4509247784284,-24.3313834527923,-36.973030099559));
#247662=CARTESIAN_POINT('Origin',(-53.6875578148366,-24.3816925946992,-36.0027343734933));
#247663=CARTESIAN_POINT('Origin',(2171.9425404878,-684.86429331655,-7395.89927355314));
#247664=CARTESIAN_POINT('Origin',(1653.54988594156,681.696820180718,-7571.86104389537));
#247665=CARTESIAN_POINT('Origin',(-53.6875578148366,-24.3816925946992,-36.0027343734933));
#247666=CARTESIAN_POINT('',(-52.7094196628928,-24.1737364557848,-36.0027343734933));
#247667=CARTESIAN_POINT('Origin',(-53.6875578148366,-24.3816925946992,-36.0027343734933));
#247668=CARTESIAN_POINT('Origin',(-53.6875578148366,-24.3816925946992,-36.0027343734933));
#247669=CARTESIAN_POINT('Origin',(-53.6875578148366,-24.3816925946992,-55.24995));
#247670=CARTESIAN_POINT('',(-53.3048743824714,-25.3055721272105,-28.64995));
#247671=CARTESIAN_POINT('',(-52.7094196628928,-24.1737364557848,-28.64995));
#247672=CARTESIAN_POINT('Origin',(-53.6875578148365,-24.3816925946992,-28.64995));
#247673=CARTESIAN_POINT('',(-52.7094196628929,-24.1737364557848,-55.24995));
#247674=CARTESIAN_POINT('',(-53.3048743824714,-25.3055721272105,-36.0027343734933));
#247675=CARTESIAN_POINT('Ctrl Pts',(-52.7094196628928,-24.1737364557848,
-28.64995));
#247676=CARTESIAN_POINT('Ctrl Pts',(-52.5364563745167,-24.9872829667439,
-28.64995));
#247677=CARTESIAN_POINT('Ctrl Pts',(-53.3048743824714,-25.3055721272105,
-28.64995));
#247678=CARTESIAN_POINT('Ctrl Pts',(-52.709419661177,-24.1737364638552,
-28.4522245494749));
#247679=CARTESIAN_POINT('Ctrl Pts',(-52.5364564758209,-24.9872830087068,
-28.4725838150348));
#247680=CARTESIAN_POINT('Ctrl Pts',(-53.3048744251021,-25.3055721448687,
-28.584041512097));
#247681=CARTESIAN_POINT('Ctrl Pts',(-52.7478129283917,-24.18436087427,-28.2540622406394));
#247682=CARTESIAN_POINT('Ctrl Pts',(-52.5661365121454,-24.9995768822825,
-28.2939908458137));
#247683=CARTESIAN_POINT('Ctrl Pts',(-53.3173284366389,-25.3107307653532,
-28.5179874195064));
#247684=CARTESIAN_POINT('Ctrl Pts',(-52.8580751908351,-24.2149033446468,
-27.980658832839));
#247685=CARTESIAN_POINT('Ctrl Pts',(-52.652344235038,-25.0352852902864,
-28.0433521906345));
#247686=CARTESIAN_POINT('Ctrl Pts',(-53.3530964953807,-25.3255463803838,
-28.4268529412997));
#247687=CARTESIAN_POINT('Ctrl Pts',(-52.9030108008295,-24.227353663694,
-27.8942996676949));
#247688=CARTESIAN_POINT('Ctrl Pts',(-52.6878047550409,-25.0499735186003,
-27.9629661172779));
#247689=CARTESIAN_POINT('Ctrl Pts',(-53.3676733222451,-25.3315842997674,
-28.3980665530275));
#247690=CARTESIAN_POINT('Ctrl Pts',(-53.0090582923966,-24.2567524735255,
-27.7310236386286));
#247691=CARTESIAN_POINT('Ctrl Pts',(-52.7723574461003,-25.0849963899722,
-27.8083075481136));
#247692=CARTESIAN_POINT('Ctrl Pts',(-53.4020750585865,-25.3458339655292,
-28.343641215747));
#247693=CARTESIAN_POINT('Ctrl Pts',(-53.0705147380728,-24.2737967964412,
-27.6541049946696));
#247694=CARTESIAN_POINT('Ctrl Pts',(-52.8218880255259,-25.1055126277224,
-27.7338993339231));
#247695=CARTESIAN_POINT('Ctrl Pts',(-53.4220117490162,-25.354092013094,
-28.3180016675465));
#247696=CARTESIAN_POINT('Ctrl Pts',(-53.271425280039,-24.329554436308,-27.4475644489341));
#247697=CARTESIAN_POINT('Ctrl Pts',(-52.986650618978,-25.1737595285021,
-27.5280515041845));
#247698=CARTESIAN_POINT('Ctrl Pts',(-53.487189224505,-25.3810894074027,
-28.2491548109981));
#247699=CARTESIAN_POINT('Ctrl Pts',(-53.4327530160742,-24.374374360655,
-27.3369024763037));
#247700=CARTESIAN_POINT('Ctrl Pts',(-53.1222572959679,-25.2299296532595,
-27.4101121807186));
#247701=CARTESIAN_POINT('Ctrl Pts',(-53.5395274002361,-25.4027685896203,
-28.2122674917371));
#247702=CARTESIAN_POINT('Ctrl Pts',(-53.7793279888276,-24.4708259099888,
-27.1890241015641));
#247703=CARTESIAN_POINT('Ctrl Pts',(-53.4249980376239,-25.3553289743366,
-27.233364160377));
#247704=CARTESIAN_POINT('Ctrl Pts',(-53.6519699663366,-25.4493438254873,
-28.1629747008856));
#247705=CARTESIAN_POINT('Ctrl Pts',(-53.9688606392783,-24.5236518439783,
-27.14995));
#247706=CARTESIAN_POINT('Ctrl Pts',(-53.5971493048004,-25.4266363639807,
-27.1731944252321));
#247707=CARTESIAN_POINT('Ctrl Pts',(-53.7134648732951,-25.4748158499664,
-28.1499500287456));
#247708=CARTESIAN_POINT('Ctrl Pts',(-54.1572878000337,-24.5762611252212,
-27.14995));
#247709=CARTESIAN_POINT('Ctrl Pts',(-53.7746043676686,-25.5001406577324,
-27.14995));
#247710=CARTESIAN_POINT('Ctrl Pts',(-53.7746043676686,-25.5001406577325,
-28.14995));
#247711=CARTESIAN_POINT('',(-53.7746043676686,-25.5001406577325,-28.14995));
#247712=CARTESIAN_POINT('Origin',(-54.1572878000337,-24.5762611252212,-28.14995));
#247713=CARTESIAN_POINT('Ctrl Pts',(-52.7094196628928,-24.1737364557848,
-28.64995));
#247714=CARTESIAN_POINT('Ctrl Pts',(-52.7094196623825,-24.1737364581851,
-28.5911408946036));
#247715=CARTESIAN_POINT('Ctrl Pts',(-52.7128129245313,-24.1746866093358,
-28.5317681320255));
#247716=CARTESIAN_POINT('Ctrl Pts',(-52.7197005445987,-24.1766085300182,
-28.4722462243672));
#247717=CARTESIAN_POINT('Ctrl Pts',(-52.7264036735814,-24.1784789703302,
-28.4143186644234));
#247718=CARTESIAN_POINT('Ctrl Pts',(-52.736416539613,-24.1812698432637,
-28.3562495690729));
#247719=CARTESIAN_POINT('Ctrl Pts',(-52.7498419130618,-24.1850037883381,
-28.2984688589346));
#247720=CARTESIAN_POINT('Ctrl Pts',(-52.7627900625724,-24.1886050050396,
-28.242742046079));
#247721=CARTESIAN_POINT('Ctrl Pts',(-52.7789125032754,-24.1930834657548,
-28.1872833154782));
#247722=CARTESIAN_POINT('Ctrl Pts',(-52.7983093839467,-24.1984616617822,
-28.1325264875571));
#247723=CARTESIAN_POINT('Ctrl Pts',(-52.8031630965455,-24.1998074564107,
-28.1188245985753));
#247724=CARTESIAN_POINT('Ctrl Pts',(-52.8082218780349,-24.2012095986938,
-28.1051669098548));
#247725=CARTESIAN_POINT('Ctrl Pts',(-52.8134873707718,-24.2026684605618,
-28.0915607337429));
#247726=CARTESIAN_POINT('Ctrl Pts',(-52.8160396530933,-24.203375598059,
-28.0849655669677));
#247727=CARTESIAN_POINT('Ctrl Pts',(-52.8186421023036,-24.2040965209239,
-28.0783783736381));
#247728=CARTESIAN_POINT('Ctrl Pts',(-52.8212948296775,-24.2048312666952,
-28.0718006689512));
#247729=CARTESIAN_POINT('Ctrl Pts',(-52.8382986680715,-24.2095409471842,
-28.0296379391516));
#247730=CARTESIAN_POINT('Ctrl Pts',(-52.8572442526181,-24.2147843387079,
-27.9880389891984));
#247731=CARTESIAN_POINT('Ctrl Pts',(-52.878156523599,-24.2205704318867,
-27.947193588991));
#247732=CARTESIAN_POINT('Ctrl Pts',(-52.8990687945799,-24.2263565250655,
-27.9063481887835));
#247733=CARTESIAN_POINT('Ctrl Pts',(-52.9219478322349,-24.2326853437507,
-27.8662563850818));
#247734=CARTESIAN_POINT('Ctrl Pts',(-52.9467712010785,-24.2395527832638,
-27.8270804380994));
#247735=CARTESIAN_POINT('Ctrl Pts',(-52.949825104249,-24.2403976522835,
-27.8222608042517));
#247736=CARTESIAN_POINT('Ctrl Pts',(-52.9529075011859,-24.2412504051661,
-27.8174563757837));
#247737=CARTESIAN_POINT('Ctrl Pts',(-52.9560186463722,-24.2421111243394,
-27.8126668029462));
#247738=CARTESIAN_POINT('Ctrl Pts',(-52.9780675057062,-24.2482110890927,
-27.7787228333006));
#247739=CARTESIAN_POINT('Ctrl Pts',(-53.0016171799217,-24.2547269870702,
-27.7455215338308));
#247740=CARTESIAN_POINT('Ctrl Pts',(-53.0265760983851,-24.2616377598036,
-27.7132033055052));
#247741=CARTESIAN_POINT('Ctrl Pts',(-53.0289546891742,-24.2622963580675,
-27.7101233707585));
#247742=CARTESIAN_POINT('Ctrl Pts',(-53.0313461012784,-24.2629585489486,
-27.7070514878665));
#247743=CARTESIAN_POINT('Ctrl Pts',(-53.0337502686034,-24.2636243179425,
-27.7039877996));
#247744=CARTESIAN_POINT('Ctrl Pts',(-53.049345815812,-24.2679430821423,
-27.6841140185629));
#247745=CARTESIAN_POINT('Ctrl Pts',(-53.0654807379639,-24.2724132274182,
-27.6645804228689));
#247746=CARTESIAN_POINT('Ctrl Pts',(-53.0821467732563,-24.2770331862523,
-27.6454233566967));
#247747=CARTESIAN_POINT('Ctrl Pts',(-53.0904797909025,-24.2793431656693,
-27.6358448236106));
#247748=CARTESIAN_POINT('Ctrl Pts',(-53.0989456970375,-24.2816906220258,
-27.6263605258861));
#247749=CARTESIAN_POINT('Ctrl Pts',(-53.107543962866,-24.2840754684918,
-27.6169758713563));
#247750=CARTESIAN_POINT('Ctrl Pts',(-53.1118430957802,-24.2852678917247,
-27.6122835440914));
#247751=CARTESIAN_POINT('Ctrl Pts',(-53.1161753245165,-24.2864696637492,
-27.6076161364291));
#247752=CARTESIAN_POINT('Ctrl Pts',(-53.1205406140096,-24.2876807803625,
-27.6029743847767));
#247753=CARTESIAN_POINT('Ctrl Pts',(-53.1227232587562,-24.2882863386692,
-27.6006535089506));
#247754=CARTESIAN_POINT('Ctrl Pts',(-53.1249141690336,-24.2888942331957,
-27.5983390477616));
#247755=CARTESIAN_POINT('Ctrl Pts',(-53.1271133420458,-24.289504463756,
-27.5960310976378));
#247756=CARTESIAN_POINT('Ctrl Pts',(-53.1290394097302,-24.2900389125492,
-27.5940097613784));
#247757=CARTESIAN_POINT('Ctrl Pts',(-53.1316083240647,-24.2907518064033,
-27.5913323973162));
#247758=CARTESIAN_POINT('Ctrl Pts',(-53.1331478191429,-24.291179042896,
-27.5897360553741));
#247759=CARTESIAN_POINT('Ctrl Pts',(-53.1333661106969,-24.2912396225752,
-27.5895097032615));
#247760=CARTESIAN_POINT('Ctrl Pts',(-53.1335636543095,-24.2912944447278,
-27.5893050130261));
#247761=CARTESIAN_POINT('Ctrl Pts',(-53.1337356439429,-24.2913421754602,
-27.5891268809258));
#247762=CARTESIAN_POINT('Ctrl Pts',(-53.1349790940228,-24.2916872589505,
-27.5878390220597));
#247763=CARTESIAN_POINT('Ctrl Pts',(-53.1362288224179,-24.292034158616,
-27.5865494247887));
#247764=CARTESIAN_POINT('Ctrl Pts',(-53.1374848551265,-24.2923828799776,
-27.5852581657108));
#247765=CARTESIAN_POINT('Ctrl Pts',(-53.1573367030932,-24.2978944907865,
-27.5648495579378));
#247766=CARTESIAN_POINT('Ctrl Pts',(-53.1788814445988,-24.3038939694486,
-27.5439062900081));
#247767=CARTESIAN_POINT('Ctrl Pts',(-53.2022803852861,-24.3104194037623,
-27.5226638270178));
#247768=CARTESIAN_POINT('Ctrl Pts',(-53.2241989150423,-24.316531985015,
-27.5027653383055));
#247769=CARTESIAN_POINT('Ctrl Pts',(-53.2477448421254,-24.3231061872658,
-27.4826043546765));
#247770=CARTESIAN_POINT('Ctrl Pts',(-53.2730374239921,-24.330169670055,
-27.4624174062464));
#247771=CARTESIAN_POINT('Ctrl Pts',(-53.2974626786647,-24.3369909335745,
-27.4429227038444));
#247772=CARTESIAN_POINT('Ctrl Pts',(-53.32351725015,-24.34426860855,-27.4234036353704));
#247773=CARTESIAN_POINT('Ctrl Pts',(-53.3512899421954,-24.3520224739381,
-27.4041157829931));
#247774=CARTESIAN_POINT('Ctrl Pts',(-53.3776321832186,-24.3593769713192,
-27.3858213643135));
#247775=CARTESIAN_POINT('Ctrl Pts',(-53.4055203797343,-24.3671599432765,
-27.367734961942));
#247776=CARTESIAN_POINT('Ctrl Pts',(-53.4350087013824,-24.3753822836722,
-27.3501144502417));
#247777=CARTESIAN_POINT('Ctrl Pts',(-53.4606967054725,-24.3825449671316,
-27.3347647880254));
#247778=CARTESIAN_POINT('Ctrl Pts',(-53.4875988516975,-24.3900410344375,
-27.3197691139046));
#247779=CARTESIAN_POINT('Ctrl Pts',(-53.5157338737957,-24.3978729492133,
-27.3053249748031));
#247780=CARTESIAN_POINT('Ctrl Pts',(-53.5444237498552,-24.4058593180685,
-27.2905959811964));
#247781=CARTESIAN_POINT('Ctrl Pts',(-53.5745393269424,-24.414230882692,
-27.2763718188066));
#247782=CARTESIAN_POINT('Ctrl Pts',(-53.6059083724541,-24.4229441848809,
-27.2629869669082));
#247783=CARTESIAN_POINT('Ctrl Pts',(-53.6209445451166,-24.4271207453735,
-27.2565711853336));
#247784=CARTESIAN_POINT('Ctrl Pts',(-53.6363003452189,-24.4313846413295,
-27.250334067976));
#247785=CARTESIAN_POINT('Ctrl Pts',(-53.6519543084626,-24.4357303721746,
-27.2443059491307));
#247786=CARTESIAN_POINT('Ctrl Pts',(-53.6881882089995,-24.445789344254,
-27.2303527888184));
#247787=CARTESIAN_POINT('Ctrl Pts',(-53.725938196618,-24.4562659038156,
-27.2175466562902));
#247788=CARTESIAN_POINT('Ctrl Pts',(-53.7651942802866,-24.4671634152115,
-27.2061405089377));
#247789=CARTESIAN_POINT('Ctrl Pts',(-53.8008938818551,-24.4770736451316,
-27.1957677239357));
#247790=CARTESIAN_POINT('Ctrl Pts',(-53.837839120707,-24.4873320299336,
-27.1865530465471));
#247791=CARTESIAN_POINT('Ctrl Pts',(-53.8759926239344,-24.4979329922837,
-27.1787222605505));
#247792=CARTESIAN_POINT('Ctrl Pts',(-53.9129275881487,-24.5081953832024,
-27.1711415726428));
#247793=CARTESIAN_POINT('Ctrl Pts',(-53.9509952084681,-24.5187789120278,
-27.1648577255513));
#247794=CARTESIAN_POINT('Ctrl Pts',(-53.9901288761984,-24.5296696175481,
-27.1601094004118));
#247795=CARTESIAN_POINT('Ctrl Pts',(-54.0275148318809,-24.540073943479,
-27.1555731357699));
#247796=CARTESIAN_POINT('Ctrl Pts',(-54.0658739630156,-24.5507586832984,
-27.1524383207612));
#247797=CARTESIAN_POINT('Ctrl Pts',(-54.1051139954855,-24.5617023371624,
-27.1509446747599));
#247798=CARTESIAN_POINT('Ctrl Pts',(-54.1223393936945,-24.5665063289994,
-27.1502890013179));
#247799=CARTESIAN_POINT('Ctrl Pts',(-54.1397340652788,-24.571360083541,
-27.14995));
#247800=CARTESIAN_POINT('Ctrl Pts',(-54.1572878000336,-24.5762611252214,
-27.14995));
#247801=CARTESIAN_POINT('Ctrl Pts',(-53.7746043676686,-25.5001406577325,
-28.14995));
#247802=CARTESIAN_POINT('Ctrl Pts',(-53.7400313146559,-25.485820030282,
-28.14995));
#247803=CARTESIAN_POINT('Ctrl Pts',(-53.7054590384781,-25.471499724607,
-28.1541104421107));
#247804=CARTESIAN_POINT('Ctrl Pts',(-53.6718442132407,-25.4575760080969,
-28.1621235025489));
#247805=CARTESIAN_POINT('Ctrl Pts',(-53.6457564066785,-25.4467700848063,
-28.1683422815909));
#247806=CARTESIAN_POINT('Ctrl Pts',(-53.6202442011515,-25.4362025832709,
-28.1768826771709));
#247807=CARTESIAN_POINT('Ctrl Pts',(-53.5957486758074,-25.4260562044559,
-28.187621076324));
#247808=CARTESIAN_POINT('Ctrl Pts',(-53.562916032086,-25.4124564781379,
-28.2020143187052));
#247809=CARTESIAN_POINT('Ctrl Pts',(-53.5314342202936,-25.3994162847254,
-28.2205659399078));
#247810=CARTESIAN_POINT('Ctrl Pts',(-53.5022513514982,-25.3873283446814,
-28.242657912297));
#247811=CARTESIAN_POINT('Ctrl Pts',(-53.4814624525329,-25.3787173007832,
-28.2583954939983));
#247812=CARTESIAN_POINT('Ctrl Pts',(-53.461840238405,-25.3705895135676,
-28.2759308966333));
#247813=CARTESIAN_POINT('Ctrl Pts',(-53.4437375711116,-25.3630911432596,
-28.2950527119614));
#247814=CARTESIAN_POINT('Ctrl Pts',(-53.4271303962018,-25.3562122261793,
-28.3125948413394));
#247815=CARTESIAN_POINT('Ctrl Pts',(-53.4116292338695,-25.3497914345087,
-28.3316389938391));
#247816=CARTESIAN_POINT('Ctrl Pts',(-53.3975863960872,-25.3439747006451,
-28.3517369823159));
#247817=CARTESIAN_POINT('Ctrl Pts',(-53.3932029374535,-25.3421590126289,
-28.3580105505558));
#247818=CARTESIAN_POINT('Ctrl Pts',(-53.3889617532722,-25.3404022566205,
-28.3643871416707));
#247819=CARTESIAN_POINT('Ctrl Pts',(-53.3848741883221,-25.338709131781,
-28.3708538828368));
#247820=CARTESIAN_POINT('Ctrl Pts',(-53.3717588132892,-25.3332765655668,
-28.3916030909026));
#247821=CARTESIAN_POINT('Ctrl Pts',(-53.3601568354504,-25.3284708689956,
-28.4132788617422));
#247822=CARTESIAN_POINT('Ctrl Pts',(-53.3500641460493,-25.3242903401649,
-28.4359756086709));
#247823=CARTESIAN_POINT('Ctrl Pts',(-53.3491805785529,-25.3239243545245,
-28.4379626021337));
#247824=CARTESIAN_POINT('Ctrl Pts',(-53.348308605256,-25.323563171359,-28.4399574365791));
#247825=CARTESIAN_POINT('Ctrl Pts',(-53.3474482388699,-25.3232067959332,
-28.4419601846317));
#247826=CARTESIAN_POINT('Ctrl Pts',(-53.3452788063953,-25.3223081875796,
-28.4470101572176));
#247827=CARTESIAN_POINT('Ctrl Pts',(-53.3431878049941,-25.3214420664403,
-28.4520995820139));
#247828=CARTESIAN_POINT('Ctrl Pts',(-53.3411738091334,-25.3206078420402,
-28.4572311007019));
#247829=CARTESIAN_POINT('Ctrl Pts',(-53.3367395978111,-25.3187711315721,
-28.4685291568261));
#247830=CARTESIAN_POINT('Ctrl Pts',(-53.3327048917567,-25.3170999016042,
-28.4799940523333));
#247831=CARTESIAN_POINT('Ctrl Pts',(-53.3290655208329,-25.315592424809,
-28.4916214078187));
#247832=CARTESIAN_POINT('Ctrl Pts',(-53.3209950143511,-25.3122495115691,
-28.5174057122425));
#247833=CARTESIAN_POINT('Ctrl Pts',(-53.3148900299868,-25.3097207442473,
-28.5439203032342));
#247834=CARTESIAN_POINT('Ctrl Pts',(-53.3108262630393,-25.3080374768633,
-28.5708597425681));
#247835=CARTESIAN_POINT('Ctrl Pts',(-53.3068954035518,-25.3064092615518,
-28.5969181145328));
#247836=CARTESIAN_POINT('Ctrl Pts',(-53.3048743824714,-25.3055721272105,
-28.6233752345599));
#247837=CARTESIAN_POINT('Ctrl Pts',(-53.3048743824714,-25.3055721272105,
-28.64995));
#247838=CARTESIAN_POINT('Origin',(0.757869275948407,-1.82965828450052,-28.14995));
#247839=CARTESIAN_POINT('',(-53.9354576832443,-25.5667682825966,-28.14995));
#247840=CARTESIAN_POINT('Ctrl Pts',(-45.8309904068109,-42.7275323570066,
-36.9730300997693));
#247841=CARTESIAN_POINT('Ctrl Pts',(-46.2060841796464,-41.8482165540222,
-36.9320687979064));
#247842=CARTESIAN_POINT('Ctrl Pts',(-46.4165725998998,-41.9354037124137,
-36.0027343734933));
#247843=CARTESIAN_POINT('Ctrl Pts',(-46.7534506368482,-43.1104816252375,
-37.2179244522577));
#247844=CARTESIAN_POINT('Ctrl Pts',(-47.1290415487049,-42.2305180137903,
-37.1777580130411));
#247845=CARTESIAN_POINT('Ctrl Pts',(-47.3394696831815,-42.3176802009835,
-36.2476287235887));
#247846=CARTESIAN_POINT('Ctrl Pts',(-47.6758891195153,-43.4933769026755,
-37.463031047121));
#247847=CARTESIAN_POINT('Ctrl Pts',(-48.0515862359126,-42.6126485351233,
-37.4235224076789));
#247848=CARTESIAN_POINT('Ctrl Pts',(-48.2623182897497,-42.6999366098412,
-36.4927353185438));
#247849=CARTESIAN_POINT('Ctrl Pts',(-48.5983086357822,-43.8762256986891,
-37.7083189393204));
#247850=CARTESIAN_POINT('Ctrl Pts',(-48.9738234376089,-42.9946516917827,
-37.6693623947416));
#247851=CARTESIAN_POINT('Ctrl Pts',(-49.1851254866488,-43.0821758662522,
-36.7380232130444));
#247852=CARTESIAN_POINT('',(-46.4165725996979,-41.9354037129011,-36.0027343734932));
#247853=CARTESIAN_POINT('Origin',(1674.91246247384,671.062426055257,-7635.73196693816));
#247854=CARTESIAN_POINT('',(-45.8309904070058,-42.727532356592,-36.9730300996838));
#247855=CARTESIAN_POINT('Origin',(1064.10886932915,2004.44184216393,-7418.93704427589));
#247856=CARTESIAN_POINT('Origin',(-46.0338891675347,-42.859283244925,-36.0027343734933));
#247857=CARTESIAN_POINT('Origin',(-46.0338891675347,-42.859283244925,-36.0027343734933));
#247858=CARTESIAN_POINT('',(-45.1951938513423,-42.314682320764,-36.0027343734933));
#247859=CARTESIAN_POINT('Origin',(-46.0338891675347,-42.8592832449249,-36.0027343734933));
#247860=CARTESIAN_POINT('Origin',(-46.0338891675347,-42.8592832449249,-36.0027343734933));
#247861=CARTESIAN_POINT('Origin',(-46.0338891675347,-42.8592832449249,-55.24995));
#247862=CARTESIAN_POINT('',(-45.1951938513423,-42.314682320764,-28.64995));
#247863=CARTESIAN_POINT('',(-46.4165725998998,-41.9354037124137,-28.64995));
#247864=CARTESIAN_POINT('Origin',(-46.0338891675347,-42.8592832449249,-28.64995));
#247865=CARTESIAN_POINT('',(-46.4165725998998,-41.9354037124137,-7.34233313511216E-15));
#247866=CARTESIAN_POINT('',(-45.1951938513423,-42.314682320764,-55.24995));
#247867=CARTESIAN_POINT('Ctrl Pts',(-46.5036191527319,-43.0538517754469,
-27.14995));
#247868=CARTESIAN_POINT('Ctrl Pts',(-46.886302585097,-42.1299722429357,
-27.1499500000001));
#247869=CARTESIAN_POINT('Ctrl Pts',(-46.886302585097,-42.1299722429356,
-28.14995));
#247870=CARTESIAN_POINT('Ctrl Pts',(-46.3336353463682,-42.9580702414852,
-27.14995));
#247871=CARTESIAN_POINT('Ctrl Pts',(-46.7093272072494,-42.0566666412253,
-27.1731316302543));
#247872=CARTESIAN_POINT('Ctrl Pts',(-46.8253261772413,-42.104714987817,
-28.149950041602));
#247873=CARTESIAN_POINT('Ctrl Pts',(-46.1640497973707,-42.8624134989651,
-27.1881541167863));
#247874=CARTESIAN_POINT('Ctrl Pts',(-46.5389139774209,-41.9860791702219,
-27.2322497625617));
#247875=CARTESIAN_POINT('Ctrl Pts',(-46.7644730427604,-42.0795087942021,
-28.1626847185045));
#247876=CARTESIAN_POINT('Ctrl Pts',(-45.9273486281662,-42.7287775839517,
-27.2996074426928));
#247877=CARTESIAN_POINT('Ctrl Pts',(-46.3089587420652,-41.8908285929994,
-27.3662354207734));
#247878=CARTESIAN_POINT('Ctrl Pts',(-46.6795127713057,-42.0443170975027,
-28.1998358077765));
#247879=CARTESIAN_POINT('Ctrl Pts',(-45.8524382410723,-42.6864641790425,
-27.3451208446555));
#247880=CARTESIAN_POINT('Ctrl Pts',(-46.2379326487285,-41.8614086218567,
-27.4172101718477));
#247881=CARTESIAN_POINT('Ctrl Pts',(-46.6526207729806,-42.0331780670771,
-28.2150069437025));
#247882=CARTESIAN_POINT('Ctrl Pts',(-45.7105338998473,-42.6062770391952,
-27.4527521127821));
#247883=CARTESIAN_POINT('Ctrl Pts',(-46.1056152152263,-41.8066009463618,
-27.5319438042374));
#247884=CARTESIAN_POINT('Ctrl Pts',(-46.6016724405327,-42.0120745767969,
-28.2508840421101));
#247885=CARTESIAN_POINT('Ctrl Pts',(-45.6430616909817,-42.5681325640035,
-27.515614264563));
#247886=CARTESIAN_POINT('Ctrl Pts',(-46.0437329340899,-41.7809684662446,
-27.5963774980067));
#247887=CARTESIAN_POINT('Ctrl Pts',(-46.5774442952742,-42.0020389504397,
-28.2718380908663));
#247888=CARTESIAN_POINT('Ctrl Pts',(-45.461192857402,-42.4652810208128,
-27.7222891160844));
#247889=CARTESIAN_POINT('Ctrl Pts',(-45.8798463955735,-41.7130844393005,
-27.8008611479946));
#247890=CARTESIAN_POINT('Ctrl Pts',(-46.5121314621695,-41.9749854891707,
-28.3407297000044));
#247891=CARTESIAN_POINT('Ctrl Pts',(-45.3628210526023,-42.4095997698276,
-27.889382888041));
#247892=CARTESIAN_POINT('Ctrl Pts',(-45.7931967067073,-41.6771929629972,
-27.958995177229));
#247893=CARTESIAN_POINT('Ctrl Pts',(-46.4767944547823,-41.9603484214572,
-28.3964276298892));
#247894=CARTESIAN_POINT('Ctrl Pts',(-45.2305230591413,-42.3346964000699,
-28.2517820805544));
#247895=CARTESIAN_POINT('Ctrl Pts',(-45.6784095350839,-41.6296465597236,
-28.2919200601672));
#247896=CARTESIAN_POINT('Ctrl Pts',(-46.4292667992664,-41.9406618219547,
-28.5172273596426));
#247897=CARTESIAN_POINT('Ctrl Pts',(-45.1951938541106,-42.3146823164992,
-28.4504081177447));
#247898=CARTESIAN_POINT('Ctrl Pts',(-45.648154654201,-41.6171145777345,
-28.4709599502677));
#247899=CARTESIAN_POINT('Ctrl Pts',(-46.4165726261775,-41.9354037232982,
-28.5834360396918));
#247900=CARTESIAN_POINT('Ctrl Pts',(-45.1951938513414,-42.3146823207637,
-28.6499499999994));
#247901=CARTESIAN_POINT('Ctrl Pts',(-45.6481545919442,-41.6171145519467,
-28.6499499999995));
#247902=CARTESIAN_POINT('Ctrl Pts',(-46.4165725998989,-41.9354037124133,
-28.64995));
#247903=CARTESIAN_POINT('',(-46.886302585097,-42.1299722429356,-28.14995));
#247904=CARTESIAN_POINT('Origin',(-46.5036191527319,-43.0538517754469,-28.14995));
#247905=CARTESIAN_POINT('Ctrl Pts',(-46.4165725998989,-41.9354037124133,
-28.64995));
#247906=CARTESIAN_POINT('Ctrl Pts',(-46.4165725998989,-41.9354037124133,
-28.6226248135972));
#247907=CARTESIAN_POINT('Ctrl Pts',(-46.4187109381147,-41.9362894411032,
-28.5954211970934));
#247908=CARTESIAN_POINT('Ctrl Pts',(-46.4228669716073,-41.9380109265415,
-28.5686411074116));
#247909=CARTESIAN_POINT('Ctrl Pts',(-46.4270499742658,-41.9397435829741,
-28.5416872374458));
#247910=CARTESIAN_POINT('Ctrl Pts',(-46.433277320163,-41.9423230341023,
-28.5151609373024));
#247911=CARTESIAN_POINT('Ctrl Pts',(-46.4414722606413,-41.9457174895913,
-28.489381232746));
#247912=CARTESIAN_POINT('Ctrl Pts',(-46.4427468468602,-41.9462454404895,
-28.4853716299623));
#247913=CARTESIAN_POINT('Ctrl Pts',(-46.4440691143792,-41.946793141629,
-28.4813801353776));
#247914=CARTESIAN_POINT('Ctrl Pts',(-46.4454388651654,-41.9473605109817,
-28.4774080096258));
#247915=CARTESIAN_POINT('Ctrl Pts',(-46.4478264096847,-41.9483494643023,
-28.4704843946408));
#247916=CARTESIAN_POINT('Ctrl Pts',(-46.45035857188,-41.9493983202258,-28.463618983549));
#247917=CARTESIAN_POINT('Ctrl Pts',(-46.4530306270243,-41.950505121706,
-28.4568274947659));
#247918=CARTESIAN_POINT('Ctrl Pts',(-46.456999039382,-41.9521488919256,
-28.446741090647));
#247919=CARTESIAN_POINT('Ctrl Pts',(-46.4612903227467,-41.9539263996952,
-28.4367870158134));
#247920=CARTESIAN_POINT('Ctrl Pts',(-46.4658757275553,-41.9558257365559,
-28.4270122638807));
#247921=CARTESIAN_POINT('Ctrl Pts',(-46.4765029911984,-41.9602276932878,
-28.4043580228328));
#247922=CARTESIAN_POINT('Ctrl Pts',(-46.4887247847145,-41.9652901259187,
-28.3826189531785));
#247923=CARTESIAN_POINT('Ctrl Pts',(-46.5023672130988,-41.9709410047792,
-28.3619996399708));
#247924=CARTESIAN_POINT('Ctrl Pts',(-46.5160732539531,-41.9766182327875,
-28.3412841821907));
#247925=CARTESIAN_POINT('Ctrl Pts',(-46.5312140385135,-41.9828897510974,
-28.3216976523455));
#247926=CARTESIAN_POINT('Ctrl Pts',(-46.5476531664069,-41.9896990608245,
-28.3034746152985));
#247927=CARTESIAN_POINT('Ctrl Pts',(-46.5502931718124,-41.9907925868682,
-28.3005481269458));
#247928=CARTESIAN_POINT('Ctrl Pts',(-46.5529667295821,-41.9919000107562,
-28.2976568837582));
#247929=CARTESIAN_POINT('Ctrl Pts',(-46.5556733480225,-41.9930211288223,
-28.2948019573763));
#247930=CARTESIAN_POINT('Ctrl Pts',(-46.5774801822152,-42.0020538152974,
-28.2718002275009));
#247931=CARTESIAN_POINT('Ctrl Pts',(-46.6017003997271,-42.0120861578744,
-28.2508643378562));
#247932=CARTESIAN_POINT('Ctrl Pts',(-46.6271465968548,-42.0226263178355,
-28.2329454764323));
#247933=CARTESIAN_POINT('Ctrl Pts',(-46.6526206528053,-42.0331780172989,
-28.2150069972093));
#247934=CARTESIAN_POINT('Ctrl Pts',(-46.679496989526,-42.0443105604755,
-28.1998426732967));
#247935=CARTESIAN_POINT('Ctrl Pts',(-46.7078328490258,-42.0560476577818,
-28.1874520771524));
#247936=CARTESIAN_POINT('Ctrl Pts',(-46.7371092175932,-42.0681743266994,
-28.1746502188044));
#247937=CARTESIAN_POINT('Ctrl Pts',(-46.7675446777706,-42.080781107082,
-28.1650444274588));
#247938=CARTESIAN_POINT('Ctrl Pts',(-46.7986350690308,-42.0936591688014,
-28.1587550972375));
#247939=CARTESIAN_POINT('Ctrl Pts',(-46.827431271788,-42.1055869465283,
-28.152929862465));
#247940=CARTESIAN_POINT('Ctrl Pts',(-46.8567902372224,-42.1177478281885,
-28.14995));
#247941=CARTESIAN_POINT('Ctrl Pts',(-46.886302585097,-42.1299722429356,
-28.14995));
#247942=CARTESIAN_POINT('Ctrl Pts',(-46.5036191527319,-43.0538517754469,
-27.14995));
#247943=CARTESIAN_POINT('Ctrl Pts',(-46.2744683037554,-42.9247311243421,
-27.14995));
#247944=CARTESIAN_POINT('Ctrl Pts',(-46.0777393610381,-42.8132290539286,
-27.2181464165627));
#247945=CARTESIAN_POINT('Ctrl Pts',(-45.8475944848875,-42.683304170092,
-27.3484057282222));
#247946=CARTESIAN_POINT('Ctrl Pts',(-45.7811408576611,-42.6458517787015,
-27.39666449696));
#247947=CARTESIAN_POINT('Ctrl Pts',(-45.6954623428615,-42.597586077303,
-27.4694662134751));
#247948=CARTESIAN_POINT('Ctrl Pts',(-45.6692215721777,-42.5828065424626,
-27.4938232175497));
#247949=CARTESIAN_POINT('Ctrl Pts',(-45.6330713242968,-42.5624303622357,
-27.5298221771973));
#247950=CARTESIAN_POINT('Ctrl Pts',(-45.6157982810954,-42.552690123496,
-27.5476894082045));
#247951=CARTESIAN_POINT('Ctrl Pts',(-45.5969866223692,-42.5420696469704,
-27.5681755773823));
#247952=CARTESIAN_POINT('Ctrl Pts',(-45.5879077094426,-42.536939971722,
-27.578314372819));
#247953=CARTESIAN_POINT('Ctrl Pts',(-45.5840859290262,-42.5347796725811,
-27.5826356936761));
#247954=CARTESIAN_POINT('Ctrl Pts',(-45.5815533520825,-42.533347884816,
-27.5855111018876));
#247955=CARTESIAN_POINT('Ctrl Pts',(-45.581048615305,-42.5330625581288,
-27.5860830286103));
#247956=CARTESIAN_POINT('Ctrl Pts',(-45.4507253194287,-42.4593606968009,
-27.7352703996687));
#247957=CARTESIAN_POINT('Ctrl Pts',(-45.3532470316574,-42.4040488934299,
-27.9086811930516));
#247958=CARTESIAN_POINT('Ctrl Pts',(-45.2255529238554,-42.3317558836558,
-28.2735063897175));
#247959=CARTESIAN_POINT('Ctrl Pts',(-45.1951938513423,-42.3146823207641,
-28.4647367626832));
#247960=CARTESIAN_POINT('Ctrl Pts',(-45.1951938513423,-42.314682320764,
-28.64995));
#247961=CARTESIAN_POINT('Origin',(3.82683432365091,-22.2062953451411,-28.14995));
#247962=CARTESIAN_POINT('',(8.02885449088512,-19.3833694022149,-28.14995));
#247963=CARTESIAN_POINT('Origin',(-65.4282127731639,-49.8102829151368,-43.9323406555977));
#247964=CARTESIAN_POINT('Ctrl Pts',(-49.5640573010081,-43.2391345629745,
-37.8286434305112));
#247965=CARTESIAN_POINT('Ctrl Pts',(-49.842046725293,-43.3542815527096,
-37.9027583562636));
#247966=CARTESIAN_POINT('Ctrl Pts',(-50.1228968347622,-43.4706134770457,
-37.9776546393184));
#247967=CARTESIAN_POINT('Origin',(-74.5160435483921,-43.8330558721564,-27.1488937903833));
#247968=CARTESIAN_POINT('Origin',(-58.8891135228643,-37.3601695173274,-20.9925312105213));
#247969=CARTESIAN_POINT('Origin',(8.02885449088512,-19.383369402215,-4.55788165120213E-15));
#247970=CARTESIAN_POINT('Origin',(1.1405527083135,-2.75353781701182,-1.76005755589152E-15));
#247971=CARTESIAN_POINT('Origin',(-55.5229609888525,-26.2243336820917,-41.2453393117887));
#247972=CARTESIAN_POINT('Origin',(-26.5085260991663,-68.3364732839715,-55.24995));
#247973=CARTESIAN_POINT('',(-26.299256677934,-65.343781133192,-39.1625636424987));
#247974=CARTESIAN_POINT('',(-26.299256677934,-65.343781133192,-52.64995));
#247975=CARTESIAN_POINT('',(-26.299256677934,-65.343781133192,-52.64995));
#247976=CARTESIAN_POINT('',(-25.2130575054386,-65.6305979870176,-52.64995));
#247977=CARTESIAN_POINT('Origin',(-26.5085260991663,-68.3364732839715,-52.64995));
#247978=CARTESIAN_POINT('',(-25.2130575054386,-65.6305979870176,-39.0779244525544));
#247979=CARTESIAN_POINT('',(-25.2130575054386,-65.6305979870176,-55.24995));
#247980=CARTESIAN_POINT('Ctrl Pts',(-26.299256677934,-65.343781133192,-39.1625636424987));
#247981=CARTESIAN_POINT('Ctrl Pts',(-26.2191817227488,-65.3493805195246,
-39.150717625587));
#247982=CARTESIAN_POINT('Ctrl Pts',(-26.1398068688508,-65.3581562279599,
-39.1400968863451));
#247983=CARTESIAN_POINT('Ctrl Pts',(-26.0611578132232,-65.3700172137199,
-39.1307129226473));
#247984=CARTESIAN_POINT('Ctrl Pts',(-25.9815936509173,-65.3820162058069,
-39.121219773559));
#247985=CARTESIAN_POINT('Ctrl Pts',(-25.902771422632,-65.3971727049329,
-39.1129923480007));
#247986=CARTESIAN_POINT('Ctrl Pts',(-25.8247155096153,-65.4154455405877,
-39.1060425498786));
#247987=CARTESIAN_POINT('Ctrl Pts',(-25.7467575651693,-65.4336954418673,
-39.0991014745011));
#247988=CARTESIAN_POINT('Ctrl Pts',(-25.6695631782055,-65.4550540670665,
-39.0934348214525));
#247989=CARTESIAN_POINT('Ctrl Pts',(-25.5931671353121,-65.4795312181795,
-39.0890544498735));
#247990=CARTESIAN_POINT('Ctrl Pts',(-25.5176849950404,-65.5037155565796,
-39.0847264793471));
#247991=CARTESIAN_POINT('Ctrl Pts',(-25.4429814678376,-65.5309446076645,
-39.0816541995771));
#247992=CARTESIAN_POINT('Ctrl Pts',(-25.3691120394327,-65.5612731829912,
-39.079849049173));
#247993=CARTESIAN_POINT('Ctrl Pts',(-25.3166630024623,-65.5828071870157,
-39.0785673497971));
#247994=CARTESIAN_POINT('Ctrl Pts',(-25.2646348944175,-65.6059047250466,
-39.0779244527868));
#247995=CARTESIAN_POINT('Ctrl Pts',(-25.2130575054386,-65.6305979870177,
-39.0779244525544));
#247996=CARTESIAN_POINT('Origin',(-55.3689732639433,13.5410260791383,-55.24995));
#247997=CARTESIAN_POINT('',(-52.3762811131638,13.3317566579059,-39.1625636424987));
#247998=CARTESIAN_POINT('',(-52.3762811131638,13.3317566579059,-52.64995));
#247999=CARTESIAN_POINT('',(-52.3762811131638,13.3317566579059,-52.64995));
#248000=CARTESIAN_POINT('',(-52.6630979669895,12.2455574854105,-52.64995));
#248001=CARTESIAN_POINT('Origin',(-55.3689732639433,13.5410260791383,-52.64995));
#248002=CARTESIAN_POINT('',(-52.6630979669895,12.2455574854105,-39.0779244525544));
#248003=CARTESIAN_POINT('',(-52.6630979669895,12.2455574854105,-55.24995));
#248004=CARTESIAN_POINT('Ctrl Pts',(-52.3762811131638,13.3317566579059,
-39.1625636424987));
#248005=CARTESIAN_POINT('Ctrl Pts',(-52.3818804994966,13.2516817027191,
-39.1507176255866));
#248006=CARTESIAN_POINT('Ctrl Pts',(-52.390656207932,13.1723068488195,-39.1400968863444));
#248007=CARTESIAN_POINT('Ctrl Pts',(-52.4025171936925,13.0936577931905,
-39.1307129226464));
#248008=CARTESIAN_POINT('Ctrl Pts',(-52.4145161857798,13.0140936308831,
-39.1212197735579));
#248009=CARTESIAN_POINT('Ctrl Pts',(-52.4296726849063,12.9352714025963,
-39.1129923479995));
#248010=CARTESIAN_POINT('Ctrl Pts',(-52.4479455205616,12.8572154895783,
-39.1060425498774));
#248011=CARTESIAN_POINT('Ctrl Pts',(-52.4661954218418,12.779257545131,-39.0991014744999));
#248012=CARTESIAN_POINT('Ctrl Pts',(-52.4875540470417,12.7020631581658,
-39.0934348214514));
#248013=CARTESIAN_POINT('Ctrl Pts',(-52.5120311981555,12.6256671152711,
-39.0890544498725));
#248014=CARTESIAN_POINT('Ctrl Pts',(-52.5362155365564,12.5501849749981,
-39.0847264793463));
#248015=CARTESIAN_POINT('Ctrl Pts',(-52.5634445876421,12.4754814477942,
-39.0816541995765));
#248016=CARTESIAN_POINT('Ctrl Pts',(-52.5937731629698,12.4016120193881,
-39.0798490491726));
#248017=CARTESIAN_POINT('Ctrl Pts',(-52.6153071669924,12.3491629824233,
-39.078567349797));
#248018=CARTESIAN_POINT('Ctrl Pts',(-52.638404705021,12.297134874384,-39.0779244527868));
#248019=CARTESIAN_POINT('Ctrl Pts',(-52.6630979669895,12.2455574854105,
-39.0779244525544));
#248020=CARTESIAN_POINT('Origin',(-26.5085260991666,42.4014732439151,-55.24995));
#248021=CARTESIAN_POINT('',(-25.2130575054389,39.6955979469612,-39.0779244525544));
#248022=CARTESIAN_POINT('',(-25.2130575054389,39.6955979469612,-52.64995));
#248023=CARTESIAN_POINT('',(-25.2130575054389,39.6955979469612,-55.24995));
#248024=CARTESIAN_POINT('',(-26.2992566779342,39.4087810931356,-52.64995));
#248025=CARTESIAN_POINT('Origin',(-26.5085260991666,42.4014732439151,-52.64995));
#248026=CARTESIAN_POINT('',(-26.2992566779342,39.4087810931356,-39.1625636424987));
#248027=CARTESIAN_POINT('',(-26.2992566779342,39.4087810931356,-37.9059960127943));
#248028=CARTESIAN_POINT('Ctrl Pts',(-25.2130575054389,39.6955979469613,
-39.0779244525544));
#248029=CARTESIAN_POINT('Ctrl Pts',(-25.2853758087053,39.6609747362246,
-39.0779244528815));
#248030=CARTESIAN_POINT('Ctrl Pts',(-25.358578777861,39.6294870816771,-39.0791883715014));
#248031=CARTESIAN_POINT('Ctrl Pts',(-25.4325893318994,39.6010518340479,
-39.0817049219424));
#248032=CARTESIAN_POINT('Ctrl Pts',(-25.5078024392622,39.5721545590496,
-39.0842623623096));
#248033=CARTESIAN_POINT('Ctrl Pts',(-25.5838503061877,39.5464092486697,
-39.0881134717398));
#248034=CARTESIAN_POINT('Ctrl Pts',(-25.6606832984686,39.5237723238568,
-39.0932464046122));
#248035=CARTESIAN_POINT('Ctrl Pts',(-25.737639668794,39.5010990487803,-39.0983875799231));
#248036=CARTESIAN_POINT('Ctrl Pts',(-25.8153845108865,39.4815438876141,
-39.1048146986732));
#248037=CARTESIAN_POINT('Ctrl Pts',(-25.893887314254,39.4651116919121,-39.112515858085));
#248038=CARTESIAN_POINT('Ctrl Pts',(-25.9717768804289,39.4488078589327,
-39.1201568586595));
#248039=CARTESIAN_POINT('Ctrl Pts',(-26.0504134462025,39.4355782885041,
-39.1290520728958));
#248040=CARTESIAN_POINT('Ctrl Pts',(-26.1297738690388,39.4254781585406,
-39.1391898747846));
#248041=CARTESIAN_POINT('Ctrl Pts',(-26.1859090101704,39.4183338893862,
-39.1463607909599));
#248042=CARTESIAN_POINT('Ctrl Pts',(-26.242406487351,39.4127564457215,-39.154153418384));
#248043=CARTESIAN_POINT('Ctrl Pts',(-26.2992566779342,39.4087810931356,
-39.1625636424987));
#248044=CARTESIAN_POINT('Ctrl Pts',(-25.2130575054389,39.6955979469612,
-39.0779244525544));
#248045=CARTESIAN_POINT('Ctrl Pts',(-25.2130575054388,39.6955979469612,
-37.9059960127943));
#248046=CARTESIAN_POINT('Ctrl Pts',(-24.7220243175171,38.669965539032,-37.6224808631404));
#248047=CARTESIAN_POINT('Ctrl Pts',(-25.5571787362036,39.5308459913215,
-39.077924454111));
#248048=CARTESIAN_POINT('Ctrl Pts',(-25.5933889787397,39.5135099307705,
-37.9059960140155));
#248049=CARTESIAN_POINT('Ctrl Pts',(-25.2415430286799,38.4212400498976,
-37.6224808645859));
#248050=CARTESIAN_POINT('Ctrl Pts',(-25.9205756959913,39.4352610469465,
-39.1065428641433));
#248051=CARTESIAN_POINT('Ctrl Pts',(-26.0004074167487,39.4148955857669,
-37.9286345805798));
#248052=CARTESIAN_POINT('Ctrl Pts',(-25.7896847017763,38.2763141299578,
-37.6510924855219));
#248053=CARTESIAN_POINT('Ctrl Pts',(-26.2992566779342,39.4087810931356,
-39.1625636424987));
#248054=CARTESIAN_POINT('Ctrl Pts',(-26.4161222952889,39.4006090530882,
-37.971813107807));
#248055=CARTESIAN_POINT('Ctrl Pts',(-26.3607251006129,38.2350705817238,
-37.7071200530847));
#248056=CARTESIAN_POINT('',(-24.7220243175171,38.669965539032,-37.6224808631404));
#248057=CARTESIAN_POINT('Origin',(-24.5653232085749,38.3426602984844,-39.0779244525544));
#248058=CARTESIAN_POINT('',(-26.3607251006129,38.2350705817238,-37.7071200530847));
#248059=CARTESIAN_POINT('Origin',(-26.194621967318,37.9124350177459,-39.1625636424987));
#248060=CARTESIAN_POINT('Ctrl Pts',(-26.3607251006129,38.2350705817238,
-37.7071200530847));
#248061=CARTESIAN_POINT('Ctrl Pts',(-26.2011255350992,38.2465977037834,
-37.6914609588104));
#248062=CARTESIAN_POINT('Ctrl Pts',(-26.0435569434565,38.2662022062977,
-37.6779662189505));
#248063=CARTESIAN_POINT('Ctrl Pts',(-25.8880107550447,38.2938462174384,
-37.6666367941389));
#248064=CARTESIAN_POINT('Ctrl Pts',(-25.7326779997653,38.3214522967729,
-37.6553229150289));
#248065=CARTESIAN_POINT('Ctrl Pts',(-25.5793619804298,38.3570758581462,
-37.6461683926629));
#248066=CARTESIAN_POINT('Ctrl Pts',(-25.4280646493686,38.4007283517996,
-37.6391871086171));
#248067=CARTESIAN_POINT('Ctrl Pts',(-25.2772986540836,38.4442275437957,
-37.6322303418973));
#248068=CARTESIAN_POINT('Ctrl Pts',(-25.1285370763277,38.4956993999497,
-37.6274315578454));
#248069=CARTESIAN_POINT('Ctrl Pts',(-24.9817940407081,38.5552037278875,
-37.624817614644));
#248070=CARTESIAN_POINT('Ctrl Pts',(-24.8944876056226,38.5906065033751,
-37.6232624194589));
#248071=CARTESIAN_POINT('Ctrl Pts',(-24.8078959327013,38.6288535270284,
-37.6224808633793));
#248072=CARTESIAN_POINT('Ctrl Pts',(-24.7220243175172,38.669965539032,-37.6224808631404));
#248073=CARTESIAN_POINT('Origin',(-48.2118204350716,29.879557875893,235.35105));
#248074=CARTESIAN_POINT('',(-50.4542306878656,31.8724442896568,-41.3499258784557));
#248075=CARTESIAN_POINT('',(-50.4542306878656,31.8724442896568,-52.64995));
#248076=CARTESIAN_POINT('',(-50.4542306878656,31.8724442896567,235.35105));
#248077=CARTESIAN_POINT('',(-51.2045125858511,30.0888272971254,-52.64995));
#248078=CARTESIAN_POINT('Origin',(-48.2118204350716,29.879557875893,-52.64995));
#248079=CARTESIAN_POINT('',(-51.2045125858511,30.0888272971254,-41.2737227474219));
#248080=CARTESIAN_POINT('',(-51.2045125858511,30.0888272971253,235.35105));
#248081=CARTESIAN_POINT('Ctrl Pts',(-50.4542306878656,31.8724442896568,
-41.3499258784557));
#248082=CARTESIAN_POINT('Ctrl Pts',(-50.6751042513768,31.6239157533749,
-41.3499258753262));
#248083=CARTESIAN_POINT('Ctrl Pts',(-50.8500106529935,31.3458145441506,
-41.3433504080566));
#248084=CARTESIAN_POINT('Ctrl Pts',(-51.1065500370229,30.7342489164072,
-41.3171858838447));
#248085=CARTESIAN_POINT('Ctrl Pts',(-51.1815637992349,30.4170102355187,
-41.298307134608));
#248086=CARTESIAN_POINT('Ctrl Pts',(-51.2045125858511,30.0888272971254,
-41.2737227474219));
#248087=CARTESIAN_POINT('Origin',(-42.8470578959213,35.2443204150433,235.35105));
#248088=CARTESIAN_POINT('',(-43.0563273171537,38.2370125658228,-41.2737227474219));
#248089=CARTESIAN_POINT('',(-43.0563273171537,38.2370125658228,-52.64995));
#248090=CARTESIAN_POINT('',(-43.0563273171537,38.2370125658227,235.35105));
#248091=CARTESIAN_POINT('',(-44.839944309685,37.4867306678373,-52.64995));
#248092=CARTESIAN_POINT('Origin',(-42.8470578959213,35.2443204150433,-52.64995));
#248093=CARTESIAN_POINT('',(-44.839944309685,37.4867306678373,-41.3499258784557));
#248094=CARTESIAN_POINT('',(-44.839944309685,37.4867306678373,235.35105));
#248095=CARTESIAN_POINT('Ctrl Pts',(-43.0563273171537,38.2370125658228,
-41.2737227474219));
#248096=CARTESIAN_POINT('Ctrl Pts',(-43.3844623716888,38.2140671259236,
-41.2983034469791));
#248097=CARTESIAN_POINT('Ctrl Pts',(-43.7019124525045,38.1390166933963,
-41.3171960016465));
#248098=CARTESIAN_POINT('Ctrl Pts',(-44.3136937257824,37.8823162829827,
-41.3433633063114));
#248099=CARTESIAN_POINT('Ctrl Pts',(-44.5912415362924,37.707759080253,-41.3499257769023));
#248100=CARTESIAN_POINT('Ctrl Pts',(-44.839944309685,37.4867306678373,-41.3499258784558));
#248101=CARTESIAN_POINT('Origin',(-44.0630480057168,38.1666157975539,235.35105));
#248102=CARTESIAN_POINT('',(-44.0630480057168,38.166615797554,-52.64995));
#248103=CARTESIAN_POINT('Ctrl Pts',(-26.2992566779342,39.4087810931356,
-39.1625636424987));
#248104=CARTESIAN_POINT('Ctrl Pts',(-31.903874175502,39.0168680593679,-39.7153157040946));
#248105=CARTESIAN_POINT('Ctrl Pts',(-37.4870209577723,38.6264564042711,
-40.4393222961257));
#248106=CARTESIAN_POINT('Ctrl Pts',(-43.0563273171537,38.2370125658228,
-41.2737227474219));
#248107=CARTESIAN_POINT('Ctrl Pts',(-44.0845625322695,36.6367696109743,
-39.8944822890418));
#248108=CARTESIAN_POINT('Ctrl Pts',(-44.8399443096851,37.4867306678373,
-40.1779974386957));
#248109=CARTESIAN_POINT('Ctrl Pts',(-44.839944309685,37.4867306678373,-41.3499258784558));
#248110=CARTESIAN_POINT('Ctrl Pts',(-43.9595274298496,36.7478914351849,
-39.8944822858058));
#248111=CARTESIAN_POINT('Ctrl Pts',(-44.6149072014685,37.6867267800097,
-40.1779974336417));
#248112=CARTESIAN_POINT('Ctrl Pts',(-44.5912415343056,37.7077590820187,
-41.3499258752894));
#248113=CARTESIAN_POINT('Ctrl Pts',(-43.8200866324971,36.835758129222,-39.887919815423));
#248114=CARTESIAN_POINT('Ctrl Pts',(-44.3663746862182,37.849051706332,-40.1674920635188));
#248115=CARTESIAN_POINT('Ctrl Pts',(-44.3136937213669,37.8823162857708,
-41.343363404867));
#248116=CARTESIAN_POINT('Ctrl Pts',(-43.5128927223798,36.9652495181622,
-39.8617525114841));
#248117=CARTESIAN_POINT('Ctrl Pts',(-43.8196015906779,38.1008702319186,
-40.1253788430241));
#248118=CARTESIAN_POINT('Ctrl Pts',(-43.7019124427066,38.1390166965721,
-41.3171961008681));
#248119=CARTESIAN_POINT('Ctrl Pts',(-43.3535628849498,37.0032968338361,
-39.8428593266731));
#248120=CARTESIAN_POINT('Ctrl Pts',(-43.5344232858197,38.1836802846001,
-40.0946545134465));
#248121=CARTESIAN_POINT('Ctrl Pts',(-43.3844623592655,38.214067128441,-41.2983035466937));
#248122=CARTESIAN_POINT('Ctrl Pts',(-43.1889493654704,37.0152446912691,
-39.8182791580079));
#248123=CARTESIAN_POINT('Ctrl Pts',(-43.23812030497,38.224300361751,-40.0543903140502));
#248124=CARTESIAN_POINT('Ctrl Pts',(-43.0563273171537,38.2370125658228,
-41.2737227474219));
#248125=CARTESIAN_POINT('',(-43.1889493654704,37.0152446912691,-39.8182791580079));
#248126=CARTESIAN_POINT('Origin',(-42.9516926065375,36.740666490433,-41.2737227474219));
#248127=CARTESIAN_POINT('',(-44.0845625322695,36.6367696109743,-39.8944822890418));
#248128=CARTESIAN_POINT('Origin',(-43.8435011028032,36.3655255414403,-41.3499258784558));
#248129=CARTESIAN_POINT('Ctrl Pts',(-44.0845625322695,36.6367696109743,
-39.8944822890418));
#248130=CARTESIAN_POINT('Ctrl Pts',(-43.9941797939522,36.7170950246701,
-39.8944822890418));
#248131=CARTESIAN_POINT('Ctrl Pts',(-43.8962901478109,36.7852564677648,
-39.8910542505833));
#248132=CARTESIAN_POINT('Ctrl Pts',(-43.7909432593834,36.8413335920192,
-39.8842118316082));
#248133=CARTESIAN_POINT('Ctrl Pts',(-43.7506303648289,36.8627925191003,
-39.8815934560799));
#248134=CARTESIAN_POINT('Ctrl Pts',(-43.7092251907661,36.8824814307078,
-39.8784749689682));
#248135=CARTESIAN_POINT('Ctrl Pts',(-43.6667294913925,36.9004031219782,
-39.8748566639276));
#248136=CARTESIAN_POINT('Ctrl Pts',(-43.6666496039709,36.9004368128629,
-39.8748498618967));
#248137=CARTESIAN_POINT('Ctrl Pts',(-43.666569712705,36.9004704974974,-39.8748430581001));
#248138=CARTESIAN_POINT('Ctrl Pts',(-43.6664898175948,36.9005041758817,
-39.8748362525378));
#248139=CARTESIAN_POINT('Ctrl Pts',(-43.5643771770594,36.9435479709187,
-39.8661381741221));
#248140=CARTESIAN_POINT('Ctrl Pts',(-43.4597085659162,36.9748052400737,
-39.8548713027025));
#248141=CARTESIAN_POINT('Ctrl Pts',(-43.3525514979881,36.9944348238143,
-39.8410580051272));
#248142=CARTESIAN_POINT('Ctrl Pts',(-43.2986448352414,37.0043097240054,
-39.8341090582383));
#248143=CARTESIAN_POINT('Ctrl Pts',(-43.2441082468331,37.0112411932519,
-39.8265155089205));
#248144=CARTESIAN_POINT('Ctrl Pts',(-43.1889493654704,37.0152446912691,
-39.8182791580079));
#248145=CARTESIAN_POINT('Origin',(0.,-12.9675000200282,235.35105));
#248146=CARTESIAN_POINT('Origin',(0.,-12.9675000200281,-52.64995));
#248147=CARTESIAN_POINT('Origin',(0.,-12.9675000200281,-41.3499258784557));
#248148=CARTESIAN_POINT('Ctrl Pts',(-49.9827447112974,30.221449345442,-39.8182791580079));
#248149=CARTESIAN_POINT('Ctrl Pts',(-51.1918003817794,30.2706202849417,
-40.0543903140502));
#248150=CARTESIAN_POINT('Ctrl Pts',(-51.204512585851,30.0888272971254,-41.2737227474219));
#248151=CARTESIAN_POINT('Ctrl Pts',(-49.970795119399,30.3860867600489,-39.8428628946809));
#248152=CARTESIAN_POINT('Ctrl Pts',(-51.1511744833359,30.5669657276558,
-40.0946602834914));
#248153=CARTESIAN_POINT('Ctrl Pts',(-51.1815637992349,30.4170102355187,
-41.298307134608));
#248154=CARTESIAN_POINT('Ctrl Pts',(-49.9327664722994,30.5453106517579,
-39.8617422945218));
#248155=CARTESIAN_POINT('Ctrl Pts',(-51.0684082345096,30.8519555741622,
-40.125362313696));
#248156=CARTESIAN_POINT('Ctrl Pts',(-51.1065500370229,30.7342489164072,
-41.3171858838447));
#248157=CARTESIAN_POINT('Ctrl Pts',(-49.8033560611762,30.8523961753476,
-39.8879068185516));
#248158=CARTESIAN_POINT('Ctrl Pts',(-50.8167365053657,31.3985364985707,
-40.1674712617341));
#248159=CARTESIAN_POINT('Ctrl Pts',(-50.8500106529935,31.3458145441506,
-41.3433504080566));
#248160=CARTESIAN_POINT('Ctrl Pts',(-49.715313604986,30.9921150076825,-39.8944822858423));
#248161=CARTESIAN_POINT('Ctrl Pts',(-50.6540845266555,31.647567268839,-40.1779974337035));
#248162=CARTESIAN_POINT('Ctrl Pts',(-50.6751042513768,31.6239157533749,
-41.3499258753262));
#248163=CARTESIAN_POINT('Ctrl Pts',(-49.6042696310026,31.1170625122411,
-39.8944822890418));
#248164=CARTESIAN_POINT('Ctrl Pts',(-50.4542306878656,31.8724442896567,
-40.1779974386957));
#248165=CARTESIAN_POINT('Ctrl Pts',(-50.4542306878656,31.8724442896568,
-41.3499258784558));
#248166=CARTESIAN_POINT('',(-49.6042696310026,31.1170625122412,-39.8944822890418));
#248167=CARTESIAN_POINT('Origin',(-49.3330255614686,30.8760010827748,-41.3499258784557));
#248168=CARTESIAN_POINT('',(-49.9827447112974,30.221449345442,-39.8182791580079));
#248169=CARTESIAN_POINT('Origin',(-49.7081665104613,29.9841925865092,-41.2737227474219));
#248170=CARTESIAN_POINT('Ctrl Pts',(-49.9827447112974,30.221449345442,-39.8182791580079));
#248171=CARTESIAN_POINT('Ctrl Pts',(-49.974247842649,30.3385164122215,-39.8357596691873));
#248172=CARTESIAN_POINT('Ctrl Pts',(-49.9525777122483,30.4527365881441,
-39.8503404873507));
#248173=CARTESIAN_POINT('Ctrl Pts',(-49.9175649839551,30.5640807882622,
-39.8620074889827));
#248174=CARTESIAN_POINT('Ctrl Pts',(-49.903287657114,30.6094842062316,-39.8667650044257));
#248175=CARTESIAN_POINT('Ctrl Pts',(-49.8867911421682,30.6544092836455,
-39.871037881299));
#248176=CARTESIAN_POINT('Ctrl Pts',(-49.8680615705257,30.6988535344112,
-39.8748246333721));
#248177=CARTESIAN_POINT('Ctrl Pts',(-49.8680277409604,30.6989338101224,
-39.8748314730468));
#248178=CARTESIAN_POINT('Ctrl Pts',(-49.8679939050224,30.699014082039,-39.8748383109414));
#248179=CARTESIAN_POINT('Ctrl Pts',(-49.8679600627116,30.6990943501611,
-39.8748451470561));
#248180=CARTESIAN_POINT('Ctrl Pts',(-49.8342106733128,30.7791420788837,
-39.8816624916982));
#248181=CARTESIAN_POINT('Ctrl Pts',(-49.7941455915935,30.8553753559231,
-39.8867070324262));
#248182=CARTESIAN_POINT('Ctrl Pts',(-49.747789476607,30.9277322498084,-39.889976576145));
#248183=CARTESIAN_POINT('Ctrl Pts',(-49.7052516615012,30.9941291895568,
-39.8929768113077));
#248184=CARTESIAN_POINT('Ctrl Pts',(-49.6574159846451,31.0572618495022,
-39.8944822890418));
#248185=CARTESIAN_POINT('Ctrl Pts',(-49.6042696310026,31.1170625122411,
-39.8944822890418));
#248186=CARTESIAN_POINT('Origin',(-51.1341158175823,31.0955479856884,235.35105));
#248187=CARTESIAN_POINT('',(-51.1341158175823,31.0955479856884,-52.64995));
#248188=CARTESIAN_POINT('Ctrl Pts',(-51.2045125858511,30.0888272971254,
-41.2737227474219));
#248189=CARTESIAN_POINT('Ctrl Pts',(-51.5939564242993,24.519520937744,-40.4393222961257));
#248190=CARTESIAN_POINT('Ctrl Pts',(-51.9843680793961,18.9363741554737,
-39.7153157040947));
#248191=CARTESIAN_POINT('Ctrl Pts',(-52.3762811131638,13.3317566579059,
-39.1625636424987));
#248192=CARTESIAN_POINT('Ctrl Pts',(-52.3762811131638,13.3317566579059,
-39.1625636424987));
#248193=CARTESIAN_POINT('Ctrl Pts',(-52.3681090731164,13.4486222752606,
-37.971813107807));
#248194=CARTESIAN_POINT('Ctrl Pts',(-51.202570601752,13.3932250805846,-37.7071200530847));
#248195=CARTESIAN_POINT('Ctrl Pts',(-52.4027610669746,12.9530756759645,
-39.1065428641427));
#248196=CARTESIAN_POINT('Ctrl Pts',(-52.3823956057955,13.0329073967221,
-37.9286345805849));
#248197=CARTESIAN_POINT('Ctrl Pts',(-51.243814149994,12.8221846817494,-37.6510924855238));
#248198=CARTESIAN_POINT('Ctrl Pts',(-52.4983460113501,12.5896787161743,
-39.0779244541051));
#248199=CARTESIAN_POINT('Ctrl Pts',(-52.4810099507979,12.6258889587099,
-37.9059960140017));
#248200=CARTESIAN_POINT('Ctrl Pts',(-51.3887400699185,12.2740430086498,
-37.6224808645841));
#248201=CARTESIAN_POINT('Ctrl Pts',(-52.6630979669895,12.2455574854105,
-39.0779244525544));
#248202=CARTESIAN_POINT('Ctrl Pts',(-52.6630979669895,12.2455574854105,
-37.9059960127943));
#248203=CARTESIAN_POINT('Ctrl Pts',(-51.6374655590603,11.7545242974889,
-37.6224808631404));
#248204=CARTESIAN_POINT('',(-51.202570601752,13.3932250805846,-37.7071200530847));
#248205=CARTESIAN_POINT('Origin',(-50.8799350377741,13.2271219472897,-39.1625636424987));
#248206=CARTESIAN_POINT('',(-51.6374655590603,11.7545242974889,-37.6224808631404));
#248207=CARTESIAN_POINT('Origin',(-51.3101603185126,11.5978231885467,-39.0779244525544));
#248208=CARTESIAN_POINT('Ctrl Pts',(-51.6374655590603,11.7545242974889,
-37.6224808631404));
#248209=CARTESIAN_POINT('Ctrl Pts',(-51.5683401737289,11.898908096752,-37.6224808635416));
#248210=CARTESIAN_POINT('Ctrl Pts',(-51.5073117137531,12.0453267862122,
-37.6246896514879));
#248211=CARTESIAN_POINT('Ctrl Pts',(-51.4542914421326,12.1937580895559,
-37.6290723471549));
#248212=CARTESIAN_POINT('Ctrl Pts',(-51.401143473863,12.3425468822047,-37.6334655983234));
#248213=CARTESIAN_POINT('Ctrl Pts',(-51.3560423053795,12.4933581163811,
-37.6400432640145));
#248214=CARTESIAN_POINT('Ctrl Pts',(-51.3189474852191,12.6461827680856,
-37.6487836824747));
#248215=CARTESIAN_POINT('Ctrl Pts',(-51.281768224475,12.7993553013203,-37.6575439971369));
#248216=CARTESIAN_POINT('Ctrl Pts',(-51.2526317828013,12.9545505495527,
-37.6684769421211));
#248217=CARTESIAN_POINT('Ctrl Pts',(-51.2315467536768,13.1117710662236,
-37.6815739017301));
#248218=CARTESIAN_POINT('Ctrl Pts',(-51.2190600923228,13.2048778548359,
-37.6893299877397));
#248219=CARTESIAN_POINT('Ctrl Pts',(-51.2093980530995,13.2986951308913,
-37.6978452571967));
#248220=CARTESIAN_POINT('Ctrl Pts',(-51.202570601752,13.3932250805846,-37.7071200530847));
#248221=CARTESIAN_POINT('Origin',(-42.8470578959211,-61.1793204550998,235.35105));
#248222=CARTESIAN_POINT('',(-44.8399443096849,-63.4217307078938,-41.3499258784557));
#248223=CARTESIAN_POINT('',(-44.8399443096849,-63.4217307078937,-52.64995));
#248224=CARTESIAN_POINT('',(-44.8399443096849,-63.4217307078938,235.35105));
#248225=CARTESIAN_POINT('',(-43.0563273171535,-64.1720126058792,-52.64995));
#248226=CARTESIAN_POINT('Origin',(-42.8470578959211,-61.1793204550997,-52.64995));
#248227=CARTESIAN_POINT('',(-43.0563273171535,-64.1720126058792,-41.273722747422));
#248228=CARTESIAN_POINT('',(-43.0563273171535,-64.1720126058792,235.35105));
#248229=CARTESIAN_POINT('Ctrl Pts',(-44.8399443096849,-63.4217307078938,
-41.3499258784557));
#248230=CARTESIAN_POINT('Ctrl Pts',(-44.5914157734028,-63.6426042714052,
-41.3499258753244));
#248231=CARTESIAN_POINT('Ctrl Pts',(-44.3133145641792,-63.8175106730215,
-41.3433504080572));
#248232=CARTESIAN_POINT('Ctrl Pts',(-43.7017489364349,-64.0740500570513,
-41.3171858838442));
#248233=CARTESIAN_POINT('Ctrl Pts',(-43.3845102555472,-64.1490638192631,
-41.2983071346081));
#248234=CARTESIAN_POINT('Ctrl Pts',(-43.0563273171535,-64.1720126058792,
-41.273722747422));
#248235=CARTESIAN_POINT('Origin',(-48.2118204350714,-55.8145579159494,235.35105));
#248236=CARTESIAN_POINT('',(-51.2045125858509,-56.0238273371818,-41.2737227474219));
#248237=CARTESIAN_POINT('',(-51.2045125858509,-56.0238273371818,-52.64995));
#248238=CARTESIAN_POINT('',(-51.2045125858509,-56.0238273371818,235.35105));
#248239=CARTESIAN_POINT('',(-50.4542306878654,-57.8074443297132,-52.64995));
#248240=CARTESIAN_POINT('Origin',(-48.2118204350714,-55.8145579159494,-52.64995));
#248241=CARTESIAN_POINT('',(-50.4542306878654,-57.8074443297132,-41.3499258784557));
#248242=CARTESIAN_POINT('',(-50.4542306878654,-57.8074443297133,235.35105));
#248243=CARTESIAN_POINT('Ctrl Pts',(-51.2045125858509,-56.0238273371818,
-41.2737227474219));
#248244=CARTESIAN_POINT('Ctrl Pts',(-51.1815671459517,-56.3519623917163,
-41.2983034469768));
#248245=CARTESIAN_POINT('Ctrl Pts',(-51.106516713424,-56.6694124725336,
-41.317196001646));
#248246=CARTESIAN_POINT('Ctrl Pts',(-50.8498163030113,-57.2811937458096,
-41.343363306312));
#248247=CARTESIAN_POINT('Ctrl Pts',(-50.6752591002806,-57.5587415563211,
-41.3499257769023));
#248248=CARTESIAN_POINT('Ctrl Pts',(-50.4542306878654,-57.8074443297132,
-41.3499258784557));
#248249=CARTESIAN_POINT('Origin',(-51.1341158175821,-57.030548025745,235.35105));
#248250=CARTESIAN_POINT('Ctrl Pts',(-52.1363779740716,-42.6975314240561,
-39.5221562118214));
#248251=CARTESIAN_POINT('Ctrl Pts',(-51.8249654425107,-47.1509381060673,
-40.0158159854806));
#248252=CARTESIAN_POINT('Ctrl Pts',(-51.5144316274106,-51.5917785572367,
-40.6097076503739));
#248253=CARTESIAN_POINT('Ctrl Pts',(-51.2045125858509,-56.0238273371818,
-41.2737227474219));
#248254=CARTESIAN_POINT('',(-52.3762811131638,-39.2667566979623,-52.64995));
#248255=CARTESIAN_POINT('',(-52.3762811131638,-39.2667566979623,-37.9059960127943));
#248256=CARTESIAN_POINT('',(-51.1341158175821,-57.0305480257449,-52.64995));
#248257=CARTESIAN_POINT('Ctrl Pts',(-49.6042696310024,-57.0520625522976,
-39.8944822890418));
#248258=CARTESIAN_POINT('Ctrl Pts',(-50.4542306878655,-57.8074443297132,
-40.1779974386957));
#248259=CARTESIAN_POINT('Ctrl Pts',(-50.4542306878654,-57.8074443297132,
-41.3499258784558));
#248260=CARTESIAN_POINT('Ctrl Pts',(-49.7153914552119,-56.9270274498771,
-39.8944822858055));
#248261=CARTESIAN_POINT('Ctrl Pts',(-50.6542268000352,-57.5824072214955,
-40.177997433644));
#248262=CARTESIAN_POINT('Ctrl Pts',(-50.6752591020463,-57.5587415543343,
-41.3499258752894));
#248263=CARTESIAN_POINT('Ctrl Pts',(-49.8032581492502,-56.7875866525247,
-39.887919815423));
#248264=CARTESIAN_POINT('Ctrl Pts',(-50.8165517263607,-57.3338747062451,
-40.1674920635201));
#248265=CARTESIAN_POINT('Ctrl Pts',(-50.8498163057994,-57.2811937413941,
-41.3433634048676));
#248266=CARTESIAN_POINT('Ctrl Pts',(-49.9327495381902,-56.4803927424085,
-39.8617525114842));
#248267=CARTESIAN_POINT('Ctrl Pts',(-51.0683702519462,-56.7871016107072,
-40.125378843023));
#248268=CARTESIAN_POINT('Ctrl Pts',(-51.1065167165998,-56.6694124627357,
-41.3171961008675));
#248269=CARTESIAN_POINT('Ctrl Pts',(-49.9707968538638,-56.3210629049775,
-39.8428593266729));
#248270=CARTESIAN_POINT('Ctrl Pts',(-51.1511803046297,-56.5019233058474,
-40.094654513445));
#248271=CARTESIAN_POINT('Ctrl Pts',(-51.1815671484691,-56.351962379293,
-41.2983035466914));
#248272=CARTESIAN_POINT('Ctrl Pts',(-49.9827447112972,-56.1564493854985,
-39.8182791580079));
#248273=CARTESIAN_POINT('Ctrl Pts',(-51.1918003817792,-56.2056203249981,
-40.0543903140502));
#248274=CARTESIAN_POINT('Ctrl Pts',(-51.2045125858509,-56.0238273371818,
-41.2737227474219));
#248275=CARTESIAN_POINT('',(-49.9827447112972,-56.1564493854985,-39.8182791580079));
#248276=CARTESIAN_POINT('Origin',(-49.7081665104611,-55.9191926265656,-41.2737227474219));
#248277=CARTESIAN_POINT('',(-49.6042696310024,-57.0520625522976,-39.8944822890418));
#248278=CARTESIAN_POINT('Origin',(-49.3330255614684,-56.8110011228313,-41.3499258784558));
#248279=CARTESIAN_POINT('Ctrl Pts',(-49.6042696310024,-57.0520625522976,
-39.8944822890418));
#248280=CARTESIAN_POINT('Ctrl Pts',(-49.6845950444292,-56.9616798142831,
-39.8944822890418));
#248281=CARTESIAN_POINT('Ctrl Pts',(-49.7527564873363,-56.8637901684946,
-39.8910542506063));
#248282=CARTESIAN_POINT('Ctrl Pts',(-49.8088336114838,-56.75844328047,-39.884211831677));
#248283=CARTESIAN_POINT('Ctrl Pts',(-49.8302925387837,-56.7181303855818,
-39.8815934561345));
#248284=CARTESIAN_POINT('Ctrl Pts',(-49.8499814505791,-56.6767252111662,
-39.8784749689999));
#248285=CARTESIAN_POINT('Ctrl Pts',(-49.8679031420063,-56.6342295114207,
-39.8748566639276));
#248286=CARTESIAN_POINT('Ctrl Pts',(-49.867936832891,-56.6341496239991,
-39.8748498618967));
#248287=CARTESIAN_POINT('Ctrl Pts',(-49.8679705175255,-56.6340697327332,
-39.8748430581001));
#248288=CARTESIAN_POINT('Ctrl Pts',(-49.8680041959098,-56.6339898376229,
-39.8748362525379));
#248289=CARTESIAN_POINT('Ctrl Pts',(-49.9110479907906,-56.531877197458,
-39.8661381741537));
#248290=CARTESIAN_POINT('Ctrl Pts',(-49.9423052598749,-56.4272085867039,
-39.8548713027842));
#248291=CARTESIAN_POINT('Ctrl Pts',(-49.9619348436287,-56.3200515191826,
-39.8410580052776));
#248292=CARTESIAN_POINT('Ctrl Pts',(-49.9718097439335,-56.2661448560562,
-39.8341090583478));
#248293=CARTESIAN_POINT('Ctrl Pts',(-49.9787412132511,-56.2116082672591,
-39.8265155089799));
#248294=CARTESIAN_POINT('Ctrl Pts',(-49.9827447112972,-56.1564493854985,
-39.8182791580079));
#248295=CARTESIAN_POINT('Origin',(0.,-12.9675000200282,235.35105));
#248296=CARTESIAN_POINT('Origin',(0.,-12.9675000200281,-52.64995));
#248297=CARTESIAN_POINT('Origin',(0.,-12.9675000200281,-41.3499258784557));
#248298=CARTESIAN_POINT('Ctrl Pts',(-43.1889493654702,-62.9502447313255,
-39.8182791580079));
#248299=CARTESIAN_POINT('Ctrl Pts',(-43.2381203049698,-64.1593004018075,
-40.0543903140503));
#248300=CARTESIAN_POINT('Ctrl Pts',(-43.0563273171535,-64.1720126058792,
-41.2737227474219));
#248301=CARTESIAN_POINT('Ctrl Pts',(-43.3535867800773,-62.9382951394238,
-39.8428628946803));
#248302=CARTESIAN_POINT('Ctrl Pts',(-43.5344657476846,-64.1186745033647,
-40.0946602834885));
#248303=CARTESIAN_POINT('Ctrl Pts',(-43.3845102555472,-64.1490638192631,
-41.2983071346081));
#248304=CARTESIAN_POINT('Ctrl Pts',(-43.5128106717856,-62.900266492328,
-39.8617422945218));
#248305=CARTESIAN_POINT('Ctrl Pts',(-43.8194555941901,-64.0359082545366,
-40.1253623136954));
#248306=CARTESIAN_POINT('Ctrl Pts',(-43.7017489364349,-64.0740500570513,
-41.3171858838442));
#248307=CARTESIAN_POINT('Ctrl Pts',(-43.8198961953762,-62.7708560812039,
-39.8879068185516));
#248308=CARTESIAN_POINT('Ctrl Pts',(-44.3660365185992,-63.784236525395,
-40.1674712617347));
#248309=CARTESIAN_POINT('Ctrl Pts',(-44.3133145641792,-63.8175106730215,
-41.3433504080572));
#248310=CARTESIAN_POINT('Ctrl Pts',(-43.9596150277081,-62.6828136250119,
-39.8944822858415));
#248311=CARTESIAN_POINT('Ctrl Pts',(-44.6150672888654,-63.6215845466811,
-40.1779974336972));
#248312=CARTESIAN_POINT('Ctrl Pts',(-44.5914157734028,-63.6426042714052,
-41.3499258753244));
#248313=CARTESIAN_POINT('Ctrl Pts',(-44.0845625322693,-62.5717696510307,
-39.8944822890418));
#248314=CARTESIAN_POINT('Ctrl Pts',(-44.8399443096849,-63.4217307078938,
-40.1779974386957));
#248315=CARTESIAN_POINT('Ctrl Pts',(-44.8399443096849,-63.4217307078937,
-41.3499258784558));
#248316=CARTESIAN_POINT('',(-44.0845625322693,-62.5717696510307,-39.8944822890418));
#248317=CARTESIAN_POINT('Origin',(-43.843501102803,-62.3005255814968,-41.3499258784557));
#248318=CARTESIAN_POINT('',(-43.1889493654702,-62.9502447313255,-39.8182791580079));
#248319=CARTESIAN_POINT('Origin',(-42.9516926065373,-62.6756665304895,-41.2737227474219));
#248320=CARTESIAN_POINT('Ctrl Pts',(-43.1889493654702,-62.9502447313255,
-39.8182791580079));
#248321=CARTESIAN_POINT('Ctrl Pts',(-43.3060164327879,-62.941747862638,
-39.8357596692676));
#248322=CARTESIAN_POINT('Ctrl Pts',(-43.4202366092229,-62.9200777320772,
-39.8503404874849));
#248323=CARTESIAN_POINT('Ctrl Pts',(-43.5315808098265,-62.8850650035002,
-39.8620074891437));
#248324=CARTESIAN_POINT('Ctrl Pts',(-43.576984227273,-62.8707876767701,
-39.8667650045221));
#248325=CARTESIAN_POINT('Ctrl Pts',(-43.6219093041748,-62.8542911619851,
-39.8710378813417));
#248326=CARTESIAN_POINT('Ctrl Pts',(-43.6663535544392,-62.8355615905537,
-39.8748246333721));
#248327=CARTESIAN_POINT('Ctrl Pts',(-43.6664338301504,-62.8355277609885,
-39.8748314730468));
#248328=CARTESIAN_POINT('Ctrl Pts',(-43.6665141020671,-62.8354939250504,
-39.8748383109414));
#248329=CARTESIAN_POINT('Ctrl Pts',(-43.6665943701892,-62.8354600827397,
-39.8748451470561));
#248330=CARTESIAN_POINT('Ctrl Pts',(-43.7466420990545,-62.8017106932806,
-39.8816624917103));
#248331=CARTESIAN_POINT('Ctrl Pts',(-43.8228753762229,-62.7616456114789,
-39.8867070324442));
#248332=CARTESIAN_POINT('Ctrl Pts',(-43.8952322702234,-62.7152894963873,
-39.8899765761625));
#248333=CARTESIAN_POINT('Ctrl Pts',(-43.9616292098301,-62.6727516813436,
-39.8929768113136));
#248334=CARTESIAN_POINT('Ctrl Pts',(-44.0247618696465,-62.62491600457,-39.8944822890418));
#248335=CARTESIAN_POINT('Ctrl Pts',(-44.0845625322693,-62.5717696510307,
-39.8944822890418));
#248336=CARTESIAN_POINT('Origin',(-44.0630480057166,-64.1016158376104,235.35105));
#248337=CARTESIAN_POINT('',(-44.0630480057166,-64.1016158376104,-52.64995));
#248338=CARTESIAN_POINT('Ctrl Pts',(-43.0563273171535,-64.1720126058792,
-41.273722747422));
#248339=CARTESIAN_POINT('Ctrl Pts',(-37.4870209577721,-64.5614564443275,
-40.4393222961258));
#248340=CARTESIAN_POINT('Ctrl Pts',(-31.9038741755017,-64.9518680994243,
-39.7153157040947));
#248341=CARTESIAN_POINT('Ctrl Pts',(-26.299256677934,-65.343781133192,-39.1625636424987));
#248342=CARTESIAN_POINT('Ctrl Pts',(-26.299256677934,-65.343781133192,-39.1625636424987));
#248343=CARTESIAN_POINT('Ctrl Pts',(-26.4161222952887,-65.3356090931445,
-37.971813107807));
#248344=CARTESIAN_POINT('Ctrl Pts',(-26.3607251006126,-64.1700706217802,
-37.7071200530847));
#248345=CARTESIAN_POINT('Ctrl Pts',(-25.9205756959923,-65.3702610870028,
-39.1065428641436));
#248346=CARTESIAN_POINT('Ctrl Pts',(-26.0004074167526,-65.3498956258429,
-37.9286345805822));
#248347=CARTESIAN_POINT('Ctrl Pts',(-25.7896847017718,-64.2113141700146,
-37.6510924855215));
#248348=CARTESIAN_POINT('Ctrl Pts',(-25.5571787362025,-65.4658460313782,
-39.0779244541051));
#248349=CARTESIAN_POINT('Ctrl Pts',(-25.5933889787346,-65.4485099708086,
-37.9059960140076));
#248350=CARTESIAN_POINT('Ctrl Pts',(-25.2415430286856,-64.3562400899596,
-37.6224808645879));
#248351=CARTESIAN_POINT('Ctrl Pts',(-25.2130575054386,-65.6305979870176,
-39.0779244525544));
#248352=CARTESIAN_POINT('Ctrl Pts',(-25.2130575054386,-65.6305979870177,
-37.9059960127943));
#248353=CARTESIAN_POINT('Ctrl Pts',(-24.722024317517,-64.6049655790884,
-37.6224808631404));
#248354=CARTESIAN_POINT('',(-26.3607251006126,-64.1700706217802,-37.7071200530847));
#248355=CARTESIAN_POINT('Origin',(-26.1946219673178,-63.8474350578023,-39.1625636424987));
#248356=CARTESIAN_POINT('',(-24.722024317517,-64.6049655790884,-37.6224808631404));
#248357=CARTESIAN_POINT('Origin',(-24.5653232085747,-64.2776603385407,-39.0779244525544));
#248358=CARTESIAN_POINT('Ctrl Pts',(-24.722024317517,-64.6049655790884,
-37.6224808631404));
#248359=CARTESIAN_POINT('Ctrl Pts',(-24.8664081169227,-64.5358401936933,
-37.6224808635427));
#248360=CARTESIAN_POINT('Ctrl Pts',(-25.0128268065285,-64.4748117336668,
-37.6246896514935));
#248361=CARTESIAN_POINT('Ctrl Pts',(-25.1612581100212,-64.4217914620098,
-37.629072347169));
#248362=CARTESIAN_POINT('Ctrl Pts',(-25.3100469028066,-64.3686434937081,
-37.6334655983456));
#248363=CARTESIAN_POINT('Ctrl Pts',(-25.4608581371227,-64.3235423252056,
-37.6400432640483));
#248364=CARTESIAN_POINT('Ctrl Pts',(-25.6136827889703,-64.2864475050405,
-37.648783682524));
#248365=CARTESIAN_POINT('Ctrl Pts',(-25.7668553223293,-64.2492682442964,
-37.6575439972006));
#248366=CARTESIAN_POINT('Ctrl Pts',(-25.9220505706891,-64.2201318026351,
-37.6684769422025));
#248367=CARTESIAN_POINT('Ctrl Pts',(-26.0792710874908,-64.1990467735369,
-37.6815739018329));
#248368=CARTESIAN_POINT('Ctrl Pts',(-26.1723778756961,-64.1865601122634,
-37.6893299878148));
#248369=CARTESIAN_POINT('Ctrl Pts',(-26.2661951513385,-64.1768980730961,
-37.6978452572376));
#248370=CARTESIAN_POINT('Ctrl Pts',(-26.3607251006126,-64.1700706217802,
-37.7071200530847));
#248371=CARTESIAN_POINT('Ctrl Pts',(-43.9586137318958,-64.1089185934363,
-41.4098789472402));
#248372=CARTESIAN_POINT('Ctrl Pts',(-44.1434687505058,-64.0959922713062,
-40.1874603719527));
#248373=CARTESIAN_POINT('Ctrl Pts',(-44.0941462007501,-62.8828332296677,
-39.9541044945113));
#248374=CARTESIAN_POINT('Ctrl Pts',(-37.7893866621767,-64.5403129745774,
-40.4723364366453));
#248375=CARTESIAN_POINT('Ctrl Pts',(-37.983387269697,-64.5267471306234,
-39.2654008360683));
#248376=CARTESIAN_POINT('Ctrl Pts',(-37.9047806371077,-63.3320208489792,
-39.0165447742965));
#248377=CARTESIAN_POINT('Ctrl Pts',(-31.6035178480626,-64.9728710598491,
-39.6662697593448));
#248378=CARTESIAN_POINT('Ctrl Pts',(-31.7696060423701,-64.9612570419197,
-38.4686952332404));
#248379=CARTESIAN_POINT('Ctrl Pts',(-31.6931000950573,-63.7835313257006,
-38.2104625119264));
#248380=CARTESIAN_POINT('Ctrl Pts',(-25.390939784773,-65.4072968377652,
-39.074508439621));
#248381=CARTESIAN_POINT('Ctrl Pts',(-25.503745040343,-65.3994087258724,
-37.8837048863563));
#248382=CARTESIAN_POINT('Ctrl Pts',(-25.4475537226946,-64.2343331337137,
-37.6186845317716));
#248383=CARTESIAN_POINT('Ctrl Pts',(-26.3607251006126,-64.1700706217802,
-37.7071200530847));
#248384=CARTESIAN_POINT('Ctrl Pts',(-26.9782676591259,-64.1254684477288,
-37.7677101762428));
#248385=CARTESIAN_POINT('Ctrl Pts',(-27.5952002861798,-64.0809650014557,
-37.830358117877));
#248386=CARTESIAN_POINT('Ctrl Pts',(-28.2117112797203,-64.0365095004908,
-37.894983680275));
#248387=CARTESIAN_POINT('Ctrl Pts',(-28.8402455667364,-63.9911870214179,
-37.9608695804625));
#248388=CARTESIAN_POINT('Ctrl Pts',(-29.4683415491132,-63.9459140349067,
-38.0288109893072));
#248389=CARTESIAN_POINT('Ctrl Pts',(-30.0961447214576,-63.9006435374936,
-38.0987229249114));
#248390=CARTESIAN_POINT('Ctrl Pts',(-30.7311061421422,-63.854856863232,
-38.1694320004778));
#248391=CARTESIAN_POINT('Ctrl Pts',(-31.365767875829,-63.8090724214961,
-38.2421567951076));
#248392=CARTESIAN_POINT('Ctrl Pts',(-32.0002275449116,-63.7632534702054,
-38.3168093867271));
#248393=CARTESIAN_POINT('Ctrl Pts',(-32.6418016585458,-63.7169207330836,
-38.39229908707));
#248394=CARTESIAN_POINT('Ctrl Pts',(-33.283168966963,-63.6705524205074,
-38.4697600610882));
#248395=CARTESIAN_POINT('Ctrl Pts',(-33.9243792500023,-63.6241272043221,
-38.5491013957037));
#248396=CARTESIAN_POINT('Ctrl Pts',(-34.5727070787781,-63.5771866601574,
-38.6293234329419));
#248397=CARTESIAN_POINT('Ctrl Pts',(-35.2208741753138,-63.5301876833421,
-38.7114678071238));
#248398=CARTESIAN_POINT('Ctrl Pts',(-35.8688829127333,-63.4831293271622,
-38.7954405439891));
#248399=CARTESIAN_POINT('Ctrl Pts',(-36.528007916167,-63.4352637084019,
-38.8808537911855));
#248400=CARTESIAN_POINT('Ctrl Pts',(-37.1869689079169,-63.3873363978492,
-38.9681586684062));
#248401=CARTESIAN_POINT('Ctrl Pts',(-37.8457206741843,-63.3393720909894,
-39.0572562817087));
#248402=CARTESIAN_POINT('Ctrl Pts',(-38.5108024898544,-63.290946887556,
-39.1472100480005));
#248403=CARTESIAN_POINT('Ctrl Pts',(-39.1756707976568,-63.2424837816027,
-39.2389911692744));
#248404=CARTESIAN_POINT('Ctrl Pts',(-39.840234097892,-63.1940375338189,
-39.3324978732434));
#248405=CARTESIAN_POINT('Ctrl Pts',(-40.5151066360261,-63.144839749058,
-39.4274551280569));
#248406=CARTESIAN_POINT('Ctrl Pts',(-41.1896644203457,-63.095659160954,
-39.524191918062));
#248407=CARTESIAN_POINT('Ctrl Pts',(-41.8637688574652,-63.0465861854865,
-39.6226016607987));
#248408=CARTESIAN_POINT('Ctrl Pts',(-42.3057074499343,-63.014414254088,
-39.6871184638273));
#248409=CARTESIAN_POINT('Ctrl Pts',(-42.7474503238866,-62.9822892633039,
-39.7523543070286));
#248410=CARTESIAN_POINT('Ctrl Pts',(-43.1889493654702,-62.9502447313255,
-39.8182791580079));
#248411=CARTESIAN_POINT('Origin',(0.,-12.9675000200281,-41.3499258784557));
#248412=CARTESIAN_POINT('Origin',(0.,-12.9675000200281,-39.8944822890418));
#248413=CARTESIAN_POINT('Ctrl Pts',(-51.14141857343,30.9911137115562,-41.409878947203));
#248414=CARTESIAN_POINT('Ctrl Pts',(-51.1284922512846,31.175968730169,-40.1874603718989));
#248415=CARTESIAN_POINT('Ctrl Pts',(-49.9153332096598,31.1266461804112,
-39.9541044944637));
#248416=CARTESIAN_POINT('Ctrl Pts',(-51.5728129545556,24.8218866420576,
-40.4723364365686));
#248417=CARTESIAN_POINT('Ctrl Pts',(-51.5592471107002,25.0158872495489,
-39.2654008361028));
#248418=CARTESIAN_POINT('Ctrl Pts',(-50.3645208289796,24.9372806169763,
-39.0165447742893));
#248419=CARTESIAN_POINT('Ctrl Pts',(-52.0053710398143,18.6360178281302,
-39.6662697593861));
#248420=CARTESIAN_POINT('Ctrl Pts',(-51.9937570218959,18.8021060224485,
-38.4686952333466));
#248421=CARTESIAN_POINT('Ctrl Pts',(-50.8160313056482,18.7256000751318,
-38.2104625119396));
#248422=CARTESIAN_POINT('Ctrl Pts',(-52.4397968177151,12.4234397650578,
-39.0745084396475));
#248423=CARTESIAN_POINT('Ctrl Pts',(-52.4319087058198,12.5362450206276,
-37.883704886372));
#248424=CARTESIAN_POINT('Ctrl Pts',(-51.266833113666,12.4800537029801,-37.618684531802));
#248425=CARTESIAN_POINT('Ctrl Pts',(-51.202570601752,13.3932250805846,-37.7071200530847));
#248426=CARTESIAN_POINT('Ctrl Pts',(-51.1579684277001,14.0107676390858,
-37.7677101762413));
#248427=CARTESIAN_POINT('Ctrl Pts',(-51.1134649814269,14.6277002661276,
-37.830358117874));
#248428=CARTESIAN_POINT('Ctrl Pts',(-51.0690094804622,15.2442112596561,
-37.8949836802706));
#248429=CARTESIAN_POINT('Ctrl Pts',(-51.023687001393,15.8727455466137,-37.9608695804517));
#248430=CARTESIAN_POINT('Ctrl Pts',(-50.9784140148859,16.5008415289319,
-38.0288109892898));
#248431=CARTESIAN_POINT('Ctrl Pts',(-50.9331435174771,17.1286447012179,
-38.0987229248871));
#248432=CARTESIAN_POINT('Ctrl Pts',(-50.8873568432167,17.7636061218883,
-38.1694320004514));
#248433=CARTESIAN_POINT('Ctrl Pts',(-50.8415724014823,18.3982678555611,
-38.2421567950793));
#248434=CARTESIAN_POINT('Ctrl Pts',(-50.7957534501932,19.0327275246296,
-38.3168093866967));
#248435=CARTESIAN_POINT('Ctrl Pts',(-50.749420713076,19.6743016382088,-38.3922990870328));
#248436=CARTESIAN_POINT('Ctrl Pts',(-50.7030524005045,20.315668946571,-38.4697600610437));
#248437=CARTESIAN_POINT('Ctrl Pts',(-50.656627184324,20.9568792295554,-38.5491013956518));
#248438=CARTESIAN_POINT('Ctrl Pts',(-50.6096866401672,21.6052070582347,
-38.6293234328774));
#248439=CARTESIAN_POINT('Ctrl Pts',(-50.5626876633598,22.2533741546739,
-38.7114678070461));
#248440=CARTESIAN_POINT('Ctrl Pts',(-50.5156293071878,22.9013828919971,
-38.7954405438977));
#248441=CARTESIAN_POINT('Ctrl Pts',(-50.4677636884305,23.5605078954009,
-38.8808537910891));
#248442=CARTESIAN_POINT('Ctrl Pts',(-50.4198363778808,24.2194688871211,
-38.9681586683046));
#248443=CARTESIAN_POINT('Ctrl Pts',(-50.3718720710237,24.8782206533588,
-39.0572562816017));
#248444=CARTESIAN_POINT('Ctrl Pts',(-50.3234468675883,25.5433024690615,
-39.1472100478965));
#248445=CARTESIAN_POINT('Ctrl Pts',(-50.2749837616329,26.2081707768964,
-39.2389911691736));
#248446=CARTESIAN_POINT('Ctrl Pts',(-50.2265375138466,26.8727340771642,
-39.3324978731459));
#248447=CARTESIAN_POINT('Ctrl Pts',(-50.1773397290819,27.5476066153477,
-39.4274551279651));
#248448=CARTESIAN_POINT('Ctrl Pts',(-50.1281591409739,28.2221643997166,
-39.524191917976));
#248449=CARTESIAN_POINT('Ctrl Pts',(-50.0790861655016,28.8962688368852,
-39.6226016607187));
#248450=CARTESIAN_POINT('Ctrl Pts',(-50.0469142340889,29.3382074295385,
-39.6871184637734));
#248451=CARTESIAN_POINT('Ctrl Pts',(-50.0147892432904,29.7799503036747,
-39.7523543070014));
#248452=CARTESIAN_POINT('Ctrl Pts',(-49.9827447112974,30.221449345442,-39.8182791580079));
#248453=CARTESIAN_POINT('Origin',(0.,-12.9675000200281,-41.3499258784557));
#248454=CARTESIAN_POINT('Origin',(0.,-12.9675000200281,-39.8944822890418));
#248455=CARTESIAN_POINT('Ctrl Pts',(-25.390939784986,39.4722967976939,-39.0745084396377));
#248456=CARTESIAN_POINT('Ctrl Pts',(-25.5037450405553,39.4644086857989,
-37.8837048863654));
#248457=CARTESIAN_POINT('Ctrl Pts',(-25.4475537229077,38.2993330936448,
-37.6186845317924));
#248458=CARTESIAN_POINT('Ctrl Pts',(-31.6035178481249,39.0378710197884,
-39.6662697593827));
#248459=CARTESIAN_POINT('Ctrl Pts',(-31.7696060424436,39.0262570018692,
-38.4686952333224));
#248460=CARTESIAN_POINT('Ctrl Pts',(-31.6931000951265,37.8485312856233,
-38.2104625119342));
#248461=CARTESIAN_POINT('Ctrl Pts',(-37.78938666212,38.6053129345249,-40.4723364365685));
#248462=CARTESIAN_POINT('Ctrl Pts',(-37.9833872696133,38.59174709065,-39.2654008361018));
#248463=CARTESIAN_POINT('Ctrl Pts',(-37.9047806370375,37.397020808928,-39.0165447742889));
#248464=CARTESIAN_POINT('Ctrl Pts',(-43.9586137316839,38.1739185533947,
-41.4098789472187));
#248465=CARTESIAN_POINT('Ctrl Pts',(-44.143468750297,38.1609922312524,-40.1874603719145));
#248466=CARTESIAN_POINT('Ctrl Pts',(-44.0941462005395,36.9478331896271,
-39.9541044944794));
#248467=CARTESIAN_POINT('Ctrl Pts',(-43.1889493654703,37.0152446912691,
-39.8182791580079));
#248468=CARTESIAN_POINT('Ctrl Pts',(-42.4904603455135,37.0659418652793,
-39.7139804388393));
#248469=CARTESIAN_POINT('Ctrl Pts',(-41.7913631998226,37.1168384172332,
-39.6114063013225));
#248470=CARTESIAN_POINT('Ctrl Pts',(-41.0918404324428,37.1678090072805,
-39.5106756721723));
#248471=CARTESIAN_POINT('Ctrl Pts',(-40.4273733396133,37.2162252724371,
-39.4149930276158));
#248472=CARTESIAN_POINT('Ctrl Pts',(-39.7625221889097,37.264708707939,-39.3209737511287));
#248473=CARTESIAN_POINT('Ctrl Pts',(-39.0974046393108,37.3131849458321,
-39.2287197708965));
#248474=CARTESIAN_POINT('Ctrl Pts',(-38.4397880037208,37.3611144892467,
-39.1375061919785));
#248475=CARTESIAN_POINT('Ctrl Pts',(-37.7819111637672,37.4090371649522,
-39.0480183173054));
#248476=CARTESIAN_POINT('Ctrl Pts',(-37.1238471677498,37.4569106864784,
-38.9603546652988));
#248477=CARTESIAN_POINT('Ctrl Pts',(-36.4731112694083,37.5042510959609,
-38.873667222002));
#248478=CARTESIAN_POINT('Ctrl Pts',(-35.8221925731159,37.551543640539,-38.7887635990717));
#248479=CARTESIAN_POINT('Ctrl Pts',(-35.1711185085701,37.5987738016015,
-38.7057390601872));
#248480=CARTESIAN_POINT('Ctrl Pts',(-34.5272799080192,37.6454790882318,
-38.623637182939));
#248481=CARTESIAN_POINT('Ctrl Pts',(-33.8832895753389,37.6921236016348,
-38.5433728568344));
#248482=CARTESIAN_POINT('Ctrl Pts',(-33.2391284750776,37.738716035705,-38.4650382046873));
#248483=CARTESIAN_POINT('Ctrl Pts',(-32.6058302106908,37.7845227564434,
-38.3880245520065));
#248484=CARTESIAN_POINT('Ctrl Pts',(-31.9723670273983,37.8302794124422,
-38.3128760397775));
#248485=CARTESIAN_POINT('Ctrl Pts',(-31.3386741185916,37.8760126096808,
-38.2396802084161));
#248486=CARTESIAN_POINT('Ctrl Pts',(-30.7112206329954,37.9212955118816,
-38.1672050727778));
#248487=CARTESIAN_POINT('Ctrl Pts',(-30.0835420992274,37.9665556913751,
-38.09664435461));
#248488=CARTESIAN_POINT('Ctrl Pts',(-29.4555270109952,38.0118330876516,
-38.0280830339018));
#248489=CARTESIAN_POINT('Ctrl Pts',(-28.8372567832138,38.0564079181513,
-37.9605855737842));
#248490=CARTESIAN_POINT('Ctrl Pts',(-28.2186604708678,38.1009997405071,
-37.8950259435464));
#248491=CARTESIAN_POINT('Ctrl Pts',(-27.5995823364983,38.1456560947805,
-37.8314852283597));
#248492=CARTESIAN_POINT('Ctrl Pts',(-27.1868647446055,38.1754269136404,
-37.789124871075));
#248493=CARTESIAN_POINT('Ctrl Pts',(-26.7739319975608,38.2052266046837,
-37.7476618043058));
#248494=CARTESIAN_POINT('Ctrl Pts',(-26.3607251006129,38.2350705817238,
-37.7071200530847));
#248495=CARTESIAN_POINT('Origin',(26.5085260991663,-68.3364732839715,-55.24995));
#248496=CARTESIAN_POINT('',(26.299256677934,-65.343781133192,-39.1625636424987));
#248497=CARTESIAN_POINT('',(26.299256677934,-65.343781133192,-52.64995));
#248498=CARTESIAN_POINT('',(26.299256677934,-65.343781133192,-52.64995));
#248499=CARTESIAN_POINT('',(25.2130575054386,-65.6305979870176,-39.0779244525544));
#248500=CARTESIAN_POINT('Ctrl Pts',(26.299256677934,-65.343781133192,-39.1625636424987));
#248501=CARTESIAN_POINT('Ctrl Pts',(26.2254373064082,-65.3489430865025,
-39.1516430551934));
#248502=CARTESIAN_POINT('Ctrl Pts',(26.1520152366826,-65.3567479315796,
-39.1417380677395));
#248503=CARTESIAN_POINT('Ctrl Pts',(26.0791903717072,-65.3672001454729,
-39.1328886242715));
#248504=CARTESIAN_POINT('Ctrl Pts',(26.0033259821766,-65.3780886081775,
-39.1236698275513));
#248505=CARTESIAN_POINT('Ctrl Pts',(25.9281098779661,-65.3918504119504,
-39.1155967042653));
#248506=CARTESIAN_POINT('Ctrl Pts',(25.8537553847433,-65.4084357764527,
-39.1086925042226));
#248507=CARTESIAN_POINT('Ctrl Pts',(25.7824469356956,-65.4243416964353,
-39.1020711451678));
#248508=CARTESIAN_POINT('Ctrl Pts',(25.711930945636,-65.4428441967757,-39.0965247723696));
#248509=CARTESIAN_POINT('Ctrl Pts',(25.6423830881242,-65.4638512240535,
-39.0920542502616));
#248510=CARTESIAN_POINT('Ctrl Pts',(25.5726544940153,-65.4849128430724,
-39.087572110442));
#248511=CARTESIAN_POINT('Ctrl Pts',(25.5038991449303,-65.5084919753254,
-39.0841714266781));
#248512=CARTESIAN_POINT('Ctrl Pts',(25.4362806067455,-65.5344490373293,
-39.081833571492));
#248513=CARTESIAN_POINT('Ctrl Pts',(25.3682218634524,-65.5605750830409,
-39.0794804965774));
#248514=CARTESIAN_POINT('Ctrl Pts',(25.3013148512129,-65.5891100638622,
-39.0782041359531));
#248515=CARTESIAN_POINT('Ctrl Pts',(25.2357116044156,-65.6198650319822,
-39.0779656809084));
#248516=CARTESIAN_POINT('Ctrl Pts',(25.2281428273083,-65.6234132938444,
-39.0779381698754));
#248517=CARTESIAN_POINT('Ctrl Pts',(25.2205913875361,-65.626991055221,-39.0779244525544));
#248518=CARTESIAN_POINT('Ctrl Pts',(25.2130575054386,-65.6305979870176,
-39.0779244525544));
#248519=CARTESIAN_POINT('',(25.2130575054386,-65.6305979870176,-52.64995));
#248520=CARTESIAN_POINT('',(25.2130575054386,-65.6305979870176,-55.24995));
#248521=CARTESIAN_POINT('Origin',(26.5085260991663,-68.3364732839715,-52.64995));
#248522=CARTESIAN_POINT('Origin',(55.3689732639432,-39.4760261191947,-55.24995));
#248523=CARTESIAN_POINT('',(52.6630979669894,-38.1805575254669,-39.0779244525544));
#248524=CARTESIAN_POINT('',(52.6630979669894,-38.1805575254669,-52.64995));
#248525=CARTESIAN_POINT('',(52.6630979669894,-38.1805575254669,-55.24995));
#248526=CARTESIAN_POINT('',(52.3762811131638,-39.2667566979623,-39.1625636424987));
#248527=CARTESIAN_POINT('Ctrl Pts',(52.6630979669894,-38.1805575254669,
-39.0779244525544));
#248528=CARTESIAN_POINT('Ctrl Pts',(52.6318538057676,-38.2458179296431,
-39.0779244525544));
#248529=CARTESIAN_POINT('Ctrl Pts',(52.6028021694694,-38.3123970248505,
-39.0789553362961));
#248530=CARTESIAN_POINT('Ctrl Pts',(52.5761369448303,-38.380144816412,-39.0810581140022));
#248531=CARTESIAN_POINT('Ctrl Pts',(52.5486170513734,-38.4500640475814,
-39.0832282895481));
#248532=CARTESIAN_POINT('Ctrl Pts',(52.5236393921055,-38.5212281199008,
-39.0865403103588));
#248533=CARTESIAN_POINT('Ctrl Pts',(52.5013651848038,-38.5934555718355,
-39.091017145468));
#248534=CARTESIAN_POINT('Ctrl Pts',(52.4799837840479,-38.6627879648801,
-39.095314537707));
#248535=CARTESIAN_POINT('Ctrl Pts',(52.4610932034441,-38.7331000345627,
-39.1006851051596));
#248536=CARTESIAN_POINT('Ctrl Pts',(52.4447889514025,-38.804217595539,-39.1071295131387));
#248537=CARTESIAN_POINT('Ctrl Pts',(52.4284881332189,-38.8753201783607,
-39.1135725638534));
#248538=CARTESIAN_POINT('Ctrl Pts',(52.4147725871611,-38.9472278341315,
-39.1210889899846));
#248539=CARTESIAN_POINT('Ctrl Pts',(52.4036908710759,-39.0197541971,-39.1296602879662));
#248540=CARTESIAN_POINT('Ctrl Pts',(52.3925835339235,-39.0924482419338,
-39.1382514028967));
#248541=CARTESIAN_POINT('Ctrl Pts',(52.3841222371824,-39.1657637734407,
-39.1479022534551));
#248542=CARTESIAN_POINT('Ctrl Pts',(52.3783083555277,-39.2395020072502,
-39.158575180387));
#248543=CARTESIAN_POINT('Ctrl Pts',(52.377592552146,-39.248580636685,-39.1598892279794));
#248544=CARTESIAN_POINT('Ctrl Pts',(52.3769168204106,-39.2576656607894,
-39.1612187453113));
#248545=CARTESIAN_POINT('Ctrl Pts',(52.3762811131638,-39.2667566979623,
-39.1625636424987));
#248546=CARTESIAN_POINT('',(52.3762811131638,-39.2667566979623,-52.64995));
#248547=CARTESIAN_POINT('',(52.3762811131638,-39.2667566979623,-37.9059960127943));
#248548=CARTESIAN_POINT('Origin',(55.3689732639432,-39.4760261191947,-52.64995));
#248549=CARTESIAN_POINT('Origin',(55.3689732639433,13.5410260791383,-55.24995));
#248550=CARTESIAN_POINT('',(52.3762811131638,13.3317566579059,-39.1625636424987));
#248551=CARTESIAN_POINT('',(52.3762811131638,13.3317566579059,-52.64995));
#248552=CARTESIAN_POINT('',(52.3762811131638,13.3317566579059,-52.64995));
#248553=CARTESIAN_POINT('',(52.6630979669895,12.2455574854105,-39.0779244525544));
#248554=CARTESIAN_POINT('Ctrl Pts',(52.3762811131638,13.3317566579059,-39.1625636424987));
#248555=CARTESIAN_POINT('Ctrl Pts',(52.3814430664743,13.257937286379,-39.1516430551932));
#248556=CARTESIAN_POINT('Ctrl Pts',(52.3892479115517,13.1845152166523,-39.1417380677392));
#248557=CARTESIAN_POINT('Ctrl Pts',(52.3997001254452,13.1116903516758,-39.1328886242711));
#248558=CARTESIAN_POINT('Ctrl Pts',(52.4105885881499,13.0358259621455,-39.1236698275509));
#248559=CARTESIAN_POINT('Ctrl Pts',(52.4243503919228,12.9606098579354,-39.115596704265));
#248560=CARTESIAN_POINT('Ctrl Pts',(52.4409357564251,12.8862553647129,-39.1086925042223));
#248561=CARTESIAN_POINT('Ctrl Pts',(52.4568416764079,12.8149469156643,-39.1020711451675));
#248562=CARTESIAN_POINT('Ctrl Pts',(52.4753441767486,12.7444309256038,-39.0965247723692));
#248563=CARTESIAN_POINT('Ctrl Pts',(52.4963512040269,12.6748830680911,-39.0920542502613));
#248564=CARTESIAN_POINT('Ctrl Pts',(52.5174128230462,12.6051544739813,-39.0875721104417));
#248565=CARTESIAN_POINT('Ctrl Pts',(52.5409919552997,12.5363991248954,-39.0841714266778));
#248566=CARTESIAN_POINT('Ctrl Pts',(52.5669490173042,12.4687805867097,-39.0818335714918));
#248567=CARTESIAN_POINT('Ctrl Pts',(52.5930750630163,12.4007218434158,-39.0794804965772));
#248568=CARTESIAN_POINT('Ctrl Pts',(52.6216100438381,12.3338148311756,-39.078204135953));
#248569=CARTESIAN_POINT('Ctrl Pts',(52.6523650119588,12.2682115843776,-39.0779656809083));
#248570=CARTESIAN_POINT('Ctrl Pts',(52.6559132738194,12.2606428072736,-39.0779381698754));
#248571=CARTESIAN_POINT('Ctrl Pts',(52.6594910351945,12.2530913675048,-39.0779244525544));
#248572=CARTESIAN_POINT('Ctrl Pts',(52.6630979669895,12.2455574854105,-39.0779244525544));
#248573=CARTESIAN_POINT('',(52.6630979669895,12.2455574854105,-52.64995));
#248574=CARTESIAN_POINT('',(52.6630979669895,12.2455574854105,-55.24995));
#248575=CARTESIAN_POINT('Origin',(55.3689732639433,13.5410260791383,-52.64995));
#248576=CARTESIAN_POINT('Origin',(26.5085260991666,42.4014732439151,-55.24995));
#248577=CARTESIAN_POINT('',(25.2130575054389,39.6955979469612,-39.0779244525544));
#248578=CARTESIAN_POINT('',(25.2130575054389,39.6955979469612,-52.64995));
#248579=CARTESIAN_POINT('',(25.2130575054389,39.6955979469612,-55.24995));
#248580=CARTESIAN_POINT('',(26.2992566779342,39.4087810931356,-39.1625636424987));
#248581=CARTESIAN_POINT('Ctrl Pts',(25.2130575054389,39.6955979469612,-39.0779244525544));
#248582=CARTESIAN_POINT('Ctrl Pts',(25.2783179096223,39.6643537857359,-39.0779244525544));
#248583=CARTESIAN_POINT('Ctrl Pts',(25.3448970048371,39.6353021494348,-39.0789553362963));
#248584=CARTESIAN_POINT('Ctrl Pts',(25.4126447964065,39.6086369247934,-39.081058114003));
#248585=CARTESIAN_POINT('Ctrl Pts',(25.4825640275743,39.5811170313378,-39.083228289549));
#248586=CARTESIAN_POINT('Ctrl Pts',(25.553728099892,39.5561393720712,-39.0865403103599));
#248587=CARTESIAN_POINT('Ctrl Pts',(25.625955551825,39.5338651647706,-39.0910171454692));
#248588=CARTESIAN_POINT('Ctrl Pts',(25.6952879448785,39.5124837640123,-39.0953145377089));
#248589=CARTESIAN_POINT('Ctrl Pts',(25.7656000145702,39.4935931834069,-39.1006851051625));
#248590=CARTESIAN_POINT('Ctrl Pts',(25.8367175755558,39.4772889313643,-39.1071295131429));
#248591=CARTESIAN_POINT('Ctrl Pts',(25.9078201583872,39.4609881131796,-39.1135725638588));
#248592=CARTESIAN_POINT('Ctrl Pts',(25.9797278141677,39.4472725671214,-39.1210889899916));
#248593=CARTESIAN_POINT('Ctrl Pts',(26.0522541771461,39.4361908510365,-39.1296602879749));
#248594=CARTESIAN_POINT('Ctrl Pts',(26.1249482219899,39.4250835138844,-39.1382514029073));
#248595=CARTESIAN_POINT('Ctrl Pts',(26.198263753507,39.4166222171442,-39.1479022534678));
#248596=CARTESIAN_POINT('Ctrl Pts',(26.2720019873267,39.4108083354913,-39.1585751804022));
#248597=CARTESIAN_POINT('Ctrl Pts',(26.2810806167268,39.4100925321126,-39.1598892279896));
#248598=CARTESIAN_POINT('Ctrl Pts',(26.2901656407963,39.4094168003799,-39.1612187453165));
#248599=CARTESIAN_POINT('Ctrl Pts',(26.2992566779342,39.4087810931356,-39.1625636424987));
#248600=CARTESIAN_POINT('',(26.2992566779342,39.4087810931356,-52.64995));
#248601=CARTESIAN_POINT('',(26.2992566779342,39.4087810931356,-37.9059960127943));
#248602=CARTESIAN_POINT('Origin',(26.5085260991666,42.4014732439151,-52.64995));
#248603=CARTESIAN_POINT('Origin',(0.,-12.9675000200281,-55.24995));
#248604=CARTESIAN_POINT('Origin',(0.,-12.9675000200281,-39.0779244525544));
#248605=CARTESIAN_POINT('Origin',(0.,-12.9675000200281,-52.64995));
#248606=CARTESIAN_POINT('Ctrl Pts',(24.7220243175171,38.669965539032,-37.6224808631404));
#248607=CARTESIAN_POINT('Ctrl Pts',(25.2130575054388,39.6955979469612,-37.9059960127943));
#248608=CARTESIAN_POINT('Ctrl Pts',(25.2130575054389,39.6955979469612,-39.0779244525544));
#248609=CARTESIAN_POINT('Ctrl Pts',(25.2415430286799,38.4212400498976,-37.6224808645859));
#248610=CARTESIAN_POINT('Ctrl Pts',(25.5933889787397,39.5135099307705,-37.9059960140155));
#248611=CARTESIAN_POINT('Ctrl Pts',(25.5571787362036,39.5308459913215,-39.077924454111));
#248612=CARTESIAN_POINT('Ctrl Pts',(25.7896847017763,38.2763141299578,-37.6510924855219));
#248613=CARTESIAN_POINT('Ctrl Pts',(26.0004074167487,39.4148955857669,-37.9286345805798));
#248614=CARTESIAN_POINT('Ctrl Pts',(25.9205756959913,39.4352610469465,-39.1065428641433));
#248615=CARTESIAN_POINT('Ctrl Pts',(26.3607251006129,38.2350705817238,-37.7071200530847));
#248616=CARTESIAN_POINT('Ctrl Pts',(26.4161222952889,39.4006090530882,-37.971813107807));
#248617=CARTESIAN_POINT('Ctrl Pts',(26.2992566779342,39.4087810931356,-39.1625636424987));
#248618=CARTESIAN_POINT('',(24.7220243175171,38.669965539032,-37.6224808631404));
#248619=CARTESIAN_POINT('Origin',(24.5653232085749,38.3426602984844,-39.0779244525544));
#248620=CARTESIAN_POINT('',(26.3607251006129,38.2350705817238,-37.7071200530847));
#248621=CARTESIAN_POINT('Ctrl Pts',(26.3607251006129,38.2350705817238,-37.7071200530847));
#248622=CARTESIAN_POINT('Ctrl Pts',(26.2011255350992,38.2465977037834,-37.6914609588104));
#248623=CARTESIAN_POINT('Ctrl Pts',(26.0435569434565,38.2662022062977,-37.6779662189505));
#248624=CARTESIAN_POINT('Ctrl Pts',(25.8880107550447,38.2938462174384,-37.6666367941389));
#248625=CARTESIAN_POINT('Ctrl Pts',(25.7326779997654,38.3214522967729,-37.6553229150289));
#248626=CARTESIAN_POINT('Ctrl Pts',(25.5793619804298,38.3570758581462,-37.6461683926629));
#248627=CARTESIAN_POINT('Ctrl Pts',(25.4280646493686,38.4007283517996,-37.6391871086171));
#248628=CARTESIAN_POINT('Ctrl Pts',(25.2772986540836,38.4442275437957,-37.6322303418973));
#248629=CARTESIAN_POINT('Ctrl Pts',(25.1285370763278,38.4956993999497,-37.6274315578455));
#248630=CARTESIAN_POINT('Ctrl Pts',(24.9817940407082,38.5552037278875,-37.624817614644));
#248631=CARTESIAN_POINT('Ctrl Pts',(24.8944876056227,38.590606503375,-37.623262419459));
#248632=CARTESIAN_POINT('Ctrl Pts',(24.8078959327013,38.6288535270284,-37.6224808633793));
#248633=CARTESIAN_POINT('Ctrl Pts',(24.7220243175172,38.669965539032,-37.6224808631404));
#248634=CARTESIAN_POINT('Origin',(26.194621967318,37.9124350177459,-39.1625636424987));
#248635=CARTESIAN_POINT('Origin',(48.2118204350716,29.879557875893,235.35105));
#248636=CARTESIAN_POINT('',(50.4542306878656,31.8724442896568,-41.3499258784557));
#248637=CARTESIAN_POINT('',(50.4542306878656,31.8724442896568,-52.64995));
#248638=CARTESIAN_POINT('',(50.4542306878656,31.8724442896567,235.35105));
#248639=CARTESIAN_POINT('',(51.2045125858511,30.0888272971254,-41.2737227474219));
#248640=CARTESIAN_POINT('Ctrl Pts',(50.4542306878656,31.8724442896568,-41.3499258784557));
#248641=CARTESIAN_POINT('Ctrl Pts',(50.5181129933322,31.8005634560272,-41.3499258784558));
#248642=CARTESIAN_POINT('Ctrl Pts',(50.5788912011241,31.7252093793369,-41.3493408309145));
#248643=CARTESIAN_POINT('Ctrl Pts',(50.6361616709643,31.6466372662856,-41.3481707358316));
#248644=CARTESIAN_POINT('Ctrl Pts',(50.6929598518543,31.5687131091685,-41.3470102901017));
#248645=CARTESIAN_POINT('Ctrl Pts',(50.7463075433695,31.4876238374954,-41.3452744063958));
#248646=CARTESIAN_POINT('Ctrl Pts',(50.7958274996612,31.403666628624,-41.3429630847142));
#248647=CARTESIAN_POINT('Ctrl Pts',(50.8449448069292,31.3203920796478,-41.3406705564946));
#248648=CARTESIAN_POINT('Ctrl Pts',(50.8902960139758,31.2342961473852,-41.3378119100797));
#248649=CARTESIAN_POINT('Ctrl Pts',(50.9315346868522,31.1457152076104,-41.3343871454692));
#248650=CARTESIAN_POINT('Ctrl Pts',(50.9722785909486,31.0581970344193,-41.3310034701201));
#248651=CARTESIAN_POINT('Ctrl Pts',(51.0090077268708,30.9682532960156,-41.3270671793063));
#248652=CARTESIAN_POINT('Ctrl Pts',(51.0414142689238,30.8762517784658,-41.3225782730277));
#248653=CARTESIAN_POINT('Ctrl Pts',(51.0735998270302,30.784877629871,-41.3181199771185));
#248654=CARTESIAN_POINT('Ctrl Pts',(51.1015212128023,30.6914738422423,-41.3131165767449));
#248655=CARTESIAN_POINT('Ctrl Pts',(51.1249078316996,30.5964412831547,-41.3075680719069));
#248656=CARTESIAN_POINT('Ctrl Pts',(51.1480518192897,30.5023946671032,-41.3020771316527));
#248657=CARTESIAN_POINT('Ctrl Pts',(51.1667543600226,30.4067531287956,-41.2960523389518));
#248658=CARTESIAN_POINT('Ctrl Pts',(51.1807881805032,30.3099420375285,-41.2894936938044));
#248659=CARTESIAN_POINT('Ctrl Pts',(51.191385421931,30.2368378882726,-41.2845411189755));
#248660=CARTESIAN_POINT('Ctrl Pts',(51.1993211964125,30.1630676248948,-41.279284136848));
#248661=CARTESIAN_POINT('Ctrl Pts',(51.2045125858511,30.0888272971254,-41.2737227474219));
#248662=CARTESIAN_POINT('',(51.2045125858511,30.0888272971254,-52.64995));
#248663=CARTESIAN_POINT('',(51.2045125858511,30.0888272971253,235.35105));
#248664=CARTESIAN_POINT('Origin',(48.2118204350716,29.879557875893,-52.64995));
#248665=CARTESIAN_POINT('Origin',(42.8470578959213,35.2443204150433,235.35105));
#248666=CARTESIAN_POINT('',(43.0563273171537,38.2370125658228,-41.2737227474219));
#248667=CARTESIAN_POINT('',(43.0563273171537,38.2370125658228,-52.64995));
#248668=CARTESIAN_POINT('',(43.0563273171537,38.2370125658227,235.35105));
#248669=CARTESIAN_POINT('',(44.839944309685,37.4867306678373,-41.3499258784557));
#248670=CARTESIAN_POINT('Ctrl Pts',(43.0563273171537,38.2370125658227,-41.2737227474219));
#248671=CARTESIAN_POINT('Ctrl Pts',(43.154629171652,38.2301386305295,-41.2810866008773));
#248672=CARTESIAN_POINT('Ctrl Pts',(43.2521056977309,38.2184516355055,-41.2879167524659));
#248673=CARTESIAN_POINT('Ctrl Pts',(43.3483058302563,38.2021490964115,-41.2942132021878));
#248674=CARTESIAN_POINT('Ctrl Pts',(43.4452418270719,38.1857218542009,-41.3005578153829));
#248675=CARTESIAN_POINT('Ctrl Pts',(43.5408815832291,38.1646084828715,-41.3063605305851));
#248676=CARTESIAN_POINT('Ctrl Pts',(43.6347991557083,38.1390507492245,-41.3116213477944));
#248677=CARTESIAN_POINT('Ctrl Pts',(43.7294452772313,38.1132947559556,-41.3169229748677));
#248678=CARTESIAN_POINT('Ctrl Pts',(43.8223421816389,38.0830255004283,-41.3216742639821));
#248679=CARTESIAN_POINT('Ctrl Pts',(43.9130933638555,38.0485258962993,-41.3258752151377));
#248680=CARTESIAN_POINT('Ctrl Pts',(44.0049695254192,38.01359862455,-41.3301282425657));
#248681=CARTESIAN_POINT('Ctrl Pts',(44.0946462283388,37.9743357949492,-41.3338172031509));
#248682=CARTESIAN_POINT('Ctrl Pts',(44.1817555311144,37.9310623495449,-41.3369420968931));
#248683=CARTESIAN_POINT('Ctrl Pts',(44.2694569033968,37.8874947807043,-41.3400882300923));
#248684=CARTESIAN_POINT('Ctrl Pts',(44.3545557283222,37.8398622590698,-41.3426626026266));
#248685=CARTESIAN_POINT('Ctrl Pts',(44.4367228234257,37.7885227297703,-41.3446652144958));
#248686=CARTESIAN_POINT('Ctrl Pts',(44.5198078063777,37.7366096870706,-41.3466901975235));
#248687=CARTESIAN_POINT('Ctrl Pts',(44.5998950713162,37.6809067185249,-41.3481305742695));
#248688=CARTESIAN_POINT('Ctrl Pts',(44.6766934223472,37.6218051869062,-41.3489863447338));
#248689=CARTESIAN_POINT('Ctrl Pts',(44.7329036980364,37.5785475734113,-41.3496127005485));
#248690=CARTESIAN_POINT('Ctrl Pts',(44.7873531091644,37.5334697910065,-41.3499258784558));
#248691=CARTESIAN_POINT('Ctrl Pts',(44.8399443096851,37.4867306678373,-41.3499258784558));
#248692=CARTESIAN_POINT('',(44.839944309685,37.4867306678373,-52.64995));
#248693=CARTESIAN_POINT('',(44.839944309685,37.4867306678373,235.35105));
#248694=CARTESIAN_POINT('Origin',(42.8470578959213,35.2443204150433,-52.64995));
#248695=CARTESIAN_POINT('Origin',(44.0630480057168,38.1666157975539,235.35105));
#248696=CARTESIAN_POINT('Ctrl Pts',(26.2992566779342,39.4087810931356,-39.1625636424987));
#248697=CARTESIAN_POINT('Ctrl Pts',(31.903874175502,39.0168680593679,-39.7153157040946));
#248698=CARTESIAN_POINT('Ctrl Pts',(37.4870209577723,38.6264564042711,-40.4393222961257));
#248699=CARTESIAN_POINT('Ctrl Pts',(43.0563273171537,38.2370125658228,-41.2737227474219));
#248700=CARTESIAN_POINT('',(44.0630480057168,38.166615797554,-52.64995));
#248701=CARTESIAN_POINT('Ctrl Pts',(44.839944309685,37.4867306678373,-41.3499258784558));
#248702=CARTESIAN_POINT('Ctrl Pts',(44.8399443096851,37.4867306678373,-40.1779974386957));
#248703=CARTESIAN_POINT('Ctrl Pts',(44.0845625322695,36.6367696109743,-39.8944822890418));
#248704=CARTESIAN_POINT('Ctrl Pts',(44.5912415343056,37.7077590820187,-41.3499258752894));
#248705=CARTESIAN_POINT('Ctrl Pts',(44.6149072014673,37.6867267800084,-40.1779974336417));
#248706=CARTESIAN_POINT('Ctrl Pts',(43.9595274298496,36.7478914351849,-39.8944822858058));
#248707=CARTESIAN_POINT('Ctrl Pts',(44.3136937213669,37.8823162857708,-41.343363404867));
#248708=CARTESIAN_POINT('Ctrl Pts',(44.3663746862182,37.849051706332,-40.1674920635188));
#248709=CARTESIAN_POINT('Ctrl Pts',(43.8200866324971,36.835758129222,-39.887919815423));
#248710=CARTESIAN_POINT('Ctrl Pts',(43.7019124427066,38.1390166965721,-41.3171961008681));
#248711=CARTESIAN_POINT('Ctrl Pts',(43.8196015906779,38.1008702319186,-40.1253788430241));
#248712=CARTESIAN_POINT('Ctrl Pts',(43.5128927223798,36.9652495181622,-39.8617525114841));
#248713=CARTESIAN_POINT('Ctrl Pts',(43.3844623592655,38.214067128441,-41.2983035466937));
#248714=CARTESIAN_POINT('Ctrl Pts',(43.5344232858197,38.1836802846001,-40.0946545134465));
#248715=CARTESIAN_POINT('Ctrl Pts',(43.3535628849498,37.0032968338361,-39.8428593266731));
#248716=CARTESIAN_POINT('Ctrl Pts',(43.0563273171537,38.2370125658228,-41.2737227474219));
#248717=CARTESIAN_POINT('Ctrl Pts',(43.23812030497,38.224300361751,-40.0543903140502));
#248718=CARTESIAN_POINT('Ctrl Pts',(43.1889493654704,37.0152446912691,-39.8182791580079));
#248719=CARTESIAN_POINT('',(43.1889493654704,37.0152446912691,-39.8182791580079));
#248720=CARTESIAN_POINT('Origin',(42.9516926065375,36.740666490433,-41.2737227474219));
#248721=CARTESIAN_POINT('',(44.0845625322695,36.6367696109743,-39.8944822890418));
#248722=CARTESIAN_POINT('Ctrl Pts',(44.0845625322695,36.6367696109743,-39.8944822890418));
#248723=CARTESIAN_POINT('Ctrl Pts',(43.9941797939515,36.7170950246707,-39.8944822890418));
#248724=CARTESIAN_POINT('Ctrl Pts',(43.8962901478094,36.7852564677658,-39.8910542505833));
#248725=CARTESIAN_POINT('Ctrl Pts',(43.7909432593811,36.8413335920204,-39.8842118316081));
#248726=CARTESIAN_POINT('Ctrl Pts',(43.7506303648273,36.862792519101,-39.8815934560798));
#248727=CARTESIAN_POINT('Ctrl Pts',(43.7092251907653,36.8824814307082,-39.8784749689682));
#248728=CARTESIAN_POINT('Ctrl Pts',(43.6667294913925,36.9004031219782,-39.8748566639276));
#248729=CARTESIAN_POINT('Ctrl Pts',(43.6666496039709,36.9004368128629,-39.8748498618967));
#248730=CARTESIAN_POINT('Ctrl Pts',(43.666569712705,36.9004704974973,-39.8748430581001));
#248731=CARTESIAN_POINT('Ctrl Pts',(43.6664898175948,36.9005041758817,-39.8748362525378));
#248732=CARTESIAN_POINT('Ctrl Pts',(43.5643771770591,36.9435479709188,-39.8661381741221));
#248733=CARTESIAN_POINT('Ctrl Pts',(43.4597085659155,36.9748052400739,-39.8548713027024));
#248734=CARTESIAN_POINT('Ctrl Pts',(43.3525514979871,36.9944348238144,-39.8410580051271));
#248735=CARTESIAN_POINT('Ctrl Pts',(43.2986448352407,37.0043097240054,-39.8341090582382));
#248736=CARTESIAN_POINT('Ctrl Pts',(43.2441082468328,37.0112411932519,-39.8265155089204));
#248737=CARTESIAN_POINT('Ctrl Pts',(43.1889493654704,37.0152446912691,-39.8182791580079));
#248738=CARTESIAN_POINT('Origin',(43.8435011028032,36.3655255414403,-41.3499258784558));
#248739=CARTESIAN_POINT('Origin',(0.,-12.9675000200282,235.35105));
#248740=CARTESIAN_POINT('Origin',(0.,-12.9675000200281,-41.3499258784557));
#248741=CARTESIAN_POINT('Origin',(0.,-12.9675000200281,-52.64995));
#248742=CARTESIAN_POINT('Ctrl Pts',(51.204512585851,30.0888272971254,-41.2737227474219));
#248743=CARTESIAN_POINT('Ctrl Pts',(51.1918003817794,30.2706202849417,-40.0543903140502));
#248744=CARTESIAN_POINT('Ctrl Pts',(49.9827447112974,30.221449345442,-39.8182791580079));
#248745=CARTESIAN_POINT('Ctrl Pts',(51.1815637992349,30.4170102355187,-41.298307134608));
#248746=CARTESIAN_POINT('Ctrl Pts',(51.1511744833359,30.5669657276558,-40.0946602834914));
#248747=CARTESIAN_POINT('Ctrl Pts',(49.970795119399,30.3860867600489,-39.8428628946809));
#248748=CARTESIAN_POINT('Ctrl Pts',(51.1065500370229,30.7342489164072,-41.3171858838447));
#248749=CARTESIAN_POINT('Ctrl Pts',(51.0684082345096,30.8519555741622,-40.125362313696));
#248750=CARTESIAN_POINT('Ctrl Pts',(49.9327664722994,30.5453106517579,-39.8617422945218));
#248751=CARTESIAN_POINT('Ctrl Pts',(50.8500106529935,31.3458145441506,-41.3433504080566));
#248752=CARTESIAN_POINT('Ctrl Pts',(50.8167365053657,31.3985364985707,-40.1674712617341));
#248753=CARTESIAN_POINT('Ctrl Pts',(49.8033560611762,30.8523961753476,-39.8879068185516));
#248754=CARTESIAN_POINT('Ctrl Pts',(50.6751042513768,31.6239157533749,-41.3499258753262));
#248755=CARTESIAN_POINT('Ctrl Pts',(50.6540845266547,31.6475672688382,-40.1779974337035));
#248756=CARTESIAN_POINT('Ctrl Pts',(49.715313604986,30.9921150076825,-39.8944822858423));
#248757=CARTESIAN_POINT('Ctrl Pts',(50.4542306878656,31.8724442896568,-41.3499258784558));
#248758=CARTESIAN_POINT('Ctrl Pts',(50.4542306878656,31.8724442896567,-40.1779974386957));
#248759=CARTESIAN_POINT('Ctrl Pts',(49.6042696310026,31.1170625122411,-39.8944822890418));
#248760=CARTESIAN_POINT('',(49.6042696310026,31.1170625122412,-39.8944822890418));
#248761=CARTESIAN_POINT('Origin',(49.3330255614686,30.8760010827748,-41.3499258784557));
#248762=CARTESIAN_POINT('',(49.9827447112974,30.221449345442,-39.8182791580079));
#248763=CARTESIAN_POINT('Ctrl Pts',(49.9827447112974,30.221449345442,-39.8182791580079));
#248764=CARTESIAN_POINT('Ctrl Pts',(49.9742478426489,30.3385164122227,-39.8357596691874));
#248765=CARTESIAN_POINT('Ctrl Pts',(49.9525777122479,30.4527365881464,-39.850340487351));
#248766=CARTESIAN_POINT('Ctrl Pts',(49.917564983954,30.5640807882657,-39.8620074889831));
#248767=CARTESIAN_POINT('Ctrl Pts',(49.9032876571132,30.6094842062339,-39.8667650044259));
#248768=CARTESIAN_POINT('Ctrl Pts',(49.8867911421677,30.6544092836466,-39.8710378812991));
#248769=CARTESIAN_POINT('Ctrl Pts',(49.8680615705257,30.6988535344112,-39.8748246333721));
#248770=CARTESIAN_POINT('Ctrl Pts',(49.8680277409604,30.6989338101224,-39.8748314730468));
#248771=CARTESIAN_POINT('Ctrl Pts',(49.8679939050223,30.699014082039,-39.8748383109414));
#248772=CARTESIAN_POINT('Ctrl Pts',(49.8679600627116,30.6990943501611,-39.8748451470561));
#248773=CARTESIAN_POINT('Ctrl Pts',(49.834210673313,30.7791420788835,-39.8816624916982));
#248774=CARTESIAN_POINT('Ctrl Pts',(49.7941455915938,30.8553753559226,-39.8867070324262));
#248775=CARTESIAN_POINT('Ctrl Pts',(49.7477894766075,30.9277322498077,-39.8899765761449));
#248776=CARTESIAN_POINT('Ctrl Pts',(49.7052516615016,30.9941291895563,-39.8929768113077));
#248777=CARTESIAN_POINT('Ctrl Pts',(49.6574159846453,31.0572618495019,-39.8944822890418));
#248778=CARTESIAN_POINT('Ctrl Pts',(49.6042696310026,31.1170625122411,-39.8944822890418));
#248779=CARTESIAN_POINT('Origin',(49.7081665104613,29.9841925865092,-41.2737227474219));
#248780=CARTESIAN_POINT('Origin',(51.1341158175823,31.0955479856884,235.35105));
#248781=CARTESIAN_POINT('Ctrl Pts',(51.2045125858511,30.0888272971254,-41.2737227474219));
#248782=CARTESIAN_POINT('Ctrl Pts',(51.5939564242993,24.519520937744,-40.4393222961257));
#248783=CARTESIAN_POINT('Ctrl Pts',(51.9843680793961,18.9363741554737,-39.7153157040947));
#248784=CARTESIAN_POINT('Ctrl Pts',(52.3762811131638,13.3317566579059,-39.1625636424987));
#248785=CARTESIAN_POINT('',(51.1341158175823,31.0955479856884,-52.64995));
#248786=CARTESIAN_POINT('Ctrl Pts',(51.202570601752,13.3932250805846,-37.7071200530847));
#248787=CARTESIAN_POINT('Ctrl Pts',(52.3681090731164,13.4486222752606,-37.971813107807));
#248788=CARTESIAN_POINT('Ctrl Pts',(52.3762811131638,13.3317566579059,-39.1625636424987));
#248789=CARTESIAN_POINT('Ctrl Pts',(51.243814149994,12.8221846817494,-37.6510924855238));
#248790=CARTESIAN_POINT('Ctrl Pts',(52.3823956057955,13.0329073967221,-37.9286345805849));
#248791=CARTESIAN_POINT('Ctrl Pts',(52.4027610669746,12.9530756759645,-39.1065428641427));
#248792=CARTESIAN_POINT('Ctrl Pts',(51.3887400699185,12.2740430086498,-37.6224808645841));
#248793=CARTESIAN_POINT('Ctrl Pts',(52.4810099507979,12.6258889587099,-37.9059960140017));
#248794=CARTESIAN_POINT('Ctrl Pts',(52.4983460113501,12.5896787161743,-39.0779244541051));
#248795=CARTESIAN_POINT('Ctrl Pts',(51.6374655590603,11.7545242974889,-37.6224808631404));
#248796=CARTESIAN_POINT('Ctrl Pts',(52.6630979669895,12.2455574854105,-37.9059960127943));
#248797=CARTESIAN_POINT('Ctrl Pts',(52.6630979669895,12.2455574854105,-39.0779244525544));
#248798=CARTESIAN_POINT('',(51.202570601752,13.3932250805846,-37.7071200530847));
#248799=CARTESIAN_POINT('Origin',(50.8799350377741,13.2271219472897,-39.1625636424987));
#248800=CARTESIAN_POINT('',(51.6374655590603,11.7545242974889,-37.6224808631404));
#248801=CARTESIAN_POINT('Ctrl Pts',(51.6374655590603,11.7545242974889,-37.6224808631404));
#248802=CARTESIAN_POINT('Ctrl Pts',(51.5683401737289,11.8989080967521,-37.6224808635416));
#248803=CARTESIAN_POINT('Ctrl Pts',(51.5073117137531,12.0453267862124,-37.6246896514879));
#248804=CARTESIAN_POINT('Ctrl Pts',(51.4542914421325,12.1937580895562,-37.629072347155));
#248805=CARTESIAN_POINT('Ctrl Pts',(51.401143473863,12.3425468822047,-37.6334655983234));
#248806=CARTESIAN_POINT('Ctrl Pts',(51.3560423053796,12.4933581163808,-37.6400432640145));
#248807=CARTESIAN_POINT('Ctrl Pts',(51.3189474852192,12.6461827680851,-37.6487836824747));
#248808=CARTESIAN_POINT('Ctrl Pts',(51.2817682244751,12.7993553013199,-37.6575439971369));
#248809=CARTESIAN_POINT('Ctrl Pts',(51.2526317828013,12.9545505495523,-37.668476942121));
#248810=CARTESIAN_POINT('Ctrl Pts',(51.2315467536769,13.1117710662234,-37.6815739017301));
#248811=CARTESIAN_POINT('Ctrl Pts',(51.2190600923228,13.2048778548357,-37.6893299877397));
#248812=CARTESIAN_POINT('Ctrl Pts',(51.2093980530995,13.2986951308912,-37.6978452571967));
#248813=CARTESIAN_POINT('Ctrl Pts',(51.202570601752,13.3932250805846,-37.7071200530847));
#248814=CARTESIAN_POINT('Origin',(51.3101603185126,11.5978231885467,-39.0779244525544));
#248815=CARTESIAN_POINT('Origin',(0.,-12.9675000200281,-55.24995));
#248816=CARTESIAN_POINT('Origin',(0.,-12.9675000200281,-52.64995));
#248817=CARTESIAN_POINT('Origin',(0.,-12.9675000200281,-39.0779244525544));
#248818=CARTESIAN_POINT('Ctrl Pts',(51.6374655590602,-37.6895243375453,
-37.6224808631404));
#248819=CARTESIAN_POINT('Ctrl Pts',(52.6630979669894,-38.180557525467,-37.9059960127944));
#248820=CARTESIAN_POINT('Ctrl Pts',(52.6630979669894,-38.1805575254669,
-39.0779244525544));
#248821=CARTESIAN_POINT('Ctrl Pts',(51.3887400699171,-38.2090430487116,
-37.6224808645844));
#248822=CARTESIAN_POINT('Ctrl Pts',(52.4810099507953,-38.5608889987718,
-37.9059960140155));
#248823=CARTESIAN_POINT('Ctrl Pts',(52.4983460113489,-38.5246787562331,
-39.077924454111));
#248824=CARTESIAN_POINT('Ctrl Pts',(51.2438141500031,-38.7571847218022,
-37.6510924855255));
#248825=CARTESIAN_POINT('Ctrl Pts',(52.3823956058033,-38.9679074367732,
-37.9286345805868));
#248826=CARTESIAN_POINT('Ctrl Pts',(52.4027610669748,-38.8880757160172,
-39.1065428641511));
#248827=CARTESIAN_POINT('Ctrl Pts',(51.2025706017519,-39.328225120641,-37.7071200530847));
#248828=CARTESIAN_POINT('Ctrl Pts',(52.3681090731163,-39.383622315317,-37.971813107807));
#248829=CARTESIAN_POINT('Ctrl Pts',(52.3762811131638,-39.2667566979623,
-39.1625636424987));
#248830=CARTESIAN_POINT('',(51.6374655590602,-37.6895243375453,-37.6224808631404));
#248831=CARTESIAN_POINT('Origin',(51.3101603185125,-37.532823228603,-39.0779244525544));
#248832=CARTESIAN_POINT('',(51.2025706017519,-39.328225120641,-37.7071200530847));
#248833=CARTESIAN_POINT('Ctrl Pts',(51.2025706017519,-39.328225120641,-37.7071200530847));
#248834=CARTESIAN_POINT('Ctrl Pts',(51.2140977238333,-39.1686255548923,
-37.6914609587884));
#248835=CARTESIAN_POINT('Ctrl Pts',(51.2337022263897,-39.0110569630202,
-37.6779662189121));
#248836=CARTESIAN_POINT('Ctrl Pts',(51.2613462375948,-38.8555107743848,
-37.6666367940901));
#248837=CARTESIAN_POINT('Ctrl Pts',(51.2889523169909,-38.7001780188965,
-37.6553229149708));
#248838=CARTESIAN_POINT('Ctrl Pts',(51.3245758784465,-38.5468619993575,
-37.646168392601));
#248839=CARTESIAN_POINT('Ctrl Pts',(51.3682283722045,-38.3955646680986,
-37.6391871085577));
#248840=CARTESIAN_POINT('Ctrl Pts',(51.4117275642993,-38.2447986726358,
-37.6322303418412));
#248841=CARTESIAN_POINT('Ctrl Pts',(51.4631994205721,-38.0960370947074,
-37.6274315577981));
#248842=CARTESIAN_POINT('Ctrl Pts',(51.5227037486505,-37.9492940589207,
-37.6248176146113));
#248843=CARTESIAN_POINT('Ctrl Pts',(51.558106523932,-37.8619876244502,-37.6232624194478));
#248844=CARTESIAN_POINT('Ctrl Pts',(51.5963535473405,-37.7753959521341,
-37.6224808633791));
#248845=CARTESIAN_POINT('Ctrl Pts',(51.6374655590602,-37.6895243375453,
-37.6224808631404));
#248846=CARTESIAN_POINT('Origin',(50.879935037774,-39.1621219873461,-39.1625636424987));
#248847=CARTESIAN_POINT('Origin',(42.8470578959211,-61.1793204550998,235.35105));
#248848=CARTESIAN_POINT('',(44.8399443096849,-63.4217307078938,-41.3499258784557));
#248849=CARTESIAN_POINT('',(44.8399443096849,-63.4217307078937,-52.64995));
#248850=CARTESIAN_POINT('',(44.8399443096849,-63.4217307078938,235.35105));
#248851=CARTESIAN_POINT('',(43.0563273171535,-64.1720126058792,-41.273722747422));
#248852=CARTESIAN_POINT('Ctrl Pts',(44.8399443096849,-63.4217307078938,
-41.3499258784558));
#248853=CARTESIAN_POINT('Ctrl Pts',(44.7680634760552,-63.4856130133605,
-41.3499258784558));
#248854=CARTESIAN_POINT('Ctrl Pts',(44.6927093993648,-63.5463912211525,
-41.3493408309145));
#248855=CARTESIAN_POINT('Ctrl Pts',(44.6141372863133,-63.6036616909928,
-41.3481707358316));
#248856=CARTESIAN_POINT('Ctrl Pts',(44.5362131291965,-63.6604598718826,
-41.3470102901017));
#248857=CARTESIAN_POINT('Ctrl Pts',(44.4551238575238,-63.7138075633975,
-41.3452744063959));
#248858=CARTESIAN_POINT('Ctrl Pts',(44.3711666486527,-63.763327519689,-41.3429630847143));
#248859=CARTESIAN_POINT('Ctrl Pts',(44.287892099677,-63.8124448269568,-41.3406705564948));
#248860=CARTESIAN_POINT('Ctrl Pts',(44.2017961674148,-63.8577960340032,
-41.3378119100798));
#248861=CARTESIAN_POINT('Ctrl Pts',(44.1132152276405,-63.8990347068794,
-41.3343871454693));
#248862=CARTESIAN_POINT('Ctrl Pts',(44.0256970544502,-63.9397786109757,
-41.3310034701203));
#248863=CARTESIAN_POINT('Ctrl Pts',(43.9357533160473,-63.9765077468977,
-41.3270671793065));
#248864=CARTESIAN_POINT('Ctrl Pts',(43.8437517984982,-64.0089142889505,
-41.3225782730279));
#248865=CARTESIAN_POINT('Ctrl Pts',(43.752377649904,-64.0410998470569,-41.3181199771188));
#248866=CARTESIAN_POINT('Ctrl Pts',(43.6589738622758,-64.0690212328289,
-41.3131165767453));
#248867=CARTESIAN_POINT('Ctrl Pts',(43.5639413031887,-64.0924078517263,
-41.3075680719073));
#248868=CARTESIAN_POINT('Ctrl Pts',(43.4698946871375,-64.1155518393166,
-41.3020771316531));
#248869=CARTESIAN_POINT('Ctrl Pts',(43.3742531488302,-64.1342543800497,
-41.2960523389522));
#248870=CARTESIAN_POINT('Ctrl Pts',(43.2774420575633,-64.1482882005304,
-41.2894936938049));
#248871=CARTESIAN_POINT('Ctrl Pts',(43.2043379083053,-64.1588854419587,
-41.2845411189758));
#248872=CARTESIAN_POINT('Ctrl Pts',(43.1305676449252,-64.1668212164406,
-41.2792841368482));
#248873=CARTESIAN_POINT('Ctrl Pts',(43.0563273171535,-64.1720126058793,
-41.2737227474219));
#248874=CARTESIAN_POINT('',(43.0563273171535,-64.1720126058792,-52.64995));
#248875=CARTESIAN_POINT('',(43.0563273171535,-64.1720126058792,235.35105));
#248876=CARTESIAN_POINT('Origin',(42.8470578959211,-61.1793204550997,-52.64995));
#248877=CARTESIAN_POINT('Origin',(48.2118204350714,-55.8145579159494,235.35105));
#248878=CARTESIAN_POINT('',(51.2045125858509,-56.0238273371818,-41.2737227474219));
#248879=CARTESIAN_POINT('',(51.2045125858509,-56.0238273371818,-52.64995));
#248880=CARTESIAN_POINT('',(51.2045125858509,-56.0238273371818,235.35105));
#248881=CARTESIAN_POINT('',(50.4542306878654,-57.8074443297132,-41.3499258784557));
#248882=CARTESIAN_POINT('Ctrl Pts',(51.2045125858509,-56.0238273371818,
-41.2737227474219));
#248883=CARTESIAN_POINT('Ctrl Pts',(51.1976386505577,-56.1221291916803,
-41.2810866008773));
#248884=CARTESIAN_POINT('Ctrl Pts',(51.1859516555336,-56.2196057177593,
-41.2879167524659));
#248885=CARTESIAN_POINT('Ctrl Pts',(51.1696491164396,-56.3158058502849,
-41.2942132021878));
#248886=CARTESIAN_POINT('Ctrl Pts',(51.1532218742289,-56.4127418471005,
-41.3005578153829));
#248887=CARTESIAN_POINT('Ctrl Pts',(51.1321085028996,-56.5083816032577,
-41.3063605305851));
#248888=CARTESIAN_POINT('Ctrl Pts',(51.1065507692525,-56.602299175737,-41.3116213477945));
#248889=CARTESIAN_POINT('Ctrl Pts',(51.0807947759837,-56.6969452972597,
-41.3169229748677));
#248890=CARTESIAN_POINT('Ctrl Pts',(51.0505255204564,-56.7898422016671,
-41.3216742639821));
#248891=CARTESIAN_POINT('Ctrl Pts',(51.0160259163275,-56.8805933838835,
-41.3258752151377));
#248892=CARTESIAN_POINT('Ctrl Pts',(50.9810986445782,-56.9724695454474,
-41.3301282425657));
#248893=CARTESIAN_POINT('Ctrl Pts',(50.9418358149772,-57.0621462483671,
-41.3338172031508));
#248894=CARTESIAN_POINT('Ctrl Pts',(50.8985623695729,-57.149255551143,-41.336942096893));
#248895=CARTESIAN_POINT('Ctrl Pts',(50.854994800732,-57.2369569234258,-41.3400882300923));
#248896=CARTESIAN_POINT('Ctrl Pts',(50.8073622790973,-57.3220557483516,
-41.3426626026266));
#248897=CARTESIAN_POINT('Ctrl Pts',(50.7560227497974,-57.4042228434554,
-41.3446652144958));
#248898=CARTESIAN_POINT('Ctrl Pts',(50.7041097070974,-57.4873078264078,
-41.3466901975235));
#248899=CARTESIAN_POINT('Ctrl Pts',(50.6484067385514,-57.5673950913467,
-41.3481305742695));
#248900=CARTESIAN_POINT('Ctrl Pts',(50.5893052069323,-57.644193442378,-41.3489863447338));
#248901=CARTESIAN_POINT('Ctrl Pts',(50.546047593438,-57.7004037180663,-41.3496127005485));
#248902=CARTESIAN_POINT('Ctrl Pts',(50.5009698110338,-57.7548531291934,
-41.3499258784558));
#248903=CARTESIAN_POINT('Ctrl Pts',(50.4542306878654,-57.8074443297132,
-41.3499258784558));
#248904=CARTESIAN_POINT('',(50.4542306878654,-57.8074443297132,-52.64995));
#248905=CARTESIAN_POINT('',(50.4542306878654,-57.8074443297133,235.35105));
#248906=CARTESIAN_POINT('Origin',(48.2118204350714,-55.8145579159494,-52.64995));
#248907=CARTESIAN_POINT('Origin',(51.1341158175821,-57.030548025745,235.35105));
#248908=CARTESIAN_POINT('Ctrl Pts',(52.3762811131638,-39.2667566979623,
-39.1625636424987));
#248909=CARTESIAN_POINT('Ctrl Pts',(51.984368079396,-44.8713741955301,-39.7153157040947));
#248910=CARTESIAN_POINT('Ctrl Pts',(51.5939564242992,-50.4545209778004,
-40.4393222961257));
#248911=CARTESIAN_POINT('Ctrl Pts',(51.2045125858509,-56.0238273371818,
-41.2737227474219));
#248912=CARTESIAN_POINT('',(51.1341158175821,-57.0305480257449,-52.64995));
#248913=CARTESIAN_POINT('Ctrl Pts',(50.4542306878654,-57.8074443297132,
-41.3499258784558));
#248914=CARTESIAN_POINT('Ctrl Pts',(50.4542306878655,-57.8074443297132,
-40.1779974386957));
#248915=CARTESIAN_POINT('Ctrl Pts',(49.6042696310024,-57.0520625522976,
-39.8944822890418));
#248916=CARTESIAN_POINT('Ctrl Pts',(50.6752591020463,-57.5587415543343,
-41.3499258752894));
#248917=CARTESIAN_POINT('Ctrl Pts',(50.6542268000352,-57.5824072214955,
-40.177997433644));
#248918=CARTESIAN_POINT('Ctrl Pts',(49.7153914552119,-56.9270274498771,
-39.8944822858055));
#248919=CARTESIAN_POINT('Ctrl Pts',(50.8498163057994,-57.2811937413941,
-41.3433634048676));
#248920=CARTESIAN_POINT('Ctrl Pts',(50.8165517263607,-57.3338747062451,
-40.1674920635201));
#248921=CARTESIAN_POINT('Ctrl Pts',(49.8032581492502,-56.7875866525247,
-39.887919815423));
#248922=CARTESIAN_POINT('Ctrl Pts',(51.1065167165998,-56.6694124627357,
-41.3171961008675));
#248923=CARTESIAN_POINT('Ctrl Pts',(51.0683702519462,-56.7871016107072,
-40.125378843023));
#248924=CARTESIAN_POINT('Ctrl Pts',(49.9327495381902,-56.4803927424085,
-39.8617525114842));
#248925=CARTESIAN_POINT('Ctrl Pts',(51.1815671484691,-56.351962379293,-41.2983035466914));
#248926=CARTESIAN_POINT('Ctrl Pts',(51.1511803046297,-56.5019233058474,
-40.094654513445));
#248927=CARTESIAN_POINT('Ctrl Pts',(49.9707968538638,-56.3210629049775,
-39.8428593266729));
#248928=CARTESIAN_POINT('Ctrl Pts',(51.2045125858509,-56.0238273371818,
-41.2737227474219));
#248929=CARTESIAN_POINT('Ctrl Pts',(51.1918003817792,-56.2056203249981,
-40.0543903140502));
#248930=CARTESIAN_POINT('Ctrl Pts',(49.9827447112972,-56.1564493854985,
-39.8182791580079));
#248931=CARTESIAN_POINT('',(49.9827447112972,-56.1564493854985,-39.8182791580079));
#248932=CARTESIAN_POINT('Origin',(49.7081665104611,-55.9191926265656,-41.2737227474219));
#248933=CARTESIAN_POINT('',(49.6042696310024,-57.0520625522976,-39.8944822890418));
#248934=CARTESIAN_POINT('Ctrl Pts',(49.6042696310024,-57.0520625522976,
-39.8944822890418));
#248935=CARTESIAN_POINT('Ctrl Pts',(49.6845950444281,-56.9616798142842,
-39.8944822890418));
#248936=CARTESIAN_POINT('Ctrl Pts',(49.7527564873346,-56.8637901684971,
-39.8910542506064));
#248937=CARTESIAN_POINT('Ctrl Pts',(49.8088336114817,-56.7584432804741,
-39.8842118316772));
#248938=CARTESIAN_POINT('Ctrl Pts',(49.8302925387824,-56.7181303855846,
-39.8815934561347));
#248939=CARTESIAN_POINT('Ctrl Pts',(49.8499814505784,-56.6767252111676,
-39.878474969));
#248940=CARTESIAN_POINT('Ctrl Pts',(49.8679031420063,-56.6342295114207,
-39.8748566639276));
#248941=CARTESIAN_POINT('Ctrl Pts',(49.867936832891,-56.6341496239991,-39.8748498618967));
#248942=CARTESIAN_POINT('Ctrl Pts',(49.8679705175255,-56.6340697327332,
-39.8748430581001));
#248943=CARTESIAN_POINT('Ctrl Pts',(49.8680041959098,-56.6339898376229,
-39.8748362525379));
#248944=CARTESIAN_POINT('Ctrl Pts',(49.9110479907903,-56.5318771974589,
-39.8661381741537));
#248945=CARTESIAN_POINT('Ctrl Pts',(49.9423052598744,-56.4272085867056,
-39.8548713027844));
#248946=CARTESIAN_POINT('Ctrl Pts',(49.9619348436282,-56.3200515191852,
-39.8410580052779));
#248947=CARTESIAN_POINT('Ctrl Pts',(49.9718097439332,-56.266144856058,-39.8341090583481));
#248948=CARTESIAN_POINT('Ctrl Pts',(49.9787412132511,-56.21160826726,-39.82651550898));
#248949=CARTESIAN_POINT('Ctrl Pts',(49.9827447112972,-56.1564493854985,
-39.8182791580079));
#248950=CARTESIAN_POINT('Origin',(49.3330255614684,-56.8110011228313,-41.3499258784558));
#248951=CARTESIAN_POINT('Origin',(0.,-12.9675000200282,235.35105));
#248952=CARTESIAN_POINT('Origin',(0.,-12.9675000200281,-41.3499258784557));
#248953=CARTESIAN_POINT('Origin',(0.,-12.9675000200281,-52.64995));
#248954=CARTESIAN_POINT('Ctrl Pts',(43.0563273171535,-64.1720126058792,
-41.2737227474219));
#248955=CARTESIAN_POINT('Ctrl Pts',(43.2381203049698,-64.1593004018075,
-40.0543903140503));
#248956=CARTESIAN_POINT('Ctrl Pts',(43.1889493654702,-62.9502447313255,
-39.8182791580079));
#248957=CARTESIAN_POINT('Ctrl Pts',(43.3845102555472,-64.1490638192631,
-41.2983071346081));
#248958=CARTESIAN_POINT('Ctrl Pts',(43.5344657476846,-64.1186745033647,
-40.0946602834885));
#248959=CARTESIAN_POINT('Ctrl Pts',(43.3535867800773,-62.9382951394238,
-39.8428628946803));
#248960=CARTESIAN_POINT('Ctrl Pts',(43.7017489364349,-64.0740500570513,
-41.3171858838442));
#248961=CARTESIAN_POINT('Ctrl Pts',(43.8194555941901,-64.0359082545366,
-40.1253623136954));
#248962=CARTESIAN_POINT('Ctrl Pts',(43.5128106717856,-62.900266492328,-39.8617422945218));
#248963=CARTESIAN_POINT('Ctrl Pts',(44.3133145641792,-63.8175106730215,
-41.3433504080572));
#248964=CARTESIAN_POINT('Ctrl Pts',(44.3660365185992,-63.784236525395,-40.1674712617347));
#248965=CARTESIAN_POINT('Ctrl Pts',(43.8198961953762,-62.7708560812039,
-39.8879068185516));
#248966=CARTESIAN_POINT('Ctrl Pts',(44.5914157734028,-63.6426042714052,
-41.3499258753244));
#248967=CARTESIAN_POINT('Ctrl Pts',(44.6150672888642,-63.6215845466798,
-40.1779974336972));
#248968=CARTESIAN_POINT('Ctrl Pts',(43.9596150277081,-62.6828136250119,
-39.8944822858415));
#248969=CARTESIAN_POINT('Ctrl Pts',(44.8399443096849,-63.4217307078937,
-41.3499258784558));
#248970=CARTESIAN_POINT('Ctrl Pts',(44.8399443096849,-63.4217307078938,
-40.1779974386957));
#248971=CARTESIAN_POINT('Ctrl Pts',(44.0845625322693,-62.5717696510307,
-39.8944822890418));
#248972=CARTESIAN_POINT('',(44.0845625322693,-62.5717696510307,-39.8944822890418));
#248973=CARTESIAN_POINT('Origin',(43.843501102803,-62.3005255814968,-41.3499258784557));
#248974=CARTESIAN_POINT('',(43.1889493654702,-62.9502447313255,-39.8182791580079));
#248975=CARTESIAN_POINT('Ctrl Pts',(43.1889493654702,-62.9502447313255,
-39.8182791580079));
#248976=CARTESIAN_POINT('Ctrl Pts',(43.3060164327881,-62.941747862638,-39.8357596692677));
#248977=CARTESIAN_POINT('Ctrl Pts',(43.4202366092234,-62.9200777320771,
-39.8503404874849));
#248978=CARTESIAN_POINT('Ctrl Pts',(43.5315808098271,-62.8850650035,-39.8620074891438));
#248979=CARTESIAN_POINT('Ctrl Pts',(43.5769842272734,-62.8707876767699,
-39.8667650045221));
#248980=CARTESIAN_POINT('Ctrl Pts',(43.6219093041749,-62.854291161985,-39.8710378813417));
#248981=CARTESIAN_POINT('Ctrl Pts',(43.6663535544392,-62.8355615905537,
-39.8748246333721));
#248982=CARTESIAN_POINT('Ctrl Pts',(43.6664338301504,-62.8355277609884,
-39.8748314730468));
#248983=CARTESIAN_POINT('Ctrl Pts',(43.6665141020671,-62.8354939250504,
-39.8748383109414));
#248984=CARTESIAN_POINT('Ctrl Pts',(43.6665943701892,-62.8354600827397,
-39.8748451470561));
#248985=CARTESIAN_POINT('Ctrl Pts',(43.7466420990542,-62.8017106932808,
-39.8816624917103));
#248986=CARTESIAN_POINT('Ctrl Pts',(43.8228753762223,-62.7616456114792,
-39.8867070324441));
#248987=CARTESIAN_POINT('Ctrl Pts',(43.8952322702226,-62.7152894963879,
-39.8899765761624));
#248988=CARTESIAN_POINT('Ctrl Pts',(43.9616292098295,-62.672751681344,-39.8929768113136));
#248989=CARTESIAN_POINT('Ctrl Pts',(44.0247618696462,-62.6249160045702,
-39.8944822890418));
#248990=CARTESIAN_POINT('Ctrl Pts',(44.0845625322693,-62.5717696510307,
-39.8944822890418));
#248991=CARTESIAN_POINT('Origin',(42.9516926065373,-62.6756665304895,-41.2737227474219));
#248992=CARTESIAN_POINT('Origin',(44.0630480057166,-64.1016158376104,235.35105));
#248993=CARTESIAN_POINT('Ctrl Pts',(43.0563273171535,-64.1720126058792,
-41.273722747422));
#248994=CARTESIAN_POINT('Ctrl Pts',(37.4870209577721,-64.5614564443275,
-40.4393222961258));
#248995=CARTESIAN_POINT('Ctrl Pts',(31.9038741755017,-64.9518680994243,
-39.7153157040947));
#248996=CARTESIAN_POINT('Ctrl Pts',(26.299256677934,-65.343781133192,-39.1625636424987));
#248997=CARTESIAN_POINT('',(44.0630480057166,-64.1016158376104,-52.64995));
#248998=CARTESIAN_POINT('Ctrl Pts',(26.3607251006126,-64.1700706217802,
-37.7071200530847));
#248999=CARTESIAN_POINT('Ctrl Pts',(26.4161222952887,-65.3356090931445,
-37.971813107807));
#249000=CARTESIAN_POINT('Ctrl Pts',(26.299256677934,-65.343781133192,-39.1625636424987));
#249001=CARTESIAN_POINT('Ctrl Pts',(25.7896847017718,-64.2113141700146,
-37.6510924855215));
#249002=CARTESIAN_POINT('Ctrl Pts',(26.0004074167582,-65.3498956258269,
-37.9286345805828));
#249003=CARTESIAN_POINT('Ctrl Pts',(25.9205756959923,-65.3702610870028,
-39.1065428641436));
#249004=CARTESIAN_POINT('Ctrl Pts',(25.2415430286856,-64.3562400899596,
-37.6224808645879));
#249005=CARTESIAN_POINT('Ctrl Pts',(25.5933889787265,-65.4485099708125,
-37.9059960140076));
#249006=CARTESIAN_POINT('Ctrl Pts',(25.5571787362025,-65.4658460313782,
-39.0779244541051));
#249007=CARTESIAN_POINT('Ctrl Pts',(24.722024317517,-64.6049655790884,-37.6224808631404));
#249008=CARTESIAN_POINT('Ctrl Pts',(25.2130575054386,-65.6305979870177,
-37.9059960127943));
#249009=CARTESIAN_POINT('Ctrl Pts',(25.2130575054386,-65.6305979870176,
-39.0779244525544));
#249010=CARTESIAN_POINT('',(26.3607251006126,-64.1700706217802,-37.7071200530847));
#249011=CARTESIAN_POINT('Origin',(26.1946219673178,-63.8474350578023,-39.1625636424987));
#249012=CARTESIAN_POINT('',(24.722024317517,-64.6049655790884,-37.6224808631404));
#249013=CARTESIAN_POINT('Ctrl Pts',(24.722024317517,-64.6049655790884,-37.6224808631404));
#249014=CARTESIAN_POINT('Ctrl Pts',(24.8664081169227,-64.5358401936933,
-37.6224808635427));
#249015=CARTESIAN_POINT('Ctrl Pts',(25.0128268065285,-64.4748117336668,
-37.6246896514935));
#249016=CARTESIAN_POINT('Ctrl Pts',(25.1612581100212,-64.4217914620098,
-37.629072347169));
#249017=CARTESIAN_POINT('Ctrl Pts',(25.3100469028066,-64.3686434937081,
-37.6334655983456));
#249018=CARTESIAN_POINT('Ctrl Pts',(25.4608581371227,-64.3235423252056,
-37.6400432640483));
#249019=CARTESIAN_POINT('Ctrl Pts',(25.6136827889703,-64.2864475050405,
-37.648783682524));
#249020=CARTESIAN_POINT('Ctrl Pts',(25.7668553223293,-64.2492682442964,
-37.6575439972006));
#249021=CARTESIAN_POINT('Ctrl Pts',(25.9220505706891,-64.2201318026351,
-37.6684769422025));
#249022=CARTESIAN_POINT('Ctrl Pts',(26.0792710874908,-64.1990467735369,
-37.6815739018329));
#249023=CARTESIAN_POINT('Ctrl Pts',(26.1723778756961,-64.1865601122634,
-37.6893299878148));
#249024=CARTESIAN_POINT('Ctrl Pts',(26.2661951513385,-64.1768980730961,
-37.6978452572376));
#249025=CARTESIAN_POINT('Ctrl Pts',(26.3607251006126,-64.1700706217802,
-37.7071200530847));
#249026=CARTESIAN_POINT('Origin',(24.5653232085747,-64.2776603385407,-39.0779244525544));
#249027=CARTESIAN_POINT('Origin',(0.,-12.9675000200281,-55.24995));
#249028=CARTESIAN_POINT('Origin',(0.,-12.9675000200281,-39.0779244525544));
#249029=CARTESIAN_POINT('Origin',(0.,-12.9675000200281,-52.64995));
#249030=CARTESIAN_POINT('Origin',(0.,-12.9675000200281,-39.0779244525544));
#249031=CARTESIAN_POINT('Origin',(0.,-12.9675000200281,-37.6224808631404));
#249032=CARTESIAN_POINT('Origin',(0.,-12.9675000200281,-36.0027343734933));
#249033=CARTESIAN_POINT('Origin',(0.,-12.9675000200281,-36.9730300997693));
#249034=CARTESIAN_POINT('Origin',(0.,-12.9675000200281,-36.0027343734933));
#249035=CARTESIAN_POINT('Origin',(0.,-12.9675000200281,-28.64995));
#249036=CARTESIAN_POINT('Origin',(0.,-12.9675000200281,-28.64995));
#249037=CARTESIAN_POINT('Origin',(0.,-12.9675000200281,-39.0779244525544));
#249038=CARTESIAN_POINT('Origin',(0.,-12.9675000200281,-37.6224808631404));
#249039=CARTESIAN_POINT('Origin',(0.,-12.9675000200281,-39.0779244525544));
#249040=CARTESIAN_POINT('Origin',(0.,-12.9675000200281,-37.6224808631404));
#249041=CARTESIAN_POINT('Ctrl Pts',(43.1889493654702,-62.9502447313255,
-39.8182791580079));
#249042=CARTESIAN_POINT('Ctrl Pts',(43.2381203049698,-64.1593004018075,
-40.0543903140503));
#249043=CARTESIAN_POINT('Ctrl Pts',(43.0563273171535,-64.1720126058792,
-41.2737227474219));
#249044=CARTESIAN_POINT('Ctrl Pts',(37.601037205815,-63.3558221234085,-38.9838894046597));
#249045=CARTESIAN_POINT('Ctrl Pts',(37.6737894092837,-64.5483963219802,
-39.2334583931343));
#249046=CARTESIAN_POINT('Ctrl Pts',(37.4870588216962,-64.561453796624,-40.4393279688782));
#249047=CARTESIAN_POINT('Ctrl Pts',(31.9944550772227,-63.7631729893641,
-38.2598728770263));
#249048=CARTESIAN_POINT('Ctrl Pts',(32.0660652327991,-64.9405265958656,
-38.5181051330294));
#249049=CARTESIAN_POINT('Ctrl Pts',(31.9038355290703,-64.951870801846,-39.7153118927587));
#249050=CARTESIAN_POINT('Ctrl Pts',(26.3607251006126,-64.1700706217802,
-37.7071200530847));
#249051=CARTESIAN_POINT('Ctrl Pts',(26.4161222952887,-65.3356090931446,
-37.971813107807));
#249052=CARTESIAN_POINT('Ctrl Pts',(26.299256677934,-65.343781133192,-39.1625636424987));
#249053=CARTESIAN_POINT('Ctrl Pts',(26.3607251006126,-64.1700706217802,
-37.7071200530847));
#249054=CARTESIAN_POINT('Ctrl Pts',(27.4631807689973,-64.0904454705621,
-37.8152873750011));
#249055=CARTESIAN_POINT('Ctrl Pts',(28.5708560659873,-64.0103508505359,
-37.9306225804214));
#249056=CARTESIAN_POINT('Ctrl Pts',(29.6856323200486,-63.9296692017906,
-38.0531029163005));
#249057=CARTESIAN_POINT('Ctrl Pts',(30.7751530506771,-63.8508154151505,
-38.1728084307914));
#249058=CARTESIAN_POINT('Ctrl Pts',(31.8714564875302,-63.7714008635034,
-38.2993400360045));
#249059=CARTESIAN_POINT('Ctrl Pts',(32.9762913921302,-63.6913171853042,
-38.4327189046099));
#249060=CARTESIAN_POINT('Ctrl Pts',(33.5084198852201,-63.6527459862737,
-38.4969589970124));
#249061=CARTESIAN_POINT('Ctrl Pts',(34.0425273518562,-63.614019591588,-38.5627880146862));
#249062=CARTESIAN_POINT('Ctrl Pts',(34.5788086790266,-63.5751260489737,
-38.6302108770047));
#249063=CARTESIAN_POINT('Ctrl Pts',(36.1448893682756,-63.4615468081186,
-38.8271031373561));
#249064=CARTESIAN_POINT('Ctrl Pts',(37.7294988066828,-63.3465421354812,
-39.0375887447045));
#249065=CARTESIAN_POINT('Ctrl Pts',(39.3360623391576,-63.2299236849227,
-39.2616214281767));
#249066=CARTESIAN_POINT('Ctrl Pts',(40.6060743557284,-63.1377350907157,
-39.4387225476549));
#249067=CARTESIAN_POINT('Ctrl Pts',(41.889805634289,-63.0445381474314,-39.6242903860922));
#249068=CARTESIAN_POINT('Ctrl Pts',(43.1889493654701,-62.9502447313255,
-39.8182791580079));
#249069=CARTESIAN_POINT('Origin',(0.,-12.9675000200281,-41.3499258784557));
#249070=CARTESIAN_POINT('Origin',(0.,-12.9675000200281,-39.8944822890418));
#249071=CARTESIAN_POINT('Ctrl Pts',(51.2025706017519,-39.328225120641,-37.7071200530847));
#249072=CARTESIAN_POINT('Ctrl Pts',(52.3681090731163,-39.383622315317,-37.971813107807));
#249073=CARTESIAN_POINT('Ctrl Pts',(52.3762811131638,-39.2667566979623,
-39.1625636424987));
#249074=CARTESIAN_POINT('Ctrl Pts',(50.7956729692978,-44.9619550972486,
-38.2598728770176));
#249075=CARTESIAN_POINT('Ctrl Pts',(51.9730265758272,-45.0335652528346,
-38.518105133122));
#249076=CARTESIAN_POINT('Ctrl Pts',(51.9843707818182,-44.8713355490926,
-39.7153118927877));
#249077=CARTESIAN_POINT('Ctrl Pts',(50.3883221033785,-50.568537225844,-38.9838894046595));
#249078=CARTESIAN_POINT('Ctrl Pts',(51.5808963019407,-50.6412894292773,
-39.2334583932555));
#249079=CARTESIAN_POINT('Ctrl Pts',(51.593953776595,-50.4545588417343,-40.439327968821));
#249080=CARTESIAN_POINT('Ctrl Pts',(49.9827447112972,-56.1564493854985,
-39.8182791580079));
#249081=CARTESIAN_POINT('Ctrl Pts',(51.1918003817792,-56.2056203249982,
-40.0543903140503));
#249082=CARTESIAN_POINT('Ctrl Pts',(51.2045125858509,-56.0238273371818,
-41.2737227474219));
#249083=CARTESIAN_POINT('Ctrl Pts',(49.9827447112972,-56.1564493854985,
-39.8182791580079));
#249084=CARTESIAN_POINT('Ctrl Pts',(50.0911214886949,-54.6632697259096,
-39.5953168471712));
#249085=CARTESIAN_POINT('Ctrl Pts',(50.1980496341728,-53.1904501707553,
-39.383479797693));
#249086=CARTESIAN_POINT('Ctrl Pts',(50.3036634881978,-51.7354201301719,
-39.1828342154937));
#249087=CARTESIAN_POINT('Ctrl Pts',(50.3810449553401,-50.6693444688322,
-39.0358246240957));
#249088=CARTESIAN_POINT('Ctrl Pts',(50.4577210805591,-49.6128188084273,
-38.8948211810747));
#249089=CARTESIAN_POINT('Ctrl Pts',(50.53374730462,-48.5648325682818,-38.7598376298278));
#249090=CARTESIAN_POINT('Ctrl Pts',(50.5689702478275,-48.0793006314427,
-38.6972997618981));
#249091=CARTESIAN_POINT('Ctrl Pts',(50.6040535531298,-47.5956039481458,
-38.6360542494831));
#249092=CARTESIAN_POINT('Ctrl Pts',(50.6390034272056,-47.1136342590436,
-38.5761013219299));
#249093=CARTESIAN_POINT('Ctrl Pts',(50.7295722452733,-45.8646619453888,
-38.4207397954076));
#249094=CARTESIAN_POINT('Ctrl Pts',(50.8192477956374,-44.6272466675281,
-38.2740493733813));
#249095=CARTESIAN_POINT('Ctrl Pts',(50.9081832836966,-43.3989068589922,
-38.1359863030349));
#249096=CARTESIAN_POINT('Ctrl Pts',(50.9891192449324,-42.281053173163,-38.0103416638308));
#249097=CARTESIAN_POINT('Ctrl Pts',(51.0694423684864,-41.1707157672133,
-37.8918417736258));
#249098=CARTESIAN_POINT('Ctrl Pts',(51.149269876778,-40.0660162000401,-37.7804979349991));
#249099=CARTESIAN_POINT('Ctrl Pts',(51.1670609623838,-39.8198127923561,
-37.7556828329486));
#249100=CARTESIAN_POINT('Ctrl Pts',(51.1848274355191,-39.573889384857,-37.7312233765221));
#249101=CARTESIAN_POINT('Ctrl Pts',(51.2025706017519,-39.328225120641,-37.7071200530847));
#249102=CARTESIAN_POINT('Ctrl Pts',(49.9827447112974,30.221449345442,-39.8182791580079));
#249103=CARTESIAN_POINT('Ctrl Pts',(51.1918003817794,30.2706202849417,-40.0543903140502));
#249104=CARTESIAN_POINT('Ctrl Pts',(51.2045125858511,30.0888272971254,-41.2737227474219));
#249105=CARTESIAN_POINT('Ctrl Pts',(50.3883221033964,24.6335371857877,-38.9838894046629));
#249106=CARTESIAN_POINT('Ctrl Pts',(51.5808963020367,24.7062893892444,-39.233458393181));
#249107=CARTESIAN_POINT('Ctrl Pts',(51.5939537765951,24.5195588016784,-40.4393279688242));
#249108=CARTESIAN_POINT('Ctrl Pts',(50.7956729693229,19.0269550571941,-38.2598728770233));
#249109=CARTESIAN_POINT('Ctrl Pts',(51.9730265758558,19.098565212774,-38.5181051331097));
#249110=CARTESIAN_POINT('Ctrl Pts',(51.9843707818182,18.9363355090369,-39.7153118927739));
#249111=CARTESIAN_POINT('Ctrl Pts',(51.202570601752,13.3932250805846,-37.7071200530847));
#249112=CARTESIAN_POINT('Ctrl Pts',(52.3681090731165,13.4486222752606,-37.971813107807));
#249113=CARTESIAN_POINT('Ctrl Pts',(52.3762811131638,13.3317566579059,-39.1625636424987));
#249114=CARTESIAN_POINT('Ctrl Pts',(51.202570601752,13.3932250805846,-37.7071200530847));
#249115=CARTESIAN_POINT('Ctrl Pts',(51.122945450528,14.4956807490165,-37.8152873750052));
#249116=CARTESIAN_POINT('Ctrl Pts',(51.0428508304973,15.6033560460543,-37.9306225804305));
#249117=CARTESIAN_POINT('Ctrl Pts',(50.9621691817486,16.7181323001641,-38.0531029163155));
#249118=CARTESIAN_POINT('Ctrl Pts',(50.8833153951093,17.8076530307813,-38.1728084308057));
#249119=CARTESIAN_POINT('Ctrl Pts',(50.803900843464,18.903956467623,-38.2993400360181));
#249120=CARTESIAN_POINT('Ctrl Pts',(50.723817165267,20.0087913722114,-38.4327189046227));
#249121=CARTESIAN_POINT('Ctrl Pts',(50.6852459662377,20.540919865293,-38.4969589970245));
#249122=CARTESIAN_POINT('Ctrl Pts',(50.6465195715533,21.0750273319207,-38.5627880146976));
#249123=CARTESIAN_POINT('Ctrl Pts',(50.6076260289403,21.6113086590827,-38.6302108770153));
#249124=CARTESIAN_POINT('Ctrl Pts',(50.4940467880895,23.1773893483014,-38.8271031373637));
#249125=CARTESIAN_POINT('Ctrl Pts',(50.3790421154564,24.7619987866776,-39.0375887447086));
#249126=CARTESIAN_POINT('Ctrl Pts',(50.2624236649002,26.3685623191205,-39.2616214281763));
#249127=CARTESIAN_POINT('Ctrl Pts',(50.170235070693,27.6385743356943,-39.438722547655));
#249128=CARTESIAN_POINT('Ctrl Pts',(50.0770381274072,28.9223056142579,-39.6242903860925));
#249129=CARTESIAN_POINT('Ctrl Pts',(49.9827447112974,30.221449345442,-39.8182791580079));
#249130=CARTESIAN_POINT('Origin',(0.,-12.9675000200281,-41.3499258784557));
#249131=CARTESIAN_POINT('Origin',(0.,-12.9675000200281,-39.8944822890418));
#249132=CARTESIAN_POINT('Ctrl Pts',(26.3607251006129,38.2350705817238,-37.7071200530847));
#249133=CARTESIAN_POINT('Ctrl Pts',(26.4161222952889,39.4006090530882,-37.971813107807));
#249134=CARTESIAN_POINT('Ctrl Pts',(26.2992566779342,39.4087810931356,-39.1625636424987));
#249135=CARTESIAN_POINT('Ctrl Pts',(31.994455077222,37.8281729492938,-38.2598728770231));
#249136=CARTESIAN_POINT('Ctrl Pts',(32.0660652328021,39.0055265558251,-38.5181051330933));
#249137=CARTESIAN_POINT('Ctrl Pts',(31.9038355290649,39.01687076179,-39.7153118927753));
#249138=CARTESIAN_POINT('Ctrl Pts',(37.6010372058154,37.4208220833505,-38.9838894046594));
#249139=CARTESIAN_POINT('Ctrl Pts',(37.6737894092744,38.6133962819915,-39.2334583931755));
#249140=CARTESIAN_POINT('Ctrl Pts',(37.4870588217073,38.6264537565668,-40.4393279688211));
#249141=CARTESIAN_POINT('Ctrl Pts',(43.1889493654704,37.015244691269,-39.8182791580079));
#249142=CARTESIAN_POINT('Ctrl Pts',(43.23812030497,38.224300361751,-40.0543903140502));
#249143=CARTESIAN_POINT('Ctrl Pts',(43.0563273171537,38.2370125658228,-41.2737227474219));
#249144=CARTESIAN_POINT('Ctrl Pts',(43.1889493654704,37.015244691269,-39.8182791580079));
#249145=CARTESIAN_POINT('Ctrl Pts',(41.6957697057964,37.123621468673,-39.5953168471585));
#249146=CARTESIAN_POINT('Ctrl Pts',(40.2229501505596,37.2305496141585,-39.3834797976693));
#249147=CARTESIAN_POINT('Ctrl Pts',(38.7679201098954,37.3361634681915,-39.1828342154603));
#249148=CARTESIAN_POINT('Ctrl Pts',(37.701844448578,37.4135449353336,-39.0358246240664));
#249149=CARTESIAN_POINT('Ctrl Pts',(36.6453187881949,37.4902210605526,-38.8948211810493));
#249150=CARTESIAN_POINT('Ctrl Pts',(35.5973325480708,37.5662472846133,-38.759837629806));
#249151=CARTESIAN_POINT('Ctrl Pts',(35.1118006112682,37.6014702278188,-38.6972997618815));
#249152=CARTESIAN_POINT('Ctrl Pts',(34.6281039280075,37.636553533119,-38.6360542494713));
#249153=CARTESIAN_POINT('Ctrl Pts',(34.1461342389413,37.6715034071926,-38.5761013219228));
#249154=CARTESIAN_POINT('Ctrl Pts',(32.897161925551,37.762072225242,-38.4207397954338));
#249155=CARTESIAN_POINT('Ctrl Pts',(31.6597466479497,37.8517477755866,-38.274049373437));
#249156=CARTESIAN_POINT('Ctrl Pts',(30.4314068396699,37.9406832636257,-38.1359863031161));
#249157=CARTESIAN_POINT('Ctrl Pts',(29.3135531539302,38.0216192248535,-38.010341663919));
#249158=CARTESIAN_POINT('Ctrl Pts',(28.2032157480691,38.1019423483989,-37.8918417737198));
#249159=CARTESIAN_POINT('Ctrl Pts',(27.098516180984,38.1817698566814,-37.7804979350974));
#249160=CARTESIAN_POINT('Ctrl Pts',(26.8523127729753,38.1995609423102,-37.7556828330132));
#249161=CARTESIAN_POINT('Ctrl Pts',(26.6063893651522,38.2173274154682,-37.731223376554));
#249162=CARTESIAN_POINT('Ctrl Pts',(26.3607251006129,38.2350705817238,-37.7071200530847));
#249163=CARTESIAN_POINT('Origin',(-55.3689732639432,-39.4760261191947,-55.24995));
#249164=CARTESIAN_POINT('',(-52.6630979669894,-38.1805575254669,-52.64995));
#249165=CARTESIAN_POINT('',(-52.6630979669894,-38.1805575254669,-55.24995));
#249166=CARTESIAN_POINT('Origin',(-55.3689732639432,-39.4760261191947,-52.64995));
#249167=CARTESIAN_POINT('Origin',(0.,-12.9675000200281,-55.24995));
#249168=CARTESIAN_POINT('Origin',(0.,-12.9675000200281,-39.0779244525544));
#249169=CARTESIAN_POINT('Origin',(0.,-12.9675000200281,-52.64995));
#249170=CARTESIAN_POINT('Origin',(0.,-12.9675000200281,-39.0779244525544));
#249171=CARTESIAN_POINT('Origin',(0.,-12.9675000200281,-37.6224808631404));
#249172=CARTESIAN_POINT('Ctrl Pts',(-52.1419834946474,-42.6173687451066,
-39.5132811674967));
#249173=CARTESIAN_POINT('Ctrl Pts',(-52.1327810050217,-42.7489704779756,
-38.3173126020845));
#249174=CARTESIAN_POINT('Ctrl Pts',(-50.9590827221993,-42.6955891686747,
-38.0578375780827));
#249175=CARTESIAN_POINT('Ctrl Pts',(-51.8286928526804,-47.0976336572277,
-40.0086902420288));
#249176=CARTESIAN_POINT('Ctrl Pts',(-51.817197900376,-47.2620191329047,
-38.806978691719));
#249177=CARTESIAN_POINT('Ctrl Pts',(-50.6332299575652,-47.1974014010278,
-38.5532483700491));
#249178=CARTESIAN_POINT('Ctrl Pts',(-51.5162900940338,-51.5652012463084,
-40.6057258043764));
#249179=CARTESIAN_POINT('Ctrl Pts',(-51.5035559922642,-51.7473073860814,
-39.3966344269474));
#249180=CARTESIAN_POINT('Ctrl Pts',(-50.307441595963,-51.6828823044661,
-39.1502839521633));
#249181=CARTESIAN_POINT('Ctrl Pts',(-51.2045125858509,-56.0238273371818,
-41.2737227474219));
#249182=CARTESIAN_POINT('Ctrl Pts',(-51.1918003817792,-56.2056203249982,
-40.0543903140503));
#249183=CARTESIAN_POINT('Ctrl Pts',(-49.9827447112972,-56.1564493854985,
-39.8182791580079));
#249184=CARTESIAN_POINT('Ctrl Pts',(-49.9827447112972,-56.1564493854985,
-39.8182791580079));
#249185=CARTESIAN_POINT('Ctrl Pts',(-50.2766098672488,-52.1076717408327,
-39.2137137167888));
#249186=CARTESIAN_POINT('Ctrl Pts',(-50.5713690581735,-48.0491354164006,
-38.6672717073897));
#249187=CARTESIAN_POINT('Ctrl Pts',(-50.8662592829545,-43.9775643489176,
-38.2016959289247));
#249188=CARTESIAN_POINT('Ctrl Pts',(46.6981266849492,30.7091523375488,-39.2904704603133));
#249189=CARTESIAN_POINT('Ctrl Pts',(46.6689684123063,30.6404043382273,-39.273452295095));
#249190=CARTESIAN_POINT('Ctrl Pts',(46.6043681216411,30.5066861069553,-39.238925705885));
#249191=CARTESIAN_POINT('Ctrl Pts',(46.5083209189471,30.3487389562033,-39.1945593129175));
#249192=CARTESIAN_POINT('Ctrl Pts',(46.4437937583117,30.2581216171786,-39.1673894861782));
#249193=CARTESIAN_POINT('Ctrl Pts',(46.3992224148768,30.1986447451181,-39.1491520227249));
#249194=CARTESIAN_POINT('Ctrl Pts',(46.3761748773305,30.1693908446446,-39.1399767764946));
#249195=CARTESIAN_POINT('Ctrl Pts',(46.3284414024809,30.1117648114071,-39.1214771434543));
#249196=CARTESIAN_POINT('Ctrl Pts',(46.3038983378397,30.083571828401,-39.112209259666));
#249197=CARTESIAN_POINT('Ctrl Pts',(46.253707387608,30.0286632749651,-39.0937226519629));
#249198=CARTESIAN_POINT('Ctrl Pts',(46.2280147026909,30.001893564456,-39.0844865568113));
#249199=CARTESIAN_POINT('Ctrl Pts',(46.1492148010453,29.9236586721517,-39.0568159196779));
#249200=CARTESIAN_POINT('Ctrl Pts',(46.0669347173688,29.8495134741745,-39.0292038481275));
#249201=CARTESIAN_POINT('Ctrl Pts',(45.9503410384262,29.7587889734315,-38.9925114043613));
#249202=CARTESIAN_POINT('Ctrl Pts',(45.8594191065401,29.6948377475824,-38.9650526418885));
#249203=CARTESIAN_POINT('Ctrl Pts',(45.7964751089327,29.6549785818455,-38.9467936623891));
#249204=CARTESIAN_POINT('Ctrl Pts',(45.748348603817,29.6261284949947,-38.9331097524421));
#249205=CARTESIAN_POINT('Ctrl Pts',(45.7321473284057,29.616684052073,-38.9285487676403));
#249206=CARTESIAN_POINT('Ctrl Pts',(45.6996106203311,29.5982459977232,-38.9194791520014));
#249207=CARTESIAN_POINT('Ctrl Pts',(45.683249044345,29.5892352448745,-38.9149628379356));
#249208=CARTESIAN_POINT('Ctrl Pts',(45.6010439155842,29.5452684013657,-38.8924942188443));
#249209=CARTESIAN_POINT('Ctrl Pts',(45.4667739830181,29.4816584171599,-38.8571935516581));
#249210=CARTESIAN_POINT('Ctrl Pts',(45.2922645146651,29.4187721922835,-38.8147007629208));
#249211=CARTESIAN_POINT('Ctrl Pts',(45.184512437616,29.3885937253944,-38.7899522655792));
#249212=CARTESIAN_POINT('Ctrl Pts',(45.1119891467798,29.3701842541612,-38.7736235920333));
#249213=CARTESIAN_POINT('Ctrl Pts',(45.0754052578815,29.3618381514785,-38.7655490803555));
#249214=CARTESIAN_POINT('Ctrl Pts',(45.0014447932705,29.3468760834356,-38.7495561846596));
#249215=CARTESIAN_POINT('Ctrl Pts',(44.964301863367,29.3403115562353,-38.7416890516424));
#249216=CARTESIAN_POINT('Ctrl Pts',(44.8900079594565,29.3290481892184,-38.726277749838));
#249217=CARTESIAN_POINT('Ctrl Pts',(44.8527936282157,29.324336495618,-38.7187198739728));
#249218=CARTESIAN_POINT('Ctrl Pts',(44.7410083373266,29.3129455735289,-38.6964994820139));
#249219=CARTESIAN_POINT('Ctrl Pts',(44.6662563757167,29.3089967422249,-38.6822807693139));
#249220=CARTESIAN_POINT('Ctrl Pts',(44.516312468428,29.3084067934202,-38.6550493453909));
#249221=CARTESIAN_POINT('Ctrl Pts',(44.441103189525,29.3117700143417,-38.6420342479066));
#249222=CARTESIAN_POINT('Ctrl Pts',(44.3468378615956,29.3206690055189,-38.6265520162729));
#249223=CARTESIAN_POINT('Ctrl Pts',(44.3279589148655,29.3226883315868,-38.6234933649988));
#249224=CARTESIAN_POINT('Ctrl Pts',(44.2901960653062,29.3271995080042,-38.6174591262491));
#249225=CARTESIAN_POINT('Ctrl Pts',(44.271274393292,29.329697893027,-38.614477863833));
#249226=CARTESIAN_POINT('Ctrl Pts',(44.2146592782019,29.3378915995821,-38.60568558559));
#249227=CARTESIAN_POINT('Ctrl Pts',(44.1772069502033,29.344266758826,-38.6000392683017));
#249228=CARTESIAN_POINT('Ctrl Pts',(44.0655444875092,29.3661148598052,-38.5837127379559));
#249229=CARTESIAN_POINT('Ctrl Pts',(43.9553791862171,29.3933792052515,-38.5686255047386));
#249230=CARTESIAN_POINT('Ctrl Pts',(43.8114622524781,29.4404829778103,-38.5509833019505));
#249231=CARTESIAN_POINT('Ctrl Pts',(43.705021834675,29.481230340464,-38.5390021142185));
#249232=CARTESIAN_POINT('Ctrl Pts',(43.6350719757086,29.512061063653,-38.5318621614261));
#249233=CARTESIAN_POINT('Ctrl Pts',(43.5656410085295,29.5447591316771,-38.525155654825));
#249234=CARTESIAN_POINT('Ctrl Pts',(43.5311320054746,29.5620794464364,-38.5220163122062));
#249235=CARTESIAN_POINT('Ctrl Pts',(43.4634866412134,29.5981758355574,-38.5162526847879));
#249236=CARTESIAN_POINT('Ctrl Pts',(43.4301834663392,29.6170276546,-38.5136117755133));
#249237=CARTESIAN_POINT('Ctrl Pts',(43.3647025891651,29.6562685687332,-38.5088155315793));
#249238=CARTESIAN_POINT('Ctrl Pts',(43.2681192378476,29.7174608121974,-38.5023448938576));
#249239=CARTESIAN_POINT('Ctrl Pts',(43.1764049274077,29.7855824582168,-38.4980286134812));
#249240=CARTESIAN_POINT('Ctrl Pts',(43.0584774180437,29.8826126224142,-38.4942050936184));
#249241=CARTESIAN_POINT('Ctrl Pts',(43.001681818637,29.9342392650769,-38.4932590761897));
#249242=CARTESIAN_POINT('Ctrl Pts',(42.8926599718677,30.0438904492243,-38.4933742455196));
#249243=CARTESIAN_POINT('Ctrl Pts',(42.8414047150844,30.1009342501745,-38.4944336470273));
#249244=CARTESIAN_POINT('Ctrl Pts',(42.7451036203247,30.2193471227021,-38.498479276642));
#249245=CARTESIAN_POINT('Ctrl Pts',(42.6550322643363,30.3420646399833,-38.5044516702661));
#249246=CARTESIAN_POINT('Ctrl Pts',(42.5773225406025,30.4733365238586,-38.5142428327574));
#249247=CARTESIAN_POINT('Ctrl Pts',(42.5326943378214,30.5580963840027,-38.5215739479982));
#249248=CARTESIAN_POINT('Ctrl Pts',(42.5239673850246,30.5751883092729,-38.5231018165939));
#249249=CARTESIAN_POINT('Ctrl Pts',(42.5069121510755,30.60964376351,-38.5262794637242));
#249250=CARTESIAN_POINT('Ctrl Pts',(42.4985805781952,30.627019094627,-38.5279307934181));
#249251=CARTESIAN_POINT('Ctrl Pts',(42.4743295471271,30.6792614198295,-38.5330409224498));
#249252=CARTESIAN_POINT('Ctrl Pts',(42.4438856226513,30.7493896366731,-38.5402834483744));
#249253=CARTESIAN_POINT('Ctrl Pts',(42.4037483179465,30.8560072598611,-38.5524071291592));
#249254=CARTESIAN_POINT('Ctrl Pts',(42.3690543371876,30.9640160484273,-38.5657659376104));
#249255=CARTESIAN_POINT('Ctrl Pts',(42.3397558527982,31.0734075527136,-38.5803463747351));
#249256=CARTESIAN_POINT('Ctrl Pts',(42.3238156343608,31.1472555030051,-38.5908775753381));
#249257=CARTESIAN_POINT('Ctrl Pts',(42.3096820427396,31.2215665449467,-38.6018154236264));
#249258=CARTESIAN_POINT('Ctrl Pts',(42.3035171869091,31.2589715314082,-38.6074906718877));
#249259=CARTESIAN_POINT('Ctrl Pts',(42.2930235524414,31.3341791410138,-38.6192399292287));
#249260=CARTESIAN_POINT('Ctrl Pts',(42.2886818075092,31.3721585359098,-38.6253436316658));
#249261=CARTESIAN_POINT('Ctrl Pts',(42.281930630611,31.4478003630713,-38.6378362101326));
#249262=CARTESIAN_POINT('Ctrl Pts',(42.277074994566,31.5232809912004,-38.6506356205751));
#249263=CARTESIAN_POINT('Ctrl Pts',(42.2747992363309,31.6735553614761,-38.6774229397946));
#249264=CARTESIAN_POINT('Ctrl Pts',(42.2834818483937,31.8228397562226,-38.7059581415094));
#249265=CARTESIAN_POINT('Ctrl Pts',(42.3030248127084,31.9711385758679,-38.7362097844166));
#249266=CARTESIAN_POINT('Ctrl Pts',(42.3164494406915,32.0449687602614,-38.7519128032936));
#249267=CARTESIAN_POINT('Ctrl Pts',(42.3317154579634,32.1186122141692,-38.7679009120377));
#249268=CARTESIAN_POINT('Ctrl Pts',(42.3402956643805,32.1554227583218,-38.7760569897633));
#249269=CARTESIAN_POINT('Ctrl Pts',(42.3591481714288,32.228169160774,-38.7925026060078));
#249270=CARTESIAN_POINT('Ctrl Pts',(42.3694448348212,32.2642362896146,-38.8008201507359));
#249271=CARTESIAN_POINT('Ctrl Pts',(42.4028917825415,32.3714169561226,-38.8260275044574));
#249272=CARTESIAN_POINT('Ctrl Pts',(42.428602574983,32.4415633880281,-38.8431823298655));
#249273=CARTESIAN_POINT('Ctrl Pts',(42.4722685042023,32.5448307979217,-38.8694323201497));
#249274=CARTESIAN_POINT('Ctrl Pts',(42.4876674804306,32.5789105800712,-38.8782643966373));
#249275=CARTESIAN_POINT('Ctrl Pts',(42.5202146590728,32.6464795812123,-38.8961197808447));
#249276=CARTESIAN_POINT('Ctrl Pts',(42.5373018269229,32.6798350022668,-38.9051083126545));
#249277=CARTESIAN_POINT('Ctrl Pts',(42.5906929412925,32.7780783962456,-38.9321048428364));
#249278=CARTESIAN_POINT('Ctrl Pts',(42.629225789877,32.8414173722334,-38.9502105255135));
#249279=CARTESIAN_POINT('Ctrl Pts',(42.7120000069194,32.9638220552461,-38.9866125955294));
#249280=CARTESIAN_POINT('Ctrl Pts',(42.7783647966162,33.0524402968179,-39.0140612314234));
#249281=CARTESIAN_POINT('Ctrl Pts',(42.8754380724448,33.1642175243331,-39.0509520337677));
#249282=CARTESIAN_POINT('Ctrl Pts',(42.9268673384212,33.2179450225078,-39.0694937486382));
#249283=CARTESIAN_POINT('Ctrl Pts',(42.9797817061918,33.2705900457306,-39.088089881442));
#249284=CARTESIAN_POINT('Ctrl Pts',(43.0069972096607,33.2963736994336,-39.097418269769));
#249285=CARTESIAN_POINT('Ctrl Pts',(43.0622936398443,33.3462615369726,-39.1159154063528));
#249286=CARTESIAN_POINT('Ctrl Pts',(43.0904949946047,33.3704876748183,-39.1251268688783));
#249287=CARTESIAN_POINT('Ctrl Pts',(43.176562606447,33.4408730143712,-39.1525915568785));
#249288=CARTESIAN_POINT('Ctrl Pts',(43.2360245534179,33.4848790444095,-39.1707230137558));
#249289=CARTESIAN_POINT('Ctrl Pts',(43.358992255749,33.5670176609587,-39.2066046432507));
#249290=CARTESIAN_POINT('Ctrl Pts',(43.4542745623933,33.6242424638975,-39.233238623837));
#249291=CARTESIAN_POINT('Ctrl Pts',(43.5542222374601,33.6747516510336,-39.2594493821381));
#249292=CARTESIAN_POINT('Ctrl Pts',(43.6219256430316,33.7069073870393,-39.2768314299875));
#249293=CARTESIAN_POINT('Ctrl Pts',(43.6563381479934,33.7222286468184,-39.2854811722856));
#249294=CARTESIAN_POINT('Ctrl Pts',(43.7254519170511,33.7509934760635,-39.3024907499371));
#249295=CARTESIAN_POINT('Ctrl Pts',(43.7602995448845,33.7645084608315,-39.3108885064059));
#249296=CARTESIAN_POINT('Ctrl Pts',(43.8304781084082,33.789780836939,-39.3274499785309));
#249297=CARTESIAN_POINT('Ctrl Pts',(43.9365171946568,33.8250735562425,-39.3519527568515));
#249298=CARTESIAN_POINT('Ctrl Pts',(44.0809642638621,33.8617420360433,-39.3832806139221));
#249299=CARTESIAN_POINT('Ctrl Pts',(44.1916183723467,33.8813683146414,-39.4057679385072));
#249300=CARTESIAN_POINT('Ctrl Pts',(44.2659122959159,33.8926702964892,-39.4205323411483));
#249301=CARTESIAN_POINT('Ctrl Pts',(44.3033049221432,33.8974288658374,-39.4277978831022));
#249302=CARTESIAN_POINT('Ctrl Pts',(44.3598453576919,33.9032050944765,-39.4385322478049));
#249303=CARTESIAN_POINT('Ctrl Pts',(44.3787527158677,33.9049006163346,-39.4420799976889));
#249304=CARTESIAN_POINT('Ctrl Pts',(44.4164967874688,33.9078161173588,-39.4490791780208));
#249305=CARTESIAN_POINT('Ctrl Pts',(44.4353708468856,33.9090400957878,-39.4525377314439));
#249306=CARTESIAN_POINT('Ctrl Pts',(44.4919347179527,33.9120095261765,-39.462779235967));
#249307=CARTESIAN_POINT('Ctrl Pts',(44.52962054914,33.9130584408517,-39.4694384189012));
#249308=CARTESIAN_POINT('Ctrl Pts',(44.6425299001817,33.9134342925821,-39.4889026473125));
#249309=CARTESIAN_POINT('Ctrl Pts',(44.7176656228988,33.9100023852834,-39.5012068570978));
#249310=CARTESIAN_POINT('Ctrl Pts',(44.867623327666,33.8957625538083,-39.524471978366));
#249311=CARTESIAN_POINT('Ctrl Pts',(44.9424659600731,33.8849485744664,-39.5354353652432));
#249312=CARTESIAN_POINT('Ctrl Pts',(45.0357885152669,33.8666999843662,-39.5482785606344));
#249313=CARTESIAN_POINT('Ctrl Pts',(45.0544546343785,33.8628074782943,-39.5508053225112));
#249314=CARTESIAN_POINT('Ctrl Pts',(45.091743102575,33.8545484160302,-39.5557691634051));
#249315=CARTESIAN_POINT('Ctrl Pts',(45.1104022544846,33.850171655015,-39.5582107864407));
#249316=CARTESIAN_POINT('Ctrl Pts',(45.1661672125598,33.8363538303533,-39.5653802281989));
#249317=CARTESIAN_POINT('Ctrl Pts',(45.2029511118778,33.8262578362557,-39.5699395109212));
#249318=CARTESIAN_POINT('Ctrl Pts',(45.312316831343,33.7933159380614,-39.582990524906));
#249319=CARTESIAN_POINT('Ctrl Pts',(45.4195983160475,33.7551076509549,-39.5947758536238));
#249320=CARTESIAN_POINT('Ctrl Pts',(45.5585113890164,33.6937328563153,-39.6079933748399));
#249321=CARTESIAN_POINT('Ctrl Pts',(45.6606150024606,33.6424505696195,-39.6166516297843));
#249322=CARTESIAN_POINT('Ctrl Pts',(45.7272860947277,33.6047101271221,-39.6215780075552));
#249323=CARTESIAN_POINT('Ctrl Pts',(45.7932287365117,33.5651705839516,-39.6260731428005));
#249324=CARTESIAN_POINT('Ctrl Pts',(45.8259059249178,33.5444453395394,-39.6281074988013));
#249325=CARTESIAN_POINT('Ctrl Pts',(45.8897275017006,33.5016881508368,-39.6316923737189));
#249326=CARTESIAN_POINT('Ctrl Pts',(45.9210297733036,33.4795651380848,-39.6332542688506));
#249327=CARTESIAN_POINT('Ctrl Pts',(45.9823424846244,33.4339088874735,-39.6359180193303));
#249328=CARTESIAN_POINT('Ctrl Pts',(46.0724202597563,33.3632801300718,-39.6392265347984));
#249329=CARTESIAN_POINT('Ctrl Pts',(46.1850394564173,33.2606222983665,-39.6409205727319));
#249330=CARTESIAN_POINT('Ctrl Pts',(46.2638636333332,33.1772336958075,-39.6401443034625));
#249331=CARTESIAN_POINT('Ctrl Pts',(46.3151397511292,33.1201974856456,-39.6391646017005));
#249332=CARTESIAN_POINT('Ctrl Pts',(46.3401349353408,33.0909661742941,-39.6384440851485));
#249333=CARTESIAN_POINT('Ctrl Pts',(46.3888523044997,33.0309971480077,-39.6365301000439));
#249334=CARTESIAN_POINT('Ctrl Pts',(46.4123735341802,33.0005036828642,-39.6353439924849));
#249335=CARTESIAN_POINT('Ctrl Pts',(46.4576879006691,32.9386388625828,-39.6325280276393));
#249336=CARTESIAN_POINT('Ctrl Pts',(46.52311576659,32.8444620833496,-39.6276360146217));
#249337=CARTESIAN_POINT('Ctrl Pts',(46.5810426872604,32.7462345994881,-39.6207752343847));
#249338=CARTESIAN_POINT('Ctrl Pts',(46.6516918187307,32.6117039458857,-39.6098936921283));
#249339=CARTESIAN_POINT('Ctrl Pts',(46.683723185051,32.5426422373878,-39.6035832967262));
#249340=CARTESIAN_POINT('Ctrl Pts',(46.7195635412788,32.4540883209461,-39.5945936116187));
#249341=CARTESIAN_POINT('Ctrl Pts',(46.7265235775841,32.4362514419463,-39.5927383889278));
#249342=CARTESIAN_POINT('Ctrl Pts',(46.7400123459627,32.4003742100513,-39.5889189813535));
#249343=CARTESIAN_POINT('Ctrl Pts',(46.7465535157541,32.3822946053341,-39.5869502184844));
#249344=CARTESIAN_POINT('Ctrl Pts',(46.7654644360989,32.3279072933142,-39.5808958427402));
#249345=CARTESIAN_POINT('Ctrl Pts',(46.7770937339888,32.2915493874551,-39.5766741707955));
#249346=CARTESIAN_POINT('Ctrl Pts',(46.8091770518909,32.182013131159,-39.5634457571489));
#249347=CARTESIAN_POINT('Ctrl Pts',(46.8444383818759,32.034891308334,-39.5443264312115));
#249348=CARTESIAN_POINT('Ctrl Pts',(46.8650708643864,31.8856621776612,-39.5223044891954));
#249349=CARTESIAN_POINT('Ctrl Pts',(46.8750487417844,31.7729724844591,-39.50469487268));
#249350=CARTESIAN_POINT('Ctrl Pts',(46.8774570362353,31.7352651712118,-39.4986397605723));
#249351=CARTESIAN_POINT('Ctrl Pts',(46.8796767940079,31.6785286095959,-39.4892824810203));
#249352=CARTESIAN_POINT('Ctrl Pts',(46.8801843407089,31.6595724593507,-39.4861150486293));
#249353=CARTESIAN_POINT('Ctrl Pts',(46.8807312344332,31.6216180949417,-39.479690628598));
#249354=CARTESIAN_POINT('Ctrl Pts',(46.8807699646674,31.6025797052015,-39.4764266299692));
#249355=CARTESIAN_POINT('Ctrl Pts',(46.8801790388754,31.5455906639181,-39.4665317368708));
#249356=CARTESIAN_POINT('Ctrl Pts',(46.8788490796135,31.5078273383739,-39.4598096545541));
#249357=CARTESIAN_POINT('Ctrl Pts',(46.874360617844,31.4326451774338,-39.4461013696832));
#249358=CARTESIAN_POINT('Ctrl Pts',(46.864884835636,31.320441459725,-39.4251517854185));
#249359=CARTESIAN_POINT('Ctrl Pts',(46.8414902947658,31.1730719473388,-39.3956936109857));
#249360=CARTESIAN_POINT('Ctrl Pts',(46.8074810934279,31.0279105813681,-39.364717848004));
#249361=CARTESIAN_POINT('Ctrl Pts',(46.7869180083019,30.9560697433081,-39.3487190247537));
#249362=CARTESIAN_POINT('Ctrl Pts',(46.7645577771926,30.884604709384,-39.332461491893));
#249363=CARTESIAN_POINT('Ctrl Pts',(46.7524740339114,30.8490466969583,-39.3242001683612));
#249364=CARTESIAN_POINT('Ctrl Pts',(46.7264943673172,30.7783632715819,-39.3074248425479));
#249365=CARTESIAN_POINT('Ctrl Pts',(46.7127058212706,30.7435263372096,-39.2989795429224));
#249366=CARTESIAN_POINT('Ctrl Pts',(46.6981266849492,30.7091523375488,-39.2904704603133));
#249367=CARTESIAN_POINT('Ctrl Pts',(44.7926621173534,30.9780510210195,-41.4731170634489));
#249368=CARTESIAN_POINT('Ctrl Pts',(44.7841183378731,30.958431594105,-41.4560988982307));
#249369=CARTESIAN_POINT('Ctrl Pts',(44.7652574387158,30.9202429989855,-41.4215723090211));
#249370=CARTESIAN_POINT('Ctrl Pts',(44.7373647422364,30.8750641226134,-41.3772059160528));
#249371=CARTESIAN_POINT('Ctrl Pts',(44.7186826069414,30.8491098680677,-41.3500360893141));
#249372=CARTESIAN_POINT('Ctrl Pts',(44.7057896374646,30.8320666178198,-41.3317986258606));
#249373=CARTESIAN_POINT('Ctrl Pts',(44.6991283043737,30.8236797190306,-41.3226233796301));
#249374=CARTESIAN_POINT('Ctrl Pts',(44.6853430526266,30.8071501195218,-41.3041237465898));
#249375=CARTESIAN_POINT('Ctrl Pts',(44.6782604199269,30.7990587859436,-41.2948558628018));
#249376=CARTESIAN_POINT('Ctrl Pts',(44.6637865272211,30.7832912649286,-41.2763692550984));
#249377=CARTESIAN_POINT('Ctrl Pts',(44.65638232911,30.7755995480316,-41.2671331599469));
#249378=CARTESIAN_POINT('Ctrl Pts',(44.6336879630273,30.7531065345255,-41.2394625228135));
#249379=CARTESIAN_POINT('Ctrl Pts',(44.6100194582072,30.7317609779911,-41.211850451263));
#249380=CARTESIAN_POINT('Ctrl Pts',(44.5765344835469,30.7055824366946,-41.1751580074971));
#249381=CARTESIAN_POINT('Ctrl Pts',(44.5504480754,30.6870962504203,-41.147699245024));
#249382=CARTESIAN_POINT('Ctrl Pts',(44.5324056777293,30.6755504391987,-41.1294402655247));
#249383=CARTESIAN_POINT('Ctrl Pts',(44.5186168522497,30.6671837862428,-41.1157563555777));
#249384=CARTESIAN_POINT('Ctrl Pts',(44.5139760207251,30.6644431539959,-41.1111953707762));
#249385=CARTESIAN_POINT('Ctrl Pts',(44.5046579712977,30.6590892493455,-41.102125755137));
#249386=CARTESIAN_POINT('Ctrl Pts',(44.4999732573772,30.6564710151932,-41.0976094410703));
#249387=CARTESIAN_POINT('Ctrl Pts',(44.4764410055871,30.6436866063214,-41.0751408219827));
#249388=CARTESIAN_POINT('Ctrl Pts',(44.4380363426647,30.6251318507397,-41.0398401547925));
#249389=CARTESIAN_POINT('Ctrl Pts',(44.3881999640401,30.6066279457426,-40.9973473660572));
#249390=CARTESIAN_POINT('Ctrl Pts',(44.3574626802754,30.5976558165788,-40.9725988687145));
#249391=CARTESIAN_POINT('Ctrl Pts',(44.3367823836873,30.5921565153947,-40.9562701951691));
#249392=CARTESIAN_POINT('Ctrl Pts',(44.3263541271388,30.5896491085923,-40.9481956834911));
#249393=CARTESIAN_POINT('Ctrl Pts',(44.3052793937559,30.5851218575581,-40.9322027877955));
#249394=CARTESIAN_POINT('Ctrl Pts',(44.2946995104909,30.5831174982377,-40.924335654778));
#249395=CARTESIAN_POINT('Ctrl Pts',(44.2735450602529,30.5796377993431,-40.9089243529734));
#249396=CARTESIAN_POINT('Ctrl Pts',(44.2629524396991,30.5781585711684,-40.9013664771085));
#249397=CARTESIAN_POINT('Ctrl Pts',(44.2311453972639,30.5744985086998,-40.8791460851492));
#249398=CARTESIAN_POINT('Ctrl Pts',(44.2098907431643,30.5730912421562,-40.8649273724495));
#249399=CARTESIAN_POINT('Ctrl Pts',(44.1672866942957,30.5723474200962,-40.8376959485268));
#249400=CARTESIAN_POINT('Ctrl Pts',(44.1459323927671,30.5730120277702,-40.8246808510428));
#249401=CARTESIAN_POINT('Ctrl Pts',(44.1191870166623,30.5751734135742,-40.8091986194082));
#249402=CARTESIAN_POINT('Ctrl Pts',(44.1138315874482,30.5756735271978,-40.806139968135));
#249403=CARTESIAN_POINT('Ctrl Pts',(44.1031212948485,30.5768077596639,-40.8001057293845));
#249404=CARTESIAN_POINT('Ctrl Pts',(44.0977557278508,30.5774435866632,-40.7971244669688));
#249405=CARTESIAN_POINT('Ctrl Pts',(44.0817045383335,30.5795497856634,-40.7883321887253));
#249406=CARTESIAN_POINT('Ctrl Pts',(44.0710902649836,30.5812139186595,-40.7826858714375));
#249407=CARTESIAN_POINT('Ctrl Pts',(44.0394561806682,30.5869813183234,-40.7663593410916));
#249408=CARTESIAN_POINT('Ctrl Pts',(44.0082701709188,30.5942909050994,-40.7512721078743));
#249409=CARTESIAN_POINT('Ctrl Pts',(43.9675777996734,30.6070988998346,-40.7336299050859));
#249410=CARTESIAN_POINT('Ctrl Pts',(43.9375066395073,30.6182485087226,-40.721648717354));
#249411=CARTESIAN_POINT('Ctrl Pts',(43.917761614853,30.626725808719,-40.7145087645619));
#249412=CARTESIAN_POINT('Ctrl Pts',(43.8981718083816,30.6357351147044,-40.7078022579606));
#249413=CARTESIAN_POINT('Ctrl Pts',(43.8884396229394,30.6405162381665,-40.7046629153417));
#249414=CARTESIAN_POINT('Ctrl Pts',(43.8693712864522,30.6504970769624,-40.6988992879235));
#249415=CARTESIAN_POINT('Ctrl Pts',(43.8599880575193,30.6557176389023,-40.6962583786489));
#249416=CARTESIAN_POINT('Ctrl Pts',(43.8415477166501,30.6665995934339,-40.6914621347147));
#249417=CARTESIAN_POINT('Ctrl Pts',(43.8143622090585,30.6835906587784,-40.6849914969931));
#249418=CARTESIAN_POINT('Ctrl Pts',(43.7885885365895,30.7025683103525,-40.6806752166169));
#249419=CARTESIAN_POINT('Ctrl Pts',(43.7554869731093,30.7296502406846,-40.676851696754));
#249420=CARTESIAN_POINT('Ctrl Pts',(43.7395647886014,30.744083456595,-40.6759056793254));
#249421=CARTESIAN_POINT('Ctrl Pts',(43.7090440489059,30.7747854825451,-40.6760208486551));
#249422=CARTESIAN_POINT('Ctrl Pts',(43.6947173014185,30.7907796762741,-40.6770802501629));
#249423=CARTESIAN_POINT('Ctrl Pts',(43.6678443418708,30.8240220908504,-40.6811258797777));
#249424=CARTESIAN_POINT('Ctrl Pts',(43.6427576069985,30.8585127548254,-40.687098273402));
#249425=CARTESIAN_POINT('Ctrl Pts',(43.6212142380078,30.8954846730083,-40.6968894358922));
#249426=CARTESIAN_POINT('Ctrl Pts',(43.6088787182641,30.9193798597989,-40.7042205511341));
#249427=CARTESIAN_POINT('Ctrl Pts',(43.6064685586478,30.9241994859948,-40.7057484197296));
#249428=CARTESIAN_POINT('Ctrl Pts',(43.6017624551859,30.9339175659931,-40.70892606686));
#249429=CARTESIAN_POINT('Ctrl Pts',(43.5994656231147,30.9388193592268,-40.7105773965538));
#249430=CARTESIAN_POINT('Ctrl Pts',(43.5927866482525,30.953560895212,-40.7156875255853));
#249431=CARTESIAN_POINT('Ctrl Pts',(43.5844198153918,30.9733582110501,-40.72293005151));
#249432=CARTESIAN_POINT('Ctrl Pts',(43.5734440082896,31.0034822735469,-40.7350537322951));
#249433=CARTESIAN_POINT('Ctrl Pts',(43.5640181327981,31.0340244080827,-40.7484125407461));
#249434=CARTESIAN_POINT('Ctrl Pts',(43.5561284133843,31.0649820306433,-40.7629929778707));
#249435=CARTESIAN_POINT('Ctrl Pts',(43.5518912037438,31.0858969805267,-40.7735241784737));
#249436=CARTESIAN_POINT('Ctrl Pts',(43.5481682579358,31.1069510729684,-40.7844620267622));
#249437=CARTESIAN_POINT('Ctrl Pts',(43.5465635963524,31.1175527760565,-40.7901372750232));
#249438=CARTESIAN_POINT('Ctrl Pts',(43.5438765944467,31.1388768366658,-40.8018865323646));
#249439=CARTESIAN_POINT('Ctrl Pts',(43.5427912565025,31.1496493641875,-40.8079902348016));
#249440=CARTESIAN_POINT('Ctrl Pts',(43.5411674088753,31.1711124235333,-40.8204828132684));
#249441=CARTESIAN_POINT('Ctrl Pts',(43.5400805588778,31.19253758885,-40.8332822237109));
#249442=CARTESIAN_POINT('Ctrl Pts',(43.5400129658238,31.2352236668913,-40.8600695429299));
#249443=CARTESIAN_POINT('Ctrl Pts',(43.5430492497798,31.2776738375434,-40.8886047446452));
#249444=CARTESIAN_POINT('Ctrl Pts',(43.5491614319672,31.3198884817001,-40.918856387552));
#249445=CARTESIAN_POINT('Ctrl Pts',(43.5532522131496,31.3409199794841,-40.9345594064291));
#249446=CARTESIAN_POINT('Ctrl Pts',(43.5578644352119,31.361905871423,-40.9505475151733));
#249447=CARTESIAN_POINT('Ctrl Pts',(43.560439098329,31.3723994717644,-40.9587035928991));
#249448=CARTESIAN_POINT('Ctrl Pts',(43.5660648897127,31.3931449423641,-40.9751492091434));
#249449=CARTESIAN_POINT('Ctrl Pts',(43.5691234314236,31.4034342087731,-40.9834667538713));
#249450=CARTESIAN_POINT('Ctrl Pts',(43.5790202279964,31.4340221767704,-41.0086741075936));
#249451=CARTESIAN_POINT('Ctrl Pts',(43.5865808644402,31.4540562960243,-41.0258289330007));
#249452=CARTESIAN_POINT('Ctrl Pts',(43.5993606039644,31.4835727602996,-41.0520789232858));
#249453=CARTESIAN_POINT('Ctrl Pts',(43.6038584649574,31.4933175175814,-41.0609109997729));
#249454=CARTESIAN_POINT('Ctrl Pts',(43.6133480280387,31.5126460303085,-41.0787663839806));
#249455=CARTESIAN_POINT('Ctrl Pts',(43.6183219077102,31.5221915251339,-41.0877549157913));
#249456=CARTESIAN_POINT('Ctrl Pts',(43.6338406007018,31.5503182102049,-41.1147514459697));
#249457=CARTESIAN_POINT('Ctrl Pts',(43.6450116757484,31.5684678157769,-41.13285712865));
#249458=CARTESIAN_POINT('Ctrl Pts',(43.6689569093208,31.6035742491305,-41.1692591986645));
#249459=CARTESIAN_POINT('Ctrl Pts',(43.6881189975485,31.6290150958394,-41.1967078345595));
#249460=CARTESIAN_POINT('Ctrl Pts',(43.7160805799803,31.6611548911343,-41.2335986369031));
#249461=CARTESIAN_POINT('Ctrl Pts',(43.7308739938731,31.6766212732249,-41.2521403517739));
#249462=CARTESIAN_POINT('Ctrl Pts',(43.7460847706871,31.6917854492915,-41.2707364845776));
#249463=CARTESIAN_POINT('Ctrl Pts',(43.7539033240721,31.6992171694526,-41.2800648729051));
#249464=CARTESIAN_POINT('Ctrl Pts',(43.7697797892606,31.7136063232936,-41.298562009488));
#249465=CARTESIAN_POINT('Ctrl Pts',(43.7778723272806,31.7205988773597,-41.3077734720143));
#249466=CARTESIAN_POINT('Ctrl Pts',(43.8025568401133,31.7409299545529,-41.3352381600133));
#249467=CARTESIAN_POINT('Ctrl Pts',(43.8195937300504,31.7536621581445,-41.353369616892));
#249468=CARTESIAN_POINT('Ctrl Pts',(43.8547939251157,31.7774712224987,-41.3892512463859));
#249469=CARTESIAN_POINT('Ctrl Pts',(43.8820456950658,31.7940939723408,-41.4158852269725));
#249470=CARTESIAN_POINT('Ctrl Pts',(43.9105977352555,31.8088239425505,-41.4420959852738));
#249471=CARTESIAN_POINT('Ctrl Pts',(43.9299312426308,31.8182163905263,-41.4594780331231));
#249472=CARTESIAN_POINT('Ctrl Pts',(43.9397545046832,31.8226994853967,-41.4681277754213));
#249473=CARTESIAN_POINT('Ctrl Pts',(43.959476379363,31.8311327029401,-41.4851373530728));
#249474=CARTESIAN_POINT('Ctrl Pts',(43.969416794615,31.835103670887,-41.4935351095415));
#249475=CARTESIAN_POINT('Ctrl Pts',(43.9894286782948,31.8425474915593,-41.5100965816665));
#249476=CARTESIAN_POINT('Ctrl Pts',(44.0196562937352,31.8529720625538,-41.5345993599874));
#249477=CARTESIAN_POINT('Ctrl Pts',(44.0607928561344,31.8639280327151,-41.5659272170578));
#249478=CARTESIAN_POINT('Ctrl Pts',(44.0922765794535,31.8699137146658,-41.5884145416429));
#249479=CARTESIAN_POINT('Ctrl Pts',(44.1134085621028,31.8733992175668,-41.6031789442838));
#249480=CARTESIAN_POINT('Ctrl Pts',(44.1240412545,31.8748890570172,-41.6104444862381));
#249481=CARTESIAN_POINT('Ctrl Pts',(44.1401138557838,31.8767382236783,-41.6211788509405));
#249482=CARTESIAN_POINT('Ctrl Pts',(44.1454877988083,31.8772894545129,-41.6247266008247));
#249483=CARTESIAN_POINT('Ctrl Pts',(44.1562140153048,31.878256418298,-41.6317257811562));
#249484=CARTESIAN_POINT('Ctrl Pts',(44.161576905651,31.8786734249769,-41.6351843345794));
#249485=CARTESIAN_POINT('Ctrl Pts',(44.1776466456902,31.8797244502982,-41.6454258391029));
#249486=CARTESIAN_POINT('Ctrl Pts',(44.1883500092183,31.8801603696231,-41.6520850220369));
#249487=CARTESIAN_POINT('Ctrl Pts',(44.2204087008324,31.8806796234647,-41.671549250448));
#249488=CARTESIAN_POINT('Ctrl Pts',(44.2417298059497,31.8799780982567,-41.6838534602333));
#249489=CARTESIAN_POINT('Ctrl Pts',(44.2842582084951,31.8764766164199,-41.7071185815018));
#249490=CARTESIAN_POINT('Ctrl Pts',(44.3054713486111,31.8736750129732,-41.7180819683776));
#249491=CARTESIAN_POINT('Ctrl Pts',(44.3319064277948,31.8688271235064,-41.7309251637703));
#249492=CARTESIAN_POINT('Ctrl Pts',(44.3371930873745,31.8677885276791,-41.7334519256467));
#249493=CARTESIAN_POINT('Ctrl Pts',(44.3477523920959,31.8655764110726,-41.7384157665409));
#249494=CARTESIAN_POINT('Ctrl Pts',(44.353035452149,31.8644001232798,-41.7408573895762));
#249495=CARTESIAN_POINT('Ctrl Pts',(44.368821997144,31.8606750365135,-41.7480268313348));
#249496=CARTESIAN_POINT('Ctrl Pts',(44.3792318927429,31.8579388865424,-41.752586114057));
#249497=CARTESIAN_POINT('Ctrl Pts',(44.4101727404,31.8489724804825,-41.7656371280416));
#249498=CARTESIAN_POINT('Ctrl Pts',(44.4405041748167,31.8385015328462,-41.7774224567595));
#249499=CARTESIAN_POINT('Ctrl Pts',(44.4797386522914,31.8215610256552,-41.7906399779756));
#249500=CARTESIAN_POINT('Ctrl Pts',(44.5085558494592,31.8073558935676,-41.7992982329201));
#249501=CARTESIAN_POINT('Ctrl Pts',(44.5273583247585,31.7968714183439,-41.8042246106906));
#249502=CARTESIAN_POINT('Ctrl Pts',(44.5459478308046,31.7858731708475,-41.8087197459362));
#249503=CARTESIAN_POINT('Ctrl Pts',(44.5551558111633,31.7801015230391,-41.8107541019367));
#249504=CARTESIAN_POINT('Ctrl Pts',(44.5731320510561,31.7681815367951,-41.814338976855));
#249505=CARTESIAN_POINT('Ctrl Pts',(44.5819448307914,31.7620078883687,-41.8159008719862));
#249506=CARTESIAN_POINT('Ctrl Pts',(44.5991987000126,31.7492554022398,-41.8185646224661));
#249507=CARTESIAN_POINT('Ctrl Pts',(44.6245350600795,31.7295108031857,-41.8218731379338));
#249508=CARTESIAN_POINT('Ctrl Pts',(44.6561620699444,31.7007477525095,-41.8235671758672));
#249509=CARTESIAN_POINT('Ctrl Pts',(44.6782580742923,31.6773394437008,-41.8227909065983));
#249510=CARTESIAN_POINT('Ctrl Pts',(44.6926220014235,31.6613194462407,-41.8218112048364));
#249511=CARTESIAN_POINT('Ctrl Pts',(44.6996188611148,31.6531046671394,-41.8210906882841));
#249512=CARTESIAN_POINT('Ctrl Pts',(44.7132456597446,31.6362429219073,-41.8191767031797));
#249513=CARTESIAN_POINT('Ctrl Pts',(44.7198193777268,31.627664624135,-41.8179905956202));
#249514=CARTESIAN_POINT('Ctrl Pts',(44.7324727845908,31.610252798272,-41.8151746307749));
#249515=CARTESIAN_POINT('Ctrl Pts',(44.7507253937504,31.5837345714901,-41.8102826177571));
#249516=CARTESIAN_POINT('Ctrl Pts',(44.7668325292565,31.5560404782777,-41.8034218375205));
#249517=CARTESIAN_POINT('Ctrl Pts',(44.7864242741839,31.5180816884312,-41.7925402952635));
#249518=CARTESIAN_POINT('Ctrl Pts',(44.7952779235527,31.4985810718442,-41.7862298998632));
#249519=CARTESIAN_POINT('Ctrl Pts',(44.8051436066325,31.4735589245645,-41.777240214754));
#249520=CARTESIAN_POINT('Ctrl Pts',(44.8070571630202,31.4685179927861,-41.7753849920635));
#249521=CARTESIAN_POINT('Ctrl Pts',(44.8107609555809,31.4583769076679,-41.7715655844892));
#249522=CARTESIAN_POINT('Ctrl Pts',(44.8125545845603,31.4532656516023,-41.76959682162));
#249523=CARTESIAN_POINT('Ctrl Pts',(44.8177323950795,31.4378873281915,-41.7635424458753));
#249524=CARTESIAN_POINT('Ctrl Pts',(44.8209059367305,31.4276035217402,-41.7593207739311));
#249525=CARTESIAN_POINT('Ctrl Pts',(44.8296276705658,31.3966113763671,-41.7460923602843));
#249526=CARTESIAN_POINT('Ctrl Pts',(44.8391161742293,31.3549585404116,-41.7269730343471));
#249527=CARTESIAN_POINT('Ctrl Pts',(44.8444380100638,31.312658433005,-41.7049510923314));
#249528=CARTESIAN_POINT('Ctrl Pts',(44.8468637082338,31.2806969121874,-41.6873414758157));
#249529=CARTESIAN_POINT('Ctrl Pts',(44.8474108190536,31.2699990859542,-41.6812863637077));
#249530=CARTESIAN_POINT('Ctrl Pts',(44.8478348231013,31.2538978106508,-41.671929084156));
#249531=CARTESIAN_POINT('Ctrl Pts',(44.8479099202363,31.2485174556463,-41.6687616517648));
#249532=CARTESIAN_POINT('Ctrl Pts',(44.8479268208064,31.2377432265879,-41.6623372317338));
#249533=CARTESIAN_POINT('Ctrl Pts',(44.8478683021095,31.2323379437313,-41.6590732331048));
#249534=CARTESIAN_POINT('Ctrl Pts',(44.8474921214824,31.2161555213209,-41.6491783400064));
#249535=CARTESIAN_POINT('Ctrl Pts',(44.8469759958029,31.2054292064128,-41.6424562576898));
#249536=CARTESIAN_POINT('Ctrl Pts',(44.8454249887827,31.1840681958411,-41.6287479728186));
#249537=CARTESIAN_POINT('Ctrl Pts',(44.8423204600693,31.1521790951542,-41.6077983885548));
#249538=CARTESIAN_POINT('Ctrl Pts',(44.8351290816859,31.1102584040656,-41.5783402141209));
#249539=CARTESIAN_POINT('Ctrl Pts',(44.8249268329474,31.0689281614894,-41.54736445114));
#249540=CARTESIAN_POINT('Ctrl Pts',(44.8188163283608,31.0484607830594,-41.5313656278891));
#249541=CARTESIAN_POINT('Ctrl Pts',(44.8121960627665,31.028093840338,-41.5151080950287));
#249542=CARTESIAN_POINT('Ctrl Pts',(44.808629563005,31.0179567656131,-41.5068467714969));
#249543=CARTESIAN_POINT('Ctrl Pts',(44.8009827391877,30.9977990758989,-41.4900714456835));
#249544=CARTESIAN_POINT('Ctrl Pts',(44.7969340070935,30.9878607344767,-41.4816261460579));
#249545=CARTESIAN_POINT('Ctrl Pts',(44.7926621173534,30.9780510210195,-41.4731170634489));
#249546=CARTESIAN_POINT('',(42.5465433949648,31.1494605775469,-38.9933921633854));
#249547=CARTESIAN_POINT('',(43.4124119497911,29.8671948678953,-38.9060746475284));
#249548=CARTESIAN_POINT('Ctrl Pts',(42.5465433949858,31.149460577658,-38.9933921633669));
#249549=CARTESIAN_POINT('Ctrl Pts',(42.5517121988544,31.1235309006459,-38.9890511466991));
#249550=CARTESIAN_POINT('Ctrl Pts',(42.5573895309802,31.0977319961209,-38.9848419481203));
#249551=CARTESIAN_POINT('Ctrl Pts',(42.5635729904876,31.072063191646,-38.9807642563972));
#249552=CARTESIAN_POINT('Ctrl Pts',(42.5712503905032,31.0401927347216,-38.9757013833469));
#249553=CARTESIAN_POINT('Ctrl Pts',(42.5797080333646,31.0085228392725,-38.9708412376922));
#249554=CARTESIAN_POINT('Ctrl Pts',(42.588946982225,30.9770538375888,-38.9661846968102));
#249555=CARTESIAN_POINT('Ctrl Pts',(42.598185929499,30.9455848413087,-38.9615281567277));
#249556=CARTESIAN_POINT('Ctrl Pts',(42.6082061579755,30.9143167308057,-38.9570752148634));
#249557=CARTESIAN_POINT('Ctrl Pts',(42.6190146688054,30.8832507585404,-38.9528281316886));
#249558=CARTESIAN_POINT('Ctrl Pts',(42.6298231763812,30.8521847956286,-38.9485810497924));
#249559=CARTESIAN_POINT('Ctrl Pts',(42.6414199451632,30.8213209708386,-38.9445397978418));
#249560=CARTESIAN_POINT('Ctrl Pts',(42.6538171837854,30.7906641657846,-38.9407085616));
#249561=CARTESIAN_POINT('Ctrl Pts',(42.6662144355469,30.760007328239,-38.9368773212977));
#249562=CARTESIAN_POINT('Ctrl Pts',(42.679412432567,30.7295576275844,-38.933256079272));
#249563=CARTESIAN_POINT('Ctrl Pts',(42.6934317597292,30.6993135470368,-38.929849324519));
#249564=CARTESIAN_POINT('Ctrl Pts',(42.7004414190611,30.6841915159301,-38.9281459481751));
#249565=CARTESIAN_POINT('Ctrl Pts',(42.7076664478388,30.6691033617142,-38.9264946184812));
#249566=CARTESIAN_POINT('Ctrl Pts',(42.7150618821773,30.6541435858172,-38.924905794916));
#249567=CARTESIAN_POINT('Ctrl Pts',(42.7224573165159,30.6391838099201,-38.9233169713508));
#249568=CARTESIAN_POINT('Ctrl Pts',(42.7300260074317,30.6243421619354,-38.9217891027553));
#249569=CARTESIAN_POINT('Ctrl Pts',(42.7377673957025,30.609622247504,-38.9203228797071));
#249570=CARTESIAN_POINT('Ctrl Pts',(42.7687329487861,30.5507425897785,-38.9144579875143));
#249571=CARTESIAN_POINT('Ctrl Pts',(42.8024375668609,30.4937516435998,-38.9095621141477));
#249572=CARTESIAN_POINT('Ctrl Pts',(42.8388299093084,30.438621888508,-38.9056211995292));
#249573=CARTESIAN_POINT('Ctrl Pts',(42.8752222517559,30.3834921334163,-38.9016802849107));
#249574=CARTESIAN_POINT('Ctrl Pts',(42.9142995039568,30.330221730441,-38.898694431399));
#249575=CARTESIAN_POINT('Ctrl Pts',(42.9560847992068,30.2788238207524,-38.8966716165917));
#249576=CARTESIAN_POINT('Ctrl Pts',(42.9978700944569,30.2274259110637,-38.8946488017843));
#249577=CARTESIAN_POINT('Ctrl Pts',(43.0423540539347,30.1779090615142,-38.8935894002766));
#249578=CARTESIAN_POINT('Ctrl Pts',(43.0896679045841,30.1303216200235,-38.8935318156116));
#249579=CARTESIAN_POINT('Ctrl Pts',(43.1369817552336,30.0827341785328,-38.8934742309466));
#249580=CARTESIAN_POINT('Ctrl Pts',(43.1862827102732,30.0379274090563,-38.8944202483754));
#249581=CARTESIAN_POINT('Ctrl Pts',(43.2374695236468,29.9958252623364,-38.8963320083068));
#249582=CARTESIAN_POINT('Ctrl Pts',(43.2886563370204,29.9537231156164,-38.8982437682382));
#249583=CARTESIAN_POINT('Ctrl Pts',(43.3417388904795,29.9143166390041,-38.9011209692255));
#249584=CARTESIAN_POINT('Ctrl Pts',(43.3967029760762,29.8775860305619,-38.9049562506722));
#249585=CARTESIAN_POINT('Ctrl Pts',(43.4019223133192,29.8740981269513,-38.9053204453472));
#249586=CARTESIAN_POINT('Ctrl Pts',(43.4071586307135,29.8706343666859,-38.9056932332283));
#249587=CARTESIAN_POINT('Ctrl Pts',(43.4124119245055,29.8671948319696,-38.9060746716112));
#249588=CARTESIAN_POINT('Ctrl Pts',(43.4124119916018,29.8671949277328,-38.9060746094712));
#249589=CARTESIAN_POINT('Ctrl Pts',(43.306953409283,29.9434764107567,-38.910152608303));
#249590=CARTESIAN_POINT('Ctrl Pts',(43.2083433673275,30.0286067508031,-38.9150790128273));
#249591=CARTESIAN_POINT('Ctrl Pts',(43.0323970922931,30.2092699147785,-38.926031267232));
#249592=CARTESIAN_POINT('Ctrl Pts',(42.9545167445323,30.303420598745,-38.9319503267308));
#249593=CARTESIAN_POINT('Ctrl Pts',(42.8824130593679,30.406577317803,-38.9385942614148));
#249594=CARTESIAN_POINT('Ctrl Pts',(42.8802160625943,30.4097376871659,-38.9387979558357));
#249595=CARTESIAN_POINT('Ctrl Pts',(42.873503757505,30.4194461821076,-38.9394241486516));
#249596=CARTESIAN_POINT('Ctrl Pts',(42.8690151216511,30.4260123314163,-38.9398482921576));
#249597=CARTESIAN_POINT('Ctrl Pts',(42.7974813182203,30.5318494929995,-38.9466952735419));
#249598=CARTESIAN_POINT('Ctrl Pts',(42.7379995399575,30.6368649182166,-38.953586864865));
#249599=CARTESIAN_POINT('Ctrl Pts',(42.627565466591,30.8761040070808,-38.9710040199756));
#249600=CARTESIAN_POINT('Ctrl Pts',(42.5804757556733,31.011029152592,-38.981657984184));
#249601=CARTESIAN_POINT('Ctrl Pts',(42.5465433948297,31.149460577507,-38.9933921634656));
#249602=CARTESIAN_POINT('Ctrl Pts',(44.5079524583208,33.2091977213449,-52.99995));
#249603=CARTESIAN_POINT('Ctrl Pts',(43.5445019199415,33.2091977213449,-52.9416166666667));
#249604=CARTESIAN_POINT('Ctrl Pts',(43.0627766507519,32.3748250798187,-52.8832833333334));
#249605=CARTESIAN_POINT('Ctrl Pts',(42.5810513815623,31.5404524382925,-52.82495));
#249606=CARTESIAN_POINT('Ctrl Pts',(43.0627766507519,30.7060797967663,-52.7666166666667));
#249607=CARTESIAN_POINT('Ctrl Pts',(43.5445019199415,29.87170715524,-52.7082833333333));
#249608=CARTESIAN_POINT('Ctrl Pts',(44.5079524583208,29.87170715524,-52.64995));
#249609=CARTESIAN_POINT('Ctrl Pts',(45.4714029967,29.87170715524,-52.5916166666666));
#249610=CARTESIAN_POINT('Ctrl Pts',(45.9531282658897,30.7060797967663,-52.5332833333334));
#249611=CARTESIAN_POINT('Ctrl Pts',(46.4348535350793,31.5404524382925,-52.4749500000001));
#249612=CARTESIAN_POINT('Ctrl Pts',(45.9531282658897,32.3748250798187,-52.4166166666667));
#249613=CARTESIAN_POINT('Ctrl Pts',(45.4714029967,33.2091977213449,-52.3582833333334));
#249614=CARTESIAN_POINT('Ctrl Pts',(44.5079524583208,33.2091977213449,-52.29995));
#249615=CARTESIAN_POINT('Ctrl Pts',(43.5445019199415,33.2091977213449,-52.2416166666667));
#249616=CARTESIAN_POINT('Ctrl Pts',(43.0627766507519,32.3748250798187,-52.1832833333333));
#249617=CARTESIAN_POINT('Ctrl Pts',(42.5810513815623,31.5404524382925,-52.12495));
#249618=CARTESIAN_POINT('Ctrl Pts',(43.0627766507519,30.7060797967663,-52.0666166666667));
#249619=CARTESIAN_POINT('Ctrl Pts',(43.5445019199415,29.87170715524,-52.0082833333333));
#249620=CARTESIAN_POINT('Ctrl Pts',(44.5079524583208,29.87170715524,-51.94995));
#249621=CARTESIAN_POINT('Ctrl Pts',(45.4714029967,29.87170715524,-51.8916166666667));
#249622=CARTESIAN_POINT('Ctrl Pts',(45.9531282658897,30.7060797967663,-51.8332833333333));
#249623=CARTESIAN_POINT('Ctrl Pts',(46.4348535350793,31.5404524382925,-51.77495));
#249624=CARTESIAN_POINT('Ctrl Pts',(45.9531282658897,32.3748250798187,-51.7166166666667));
#249625=CARTESIAN_POINT('Ctrl Pts',(45.4714029967,33.2091977213449,-51.6582833333333));
#249626=CARTESIAN_POINT('Ctrl Pts',(44.5079524583208,33.2091977213449,-51.59995));
#249627=CARTESIAN_POINT('Ctrl Pts',(43.5445019199415,33.2091977213449,-51.5416166666667));
#249628=CARTESIAN_POINT('Ctrl Pts',(43.0627766507519,32.3748250798187,-51.4832833333333));
#249629=CARTESIAN_POINT('Ctrl Pts',(42.5810513815623,31.5404524382925,-51.42495));
#249630=CARTESIAN_POINT('Ctrl Pts',(43.0627766507519,30.7060797967663,-51.3666166666667));
#249631=CARTESIAN_POINT('Ctrl Pts',(43.5445019199415,29.87170715524,-51.3082833333333));
#249632=CARTESIAN_POINT('Ctrl Pts',(44.5079524583208,29.87170715524,-51.24995));
#249633=CARTESIAN_POINT('Ctrl Pts',(45.4714029967,29.87170715524,-51.1916166666667));
#249634=CARTESIAN_POINT('Ctrl Pts',(45.9531282658897,30.7060797967663,-51.1332833333333));
#249635=CARTESIAN_POINT('Ctrl Pts',(46.4348535350793,31.5404524382925,-51.07495));
#249636=CARTESIAN_POINT('Ctrl Pts',(45.9531282658897,32.3748250798187,-51.0166166666667));
#249637=CARTESIAN_POINT('Ctrl Pts',(45.4714029967,33.2091977213449,-50.9582833333334));
#249638=CARTESIAN_POINT('Ctrl Pts',(44.5079524583208,33.2091977213449,-50.89995));
#249639=CARTESIAN_POINT('Ctrl Pts',(43.5445019199415,33.2091977213449,-50.8416166666667));
#249640=CARTESIAN_POINT('Ctrl Pts',(43.0627766507519,32.3748250798187,-50.7832833333333));
#249641=CARTESIAN_POINT('Ctrl Pts',(42.5810513815623,31.5404524382925,-50.72495));
#249642=CARTESIAN_POINT('Ctrl Pts',(43.0627766507519,30.7060797967663,-50.6666166666667));
#249643=CARTESIAN_POINT('Ctrl Pts',(43.5445019199415,29.87170715524,-50.6082833333334));
#249644=CARTESIAN_POINT('Ctrl Pts',(44.5079524583208,29.87170715524,-50.54995));
#249645=CARTESIAN_POINT('Ctrl Pts',(45.4714029967,29.87170715524,-50.4916166666667));
#249646=CARTESIAN_POINT('Ctrl Pts',(45.9531282658897,30.7060797967663,-50.4332833333333));
#249647=CARTESIAN_POINT('Ctrl Pts',(46.4348535350793,31.5404524382925,-50.37495));
#249648=CARTESIAN_POINT('Ctrl Pts',(45.9531282658897,32.3748250798187,-50.3166166666667));
#249649=CARTESIAN_POINT('Ctrl Pts',(45.4714029967,33.2091977213449,-50.2582833333334));
#249650=CARTESIAN_POINT('Ctrl Pts',(44.5079524583208,33.2091977213449,-50.19995));
#249651=CARTESIAN_POINT('Ctrl Pts',(43.5445019199415,33.2091977213449,-50.1416166666667));
#249652=CARTESIAN_POINT('Ctrl Pts',(43.0627766507519,32.3748250798187,-50.0832833333333));
#249653=CARTESIAN_POINT('Ctrl Pts',(42.5810513815623,31.5404524382925,-50.02495));
#249654=CARTESIAN_POINT('Ctrl Pts',(43.0627766507519,30.7060797967663,-49.9666166666667));
#249655=CARTESIAN_POINT('Ctrl Pts',(43.5445019199415,29.87170715524,-49.9082833333334));
#249656=CARTESIAN_POINT('Ctrl Pts',(44.5079524583208,29.87170715524,-49.84995));
#249657=CARTESIAN_POINT('Ctrl Pts',(45.4714029967,29.87170715524,-49.7916166666667));
#249658=CARTESIAN_POINT('Ctrl Pts',(45.9531282658897,30.7060797967663,-49.7332833333333));
#249659=CARTESIAN_POINT('Ctrl Pts',(46.4348535350793,31.5404524382925,-49.67495));
#249660=CARTESIAN_POINT('Ctrl Pts',(45.9531282658897,32.3748250798187,-49.6166166666667));
#249661=CARTESIAN_POINT('Ctrl Pts',(45.4714029967,33.2091977213449,-49.5582833333334));
#249662=CARTESIAN_POINT('Ctrl Pts',(44.5079524583208,33.2091977213449,-49.49995));
#249663=CARTESIAN_POINT('Ctrl Pts',(43.5445019199415,33.2091977213449,-49.4416166666667));
#249664=CARTESIAN_POINT('Ctrl Pts',(43.0627766507519,32.3748250798187,-49.3832833333334));
#249665=CARTESIAN_POINT('Ctrl Pts',(42.5810513815623,31.5404524382925,-49.32495));
#249666=CARTESIAN_POINT('Ctrl Pts',(43.0627766507519,30.7060797967663,-49.2666166666667));
#249667=CARTESIAN_POINT('Ctrl Pts',(43.5445019199415,29.87170715524,-49.2082833333334));
#249668=CARTESIAN_POINT('Ctrl Pts',(44.5079524583208,29.87170715524,-49.14995));
#249669=CARTESIAN_POINT('Ctrl Pts',(45.4714029967,29.87170715524,-49.0916166666667));
#249670=CARTESIAN_POINT('Ctrl Pts',(45.9531282658897,30.7060797967663,-49.0332833333333));
#249671=CARTESIAN_POINT('Ctrl Pts',(46.4348535350793,31.5404524382925,-48.97495));
#249672=CARTESIAN_POINT('Ctrl Pts',(45.9531282658897,32.3748250798187,-48.9166166666667));
#249673=CARTESIAN_POINT('Ctrl Pts',(45.4714029967,33.2091977213449,-48.8582833333333));
#249674=CARTESIAN_POINT('Ctrl Pts',(44.5079524583208,33.2091977213449,-48.79995));
#249675=CARTESIAN_POINT('Ctrl Pts',(43.5445019199415,33.2091977213449,-48.7416166666667));
#249676=CARTESIAN_POINT('Ctrl Pts',(43.0627766507519,32.3748250798187,-48.6832833333333));
#249677=CARTESIAN_POINT('Ctrl Pts',(42.5810513815623,31.5404524382925,-48.62495));
#249678=CARTESIAN_POINT('Ctrl Pts',(43.0627766507519,30.7060797967663,-48.5666166666667));
#249679=CARTESIAN_POINT('Ctrl Pts',(43.5445019199415,29.87170715524,-48.5082833333333));
#249680=CARTESIAN_POINT('Ctrl Pts',(44.5079524583208,29.87170715524,-48.44995));
#249681=CARTESIAN_POINT('Ctrl Pts',(45.4714029967,29.87170715524,-48.3916166666667));
#249682=CARTESIAN_POINT('Ctrl Pts',(45.9531282658897,30.7060797967663,-48.3332833333333));
#249683=CARTESIAN_POINT('Ctrl Pts',(46.4348535350793,31.5404524382925,-48.27495));
#249684=CARTESIAN_POINT('Ctrl Pts',(45.9531282658897,32.3748250798187,-48.2166166666667));
#249685=CARTESIAN_POINT('Ctrl Pts',(45.4714029967,33.2091977213449,-48.1582833333333));
#249686=CARTESIAN_POINT('Ctrl Pts',(44.5079524583208,33.2091977213449,-48.09995));
#249687=CARTESIAN_POINT('Ctrl Pts',(43.5445019199415,33.2091977213449,-48.0416166666667));
#249688=CARTESIAN_POINT('Ctrl Pts',(43.0627766507519,32.3748250798187,-47.9832833333334));
#249689=CARTESIAN_POINT('Ctrl Pts',(42.5810513815623,31.5404524382925,-47.92495));
#249690=CARTESIAN_POINT('Ctrl Pts',(43.0627766507519,30.7060797967663,-47.8666166666667));
#249691=CARTESIAN_POINT('Ctrl Pts',(43.5445019199415,29.87170715524,-47.8082833333333));
#249692=CARTESIAN_POINT('Ctrl Pts',(44.5079524583208,29.87170715524,-47.74995));
#249693=CARTESIAN_POINT('Ctrl Pts',(45.4714029967,29.87170715524,-47.6916166666667));
#249694=CARTESIAN_POINT('Ctrl Pts',(45.9531282658897,30.7060797967663,-47.6332833333333));
#249695=CARTESIAN_POINT('Ctrl Pts',(46.4348535350793,31.5404524382925,-47.57495));
#249696=CARTESIAN_POINT('Ctrl Pts',(45.9531282658897,32.3748250798187,-47.5166166666667));
#249697=CARTESIAN_POINT('Ctrl Pts',(45.4714029967,33.2091977213449,-47.4582833333333));
#249698=CARTESIAN_POINT('Ctrl Pts',(44.5079524583208,33.2091977213449,-47.39995));
#249699=CARTESIAN_POINT('Ctrl Pts',(43.5445019199415,33.2091977213449,-47.3416166666666));
#249700=CARTESIAN_POINT('Ctrl Pts',(43.0627766507519,32.3748250798187,-47.2832833333333));
#249701=CARTESIAN_POINT('Ctrl Pts',(42.5810513815623,31.5404524382925,-47.22495));
#249702=CARTESIAN_POINT('Ctrl Pts',(43.0627766507519,30.7060797967663,-47.1666166666667));
#249703=CARTESIAN_POINT('Ctrl Pts',(43.5445019199415,29.87170715524,-47.1082833333333));
#249704=CARTESIAN_POINT('Ctrl Pts',(44.5079524583208,29.87170715524,-47.04995));
#249705=CARTESIAN_POINT('Ctrl Pts',(45.4714029967,29.87170715524,-46.9916166666667));
#249706=CARTESIAN_POINT('Ctrl Pts',(45.9531282658897,30.7060797967663,-46.9332833333333));
#249707=CARTESIAN_POINT('Ctrl Pts',(46.4348535350793,31.5404524382925,-46.87495));
#249708=CARTESIAN_POINT('Ctrl Pts',(45.9531282658897,32.3748250798187,-46.8166166666667));
#249709=CARTESIAN_POINT('Ctrl Pts',(45.4714029967,33.2091977213449,-46.7582833333333));
#249710=CARTESIAN_POINT('Ctrl Pts',(44.5079524583208,33.2091977213449,-46.69995));
#249711=CARTESIAN_POINT('Ctrl Pts',(43.5445019199415,33.2091977213449,-46.6416166666666));
#249712=CARTESIAN_POINT('Ctrl Pts',(43.0627766507519,32.3748250798187,-46.5832833333334));
#249713=CARTESIAN_POINT('Ctrl Pts',(42.5810513815623,31.5404524382925,-46.52495));
#249714=CARTESIAN_POINT('Ctrl Pts',(43.0627766507519,30.7060797967663,-46.4666166666667));
#249715=CARTESIAN_POINT('Ctrl Pts',(43.5445019199415,29.87170715524,-46.4082833333333));
#249716=CARTESIAN_POINT('Ctrl Pts',(44.5079524583208,29.87170715524,-46.34995));
#249717=CARTESIAN_POINT('Ctrl Pts',(45.4714029967,29.87170715524,-46.2916166666667));
#249718=CARTESIAN_POINT('Ctrl Pts',(45.9531282658897,30.7060797967663,-46.2332833333334));
#249719=CARTESIAN_POINT('Ctrl Pts',(46.4348535350793,31.5404524382925,-46.17495));
#249720=CARTESIAN_POINT('Ctrl Pts',(45.9531282658897,32.3748250798187,-46.1166166666667));
#249721=CARTESIAN_POINT('Ctrl Pts',(45.4714029967,33.2091977213449,-46.0582833333333));
#249722=CARTESIAN_POINT('Ctrl Pts',(44.5079524583208,33.2091977213449,-45.99995));
#249723=CARTESIAN_POINT('Ctrl Pts',(43.5445019199415,33.2091977213449,-45.9416166666667));
#249724=CARTESIAN_POINT('Ctrl Pts',(43.0627766507519,32.3748250798187,-45.8832833333333));
#249725=CARTESIAN_POINT('Ctrl Pts',(42.5810513815623,31.5404524382925,-45.82495));
#249726=CARTESIAN_POINT('Ctrl Pts',(43.0627766507519,30.7060797967663,-45.7666166666667));
#249727=CARTESIAN_POINT('Ctrl Pts',(43.5445019199415,29.87170715524,-45.7082833333333));
#249728=CARTESIAN_POINT('Ctrl Pts',(44.5079524583208,29.87170715524,-45.64995));
#249729=CARTESIAN_POINT('Ctrl Pts',(45.4714029967,29.87170715524,-45.5916166666667));
#249730=CARTESIAN_POINT('Ctrl Pts',(45.9531282658897,30.7060797967663,-45.5332833333333));
#249731=CARTESIAN_POINT('Ctrl Pts',(46.4348535350793,31.5404524382925,-45.47495));
#249732=CARTESIAN_POINT('Ctrl Pts',(45.9531282658897,32.3748250798187,-45.4166166666667));
#249733=CARTESIAN_POINT('Ctrl Pts',(45.4714029967,33.2091977213449,-45.3582833333333));
#249734=CARTESIAN_POINT('Ctrl Pts',(44.5079524583208,33.2091977213449,-45.29995));
#249735=CARTESIAN_POINT('Ctrl Pts',(43.5445019199415,33.2091977213449,-45.2416166666667));
#249736=CARTESIAN_POINT('Ctrl Pts',(43.0627766507519,32.3748250798187,-45.1832833333333));
#249737=CARTESIAN_POINT('Ctrl Pts',(42.5810513815623,31.5404524382925,-45.12495));
#249738=CARTESIAN_POINT('Ctrl Pts',(43.0627766507519,30.7060797967663,-45.0666166666667));
#249739=CARTESIAN_POINT('Ctrl Pts',(43.5445019199415,29.87170715524,-45.0082833333334));
#249740=CARTESIAN_POINT('Ctrl Pts',(44.5079524583208,29.87170715524,-44.94995));
#249741=CARTESIAN_POINT('Ctrl Pts',(45.4714029967,29.87170715524,-44.8916166666667));
#249742=CARTESIAN_POINT('Ctrl Pts',(45.9531282658897,30.7060797967663,-44.8332833333334));
#249743=CARTESIAN_POINT('Ctrl Pts',(46.4348535350793,31.5404524382925,-44.77495));
#249744=CARTESIAN_POINT('Ctrl Pts',(45.9531282658897,32.3748250798187,-44.7166166666667));
#249745=CARTESIAN_POINT('Ctrl Pts',(45.4714029967,33.2091977213449,-44.6582833333333));
#249746=CARTESIAN_POINT('Ctrl Pts',(44.5079524583208,33.2091977213449,-44.59995));
#249747=CARTESIAN_POINT('Ctrl Pts',(43.5445019199415,33.2091977213449,-44.5416166666667));
#249748=CARTESIAN_POINT('Ctrl Pts',(43.0627766507519,32.3748250798187,-44.4832833333334));
#249749=CARTESIAN_POINT('Ctrl Pts',(42.5810513815623,31.5404524382925,-44.42495));
#249750=CARTESIAN_POINT('Ctrl Pts',(43.0627766507519,30.7060797967663,-44.3666166666667));
#249751=CARTESIAN_POINT('Ctrl Pts',(43.5445019199415,29.87170715524,-44.3082833333334));
#249752=CARTESIAN_POINT('Ctrl Pts',(44.5079524583208,29.87170715524,-44.24995));
#249753=CARTESIAN_POINT('Ctrl Pts',(45.4714029967,29.87170715524,-44.1916166666667));
#249754=CARTESIAN_POINT('Ctrl Pts',(45.9531282658897,30.7060797967663,-44.1332833333334));
#249755=CARTESIAN_POINT('Ctrl Pts',(46.4348535350793,31.5404524382925,-44.07495));
#249756=CARTESIAN_POINT('Ctrl Pts',(45.9531282658897,32.3748250798187,-44.0166166666667));
#249757=CARTESIAN_POINT('Ctrl Pts',(45.4714029967,33.2091977213449,-43.9582833333334));
#249758=CARTESIAN_POINT('Ctrl Pts',(44.5079524583208,33.2091977213449,-43.89995));
#249759=CARTESIAN_POINT('Ctrl Pts',(43.5445019199415,33.2091977213449,-43.8416166666667));
#249760=CARTESIAN_POINT('Ctrl Pts',(43.0627766507519,32.3748250798187,-43.7832833333334));
#249761=CARTESIAN_POINT('Ctrl Pts',(42.5810513815623,31.5404524382925,-43.72495));
#249762=CARTESIAN_POINT('Ctrl Pts',(43.0627766507519,30.7060797967663,-43.6666166666667));
#249763=CARTESIAN_POINT('Ctrl Pts',(43.5445019199415,29.87170715524,-43.6082833333333));
#249764=CARTESIAN_POINT('Ctrl Pts',(44.5079524583208,29.87170715524,-43.54995));
#249765=CARTESIAN_POINT('Ctrl Pts',(45.4714029967,29.87170715524,-43.4916166666667));
#249766=CARTESIAN_POINT('Ctrl Pts',(45.9531282658897,30.7060797967663,-43.4332833333333));
#249767=CARTESIAN_POINT('Ctrl Pts',(46.4348535350793,31.5404524382925,-43.37495));
#249768=CARTESIAN_POINT('Ctrl Pts',(45.9531282658897,32.3748250798187,-43.3166166666667));
#249769=CARTESIAN_POINT('Ctrl Pts',(45.4714029967,33.2091977213449,-43.2582833333333));
#249770=CARTESIAN_POINT('Ctrl Pts',(44.5079524583208,33.2091977213449,-43.19995));
#249771=CARTESIAN_POINT('Ctrl Pts',(43.5445019199415,33.2091977213449,-43.1416166666666));
#249772=CARTESIAN_POINT('Ctrl Pts',(43.0627766507519,32.3748250798187,-43.0832833333333));
#249773=CARTESIAN_POINT('Ctrl Pts',(42.5810513815623,31.5404524382925,-43.02495));
#249774=CARTESIAN_POINT('Ctrl Pts',(43.0627766507519,30.7060797967663,-42.9666166666667));
#249775=CARTESIAN_POINT('Ctrl Pts',(43.5445019199415,29.87170715524,-42.9082833333333));
#249776=CARTESIAN_POINT('Ctrl Pts',(44.5079524583208,29.87170715524,-42.84995));
#249777=CARTESIAN_POINT('Ctrl Pts',(45.4714029967,29.87170715524,-42.7916166666667));
#249778=CARTESIAN_POINT('Ctrl Pts',(45.9531282658897,30.7060797967663,-42.7332833333334));
#249779=CARTESIAN_POINT('Ctrl Pts',(46.4348535350793,31.5404524382925,-42.67495));
#249780=CARTESIAN_POINT('Ctrl Pts',(45.9531282658897,32.3748250798187,-42.6166166666667));
#249781=CARTESIAN_POINT('Ctrl Pts',(45.4714029967,33.2091977213449,-42.5582833333333));
#249782=CARTESIAN_POINT('Ctrl Pts',(44.5079524583208,33.2091977213449,-42.49995));
#249783=CARTESIAN_POINT('Ctrl Pts',(43.5445019199415,33.2091977213449,-42.4416166666667));
#249784=CARTESIAN_POINT('Ctrl Pts',(43.0627766507519,32.3748250798187,-42.3832833333333));
#249785=CARTESIAN_POINT('Ctrl Pts',(42.5810513815623,31.5404524382925,-42.32495));
#249786=CARTESIAN_POINT('Ctrl Pts',(43.0627766507519,30.7060797967663,-42.2666166666667));
#249787=CARTESIAN_POINT('Ctrl Pts',(43.5445019199415,29.87170715524,-42.2082833333333));
#249788=CARTESIAN_POINT('Ctrl Pts',(44.5079524583208,29.87170715524,-42.14995));
#249789=CARTESIAN_POINT('Ctrl Pts',(45.4714029967,29.87170715524,-42.0916166666667));
#249790=CARTESIAN_POINT('Ctrl Pts',(45.9531282658897,30.7060797967663,-42.0332833333334));
#249791=CARTESIAN_POINT('Ctrl Pts',(46.4348535350793,31.5404524382925,-41.97495));
#249792=CARTESIAN_POINT('Ctrl Pts',(45.9531282658897,32.3748250798187,-41.9166166666666));
#249793=CARTESIAN_POINT('Ctrl Pts',(45.4714029967,33.2091977213449,-41.8582833333333));
#249794=CARTESIAN_POINT('Ctrl Pts',(44.5079524583208,33.2091977213449,-41.79995));
#249795=CARTESIAN_POINT('Ctrl Pts',(43.5445019199415,33.2091977213449,-41.7416166666667));
#249796=CARTESIAN_POINT('Ctrl Pts',(43.0627766507519,32.3748250798187,-41.6832833333333));
#249797=CARTESIAN_POINT('Ctrl Pts',(42.5810513815623,31.5404524382925,-41.62495));
#249798=CARTESIAN_POINT('Ctrl Pts',(43.0627766507519,30.7060797967663,-41.5666166666667));
#249799=CARTESIAN_POINT('Ctrl Pts',(43.5445019199415,29.87170715524,-41.5082833333334));
#249800=CARTESIAN_POINT('Ctrl Pts',(44.5079524583208,29.87170715524,-41.44995));
#249801=CARTESIAN_POINT('Ctrl Pts',(45.4714029967,29.87170715524,-41.3916166666667));
#249802=CARTESIAN_POINT('Ctrl Pts',(45.9531282658897,30.7060797967663,-41.3332833333334));
#249803=CARTESIAN_POINT('Ctrl Pts',(46.4348535350793,31.5404524382925,-41.27495));
#249804=CARTESIAN_POINT('Ctrl Pts',(45.9531282658897,32.3748250798187,-41.2166166666667));
#249805=CARTESIAN_POINT('Ctrl Pts',(45.4714029967,33.2091977213449,-41.1582833333333));
#249806=CARTESIAN_POINT('Ctrl Pts',(44.5079524583208,33.2091977213449,-41.09995));
#249807=CARTESIAN_POINT('Ctrl Pts',(43.5445019199415,33.2091977213449,-41.0416166666667));
#249808=CARTESIAN_POINT('Ctrl Pts',(43.0627766507519,32.3748250798187,-40.9832833333333));
#249809=CARTESIAN_POINT('Ctrl Pts',(42.5810513815623,31.5404524382925,-40.92495));
#249810=CARTESIAN_POINT('Ctrl Pts',(43.0627766507519,30.7060797967663,-40.8666166666667));
#249811=CARTESIAN_POINT('Ctrl Pts',(43.5445019199415,29.87170715524,-40.8082833333334));
#249812=CARTESIAN_POINT('Ctrl Pts',(44.5079524583208,29.87170715524,-40.74995));
#249813=CARTESIAN_POINT('Ctrl Pts',(45.4714029967,29.87170715524,-40.6916166666667));
#249814=CARTESIAN_POINT('Ctrl Pts',(45.9531282658897,30.7060797967663,-40.6332833333334));
#249815=CARTESIAN_POINT('Ctrl Pts',(46.4348535350793,31.5404524382925,-40.57495));
#249816=CARTESIAN_POINT('Ctrl Pts',(45.9531282658897,32.3748250798187,-40.5166166666666));
#249817=CARTESIAN_POINT('Ctrl Pts',(45.4714029967,33.2091977213449,-40.4582833333333));
#249818=CARTESIAN_POINT('Ctrl Pts',(44.5079524583208,33.2091977213449,-40.39995));
#249819=CARTESIAN_POINT('Ctrl Pts',(43.5445019199415,33.2091977213449,-40.3416166666667));
#249820=CARTESIAN_POINT('Ctrl Pts',(43.0627766507519,32.3748250798187,-40.2832833333334));
#249821=CARTESIAN_POINT('Ctrl Pts',(42.5810513815623,31.5404524382925,-40.22495));
#249822=CARTESIAN_POINT('Ctrl Pts',(43.0627766507519,30.7060797967663,-40.1666166666667));
#249823=CARTESIAN_POINT('Ctrl Pts',(43.5445019199415,29.87170715524,-40.1082833333334));
#249824=CARTESIAN_POINT('Ctrl Pts',(44.5079524583208,29.87170715524,-40.04995));
#249825=CARTESIAN_POINT('Ctrl Pts',(45.4714029967,29.87170715524,-39.9916166666667));
#249826=CARTESIAN_POINT('Ctrl Pts',(45.9531282658897,30.7060797967663,-39.9332833333333));
#249827=CARTESIAN_POINT('Ctrl Pts',(46.4348535350793,31.5404524382925,-39.87495));
#249828=CARTESIAN_POINT('Ctrl Pts',(45.9531282658897,32.3748250798187,-39.8166166666667));
#249829=CARTESIAN_POINT('Ctrl Pts',(45.4714029967,33.2091977213449,-39.7582833333334));
#249830=CARTESIAN_POINT('Ctrl Pts',(44.5079524583208,33.2091977213449,-39.69995));
#249831=CARTESIAN_POINT('Ctrl Pts',(43.5445019199415,33.2091977213449,-39.6416166666667));
#249832=CARTESIAN_POINT('Ctrl Pts',(43.0627766507519,32.3748250798187,-39.5832833333333));
#249833=CARTESIAN_POINT('Ctrl Pts',(42.5810513815623,31.5404524382925,-39.52495));
#249834=CARTESIAN_POINT('Ctrl Pts',(43.0627766507519,30.7060797967663,-39.4666166666667));
#249835=CARTESIAN_POINT('Ctrl Pts',(43.5445019199415,29.87170715524,-39.4082833333333));
#249836=CARTESIAN_POINT('Ctrl Pts',(44.5079524583208,29.87170715524,-39.34995));
#249837=CARTESIAN_POINT('Ctrl Pts',(45.4714029967,29.87170715524,-39.2916166666667));
#249838=CARTESIAN_POINT('Ctrl Pts',(45.9531282658897,30.7060797967663,-39.2332833333333));
#249839=CARTESIAN_POINT('Ctrl Pts',(46.4348535350793,31.5404524382925,-39.17495));
#249840=CARTESIAN_POINT('Ctrl Pts',(45.9531282658897,32.3748250798187,-39.1166166666667));
#249841=CARTESIAN_POINT('Ctrl Pts',(45.4714029967,33.2091977213449,-39.0582833333333));
#249842=CARTESIAN_POINT('Ctrl Pts',(44.5079524583208,33.2091977213449,-38.99995));
#249843=CARTESIAN_POINT('Ctrl Pts',(43.5445019199415,33.2091977213449,-38.9416166666667));
#249844=CARTESIAN_POINT('Ctrl Pts',(43.0627766507519,32.3748250798187,-38.8832833333334));
#249845=CARTESIAN_POINT('Ctrl Pts',(42.5810513815623,31.5404524382925,-38.82495));
#249846=CARTESIAN_POINT('Ctrl Pts',(43.0627766507519,30.7060797967663,-38.7666166666667));
#249847=CARTESIAN_POINT('Ctrl Pts',(43.5445019199415,29.87170715524,-38.7082833333333));
#249848=CARTESIAN_POINT('Ctrl Pts',(44.5079524583208,29.87170715524,-38.64995));
#249849=CARTESIAN_POINT('Ctrl Pts',(45.4714029967,29.87170715524,-38.5916166666667));
#249850=CARTESIAN_POINT('Ctrl Pts',(45.9531282658897,30.7060797967663,-38.5332833333334));
#249851=CARTESIAN_POINT('Ctrl Pts',(46.4348535350793,31.5404524382925,-38.47495));
#249852=CARTESIAN_POINT('Ctrl Pts',(45.9531282658897,32.3748250798187,-38.4166166666667));
#249853=CARTESIAN_POINT('Ctrl Pts',(45.4714029967,33.2091977213449,-38.3582833333333));
#249854=CARTESIAN_POINT('Ctrl Pts',(44.5079524583208,33.2091977213449,-38.29995));
#249855=CARTESIAN_POINT('Ctrl Pts',(43.5445019199415,33.2091977213449,-38.2416166666667));
#249856=CARTESIAN_POINT('Ctrl Pts',(43.0627766507519,32.3748250798187,-38.1832833333333));
#249857=CARTESIAN_POINT('Ctrl Pts',(42.5810513815623,31.5404524382925,-38.12495));
#249858=CARTESIAN_POINT('Ctrl Pts',(43.0627766507519,30.7060797967663,-38.0666166666667));
#249859=CARTESIAN_POINT('Ctrl Pts',(43.5445019199415,29.87170715524,-38.0082833333333));
#249860=CARTESIAN_POINT('Ctrl Pts',(44.5079524583208,29.87170715524,-37.94995));
#249861=CARTESIAN_POINT('Ctrl Pts',(45.4714029967,29.87170715524,-37.8916166666667));
#249862=CARTESIAN_POINT('Ctrl Pts',(45.9531282658897,30.7060797967663,-37.8332833333334));
#249863=CARTESIAN_POINT('Ctrl Pts',(46.4348535350793,31.5404524382925,-37.77495));
#249864=CARTESIAN_POINT('Ctrl Pts',(45.9531282658897,32.3748250798187,-37.7166166666667));
#249865=CARTESIAN_POINT('Ctrl Pts',(45.4714029967,33.2091977213449,-37.6582833333333));
#249866=CARTESIAN_POINT('Ctrl Pts',(44.5079524583208,33.2091977213449,-37.59995));
#249867=CARTESIAN_POINT('Ctrl Pts',(43.5445019199415,33.2091977213449,-37.5416166666667));
#249868=CARTESIAN_POINT('Ctrl Pts',(43.0627766507519,32.3748250798187,-37.4832833333334));
#249869=CARTESIAN_POINT('Ctrl Pts',(42.5810513815623,31.5404524382925,-37.42495));
#249870=CARTESIAN_POINT('Ctrl Pts',(43.0627766507519,30.7060797967663,-37.3666166666667));
#249871=CARTESIAN_POINT('Ctrl Pts',(43.5445019199415,29.87170715524,-37.3082833333333));
#249872=CARTESIAN_POINT('Ctrl Pts',(44.5079524583208,29.87170715524,-37.24995));
#249873=CARTESIAN_POINT('Ctrl Pts',(45.4714029967,29.87170715524,-37.1916166666667));
#249874=CARTESIAN_POINT('Ctrl Pts',(45.9531282658897,30.7060797967663,-37.1332833333334));
#249875=CARTESIAN_POINT('Ctrl Pts',(46.4348535350793,31.5404524382925,-37.07495));
#249876=CARTESIAN_POINT('Ctrl Pts',(45.9531282658897,32.3748250798187,-37.0166166666667));
#249877=CARTESIAN_POINT('Ctrl Pts',(45.8905850977848,32.4831530246427,-37.0090431559831));
#249878=CARTESIAN_POINT('Ctrl Pts',(45.8125914103809,32.5809465634453,-37.0009024189827));
#249879=CARTESIAN_POINT('Ctrl Pts',(44.5079524583208,33.6091932047179,-53.2308875));
#249880=CARTESIAN_POINT('Ctrl Pts',(43.3135644199415,33.6091932047179,-53.1725541666667));
#249881=CARTESIAN_POINT('Ctrl Pts',(42.7163704007519,32.5748228215052,-53.1142208333334));
#249882=CARTESIAN_POINT('Ctrl Pts',(42.1191763815623,31.5404524382925,-53.0558875000001));
#249883=CARTESIAN_POINT('Ctrl Pts',(42.7163704007519,30.5060820550798,-52.9975541666667));
#249884=CARTESIAN_POINT('Ctrl Pts',(43.3135644199415,29.4717116718671,-52.9392208333334));
#249885=CARTESIAN_POINT('Ctrl Pts',(44.5079524583208,29.4717116718671,-52.8808875));
#249886=CARTESIAN_POINT('Ctrl Pts',(45.7023404967,29.4717116718671,-52.8225541666667));
#249887=CARTESIAN_POINT('Ctrl Pts',(46.2995345158897,30.5060820550798,-52.7642208333334));
#249888=CARTESIAN_POINT('Ctrl Pts',(46.8967285350793,31.5404524382925,-52.7058875));
#249889=CARTESIAN_POINT('Ctrl Pts',(46.2995345158897,32.5748228215052,-52.6475541666667));
#249890=CARTESIAN_POINT('Ctrl Pts',(45.7023404967,33.6091932047179,-52.5892208333333));
#249891=CARTESIAN_POINT('Ctrl Pts',(44.5079524583208,33.6091932047179,-52.5308875));
#249892=CARTESIAN_POINT('Ctrl Pts',(43.3135644199415,33.6091932047179,-52.4725541666667));
#249893=CARTESIAN_POINT('Ctrl Pts',(42.7163704007519,32.5748228215052,-52.4142208333333));
#249894=CARTESIAN_POINT('Ctrl Pts',(42.1191763815623,31.5404524382925,-52.3558875000001));
#249895=CARTESIAN_POINT('Ctrl Pts',(42.7163704007519,30.5060820550798,-52.2975541666667));
#249896=CARTESIAN_POINT('Ctrl Pts',(43.3135644199415,29.4717116718671,-52.2392208333334));
#249897=CARTESIAN_POINT('Ctrl Pts',(44.5079524583208,29.4717116718671,-52.1808875));
#249898=CARTESIAN_POINT('Ctrl Pts',(45.7023404967,29.4717116718671,-52.1225541666667));
#249899=CARTESIAN_POINT('Ctrl Pts',(46.2995345158897,30.5060820550798,-52.0642208333334));
#249900=CARTESIAN_POINT('Ctrl Pts',(46.8967285350793,31.5404524382925,-52.0058875));
#249901=CARTESIAN_POINT('Ctrl Pts',(46.2995345158897,32.5748228215052,-51.9475541666667));
#249902=CARTESIAN_POINT('Ctrl Pts',(45.7023404967,33.6091932047179,-51.8892208333334));
#249903=CARTESIAN_POINT('Ctrl Pts',(44.5079524583208,33.6091932047179,-51.8308875));
#249904=CARTESIAN_POINT('Ctrl Pts',(43.3135644199415,33.6091932047179,-51.7725541666667));
#249905=CARTESIAN_POINT('Ctrl Pts',(42.7163704007519,32.5748228215052,-51.7142208333334));
#249906=CARTESIAN_POINT('Ctrl Pts',(42.1191763815623,31.5404524382925,-51.6558875));
#249907=CARTESIAN_POINT('Ctrl Pts',(42.7163704007519,30.5060820550798,-51.5975541666667));
#249908=CARTESIAN_POINT('Ctrl Pts',(43.3135644199415,29.4717116718671,-51.5392208333333));
#249909=CARTESIAN_POINT('Ctrl Pts',(44.5079524583208,29.4717116718671,-51.4808875));
#249910=CARTESIAN_POINT('Ctrl Pts',(45.7023404967,29.4717116718671,-51.4225541666667));
#249911=CARTESIAN_POINT('Ctrl Pts',(46.2995345158897,30.5060820550798,-51.3642208333334));
#249912=CARTESIAN_POINT('Ctrl Pts',(46.8967285350793,31.5404524382925,-51.3058875));
#249913=CARTESIAN_POINT('Ctrl Pts',(46.2995345158897,32.5748228215052,-51.2475541666667));
#249914=CARTESIAN_POINT('Ctrl Pts',(45.7023404967,33.6091932047179,-51.1892208333333));
#249915=CARTESIAN_POINT('Ctrl Pts',(44.5079524583208,33.6091932047179,-51.1308875));
#249916=CARTESIAN_POINT('Ctrl Pts',(43.3135644199415,33.6091932047179,-51.0725541666667));
#249917=CARTESIAN_POINT('Ctrl Pts',(42.7163704007519,32.5748228215052,-51.0142208333334));
#249918=CARTESIAN_POINT('Ctrl Pts',(42.1191763815623,31.5404524382925,-50.9558875));
#249919=CARTESIAN_POINT('Ctrl Pts',(42.7163704007519,30.5060820550798,-50.8975541666667));
#249920=CARTESIAN_POINT('Ctrl Pts',(43.3135644199415,29.4717116718671,-50.8392208333333));
#249921=CARTESIAN_POINT('Ctrl Pts',(44.5079524583208,29.4717116718671,-50.7808875));
#249922=CARTESIAN_POINT('Ctrl Pts',(45.7023404967,29.4717116718671,-50.7225541666666));
#249923=CARTESIAN_POINT('Ctrl Pts',(46.2995345158897,30.5060820550798,-50.6642208333333));
#249924=CARTESIAN_POINT('Ctrl Pts',(46.8967285350793,31.5404524382925,-50.6058875));
#249925=CARTESIAN_POINT('Ctrl Pts',(46.2995345158897,32.5748228215052,-50.5475541666667));
#249926=CARTESIAN_POINT('Ctrl Pts',(45.7023404967,33.6091932047179,-50.4892208333333));
#249927=CARTESIAN_POINT('Ctrl Pts',(44.5079524583208,33.6091932047179,-50.4308875));
#249928=CARTESIAN_POINT('Ctrl Pts',(43.3135644199415,33.6091932047179,-50.3725541666667));
#249929=CARTESIAN_POINT('Ctrl Pts',(42.7163704007519,32.5748228215052,-50.3142208333334));
#249930=CARTESIAN_POINT('Ctrl Pts',(42.1191763815623,31.5404524382925,-50.2558875));
#249931=CARTESIAN_POINT('Ctrl Pts',(42.7163704007519,30.5060820550798,-50.1975541666667));
#249932=CARTESIAN_POINT('Ctrl Pts',(43.3135644199415,29.4717116718671,-50.1392208333333));
#249933=CARTESIAN_POINT('Ctrl Pts',(44.5079524583208,29.4717116718671,-50.0808875));
#249934=CARTESIAN_POINT('Ctrl Pts',(45.7023404967,29.4717116718671,-50.0225541666667));
#249935=CARTESIAN_POINT('Ctrl Pts',(46.2995345158897,30.5060820550798,-49.9642208333334));
#249936=CARTESIAN_POINT('Ctrl Pts',(46.8967285350793,31.5404524382925,-49.9058875));
#249937=CARTESIAN_POINT('Ctrl Pts',(46.2995345158897,32.5748228215052,-49.8475541666667));
#249938=CARTESIAN_POINT('Ctrl Pts',(45.7023404967,33.6091932047179,-49.7892208333333));
#249939=CARTESIAN_POINT('Ctrl Pts',(44.5079524583208,33.6091932047179,-49.7308875));
#249940=CARTESIAN_POINT('Ctrl Pts',(43.3135644199415,33.6091932047179,-49.6725541666667));
#249941=CARTESIAN_POINT('Ctrl Pts',(42.7163704007519,32.5748228215052,-49.6142208333334));
#249942=CARTESIAN_POINT('Ctrl Pts',(42.1191763815623,31.5404524382925,-49.5558875));
#249943=CARTESIAN_POINT('Ctrl Pts',(42.7163704007519,30.5060820550798,-49.4975541666667));
#249944=CARTESIAN_POINT('Ctrl Pts',(43.3135644199415,29.4717116718671,-49.4392208333333));
#249945=CARTESIAN_POINT('Ctrl Pts',(44.5079524583208,29.4717116718671,-49.3808875));
#249946=CARTESIAN_POINT('Ctrl Pts',(45.7023404967,29.4717116718671,-49.3225541666667));
#249947=CARTESIAN_POINT('Ctrl Pts',(46.2995345158897,30.5060820550798,-49.2642208333334));
#249948=CARTESIAN_POINT('Ctrl Pts',(46.8967285350793,31.5404524382925,-49.2058875));
#249949=CARTESIAN_POINT('Ctrl Pts',(46.2995345158897,32.5748228215052,-49.1475541666667));
#249950=CARTESIAN_POINT('Ctrl Pts',(45.7023404967,33.6091932047179,-49.0892208333333));
#249951=CARTESIAN_POINT('Ctrl Pts',(44.5079524583208,33.6091932047179,-49.0308875));
#249952=CARTESIAN_POINT('Ctrl Pts',(43.3135644199415,33.6091932047179,-48.9725541666667));
#249953=CARTESIAN_POINT('Ctrl Pts',(42.7163704007519,32.5748228215052,-48.9142208333333));
#249954=CARTESIAN_POINT('Ctrl Pts',(42.1191763815623,31.5404524382925,-48.8558875));
#249955=CARTESIAN_POINT('Ctrl Pts',(42.7163704007519,30.5060820550798,-48.7975541666667));
#249956=CARTESIAN_POINT('Ctrl Pts',(43.3135644199415,29.4717116718671,-48.7392208333334));
#249957=CARTESIAN_POINT('Ctrl Pts',(44.5079524583208,29.4717116718671,-48.6808875));
#249958=CARTESIAN_POINT('Ctrl Pts',(45.7023404967,29.4717116718671,-48.6225541666667));
#249959=CARTESIAN_POINT('Ctrl Pts',(46.2995345158897,30.5060820550798,-48.5642208333334));
#249960=CARTESIAN_POINT('Ctrl Pts',(46.8967285350793,31.5404524382925,-48.5058875));
#249961=CARTESIAN_POINT('Ctrl Pts',(46.2995345158897,32.5748228215052,-48.4475541666667));
#249962=CARTESIAN_POINT('Ctrl Pts',(45.7023404967,33.6091932047179,-48.3892208333334));
#249963=CARTESIAN_POINT('Ctrl Pts',(44.5079524583208,33.6091932047179,-48.3308875));
#249964=CARTESIAN_POINT('Ctrl Pts',(43.3135644199415,33.6091932047179,-48.2725541666667));
#249965=CARTESIAN_POINT('Ctrl Pts',(42.7163704007519,32.5748228215052,-48.2142208333334));
#249966=CARTESIAN_POINT('Ctrl Pts',(42.1191763815623,31.5404524382925,-48.1558875));
#249967=CARTESIAN_POINT('Ctrl Pts',(42.7163704007519,30.5060820550798,-48.0975541666667));
#249968=CARTESIAN_POINT('Ctrl Pts',(43.3135644199415,29.4717116718671,-48.0392208333334));
#249969=CARTESIAN_POINT('Ctrl Pts',(44.5079524583208,29.4717116718671,-47.9808875));
#249970=CARTESIAN_POINT('Ctrl Pts',(45.7023404967,29.4717116718671,-47.9225541666667));
#249971=CARTESIAN_POINT('Ctrl Pts',(46.2995345158897,30.5060820550798,-47.8642208333334));
#249972=CARTESIAN_POINT('Ctrl Pts',(46.8967285350793,31.5404524382925,-47.8058875000001));
#249973=CARTESIAN_POINT('Ctrl Pts',(46.2995345158897,32.5748228215052,-47.7475541666667));
#249974=CARTESIAN_POINT('Ctrl Pts',(45.7023404967,33.6091932047179,-47.6892208333334));
#249975=CARTESIAN_POINT('Ctrl Pts',(44.5079524583208,33.6091932047179,-47.6308875));
#249976=CARTESIAN_POINT('Ctrl Pts',(43.3135644199415,33.6091932047179,-47.5725541666667));
#249977=CARTESIAN_POINT('Ctrl Pts',(42.7163704007519,32.5748228215052,-47.5142208333333));
#249978=CARTESIAN_POINT('Ctrl Pts',(42.1191763815623,31.5404524382925,-47.4558875));
#249979=CARTESIAN_POINT('Ctrl Pts',(42.7163704007519,30.5060820550798,-47.3975541666667));
#249980=CARTESIAN_POINT('Ctrl Pts',(43.3135644199415,29.4717116718671,-47.3392208333333));
#249981=CARTESIAN_POINT('Ctrl Pts',(44.5079524583208,29.4717116718671,-47.2808875));
#249982=CARTESIAN_POINT('Ctrl Pts',(45.7023404967,29.4717116718671,-47.2225541666667));
#249983=CARTESIAN_POINT('Ctrl Pts',(46.2995345158897,30.5060820550798,-47.1642208333334));
#249984=CARTESIAN_POINT('Ctrl Pts',(46.8967285350793,31.5404524382925,-47.1058875));
#249985=CARTESIAN_POINT('Ctrl Pts',(46.2995345158897,32.5748228215052,-47.0475541666667));
#249986=CARTESIAN_POINT('Ctrl Pts',(45.7023404967,33.6091932047179,-46.9892208333334));
#249987=CARTESIAN_POINT('Ctrl Pts',(44.5079524583208,33.6091932047179,-46.9308875));
#249988=CARTESIAN_POINT('Ctrl Pts',(43.3135644199415,33.6091932047179,-46.8725541666667));
#249989=CARTESIAN_POINT('Ctrl Pts',(42.7163704007519,32.5748228215052,-46.8142208333334));
#249990=CARTESIAN_POINT('Ctrl Pts',(42.1191763815623,31.5404524382925,-46.7558875));
#249991=CARTESIAN_POINT('Ctrl Pts',(42.7163704007519,30.5060820550798,-46.6975541666667));
#249992=CARTESIAN_POINT('Ctrl Pts',(43.3135644199415,29.4717116718671,-46.6392208333333));
#249993=CARTESIAN_POINT('Ctrl Pts',(44.5079524583208,29.4717116718671,-46.5808875));
#249994=CARTESIAN_POINT('Ctrl Pts',(45.7023404967,29.4717116718671,-46.5225541666667));
#249995=CARTESIAN_POINT('Ctrl Pts',(46.2995345158897,30.5060820550798,-46.4642208333334));
#249996=CARTESIAN_POINT('Ctrl Pts',(46.8967285350793,31.5404524382925,-46.4058875));
#249997=CARTESIAN_POINT('Ctrl Pts',(46.2995345158897,32.5748228215052,-46.3475541666667));
#249998=CARTESIAN_POINT('Ctrl Pts',(45.7023404967,33.6091932047179,-46.2892208333334));
#249999=CARTESIAN_POINT('Ctrl Pts',(44.5079524583208,33.6091932047179,-46.2308875));
#250000=CARTESIAN_POINT('Ctrl Pts',(43.3135644199415,33.6091932047179,-46.1725541666667));
#250001=CARTESIAN_POINT('Ctrl Pts',(42.7163704007519,32.5748228215052,-46.1142208333334));
#250002=CARTESIAN_POINT('Ctrl Pts',(42.1191763815623,31.5404524382925,-46.0558875));
#250003=CARTESIAN_POINT('Ctrl Pts',(42.7163704007519,30.5060820550798,-45.9975541666667));
#250004=CARTESIAN_POINT('Ctrl Pts',(43.3135644199415,29.4717116718671,-45.9392208333333));
#250005=CARTESIAN_POINT('Ctrl Pts',(44.5079524583208,29.4717116718671,-45.8808875));
#250006=CARTESIAN_POINT('Ctrl Pts',(45.7023404967,29.4717116718671,-45.8225541666667));
#250007=CARTESIAN_POINT('Ctrl Pts',(46.2995345158897,30.5060820550798,-45.7642208333334));
#250008=CARTESIAN_POINT('Ctrl Pts',(46.8967285350793,31.5404524382925,-45.7058875));
#250009=CARTESIAN_POINT('Ctrl Pts',(46.2995345158897,32.5748228215052,-45.6475541666667));
#250010=CARTESIAN_POINT('Ctrl Pts',(45.7023404967,33.6091932047179,-45.5892208333333));
#250011=CARTESIAN_POINT('Ctrl Pts',(44.5079524583208,33.6091932047179,-45.5308875));
#250012=CARTESIAN_POINT('Ctrl Pts',(43.3135644199415,33.6091932047179,-45.4725541666667));
#250013=CARTESIAN_POINT('Ctrl Pts',(42.7163704007519,32.5748228215052,-45.4142208333334));
#250014=CARTESIAN_POINT('Ctrl Pts',(42.1191763815623,31.5404524382925,-45.3558875));
#250015=CARTESIAN_POINT('Ctrl Pts',(42.7163704007519,30.5060820550798,-45.2975541666667));
#250016=CARTESIAN_POINT('Ctrl Pts',(43.3135644199415,29.4717116718671,-45.2392208333333));
#250017=CARTESIAN_POINT('Ctrl Pts',(44.5079524583208,29.4717116718671,-45.1808875));
#250018=CARTESIAN_POINT('Ctrl Pts',(45.7023404967,29.4717116718671,-45.1225541666667));
#250019=CARTESIAN_POINT('Ctrl Pts',(46.2995345158897,30.5060820550798,-45.0642208333334));
#250020=CARTESIAN_POINT('Ctrl Pts',(46.8967285350793,31.5404524382925,-45.0058875));
#250021=CARTESIAN_POINT('Ctrl Pts',(46.2995345158897,32.5748228215052,-44.9475541666667));
#250022=CARTESIAN_POINT('Ctrl Pts',(45.7023404967,33.6091932047179,-44.8892208333333));
#250023=CARTESIAN_POINT('Ctrl Pts',(44.5079524583208,33.6091932047179,-44.8308875));
#250024=CARTESIAN_POINT('Ctrl Pts',(43.3135644199415,33.6091932047179,-44.7725541666666));
#250025=CARTESIAN_POINT('Ctrl Pts',(42.7163704007519,32.5748228215052,-44.7142208333334));
#250026=CARTESIAN_POINT('Ctrl Pts',(42.1191763815623,31.5404524382925,-44.6558875));
#250027=CARTESIAN_POINT('Ctrl Pts',(42.7163704007519,30.5060820550798,-44.5975541666667));
#250028=CARTESIAN_POINT('Ctrl Pts',(43.3135644199415,29.4717116718671,-44.5392208333333));
#250029=CARTESIAN_POINT('Ctrl Pts',(44.5079524583208,29.4717116718671,-44.4808875));
#250030=CARTESIAN_POINT('Ctrl Pts',(45.7023404967,29.4717116718671,-44.4225541666667));
#250031=CARTESIAN_POINT('Ctrl Pts',(46.2995345158897,30.5060820550798,-44.3642208333333));
#250032=CARTESIAN_POINT('Ctrl Pts',(46.8967285350793,31.5404524382925,-44.3058875));
#250033=CARTESIAN_POINT('Ctrl Pts',(46.2995345158897,32.5748228215052,-44.2475541666667));
#250034=CARTESIAN_POINT('Ctrl Pts',(45.7023404967,33.6091932047179,-44.1892208333334));
#250035=CARTESIAN_POINT('Ctrl Pts',(44.5079524583208,33.6091932047179,-44.1308875));
#250036=CARTESIAN_POINT('Ctrl Pts',(43.3135644199415,33.6091932047179,-44.0725541666667));
#250037=CARTESIAN_POINT('Ctrl Pts',(42.7163704007519,32.5748228215052,-44.0142208333334));
#250038=CARTESIAN_POINT('Ctrl Pts',(42.1191763815623,31.5404524382925,-43.9558875));
#250039=CARTESIAN_POINT('Ctrl Pts',(42.7163704007519,30.5060820550798,-43.8975541666667));
#250040=CARTESIAN_POINT('Ctrl Pts',(43.3135644199415,29.4717116718671,-43.8392208333333));
#250041=CARTESIAN_POINT('Ctrl Pts',(44.5079524583208,29.4717116718671,-43.7808875));
#250042=CARTESIAN_POINT('Ctrl Pts',(45.7023404967,29.4717116718671,-43.7225541666667));
#250043=CARTESIAN_POINT('Ctrl Pts',(46.2995345158897,30.5060820550798,-43.6642208333334));
#250044=CARTESIAN_POINT('Ctrl Pts',(46.8967285350793,31.5404524382925,-43.6058875));
#250045=CARTESIAN_POINT('Ctrl Pts',(46.2995345158897,32.5748228215052,-43.5475541666667));
#250046=CARTESIAN_POINT('Ctrl Pts',(45.7023404967,33.6091932047179,-43.4892208333333));
#250047=CARTESIAN_POINT('Ctrl Pts',(44.5079524583208,33.6091932047179,-43.4308875));
#250048=CARTESIAN_POINT('Ctrl Pts',(43.3135644199415,33.6091932047179,-43.3725541666667));
#250049=CARTESIAN_POINT('Ctrl Pts',(42.7163704007519,32.5748228215052,-43.3142208333334));
#250050=CARTESIAN_POINT('Ctrl Pts',(42.1191763815623,31.5404524382925,-43.2558875));
#250051=CARTESIAN_POINT('Ctrl Pts',(42.7163704007519,30.5060820550798,-43.1975541666667));
#250052=CARTESIAN_POINT('Ctrl Pts',(43.3135644199415,29.4717116718671,-43.1392208333334));
#250053=CARTESIAN_POINT('Ctrl Pts',(44.5079524583208,29.4717116718671,-43.0808875));
#250054=CARTESIAN_POINT('Ctrl Pts',(45.7023404967,29.4717116718671,-43.0225541666667));
#250055=CARTESIAN_POINT('Ctrl Pts',(46.2995345158897,30.5060820550798,-42.9642208333334));
#250056=CARTESIAN_POINT('Ctrl Pts',(46.8967285350793,31.5404524382925,-42.9058875));
#250057=CARTESIAN_POINT('Ctrl Pts',(46.2995345158897,32.5748228215052,-42.8475541666667));
#250058=CARTESIAN_POINT('Ctrl Pts',(45.7023404967,33.6091932047179,-42.7892208333334));
#250059=CARTESIAN_POINT('Ctrl Pts',(44.5079524583208,33.6091932047179,-42.7308875));
#250060=CARTESIAN_POINT('Ctrl Pts',(43.3135644199415,33.6091932047179,-42.6725541666667));
#250061=CARTESIAN_POINT('Ctrl Pts',(42.7163704007519,32.5748228215052,-42.6142208333334));
#250062=CARTESIAN_POINT('Ctrl Pts',(42.1191763815623,31.5404524382925,-42.5558875));
#250063=CARTESIAN_POINT('Ctrl Pts',(42.7163704007519,30.5060820550798,-42.4975541666667));
#250064=CARTESIAN_POINT('Ctrl Pts',(43.3135644199415,29.4717116718671,-42.4392208333334));
#250065=CARTESIAN_POINT('Ctrl Pts',(44.5079524583208,29.4717116718671,-42.3808875));
#250066=CARTESIAN_POINT('Ctrl Pts',(45.7023404967,29.4717116718671,-42.3225541666667));
#250067=CARTESIAN_POINT('Ctrl Pts',(46.2995345158897,30.5060820550798,-42.2642208333334));
#250068=CARTESIAN_POINT('Ctrl Pts',(46.8967285350793,31.5404524382925,-42.2058875));
#250069=CARTESIAN_POINT('Ctrl Pts',(46.2995345158897,32.5748228215052,-42.1475541666667));
#250070=CARTESIAN_POINT('Ctrl Pts',(45.7023404967,33.6091932047179,-42.0892208333333));
#250071=CARTESIAN_POINT('Ctrl Pts',(44.5079524583208,33.6091932047179,-42.0308875));
#250072=CARTESIAN_POINT('Ctrl Pts',(43.3135644199415,33.6091932047179,-41.9725541666667));
#250073=CARTESIAN_POINT('Ctrl Pts',(42.7163704007519,32.5748228215052,-41.9142208333334));
#250074=CARTESIAN_POINT('Ctrl Pts',(42.1191763815623,31.5404524382925,-41.8558875));
#250075=CARTESIAN_POINT('Ctrl Pts',(42.7163704007519,30.5060820550798,-41.7975541666667));
#250076=CARTESIAN_POINT('Ctrl Pts',(43.3135644199415,29.4717116718671,-41.7392208333333));
#250077=CARTESIAN_POINT('Ctrl Pts',(44.5079524583208,29.4717116718671,-41.6808875));
#250078=CARTESIAN_POINT('Ctrl Pts',(45.7023404967,29.4717116718671,-41.6225541666667));
#250079=CARTESIAN_POINT('Ctrl Pts',(46.2995345158897,30.5060820550798,-41.5642208333334));
#250080=CARTESIAN_POINT('Ctrl Pts',(46.8967285350793,31.5404524382925,-41.5058875));
#250081=CARTESIAN_POINT('Ctrl Pts',(46.2995345158897,32.5748228215052,-41.4475541666667));
#250082=CARTESIAN_POINT('Ctrl Pts',(45.7023404967,33.6091932047179,-41.3892208333333));
#250083=CARTESIAN_POINT('Ctrl Pts',(44.5079524583208,33.6091932047179,-41.3308875));
#250084=CARTESIAN_POINT('Ctrl Pts',(43.3135644199415,33.6091932047179,-41.2725541666667));
#250085=CARTESIAN_POINT('Ctrl Pts',(42.7163704007519,32.5748228215052,-41.2142208333333));
#250086=CARTESIAN_POINT('Ctrl Pts',(42.1191763815623,31.5404524382925,-41.1558875));
#250087=CARTESIAN_POINT('Ctrl Pts',(42.7163704007519,30.5060820550798,-41.0975541666667));
#250088=CARTESIAN_POINT('Ctrl Pts',(43.3135644199415,29.4717116718671,-41.0392208333333));
#250089=CARTESIAN_POINT('Ctrl Pts',(44.5079524583208,29.4717116718671,-40.9808875));
#250090=CARTESIAN_POINT('Ctrl Pts',(45.7023404967,29.4717116718671,-40.9225541666667));
#250091=CARTESIAN_POINT('Ctrl Pts',(46.2995345158897,30.5060820550798,-40.8642208333334));
#250092=CARTESIAN_POINT('Ctrl Pts',(46.8967285350793,31.5404524382925,-40.8058875));
#250093=CARTESIAN_POINT('Ctrl Pts',(46.2995345158897,32.5748228215052,-40.7475541666667));
#250094=CARTESIAN_POINT('Ctrl Pts',(45.7023404967,33.6091932047179,-40.6892208333333));
#250095=CARTESIAN_POINT('Ctrl Pts',(44.5079524583208,33.6091932047179,-40.6308875));
#250096=CARTESIAN_POINT('Ctrl Pts',(43.3135644199415,33.6091932047179,-40.5725541666667));
#250097=CARTESIAN_POINT('Ctrl Pts',(42.7163704007519,32.5748228215052,-40.5142208333333));
#250098=CARTESIAN_POINT('Ctrl Pts',(42.1191763815623,31.5404524382925,-40.4558875));
#250099=CARTESIAN_POINT('Ctrl Pts',(42.7163704007519,30.5060820550798,-40.3975541666667));
#250100=CARTESIAN_POINT('Ctrl Pts',(43.3135644199415,29.4717116718671,-40.3392208333333));
#250101=CARTESIAN_POINT('Ctrl Pts',(44.5079524583208,29.4717116718671,-40.2808875));
#250102=CARTESIAN_POINT('Ctrl Pts',(45.7023404967,29.4717116718671,-40.2225541666667));
#250103=CARTESIAN_POINT('Ctrl Pts',(46.2995345158897,30.5060820550798,-40.1642208333333));
#250104=CARTESIAN_POINT('Ctrl Pts',(46.8967285350793,31.5404524382925,-40.1058875));
#250105=CARTESIAN_POINT('Ctrl Pts',(46.2995345158897,32.5748228215052,-40.0475541666667));
#250106=CARTESIAN_POINT('Ctrl Pts',(45.7023404967,33.6091932047179,-39.9892208333333));
#250107=CARTESIAN_POINT('Ctrl Pts',(44.5079524583208,33.6091932047179,-39.9308875));
#250108=CARTESIAN_POINT('Ctrl Pts',(43.3135644199415,33.6091932047179,-39.8725541666667));
#250109=CARTESIAN_POINT('Ctrl Pts',(42.7163704007519,32.5748228215052,-39.8142208333334));
#250110=CARTESIAN_POINT('Ctrl Pts',(42.1191763815623,31.5404524382925,-39.7558875));
#250111=CARTESIAN_POINT('Ctrl Pts',(42.7163704007519,30.5060820550798,-39.6975541666667));
#250112=CARTESIAN_POINT('Ctrl Pts',(43.3135644199415,29.4717116718671,-39.6392208333334));
#250113=CARTESIAN_POINT('Ctrl Pts',(44.5079524583208,29.4717116718671,-39.5808875));
#250114=CARTESIAN_POINT('Ctrl Pts',(45.7023404967,29.4717116718671,-39.5225541666667));
#250115=CARTESIAN_POINT('Ctrl Pts',(46.2995345158897,30.5060820550798,-39.4642208333333));
#250116=CARTESIAN_POINT('Ctrl Pts',(46.8967285350793,31.5404524382925,-39.4058875));
#250117=CARTESIAN_POINT('Ctrl Pts',(46.2995345158897,32.5748228215052,-39.3475541666667));
#250118=CARTESIAN_POINT('Ctrl Pts',(45.7023404967,33.6091932047179,-39.2892208333334));
#250119=CARTESIAN_POINT('Ctrl Pts',(44.5079524583208,33.6091932047179,-39.2308875));
#250120=CARTESIAN_POINT('Ctrl Pts',(43.3135644199415,33.6091932047179,-39.1725541666667));
#250121=CARTESIAN_POINT('Ctrl Pts',(42.7163704007519,32.5748228215052,-39.1142208333333));
#250122=CARTESIAN_POINT('Ctrl Pts',(42.1191763815623,31.5404524382925,-39.0558875));
#250123=CARTESIAN_POINT('Ctrl Pts',(42.7163704007519,30.5060820550798,-38.9975541666667));
#250124=CARTESIAN_POINT('Ctrl Pts',(43.3135644199415,29.4717116718671,-38.9392208333334));
#250125=CARTESIAN_POINT('Ctrl Pts',(44.5079524583208,29.4717116718671,-38.8808875));
#250126=CARTESIAN_POINT('Ctrl Pts',(45.7023404967,29.4717116718671,-38.8225541666667));
#250127=CARTESIAN_POINT('Ctrl Pts',(46.2995345158897,30.5060820550798,-38.7642208333333));
#250128=CARTESIAN_POINT('Ctrl Pts',(46.8967285350793,31.5404524382925,-38.7058875));
#250129=CARTESIAN_POINT('Ctrl Pts',(46.2995345158897,32.5748228215052,-38.6475541666667));
#250130=CARTESIAN_POINT('Ctrl Pts',(45.7023404967,33.6091932047179,-38.5892208333334));
#250131=CARTESIAN_POINT('Ctrl Pts',(44.5079524583208,33.6091932047179,-38.5308875));
#250132=CARTESIAN_POINT('Ctrl Pts',(43.3135644199415,33.6091932047179,-38.4725541666667));
#250133=CARTESIAN_POINT('Ctrl Pts',(42.7163704007519,32.5748228215052,-38.4142208333334));
#250134=CARTESIAN_POINT('Ctrl Pts',(42.1191763815623,31.5404524382925,-38.3558875));
#250135=CARTESIAN_POINT('Ctrl Pts',(42.7163704007519,30.5060820550798,-38.2975541666667));
#250136=CARTESIAN_POINT('Ctrl Pts',(43.3135644199415,29.4717116718671,-38.2392208333333));
#250137=CARTESIAN_POINT('Ctrl Pts',(44.5079524583208,29.4717116718671,-38.1808875));
#250138=CARTESIAN_POINT('Ctrl Pts',(45.7023404967,29.4717116718671,-38.1225541666667));
#250139=CARTESIAN_POINT('Ctrl Pts',(46.2995345158897,30.5060820550798,-38.0642208333334));
#250140=CARTESIAN_POINT('Ctrl Pts',(46.8967285350793,31.5404524382925,-38.0058875));
#250141=CARTESIAN_POINT('Ctrl Pts',(46.2995345158897,32.5748228215052,-37.9475541666667));
#250142=CARTESIAN_POINT('Ctrl Pts',(45.7023404967,33.6091932047179,-37.8892208333334));
#250143=CARTESIAN_POINT('Ctrl Pts',(44.5079524583208,33.6091932047179,-37.8308875));
#250144=CARTESIAN_POINT('Ctrl Pts',(43.3135644199415,33.6091932047179,-37.7725541666667));
#250145=CARTESIAN_POINT('Ctrl Pts',(42.7163704007519,32.5748228215052,-37.7142208333333));
#250146=CARTESIAN_POINT('Ctrl Pts',(42.1191763815623,31.5404524382925,-37.6558875));
#250147=CARTESIAN_POINT('Ctrl Pts',(42.7163704007519,30.5060820550798,-37.5975541666667));
#250148=CARTESIAN_POINT('Ctrl Pts',(43.3135644199415,29.4717116718671,-37.5392208333334));
#250149=CARTESIAN_POINT('Ctrl Pts',(44.5079524583208,29.4717116718671,-37.4808875));
#250150=CARTESIAN_POINT('Ctrl Pts',(45.7023404967,29.4717116718671,-37.4225541666667));
#250151=CARTESIAN_POINT('Ctrl Pts',(46.2995345158897,30.5060820550798,-37.3642208333333));
#250152=CARTESIAN_POINT('Ctrl Pts',(46.8967285350793,31.5404524382925,-37.3058875));
#250153=CARTESIAN_POINT('Ctrl Pts',(46.2995345158897,32.5748228215052,-37.2475541666667));
#250154=CARTESIAN_POINT('Ctrl Pts',(46.2219998538691,32.7091167954726,-37.239980655983));
#250155=CARTESIAN_POINT('Ctrl Pts',(46.1253112086366,32.8303512837246,-37.2318399189827));
#250156=CARTESIAN_POINT('Ctrl Pts',(42.546543395006,31.1494605775565,-38.993392163361));
#250157=CARTESIAN_POINT('Ctrl Pts',(42.5576587142752,31.0937006569123,-38.9901394976073));
#250158=CARTESIAN_POINT('Ctrl Pts',(42.5711087182558,31.0386518233917,-38.9869283124078));
#250159=CARTESIAN_POINT('Ctrl Pts',(42.586750690162,30.9845892824225,-38.9837746614135));
#250160=CARTESIAN_POINT('Ctrl Pts',(42.602479569683,30.9302263671454,-38.9806034885691));
#250161=CARTESIAN_POINT('Ctrl Pts',(42.6204243147379,30.8768612681174,-38.977490522151));
#250162=CARTESIAN_POINT('Ctrl Pts',(42.6403992722336,30.8247394146376,-38.9744500788686));
#250163=CARTESIAN_POINT('Ctrl Pts',(42.6606375885134,30.7719303633021,-38.9713695490206));
#250164=CARTESIAN_POINT('Ctrl Pts',(42.6829593947816,30.7203979979648,-38.968363493014));
#250165=CARTESIAN_POINT('Ctrl Pts',(42.7071386920132,30.6703548651506,-38.9654443093952));
#250166=CARTESIAN_POINT('Ctrl Pts',(42.7286485792856,30.6258365263719,-38.9628474055247));
#250167=CARTESIAN_POINT('Ctrl Pts',(42.7516276640965,30.5824962164819,-38.9603192203944));
#250168=CARTESIAN_POINT('Ctrl Pts',(42.7759016507519,30.5404524382925,-38.9578666666667));
#250169=CARTESIAN_POINT('Ctrl Pts',(42.8032592290852,30.4930677226471,-38.9551025582541));
#250170=CARTESIAN_POINT('Ctrl Pts',(42.8328663425998,30.4462838661656,-38.9522423299495));
#250171=CARTESIAN_POINT('Ctrl Pts',(42.8646979426783,30.4004021978905,-38.9492960373434));
#250172=CARTESIAN_POINT('Ctrl Pts',(42.8962082750338,30.3549836008737,-38.9463794808711));
#250173=CARTESIAN_POINT('Ctrl Pts',(42.9298985291123,30.310449779292,-38.9433786035812));
#250174=CARTESIAN_POINT('Ctrl Pts',(42.9656935238546,30.2670957569757,-38.9403058097603));
#250175=CARTESIAN_POINT('Ctrl Pts',(43.0010929508448,30.2242208366478,-38.9372669731492));
#250176=CARTESIAN_POINT('Ctrl Pts',(43.0385507803684,30.1825004955475,-38.9341578253332));
#250177=CARTESIAN_POINT('Ctrl Pts',(43.0779440423292,30.1422122201699,-38.9309926733074));
#250178=CARTESIAN_POINT('Ctrl Pts',(43.1171238614532,30.1021422370424,-38.9278446708903));
#250179=CARTESIAN_POINT('Ctrl Pts',(43.1582179876216,30.0634895370743,-38.9246413003028));
#250180=CARTESIAN_POINT('Ctrl Pts',(43.2010575102137,30.026508792424,-38.9213985239789));
#250181=CARTESIAN_POINT('Ctrl Pts',(43.2436909155241,29.9897059762402,-38.9181713498887));
#250182=CARTESIAN_POINT('Ctrl Pts',(43.2880525876963,29.9545596919455,-38.914905185536));
#250183=CARTESIAN_POINT('Ctrl Pts',(43.3339328063802,29.9212928582627,-38.9116171288744));
#250184=CARTESIAN_POINT('Ctrl Pts',(43.3596308718016,29.9026597023435,-38.9097754485681));
#250185=CARTESIAN_POINT('Ctrl Pts',(43.3858045938695,29.8846156169163,-38.9079269216165));
#250186=CARTESIAN_POINT('Ctrl Pts',(43.4124119307855,29.8671948409963,-38.9060746707971));
#250187=CARTESIAN_POINT('Origin',(44.5079524583208,31.5404524382925,235.35105));
#250188=CARTESIAN_POINT('',(44.236619467102,29.5589435596493,-39.0141960675245));
#250189=CARTESIAN_POINT('Ctrl Pts',(43.4124119245055,29.8671948319696,-38.9060746716112));
#250190=CARTESIAN_POINT('Ctrl Pts',(43.4347318263428,29.8525811285912,-38.9076953057508));
#250191=CARTESIAN_POINT('Ctrl Pts',(43.4574472657287,29.8383464180801,-38.9094785669247));
#250192=CARTESIAN_POINT('Ctrl Pts',(43.4805657277221,29.8245047392673,-38.9114288083032));
#250193=CARTESIAN_POINT('Ctrl Pts',(43.5088609654949,29.807563577987,-38.913815755304));
#250194=CARTESIAN_POINT('Ctrl Pts',(43.5377748005682,29.7912042828046,-38.9164545150156));
#250195=CARTESIAN_POINT('Ctrl Pts',(43.5672796770166,29.7754780139697,-38.919349653254));
#250196=CARTESIAN_POINT('Ctrl Pts',(43.5965174949706,29.7598940888484,-38.922218586629));
#250197=CARTESIAN_POINT('Ctrl Pts',(43.6264809533112,29.7448658896409,-38.9253559403288));
#250198=CARTESIAN_POINT('Ctrl Pts',(43.6567606170124,29.7306258031448,-38.9287240628826));
#250199=CARTESIAN_POINT('Ctrl Pts',(43.6867773203878,29.7165093830744,-38.9320629353557));
#250200=CARTESIAN_POINT('Ctrl Pts',(43.7171486731233,29.7031357677765,-38.9356311637963));
#250201=CARTESIAN_POINT('Ctrl Pts',(43.74787091788,29.6905129658013,-38.9394291519851));
#250202=CARTESIAN_POINT('Ctrl Pts',(43.7783370856922,29.6779953777707,-38.9431954830728));
#250203=CARTESIAN_POINT('Ctrl Pts',(43.8091488314015,29.6662150049623,-38.9471876300055));
#250204=CARTESIAN_POINT('Ctrl Pts',(43.8403053963098,29.655181264008,-38.9514068723595));
#250205=CARTESIAN_POINT('Ctrl Pts',(43.8712126325087,29.6442358199631,-38.9555923504569));
#250206=CARTESIAN_POINT('Ctrl Pts',(43.9024591937255,29.6340251151907,-38.96000130694));
#250207=CARTESIAN_POINT('Ctrl Pts',(43.9340457277949,29.6245633327707,-38.9646362624899));
#250208=CARTESIAN_POINT('Ctrl Pts',(43.9653895268376,29.6151742619057,-38.9692355995052));
#250209=CARTESIAN_POINT('Ctrl Pts',(43.9970680900916,29.6065226347007,-38.9740574728663));
#250210=CARTESIAN_POINT('Ctrl Pts',(44.0290834665269,29.5986273975902,-38.9791056375968));
#250211=CARTESIAN_POINT('Ctrl Pts',(44.0608625364734,29.5907904354703,-38.9841165416665));
#250212=CARTESIAN_POINT('Ctrl Pts',(44.0929734563391,29.5836987046376,-38.9893504007192));
#250213=CARTESIAN_POINT('Ctrl Pts',(44.1254197237287,29.5773761007637,-38.9948122462768));
#250214=CARTESIAN_POINT('Ctrl Pts',(44.1576359403445,29.5710983254643,-39.000235366215));
#250215=CARTESIAN_POINT('Ctrl Pts',(44.1901665881168,29.5655813086992,-39.0058803943283));
#250216=CARTESIAN_POINT('Ctrl Pts',(44.2230652009806,29.5608466061619,-39.0117622591756));
#250217=CARTESIAN_POINT('Ctrl Pts',(44.2275783635669,29.5601970808328,-39.012569156794));
#250218=CARTESIAN_POINT('Ctrl Pts',(44.2320969536309,29.5595625845471,-39.0133802622792));
#250219=CARTESIAN_POINT('Ctrl Pts',(44.2366193326589,29.5589433410896,-39.0141952785063));
#250220=CARTESIAN_POINT('',(42.5996219947327,32.1390102378578,-39.2098645096971));
#250221=CARTESIAN_POINT('Ctrl Pts',(44.2366191251681,29.5589433654202,-39.0141965786228));
#250222=CARTESIAN_POINT('Ctrl Pts',(44.1816176782784,29.566474982975,-39.0171948894326));
#250223=CARTESIAN_POINT('Ctrl Pts',(44.1264789676119,29.5763621734674,-39.0202688267391));
#250224=CARTESIAN_POINT('Ctrl Pts',(44.0715029830857,29.588655665456,-39.0234047166939));
#250225=CARTESIAN_POINT('Ctrl Pts',(44.0169261942809,29.6008598910231,-39.0265178360905));
#250226=CARTESIAN_POINT('Ctrl Pts',(43.9625104680952,29.6154358140615,-39.0296919830407));
#250227=CARTESIAN_POINT('Ctrl Pts',(43.9085612350477,29.6323831987791,-39.0329117223836));
#250228=CARTESIAN_POINT('Ctrl Pts',(43.8548976765229,29.6492408429061,-39.0361144124109));
#250229=CARTESIAN_POINT('Ctrl Pts',(43.8016964116104,29.6684449522924,-39.039362178014));
#250230=CARTESIAN_POINT('Ctrl Pts',(43.7492592823951,29.6899437547989,-39.042638262187));
#250231=CARTESIAN_POINT('Ctrl Pts',(43.6969935738813,29.7113722761924,-39.045903636608));
#250232=CARTESIAN_POINT('Ctrl Pts',(43.6454877381092,29.7350803961258,-39.0491971047438));
#250233=CARTESIAN_POINT('Ctrl Pts',(43.595031006667,29.7609659628588,-39.0525010772784));
#250234=CARTESIAN_POINT('Ctrl Pts',(43.5446056724429,29.7868354220326,-39.0558029938822));
#250235=CARTESIAN_POINT('Ctrl Pts',(43.4952288227897,29.8148793433641,-39.0591153591484));
#250236=CARTESIAN_POINT('Ctrl Pts',(43.4471688705001,29.8449477707636,-39.0624202412502));
#250237=CARTESIAN_POINT('Ctrl Pts',(43.3990553382291,29.8750497201644,-39.0657288078234));
#250238=CARTESIAN_POINT('Ctrl Pts',(43.352262246232,29.9071802631789,-39.0690298314617));
#250239=CARTESIAN_POINT('Ctrl Pts',(43.3070288337395,29.9411461158919,-39.072305590473));
#250240=CARTESIAN_POINT('Ctrl Pts',(43.2616662391463,29.9752089716821,-39.0755907047243));
#250241=CARTESIAN_POINT('Ctrl Pts',(43.217872734279,30.011117076979,-39.0788503688593));
#250242=CARTESIAN_POINT('Ctrl Pts',(43.1758511046526,30.0486398807422,-39.0820676158819));
#250243=CARTESIAN_POINT('Ctrl Pts',(43.1334566861023,30.0864955627341,-39.0853134042549));
#250244=CARTESIAN_POINT('Ctrl Pts',(43.0928661024029,30.1259940743276,-39.0885159814558));
#250245=CARTESIAN_POINT('Ctrl Pts',(43.0542417580791,30.1668715695527,-39.0916594494718));
#250246=CARTESIAN_POINT('Ctrl Pts',(43.0153972412906,30.2079820810018,-39.0948208363708));
#250247=CARTESIAN_POINT('Ctrl Pts',(42.9785416250927,30.2504866150729,-39.097922407934));
#250248=CARTESIAN_POINT('Ctrl Pts',(42.9437897138948,30.2940999455835,-39.1009500473225));
#250249=CARTESIAN_POINT('Ctrl Pts',(42.9085853984175,30.3382810393245,-39.1040171008602));
#250250=CARTESIAN_POINT('Ctrl Pts',(42.8755399737454,30.3835992377108,-39.1070082600792));
#250251=CARTESIAN_POINT('Ctrl Pts',(42.844719305314,30.4297520295712,-39.109911376434));
#250252=CARTESIAN_POINT('Ctrl Pts',(42.8203919250237,30.4661813666424,-39.1122028652039));
#250253=CARTESIAN_POINT('Ctrl Pts',(42.7974495117931,30.5031304481747,-39.1144395505765));
#250254=CARTESIAN_POINT('Ctrl Pts',(42.7759016507519,30.5404524382925,-39.1166166666667));
#250255=CARTESIAN_POINT('Ctrl Pts',(42.7485193766326,30.587879928294,-39.1193832702501));
#250256=CARTESIAN_POINT('Ctrl Pts',(42.7227852103423,30.636958193604,-39.1222461931116));
#250257=CARTESIAN_POINT('Ctrl Pts',(42.6989482557022,30.6875143844291,-39.1251953452699));
#250258=CARTESIAN_POINT('Ctrl Pts',(42.6753689155071,30.7375241965227,-39.128112624892));
#250259=CARTESIAN_POINT('Ctrl Pts',(42.6536466666086,30.7889798985313,-39.1311142647052));
#250260=CARTESIAN_POINT('Ctrl Pts',(42.6339995109737,30.8416687077707,-39.1341878453422));
#250261=CARTESIAN_POINT('Ctrl Pts',(42.6145810606266,30.8937441860271,-39.1372256475614));
#250262=CARTESIAN_POINT('Ctrl Pts',(42.5971902480339,30.9470238046399,-39.1403337006506));
#250263=CARTESIAN_POINT('Ctrl Pts',(42.5820056476045,31.0012625948999,-39.143497707743));
#250264=CARTESIAN_POINT('Ctrl Pts',(42.5669082682819,31.0551898348266,-39.1466435406198));
#250265=CARTESIAN_POINT('Ctrl Pts',(42.5539923214714,31.1100647309391,-39.1498446557392));
#250266=CARTESIAN_POINT('Ctrl Pts',(42.5433935917014,31.1656142631698,-39.1530851197771));
#250267=CARTESIAN_POINT('Ctrl Pts',(42.5328373585439,31.2209410642817,-39.156312590867));
#250268=CARTESIAN_POINT('Ctrl Pts',(42.5245801588322,31.2769364683933,-39.159579058983));
#250269=CARTESIAN_POINT('Ctrl Pts',(42.5187102065973,31.3333073354667,-39.1628674169599));
#250270=CARTESIAN_POINT('Ctrl Pts',(42.5128535965813,31.3895500733124,-39.1661483006014));
#250271=CARTESIAN_POINT('Ctrl Pts',(42.5093736002375,31.4461658639795,-39.1694509335672));
#250272=CARTESIAN_POINT('Ctrl Pts',(42.5083077219769,31.502850275984,-39.172757549812));
#250273=CARTESIAN_POINT('Ctrl Pts',(42.5072408681143,31.5595865714247,-39.1760671926139));
#250274=CARTESIAN_POINT('Ctrl Pts',(42.5085926033184,31.6163908743015,-39.1793807828468));
#250275=CARTESIAN_POINT('Ctrl Pts',(42.512348305768,31.6729554658862,-39.1826803624361));
#250276=CARTESIAN_POINT('Ctrl Pts',(42.51610881692,31.7295924812843,-39.1859841667201));
#250277=CARTESIAN_POINT('Ctrl Pts',(42.522279319495,31.785988440723,-39.1892738818491));
#250278=CARTESIAN_POINT('Ctrl Pts',(42.5307934391592,31.841843081299,-39.1925319844119));
#250279=CARTESIAN_POINT('Ctrl Pts',(42.5393585830543,31.8980324529088,-39.1958096124435));
#250280=CARTESIAN_POINT('Ctrl Pts',(42.5502952384567,31.9536733046506,-39.1990552074192));
#250281=CARTESIAN_POINT('Ctrl Pts',(42.5634866283946,32.0084794812234,-39.202252068528));
#250282=CARTESIAN_POINT('Ctrl Pts',(42.5740999898522,32.0525747406936,-39.2048241585532));
#250283=CARTESIAN_POINT('Ctrl Pts',(42.5861718501526,32.0961299612849,-39.2073647175113));
#250284=CARTESIAN_POINT('Ctrl Pts',(42.5996208651864,32.1390094796345,-39.2098658272488));
#250285=CARTESIAN_POINT('Ctrl Pts',(42.5996211287169,32.1390103205417,-39.2098620634844));
#250286=CARTESIAN_POINT('Ctrl Pts',(42.5994572744447,32.1384879169033,-39.2097205819177));
#250287=CARTESIAN_POINT('Ctrl Pts',(42.5992936549467,32.1379655109967,-39.2095791463362));
#250288=CARTESIAN_POINT('Ctrl Pts',(42.599130270052,32.1374431028809,-39.2094377567205));
#250289=CARTESIAN_POINT('Ctrl Pts',(42.5893329175536,32.1061169728464,-39.2009593480741));
#250290=CARTESIAN_POINT('Ctrl Pts',(42.5803770676735,32.0747718601698,-39.1926435115987));
#250291=CARTESIAN_POINT('Ctrl Pts',(42.5722375892794,32.0434514998719,-39.184494909014));
#250292=CARTESIAN_POINT('Ctrl Pts',(42.563947246632,32.0115506204622,-39.1761952730602));
#250293=CARTESIAN_POINT('Ctrl Pts',(42.5564828395702,31.97956241044,-39.1680413954435));
#250294=CARTESIAN_POINT('Ctrl Pts',(42.5498886395242,31.9478668123839,-39.1601218550228));
#250295=CARTESIAN_POINT('Ctrl Pts',(42.5431680501022,31.9155637127605,-39.15205052276));
#250296=CARTESIAN_POINT('Ctrl Pts',(42.5373266000632,31.8834870424314,-39.1442015176493));
#250297=CARTESIAN_POINT('Ctrl Pts',(42.5323124691512,31.8516556037808,-39.1365690002841));
#250298=CARTESIAN_POINT('Ctrl Pts',(42.5271988370559,31.8191924971763,-39.128785022073));
#250299=CARTESIAN_POINT('Ctrl Pts',(42.5229439406764,31.7869791989586,-39.1212247661578));
#250300=CARTESIAN_POINT('Ctrl Pts',(42.5194951584437,31.7550189050201,-39.1138789650356));
#250301=CARTESIAN_POINT('Ctrl Pts',(42.5123805250403,31.6890867122931,-39.0987250125639));
#250302=CARTESIAN_POINT('Ctrl Pts',(42.508690420396,31.6242317713433,-39.0844826612156));
#250303=CARTESIAN_POINT('Ctrl Pts',(42.5080522085159,31.5604742687753,-39.0710861007614));
#250304=CARTESIAN_POINT('Ctrl Pts',(42.5077225703561,31.527543346495,-39.0641667411037));
#250305=CARTESIAN_POINT('Ctrl Pts',(42.5082086866532,31.4949050545532,-39.0574732885357));
#250306=CARTESIAN_POINT('Ctrl Pts',(42.5094692953678,31.4625612862931,-39.050998430158));
#250307=CARTESIAN_POINT('Ctrl Pts',(42.5107590556556,31.4294695684798,-39.0443738406978));
#250308=CARTESIAN_POINT('Ctrl Pts',(42.5128605944209,31.3966833301453,-39.0379776981527));
#250309=CARTESIAN_POINT('Ctrl Pts',(42.5157322592149,31.364212570118,-39.0318042712848));
#250310=CARTESIAN_POINT('Ctrl Pts',(42.518470838614,31.3332466458677,-39.0259169477791));
#250311=CARTESIAN_POINT('Ctrl Pts',(42.5219235433117,31.3025110976608,-39.0202232095696));
#250312=CARTESIAN_POINT('Ctrl Pts',(42.5259998070332,31.2723751844448,-39.0147819750659));
#250313=CARTESIAN_POINT('Ctrl Pts',(42.5263010222903,31.2701482929905,-39.0143798953768));
#250314=CARTESIAN_POINT('Ctrl Pts',(42.5266056457019,31.2679246529169,-39.013979190334));
#250315=CARTESIAN_POINT('Ctrl Pts',(42.5269136422624,31.2657044023431,-39.0135798817453));
#250316=CARTESIAN_POINT('Ctrl Pts',(42.5315025550251,31.2326243699617,-39.007630489726));
#250317=CARTESIAN_POINT('Ctrl Pts',(42.5368513500173,31.2001397627821,-39.0019606799009));
#250318=CARTESIAN_POINT('Ctrl Pts',(42.5428860222013,31.1682775284555,-38.9965615346981));
#250319=CARTESIAN_POINT('Ctrl Pts',(42.5440784696113,31.1619815710881,-38.9954946670181));
#250320=CARTESIAN_POINT('Ctrl Pts',(42.5452977554539,31.1557093015287,-38.9944382514666));
#250321=CARTESIAN_POINT('Ctrl Pts',(42.5465433949858,31.149460577658,-38.9933921633669));
#250322=CARTESIAN_POINT('Ctrl Pts',(46.6981266849492,30.7091523375488,-39.2904704603133));
#250323=CARTESIAN_POINT('Ctrl Pts',(46.6689684123063,30.6404043382273,-39.273452295095));
#250324=CARTESIAN_POINT('Ctrl Pts',(46.6043681216411,30.5066861069553,-39.238925705885));
#250325=CARTESIAN_POINT('Ctrl Pts',(46.5083209189471,30.3487389562033,-39.1945593129175));
#250326=CARTESIAN_POINT('Ctrl Pts',(46.4437937583117,30.2581216171786,-39.1673894861782));
#250327=CARTESIAN_POINT('Ctrl Pts',(46.3992224148768,30.1986447451181,-39.1491520227249));
#250328=CARTESIAN_POINT('Ctrl Pts',(46.3761748773305,30.1693908446446,-39.1399767764946));
#250329=CARTESIAN_POINT('Ctrl Pts',(46.3284414024809,30.1117648114071,-39.1214771434543));
#250330=CARTESIAN_POINT('Ctrl Pts',(46.3038983378397,30.083571828401,-39.112209259666));
#250331=CARTESIAN_POINT('Ctrl Pts',(46.253707387608,30.0286632749651,-39.0937226519629));
#250332=CARTESIAN_POINT('Ctrl Pts',(46.2280147026909,30.001893564456,-39.0844865568113));
#250333=CARTESIAN_POINT('Ctrl Pts',(46.1492148010453,29.9236586721517,-39.0568159196779));
#250334=CARTESIAN_POINT('Ctrl Pts',(46.0669347173688,29.8495134741745,-39.0292038481275));
#250335=CARTESIAN_POINT('Ctrl Pts',(45.9503410384262,29.7587889734315,-38.9925114043613));
#250336=CARTESIAN_POINT('Ctrl Pts',(45.8594191065401,29.6948377475824,-38.9650526418885));
#250337=CARTESIAN_POINT('Ctrl Pts',(45.7964751089327,29.6549785818455,-38.9467936623891));
#250338=CARTESIAN_POINT('Ctrl Pts',(45.748348603817,29.6261284949947,-38.9331097524421));
#250339=CARTESIAN_POINT('Ctrl Pts',(45.7321473284057,29.616684052073,-38.9285487676403));
#250340=CARTESIAN_POINT('Ctrl Pts',(45.6996106203311,29.5982459977232,-38.9194791520014));
#250341=CARTESIAN_POINT('Ctrl Pts',(45.683249044345,29.5892352448745,-38.9149628379356));
#250342=CARTESIAN_POINT('Ctrl Pts',(45.6010439155842,29.5452684013657,-38.8924942188443));
#250343=CARTESIAN_POINT('Ctrl Pts',(45.4667739830181,29.4816584171599,-38.8571935516581));
#250344=CARTESIAN_POINT('Ctrl Pts',(45.2922645146651,29.4187721922835,-38.8147007629208));
#250345=CARTESIAN_POINT('Ctrl Pts',(45.184512437616,29.3885937253944,-38.7899522655792));
#250346=CARTESIAN_POINT('Ctrl Pts',(45.1119891467798,29.3701842541612,-38.7736235920333));
#250347=CARTESIAN_POINT('Ctrl Pts',(45.0754052578815,29.3618381514785,-38.7655490803555));
#250348=CARTESIAN_POINT('Ctrl Pts',(45.0014447932705,29.3468760834356,-38.7495561846596));
#250349=CARTESIAN_POINT('Ctrl Pts',(44.964301863367,29.3403115562353,-38.7416890516424));
#250350=CARTESIAN_POINT('Ctrl Pts',(44.8900079594565,29.3290481892184,-38.726277749838));
#250351=CARTESIAN_POINT('Ctrl Pts',(44.8527936282157,29.324336495618,-38.7187198739728));
#250352=CARTESIAN_POINT('Ctrl Pts',(44.7410083373266,29.3129455735289,-38.6964994820139));
#250353=CARTESIAN_POINT('Ctrl Pts',(44.6662563757167,29.3089967422249,-38.6822807693139));
#250354=CARTESIAN_POINT('Ctrl Pts',(44.516312468428,29.3084067934202,-38.6550493453909));
#250355=CARTESIAN_POINT('Ctrl Pts',(44.441103189525,29.3117700143417,-38.6420342479066));
#250356=CARTESIAN_POINT('Ctrl Pts',(44.3468378615956,29.3206690055189,-38.6265520162729));
#250357=CARTESIAN_POINT('Ctrl Pts',(44.3279589148655,29.3226883315868,-38.6234933649988));
#250358=CARTESIAN_POINT('Ctrl Pts',(44.2901960653062,29.3271995080042,-38.6174591262491));
#250359=CARTESIAN_POINT('Ctrl Pts',(44.271274393292,29.329697893027,-38.614477863833));
#250360=CARTESIAN_POINT('Ctrl Pts',(44.2146592782019,29.3378915995821,-38.60568558559));
#250361=CARTESIAN_POINT('Ctrl Pts',(44.1772069502033,29.344266758826,-38.6000392683017));
#250362=CARTESIAN_POINT('Ctrl Pts',(44.0655444875092,29.3661148598052,-38.5837127379559));
#250363=CARTESIAN_POINT('Ctrl Pts',(43.9553791862171,29.3933792052515,-38.5686255047386));
#250364=CARTESIAN_POINT('Ctrl Pts',(43.8114622524781,29.4404829778103,-38.5509833019505));
#250365=CARTESIAN_POINT('Ctrl Pts',(43.705021834675,29.481230340464,-38.5390021142185));
#250366=CARTESIAN_POINT('Ctrl Pts',(43.6350719757086,29.512061063653,-38.5318621614261));
#250367=CARTESIAN_POINT('Ctrl Pts',(43.5656410085295,29.5447591316771,-38.525155654825));
#250368=CARTESIAN_POINT('Ctrl Pts',(43.5311320054746,29.5620794464364,-38.5220163122062));
#250369=CARTESIAN_POINT('Ctrl Pts',(43.4634866412134,29.5981758355574,-38.5162526847879));
#250370=CARTESIAN_POINT('Ctrl Pts',(43.4301834663392,29.6170276546,-38.5136117755133));
#250371=CARTESIAN_POINT('Ctrl Pts',(43.3647025891651,29.6562685687332,-38.5088155315793));
#250372=CARTESIAN_POINT('Ctrl Pts',(43.2681192378476,29.7174608121974,-38.5023448938576));
#250373=CARTESIAN_POINT('Ctrl Pts',(43.1764049274077,29.7855824582168,-38.4980286134812));
#250374=CARTESIAN_POINT('Ctrl Pts',(43.0584774180437,29.8826126224142,-38.4942050936184));
#250375=CARTESIAN_POINT('Ctrl Pts',(43.001681818637,29.9342392650769,-38.4932590761897));
#250376=CARTESIAN_POINT('Ctrl Pts',(42.8926599718677,30.0438904492243,-38.4933742455196));
#250377=CARTESIAN_POINT('Ctrl Pts',(42.8414047150844,30.1009342501745,-38.4944336470273));
#250378=CARTESIAN_POINT('Ctrl Pts',(42.7451036203247,30.2193471227021,-38.498479276642));
#250379=CARTESIAN_POINT('Ctrl Pts',(42.6550322643363,30.3420646399833,-38.5044516702661));
#250380=CARTESIAN_POINT('Ctrl Pts',(42.5773225406025,30.4733365238586,-38.5142428327574));
#250381=CARTESIAN_POINT('Ctrl Pts',(42.5326943378214,30.5580963840027,-38.5215739479982));
#250382=CARTESIAN_POINT('Ctrl Pts',(42.5239673850246,30.5751883092729,-38.5231018165939));
#250383=CARTESIAN_POINT('Ctrl Pts',(42.5069121510755,30.60964376351,-38.5262794637242));
#250384=CARTESIAN_POINT('Ctrl Pts',(42.4985805781952,30.627019094627,-38.5279307934181));
#250385=CARTESIAN_POINT('Ctrl Pts',(42.4743295471271,30.6792614198295,-38.5330409224498));
#250386=CARTESIAN_POINT('Ctrl Pts',(42.4438856226513,30.7493896366731,-38.5402834483744));
#250387=CARTESIAN_POINT('Ctrl Pts',(42.4037483179465,30.8560072598611,-38.5524071291592));
#250388=CARTESIAN_POINT('Ctrl Pts',(42.3690543371876,30.9640160484273,-38.5657659376104));
#250389=CARTESIAN_POINT('Ctrl Pts',(42.3397558527982,31.0734075527136,-38.5803463747351));
#250390=CARTESIAN_POINT('Ctrl Pts',(42.3238156343608,31.1472555030051,-38.5908775753381));
#250391=CARTESIAN_POINT('Ctrl Pts',(42.3096820427396,31.2215665449467,-38.6018154236264));
#250392=CARTESIAN_POINT('Ctrl Pts',(42.3035171869091,31.2589715314082,-38.6074906718877));
#250393=CARTESIAN_POINT('Ctrl Pts',(42.2930235524414,31.3341791410138,-38.6192399292287));
#250394=CARTESIAN_POINT('Ctrl Pts',(42.2886818075092,31.3721585359098,-38.6253436316658));
#250395=CARTESIAN_POINT('Ctrl Pts',(42.281930630611,31.4478003630713,-38.6378362101326));
#250396=CARTESIAN_POINT('Ctrl Pts',(42.277074994566,31.5232809912004,-38.6506356205751));
#250397=CARTESIAN_POINT('Ctrl Pts',(42.2747992363309,31.6735553614761,-38.6774229397946));
#250398=CARTESIAN_POINT('Ctrl Pts',(42.2834818483937,31.8228397562226,-38.7059581415094));
#250399=CARTESIAN_POINT('Ctrl Pts',(42.3030248127084,31.9711385758679,-38.7362097844166));
#250400=CARTESIAN_POINT('Ctrl Pts',(42.3164494406915,32.0449687602614,-38.7519128032936));
#250401=CARTESIAN_POINT('Ctrl Pts',(42.3317154579634,32.1186122141692,-38.7679009120377));
#250402=CARTESIAN_POINT('Ctrl Pts',(42.3402956643805,32.1554227583218,-38.7760569897633));
#250403=CARTESIAN_POINT('Ctrl Pts',(42.3591481714288,32.228169160774,-38.7925026060078));
#250404=CARTESIAN_POINT('Ctrl Pts',(42.3694448348212,32.2642362896146,-38.8008201507359));
#250405=CARTESIAN_POINT('Ctrl Pts',(42.4028917825415,32.3714169561226,-38.8260275044574));
#250406=CARTESIAN_POINT('Ctrl Pts',(42.428602574983,32.4415633880281,-38.8431823298655));
#250407=CARTESIAN_POINT('Ctrl Pts',(42.4722685042023,32.5448307979217,-38.8694323201497));
#250408=CARTESIAN_POINT('Ctrl Pts',(42.4876674804306,32.5789105800712,-38.8782643966373));
#250409=CARTESIAN_POINT('Ctrl Pts',(42.5202146590728,32.6464795812123,-38.8961197808447));
#250410=CARTESIAN_POINT('Ctrl Pts',(42.5373018269229,32.6798350022668,-38.9051083126545));
#250411=CARTESIAN_POINT('Ctrl Pts',(42.5906929412925,32.7780783962456,-38.9321048428364));
#250412=CARTESIAN_POINT('Ctrl Pts',(42.629225789877,32.8414173722334,-38.9502105255135));
#250413=CARTESIAN_POINT('Ctrl Pts',(42.7120000069194,32.9638220552461,-38.9866125955294));
#250414=CARTESIAN_POINT('Ctrl Pts',(42.7783647966162,33.0524402968179,-39.0140612314234));
#250415=CARTESIAN_POINT('Ctrl Pts',(42.8754380724448,33.1642175243331,-39.0509520337677));
#250416=CARTESIAN_POINT('Ctrl Pts',(42.9268673384212,33.2179450225078,-39.0694937486382));
#250417=CARTESIAN_POINT('Ctrl Pts',(42.9797817061918,33.2705900457306,-39.088089881442));
#250418=CARTESIAN_POINT('Ctrl Pts',(43.0069972096607,33.2963736994336,-39.097418269769));
#250419=CARTESIAN_POINT('Ctrl Pts',(43.0622936398443,33.3462615369726,-39.1159154063528));
#250420=CARTESIAN_POINT('Ctrl Pts',(43.0904949946047,33.3704876748183,-39.1251268688783));
#250421=CARTESIAN_POINT('Ctrl Pts',(43.176562606447,33.4408730143712,-39.1525915568785));
#250422=CARTESIAN_POINT('Ctrl Pts',(43.2360245534179,33.4848790444095,-39.1707230137558));
#250423=CARTESIAN_POINT('Ctrl Pts',(43.358992255749,33.5670176609587,-39.2066046432507));
#250424=CARTESIAN_POINT('Ctrl Pts',(43.4542745623933,33.6242424638975,-39.233238623837));
#250425=CARTESIAN_POINT('Ctrl Pts',(43.5542222374601,33.6747516510336,-39.2594493821381));
#250426=CARTESIAN_POINT('Ctrl Pts',(43.6219256430316,33.7069073870393,-39.2768314299875));
#250427=CARTESIAN_POINT('Ctrl Pts',(43.6563381479934,33.7222286468184,-39.2854811722856));
#250428=CARTESIAN_POINT('Ctrl Pts',(43.7254519170511,33.7509934760635,-39.3024907499371));
#250429=CARTESIAN_POINT('Ctrl Pts',(43.7602995448845,33.7645084608315,-39.3108885064059));
#250430=CARTESIAN_POINT('Ctrl Pts',(43.8304781084082,33.789780836939,-39.3274499785309));
#250431=CARTESIAN_POINT('Ctrl Pts',(43.9365171946568,33.8250735562425,-39.3519527568515));
#250432=CARTESIAN_POINT('Ctrl Pts',(44.0809642638621,33.8617420360433,-39.3832806139221));
#250433=CARTESIAN_POINT('Ctrl Pts',(44.1916183723467,33.8813683146414,-39.4057679385072));
#250434=CARTESIAN_POINT('Ctrl Pts',(44.2659122959159,33.8926702964892,-39.4205323411483));
#250435=CARTESIAN_POINT('Ctrl Pts',(44.3033049221432,33.8974288658374,-39.4277978831022));
#250436=CARTESIAN_POINT('Ctrl Pts',(44.3598453576919,33.9032050944765,-39.4385322478049));
#250437=CARTESIAN_POINT('Ctrl Pts',(44.3787527158677,33.9049006163346,-39.4420799976889));
#250438=CARTESIAN_POINT('Ctrl Pts',(44.4164967874688,33.9078161173588,-39.4490791780208));
#250439=CARTESIAN_POINT('Ctrl Pts',(44.4353708468856,33.9090400957878,-39.4525377314439));
#250440=CARTESIAN_POINT('Ctrl Pts',(44.4919347179527,33.9120095261765,-39.462779235967));
#250441=CARTESIAN_POINT('Ctrl Pts',(44.52962054914,33.9130584408517,-39.4694384189012));
#250442=CARTESIAN_POINT('Ctrl Pts',(44.6425299001817,33.9134342925821,-39.4889026473125));
#250443=CARTESIAN_POINT('Ctrl Pts',(44.7176656228988,33.9100023852834,-39.5012068570978));
#250444=CARTESIAN_POINT('Ctrl Pts',(44.867623327666,33.8957625538083,-39.524471978366));
#250445=CARTESIAN_POINT('Ctrl Pts',(44.9424659600731,33.8849485744664,-39.5354353652432));
#250446=CARTESIAN_POINT('Ctrl Pts',(45.0357885152669,33.8666999843662,-39.5482785606344));
#250447=CARTESIAN_POINT('Ctrl Pts',(45.0544546343785,33.8628074782943,-39.5508053225112));
#250448=CARTESIAN_POINT('Ctrl Pts',(45.091743102575,33.8545484160302,-39.5557691634051));
#250449=CARTESIAN_POINT('Ctrl Pts',(45.1104022544846,33.850171655015,-39.5582107864407));
#250450=CARTESIAN_POINT('Ctrl Pts',(45.1661672125598,33.8363538303533,-39.5653802281989));
#250451=CARTESIAN_POINT('Ctrl Pts',(45.2029511118778,33.8262578362557,-39.5699395109212));
#250452=CARTESIAN_POINT('Ctrl Pts',(45.312316831343,33.7933159380614,-39.582990524906));
#250453=CARTESIAN_POINT('Ctrl Pts',(45.4195983160475,33.7551076509549,-39.5947758536238));
#250454=CARTESIAN_POINT('Ctrl Pts',(45.5585113890164,33.6937328563153,-39.6079933748399));
#250455=CARTESIAN_POINT('Ctrl Pts',(45.6606150024606,33.6424505696195,-39.6166516297843));
#250456=CARTESIAN_POINT('Ctrl Pts',(45.7272860947277,33.6047101271221,-39.6215780075552));
#250457=CARTESIAN_POINT('Ctrl Pts',(45.7932287365117,33.5651705839516,-39.6260731428005));
#250458=CARTESIAN_POINT('Ctrl Pts',(45.8259059249178,33.5444453395394,-39.6281074988013));
#250459=CARTESIAN_POINT('Ctrl Pts',(45.8897275017006,33.5016881508368,-39.6316923737189));
#250460=CARTESIAN_POINT('Ctrl Pts',(45.9210297733036,33.4795651380848,-39.6332542688506));
#250461=CARTESIAN_POINT('Ctrl Pts',(45.9823424846244,33.4339088874735,-39.6359180193303));
#250462=CARTESIAN_POINT('Ctrl Pts',(46.0724202597563,33.3632801300718,-39.6392265347984));
#250463=CARTESIAN_POINT('Ctrl Pts',(46.1850394564173,33.2606222983665,-39.6409205727319));
#250464=CARTESIAN_POINT('Ctrl Pts',(46.2638636333332,33.1772336958075,-39.6401443034625));
#250465=CARTESIAN_POINT('Ctrl Pts',(46.3151397511292,33.1201974856456,-39.6391646017005));
#250466=CARTESIAN_POINT('Ctrl Pts',(46.3401349353408,33.0909661742941,-39.6384440851485));
#250467=CARTESIAN_POINT('Ctrl Pts',(46.3888523044997,33.0309971480077,-39.6365301000439));
#250468=CARTESIAN_POINT('Ctrl Pts',(46.4123735341802,33.0005036828642,-39.6353439924849));
#250469=CARTESIAN_POINT('Ctrl Pts',(46.4576879006691,32.9386388625828,-39.6325280276393));
#250470=CARTESIAN_POINT('Ctrl Pts',(46.52311576659,32.8444620833496,-39.6276360146217));
#250471=CARTESIAN_POINT('Ctrl Pts',(46.5810426872604,32.7462345994881,-39.6207752343847));
#250472=CARTESIAN_POINT('Ctrl Pts',(46.6516918187307,32.6117039458857,-39.6098936921283));
#250473=CARTESIAN_POINT('Ctrl Pts',(46.683723185051,32.5426422373878,-39.6035832967262));
#250474=CARTESIAN_POINT('Ctrl Pts',(46.7195635412788,32.4540883209461,-39.5945936116187));
#250475=CARTESIAN_POINT('Ctrl Pts',(46.7265235775841,32.4362514419463,-39.5927383889278));
#250476=CARTESIAN_POINT('Ctrl Pts',(46.7400123459627,32.4003742100513,-39.5889189813535));
#250477=CARTESIAN_POINT('Ctrl Pts',(46.7465535157541,32.3822946053341,-39.5869502184844));
#250478=CARTESIAN_POINT('Ctrl Pts',(46.7654644360989,32.3279072933142,-39.5808958427402));
#250479=CARTESIAN_POINT('Ctrl Pts',(46.7770937339888,32.2915493874551,-39.5766741707955));
#250480=CARTESIAN_POINT('Ctrl Pts',(46.8091770518909,32.182013131159,-39.5634457571489));
#250481=CARTESIAN_POINT('Ctrl Pts',(46.8444383818759,32.034891308334,-39.5443264312115));
#250482=CARTESIAN_POINT('Ctrl Pts',(46.8650708643864,31.8856621776612,-39.5223044891954));
#250483=CARTESIAN_POINT('Ctrl Pts',(46.8750487417844,31.7729724844591,-39.50469487268));
#250484=CARTESIAN_POINT('Ctrl Pts',(46.8774570362353,31.7352651712118,-39.4986397605723));
#250485=CARTESIAN_POINT('Ctrl Pts',(46.8796767940079,31.6785286095959,-39.4892824810203));
#250486=CARTESIAN_POINT('Ctrl Pts',(46.8801843407089,31.6595724593507,-39.4861150486293));
#250487=CARTESIAN_POINT('Ctrl Pts',(46.8807312344332,31.6216180949417,-39.479690628598));
#250488=CARTESIAN_POINT('Ctrl Pts',(46.8807699646674,31.6025797052015,-39.4764266299692));
#250489=CARTESIAN_POINT('Ctrl Pts',(46.8801790388754,31.5455906639181,-39.4665317368708));
#250490=CARTESIAN_POINT('Ctrl Pts',(46.8788490796135,31.5078273383739,-39.4598096545541));
#250491=CARTESIAN_POINT('Ctrl Pts',(46.874360617844,31.4326451774338,-39.4461013696832));
#250492=CARTESIAN_POINT('Ctrl Pts',(46.864884835636,31.320441459725,-39.4251517854185));
#250493=CARTESIAN_POINT('Ctrl Pts',(46.8414902947658,31.1730719473388,-39.3956936109857));
#250494=CARTESIAN_POINT('Ctrl Pts',(46.8074810934279,31.0279105813681,-39.364717848004));
#250495=CARTESIAN_POINT('Ctrl Pts',(46.7869180083019,30.9560697433081,-39.3487190247537));
#250496=CARTESIAN_POINT('Ctrl Pts',(46.7645577771926,30.884604709384,-39.332461491893));
#250497=CARTESIAN_POINT('Ctrl Pts',(46.7524740339114,30.8490466969583,-39.3242001683612));
#250498=CARTESIAN_POINT('Ctrl Pts',(46.7264943673172,30.7783632715819,-39.3074248425479));
#250499=CARTESIAN_POINT('Ctrl Pts',(46.7127058212706,30.7435263372096,-39.2989795429224));
#250500=CARTESIAN_POINT('Ctrl Pts',(46.6981266849492,30.7091523375488,-39.2904704603133));
#250501=CARTESIAN_POINT('Ctrl Pts',(44.7926621173534,30.9780510210195,-41.4731170634489));
#250502=CARTESIAN_POINT('Ctrl Pts',(44.7841183378731,30.958431594105,-41.4560988982307));
#250503=CARTESIAN_POINT('Ctrl Pts',(44.7652574387158,30.9202429989855,-41.4215723090211));
#250504=CARTESIAN_POINT('Ctrl Pts',(44.7373647422364,30.8750641226134,-41.3772059160528));
#250505=CARTESIAN_POINT('Ctrl Pts',(44.7186826069414,30.8491098680677,-41.3500360893141));
#250506=CARTESIAN_POINT('Ctrl Pts',(44.7057896374646,30.8320666178198,-41.3317986258606));
#250507=CARTESIAN_POINT('Ctrl Pts',(44.6991283043737,30.8236797190306,-41.3226233796301));
#250508=CARTESIAN_POINT('Ctrl Pts',(44.6853430526266,30.8071501195218,-41.3041237465898));
#250509=CARTESIAN_POINT('Ctrl Pts',(44.6782604199269,30.7990587859436,-41.2948558628018));
#250510=CARTESIAN_POINT('Ctrl Pts',(44.6637865272211,30.7832912649286,-41.2763692550984));
#250511=CARTESIAN_POINT('Ctrl Pts',(44.65638232911,30.7755995480316,-41.2671331599469));
#250512=CARTESIAN_POINT('Ctrl Pts',(44.6336879630273,30.7531065345255,-41.2394625228135));
#250513=CARTESIAN_POINT('Ctrl Pts',(44.6100194582072,30.7317609779911,-41.211850451263));
#250514=CARTESIAN_POINT('Ctrl Pts',(44.5765344835469,30.7055824366946,-41.1751580074971));
#250515=CARTESIAN_POINT('Ctrl Pts',(44.5504480754,30.6870962504203,-41.147699245024));
#250516=CARTESIAN_POINT('Ctrl Pts',(44.5324056777293,30.6755504391987,-41.1294402655247));
#250517=CARTESIAN_POINT('Ctrl Pts',(44.5186168522497,30.6671837862428,-41.1157563555777));
#250518=CARTESIAN_POINT('Ctrl Pts',(44.5139760207251,30.6644431539959,-41.1111953707762));
#250519=CARTESIAN_POINT('Ctrl Pts',(44.5046579712977,30.6590892493455,-41.102125755137));
#250520=CARTESIAN_POINT('Ctrl Pts',(44.4999732573772,30.6564710151932,-41.0976094410703));
#250521=CARTESIAN_POINT('Ctrl Pts',(44.4764410055871,30.6436866063214,-41.0751408219827));
#250522=CARTESIAN_POINT('Ctrl Pts',(44.4380363426647,30.6251318507397,-41.0398401547925));
#250523=CARTESIAN_POINT('Ctrl Pts',(44.3881999640401,30.6066279457426,-40.9973473660572));
#250524=CARTESIAN_POINT('Ctrl Pts',(44.3574626802754,30.5976558165788,-40.9725988687145));
#250525=CARTESIAN_POINT('Ctrl Pts',(44.3367823836873,30.5921565153947,-40.9562701951691));
#250526=CARTESIAN_POINT('Ctrl Pts',(44.3263541271388,30.5896491085923,-40.9481956834911));
#250527=CARTESIAN_POINT('Ctrl Pts',(44.3052793937559,30.5851218575581,-40.9322027877955));
#250528=CARTESIAN_POINT('Ctrl Pts',(44.2946995104909,30.5831174982377,-40.924335654778));
#250529=CARTESIAN_POINT('Ctrl Pts',(44.2735450602529,30.5796377993431,-40.9089243529734));
#250530=CARTESIAN_POINT('Ctrl Pts',(44.2629524396991,30.5781585711684,-40.9013664771085));
#250531=CARTESIAN_POINT('Ctrl Pts',(44.2311453972639,30.5744985086998,-40.8791460851492));
#250532=CARTESIAN_POINT('Ctrl Pts',(44.2098907431643,30.5730912421562,-40.8649273724495));
#250533=CARTESIAN_POINT('Ctrl Pts',(44.1672866942957,30.5723474200962,-40.8376959485268));
#250534=CARTESIAN_POINT('Ctrl Pts',(44.1459323927671,30.5730120277702,-40.8246808510428));
#250535=CARTESIAN_POINT('Ctrl Pts',(44.1191870166623,30.5751734135742,-40.8091986194082));
#250536=CARTESIAN_POINT('Ctrl Pts',(44.1138315874482,30.5756735271978,-40.806139968135));
#250537=CARTESIAN_POINT('Ctrl Pts',(44.1031212948485,30.5768077596639,-40.8001057293845));
#250538=CARTESIAN_POINT('Ctrl Pts',(44.0977557278508,30.5774435866632,-40.7971244669688));
#250539=CARTESIAN_POINT('Ctrl Pts',(44.0817045383335,30.5795497856634,-40.7883321887253));
#250540=CARTESIAN_POINT('Ctrl Pts',(44.0710902649836,30.5812139186595,-40.7826858714375));
#250541=CARTESIAN_POINT('Ctrl Pts',(44.0394561806682,30.5869813183234,-40.7663593410916));
#250542=CARTESIAN_POINT('Ctrl Pts',(44.0082701709188,30.5942909050994,-40.7512721078743));
#250543=CARTESIAN_POINT('Ctrl Pts',(43.9675777996734,30.6070988998346,-40.7336299050859));
#250544=CARTESIAN_POINT('Ctrl Pts',(43.9375066395073,30.6182485087226,-40.721648717354));
#250545=CARTESIAN_POINT('Ctrl Pts',(43.917761614853,30.626725808719,-40.7145087645619));
#250546=CARTESIAN_POINT('Ctrl Pts',(43.8981718083816,30.6357351147044,-40.7078022579606));
#250547=CARTESIAN_POINT('Ctrl Pts',(43.8884396229394,30.6405162381665,-40.7046629153417));
#250548=CARTESIAN_POINT('Ctrl Pts',(43.8693712864522,30.6504970769624,-40.6988992879235));
#250549=CARTESIAN_POINT('Ctrl Pts',(43.8599880575193,30.6557176389023,-40.6962583786489));
#250550=CARTESIAN_POINT('Ctrl Pts',(43.8415477166501,30.6665995934339,-40.6914621347147));
#250551=CARTESIAN_POINT('Ctrl Pts',(43.8143622090585,30.6835906587784,-40.6849914969931));
#250552=CARTESIAN_POINT('Ctrl Pts',(43.7885885365895,30.7025683103525,-40.6806752166169));
#250553=CARTESIAN_POINT('Ctrl Pts',(43.7554869731093,30.7296502406846,-40.676851696754));
#250554=CARTESIAN_POINT('Ctrl Pts',(43.7395647886014,30.744083456595,-40.6759056793254));
#250555=CARTESIAN_POINT('Ctrl Pts',(43.7090440489059,30.7747854825451,-40.6760208486551));
#250556=CARTESIAN_POINT('Ctrl Pts',(43.6947173014185,30.7907796762741,-40.6770802501629));
#250557=CARTESIAN_POINT('Ctrl Pts',(43.6678443418708,30.8240220908504,-40.6811258797777));
#250558=CARTESIAN_POINT('Ctrl Pts',(43.6427576069985,30.8585127548254,-40.687098273402));
#250559=CARTESIAN_POINT('Ctrl Pts',(43.6212142380078,30.8954846730083,-40.6968894358922));
#250560=CARTESIAN_POINT('Ctrl Pts',(43.6088787182641,30.9193798597989,-40.7042205511341));
#250561=CARTESIAN_POINT('Ctrl Pts',(43.6064685586478,30.9241994859948,-40.7057484197296));
#250562=CARTESIAN_POINT('Ctrl Pts',(43.6017624551859,30.9339175659931,-40.70892606686));
#250563=CARTESIAN_POINT('Ctrl Pts',(43.5994656231147,30.9388193592268,-40.7105773965538));
#250564=CARTESIAN_POINT('Ctrl Pts',(43.5927866482525,30.953560895212,-40.7156875255853));
#250565=CARTESIAN_POINT('Ctrl Pts',(43.5844198153918,30.9733582110501,-40.72293005151));
#250566=CARTESIAN_POINT('Ctrl Pts',(43.5734440082896,31.0034822735469,-40.7350537322951));
#250567=CARTESIAN_POINT('Ctrl Pts',(43.5640181327981,31.0340244080827,-40.7484125407461));
#250568=CARTESIAN_POINT('Ctrl Pts',(43.5561284133843,31.0649820306433,-40.7629929778707));
#250569=CARTESIAN_POINT('Ctrl Pts',(43.5518912037438,31.0858969805267,-40.7735241784737));
#250570=CARTESIAN_POINT('Ctrl Pts',(43.5481682579358,31.1069510729684,-40.7844620267622));
#250571=CARTESIAN_POINT('Ctrl Pts',(43.5465635963524,31.1175527760565,-40.7901372750232));
#250572=CARTESIAN_POINT('Ctrl Pts',(43.5438765944467,31.1388768366658,-40.8018865323646));
#250573=CARTESIAN_POINT('Ctrl Pts',(43.5427912565025,31.1496493641875,-40.8079902348016));
#250574=CARTESIAN_POINT('Ctrl Pts',(43.5411674088753,31.1711124235333,-40.8204828132684));
#250575=CARTESIAN_POINT('Ctrl Pts',(43.5400805588778,31.19253758885,-40.8332822237109));
#250576=CARTESIAN_POINT('Ctrl Pts',(43.5400129658238,31.2352236668913,-40.8600695429299));
#250577=CARTESIAN_POINT('Ctrl Pts',(43.5430492497798,31.2776738375434,-40.8886047446452));
#250578=CARTESIAN_POINT('Ctrl Pts',(43.5491614319672,31.3198884817001,-40.918856387552));
#250579=CARTESIAN_POINT('Ctrl Pts',(43.5532522131496,31.3409199794841,-40.9345594064291));
#250580=CARTESIAN_POINT('Ctrl Pts',(43.5578644352119,31.361905871423,-40.9505475151733));
#250581=CARTESIAN_POINT('Ctrl Pts',(43.560439098329,31.3723994717644,-40.9587035928991));
#250582=CARTESIAN_POINT('Ctrl Pts',(43.5660648897127,31.3931449423641,-40.9751492091434));
#250583=CARTESIAN_POINT('Ctrl Pts',(43.5691234314236,31.4034342087731,-40.9834667538713));
#250584=CARTESIAN_POINT('Ctrl Pts',(43.5790202279964,31.4340221767704,-41.0086741075936));
#250585=CARTESIAN_POINT('Ctrl Pts',(43.5865808644402,31.4540562960243,-41.0258289330007));
#250586=CARTESIAN_POINT('Ctrl Pts',(43.5993606039644,31.4835727602996,-41.0520789232858));
#250587=CARTESIAN_POINT('Ctrl Pts',(43.6038584649574,31.4933175175814,-41.0609109997729));
#250588=CARTESIAN_POINT('Ctrl Pts',(43.6133480280387,31.5126460303085,-41.0787663839806));
#250589=CARTESIAN_POINT('Ctrl Pts',(43.6183219077102,31.5221915251339,-41.0877549157913));
#250590=CARTESIAN_POINT('Ctrl Pts',(43.6338406007018,31.5503182102049,-41.1147514459697));
#250591=CARTESIAN_POINT('Ctrl Pts',(43.6450116757484,31.5684678157769,-41.13285712865));
#250592=CARTESIAN_POINT('Ctrl Pts',(43.6689569093208,31.6035742491305,-41.1692591986645));
#250593=CARTESIAN_POINT('Ctrl Pts',(43.6881189975485,31.6290150958394,-41.1967078345595));
#250594=CARTESIAN_POINT('Ctrl Pts',(43.7160805799803,31.6611548911343,-41.2335986369031));
#250595=CARTESIAN_POINT('Ctrl Pts',(43.7308739938731,31.6766212732249,-41.2521403517739));
#250596=CARTESIAN_POINT('Ctrl Pts',(43.7460847706871,31.6917854492915,-41.2707364845776));
#250597=CARTESIAN_POINT('Ctrl Pts',(43.7539033240721,31.6992171694526,-41.2800648729051));
#250598=CARTESIAN_POINT('Ctrl Pts',(43.7697797892606,31.7136063232936,-41.298562009488));
#250599=CARTESIAN_POINT('Ctrl Pts',(43.7778723272806,31.7205988773597,-41.3077734720143));
#250600=CARTESIAN_POINT('Ctrl Pts',(43.8025568401133,31.7409299545529,-41.3352381600133));
#250601=CARTESIAN_POINT('Ctrl Pts',(43.8195937300504,31.7536621581445,-41.353369616892));
#250602=CARTESIAN_POINT('Ctrl Pts',(43.8547939251157,31.7774712224987,-41.3892512463859));
#250603=CARTESIAN_POINT('Ctrl Pts',(43.8820456950658,31.7940939723408,-41.4158852269725));
#250604=CARTESIAN_POINT('Ctrl Pts',(43.9105977352555,31.8088239425505,-41.4420959852738));
#250605=CARTESIAN_POINT('Ctrl Pts',(43.9299312426308,31.8182163905263,-41.4594780331231));
#250606=CARTESIAN_POINT('Ctrl Pts',(43.9397545046832,31.8226994853967,-41.4681277754213));
#250607=CARTESIAN_POINT('Ctrl Pts',(43.959476379363,31.8311327029401,-41.4851373530728));
#250608=CARTESIAN_POINT('Ctrl Pts',(43.969416794615,31.835103670887,-41.4935351095415));
#250609=CARTESIAN_POINT('Ctrl Pts',(43.9894286782948,31.8425474915593,-41.5100965816665));
#250610=CARTESIAN_POINT('Ctrl Pts',(44.0196562937352,31.8529720625538,-41.5345993599874));
#250611=CARTESIAN_POINT('Ctrl Pts',(44.0607928561344,31.8639280327151,-41.5659272170578));
#250612=CARTESIAN_POINT('Ctrl Pts',(44.0922765794535,31.8699137146658,-41.5884145416429));
#250613=CARTESIAN_POINT('Ctrl Pts',(44.1134085621028,31.8733992175668,-41.6031789442838));
#250614=CARTESIAN_POINT('Ctrl Pts',(44.1240412545,31.8748890570172,-41.6104444862381));
#250615=CARTESIAN_POINT('Ctrl Pts',(44.1401138557838,31.8767382236783,-41.6211788509405));
#250616=CARTESIAN_POINT('Ctrl Pts',(44.1454877988083,31.8772894545129,-41.6247266008247));
#250617=CARTESIAN_POINT('Ctrl Pts',(44.1562140153048,31.878256418298,-41.6317257811562));
#250618=CARTESIAN_POINT('Ctrl Pts',(44.161576905651,31.8786734249769,-41.6351843345794));
#250619=CARTESIAN_POINT('Ctrl Pts',(44.1776466456902,31.8797244502982,-41.6454258391029));
#250620=CARTESIAN_POINT('Ctrl Pts',(44.1883500092183,31.8801603696231,-41.6520850220369));
#250621=CARTESIAN_POINT('Ctrl Pts',(44.2204087008324,31.8806796234647,-41.671549250448));
#250622=CARTESIAN_POINT('Ctrl Pts',(44.2417298059497,31.8799780982567,-41.6838534602333));
#250623=CARTESIAN_POINT('Ctrl Pts',(44.2842582084951,31.8764766164199,-41.7071185815018));
#250624=CARTESIAN_POINT('Ctrl Pts',(44.3054713486111,31.8736750129732,-41.7180819683776));
#250625=CARTESIAN_POINT('Ctrl Pts',(44.3319064277948,31.8688271235064,-41.7309251637703));
#250626=CARTESIAN_POINT('Ctrl Pts',(44.3371930873745,31.8677885276791,-41.7334519256467));
#250627=CARTESIAN_POINT('Ctrl Pts',(44.3477523920959,31.8655764110726,-41.7384157665409));
#250628=CARTESIAN_POINT('Ctrl Pts',(44.353035452149,31.8644001232798,-41.7408573895762));
#250629=CARTESIAN_POINT('Ctrl Pts',(44.368821997144,31.8606750365135,-41.7480268313348));
#250630=CARTESIAN_POINT('Ctrl Pts',(44.3792318927429,31.8579388865424,-41.752586114057));
#250631=CARTESIAN_POINT('Ctrl Pts',(44.4101727404,31.8489724804825,-41.7656371280416));
#250632=CARTESIAN_POINT('Ctrl Pts',(44.4405041748167,31.8385015328462,-41.7774224567595));
#250633=CARTESIAN_POINT('Ctrl Pts',(44.4797386522914,31.8215610256552,-41.7906399779756));
#250634=CARTESIAN_POINT('Ctrl Pts',(44.5085558494592,31.8073558935676,-41.7992982329201));
#250635=CARTESIAN_POINT('Ctrl Pts',(44.5273583247585,31.7968714183439,-41.8042246106906));
#250636=CARTESIAN_POINT('Ctrl Pts',(44.5459478308046,31.7858731708475,-41.8087197459362));
#250637=CARTESIAN_POINT('Ctrl Pts',(44.5551558111633,31.7801015230391,-41.8107541019367));
#250638=CARTESIAN_POINT('Ctrl Pts',(44.5731320510561,31.7681815367951,-41.814338976855));
#250639=CARTESIAN_POINT('Ctrl Pts',(44.5819448307914,31.7620078883687,-41.8159008719862));
#250640=CARTESIAN_POINT('Ctrl Pts',(44.5991987000126,31.7492554022398,-41.8185646224661));
#250641=CARTESIAN_POINT('Ctrl Pts',(44.6245350600795,31.7295108031857,-41.8218731379338));
#250642=CARTESIAN_POINT('Ctrl Pts',(44.6561620699444,31.7007477525095,-41.8235671758672));
#250643=CARTESIAN_POINT('Ctrl Pts',(44.6782580742923,31.6773394437008,-41.8227909065983));
#250644=CARTESIAN_POINT('Ctrl Pts',(44.6926220014235,31.6613194462407,-41.8218112048364));
#250645=CARTESIAN_POINT('Ctrl Pts',(44.6996188611148,31.6531046671394,-41.8210906882841));
#250646=CARTESIAN_POINT('Ctrl Pts',(44.7132456597446,31.6362429219073,-41.8191767031797));
#250647=CARTESIAN_POINT('Ctrl Pts',(44.7198193777268,31.627664624135,-41.8179905956202));
#250648=CARTESIAN_POINT('Ctrl Pts',(44.7324727845908,31.610252798272,-41.8151746307749));
#250649=CARTESIAN_POINT('Ctrl Pts',(44.7507253937504,31.5837345714901,-41.8102826177571));
#250650=CARTESIAN_POINT('Ctrl Pts',(44.7668325292565,31.5560404782777,-41.8034218375205));
#250651=CARTESIAN_POINT('Ctrl Pts',(44.7864242741839,31.5180816884312,-41.7925402952635));
#250652=CARTESIAN_POINT('Ctrl Pts',(44.7952779235527,31.4985810718442,-41.7862298998632));
#250653=CARTESIAN_POINT('Ctrl Pts',(44.8051436066325,31.4735589245645,-41.777240214754));
#250654=CARTESIAN_POINT('Ctrl Pts',(44.8070571630202,31.4685179927861,-41.7753849920635));
#250655=CARTESIAN_POINT('Ctrl Pts',(44.8107609555809,31.4583769076679,-41.7715655844892));
#250656=CARTESIAN_POINT('Ctrl Pts',(44.8125545845603,31.4532656516023,-41.76959682162));
#250657=CARTESIAN_POINT('Ctrl Pts',(44.8177323950795,31.4378873281915,-41.7635424458753));
#250658=CARTESIAN_POINT('Ctrl Pts',(44.8209059367305,31.4276035217402,-41.7593207739311));
#250659=CARTESIAN_POINT('Ctrl Pts',(44.8296276705658,31.3966113763671,-41.7460923602843));
#250660=CARTESIAN_POINT('Ctrl Pts',(44.8391161742293,31.3549585404116,-41.7269730343471));
#250661=CARTESIAN_POINT('Ctrl Pts',(44.8444380100638,31.312658433005,-41.7049510923314));
#250662=CARTESIAN_POINT('Ctrl Pts',(44.8468637082338,31.2806969121874,-41.6873414758157));
#250663=CARTESIAN_POINT('Ctrl Pts',(44.8474108190536,31.2699990859542,-41.6812863637077));
#250664=CARTESIAN_POINT('Ctrl Pts',(44.8478348231013,31.2538978106508,-41.671929084156));
#250665=CARTESIAN_POINT('Ctrl Pts',(44.8479099202363,31.2485174556463,-41.6687616517648));
#250666=CARTESIAN_POINT('Ctrl Pts',(44.8479268208064,31.2377432265879,-41.6623372317338));
#250667=CARTESIAN_POINT('Ctrl Pts',(44.8478683021095,31.2323379437313,-41.6590732331048));
#250668=CARTESIAN_POINT('Ctrl Pts',(44.8474921214824,31.2161555213209,-41.6491783400064));
#250669=CARTESIAN_POINT('Ctrl Pts',(44.8469759958029,31.2054292064128,-41.6424562576898));
#250670=CARTESIAN_POINT('Ctrl Pts',(44.8454249887827,31.1840681958411,-41.6287479728186));
#250671=CARTESIAN_POINT('Ctrl Pts',(44.8423204600693,31.1521790951542,-41.6077983885548));
#250672=CARTESIAN_POINT('Ctrl Pts',(44.8351290816859,31.1102584040656,-41.5783402141209));
#250673=CARTESIAN_POINT('Ctrl Pts',(44.8249268329474,31.0689281614894,-41.54736445114));
#250674=CARTESIAN_POINT('Ctrl Pts',(44.8188163283608,31.0484607830594,-41.5313656278891));
#250675=CARTESIAN_POINT('Ctrl Pts',(44.8121960627665,31.028093840338,-41.5151080950287));
#250676=CARTESIAN_POINT('Ctrl Pts',(44.808629563005,31.0179567656131,-41.5068467714969));
#250677=CARTESIAN_POINT('Ctrl Pts',(44.8009827391877,30.9977990758989,-41.4900714456835));
#250678=CARTESIAN_POINT('Ctrl Pts',(44.7969340070935,30.9878607344767,-41.4816261460579));
#250679=CARTESIAN_POINT('Ctrl Pts',(44.7926621173534,30.9780510210195,-41.4731170634489));
#250680=CARTESIAN_POINT('Ctrl Pts',(45.9506566843146,32.3790914166432,-40.3575678858382));
#250681=CARTESIAN_POINT('Ctrl Pts',(45.9241762187347,32.4857587342096,-40.3334357147994));
#250682=CARTESIAN_POINT('Ctrl Pts',(45.8833609513182,32.5889003369546,-40.3114654491246));
#250683=CARTESIAN_POINT('Ctrl Pts',(45.7741007712946,32.7781362580382,-40.2740055971064));
#250684=CARTESIAN_POINT('Ctrl Pts',(45.7072894462425,32.8634116806853,-40.2585741398382));
#250685=CARTESIAN_POINT('Ctrl Pts',(45.5743075775965,32.989444414025,-40.2380701272289));
#250686=CARTESIAN_POINT('Ctrl Pts',(45.5152506641723,33.0350940714751,-40.2313718283122));
#250687=CARTESIAN_POINT('Ctrl Pts',(45.4499236404499,33.0758951502756,-40.2260815011696));
#250688=CARTESIAN_POINT('Ctrl Pts',(45.4481230226174,33.0770127394939,-40.2259372093736));
#250689=CARTESIAN_POINT('Ctrl Pts',(45.4445215185278,33.0792340735076,-40.2256516559397));
#250690=CARTESIAN_POINT('Ctrl Pts',(45.4427204399715,33.0803379828413,-40.225510369052));
#250691=CARTESIAN_POINT('Ctrl Pts',(45.4373314986288,33.0836201423993,-40.2250921735013));
#250692=CARTESIAN_POINT('Ctrl Pts',(45.4337333703977,33.0857841424913,-40.2248189435083));
#250693=CARTESIAN_POINT('Ctrl Pts',(45.4263798098968,33.0901505597053,-40.2242729152289));
#250694=CARTESIAN_POINT('Ctrl Pts',(45.4226308321482,33.0923467584675,-40.2240011956117));
#250695=CARTESIAN_POINT('Ctrl Pts',(45.4112166580987,33.0989467358971,-40.2231924467728));
#250696=CARTESIAN_POINT('Ctrl Pts',(45.4034897677801,33.1032948476848,-40.2226706845611));
#250697=CARTESIAN_POINT('Ctrl Pts',(45.3208157329137,33.1485541094836,-40.2173576933466));
#250698=CARTESIAN_POINT('Ctrl Pts',(45.2416758433089,33.180918628968,-40.2146176874415));
#250699=CARTESIAN_POINT('Ctrl Pts',(44.998745313087,33.2510628523576,-40.2117974091292));
#250700=CARTESIAN_POINT('Ctrl Pts',(44.8303310441375,33.2631001270432,-40.2168378999613));
#250701=CARTESIAN_POINT('Ctrl Pts',(44.597970209409,33.2372616316389,-40.2297741904108));
#250702=CARTESIAN_POINT('Ctrl Pts',(44.5338416044383,33.2252555296773,-40.234170313172));
#250703=CARTESIAN_POINT('Ctrl Pts',(44.4689444465313,33.2087417401602,-40.238822271049));
#250704=CARTESIAN_POINT('Ctrl Pts',(46.6981266849492,30.7091523375488,-39.2904704603133));
#250705=CARTESIAN_POINT('Ctrl Pts',(46.6689684123063,30.6404043382273,-39.273452295095));
#250706=CARTESIAN_POINT('Ctrl Pts',(46.6043681216411,30.5066861069553,-39.238925705885));
#250707=CARTESIAN_POINT('Ctrl Pts',(46.5083209189471,30.3487389562033,-39.1945593129175));
#250708=CARTESIAN_POINT('Ctrl Pts',(46.4437937583117,30.2581216171786,-39.1673894861782));
#250709=CARTESIAN_POINT('Ctrl Pts',(46.3992224148768,30.1986447451181,-39.1491520227249));
#250710=CARTESIAN_POINT('Ctrl Pts',(46.3761748773305,30.1693908446446,-39.1399767764946));
#250711=CARTESIAN_POINT('Ctrl Pts',(46.3284414024809,30.1117648114071,-39.1214771434543));
#250712=CARTESIAN_POINT('Ctrl Pts',(46.3038983378397,30.083571828401,-39.112209259666));
#250713=CARTESIAN_POINT('Ctrl Pts',(46.253707387608,30.0286632749651,-39.0937226519629));
#250714=CARTESIAN_POINT('Ctrl Pts',(46.2280147026909,30.001893564456,-39.0844865568113));
#250715=CARTESIAN_POINT('Ctrl Pts',(46.1492148010453,29.9236586721517,-39.0568159196779));
#250716=CARTESIAN_POINT('Ctrl Pts',(46.0669347173688,29.8495134741745,-39.0292038481275));
#250717=CARTESIAN_POINT('Ctrl Pts',(45.9503410384262,29.7587889734315,-38.9925114043613));
#250718=CARTESIAN_POINT('Ctrl Pts',(45.8594191065401,29.6948377475824,-38.9650526418885));
#250719=CARTESIAN_POINT('Ctrl Pts',(45.7964751089327,29.6549785818455,-38.9467936623891));
#250720=CARTESIAN_POINT('Ctrl Pts',(45.748348603817,29.6261284949947,-38.9331097524421));
#250721=CARTESIAN_POINT('Ctrl Pts',(45.7321473284057,29.616684052073,-38.9285487676403));
#250722=CARTESIAN_POINT('Ctrl Pts',(45.6996106203311,29.5982459977232,-38.9194791520014));
#250723=CARTESIAN_POINT('Ctrl Pts',(45.683249044345,29.5892352448745,-38.9149628379356));
#250724=CARTESIAN_POINT('Ctrl Pts',(45.6010439155842,29.5452684013657,-38.8924942188443));
#250725=CARTESIAN_POINT('Ctrl Pts',(45.4667739830181,29.4816584171599,-38.8571935516581));
#250726=CARTESIAN_POINT('Ctrl Pts',(45.2922645146651,29.4187721922835,-38.8147007629208));
#250727=CARTESIAN_POINT('Ctrl Pts',(45.184512437616,29.3885937253944,-38.7899522655792));
#250728=CARTESIAN_POINT('Ctrl Pts',(45.1119891467798,29.3701842541612,-38.7736235920333));
#250729=CARTESIAN_POINT('Ctrl Pts',(45.0754052578815,29.3618381514785,-38.7655490803555));
#250730=CARTESIAN_POINT('Ctrl Pts',(45.0014447932705,29.3468760834356,-38.7495561846596));
#250731=CARTESIAN_POINT('Ctrl Pts',(44.964301863367,29.3403115562353,-38.7416890516424));
#250732=CARTESIAN_POINT('Ctrl Pts',(44.8900079594565,29.3290481892184,-38.726277749838));
#250733=CARTESIAN_POINT('Ctrl Pts',(44.8527936282157,29.324336495618,-38.7187198739728));
#250734=CARTESIAN_POINT('Ctrl Pts',(44.7410083373266,29.3129455735289,-38.6964994820139));
#250735=CARTESIAN_POINT('Ctrl Pts',(44.6662563757167,29.3089967422249,-38.6822807693139));
#250736=CARTESIAN_POINT('Ctrl Pts',(44.516312468428,29.3084067934202,-38.6550493453909));
#250737=CARTESIAN_POINT('Ctrl Pts',(44.441103189525,29.3117700143417,-38.6420342479066));
#250738=CARTESIAN_POINT('Ctrl Pts',(44.3468378615956,29.3206690055189,-38.6265520162729));
#250739=CARTESIAN_POINT('Ctrl Pts',(44.3279589148655,29.3226883315868,-38.6234933649988));
#250740=CARTESIAN_POINT('Ctrl Pts',(44.2901960653062,29.3271995080042,-38.6174591262491));
#250741=CARTESIAN_POINT('Ctrl Pts',(44.271274393292,29.329697893027,-38.614477863833));
#250742=CARTESIAN_POINT('Ctrl Pts',(44.2146592782019,29.3378915995821,-38.60568558559));
#250743=CARTESIAN_POINT('Ctrl Pts',(44.1772069502033,29.344266758826,-38.6000392683017));
#250744=CARTESIAN_POINT('Ctrl Pts',(44.0655444875092,29.3661148598052,-38.5837127379559));
#250745=CARTESIAN_POINT('Ctrl Pts',(43.9553791862171,29.3933792052515,-38.5686255047386));
#250746=CARTESIAN_POINT('Ctrl Pts',(43.8114622524781,29.4404829778103,-38.5509833019505));
#250747=CARTESIAN_POINT('Ctrl Pts',(43.705021834675,29.481230340464,-38.5390021142185));
#250748=CARTESIAN_POINT('Ctrl Pts',(43.6350719757086,29.512061063653,-38.5318621614261));
#250749=CARTESIAN_POINT('Ctrl Pts',(43.5656410085295,29.5447591316771,-38.525155654825));
#250750=CARTESIAN_POINT('Ctrl Pts',(43.5311320054746,29.5620794464364,-38.5220163122062));
#250751=CARTESIAN_POINT('Ctrl Pts',(43.4634866412134,29.5981758355574,-38.5162526847879));
#250752=CARTESIAN_POINT('Ctrl Pts',(43.4301834663392,29.6170276546,-38.5136117755133));
#250753=CARTESIAN_POINT('Ctrl Pts',(43.3647025891651,29.6562685687332,-38.5088155315793));
#250754=CARTESIAN_POINT('Ctrl Pts',(43.2681192378476,29.7174608121974,-38.5023448938576));
#250755=CARTESIAN_POINT('Ctrl Pts',(43.1764049274077,29.7855824582168,-38.4980286134812));
#250756=CARTESIAN_POINT('Ctrl Pts',(43.0584774180437,29.8826126224142,-38.4942050936184));
#250757=CARTESIAN_POINT('Ctrl Pts',(43.001681818637,29.9342392650769,-38.4932590761897));
#250758=CARTESIAN_POINT('Ctrl Pts',(42.8926599718677,30.0438904492243,-38.4933742455196));
#250759=CARTESIAN_POINT('Ctrl Pts',(42.8414047150844,30.1009342501745,-38.4944336470273));
#250760=CARTESIAN_POINT('Ctrl Pts',(42.7451036203247,30.2193471227021,-38.498479276642));
#250761=CARTESIAN_POINT('Ctrl Pts',(42.6550322643363,30.3420646399833,-38.5044516702661));
#250762=CARTESIAN_POINT('Ctrl Pts',(42.5773225406025,30.4733365238586,-38.5142428327574));
#250763=CARTESIAN_POINT('Ctrl Pts',(42.5326943378214,30.5580963840027,-38.5215739479982));
#250764=CARTESIAN_POINT('Ctrl Pts',(42.5239673850246,30.5751883092729,-38.5231018165939));
#250765=CARTESIAN_POINT('Ctrl Pts',(42.5069121510755,30.60964376351,-38.5262794637242));
#250766=CARTESIAN_POINT('Ctrl Pts',(42.4985805781952,30.627019094627,-38.5279307934181));
#250767=CARTESIAN_POINT('Ctrl Pts',(42.4743295471271,30.6792614198295,-38.5330409224498));
#250768=CARTESIAN_POINT('Ctrl Pts',(42.4438856226513,30.7493896366731,-38.5402834483744));
#250769=CARTESIAN_POINT('Ctrl Pts',(42.4037483179465,30.8560072598611,-38.5524071291592));
#250770=CARTESIAN_POINT('Ctrl Pts',(42.3690543371876,30.9640160484273,-38.5657659376104));
#250771=CARTESIAN_POINT('Ctrl Pts',(42.3397558527982,31.0734075527136,-38.5803463747351));
#250772=CARTESIAN_POINT('Ctrl Pts',(42.3238156343608,31.1472555030051,-38.5908775753381));
#250773=CARTESIAN_POINT('Ctrl Pts',(42.3096820427396,31.2215665449467,-38.6018154236264));
#250774=CARTESIAN_POINT('Ctrl Pts',(42.3035171869091,31.2589715314082,-38.6074906718877));
#250775=CARTESIAN_POINT('Ctrl Pts',(42.2930235524414,31.3341791410138,-38.6192399292287));
#250776=CARTESIAN_POINT('Ctrl Pts',(42.2886818075092,31.3721585359098,-38.6253436316658));
#250777=CARTESIAN_POINT('Ctrl Pts',(42.281930630611,31.4478003630713,-38.6378362101326));
#250778=CARTESIAN_POINT('Ctrl Pts',(42.277074994566,31.5232809912004,-38.6506356205751));
#250779=CARTESIAN_POINT('Ctrl Pts',(42.2747992363309,31.6735553614761,-38.6774229397946));
#250780=CARTESIAN_POINT('Ctrl Pts',(42.2834818483937,31.8228397562226,-38.7059581415094));
#250781=CARTESIAN_POINT('Ctrl Pts',(42.3030248127084,31.9711385758679,-38.7362097844166));
#250782=CARTESIAN_POINT('Ctrl Pts',(42.3164494406915,32.0449687602614,-38.7519128032936));
#250783=CARTESIAN_POINT('Ctrl Pts',(42.3317154579634,32.1186122141692,-38.7679009120377));
#250784=CARTESIAN_POINT('Ctrl Pts',(42.3402956643805,32.1554227583218,-38.7760569897633));
#250785=CARTESIAN_POINT('Ctrl Pts',(42.3591481714288,32.228169160774,-38.7925026060078));
#250786=CARTESIAN_POINT('Ctrl Pts',(42.3694448348212,32.2642362896146,-38.8008201507359));
#250787=CARTESIAN_POINT('Ctrl Pts',(42.4028917825415,32.3714169561226,-38.8260275044574));
#250788=CARTESIAN_POINT('Ctrl Pts',(42.428602574983,32.4415633880281,-38.8431823298655));
#250789=CARTESIAN_POINT('Ctrl Pts',(42.4722685042023,32.5448307979217,-38.8694323201497));
#250790=CARTESIAN_POINT('Ctrl Pts',(42.4876674804306,32.5789105800712,-38.8782643966373));
#250791=CARTESIAN_POINT('Ctrl Pts',(42.5202146590728,32.6464795812123,-38.8961197808447));
#250792=CARTESIAN_POINT('Ctrl Pts',(42.5373018269229,32.6798350022668,-38.9051083126545));
#250793=CARTESIAN_POINT('Ctrl Pts',(42.5906929412925,32.7780783962456,-38.9321048428364));
#250794=CARTESIAN_POINT('Ctrl Pts',(42.629225789877,32.8414173722334,-38.9502105255135));
#250795=CARTESIAN_POINT('Ctrl Pts',(42.7120000069194,32.9638220552461,-38.9866125955294));
#250796=CARTESIAN_POINT('Ctrl Pts',(42.7783647966162,33.0524402968179,-39.0140612314234));
#250797=CARTESIAN_POINT('Ctrl Pts',(42.8754380724448,33.1642175243331,-39.0509520337677));
#250798=CARTESIAN_POINT('Ctrl Pts',(42.9268673384212,33.2179450225078,-39.0694937486382));
#250799=CARTESIAN_POINT('Ctrl Pts',(42.9797817061918,33.2705900457306,-39.088089881442));
#250800=CARTESIAN_POINT('Ctrl Pts',(43.0069972096607,33.2963736994336,-39.097418269769));
#250801=CARTESIAN_POINT('Ctrl Pts',(43.0622936398443,33.3462615369726,-39.1159154063528));
#250802=CARTESIAN_POINT('Ctrl Pts',(43.0904949946047,33.3704876748183,-39.1251268688783));
#250803=CARTESIAN_POINT('Ctrl Pts',(43.176562606447,33.4408730143712,-39.1525915568785));
#250804=CARTESIAN_POINT('Ctrl Pts',(43.2360245534179,33.4848790444095,-39.1707230137558));
#250805=CARTESIAN_POINT('Ctrl Pts',(43.358992255749,33.5670176609587,-39.2066046432507));
#250806=CARTESIAN_POINT('Ctrl Pts',(43.4542745623933,33.6242424638975,-39.233238623837));
#250807=CARTESIAN_POINT('Ctrl Pts',(43.5542222374601,33.6747516510336,-39.2594493821381));
#250808=CARTESIAN_POINT('Ctrl Pts',(43.6219256430316,33.7069073870393,-39.2768314299875));
#250809=CARTESIAN_POINT('Ctrl Pts',(43.6563381479934,33.7222286468184,-39.2854811722856));
#250810=CARTESIAN_POINT('Ctrl Pts',(43.7254519170511,33.7509934760635,-39.3024907499371));
#250811=CARTESIAN_POINT('Ctrl Pts',(43.7602995448845,33.7645084608315,-39.3108885064059));
#250812=CARTESIAN_POINT('Ctrl Pts',(43.8304781084082,33.789780836939,-39.3274499785309));
#250813=CARTESIAN_POINT('Ctrl Pts',(43.9365171946568,33.8250735562425,-39.3519527568515));
#250814=CARTESIAN_POINT('Ctrl Pts',(44.0809642638621,33.8617420360433,-39.3832806139221));
#250815=CARTESIAN_POINT('Ctrl Pts',(44.1916183723467,33.8813683146414,-39.4057679385072));
#250816=CARTESIAN_POINT('Ctrl Pts',(44.2659122959159,33.8926702964892,-39.4205323411483));
#250817=CARTESIAN_POINT('Ctrl Pts',(44.3033049221432,33.8974288658374,-39.4277978831022));
#250818=CARTESIAN_POINT('Ctrl Pts',(44.3598453576919,33.9032050944765,-39.4385322478049));
#250819=CARTESIAN_POINT('Ctrl Pts',(44.3787527158677,33.9049006163346,-39.4420799976889));
#250820=CARTESIAN_POINT('Ctrl Pts',(44.4164967874688,33.9078161173588,-39.4490791780208));
#250821=CARTESIAN_POINT('Ctrl Pts',(44.4353708468856,33.9090400957878,-39.4525377314439));
#250822=CARTESIAN_POINT('Ctrl Pts',(44.4919347179527,33.9120095261765,-39.462779235967));
#250823=CARTESIAN_POINT('Ctrl Pts',(44.52962054914,33.9130584408517,-39.4694384189012));
#250824=CARTESIAN_POINT('Ctrl Pts',(44.6425299001817,33.9134342925821,-39.4889026473125));
#250825=CARTESIAN_POINT('Ctrl Pts',(44.7176656228988,33.9100023852834,-39.5012068570978));
#250826=CARTESIAN_POINT('Ctrl Pts',(44.867623327666,33.8957625538083,-39.524471978366));
#250827=CARTESIAN_POINT('Ctrl Pts',(44.9424659600731,33.8849485744664,-39.5354353652432));
#250828=CARTESIAN_POINT('Ctrl Pts',(45.0357885152669,33.8666999843662,-39.5482785606344));
#250829=CARTESIAN_POINT('Ctrl Pts',(45.0544546343785,33.8628074782943,-39.5508053225112));
#250830=CARTESIAN_POINT('Ctrl Pts',(45.091743102575,33.8545484160302,-39.5557691634051));
#250831=CARTESIAN_POINT('Ctrl Pts',(45.1104022544846,33.850171655015,-39.5582107864407));
#250832=CARTESIAN_POINT('Ctrl Pts',(45.1661672125598,33.8363538303533,-39.5653802281989));
#250833=CARTESIAN_POINT('Ctrl Pts',(45.2029511118778,33.8262578362557,-39.5699395109212));
#250834=CARTESIAN_POINT('Ctrl Pts',(45.312316831343,33.7933159380614,-39.582990524906));
#250835=CARTESIAN_POINT('Ctrl Pts',(45.4195983160475,33.7551076509549,-39.5947758536238));
#250836=CARTESIAN_POINT('Ctrl Pts',(45.5585113890164,33.6937328563153,-39.6079933748399));
#250837=CARTESIAN_POINT('Ctrl Pts',(45.6606150024606,33.6424505696195,-39.6166516297843));
#250838=CARTESIAN_POINT('Ctrl Pts',(45.7272860947277,33.6047101271221,-39.6215780075552));
#250839=CARTESIAN_POINT('Ctrl Pts',(45.7932287365117,33.5651705839516,-39.6260731428005));
#250840=CARTESIAN_POINT('Ctrl Pts',(45.8259059249178,33.5444453395394,-39.6281074988013));
#250841=CARTESIAN_POINT('Ctrl Pts',(45.8897275017006,33.5016881508368,-39.6316923737189));
#250842=CARTESIAN_POINT('Ctrl Pts',(45.9210297733036,33.4795651380848,-39.6332542688506));
#250843=CARTESIAN_POINT('Ctrl Pts',(45.9823424846244,33.4339088874735,-39.6359180193303));
#250844=CARTESIAN_POINT('Ctrl Pts',(46.0724202597563,33.3632801300718,-39.6392265347984));
#250845=CARTESIAN_POINT('Ctrl Pts',(46.1850394564173,33.2606222983665,-39.6409205727319));
#250846=CARTESIAN_POINT('Ctrl Pts',(46.2638636333332,33.1772336958075,-39.6401443034625));
#250847=CARTESIAN_POINT('Ctrl Pts',(46.3151397511292,33.1201974856456,-39.6391646017005));
#250848=CARTESIAN_POINT('Ctrl Pts',(46.3401349353408,33.0909661742941,-39.6384440851485));
#250849=CARTESIAN_POINT('Ctrl Pts',(46.3888523044997,33.0309971480077,-39.6365301000439));
#250850=CARTESIAN_POINT('Ctrl Pts',(46.4123735341802,33.0005036828642,-39.6353439924849));
#250851=CARTESIAN_POINT('Ctrl Pts',(46.4576879006691,32.9386388625828,-39.6325280276393));
#250852=CARTESIAN_POINT('Ctrl Pts',(46.52311576659,32.8444620833496,-39.6276360146217));
#250853=CARTESIAN_POINT('Ctrl Pts',(46.5810426872604,32.7462345994881,-39.6207752343847));
#250854=CARTESIAN_POINT('Ctrl Pts',(46.6516918187307,32.6117039458857,-39.6098936921283));
#250855=CARTESIAN_POINT('Ctrl Pts',(46.683723185051,32.5426422373878,-39.6035832967262));
#250856=CARTESIAN_POINT('Ctrl Pts',(46.7195635412788,32.4540883209461,-39.5945936116187));
#250857=CARTESIAN_POINT('Ctrl Pts',(46.7265235775841,32.4362514419463,-39.5927383889278));
#250858=CARTESIAN_POINT('Ctrl Pts',(46.7400123459627,32.4003742100513,-39.5889189813535));
#250859=CARTESIAN_POINT('Ctrl Pts',(46.7465535157541,32.3822946053341,-39.5869502184844));
#250860=CARTESIAN_POINT('Ctrl Pts',(46.7654644360989,32.3279072933142,-39.5808958427402));
#250861=CARTESIAN_POINT('Ctrl Pts',(46.7770937339888,32.2915493874551,-39.5766741707955));
#250862=CARTESIAN_POINT('Ctrl Pts',(46.8091770518909,32.182013131159,-39.5634457571489));
#250863=CARTESIAN_POINT('Ctrl Pts',(46.8444383818759,32.034891308334,-39.5443264312115));
#250864=CARTESIAN_POINT('Ctrl Pts',(46.8650708643864,31.8856621776612,-39.5223044891954));
#250865=CARTESIAN_POINT('Ctrl Pts',(46.8750487417844,31.7729724844591,-39.50469487268));
#250866=CARTESIAN_POINT('Ctrl Pts',(46.8774570362353,31.7352651712118,-39.4986397605723));
#250867=CARTESIAN_POINT('Ctrl Pts',(46.8796767940079,31.6785286095959,-39.4892824810203));
#250868=CARTESIAN_POINT('Ctrl Pts',(46.8801843407089,31.6595724593507,-39.4861150486293));
#250869=CARTESIAN_POINT('Ctrl Pts',(46.8807312344332,31.6216180949417,-39.479690628598));
#250870=CARTESIAN_POINT('Ctrl Pts',(46.8807699646674,31.6025797052015,-39.4764266299692));
#250871=CARTESIAN_POINT('Ctrl Pts',(46.8801790388754,31.5455906639181,-39.4665317368708));
#250872=CARTESIAN_POINT('Ctrl Pts',(46.8788490796135,31.5078273383739,-39.4598096545541));
#250873=CARTESIAN_POINT('Ctrl Pts',(46.874360617844,31.4326451774338,-39.4461013696832));
#250874=CARTESIAN_POINT('Ctrl Pts',(46.864884835636,31.320441459725,-39.4251517854185));
#250875=CARTESIAN_POINT('Ctrl Pts',(46.8414902947658,31.1730719473388,-39.3956936109857));
#250876=CARTESIAN_POINT('Ctrl Pts',(46.8074810934279,31.0279105813681,-39.364717848004));
#250877=CARTESIAN_POINT('Ctrl Pts',(46.7869180083019,30.9560697433081,-39.3487190247537));
#250878=CARTESIAN_POINT('Ctrl Pts',(46.7645577771926,30.884604709384,-39.332461491893));
#250879=CARTESIAN_POINT('Ctrl Pts',(46.7524740339114,30.8490466969583,-39.3242001683612));
#250880=CARTESIAN_POINT('Ctrl Pts',(46.7264943673172,30.7783632715819,-39.3074248425479));
#250881=CARTESIAN_POINT('Ctrl Pts',(46.7127058212706,30.7435263372096,-39.2989795429224));
#250882=CARTESIAN_POINT('Ctrl Pts',(46.6981266849492,30.7091523375488,-39.2904704603133));
#250883=CARTESIAN_POINT('Ctrl Pts',(44.7926621173534,30.9780510210195,-41.4731170634489));
#250884=CARTESIAN_POINT('Ctrl Pts',(44.7841183378731,30.958431594105,-41.4560988982307));
#250885=CARTESIAN_POINT('Ctrl Pts',(44.7652574387158,30.9202429989855,-41.4215723090211));
#250886=CARTESIAN_POINT('Ctrl Pts',(44.7373647422364,30.8750641226134,-41.3772059160528));
#250887=CARTESIAN_POINT('Ctrl Pts',(44.7186826069414,30.8491098680677,-41.3500360893141));
#250888=CARTESIAN_POINT('Ctrl Pts',(44.7057896374646,30.8320666178198,-41.3317986258606));
#250889=CARTESIAN_POINT('Ctrl Pts',(44.6991283043737,30.8236797190306,-41.3226233796301));
#250890=CARTESIAN_POINT('Ctrl Pts',(44.6853430526266,30.8071501195218,-41.3041237465898));
#250891=CARTESIAN_POINT('Ctrl Pts',(44.6782604199269,30.7990587859436,-41.2948558628018));
#250892=CARTESIAN_POINT('Ctrl Pts',(44.6637865272211,30.7832912649286,-41.2763692550984));
#250893=CARTESIAN_POINT('Ctrl Pts',(44.65638232911,30.7755995480316,-41.2671331599469));
#250894=CARTESIAN_POINT('Ctrl Pts',(44.6336879630273,30.7531065345255,-41.2394625228135));
#250895=CARTESIAN_POINT('Ctrl Pts',(44.6100194582072,30.7317609779911,-41.211850451263));
#250896=CARTESIAN_POINT('Ctrl Pts',(44.5765344835469,30.7055824366946,-41.1751580074971));
#250897=CARTESIAN_POINT('Ctrl Pts',(44.5504480754,30.6870962504203,-41.147699245024));
#250898=CARTESIAN_POINT('Ctrl Pts',(44.5324056777293,30.6755504391987,-41.1294402655247));
#250899=CARTESIAN_POINT('Ctrl Pts',(44.5186168522497,30.6671837862428,-41.1157563555777));
#250900=CARTESIAN_POINT('Ctrl Pts',(44.5139760207251,30.6644431539959,-41.1111953707762));
#250901=CARTESIAN_POINT('Ctrl Pts',(44.5046579712977,30.6590892493455,-41.102125755137));
#250902=CARTESIAN_POINT('Ctrl Pts',(44.4999732573772,30.6564710151932,-41.0976094410703));
#250903=CARTESIAN_POINT('Ctrl Pts',(44.4764410055871,30.6436866063214,-41.0751408219827));
#250904=CARTESIAN_POINT('Ctrl Pts',(44.4380363426647,30.6251318507397,-41.0398401547925));
#250905=CARTESIAN_POINT('Ctrl Pts',(44.3881999640401,30.6066279457426,-40.9973473660572));
#250906=CARTESIAN_POINT('Ctrl Pts',(44.3574626802754,30.5976558165788,-40.9725988687145));
#250907=CARTESIAN_POINT('Ctrl Pts',(44.3367823836873,30.5921565153947,-40.9562701951691));
#250908=CARTESIAN_POINT('Ctrl Pts',(44.3263541271388,30.5896491085923,-40.9481956834911));
#250909=CARTESIAN_POINT('Ctrl Pts',(44.3052793937559,30.5851218575581,-40.9322027877955));
#250910=CARTESIAN_POINT('Ctrl Pts',(44.2946995104909,30.5831174982377,-40.924335654778));
#250911=CARTESIAN_POINT('Ctrl Pts',(44.2735450602529,30.5796377993431,-40.9089243529734));
#250912=CARTESIAN_POINT('Ctrl Pts',(44.2629524396991,30.5781585711684,-40.9013664771085));
#250913=CARTESIAN_POINT('Ctrl Pts',(44.2311453972639,30.5744985086998,-40.8791460851492));
#250914=CARTESIAN_POINT('Ctrl Pts',(44.2098907431643,30.5730912421562,-40.8649273724495));
#250915=CARTESIAN_POINT('Ctrl Pts',(44.1672866942957,30.5723474200962,-40.8376959485268));
#250916=CARTESIAN_POINT('Ctrl Pts',(44.1459323927671,30.5730120277702,-40.8246808510428));
#250917=CARTESIAN_POINT('Ctrl Pts',(44.1191870166623,30.5751734135742,-40.8091986194082));
#250918=CARTESIAN_POINT('Ctrl Pts',(44.1138315874482,30.5756735271978,-40.806139968135));
#250919=CARTESIAN_POINT('Ctrl Pts',(44.1031212948485,30.5768077596639,-40.8001057293845));
#250920=CARTESIAN_POINT('Ctrl Pts',(44.0977557278508,30.5774435866632,-40.7971244669688));
#250921=CARTESIAN_POINT('Ctrl Pts',(44.0817045383335,30.5795497856634,-40.7883321887253));
#250922=CARTESIAN_POINT('Ctrl Pts',(44.0710902649836,30.5812139186595,-40.7826858714375));
#250923=CARTESIAN_POINT('Ctrl Pts',(44.0394561806682,30.5869813183234,-40.7663593410916));
#250924=CARTESIAN_POINT('Ctrl Pts',(44.0082701709188,30.5942909050994,-40.7512721078743));
#250925=CARTESIAN_POINT('Ctrl Pts',(43.9675777996734,30.6070988998346,-40.7336299050859));
#250926=CARTESIAN_POINT('Ctrl Pts',(43.9375066395073,30.6182485087226,-40.721648717354));
#250927=CARTESIAN_POINT('Ctrl Pts',(43.917761614853,30.626725808719,-40.7145087645619));
#250928=CARTESIAN_POINT('Ctrl Pts',(43.8981718083816,30.6357351147044,-40.7078022579606));
#250929=CARTESIAN_POINT('Ctrl Pts',(43.8884396229394,30.6405162381665,-40.7046629153417));
#250930=CARTESIAN_POINT('Ctrl Pts',(43.8693712864522,30.6504970769624,-40.6988992879235));
#250931=CARTESIAN_POINT('Ctrl Pts',(43.8599880575193,30.6557176389023,-40.6962583786489));
#250932=CARTESIAN_POINT('Ctrl Pts',(43.8415477166501,30.6665995934339,-40.6914621347147));
#250933=CARTESIAN_POINT('Ctrl Pts',(43.8143622090585,30.6835906587784,-40.6849914969931));
#250934=CARTESIAN_POINT('Ctrl Pts',(43.7885885365895,30.7025683103525,-40.6806752166169));
#250935=CARTESIAN_POINT('Ctrl Pts',(43.7554869731093,30.7296502406846,-40.676851696754));
#250936=CARTESIAN_POINT('Ctrl Pts',(43.7395647886014,30.744083456595,-40.6759056793254));
#250937=CARTESIAN_POINT('Ctrl Pts',(43.7090440489059,30.7747854825451,-40.6760208486551));
#250938=CARTESIAN_POINT('Ctrl Pts',(43.6947173014185,30.7907796762741,-40.6770802501629));
#250939=CARTESIAN_POINT('Ctrl Pts',(43.6678443418708,30.8240220908504,-40.6811258797777));
#250940=CARTESIAN_POINT('Ctrl Pts',(43.6427576069985,30.8585127548254,-40.687098273402));
#250941=CARTESIAN_POINT('Ctrl Pts',(43.6212142380078,30.8954846730083,-40.6968894358922));
#250942=CARTESIAN_POINT('Ctrl Pts',(43.6088787182641,30.9193798597989,-40.7042205511341));
#250943=CARTESIAN_POINT('Ctrl Pts',(43.6064685586478,30.9241994859948,-40.7057484197296));
#250944=CARTESIAN_POINT('Ctrl Pts',(43.6017624551859,30.9339175659931,-40.70892606686));
#250945=CARTESIAN_POINT('Ctrl Pts',(43.5994656231147,30.9388193592268,-40.7105773965538));
#250946=CARTESIAN_POINT('Ctrl Pts',(43.5927866482525,30.953560895212,-40.7156875255853));
#250947=CARTESIAN_POINT('Ctrl Pts',(43.5844198153918,30.9733582110501,-40.72293005151));
#250948=CARTESIAN_POINT('Ctrl Pts',(43.5734440082896,31.0034822735469,-40.7350537322951));
#250949=CARTESIAN_POINT('Ctrl Pts',(43.5640181327981,31.0340244080827,-40.7484125407461));
#250950=CARTESIAN_POINT('Ctrl Pts',(43.5561284133843,31.0649820306433,-40.7629929778707));
#250951=CARTESIAN_POINT('Ctrl Pts',(43.5518912037438,31.0858969805267,-40.7735241784737));
#250952=CARTESIAN_POINT('Ctrl Pts',(43.5481682579358,31.1069510729684,-40.7844620267622));
#250953=CARTESIAN_POINT('Ctrl Pts',(43.5465635963524,31.1175527760565,-40.7901372750232));
#250954=CARTESIAN_POINT('Ctrl Pts',(43.5438765944467,31.1388768366658,-40.8018865323646));
#250955=CARTESIAN_POINT('Ctrl Pts',(43.5427912565025,31.1496493641875,-40.8079902348016));
#250956=CARTESIAN_POINT('Ctrl Pts',(43.5411674088753,31.1711124235333,-40.8204828132684));
#250957=CARTESIAN_POINT('Ctrl Pts',(43.5400805588778,31.19253758885,-40.8332822237109));
#250958=CARTESIAN_POINT('Ctrl Pts',(43.5400129658238,31.2352236668913,-40.8600695429299));
#250959=CARTESIAN_POINT('Ctrl Pts',(43.5430492497798,31.2776738375434,-40.8886047446452));
#250960=CARTESIAN_POINT('Ctrl Pts',(43.5491614319672,31.3198884817001,-40.918856387552));
#250961=CARTESIAN_POINT('Ctrl Pts',(43.5532522131496,31.3409199794841,-40.9345594064291));
#250962=CARTESIAN_POINT('Ctrl Pts',(43.5578644352119,31.361905871423,-40.9505475151733));
#250963=CARTESIAN_POINT('Ctrl Pts',(43.560439098329,31.3723994717644,-40.9587035928991));
#250964=CARTESIAN_POINT('Ctrl Pts',(43.5660648897127,31.3931449423641,-40.9751492091434));
#250965=CARTESIAN_POINT('Ctrl Pts',(43.5691234314236,31.4034342087731,-40.9834667538713));
#250966=CARTESIAN_POINT('Ctrl Pts',(43.5790202279964,31.4340221767704,-41.0086741075936));
#250967=CARTESIAN_POINT('Ctrl Pts',(43.5865808644402,31.4540562960243,-41.0258289330007));
#250968=CARTESIAN_POINT('Ctrl Pts',(43.5993606039644,31.4835727602996,-41.0520789232858));
#250969=CARTESIAN_POINT('Ctrl Pts',(43.6038584649574,31.4933175175814,-41.0609109997729));
#250970=CARTESIAN_POINT('Ctrl Pts',(43.6133480280387,31.5126460303085,-41.0787663839806));
#250971=CARTESIAN_POINT('Ctrl Pts',(43.6183219077102,31.5221915251339,-41.0877549157913));
#250972=CARTESIAN_POINT('Ctrl Pts',(43.6338406007018,31.5503182102049,-41.1147514459697));
#250973=CARTESIAN_POINT('Ctrl Pts',(43.6450116757484,31.5684678157769,-41.13285712865));
#250974=CARTESIAN_POINT('Ctrl Pts',(43.6689569093208,31.6035742491305,-41.1692591986645));
#250975=CARTESIAN_POINT('Ctrl Pts',(43.6881189975485,31.6290150958394,-41.1967078345595));
#250976=CARTESIAN_POINT('Ctrl Pts',(43.7160805799803,31.6611548911343,-41.2335986369031));
#250977=CARTESIAN_POINT('Ctrl Pts',(43.7308739938731,31.6766212732249,-41.2521403517739));
#250978=CARTESIAN_POINT('Ctrl Pts',(43.7460847706871,31.6917854492915,-41.2707364845776));
#250979=CARTESIAN_POINT('Ctrl Pts',(43.7539033240721,31.6992171694526,-41.2800648729051));
#250980=CARTESIAN_POINT('Ctrl Pts',(43.7697797892606,31.7136063232936,-41.298562009488));
#250981=CARTESIAN_POINT('Ctrl Pts',(43.7778723272806,31.7205988773597,-41.3077734720143));
#250982=CARTESIAN_POINT('Ctrl Pts',(43.8025568401133,31.7409299545529,-41.3352381600133));
#250983=CARTESIAN_POINT('Ctrl Pts',(43.8195937300504,31.7536621581445,-41.353369616892));
#250984=CARTESIAN_POINT('Ctrl Pts',(43.8547939251157,31.7774712224987,-41.3892512463859));
#250985=CARTESIAN_POINT('Ctrl Pts',(43.8820456950658,31.7940939723408,-41.4158852269725));
#250986=CARTESIAN_POINT('Ctrl Pts',(43.9105977352555,31.8088239425505,-41.4420959852738));
#250987=CARTESIAN_POINT('Ctrl Pts',(43.9299312426308,31.8182163905263,-41.4594780331231));
#250988=CARTESIAN_POINT('Ctrl Pts',(43.9397545046832,31.8226994853967,-41.4681277754213));
#250989=CARTESIAN_POINT('Ctrl Pts',(43.959476379363,31.8311327029401,-41.4851373530728));
#250990=CARTESIAN_POINT('Ctrl Pts',(43.969416794615,31.835103670887,-41.4935351095415));
#250991=CARTESIAN_POINT('Ctrl Pts',(43.9894286782948,31.8425474915593,-41.5100965816665));
#250992=CARTESIAN_POINT('Ctrl Pts',(44.0196562937352,31.8529720625538,-41.5345993599874));
#250993=CARTESIAN_POINT('Ctrl Pts',(44.0607928561344,31.8639280327151,-41.5659272170578));
#250994=CARTESIAN_POINT('Ctrl Pts',(44.0922765794535,31.8699137146658,-41.5884145416429));
#250995=CARTESIAN_POINT('Ctrl Pts',(44.1134085621028,31.8733992175668,-41.6031789442838));
#250996=CARTESIAN_POINT('Ctrl Pts',(44.1240412545,31.8748890570172,-41.6104444862381));
#250997=CARTESIAN_POINT('Ctrl Pts',(44.1401138557838,31.8767382236783,-41.6211788509405));
#250998=CARTESIAN_POINT('Ctrl Pts',(44.1454877988083,31.8772894545129,-41.6247266008247));
#250999=CARTESIAN_POINT('Ctrl Pts',(44.1562140153048,31.878256418298,-41.6317257811562));
#251000=CARTESIAN_POINT('Ctrl Pts',(44.161576905651,31.8786734249769,-41.6351843345794));
#251001=CARTESIAN_POINT('Ctrl Pts',(44.1776466456902,31.8797244502982,-41.6454258391029));
#251002=CARTESIAN_POINT('Ctrl Pts',(44.1883500092183,31.8801603696231,-41.6520850220369));
#251003=CARTESIAN_POINT('Ctrl Pts',(44.2204087008324,31.8806796234647,-41.671549250448));
#251004=CARTESIAN_POINT('Ctrl Pts',(44.2417298059497,31.8799780982567,-41.6838534602333));
#251005=CARTESIAN_POINT('Ctrl Pts',(44.2842582084951,31.8764766164199,-41.7071185815018));
#251006=CARTESIAN_POINT('Ctrl Pts',(44.3054713486111,31.8736750129732,-41.7180819683776));
#251007=CARTESIAN_POINT('Ctrl Pts',(44.3319064277948,31.8688271235064,-41.7309251637703));
#251008=CARTESIAN_POINT('Ctrl Pts',(44.3371930873745,31.8677885276791,-41.7334519256467));
#251009=CARTESIAN_POINT('Ctrl Pts',(44.3477523920959,31.8655764110726,-41.7384157665409));
#251010=CARTESIAN_POINT('Ctrl Pts',(44.353035452149,31.8644001232798,-41.7408573895762));
#251011=CARTESIAN_POINT('Ctrl Pts',(44.368821997144,31.8606750365135,-41.7480268313348));
#251012=CARTESIAN_POINT('Ctrl Pts',(44.3792318927429,31.8579388865424,-41.752586114057));
#251013=CARTESIAN_POINT('Ctrl Pts',(44.4101727404,31.8489724804825,-41.7656371280416));
#251014=CARTESIAN_POINT('Ctrl Pts',(44.4405041748167,31.8385015328462,-41.7774224567595));
#251015=CARTESIAN_POINT('Ctrl Pts',(44.4797386522914,31.8215610256552,-41.7906399779756));
#251016=CARTESIAN_POINT('Ctrl Pts',(44.5085558494592,31.8073558935676,-41.7992982329201));
#251017=CARTESIAN_POINT('Ctrl Pts',(44.5273583247585,31.7968714183439,-41.8042246106906));
#251018=CARTESIAN_POINT('Ctrl Pts',(44.5459478308046,31.7858731708475,-41.8087197459362));
#251019=CARTESIAN_POINT('Ctrl Pts',(44.5551558111633,31.7801015230391,-41.8107541019367));
#251020=CARTESIAN_POINT('Ctrl Pts',(44.5731320510561,31.7681815367951,-41.814338976855));
#251021=CARTESIAN_POINT('Ctrl Pts',(44.5819448307914,31.7620078883687,-41.8159008719862));
#251022=CARTESIAN_POINT('Ctrl Pts',(44.5991987000126,31.7492554022398,-41.8185646224661));
#251023=CARTESIAN_POINT('Ctrl Pts',(44.6245350600795,31.7295108031857,-41.8218731379338));
#251024=CARTESIAN_POINT('Ctrl Pts',(44.6561620699444,31.7007477525095,-41.8235671758672));
#251025=CARTESIAN_POINT('Ctrl Pts',(44.6782580742923,31.6773394437008,-41.8227909065983));
#251026=CARTESIAN_POINT('Ctrl Pts',(44.6926220014235,31.6613194462407,-41.8218112048364));
#251027=CARTESIAN_POINT('Ctrl Pts',(44.6996188611148,31.6531046671394,-41.8210906882841));
#251028=CARTESIAN_POINT('Ctrl Pts',(44.7132456597446,31.6362429219073,-41.8191767031797));
#251029=CARTESIAN_POINT('Ctrl Pts',(44.7198193777268,31.627664624135,-41.8179905956202));
#251030=CARTESIAN_POINT('Ctrl Pts',(44.7324727845908,31.610252798272,-41.8151746307749));
#251031=CARTESIAN_POINT('Ctrl Pts',(44.7507253937504,31.5837345714901,-41.8102826177571));
#251032=CARTESIAN_POINT('Ctrl Pts',(44.7668325292565,31.5560404782777,-41.8034218375205));
#251033=CARTESIAN_POINT('Ctrl Pts',(44.7864242741839,31.5180816884312,-41.7925402952635));
#251034=CARTESIAN_POINT('Ctrl Pts',(44.7952779235527,31.4985810718442,-41.7862298998632));
#251035=CARTESIAN_POINT('Ctrl Pts',(44.8051436066325,31.4735589245645,-41.777240214754));
#251036=CARTESIAN_POINT('Ctrl Pts',(44.8070571630202,31.4685179927861,-41.7753849920635));
#251037=CARTESIAN_POINT('Ctrl Pts',(44.8107609555809,31.4583769076679,-41.7715655844892));
#251038=CARTESIAN_POINT('Ctrl Pts',(44.8125545845603,31.4532656516023,-41.76959682162));
#251039=CARTESIAN_POINT('Ctrl Pts',(44.8177323950795,31.4378873281915,-41.7635424458753));
#251040=CARTESIAN_POINT('Ctrl Pts',(44.8209059367305,31.4276035217402,-41.7593207739311));
#251041=CARTESIAN_POINT('Ctrl Pts',(44.8296276705658,31.3966113763671,-41.7460923602843));
#251042=CARTESIAN_POINT('Ctrl Pts',(44.8391161742293,31.3549585404116,-41.7269730343471));
#251043=CARTESIAN_POINT('Ctrl Pts',(44.8444380100638,31.312658433005,-41.7049510923314));
#251044=CARTESIAN_POINT('Ctrl Pts',(44.8468637082338,31.2806969121874,-41.6873414758157));
#251045=CARTESIAN_POINT('Ctrl Pts',(44.8474108190536,31.2699990859542,-41.6812863637077));
#251046=CARTESIAN_POINT('Ctrl Pts',(44.8478348231013,31.2538978106508,-41.671929084156));
#251047=CARTESIAN_POINT('Ctrl Pts',(44.8479099202363,31.2485174556463,-41.6687616517648));
#251048=CARTESIAN_POINT('Ctrl Pts',(44.8479268208064,31.2377432265879,-41.6623372317338));
#251049=CARTESIAN_POINT('Ctrl Pts',(44.8478683021095,31.2323379437313,-41.6590732331048));
#251050=CARTESIAN_POINT('Ctrl Pts',(44.8474921214824,31.2161555213209,-41.6491783400064));
#251051=CARTESIAN_POINT('Ctrl Pts',(44.8469759958029,31.2054292064128,-41.6424562576898));
#251052=CARTESIAN_POINT('Ctrl Pts',(44.8454249887827,31.1840681958411,-41.6287479728186));
#251053=CARTESIAN_POINT('Ctrl Pts',(44.8423204600693,31.1521790951542,-41.6077983885548));
#251054=CARTESIAN_POINT('Ctrl Pts',(44.8351290816859,31.1102584040656,-41.5783402141209));
#251055=CARTESIAN_POINT('Ctrl Pts',(44.8249268329474,31.0689281614894,-41.54736445114));
#251056=CARTESIAN_POINT('Ctrl Pts',(44.8188163283608,31.0484607830594,-41.5313656278891));
#251057=CARTESIAN_POINT('Ctrl Pts',(44.8121960627665,31.028093840338,-41.5151080950287));
#251058=CARTESIAN_POINT('Ctrl Pts',(44.808629563005,31.0179567656131,-41.5068467714969));
#251059=CARTESIAN_POINT('Ctrl Pts',(44.8009827391877,30.9977990758989,-41.4900714456835));
#251060=CARTESIAN_POINT('Ctrl Pts',(44.7969340070935,30.9878607344767,-41.4816261460579));
#251061=CARTESIAN_POINT('Ctrl Pts',(44.7926621173534,30.9780510210195,-41.4731170634489));
#251062=CARTESIAN_POINT('',(46.348736272544,30.7584582252104,-39.6906856150703));
#251063=CARTESIAN_POINT('',(46.0995611578475,30.7936217551105,-39.9761074628063));
#251064=CARTESIAN_POINT('',(46.348736272544,30.7584582252104,-39.6906856150703));
#251065=CARTESIAN_POINT('',(46.2910026132808,32.4463939541198,-40.0133525199849));
#251066=CARTESIAN_POINT('Ctrl Pts',(46.348736272544,30.7584582252104,-39.6906856150703));
#251067=CARTESIAN_POINT('Ctrl Pts',(46.3614254481729,30.7883280602527,-39.6991946976794));
#251068=CARTESIAN_POINT('Ctrl Pts',(46.3734280792928,30.8185995307445,-39.7076399973049));
#251069=CARTESIAN_POINT('Ctrl Pts',(46.3960461932204,30.8800184397817,-39.7244153231182));
#251070=CARTESIAN_POINT('Ctrl Pts',(46.4065681949313,30.9109152099792,-39.7326766466501));
#251071=CARTESIAN_POINT('Ctrl Pts',(46.4260423093758,30.9730107791217,-39.7489341795107));
#251072=CARTESIAN_POINT('Ctrl Pts',(46.4439553357389,31.0354316602054,-39.764933002761));
#251073=CARTESIAN_POINT('Ctrl Pts',(46.4735992389084,31.1615543100329,-39.7959087657426));
#251074=CARTESIAN_POINT('Ctrl Pts',(46.4940227302404,31.289588481428,-39.8253669401756));
#251075=CARTESIAN_POINT('Ctrl Pts',(46.5023302645975,31.3870655242667,-39.8463165244401));
#251076=CARTESIAN_POINT('Ctrl Pts',(46.506280107836,31.4523789139669,-39.8600248093111));
#251077=CARTESIAN_POINT('Ctrl Pts',(46.5074608406805,31.4851846703929,-39.8667468916278));
#251078=CARTESIAN_POINT('Ctrl Pts',(46.5080123902999,31.5346913151838,-39.8766417847262));
#251079=CARTESIAN_POINT('Ctrl Pts',(46.5079914918558,31.5512299067555,-39.879905783355));
#251080=CARTESIAN_POINT('Ctrl Pts',(46.5075417789082,31.5842004583658,-39.8863302033863));
#251081=CARTESIAN_POINT('Ctrl Pts',(46.5071135271648,31.6006673192385,-39.8894976357773));
#251082=CARTESIAN_POINT('Ctrl Pts',(46.5052230429695,31.6499529002985,-39.8988549153293));
#251083=CARTESIAN_POINT('Ctrl Pts',(46.5031560194756,31.6827076912229,-39.9049100274371));
#251084=CARTESIAN_POINT('Ctrl Pts',(46.494562927216,31.7805948790823,-39.9225196439524));
#251085=CARTESIAN_POINT('Ctrl Pts',(46.4767378404699,31.9102172554903,-39.9445415859684));
#251086=CARTESIAN_POINT('Ctrl Pts',(46.4462022758287,32.0380000397181,-39.9636609119059));
#251087=CARTESIAN_POINT('Ctrl Pts',(46.4184025922855,32.1331342652581,-39.9768893255524));
#251088=CARTESIAN_POINT('Ctrl Pts',(46.4083237615152,32.1647111636399,-39.9811109974971));
#251089=CARTESIAN_POINT('Ctrl Pts',(46.3919309761109,32.2119456968313,-39.9871653732414));
#251090=CARTESIAN_POINT('Ctrl Pts',(46.3862603264385,32.2276473949945,-39.9891341361105));
#251091=CARTESIAN_POINT('Ctrl Pts',(46.3745657539712,32.2588055871924,-39.9929535436847));
#251092=CARTESIAN_POINT('Ctrl Pts',(46.3685310519543,32.2742961715652,-39.9948087663756));
#251093=CARTESIAN_POINT('Ctrl Pts',(46.340730665806,32.3430910112799,-40.00285047101));
#251094=CARTESIAN_POINT('Ctrl Pts',(46.3169453252715,32.3953369342895,-40.0084299233149));
#251095=CARTESIAN_POINT('Ctrl Pts',(46.2910031870661,32.446394079709,-40.0133500693448));
#251096=CARTESIAN_POINT('Ctrl Pts',(46.2910021078285,32.4463936912103,-40.0133527637202));
#251097=CARTESIAN_POINT('Ctrl Pts',(46.3486217884263,32.3037296072064,-40.0136728648342));
#251098=CARTESIAN_POINT('Ctrl Pts',(46.386668413569,32.1539381754564,-40.0127279860568));
#251099=CARTESIAN_POINT('Ctrl Pts',(46.4200060593677,31.8665821327808,-40.0089408346456));
#251100=CARTESIAN_POINT('Ctrl Pts',(46.4197397558165,31.7306141336591,-40.0063483988712));
#251101=CARTESIAN_POINT('Ctrl Pts',(46.3858725160227,31.4446264987979,-39.999488756941));
#251102=CARTESIAN_POINT('Ctrl Pts',(46.3483278372589,31.2963700576375,-39.9950892255237));
#251103=CARTESIAN_POINT('Ctrl Pts',(46.2421281802311,31.027394804457,-39.9857972773175));
#251104=CARTESIAN_POINT('Ctrl Pts',(46.1774476182685,30.90637643183,-39.9810433254305));
#251105=CARTESIAN_POINT('Ctrl Pts',(46.0995611578475,30.7936217551105,-39.9761074628063));
#251106=CARTESIAN_POINT('Ctrl Pts',(46.6981266849492,30.7091523375488,-39.2904704603133));
#251107=CARTESIAN_POINT('Ctrl Pts',(46.6689684123063,30.6404043382273,-39.273452295095));
#251108=CARTESIAN_POINT('Ctrl Pts',(46.6043681216411,30.5066861069553,-39.238925705885));
#251109=CARTESIAN_POINT('Ctrl Pts',(46.5083209189471,30.3487389562033,-39.1945593129175));
#251110=CARTESIAN_POINT('Ctrl Pts',(46.4437937583117,30.2581216171786,-39.1673894861782));
#251111=CARTESIAN_POINT('Ctrl Pts',(46.3992224148768,30.1986447451181,-39.1491520227249));
#251112=CARTESIAN_POINT('Ctrl Pts',(46.3761748773305,30.1693908446446,-39.1399767764946));
#251113=CARTESIAN_POINT('Ctrl Pts',(46.3284414024809,30.1117648114071,-39.1214771434543));
#251114=CARTESIAN_POINT('Ctrl Pts',(46.3038983378397,30.083571828401,-39.112209259666));
#251115=CARTESIAN_POINT('Ctrl Pts',(46.253707387608,30.0286632749651,-39.0937226519629));
#251116=CARTESIAN_POINT('Ctrl Pts',(46.2280147026909,30.001893564456,-39.0844865568113));
#251117=CARTESIAN_POINT('Ctrl Pts',(46.1492148010453,29.9236586721517,-39.0568159196779));
#251118=CARTESIAN_POINT('Ctrl Pts',(46.0669347173688,29.8495134741745,-39.0292038481275));
#251119=CARTESIAN_POINT('Ctrl Pts',(45.9503410384262,29.7587889734315,-38.9925114043613));
#251120=CARTESIAN_POINT('Ctrl Pts',(45.8594191065401,29.6948377475824,-38.9650526418885));
#251121=CARTESIAN_POINT('Ctrl Pts',(45.7964751089327,29.6549785818455,-38.9467936623891));
#251122=CARTESIAN_POINT('Ctrl Pts',(45.748348603817,29.6261284949947,-38.9331097524421));
#251123=CARTESIAN_POINT('Ctrl Pts',(45.7321473284057,29.616684052073,-38.9285487676403));
#251124=CARTESIAN_POINT('Ctrl Pts',(45.6996106203311,29.5982459977232,-38.9194791520014));
#251125=CARTESIAN_POINT('Ctrl Pts',(45.683249044345,29.5892352448745,-38.9149628379356));
#251126=CARTESIAN_POINT('Ctrl Pts',(45.6010439155842,29.5452684013657,-38.8924942188443));
#251127=CARTESIAN_POINT('Ctrl Pts',(45.4667739830181,29.4816584171599,-38.8571935516581));
#251128=CARTESIAN_POINT('Ctrl Pts',(45.2922645146651,29.4187721922835,-38.8147007629208));
#251129=CARTESIAN_POINT('Ctrl Pts',(45.184512437616,29.3885937253944,-38.7899522655792));
#251130=CARTESIAN_POINT('Ctrl Pts',(45.1119891467798,29.3701842541612,-38.7736235920333));
#251131=CARTESIAN_POINT('Ctrl Pts',(45.0754052578815,29.3618381514785,-38.7655490803555));
#251132=CARTESIAN_POINT('Ctrl Pts',(45.0014447932705,29.3468760834356,-38.7495561846596));
#251133=CARTESIAN_POINT('Ctrl Pts',(44.964301863367,29.3403115562353,-38.7416890516424));
#251134=CARTESIAN_POINT('Ctrl Pts',(44.8900079594565,29.3290481892184,-38.726277749838));
#251135=CARTESIAN_POINT('Ctrl Pts',(44.8527936282157,29.324336495618,-38.7187198739728));
#251136=CARTESIAN_POINT('Ctrl Pts',(44.7410083373266,29.3129455735289,-38.6964994820139));
#251137=CARTESIAN_POINT('Ctrl Pts',(44.6662563757167,29.3089967422249,-38.6822807693139));
#251138=CARTESIAN_POINT('Ctrl Pts',(44.516312468428,29.3084067934202,-38.6550493453909));
#251139=CARTESIAN_POINT('Ctrl Pts',(44.441103189525,29.3117700143417,-38.6420342479066));
#251140=CARTESIAN_POINT('Ctrl Pts',(44.3468378615956,29.3206690055189,-38.6265520162729));
#251141=CARTESIAN_POINT('Ctrl Pts',(44.3279589148655,29.3226883315868,-38.6234933649988));
#251142=CARTESIAN_POINT('Ctrl Pts',(44.2901960653062,29.3271995080042,-38.6174591262491));
#251143=CARTESIAN_POINT('Ctrl Pts',(44.271274393292,29.329697893027,-38.614477863833));
#251144=CARTESIAN_POINT('Ctrl Pts',(44.2146592782019,29.3378915995821,-38.60568558559));
#251145=CARTESIAN_POINT('Ctrl Pts',(44.1772069502033,29.344266758826,-38.6000392683017));
#251146=CARTESIAN_POINT('Ctrl Pts',(44.0655444875092,29.3661148598052,-38.5837127379559));
#251147=CARTESIAN_POINT('Ctrl Pts',(43.9553791862171,29.3933792052515,-38.5686255047386));
#251148=CARTESIAN_POINT('Ctrl Pts',(43.8114622524781,29.4404829778103,-38.5509833019505));
#251149=CARTESIAN_POINT('Ctrl Pts',(43.705021834675,29.481230340464,-38.5390021142185));
#251150=CARTESIAN_POINT('Ctrl Pts',(43.6350719757086,29.512061063653,-38.5318621614261));
#251151=CARTESIAN_POINT('Ctrl Pts',(43.5656410085295,29.5447591316771,-38.525155654825));
#251152=CARTESIAN_POINT('Ctrl Pts',(43.5311320054746,29.5620794464364,-38.5220163122062));
#251153=CARTESIAN_POINT('Ctrl Pts',(43.4634866412134,29.5981758355574,-38.5162526847879));
#251154=CARTESIAN_POINT('Ctrl Pts',(43.4301834663392,29.6170276546,-38.5136117755133));
#251155=CARTESIAN_POINT('Ctrl Pts',(43.3647025891651,29.6562685687332,-38.5088155315793));
#251156=CARTESIAN_POINT('Ctrl Pts',(43.2681192378476,29.7174608121974,-38.5023448938576));
#251157=CARTESIAN_POINT('Ctrl Pts',(43.1764049274077,29.7855824582168,-38.4980286134812));
#251158=CARTESIAN_POINT('Ctrl Pts',(43.0584774180437,29.8826126224142,-38.4942050936184));
#251159=CARTESIAN_POINT('Ctrl Pts',(43.001681818637,29.9342392650769,-38.4932590761897));
#251160=CARTESIAN_POINT('Ctrl Pts',(42.8926599718677,30.0438904492243,-38.4933742455196));
#251161=CARTESIAN_POINT('Ctrl Pts',(42.8414047150844,30.1009342501745,-38.4944336470273));
#251162=CARTESIAN_POINT('Ctrl Pts',(42.7451036203247,30.2193471227021,-38.498479276642));
#251163=CARTESIAN_POINT('Ctrl Pts',(42.6550322643363,30.3420646399833,-38.5044516702661));
#251164=CARTESIAN_POINT('Ctrl Pts',(42.5773225406025,30.4733365238586,-38.5142428327574));
#251165=CARTESIAN_POINT('Ctrl Pts',(42.5326943378214,30.5580963840027,-38.5215739479982));
#251166=CARTESIAN_POINT('Ctrl Pts',(42.5239673850246,30.5751883092729,-38.5231018165939));
#251167=CARTESIAN_POINT('Ctrl Pts',(42.5069121510755,30.60964376351,-38.5262794637242));
#251168=CARTESIAN_POINT('Ctrl Pts',(42.4985805781952,30.627019094627,-38.5279307934181));
#251169=CARTESIAN_POINT('Ctrl Pts',(42.4743295471271,30.6792614198295,-38.5330409224498));
#251170=CARTESIAN_POINT('Ctrl Pts',(42.4438856226513,30.7493896366731,-38.5402834483744));
#251171=CARTESIAN_POINT('Ctrl Pts',(42.4037483179465,30.8560072598611,-38.5524071291592));
#251172=CARTESIAN_POINT('Ctrl Pts',(42.3690543371876,30.9640160484273,-38.5657659376104));
#251173=CARTESIAN_POINT('Ctrl Pts',(42.3397558527982,31.0734075527136,-38.5803463747351));
#251174=CARTESIAN_POINT('Ctrl Pts',(42.3238156343608,31.1472555030051,-38.5908775753381));
#251175=CARTESIAN_POINT('Ctrl Pts',(42.3096820427396,31.2215665449467,-38.6018154236264));
#251176=CARTESIAN_POINT('Ctrl Pts',(42.3035171869091,31.2589715314082,-38.6074906718877));
#251177=CARTESIAN_POINT('Ctrl Pts',(42.2930235524414,31.3341791410138,-38.6192399292287));
#251178=CARTESIAN_POINT('Ctrl Pts',(42.2886818075092,31.3721585359098,-38.6253436316658));
#251179=CARTESIAN_POINT('Ctrl Pts',(42.281930630611,31.4478003630713,-38.6378362101326));
#251180=CARTESIAN_POINT('Ctrl Pts',(42.277074994566,31.5232809912004,-38.6506356205751));
#251181=CARTESIAN_POINT('Ctrl Pts',(42.2747992363309,31.6735553614761,-38.6774229397946));
#251182=CARTESIAN_POINT('Ctrl Pts',(42.2834818483937,31.8228397562226,-38.7059581415094));
#251183=CARTESIAN_POINT('Ctrl Pts',(42.3030248127084,31.9711385758679,-38.7362097844166));
#251184=CARTESIAN_POINT('Ctrl Pts',(42.3164494406915,32.0449687602614,-38.7519128032936));
#251185=CARTESIAN_POINT('Ctrl Pts',(42.3317154579634,32.1186122141692,-38.7679009120377));
#251186=CARTESIAN_POINT('Ctrl Pts',(42.3402956643805,32.1554227583218,-38.7760569897633));
#251187=CARTESIAN_POINT('Ctrl Pts',(42.3591481714288,32.228169160774,-38.7925026060078));
#251188=CARTESIAN_POINT('Ctrl Pts',(42.3694448348212,32.2642362896146,-38.8008201507359));
#251189=CARTESIAN_POINT('Ctrl Pts',(42.4028917825415,32.3714169561226,-38.8260275044574));
#251190=CARTESIAN_POINT('Ctrl Pts',(42.428602574983,32.4415633880281,-38.8431823298655));
#251191=CARTESIAN_POINT('Ctrl Pts',(42.4722685042023,32.5448307979217,-38.8694323201497));
#251192=CARTESIAN_POINT('Ctrl Pts',(42.4876674804306,32.5789105800712,-38.8782643966373));
#251193=CARTESIAN_POINT('Ctrl Pts',(42.5202146590728,32.6464795812123,-38.8961197808447));
#251194=CARTESIAN_POINT('Ctrl Pts',(42.5373018269229,32.6798350022668,-38.9051083126545));
#251195=CARTESIAN_POINT('Ctrl Pts',(42.5906929412925,32.7780783962456,-38.9321048428364));
#251196=CARTESIAN_POINT('Ctrl Pts',(42.629225789877,32.8414173722334,-38.9502105255135));
#251197=CARTESIAN_POINT('Ctrl Pts',(42.7120000069194,32.9638220552461,-38.9866125955294));
#251198=CARTESIAN_POINT('Ctrl Pts',(42.7783647966162,33.0524402968179,-39.0140612314234));
#251199=CARTESIAN_POINT('Ctrl Pts',(42.8754380724448,33.1642175243331,-39.0509520337677));
#251200=CARTESIAN_POINT('Ctrl Pts',(42.9268673384212,33.2179450225078,-39.0694937486382));
#251201=CARTESIAN_POINT('Ctrl Pts',(42.9797817061918,33.2705900457306,-39.088089881442));
#251202=CARTESIAN_POINT('Ctrl Pts',(43.0069972096607,33.2963736994336,-39.097418269769));
#251203=CARTESIAN_POINT('Ctrl Pts',(43.0622936398443,33.3462615369726,-39.1159154063528));
#251204=CARTESIAN_POINT('Ctrl Pts',(43.0904949946047,33.3704876748183,-39.1251268688783));
#251205=CARTESIAN_POINT('Ctrl Pts',(43.176562606447,33.4408730143712,-39.1525915568785));
#251206=CARTESIAN_POINT('Ctrl Pts',(43.2360245534179,33.4848790444095,-39.1707230137558));
#251207=CARTESIAN_POINT('Ctrl Pts',(43.358992255749,33.5670176609587,-39.2066046432507));
#251208=CARTESIAN_POINT('Ctrl Pts',(43.4542745623933,33.6242424638975,-39.233238623837));
#251209=CARTESIAN_POINT('Ctrl Pts',(43.5542222374601,33.6747516510336,-39.2594493821381));
#251210=CARTESIAN_POINT('Ctrl Pts',(43.6219256430316,33.7069073870393,-39.2768314299875));
#251211=CARTESIAN_POINT('Ctrl Pts',(43.6563381479934,33.7222286468184,-39.2854811722856));
#251212=CARTESIAN_POINT('Ctrl Pts',(43.7254519170511,33.7509934760635,-39.3024907499371));
#251213=CARTESIAN_POINT('Ctrl Pts',(43.7602995448845,33.7645084608315,-39.3108885064059));
#251214=CARTESIAN_POINT('Ctrl Pts',(43.8304781084082,33.789780836939,-39.3274499785309));
#251215=CARTESIAN_POINT('Ctrl Pts',(43.9365171946568,33.8250735562425,-39.3519527568515));
#251216=CARTESIAN_POINT('Ctrl Pts',(44.0809642638621,33.8617420360433,-39.3832806139221));
#251217=CARTESIAN_POINT('Ctrl Pts',(44.1916183723467,33.8813683146414,-39.4057679385072));
#251218=CARTESIAN_POINT('Ctrl Pts',(44.2659122959159,33.8926702964892,-39.4205323411483));
#251219=CARTESIAN_POINT('Ctrl Pts',(44.3033049221432,33.8974288658374,-39.4277978831022));
#251220=CARTESIAN_POINT('Ctrl Pts',(44.3598453576919,33.9032050944765,-39.4385322478049));
#251221=CARTESIAN_POINT('Ctrl Pts',(44.3787527158677,33.9049006163346,-39.4420799976889));
#251222=CARTESIAN_POINT('Ctrl Pts',(44.4164967874688,33.9078161173588,-39.4490791780208));
#251223=CARTESIAN_POINT('Ctrl Pts',(44.4353708468856,33.9090400957878,-39.4525377314439));
#251224=CARTESIAN_POINT('Ctrl Pts',(44.4919347179527,33.9120095261765,-39.462779235967));
#251225=CARTESIAN_POINT('Ctrl Pts',(44.52962054914,33.9130584408517,-39.4694384189012));
#251226=CARTESIAN_POINT('Ctrl Pts',(44.6425299001817,33.9134342925821,-39.4889026473125));
#251227=CARTESIAN_POINT('Ctrl Pts',(44.7176656228988,33.9100023852834,-39.5012068570978));
#251228=CARTESIAN_POINT('Ctrl Pts',(44.867623327666,33.8957625538083,-39.524471978366));
#251229=CARTESIAN_POINT('Ctrl Pts',(44.9424659600731,33.8849485744664,-39.5354353652432));
#251230=CARTESIAN_POINT('Ctrl Pts',(45.0357885152669,33.8666999843662,-39.5482785606344));
#251231=CARTESIAN_POINT('Ctrl Pts',(45.0544546343785,33.8628074782943,-39.5508053225112));
#251232=CARTESIAN_POINT('Ctrl Pts',(45.091743102575,33.8545484160302,-39.5557691634051));
#251233=CARTESIAN_POINT('Ctrl Pts',(45.1104022544846,33.850171655015,-39.5582107864407));
#251234=CARTESIAN_POINT('Ctrl Pts',(45.1661672125598,33.8363538303533,-39.5653802281989));
#251235=CARTESIAN_POINT('Ctrl Pts',(45.2029511118778,33.8262578362557,-39.5699395109212));
#251236=CARTESIAN_POINT('Ctrl Pts',(45.312316831343,33.7933159380614,-39.582990524906));
#251237=CARTESIAN_POINT('Ctrl Pts',(45.4195983160475,33.7551076509549,-39.5947758536238));
#251238=CARTESIAN_POINT('Ctrl Pts',(45.5585113890164,33.6937328563153,-39.6079933748399));
#251239=CARTESIAN_POINT('Ctrl Pts',(45.6606150024606,33.6424505696195,-39.6166516297843));
#251240=CARTESIAN_POINT('Ctrl Pts',(45.7272860947277,33.6047101271221,-39.6215780075552));
#251241=CARTESIAN_POINT('Ctrl Pts',(45.7932287365117,33.5651705839516,-39.6260731428005));
#251242=CARTESIAN_POINT('Ctrl Pts',(45.8259059249178,33.5444453395394,-39.6281074988013));
#251243=CARTESIAN_POINT('Ctrl Pts',(45.8897275017006,33.5016881508368,-39.6316923737189));
#251244=CARTESIAN_POINT('Ctrl Pts',(45.9210297733036,33.4795651380848,-39.6332542688506));
#251245=CARTESIAN_POINT('Ctrl Pts',(45.9823424846244,33.4339088874735,-39.6359180193303));
#251246=CARTESIAN_POINT('Ctrl Pts',(46.0724202597563,33.3632801300718,-39.6392265347984));
#251247=CARTESIAN_POINT('Ctrl Pts',(46.1850394564173,33.2606222983665,-39.6409205727319));
#251248=CARTESIAN_POINT('Ctrl Pts',(46.2638636333332,33.1772336958075,-39.6401443034625));
#251249=CARTESIAN_POINT('Ctrl Pts',(46.3151397511292,33.1201974856456,-39.6391646017005));
#251250=CARTESIAN_POINT('Ctrl Pts',(46.3401349353408,33.0909661742941,-39.6384440851485));
#251251=CARTESIAN_POINT('Ctrl Pts',(46.3888523044997,33.0309971480077,-39.6365301000439));
#251252=CARTESIAN_POINT('Ctrl Pts',(46.4123735341802,33.0005036828642,-39.6353439924849));
#251253=CARTESIAN_POINT('Ctrl Pts',(46.4576879006691,32.9386388625828,-39.6325280276393));
#251254=CARTESIAN_POINT('Ctrl Pts',(46.52311576659,32.8444620833496,-39.6276360146217));
#251255=CARTESIAN_POINT('Ctrl Pts',(46.5810426872604,32.7462345994881,-39.6207752343847));
#251256=CARTESIAN_POINT('Ctrl Pts',(46.6516918187307,32.6117039458857,-39.6098936921283));
#251257=CARTESIAN_POINT('Ctrl Pts',(46.683723185051,32.5426422373878,-39.6035832967262));
#251258=CARTESIAN_POINT('Ctrl Pts',(46.7195635412788,32.4540883209461,-39.5945936116187));
#251259=CARTESIAN_POINT('Ctrl Pts',(46.7265235775841,32.4362514419463,-39.5927383889278));
#251260=CARTESIAN_POINT('Ctrl Pts',(46.7400123459627,32.4003742100513,-39.5889189813535));
#251261=CARTESIAN_POINT('Ctrl Pts',(46.7465535157541,32.3822946053341,-39.5869502184844));
#251262=CARTESIAN_POINT('Ctrl Pts',(46.7654644360989,32.3279072933142,-39.5808958427402));
#251263=CARTESIAN_POINT('Ctrl Pts',(46.7770937339888,32.2915493874551,-39.5766741707955));
#251264=CARTESIAN_POINT('Ctrl Pts',(46.8091770518909,32.182013131159,-39.5634457571489));
#251265=CARTESIAN_POINT('Ctrl Pts',(46.8444383818759,32.034891308334,-39.5443264312115));
#251266=CARTESIAN_POINT('Ctrl Pts',(46.8650708643864,31.8856621776612,-39.5223044891954));
#251267=CARTESIAN_POINT('Ctrl Pts',(46.8750487417844,31.7729724844591,-39.50469487268));
#251268=CARTESIAN_POINT('Ctrl Pts',(46.8774570362353,31.7352651712118,-39.4986397605723));
#251269=CARTESIAN_POINT('Ctrl Pts',(46.8796767940079,31.6785286095959,-39.4892824810203));
#251270=CARTESIAN_POINT('Ctrl Pts',(46.8801843407089,31.6595724593507,-39.4861150486293));
#251271=CARTESIAN_POINT('Ctrl Pts',(46.8807312344332,31.6216180949417,-39.479690628598));
#251272=CARTESIAN_POINT('Ctrl Pts',(46.8807699646674,31.6025797052015,-39.4764266299692));
#251273=CARTESIAN_POINT('Ctrl Pts',(46.8801790388754,31.5455906639181,-39.4665317368708));
#251274=CARTESIAN_POINT('Ctrl Pts',(46.8788490796135,31.5078273383739,-39.4598096545541));
#251275=CARTESIAN_POINT('Ctrl Pts',(46.874360617844,31.4326451774338,-39.4461013696832));
#251276=CARTESIAN_POINT('Ctrl Pts',(46.864884835636,31.320441459725,-39.4251517854185));
#251277=CARTESIAN_POINT('Ctrl Pts',(46.8414902947658,31.1730719473388,-39.3956936109857));
#251278=CARTESIAN_POINT('Ctrl Pts',(46.8074810934279,31.0279105813681,-39.364717848004));
#251279=CARTESIAN_POINT('Ctrl Pts',(46.7869180083019,30.9560697433081,-39.3487190247537));
#251280=CARTESIAN_POINT('Ctrl Pts',(46.7645577771926,30.884604709384,-39.332461491893));
#251281=CARTESIAN_POINT('Ctrl Pts',(46.7524740339114,30.8490466969583,-39.3242001683612));
#251282=CARTESIAN_POINT('Ctrl Pts',(46.7264943673172,30.7783632715819,-39.3074248425479));
#251283=CARTESIAN_POINT('Ctrl Pts',(46.7127058212706,30.7435263372096,-39.2989795429224));
#251284=CARTESIAN_POINT('Ctrl Pts',(46.6981266849492,30.7091523375488,-39.2904704603133));
#251285=CARTESIAN_POINT('Ctrl Pts',(44.7926621173534,30.9780510210195,-41.4731170634489));
#251286=CARTESIAN_POINT('Ctrl Pts',(44.7841183378731,30.958431594105,-41.4560988982307));
#251287=CARTESIAN_POINT('Ctrl Pts',(44.7652574387158,30.9202429989855,-41.4215723090211));
#251288=CARTESIAN_POINT('Ctrl Pts',(44.7373647422364,30.8750641226134,-41.3772059160528));
#251289=CARTESIAN_POINT('Ctrl Pts',(44.7186826069414,30.8491098680677,-41.3500360893141));
#251290=CARTESIAN_POINT('Ctrl Pts',(44.7057896374646,30.8320666178198,-41.3317986258606));
#251291=CARTESIAN_POINT('Ctrl Pts',(44.6991283043737,30.8236797190306,-41.3226233796301));
#251292=CARTESIAN_POINT('Ctrl Pts',(44.6853430526266,30.8071501195218,-41.3041237465898));
#251293=CARTESIAN_POINT('Ctrl Pts',(44.6782604199269,30.7990587859436,-41.2948558628018));
#251294=CARTESIAN_POINT('Ctrl Pts',(44.6637865272211,30.7832912649286,-41.2763692550984));
#251295=CARTESIAN_POINT('Ctrl Pts',(44.65638232911,30.7755995480316,-41.2671331599469));
#251296=CARTESIAN_POINT('Ctrl Pts',(44.6336879630273,30.7531065345255,-41.2394625228135));
#251297=CARTESIAN_POINT('Ctrl Pts',(44.6100194582072,30.7317609779911,-41.211850451263));
#251298=CARTESIAN_POINT('Ctrl Pts',(44.5765344835469,30.7055824366946,-41.1751580074971));
#251299=CARTESIAN_POINT('Ctrl Pts',(44.5504480754,30.6870962504203,-41.147699245024));
#251300=CARTESIAN_POINT('Ctrl Pts',(44.5324056777293,30.6755504391987,-41.1294402655247));
#251301=CARTESIAN_POINT('Ctrl Pts',(44.5186168522497,30.6671837862428,-41.1157563555777));
#251302=CARTESIAN_POINT('Ctrl Pts',(44.5139760207251,30.6644431539959,-41.1111953707762));
#251303=CARTESIAN_POINT('Ctrl Pts',(44.5046579712977,30.6590892493455,-41.102125755137));
#251304=CARTESIAN_POINT('Ctrl Pts',(44.4999732573772,30.6564710151932,-41.0976094410703));
#251305=CARTESIAN_POINT('Ctrl Pts',(44.4764410055871,30.6436866063214,-41.0751408219827));
#251306=CARTESIAN_POINT('Ctrl Pts',(44.4380363426647,30.6251318507397,-41.0398401547925));
#251307=CARTESIAN_POINT('Ctrl Pts',(44.3881999640401,30.6066279457426,-40.9973473660572));
#251308=CARTESIAN_POINT('Ctrl Pts',(44.3574626802754,30.5976558165788,-40.9725988687145));
#251309=CARTESIAN_POINT('Ctrl Pts',(44.3367823836873,30.5921565153947,-40.9562701951691));
#251310=CARTESIAN_POINT('Ctrl Pts',(44.3263541271388,30.5896491085923,-40.9481956834911));
#251311=CARTESIAN_POINT('Ctrl Pts',(44.3052793937559,30.5851218575581,-40.9322027877955));
#251312=CARTESIAN_POINT('Ctrl Pts',(44.2946995104909,30.5831174982377,-40.924335654778));
#251313=CARTESIAN_POINT('Ctrl Pts',(44.2735450602529,30.5796377993431,-40.9089243529734));
#251314=CARTESIAN_POINT('Ctrl Pts',(44.2629524396991,30.5781585711684,-40.9013664771085));
#251315=CARTESIAN_POINT('Ctrl Pts',(44.2311453972639,30.5744985086998,-40.8791460851492));
#251316=CARTESIAN_POINT('Ctrl Pts',(44.2098907431643,30.5730912421562,-40.8649273724495));
#251317=CARTESIAN_POINT('Ctrl Pts',(44.1672866942957,30.5723474200962,-40.8376959485268));
#251318=CARTESIAN_POINT('Ctrl Pts',(44.1459323927671,30.5730120277702,-40.8246808510428));
#251319=CARTESIAN_POINT('Ctrl Pts',(44.1191870166623,30.5751734135742,-40.8091986194082));
#251320=CARTESIAN_POINT('Ctrl Pts',(44.1138315874482,30.5756735271978,-40.806139968135));
#251321=CARTESIAN_POINT('Ctrl Pts',(44.1031212948485,30.5768077596639,-40.8001057293845));
#251322=CARTESIAN_POINT('Ctrl Pts',(44.0977557278508,30.5774435866632,-40.7971244669688));
#251323=CARTESIAN_POINT('Ctrl Pts',(44.0817045383335,30.5795497856634,-40.7883321887253));
#251324=CARTESIAN_POINT('Ctrl Pts',(44.0710902649836,30.5812139186595,-40.7826858714375));
#251325=CARTESIAN_POINT('Ctrl Pts',(44.0394561806682,30.5869813183234,-40.7663593410916));
#251326=CARTESIAN_POINT('Ctrl Pts',(44.0082701709188,30.5942909050994,-40.7512721078743));
#251327=CARTESIAN_POINT('Ctrl Pts',(43.9675777996734,30.6070988998346,-40.7336299050859));
#251328=CARTESIAN_POINT('Ctrl Pts',(43.9375066395073,30.6182485087226,-40.721648717354));
#251329=CARTESIAN_POINT('Ctrl Pts',(43.917761614853,30.626725808719,-40.7145087645619));
#251330=CARTESIAN_POINT('Ctrl Pts',(43.8981718083816,30.6357351147044,-40.7078022579606));
#251331=CARTESIAN_POINT('Ctrl Pts',(43.8884396229394,30.6405162381665,-40.7046629153417));
#251332=CARTESIAN_POINT('Ctrl Pts',(43.8693712864522,30.6504970769624,-40.6988992879235));
#251333=CARTESIAN_POINT('Ctrl Pts',(43.8599880575193,30.6557176389023,-40.6962583786489));
#251334=CARTESIAN_POINT('Ctrl Pts',(43.8415477166501,30.6665995934339,-40.6914621347147));
#251335=CARTESIAN_POINT('Ctrl Pts',(43.8143622090585,30.6835906587784,-40.6849914969931));
#251336=CARTESIAN_POINT('Ctrl Pts',(43.7885885365895,30.7025683103525,-40.6806752166169));
#251337=CARTESIAN_POINT('Ctrl Pts',(43.7554869731093,30.7296502406846,-40.676851696754));
#251338=CARTESIAN_POINT('Ctrl Pts',(43.7395647886014,30.744083456595,-40.6759056793254));
#251339=CARTESIAN_POINT('Ctrl Pts',(43.7090440489059,30.7747854825451,-40.6760208486551));
#251340=CARTESIAN_POINT('Ctrl Pts',(43.6947173014185,30.7907796762741,-40.6770802501629));
#251341=CARTESIAN_POINT('Ctrl Pts',(43.6678443418708,30.8240220908504,-40.6811258797777));
#251342=CARTESIAN_POINT('Ctrl Pts',(43.6427576069985,30.8585127548254,-40.687098273402));
#251343=CARTESIAN_POINT('Ctrl Pts',(43.6212142380078,30.8954846730083,-40.6968894358922));
#251344=CARTESIAN_POINT('Ctrl Pts',(43.6088787182641,30.9193798597989,-40.7042205511341));
#251345=CARTESIAN_POINT('Ctrl Pts',(43.6064685586478,30.9241994859948,-40.7057484197296));
#251346=CARTESIAN_POINT('Ctrl Pts',(43.6017624551859,30.9339175659931,-40.70892606686));
#251347=CARTESIAN_POINT('Ctrl Pts',(43.5994656231147,30.9388193592268,-40.7105773965538));
#251348=CARTESIAN_POINT('Ctrl Pts',(43.5927866482525,30.953560895212,-40.7156875255853));
#251349=CARTESIAN_POINT('Ctrl Pts',(43.5844198153918,30.9733582110501,-40.72293005151));
#251350=CARTESIAN_POINT('Ctrl Pts',(43.5734440082896,31.0034822735469,-40.7350537322951));
#251351=CARTESIAN_POINT('Ctrl Pts',(43.5640181327981,31.0340244080827,-40.7484125407461));
#251352=CARTESIAN_POINT('Ctrl Pts',(43.5561284133843,31.0649820306433,-40.7629929778707));
#251353=CARTESIAN_POINT('Ctrl Pts',(43.5518912037438,31.0858969805267,-40.7735241784737));
#251354=CARTESIAN_POINT('Ctrl Pts',(43.5481682579358,31.1069510729684,-40.7844620267622));
#251355=CARTESIAN_POINT('Ctrl Pts',(43.5465635963524,31.1175527760565,-40.7901372750232));
#251356=CARTESIAN_POINT('Ctrl Pts',(43.5438765944467,31.1388768366658,-40.8018865323646));
#251357=CARTESIAN_POINT('Ctrl Pts',(43.5427912565025,31.1496493641875,-40.8079902348016));
#251358=CARTESIAN_POINT('Ctrl Pts',(43.5411674088753,31.1711124235333,-40.8204828132684));
#251359=CARTESIAN_POINT('Ctrl Pts',(43.5400805588778,31.19253758885,-40.8332822237109));
#251360=CARTESIAN_POINT('Ctrl Pts',(43.5400129658238,31.2352236668913,-40.8600695429299));
#251361=CARTESIAN_POINT('Ctrl Pts',(43.5430492497798,31.2776738375434,-40.8886047446452));
#251362=CARTESIAN_POINT('Ctrl Pts',(43.5491614319672,31.3198884817001,-40.918856387552));
#251363=CARTESIAN_POINT('Ctrl Pts',(43.5532522131496,31.3409199794841,-40.9345594064291));
#251364=CARTESIAN_POINT('Ctrl Pts',(43.5578644352119,31.361905871423,-40.9505475151733));
#251365=CARTESIAN_POINT('Ctrl Pts',(43.560439098329,31.3723994717644,-40.9587035928991));
#251366=CARTESIAN_POINT('Ctrl Pts',(43.5660648897127,31.3931449423641,-40.9751492091434));
#251367=CARTESIAN_POINT('Ctrl Pts',(43.5691234314236,31.4034342087731,-40.9834667538713));
#251368=CARTESIAN_POINT('Ctrl Pts',(43.5790202279964,31.4340221767704,-41.0086741075936));
#251369=CARTESIAN_POINT('Ctrl Pts',(43.5865808644402,31.4540562960243,-41.0258289330007));
#251370=CARTESIAN_POINT('Ctrl Pts',(43.5993606039644,31.4835727602996,-41.0520789232858));
#251371=CARTESIAN_POINT('Ctrl Pts',(43.6038584649574,31.4933175175814,-41.0609109997729));
#251372=CARTESIAN_POINT('Ctrl Pts',(43.6133480280387,31.5126460303085,-41.0787663839806));
#251373=CARTESIAN_POINT('Ctrl Pts',(43.6183219077102,31.5221915251339,-41.0877549157913));
#251374=CARTESIAN_POINT('Ctrl Pts',(43.6338406007018,31.5503182102049,-41.1147514459697));
#251375=CARTESIAN_POINT('Ctrl Pts',(43.6450116757484,31.5684678157769,-41.13285712865));
#251376=CARTESIAN_POINT('Ctrl Pts',(43.6689569093208,31.6035742491305,-41.1692591986645));
#251377=CARTESIAN_POINT('Ctrl Pts',(43.6881189975485,31.6290150958394,-41.1967078345595));
#251378=CARTESIAN_POINT('Ctrl Pts',(43.7160805799803,31.6611548911343,-41.2335986369031));
#251379=CARTESIAN_POINT('Ctrl Pts',(43.7308739938731,31.6766212732249,-41.2521403517739));
#251380=CARTESIAN_POINT('Ctrl Pts',(43.7460847706871,31.6917854492915,-41.2707364845776));
#251381=CARTESIAN_POINT('Ctrl Pts',(43.7539033240721,31.6992171694526,-41.2800648729051));
#251382=CARTESIAN_POINT('Ctrl Pts',(43.7697797892606,31.7136063232936,-41.298562009488));
#251383=CARTESIAN_POINT('Ctrl Pts',(43.7778723272806,31.7205988773597,-41.3077734720143));
#251384=CARTESIAN_POINT('Ctrl Pts',(43.8025568401133,31.7409299545529,-41.3352381600133));
#251385=CARTESIAN_POINT('Ctrl Pts',(43.8195937300504,31.7536621581445,-41.353369616892));
#251386=CARTESIAN_POINT('Ctrl Pts',(43.8547939251157,31.7774712224987,-41.3892512463859));
#251387=CARTESIAN_POINT('Ctrl Pts',(43.8820456950658,31.7940939723408,-41.4158852269725));
#251388=CARTESIAN_POINT('Ctrl Pts',(43.9105977352555,31.8088239425505,-41.4420959852738));
#251389=CARTESIAN_POINT('Ctrl Pts',(43.9299312426308,31.8182163905263,-41.4594780331231));
#251390=CARTESIAN_POINT('Ctrl Pts',(43.9397545046832,31.8226994853967,-41.4681277754213));
#251391=CARTESIAN_POINT('Ctrl Pts',(43.959476379363,31.8311327029401,-41.4851373530728));
#251392=CARTESIAN_POINT('Ctrl Pts',(43.969416794615,31.835103670887,-41.4935351095415));
#251393=CARTESIAN_POINT('Ctrl Pts',(43.9894286782948,31.8425474915593,-41.5100965816665));
#251394=CARTESIAN_POINT('Ctrl Pts',(44.0196562937352,31.8529720625538,-41.5345993599874));
#251395=CARTESIAN_POINT('Ctrl Pts',(44.0607928561344,31.8639280327151,-41.5659272170578));
#251396=CARTESIAN_POINT('Ctrl Pts',(44.0922765794535,31.8699137146658,-41.5884145416429));
#251397=CARTESIAN_POINT('Ctrl Pts',(44.1134085621028,31.8733992175668,-41.6031789442838));
#251398=CARTESIAN_POINT('Ctrl Pts',(44.1240412545,31.8748890570172,-41.6104444862381));
#251399=CARTESIAN_POINT('Ctrl Pts',(44.1401138557838,31.8767382236783,-41.6211788509405));
#251400=CARTESIAN_POINT('Ctrl Pts',(44.1454877988083,31.8772894545129,-41.6247266008247));
#251401=CARTESIAN_POINT('Ctrl Pts',(44.1562140153048,31.878256418298,-41.6317257811562));
#251402=CARTESIAN_POINT('Ctrl Pts',(44.161576905651,31.8786734249769,-41.6351843345794));
#251403=CARTESIAN_POINT('Ctrl Pts',(44.1776466456902,31.8797244502982,-41.6454258391029));
#251404=CARTESIAN_POINT('Ctrl Pts',(44.1883500092183,31.8801603696231,-41.6520850220369));
#251405=CARTESIAN_POINT('Ctrl Pts',(44.2204087008324,31.8806796234647,-41.671549250448));
#251406=CARTESIAN_POINT('Ctrl Pts',(44.2417298059497,31.8799780982567,-41.6838534602333));
#251407=CARTESIAN_POINT('Ctrl Pts',(44.2842582084951,31.8764766164199,-41.7071185815018));
#251408=CARTESIAN_POINT('Ctrl Pts',(44.3054713486111,31.8736750129732,-41.7180819683776));
#251409=CARTESIAN_POINT('Ctrl Pts',(44.3319064277948,31.8688271235064,-41.7309251637703));
#251410=CARTESIAN_POINT('Ctrl Pts',(44.3371930873745,31.8677885276791,-41.7334519256467));
#251411=CARTESIAN_POINT('Ctrl Pts',(44.3477523920959,31.8655764110726,-41.7384157665409));
#251412=CARTESIAN_POINT('Ctrl Pts',(44.353035452149,31.8644001232798,-41.7408573895762));
#251413=CARTESIAN_POINT('Ctrl Pts',(44.368821997144,31.8606750365135,-41.7480268313348));
#251414=CARTESIAN_POINT('Ctrl Pts',(44.3792318927429,31.8579388865424,-41.752586114057));
#251415=CARTESIAN_POINT('Ctrl Pts',(44.4101727404,31.8489724804825,-41.7656371280416));
#251416=CARTESIAN_POINT('Ctrl Pts',(44.4405041748167,31.8385015328462,-41.7774224567595));
#251417=CARTESIAN_POINT('Ctrl Pts',(44.4797386522914,31.8215610256552,-41.7906399779756));
#251418=CARTESIAN_POINT('Ctrl Pts',(44.5085558494592,31.8073558935676,-41.7992982329201));
#251419=CARTESIAN_POINT('Ctrl Pts',(44.5273583247585,31.7968714183439,-41.8042246106906));
#251420=CARTESIAN_POINT('Ctrl Pts',(44.5459478308046,31.7858731708475,-41.8087197459362));
#251421=CARTESIAN_POINT('Ctrl Pts',(44.5551558111633,31.7801015230391,-41.8107541019367));
#251422=CARTESIAN_POINT('Ctrl Pts',(44.5731320510561,31.7681815367951,-41.814338976855));
#251423=CARTESIAN_POINT('Ctrl Pts',(44.5819448307914,31.7620078883687,-41.8159008719862));
#251424=CARTESIAN_POINT('Ctrl Pts',(44.5991987000126,31.7492554022398,-41.8185646224661));
#251425=CARTESIAN_POINT('Ctrl Pts',(44.6245350600795,31.7295108031857,-41.8218731379338));
#251426=CARTESIAN_POINT('Ctrl Pts',(44.6561620699444,31.7007477525095,-41.8235671758672));
#251427=CARTESIAN_POINT('Ctrl Pts',(44.6782580742923,31.6773394437008,-41.8227909065983));
#251428=CARTESIAN_POINT('Ctrl Pts',(44.6926220014235,31.6613194462407,-41.8218112048364));
#251429=CARTESIAN_POINT('Ctrl Pts',(44.6996188611148,31.6531046671394,-41.8210906882841));
#251430=CARTESIAN_POINT('Ctrl Pts',(44.7132456597446,31.6362429219073,-41.8191767031797));
#251431=CARTESIAN_POINT('Ctrl Pts',(44.7198193777268,31.627664624135,-41.8179905956202));
#251432=CARTESIAN_POINT('Ctrl Pts',(44.7324727845908,31.610252798272,-41.8151746307749));
#251433=CARTESIAN_POINT('Ctrl Pts',(44.7507253937504,31.5837345714901,-41.8102826177571));
#251434=CARTESIAN_POINT('Ctrl Pts',(44.7668325292565,31.5560404782777,-41.8034218375205));
#251435=CARTESIAN_POINT('Ctrl Pts',(44.7864242741839,31.5180816884312,-41.7925402952635));
#251436=CARTESIAN_POINT('Ctrl Pts',(44.7952779235527,31.4985810718442,-41.7862298998632));
#251437=CARTESIAN_POINT('Ctrl Pts',(44.8051436066325,31.4735589245645,-41.777240214754));
#251438=CARTESIAN_POINT('Ctrl Pts',(44.8070571630202,31.4685179927861,-41.7753849920635));
#251439=CARTESIAN_POINT('Ctrl Pts',(44.8107609555809,31.4583769076679,-41.7715655844892));
#251440=CARTESIAN_POINT('Ctrl Pts',(44.8125545845603,31.4532656516023,-41.76959682162));
#251441=CARTESIAN_POINT('Ctrl Pts',(44.8177323950795,31.4378873281915,-41.7635424458753));
#251442=CARTESIAN_POINT('Ctrl Pts',(44.8209059367305,31.4276035217402,-41.7593207739311));
#251443=CARTESIAN_POINT('Ctrl Pts',(44.8296276705658,31.3966113763671,-41.7460923602843));
#251444=CARTESIAN_POINT('Ctrl Pts',(44.8391161742293,31.3549585404116,-41.7269730343471));
#251445=CARTESIAN_POINT('Ctrl Pts',(44.8444380100638,31.312658433005,-41.7049510923314));
#251446=CARTESIAN_POINT('Ctrl Pts',(44.8468637082338,31.2806969121874,-41.6873414758157));
#251447=CARTESIAN_POINT('Ctrl Pts',(44.8474108190536,31.2699990859542,-41.6812863637077));
#251448=CARTESIAN_POINT('Ctrl Pts',(44.8478348231013,31.2538978106508,-41.671929084156));
#251449=CARTESIAN_POINT('Ctrl Pts',(44.8479099202363,31.2485174556463,-41.6687616517648));
#251450=CARTESIAN_POINT('Ctrl Pts',(44.8479268208064,31.2377432265879,-41.6623372317338));
#251451=CARTESIAN_POINT('Ctrl Pts',(44.8478683021095,31.2323379437313,-41.6590732331048));
#251452=CARTESIAN_POINT('Ctrl Pts',(44.8474921214824,31.2161555213209,-41.6491783400064));
#251453=CARTESIAN_POINT('Ctrl Pts',(44.8469759958029,31.2054292064128,-41.6424562576898));
#251454=CARTESIAN_POINT('Ctrl Pts',(44.8454249887827,31.1840681958411,-41.6287479728186));
#251455=CARTESIAN_POINT('Ctrl Pts',(44.8423204600693,31.1521790951542,-41.6077983885548));
#251456=CARTESIAN_POINT('Ctrl Pts',(44.8351290816859,31.1102584040656,-41.5783402141209));
#251457=CARTESIAN_POINT('Ctrl Pts',(44.8249268329474,31.0689281614894,-41.54736445114));
#251458=CARTESIAN_POINT('Ctrl Pts',(44.8188163283608,31.0484607830594,-41.5313656278891));
#251459=CARTESIAN_POINT('Ctrl Pts',(44.8121960627665,31.028093840338,-41.5151080950287));
#251460=CARTESIAN_POINT('Ctrl Pts',(44.808629563005,31.0179567656131,-41.5068467714969));
#251461=CARTESIAN_POINT('Ctrl Pts',(44.8009827391877,30.9977990758989,-41.4900714456835));
#251462=CARTESIAN_POINT('Ctrl Pts',(44.7969340070935,30.9878607344767,-41.4816261460579));
#251463=CARTESIAN_POINT('Ctrl Pts',(44.7926621173534,30.9780510210195,-41.4731170634489));
#251464=CARTESIAN_POINT('',(42.6662672096693,32.3203213022045,-39.2608974781454));
#251465=CARTESIAN_POINT('',(42.8533186609869,32.1498328366219,-39.6198492128429));
#251466=CARTESIAN_POINT('',(42.6662672096693,32.3203213022045,-39.2608974781454));
#251467=CARTESIAN_POINT('Origin',(44.5948075437535,31.4456508901469,-39.4587542606758));
#251468=CARTESIAN_POINT('Ctrl Pts',(42.5996246294394,32.1390101092634,-39.2098678882799));
#251469=CARTESIAN_POINT('Ctrl Pts',(42.5778854323284,31.9533222655754,-39.2197530981027));
#251470=CARTESIAN_POINT('Ctrl Pts',(42.5749625469443,31.7663344672666,-39.2248889570454));
#251471=CARTESIAN_POINT('Ctrl Pts',(42.6153194208193,31.3447914220134,-39.227652546232));
#251472=CARTESIAN_POINT('Ctrl Pts',(42.6710207843962,31.1137099758597,-39.2229144237327));
#251473=CARTESIAN_POINT('Ctrl Pts',(42.8122767959315,30.7727304789194,-39.2094810818855));
#251474=CARTESIAN_POINT('Ctrl Pts',(42.8730213773354,30.6564231621241,-39.2038964044379));
#251475=CARTESIAN_POINT('Ctrl Pts',(42.9570024701842,30.5246587771562,-39.1952391038725));
#251476=CARTESIAN_POINT('Ctrl Pts',(42.9703798319536,30.5043770417005,-39.1938226714298));
#251477=CARTESIAN_POINT('Ctrl Pts',(42.9857295783759,30.4818787161795,-39.1921578967565));
#251478=CARTESIAN_POINT('Ctrl Pts',(42.9874048472462,30.4794333222496,-39.1919756969673));
#251479=CARTESIAN_POINT('Ctrl Pts',(43.0478538286388,30.3915574743341,-39.1853833703606));
#251480=CARTESIAN_POINT('Ctrl Pts',(43.1120893711745,30.3104168174511,-39.1777786535206));
#251481=CARTESIAN_POINT('Ctrl Pts',(43.2866950275929,30.1179734855588,-39.1559135146894));
#251482=CARTESIAN_POINT('Ctrl Pts',(43.4026330192994,30.0137306736984,-39.1404076188054));
#251483=CARTESIAN_POINT('Ctrl Pts',(43.7432241441741,29.7628250133007,-39.0923982295612));
#251484=CARTESIAN_POINT('Ctrl Pts',(43.9830229737115,29.6420959083149,-39.0560763077533));
#251485=CARTESIAN_POINT('Ctrl Pts',(44.236619853131,29.5589442208509,-39.0141970922745));
#251486=CARTESIAN_POINT('Ctrl Pts',(44.2366195673479,29.558943308954,-39.0141953208016));
#251487=CARTESIAN_POINT('Ctrl Pts',(44.2485133712811,29.5573147073404,-39.016338804237));
#251488=CARTESIAN_POINT('Ctrl Pts',(44.2604132202835,29.5557943338693,-39.0185056969943));
#251489=CARTESIAN_POINT('Ctrl Pts',(44.2722948154515,29.5543845957057,-39.0206914003809));
#251490=CARTESIAN_POINT('Ctrl Pts',(44.288696030367,29.5524386096434,-39.0237085197559));
#251491=CARTESIAN_POINT('Ctrl Pts',(44.3050952734897,29.5506978499007,-39.0267671710297));
#251492=CARTESIAN_POINT('Ctrl Pts',(44.3214722160119,29.5491651362618,-39.0298636173565));
#251493=CARTESIAN_POINT('Ctrl Pts',(44.386979986101,29.5430342817064,-39.0422494026637));
#251494=CARTESIAN_POINT('Ctrl Pts',(44.4523142911657,29.540165884783,-39.055264500148));
#251495=CARTESIAN_POINT('Ctrl Pts',(44.5174452018332,29.5404749664642,-39.0688802121094));
#251496=CARTESIAN_POINT('Ctrl Pts',(44.5825761125008,29.5407840481455,-39.0824959240709));
#251497=CARTESIAN_POINT('Ctrl Pts',(44.64751868345,29.5442668522271,-39.0967146367708));
#251498=CARTESIAN_POINT('Ctrl Pts',(44.7122655456777,29.5509157680261,-39.1115282314101));
#251499=CARTESIAN_POINT('Ctrl Pts',(44.7446389767916,29.5542402259256,-39.1189350287298));
#251500=CARTESIAN_POINT('Ctrl Pts',(44.7769718892781,29.5583592071516,-39.126492904595));
#251501=CARTESIAN_POINT('Ctrl Pts',(44.8092469543587,29.5632772749199,-39.1341985554972));
#251502=CARTESIAN_POINT('Ctrl Pts',(44.8415220194394,29.5681953426883,-39.1419042063993));
#251503=CARTESIAN_POINT('Ctrl Pts',(44.8737942873649,29.5739237069059,-39.1497713394166));
#251504=CARTESIAN_POINT('Ctrl Pts',(44.9059258943645,29.5804480647761,-39.1577677872645));
#251505=CARTESIAN_POINT('Ctrl Pts',(44.938057501364,29.5869724226462,-39.1657642351124));
#251506=CARTESIAN_POINT('Ctrl Pts',(44.9698454327154,29.5942479284802,-39.1738387467903));
#251507=CARTESIAN_POINT('Ctrl Pts',(45.0013540521658,29.6022690447017,-39.1820030835632));
#251508=CARTESIAN_POINT('Ctrl Pts',(45.0328626716162,29.6102901609231,-39.1901674203362));
#251509=CARTESIAN_POINT('Ctrl Pts',(45.0640729757577,29.6190530375165,-39.1984168566288));
#251510=CARTESIAN_POINT('Ctrl Pts',(45.0949896013656,29.6285455570274,-39.2067492398949));
#251511=CARTESIAN_POINT('Ctrl Pts',(45.156822852581,29.6475305960497,-39.2234140064273));
#251512=CARTESIAN_POINT('Ctrl Pts',(45.2174823675629,29.6694301295854,-39.2404109353306));
#251513=CARTESIAN_POINT('Ctrl Pts',(45.2769854784582,29.6942159135793,-39.2577349344145));
#251514=CARTESIAN_POINT('Ctrl Pts',(45.3364885893535,29.7190016975732,-39.2750589334985));
#251515=CARTESIAN_POINT('Ctrl Pts',(45.394834111845,29.7466769167217,-39.2927093736018));
#251516=CARTESIAN_POINT('Ctrl Pts',(45.4519914987675,29.7772762445693,-39.3106842688742));
#251517=CARTESIAN_POINT('Ctrl Pts',(45.4662808454981,29.7849260765312,-39.3151779926924));
#251518=CARTESIAN_POINT('Ctrl Pts',(45.4805013249128,29.7927646822922,-39.3196943067583));
#251519=CARTESIAN_POINT('Ctrl Pts',(45.4946409653392,29.8007841394154,-39.3242291145778));
#251520=CARTESIAN_POINT('Ctrl Pts',(45.5087806057656,29.8088035965387,-39.3287639223973));
#251521=CARTESIAN_POINT('Ctrl Pts',(45.5228621313133,29.8170188131519,-39.333324907199));
#251522=CARTESIAN_POINT('Ctrl Pts',(45.5368055540997,29.8253835454178,-39.3378862105147));
#251523=CARTESIAN_POINT('Ctrl Pts',(45.5646923996724,29.8421130099497,-39.3470088171461));
#251524=CARTESIAN_POINT('Ctrl Pts',(45.592047766323,29.8594467945522,-39.3561383047734));
#251525=CARTESIAN_POINT('Ctrl Pts',(45.6188977087295,29.8773827904181,-39.3652795111332));
#251526=CARTESIAN_POINT('Ctrl Pts',(45.645747651136,29.8953187862839,-39.3744207174929));
#251527=CARTESIAN_POINT('Ctrl Pts',(45.6720921468082,29.913857035864,-39.3835736164339));
#251528=CARTESIAN_POINT('Ctrl Pts',(45.6979337955271,29.9329872123234,-39.3927366395782));
#251529=CARTESIAN_POINT('Ctrl Pts',(45.723775444246,29.9521173887828,-39.4018996627226));
#251530=CARTESIAN_POINT('Ctrl Pts',(45.7491143076062,29.9718394539443,-39.4110727653601));
#251531=CARTESIAN_POINT('Ctrl Pts',(45.7739546683399,29.9921505677002,-39.4202560992287));
#251532=CARTESIAN_POINT('Ctrl Pts',(45.8068346095582,30.0190353715716,-39.4324116182663));
#251533=CARTESIAN_POINT('Ctrl Pts',(45.8388420879535,30.0469508662714,-39.4445853507697));
#251534=CARTESIAN_POINT('Ctrl Pts',(45.8699706488795,30.0759012064987,-39.4567766090453));
#251535=CARTESIAN_POINT('Ctrl Pts',(45.8699705802672,30.0759010588502,-39.4567767210169));
#251536=CARTESIAN_POINT('Ctrl Pts',(45.7207779205447,29.9782872881653,-39.4493772126299));
#251537=CARTESIAN_POINT('Ctrl Pts',(45.5599480087114,29.8999062682101,-39.443153002748));
#251538=CARTESIAN_POINT('Ctrl Pts',(45.2312083411652,29.7880737938443,-39.4337065378474));
#251539=CARTESIAN_POINT('Ctrl Pts',(45.0639383024835,29.7527249035763,-39.4303654026819));
#251540=CARTESIAN_POINT('Ctrl Pts',(44.7172828005758,29.7227187429158,-39.4261204619104));
#251541=CARTESIAN_POINT('Ctrl Pts',(44.4580078817622,29.7223780036854,-39.4233297449024));
#251542=CARTESIAN_POINT('Ctrl Pts',(43.9688200623754,29.8616791617328,-39.4312638039626));
#251543=CARTESIAN_POINT('Ctrl Pts',(43.7845565914904,29.9464353434952,-39.4372490396889));
#251544=CARTESIAN_POINT('Ctrl Pts',(43.4833583146081,30.1477786147003,-39.451636962852));
#251545=CARTESIAN_POINT('Ctrl Pts',(43.3618510615377,30.253415997476,-39.4592126441986));
#251546=CARTESIAN_POINT('Ctrl Pts',(43.2339064911603,30.3970340532892,-39.4692641092024));
#251547=CARTESIAN_POINT('Ctrl Pts',(43.2133112308633,30.4213696846452,-39.4709597499161));
#251548=CARTESIAN_POINT('Ctrl Pts',(43.1834134449199,30.4585680431386,-39.4735415640413));
#251549=CARTESIAN_POINT('Ctrl Pts',(43.1736501665408,30.4710326685332,-39.4744052149167));
#251550=CARTESIAN_POINT('Ctrl Pts',(43.1592837513826,30.4898576355279,-39.4757067642036));
#251551=CARTESIAN_POINT('Ctrl Pts',(43.1545612559406,30.4961264783958,-39.4761397377086));
#251552=CARTESIAN_POINT('Ctrl Pts',(43.1475388808391,30.5055703919114,-39.476791296143));
#251553=CARTESIAN_POINT('Ctrl Pts',(43.1452096879129,30.5087232484512,-39.4770087021575));
#251554=CARTESIAN_POINT('Ctrl Pts',(43.0728360470021,30.6073319480963,-39.4838046000217));
#251555=CARTESIAN_POINT('Ctrl Pts',(42.9826289996721,30.7481521195083,-39.4928576045613));
#251556=CARTESIAN_POINT('Ctrl Pts',(42.8339657780202,31.1281625580106,-39.5216333315955));
#251557=CARTESIAN_POINT('Ctrl Pts',(42.791434110928,31.331147172449,-39.5386487817205));
#251558=CARTESIAN_POINT('Ctrl Pts',(42.7726932000113,31.7434993189507,-39.5768149205341));
#251559=CARTESIAN_POINT('Ctrl Pts',(42.7969939924394,31.9505108240015,-39.5977725133492));
#251560=CARTESIAN_POINT('Ctrl Pts',(42.8533186609868,32.1498328366219,-39.6198492128429));
#251561=CARTESIAN_POINT('Ctrl Pts',(46.6981267205988,30.7091523325179,-39.2904704194778));
#251562=CARTESIAN_POINT('Ctrl Pts',(46.6835475840845,30.6747783323977,-39.2819613368687));
#251563=CARTESIAN_POINT('Ctrl Pts',(46.6681815313185,30.6408774203964,-39.2733908710118));
#251564=CARTESIAN_POINT('Ctrl Pts',(46.6359019577837,30.5740061471226,-39.2561284474008));
#251565=CARTESIAN_POINT('Ctrl Pts',(46.6189883510676,30.5410358371774,-39.2474364841832));
#251566=CARTESIAN_POINT('Ctrl Pts',(46.5659489722029,30.4435074198558,-39.2211790841066));
#251567=CARTESIAN_POINT('Ctrl Pts',(46.5275294727818,30.380328928234,-39.2034324856053));
#251568=CARTESIAN_POINT('Ctrl Pts',(46.4653032277899,30.2883271564893,-39.1764460813684));
#251569=CARTESIAN_POINT('Ctrl Pts',(46.4437937905871,30.2581216061217,-39.1673894453427));
#251570=CARTESIAN_POINT('Ctrl Pts',(46.3992224465595,30.1986447332673,-39.1491519818895));
#251571=CARTESIAN_POINT('Ctrl Pts',(46.3761749087066,30.1693908324035,-39.1399767356591));
#251572=CARTESIAN_POINT('Ctrl Pts',(46.3284414332219,30.1117647983971,-39.1214771026188));
#251573=CARTESIAN_POINT('Ctrl Pts',(46.303898368254,30.0835718150149,-39.1122092188305));
#251574=CARTESIAN_POINT('Ctrl Pts',(46.2537074173542,30.0286632608467,-39.0937226111275));
#251575=CARTESIAN_POINT('Ctrl Pts',(46.2280147320948,30.0018935499806,-39.0844865159759));
#251576=CARTESIAN_POINT('Ctrl Pts',(46.1492148293995,29.9236586566334,-39.0568158788424));
#251577=CARTESIAN_POINT('Ctrl Pts',(46.0943604073998,29.8742287721887,-39.0384076932709));
#251578=CARTESIAN_POINT('Ctrl Pts',(46.0086385620827,29.8041510367818,-39.0108576711398));
#251579=CARTESIAN_POINT('Ctrl Pts',(45.9794896966975,29.7814700124874,-39.0016844996603));
#251580=CARTESIAN_POINT('Ctrl Pts',(45.9200349383669,29.7374728126538,-38.9833588188378));
#251581=CARTESIAN_POINT('Ctrl Pts',(45.8897290958639,29.7161565779658,-38.9742063077404));
#251582=CARTESIAN_POINT('Ctrl Pts',(45.8279451414554,29.674906815849,-38.9559225219059));
#251583=CARTESIAN_POINT('Ctrl Pts',(45.7964751325824,29.6549785627515,-38.9467936215536));
#251584=CARTESIAN_POINT('Ctrl Pts',(45.7483486268243,29.6261284755174,-38.9331097116066));
#251585=CARTESIAN_POINT('Ctrl Pts',(45.7321473511967,29.6166840324703,-38.9285487268047));
#251586=CARTESIAN_POINT('Ctrl Pts',(45.6996106426877,29.5982459778757,-38.9194791111659));
#251587=CARTESIAN_POINT('Ctrl Pts',(45.6832490664831,29.5892352249074,-38.9149627971));
#251588=CARTESIAN_POINT('Ctrl Pts',(45.6010439366246,29.5452683808152,-38.8924941780088));
#251589=CARTESIAN_POINT('Ctrl Pts',(45.533907519743,29.5134615094348,-38.8748432564238));
#251590=CARTESIAN_POINT('Ctrl Pts',(45.3969716065162,29.4565064723111,-38.8401970944675));
#251591=CARTESIAN_POINT('Ctrl Pts',(45.3271663113639,29.4313507911438,-38.8231995021285));
#251592=CARTESIAN_POINT('Ctrl Pts',(45.220429860233,29.3986526185597,-38.7982016312344));
#251593=CARTESIAN_POINT('Ctrl Pts',(45.1845124530894,29.3885937027738,-38.7899522247438));
#251594=CARTESIAN_POINT('Ctrl Pts',(45.1119891612833,29.3701842312991,-38.7736235511978));
#251595=CARTESIAN_POINT('Ctrl Pts',(45.0754052718956,29.3618381285072,-38.76554903952));
#251596=CARTESIAN_POINT('Ctrl Pts',(45.0014448062951,29.346876060269,-38.7495561438242));
#251597=CARTESIAN_POINT('Ctrl Pts',(44.9643018758947,29.3403115329834,-38.7416890108069));
#251598=CARTESIAN_POINT('Ctrl Pts',(44.89000797099,29.3290481658209,-38.7262777090026));
#251599=CARTESIAN_POINT('Ctrl Pts',(44.8527936392512,29.32433647216,-38.7187198331373));
#251600=CARTESIAN_POINT('Ctrl Pts',(44.7410083468657,29.3129455499263,-38.6964994411784));
#251601=CARTESIAN_POINT('Ctrl Pts',(44.6662563842549,29.3089967185748,-38.6822807284784));
#251602=CARTESIAN_POINT('Ctrl Pts',(44.516312474958,29.3084067697729,-38.6550493045554));
#251603=CARTESIAN_POINT('Ctrl Pts',(44.4411031950474,29.3117699907449,-38.6420342070711));
#251604=CARTESIAN_POINT('Ctrl Pts',(44.3468378658548,29.3206689820482,-38.6265519754374));
#251605=CARTESIAN_POINT('Ctrl Pts',(44.3279589188716,29.3226883081445,-38.6234933241634));
#251606=CARTESIAN_POINT('Ctrl Pts',(44.2901960688061,29.327199484625,-38.6174590854136));
#251607=CARTESIAN_POINT('Ctrl Pts',(44.2712743965384,29.3296978696828,-38.6144778229975));
#251608=CARTESIAN_POINT('Ctrl Pts',(44.2146592806893,29.3378915763517,-38.6056855447545));
#251609=CARTESIAN_POINT('Ctrl Pts',(44.1772069521887,29.3442667356837,-38.6000392274662));
#251610=CARTESIAN_POINT('Ctrl Pts',(44.1027653093944,29.3588321365371,-38.5891548739024));
#251611=CARTESIAN_POINT('Ctrl Pts',(44.0657945493931,29.367019473238,-38.5839196795321));
#251612=CARTESIAN_POINT('Ctrl Pts',(43.9923490651605,29.3851891795989,-38.5738612044767));
#251613=CARTESIAN_POINT('Ctrl Pts',(43.9558743453872,29.3951715650289,-38.5690379266201));
#251614=CARTESIAN_POINT('Ctrl Pts',(43.8834205256851,29.4169303775312,-38.5598042071748));
#251615=CARTESIAN_POINT('Ctrl Pts',(43.8474414227296,29.4287067933557,-38.5553937623361));
#251616=CARTESIAN_POINT('Ctrl Pts',(43.7759820552624,29.4540657978905,-38.546989591198));
#251617=CARTESIAN_POINT('Ctrl Pts',(43.7405017799738,29.4676483473598,-38.542995855313));
#251618=CARTESIAN_POINT('Ctrl Pts',(43.6700470429442,29.4966453190668,-38.5354320574723));
#251619=CARTESIAN_POINT('Ctrl Pts',(43.6350719704198,29.5120610427986,-38.5318621205907));
#251620=CARTESIAN_POINT('Ctrl Pts',(43.5656410023081,29.5447591112658,-38.5251556139896));
#251621=CARTESIAN_POINT('Ctrl Pts',(43.5311319987896,29.5620794262597,-38.5220162713707));
#251622=CARTESIAN_POINT('Ctrl Pts',(43.4634866336197,29.5981758158694,-38.5162526439524));
#251623=CARTESIAN_POINT('Ctrl Pts',(43.4301834582978,29.617027635167,-38.5136117346778));
#251624=CARTESIAN_POINT('Ctrl Pts',(43.3647025802437,29.6562685498308,-38.5088154907438));
#251625=CARTESIAN_POINT('Ctrl Pts',(43.3325078138225,29.6766655352735,-38.5066584800714));
#251626=CARTESIAN_POINT('Ctrl Pts',(43.2375484215017,29.7401688684101,-38.5009063557603));
#251627=CARTESIAN_POINT('Ctrl Pts',(43.1764049159542,29.7855824410607,-38.4980285726457));
#251628=CARTESIAN_POINT('Ctrl Pts',(43.0584774050032,29.8826126065668,-38.494205052783));
#251629=CARTESIAN_POINT('Ctrl Pts',(43.0016818048319,29.9342392499254,-38.4932590353542));
#251630=CARTESIAN_POINT('Ctrl Pts',(42.8926599565938,30.0438904355498,-38.4933742046842));
#251631=CARTESIAN_POINT('Ctrl Pts',(42.8414046991196,30.1009342372681,-38.4944336061919));
#251632=CARTESIAN_POINT('Ctrl Pts',(42.745103603061,30.2193471113892,-38.4984792358066));
#251633=CARTESIAN_POINT('Ctrl Pts',(42.7000683931882,30.2807072512537,-38.5014657717858));
#251634=CARTESIAN_POINT('Ctrl Pts',(42.6161769147351,30.4076991927421,-38.509346871509));
#251635=CARTESIAN_POINT('Ctrl Pts',(42.5773225210722,30.4733365159606,-38.5142427919219));
#251636=CARTESIAN_POINT('Ctrl Pts',(42.5326943176869,30.5580963772433,-38.5215739071627));
#251637=CARTESIAN_POINT('Ctrl Pts',(42.5239673647719,30.5751883027432,-38.5231017757584));
#251638=CARTESIAN_POINT('Ctrl Pts',(42.5069121305918,30.6096437574431,-38.5262794228887));
#251639=CARTESIAN_POINT('Ctrl Pts',(42.4985805575985,30.6270190887935,-38.5279307525826));
#251640=CARTESIAN_POINT('Ctrl Pts',(42.4743295262018,30.6792614146976,-38.5330408816144));
#251641=CARTESIAN_POINT('Ctrl Pts',(42.4591077838217,30.7143247126095,-38.5366620368727));
#251642=CARTESIAN_POINT('Ctrl Pts',(42.4305062506586,30.7849297888302,-38.5443247619881));
#251643=CARTESIAN_POINT('Ctrl Pts',(42.4171273401332,30.8204683232161,-38.5483659010294));
#251644=CARTESIAN_POINT('Ctrl Pts',(42.3921836892083,30.892009947854,-38.5568599906005));
#251645=CARTESIAN_POINT('Ctrl Pts',(42.380618995835,30.9280130500868,-38.5613129523282));
#251646=CARTESIAN_POINT('Ctrl Pts',(42.3592881338188,31.0004799406419,-38.5706260495541));
#251647=CARTESIAN_POINT('Ctrl Pts',(42.3495219836973,31.036943733628,-38.5754861898888));
#251648=CARTESIAN_POINT('Ctrl Pts',(42.3317857266679,31.110331516506,-38.585611932928));
#251649=CARTESIAN_POINT('Ctrl Pts',(42.3238156113846,31.147255504153,-38.5908775345026));
#251650=CARTESIAN_POINT('Ctrl Pts',(42.3096820195686,31.2215665470911,-38.6018153827909));
#251651=CARTESIAN_POINT('Ctrl Pts',(42.3035171636528,31.258971534054,-38.6074906310522));
#251652=CARTESIAN_POINT('Ctrl Pts',(42.293023529039,31.3341791446678,-38.6192398883933));
#251653=CARTESIAN_POINT('Ctrl Pts',(42.2886817840459,31.3721585400728,-38.6253435908304));
#251654=CARTESIAN_POINT('Ctrl Pts',(42.2819306070517,31.4478003682479,-38.6378361692971));
#251655=CARTESIAN_POINT('Ctrl Pts',(42.2795025001241,31.4855415035392,-38.6442359720864));
#251656=CARTESIAN_POINT('Ctrl Pts',(42.2765060406855,31.560848596424,-38.6573322314144));
#251657=CARTESIAN_POINT('Ctrl Pts',(42.2759365326951,31.5984178369017,-38.664029078225));
#251658=CARTESIAN_POINT('Ctrl Pts',(42.2769710380182,31.7108769251965,-38.6845569897124));
#251659=CARTESIAN_POINT('Ctrl Pts',(42.2813124523233,31.7855186497121,-38.6988245267215));
#251660=CARTESIAN_POINT('Ctrl Pts',(42.2932530869353,31.8969906246886,-38.721084142073));
#251661=CARTESIAN_POINT('Ctrl Pts',(42.2981395716803,31.9340660421392,-38.7286473137566));
#251662=CARTESIAN_POINT('Ctrl Pts',(42.3097367545214,32.0080522410799,-38.744060932418));
#251663=CARTESIAN_POINT('Ctrl Pts',(42.316449417552,32.0449687734335,-38.7519127624581));
#251664=CARTESIAN_POINT('Ctrl Pts',(42.3317154350232,32.1186122283265,-38.7679008712022));
#251665=CARTESIAN_POINT('Ctrl Pts',(42.3402956415526,32.1554227729715,-38.7760569489278));
#251666=CARTESIAN_POINT('Ctrl Pts',(42.3591481488484,32.2281691763966,-38.7925025651723));
#251667=CARTESIAN_POINT('Ctrl Pts',(42.3694448123762,32.2642363057195,-38.8008201099004));
#251668=CARTESIAN_POINT('Ctrl Pts',(42.3917427778168,32.3356900843468,-38.8176250123815));
#251669=CARTESIAN_POINT('Ctrl Pts',(42.4037464930944,32.3710895501939,-38.8261151112762));
#251670=CARTESIAN_POINT('Ctrl Pts',(42.4294540323857,32.4412374478768,-38.8432687473174));
#251671=CARTESIAN_POINT('Ctrl Pts',(42.4431578632506,32.4759858769281,-38.8519322857914));
#251672=CARTESIAN_POINT('Ctrl Pts',(42.4722684831154,32.544830817777,-38.8694322793142));
#251673=CARTESIAN_POINT('Ctrl Pts',(42.4876674595477,32.5789106003817,-38.8782643558018));
#251674=CARTESIAN_POINT('Ctrl Pts',(42.5202146386211,32.6464796024254,-38.8961197400092));
#251675=CARTESIAN_POINT('Ctrl Pts',(42.5373018066979,32.6798350239254,-38.905108271819));
#251676=CARTESIAN_POINT('Ctrl Pts',(42.5906929217761,32.7780784192159,-38.9321048020009));
#251677=CARTESIAN_POINT('Ctrl Pts',(42.6292257708725,32.8414173960492,-38.950210484678));
#251678=CARTESIAN_POINT('Ctrl Pts',(42.7119999890155,32.9638220806952,-38.986612554694));
#251679=CARTESIAN_POINT('Ctrl Pts',(42.7562439154297,33.0229003618273,-39.004911678637));
#251680=CARTESIAN_POINT('Ctrl Pts',(42.826900203736,33.1083283039828,-39.0325062641257));
#251681=CARTESIAN_POINT('Ctrl Pts',(42.851168465327,33.1362718837218,-39.041728825905));
#251682=CARTESIAN_POINT('Ctrl Pts',(42.9011535381211,33.1910822095534,-39.0602231613282));
#251683=CARTESIAN_POINT('Ctrl Pts',(42.926867323379,33.2179450513447,-39.0694937078027));
#251684=CARTESIAN_POINT('Ctrl Pts',(42.9797816918549,33.2705900752688,-39.0880898406065));
#251685=CARTESIAN_POINT('Ctrl Pts',(43.0069971956867,33.2963737293151,-39.0974182289335));
#251686=CARTESIAN_POINT('Ctrl Pts',(43.0622936266078,33.3462615675182,-39.1159153655173));
#251687=CARTESIAN_POINT('Ctrl Pts',(43.0904949817445,33.3704877056864,-39.1251268280428));
#251688=CARTESIAN_POINT('Ctrl Pts',(43.1765625947351,33.4408730461757,-39.1525915160431));
#251689=CARTESIAN_POINT('Ctrl Pts',(43.2360245424999,33.4848790767991,-39.1707229729204));
#251690=CARTESIAN_POINT('Ctrl Pts',(43.3282503204797,33.5464830400295,-39.1976341950415));
#251691=CARTESIAN_POINT('Ctrl Pts',(43.359502217261,33.566285970248,-39.206558164691));
#251692=CARTESIAN_POINT('Ctrl Pts',(43.4230323912785,33.6044189036262,-39.2243131706243));
#251693=CARTESIAN_POINT('Ctrl Pts',(43.4553106240002,33.6227489710991,-39.2331442099428));
#251694=CARTESIAN_POINT('Ctrl Pts',(43.5209070176006,33.65791645796,-39.2507127455309));
#251695=CARTESIAN_POINT('Ctrl Pts',(43.5542222307926,33.6747516859435,-39.2594493413026));
#251696=CARTESIAN_POINT('Ctrl Pts',(43.6219256372691,33.706907422375,-39.276831389152));
#251697=CARTESIAN_POINT('Ctrl Pts',(43.6563381426909,33.722228682357,-39.2854811314501));
#251698=CARTESIAN_POINT('Ctrl Pts',(43.7254519126727,33.7509935119824,-39.3024907091016));
#251699=CARTESIAN_POINT('Ctrl Pts',(43.7602995409721,33.764508496929,-39.3108884655704));
#251700=CARTESIAN_POINT('Ctrl Pts',(43.8304781054344,33.7897808733701,-39.3274499376954));
#251701=CARTESIAN_POINT('Ctrl Pts',(43.8658243260975,33.8015455969846,-39.3356175899088));
#251702=CARTESIAN_POINT('Ctrl Pts',(43.9726293596981,33.8342393544862,-39.3597845122642));
#251703=CARTESIAN_POINT('Ctrl Pts',(44.0448528415367,33.8525737793304,-39.3754484613995));
#251704=CARTESIAN_POINT('Ctrl Pts',(44.1547335175137,33.8748267811095,-39.3982721883298));
#251705=CARTESIAN_POINT('Ctrl Pts',(44.1916183742053,33.881368352274,-39.4057678976717));
#251706=CARTESIAN_POINT('Ctrl Pts',(44.265912298769,33.8926703342681,-39.4205323003128));
#251707=CARTESIAN_POINT('Ctrl Pts',(44.3033049254971,33.8974289036774,-39.4277978422667));
#251708=CARTESIAN_POINT('Ctrl Pts',(44.3598453618029,33.90320513239,-39.4385322069694));
#251709=CARTESIAN_POINT('Ctrl Pts',(44.3787527202319,33.9049006542695,-39.4420799568534));
#251710=CARTESIAN_POINT('Ctrl Pts',(44.4164967923385,33.9078161553301,-39.4490791371853));
#251711=CARTESIAN_POINT('Ctrl Pts',(44.4353708520081,33.9090401337743,-39.4525376906084));
#251712=CARTESIAN_POINT('Ctrl Pts',(44.4919347238328,33.9120095641989,-39.4627791951316));
#251713=CARTESIAN_POINT('Ctrl Pts',(44.5296205555248,33.9130584788855,-39.4694383780658));
#251714=CARTESIAN_POINT('Ctrl Pts',(44.6425299080792,33.9134343306132,-39.4889026064771));
#251715=CARTESIAN_POINT('Ctrl Pts',(44.7176656318032,33.9100024232635,-39.5012068162623));
#251716=CARTESIAN_POINT('Ctrl Pts',(44.8676233385802,33.8957625915874,-39.5244719375305));
#251717=CARTESIAN_POINT('Ctrl Pts',(44.9424659719907,33.8849486120956,-39.5354353244078));
#251718=CARTESIAN_POINT('Ctrl Pts',(45.0357885284359,33.8667000217447,-39.5482785197989));
#251719=CARTESIAN_POINT('Ctrl Pts',(45.0544546477979,33.8628075156194,-39.5508052816758));
#251720=CARTESIAN_POINT('Ctrl Pts',(45.0917431164945,33.8545484532422,-39.5557691225697));
#251721=CARTESIAN_POINT('Ctrl Pts',(45.1104022686543,33.850171692167,-39.5582107456052));
#251722=CARTESIAN_POINT('Ctrl Pts',(45.1661672274775,33.8363538673165,-39.5653801873635));
#251723=CARTESIAN_POINT('Ctrl Pts',(45.2029511272889,33.8262578730812,-39.5699394700858));
#251724=CARTESIAN_POINT('Ctrl Pts',(45.2758616079105,33.8042966073194,-39.5786401460756));
#251725=CARTESIAN_POINT('Ctrl Pts',(45.311968730411,33.7924363563062,-39.5827790715619));
#251726=CARTESIAN_POINT('Ctrl Pts',(45.3834929256923,33.7669724612522,-39.590638826668));
#251727=CARTESIAN_POINT('Ctrl Pts',(45.4189099909314,33.7533687979858,-39.5943596509345));
#251728=CARTESIAN_POINT('Ctrl Pts',(45.4890551389974,33.724420965446,-39.6013847400349));
#251729=CARTESIAN_POINT('Ctrl Pts',(45.523783224749,33.7090768034382,-39.6046890060346));
#251730=CARTESIAN_POINT('Ctrl Pts',(45.5925464395182,33.676638101801,-39.6108793832571));
#251731=CARTESIAN_POINT('Ctrl Pts',(45.6265815821811,33.6595435965646,-39.6137655022888));
#251732=CARTESIAN_POINT('Ctrl Pts',(45.6939497482673,33.6235812098373,-39.6191147790932));
#251733=CARTESIAN_POINT('Ctrl Pts',(45.7272861171773,33.6047101609453,-39.6215779667197));
#251734=CARTESIAN_POINT('Ctrl Pts',(45.7932287598473,33.5651706172408,-39.626073101965));
#251735=CARTESIAN_POINT('Ctrl Pts',(45.8259059486925,33.5444453725487,-39.6281074579657));
#251736=CARTESIAN_POINT('Ctrl Pts',(45.889727526333,33.5016881832693,-39.6316923328834));
#251737=CARTESIAN_POINT('Ctrl Pts',(45.9210297983567,33.4795651702188,-39.6332542280151));
#251738=CARTESIAN_POINT('Ctrl Pts',(45.9823425105019,33.4339089189919,-39.6359179784948));
#251739=CARTESIAN_POINT('Ctrl Pts',(46.0123687882815,33.4103663991699,-39.6370209490844));
#251740=CARTESIAN_POINT('Ctrl Pts',(46.1005740843723,33.3376145658878,-39.6396496275905));
#251741=CARTESIAN_POINT('Ctrl Pts',(46.1568837934186,33.2862857741618,-39.6404966874468));
#251742=CARTESIAN_POINT('Ctrl Pts',(46.2375893334767,33.2050303747233,-39.640403167924));
#251743=CARTESIAN_POINT('Ctrl Pts',(46.2638636629985,33.1772337238693,-39.6401442626271));
#251744=CARTESIAN_POINT('Ctrl Pts',(46.3151397814851,33.1201975129399,-39.639164560865));
#251745=CARTESIAN_POINT('Ctrl Pts',(46.3401349660335,33.0909662011952,-39.6384440443131));
#251746=CARTESIAN_POINT('Ctrl Pts',(46.3888523358489,33.0309971741023,-39.6365300592084));
#251747=CARTESIAN_POINT('Ctrl Pts',(46.4123735658465,33.0005037085489,-39.6353439516494));
#251748=CARTESIAN_POINT('Ctrl Pts',(46.4576879329464,32.9386388874358,-39.6325279868037));
#251749=CARTESIAN_POINT('Ctrl Pts',(46.4794980193706,32.9072464072476,-39.63089741826));
#251750=CARTESIAN_POINT('Ctrl Pts',(46.5424231785881,32.8117200519201,-39.6253488421165));
#251751=CARTESIAN_POINT('Ctrl Pts',(46.5810427212027,32.7462346217556,-39.6207751935492));
#251752=CARTESIAN_POINT('Ctrl Pts',(46.6516918536282,32.6117039663465,-39.6098936512928));
#251753=CARTESIAN_POINT('Ctrl Pts',(46.6837232203822,32.5426422569213,-39.6035832558907));
#251754=CARTESIAN_POINT('Ctrl Pts',(46.719563577096,32.4540883392911,-39.5945935707833));
#251755=CARTESIAN_POINT('Ctrl Pts',(46.7265236134956,32.4362514600518,-39.5927383480922));
#251756=CARTESIAN_POINT('Ctrl Pts',(46.7400123820574,32.4003742276752,-39.588918940518));
#251757=CARTESIAN_POINT('Ctrl Pts',(46.7465535519376,32.3822946227154,-39.5869501776489));
#251758=CARTESIAN_POINT('Ctrl Pts',(46.7654644725393,32.3279073099657,-39.5808958019048));
#251759=CARTESIAN_POINT('Ctrl Pts',(46.7770937705874,32.2915494036189,-39.57667412996));
#251760=CARTESIAN_POINT('Ctrl Pts',(46.7984826494802,32.2185252317751,-39.5678551875289));
#251761=CARTESIAN_POINT('Ctrl Pts',(46.8082357339547,32.1818782773392,-39.5632601045207));
#251762=CARTESIAN_POINT('Ctrl Pts',(46.8258916494835,32.1083194173387,-39.5537041356314));
#251763=CARTESIAN_POINT('Ctrl Pts',(46.8337943715014,32.0714074960361,-39.548743229206));
#251764=CARTESIAN_POINT('Ctrl Pts',(46.854754879426,31.9602784901863,-39.533315750657));
#251765=CARTESIAN_POINT('Ctrl Pts',(46.8650709021906,31.8856621883816,-39.5223044483599));
#251766=CARTESIAN_POINT('Ctrl Pts',(46.87504877973,31.7729724936691,-39.5046948318446));
#251767=CARTESIAN_POINT('Ctrl Pts',(46.8774570742158,31.7352651799165,-39.4986397197368));
#251768=CARTESIAN_POINT('Ctrl Pts',(46.879676832022,31.6785286175404,-39.4892824401848));
#251769=CARTESIAN_POINT('Ctrl Pts',(46.880184378731,31.6595724670412,-39.4861150077938));
#251770=CARTESIAN_POINT('Ctrl Pts',(46.8807312724654,31.6216181021237,-39.4796905877625));
#251771=CARTESIAN_POINT('Ctrl Pts',(46.8807700027013,31.6025797121284,-39.4764265891337));
#251772=CARTESIAN_POINT('Ctrl Pts',(46.8801790769053,31.5455906700815,-39.4665316960354));
#251773=CARTESIAN_POINT('Ctrl Pts',(46.8788491176281,31.5078273440315,-39.4598096137186));
#251774=CARTESIAN_POINT('Ctrl Pts',(46.8743606558037,31.4326451820844,-39.4461013288477));
#251775=CARTESIAN_POINT('Ctrl Pts',(46.8712025098556,31.3952438492793,-39.4391181973417));
#251776=CARTESIAN_POINT('Ctrl Pts',(46.8590349081897,31.2835993602235,-39.4177870145467));
#251777=CARTESIAN_POINT('Ctrl Pts',(46.8473376665826,31.2099145965172,-39.4030579339673));
#251778=CARTESIAN_POINT('Ctrl Pts',(46.8244864324902,31.1004910083645,-39.380205766645));
#251779=CARTESIAN_POINT('Ctrl Pts',(46.8159836152412,31.0642007178987,-39.3724617450316));
#251780=CARTESIAN_POINT('Ctrl Pts',(46.7971994649713,30.9919902975437,-39.356718397465));
#251781=CARTESIAN_POINT('Ctrl Pts',(46.7869180451234,30.9560697415795,-39.3487189839183));
#251782=CARTESIAN_POINT('Ctrl Pts',(46.7645578137196,30.8846047066995,-39.3324614510575));
#251783=CARTESIAN_POINT('Ctrl Pts',(46.7524740702791,30.8490466937981,-39.3242001275257));
#251784=CARTESIAN_POINT('Ctrl Pts',(46.7264944033419,30.7783632674765,-39.3074248017124));
#251785=CARTESIAN_POINT('Ctrl Pts',(46.7127058571131,30.7435263326383,-39.298979502087));
#251786=CARTESIAN_POINT('Ctrl Pts',(46.6981267205988,30.7091523325179,-39.2904704194778));
#251787=CARTESIAN_POINT('Ctrl Pts',(46.3487357027272,30.7584583056228,-39.6906862677766));
#251788=CARTESIAN_POINT('Ctrl Pts',(46.3360465301806,30.7285884779263,-39.6821771851674));
#251789=CARTESIAN_POINT('Ctrl Pts',(46.322674012045,30.6991291081308,-39.6736067193105));
#251790=CARTESIAN_POINT('Ctrl Pts',(46.2945851820176,30.641017718271,-39.6563442956996));
#251791=CARTESIAN_POINT('Ctrl Pts',(46.2798687954904,30.612365742748,-39.6476523324819));
#251792=CARTESIAN_POINT('Ctrl Pts',(46.2337236139186,30.5276092756908,-39.6213949324054));
#251793=CARTESIAN_POINT('Ctrl Pts',(46.2003029919731,30.4727017306776,-39.603648333904));
#251794=CARTESIAN_POINT('Ctrl Pts',(46.1461801500453,30.3927400894707,-39.5766619296672));
#251795=CARTESIAN_POINT('Ctrl Pts',(46.1274728516574,30.3664867733569,-39.5676052936415));
#251796=CARTESIAN_POINT('Ctrl Pts',(46.0887101379817,30.3147906415192,-39.5493678301882));
#251797=CARTESIAN_POINT('Ctrl Pts',(46.0686672178747,30.2893629692206,-39.5401925839578));
#251798=CARTESIAN_POINT('Ctrl Pts',(46.0271585782785,30.2392724858907,-39.5216929509175));
#251799=CARTESIAN_POINT('Ctrl Pts',(46.0058171042466,30.2147653940616,-39.5124250671292));
#251800=CARTESIAN_POINT('Ctrl Pts',(45.9621753273889,30.1670338430194,-39.4939384594262));
#251801=CARTESIAN_POINT('Ctrl Pts',(45.9398360673935,30.1437623234713,-39.4847023642746));
#251802=CARTESIAN_POINT('Ctrl Pts',(45.8713238239452,30.0757484083058,-39.4570317271412));
#251803=CARTESIAN_POINT('Ctrl Pts',(45.8236343202356,30.0327728117785,-39.4386235415696));
#251804=CARTESIAN_POINT('Ctrl Pts',(45.7491141599547,29.9718399517963,-39.4110735194385));
#251805=CARTESIAN_POINT('Ctrl Pts',(45.7237751109832,29.9521177433449,-39.401900347959));
#251806=CARTESIAN_POINT('Ctrl Pts',(45.672092787902,29.9138581053763,-39.3835746671366));
#251807=CARTESIAN_POINT('Ctrl Pts',(45.6457495575596,29.8953206245202,-39.3744221560391));
#251808=CARTESIAN_POINT('Ctrl Pts',(45.5920456528258,29.8594459358056,-39.3561383702047));
#251809=CARTESIAN_POINT('Ctrl Pts',(45.5646920216606,29.842113315145,-39.3470094698523));
#251810=CARTESIAN_POINT('Ctrl Pts',(45.52286176357,29.8170191244728,-39.3333255599053));
#251811=CARTESIAN_POINT('Ctrl Pts',(45.5087802414794,29.8088039098643,-39.3287645751035));
#251812=CARTESIAN_POINT('Ctrl Pts',(45.48050096757,29.7927649995304,-39.3196949594646));
#251813=CARTESIAN_POINT('Ctrl Pts',(45.4662804916472,29.7849263956811,-39.3151786453986));
#251814=CARTESIAN_POINT('Ctrl Pts',(45.3948337755398,29.7466772451965,-39.2927100263081));
#251815=CARTESIAN_POINT('Ctrl Pts',(45.3364866021309,29.7190013424949,-39.2750591047224));
#251816=CARTESIAN_POINT('Ctrl Pts',(45.2174835285277,29.6694316700735,-39.2404129427663));
#251817=CARTESIAN_POINT('Ctrl Pts',(45.156822585129,29.6475313681073,-39.2234153504273));
#251818=CARTESIAN_POINT('Ctrl Pts',(45.0640726127793,29.6190533635405,-39.1984174795332));
#251819=CARTESIAN_POINT('Ctrl Pts',(45.0328624242923,29.6102905224853,-39.1901680730424));
#251820=CARTESIAN_POINT('Ctrl Pts',(44.9698452008949,29.594248293903,-39.1738393994966));
#251821=CARTESIAN_POINT('Ctrl Pts',(44.9380572773652,29.5869727898151,-39.1657648878187));
#251822=CARTESIAN_POINT('Ctrl Pts',(44.8737940791812,29.5739240771953,-39.1497719921229));
#251823=CARTESIAN_POINT('Ctrl Pts',(44.8415218191992,29.5681957143413,-39.1419048591056));
#251824=CARTESIAN_POINT('Ctrl Pts',(44.7769717049288,29.5583595811323,-39.1264935573013));
#251825=CARTESIAN_POINT('Ctrl Pts',(44.7446388004034,29.554240600873,-39.118935681436));
#251826=CARTESIAN_POINT('Ctrl Pts',(44.6475185309788,29.5442672294863,-39.0967152894771));
#251827=CARTESIAN_POINT('Ctrl Pts',(44.5825759760276,29.5407844261647,-39.0824965767772));
#251828=CARTESIAN_POINT('Ctrl Pts',(44.4523141867918,29.5401662627562,-39.0552651528542));
#251829=CARTESIAN_POINT('Ctrl Pts',(44.3869798978321,29.5430346588726,-39.0422500553699));
#251830=CARTESIAN_POINT('Ctrl Pts',(44.3050952054121,29.5506982250521,-39.026767823736));
#251831=CARTESIAN_POINT('Ctrl Pts',(44.2886959663336,29.5524389843404,-39.0237091724622));
#251832=CARTESIAN_POINT('Ctrl Pts',(44.2558935445924,29.5563309554553,-39.0176749337123));
#251833=CARTESIAN_POINT('Ctrl Pts',(44.2394575555595,29.5584878169524,-39.0146936712963));
#251834=CARTESIAN_POINT('Ctrl Pts',(44.1902803482843,29.5655653021513,-39.0059013930531));
#251835=CARTESIAN_POINT('Ctrl Pts',(44.1577491163975,29.5710766352626,-39.000255075765));
#251836=CARTESIAN_POINT('Ctrl Pts',(44.0930902835475,29.5836763028609,-38.9893707222011));
#251837=CARTESIAN_POINT('Ctrl Pts',(44.0609787991037,29.5907621271768,-38.9841355278308));
#251838=CARTESIAN_POINT('Ctrl Pts',(43.9971881339881,29.6064933938242,-38.9740770527754));
#251839=CARTESIAN_POINT('Ctrl Pts',(43.9655089572005,29.6151388498521,-38.9692537749189));
#251840=CARTESIAN_POINT('Ctrl Pts',(43.9025825453534,29.6339885284277,-38.9600200554735));
#251841=CARTESIAN_POINT('Ctrl Pts',(43.8713353076576,29.6441927411959,-38.9556096106348));
#251842=CARTESIAN_POINT('Ctrl Pts',(43.8092755782281,29.6661704841714,-38.9472054394967));
#251843=CARTESIAN_POINT('Ctrl Pts',(43.7784630771063,29.6779439802752,-38.9432117036118));
#251844=CARTESIAN_POINT('Ctrl Pts',(43.717278897594,29.7030826309711,-38.935647905771));
#251845=CARTESIAN_POINT('Ctrl Pts',(43.6869066895965,29.7164489157022,-38.9320779688894));
#251846=CARTESIAN_POINT('Ctrl Pts',(43.626614728406,29.7448033501699,-38.9253714622882));
#251847=CARTESIAN_POINT('Ctrl Pts',(43.5966488676322,29.7598244459156,-38.9222321196694));
#251848=CARTESIAN_POINT('Ctrl Pts',(43.5379107146287,29.7911322192132,-38.9164684922511));
#251849=CARTESIAN_POINT('Ctrl Pts',(43.5089935637976,29.807484575191,-38.9138275829765));
#251850=CARTESIAN_POINT('Ctrl Pts',(43.4521381627742,29.8415255160901,-38.9090313390425));
#251851=CARTESIAN_POINT('Ctrl Pts',(43.4241850948297,29.8592209427306,-38.9068743283701));
#251852=CARTESIAN_POINT('Ctrl Pts',(43.3417392436055,29.9143171533634,-38.901122204059));
#251853=CARTESIAN_POINT('Ctrl Pts',(43.2886565200899,29.9537233898351,-38.8982444209444));
#251854=CARTESIAN_POINT('Ctrl Pts',(43.1862829187094,30.0379276623574,-38.8944209010817));
#251855=CARTESIAN_POINT('Ctrl Pts',(43.1369819758927,30.0827344207114,-38.8934748836529));
#251856=CARTESIAN_POINT('Ctrl Pts',(43.042354298069,30.1779092800836,-38.8935900529829));
#251857=CARTESIAN_POINT('Ctrl Pts',(42.9978703496345,30.2274261173575,-38.8946494544906));
#251858=CARTESIAN_POINT('Ctrl Pts',(42.9142997798964,30.3302219112651,-38.8986950841053));
#251859=CARTESIAN_POINT('Ctrl Pts',(42.8752223854268,30.3834931157852,-38.9016816200845));
#251860=CARTESIAN_POINT('Ctrl Pts',(42.8024383095261,30.4937511191122,-38.9095627198077));
#251861=CARTESIAN_POINT('Ctrl Pts',(42.7687332609551,30.5507427160192,-38.9144586402205));
#251862=CARTESIAN_POINT('Ctrl Pts',(42.7300263292576,30.6243422699748,-38.9217897554615));
#251863=CARTESIAN_POINT('Ctrl Pts',(42.7224576402308,30.6391839142897,-38.9233176240571));
#251864=CARTESIAN_POINT('Ctrl Pts',(42.7076667752466,30.6691034586862,-38.9264952711875));
#251865=CARTESIAN_POINT('Ctrl Pts',(42.7004417482736,30.6841916091719,-38.9281466008814));
#251866=CARTESIAN_POINT('Ctrl Pts',(42.6794127755329,30.7295576912778,-38.9332567299131));
#251867=CARTESIAN_POINT('Ctrl Pts',(42.6662150606011,30.7600066923132,-38.9368778851714));
#251868=CARTESIAN_POINT('Ctrl Pts',(42.6414200236241,30.8213217799634,-38.9445406102868));
#251869=CARTESIAN_POINT('Ctrl Pts',(42.629823463925,30.8521850491422,-38.9485817493281));
#251870=CARTESIAN_POINT('Ctrl Pts',(42.6082065832887,30.9143165573564,-38.9570758388993));
#251871=CARTESIAN_POINT('Ctrl Pts',(42.5981863032189,30.9455848068317,-38.961528800627));
#251872=CARTESIAN_POINT('Ctrl Pts',(42.5797083779644,31.0085229028534,-38.9708418978528));
#251873=CARTESIAN_POINT('Ctrl Pts',(42.571250748879,31.0401927534638,-38.9757020381876));
#251874=CARTESIAN_POINT('Ctrl Pts',(42.5558959598811,31.103933624688,-38.9858277812267));
#251875=CARTESIAN_POINT('Ctrl Pts',(42.5489987926973,31.1360046433454,-38.9910933828013));
#251876=CARTESIAN_POINT('Ctrl Pts',(42.5367741244054,31.2005503513038,-39.0020312310896));
#251877=CARTESIAN_POINT('Ctrl Pts',(42.531445437756,31.2330406174058,-39.0077064793509));
#251878=CARTESIAN_POINT('Ctrl Pts',(42.5223832479161,31.2983679981005,-39.0194557366921));
#251879=CARTESIAN_POINT('Ctrl Pts',(42.5186386063126,31.3313586704159,-39.0255594391291));
#251880=CARTESIAN_POINT('Ctrl Pts',(42.5128275899613,31.3970661365692,-39.0380520175959));
#251881=CARTESIAN_POINT('Ctrl Pts',(42.5107450488446,31.4298512876605,-39.0444518203851));
#251882=CARTESIAN_POINT('Ctrl Pts',(42.5081952999573,31.495270824389,-39.0575480797132));
#251883=CARTESIAN_POINT('Ctrl Pts',(42.507727090815,31.5279080610915,-39.0642449265238));
#251884=CARTESIAN_POINT('Ctrl Pts',(42.5087049855303,31.625605856974,-39.084772838011));
#251885=CARTESIAN_POINT('Ctrl Pts',(42.5125287224658,31.6904529409863,-39.0990403750203));
#251886=CARTESIAN_POINT('Ctrl Pts',(42.5229793717988,31.7873014338719,-39.1212999903717));
#251887=CARTESIAN_POINT('Ctrl Pts',(42.527250083485,31.8195137897082,-39.1288631620553));
#251888=CARTESIAN_POINT('Ctrl Pts',(42.5373759630957,31.8837968383997,-39.1442767807167));
#251889=CARTESIAN_POINT('Ctrl Pts',(42.5432328418803,31.9158725287012,-39.1521286107568));
#251890=CARTESIAN_POINT('Ctrl Pts',(42.5565453513116,31.979860553896,-39.1681167195009));
#251891=CARTESIAN_POINT('Ctrl Pts',(42.5640243655532,32.0118455541873,-39.1762727972266));
#251892=CARTESIAN_POINT('Ctrl Pts',(42.5804515873162,32.0750569293471,-39.192718413471));
#251893=CARTESIAN_POINT('Ctrl Pts',(42.5894210497274,32.1063973617025,-39.2010359581991));
#251894=CARTESIAN_POINT('Ctrl Pts',(42.6088402032077,32.1684883139446,-39.2178408606802));
#251895=CARTESIAN_POINT('Ctrl Pts',(42.619291999646,32.1992499698161,-39.2263309595749));
#251896=CARTESIAN_POINT('Ctrl Pts',(42.6416719105595,32.2602089363087,-39.2434845956161));
#251897=CARTESIAN_POINT('Ctrl Pts',(42.6536000309827,32.2904062445222,-39.2521481340902));
#251898=CARTESIAN_POINT('Ctrl Pts',(42.6789350686126,32.3502357398653,-39.269648127613));
#251899=CARTESIAN_POINT('Ctrl Pts',(42.6923351877516,32.3798533880106,-39.2784802041006));
#251900=CARTESIAN_POINT('Ctrl Pts',(42.7206544615113,32.438576886634,-39.296335588308));
#251901=CARTESIAN_POINT('Ctrl Pts',(42.735520505061,32.4675664571484,-39.305324120118));
#251902=CARTESIAN_POINT('Ctrl Pts',(42.781967232886,32.5529530674262,-39.3323206502992));
#251903=CARTESIAN_POINT('Ctrl Pts',(42.8154829548893,32.6080060018973,-39.3504263329769));
#251904=CARTESIAN_POINT('Ctrl Pts',(42.8874701351811,32.7144034488201,-39.3868284029926));
#251905=CARTESIAN_POINT('Ctrl Pts',(42.9259438236345,32.7657588863051,-39.4051275269359));
#251906=CARTESIAN_POINT('Ctrl Pts',(42.9873790455293,32.8400241153901,-39.4327221124244));
#251907=CARTESIAN_POINT('Ctrl Pts',(43.0084791885273,32.8643171580889,-39.4419446742037));
#251908=CARTESIAN_POINT('Ctrl Pts',(43.0519370354341,32.9119687254291,-39.4604390096269));
#251909=CARTESIAN_POINT('Ctrl Pts',(43.0742921081275,32.9353238560783,-39.4697095561015));
#251910=CARTESIAN_POINT('Ctrl Pts',(43.1202930465425,32.9810962928332,-39.4883056889052));
#251911=CARTESIAN_POINT('Ctrl Pts',(43.1439518743549,33.0035148878545,-39.4976340772323));
#251912=CARTESIAN_POINT('Ctrl Pts',(43.1920201563362,33.0468935936175,-39.516131213816));
#251913=CARTESIAN_POINT('Ctrl Pts',(43.2165343057023,33.067959736328,-39.5253426763416));
#251914=CARTESIAN_POINT('Ctrl Pts',(43.2913465514678,33.1291669950141,-39.5528073643416));
#251915=CARTESIAN_POINT('Ctrl Pts',(43.3430293286761,33.1674385741862,-39.5709388212192));
#251916=CARTESIAN_POINT('Ctrl Pts',(43.4231851451275,33.2210209418068,-39.5978500433402));
#251917=CARTESIAN_POINT('Ctrl Pts',(43.4503462651464,33.2382463679058,-39.6067740129897));
#251918=CARTESIAN_POINT('Ctrl Pts',(43.5055591314263,33.2714182581268,-39.624529018923));
#251919=CARTESIAN_POINT('Ctrl Pts',(43.5336108390501,33.2873647780958,-39.6333600582416));
#251920=CARTESIAN_POINT('Ctrl Pts',(43.5906166462187,33.3179617274633,-39.6509285938296));
#251921=CARTESIAN_POINT('Ctrl Pts',(43.6195681837097,33.332610251026,-39.6596651896014));
#251922=CARTESIAN_POINT('Ctrl Pts',(43.6784023578464,33.3605920508175,-39.6770472374507));
#251923=CARTESIAN_POINT('Ctrl Pts',(43.7083061147169,33.3739259962444,-39.6856969797488));
#251924=CARTESIAN_POINT('Ctrl Pts',(43.7683632564387,33.3989627678266,-39.7027065574003));
#251925=CARTESIAN_POINT('Ctrl Pts',(43.7986438324276,33.4107277366309,-39.7111043138692));
#251926=CARTESIAN_POINT('Ctrl Pts',(43.8596237019195,33.4327310220396,-39.7276657859941));
#251927=CARTESIAN_POINT('Ctrl Pts',(43.890336277669,33.4429757189306,-39.7358334382075));
#251928=CARTESIAN_POINT('Ctrl Pts',(43.9831380894244,33.4714511139933,-39.7600003605629));
#251929=CARTESIAN_POINT('Ctrl Pts',(44.0458899346709,33.4874281577014,-39.7756643096983));
#251930=CARTESIAN_POINT('Ctrl Pts',(44.1413569280506,33.506834807521,-39.7984880366286));
#251931=CARTESIAN_POINT('Ctrl Pts',(44.1734028005723,33.5125427220107,-39.8059837459705));
#251932=CARTESIAN_POINT('Ctrl Pts',(44.2379488111806,33.5224114537718,-39.8207481486115));
#251933=CARTESIAN_POINT('Ctrl Pts',(44.2704346657345,33.5265706602302,-39.8280136905655));
#251934=CARTESIAN_POINT('Ctrl Pts',(44.3195548130225,33.5316268124821,-39.8387480552682));
#251935=CARTESIAN_POINT('Ctrl Pts',(44.3359806486903,33.533112514136,-39.8422958051522));
#251936=CARTESIAN_POINT('Ctrl Pts',(44.3687706554964,33.5356707262599,-39.849294985484));
#251937=CARTESIAN_POINT('Ctrl Pts',(44.385167271505,33.5367467362316,-39.8527535389071));
#251938=CARTESIAN_POINT('Ctrl Pts',(44.4343060324679,33.5393644028343,-39.8629950434304));
#251939=CARTESIAN_POINT('Ctrl Pts',(44.4670442875949,33.5403009170737,-39.8696542263645));
#251940=CARTESIAN_POINT('Ctrl Pts',(44.5651286496071,33.5407030633914,-39.8891184547758));
#251941=CARTESIAN_POINT('Ctrl Pts',(44.6303967828551,33.5377718061163,-39.901422664561));
#251942=CARTESIAN_POINT('Ctrl Pts',(44.7606559689193,33.5255009866035,-39.9246877858293));
#251943=CARTESIAN_POINT('Ctrl Pts',(44.8256649569195,33.5161561775268,-39.9356511727063));
#251944=CARTESIAN_POINT('Ctrl Pts',(44.9067228490285,33.5003647750523,-39.9484943680977));
#251945=CARTESIAN_POINT('Ctrl Pts',(44.9229356753385,33.4969955694502,-39.9510211299745));
#251946=CARTESIAN_POINT('Ctrl Pts',(44.9553230139946,33.4898452910065,-39.9559849708684));
#251947=CARTESIAN_POINT('Ctrl Pts',(44.9715294906083,33.4860553771579,-39.9584265939039));
#251948=CARTESIAN_POINT('Ctrl Pts',(45.0199639019752,33.4740881833957,-39.9655960356623));
#251949=CARTESIAN_POINT('Ctrl Pts',(45.0519117947774,33.4653417096262,-39.9701553183846));
#251950=CARTESIAN_POINT('Ctrl Pts',(45.1152354809225,33.446311250256,-39.9788559943743));
#251951=CARTESIAN_POINT('Ctrl Pts',(45.1465943739562,33.4360316133009,-39.9829949198606));
#251952=CARTESIAN_POINT('Ctrl Pts',(45.2087116410455,33.4139573018935,-39.9908546749667));
#251953=CARTESIAN_POINT('Ctrl Pts',(45.2394700085385,33.4021626107272,-39.9945754992332));
#251954=CARTESIAN_POINT('Ctrl Pts',(45.3003871502801,33.3770607090048,-40.0016005883336));
#251955=CARTESIAN_POINT('Ctrl Pts',(45.3305459270765,33.3637535047555,-40.0049048543333));
#251956=CARTESIAN_POINT('Ctrl Pts',(45.3902604247426,33.3356180078757,-40.0110952315559));
#251957=CARTESIAN_POINT('Ctrl Pts',(45.4198161574923,33.320789745125,-40.0139813505875));
#251958=CARTESIAN_POINT('Ctrl Pts',(45.4783165883616,33.2895921551583,-40.0193306273919));
#251959=CARTESIAN_POINT('Ctrl Pts',(45.5072641907393,33.2732200785006,-40.0217938150184));
#251960=CARTESIAN_POINT('Ctrl Pts',(45.5645240373204,33.2389139421848,-40.0262889502638));
#251961=CARTESIAN_POINT('Ctrl Pts',(45.5928978501659,33.2209306284775,-40.0283233062644));
#251962=CARTESIAN_POINT('Ctrl Pts',(45.6483131056985,33.1838278301212,-40.0319081811822));
#251963=CARTESIAN_POINT('Ctrl Pts',(45.67549164507,33.164629334656,-40.0334700763139));
#251964=CARTESIAN_POINT('Ctrl Pts',(45.7287256115122,33.1250064046253,-40.0361338267936));
#251965=CARTESIAN_POINT('Ctrl Pts',(45.7547947910058,33.1045739171436,-40.0372367973831));
#251966=CARTESIAN_POINT('Ctrl Pts',(45.8313734238719,33.0414298393551,-40.0398654758892));
#251967=CARTESIAN_POINT('Ctrl Pts',(45.8802576479033,32.9968758024409,-40.0407125357455));
#251968=CARTESIAN_POINT('Ctrl Pts',(45.9503157326903,32.9263396943911,-40.0406190162228));
#251969=CARTESIAN_POINT('Ctrl Pts',(45.9731228380904,32.9022091506732,-40.0403601109258));
#251970=CARTESIAN_POINT('Ctrl Pts',(46.0176306397645,32.8526937808809,-40.0393804091637));
#251971=CARTESIAN_POINT('Ctrl Pts',(46.0393256039723,32.827316116021,-40.0386598926118));
#251972=CARTESIAN_POINT('Ctrl Pts',(46.0816086740566,32.7752513538834,-40.0367459075072));
#251973=CARTESIAN_POINT('Ctrl Pts',(46.1020223635294,32.748776311325,-40.0355597999481));
#251974=CARTESIAN_POINT('Ctrl Pts',(46.1413479307733,32.6950625087254,-40.0327438351025));
#251975=CARTESIAN_POINT('Ctrl Pts',(46.1602745191316,32.667805408264,-40.0311132665587));
#251976=CARTESIAN_POINT('Ctrl Pts',(46.2148771442285,32.5848607282983,-40.0255646904152));
#251977=CARTESIAN_POINT('Ctrl Pts',(46.2483843529929,32.5279974828729,-40.020991041848));
#251978=CARTESIAN_POINT('Ctrl Pts',(46.3096714681144,32.4111744995713,-40.0101094995915));
#251979=CARTESIAN_POINT('Ctrl Pts',(46.3374529074462,32.3512004429127,-40.0037991041897));
#251980=CARTESIAN_POINT('Ctrl Pts',(46.3685304794595,32.2742958783444,-39.9948094190819));
#251981=CARTESIAN_POINT('Ctrl Pts',(46.3745651799673,32.258805297798,-39.992954196391));
#251982=CARTESIAN_POINT('Ctrl Pts',(46.3862597495084,32.2276471132964,-39.9891347888168));
#251983=CARTESIAN_POINT('Ctrl Pts',(46.3919303977612,32.2119454190112,-39.9871660259476));
#251984=CARTESIAN_POINT('Ctrl Pts',(46.4083231790586,32.1647108974852,-39.9811116502034));
#251985=CARTESIAN_POINT('Ctrl Pts',(46.4184020073002,32.1331340069007,-39.9768899782587));
#251986=CARTESIAN_POINT('Ctrl Pts',(46.436935125005,32.0697112055328,-39.9680710358276));
#251987=CARTESIAN_POINT('Ctrl Pts',(46.445383783564,32.0378820662313,-39.9634759528194));
#251988=CARTESIAN_POINT('Ctrl Pts',(46.4606734917644,31.9739924890849,-39.9539199839301));
#251989=CARTESIAN_POINT('Ctrl Pts',(46.4675144466818,31.9419320374959,-39.9489590775047));
#251990=CARTESIAN_POINT('Ctrl Pts',(46.4856499729356,31.845407387683,-39.9335315989557));
#251991=CARTESIAN_POINT('Ctrl Pts',(46.4945623229588,31.7805947077293,-39.9225202966587));
#251992=CARTESIAN_POINT('Ctrl Pts',(46.50315541296,31.682707544011,-39.9049106801433));
#251993=CARTESIAN_POINT('Ctrl Pts',(46.5052224358974,31.6499527611637,-39.8988555680355));
#251994=CARTESIAN_POINT('Ctrl Pts',(46.5071129195558,31.6006671922554,-39.8894982884836));
#251995=CARTESIAN_POINT('Ctrl Pts',(46.5075411711697,31.5842003354425,-39.8863308560925));
#251996=CARTESIAN_POINT('Ctrl Pts',(46.5079908839588,31.5512297919602,-39.8799064360613));
#251997=CARTESIAN_POINT('Ctrl Pts',(46.5080117823738,31.5346912044655,-39.8766424374324));
#251998=CARTESIAN_POINT('Ctrl Pts',(46.5074602328187,31.4851845718774,-39.8667475443341));
#251999=CARTESIAN_POINT('Ctrl Pts',(46.5062795002176,31.4523788235367,-39.8600254620174));
#252000=CARTESIAN_POINT('Ctrl Pts',(46.5023296578576,31.3870654499314,-39.8463171771464));
#252001=CARTESIAN_POINT('Ctrl Pts',(46.4995608696366,31.3545730297871,-39.8393340456404));
#252002=CARTESIAN_POINT('Ctrl Pts',(46.4889150985814,31.2575801349411,-39.8180028628456));
#252003=CARTESIAN_POINT('Ctrl Pts',(46.4787033805107,31.1935630593794,-39.8032737822661));
#252004=CARTESIAN_POINT('Ctrl Pts',(46.4587772997576,31.0984927597808,-39.7804216149437));
#252005=CARTESIAN_POINT('Ctrl Pts',(46.4513658768236,31.0669621494902,-39.7726775933303));
#252006=CARTESIAN_POINT('Ctrl Pts',(46.4349981252203,31.0042213580613,-39.7569342457637));
#252007=CARTESIAN_POINT('Ctrl Pts',(46.4260417208278,30.9730108067506,-39.748934832217));
#252008=CARTESIAN_POINT('Ctrl Pts',(46.4065676110902,30.9109152528886,-39.7326772993563));
#252009=CARTESIAN_POINT('Ctrl Pts',(46.3960456119263,30.8800184902932,-39.7244159758245));
#252010=CARTESIAN_POINT('Ctrl Pts',(46.3734275034811,30.8185995963653,-39.7076406500112));
#252011=CARTESIAN_POINT('Ctrl Pts',(46.3614248752738,30.7883281333193,-39.6991953503857));
#252012=CARTESIAN_POINT('Ctrl Pts',(46.3487357027272,30.7584583056228,-39.6906862677766));
#252013=CARTESIAN_POINT('',(42.4577131940165,32.5104083281549,-38.8606823233484));
#252014=CARTESIAN_POINT('',(42.4577131944622,32.5104083279563,-38.8606823233881));
#252015=CARTESIAN_POINT('',(46.6981266849484,30.7091523375492,-39.2904704603132));
#252016=CARTESIAN_POINT('Ctrl Pts',(46.6981266849492,30.7091523375488,-39.2904704603133));
#252017=CARTESIAN_POINT('Ctrl Pts',(46.5797439954818,30.4300352196549,-39.2213766504479));
#252018=CARTESIAN_POINT('Ctrl Pts',(46.4077912398568,30.1779725313306,-39.1472063538299));
#252019=CARTESIAN_POINT('Ctrl Pts',(45.9737831093239,29.752035876432,-38.9956460041782));
#252020=CARTESIAN_POINT('Ctrl Pts',(45.7147235512157,29.5834083339364,-38.9196908388693));
#252021=CARTESIAN_POINT('Ctrl Pts',(45.1527139049587,29.3607146626067,-38.7793910205612));
#252022=CARTESIAN_POINT('Ctrl Pts',(44.8561434351563,29.3053774688171,-38.7159976418443));
#252023=CARTESIAN_POINT('Ctrl Pts',(44.2653011709016,29.3121801855873,-38.6103011000027));
#252024=CARTESIAN_POINT('Ctrl Pts',(43.9766018912819,29.3704766749623,-38.5683428118836));
#252025=CARTESIAN_POINT('Ctrl Pts',(43.4335518958791,29.5939796223262,-38.5100427719152));
#252026=CARTESIAN_POINT('Ctrl Pts',(43.1848178911664,29.7570960269132,-38.4943558284383));
#252027=CARTESIAN_POINT('Ctrl Pts',(42.7660055088704,30.1651877888254,-38.4923938387362));
#252028=CARTESIAN_POINT('Ctrl Pts',(42.5990769824729,30.4036630363023,-38.5055049887944));
#252029=CARTESIAN_POINT('Ctrl Pts',(42.3602851983405,30.9324943875122,-38.5584474017113));
#252030=CARTESIAN_POINT('Ctrl Pts',(42.292408067155,31.2174998265278,-38.5980179340525));
#252031=CARTESIAN_POINT('Ctrl Pts',(42.270619938325,31.6778293530179,-38.6774582907849));
#252032=CARTESIAN_POINT('Ctrl Pts',(42.2818103158114,31.8495778784957,-38.7105098844616));
#252033=CARTESIAN_POINT('Ctrl Pts',(42.3419700050574,32.1874945526906,-38.7821575613242));
#252034=CARTESIAN_POINT('Ctrl Pts',(42.39095049389,32.3525183831361,-38.8205475941614));
#252035=CARTESIAN_POINT('Ctrl Pts',(42.4577131944621,32.5104083279563,-38.8606823233881));
#252036=CARTESIAN_POINT('',(46.6981266849484,30.7091523375492,-39.2904704603132));
#252037=CARTESIAN_POINT('Origin',(44.4157001211388,31.6455025209913,-39.4611695540092));
#252038=CARTESIAN_POINT('Origin',(44.5079524583208,31.5404524382925,-52.920575));
#252039=CARTESIAN_POINT('Ctrl Pts',(44.5079524583208,29.87170715524,-52.4912));
#252040=CARTESIAN_POINT('Ctrl Pts',(45.4714029967,29.87170715524,-52.4328666666667));
#252041=CARTESIAN_POINT('Ctrl Pts',(45.9531282658897,30.7060797967663,-52.3745333333334));
#252042=CARTESIAN_POINT('Ctrl Pts',(46.4348535350793,31.5404524382925,-52.3162000000001));
#252043=CARTESIAN_POINT('Ctrl Pts',(45.9531282658897,32.3748250798187,-52.2578666666667));
#252044=CARTESIAN_POINT('Ctrl Pts',(45.4714029967,33.2091977213449,-52.1995333333334));
#252045=CARTESIAN_POINT('Ctrl Pts',(44.5079524583208,33.2091977213449,-52.1412));
#252046=CARTESIAN_POINT('Ctrl Pts',(43.5445019199415,33.2091977213449,-52.0828666666667));
#252047=CARTESIAN_POINT('Ctrl Pts',(43.0627766507519,32.3748250798187,-52.0245333333333));
#252048=CARTESIAN_POINT('Ctrl Pts',(42.5810513815623,31.5404524382925,-51.9662));
#252049=CARTESIAN_POINT('Ctrl Pts',(43.0627766507519,30.7060797967663,-51.9078666666667));
#252050=CARTESIAN_POINT('Ctrl Pts',(43.5445019199415,29.87170715524,-51.8495333333334));
#252051=CARTESIAN_POINT('Ctrl Pts',(44.5079524583208,29.87170715524,-51.7912));
#252052=CARTESIAN_POINT('Ctrl Pts',(44.5079524583208,29.87170715524,-52.64995));
#252053=CARTESIAN_POINT('Ctrl Pts',(45.4714029967001,29.8717071552401,-52.5916166666667));
#252054=CARTESIAN_POINT('Ctrl Pts',(45.9531282658897,30.7060797967663,-52.5332833333334));
#252055=CARTESIAN_POINT('Ctrl Pts',(46.4348535350793,31.5404524382925,-52.47495));
#252056=CARTESIAN_POINT('Ctrl Pts',(45.9531282658897,32.3748250798187,-52.4166166666667));
#252057=CARTESIAN_POINT('Ctrl Pts',(45.4714029967,33.2091977213449,-52.3582833333334));
#252058=CARTESIAN_POINT('Ctrl Pts',(44.5079524583208,33.2091977213449,-52.29995));
#252059=CARTESIAN_POINT('Ctrl Pts',(43.5445019199415,33.2091977213449,-52.2416166666667));
#252060=CARTESIAN_POINT('Ctrl Pts',(43.0627766507519,32.3748250798187,-52.1832833333333));
#252061=CARTESIAN_POINT('Ctrl Pts',(42.5810513815623,31.5404524382925,-52.12495));
#252062=CARTESIAN_POINT('Ctrl Pts',(43.0627766507519,30.7060797967663,-52.0666166666667));
#252063=CARTESIAN_POINT('Ctrl Pts',(43.5445019199415,29.87170715524,-52.0082833333333));
#252064=CARTESIAN_POINT('Ctrl Pts',(44.5079524583208,29.87170715524,-51.94995));
#252065=CARTESIAN_POINT('Ctrl Pts',(44.5079524583208,33.6091932047179,-52.6102625));
#252066=CARTESIAN_POINT('Ctrl Pts',(43.3135644199415,33.6091932047179,-52.5519291666666));
#252067=CARTESIAN_POINT('Ctrl Pts',(42.7163704007519,32.5748228215052,-52.4935958333333));
#252068=CARTESIAN_POINT('Ctrl Pts',(42.1191763815623,31.5404524382925,-52.4352625));
#252069=CARTESIAN_POINT('Ctrl Pts',(42.7163704007519,30.5060820550798,-52.3769291666667));
#252070=CARTESIAN_POINT('Ctrl Pts',(43.3135644199415,29.4717116718671,-52.3185958333334));
#252071=CARTESIAN_POINT('Ctrl Pts',(44.5079524583208,29.4717116718671,-52.2602625));
#252072=CARTESIAN_POINT('Ctrl Pts',(45.7023404967,29.4717116718671,-52.2019291666667));
#252073=CARTESIAN_POINT('Ctrl Pts',(46.2995345158897,30.5060820550798,-52.1435958333333));
#252074=CARTESIAN_POINT('Ctrl Pts',(46.8967285350793,31.5404524382925,-52.0852625));
#252075=CARTESIAN_POINT('Ctrl Pts',(46.2995345158897,32.5748228215052,-52.0269291666667));
#252076=CARTESIAN_POINT('Ctrl Pts',(45.7023404967,33.6091932047179,-51.9685958333333));
#252077=CARTESIAN_POINT('Ctrl Pts',(44.5079524583208,33.6091932047179,-51.9102625));
#252078=CARTESIAN_POINT('Ctrl Pts',(43.3135644199415,33.6091932047179,-51.8519291666667));
#252079=CARTESIAN_POINT('Ctrl Pts',(42.7163704007519,32.5748228215052,-51.7935958333333));
#252080=CARTESIAN_POINT('Ctrl Pts',(42.1191763815623,31.5404524382925,-51.7352625));
#252081=CARTESIAN_POINT('Ctrl Pts',(42.7163704007519,30.5060820550798,-51.6769291666667));
#252082=CARTESIAN_POINT('Ctrl Pts',(43.3135644199415,29.4717116718671,-51.6185958333333));
#252083=CARTESIAN_POINT('Ctrl Pts',(44.5079524583208,29.4717116718671,-51.5602625));
#252084=CARTESIAN_POINT('Ctrl Pts',(45.7023404967,29.4717116718671,-51.5019291666666));
#252085=CARTESIAN_POINT('Ctrl Pts',(46.2995345158897,30.5060820550798,-51.4435958333333));
#252086=CARTESIAN_POINT('Ctrl Pts',(46.8967285350793,31.5404524382925,-51.3852625));
#252087=CARTESIAN_POINT('Ctrl Pts',(46.2995345158897,32.5748228215052,-51.3269291666667));
#252088=CARTESIAN_POINT('Ctrl Pts',(45.7023404967,33.6091932047179,-51.2685958333333));
#252089=CARTESIAN_POINT('Ctrl Pts',(44.5079524583208,33.6091932047179,-51.2102625));
#252090=CARTESIAN_POINT('Ctrl Pts',(43.3135644199415,33.6091932047179,-51.1519291666666));
#252091=CARTESIAN_POINT('Ctrl Pts',(42.7163704007519,32.5748228215052,-51.0935958333334));
#252092=CARTESIAN_POINT('Ctrl Pts',(42.1191763815623,31.5404524382925,-51.0352625));
#252093=CARTESIAN_POINT('Ctrl Pts',(42.7163704007519,30.5060820550798,-50.9769291666667));
#252094=CARTESIAN_POINT('Ctrl Pts',(43.3135644199415,29.4717116718671,-50.9185958333333));
#252095=CARTESIAN_POINT('Ctrl Pts',(44.5079524583208,29.4717116718671,-50.8602625));
#252096=CARTESIAN_POINT('Ctrl Pts',(45.7023404967,29.4717116718671,-50.8019291666667));
#252097=CARTESIAN_POINT('Ctrl Pts',(46.2995345158897,30.5060820550798,-50.7435958333333));
#252098=CARTESIAN_POINT('Ctrl Pts',(46.8967285350793,31.5404524382925,-50.6852625));
#252099=CARTESIAN_POINT('Ctrl Pts',(46.2995345158897,32.5748228215052,-50.6269291666667));
#252100=CARTESIAN_POINT('Ctrl Pts',(45.7023404967,33.6091932047179,-50.5685958333333));
#252101=CARTESIAN_POINT('Ctrl Pts',(44.5079524583208,33.6091932047179,-50.5102625));
#252102=CARTESIAN_POINT('Ctrl Pts',(43.3135644199415,33.6091932047179,-50.4519291666667));
#252103=CARTESIAN_POINT('Ctrl Pts',(42.7163704007519,32.5748228215052,-50.3935958333333));
#252104=CARTESIAN_POINT('Ctrl Pts',(42.1191763815623,31.5404524382925,-50.3352625));
#252105=CARTESIAN_POINT('Ctrl Pts',(42.7163704007519,30.5060820550798,-50.2769291666667));
#252106=CARTESIAN_POINT('Ctrl Pts',(43.3135644199415,29.4717116718671,-50.2185958333333));
#252107=CARTESIAN_POINT('Ctrl Pts',(44.5079524583208,29.4717116718671,-50.1602625));
#252108=CARTESIAN_POINT('Ctrl Pts',(45.7023404967,29.4717116718671,-50.1019291666667));
#252109=CARTESIAN_POINT('Ctrl Pts',(46.2995345158897,30.5060820550798,-50.0435958333333));
#252110=CARTESIAN_POINT('Ctrl Pts',(46.8967285350793,31.5404524382925,-49.9852625));
#252111=CARTESIAN_POINT('Ctrl Pts',(46.2995345158897,32.5748228215052,-49.9269291666667));
#252112=CARTESIAN_POINT('Ctrl Pts',(45.7023404967,33.6091932047179,-49.8685958333333));
#252113=CARTESIAN_POINT('Ctrl Pts',(44.5079524583208,33.6091932047179,-49.8102625));
#252114=CARTESIAN_POINT('Ctrl Pts',(43.3135644199415,33.6091932047179,-49.7519291666667));
#252115=CARTESIAN_POINT('Ctrl Pts',(42.7163704007519,32.5748228215052,-49.6935958333334));
#252116=CARTESIAN_POINT('Ctrl Pts',(42.1191763815623,31.5404524382925,-49.6352625));
#252117=CARTESIAN_POINT('Ctrl Pts',(42.7163704007519,30.5060820550798,-49.5769291666667));
#252118=CARTESIAN_POINT('Ctrl Pts',(43.3135644199415,29.4717116718671,-49.5185958333334));
#252119=CARTESIAN_POINT('Ctrl Pts',(44.5079524583208,29.4717116718671,-49.4602625));
#252120=CARTESIAN_POINT('Ctrl Pts',(45.7023404967,29.4717116718671,-49.4019291666667));
#252121=CARTESIAN_POINT('Ctrl Pts',(46.2995345158897,30.5060820550798,-49.3435958333333));
#252122=CARTESIAN_POINT('Ctrl Pts',(46.8967285350793,31.5404524382925,-49.2852625));
#252123=CARTESIAN_POINT('Ctrl Pts',(46.2995345158897,32.5748228215052,-49.2269291666667));
#252124=CARTESIAN_POINT('Ctrl Pts',(45.7023404967,33.6091932047179,-49.1685958333334));
#252125=CARTESIAN_POINT('Ctrl Pts',(44.5079524583208,33.6091932047179,-49.1102625));
#252126=CARTESIAN_POINT('Ctrl Pts',(43.3135644199415,33.6091932047179,-49.0519291666667));
#252127=CARTESIAN_POINT('Ctrl Pts',(42.7163704007519,32.5748228215052,-48.9935958333333));
#252128=CARTESIAN_POINT('Ctrl Pts',(42.1191763815623,31.5404524382925,-48.9352625));
#252129=CARTESIAN_POINT('Ctrl Pts',(42.7163704007519,30.5060820550798,-48.8769291666667));
#252130=CARTESIAN_POINT('Ctrl Pts',(43.3135644199415,29.4717116718671,-48.8185958333333));
#252131=CARTESIAN_POINT('Ctrl Pts',(44.5079524583208,29.4717116718671,-48.7602625));
#252132=CARTESIAN_POINT('Ctrl Pts',(45.7023404967,29.4717116718671,-48.7019291666667));
#252133=CARTESIAN_POINT('Ctrl Pts',(46.2995345158897,30.5060820550798,-48.6435958333333));
#252134=CARTESIAN_POINT('Ctrl Pts',(46.8967285350793,31.5404524382925,-48.5852625));
#252135=CARTESIAN_POINT('Ctrl Pts',(46.2995345158897,32.5748228215052,-48.5269291666667));
#252136=CARTESIAN_POINT('Ctrl Pts',(45.7023404967,33.6091932047179,-48.4685958333333));
#252137=CARTESIAN_POINT('Ctrl Pts',(44.5079524583208,33.6091932047179,-48.4102625));
#252138=CARTESIAN_POINT('Ctrl Pts',(43.3135644199415,33.6091932047179,-48.3519291666667));
#252139=CARTESIAN_POINT('Ctrl Pts',(42.7163704007519,32.5748228215052,-48.2935958333333));
#252140=CARTESIAN_POINT('Ctrl Pts',(42.1191763815623,31.5404524382925,-48.2352625));
#252141=CARTESIAN_POINT('Ctrl Pts',(42.7163704007519,30.5060820550798,-48.1769291666667));
#252142=CARTESIAN_POINT('Ctrl Pts',(43.3135644199415,29.4717116718671,-48.1185958333334));
#252143=CARTESIAN_POINT('Ctrl Pts',(44.5079524583208,29.4717116718671,-48.0602625));
#252144=CARTESIAN_POINT('Ctrl Pts',(45.7023404967,29.4717116718671,-48.0019291666667));
#252145=CARTESIAN_POINT('Ctrl Pts',(46.2995345158897,30.5060820550798,-47.9435958333334));
#252146=CARTESIAN_POINT('Ctrl Pts',(46.8967285350793,31.5404524382925,-47.8852625));
#252147=CARTESIAN_POINT('Ctrl Pts',(46.2995345158897,32.5748228215052,-47.8269291666667));
#252148=CARTESIAN_POINT('Ctrl Pts',(45.7023404967,33.6091932047179,-47.7685958333333));
#252149=CARTESIAN_POINT('Ctrl Pts',(44.5079524583208,33.6091932047179,-47.7102625));
#252150=CARTESIAN_POINT('Ctrl Pts',(43.3135644199415,33.6091932047179,-47.6519291666667));
#252151=CARTESIAN_POINT('Ctrl Pts',(42.7163704007519,32.5748228215052,-47.5935958333333));
#252152=CARTESIAN_POINT('Ctrl Pts',(42.1191763815623,31.5404524382925,-47.5352625));
#252153=CARTESIAN_POINT('Ctrl Pts',(42.7163704007519,30.5060820550798,-47.4769291666667));
#252154=CARTESIAN_POINT('Ctrl Pts',(43.3135644199415,29.4717116718671,-47.4185958333333));
#252155=CARTESIAN_POINT('Ctrl Pts',(44.5079524583208,29.4717116718671,-47.3602625));
#252156=CARTESIAN_POINT('Ctrl Pts',(45.7023404967,29.4717116718671,-47.3019291666666));
#252157=CARTESIAN_POINT('Ctrl Pts',(46.2995345158897,30.5060820550798,-47.2435958333333));
#252158=CARTESIAN_POINT('Ctrl Pts',(46.8967285350793,31.5404524382925,-47.1852625));
#252159=CARTESIAN_POINT('Ctrl Pts',(46.2995345158897,32.5748228215052,-47.1269291666667));
#252160=CARTESIAN_POINT('Ctrl Pts',(45.7023404967,33.6091932047179,-47.0685958333333));
#252161=CARTESIAN_POINT('Ctrl Pts',(44.5079524583208,33.6091932047179,-47.0102625));
#252162=CARTESIAN_POINT('Ctrl Pts',(43.3135644199415,33.6091932047179,-46.9519291666667));
#252163=CARTESIAN_POINT('Ctrl Pts',(42.7163704007519,32.5748228215052,-46.8935958333333));
#252164=CARTESIAN_POINT('Ctrl Pts',(42.1191763815623,31.5404524382925,-46.8352625));
#252165=CARTESIAN_POINT('Ctrl Pts',(42.7163704007519,30.5060820550798,-46.7769291666667));
#252166=CARTESIAN_POINT('Ctrl Pts',(43.3135644199415,29.4717116718671,-46.7185958333333));
#252167=CARTESIAN_POINT('Ctrl Pts',(44.5079524583208,29.4717116718671,-46.6602625));
#252168=CARTESIAN_POINT('Ctrl Pts',(45.7023404967,29.4717116718671,-46.6019291666667));
#252169=CARTESIAN_POINT('Ctrl Pts',(46.2995345158897,30.5060820550798,-46.5435958333334));
#252170=CARTESIAN_POINT('Ctrl Pts',(46.8967285350793,31.5404524382925,-46.4852625));
#252171=CARTESIAN_POINT('Ctrl Pts',(46.2995345158897,32.5748228215052,-46.4269291666667));
#252172=CARTESIAN_POINT('Ctrl Pts',(45.7023404967,33.6091932047179,-46.3685958333333));
#252173=CARTESIAN_POINT('Ctrl Pts',(44.5079524583208,33.6091932047179,-46.3102625));
#252174=CARTESIAN_POINT('Ctrl Pts',(43.3135644199415,33.6091932047179,-46.2519291666667));
#252175=CARTESIAN_POINT('Ctrl Pts',(42.7163704007519,32.5748228215052,-46.1935958333333));
#252176=CARTESIAN_POINT('Ctrl Pts',(42.1191763815623,31.5404524382925,-46.1352625));
#252177=CARTESIAN_POINT('Ctrl Pts',(42.7163704007519,30.5060820550798,-46.0769291666667));
#252178=CARTESIAN_POINT('Ctrl Pts',(43.3135644199415,29.4717116718671,-46.0185958333334));
#252179=CARTESIAN_POINT('Ctrl Pts',(44.5079524583208,29.4717116718671,-45.9602625));
#252180=CARTESIAN_POINT('Ctrl Pts',(45.7023404967,29.4717116718671,-45.9019291666667));
#252181=CARTESIAN_POINT('Ctrl Pts',(46.2995345158897,30.5060820550798,-45.8435958333333));
#252182=CARTESIAN_POINT('Ctrl Pts',(46.8967285350793,31.5404524382925,-45.7852625));
#252183=CARTESIAN_POINT('Ctrl Pts',(46.2995345158897,32.5748228215052,-45.7269291666667));
#252184=CARTESIAN_POINT('Ctrl Pts',(45.7023404967,33.6091932047179,-45.6685958333334));
#252185=CARTESIAN_POINT('Ctrl Pts',(44.5079524583208,33.6091932047179,-45.6102625));
#252186=CARTESIAN_POINT('Ctrl Pts',(43.3135644199415,33.6091932047179,-45.5519291666667));
#252187=CARTESIAN_POINT('Ctrl Pts',(42.7163704007519,32.5748228215052,-45.4935958333333));
#252188=CARTESIAN_POINT('Ctrl Pts',(42.1191763815623,31.5404524382925,-45.4352625));
#252189=CARTESIAN_POINT('Ctrl Pts',(42.7163704007519,30.5060820550798,-45.3769291666667));
#252190=CARTESIAN_POINT('Ctrl Pts',(43.3135644199415,29.4717116718671,-45.3185958333333));
#252191=CARTESIAN_POINT('Ctrl Pts',(44.5079524583208,29.4717116718671,-45.2602625));
#252192=CARTESIAN_POINT('Ctrl Pts',(45.7023404967,29.4717116718671,-45.2019291666667));
#252193=CARTESIAN_POINT('Ctrl Pts',(46.2995345158897,30.5060820550798,-45.1435958333333));
#252194=CARTESIAN_POINT('Ctrl Pts',(46.8967285350793,31.5404524382925,-45.0852625));
#252195=CARTESIAN_POINT('Ctrl Pts',(46.2995345158897,32.5748228215052,-45.0269291666667));
#252196=CARTESIAN_POINT('Ctrl Pts',(45.7023404967,33.6091932047179,-44.9685958333334));
#252197=CARTESIAN_POINT('Ctrl Pts',(44.5079524583208,33.6091932047179,-44.9102625));
#252198=CARTESIAN_POINT('Ctrl Pts',(43.3135644199415,33.6091932047179,-44.8519291666667));
#252199=CARTESIAN_POINT('Ctrl Pts',(42.7163704007519,32.5748228215052,-44.7935958333333));
#252200=CARTESIAN_POINT('Ctrl Pts',(42.1191763815623,31.5404524382925,-44.7352625));
#252201=CARTESIAN_POINT('Ctrl Pts',(42.7163704007519,30.5060820550798,-44.6769291666667));
#252202=CARTESIAN_POINT('Ctrl Pts',(43.3135644199415,29.4717116718671,-44.6185958333334));
#252203=CARTESIAN_POINT('Ctrl Pts',(44.5079524583208,29.4717116718671,-44.5602625));
#252204=CARTESIAN_POINT('Ctrl Pts',(45.7023404967,29.4717116718671,-44.5019291666667));
#252205=CARTESIAN_POINT('Ctrl Pts',(46.2995345158897,30.5060820550798,-44.4435958333333));
#252206=CARTESIAN_POINT('Ctrl Pts',(46.8967285350793,31.5404524382925,-44.3852625));
#252207=CARTESIAN_POINT('Ctrl Pts',(46.2995345158897,32.5748228215052,-44.3269291666667));
#252208=CARTESIAN_POINT('Ctrl Pts',(45.7023404967,33.6091932047179,-44.2685958333334));
#252209=CARTESIAN_POINT('Ctrl Pts',(44.5079524583208,33.6091932047179,-44.2102625));
#252210=CARTESIAN_POINT('Ctrl Pts',(43.3135644199415,33.6091932047179,-44.1519291666667));
#252211=CARTESIAN_POINT('Ctrl Pts',(42.7163704007519,32.5748228215052,-44.0935958333334));
#252212=CARTESIAN_POINT('Ctrl Pts',(42.1191763815623,31.5404524382925,-44.0352625));
#252213=CARTESIAN_POINT('Ctrl Pts',(42.7163704007519,30.5060820550798,-43.9769291666667));
#252214=CARTESIAN_POINT('Ctrl Pts',(43.3135644199415,29.4717116718671,-43.9185958333333));
#252215=CARTESIAN_POINT('Ctrl Pts',(44.5079524583208,29.4717116718671,-43.8602625));
#252216=CARTESIAN_POINT('Ctrl Pts',(45.7023404967,29.4717116718671,-43.8019291666667));
#252217=CARTESIAN_POINT('Ctrl Pts',(46.2995345158897,30.5060820550798,-43.7435958333334));
#252218=CARTESIAN_POINT('Ctrl Pts',(46.8967285350793,31.5404524382925,-43.6852625));
#252219=CARTESIAN_POINT('Ctrl Pts',(46.2995345158897,32.5748228215052,-43.6269291666667));
#252220=CARTESIAN_POINT('Ctrl Pts',(45.7023404967,33.6091932047179,-43.5685958333333));
#252221=CARTESIAN_POINT('Ctrl Pts',(44.5079524583208,33.6091932047179,-43.5102625));
#252222=CARTESIAN_POINT('Ctrl Pts',(43.3135644199415,33.6091932047179,-43.4519291666667));
#252223=CARTESIAN_POINT('Ctrl Pts',(42.7163704007519,32.5748228215052,-43.3935958333334));
#252224=CARTESIAN_POINT('Ctrl Pts',(42.1191763815623,31.5404524382925,-43.3352625));
#252225=CARTESIAN_POINT('Ctrl Pts',(42.7163704007519,30.5060820550798,-43.2769291666667));
#252226=CARTESIAN_POINT('Ctrl Pts',(43.3135644199415,29.4717116718671,-43.2185958333333));
#252227=CARTESIAN_POINT('Ctrl Pts',(44.5079524583208,29.4717116718671,-43.1602625));
#252228=CARTESIAN_POINT('Ctrl Pts',(45.7023404967,29.4717116718671,-43.1019291666667));
#252229=CARTESIAN_POINT('Ctrl Pts',(46.2995345158897,30.5060820550798,-43.0435958333334));
#252230=CARTESIAN_POINT('Ctrl Pts',(46.8967285350793,31.5404524382925,-42.9852625));
#252231=CARTESIAN_POINT('Ctrl Pts',(46.2995345158897,32.5748228215052,-42.9269291666667));
#252232=CARTESIAN_POINT('Ctrl Pts',(45.7023404967,33.6091932047179,-42.8685958333333));
#252233=CARTESIAN_POINT('Ctrl Pts',(44.5079524583208,33.6091932047179,-42.8102625));
#252234=CARTESIAN_POINT('Ctrl Pts',(43.3135644199415,33.6091932047179,-42.7519291666666));
#252235=CARTESIAN_POINT('Ctrl Pts',(42.7163704007519,32.5748228215052,-42.6935958333333));
#252236=CARTESIAN_POINT('Ctrl Pts',(42.1191763815623,31.5404524382925,-42.6352625));
#252237=CARTESIAN_POINT('Ctrl Pts',(42.7163704007519,30.5060820550798,-42.5769291666667));
#252238=CARTESIAN_POINT('Ctrl Pts',(43.3135644199415,29.4717116718671,-42.5185958333333));
#252239=CARTESIAN_POINT('Ctrl Pts',(44.5079524583208,29.4717116718671,-42.4602625));
#252240=CARTESIAN_POINT('Ctrl Pts',(45.7023404967,29.4717116718671,-42.4019291666666));
#252241=CARTESIAN_POINT('Ctrl Pts',(46.2995345158897,30.5060820550798,-42.3435958333334));
#252242=CARTESIAN_POINT('Ctrl Pts',(46.8967285350793,31.5404524382925,-42.2852625));
#252243=CARTESIAN_POINT('Ctrl Pts',(46.2995345158897,32.5748228215052,-42.2269291666667));
#252244=CARTESIAN_POINT('Ctrl Pts',(45.7023404967,33.6091932047179,-42.1685958333333));
#252245=CARTESIAN_POINT('Ctrl Pts',(44.5079524583208,33.6091932047179,-42.1102625));
#252246=CARTESIAN_POINT('Ctrl Pts',(43.3135644199415,33.6091932047179,-42.0519291666666));
#252247=CARTESIAN_POINT('Ctrl Pts',(42.7163704007519,32.5748228215052,-41.9935958333334));
#252248=CARTESIAN_POINT('Ctrl Pts',(42.1191763815623,31.5404524382925,-41.9352625));
#252249=CARTESIAN_POINT('Ctrl Pts',(42.7163704007519,30.5060820550798,-41.8769291666667));
#252250=CARTESIAN_POINT('Ctrl Pts',(43.3135644199415,29.4717116718671,-41.8185958333333));
#252251=CARTESIAN_POINT('Ctrl Pts',(44.5079524583208,29.4717116718671,-41.7602625));
#252252=CARTESIAN_POINT('Ctrl Pts',(45.7023404967,29.4717116718671,-41.7019291666666));
#252253=CARTESIAN_POINT('Ctrl Pts',(46.2995345158897,30.5060820550798,-41.6435958333334));
#252254=CARTESIAN_POINT('Ctrl Pts',(46.8967285350793,31.5404524382925,-41.5852625));
#252255=CARTESIAN_POINT('Ctrl Pts',(46.2995345158897,32.5748228215052,-41.5269291666667));
#252256=CARTESIAN_POINT('Ctrl Pts',(45.7023404967,33.6091932047179,-41.4685958333333));
#252257=CARTESIAN_POINT('Ctrl Pts',(44.5079524583208,33.6091932047179,-41.4102625));
#252258=CARTESIAN_POINT('Ctrl Pts',(43.3135644199415,33.6091932047179,-41.3519291666666));
#252259=CARTESIAN_POINT('Ctrl Pts',(42.7163704007519,32.5748228215052,-41.2935958333334));
#252260=CARTESIAN_POINT('Ctrl Pts',(42.1191763815623,31.5404524382925,-41.2352625));
#252261=CARTESIAN_POINT('Ctrl Pts',(42.7163704007519,30.5060820550798,-41.1769291666667));
#252262=CARTESIAN_POINT('Ctrl Pts',(43.3135644199415,29.4717116718671,-41.1185958333333));
#252263=CARTESIAN_POINT('Ctrl Pts',(44.5079524583208,29.4717116718671,-41.0602625));
#252264=CARTESIAN_POINT('Ctrl Pts',(45.7023404967,29.4717116718671,-41.0019291666666));
#252265=CARTESIAN_POINT('Ctrl Pts',(46.2995345158897,30.5060820550798,-40.9435958333334));
#252266=CARTESIAN_POINT('Ctrl Pts',(46.8967285350793,31.5404524382925,-40.8852625));
#252267=CARTESIAN_POINT('Ctrl Pts',(46.2995345158897,32.5748228215052,-40.8269291666667));
#252268=CARTESIAN_POINT('Ctrl Pts',(45.7023404967,33.6091932047179,-40.7685958333333));
#252269=CARTESIAN_POINT('Ctrl Pts',(44.5079524583208,33.6091932047179,-40.7102625));
#252270=CARTESIAN_POINT('Ctrl Pts',(43.3135644199415,33.6091932047179,-40.6519291666667));
#252271=CARTESIAN_POINT('Ctrl Pts',(42.7163704007519,32.5748228215052,-40.5935958333334));
#252272=CARTESIAN_POINT('Ctrl Pts',(42.1191763815623,31.5404524382925,-40.5352625));
#252273=CARTESIAN_POINT('Ctrl Pts',(42.7163704007519,30.5060820550798,-40.4769291666667));
#252274=CARTESIAN_POINT('Ctrl Pts',(43.3135644199415,29.4717116718671,-40.4185958333333));
#252275=CARTESIAN_POINT('Ctrl Pts',(44.5079524583208,29.4717116718671,-40.3602625));
#252276=CARTESIAN_POINT('Ctrl Pts',(45.7023404967,29.4717116718671,-40.3019291666667));
#252277=CARTESIAN_POINT('Ctrl Pts',(46.2995345158897,30.5060820550798,-40.2435958333334));
#252278=CARTESIAN_POINT('Ctrl Pts',(46.8967285350793,31.5404524382925,-40.1852625));
#252279=CARTESIAN_POINT('Ctrl Pts',(46.2995345158897,32.5748228215052,-40.1269291666666));
#252280=CARTESIAN_POINT('Ctrl Pts',(45.7023404967,33.6091932047179,-40.0685958333333));
#252281=CARTESIAN_POINT('Ctrl Pts',(44.5079524583208,33.6091932047179,-40.0102625));
#252282=CARTESIAN_POINT('Ctrl Pts',(43.3135644199415,33.6091932047179,-39.9519291666667));
#252283=CARTESIAN_POINT('Ctrl Pts',(42.7163704007519,32.5748228215052,-39.8935958333334));
#252284=CARTESIAN_POINT('Ctrl Pts',(42.1191763815623,31.5404524382925,-39.8352625));
#252285=CARTESIAN_POINT('Ctrl Pts',(42.7163704007519,30.5060820550798,-39.7769291666666));
#252286=CARTESIAN_POINT('Ctrl Pts',(43.3135644199415,29.4717116718671,-39.7185958333334));
#252287=CARTESIAN_POINT('Ctrl Pts',(44.5079524583208,29.4717116718671,-39.6602625));
#252288=CARTESIAN_POINT('Ctrl Pts',(45.7023404967,29.4717116718671,-39.6019291666667));
#252289=CARTESIAN_POINT('Ctrl Pts',(46.2995345158897,30.5060820550798,-39.5435958333333));
#252290=CARTESIAN_POINT('Ctrl Pts',(46.8967285350793,31.5404524382925,-39.4852625));
#252291=CARTESIAN_POINT('Ctrl Pts',(46.2995345158897,32.5748228215052,-39.4269291666667));
#252292=CARTESIAN_POINT('Ctrl Pts',(45.7023404967,33.6091932047179,-39.3685958333334));
#252293=CARTESIAN_POINT('Ctrl Pts',(44.5079524583208,33.6091932047179,-39.3102625));
#252294=CARTESIAN_POINT('Ctrl Pts',(43.3135644199415,33.6091932047179,-39.2519291666667));
#252295=CARTESIAN_POINT('Ctrl Pts',(42.7163704007519,32.5748228215052,-39.1935958333334));
#252296=CARTESIAN_POINT('Ctrl Pts',(42.1191763815623,31.5404524382925,-39.1352625));
#252297=CARTESIAN_POINT('Ctrl Pts',(42.7163704007519,30.5060820550798,-39.0769291666667));
#252298=CARTESIAN_POINT('Ctrl Pts',(43.3135644199415,29.4717116718671,-39.0185958333333));
#252299=CARTESIAN_POINT('Ctrl Pts',(44.5079524583208,29.4717116718671,-38.9602625));
#252300=CARTESIAN_POINT('Ctrl Pts',(45.7023404967,29.4717116718671,-38.9019291666667));
#252301=CARTESIAN_POINT('Ctrl Pts',(46.2995345158897,30.5060820550798,-38.8435958333333));
#252302=CARTESIAN_POINT('Ctrl Pts',(46.8967285350793,31.5404524382925,-38.7852625));
#252303=CARTESIAN_POINT('Ctrl Pts',(46.2995345158897,32.5748228215052,-38.7269291666667));
#252304=CARTESIAN_POINT('Ctrl Pts',(45.7023404967,33.6091932047179,-38.6685958333334));
#252305=CARTESIAN_POINT('Ctrl Pts',(44.5079524583208,33.6091932047179,-38.6102625));
#252306=CARTESIAN_POINT('Ctrl Pts',(43.3135644199415,33.6091932047179,-38.5519291666667));
#252307=CARTESIAN_POINT('Ctrl Pts',(42.7163704007519,32.5748228215052,-38.4935958333334));
#252308=CARTESIAN_POINT('Ctrl Pts',(42.1191763815623,31.5404524382925,-38.4352625));
#252309=CARTESIAN_POINT('Ctrl Pts',(42.7163704007519,30.5060820550798,-38.3769291666666));
#252310=CARTESIAN_POINT('Ctrl Pts',(43.3135644199415,29.4717116718671,-38.3185958333333));
#252311=CARTESIAN_POINT('Ctrl Pts',(44.5079524583208,29.4717116718671,-38.2602625));
#252312=CARTESIAN_POINT('Ctrl Pts',(45.7023404967,29.4717116718671,-38.2019291666667));
#252313=CARTESIAN_POINT('Ctrl Pts',(46.2995345158897,30.5060820550798,-38.1435958333334));
#252314=CARTESIAN_POINT('Ctrl Pts',(46.8967285350793,31.5404524382925,-38.0852625));
#252315=CARTESIAN_POINT('Ctrl Pts',(46.2995345158897,32.5748228215052,-38.0269291666667));
#252316=CARTESIAN_POINT('Ctrl Pts',(45.7023404967,33.6091932047179,-37.9685958333333));
#252317=CARTESIAN_POINT('Ctrl Pts',(44.5079524583208,33.6091932047179,-37.9102625));
#252318=CARTESIAN_POINT('Ctrl Pts',(43.3135644199415,33.6091932047179,-37.8519291666667));
#252319=CARTESIAN_POINT('Ctrl Pts',(42.7163704007519,32.5748228215052,-37.7935958333334));
#252320=CARTESIAN_POINT('Ctrl Pts',(42.1191763815623,31.5404524382925,-37.7352625));
#252321=CARTESIAN_POINT('Ctrl Pts',(42.7163704007519,30.5060820550798,-37.6769291666667));
#252322=CARTESIAN_POINT('Ctrl Pts',(43.3135644199415,29.4717116718671,-37.6185958333333));
#252323=CARTESIAN_POINT('Ctrl Pts',(44.5079524583208,29.4717116718671,-37.5602625));
#252324=CARTESIAN_POINT('Ctrl Pts',(45.7023404967,29.4717116718671,-37.5019291666666));
#252325=CARTESIAN_POINT('Ctrl Pts',(46.2995345158897,30.5060820550798,-37.4435958333333));
#252326=CARTESIAN_POINT('Ctrl Pts',(46.8967285350793,31.5404524382925,-37.3852625));
#252327=CARTESIAN_POINT('Ctrl Pts',(46.2995345158897,32.5748228215052,-37.3269291666667));
#252328=CARTESIAN_POINT('Ctrl Pts',(45.7023404967,33.6091932047179,-37.2685958333333));
#252329=CARTESIAN_POINT('Ctrl Pts',(44.5079524583208,33.6091932047179,-37.2102625));
#252330=CARTESIAN_POINT('Ctrl Pts',(43.3135644199415,33.6091932047179,-37.1519291666667));
#252331=CARTESIAN_POINT('Ctrl Pts',(42.7163704007519,32.5748228215052,-37.0935958333333));
#252332=CARTESIAN_POINT('Ctrl Pts',(42.1191763815623,31.5404524382925,-37.0352625));
#252333=CARTESIAN_POINT('Ctrl Pts',(42.7163704007519,30.5060820550798,-36.9769291666667));
#252334=CARTESIAN_POINT('Ctrl Pts',(43.3135644199415,29.4717116718671,-36.9185958333333));
#252335=CARTESIAN_POINT('Ctrl Pts',(44.5079524583208,29.4717116718671,-36.8602625));
#252336=CARTESIAN_POINT('Ctrl Pts',(45.7023404967,29.4717116718671,-36.8019291666666));
#252337=CARTESIAN_POINT('Ctrl Pts',(46.2995345158897,30.5060820550798,-36.7435958333334));
#252338=CARTESIAN_POINT('Ctrl Pts',(46.8967285350793,31.5404524382925,-36.6852625));
#252339=CARTESIAN_POINT('Ctrl Pts',(46.2995345158897,32.5748228215052,-36.6269291666666));
#252340=CARTESIAN_POINT('Ctrl Pts',(46.222006582932,32.7091051403937,-36.6193563132714));
#252341=CARTESIAN_POINT('Ctrl Pts',(46.1253278975281,32.8303303578336,-36.611216324118));
#252342=CARTESIAN_POINT('Ctrl Pts',(44.5079524583208,33.2091977213449,-52.8412));
#252343=CARTESIAN_POINT('Ctrl Pts',(43.5445019199415,33.2091977213449,-52.7828666666667));
#252344=CARTESIAN_POINT('Ctrl Pts',(43.0627766507519,32.3748250798187,-52.7245333333334));
#252345=CARTESIAN_POINT('Ctrl Pts',(42.5810513815623,31.5404524382925,-52.6662));
#252346=CARTESIAN_POINT('Ctrl Pts',(43.0627766507519,30.7060797967663,-52.6078666666667));
#252347=CARTESIAN_POINT('Ctrl Pts',(43.5445019199415,29.87170715524,-52.5495333333333));
#252348=CARTESIAN_POINT('Ctrl Pts',(44.5079524583208,29.87170715524,-52.4912));
#252349=CARTESIAN_POINT('Ctrl Pts',(45.4714029967,29.87170715524,-52.4328666666667));
#252350=CARTESIAN_POINT('Ctrl Pts',(45.9531282658897,30.7060797967663,-52.3745333333334));
#252351=CARTESIAN_POINT('Ctrl Pts',(46.4348535350793,31.5404524382925,-52.3162000000001));
#252352=CARTESIAN_POINT('Ctrl Pts',(45.9531282658897,32.3748250798187,-52.2578666666667));
#252353=CARTESIAN_POINT('Ctrl Pts',(45.4714029967,33.2091977213449,-52.1995333333334));
#252354=CARTESIAN_POINT('Ctrl Pts',(44.5079524583208,33.2091977213449,-52.1412));
#252355=CARTESIAN_POINT('Ctrl Pts',(43.5445019199415,33.2091977213449,-52.0828666666667));
#252356=CARTESIAN_POINT('Ctrl Pts',(43.0627766507519,32.3748250798187,-52.0245333333333));
#252357=CARTESIAN_POINT('Ctrl Pts',(42.5810513815623,31.5404524382925,-51.9662));
#252358=CARTESIAN_POINT('Ctrl Pts',(43.0627766507519,30.7060797967663,-51.9078666666667));
#252359=CARTESIAN_POINT('Ctrl Pts',(43.5445019199415,29.87170715524,-51.8495333333334));
#252360=CARTESIAN_POINT('Ctrl Pts',(44.5079524583208,29.87170715524,-51.7912));
#252361=CARTESIAN_POINT('Ctrl Pts',(45.4714029967,29.87170715524,-51.7328666666667));
#252362=CARTESIAN_POINT('Ctrl Pts',(45.9531282658897,30.7060797967663,-51.6745333333333));
#252363=CARTESIAN_POINT('Ctrl Pts',(46.4348535350793,31.5404524382925,-51.6162));
#252364=CARTESIAN_POINT('Ctrl Pts',(45.9531282658897,32.3748250798187,-51.5578666666667));
#252365=CARTESIAN_POINT('Ctrl Pts',(45.4714029967,33.2091977213449,-51.4995333333333));
#252366=CARTESIAN_POINT('Ctrl Pts',(44.5079524583208,33.2091977213449,-51.4412));
#252367=CARTESIAN_POINT('Ctrl Pts',(43.5445019199415,33.2091977213449,-51.3828666666667));
#252368=CARTESIAN_POINT('Ctrl Pts',(43.0627766507519,32.3748250798187,-51.3245333333334));
#252369=CARTESIAN_POINT('Ctrl Pts',(42.5810513815623,31.5404524382925,-51.2662));
#252370=CARTESIAN_POINT('Ctrl Pts',(43.0627766507519,30.7060797967663,-51.2078666666667));
#252371=CARTESIAN_POINT('Ctrl Pts',(43.5445019199415,29.87170715524,-51.1495333333333));
#252372=CARTESIAN_POINT('Ctrl Pts',(44.5079524583208,29.87170715524,-51.0912));
#252373=CARTESIAN_POINT('Ctrl Pts',(45.4714029967,29.87170715524,-51.0328666666667));
#252374=CARTESIAN_POINT('Ctrl Pts',(45.9531282658897,30.7060797967663,-50.9745333333333));
#252375=CARTESIAN_POINT('Ctrl Pts',(46.4348535350793,31.5404524382925,-50.9162));
#252376=CARTESIAN_POINT('Ctrl Pts',(45.9531282658897,32.3748250798187,-50.8578666666667));
#252377=CARTESIAN_POINT('Ctrl Pts',(45.4714029967,33.2091977213449,-50.7995333333333));
#252378=CARTESIAN_POINT('Ctrl Pts',(44.5079524583208,33.2091977213449,-50.7412));
#252379=CARTESIAN_POINT('Ctrl Pts',(43.5445019199415,33.2091977213449,-50.6828666666667));
#252380=CARTESIAN_POINT('Ctrl Pts',(43.0627766507519,32.3748250798187,-50.6245333333333));
#252381=CARTESIAN_POINT('Ctrl Pts',(42.5810513815623,31.5404524382925,-50.5662));
#252382=CARTESIAN_POINT('Ctrl Pts',(43.0627766507519,30.7060797967663,-50.5078666666667));
#252383=CARTESIAN_POINT('Ctrl Pts',(43.5445019199415,29.87170715524,-50.4495333333333));
#252384=CARTESIAN_POINT('Ctrl Pts',(44.5079524583208,29.87170715524,-50.3912));
#252385=CARTESIAN_POINT('Ctrl Pts',(45.4714029967,29.87170715524,-50.3328666666666));
#252386=CARTESIAN_POINT('Ctrl Pts',(45.9531282658897,30.7060797967663,-50.2745333333333));
#252387=CARTESIAN_POINT('Ctrl Pts',(46.4348535350793,31.5404524382925,-50.2162));
#252388=CARTESIAN_POINT('Ctrl Pts',(45.9531282658897,32.3748250798187,-50.1578666666667));
#252389=CARTESIAN_POINT('Ctrl Pts',(45.4714029967,33.2091977213449,-50.0995333333333));
#252390=CARTESIAN_POINT('Ctrl Pts',(44.5079524583208,33.2091977213449,-50.0412));
#252391=CARTESIAN_POINT('Ctrl Pts',(43.5445019199415,33.2091977213449,-49.9828666666667));
#252392=CARTESIAN_POINT('Ctrl Pts',(43.0627766507519,32.3748250798187,-49.9245333333334));
#252393=CARTESIAN_POINT('Ctrl Pts',(42.5810513815623,31.5404524382925,-49.8662));
#252394=CARTESIAN_POINT('Ctrl Pts',(43.0627766507519,30.7060797967663,-49.8078666666667));
#252395=CARTESIAN_POINT('Ctrl Pts',(43.5445019199415,29.87170715524,-49.7495333333333));
#252396=CARTESIAN_POINT('Ctrl Pts',(44.5079524583208,29.87170715524,-49.6912));
#252397=CARTESIAN_POINT('Ctrl Pts',(45.4714029967,29.87170715524,-49.6328666666667));
#252398=CARTESIAN_POINT('Ctrl Pts',(45.9531282658897,30.7060797967663,-49.5745333333333));
#252399=CARTESIAN_POINT('Ctrl Pts',(46.4348535350793,31.5404524382925,-49.5162));
#252400=CARTESIAN_POINT('Ctrl Pts',(45.9531282658897,32.3748250798187,-49.4578666666667));
#252401=CARTESIAN_POINT('Ctrl Pts',(45.4714029967,33.2091977213449,-49.3995333333333));
#252402=CARTESIAN_POINT('Ctrl Pts',(44.5079524583208,33.2091977213449,-49.3412));
#252403=CARTESIAN_POINT('Ctrl Pts',(43.5445019199415,33.2091977213449,-49.2828666666666));
#252404=CARTESIAN_POINT('Ctrl Pts',(43.0627766507519,32.3748250798187,-49.2245333333333));
#252405=CARTESIAN_POINT('Ctrl Pts',(42.5810513815623,31.5404524382925,-49.1662));
#252406=CARTESIAN_POINT('Ctrl Pts',(43.0627766507519,30.7060797967663,-49.1078666666667));
#252407=CARTESIAN_POINT('Ctrl Pts',(43.5445019199415,29.87170715524,-49.0495333333334));
#252408=CARTESIAN_POINT('Ctrl Pts',(44.5079524583208,29.87170715524,-48.9912));
#252409=CARTESIAN_POINT('Ctrl Pts',(45.4714029967,29.87170715524,-48.9328666666667));
#252410=CARTESIAN_POINT('Ctrl Pts',(45.9531282658897,30.7060797967663,-48.8745333333333));
#252411=CARTESIAN_POINT('Ctrl Pts',(46.4348535350793,31.5404524382925,-48.8162));
#252412=CARTESIAN_POINT('Ctrl Pts',(45.9531282658897,32.3748250798187,-48.7578666666667));
#252413=CARTESIAN_POINT('Ctrl Pts',(45.4714029967,33.2091977213449,-48.6995333333334));
#252414=CARTESIAN_POINT('Ctrl Pts',(44.5079524583208,33.2091977213449,-48.6412));
#252415=CARTESIAN_POINT('Ctrl Pts',(43.5445019199415,33.2091977213449,-48.5828666666667));
#252416=CARTESIAN_POINT('Ctrl Pts',(43.0627766507519,32.3748250798187,-48.5245333333333));
#252417=CARTESIAN_POINT('Ctrl Pts',(42.5810513815623,31.5404524382925,-48.4662));
#252418=CARTESIAN_POINT('Ctrl Pts',(43.0627766507519,30.7060797967663,-48.4078666666667));
#252419=CARTESIAN_POINT('Ctrl Pts',(43.5445019199415,29.87170715524,-48.3495333333333));
#252420=CARTESIAN_POINT('Ctrl Pts',(44.5079524583208,29.87170715524,-48.2912));
#252421=CARTESIAN_POINT('Ctrl Pts',(45.4714029967,29.87170715524,-48.2328666666667));
#252422=CARTESIAN_POINT('Ctrl Pts',(45.9531282658897,30.7060797967663,-48.1745333333334));
#252423=CARTESIAN_POINT('Ctrl Pts',(46.4348535350793,31.5404524382925,-48.1162));
#252424=CARTESIAN_POINT('Ctrl Pts',(45.9531282658897,32.3748250798187,-48.0578666666667));
#252425=CARTESIAN_POINT('Ctrl Pts',(45.4714029967,33.2091977213449,-47.9995333333334));
#252426=CARTESIAN_POINT('Ctrl Pts',(44.5079524583208,33.2091977213449,-47.9412));
#252427=CARTESIAN_POINT('Ctrl Pts',(43.5445019199415,33.2091977213449,-47.8828666666667));
#252428=CARTESIAN_POINT('Ctrl Pts',(43.0627766507519,32.3748250798187,-47.8245333333333));
#252429=CARTESIAN_POINT('Ctrl Pts',(42.5810513815623,31.5404524382925,-47.7662));
#252430=CARTESIAN_POINT('Ctrl Pts',(43.0627766507519,30.7060797967663,-47.7078666666667));
#252431=CARTESIAN_POINT('Ctrl Pts',(43.5445019199415,29.87170715524,-47.6495333333334));
#252432=CARTESIAN_POINT('Ctrl Pts',(44.5079524583208,29.87170715524,-47.5912));
#252433=CARTESIAN_POINT('Ctrl Pts',(45.4714029967,29.87170715524,-47.5328666666667));
#252434=CARTESIAN_POINT('Ctrl Pts',(45.9531282658897,30.7060797967663,-47.4745333333334));
#252435=CARTESIAN_POINT('Ctrl Pts',(46.4348535350793,31.5404524382925,-47.4162));
#252436=CARTESIAN_POINT('Ctrl Pts',(45.9531282658897,32.3748250798187,-47.3578666666667));
#252437=CARTESIAN_POINT('Ctrl Pts',(45.4714029967,33.2091977213449,-47.2995333333334));
#252438=CARTESIAN_POINT('Ctrl Pts',(44.5079524583208,33.2091977213449,-47.2412));
#252439=CARTESIAN_POINT('Ctrl Pts',(43.5445019199415,33.2091977213449,-47.1828666666667));
#252440=CARTESIAN_POINT('Ctrl Pts',(43.0627766507519,32.3748250798187,-47.1245333333333));
#252441=CARTESIAN_POINT('Ctrl Pts',(42.5810513815623,31.5404524382925,-47.0662));
#252442=CARTESIAN_POINT('Ctrl Pts',(43.0627766507519,30.7060797967663,-47.0078666666667));
#252443=CARTESIAN_POINT('Ctrl Pts',(43.5445019199415,29.87170715524,-46.9495333333334));
#252444=CARTESIAN_POINT('Ctrl Pts',(44.5079524583208,29.87170715524,-46.8912));
#252445=CARTESIAN_POINT('Ctrl Pts',(45.4714029967,29.87170715524,-46.8328666666667));
#252446=CARTESIAN_POINT('Ctrl Pts',(45.9531282658897,30.7060797967663,-46.7745333333333));
#252447=CARTESIAN_POINT('Ctrl Pts',(46.4348535350793,31.5404524382925,-46.7162));
#252448=CARTESIAN_POINT('Ctrl Pts',(45.9531282658897,32.3748250798187,-46.6578666666667));
#252449=CARTESIAN_POINT('Ctrl Pts',(45.4714029967,33.2091977213449,-46.5995333333333));
#252450=CARTESIAN_POINT('Ctrl Pts',(44.5079524583208,33.2091977213449,-46.5412));
#252451=CARTESIAN_POINT('Ctrl Pts',(43.5445019199415,33.2091977213449,-46.4828666666667));
#252452=CARTESIAN_POINT('Ctrl Pts',(43.0627766507519,32.3748250798187,-46.4245333333333));
#252453=CARTESIAN_POINT('Ctrl Pts',(42.5810513815623,31.5404524382925,-46.3662));
#252454=CARTESIAN_POINT('Ctrl Pts',(43.0627766507519,30.7060797967663,-46.3078666666667));
#252455=CARTESIAN_POINT('Ctrl Pts',(43.5445019199415,29.87170715524,-46.2495333333334));
#252456=CARTESIAN_POINT('Ctrl Pts',(44.5079524583208,29.87170715524,-46.1912));
#252457=CARTESIAN_POINT('Ctrl Pts',(45.4714029967,29.87170715524,-46.1328666666667));
#252458=CARTESIAN_POINT('Ctrl Pts',(45.9531282658897,30.7060797967663,-46.0745333333334));
#252459=CARTESIAN_POINT('Ctrl Pts',(46.4348535350793,31.5404524382925,-46.0162));
#252460=CARTESIAN_POINT('Ctrl Pts',(45.9531282658897,32.3748250798187,-45.9578666666667));
#252461=CARTESIAN_POINT('Ctrl Pts',(45.4714029967,33.2091977213449,-45.8995333333333));
#252462=CARTESIAN_POINT('Ctrl Pts',(44.5079524583208,33.2091977213449,-45.8412));
#252463=CARTESIAN_POINT('Ctrl Pts',(43.5445019199415,33.2091977213449,-45.7828666666667));
#252464=CARTESIAN_POINT('Ctrl Pts',(43.0627766507519,32.3748250798187,-45.7245333333333));
#252465=CARTESIAN_POINT('Ctrl Pts',(42.5810513815623,31.5404524382925,-45.6662));
#252466=CARTESIAN_POINT('Ctrl Pts',(43.0627766507519,30.7060797967663,-45.6078666666667));
#252467=CARTESIAN_POINT('Ctrl Pts',(43.5445019199415,29.87170715524,-45.5495333333333));
#252468=CARTESIAN_POINT('Ctrl Pts',(44.5079524583208,29.87170715524,-45.4912));
#252469=CARTESIAN_POINT('Ctrl Pts',(45.4714029967,29.87170715524,-45.4328666666666));
#252470=CARTESIAN_POINT('Ctrl Pts',(45.9531282658897,30.7060797967663,-45.3745333333333));
#252471=CARTESIAN_POINT('Ctrl Pts',(46.4348535350793,31.5404524382925,-45.3162));
#252472=CARTESIAN_POINT('Ctrl Pts',(45.9531282658897,32.3748250798187,-45.2578666666667));
#252473=CARTESIAN_POINT('Ctrl Pts',(45.4714029967,33.2091977213449,-45.1995333333333));
#252474=CARTESIAN_POINT('Ctrl Pts',(44.5079524583208,33.2091977213449,-45.1412));
#252475=CARTESIAN_POINT('Ctrl Pts',(43.5445019199415,33.2091977213449,-45.0828666666667));
#252476=CARTESIAN_POINT('Ctrl Pts',(43.0627766507519,32.3748250798187,-45.0245333333333));
#252477=CARTESIAN_POINT('Ctrl Pts',(42.5810513815623,31.5404524382925,-44.9662));
#252478=CARTESIAN_POINT('Ctrl Pts',(43.0627766507519,30.7060797967663,-44.9078666666666));
#252479=CARTESIAN_POINT('Ctrl Pts',(43.5445019199415,29.87170715524,-44.8495333333333));
#252480=CARTESIAN_POINT('Ctrl Pts',(44.5079524583208,29.87170715524,-44.7912));
#252481=CARTESIAN_POINT('Ctrl Pts',(45.4714029967,29.87170715524,-44.7328666666666));
#252482=CARTESIAN_POINT('Ctrl Pts',(45.9531282658897,30.7060797967663,-44.6745333333334));
#252483=CARTESIAN_POINT('Ctrl Pts',(46.4348535350793,31.5404524382925,-44.6162));
#252484=CARTESIAN_POINT('Ctrl Pts',(45.9531282658897,32.3748250798187,-44.5578666666667));
#252485=CARTESIAN_POINT('Ctrl Pts',(45.4714029967,33.2091977213449,-44.4995333333333));
#252486=CARTESIAN_POINT('Ctrl Pts',(44.5079524583208,33.2091977213449,-44.4412));
#252487=CARTESIAN_POINT('Ctrl Pts',(43.5445019199415,33.2091977213449,-44.3828666666667));
#252488=CARTESIAN_POINT('Ctrl Pts',(43.0627766507519,32.3748250798187,-44.3245333333334));
#252489=CARTESIAN_POINT('Ctrl Pts',(42.5810513815623,31.5404524382925,-44.2662));
#252490=CARTESIAN_POINT('Ctrl Pts',(43.0627766507519,30.7060797967663,-44.2078666666667));
#252491=CARTESIAN_POINT('Ctrl Pts',(43.5445019199415,29.87170715524,-44.1495333333334));
#252492=CARTESIAN_POINT('Ctrl Pts',(44.5079524583208,29.87170715524,-44.0912));
#252493=CARTESIAN_POINT('Ctrl Pts',(45.4714029967,29.87170715524,-44.0328666666667));
#252494=CARTESIAN_POINT('Ctrl Pts',(45.9531282658897,30.7060797967663,-43.9745333333333));
#252495=CARTESIAN_POINT('Ctrl Pts',(46.4348535350793,31.5404524382925,-43.9162));
#252496=CARTESIAN_POINT('Ctrl Pts',(45.9531282658897,32.3748250798187,-43.8578666666667));
#252497=CARTESIAN_POINT('Ctrl Pts',(45.4714029967,33.2091977213449,-43.7995333333334));
#252498=CARTESIAN_POINT('Ctrl Pts',(44.5079524583208,33.2091977213449,-43.7412));
#252499=CARTESIAN_POINT('Ctrl Pts',(43.5445019199415,33.2091977213449,-43.6828666666667));
#252500=CARTESIAN_POINT('Ctrl Pts',(43.0627766507519,32.3748250798187,-43.6245333333333));
#252501=CARTESIAN_POINT('Ctrl Pts',(42.5810513815623,31.5404524382925,-43.5662));
#252502=CARTESIAN_POINT('Ctrl Pts',(43.0627766507519,30.7060797967663,-43.5078666666667));
#252503=CARTESIAN_POINT('Ctrl Pts',(43.5445019199415,29.87170715524,-43.4495333333334));
#252504=CARTESIAN_POINT('Ctrl Pts',(44.5079524583208,29.87170715524,-43.3912));
#252505=CARTESIAN_POINT('Ctrl Pts',(45.4714029967,29.87170715524,-43.3328666666667));
#252506=CARTESIAN_POINT('Ctrl Pts',(45.9531282658897,30.7060797967663,-43.2745333333334));
#252507=CARTESIAN_POINT('Ctrl Pts',(46.4348535350793,31.5404524382925,-43.2162));
#252508=CARTESIAN_POINT('Ctrl Pts',(45.9531282658897,32.3748250798187,-43.1578666666667));
#252509=CARTESIAN_POINT('Ctrl Pts',(45.4714029967,33.2091977213449,-43.0995333333334));
#252510=CARTESIAN_POINT('Ctrl Pts',(44.5079524583208,33.2091977213449,-43.0412));
#252511=CARTESIAN_POINT('Ctrl Pts',(43.5445019199415,33.2091977213449,-42.9828666666667));
#252512=CARTESIAN_POINT('Ctrl Pts',(43.0627766507519,32.3748250798187,-42.9245333333334));
#252513=CARTESIAN_POINT('Ctrl Pts',(42.5810513815623,31.5404524382925,-42.8662));
#252514=CARTESIAN_POINT('Ctrl Pts',(43.0627766507519,30.7060797967663,-42.8078666666667));
#252515=CARTESIAN_POINT('Ctrl Pts',(43.5445019199415,29.87170715524,-42.7495333333334));
#252516=CARTESIAN_POINT('Ctrl Pts',(44.5079524583208,29.87170715524,-42.6912));
#252517=CARTESIAN_POINT('Ctrl Pts',(45.4714029967,29.87170715524,-42.6328666666667));
#252518=CARTESIAN_POINT('Ctrl Pts',(45.9531282658897,30.7060797967663,-42.5745333333333));
#252519=CARTESIAN_POINT('Ctrl Pts',(46.4348535350793,31.5404524382925,-42.5162));
#252520=CARTESIAN_POINT('Ctrl Pts',(45.9531282658897,32.3748250798187,-42.4578666666667));
#252521=CARTESIAN_POINT('Ctrl Pts',(45.4714029967,33.2091977213449,-42.3995333333334));
#252522=CARTESIAN_POINT('Ctrl Pts',(44.5079524583208,33.2091977213449,-42.3412));
#252523=CARTESIAN_POINT('Ctrl Pts',(43.5445019199415,33.2091977213449,-42.2828666666667));
#252524=CARTESIAN_POINT('Ctrl Pts',(43.0627766507519,32.3748250798187,-42.2245333333333));
#252525=CARTESIAN_POINT('Ctrl Pts',(42.5810513815623,31.5404524382925,-42.1662));
#252526=CARTESIAN_POINT('Ctrl Pts',(43.0627766507519,30.7060797967663,-42.1078666666667));
#252527=CARTESIAN_POINT('Ctrl Pts',(43.5445019199415,29.87170715524,-42.0495333333334));
#252528=CARTESIAN_POINT('Ctrl Pts',(44.5079524583208,29.87170715524,-41.9912));
#252529=CARTESIAN_POINT('Ctrl Pts',(45.4714029967,29.87170715524,-41.9328666666667));
#252530=CARTESIAN_POINT('Ctrl Pts',(45.9531282658897,30.7060797967663,-41.8745333333334));
#252531=CARTESIAN_POINT('Ctrl Pts',(46.4348535350793,31.5404524382925,-41.8162));
#252532=CARTESIAN_POINT('Ctrl Pts',(45.9531282658897,32.3748250798187,-41.7578666666667));
#252533=CARTESIAN_POINT('Ctrl Pts',(45.4714029967,33.2091977213449,-41.6995333333333));
#252534=CARTESIAN_POINT('Ctrl Pts',(44.5079524583208,33.2091977213449,-41.6412));
#252535=CARTESIAN_POINT('Ctrl Pts',(43.5445019199415,33.2091977213449,-41.5828666666667));
#252536=CARTESIAN_POINT('Ctrl Pts',(43.0627766507519,32.3748250798187,-41.5245333333334));
#252537=CARTESIAN_POINT('Ctrl Pts',(42.5810513815623,31.5404524382925,-41.4662));
#252538=CARTESIAN_POINT('Ctrl Pts',(43.0627766507519,30.7060797967663,-41.4078666666667));
#252539=CARTESIAN_POINT('Ctrl Pts',(43.5445019199415,29.87170715524,-41.3495333333333));
#252540=CARTESIAN_POINT('Ctrl Pts',(44.5079524583208,29.87170715524,-41.2912));
#252541=CARTESIAN_POINT('Ctrl Pts',(45.4714029967,29.87170715524,-41.2328666666667));
#252542=CARTESIAN_POINT('Ctrl Pts',(45.9531282658897,30.7060797967663,-41.1745333333334));
#252543=CARTESIAN_POINT('Ctrl Pts',(46.4348535350793,31.5404524382925,-41.1162));
#252544=CARTESIAN_POINT('Ctrl Pts',(45.9531282658897,32.3748250798187,-41.0578666666667));
#252545=CARTESIAN_POINT('Ctrl Pts',(45.4714029967,33.2091977213449,-40.9995333333333));
#252546=CARTESIAN_POINT('Ctrl Pts',(44.5079524583208,33.2091977213449,-40.9412));
#252547=CARTESIAN_POINT('Ctrl Pts',(43.5445019199415,33.2091977213449,-40.8828666666667));
#252548=CARTESIAN_POINT('Ctrl Pts',(43.0627766507519,32.3748250798187,-40.8245333333333));
#252549=CARTESIAN_POINT('Ctrl Pts',(42.5810513815623,31.5404524382925,-40.7662));
#252550=CARTESIAN_POINT('Ctrl Pts',(43.0627766507519,30.7060797967663,-40.7078666666667));
#252551=CARTESIAN_POINT('Ctrl Pts',(43.5445019199415,29.87170715524,-40.6495333333333));
#252552=CARTESIAN_POINT('Ctrl Pts',(44.5079524583208,29.87170715524,-40.5912));
#252553=CARTESIAN_POINT('Ctrl Pts',(45.4714029967,29.87170715524,-40.5328666666667));
#252554=CARTESIAN_POINT('Ctrl Pts',(45.9531282658897,30.7060797967663,-40.4745333333334));
#252555=CARTESIAN_POINT('Ctrl Pts',(46.4348535350793,31.5404524382925,-40.4162));
#252556=CARTESIAN_POINT('Ctrl Pts',(45.9531282658897,32.3748250798187,-40.3578666666667));
#252557=CARTESIAN_POINT('Ctrl Pts',(45.4714029967,33.2091977213449,-40.2995333333333));
#252558=CARTESIAN_POINT('Ctrl Pts',(44.5079524583208,33.2091977213449,-40.2412));
#252559=CARTESIAN_POINT('Ctrl Pts',(43.5445019199415,33.2091977213449,-40.1828666666667));
#252560=CARTESIAN_POINT('Ctrl Pts',(43.0627766507519,32.3748250798187,-40.1245333333334));
#252561=CARTESIAN_POINT('Ctrl Pts',(42.5810513815623,31.5404524382925,-40.0662));
#252562=CARTESIAN_POINT('Ctrl Pts',(43.0627766507519,30.7060797967663,-40.0078666666667));
#252563=CARTESIAN_POINT('Ctrl Pts',(43.5445019199415,29.87170715524,-39.9495333333333));
#252564=CARTESIAN_POINT('Ctrl Pts',(44.5079524583208,29.87170715524,-39.8912));
#252565=CARTESIAN_POINT('Ctrl Pts',(45.4714029967,29.87170715524,-39.8328666666666));
#252566=CARTESIAN_POINT('Ctrl Pts',(45.9531282658897,30.7060797967663,-39.7745333333334));
#252567=CARTESIAN_POINT('Ctrl Pts',(46.4348535350793,31.5404524382925,-39.7162));
#252568=CARTESIAN_POINT('Ctrl Pts',(45.9531282658897,32.3748250798187,-39.6578666666667));
#252569=CARTESIAN_POINT('Ctrl Pts',(45.4714029967,33.2091977213449,-39.5995333333333));
#252570=CARTESIAN_POINT('Ctrl Pts',(44.5079524583208,33.2091977213449,-39.5412));
#252571=CARTESIAN_POINT('Ctrl Pts',(43.5445019199415,33.2091977213449,-39.4828666666666));
#252572=CARTESIAN_POINT('Ctrl Pts',(43.0627766507519,32.3748250798187,-39.4245333333334));
#252573=CARTESIAN_POINT('Ctrl Pts',(42.5810513815623,31.5404524382925,-39.3662));
#252574=CARTESIAN_POINT('Ctrl Pts',(43.0627766507519,30.7060797967663,-39.3078666666666));
#252575=CARTESIAN_POINT('Ctrl Pts',(43.5445019199415,29.87170715524,-39.2495333333333));
#252576=CARTESIAN_POINT('Ctrl Pts',(44.5079524583208,29.87170715524,-39.1912));
#252577=CARTESIAN_POINT('Ctrl Pts',(45.4714029967,29.87170715524,-39.1328666666667));
#252578=CARTESIAN_POINT('Ctrl Pts',(45.9531282658897,30.7060797967663,-39.0745333333333));
#252579=CARTESIAN_POINT('Ctrl Pts',(46.4348535350793,31.5404524382925,-39.0162));
#252580=CARTESIAN_POINT('Ctrl Pts',(45.9531282658897,32.3748250798187,-38.9578666666667));
#252581=CARTESIAN_POINT('Ctrl Pts',(45.4714029967,33.2091977213449,-38.8995333333334));
#252582=CARTESIAN_POINT('Ctrl Pts',(44.5079524583208,33.2091977213449,-38.8412));
#252583=CARTESIAN_POINT('Ctrl Pts',(43.5445019199415,33.2091977213449,-38.7828666666667));
#252584=CARTESIAN_POINT('Ctrl Pts',(43.0627766507519,32.3748250798187,-38.7245333333334));
#252585=CARTESIAN_POINT('Ctrl Pts',(42.5810513815623,31.5404524382925,-38.6662));
#252586=CARTESIAN_POINT('Ctrl Pts',(43.0627766507519,30.7060797967663,-38.6078666666667));
#252587=CARTESIAN_POINT('Ctrl Pts',(43.5445019199415,29.87170715524,-38.5495333333334));
#252588=CARTESIAN_POINT('Ctrl Pts',(44.5079524583208,29.87170715524,-38.4912));
#252589=CARTESIAN_POINT('Ctrl Pts',(45.4714029967,29.87170715524,-38.4328666666667));
#252590=CARTESIAN_POINT('Ctrl Pts',(45.9531282658897,30.7060797967663,-38.3745333333333));
#252591=CARTESIAN_POINT('Ctrl Pts',(46.4348535350793,31.5404524382925,-38.3162));
#252592=CARTESIAN_POINT('Ctrl Pts',(45.9531282658897,32.3748250798187,-38.2578666666667));
#252593=CARTESIAN_POINT('Ctrl Pts',(45.4714029967,33.2091977213449,-38.1995333333333));
#252594=CARTESIAN_POINT('Ctrl Pts',(44.5079524583208,33.2091977213449,-38.1412));
#252595=CARTESIAN_POINT('Ctrl Pts',(43.5445019199415,33.2091977213449,-38.0828666666667));
#252596=CARTESIAN_POINT('Ctrl Pts',(43.0627766507519,32.3748250798187,-38.0245333333334));
#252597=CARTESIAN_POINT('Ctrl Pts',(42.5810513815623,31.5404524382925,-37.9662));
#252598=CARTESIAN_POINT('Ctrl Pts',(43.0627766507519,30.7060797967663,-37.9078666666667));
#252599=CARTESIAN_POINT('Ctrl Pts',(43.5445019199415,29.87170715524,-37.8495333333334));
#252600=CARTESIAN_POINT('Ctrl Pts',(44.5079524583208,29.87170715524,-37.7912));
#252601=CARTESIAN_POINT('Ctrl Pts',(45.4714029967,29.87170715524,-37.7328666666667));
#252602=CARTESIAN_POINT('Ctrl Pts',(45.9531282658897,30.7060797967663,-37.6745333333334));
#252603=CARTESIAN_POINT('Ctrl Pts',(46.4348535350793,31.5404524382925,-37.6162));
#252604=CARTESIAN_POINT('Ctrl Pts',(45.9531282658897,32.3748250798187,-37.5578666666667));
#252605=CARTESIAN_POINT('Ctrl Pts',(45.4714029967,33.2091977213449,-37.4995333333334));
#252606=CARTESIAN_POINT('Ctrl Pts',(44.5079524583208,33.2091977213449,-37.4412));
#252607=CARTESIAN_POINT('Ctrl Pts',(43.5445019199415,33.2091977213449,-37.3828666666667));
#252608=CARTESIAN_POINT('Ctrl Pts',(43.0627766507519,32.3748250798187,-37.3245333333333));
#252609=CARTESIAN_POINT('Ctrl Pts',(42.5810513815623,31.5404524382925,-37.2662));
#252610=CARTESIAN_POINT('Ctrl Pts',(43.0627766507519,30.7060797967663,-37.2078666666667));
#252611=CARTESIAN_POINT('Ctrl Pts',(43.5445019199415,29.87170715524,-37.1495333333334));
#252612=CARTESIAN_POINT('Ctrl Pts',(44.5079524583208,29.87170715524,-37.0912));
#252613=CARTESIAN_POINT('Ctrl Pts',(45.4714029967,29.87170715524,-37.0328666666667));
#252614=CARTESIAN_POINT('Ctrl Pts',(45.9531282658897,30.7060797967663,-36.9745333333333));
#252615=CARTESIAN_POINT('Ctrl Pts',(46.4348535350793,31.5404524382925,-36.9162));
#252616=CARTESIAN_POINT('Ctrl Pts',(45.9531282658897,32.3748250798187,-36.8578666666667));
#252617=CARTESIAN_POINT('Ctrl Pts',(45.8905905257689,32.4831436230984,-36.8502938132714));
#252618=CARTESIAN_POINT('Ctrl Pts',(45.8126048724392,32.5809296836203,-36.8421538241181));
#252619=CARTESIAN_POINT('Ctrl Pts',(44.5079524583208,33.6091932047179,-52.6102625));
#252620=CARTESIAN_POINT('Ctrl Pts',(43.3135644199415,33.6091932047179,-52.5519291666666));
#252621=CARTESIAN_POINT('Ctrl Pts',(42.7163704007519,32.5748228215052,-52.4935958333333));
#252622=CARTESIAN_POINT('Ctrl Pts',(42.1191763815623,31.5404524382925,-52.4352625));
#252623=CARTESIAN_POINT('Ctrl Pts',(42.7163704007519,30.5060820550798,-52.3769291666667));
#252624=CARTESIAN_POINT('Ctrl Pts',(43.3135644199415,29.4717116718671,-52.3185958333334));
#252625=CARTESIAN_POINT('Ctrl Pts',(44.5079524583208,29.4717116718671,-52.2602625));
#252626=CARTESIAN_POINT('Ctrl Pts',(45.7023404967,29.4717116718671,-52.2019291666667));
#252627=CARTESIAN_POINT('Ctrl Pts',(46.2995345158897,30.5060820550798,-52.1435958333333));
#252628=CARTESIAN_POINT('Ctrl Pts',(46.8967285350793,31.5404524382925,-52.0852625));
#252629=CARTESIAN_POINT('Ctrl Pts',(46.2995345158897,32.5748228215052,-52.0269291666667));
#252630=CARTESIAN_POINT('Ctrl Pts',(45.7023404967,33.6091932047179,-51.9685958333333));
#252631=CARTESIAN_POINT('Ctrl Pts',(44.5079524583208,33.6091932047179,-51.9102625));
#252632=CARTESIAN_POINT('Ctrl Pts',(43.3135644199415,33.6091932047179,-51.8519291666667));
#252633=CARTESIAN_POINT('Ctrl Pts',(42.7163704007519,32.5748228215052,-51.7935958333333));
#252634=CARTESIAN_POINT('Ctrl Pts',(42.1191763815623,31.5404524382925,-51.7352625));
#252635=CARTESIAN_POINT('Ctrl Pts',(42.7163704007519,30.5060820550798,-51.6769291666667));
#252636=CARTESIAN_POINT('Ctrl Pts',(43.3135644199415,29.4717116718671,-51.6185958333333));
#252637=CARTESIAN_POINT('Ctrl Pts',(44.5079524583208,29.4717116718671,-51.5602625));
#252638=CARTESIAN_POINT('Ctrl Pts',(45.7023404967,29.4717116718671,-51.5019291666666));
#252639=CARTESIAN_POINT('Ctrl Pts',(46.2995345158897,30.5060820550798,-51.4435958333333));
#252640=CARTESIAN_POINT('Ctrl Pts',(46.8967285350793,31.5404524382925,-51.3852625));
#252641=CARTESIAN_POINT('Ctrl Pts',(46.2995345158897,32.5748228215052,-51.3269291666667));
#252642=CARTESIAN_POINT('Ctrl Pts',(45.7023404967,33.6091932047179,-51.2685958333333));
#252643=CARTESIAN_POINT('Ctrl Pts',(44.5079524583208,33.6091932047179,-51.2102625));
#252644=CARTESIAN_POINT('Ctrl Pts',(43.3135644199415,33.6091932047179,-51.1519291666666));
#252645=CARTESIAN_POINT('Ctrl Pts',(42.7163704007519,32.5748228215052,-51.0935958333334));
#252646=CARTESIAN_POINT('Ctrl Pts',(42.1191763815623,31.5404524382925,-51.0352625));
#252647=CARTESIAN_POINT('Ctrl Pts',(42.7163704007519,30.5060820550798,-50.9769291666667));
#252648=CARTESIAN_POINT('Ctrl Pts',(43.3135644199415,29.4717116718671,-50.9185958333333));
#252649=CARTESIAN_POINT('Ctrl Pts',(44.5079524583208,29.4717116718671,-50.8602625));
#252650=CARTESIAN_POINT('Ctrl Pts',(45.7023404967,29.4717116718671,-50.8019291666667));
#252651=CARTESIAN_POINT('Ctrl Pts',(46.2995345158897,30.5060820550798,-50.7435958333333));
#252652=CARTESIAN_POINT('Ctrl Pts',(46.8967285350793,31.5404524382925,-50.6852625));
#252653=CARTESIAN_POINT('Ctrl Pts',(46.2995345158897,32.5748228215052,-50.6269291666667));
#252654=CARTESIAN_POINT('Ctrl Pts',(45.7023404967,33.6091932047179,-50.5685958333333));
#252655=CARTESIAN_POINT('Ctrl Pts',(44.5079524583208,33.6091932047179,-50.5102625));
#252656=CARTESIAN_POINT('Ctrl Pts',(43.3135644199415,33.6091932047179,-50.4519291666667));
#252657=CARTESIAN_POINT('Ctrl Pts',(42.7163704007519,32.5748228215052,-50.3935958333333));
#252658=CARTESIAN_POINT('Ctrl Pts',(42.1191763815623,31.5404524382925,-50.3352625));
#252659=CARTESIAN_POINT('Ctrl Pts',(42.7163704007519,30.5060820550798,-50.2769291666667));
#252660=CARTESIAN_POINT('Ctrl Pts',(43.3135644199415,29.4717116718671,-50.2185958333333));
#252661=CARTESIAN_POINT('Ctrl Pts',(44.5079524583208,29.4717116718671,-50.1602625));
#252662=CARTESIAN_POINT('Ctrl Pts',(45.7023404967,29.4717116718671,-50.1019291666667));
#252663=CARTESIAN_POINT('Ctrl Pts',(46.2995345158897,30.5060820550798,-50.0435958333333));
#252664=CARTESIAN_POINT('Ctrl Pts',(46.8967285350793,31.5404524382925,-49.9852625));
#252665=CARTESIAN_POINT('Ctrl Pts',(46.2995345158897,32.5748228215052,-49.9269291666667));
#252666=CARTESIAN_POINT('Ctrl Pts',(45.7023404967,33.6091932047179,-49.8685958333333));
#252667=CARTESIAN_POINT('Ctrl Pts',(44.5079524583208,33.6091932047179,-49.8102625));
#252668=CARTESIAN_POINT('Ctrl Pts',(43.3135644199415,33.6091932047179,-49.7519291666667));
#252669=CARTESIAN_POINT('Ctrl Pts',(42.7163704007519,32.5748228215052,-49.6935958333334));
#252670=CARTESIAN_POINT('Ctrl Pts',(42.1191763815623,31.5404524382925,-49.6352625));
#252671=CARTESIAN_POINT('Ctrl Pts',(42.7163704007519,30.5060820550798,-49.5769291666667));
#252672=CARTESIAN_POINT('Ctrl Pts',(43.3135644199415,29.4717116718671,-49.5185958333334));
#252673=CARTESIAN_POINT('Ctrl Pts',(44.5079524583208,29.4717116718671,-49.4602625));
#252674=CARTESIAN_POINT('Ctrl Pts',(45.7023404967,29.4717116718671,-49.4019291666667));
#252675=CARTESIAN_POINT('Ctrl Pts',(46.2995345158897,30.5060820550798,-49.3435958333333));
#252676=CARTESIAN_POINT('Ctrl Pts',(46.8967285350793,31.5404524382925,-49.2852625));
#252677=CARTESIAN_POINT('Ctrl Pts',(46.2995345158897,32.5748228215052,-49.2269291666667));
#252678=CARTESIAN_POINT('Ctrl Pts',(45.7023404967,33.6091932047179,-49.1685958333334));
#252679=CARTESIAN_POINT('Ctrl Pts',(44.5079524583208,33.6091932047179,-49.1102625));
#252680=CARTESIAN_POINT('Ctrl Pts',(43.3135644199415,33.6091932047179,-49.0519291666667));
#252681=CARTESIAN_POINT('Ctrl Pts',(42.7163704007519,32.5748228215052,-48.9935958333333));
#252682=CARTESIAN_POINT('Ctrl Pts',(42.1191763815623,31.5404524382925,-48.9352625));
#252683=CARTESIAN_POINT('Ctrl Pts',(42.7163704007519,30.5060820550798,-48.8769291666667));
#252684=CARTESIAN_POINT('Ctrl Pts',(43.3135644199415,29.4717116718671,-48.8185958333333));
#252685=CARTESIAN_POINT('Ctrl Pts',(44.5079524583208,29.4717116718671,-48.7602625));
#252686=CARTESIAN_POINT('Ctrl Pts',(45.7023404967,29.4717116718671,-48.7019291666667));
#252687=CARTESIAN_POINT('Ctrl Pts',(46.2995345158897,30.5060820550798,-48.6435958333333));
#252688=CARTESIAN_POINT('Ctrl Pts',(46.8967285350793,31.5404524382925,-48.5852625));
#252689=CARTESIAN_POINT('Ctrl Pts',(46.2995345158897,32.5748228215052,-48.5269291666667));
#252690=CARTESIAN_POINT('Ctrl Pts',(45.7023404967,33.6091932047179,-48.4685958333333));
#252691=CARTESIAN_POINT('Ctrl Pts',(44.5079524583208,33.6091932047179,-48.4102625));
#252692=CARTESIAN_POINT('Ctrl Pts',(43.3135644199415,33.6091932047179,-48.3519291666667));
#252693=CARTESIAN_POINT('Ctrl Pts',(42.7163704007519,32.5748228215052,-48.2935958333333));
#252694=CARTESIAN_POINT('Ctrl Pts',(42.1191763815623,31.5404524382925,-48.2352625));
#252695=CARTESIAN_POINT('Ctrl Pts',(42.7163704007519,30.5060820550798,-48.1769291666667));
#252696=CARTESIAN_POINT('Ctrl Pts',(43.3135644199415,29.4717116718671,-48.1185958333334));
#252697=CARTESIAN_POINT('Ctrl Pts',(44.5079524583208,29.4717116718671,-48.0602625));
#252698=CARTESIAN_POINT('Ctrl Pts',(45.7023404967,29.4717116718671,-48.0019291666667));
#252699=CARTESIAN_POINT('Ctrl Pts',(46.2995345158897,30.5060820550798,-47.9435958333334));
#252700=CARTESIAN_POINT('Ctrl Pts',(46.8967285350793,31.5404524382925,-47.8852625));
#252701=CARTESIAN_POINT('Ctrl Pts',(46.2995345158897,32.5748228215052,-47.8269291666667));
#252702=CARTESIAN_POINT('Ctrl Pts',(45.7023404967,33.6091932047179,-47.7685958333333));
#252703=CARTESIAN_POINT('Ctrl Pts',(44.5079524583208,33.6091932047179,-47.7102625));
#252704=CARTESIAN_POINT('Ctrl Pts',(43.3135644199415,33.6091932047179,-47.6519291666667));
#252705=CARTESIAN_POINT('Ctrl Pts',(42.7163704007519,32.5748228215052,-47.5935958333333));
#252706=CARTESIAN_POINT('Ctrl Pts',(42.1191763815623,31.5404524382925,-47.5352625));
#252707=CARTESIAN_POINT('Ctrl Pts',(42.7163704007519,30.5060820550798,-47.4769291666667));
#252708=CARTESIAN_POINT('Ctrl Pts',(43.3135644199415,29.4717116718671,-47.4185958333333));
#252709=CARTESIAN_POINT('Ctrl Pts',(44.5079524583208,29.4717116718671,-47.3602625));
#252710=CARTESIAN_POINT('Ctrl Pts',(45.7023404967,29.4717116718671,-47.3019291666666));
#252711=CARTESIAN_POINT('Ctrl Pts',(46.2995345158897,30.5060820550798,-47.2435958333333));
#252712=CARTESIAN_POINT('Ctrl Pts',(46.8967285350793,31.5404524382925,-47.1852625));
#252713=CARTESIAN_POINT('Ctrl Pts',(46.2995345158897,32.5748228215052,-47.1269291666667));
#252714=CARTESIAN_POINT('Ctrl Pts',(45.7023404967,33.6091932047179,-47.0685958333333));
#252715=CARTESIAN_POINT('Ctrl Pts',(44.5079524583208,33.6091932047179,-47.0102625));
#252716=CARTESIAN_POINT('Ctrl Pts',(43.3135644199415,33.6091932047179,-46.9519291666667));
#252717=CARTESIAN_POINT('Ctrl Pts',(42.7163704007519,32.5748228215052,-46.8935958333333));
#252718=CARTESIAN_POINT('Ctrl Pts',(42.1191763815623,31.5404524382925,-46.8352625));
#252719=CARTESIAN_POINT('Ctrl Pts',(42.7163704007519,30.5060820550798,-46.7769291666667));
#252720=CARTESIAN_POINT('Ctrl Pts',(43.3135644199415,29.4717116718671,-46.7185958333333));
#252721=CARTESIAN_POINT('Ctrl Pts',(44.5079524583208,29.4717116718671,-46.6602625));
#252722=CARTESIAN_POINT('Ctrl Pts',(45.7023404967,29.4717116718671,-46.6019291666667));
#252723=CARTESIAN_POINT('Ctrl Pts',(46.2995345158897,30.5060820550798,-46.5435958333334));
#252724=CARTESIAN_POINT('Ctrl Pts',(46.8967285350793,31.5404524382925,-46.4852625));
#252725=CARTESIAN_POINT('Ctrl Pts',(46.2995345158897,32.5748228215052,-46.4269291666667));
#252726=CARTESIAN_POINT('Ctrl Pts',(45.7023404967,33.6091932047179,-46.3685958333333));
#252727=CARTESIAN_POINT('Ctrl Pts',(44.5079524583208,33.6091932047179,-46.3102625));
#252728=CARTESIAN_POINT('Ctrl Pts',(43.3135644199415,33.6091932047179,-46.2519291666667));
#252729=CARTESIAN_POINT('Ctrl Pts',(42.7163704007519,32.5748228215052,-46.1935958333333));
#252730=CARTESIAN_POINT('Ctrl Pts',(42.1191763815623,31.5404524382925,-46.1352625));
#252731=CARTESIAN_POINT('Ctrl Pts',(42.7163704007519,30.5060820550798,-46.0769291666667));
#252732=CARTESIAN_POINT('Ctrl Pts',(43.3135644199415,29.4717116718671,-46.0185958333334));
#252733=CARTESIAN_POINT('Ctrl Pts',(44.5079524583208,29.4717116718671,-45.9602625));
#252734=CARTESIAN_POINT('Ctrl Pts',(45.7023404967,29.4717116718671,-45.9019291666667));
#252735=CARTESIAN_POINT('Ctrl Pts',(46.2995345158897,30.5060820550798,-45.8435958333333));
#252736=CARTESIAN_POINT('Ctrl Pts',(46.8967285350793,31.5404524382925,-45.7852625));
#252737=CARTESIAN_POINT('Ctrl Pts',(46.2995345158897,32.5748228215052,-45.7269291666667));
#252738=CARTESIAN_POINT('Ctrl Pts',(45.7023404967,33.6091932047179,-45.6685958333334));
#252739=CARTESIAN_POINT('Ctrl Pts',(44.5079524583208,33.6091932047179,-45.6102625));
#252740=CARTESIAN_POINT('Ctrl Pts',(43.3135644199415,33.6091932047179,-45.5519291666667));
#252741=CARTESIAN_POINT('Ctrl Pts',(42.7163704007519,32.5748228215052,-45.4935958333333));
#252742=CARTESIAN_POINT('Ctrl Pts',(42.1191763815623,31.5404524382925,-45.4352625));
#252743=CARTESIAN_POINT('Ctrl Pts',(42.7163704007519,30.5060820550798,-45.3769291666667));
#252744=CARTESIAN_POINT('Ctrl Pts',(43.3135644199415,29.4717116718671,-45.3185958333333));
#252745=CARTESIAN_POINT('Ctrl Pts',(44.5079524583208,29.4717116718671,-45.2602625));
#252746=CARTESIAN_POINT('Ctrl Pts',(45.7023404967,29.4717116718671,-45.2019291666667));
#252747=CARTESIAN_POINT('Ctrl Pts',(46.2995345158897,30.5060820550798,-45.1435958333333));
#252748=CARTESIAN_POINT('Ctrl Pts',(46.8967285350793,31.5404524382925,-45.0852625));
#252749=CARTESIAN_POINT('Ctrl Pts',(46.2995345158897,32.5748228215052,-45.0269291666667));
#252750=CARTESIAN_POINT('Ctrl Pts',(45.7023404967,33.6091932047179,-44.9685958333334));
#252751=CARTESIAN_POINT('Ctrl Pts',(44.5079524583208,33.6091932047179,-44.9102625));
#252752=CARTESIAN_POINT('Ctrl Pts',(43.3135644199415,33.6091932047179,-44.8519291666667));
#252753=CARTESIAN_POINT('Ctrl Pts',(42.7163704007519,32.5748228215052,-44.7935958333333));
#252754=CARTESIAN_POINT('Ctrl Pts',(42.1191763815623,31.5404524382925,-44.7352625));
#252755=CARTESIAN_POINT('Ctrl Pts',(42.7163704007519,30.5060820550798,-44.6769291666667));
#252756=CARTESIAN_POINT('Ctrl Pts',(43.3135644199415,29.4717116718671,-44.6185958333334));
#252757=CARTESIAN_POINT('Ctrl Pts',(44.5079524583208,29.4717116718671,-44.5602625));
#252758=CARTESIAN_POINT('Ctrl Pts',(45.7023404967,29.4717116718671,-44.5019291666667));
#252759=CARTESIAN_POINT('Ctrl Pts',(46.2995345158897,30.5060820550798,-44.4435958333333));
#252760=CARTESIAN_POINT('Ctrl Pts',(46.8967285350793,31.5404524382925,-44.3852625));
#252761=CARTESIAN_POINT('Ctrl Pts',(46.2995345158897,32.5748228215052,-44.3269291666667));
#252762=CARTESIAN_POINT('Ctrl Pts',(45.7023404967,33.6091932047179,-44.2685958333334));
#252763=CARTESIAN_POINT('Ctrl Pts',(44.5079524583208,33.6091932047179,-44.2102625));
#252764=CARTESIAN_POINT('Ctrl Pts',(43.3135644199415,33.6091932047179,-44.1519291666667));
#252765=CARTESIAN_POINT('Ctrl Pts',(42.7163704007519,32.5748228215052,-44.0935958333334));
#252766=CARTESIAN_POINT('Ctrl Pts',(42.1191763815623,31.5404524382925,-44.0352625));
#252767=CARTESIAN_POINT('Ctrl Pts',(42.7163704007519,30.5060820550798,-43.9769291666667));
#252768=CARTESIAN_POINT('Ctrl Pts',(43.3135644199415,29.4717116718671,-43.9185958333333));
#252769=CARTESIAN_POINT('Ctrl Pts',(44.5079524583208,29.4717116718671,-43.8602625));
#252770=CARTESIAN_POINT('Ctrl Pts',(45.7023404967,29.4717116718671,-43.8019291666667));
#252771=CARTESIAN_POINT('Ctrl Pts',(46.2995345158897,30.5060820550798,-43.7435958333334));
#252772=CARTESIAN_POINT('Ctrl Pts',(46.8967285350793,31.5404524382925,-43.6852625));
#252773=CARTESIAN_POINT('Ctrl Pts',(46.2995345158897,32.5748228215052,-43.6269291666667));
#252774=CARTESIAN_POINT('Ctrl Pts',(45.7023404967,33.6091932047179,-43.5685958333333));
#252775=CARTESIAN_POINT('Ctrl Pts',(44.5079524583208,33.6091932047179,-43.5102625));
#252776=CARTESIAN_POINT('Ctrl Pts',(43.3135644199415,33.6091932047179,-43.4519291666667));
#252777=CARTESIAN_POINT('Ctrl Pts',(42.7163704007519,32.5748228215052,-43.3935958333334));
#252778=CARTESIAN_POINT('Ctrl Pts',(42.1191763815623,31.5404524382925,-43.3352625));
#252779=CARTESIAN_POINT('Ctrl Pts',(42.7163704007519,30.5060820550798,-43.2769291666667));
#252780=CARTESIAN_POINT('Ctrl Pts',(43.3135644199415,29.4717116718671,-43.2185958333333));
#252781=CARTESIAN_POINT('Ctrl Pts',(44.5079524583208,29.4717116718671,-43.1602625));
#252782=CARTESIAN_POINT('Ctrl Pts',(45.7023404967,29.4717116718671,-43.1019291666667));
#252783=CARTESIAN_POINT('Ctrl Pts',(46.2995345158897,30.5060820550798,-43.0435958333334));
#252784=CARTESIAN_POINT('Ctrl Pts',(46.8967285350793,31.5404524382925,-42.9852625));
#252785=CARTESIAN_POINT('Ctrl Pts',(46.2995345158897,32.5748228215052,-42.9269291666667));
#252786=CARTESIAN_POINT('Ctrl Pts',(45.7023404967,33.6091932047179,-42.8685958333333));
#252787=CARTESIAN_POINT('Ctrl Pts',(44.5079524583208,33.6091932047179,-42.8102625));
#252788=CARTESIAN_POINT('Ctrl Pts',(43.3135644199415,33.6091932047179,-42.7519291666666));
#252789=CARTESIAN_POINT('Ctrl Pts',(42.7163704007519,32.5748228215052,-42.6935958333333));
#252790=CARTESIAN_POINT('Ctrl Pts',(42.1191763815623,31.5404524382925,-42.6352625));
#252791=CARTESIAN_POINT('Ctrl Pts',(42.7163704007519,30.5060820550798,-42.5769291666667));
#252792=CARTESIAN_POINT('Ctrl Pts',(43.3135644199415,29.4717116718671,-42.5185958333333));
#252793=CARTESIAN_POINT('Ctrl Pts',(44.5079524583208,29.4717116718671,-42.4602625));
#252794=CARTESIAN_POINT('Ctrl Pts',(45.7023404967,29.4717116718671,-42.4019291666666));
#252795=CARTESIAN_POINT('Ctrl Pts',(46.2995345158897,30.5060820550798,-42.3435958333334));
#252796=CARTESIAN_POINT('Ctrl Pts',(46.8967285350793,31.5404524382925,-42.2852625));
#252797=CARTESIAN_POINT('Ctrl Pts',(46.2995345158897,32.5748228215052,-42.2269291666667));
#252798=CARTESIAN_POINT('Ctrl Pts',(45.7023404967,33.6091932047179,-42.1685958333333));
#252799=CARTESIAN_POINT('Ctrl Pts',(44.5079524583208,33.6091932047179,-42.1102625));
#252800=CARTESIAN_POINT('Ctrl Pts',(43.3135644199415,33.6091932047179,-42.0519291666666));
#252801=CARTESIAN_POINT('Ctrl Pts',(42.7163704007519,32.5748228215052,-41.9935958333334));
#252802=CARTESIAN_POINT('Ctrl Pts',(42.1191763815623,31.5404524382925,-41.9352625));
#252803=CARTESIAN_POINT('Ctrl Pts',(42.7163704007519,30.5060820550798,-41.8769291666667));
#252804=CARTESIAN_POINT('Ctrl Pts',(43.3135644199415,29.4717116718671,-41.8185958333333));
#252805=CARTESIAN_POINT('Ctrl Pts',(44.5079524583208,29.4717116718671,-41.7602625));
#252806=CARTESIAN_POINT('Ctrl Pts',(45.7023404967,29.4717116718671,-41.7019291666666));
#252807=CARTESIAN_POINT('Ctrl Pts',(46.2995345158897,30.5060820550798,-41.6435958333334));
#252808=CARTESIAN_POINT('Ctrl Pts',(46.8967285350793,31.5404524382925,-41.5852625));
#252809=CARTESIAN_POINT('Ctrl Pts',(46.2995345158897,32.5748228215052,-41.5269291666667));
#252810=CARTESIAN_POINT('Ctrl Pts',(45.7023404967,33.6091932047179,-41.4685958333333));
#252811=CARTESIAN_POINT('Ctrl Pts',(44.5079524583208,33.6091932047179,-41.4102625));
#252812=CARTESIAN_POINT('Ctrl Pts',(43.3135644199415,33.6091932047179,-41.3519291666666));
#252813=CARTESIAN_POINT('Ctrl Pts',(42.7163704007519,32.5748228215052,-41.2935958333334));
#252814=CARTESIAN_POINT('Ctrl Pts',(42.1191763815623,31.5404524382925,-41.2352625));
#252815=CARTESIAN_POINT('Ctrl Pts',(42.7163704007519,30.5060820550798,-41.1769291666667));
#252816=CARTESIAN_POINT('Ctrl Pts',(43.3135644199415,29.4717116718671,-41.1185958333333));
#252817=CARTESIAN_POINT('Ctrl Pts',(44.5079524583208,29.4717116718671,-41.0602625));
#252818=CARTESIAN_POINT('Ctrl Pts',(45.7023404967,29.4717116718671,-41.0019291666666));
#252819=CARTESIAN_POINT('Ctrl Pts',(46.2995345158897,30.5060820550798,-40.9435958333334));
#252820=CARTESIAN_POINT('Ctrl Pts',(46.8967285350793,31.5404524382925,-40.8852625));
#252821=CARTESIAN_POINT('Ctrl Pts',(46.2995345158897,32.5748228215052,-40.8269291666667));
#252822=CARTESIAN_POINT('Ctrl Pts',(45.7023404967,33.6091932047179,-40.7685958333333));
#252823=CARTESIAN_POINT('Ctrl Pts',(44.5079524583208,33.6091932047179,-40.7102625));
#252824=CARTESIAN_POINT('Ctrl Pts',(43.3135644199415,33.6091932047179,-40.6519291666667));
#252825=CARTESIAN_POINT('Ctrl Pts',(42.7163704007519,32.5748228215052,-40.5935958333334));
#252826=CARTESIAN_POINT('Ctrl Pts',(42.1191763815623,31.5404524382925,-40.5352625));
#252827=CARTESIAN_POINT('Ctrl Pts',(42.7163704007519,30.5060820550798,-40.4769291666667));
#252828=CARTESIAN_POINT('Ctrl Pts',(43.3135644199415,29.4717116718671,-40.4185958333333));
#252829=CARTESIAN_POINT('Ctrl Pts',(44.5079524583208,29.4717116718671,-40.3602625));
#252830=CARTESIAN_POINT('Ctrl Pts',(45.7023404967,29.4717116718671,-40.3019291666667));
#252831=CARTESIAN_POINT('Ctrl Pts',(46.2995345158897,30.5060820550798,-40.2435958333334));
#252832=CARTESIAN_POINT('Ctrl Pts',(46.8967285350793,31.5404524382925,-40.1852625));
#252833=CARTESIAN_POINT('Ctrl Pts',(46.2995345158897,32.5748228215052,-40.1269291666666));
#252834=CARTESIAN_POINT('Ctrl Pts',(45.7023404967,33.6091932047179,-40.0685958333333));
#252835=CARTESIAN_POINT('Ctrl Pts',(44.5079524583208,33.6091932047179,-40.0102625));
#252836=CARTESIAN_POINT('Ctrl Pts',(43.3135644199415,33.6091932047179,-39.9519291666667));
#252837=CARTESIAN_POINT('Ctrl Pts',(42.7163704007519,32.5748228215052,-39.8935958333334));
#252838=CARTESIAN_POINT('Ctrl Pts',(42.1191763815623,31.5404524382925,-39.8352625));
#252839=CARTESIAN_POINT('Ctrl Pts',(42.7163704007519,30.5060820550798,-39.7769291666666));
#252840=CARTESIAN_POINT('Ctrl Pts',(43.3135644199415,29.4717116718671,-39.7185958333334));
#252841=CARTESIAN_POINT('Ctrl Pts',(44.5079524583208,29.4717116718671,-39.6602625));
#252842=CARTESIAN_POINT('Ctrl Pts',(45.7023404967,29.4717116718671,-39.6019291666667));
#252843=CARTESIAN_POINT('Ctrl Pts',(46.2995345158897,30.5060820550798,-39.5435958333333));
#252844=CARTESIAN_POINT('Ctrl Pts',(46.8967285350793,31.5404524382925,-39.4852625));
#252845=CARTESIAN_POINT('Ctrl Pts',(46.2995345158897,32.5748228215052,-39.4269291666667));
#252846=CARTESIAN_POINT('Ctrl Pts',(45.7023404967,33.6091932047179,-39.3685958333334));
#252847=CARTESIAN_POINT('Ctrl Pts',(44.5079524583208,33.6091932047179,-39.3102625));
#252848=CARTESIAN_POINT('Ctrl Pts',(43.3135644199415,33.6091932047179,-39.2519291666667));
#252849=CARTESIAN_POINT('Ctrl Pts',(42.7163704007519,32.5748228215052,-39.1935958333334));
#252850=CARTESIAN_POINT('Ctrl Pts',(42.1191763815623,31.5404524382925,-39.1352625));
#252851=CARTESIAN_POINT('Ctrl Pts',(42.7163704007519,30.5060820550798,-39.0769291666667));
#252852=CARTESIAN_POINT('Ctrl Pts',(43.3135644199415,29.4717116718671,-39.0185958333333));
#252853=CARTESIAN_POINT('Ctrl Pts',(44.5079524583208,29.4717116718671,-38.9602625));
#252854=CARTESIAN_POINT('Ctrl Pts',(45.7023404967,29.4717116718671,-38.9019291666667));
#252855=CARTESIAN_POINT('Ctrl Pts',(46.2995345158897,30.5060820550798,-38.8435958333333));
#252856=CARTESIAN_POINT('Ctrl Pts',(46.8967285350793,31.5404524382925,-38.7852625));
#252857=CARTESIAN_POINT('Ctrl Pts',(46.2995345158897,32.5748228215052,-38.7269291666667));
#252858=CARTESIAN_POINT('Ctrl Pts',(45.7023404967,33.6091932047179,-38.6685958333334));
#252859=CARTESIAN_POINT('Ctrl Pts',(44.5079524583208,33.6091932047179,-38.6102625));
#252860=CARTESIAN_POINT('Ctrl Pts',(43.3135644199415,33.6091932047179,-38.5519291666667));
#252861=CARTESIAN_POINT('Ctrl Pts',(42.7163704007519,32.5748228215052,-38.4935958333334));
#252862=CARTESIAN_POINT('Ctrl Pts',(42.1191763815623,31.5404524382925,-38.4352625));
#252863=CARTESIAN_POINT('Ctrl Pts',(42.7163704007519,30.5060820550798,-38.3769291666666));
#252864=CARTESIAN_POINT('Ctrl Pts',(43.3135644199415,29.4717116718671,-38.3185958333333));
#252865=CARTESIAN_POINT('Ctrl Pts',(44.5079524583208,29.4717116718671,-38.2602625));
#252866=CARTESIAN_POINT('Ctrl Pts',(45.7023404967,29.4717116718671,-38.2019291666667));
#252867=CARTESIAN_POINT('Ctrl Pts',(46.2995345158897,30.5060820550798,-38.1435958333334));
#252868=CARTESIAN_POINT('Ctrl Pts',(46.8967285350793,31.5404524382925,-38.0852625));
#252869=CARTESIAN_POINT('Ctrl Pts',(46.2995345158897,32.5748228215052,-38.0269291666667));
#252870=CARTESIAN_POINT('Ctrl Pts',(45.7023404967,33.6091932047179,-37.9685958333333));
#252871=CARTESIAN_POINT('Ctrl Pts',(44.5079524583208,33.6091932047179,-37.9102625));
#252872=CARTESIAN_POINT('Ctrl Pts',(43.3135644199415,33.6091932047179,-37.8519291666667));
#252873=CARTESIAN_POINT('Ctrl Pts',(42.7163704007519,32.5748228215052,-37.7935958333334));
#252874=CARTESIAN_POINT('Ctrl Pts',(42.1191763815623,31.5404524382925,-37.7352625));
#252875=CARTESIAN_POINT('Ctrl Pts',(42.7163704007519,30.5060820550798,-37.6769291666667));
#252876=CARTESIAN_POINT('Ctrl Pts',(43.3135644199415,29.4717116718671,-37.6185958333333));
#252877=CARTESIAN_POINT('Ctrl Pts',(44.5079524583208,29.4717116718671,-37.5602625));
#252878=CARTESIAN_POINT('Ctrl Pts',(45.7023404967,29.4717116718671,-37.5019291666666));
#252879=CARTESIAN_POINT('Ctrl Pts',(46.2995345158897,30.5060820550798,-37.4435958333333));
#252880=CARTESIAN_POINT('Ctrl Pts',(46.8967285350793,31.5404524382925,-37.3852625));
#252881=CARTESIAN_POINT('Ctrl Pts',(46.2995345158897,32.5748228215052,-37.3269291666667));
#252882=CARTESIAN_POINT('Ctrl Pts',(45.7023404967,33.6091932047179,-37.2685958333333));
#252883=CARTESIAN_POINT('Ctrl Pts',(44.5079524583208,33.6091932047179,-37.2102625));
#252884=CARTESIAN_POINT('Ctrl Pts',(43.3135644199415,33.6091932047179,-37.1519291666667));
#252885=CARTESIAN_POINT('Ctrl Pts',(42.7163704007519,32.5748228215052,-37.0935958333333));
#252886=CARTESIAN_POINT('Ctrl Pts',(42.1191763815623,31.5404524382925,-37.0352625));
#252887=CARTESIAN_POINT('Ctrl Pts',(42.7163704007519,30.5060820550798,-36.9769291666667));
#252888=CARTESIAN_POINT('Ctrl Pts',(43.3135644199415,29.4717116718671,-36.9185958333333));
#252889=CARTESIAN_POINT('Ctrl Pts',(44.5079524583208,29.4717116718671,-36.8602625));
#252890=CARTESIAN_POINT('Ctrl Pts',(45.7023404967,29.4717116718671,-36.8019291666666));
#252891=CARTESIAN_POINT('Ctrl Pts',(46.2995345158897,30.5060820550798,-36.7435958333334));
#252892=CARTESIAN_POINT('Ctrl Pts',(46.8967285350793,31.5404524382925,-36.6852625));
#252893=CARTESIAN_POINT('Ctrl Pts',(46.2995345158897,32.5748228215052,-36.6269291666666));
#252894=CARTESIAN_POINT('Ctrl Pts',(46.222006582932,32.7091051403937,-36.6193563132714));
#252895=CARTESIAN_POINT('Ctrl Pts',(46.1253278975281,32.8303303578336,-36.611216324118));
#252896=CARTESIAN_POINT('Ctrl Pts',(44.5079524583208,33.2091975287062,-52.84120011122));
#252897=CARTESIAN_POINT('Ctrl Pts',(43.5445020311616,33.2091975287062,-52.7828667778867));
#252898=CARTESIAN_POINT('Ctrl Pts',(43.0627768175819,32.3748249834993,-52.7245334445534));
#252899=CARTESIAN_POINT('Ctrl Pts',(42.5810516040023,31.5404524382925,-52.66620011122));
#252900=CARTESIAN_POINT('Ctrl Pts',(43.0627768175819,30.7060798930856,-52.6078667778867));
#252901=CARTESIAN_POINT('Ctrl Pts',(43.5445020311616,29.8717073478788,-52.5495334445533));
#252902=CARTESIAN_POINT('Ctrl Pts',(44.5079524583208,29.8717073478787,-52.49120011122));
#252903=CARTESIAN_POINT('Ctrl Pts',(45.47140288548,29.8717073478788,-52.4328667778868));
#252904=CARTESIAN_POINT('Ctrl Pts',(45.9531280990597,30.7060798930856,-52.3745334445534));
#252905=CARTESIAN_POINT('Ctrl Pts',(46.4348533126392,31.5404524382925,-52.3162001112201));
#252906=CARTESIAN_POINT('Ctrl Pts',(45.9531280990597,32.3748249834993,-52.2578667778867));
#252907=CARTESIAN_POINT('Ctrl Pts',(45.47140288548,33.2091975287062,-52.1995334445534));
#252908=CARTESIAN_POINT('Ctrl Pts',(44.5079524583208,33.2091975287062,-52.14120011122));
#252909=CARTESIAN_POINT('Ctrl Pts',(43.5445020311616,33.2091975287062,-52.0828667778867));
#252910=CARTESIAN_POINT('Ctrl Pts',(43.0627768175819,32.3748249834993,-52.0245334445533));
#252911=CARTESIAN_POINT('Ctrl Pts',(42.5810516040023,31.5404524382925,-51.96620011122));
#252912=CARTESIAN_POINT('Ctrl Pts',(43.0627768175819,30.7060798930856,-51.9078667778867));
#252913=CARTESIAN_POINT('Ctrl Pts',(43.5445020311616,29.8717073478788,-51.8495334445534));
#252914=CARTESIAN_POINT('Ctrl Pts',(44.5079524583208,29.8717073478787,-51.79120011122));
#252915=CARTESIAN_POINT('Ctrl Pts',(45.47140288548,29.8717073478788,-51.7328667778867));
#252916=CARTESIAN_POINT('Ctrl Pts',(45.9531280990597,30.7060798930856,-51.6745334445533));
#252917=CARTESIAN_POINT('Ctrl Pts',(46.4348533126392,31.5404524382925,-51.61620011122));
#252918=CARTESIAN_POINT('Ctrl Pts',(45.9531280990597,32.3748249834993,-51.5578667778867));
#252919=CARTESIAN_POINT('Ctrl Pts',(45.47140288548,33.2091975287062,-51.4995334445534));
#252920=CARTESIAN_POINT('Ctrl Pts',(44.5079524583208,33.2091975287062,-51.44120011122));
#252921=CARTESIAN_POINT('Ctrl Pts',(43.5445020311616,33.2091975287062,-51.3828667778867));
#252922=CARTESIAN_POINT('Ctrl Pts',(43.0627768175819,32.3748249834993,-51.3245334445534));
#252923=CARTESIAN_POINT('Ctrl Pts',(42.5810516040023,31.5404524382925,-51.26620011122));
#252924=CARTESIAN_POINT('Ctrl Pts',(43.0627768175819,30.7060798930856,-51.2078667778867));
#252925=CARTESIAN_POINT('Ctrl Pts',(43.5445020311616,29.8717073478788,-51.1495334445534));
#252926=CARTESIAN_POINT('Ctrl Pts',(44.5079524583208,29.8717073478787,-51.09120011122));
#252927=CARTESIAN_POINT('Ctrl Pts',(45.47140288548,29.8717073478788,-51.0328667778867));
#252928=CARTESIAN_POINT('Ctrl Pts',(45.9531280990597,30.7060798930856,-50.9745334445533));
#252929=CARTESIAN_POINT('Ctrl Pts',(46.4348533126392,31.5404524382925,-50.91620011122));
#252930=CARTESIAN_POINT('Ctrl Pts',(45.9531280990597,32.3748249834993,-50.8578667778867));
#252931=CARTESIAN_POINT('Ctrl Pts',(45.47140288548,33.2091975287062,-50.7995334445533));
#252932=CARTESIAN_POINT('Ctrl Pts',(44.5079524583208,33.2091975287062,-50.74120011122));
#252933=CARTESIAN_POINT('Ctrl Pts',(43.5445020311616,33.2091975287062,-50.6828667778867));
#252934=CARTESIAN_POINT('Ctrl Pts',(43.0627768175819,32.3748249834993,-50.6245334445533));
#252935=CARTESIAN_POINT('Ctrl Pts',(42.5810516040023,31.5404524382925,-50.56620011122));
#252936=CARTESIAN_POINT('Ctrl Pts',(43.0627768175819,30.7060798930856,-50.5078667778867));
#252937=CARTESIAN_POINT('Ctrl Pts',(43.5445020311616,29.8717073478788,-50.4495334445534));
#252938=CARTESIAN_POINT('Ctrl Pts',(44.5079524583208,29.8717073478787,-50.39120011122));
#252939=CARTESIAN_POINT('Ctrl Pts',(45.47140288548,29.8717073478788,-50.3328667778867));
#252940=CARTESIAN_POINT('Ctrl Pts',(45.9531280990597,30.7060798930856,-50.2745334445533));
#252941=CARTESIAN_POINT('Ctrl Pts',(46.4348533126392,31.5404524382925,-50.21620011122));
#252942=CARTESIAN_POINT('Ctrl Pts',(45.9531280990597,32.3748249834993,-50.1578667778867));
#252943=CARTESIAN_POINT('Ctrl Pts',(45.47140288548,33.2091975287062,-50.0995334445534));
#252944=CARTESIAN_POINT('Ctrl Pts',(44.5079524583208,33.2091975287062,-50.04120011122));
#252945=CARTESIAN_POINT('Ctrl Pts',(43.5445020311616,33.2091975287062,-49.9828667778867));
#252946=CARTESIAN_POINT('Ctrl Pts',(43.0627768175819,32.3748249834993,-49.9245334445534));
#252947=CARTESIAN_POINT('Ctrl Pts',(42.5810516040023,31.5404524382925,-49.8662001112201));
#252948=CARTESIAN_POINT('Ctrl Pts',(43.0627768175819,30.7060798930856,-49.8078667778867));
#252949=CARTESIAN_POINT('Ctrl Pts',(43.5445020311616,29.8717073478788,-49.7495334445534));
#252950=CARTESIAN_POINT('Ctrl Pts',(44.5079524583208,29.8717073478787,-49.69120011122));
#252951=CARTESIAN_POINT('Ctrl Pts',(45.47140288548,29.8717073478788,-49.6328667778867));
#252952=CARTESIAN_POINT('Ctrl Pts',(45.9531280990597,30.7060798930856,-49.5745334445533));
#252953=CARTESIAN_POINT('Ctrl Pts',(46.4348533126392,31.5404524382925,-49.51620011122));
#252954=CARTESIAN_POINT('Ctrl Pts',(45.9531280990597,32.3748249834993,-49.4578667778867));
#252955=CARTESIAN_POINT('Ctrl Pts',(45.47140288548,33.2091975287062,-49.3995334445534));
#252956=CARTESIAN_POINT('Ctrl Pts',(44.5079524583208,33.2091975287062,-49.34120011122));
#252957=CARTESIAN_POINT('Ctrl Pts',(43.5445020311616,33.2091975287062,-49.2828667778867));
#252958=CARTESIAN_POINT('Ctrl Pts',(43.0627768175819,32.3748249834993,-49.2245334445533));
#252959=CARTESIAN_POINT('Ctrl Pts',(42.5810516040023,31.5404524382925,-49.16620011122));
#252960=CARTESIAN_POINT('Ctrl Pts',(43.0627768175819,30.7060798930856,-49.1078667778867));
#252961=CARTESIAN_POINT('Ctrl Pts',(43.5445020311616,29.8717073478788,-49.0495334445534));
#252962=CARTESIAN_POINT('Ctrl Pts',(44.5079524583208,29.8717073478787,-48.99120011122));
#252963=CARTESIAN_POINT('Ctrl Pts',(45.47140288548,29.8717073478788,-48.9328667778867));
#252964=CARTESIAN_POINT('Ctrl Pts',(45.9531280990597,30.7060798930856,-48.8745334445533));
#252965=CARTESIAN_POINT('Ctrl Pts',(46.4348533126392,31.5404524382925,-48.81620011122));
#252966=CARTESIAN_POINT('Ctrl Pts',(45.9531280990597,32.3748249834993,-48.7578667778867));
#252967=CARTESIAN_POINT('Ctrl Pts',(45.47140288548,33.2091975287062,-48.6995334445534));
#252968=CARTESIAN_POINT('Ctrl Pts',(44.5079524583208,33.2091975287062,-48.64120011122));
#252969=CARTESIAN_POINT('Ctrl Pts',(43.5445020311616,33.2091975287062,-48.5828667778867));
#252970=CARTESIAN_POINT('Ctrl Pts',(43.0627768175819,32.3748249834993,-48.5245334445533));
#252971=CARTESIAN_POINT('Ctrl Pts',(42.5810516040023,31.5404524382925,-48.46620011122));
#252972=CARTESIAN_POINT('Ctrl Pts',(43.0627768175819,30.7060798930856,-48.4078667778867));
#252973=CARTESIAN_POINT('Ctrl Pts',(43.5445020311616,29.8717073478788,-48.3495334445534));
#252974=CARTESIAN_POINT('Ctrl Pts',(44.5079524583208,29.8717073478787,-48.29120011122));
#252975=CARTESIAN_POINT('Ctrl Pts',(45.47140288548,29.8717073478788,-48.2328667778867));
#252976=CARTESIAN_POINT('Ctrl Pts',(45.9531280990597,30.7060798930856,-48.1745334445534));
#252977=CARTESIAN_POINT('Ctrl Pts',(46.4348533126392,31.5404524382925,-48.11620011122));
#252978=CARTESIAN_POINT('Ctrl Pts',(45.9531280990597,32.3748249834993,-48.0578667778867));
#252979=CARTESIAN_POINT('Ctrl Pts',(45.47140288548,33.2091975287062,-47.9995334445534));
#252980=CARTESIAN_POINT('Ctrl Pts',(44.5079524583208,33.2091975287062,-47.94120011122));
#252981=CARTESIAN_POINT('Ctrl Pts',(43.5445020311616,33.2091975287062,-47.8828667778867));
#252982=CARTESIAN_POINT('Ctrl Pts',(43.0627768175819,32.3748249834993,-47.8245334445533));
#252983=CARTESIAN_POINT('Ctrl Pts',(42.5810516040023,31.5404524382925,-47.76620011122));
#252984=CARTESIAN_POINT('Ctrl Pts',(43.0627768175819,30.7060798930856,-47.7078667778867));
#252985=CARTESIAN_POINT('Ctrl Pts',(43.5445020311616,29.8717073478788,-47.6495334445534));
#252986=CARTESIAN_POINT('Ctrl Pts',(44.5079524583208,29.8717073478787,-47.59120011122));
#252987=CARTESIAN_POINT('Ctrl Pts',(45.47140288548,29.8717073478788,-47.5328667778867));
#252988=CARTESIAN_POINT('Ctrl Pts',(45.9531280990597,30.7060798930856,-47.4745334445534));
#252989=CARTESIAN_POINT('Ctrl Pts',(46.4348533126392,31.5404524382925,-47.41620011122));
#252990=CARTESIAN_POINT('Ctrl Pts',(45.9531280990597,32.3748249834993,-47.3578667778867));
#252991=CARTESIAN_POINT('Ctrl Pts',(45.47140288548,33.2091975287062,-47.2995334445534));
#252992=CARTESIAN_POINT('Ctrl Pts',(44.5079524583208,33.2091975287062,-47.24120011122));
#252993=CARTESIAN_POINT('Ctrl Pts',(43.5445020311616,33.2091975287062,-47.1828667778867));
#252994=CARTESIAN_POINT('Ctrl Pts',(43.0627768175819,32.3748249834993,-47.1245334445533));
#252995=CARTESIAN_POINT('Ctrl Pts',(42.5810516040023,31.5404524382925,-47.06620011122));
#252996=CARTESIAN_POINT('Ctrl Pts',(43.0627768175819,30.7060798930856,-47.0078667778867));
#252997=CARTESIAN_POINT('Ctrl Pts',(43.5445020311616,29.8717073478788,-46.9495334445534));
#252998=CARTESIAN_POINT('Ctrl Pts',(44.5079524583208,29.8717073478787,-46.89120011122));
#252999=CARTESIAN_POINT('Ctrl Pts',(45.47140288548,29.8717073478788,-46.8328667778867));
#253000=CARTESIAN_POINT('Ctrl Pts',(45.9531280990597,30.7060798930856,-46.7745334445533));
#253001=CARTESIAN_POINT('Ctrl Pts',(46.4348533126392,31.5404524382925,-46.71620011122));
#253002=CARTESIAN_POINT('Ctrl Pts',(45.9531280990597,32.3748249834993,-46.6578667778867));
#253003=CARTESIAN_POINT('Ctrl Pts',(45.47140288548,33.2091975287062,-46.5995334445534));
#253004=CARTESIAN_POINT('Ctrl Pts',(44.5079524583208,33.2091975287062,-46.54120011122));
#253005=CARTESIAN_POINT('Ctrl Pts',(43.5445020311616,33.2091975287062,-46.4828667778867));
#253006=CARTESIAN_POINT('Ctrl Pts',(43.0627768175819,32.3748249834993,-46.4245334445533));
#253007=CARTESIAN_POINT('Ctrl Pts',(42.5810516040023,31.5404524382925,-46.36620011122));
#253008=CARTESIAN_POINT('Ctrl Pts',(43.0627768175819,30.7060798930856,-46.3078667778867));
#253009=CARTESIAN_POINT('Ctrl Pts',(43.5445020311616,29.8717073478788,-46.2495334445534));
#253010=CARTESIAN_POINT('Ctrl Pts',(44.5079524583208,29.8717073478787,-46.19120011122));
#253011=CARTESIAN_POINT('Ctrl Pts',(45.47140288548,29.8717073478788,-46.1328667778867));
#253012=CARTESIAN_POINT('Ctrl Pts',(45.9531280990597,30.7060798930856,-46.0745334445534));
#253013=CARTESIAN_POINT('Ctrl Pts',(46.4348533126392,31.5404524382925,-46.01620011122));
#253014=CARTESIAN_POINT('Ctrl Pts',(45.9531280990597,32.3748249834993,-45.9578667778867));
#253015=CARTESIAN_POINT('Ctrl Pts',(45.47140288548,33.2091975287062,-45.8995334445533));
#253016=CARTESIAN_POINT('Ctrl Pts',(44.5079524583208,33.2091975287062,-45.84120011122));
#253017=CARTESIAN_POINT('Ctrl Pts',(43.5445020311616,33.2091975287062,-45.7828667778867));
#253018=CARTESIAN_POINT('Ctrl Pts',(43.0627768175819,32.3748249834993,-45.7245334445533));
#253019=CARTESIAN_POINT('Ctrl Pts',(42.5810516040023,31.5404524382925,-45.66620011122));
#253020=CARTESIAN_POINT('Ctrl Pts',(43.0627768175819,30.7060798930856,-45.6078667778867));
#253021=CARTESIAN_POINT('Ctrl Pts',(43.5445020311616,29.8717073478788,-45.5495334445534));
#253022=CARTESIAN_POINT('Ctrl Pts',(44.5079524583208,29.8717073478787,-45.49120011122));
#253023=CARTESIAN_POINT('Ctrl Pts',(45.47140288548,29.8717073478788,-45.4328667778867));
#253024=CARTESIAN_POINT('Ctrl Pts',(45.9531280990597,30.7060798930856,-45.3745334445533));
#253025=CARTESIAN_POINT('Ctrl Pts',(46.4348533126392,31.5404524382925,-45.31620011122));
#253026=CARTESIAN_POINT('Ctrl Pts',(45.9531280990597,32.3748249834993,-45.2578667778867));
#253027=CARTESIAN_POINT('Ctrl Pts',(45.47140288548,33.2091975287062,-45.1995334445534));
#253028=CARTESIAN_POINT('Ctrl Pts',(44.5079524583208,33.2091975287062,-45.14120011122));
#253029=CARTESIAN_POINT('Ctrl Pts',(43.5445020311616,33.2091975287062,-45.0828667778867));
#253030=CARTESIAN_POINT('Ctrl Pts',(43.0627768175819,32.3748249834993,-45.0245334445533));
#253031=CARTESIAN_POINT('Ctrl Pts',(42.5810516040023,31.5404524382925,-44.9662001112201));
#253032=CARTESIAN_POINT('Ctrl Pts',(43.0627768175819,30.7060798930856,-44.9078667778867));
#253033=CARTESIAN_POINT('Ctrl Pts',(43.5445020311616,29.8717073478788,-44.8495334445534));
#253034=CARTESIAN_POINT('Ctrl Pts',(44.5079524583208,29.8717073478787,-44.79120011122));
#253035=CARTESIAN_POINT('Ctrl Pts',(45.47140288548,29.8717073478788,-44.7328667778867));
#253036=CARTESIAN_POINT('Ctrl Pts',(45.9531280990597,30.7060798930856,-44.6745334445534));
#253037=CARTESIAN_POINT('Ctrl Pts',(46.4348533126392,31.5404524382925,-44.6162001112201));
#253038=CARTESIAN_POINT('Ctrl Pts',(45.9531280990597,32.3748249834993,-44.5578667778867));
#253039=CARTESIAN_POINT('Ctrl Pts',(45.47140288548,33.2091975287062,-44.4995334445534));
#253040=CARTESIAN_POINT('Ctrl Pts',(44.5079524583208,33.2091975287062,-44.44120011122));
#253041=CARTESIAN_POINT('Ctrl Pts',(43.5445020311616,33.2091975287062,-44.3828667778867));
#253042=CARTESIAN_POINT('Ctrl Pts',(43.0627768175819,32.3748249834993,-44.3245334445534));
#253043=CARTESIAN_POINT('Ctrl Pts',(42.5810516040023,31.5404524382925,-44.26620011122));
#253044=CARTESIAN_POINT('Ctrl Pts',(43.0627768175819,30.7060798930856,-44.2078667778867));
#253045=CARTESIAN_POINT('Ctrl Pts',(43.5445020311616,29.8717073478788,-44.1495334445534));
#253046=CARTESIAN_POINT('Ctrl Pts',(44.5079524583208,29.8717073478787,-44.09120011122));
#253047=CARTESIAN_POINT('Ctrl Pts',(45.47140288548,29.8717073478788,-44.0328667778867));
#253048=CARTESIAN_POINT('Ctrl Pts',(45.9531280990597,30.7060798930856,-43.9745334445534));
#253049=CARTESIAN_POINT('Ctrl Pts',(46.4348533126392,31.5404524382925,-43.9162001112201));
#253050=CARTESIAN_POINT('Ctrl Pts',(45.9531280990597,32.3748249834993,-43.8578667778867));
#253051=CARTESIAN_POINT('Ctrl Pts',(45.47140288548,33.2091975287062,-43.7995334445534));
#253052=CARTESIAN_POINT('Ctrl Pts',(44.5079524583208,33.2091975287062,-43.74120011122));
#253053=CARTESIAN_POINT('Ctrl Pts',(43.5445020311616,33.2091975287062,-43.6828667778867));
#253054=CARTESIAN_POINT('Ctrl Pts',(43.0627768175819,32.3748249834993,-43.6245334445534));
#253055=CARTESIAN_POINT('Ctrl Pts',(42.5810516040023,31.5404524382925,-43.5662001112201));
#253056=CARTESIAN_POINT('Ctrl Pts',(43.0627768175819,30.7060798930856,-43.5078667778867));
#253057=CARTESIAN_POINT('Ctrl Pts',(43.5445020311616,29.8717073478788,-43.4495334445534));
#253058=CARTESIAN_POINT('Ctrl Pts',(44.5079524583208,29.8717073478787,-43.39120011122));
#253059=CARTESIAN_POINT('Ctrl Pts',(45.47140288548,29.8717073478788,-43.3328667778867));
#253060=CARTESIAN_POINT('Ctrl Pts',(45.9531280990597,30.7060798930856,-43.2745334445534));
#253061=CARTESIAN_POINT('Ctrl Pts',(46.4348533126392,31.5404524382925,-43.21620011122));
#253062=CARTESIAN_POINT('Ctrl Pts',(45.9531280990597,32.3748249834993,-43.1578667778867));
#253063=CARTESIAN_POINT('Ctrl Pts',(45.47140288548,33.2091975287062,-43.0995334445534));
#253064=CARTESIAN_POINT('Ctrl Pts',(44.5079524583208,33.2091975287062,-43.04120011122));
#253065=CARTESIAN_POINT('Ctrl Pts',(43.5445020311616,33.2091975287062,-42.9828667778867));
#253066=CARTESIAN_POINT('Ctrl Pts',(43.0627768175819,32.3748249834993,-42.9245334445534));
#253067=CARTESIAN_POINT('Ctrl Pts',(42.5810516040023,31.5404524382925,-42.86620011122));
#253068=CARTESIAN_POINT('Ctrl Pts',(43.0627768175819,30.7060798930856,-42.8078667778867));
#253069=CARTESIAN_POINT('Ctrl Pts',(43.5445020311616,29.8717073478788,-42.7495334445534));
#253070=CARTESIAN_POINT('Ctrl Pts',(44.5079524583208,29.8717073478787,-42.69120011122));
#253071=CARTESIAN_POINT('Ctrl Pts',(45.47140288548,29.8717073478788,-42.6328667778867));
#253072=CARTESIAN_POINT('Ctrl Pts',(45.9531280990597,30.7060798930856,-42.5745334445534));
#253073=CARTESIAN_POINT('Ctrl Pts',(46.4348533126392,31.5404524382925,-42.51620011122));
#253074=CARTESIAN_POINT('Ctrl Pts',(45.9531280990597,32.3748249834993,-42.4578667778867));
#253075=CARTESIAN_POINT('Ctrl Pts',(45.47140288548,33.2091975287062,-42.3995334445534));
#253076=CARTESIAN_POINT('Ctrl Pts',(44.5079524583208,33.2091975287062,-42.34120011122));
#253077=CARTESIAN_POINT('Ctrl Pts',(43.5445020311616,33.2091975287062,-42.2828667778867));
#253078=CARTESIAN_POINT('Ctrl Pts',(43.0627768175819,32.3748249834993,-42.2245334445534));
#253079=CARTESIAN_POINT('Ctrl Pts',(42.5810516040023,31.5404524382925,-42.16620011122));
#253080=CARTESIAN_POINT('Ctrl Pts',(43.0627768175819,30.7060798930856,-42.1078667778867));
#253081=CARTESIAN_POINT('Ctrl Pts',(43.5445020311616,29.8717073478788,-42.0495334445534));
#253082=CARTESIAN_POINT('Ctrl Pts',(44.5079524583208,29.8717073478787,-41.99120011122));
#253083=CARTESIAN_POINT('Ctrl Pts',(45.47140288548,29.8717073478788,-41.9328667778867));
#253084=CARTESIAN_POINT('Ctrl Pts',(45.9531280990597,30.7060798930856,-41.8745334445534));
#253085=CARTESIAN_POINT('Ctrl Pts',(46.4348533126392,31.5404524382925,-41.81620011122));
#253086=CARTESIAN_POINT('Ctrl Pts',(45.9531280990597,32.3748249834993,-41.7578667778867));
#253087=CARTESIAN_POINT('Ctrl Pts',(45.47140288548,33.2091975287062,-41.6995334445533));
#253088=CARTESIAN_POINT('Ctrl Pts',(44.5079524583208,33.2091975287062,-41.64120011122));
#253089=CARTESIAN_POINT('Ctrl Pts',(43.5445020311616,33.2091975287062,-41.5828667778867));
#253090=CARTESIAN_POINT('Ctrl Pts',(43.0627768175819,32.3748249834993,-41.5245334445534));
#253091=CARTESIAN_POINT('Ctrl Pts',(42.5810516040023,31.5404524382925,-41.46620011122));
#253092=CARTESIAN_POINT('Ctrl Pts',(43.0627768175819,30.7060798930856,-41.4078667778867));
#253093=CARTESIAN_POINT('Ctrl Pts',(43.5445020311616,29.8717073478788,-41.3495334445533));
#253094=CARTESIAN_POINT('Ctrl Pts',(44.5079524583208,29.8717073478787,-41.29120011122));
#253095=CARTESIAN_POINT('Ctrl Pts',(45.47140288548,29.8717073478788,-41.2328667778867));
#253096=CARTESIAN_POINT('Ctrl Pts',(45.9531280990597,30.7060798930856,-41.1745334445534));
#253097=CARTESIAN_POINT('Ctrl Pts',(46.4348533126392,31.5404524382925,-41.11620011122));
#253098=CARTESIAN_POINT('Ctrl Pts',(45.9531280990597,32.3748249834993,-41.0578667778867));
#253099=CARTESIAN_POINT('Ctrl Pts',(45.47140288548,33.2091975287062,-40.9995334445534));
#253100=CARTESIAN_POINT('Ctrl Pts',(44.5079524583208,33.2091975287062,-40.94120011122));
#253101=CARTESIAN_POINT('Ctrl Pts',(43.5445020311616,33.2091975287062,-40.8828667778867));
#253102=CARTESIAN_POINT('Ctrl Pts',(43.0627768175819,32.3748249834993,-40.8245334445534));
#253103=CARTESIAN_POINT('Ctrl Pts',(42.5810516040023,31.5404524382925,-40.76620011122));
#253104=CARTESIAN_POINT('Ctrl Pts',(43.0627768175819,30.7060798930856,-40.7078667778867));
#253105=CARTESIAN_POINT('Ctrl Pts',(43.5445020311616,29.8717073478788,-40.6495334445533));
#253106=CARTESIAN_POINT('Ctrl Pts',(44.5079524583208,29.8717073478787,-40.59120011122));
#253107=CARTESIAN_POINT('Ctrl Pts',(45.47140288548,29.8717073478788,-40.5328667778867));
#253108=CARTESIAN_POINT('Ctrl Pts',(45.9531280990597,30.7060798930856,-40.4745334445534));
#253109=CARTESIAN_POINT('Ctrl Pts',(46.4348533126392,31.5404524382925,-40.41620011122));
#253110=CARTESIAN_POINT('Ctrl Pts',(45.9531280990597,32.3748249834993,-40.3578667778867));
#253111=CARTESIAN_POINT('Ctrl Pts',(45.47140288548,33.2091975287062,-40.2995334445534));
#253112=CARTESIAN_POINT('Ctrl Pts',(44.5079524583208,33.2091975287062,-40.24120011122));
#253113=CARTESIAN_POINT('Ctrl Pts',(43.5445020311616,33.2091975287062,-40.1828667778867));
#253114=CARTESIAN_POINT('Ctrl Pts',(43.0627768175819,32.3748249834993,-40.1245334445534));
#253115=CARTESIAN_POINT('Ctrl Pts',(42.5810516040023,31.5404524382925,-40.0662001112201));
#253116=CARTESIAN_POINT('Ctrl Pts',(43.0627768175819,30.7060798930856,-40.0078667778867));
#253117=CARTESIAN_POINT('Ctrl Pts',(43.5445020311616,29.8717073478788,-39.9495334445534));
#253118=CARTESIAN_POINT('Ctrl Pts',(44.5079524583208,29.8717073478787,-39.89120011122));
#253119=CARTESIAN_POINT('Ctrl Pts',(45.47140288548,29.8717073478788,-39.8328667778867));
#253120=CARTESIAN_POINT('Ctrl Pts',(45.9531280990597,30.7060798930856,-39.7745334445534));
#253121=CARTESIAN_POINT('Ctrl Pts',(46.4348533126392,31.5404524382925,-39.7162001112201));
#253122=CARTESIAN_POINT('Ctrl Pts',(45.9531280990597,32.3748249834993,-39.6578667778867));
#253123=CARTESIAN_POINT('Ctrl Pts',(45.47140288548,33.2091975287062,-39.5995334445534));
#253124=CARTESIAN_POINT('Ctrl Pts',(44.5079524583208,33.2091975287062,-39.54120011122));
#253125=CARTESIAN_POINT('Ctrl Pts',(43.5445020311616,33.2091975287062,-39.4828667778867));
#253126=CARTESIAN_POINT('Ctrl Pts',(43.0627768175819,32.3748249834993,-39.4245334445534));
#253127=CARTESIAN_POINT('Ctrl Pts',(42.5810516040023,31.5404524382925,-39.36620011122));
#253128=CARTESIAN_POINT('Ctrl Pts',(43.0627768175819,30.7060798930856,-39.3078667778867));
#253129=CARTESIAN_POINT('Ctrl Pts',(43.5445020311616,29.8717073478788,-39.2495334445534));
#253130=CARTESIAN_POINT('Ctrl Pts',(44.5079524583208,29.8717073478787,-39.19120011122));
#253131=CARTESIAN_POINT('Ctrl Pts',(45.47140288548,29.8717073478788,-39.1328667778867));
#253132=CARTESIAN_POINT('Ctrl Pts',(45.9531280990597,30.7060798930856,-39.0745334445534));
#253133=CARTESIAN_POINT('Ctrl Pts',(46.4348533126392,31.5404524382925,-39.0162001112201));
#253134=CARTESIAN_POINT('Ctrl Pts',(45.9531280990597,32.3748249834993,-38.9578667778867));
#253135=CARTESIAN_POINT('Ctrl Pts',(45.47140288548,33.2091975287062,-38.8995334445534));
#253136=CARTESIAN_POINT('Ctrl Pts',(44.5079524583208,33.2091975287062,-38.84120011122));
#253137=CARTESIAN_POINT('Ctrl Pts',(43.5445020311616,33.2091975287062,-38.7828667778867));
#253138=CARTESIAN_POINT('Ctrl Pts',(43.0627768175819,32.3748249834993,-38.7245334445534));
#253139=CARTESIAN_POINT('Ctrl Pts',(42.5810516040023,31.5404524382925,-38.66620011122));
#253140=CARTESIAN_POINT('Ctrl Pts',(43.0627768175819,30.7060798930856,-38.6078667778867));
#253141=CARTESIAN_POINT('Ctrl Pts',(43.5445020311616,29.8717073478788,-38.5495334445534));
#253142=CARTESIAN_POINT('Ctrl Pts',(44.5079524583208,29.8717073478787,-38.49120011122));
#253143=CARTESIAN_POINT('Ctrl Pts',(45.47140288548,29.8717073478788,-38.4328667778867));
#253144=CARTESIAN_POINT('Ctrl Pts',(45.9531280990597,30.7060798930856,-38.3745334445534));
#253145=CARTESIAN_POINT('Ctrl Pts',(46.4348533126392,31.5404524382925,-38.31620011122));
#253146=CARTESIAN_POINT('Ctrl Pts',(45.9531280990597,32.3748249834993,-38.2578667778867));
#253147=CARTESIAN_POINT('Ctrl Pts',(45.47140288548,33.2091975287062,-38.1995334445534));
#253148=CARTESIAN_POINT('Ctrl Pts',(44.5079524583208,33.2091975287062,-38.14120011122));
#253149=CARTESIAN_POINT('Ctrl Pts',(43.5445020311616,33.2091975287062,-38.0828667778867));
#253150=CARTESIAN_POINT('Ctrl Pts',(43.0627768175819,32.3748249834993,-38.0245334445534));
#253151=CARTESIAN_POINT('Ctrl Pts',(42.5810516040023,31.5404524382925,-37.96620011122));
#253152=CARTESIAN_POINT('Ctrl Pts',(43.0627768175819,30.7060798930856,-37.9078667778867));
#253153=CARTESIAN_POINT('Ctrl Pts',(43.5445020311616,29.8717073478788,-37.8495334445534));
#253154=CARTESIAN_POINT('Ctrl Pts',(44.5079524583208,29.8717073478787,-37.79120011122));
#253155=CARTESIAN_POINT('Ctrl Pts',(45.47140288548,29.8717073478788,-37.7328667778867));
#253156=CARTESIAN_POINT('Ctrl Pts',(45.9531280990597,30.7060798930856,-37.6745334445534));
#253157=CARTESIAN_POINT('Ctrl Pts',(46.4348533126392,31.5404524382925,-37.61620011122));
#253158=CARTESIAN_POINT('Ctrl Pts',(45.9531280990597,32.3748249834993,-37.5578667778867));
#253159=CARTESIAN_POINT('Ctrl Pts',(45.47140288548,33.2091975287062,-37.4995334445534));
#253160=CARTESIAN_POINT('Ctrl Pts',(44.5079524583208,33.2091975287062,-37.44120011122));
#253161=CARTESIAN_POINT('Ctrl Pts',(43.5445020311616,33.2091975287062,-37.3828667778867));
#253162=CARTESIAN_POINT('Ctrl Pts',(43.0627768175819,32.3748249834993,-37.3245334445534));
#253163=CARTESIAN_POINT('Ctrl Pts',(42.5810516040023,31.5404524382925,-37.26620011122));
#253164=CARTESIAN_POINT('Ctrl Pts',(43.0627768175819,30.7060798930856,-37.2078667778867));
#253165=CARTESIAN_POINT('Ctrl Pts',(43.5445020311616,29.8717073478788,-37.1495334445534));
#253166=CARTESIAN_POINT('Ctrl Pts',(44.5079524583208,29.8717073478787,-37.09120011122));
#253167=CARTESIAN_POINT('Ctrl Pts',(45.47140288548,29.8717073478788,-37.0328667778867));
#253168=CARTESIAN_POINT('Ctrl Pts',(45.9531280990597,30.7060798930856,-36.9745334445534));
#253169=CARTESIAN_POINT('Ctrl Pts',(46.4348533126392,31.5404524382925,-36.91620011122));
#253170=CARTESIAN_POINT('Ctrl Pts',(45.9531280990597,32.3748249834993,-36.8578667778867));
#253171=CARTESIAN_POINT('Ctrl Pts',(45.8905903661582,32.4831435142748,-36.8502939244914));
#253172=CARTESIAN_POINT('Ctrl Pts',(45.812604721831,32.5809295635084,-36.8421539353381));
#253173=CARTESIAN_POINT('Ctrl Pts',(45.3258959266108,30.0859149508445,-39.8341886424312));
#253174=CARTESIAN_POINT('Ctrl Pts',(45.4766887394293,30.1176683184879,-39.7972186137753));
#253175=CARTESIAN_POINT('Ctrl Pts',(45.6240618430092,30.1634775829848,-39.7576376985697));
#253176=CARTESIAN_POINT('Ctrl Pts',(45.9073780736838,30.2797207149013,-39.6755711641234));
#253177=CARTESIAN_POINT('Ctrl Pts',(46.0435967979149,30.3502619798024,-39.6330190481983));
#253178=CARTESIAN_POINT('Ctrl Pts',(46.1726018521413,30.4318752072269,-39.5898550147568));
#253179=CARTESIAN_POINT('Ctrl Pts',(44.5079524583208,33.5404524382925,-52.64995));
#253180=CARTESIAN_POINT('Ctrl Pts',(44.3600617863363,33.5275120044939,-52.64995));
#253181=CARTESIAN_POINT('Ctrl Pts',(44.2142042532552,33.4972658634834,-52.64995));
#253182=CARTESIAN_POINT('Ctrl Pts',(43.9445256487737,33.4073033028498,-52.64995));
#253183=CARTESIAN_POINT('Ctrl Pts',(43.8206799356498,33.3505752618931,-52.64995));
#253184=CARTESIAN_POINT('Ctrl Pts',(43.4951040594958,33.1566199207942,-52.64995));
#253185=CARTESIAN_POINT('Ctrl Pts',(43.3122546189713,32.993061702941,-52.6499500000001));
#253186=CARTESIAN_POINT('Ctrl Pts',(43.0527600317385,32.6506630729424,-52.6499500000001));
#253187=CARTESIAN_POINT('Ctrl Pts',(42.923716913873,32.4362244619228,-52.6499500000282));
#253188=CARTESIAN_POINT('Ctrl Pts',(42.815884786658,32.0187869403626,-52.6499500000282));
#253189=CARTESIAN_POINT('Ctrl Pts',(42.7978378140676,31.8711017322126,-52.64995));
#253190=CARTESIAN_POINT('Ctrl Pts',(42.8007193914761,31.5828389853602,-52.64995));
#253191=CARTESIAN_POINT('Ctrl Pts',(42.8195756983132,31.4434642093936,-52.64995));
#253192=CARTESIAN_POINT('Ctrl Pts',(42.8554737113965,31.3080200595814,-52.64995));
#253193=CARTESIAN_POINT('Ctrl Pts',(44.5079524583206,29.5404524382925,-40.39995));
#253194=CARTESIAN_POINT('Ctrl Pts',(44.6726735707786,29.5404524382924,-40.3916285943709));
#253195=CARTESIAN_POINT('Ctrl Pts',(44.8370885939324,29.560796052526,-40.3827292963916));
#253196=CARTESIAN_POINT('Ctrl Pts',(45.2540545582999,29.6660593396596,-40.3585947686536));
#253197=CARTESIAN_POINT('Ctrl Pts',(45.4952144476034,29.781100880629,-40.3430564392622));
#253198=CARTESIAN_POINT('Ctrl Pts',(45.9107928369525,30.0923892617563,-40.3129829440037));
#253199=CARTESIAN_POINT('Ctrl Pts',(46.0836233502634,30.2826150347246,-40.298703614746));
#253200=CARTESIAN_POINT('Ctrl Pts',(46.3539827028743,30.7265592826002,-40.2720971869114));
#253201=CARTESIAN_POINT('Ctrl Pts',(46.4455209456663,30.9781639989288,-40.257750158963));
#253202=CARTESIAN_POINT('Ctrl Pts',(46.5245281260493,31.498788220226,-40.2273804127207));
#253203=CARTESIAN_POINT('Ctrl Pts',(46.51271142587,31.7624037383698,-40.2120028408289));
#253204=CARTESIAN_POINT('Ctrl Pts',(46.390237568377,32.2624037194517,-40.1828361752658));
#253205=CARTESIAN_POINT('Ctrl Pts',(46.2837494529182,32.4947747783608,-40.1701589081232));
#253206=CARTESIAN_POINT('Ctrl Pts',(45.9828009175854,32.9171053148226,-40.1426375713279));
#253207=CARTESIAN_POINT('Ctrl Pts',(45.7874580424598,33.1003170079869,-40.1274255365594));
#253208=CARTESIAN_POINT('Ctrl Pts',(45.3425464845978,33.3762658448928,-40.0969009206428));
#253209=CARTESIAN_POINT('Ctrl Pts',(45.0986295415486,33.4686341292234,-40.0818846133193));
#253210=CARTESIAN_POINT('Ctrl Pts',(44.5906612810477,33.5551825985649,-40.0536986669188));
#253211=CARTESIAN_POINT('Ctrl Pts',(44.3315471104784,33.5491493054718,-40.0412919870582));
#253212=CARTESIAN_POINT('Ctrl Pts',(43.8212908135486,33.4375447334715,-40.0122596502992));
#253213=CARTESIAN_POINT('Ctrl Pts',(43.5758589971117,33.3297668085751,-39.9967173665271));
#253214=CARTESIAN_POINT('Ctrl Pts',(43.1496219859757,33.0304761630696,-39.9664553513854));
#253215=CARTESIAN_POINT('Ctrl Pts',(42.9706008156226,32.8449923244166,-39.9520015880131));
#253216=CARTESIAN_POINT('Ctrl Pts',(42.6865838608895,32.4082610549434,-39.9249155819424));
#253217=CARTESIAN_POINT('Ctrl Pts',(42.5875791924248,32.1590797911578,-39.911036595584));
#253218=CARTESIAN_POINT('Ctrl Pts',(42.4933024988169,31.6398809877825,-39.8807499987204));
#253219=CARTESIAN_POINT('Ctrl Pts',(42.4976238199733,31.375279663566,-39.8653149214744));
#253220=CARTESIAN_POINT('Ctrl Pts',(42.6062198512718,30.8714461891254,-39.8359246354654));
#253221=CARTESIAN_POINT('Ctrl Pts',(42.7061181645385,30.63629095421,-39.8229372892375));
#253222=CARTESIAN_POINT('Ctrl Pts',(42.9949839972762,30.2058136577985,-39.7957887343751));
#253223=CARTESIAN_POINT('Ctrl Pts',(43.1850710842596,30.0172073370075,-39.7806848689869));
#253224=CARTESIAN_POINT('Ctrl Pts',(43.6225900977621,29.7284769831686,-39.7501609164806));
#253225=CARTESIAN_POINT('Ctrl Pts',(43.8645262589039,29.6291319201338,-39.7350411852129));
#253226=CARTESIAN_POINT('Ctrl Pts',(44.2471843430749,29.553202963529,-39.7134954127037));
#253227=CARTESIAN_POINT('Ctrl Pts',(44.3775512255878,29.5404524382925,-39.7065376288468));
#253228=CARTESIAN_POINT('Ctrl Pts',(44.5079524583208,29.5404524382925,-39.69995));
#253229=CARTESIAN_POINT('Ctrl Pts',(44.5079524583208,33.2091977213449,-52.99995));
#253230=CARTESIAN_POINT('Ctrl Pts',(43.5445019199415,33.2091977213449,-52.9416166666667));
#253231=CARTESIAN_POINT('Ctrl Pts',(43.0627766507519,32.3748250798187,-52.8832833333334));
#253232=CARTESIAN_POINT('Ctrl Pts',(42.5810513815623,31.5404524382925,-52.82495));
#253233=CARTESIAN_POINT('Ctrl Pts',(43.0627766507519,30.7060797967663,-52.7666166666667));
#253234=CARTESIAN_POINT('Ctrl Pts',(43.5445019199415,29.87170715524,-52.7082833333333));
#253235=CARTESIAN_POINT('Ctrl Pts',(44.5079524583208,29.87170715524,-52.64995));
#253236=CARTESIAN_POINT('Ctrl Pts',(45.4714029967,29.87170715524,-52.5916166666666));
#253237=CARTESIAN_POINT('Ctrl Pts',(45.9531282658897,30.7060797967663,-52.5332833333334));
#253238=CARTESIAN_POINT('Ctrl Pts',(46.4348535350793,31.5404524382925,-52.4749500000001));
#253239=CARTESIAN_POINT('Ctrl Pts',(45.9531282658897,32.3748250798187,-52.4166166666667));
#253240=CARTESIAN_POINT('Ctrl Pts',(45.4714029967,33.2091977213449,-52.3582833333334));
#253241=CARTESIAN_POINT('Ctrl Pts',(44.5079524583208,33.2091977213449,-52.29995));
#253242=CARTESIAN_POINT('Ctrl Pts',(43.5445019199415,33.2091977213449,-52.2416166666667));
#253243=CARTESIAN_POINT('Ctrl Pts',(43.0627766507519,32.3748250798187,-52.1832833333333));
#253244=CARTESIAN_POINT('Ctrl Pts',(42.5810513815623,31.5404524382925,-52.12495));
#253245=CARTESIAN_POINT('Ctrl Pts',(43.0627766507519,30.7060797967663,-52.0666166666667));
#253246=CARTESIAN_POINT('Ctrl Pts',(43.5445019199415,29.87170715524,-52.0082833333333));
#253247=CARTESIAN_POINT('Ctrl Pts',(44.5079524583208,29.87170715524,-51.94995));
#253248=CARTESIAN_POINT('Ctrl Pts',(45.4714029967,29.87170715524,-51.8916166666667));
#253249=CARTESIAN_POINT('Ctrl Pts',(45.9531282658897,30.7060797967663,-51.8332833333333));
#253250=CARTESIAN_POINT('Ctrl Pts',(46.4348535350793,31.5404524382925,-51.77495));
#253251=CARTESIAN_POINT('Ctrl Pts',(45.9531282658897,32.3748250798187,-51.7166166666667));
#253252=CARTESIAN_POINT('Ctrl Pts',(45.4714029967,33.2091977213449,-51.6582833333333));
#253253=CARTESIAN_POINT('Ctrl Pts',(44.5079524583208,33.2091977213449,-51.59995));
#253254=CARTESIAN_POINT('Ctrl Pts',(43.5445019199415,33.2091977213449,-51.5416166666667));
#253255=CARTESIAN_POINT('Ctrl Pts',(43.0627766507519,32.3748250798187,-51.4832833333333));
#253256=CARTESIAN_POINT('Ctrl Pts',(42.5810513815623,31.5404524382925,-51.42495));
#253257=CARTESIAN_POINT('Ctrl Pts',(43.0627766507519,30.7060797967663,-51.3666166666667));
#253258=CARTESIAN_POINT('Ctrl Pts',(43.5445019199415,29.87170715524,-51.3082833333333));
#253259=CARTESIAN_POINT('Ctrl Pts',(44.5079524583208,29.87170715524,-51.24995));
#253260=CARTESIAN_POINT('Ctrl Pts',(45.4714029967,29.87170715524,-51.1916166666667));
#253261=CARTESIAN_POINT('Ctrl Pts',(45.9531282658897,30.7060797967663,-51.1332833333333));
#253262=CARTESIAN_POINT('Ctrl Pts',(46.4348535350793,31.5404524382925,-51.07495));
#253263=CARTESIAN_POINT('Ctrl Pts',(45.9531282658897,32.3748250798187,-51.0166166666667));
#253264=CARTESIAN_POINT('Ctrl Pts',(45.4714029967,33.2091977213449,-50.9582833333334));
#253265=CARTESIAN_POINT('Ctrl Pts',(44.5079524583208,33.2091977213449,-50.89995));
#253266=CARTESIAN_POINT('Ctrl Pts',(43.5445019199415,33.2091977213449,-50.8416166666667));
#253267=CARTESIAN_POINT('Ctrl Pts',(43.0627766507519,32.3748250798187,-50.7832833333333));
#253268=CARTESIAN_POINT('Ctrl Pts',(42.5810513815623,31.5404524382925,-50.72495));
#253269=CARTESIAN_POINT('Ctrl Pts',(43.0627766507519,30.7060797967663,-50.6666166666667));
#253270=CARTESIAN_POINT('Ctrl Pts',(43.5445019199415,29.87170715524,-50.6082833333334));
#253271=CARTESIAN_POINT('Ctrl Pts',(44.5079524583208,29.87170715524,-50.54995));
#253272=CARTESIAN_POINT('Ctrl Pts',(45.4714029967,29.87170715524,-50.4916166666667));
#253273=CARTESIAN_POINT('Ctrl Pts',(45.9531282658897,30.7060797967663,-50.4332833333333));
#253274=CARTESIAN_POINT('Ctrl Pts',(46.4348535350793,31.5404524382925,-50.37495));
#253275=CARTESIAN_POINT('Ctrl Pts',(45.9531282658897,32.3748250798187,-50.3166166666667));
#253276=CARTESIAN_POINT('Ctrl Pts',(45.4714029967,33.2091977213449,-50.2582833333334));
#253277=CARTESIAN_POINT('Ctrl Pts',(44.5079524583208,33.2091977213449,-50.19995));
#253278=CARTESIAN_POINT('Ctrl Pts',(43.5445019199415,33.2091977213449,-50.1416166666667));
#253279=CARTESIAN_POINT('Ctrl Pts',(43.0627766507519,32.3748250798187,-50.0832833333333));
#253280=CARTESIAN_POINT('Ctrl Pts',(42.5810513815623,31.5404524382925,-50.02495));
#253281=CARTESIAN_POINT('Ctrl Pts',(43.0627766507519,30.7060797967663,-49.9666166666667));
#253282=CARTESIAN_POINT('Ctrl Pts',(43.5445019199415,29.87170715524,-49.9082833333334));
#253283=CARTESIAN_POINT('Ctrl Pts',(44.5079524583208,29.87170715524,-49.84995));
#253284=CARTESIAN_POINT('Ctrl Pts',(45.4714029967,29.87170715524,-49.7916166666667));
#253285=CARTESIAN_POINT('Ctrl Pts',(45.9531282658897,30.7060797967663,-49.7332833333333));
#253286=CARTESIAN_POINT('Ctrl Pts',(46.4348535350793,31.5404524382925,-49.67495));
#253287=CARTESIAN_POINT('Ctrl Pts',(45.9531282658897,32.3748250798187,-49.6166166666667));
#253288=CARTESIAN_POINT('Ctrl Pts',(45.4714029967,33.2091977213449,-49.5582833333334));
#253289=CARTESIAN_POINT('Ctrl Pts',(44.5079524583208,33.2091977213449,-49.49995));
#253290=CARTESIAN_POINT('Ctrl Pts',(43.5445019199415,33.2091977213449,-49.4416166666667));
#253291=CARTESIAN_POINT('Ctrl Pts',(43.0627766507519,32.3748250798187,-49.3832833333334));
#253292=CARTESIAN_POINT('Ctrl Pts',(42.5810513815623,31.5404524382925,-49.32495));
#253293=CARTESIAN_POINT('Ctrl Pts',(43.0627766507519,30.7060797967663,-49.2666166666667));
#253294=CARTESIAN_POINT('Ctrl Pts',(43.5445019199415,29.87170715524,-49.2082833333334));
#253295=CARTESIAN_POINT('Ctrl Pts',(44.5079524583208,29.87170715524,-49.14995));
#253296=CARTESIAN_POINT('Ctrl Pts',(45.4714029967,29.87170715524,-49.0916166666667));
#253297=CARTESIAN_POINT('Ctrl Pts',(45.9531282658897,30.7060797967663,-49.0332833333333));
#253298=CARTESIAN_POINT('Ctrl Pts',(46.4348535350793,31.5404524382925,-48.97495));
#253299=CARTESIAN_POINT('Ctrl Pts',(45.9531282658897,32.3748250798187,-48.9166166666667));
#253300=CARTESIAN_POINT('Ctrl Pts',(45.4714029967,33.2091977213449,-48.8582833333333));
#253301=CARTESIAN_POINT('Ctrl Pts',(44.5079524583208,33.2091977213449,-48.79995));
#253302=CARTESIAN_POINT('Ctrl Pts',(43.5445019199415,33.2091977213449,-48.7416166666667));
#253303=CARTESIAN_POINT('Ctrl Pts',(43.0627766507519,32.3748250798187,-48.6832833333333));
#253304=CARTESIAN_POINT('Ctrl Pts',(42.5810513815623,31.5404524382925,-48.62495));
#253305=CARTESIAN_POINT('Ctrl Pts',(43.0627766507519,30.7060797967663,-48.5666166666667));
#253306=CARTESIAN_POINT('Ctrl Pts',(43.5445019199415,29.87170715524,-48.5082833333333));
#253307=CARTESIAN_POINT('Ctrl Pts',(44.5079524583208,29.87170715524,-48.44995));
#253308=CARTESIAN_POINT('Ctrl Pts',(45.4714029967,29.87170715524,-48.3916166666667));
#253309=CARTESIAN_POINT('Ctrl Pts',(45.9531282658897,30.7060797967663,-48.3332833333333));
#253310=CARTESIAN_POINT('Ctrl Pts',(46.4348535350793,31.5404524382925,-48.27495));
#253311=CARTESIAN_POINT('Ctrl Pts',(45.9531282658897,32.3748250798187,-48.2166166666667));
#253312=CARTESIAN_POINT('Ctrl Pts',(45.4714029967,33.2091977213449,-48.1582833333333));
#253313=CARTESIAN_POINT('Ctrl Pts',(44.5079524583208,33.2091977213449,-48.09995));
#253314=CARTESIAN_POINT('Ctrl Pts',(43.5445019199415,33.2091977213449,-48.0416166666667));
#253315=CARTESIAN_POINT('Ctrl Pts',(43.0627766507519,32.3748250798187,-47.9832833333334));
#253316=CARTESIAN_POINT('Ctrl Pts',(42.5810513815623,31.5404524382925,-47.92495));
#253317=CARTESIAN_POINT('Ctrl Pts',(43.0627766507519,30.7060797967663,-47.8666166666667));
#253318=CARTESIAN_POINT('Ctrl Pts',(43.5445019199415,29.87170715524,-47.8082833333333));
#253319=CARTESIAN_POINT('Ctrl Pts',(44.5079524583208,29.87170715524,-47.74995));
#253320=CARTESIAN_POINT('Ctrl Pts',(45.4714029967,29.87170715524,-47.6916166666667));
#253321=CARTESIAN_POINT('Ctrl Pts',(45.9531282658897,30.7060797967663,-47.6332833333333));
#253322=CARTESIAN_POINT('Ctrl Pts',(46.4348535350793,31.5404524382925,-47.57495));
#253323=CARTESIAN_POINT('Ctrl Pts',(45.9531282658897,32.3748250798187,-47.5166166666667));
#253324=CARTESIAN_POINT('Ctrl Pts',(45.4714029967,33.2091977213449,-47.4582833333333));
#253325=CARTESIAN_POINT('Ctrl Pts',(44.5079524583208,33.2091977213449,-47.39995));
#253326=CARTESIAN_POINT('Ctrl Pts',(43.5445019199415,33.2091977213449,-47.3416166666666));
#253327=CARTESIAN_POINT('Ctrl Pts',(43.0627766507519,32.3748250798187,-47.2832833333333));
#253328=CARTESIAN_POINT('Ctrl Pts',(42.5810513815623,31.5404524382925,-47.22495));
#253329=CARTESIAN_POINT('Ctrl Pts',(43.0627766507519,30.7060797967663,-47.1666166666667));
#253330=CARTESIAN_POINT('Ctrl Pts',(43.5445019199415,29.87170715524,-47.1082833333333));
#253331=CARTESIAN_POINT('Ctrl Pts',(44.5079524583208,29.87170715524,-47.04995));
#253332=CARTESIAN_POINT('Ctrl Pts',(45.4714029967,29.87170715524,-46.9916166666667));
#253333=CARTESIAN_POINT('Ctrl Pts',(45.9531282658897,30.7060797967663,-46.9332833333333));
#253334=CARTESIAN_POINT('Ctrl Pts',(46.4348535350793,31.5404524382925,-46.87495));
#253335=CARTESIAN_POINT('Ctrl Pts',(45.9531282658897,32.3748250798187,-46.8166166666667));
#253336=CARTESIAN_POINT('Ctrl Pts',(45.4714029967,33.2091977213449,-46.7582833333333));
#253337=CARTESIAN_POINT('Ctrl Pts',(44.5079524583208,33.2091977213449,-46.69995));
#253338=CARTESIAN_POINT('Ctrl Pts',(43.5445019199415,33.2091977213449,-46.6416166666666));
#253339=CARTESIAN_POINT('Ctrl Pts',(43.0627766507519,32.3748250798187,-46.5832833333334));
#253340=CARTESIAN_POINT('Ctrl Pts',(42.5810513815623,31.5404524382925,-46.52495));
#253341=CARTESIAN_POINT('Ctrl Pts',(43.0627766507519,30.7060797967663,-46.4666166666667));
#253342=CARTESIAN_POINT('Ctrl Pts',(43.5445019199415,29.87170715524,-46.4082833333333));
#253343=CARTESIAN_POINT('Ctrl Pts',(44.5079524583208,29.87170715524,-46.34995));
#253344=CARTESIAN_POINT('Ctrl Pts',(45.4714029967,29.87170715524,-46.2916166666667));
#253345=CARTESIAN_POINT('Ctrl Pts',(45.9531282658897,30.7060797967663,-46.2332833333334));
#253346=CARTESIAN_POINT('Ctrl Pts',(46.4348535350793,31.5404524382925,-46.17495));
#253347=CARTESIAN_POINT('Ctrl Pts',(45.9531282658897,32.3748250798187,-46.1166166666667));
#253348=CARTESIAN_POINT('Ctrl Pts',(45.4714029967,33.2091977213449,-46.0582833333333));
#253349=CARTESIAN_POINT('Ctrl Pts',(44.5079524583208,33.2091977213449,-45.99995));
#253350=CARTESIAN_POINT('Ctrl Pts',(43.5445019199415,33.2091977213449,-45.9416166666667));
#253351=CARTESIAN_POINT('Ctrl Pts',(43.0627766507519,32.3748250798187,-45.8832833333333));
#253352=CARTESIAN_POINT('Ctrl Pts',(42.5810513815623,31.5404524382925,-45.82495));
#253353=CARTESIAN_POINT('Ctrl Pts',(43.0627766507519,30.7060797967663,-45.7666166666667));
#253354=CARTESIAN_POINT('Ctrl Pts',(43.5445019199415,29.87170715524,-45.7082833333333));
#253355=CARTESIAN_POINT('Ctrl Pts',(44.5079524583208,29.87170715524,-45.64995));
#253356=CARTESIAN_POINT('Ctrl Pts',(45.4714029967,29.87170715524,-45.5916166666667));
#253357=CARTESIAN_POINT('Ctrl Pts',(45.9531282658897,30.7060797967663,-45.5332833333333));
#253358=CARTESIAN_POINT('Ctrl Pts',(46.4348535350793,31.5404524382925,-45.47495));
#253359=CARTESIAN_POINT('Ctrl Pts',(45.9531282658897,32.3748250798187,-45.4166166666667));
#253360=CARTESIAN_POINT('Ctrl Pts',(45.4714029967,33.2091977213449,-45.3582833333333));
#253361=CARTESIAN_POINT('Ctrl Pts',(44.5079524583208,33.2091977213449,-45.29995));
#253362=CARTESIAN_POINT('Ctrl Pts',(43.5445019199415,33.2091977213449,-45.2416166666667));
#253363=CARTESIAN_POINT('Ctrl Pts',(43.0627766507519,32.3748250798187,-45.1832833333333));
#253364=CARTESIAN_POINT('Ctrl Pts',(42.5810513815623,31.5404524382925,-45.12495));
#253365=CARTESIAN_POINT('Ctrl Pts',(43.0627766507519,30.7060797967663,-45.0666166666667));
#253366=CARTESIAN_POINT('Ctrl Pts',(43.5445019199415,29.87170715524,-45.0082833333334));
#253367=CARTESIAN_POINT('Ctrl Pts',(44.5079524583208,29.87170715524,-44.94995));
#253368=CARTESIAN_POINT('Ctrl Pts',(45.4714029967,29.87170715524,-44.8916166666667));
#253369=CARTESIAN_POINT('Ctrl Pts',(45.9531282658897,30.7060797967663,-44.8332833333334));
#253370=CARTESIAN_POINT('Ctrl Pts',(46.4348535350793,31.5404524382925,-44.77495));
#253371=CARTESIAN_POINT('Ctrl Pts',(45.9531282658897,32.3748250798187,-44.7166166666667));
#253372=CARTESIAN_POINT('Ctrl Pts',(45.4714029967,33.2091977213449,-44.6582833333333));
#253373=CARTESIAN_POINT('Ctrl Pts',(44.5079524583208,33.2091977213449,-44.59995));
#253374=CARTESIAN_POINT('Ctrl Pts',(43.5445019199415,33.2091977213449,-44.5416166666667));
#253375=CARTESIAN_POINT('Ctrl Pts',(43.0627766507519,32.3748250798187,-44.4832833333334));
#253376=CARTESIAN_POINT('Ctrl Pts',(42.5810513815623,31.5404524382925,-44.42495));
#253377=CARTESIAN_POINT('Ctrl Pts',(43.0627766507519,30.7060797967663,-44.3666166666667));
#253378=CARTESIAN_POINT('Ctrl Pts',(43.5445019199415,29.87170715524,-44.3082833333334));
#253379=CARTESIAN_POINT('Ctrl Pts',(44.5079524583208,29.87170715524,-44.24995));
#253380=CARTESIAN_POINT('Ctrl Pts',(45.4714029967,29.87170715524,-44.1916166666667));
#253381=CARTESIAN_POINT('Ctrl Pts',(45.9531282658897,30.7060797967663,-44.1332833333334));
#253382=CARTESIAN_POINT('Ctrl Pts',(46.4348535350793,31.5404524382925,-44.07495));
#253383=CARTESIAN_POINT('Ctrl Pts',(45.9531282658897,32.3748250798187,-44.0166166666667));
#253384=CARTESIAN_POINT('Ctrl Pts',(45.4714029967,33.2091977213449,-43.9582833333334));
#253385=CARTESIAN_POINT('Ctrl Pts',(44.5079524583208,33.2091977213449,-43.89995));
#253386=CARTESIAN_POINT('Ctrl Pts',(43.5445019199415,33.2091977213449,-43.8416166666667));
#253387=CARTESIAN_POINT('Ctrl Pts',(43.0627766507519,32.3748250798187,-43.7832833333334));
#253388=CARTESIAN_POINT('Ctrl Pts',(42.5810513815623,31.5404524382925,-43.72495));
#253389=CARTESIAN_POINT('Ctrl Pts',(43.0627766507519,30.7060797967663,-43.6666166666667));
#253390=CARTESIAN_POINT('Ctrl Pts',(43.5445019199415,29.87170715524,-43.6082833333333));
#253391=CARTESIAN_POINT('Ctrl Pts',(44.5079524583208,29.87170715524,-43.54995));
#253392=CARTESIAN_POINT('Ctrl Pts',(45.4714029967,29.87170715524,-43.4916166666667));
#253393=CARTESIAN_POINT('Ctrl Pts',(45.9531282658897,30.7060797967663,-43.4332833333333));
#253394=CARTESIAN_POINT('Ctrl Pts',(46.4348535350793,31.5404524382925,-43.37495));
#253395=CARTESIAN_POINT('Ctrl Pts',(45.9531282658897,32.3748250798187,-43.3166166666667));
#253396=CARTESIAN_POINT('Ctrl Pts',(45.4714029967,33.2091977213449,-43.2582833333333));
#253397=CARTESIAN_POINT('Ctrl Pts',(44.5079524583208,33.2091977213449,-43.19995));
#253398=CARTESIAN_POINT('Ctrl Pts',(43.5445019199415,33.2091977213449,-43.1416166666666));
#253399=CARTESIAN_POINT('Ctrl Pts',(43.0627766507519,32.3748250798187,-43.0832833333333));
#253400=CARTESIAN_POINT('Ctrl Pts',(42.5810513815623,31.5404524382925,-43.02495));
#253401=CARTESIAN_POINT('Ctrl Pts',(43.0627766507519,30.7060797967663,-42.9666166666667));
#253402=CARTESIAN_POINT('Ctrl Pts',(43.5445019199415,29.87170715524,-42.9082833333333));
#253403=CARTESIAN_POINT('Ctrl Pts',(44.5079524583208,29.87170715524,-42.84995));
#253404=CARTESIAN_POINT('Ctrl Pts',(45.4714029967,29.87170715524,-42.7916166666667));
#253405=CARTESIAN_POINT('Ctrl Pts',(45.9531282658897,30.7060797967663,-42.7332833333334));
#253406=CARTESIAN_POINT('Ctrl Pts',(46.4348535350793,31.5404524382925,-42.67495));
#253407=CARTESIAN_POINT('Ctrl Pts',(45.9531282658897,32.3748250798187,-42.6166166666667));
#253408=CARTESIAN_POINT('Ctrl Pts',(45.4714029967,33.2091977213449,-42.5582833333333));
#253409=CARTESIAN_POINT('Ctrl Pts',(44.5079524583208,33.2091977213449,-42.49995));
#253410=CARTESIAN_POINT('Ctrl Pts',(43.5445019199415,33.2091977213449,-42.4416166666667));
#253411=CARTESIAN_POINT('Ctrl Pts',(43.0627766507519,32.3748250798187,-42.3832833333333));
#253412=CARTESIAN_POINT('Ctrl Pts',(42.5810513815623,31.5404524382925,-42.32495));
#253413=CARTESIAN_POINT('Ctrl Pts',(43.0627766507519,30.7060797967663,-42.2666166666667));
#253414=CARTESIAN_POINT('Ctrl Pts',(43.5445019199415,29.87170715524,-42.2082833333333));
#253415=CARTESIAN_POINT('Ctrl Pts',(44.5079524583208,29.87170715524,-42.14995));
#253416=CARTESIAN_POINT('Ctrl Pts',(45.4714029967,29.87170715524,-42.0916166666667));
#253417=CARTESIAN_POINT('Ctrl Pts',(45.9531282658897,30.7060797967663,-42.0332833333334));
#253418=CARTESIAN_POINT('Ctrl Pts',(46.4348535350793,31.5404524382925,-41.97495));
#253419=CARTESIAN_POINT('Ctrl Pts',(45.9531282658897,32.3748250798187,-41.9166166666666));
#253420=CARTESIAN_POINT('Ctrl Pts',(45.4714029967,33.2091977213449,-41.8582833333333));
#253421=CARTESIAN_POINT('Ctrl Pts',(44.5079524583208,33.2091977213449,-41.79995));
#253422=CARTESIAN_POINT('Ctrl Pts',(43.5445019199415,33.2091977213449,-41.7416166666667));
#253423=CARTESIAN_POINT('Ctrl Pts',(43.0627766507519,32.3748250798187,-41.6832833333333));
#253424=CARTESIAN_POINT('Ctrl Pts',(42.5810513815623,31.5404524382925,-41.62495));
#253425=CARTESIAN_POINT('Ctrl Pts',(43.0627766507519,30.7060797967663,-41.5666166666667));
#253426=CARTESIAN_POINT('Ctrl Pts',(43.5445019199415,29.87170715524,-41.5082833333334));
#253427=CARTESIAN_POINT('Ctrl Pts',(44.5079524583208,29.87170715524,-41.44995));
#253428=CARTESIAN_POINT('Ctrl Pts',(45.4714029967,29.87170715524,-41.3916166666667));
#253429=CARTESIAN_POINT('Ctrl Pts',(45.9531282658897,30.7060797967663,-41.3332833333334));
#253430=CARTESIAN_POINT('Ctrl Pts',(46.4348535350793,31.5404524382925,-41.27495));
#253431=CARTESIAN_POINT('Ctrl Pts',(45.9531282658897,32.3748250798187,-41.2166166666667));
#253432=CARTESIAN_POINT('Ctrl Pts',(45.4714029967,33.2091977213449,-41.1582833333333));
#253433=CARTESIAN_POINT('Ctrl Pts',(44.5079524583208,33.2091977213449,-41.09995));
#253434=CARTESIAN_POINT('Ctrl Pts',(43.5445019199415,33.2091977213449,-41.0416166666667));
#253435=CARTESIAN_POINT('Ctrl Pts',(43.0627766507519,32.3748250798187,-40.9832833333333));
#253436=CARTESIAN_POINT('Ctrl Pts',(42.5810513815623,31.5404524382925,-40.92495));
#253437=CARTESIAN_POINT('Ctrl Pts',(43.0627766507519,30.7060797967663,-40.8666166666667));
#253438=CARTESIAN_POINT('Ctrl Pts',(43.5445019199415,29.87170715524,-40.8082833333334));
#253439=CARTESIAN_POINT('Ctrl Pts',(44.5079524583208,29.87170715524,-40.74995));
#253440=CARTESIAN_POINT('Ctrl Pts',(45.4714029967,29.87170715524,-40.6916166666667));
#253441=CARTESIAN_POINT('Ctrl Pts',(45.9531282658897,30.7060797967663,-40.6332833333334));
#253442=CARTESIAN_POINT('Ctrl Pts',(46.4348535350793,31.5404524382925,-40.57495));
#253443=CARTESIAN_POINT('Ctrl Pts',(45.9531282658897,32.3748250798187,-40.5166166666666));
#253444=CARTESIAN_POINT('Ctrl Pts',(45.4714029967,33.2091977213449,-40.4582833333333));
#253445=CARTESIAN_POINT('Ctrl Pts',(44.5079524583208,33.2091977213449,-40.39995));
#253446=CARTESIAN_POINT('Ctrl Pts',(43.5445019199415,33.2091977213449,-40.3416166666667));
#253447=CARTESIAN_POINT('Ctrl Pts',(43.0627766507519,32.3748250798187,-40.2832833333334));
#253448=CARTESIAN_POINT('Ctrl Pts',(42.5810513815623,31.5404524382925,-40.22495));
#253449=CARTESIAN_POINT('Ctrl Pts',(43.0627766507519,30.7060797967663,-40.1666166666667));
#253450=CARTESIAN_POINT('Ctrl Pts',(43.5445019199415,29.87170715524,-40.1082833333334));
#253451=CARTESIAN_POINT('Ctrl Pts',(44.5079524583208,29.87170715524,-40.04995));
#253452=CARTESIAN_POINT('Ctrl Pts',(45.4714029967,29.87170715524,-39.9916166666667));
#253453=CARTESIAN_POINT('Ctrl Pts',(45.9531282658897,30.7060797967663,-39.9332833333333));
#253454=CARTESIAN_POINT('Ctrl Pts',(46.4348535350793,31.5404524382925,-39.87495));
#253455=CARTESIAN_POINT('Ctrl Pts',(45.9531282658897,32.3748250798187,-39.8166166666667));
#253456=CARTESIAN_POINT('Ctrl Pts',(45.4714029967,33.2091977213449,-39.7582833333334));
#253457=CARTESIAN_POINT('Ctrl Pts',(44.5079524583208,33.2091977213449,-39.69995));
#253458=CARTESIAN_POINT('Ctrl Pts',(43.5445019199415,33.2091977213449,-39.6416166666667));
#253459=CARTESIAN_POINT('Ctrl Pts',(43.0627766507519,32.3748250798187,-39.5832833333333));
#253460=CARTESIAN_POINT('Ctrl Pts',(42.5810513815623,31.5404524382925,-39.52495));
#253461=CARTESIAN_POINT('Ctrl Pts',(43.0627766507519,30.7060797967663,-39.4666166666667));
#253462=CARTESIAN_POINT('Ctrl Pts',(43.5445019199415,29.87170715524,-39.4082833333333));
#253463=CARTESIAN_POINT('Ctrl Pts',(44.5079524583208,29.87170715524,-39.34995));
#253464=CARTESIAN_POINT('Ctrl Pts',(45.4714029967,29.87170715524,-39.2916166666667));
#253465=CARTESIAN_POINT('Ctrl Pts',(45.9531282658897,30.7060797967663,-39.2332833333333));
#253466=CARTESIAN_POINT('Ctrl Pts',(46.4348535350793,31.5404524382925,-39.17495));
#253467=CARTESIAN_POINT('Ctrl Pts',(45.9531282658897,32.3748250798187,-39.1166166666667));
#253468=CARTESIAN_POINT('Ctrl Pts',(45.4714029967,33.2091977213449,-39.0582833333333));
#253469=CARTESIAN_POINT('Ctrl Pts',(44.5079524583208,33.2091977213449,-38.99995));
#253470=CARTESIAN_POINT('Ctrl Pts',(43.5445019199415,33.2091977213449,-38.9416166666667));
#253471=CARTESIAN_POINT('Ctrl Pts',(43.0627766507519,32.3748250798187,-38.8832833333334));
#253472=CARTESIAN_POINT('Ctrl Pts',(42.5810513815623,31.5404524382925,-38.82495));
#253473=CARTESIAN_POINT('Ctrl Pts',(43.0627766507519,30.7060797967663,-38.7666166666667));
#253474=CARTESIAN_POINT('Ctrl Pts',(43.5445019199415,29.87170715524,-38.7082833333333));
#253475=CARTESIAN_POINT('Ctrl Pts',(44.5079524583208,29.87170715524,-38.64995));
#253476=CARTESIAN_POINT('Ctrl Pts',(45.4714029967,29.87170715524,-38.5916166666667));
#253477=CARTESIAN_POINT('Ctrl Pts',(45.9531282658897,30.7060797967663,-38.5332833333334));
#253478=CARTESIAN_POINT('Ctrl Pts',(46.4348535350793,31.5404524382925,-38.47495));
#253479=CARTESIAN_POINT('Ctrl Pts',(45.9531282658897,32.3748250798187,-38.4166166666667));
#253480=CARTESIAN_POINT('Ctrl Pts',(45.4714029967,33.2091977213449,-38.3582833333333));
#253481=CARTESIAN_POINT('Ctrl Pts',(44.5079524583208,33.2091977213449,-38.29995));
#253482=CARTESIAN_POINT('Ctrl Pts',(43.5445019199415,33.2091977213449,-38.2416166666667));
#253483=CARTESIAN_POINT('Ctrl Pts',(43.0627766507519,32.3748250798187,-38.1832833333333));
#253484=CARTESIAN_POINT('Ctrl Pts',(42.5810513815623,31.5404524382925,-38.12495));
#253485=CARTESIAN_POINT('Ctrl Pts',(43.0627766507519,30.7060797967663,-38.0666166666667));
#253486=CARTESIAN_POINT('Ctrl Pts',(43.5445019199415,29.87170715524,-38.0082833333333));
#253487=CARTESIAN_POINT('Ctrl Pts',(44.5079524583208,29.87170715524,-37.94995));
#253488=CARTESIAN_POINT('Ctrl Pts',(45.4714029967,29.87170715524,-37.8916166666667));
#253489=CARTESIAN_POINT('Ctrl Pts',(45.9531282658897,30.7060797967663,-37.8332833333334));
#253490=CARTESIAN_POINT('Ctrl Pts',(46.4348535350793,31.5404524382925,-37.77495));
#253491=CARTESIAN_POINT('Ctrl Pts',(45.9531282658897,32.3748250798187,-37.7166166666667));
#253492=CARTESIAN_POINT('Ctrl Pts',(45.4714029967,33.2091977213449,-37.6582833333333));
#253493=CARTESIAN_POINT('Ctrl Pts',(44.5079524583208,33.2091977213449,-37.59995));
#253494=CARTESIAN_POINT('Ctrl Pts',(43.5445019199415,33.2091977213449,-37.5416166666667));
#253495=CARTESIAN_POINT('Ctrl Pts',(43.0627766507519,32.3748250798187,-37.4832833333334));
#253496=CARTESIAN_POINT('Ctrl Pts',(42.5810513815623,31.5404524382925,-37.42495));
#253497=CARTESIAN_POINT('Ctrl Pts',(43.0627766507519,30.7060797967663,-37.3666166666667));
#253498=CARTESIAN_POINT('Ctrl Pts',(43.5445019199415,29.87170715524,-37.3082833333333));
#253499=CARTESIAN_POINT('Ctrl Pts',(44.5079524583208,29.87170715524,-37.24995));
#253500=CARTESIAN_POINT('Ctrl Pts',(45.4714029967,29.87170715524,-37.1916166666667));
#253501=CARTESIAN_POINT('Ctrl Pts',(45.9531282658897,30.7060797967663,-37.1332833333334));
#253502=CARTESIAN_POINT('Ctrl Pts',(46.4348535350793,31.5404524382925,-37.07495));
#253503=CARTESIAN_POINT('Ctrl Pts',(45.9531282658897,32.3748250798187,-37.0166166666667));
#253504=CARTESIAN_POINT('Ctrl Pts',(45.8905850977848,32.4831530246427,-37.0090431559831));
#253505=CARTESIAN_POINT('Ctrl Pts',(45.8125914103809,32.5809465634453,-37.0009024189827));
#253506=CARTESIAN_POINT('Ctrl Pts',(44.5079524583208,33.6091932047179,-53.2308875));
#253507=CARTESIAN_POINT('Ctrl Pts',(43.3135644199415,33.6091932047179,-53.1725541666667));
#253508=CARTESIAN_POINT('Ctrl Pts',(42.7163704007519,32.5748228215052,-53.1142208333334));
#253509=CARTESIAN_POINT('Ctrl Pts',(42.1191763815623,31.5404524382925,-53.0558875000001));
#253510=CARTESIAN_POINT('Ctrl Pts',(42.7163704007519,30.5060820550798,-52.9975541666667));
#253511=CARTESIAN_POINT('Ctrl Pts',(43.3135644199415,29.4717116718671,-52.9392208333334));
#253512=CARTESIAN_POINT('Ctrl Pts',(44.5079524583208,29.4717116718671,-52.8808875));
#253513=CARTESIAN_POINT('Ctrl Pts',(45.7023404967,29.4717116718671,-52.8225541666667));
#253514=CARTESIAN_POINT('Ctrl Pts',(46.2995345158897,30.5060820550798,-52.7642208333334));
#253515=CARTESIAN_POINT('Ctrl Pts',(46.8967285350793,31.5404524382925,-52.7058875));
#253516=CARTESIAN_POINT('Ctrl Pts',(46.2995345158897,32.5748228215052,-52.6475541666667));
#253517=CARTESIAN_POINT('Ctrl Pts',(45.7023404967,33.6091932047179,-52.5892208333333));
#253518=CARTESIAN_POINT('Ctrl Pts',(44.5079524583208,33.6091932047179,-52.5308875));
#253519=CARTESIAN_POINT('Ctrl Pts',(43.3135644199415,33.6091932047179,-52.4725541666667));
#253520=CARTESIAN_POINT('Ctrl Pts',(42.7163704007519,32.5748228215052,-52.4142208333333));
#253521=CARTESIAN_POINT('Ctrl Pts',(42.1191763815623,31.5404524382925,-52.3558875000001));
#253522=CARTESIAN_POINT('Ctrl Pts',(42.7163704007519,30.5060820550798,-52.2975541666667));
#253523=CARTESIAN_POINT('Ctrl Pts',(43.3135644199415,29.4717116718671,-52.2392208333334));
#253524=CARTESIAN_POINT('Ctrl Pts',(44.5079524583208,29.4717116718671,-52.1808875));
#253525=CARTESIAN_POINT('Ctrl Pts',(45.7023404967,29.4717116718671,-52.1225541666667));
#253526=CARTESIAN_POINT('Ctrl Pts',(46.2995345158897,30.5060820550798,-52.0642208333334));
#253527=CARTESIAN_POINT('Ctrl Pts',(46.8967285350793,31.5404524382925,-52.0058875));
#253528=CARTESIAN_POINT('Ctrl Pts',(46.2995345158897,32.5748228215052,-51.9475541666667));
#253529=CARTESIAN_POINT('Ctrl Pts',(45.7023404967,33.6091932047179,-51.8892208333334));
#253530=CARTESIAN_POINT('Ctrl Pts',(44.5079524583208,33.6091932047179,-51.8308875));
#253531=CARTESIAN_POINT('Ctrl Pts',(43.3135644199415,33.6091932047179,-51.7725541666667));
#253532=CARTESIAN_POINT('Ctrl Pts',(42.7163704007519,32.5748228215052,-51.7142208333334));
#253533=CARTESIAN_POINT('Ctrl Pts',(42.1191763815623,31.5404524382925,-51.6558875));
#253534=CARTESIAN_POINT('Ctrl Pts',(42.7163704007519,30.5060820550798,-51.5975541666667));
#253535=CARTESIAN_POINT('Ctrl Pts',(43.3135644199415,29.4717116718671,-51.5392208333333));
#253536=CARTESIAN_POINT('Ctrl Pts',(44.5079524583208,29.4717116718671,-51.4808875));
#253537=CARTESIAN_POINT('Ctrl Pts',(45.7023404967,29.4717116718671,-51.4225541666667));
#253538=CARTESIAN_POINT('Ctrl Pts',(46.2995345158897,30.5060820550798,-51.3642208333334));
#253539=CARTESIAN_POINT('Ctrl Pts',(46.8967285350793,31.5404524382925,-51.3058875));
#253540=CARTESIAN_POINT('Ctrl Pts',(46.2995345158897,32.5748228215052,-51.2475541666667));
#253541=CARTESIAN_POINT('Ctrl Pts',(45.7023404967,33.6091932047179,-51.1892208333333));
#253542=CARTESIAN_POINT('Ctrl Pts',(44.5079524583208,33.6091932047179,-51.1308875));
#253543=CARTESIAN_POINT('Ctrl Pts',(43.3135644199415,33.6091932047179,-51.0725541666667));
#253544=CARTESIAN_POINT('Ctrl Pts',(42.7163704007519,32.5748228215052,-51.0142208333334));
#253545=CARTESIAN_POINT('Ctrl Pts',(42.1191763815623,31.5404524382925,-50.9558875));
#253546=CARTESIAN_POINT('Ctrl Pts',(42.7163704007519,30.5060820550798,-50.8975541666667));
#253547=CARTESIAN_POINT('Ctrl Pts',(43.3135644199415,29.4717116718671,-50.8392208333333));
#253548=CARTESIAN_POINT('Ctrl Pts',(44.5079524583208,29.4717116718671,-50.7808875));
#253549=CARTESIAN_POINT('Ctrl Pts',(45.7023404967,29.4717116718671,-50.7225541666666));
#253550=CARTESIAN_POINT('Ctrl Pts',(46.2995345158897,30.5060820550798,-50.6642208333333));
#253551=CARTESIAN_POINT('Ctrl Pts',(46.8967285350793,31.5404524382925,-50.6058875));
#253552=CARTESIAN_POINT('Ctrl Pts',(46.2995345158897,32.5748228215052,-50.5475541666667));
#253553=CARTESIAN_POINT('Ctrl Pts',(45.7023404967,33.6091932047179,-50.4892208333333));
#253554=CARTESIAN_POINT('Ctrl Pts',(44.5079524583208,33.6091932047179,-50.4308875));
#253555=CARTESIAN_POINT('Ctrl Pts',(43.3135644199415,33.6091932047179,-50.3725541666667));
#253556=CARTESIAN_POINT('Ctrl Pts',(42.7163704007519,32.5748228215052,-50.3142208333334));
#253557=CARTESIAN_POINT('Ctrl Pts',(42.1191763815623,31.5404524382925,-50.2558875));
#253558=CARTESIAN_POINT('Ctrl Pts',(42.7163704007519,30.5060820550798,-50.1975541666667));
#253559=CARTESIAN_POINT('Ctrl Pts',(43.3135644199415,29.4717116718671,-50.1392208333333));
#253560=CARTESIAN_POINT('Ctrl Pts',(44.5079524583208,29.4717116718671,-50.0808875));
#253561=CARTESIAN_POINT('Ctrl Pts',(45.7023404967,29.4717116718671,-50.0225541666667));
#253562=CARTESIAN_POINT('Ctrl Pts',(46.2995345158897,30.5060820550798,-49.9642208333334));
#253563=CARTESIAN_POINT('Ctrl Pts',(46.8967285350793,31.5404524382925,-49.9058875));
#253564=CARTESIAN_POINT('Ctrl Pts',(46.2995345158897,32.5748228215052,-49.8475541666667));
#253565=CARTESIAN_POINT('Ctrl Pts',(45.7023404967,33.6091932047179,-49.7892208333333));
#253566=CARTESIAN_POINT('Ctrl Pts',(44.5079524583208,33.6091932047179,-49.7308875));
#253567=CARTESIAN_POINT('Ctrl Pts',(43.3135644199415,33.6091932047179,-49.6725541666667));
#253568=CARTESIAN_POINT('Ctrl Pts',(42.7163704007519,32.5748228215052,-49.6142208333334));
#253569=CARTESIAN_POINT('Ctrl Pts',(42.1191763815623,31.5404524382925,-49.5558875));
#253570=CARTESIAN_POINT('Ctrl Pts',(42.7163704007519,30.5060820550798,-49.4975541666667));
#253571=CARTESIAN_POINT('Ctrl Pts',(43.3135644199415,29.4717116718671,-49.4392208333333));
#253572=CARTESIAN_POINT('Ctrl Pts',(44.5079524583208,29.4717116718671,-49.3808875));
#253573=CARTESIAN_POINT('Ctrl Pts',(45.7023404967,29.4717116718671,-49.3225541666667));
#253574=CARTESIAN_POINT('Ctrl Pts',(46.2995345158897,30.5060820550798,-49.2642208333334));
#253575=CARTESIAN_POINT('Ctrl Pts',(46.8967285350793,31.5404524382925,-49.2058875));
#253576=CARTESIAN_POINT('Ctrl Pts',(46.2995345158897,32.5748228215052,-49.1475541666667));
#253577=CARTESIAN_POINT('Ctrl Pts',(45.7023404967,33.6091932047179,-49.0892208333333));
#253578=CARTESIAN_POINT('Ctrl Pts',(44.5079524583208,33.6091932047179,-49.0308875));
#253579=CARTESIAN_POINT('Ctrl Pts',(43.3135644199415,33.6091932047179,-48.9725541666667));
#253580=CARTESIAN_POINT('Ctrl Pts',(42.7163704007519,32.5748228215052,-48.9142208333333));
#253581=CARTESIAN_POINT('Ctrl Pts',(42.1191763815623,31.5404524382925,-48.8558875));
#253582=CARTESIAN_POINT('Ctrl Pts',(42.7163704007519,30.5060820550798,-48.7975541666667));
#253583=CARTESIAN_POINT('Ctrl Pts',(43.3135644199415,29.4717116718671,-48.7392208333334));
#253584=CARTESIAN_POINT('Ctrl Pts',(44.5079524583208,29.4717116718671,-48.6808875));
#253585=CARTESIAN_POINT('Ctrl Pts',(45.7023404967,29.4717116718671,-48.6225541666667));
#253586=CARTESIAN_POINT('Ctrl Pts',(46.2995345158897,30.5060820550798,-48.5642208333334));
#253587=CARTESIAN_POINT('Ctrl Pts',(46.8967285350793,31.5404524382925,-48.5058875));
#253588=CARTESIAN_POINT('Ctrl Pts',(46.2995345158897,32.5748228215052,-48.4475541666667));
#253589=CARTESIAN_POINT('Ctrl Pts',(45.7023404967,33.6091932047179,-48.3892208333334));
#253590=CARTESIAN_POINT('Ctrl Pts',(44.5079524583208,33.6091932047179,-48.3308875));
#253591=CARTESIAN_POINT('Ctrl Pts',(43.3135644199415,33.6091932047179,-48.2725541666667));
#253592=CARTESIAN_POINT('Ctrl Pts',(42.7163704007519,32.5748228215052,-48.2142208333334));
#253593=CARTESIAN_POINT('Ctrl Pts',(42.1191763815623,31.5404524382925,-48.1558875));
#253594=CARTESIAN_POINT('Ctrl Pts',(42.7163704007519,30.5060820550798,-48.0975541666667));
#253595=CARTESIAN_POINT('Ctrl Pts',(43.3135644199415,29.4717116718671,-48.0392208333334));
#253596=CARTESIAN_POINT('Ctrl Pts',(44.5079524583208,29.4717116718671,-47.9808875));
#253597=CARTESIAN_POINT('Ctrl Pts',(45.7023404967,29.4717116718671,-47.9225541666667));
#253598=CARTESIAN_POINT('Ctrl Pts',(46.2995345158897,30.5060820550798,-47.8642208333334));
#253599=CARTESIAN_POINT('Ctrl Pts',(46.8967285350793,31.5404524382925,-47.8058875000001));
#253600=CARTESIAN_POINT('Ctrl Pts',(46.2995345158897,32.5748228215052,-47.7475541666667));
#253601=CARTESIAN_POINT('Ctrl Pts',(45.7023404967,33.6091932047179,-47.6892208333334));
#253602=CARTESIAN_POINT('Ctrl Pts',(44.5079524583208,33.6091932047179,-47.6308875));
#253603=CARTESIAN_POINT('Ctrl Pts',(43.3135644199415,33.6091932047179,-47.5725541666667));
#253604=CARTESIAN_POINT('Ctrl Pts',(42.7163704007519,32.5748228215052,-47.5142208333333));
#253605=CARTESIAN_POINT('Ctrl Pts',(42.1191763815623,31.5404524382925,-47.4558875));
#253606=CARTESIAN_POINT('Ctrl Pts',(42.7163704007519,30.5060820550798,-47.3975541666667));
#253607=CARTESIAN_POINT('Ctrl Pts',(43.3135644199415,29.4717116718671,-47.3392208333333));
#253608=CARTESIAN_POINT('Ctrl Pts',(44.5079524583208,29.4717116718671,-47.2808875));
#253609=CARTESIAN_POINT('Ctrl Pts',(45.7023404967,29.4717116718671,-47.2225541666667));
#253610=CARTESIAN_POINT('Ctrl Pts',(46.2995345158897,30.5060820550798,-47.1642208333334));
#253611=CARTESIAN_POINT('Ctrl Pts',(46.8967285350793,31.5404524382925,-47.1058875));
#253612=CARTESIAN_POINT('Ctrl Pts',(46.2995345158897,32.5748228215052,-47.0475541666667));
#253613=CARTESIAN_POINT('Ctrl Pts',(45.7023404967,33.6091932047179,-46.9892208333334));
#253614=CARTESIAN_POINT('Ctrl Pts',(44.5079524583208,33.6091932047179,-46.9308875));
#253615=CARTESIAN_POINT('Ctrl Pts',(43.3135644199415,33.6091932047179,-46.8725541666667));
#253616=CARTESIAN_POINT('Ctrl Pts',(42.7163704007519,32.5748228215052,-46.8142208333334));
#253617=CARTESIAN_POINT('Ctrl Pts',(42.1191763815623,31.5404524382925,-46.7558875));
#253618=CARTESIAN_POINT('Ctrl Pts',(42.7163704007519,30.5060820550798,-46.6975541666667));
#253619=CARTESIAN_POINT('Ctrl Pts',(43.3135644199415,29.4717116718671,-46.6392208333333));
#253620=CARTESIAN_POINT('Ctrl Pts',(44.5079524583208,29.4717116718671,-46.5808875));
#253621=CARTESIAN_POINT('Ctrl Pts',(45.7023404967,29.4717116718671,-46.5225541666667));
#253622=CARTESIAN_POINT('Ctrl Pts',(46.2995345158897,30.5060820550798,-46.4642208333334));
#253623=CARTESIAN_POINT('Ctrl Pts',(46.8967285350793,31.5404524382925,-46.4058875));
#253624=CARTESIAN_POINT('Ctrl Pts',(46.2995345158897,32.5748228215052,-46.3475541666667));
#253625=CARTESIAN_POINT('Ctrl Pts',(45.7023404967,33.6091932047179,-46.2892208333334));
#253626=CARTESIAN_POINT('Ctrl Pts',(44.5079524583208,33.6091932047179,-46.2308875));
#253627=CARTESIAN_POINT('Ctrl Pts',(43.3135644199415,33.6091932047179,-46.1725541666667));
#253628=CARTESIAN_POINT('Ctrl Pts',(42.7163704007519,32.5748228215052,-46.1142208333334));
#253629=CARTESIAN_POINT('Ctrl Pts',(42.1191763815623,31.5404524382925,-46.0558875));
#253630=CARTESIAN_POINT('Ctrl Pts',(42.7163704007519,30.5060820550798,-45.9975541666667));
#253631=CARTESIAN_POINT('Ctrl Pts',(43.3135644199415,29.4717116718671,-45.9392208333333));
#253632=CARTESIAN_POINT('Ctrl Pts',(44.5079524583208,29.4717116718671,-45.8808875));
#253633=CARTESIAN_POINT('Ctrl Pts',(45.7023404967,29.4717116718671,-45.8225541666667));
#253634=CARTESIAN_POINT('Ctrl Pts',(46.2995345158897,30.5060820550798,-45.7642208333334));
#253635=CARTESIAN_POINT('Ctrl Pts',(46.8967285350793,31.5404524382925,-45.7058875));
#253636=CARTESIAN_POINT('Ctrl Pts',(46.2995345158897,32.5748228215052,-45.6475541666667));
#253637=CARTESIAN_POINT('Ctrl Pts',(45.7023404967,33.6091932047179,-45.5892208333333));
#253638=CARTESIAN_POINT('Ctrl Pts',(44.5079524583208,33.6091932047179,-45.5308875));
#253639=CARTESIAN_POINT('Ctrl Pts',(43.3135644199415,33.6091932047179,-45.4725541666667));
#253640=CARTESIAN_POINT('Ctrl Pts',(42.7163704007519,32.5748228215052,-45.4142208333334));
#253641=CARTESIAN_POINT('Ctrl Pts',(42.1191763815623,31.5404524382925,-45.3558875));
#253642=CARTESIAN_POINT('Ctrl Pts',(42.7163704007519,30.5060820550798,-45.2975541666667));
#253643=CARTESIAN_POINT('Ctrl Pts',(43.3135644199415,29.4717116718671,-45.2392208333333));
#253644=CARTESIAN_POINT('Ctrl Pts',(44.5079524583208,29.4717116718671,-45.1808875));
#253645=CARTESIAN_POINT('Ctrl Pts',(45.7023404967,29.4717116718671,-45.1225541666667));
#253646=CARTESIAN_POINT('Ctrl Pts',(46.2995345158897,30.5060820550798,-45.0642208333334));
#253647=CARTESIAN_POINT('Ctrl Pts',(46.8967285350793,31.5404524382925,-45.0058875));
#253648=CARTESIAN_POINT('Ctrl Pts',(46.2995345158897,32.5748228215052,-44.9475541666667));
#253649=CARTESIAN_POINT('Ctrl Pts',(45.7023404967,33.6091932047179,-44.8892208333333));
#253650=CARTESIAN_POINT('Ctrl Pts',(44.5079524583208,33.6091932047179,-44.8308875));
#253651=CARTESIAN_POINT('Ctrl Pts',(43.3135644199415,33.6091932047179,-44.7725541666666));
#253652=CARTESIAN_POINT('Ctrl Pts',(42.7163704007519,32.5748228215052,-44.7142208333334));
#253653=CARTESIAN_POINT('Ctrl Pts',(42.1191763815623,31.5404524382925,-44.6558875));
#253654=CARTESIAN_POINT('Ctrl Pts',(42.7163704007519,30.5060820550798,-44.5975541666667));
#253655=CARTESIAN_POINT('Ctrl Pts',(43.3135644199415,29.4717116718671,-44.5392208333333));
#253656=CARTESIAN_POINT('Ctrl Pts',(44.5079524583208,29.4717116718671,-44.4808875));
#253657=CARTESIAN_POINT('Ctrl Pts',(45.7023404967,29.4717116718671,-44.4225541666667));
#253658=CARTESIAN_POINT('Ctrl Pts',(46.2995345158897,30.5060820550798,-44.3642208333333));
#253659=CARTESIAN_POINT('Ctrl Pts',(46.8967285350793,31.5404524382925,-44.3058875));
#253660=CARTESIAN_POINT('Ctrl Pts',(46.2995345158897,32.5748228215052,-44.2475541666667));
#253661=CARTESIAN_POINT('Ctrl Pts',(45.7023404967,33.6091932047179,-44.1892208333334));
#253662=CARTESIAN_POINT('Ctrl Pts',(44.5079524583208,33.6091932047179,-44.1308875));
#253663=CARTESIAN_POINT('Ctrl Pts',(43.3135644199415,33.6091932047179,-44.0725541666667));
#253664=CARTESIAN_POINT('Ctrl Pts',(42.7163704007519,32.5748228215052,-44.0142208333334));
#253665=CARTESIAN_POINT('Ctrl Pts',(42.1191763815623,31.5404524382925,-43.9558875));
#253666=CARTESIAN_POINT('Ctrl Pts',(42.7163704007519,30.5060820550798,-43.8975541666667));
#253667=CARTESIAN_POINT('Ctrl Pts',(43.3135644199415,29.4717116718671,-43.8392208333333));
#253668=CARTESIAN_POINT('Ctrl Pts',(44.5079524583208,29.4717116718671,-43.7808875));
#253669=CARTESIAN_POINT('Ctrl Pts',(45.7023404967,29.4717116718671,-43.7225541666667));
#253670=CARTESIAN_POINT('Ctrl Pts',(46.2995345158897,30.5060820550798,-43.6642208333334));
#253671=CARTESIAN_POINT('Ctrl Pts',(46.8967285350793,31.5404524382925,-43.6058875));
#253672=CARTESIAN_POINT('Ctrl Pts',(46.2995345158897,32.5748228215052,-43.5475541666667));
#253673=CARTESIAN_POINT('Ctrl Pts',(45.7023404967,33.6091932047179,-43.4892208333333));
#253674=CARTESIAN_POINT('Ctrl Pts',(44.5079524583208,33.6091932047179,-43.4308875));
#253675=CARTESIAN_POINT('Ctrl Pts',(43.3135644199415,33.6091932047179,-43.3725541666667));
#253676=CARTESIAN_POINT('Ctrl Pts',(42.7163704007519,32.5748228215052,-43.3142208333334));
#253677=CARTESIAN_POINT('Ctrl Pts',(42.1191763815623,31.5404524382925,-43.2558875));
#253678=CARTESIAN_POINT('Ctrl Pts',(42.7163704007519,30.5060820550798,-43.1975541666667));
#253679=CARTESIAN_POINT('Ctrl Pts',(43.3135644199415,29.4717116718671,-43.1392208333334));
#253680=CARTESIAN_POINT('Ctrl Pts',(44.5079524583208,29.4717116718671,-43.0808875));
#253681=CARTESIAN_POINT('Ctrl Pts',(45.7023404967,29.4717116718671,-43.0225541666667));
#253682=CARTESIAN_POINT('Ctrl Pts',(46.2995345158897,30.5060820550798,-42.9642208333334));
#253683=CARTESIAN_POINT('Ctrl Pts',(46.8967285350793,31.5404524382925,-42.9058875));
#253684=CARTESIAN_POINT('Ctrl Pts',(46.2995345158897,32.5748228215052,-42.8475541666667));
#253685=CARTESIAN_POINT('Ctrl Pts',(45.7023404967,33.6091932047179,-42.7892208333334));
#253686=CARTESIAN_POINT('Ctrl Pts',(44.5079524583208,33.6091932047179,-42.7308875));
#253687=CARTESIAN_POINT('Ctrl Pts',(43.3135644199415,33.6091932047179,-42.6725541666667));
#253688=CARTESIAN_POINT('Ctrl Pts',(42.7163704007519,32.5748228215052,-42.6142208333334));
#253689=CARTESIAN_POINT('Ctrl Pts',(42.1191763815623,31.5404524382925,-42.5558875));
#253690=CARTESIAN_POINT('Ctrl Pts',(42.7163704007519,30.5060820550798,-42.4975541666667));
#253691=CARTESIAN_POINT('Ctrl Pts',(43.3135644199415,29.4717116718671,-42.4392208333334));
#253692=CARTESIAN_POINT('Ctrl Pts',(44.5079524583208,29.4717116718671,-42.3808875));
#253693=CARTESIAN_POINT('Ctrl Pts',(45.7023404967,29.4717116718671,-42.3225541666667));
#253694=CARTESIAN_POINT('Ctrl Pts',(46.2995345158897,30.5060820550798,-42.2642208333334));
#253695=CARTESIAN_POINT('Ctrl Pts',(46.8967285350793,31.5404524382925,-42.2058875));
#253696=CARTESIAN_POINT('Ctrl Pts',(46.2995345158897,32.5748228215052,-42.1475541666667));
#253697=CARTESIAN_POINT('Ctrl Pts',(45.7023404967,33.6091932047179,-42.0892208333333));
#253698=CARTESIAN_POINT('Ctrl Pts',(44.5079524583208,33.6091932047179,-42.0308875));
#253699=CARTESIAN_POINT('Ctrl Pts',(43.3135644199415,33.6091932047179,-41.9725541666667));
#253700=CARTESIAN_POINT('Ctrl Pts',(42.7163704007519,32.5748228215052,-41.9142208333334));
#253701=CARTESIAN_POINT('Ctrl Pts',(42.1191763815623,31.5404524382925,-41.8558875));
#253702=CARTESIAN_POINT('Ctrl Pts',(42.7163704007519,30.5060820550798,-41.7975541666667));
#253703=CARTESIAN_POINT('Ctrl Pts',(43.3135644199415,29.4717116718671,-41.7392208333333));
#253704=CARTESIAN_POINT('Ctrl Pts',(44.5079524583208,29.4717116718671,-41.6808875));
#253705=CARTESIAN_POINT('Ctrl Pts',(45.7023404967,29.4717116718671,-41.6225541666667));
#253706=CARTESIAN_POINT('Ctrl Pts',(46.2995345158897,30.5060820550798,-41.5642208333334));
#253707=CARTESIAN_POINT('Ctrl Pts',(46.8967285350793,31.5404524382925,-41.5058875));
#253708=CARTESIAN_POINT('Ctrl Pts',(46.2995345158897,32.5748228215052,-41.4475541666667));
#253709=CARTESIAN_POINT('Ctrl Pts',(45.7023404967,33.6091932047179,-41.3892208333333));
#253710=CARTESIAN_POINT('Ctrl Pts',(44.5079524583208,33.6091932047179,-41.3308875));
#253711=CARTESIAN_POINT('Ctrl Pts',(43.3135644199415,33.6091932047179,-41.2725541666667));
#253712=CARTESIAN_POINT('Ctrl Pts',(42.7163704007519,32.5748228215052,-41.2142208333333));
#253713=CARTESIAN_POINT('Ctrl Pts',(42.1191763815623,31.5404524382925,-41.1558875));
#253714=CARTESIAN_POINT('Ctrl Pts',(42.7163704007519,30.5060820550798,-41.0975541666667));
#253715=CARTESIAN_POINT('Ctrl Pts',(43.3135644199415,29.4717116718671,-41.0392208333333));
#253716=CARTESIAN_POINT('Ctrl Pts',(44.5079524583208,29.4717116718671,-40.9808875));
#253717=CARTESIAN_POINT('Ctrl Pts',(45.7023404967,29.4717116718671,-40.9225541666667));
#253718=CARTESIAN_POINT('Ctrl Pts',(46.2995345158897,30.5060820550798,-40.8642208333334));
#253719=CARTESIAN_POINT('Ctrl Pts',(46.8967285350793,31.5404524382925,-40.8058875));
#253720=CARTESIAN_POINT('Ctrl Pts',(46.2995345158897,32.5748228215052,-40.7475541666667));
#253721=CARTESIAN_POINT('Ctrl Pts',(45.7023404967,33.6091932047179,-40.6892208333333));
#253722=CARTESIAN_POINT('Ctrl Pts',(44.5079524583208,33.6091932047179,-40.6308875));
#253723=CARTESIAN_POINT('Ctrl Pts',(43.3135644199415,33.6091932047179,-40.5725541666667));
#253724=CARTESIAN_POINT('Ctrl Pts',(42.7163704007519,32.5748228215052,-40.5142208333333));
#253725=CARTESIAN_POINT('Ctrl Pts',(42.1191763815623,31.5404524382925,-40.4558875));
#253726=CARTESIAN_POINT('Ctrl Pts',(42.7163704007519,30.5060820550798,-40.3975541666667));
#253727=CARTESIAN_POINT('Ctrl Pts',(43.3135644199415,29.4717116718671,-40.3392208333333));
#253728=CARTESIAN_POINT('Ctrl Pts',(44.5079524583208,29.4717116718671,-40.2808875));
#253729=CARTESIAN_POINT('Ctrl Pts',(45.7023404967,29.4717116718671,-40.2225541666667));
#253730=CARTESIAN_POINT('Ctrl Pts',(46.2995345158897,30.5060820550798,-40.1642208333333));
#253731=CARTESIAN_POINT('Ctrl Pts',(46.8967285350793,31.5404524382925,-40.1058875));
#253732=CARTESIAN_POINT('Ctrl Pts',(46.2995345158897,32.5748228215052,-40.0475541666667));
#253733=CARTESIAN_POINT('Ctrl Pts',(45.7023404967,33.6091932047179,-39.9892208333333));
#253734=CARTESIAN_POINT('Ctrl Pts',(44.5079524583208,33.6091932047179,-39.9308875));
#253735=CARTESIAN_POINT('Ctrl Pts',(43.3135644199415,33.6091932047179,-39.8725541666667));
#253736=CARTESIAN_POINT('Ctrl Pts',(42.7163704007519,32.5748228215052,-39.8142208333334));
#253737=CARTESIAN_POINT('Ctrl Pts',(42.1191763815623,31.5404524382925,-39.7558875));
#253738=CARTESIAN_POINT('Ctrl Pts',(42.7163704007519,30.5060820550798,-39.6975541666667));
#253739=CARTESIAN_POINT('Ctrl Pts',(43.3135644199415,29.4717116718671,-39.6392208333334));
#253740=CARTESIAN_POINT('Ctrl Pts',(44.5079524583208,29.4717116718671,-39.5808875));
#253741=CARTESIAN_POINT('Ctrl Pts',(45.7023404967,29.4717116718671,-39.5225541666667));
#253742=CARTESIAN_POINT('Ctrl Pts',(46.2995345158897,30.5060820550798,-39.4642208333333));
#253743=CARTESIAN_POINT('Ctrl Pts',(46.8967285350793,31.5404524382925,-39.4058875));
#253744=CARTESIAN_POINT('Ctrl Pts',(46.2995345158897,32.5748228215052,-39.3475541666667));
#253745=CARTESIAN_POINT('Ctrl Pts',(45.7023404967,33.6091932047179,-39.2892208333334));
#253746=CARTESIAN_POINT('Ctrl Pts',(44.5079524583208,33.6091932047179,-39.2308875));
#253747=CARTESIAN_POINT('Ctrl Pts',(43.3135644199415,33.6091932047179,-39.1725541666667));
#253748=CARTESIAN_POINT('Ctrl Pts',(42.7163704007519,32.5748228215052,-39.1142208333333));
#253749=CARTESIAN_POINT('Ctrl Pts',(42.1191763815623,31.5404524382925,-39.0558875));
#253750=CARTESIAN_POINT('Ctrl Pts',(42.7163704007519,30.5060820550798,-38.9975541666667));
#253751=CARTESIAN_POINT('Ctrl Pts',(43.3135644199415,29.4717116718671,-38.9392208333334));
#253752=CARTESIAN_POINT('Ctrl Pts',(44.5079524583208,29.4717116718671,-38.8808875));
#253753=CARTESIAN_POINT('Ctrl Pts',(45.7023404967,29.4717116718671,-38.8225541666667));
#253754=CARTESIAN_POINT('Ctrl Pts',(46.2995345158897,30.5060820550798,-38.7642208333333));
#253755=CARTESIAN_POINT('Ctrl Pts',(46.8967285350793,31.5404524382925,-38.7058875));
#253756=CARTESIAN_POINT('Ctrl Pts',(46.2995345158897,32.5748228215052,-38.6475541666667));
#253757=CARTESIAN_POINT('Ctrl Pts',(45.7023404967,33.6091932047179,-38.5892208333334));
#253758=CARTESIAN_POINT('Ctrl Pts',(44.5079524583208,33.6091932047179,-38.5308875));
#253759=CARTESIAN_POINT('Ctrl Pts',(43.3135644199415,33.6091932047179,-38.4725541666667));
#253760=CARTESIAN_POINT('Ctrl Pts',(42.7163704007519,32.5748228215052,-38.4142208333334));
#253761=CARTESIAN_POINT('Ctrl Pts',(42.1191763815623,31.5404524382925,-38.3558875));
#253762=CARTESIAN_POINT('Ctrl Pts',(42.7163704007519,30.5060820550798,-38.2975541666667));
#253763=CARTESIAN_POINT('Ctrl Pts',(43.3135644199415,29.4717116718671,-38.2392208333333));
#253764=CARTESIAN_POINT('Ctrl Pts',(44.5079524583208,29.4717116718671,-38.1808875));
#253765=CARTESIAN_POINT('Ctrl Pts',(45.7023404967,29.4717116718671,-38.1225541666667));
#253766=CARTESIAN_POINT('Ctrl Pts',(46.2995345158897,30.5060820550798,-38.0642208333334));
#253767=CARTESIAN_POINT('Ctrl Pts',(46.8967285350793,31.5404524382925,-38.0058875));
#253768=CARTESIAN_POINT('Ctrl Pts',(46.2995345158897,32.5748228215052,-37.9475541666667));
#253769=CARTESIAN_POINT('Ctrl Pts',(45.7023404967,33.6091932047179,-37.8892208333334));
#253770=CARTESIAN_POINT('Ctrl Pts',(44.5079524583208,33.6091932047179,-37.8308875));
#253771=CARTESIAN_POINT('Ctrl Pts',(43.3135644199415,33.6091932047179,-37.7725541666667));
#253772=CARTESIAN_POINT('Ctrl Pts',(42.7163704007519,32.5748228215052,-37.7142208333333));
#253773=CARTESIAN_POINT('Ctrl Pts',(42.1191763815623,31.5404524382925,-37.6558875));
#253774=CARTESIAN_POINT('Ctrl Pts',(42.7163704007519,30.5060820550798,-37.5975541666667));
#253775=CARTESIAN_POINT('Ctrl Pts',(43.3135644199415,29.4717116718671,-37.5392208333334));
#253776=CARTESIAN_POINT('Ctrl Pts',(44.5079524583208,29.4717116718671,-37.4808875));
#253777=CARTESIAN_POINT('Ctrl Pts',(45.7023404967,29.4717116718671,-37.4225541666667));
#253778=CARTESIAN_POINT('Ctrl Pts',(46.2995345158897,30.5060820550798,-37.3642208333333));
#253779=CARTESIAN_POINT('Ctrl Pts',(46.8967285350793,31.5404524382925,-37.3058875));
#253780=CARTESIAN_POINT('Ctrl Pts',(46.2995345158897,32.5748228215052,-37.2475541666667));
#253781=CARTESIAN_POINT('Ctrl Pts',(46.2219998538691,32.7091167954726,-37.239980655983));
#253782=CARTESIAN_POINT('Ctrl Pts',(46.1253112086366,32.8303512837246,-37.2318399189827));
#253783=CARTESIAN_POINT('',(44.6028101950443,33.5382023184728,-39.8960584192517));
#253784=CARTESIAN_POINT('Ctrl Pts',(44.5079524583207,29.5404524382925,-39.5412));
#253785=CARTESIAN_POINT('Ctrl Pts',(44.4819640599349,29.5404524382925,-39.5425128857704));
#253786=CARTESIAN_POINT('Ctrl Pts',(44.4559582185953,29.5409589821351,-39.5438414269218));
#253787=CARTESIAN_POINT('Ctrl Pts',(44.1649835932381,29.5523160589081,-39.5588721743436));
#253788=CARTESIAN_POINT('Ctrl Pts',(43.9047498818082,29.6152478208572,-39.5738542093599));
#253789=CARTESIAN_POINT('Ctrl Pts',(43.4288502962916,29.8366243048529,-39.6043525894344));
#253790=CARTESIAN_POINT('Ctrl Pts',(43.2168722113724,29.9910586609984,-39.6195656652062));
#253791=CARTESIAN_POINT('Ctrl Pts',(42.8673886165607,30.3685431738061,-39.648230894323));
#253792=CARTESIAN_POINT('Ctrl Pts',(42.7317086737687,30.5866318895618,-39.6605604679907));
#253793=CARTESIAN_POINT('Ctrl Pts',(42.5449531333681,31.0736341008157,-39.6889689303139));
#253794=CARTESIAN_POINT('Ctrl Pts',(42.5002450908835,31.3395359025595,-39.7044798687489));
#253795=CARTESIAN_POINT('Ctrl Pts',(42.5174955965406,31.8629669597781,-39.7350133470867));
#253796=CARTESIAN_POINT('Ctrl Pts',(42.5752997723599,32.1156243266577,-39.749751693488));
#253797=CARTESIAN_POINT('Ctrl Pts',(42.7849619712644,32.5889458204941,-39.7773621139617));
#253798=CARTESIAN_POINT('Ctrl Pts',(42.9362187959742,32.8044575732572,-39.7903324084612));
#253799=CARTESIAN_POINT('Ctrl Pts',(43.3150542526911,33.1672635258398,-39.8200523146249));
#253800=CARTESIAN_POINT('Ctrl Pts',(43.5396719441365,33.3101828782814,-39.8355680656421));
#253801=CARTESIAN_POINT('Ctrl Pts',(43.917558345171,33.4565640653462,-39.8589276382755));
#253802=CARTESIAN_POINT('Ctrl Pts',(44.0546632593971,33.4935486751892,-39.8669326424869));
#253803=CARTESIAN_POINT('Ctrl Pts',(44.3295436040989,33.5371640157393,-39.8820912026746));
#253804=CARTESIAN_POINT('Ctrl Pts',(44.4663202768198,33.5446825305706,-39.8889734415788));
#253805=CARTESIAN_POINT('Ctrl Pts',(44.602810202553,33.5382016738972,-39.8960576849095));
#253806=CARTESIAN_POINT('Ctrl Pts',(42.8533186609868,32.1498328366219,-39.6198492128429));
#253807=CARTESIAN_POINT('Ctrl Pts',(42.9050935173468,32.3330539516136,-39.6401425936059));
#253808=CARTESIAN_POINT('Ctrl Pts',(42.982691066735,32.5080524772143,-39.6607364267285));
#253809=CARTESIAN_POINT('Ctrl Pts',(43.2002172353721,32.8455798638486,-39.7078850703729));
#253810=CARTESIAN_POINT('Ctrl Pts',(43.3395359031206,32.9998044792065,-39.7334291314113));
#253811=CARTESIAN_POINT('Ctrl Pts',(43.648144630106,33.246187293655,-39.7824493941379));
#253812=CARTESIAN_POINT('Ctrl Pts',(43.812496663251,33.3413573589809,-39.8056860731073));
#253813=CARTESIAN_POINT('Ctrl Pts',(44.1843827211634,33.4874274508034,-39.8525699812779));
#253814=CARTESIAN_POINT('Ctrl Pts',(44.3929618843463,33.5311592418717,-39.8754000806208));
#253815=CARTESIAN_POINT('Ctrl Pts',(44.6028101816435,33.5382028669661,-39.8960583683639));
#253816=CARTESIAN_POINT('Ctrl Pts',(44.5079524583208,33.2091977213449,-52.99995));
#253817=CARTESIAN_POINT('Ctrl Pts',(43.5445019199415,33.2091977213449,-52.9416166666667));
#253818=CARTESIAN_POINT('Ctrl Pts',(43.0627766507519,32.3748250798187,-52.8832833333334));
#253819=CARTESIAN_POINT('Ctrl Pts',(42.5810513815623,31.5404524382925,-52.82495));
#253820=CARTESIAN_POINT('Ctrl Pts',(43.0627766507519,30.7060797967663,-52.7666166666667));
#253821=CARTESIAN_POINT('Ctrl Pts',(43.5445019199415,29.87170715524,-52.7082833333333));
#253822=CARTESIAN_POINT('Ctrl Pts',(44.5079524583208,29.87170715524,-52.64995));
#253823=CARTESIAN_POINT('Ctrl Pts',(45.4714029967,29.87170715524,-52.5916166666666));
#253824=CARTESIAN_POINT('Ctrl Pts',(45.9531282658897,30.7060797967663,-52.5332833333334));
#253825=CARTESIAN_POINT('Ctrl Pts',(46.4348535350793,31.5404524382925,-52.4749500000001));
#253826=CARTESIAN_POINT('Ctrl Pts',(45.9531282658897,32.3748250798187,-52.4166166666667));
#253827=CARTESIAN_POINT('Ctrl Pts',(45.4714029967,33.2091977213449,-52.3582833333334));
#253828=CARTESIAN_POINT('Ctrl Pts',(44.5079524583208,33.2091977213449,-52.29995));
#253829=CARTESIAN_POINT('Ctrl Pts',(43.5445019199415,33.2091977213449,-52.2416166666667));
#253830=CARTESIAN_POINT('Ctrl Pts',(43.0627766507519,32.3748250798187,-52.1832833333333));
#253831=CARTESIAN_POINT('Ctrl Pts',(42.5810513815623,31.5404524382925,-52.12495));
#253832=CARTESIAN_POINT('Ctrl Pts',(43.0627766507519,30.7060797967663,-52.0666166666667));
#253833=CARTESIAN_POINT('Ctrl Pts',(43.5445019199415,29.87170715524,-52.0082833333333));
#253834=CARTESIAN_POINT('Ctrl Pts',(44.5079524583208,29.87170715524,-51.94995));
#253835=CARTESIAN_POINT('Ctrl Pts',(45.4714029967,29.87170715524,-51.8916166666667));
#253836=CARTESIAN_POINT('Ctrl Pts',(45.9531282658897,30.7060797967663,-51.8332833333333));
#253837=CARTESIAN_POINT('Ctrl Pts',(46.4348535350793,31.5404524382925,-51.77495));
#253838=CARTESIAN_POINT('Ctrl Pts',(45.9531282658897,32.3748250798187,-51.7166166666667));
#253839=CARTESIAN_POINT('Ctrl Pts',(45.4714029967,33.2091977213449,-51.6582833333333));
#253840=CARTESIAN_POINT('Ctrl Pts',(44.5079524583208,33.2091977213449,-51.59995));
#253841=CARTESIAN_POINT('Ctrl Pts',(43.5445019199415,33.2091977213449,-51.5416166666667));
#253842=CARTESIAN_POINT('Ctrl Pts',(43.0627766507519,32.3748250798187,-51.4832833333333));
#253843=CARTESIAN_POINT('Ctrl Pts',(42.5810513815623,31.5404524382925,-51.42495));
#253844=CARTESIAN_POINT('Ctrl Pts',(43.0627766507519,30.7060797967663,-51.3666166666667));
#253845=CARTESIAN_POINT('Ctrl Pts',(43.5445019199415,29.87170715524,-51.3082833333333));
#253846=CARTESIAN_POINT('Ctrl Pts',(44.5079524583208,29.87170715524,-51.24995));
#253847=CARTESIAN_POINT('Ctrl Pts',(45.4714029967,29.87170715524,-51.1916166666667));
#253848=CARTESIAN_POINT('Ctrl Pts',(45.9531282658897,30.7060797967663,-51.1332833333333));
#253849=CARTESIAN_POINT('Ctrl Pts',(46.4348535350793,31.5404524382925,-51.07495));
#253850=CARTESIAN_POINT('Ctrl Pts',(45.9531282658897,32.3748250798187,-51.0166166666667));
#253851=CARTESIAN_POINT('Ctrl Pts',(45.4714029967,33.2091977213449,-50.9582833333334));
#253852=CARTESIAN_POINT('Ctrl Pts',(44.5079524583208,33.2091977213449,-50.89995));
#253853=CARTESIAN_POINT('Ctrl Pts',(43.5445019199415,33.2091977213449,-50.8416166666667));
#253854=CARTESIAN_POINT('Ctrl Pts',(43.0627766507519,32.3748250798187,-50.7832833333333));
#253855=CARTESIAN_POINT('Ctrl Pts',(42.5810513815623,31.5404524382925,-50.72495));
#253856=CARTESIAN_POINT('Ctrl Pts',(43.0627766507519,30.7060797967663,-50.6666166666667));
#253857=CARTESIAN_POINT('Ctrl Pts',(43.5445019199415,29.87170715524,-50.6082833333334));
#253858=CARTESIAN_POINT('Ctrl Pts',(44.5079524583208,29.87170715524,-50.54995));
#253859=CARTESIAN_POINT('Ctrl Pts',(45.4714029967,29.87170715524,-50.4916166666667));
#253860=CARTESIAN_POINT('Ctrl Pts',(45.9531282658897,30.7060797967663,-50.4332833333333));
#253861=CARTESIAN_POINT('Ctrl Pts',(46.4348535350793,31.5404524382925,-50.37495));
#253862=CARTESIAN_POINT('Ctrl Pts',(45.9531282658897,32.3748250798187,-50.3166166666667));
#253863=CARTESIAN_POINT('Ctrl Pts',(45.4714029967,33.2091977213449,-50.2582833333334));
#253864=CARTESIAN_POINT('Ctrl Pts',(44.5079524583208,33.2091977213449,-50.19995));
#253865=CARTESIAN_POINT('Ctrl Pts',(43.5445019199415,33.2091977213449,-50.1416166666667));
#253866=CARTESIAN_POINT('Ctrl Pts',(43.0627766507519,32.3748250798187,-50.0832833333333));
#253867=CARTESIAN_POINT('Ctrl Pts',(42.5810513815623,31.5404524382925,-50.02495));
#253868=CARTESIAN_POINT('Ctrl Pts',(43.0627766507519,30.7060797967663,-49.9666166666667));
#253869=CARTESIAN_POINT('Ctrl Pts',(43.5445019199415,29.87170715524,-49.9082833333334));
#253870=CARTESIAN_POINT('Ctrl Pts',(44.5079524583208,29.87170715524,-49.84995));
#253871=CARTESIAN_POINT('Ctrl Pts',(45.4714029967,29.87170715524,-49.7916166666667));
#253872=CARTESIAN_POINT('Ctrl Pts',(45.9531282658897,30.7060797967663,-49.7332833333333));
#253873=CARTESIAN_POINT('Ctrl Pts',(46.4348535350793,31.5404524382925,-49.67495));
#253874=CARTESIAN_POINT('Ctrl Pts',(45.9531282658897,32.3748250798187,-49.6166166666667));
#253875=CARTESIAN_POINT('Ctrl Pts',(45.4714029967,33.2091977213449,-49.5582833333334));
#253876=CARTESIAN_POINT('Ctrl Pts',(44.5079524583208,33.2091977213449,-49.49995));
#253877=CARTESIAN_POINT('Ctrl Pts',(43.5445019199415,33.2091977213449,-49.4416166666667));
#253878=CARTESIAN_POINT('Ctrl Pts',(43.0627766507519,32.3748250798187,-49.3832833333334));
#253879=CARTESIAN_POINT('Ctrl Pts',(42.5810513815623,31.5404524382925,-49.32495));
#253880=CARTESIAN_POINT('Ctrl Pts',(43.0627766507519,30.7060797967663,-49.2666166666667));
#253881=CARTESIAN_POINT('Ctrl Pts',(43.5445019199415,29.87170715524,-49.2082833333334));
#253882=CARTESIAN_POINT('Ctrl Pts',(44.5079524583208,29.87170715524,-49.14995));
#253883=CARTESIAN_POINT('Ctrl Pts',(45.4714029967,29.87170715524,-49.0916166666667));
#253884=CARTESIAN_POINT('Ctrl Pts',(45.9531282658897,30.7060797967663,-49.0332833333333));
#253885=CARTESIAN_POINT('Ctrl Pts',(46.4348535350793,31.5404524382925,-48.97495));
#253886=CARTESIAN_POINT('Ctrl Pts',(45.9531282658897,32.3748250798187,-48.9166166666667));
#253887=CARTESIAN_POINT('Ctrl Pts',(45.4714029967,33.2091977213449,-48.8582833333333));
#253888=CARTESIAN_POINT('Ctrl Pts',(44.5079524583208,33.2091977213449,-48.79995));
#253889=CARTESIAN_POINT('Ctrl Pts',(43.5445019199415,33.2091977213449,-48.7416166666667));
#253890=CARTESIAN_POINT('Ctrl Pts',(43.0627766507519,32.3748250798187,-48.6832833333333));
#253891=CARTESIAN_POINT('Ctrl Pts',(42.5810513815623,31.5404524382925,-48.62495));
#253892=CARTESIAN_POINT('Ctrl Pts',(43.0627766507519,30.7060797967663,-48.5666166666667));
#253893=CARTESIAN_POINT('Ctrl Pts',(43.5445019199415,29.87170715524,-48.5082833333333));
#253894=CARTESIAN_POINT('Ctrl Pts',(44.5079524583208,29.87170715524,-48.44995));
#253895=CARTESIAN_POINT('Ctrl Pts',(45.4714029967,29.87170715524,-48.3916166666667));
#253896=CARTESIAN_POINT('Ctrl Pts',(45.9531282658897,30.7060797967663,-48.3332833333333));
#253897=CARTESIAN_POINT('Ctrl Pts',(46.4348535350793,31.5404524382925,-48.27495));
#253898=CARTESIAN_POINT('Ctrl Pts',(45.9531282658897,32.3748250798187,-48.2166166666667));
#253899=CARTESIAN_POINT('Ctrl Pts',(45.4714029967,33.2091977213449,-48.1582833333333));
#253900=CARTESIAN_POINT('Ctrl Pts',(44.5079524583208,33.2091977213449,-48.09995));
#253901=CARTESIAN_POINT('Ctrl Pts',(43.5445019199415,33.2091977213449,-48.0416166666667));
#253902=CARTESIAN_POINT('Ctrl Pts',(43.0627766507519,32.3748250798187,-47.9832833333334));
#253903=CARTESIAN_POINT('Ctrl Pts',(42.5810513815623,31.5404524382925,-47.92495));
#253904=CARTESIAN_POINT('Ctrl Pts',(43.0627766507519,30.7060797967663,-47.8666166666667));
#253905=CARTESIAN_POINT('Ctrl Pts',(43.5445019199415,29.87170715524,-47.8082833333333));
#253906=CARTESIAN_POINT('Ctrl Pts',(44.5079524583208,29.87170715524,-47.74995));
#253907=CARTESIAN_POINT('Ctrl Pts',(45.4714029967,29.87170715524,-47.6916166666667));
#253908=CARTESIAN_POINT('Ctrl Pts',(45.9531282658897,30.7060797967663,-47.6332833333333));
#253909=CARTESIAN_POINT('Ctrl Pts',(46.4348535350793,31.5404524382925,-47.57495));
#253910=CARTESIAN_POINT('Ctrl Pts',(45.9531282658897,32.3748250798187,-47.5166166666667));
#253911=CARTESIAN_POINT('Ctrl Pts',(45.4714029967,33.2091977213449,-47.4582833333333));
#253912=CARTESIAN_POINT('Ctrl Pts',(44.5079524583208,33.2091977213449,-47.39995));
#253913=CARTESIAN_POINT('Ctrl Pts',(43.5445019199415,33.2091977213449,-47.3416166666666));
#253914=CARTESIAN_POINT('Ctrl Pts',(43.0627766507519,32.3748250798187,-47.2832833333333));
#253915=CARTESIAN_POINT('Ctrl Pts',(42.5810513815623,31.5404524382925,-47.22495));
#253916=CARTESIAN_POINT('Ctrl Pts',(43.0627766507519,30.7060797967663,-47.1666166666667));
#253917=CARTESIAN_POINT('Ctrl Pts',(43.5445019199415,29.87170715524,-47.1082833333333));
#253918=CARTESIAN_POINT('Ctrl Pts',(44.5079524583208,29.87170715524,-47.04995));
#253919=CARTESIAN_POINT('Ctrl Pts',(45.4714029967,29.87170715524,-46.9916166666667));
#253920=CARTESIAN_POINT('Ctrl Pts',(45.9531282658897,30.7060797967663,-46.9332833333333));
#253921=CARTESIAN_POINT('Ctrl Pts',(46.4348535350793,31.5404524382925,-46.87495));
#253922=CARTESIAN_POINT('Ctrl Pts',(45.9531282658897,32.3748250798187,-46.8166166666667));
#253923=CARTESIAN_POINT('Ctrl Pts',(45.4714029967,33.2091977213449,-46.7582833333333));
#253924=CARTESIAN_POINT('Ctrl Pts',(44.5079524583208,33.2091977213449,-46.69995));
#253925=CARTESIAN_POINT('Ctrl Pts',(43.5445019199415,33.2091977213449,-46.6416166666666));
#253926=CARTESIAN_POINT('Ctrl Pts',(43.0627766507519,32.3748250798187,-46.5832833333334));
#253927=CARTESIAN_POINT('Ctrl Pts',(42.5810513815623,31.5404524382925,-46.52495));
#253928=CARTESIAN_POINT('Ctrl Pts',(43.0627766507519,30.7060797967663,-46.4666166666667));
#253929=CARTESIAN_POINT('Ctrl Pts',(43.5445019199415,29.87170715524,-46.4082833333333));
#253930=CARTESIAN_POINT('Ctrl Pts',(44.5079524583208,29.87170715524,-46.34995));
#253931=CARTESIAN_POINT('Ctrl Pts',(45.4714029967,29.87170715524,-46.2916166666667));
#253932=CARTESIAN_POINT('Ctrl Pts',(45.9531282658897,30.7060797967663,-46.2332833333334));
#253933=CARTESIAN_POINT('Ctrl Pts',(46.4348535350793,31.5404524382925,-46.17495));
#253934=CARTESIAN_POINT('Ctrl Pts',(45.9531282658897,32.3748250798187,-46.1166166666667));
#253935=CARTESIAN_POINT('Ctrl Pts',(45.4714029967,33.2091977213449,-46.0582833333333));
#253936=CARTESIAN_POINT('Ctrl Pts',(44.5079524583208,33.2091977213449,-45.99995));
#253937=CARTESIAN_POINT('Ctrl Pts',(43.5445019199415,33.2091977213449,-45.9416166666667));
#253938=CARTESIAN_POINT('Ctrl Pts',(43.0627766507519,32.3748250798187,-45.8832833333333));
#253939=CARTESIAN_POINT('Ctrl Pts',(42.5810513815623,31.5404524382925,-45.82495));
#253940=CARTESIAN_POINT('Ctrl Pts',(43.0627766507519,30.7060797967663,-45.7666166666667));
#253941=CARTESIAN_POINT('Ctrl Pts',(43.5445019199415,29.87170715524,-45.7082833333333));
#253942=CARTESIAN_POINT('Ctrl Pts',(44.5079524583208,29.87170715524,-45.64995));
#253943=CARTESIAN_POINT('Ctrl Pts',(45.4714029967,29.87170715524,-45.5916166666667));
#253944=CARTESIAN_POINT('Ctrl Pts',(45.9531282658897,30.7060797967663,-45.5332833333333));
#253945=CARTESIAN_POINT('Ctrl Pts',(46.4348535350793,31.5404524382925,-45.47495));
#253946=CARTESIAN_POINT('Ctrl Pts',(45.9531282658897,32.3748250798187,-45.4166166666667));
#253947=CARTESIAN_POINT('Ctrl Pts',(45.4714029967,33.2091977213449,-45.3582833333333));
#253948=CARTESIAN_POINT('Ctrl Pts',(44.5079524583208,33.2091977213449,-45.29995));
#253949=CARTESIAN_POINT('Ctrl Pts',(43.5445019199415,33.2091977213449,-45.2416166666667));
#253950=CARTESIAN_POINT('Ctrl Pts',(43.0627766507519,32.3748250798187,-45.1832833333333));
#253951=CARTESIAN_POINT('Ctrl Pts',(42.5810513815623,31.5404524382925,-45.12495));
#253952=CARTESIAN_POINT('Ctrl Pts',(43.0627766507519,30.7060797967663,-45.0666166666667));
#253953=CARTESIAN_POINT('Ctrl Pts',(43.5445019199415,29.87170715524,-45.0082833333334));
#253954=CARTESIAN_POINT('Ctrl Pts',(44.5079524583208,29.87170715524,-44.94995));
#253955=CARTESIAN_POINT('Ctrl Pts',(45.4714029967,29.87170715524,-44.8916166666667));
#253956=CARTESIAN_POINT('Ctrl Pts',(45.9531282658897,30.7060797967663,-44.8332833333334));
#253957=CARTESIAN_POINT('Ctrl Pts',(46.4348535350793,31.5404524382925,-44.77495));
#253958=CARTESIAN_POINT('Ctrl Pts',(45.9531282658897,32.3748250798187,-44.7166166666667));
#253959=CARTESIAN_POINT('Ctrl Pts',(45.4714029967,33.2091977213449,-44.6582833333333));
#253960=CARTESIAN_POINT('Ctrl Pts',(44.5079524583208,33.2091977213449,-44.59995));
#253961=CARTESIAN_POINT('Ctrl Pts',(43.5445019199415,33.2091977213449,-44.5416166666667));
#253962=CARTESIAN_POINT('Ctrl Pts',(43.0627766507519,32.3748250798187,-44.4832833333334));
#253963=CARTESIAN_POINT('Ctrl Pts',(42.5810513815623,31.5404524382925,-44.42495));
#253964=CARTESIAN_POINT('Ctrl Pts',(43.0627766507519,30.7060797967663,-44.3666166666667));
#253965=CARTESIAN_POINT('Ctrl Pts',(43.5445019199415,29.87170715524,-44.3082833333334));
#253966=CARTESIAN_POINT('Ctrl Pts',(44.5079524583208,29.87170715524,-44.24995));
#253967=CARTESIAN_POINT('Ctrl Pts',(45.4714029967,29.87170715524,-44.1916166666667));
#253968=CARTESIAN_POINT('Ctrl Pts',(45.9531282658897,30.7060797967663,-44.1332833333334));
#253969=CARTESIAN_POINT('Ctrl Pts',(46.4348535350793,31.5404524382925,-44.07495));
#253970=CARTESIAN_POINT('Ctrl Pts',(45.9531282658897,32.3748250798187,-44.0166166666667));
#253971=CARTESIAN_POINT('Ctrl Pts',(45.4714029967,33.2091977213449,-43.9582833333334));
#253972=CARTESIAN_POINT('Ctrl Pts',(44.5079524583208,33.2091977213449,-43.89995));
#253973=CARTESIAN_POINT('Ctrl Pts',(43.5445019199415,33.2091977213449,-43.8416166666667));
#253974=CARTESIAN_POINT('Ctrl Pts',(43.0627766507519,32.3748250798187,-43.7832833333334));
#253975=CARTESIAN_POINT('Ctrl Pts',(42.5810513815623,31.5404524382925,-43.72495));
#253976=CARTESIAN_POINT('Ctrl Pts',(43.0627766507519,30.7060797967663,-43.6666166666667));
#253977=CARTESIAN_POINT('Ctrl Pts',(43.5445019199415,29.87170715524,-43.6082833333333));
#253978=CARTESIAN_POINT('Ctrl Pts',(44.5079524583208,29.87170715524,-43.54995));
#253979=CARTESIAN_POINT('Ctrl Pts',(45.4714029967,29.87170715524,-43.4916166666667));
#253980=CARTESIAN_POINT('Ctrl Pts',(45.9531282658897,30.7060797967663,-43.4332833333333));
#253981=CARTESIAN_POINT('Ctrl Pts',(46.4348535350793,31.5404524382925,-43.37495));
#253982=CARTESIAN_POINT('Ctrl Pts',(45.9531282658897,32.3748250798187,-43.3166166666667));
#253983=CARTESIAN_POINT('Ctrl Pts',(45.4714029967,33.2091977213449,-43.2582833333333));
#253984=CARTESIAN_POINT('Ctrl Pts',(44.5079524583208,33.2091977213449,-43.19995));
#253985=CARTESIAN_POINT('Ctrl Pts',(43.5445019199415,33.2091977213449,-43.1416166666666));
#253986=CARTESIAN_POINT('Ctrl Pts',(43.0627766507519,32.3748250798187,-43.0832833333333));
#253987=CARTESIAN_POINT('Ctrl Pts',(42.5810513815623,31.5404524382925,-43.02495));
#253988=CARTESIAN_POINT('Ctrl Pts',(43.0627766507519,30.7060797967663,-42.9666166666667));
#253989=CARTESIAN_POINT('Ctrl Pts',(43.5445019199415,29.87170715524,-42.9082833333333));
#253990=CARTESIAN_POINT('Ctrl Pts',(44.5079524583208,29.87170715524,-42.84995));
#253991=CARTESIAN_POINT('Ctrl Pts',(45.4714029967,29.87170715524,-42.7916166666667));
#253992=CARTESIAN_POINT('Ctrl Pts',(45.9531282658897,30.7060797967663,-42.7332833333334));
#253993=CARTESIAN_POINT('Ctrl Pts',(46.4348535350793,31.5404524382925,-42.67495));
#253994=CARTESIAN_POINT('Ctrl Pts',(45.9531282658897,32.3748250798187,-42.6166166666667));
#253995=CARTESIAN_POINT('Ctrl Pts',(45.4714029967,33.2091977213449,-42.5582833333333));
#253996=CARTESIAN_POINT('Ctrl Pts',(44.5079524583208,33.2091977213449,-42.49995));
#253997=CARTESIAN_POINT('Ctrl Pts',(43.5445019199415,33.2091977213449,-42.4416166666667));
#253998=CARTESIAN_POINT('Ctrl Pts',(43.0627766507519,32.3748250798187,-42.3832833333333));
#253999=CARTESIAN_POINT('Ctrl Pts',(42.5810513815623,31.5404524382925,-42.32495));
#254000=CARTESIAN_POINT('Ctrl Pts',(43.0627766507519,30.7060797967663,-42.2666166666667));
#254001=CARTESIAN_POINT('Ctrl Pts',(43.5445019199415,29.87170715524,-42.2082833333333));
#254002=CARTESIAN_POINT('Ctrl Pts',(44.5079524583208,29.87170715524,-42.14995));
#254003=CARTESIAN_POINT('Ctrl Pts',(45.4714029967,29.87170715524,-42.0916166666667));
#254004=CARTESIAN_POINT('Ctrl Pts',(45.9531282658897,30.7060797967663,-42.0332833333334));
#254005=CARTESIAN_POINT('Ctrl Pts',(46.4348535350793,31.5404524382925,-41.97495));
#254006=CARTESIAN_POINT('Ctrl Pts',(45.9531282658897,32.3748250798187,-41.9166166666666));
#254007=CARTESIAN_POINT('Ctrl Pts',(45.4714029967,33.2091977213449,-41.8582833333333));
#254008=CARTESIAN_POINT('Ctrl Pts',(44.5079524583208,33.2091977213449,-41.79995));
#254009=CARTESIAN_POINT('Ctrl Pts',(43.5445019199415,33.2091977213449,-41.7416166666667));
#254010=CARTESIAN_POINT('Ctrl Pts',(43.0627766507519,32.3748250798187,-41.6832833333333));
#254011=CARTESIAN_POINT('Ctrl Pts',(42.5810513815623,31.5404524382925,-41.62495));
#254012=CARTESIAN_POINT('Ctrl Pts',(43.0627766507519,30.7060797967663,-41.5666166666667));
#254013=CARTESIAN_POINT('Ctrl Pts',(43.5445019199415,29.87170715524,-41.5082833333334));
#254014=CARTESIAN_POINT('Ctrl Pts',(44.5079524583208,29.87170715524,-41.44995));
#254015=CARTESIAN_POINT('Ctrl Pts',(45.4714029967,29.87170715524,-41.3916166666667));
#254016=CARTESIAN_POINT('Ctrl Pts',(45.9531282658897,30.7060797967663,-41.3332833333334));
#254017=CARTESIAN_POINT('Ctrl Pts',(46.4348535350793,31.5404524382925,-41.27495));
#254018=CARTESIAN_POINT('Ctrl Pts',(45.9531282658897,32.3748250798187,-41.2166166666667));
#254019=CARTESIAN_POINT('Ctrl Pts',(45.4714029967,33.2091977213449,-41.1582833333333));
#254020=CARTESIAN_POINT('Ctrl Pts',(44.5079524583208,33.2091977213449,-41.09995));
#254021=CARTESIAN_POINT('Ctrl Pts',(43.5445019199415,33.2091977213449,-41.0416166666667));
#254022=CARTESIAN_POINT('Ctrl Pts',(43.0627766507519,32.3748250798187,-40.9832833333333));
#254023=CARTESIAN_POINT('Ctrl Pts',(42.5810513815623,31.5404524382925,-40.92495));
#254024=CARTESIAN_POINT('Ctrl Pts',(43.0627766507519,30.7060797967663,-40.8666166666667));
#254025=CARTESIAN_POINT('Ctrl Pts',(43.5445019199415,29.87170715524,-40.8082833333334));
#254026=CARTESIAN_POINT('Ctrl Pts',(44.5079524583208,29.87170715524,-40.74995));
#254027=CARTESIAN_POINT('Ctrl Pts',(45.4714029967,29.87170715524,-40.6916166666667));
#254028=CARTESIAN_POINT('Ctrl Pts',(45.9531282658897,30.7060797967663,-40.6332833333334));
#254029=CARTESIAN_POINT('Ctrl Pts',(46.4348535350793,31.5404524382925,-40.57495));
#254030=CARTESIAN_POINT('Ctrl Pts',(45.9531282658897,32.3748250798187,-40.5166166666666));
#254031=CARTESIAN_POINT('Ctrl Pts',(45.4714029967,33.2091977213449,-40.4582833333333));
#254032=CARTESIAN_POINT('Ctrl Pts',(44.5079524583208,33.2091977213449,-40.39995));
#254033=CARTESIAN_POINT('Ctrl Pts',(43.5445019199415,33.2091977213449,-40.3416166666667));
#254034=CARTESIAN_POINT('Ctrl Pts',(43.0627766507519,32.3748250798187,-40.2832833333334));
#254035=CARTESIAN_POINT('Ctrl Pts',(42.5810513815623,31.5404524382925,-40.22495));
#254036=CARTESIAN_POINT('Ctrl Pts',(43.0627766507519,30.7060797967663,-40.1666166666667));
#254037=CARTESIAN_POINT('Ctrl Pts',(43.5445019199415,29.87170715524,-40.1082833333334));
#254038=CARTESIAN_POINT('Ctrl Pts',(44.5079524583208,29.87170715524,-40.04995));
#254039=CARTESIAN_POINT('Ctrl Pts',(45.4714029967,29.87170715524,-39.9916166666667));
#254040=CARTESIAN_POINT('Ctrl Pts',(45.9531282658897,30.7060797967663,-39.9332833333333));
#254041=CARTESIAN_POINT('Ctrl Pts',(46.4348535350793,31.5404524382925,-39.87495));
#254042=CARTESIAN_POINT('Ctrl Pts',(45.9531282658897,32.3748250798187,-39.8166166666667));
#254043=CARTESIAN_POINT('Ctrl Pts',(45.4714029967,33.2091977213449,-39.7582833333334));
#254044=CARTESIAN_POINT('Ctrl Pts',(44.5079524583208,33.2091977213449,-39.69995));
#254045=CARTESIAN_POINT('Ctrl Pts',(43.5445019199415,33.2091977213449,-39.6416166666667));
#254046=CARTESIAN_POINT('Ctrl Pts',(43.0627766507519,32.3748250798187,-39.5832833333333));
#254047=CARTESIAN_POINT('Ctrl Pts',(42.5810513815623,31.5404524382925,-39.52495));
#254048=CARTESIAN_POINT('Ctrl Pts',(43.0627766507519,30.7060797967663,-39.4666166666667));
#254049=CARTESIAN_POINT('Ctrl Pts',(43.5445019199415,29.87170715524,-39.4082833333333));
#254050=CARTESIAN_POINT('Ctrl Pts',(44.5079524583208,29.87170715524,-39.34995));
#254051=CARTESIAN_POINT('Ctrl Pts',(45.4714029967,29.87170715524,-39.2916166666667));
#254052=CARTESIAN_POINT('Ctrl Pts',(45.9531282658897,30.7060797967663,-39.2332833333333));
#254053=CARTESIAN_POINT('Ctrl Pts',(46.4348535350793,31.5404524382925,-39.17495));
#254054=CARTESIAN_POINT('Ctrl Pts',(45.9531282658897,32.3748250798187,-39.1166166666667));
#254055=CARTESIAN_POINT('Ctrl Pts',(45.4714029967,33.2091977213449,-39.0582833333333));
#254056=CARTESIAN_POINT('Ctrl Pts',(44.5079524583208,33.2091977213449,-38.99995));
#254057=CARTESIAN_POINT('Ctrl Pts',(43.5445019199415,33.2091977213449,-38.9416166666667));
#254058=CARTESIAN_POINT('Ctrl Pts',(43.0627766507519,32.3748250798187,-38.8832833333334));
#254059=CARTESIAN_POINT('Ctrl Pts',(42.5810513815623,31.5404524382925,-38.82495));
#254060=CARTESIAN_POINT('Ctrl Pts',(43.0627766507519,30.7060797967663,-38.7666166666667));
#254061=CARTESIAN_POINT('Ctrl Pts',(43.5445019199415,29.87170715524,-38.7082833333333));
#254062=CARTESIAN_POINT('Ctrl Pts',(44.5079524583208,29.87170715524,-38.64995));
#254063=CARTESIAN_POINT('Ctrl Pts',(45.4714029967,29.87170715524,-38.5916166666667));
#254064=CARTESIAN_POINT('Ctrl Pts',(45.9531282658897,30.7060797967663,-38.5332833333334));
#254065=CARTESIAN_POINT('Ctrl Pts',(46.4348535350793,31.5404524382925,-38.47495));
#254066=CARTESIAN_POINT('Ctrl Pts',(45.9531282658897,32.3748250798187,-38.4166166666667));
#254067=CARTESIAN_POINT('Ctrl Pts',(45.4714029967,33.2091977213449,-38.3582833333333));
#254068=CARTESIAN_POINT('Ctrl Pts',(44.5079524583208,33.2091977213449,-38.29995));
#254069=CARTESIAN_POINT('Ctrl Pts',(43.5445019199415,33.2091977213449,-38.2416166666667));
#254070=CARTESIAN_POINT('Ctrl Pts',(43.0627766507519,32.3748250798187,-38.1832833333333));
#254071=CARTESIAN_POINT('Ctrl Pts',(42.5810513815623,31.5404524382925,-38.12495));
#254072=CARTESIAN_POINT('Ctrl Pts',(43.0627766507519,30.7060797967663,-38.0666166666667));
#254073=CARTESIAN_POINT('Ctrl Pts',(43.5445019199415,29.87170715524,-38.0082833333333));
#254074=CARTESIAN_POINT('Ctrl Pts',(44.5079524583208,29.87170715524,-37.94995));
#254075=CARTESIAN_POINT('Ctrl Pts',(45.4714029967,29.87170715524,-37.8916166666667));
#254076=CARTESIAN_POINT('Ctrl Pts',(45.9531282658897,30.7060797967663,-37.8332833333334));
#254077=CARTESIAN_POINT('Ctrl Pts',(46.4348535350793,31.5404524382925,-37.77495));
#254078=CARTESIAN_POINT('Ctrl Pts',(45.9531282658897,32.3748250798187,-37.7166166666667));
#254079=CARTESIAN_POINT('Ctrl Pts',(45.4714029967,33.2091977213449,-37.6582833333333));
#254080=CARTESIAN_POINT('Ctrl Pts',(44.5079524583208,33.2091977213449,-37.59995));
#254081=CARTESIAN_POINT('Ctrl Pts',(43.5445019199415,33.2091977213449,-37.5416166666667));
#254082=CARTESIAN_POINT('Ctrl Pts',(43.0627766507519,32.3748250798187,-37.4832833333334));
#254083=CARTESIAN_POINT('Ctrl Pts',(42.5810513815623,31.5404524382925,-37.42495));
#254084=CARTESIAN_POINT('Ctrl Pts',(43.0627766507519,30.7060797967663,-37.3666166666667));
#254085=CARTESIAN_POINT('Ctrl Pts',(43.5445019199415,29.87170715524,-37.3082833333333));
#254086=CARTESIAN_POINT('Ctrl Pts',(44.5079524583208,29.87170715524,-37.24995));
#254087=CARTESIAN_POINT('Ctrl Pts',(45.4714029967,29.87170715524,-37.1916166666667));
#254088=CARTESIAN_POINT('Ctrl Pts',(45.9531282658897,30.7060797967663,-37.1332833333334));
#254089=CARTESIAN_POINT('Ctrl Pts',(46.4348535350793,31.5404524382925,-37.07495));
#254090=CARTESIAN_POINT('Ctrl Pts',(45.9531282658897,32.3748250798187,-37.0166166666667));
#254091=CARTESIAN_POINT('Ctrl Pts',(45.8905850977848,32.4831530246427,-37.0090431559831));
#254092=CARTESIAN_POINT('Ctrl Pts',(45.8125914103809,32.5809465634453,-37.0009024189827));
#254093=CARTESIAN_POINT('Ctrl Pts',(44.5079524583208,33.6091932047179,-53.2308875));
#254094=CARTESIAN_POINT('Ctrl Pts',(43.3135644199415,33.6091932047179,-53.1725541666667));
#254095=CARTESIAN_POINT('Ctrl Pts',(42.7163704007519,32.5748228215052,-53.1142208333334));
#254096=CARTESIAN_POINT('Ctrl Pts',(42.1191763815623,31.5404524382925,-53.0558875000001));
#254097=CARTESIAN_POINT('Ctrl Pts',(42.7163704007519,30.5060820550798,-52.9975541666667));
#254098=CARTESIAN_POINT('Ctrl Pts',(43.3135644199415,29.4717116718671,-52.9392208333334));
#254099=CARTESIAN_POINT('Ctrl Pts',(44.5079524583208,29.4717116718671,-52.8808875));
#254100=CARTESIAN_POINT('Ctrl Pts',(45.7023404967,29.4717116718671,-52.8225541666667));
#254101=CARTESIAN_POINT('Ctrl Pts',(46.2995345158897,30.5060820550798,-52.7642208333334));
#254102=CARTESIAN_POINT('Ctrl Pts',(46.8967285350793,31.5404524382925,-52.7058875));
#254103=CARTESIAN_POINT('Ctrl Pts',(46.2995345158897,32.5748228215052,-52.6475541666667));
#254104=CARTESIAN_POINT('Ctrl Pts',(45.7023404967,33.6091932047179,-52.5892208333333));
#254105=CARTESIAN_POINT('Ctrl Pts',(44.5079524583208,33.6091932047179,-52.5308875));
#254106=CARTESIAN_POINT('Ctrl Pts',(43.3135644199415,33.6091932047179,-52.4725541666667));
#254107=CARTESIAN_POINT('Ctrl Pts',(42.7163704007519,32.5748228215052,-52.4142208333333));
#254108=CARTESIAN_POINT('Ctrl Pts',(42.1191763815623,31.5404524382925,-52.3558875000001));
#254109=CARTESIAN_POINT('Ctrl Pts',(42.7163704007519,30.5060820550798,-52.2975541666667));
#254110=CARTESIAN_POINT('Ctrl Pts',(43.3135644199415,29.4717116718671,-52.2392208333334));
#254111=CARTESIAN_POINT('Ctrl Pts',(44.5079524583208,29.4717116718671,-52.1808875));
#254112=CARTESIAN_POINT('Ctrl Pts',(45.7023404967,29.4717116718671,-52.1225541666667));
#254113=CARTESIAN_POINT('Ctrl Pts',(46.2995345158897,30.5060820550798,-52.0642208333334));
#254114=CARTESIAN_POINT('Ctrl Pts',(46.8967285350793,31.5404524382925,-52.0058875));
#254115=CARTESIAN_POINT('Ctrl Pts',(46.2995345158897,32.5748228215052,-51.9475541666667));
#254116=CARTESIAN_POINT('Ctrl Pts',(45.7023404967,33.6091932047179,-51.8892208333334));
#254117=CARTESIAN_POINT('Ctrl Pts',(44.5079524583208,33.6091932047179,-51.8308875));
#254118=CARTESIAN_POINT('Ctrl Pts',(43.3135644199415,33.6091932047179,-51.7725541666667));
#254119=CARTESIAN_POINT('Ctrl Pts',(42.7163704007519,32.5748228215052,-51.7142208333334));
#254120=CARTESIAN_POINT('Ctrl Pts',(42.1191763815623,31.5404524382925,-51.6558875));
#254121=CARTESIAN_POINT('Ctrl Pts',(42.7163704007519,30.5060820550798,-51.5975541666667));
#254122=CARTESIAN_POINT('Ctrl Pts',(43.3135644199415,29.4717116718671,-51.5392208333333));
#254123=CARTESIAN_POINT('Ctrl Pts',(44.5079524583208,29.4717116718671,-51.4808875));
#254124=CARTESIAN_POINT('Ctrl Pts',(45.7023404967,29.4717116718671,-51.4225541666667));
#254125=CARTESIAN_POINT('Ctrl Pts',(46.2995345158897,30.5060820550798,-51.3642208333334));
#254126=CARTESIAN_POINT('Ctrl Pts',(46.8967285350793,31.5404524382925,-51.3058875));
#254127=CARTESIAN_POINT('Ctrl Pts',(46.2995345158897,32.5748228215052,-51.2475541666667));
#254128=CARTESIAN_POINT('Ctrl Pts',(45.7023404967,33.6091932047179,-51.1892208333333));
#254129=CARTESIAN_POINT('Ctrl Pts',(44.5079524583208,33.6091932047179,-51.1308875));
#254130=CARTESIAN_POINT('Ctrl Pts',(43.3135644199415,33.6091932047179,-51.0725541666667));
#254131=CARTESIAN_POINT('Ctrl Pts',(42.7163704007519,32.5748228215052,-51.0142208333334));
#254132=CARTESIAN_POINT('Ctrl Pts',(42.1191763815623,31.5404524382925,-50.9558875));
#254133=CARTESIAN_POINT('Ctrl Pts',(42.7163704007519,30.5060820550798,-50.8975541666667));
#254134=CARTESIAN_POINT('Ctrl Pts',(43.3135644199415,29.4717116718671,-50.8392208333333));
#254135=CARTESIAN_POINT('Ctrl Pts',(44.5079524583208,29.4717116718671,-50.7808875));
#254136=CARTESIAN_POINT('Ctrl Pts',(45.7023404967,29.4717116718671,-50.7225541666666));
#254137=CARTESIAN_POINT('Ctrl Pts',(46.2995345158897,30.5060820550798,-50.6642208333333));
#254138=CARTESIAN_POINT('Ctrl Pts',(46.8967285350793,31.5404524382925,-50.6058875));
#254139=CARTESIAN_POINT('Ctrl Pts',(46.2995345158897,32.5748228215052,-50.5475541666667));
#254140=CARTESIAN_POINT('Ctrl Pts',(45.7023404967,33.6091932047179,-50.4892208333333));
#254141=CARTESIAN_POINT('Ctrl Pts',(44.5079524583208,33.6091932047179,-50.4308875));
#254142=CARTESIAN_POINT('Ctrl Pts',(43.3135644199415,33.6091932047179,-50.3725541666667));
#254143=CARTESIAN_POINT('Ctrl Pts',(42.7163704007519,32.5748228215052,-50.3142208333334));
#254144=CARTESIAN_POINT('Ctrl Pts',(42.1191763815623,31.5404524382925,-50.2558875));
#254145=CARTESIAN_POINT('Ctrl Pts',(42.7163704007519,30.5060820550798,-50.1975541666667));
#254146=CARTESIAN_POINT('Ctrl Pts',(43.3135644199415,29.4717116718671,-50.1392208333333));
#254147=CARTESIAN_POINT('Ctrl Pts',(44.5079524583208,29.4717116718671,-50.0808875));
#254148=CARTESIAN_POINT('Ctrl Pts',(45.7023404967,29.4717116718671,-50.0225541666667));
#254149=CARTESIAN_POINT('Ctrl Pts',(46.2995345158897,30.5060820550798,-49.9642208333334));
#254150=CARTESIAN_POINT('Ctrl Pts',(46.8967285350793,31.5404524382925,-49.9058875));
#254151=CARTESIAN_POINT('Ctrl Pts',(46.2995345158897,32.5748228215052,-49.8475541666667));
#254152=CARTESIAN_POINT('Ctrl Pts',(45.7023404967,33.6091932047179,-49.7892208333333));
#254153=CARTESIAN_POINT('Ctrl Pts',(44.5079524583208,33.6091932047179,-49.7308875));
#254154=CARTESIAN_POINT('Ctrl Pts',(43.3135644199415,33.6091932047179,-49.6725541666667));
#254155=CARTESIAN_POINT('Ctrl Pts',(42.7163704007519,32.5748228215052,-49.6142208333334));
#254156=CARTESIAN_POINT('Ctrl Pts',(42.1191763815623,31.5404524382925,-49.5558875));
#254157=CARTESIAN_POINT('Ctrl Pts',(42.7163704007519,30.5060820550798,-49.4975541666667));
#254158=CARTESIAN_POINT('Ctrl Pts',(43.3135644199415,29.4717116718671,-49.4392208333333));
#254159=CARTESIAN_POINT('Ctrl Pts',(44.5079524583208,29.4717116718671,-49.3808875));
#254160=CARTESIAN_POINT('Ctrl Pts',(45.7023404967,29.4717116718671,-49.3225541666667));
#254161=CARTESIAN_POINT('Ctrl Pts',(46.2995345158897,30.5060820550798,-49.2642208333334));
#254162=CARTESIAN_POINT('Ctrl Pts',(46.8967285350793,31.5404524382925,-49.2058875));
#254163=CARTESIAN_POINT('Ctrl Pts',(46.2995345158897,32.5748228215052,-49.1475541666667));
#254164=CARTESIAN_POINT('Ctrl Pts',(45.7023404967,33.6091932047179,-49.0892208333333));
#254165=CARTESIAN_POINT('Ctrl Pts',(44.5079524583208,33.6091932047179,-49.0308875));
#254166=CARTESIAN_POINT('Ctrl Pts',(43.3135644199415,33.6091932047179,-48.9725541666667));
#254167=CARTESIAN_POINT('Ctrl Pts',(42.7163704007519,32.5748228215052,-48.9142208333333));
#254168=CARTESIAN_POINT('Ctrl Pts',(42.1191763815623,31.5404524382925,-48.8558875));
#254169=CARTESIAN_POINT('Ctrl Pts',(42.7163704007519,30.5060820550798,-48.7975541666667));
#254170=CARTESIAN_POINT('Ctrl Pts',(43.3135644199415,29.4717116718671,-48.7392208333334));
#254171=CARTESIAN_POINT('Ctrl Pts',(44.5079524583208,29.4717116718671,-48.6808875));
#254172=CARTESIAN_POINT('Ctrl Pts',(45.7023404967,29.4717116718671,-48.6225541666667));
#254173=CARTESIAN_POINT('Ctrl Pts',(46.2995345158897,30.5060820550798,-48.5642208333334));
#254174=CARTESIAN_POINT('Ctrl Pts',(46.8967285350793,31.5404524382925,-48.5058875));
#254175=CARTESIAN_POINT('Ctrl Pts',(46.2995345158897,32.5748228215052,-48.4475541666667));
#254176=CARTESIAN_POINT('Ctrl Pts',(45.7023404967,33.6091932047179,-48.3892208333334));
#254177=CARTESIAN_POINT('Ctrl Pts',(44.5079524583208,33.6091932047179,-48.3308875));
#254178=CARTESIAN_POINT('Ctrl Pts',(43.3135644199415,33.6091932047179,-48.2725541666667));
#254179=CARTESIAN_POINT('Ctrl Pts',(42.7163704007519,32.5748228215052,-48.2142208333334));
#254180=CARTESIAN_POINT('Ctrl Pts',(42.1191763815623,31.5404524382925,-48.1558875));
#254181=CARTESIAN_POINT('Ctrl Pts',(42.7163704007519,30.5060820550798,-48.0975541666667));
#254182=CARTESIAN_POINT('Ctrl Pts',(43.3135644199415,29.4717116718671,-48.0392208333334));
#254183=CARTESIAN_POINT('Ctrl Pts',(44.5079524583208,29.4717116718671,-47.9808875));
#254184=CARTESIAN_POINT('Ctrl Pts',(45.7023404967,29.4717116718671,-47.9225541666667));
#254185=CARTESIAN_POINT('Ctrl Pts',(46.2995345158897,30.5060820550798,-47.8642208333334));
#254186=CARTESIAN_POINT('Ctrl Pts',(46.8967285350793,31.5404524382925,-47.8058875000001));
#254187=CARTESIAN_POINT('Ctrl Pts',(46.2995345158897,32.5748228215052,-47.7475541666667));
#254188=CARTESIAN_POINT('Ctrl Pts',(45.7023404967,33.6091932047179,-47.6892208333334));
#254189=CARTESIAN_POINT('Ctrl Pts',(44.5079524583208,33.6091932047179,-47.6308875));
#254190=CARTESIAN_POINT('Ctrl Pts',(43.3135644199415,33.6091932047179,-47.5725541666667));
#254191=CARTESIAN_POINT('Ctrl Pts',(42.7163704007519,32.5748228215052,-47.5142208333333));
#254192=CARTESIAN_POINT('Ctrl Pts',(42.1191763815623,31.5404524382925,-47.4558875));
#254193=CARTESIAN_POINT('Ctrl Pts',(42.7163704007519,30.5060820550798,-47.3975541666667));
#254194=CARTESIAN_POINT('Ctrl Pts',(43.3135644199415,29.4717116718671,-47.3392208333333));
#254195=CARTESIAN_POINT('Ctrl Pts',(44.5079524583208,29.4717116718671,-47.2808875));
#254196=CARTESIAN_POINT('Ctrl Pts',(45.7023404967,29.4717116718671,-47.2225541666667));
#254197=CARTESIAN_POINT('Ctrl Pts',(46.2995345158897,30.5060820550798,-47.1642208333334));
#254198=CARTESIAN_POINT('Ctrl Pts',(46.8967285350793,31.5404524382925,-47.1058875));
#254199=CARTESIAN_POINT('Ctrl Pts',(46.2995345158897,32.5748228215052,-47.0475541666667));
#254200=CARTESIAN_POINT('Ctrl Pts',(45.7023404967,33.6091932047179,-46.9892208333334));
#254201=CARTESIAN_POINT('Ctrl Pts',(44.5079524583208,33.6091932047179,-46.9308875));
#254202=CARTESIAN_POINT('Ctrl Pts',(43.3135644199415,33.6091932047179,-46.8725541666667));
#254203=CARTESIAN_POINT('Ctrl Pts',(42.7163704007519,32.5748228215052,-46.8142208333334));
#254204=CARTESIAN_POINT('Ctrl Pts',(42.1191763815623,31.5404524382925,-46.7558875));
#254205=CARTESIAN_POINT('Ctrl Pts',(42.7163704007519,30.5060820550798,-46.6975541666667));
#254206=CARTESIAN_POINT('Ctrl Pts',(43.3135644199415,29.4717116718671,-46.6392208333333));
#254207=CARTESIAN_POINT('Ctrl Pts',(44.5079524583208,29.4717116718671,-46.5808875));
#254208=CARTESIAN_POINT('Ctrl Pts',(45.7023404967,29.4717116718671,-46.5225541666667));
#254209=CARTESIAN_POINT('Ctrl Pts',(46.2995345158897,30.5060820550798,-46.4642208333334));
#254210=CARTESIAN_POINT('Ctrl Pts',(46.8967285350793,31.5404524382925,-46.4058875));
#254211=CARTESIAN_POINT('Ctrl Pts',(46.2995345158897,32.5748228215052,-46.3475541666667));
#254212=CARTESIAN_POINT('Ctrl Pts',(45.7023404967,33.6091932047179,-46.2892208333334));
#254213=CARTESIAN_POINT('Ctrl Pts',(44.5079524583208,33.6091932047179,-46.2308875));
#254214=CARTESIAN_POINT('Ctrl Pts',(43.3135644199415,33.6091932047179,-46.1725541666667));
#254215=CARTESIAN_POINT('Ctrl Pts',(42.7163704007519,32.5748228215052,-46.1142208333334));
#254216=CARTESIAN_POINT('Ctrl Pts',(42.1191763815623,31.5404524382925,-46.0558875));
#254217=CARTESIAN_POINT('Ctrl Pts',(42.7163704007519,30.5060820550798,-45.9975541666667));
#254218=CARTESIAN_POINT('Ctrl Pts',(43.3135644199415,29.4717116718671,-45.9392208333333));
#254219=CARTESIAN_POINT('Ctrl Pts',(44.5079524583208,29.4717116718671,-45.8808875));
#254220=CARTESIAN_POINT('Ctrl Pts',(45.7023404967,29.4717116718671,-45.8225541666667));
#254221=CARTESIAN_POINT('Ctrl Pts',(46.2995345158897,30.5060820550798,-45.7642208333334));
#254222=CARTESIAN_POINT('Ctrl Pts',(46.8967285350793,31.5404524382925,-45.7058875));
#254223=CARTESIAN_POINT('Ctrl Pts',(46.2995345158897,32.5748228215052,-45.6475541666667));
#254224=CARTESIAN_POINT('Ctrl Pts',(45.7023404967,33.6091932047179,-45.5892208333333));
#254225=CARTESIAN_POINT('Ctrl Pts',(44.5079524583208,33.6091932047179,-45.5308875));
#254226=CARTESIAN_POINT('Ctrl Pts',(43.3135644199415,33.6091932047179,-45.4725541666667));
#254227=CARTESIAN_POINT('Ctrl Pts',(42.7163704007519,32.5748228215052,-45.4142208333334));
#254228=CARTESIAN_POINT('Ctrl Pts',(42.1191763815623,31.5404524382925,-45.3558875));
#254229=CARTESIAN_POINT('Ctrl Pts',(42.7163704007519,30.5060820550798,-45.2975541666667));
#254230=CARTESIAN_POINT('Ctrl Pts',(43.3135644199415,29.4717116718671,-45.2392208333333));
#254231=CARTESIAN_POINT('Ctrl Pts',(44.5079524583208,29.4717116718671,-45.1808875));
#254232=CARTESIAN_POINT('Ctrl Pts',(45.7023404967,29.4717116718671,-45.1225541666667));
#254233=CARTESIAN_POINT('Ctrl Pts',(46.2995345158897,30.5060820550798,-45.0642208333334));
#254234=CARTESIAN_POINT('Ctrl Pts',(46.8967285350793,31.5404524382925,-45.0058875));
#254235=CARTESIAN_POINT('Ctrl Pts',(46.2995345158897,32.5748228215052,-44.9475541666667));
#254236=CARTESIAN_POINT('Ctrl Pts',(45.7023404967,33.6091932047179,-44.8892208333333));
#254237=CARTESIAN_POINT('Ctrl Pts',(44.5079524583208,33.6091932047179,-44.8308875));
#254238=CARTESIAN_POINT('Ctrl Pts',(43.3135644199415,33.6091932047179,-44.7725541666666));
#254239=CARTESIAN_POINT('Ctrl Pts',(42.7163704007519,32.5748228215052,-44.7142208333334));
#254240=CARTESIAN_POINT('Ctrl Pts',(42.1191763815623,31.5404524382925,-44.6558875));
#254241=CARTESIAN_POINT('Ctrl Pts',(42.7163704007519,30.5060820550798,-44.5975541666667));
#254242=CARTESIAN_POINT('Ctrl Pts',(43.3135644199415,29.4717116718671,-44.5392208333333));
#254243=CARTESIAN_POINT('Ctrl Pts',(44.5079524583208,29.4717116718671,-44.4808875));
#254244=CARTESIAN_POINT('Ctrl Pts',(45.7023404967,29.4717116718671,-44.4225541666667));
#254245=CARTESIAN_POINT('Ctrl Pts',(46.2995345158897,30.5060820550798,-44.3642208333333));
#254246=CARTESIAN_POINT('Ctrl Pts',(46.8967285350793,31.5404524382925,-44.3058875));
#254247=CARTESIAN_POINT('Ctrl Pts',(46.2995345158897,32.5748228215052,-44.2475541666667));
#254248=CARTESIAN_POINT('Ctrl Pts',(45.7023404967,33.6091932047179,-44.1892208333334));
#254249=CARTESIAN_POINT('Ctrl Pts',(44.5079524583208,33.6091932047179,-44.1308875));
#254250=CARTESIAN_POINT('Ctrl Pts',(43.3135644199415,33.6091932047179,-44.0725541666667));
#254251=CARTESIAN_POINT('Ctrl Pts',(42.7163704007519,32.5748228215052,-44.0142208333334));
#254252=CARTESIAN_POINT('Ctrl Pts',(42.1191763815623,31.5404524382925,-43.9558875));
#254253=CARTESIAN_POINT('Ctrl Pts',(42.7163704007519,30.5060820550798,-43.8975541666667));
#254254=CARTESIAN_POINT('Ctrl Pts',(43.3135644199415,29.4717116718671,-43.8392208333333));
#254255=CARTESIAN_POINT('Ctrl Pts',(44.5079524583208,29.4717116718671,-43.7808875));
#254256=CARTESIAN_POINT('Ctrl Pts',(45.7023404967,29.4717116718671,-43.7225541666667));
#254257=CARTESIAN_POINT('Ctrl Pts',(46.2995345158897,30.5060820550798,-43.6642208333334));
#254258=CARTESIAN_POINT('Ctrl Pts',(46.8967285350793,31.5404524382925,-43.6058875));
#254259=CARTESIAN_POINT('Ctrl Pts',(46.2995345158897,32.5748228215052,-43.5475541666667));
#254260=CARTESIAN_POINT('Ctrl Pts',(45.7023404967,33.6091932047179,-43.4892208333333));
#254261=CARTESIAN_POINT('Ctrl Pts',(44.5079524583208,33.6091932047179,-43.4308875));
#254262=CARTESIAN_POINT('Ctrl Pts',(43.3135644199415,33.6091932047179,-43.3725541666667));
#254263=CARTESIAN_POINT('Ctrl Pts',(42.7163704007519,32.5748228215052,-43.3142208333334));
#254264=CARTESIAN_POINT('Ctrl Pts',(42.1191763815623,31.5404524382925,-43.2558875));
#254265=CARTESIAN_POINT('Ctrl Pts',(42.7163704007519,30.5060820550798,-43.1975541666667));
#254266=CARTESIAN_POINT('Ctrl Pts',(43.3135644199415,29.4717116718671,-43.1392208333334));
#254267=CARTESIAN_POINT('Ctrl Pts',(44.5079524583208,29.4717116718671,-43.0808875));
#254268=CARTESIAN_POINT('Ctrl Pts',(45.7023404967,29.4717116718671,-43.0225541666667));
#254269=CARTESIAN_POINT('Ctrl Pts',(46.2995345158897,30.5060820550798,-42.9642208333334));
#254270=CARTESIAN_POINT('Ctrl Pts',(46.8967285350793,31.5404524382925,-42.9058875));
#254271=CARTESIAN_POINT('Ctrl Pts',(46.2995345158897,32.5748228215052,-42.8475541666667));
#254272=CARTESIAN_POINT('Ctrl Pts',(45.7023404967,33.6091932047179,-42.7892208333334));
#254273=CARTESIAN_POINT('Ctrl Pts',(44.5079524583208,33.6091932047179,-42.7308875));
#254274=CARTESIAN_POINT('Ctrl Pts',(43.3135644199415,33.6091932047179,-42.6725541666667));
#254275=CARTESIAN_POINT('Ctrl Pts',(42.7163704007519,32.5748228215052,-42.6142208333334));
#254276=CARTESIAN_POINT('Ctrl Pts',(42.1191763815623,31.5404524382925,-42.5558875));
#254277=CARTESIAN_POINT('Ctrl Pts',(42.7163704007519,30.5060820550798,-42.4975541666667));
#254278=CARTESIAN_POINT('Ctrl Pts',(43.3135644199415,29.4717116718671,-42.4392208333334));
#254279=CARTESIAN_POINT('Ctrl Pts',(44.5079524583208,29.4717116718671,-42.3808875));
#254280=CARTESIAN_POINT('Ctrl Pts',(45.7023404967,29.4717116718671,-42.3225541666667));
#254281=CARTESIAN_POINT('Ctrl Pts',(46.2995345158897,30.5060820550798,-42.2642208333334));
#254282=CARTESIAN_POINT('Ctrl Pts',(46.8967285350793,31.5404524382925,-42.2058875));
#254283=CARTESIAN_POINT('Ctrl Pts',(46.2995345158897,32.5748228215052,-42.1475541666667));
#254284=CARTESIAN_POINT('Ctrl Pts',(45.7023404967,33.6091932047179,-42.0892208333333));
#254285=CARTESIAN_POINT('Ctrl Pts',(44.5079524583208,33.6091932047179,-42.0308875));
#254286=CARTESIAN_POINT('Ctrl Pts',(43.3135644199415,33.6091932047179,-41.9725541666667));
#254287=CARTESIAN_POINT('Ctrl Pts',(42.7163704007519,32.5748228215052,-41.9142208333334));
#254288=CARTESIAN_POINT('Ctrl Pts',(42.1191763815623,31.5404524382925,-41.8558875));
#254289=CARTESIAN_POINT('Ctrl Pts',(42.7163704007519,30.5060820550798,-41.7975541666667));
#254290=CARTESIAN_POINT('Ctrl Pts',(43.3135644199415,29.4717116718671,-41.7392208333333));
#254291=CARTESIAN_POINT('Ctrl Pts',(44.5079524583208,29.4717116718671,-41.6808875));
#254292=CARTESIAN_POINT('Ctrl Pts',(45.7023404967,29.4717116718671,-41.6225541666667));
#254293=CARTESIAN_POINT('Ctrl Pts',(46.2995345158897,30.5060820550798,-41.5642208333334));
#254294=CARTESIAN_POINT('Ctrl Pts',(46.8967285350793,31.5404524382925,-41.5058875));
#254295=CARTESIAN_POINT('Ctrl Pts',(46.2995345158897,32.5748228215052,-41.4475541666667));
#254296=CARTESIAN_POINT('Ctrl Pts',(45.7023404967,33.6091932047179,-41.3892208333333));
#254297=CARTESIAN_POINT('Ctrl Pts',(44.5079524583208,33.6091932047179,-41.3308875));
#254298=CARTESIAN_POINT('Ctrl Pts',(43.3135644199415,33.6091932047179,-41.2725541666667));
#254299=CARTESIAN_POINT('Ctrl Pts',(42.7163704007519,32.5748228215052,-41.2142208333333));
#254300=CARTESIAN_POINT('Ctrl Pts',(42.1191763815623,31.5404524382925,-41.1558875));
#254301=CARTESIAN_POINT('Ctrl Pts',(42.7163704007519,30.5060820550798,-41.0975541666667));
#254302=CARTESIAN_POINT('Ctrl Pts',(43.3135644199415,29.4717116718671,-41.0392208333333));
#254303=CARTESIAN_POINT('Ctrl Pts',(44.5079524583208,29.4717116718671,-40.9808875));
#254304=CARTESIAN_POINT('Ctrl Pts',(45.7023404967,29.4717116718671,-40.9225541666667));
#254305=CARTESIAN_POINT('Ctrl Pts',(46.2995345158897,30.5060820550798,-40.8642208333334));
#254306=CARTESIAN_POINT('Ctrl Pts',(46.8967285350793,31.5404524382925,-40.8058875));
#254307=CARTESIAN_POINT('Ctrl Pts',(46.2995345158897,32.5748228215052,-40.7475541666667));
#254308=CARTESIAN_POINT('Ctrl Pts',(45.7023404967,33.6091932047179,-40.6892208333333));
#254309=CARTESIAN_POINT('Ctrl Pts',(44.5079524583208,33.6091932047179,-40.6308875));
#254310=CARTESIAN_POINT('Ctrl Pts',(43.3135644199415,33.6091932047179,-40.5725541666667));
#254311=CARTESIAN_POINT('Ctrl Pts',(42.7163704007519,32.5748228215052,-40.5142208333333));
#254312=CARTESIAN_POINT('Ctrl Pts',(42.1191763815623,31.5404524382925,-40.4558875));
#254313=CARTESIAN_POINT('Ctrl Pts',(42.7163704007519,30.5060820550798,-40.3975541666667));
#254314=CARTESIAN_POINT('Ctrl Pts',(43.3135644199415,29.4717116718671,-40.3392208333333));
#254315=CARTESIAN_POINT('Ctrl Pts',(44.5079524583208,29.4717116718671,-40.2808875));
#254316=CARTESIAN_POINT('Ctrl Pts',(45.7023404967,29.4717116718671,-40.2225541666667));
#254317=CARTESIAN_POINT('Ctrl Pts',(46.2995345158897,30.5060820550798,-40.1642208333333));
#254318=CARTESIAN_POINT('Ctrl Pts',(46.8967285350793,31.5404524382925,-40.1058875));
#254319=CARTESIAN_POINT('Ctrl Pts',(46.2995345158897,32.5748228215052,-40.0475541666667));
#254320=CARTESIAN_POINT('Ctrl Pts',(45.7023404967,33.6091932047179,-39.9892208333333));
#254321=CARTESIAN_POINT('Ctrl Pts',(44.5079524583208,33.6091932047179,-39.9308875));
#254322=CARTESIAN_POINT('Ctrl Pts',(43.3135644199415,33.6091932047179,-39.8725541666667));
#254323=CARTESIAN_POINT('Ctrl Pts',(42.7163704007519,32.5748228215052,-39.8142208333334));
#254324=CARTESIAN_POINT('Ctrl Pts',(42.1191763815623,31.5404524382925,-39.7558875));
#254325=CARTESIAN_POINT('Ctrl Pts',(42.7163704007519,30.5060820550798,-39.6975541666667));
#254326=CARTESIAN_POINT('Ctrl Pts',(43.3135644199415,29.4717116718671,-39.6392208333334));
#254327=CARTESIAN_POINT('Ctrl Pts',(44.5079524583208,29.4717116718671,-39.5808875));
#254328=CARTESIAN_POINT('Ctrl Pts',(45.7023404967,29.4717116718671,-39.5225541666667));
#254329=CARTESIAN_POINT('Ctrl Pts',(46.2995345158897,30.5060820550798,-39.4642208333333));
#254330=CARTESIAN_POINT('Ctrl Pts',(46.8967285350793,31.5404524382925,-39.4058875));
#254331=CARTESIAN_POINT('Ctrl Pts',(46.2995345158897,32.5748228215052,-39.3475541666667));
#254332=CARTESIAN_POINT('Ctrl Pts',(45.7023404967,33.6091932047179,-39.2892208333334));
#254333=CARTESIAN_POINT('Ctrl Pts',(44.5079524583208,33.6091932047179,-39.2308875));
#254334=CARTESIAN_POINT('Ctrl Pts',(43.3135644199415,33.6091932047179,-39.1725541666667));
#254335=CARTESIAN_POINT('Ctrl Pts',(42.7163704007519,32.5748228215052,-39.1142208333333));
#254336=CARTESIAN_POINT('Ctrl Pts',(42.1191763815623,31.5404524382925,-39.0558875));
#254337=CARTESIAN_POINT('Ctrl Pts',(42.7163704007519,30.5060820550798,-38.9975541666667));
#254338=CARTESIAN_POINT('Ctrl Pts',(43.3135644199415,29.4717116718671,-38.9392208333334));
#254339=CARTESIAN_POINT('Ctrl Pts',(44.5079524583208,29.4717116718671,-38.8808875));
#254340=CARTESIAN_POINT('Ctrl Pts',(45.7023404967,29.4717116718671,-38.8225541666667));
#254341=CARTESIAN_POINT('Ctrl Pts',(46.2995345158897,30.5060820550798,-38.7642208333333));
#254342=CARTESIAN_POINT('Ctrl Pts',(46.8967285350793,31.5404524382925,-38.7058875));
#254343=CARTESIAN_POINT('Ctrl Pts',(46.2995345158897,32.5748228215052,-38.6475541666667));
#254344=CARTESIAN_POINT('Ctrl Pts',(45.7023404967,33.6091932047179,-38.5892208333334));
#254345=CARTESIAN_POINT('Ctrl Pts',(44.5079524583208,33.6091932047179,-38.5308875));
#254346=CARTESIAN_POINT('Ctrl Pts',(43.3135644199415,33.6091932047179,-38.4725541666667));
#254347=CARTESIAN_POINT('Ctrl Pts',(42.7163704007519,32.5748228215052,-38.4142208333334));
#254348=CARTESIAN_POINT('Ctrl Pts',(42.1191763815623,31.5404524382925,-38.3558875));
#254349=CARTESIAN_POINT('Ctrl Pts',(42.7163704007519,30.5060820550798,-38.2975541666667));
#254350=CARTESIAN_POINT('Ctrl Pts',(43.3135644199415,29.4717116718671,-38.2392208333333));
#254351=CARTESIAN_POINT('Ctrl Pts',(44.5079524583208,29.4717116718671,-38.1808875));
#254352=CARTESIAN_POINT('Ctrl Pts',(45.7023404967,29.4717116718671,-38.1225541666667));
#254353=CARTESIAN_POINT('Ctrl Pts',(46.2995345158897,30.5060820550798,-38.0642208333334));
#254354=CARTESIAN_POINT('Ctrl Pts',(46.8967285350793,31.5404524382925,-38.0058875));
#254355=CARTESIAN_POINT('Ctrl Pts',(46.2995345158897,32.5748228215052,-37.9475541666667));
#254356=CARTESIAN_POINT('Ctrl Pts',(45.7023404967,33.6091932047179,-37.8892208333334));
#254357=CARTESIAN_POINT('Ctrl Pts',(44.5079524583208,33.6091932047179,-37.8308875));
#254358=CARTESIAN_POINT('Ctrl Pts',(43.3135644199415,33.6091932047179,-37.7725541666667));
#254359=CARTESIAN_POINT('Ctrl Pts',(42.7163704007519,32.5748228215052,-37.7142208333333));
#254360=CARTESIAN_POINT('Ctrl Pts',(42.1191763815623,31.5404524382925,-37.6558875));
#254361=CARTESIAN_POINT('Ctrl Pts',(42.7163704007519,30.5060820550798,-37.5975541666667));
#254362=CARTESIAN_POINT('Ctrl Pts',(43.3135644199415,29.4717116718671,-37.5392208333334));
#254363=CARTESIAN_POINT('Ctrl Pts',(44.5079524583208,29.4717116718671,-37.4808875));
#254364=CARTESIAN_POINT('Ctrl Pts',(45.7023404967,29.4717116718671,-37.4225541666667));
#254365=CARTESIAN_POINT('Ctrl Pts',(46.2995345158897,30.5060820550798,-37.3642208333333));
#254366=CARTESIAN_POINT('Ctrl Pts',(46.8967285350793,31.5404524382925,-37.3058875));
#254367=CARTESIAN_POINT('Ctrl Pts',(46.2995345158897,32.5748228215052,-37.2475541666667));
#254368=CARTESIAN_POINT('Ctrl Pts',(46.2219998538691,32.7091167954726,-37.239980655983));
#254369=CARTESIAN_POINT('Ctrl Pts',(46.1253112086366,32.8303512837246,-37.2318399189827));
#254370=CARTESIAN_POINT('Ctrl Pts',(44.5079524583208,29.87170715524,-52.64995));
#254371=CARTESIAN_POINT('Ctrl Pts',(44.6656844499377,29.8551659258425,-52.64995));
#254372=CARTESIAN_POINT('Ctrl Pts',(44.8248930522266,29.859971256401,-52.64995));
#254373=CARTESIAN_POINT('Ctrl Pts',(45.1318235221548,29.9111573974697,-52.64995));
#254374=CARTESIAN_POINT('Ctrl Pts',(45.2783921862532,29.9557286678636,-52.64995));
#254375=CARTESIAN_POINT('Ctrl Pts',(45.6136601602179,30.1075367973101,-52.64995));
#254376=CARTESIAN_POINT('Ctrl Pts',(45.7919027673363,30.2317049318369,-52.64995));
#254377=CARTESIAN_POINT('Ctrl Pts',(46.142958313814,30.586793325784,-52.64995));
#254378=CARTESIAN_POINT('Ctrl Pts',(46.263796418765,30.8067269086716,-52.64995));
#254379=CARTESIAN_POINT('Ctrl Pts',(46.3921330992279,31.1120088134361,-52.64995));
#254380=CARTESIAN_POINT('Ctrl Pts',(46.4329712831975,31.2494771622503,-52.64995));
#254381=CARTESIAN_POINT('Ctrl Pts',(46.4841685595433,31.5316010230531,-52.64995));
#254382=CARTESIAN_POINT('Ctrl Pts',(46.4942078616458,31.6754009245257,-52.64995));
#254383=CARTESIAN_POINT('Ctrl Pts',(46.4884569292028,31.8190238668641,-52.64995));
#254384=CARTESIAN_POINT('Ctrl Pts',(46.0995611578475,30.7936217551105,-39.9761074628063));
#254385=CARTESIAN_POINT('Ctrl Pts',(46.0446831314069,30.7141759297788,-39.9726297030245));
#254386=CARTESIAN_POINT('Ctrl Pts',(45.9828153631749,30.6382127772846,-39.9689296509816));
#254387=CARTESIAN_POINT('Ctrl Pts',(45.8549789121757,30.5059161072079,-39.9628399295649));
#254388=CARTESIAN_POINT('Ctrl Pts',(45.7905370337022,30.4483633401059,-39.9602898047892));
#254389=CARTESIAN_POINT('Ctrl Pts',(45.7222548898542,30.3958213079794,-39.958107375254));
#254390=CARTESIAN_POINT('Ctrl Pts',(46.2910030640114,32.4463942341858,-40.0133533952396));
#254391=CARTESIAN_POINT('Ctrl Pts',(46.3764819107672,32.2781570359765,-40.0231672318018));
#254392=CARTESIAN_POINT('Ctrl Pts',(46.4377090636024,32.0986904899845,-40.0336361136513));
#254393=CARTESIAN_POINT('Ctrl Pts',(46.5090199982574,31.7229223169541,-40.0555559237447));
#254394=CARTESIAN_POINT('Ctrl Pts',(46.5172843967059,31.5282582026595,-40.0669113304119));
#254395=CARTESIAN_POINT('Ctrl Pts',(46.4702537911306,31.0718097984373,-40.0935374873249));
#254396=CARTESIAN_POINT('Ctrl Pts',(46.3909400941642,30.8161183615257,-40.1084528211447));
#254397=CARTESIAN_POINT('Ctrl Pts',(46.1427211482668,30.3607052140246,-40.1350185880823));
#254398=CARTESIAN_POINT('Ctrl Pts',(45.9801328439062,30.1631221897528,-40.1486669714983));
#254399=CARTESIAN_POINT('Ctrl Pts',(45.582272314324,29.8330739088149,-40.1783925570296));
#254400=CARTESIAN_POINT('Ctrl Pts',(45.3484458708397,29.7066366803743,-40.1938927885336));
#254401=CARTESIAN_POINT('Ctrl Pts',(44.9057198187658,29.5702291161657,-40.2202370429571));
#254402=CARTESIAN_POINT('Ctrl Pts',(44.707236793135,29.5404524382924,-40.2311325243694));
#254403=CARTESIAN_POINT('Ctrl Pts',(44.5079524583204,29.5404524382925,-40.2412));
#254404=CARTESIAN_POINT('Origin',(-44.5079524583208,31.5404524382925,235.35105));
#254405=CARTESIAN_POINT('',(-42.526443553871,31.2691191501876,-39.0141960261087));
#254406=CARTESIAN_POINT('',(-45.1065106637223,29.6321218916505,-39.2098644727505));
#254407=CARTESIAN_POINT('Ctrl Pts',(-42.5264433182785,31.2691190101349,
-39.0141952067154));
#254408=CARTESIAN_POINT('Ctrl Pts',(-42.5265992442052,31.2679804248256,
-39.013990016886));
#254409=CARTESIAN_POINT('Ctrl Pts',(-42.5267561298879,31.2668421931591,
-39.0137850971281));
#254410=CARTESIAN_POINT('Ctrl Pts',(-42.5269139699439,31.2657043581003,
-39.0135804553152));
#254411=CARTESIAN_POINT('Ctrl Pts',(-42.5314450660311,31.2330406596962,
-39.0077058266447));
#254412=CARTESIAN_POINT('Ctrl Pts',(-42.5367737540441,31.2005503855788,
-39.0020305783833));
#254413=CARTESIAN_POINT('Ctrl Pts',(-42.5428860897467,31.1682775236366,
-38.9965616542392));
#254414=CARTESIAN_POINT('Ctrl Pts',(-42.5489984254493,31.1360046616943,
-38.991092730095));
#254415=CARTESIAN_POINT('Ctrl Pts',(-42.555895594383,31.1039336351222,-38.9858271285204));
#254416=CARTESIAN_POINT('Ctrl Pts',(-42.5635729908238,31.0720631916436,
-38.9807642570009));
#254417=CARTESIAN_POINT('Ctrl Pts',(-42.5712503872647,31.040192748165,-38.9757013854813));
#254418=CARTESIAN_POINT('Ctrl Pts',(-42.5797080184842,31.0085228897363,
-38.9708412451465));
#254419=CARTESIAN_POINT('Ctrl Pts',(-42.5889469834378,30.9770538339552,
-38.9661846965336));
#254420=CARTESIAN_POINT('Ctrl Pts',(-42.5981859483915,30.9455847781742,
-38.9615281479207));
#254421=CARTESIAN_POINT('Ctrl Pts',(-42.60820623098,30.9143165209769,-38.957075186193));
#254422=CARTESIAN_POINT('Ctrl Pts',(-42.619014674011,30.8832507591964,-38.9528281414074));
#254423=CARTESIAN_POINT('Ctrl Pts',(-42.6298231170419,30.8521849974158,
-38.9485810966219));
#254424=CARTESIAN_POINT('Ctrl Pts',(-42.6414196796478,30.8213217206122,
-38.9445399575805));
#254425=CARTESIAN_POINT('Ctrl Pts',(-42.6538172012403,30.7906641692117,
-38.9407085950228));
#254426=CARTESIAN_POINT('Ctrl Pts',(-42.6662147228328,30.7600066178112,
-38.9368772324651));
#254427=CARTESIAN_POINT('Ctrl Pts',(-42.6794124410656,30.7295576092503,
-38.9332560772068));
#254428=CARTESIAN_POINT('Ctrl Pts',(-42.6934317597292,30.6993135470368,
-38.929849324519));
#254429=CARTESIAN_POINT('Ctrl Pts',(-42.700441419061,30.6841915159301,-38.9281459481751));
#254430=CARTESIAN_POINT('Ctrl Pts',(-42.7076664478387,30.6691033617142,
-38.9264946184812));
#254431=CARTESIAN_POINT('Ctrl Pts',(-42.7150618821773,30.6541435858172,
-38.924905794916));
#254432=CARTESIAN_POINT('Ctrl Pts',(-42.7224573165159,30.6391838099201,
-38.9233169713508));
#254433=CARTESIAN_POINT('Ctrl Pts',(-42.7300260074317,30.6243421619354,
-38.9217891027552));
#254434=CARTESIAN_POINT('Ctrl Pts',(-42.7377673957025,30.609622247504,-38.920322879707));
#254435=CARTESIAN_POINT('Ctrl Pts',(-42.768732948786,30.5507425897785,-38.9144579875142));
#254436=CARTESIAN_POINT('Ctrl Pts',(-42.802438005755,30.4937509787714,-38.9095620671014));
#254437=CARTESIAN_POINT('Ctrl Pts',(-42.8388300527629,30.4386219634623,
-38.9056215172398));
#254438=CARTESIAN_POINT('Ctrl Pts',(-42.8752220997707,30.3834929481532,
-38.9016809673782));
#254439=CARTESIAN_POINT('Ctrl Pts',(-42.9142995039568,30.330221730441,-38.898694431399));
#254440=CARTESIAN_POINT('Ctrl Pts',(-42.9560847992068,30.2788238207523,
-38.8966716165916));
#254441=CARTESIAN_POINT('Ctrl Pts',(-42.9978700944569,30.2274259110637,
-38.8946488017843));
#254442=CARTESIAN_POINT('Ctrl Pts',(-43.0423540539347,30.1779090615142,
-38.8935894002766));
#254443=CARTESIAN_POINT('Ctrl Pts',(-43.0896679045841,30.1303216200235,
-38.8935318156116));
#254444=CARTESIAN_POINT('Ctrl Pts',(-43.1369817552336,30.0827341785328,
-38.8934742309467));
#254445=CARTESIAN_POINT('Ctrl Pts',(-43.1862827102732,30.0379274090563,
-38.8944202483754));
#254446=CARTESIAN_POINT('Ctrl Pts',(-43.2374695236468,29.9958252623364,
-38.8963320083068));
#254447=CARTESIAN_POINT('Ctrl Pts',(-43.2886563370204,29.9537231156165,
-38.8982437682382));
#254448=CARTESIAN_POINT('Ctrl Pts',(-43.3417390736822,29.9143168693475,
-38.9011215513527));
#254449=CARTESIAN_POINT('Ctrl Pts',(-43.3967029881038,29.8775860531183,
-38.9049563008935));
#254450=CARTESIAN_POINT('Ctrl Pts',(-43.4241849453145,29.8592206450036,
-38.9068736756638));
#254451=CARTESIAN_POINT('Ctrl Pts',(-43.4521380201768,29.8415252139572,
-38.9090306863362));
#254452=CARTESIAN_POINT('Ctrl Pts',(-43.4805657277221,29.8245047392673,
-38.9114288083032));
#254453=CARTESIAN_POINT('Ctrl Pts',(-43.5089934352673,29.8074842645775,
-38.9138269302702));
#254454=CARTESIAN_POINT('Ctrl Pts',(-43.5379105932515,29.7911319045234,
-38.9164678395448));
#254455=CARTESIAN_POINT('Ctrl Pts',(-43.5672796770166,29.7754780139697,
-38.919349653254));
#254456=CARTESIAN_POINT('Ctrl Pts',(-43.5966487607817,29.7598241234161,
-38.9222314669631));
#254457=CARTESIAN_POINT('Ctrl Pts',(-43.6266146289649,29.7448030239206,
-38.9253708095819));
#254458=CARTESIAN_POINT('Ctrl Pts',(-43.6567606170124,29.7306258031448,
-38.9287240628825));
#254459=CARTESIAN_POINT('Ctrl Pts',(-43.68690660506,29.7164485823689,-38.9320773161831));
#254460=CARTESIAN_POINT('Ctrl Pts',(-43.7172788205642,29.7030822942954,
-38.9356472530647));
#254461=CARTESIAN_POINT('Ctrl Pts',(-43.74787091788,29.6905129658013,-38.9394291519851));
#254462=CARTESIAN_POINT('Ctrl Pts',(-43.7784630151957,29.6779436373071,
-38.9432110509055));
#254463=CARTESIAN_POINT('Ctrl Pts',(-43.8092755239302,29.666170138253,-38.9472047867905));
#254464=CARTESIAN_POINT('Ctrl Pts',(-43.8403053963098,29.655181264008,-38.9514068723595));
#254465=CARTESIAN_POINT('Ctrl Pts',(-43.8713352686894,29.644192389763,-38.9556089579285));
#254466=CARTESIAN_POINT('Ctrl Pts',(-43.9025825141023,29.6339881744307,
-38.9600194027673));
#254467=CARTESIAN_POINT('Ctrl Pts',(-43.9340457277949,29.6245633327707,
-38.9646362624899));
#254468=CARTESIAN_POINT('Ctrl Pts',(-43.9655089414875,29.6151384911106,
-38.9692531222126));
#254469=CARTESIAN_POINT('Ctrl Pts',(-43.9971881260961,29.6064930329024,
-38.9740764000692));
#254470=CARTESIAN_POINT('Ctrl Pts',(-44.0290834665269,29.5986273975902,
-38.9791056375968));
#254471=CARTESIAN_POINT('Ctrl Pts',(-44.0609788069577,29.5907617622781,
-38.9841348751245));
#254472=CARTESIAN_POINT('Ctrl Pts',(-44.0930902993264,29.5836759361658,
-38.9893700694948));
#254473=CARTESIAN_POINT('Ctrl Pts',(-44.1254197237287,29.5773761007637,
-38.9948122462768));
#254474=CARTESIAN_POINT('Ctrl Pts',(-44.157749148131,29.5710762653616,-39.0002544230587));
#254475=CARTESIAN_POINT('Ctrl Pts',(-44.1902803880436,29.5655649308414,
-39.0059007403469));
#254476=CARTESIAN_POINT('Ctrl Pts',(-44.2230652009806,29.5608466061619,
-39.0117622591756));
#254477=CARTESIAN_POINT('Ctrl Pts',(-44.2394576074491,29.5584874438222,
-39.01469301859));
#254478=CARTESIAN_POINT('Ctrl Pts',(-44.2558936005359,29.556330581768,-39.017674281006));
#254479=CARTESIAN_POINT('Ctrl Pts',(-44.2722948154515,29.5543845957057,
-39.0206914003809));
#254480=CARTESIAN_POINT('Ctrl Pts',(-44.288696030367,29.5524386096434,-39.0237085197559));
#254481=CARTESIAN_POINT('Ctrl Pts',(-44.3050952734896,29.5506978499007,
-39.0267671710297));
#254482=CARTESIAN_POINT('Ctrl Pts',(-44.3214722160119,29.5491651362618,
-39.0298636173565));
#254483=CARTESIAN_POINT('Ctrl Pts',(-44.386979986101,29.5430342817064,-39.0422494026637));
#254484=CARTESIAN_POINT('Ctrl Pts',(-44.4523142911657,29.5401658847829,
-39.0552645001479));
#254485=CARTESIAN_POINT('Ctrl Pts',(-44.5174452018332,29.5404749664642,
-39.0688802121094));
#254486=CARTESIAN_POINT('Ctrl Pts',(-44.5825761125008,29.5407840481454,
-39.0824959240709));
#254487=CARTESIAN_POINT('Ctrl Pts',(-44.64751868345,29.5442668522271,-39.0967146367708));
#254488=CARTESIAN_POINT('Ctrl Pts',(-44.7122655456777,29.5509157680261,
-39.1115282314101));
#254489=CARTESIAN_POINT('Ctrl Pts',(-44.7446389767916,29.5542402259256,
-39.1189350287298));
#254490=CARTESIAN_POINT('Ctrl Pts',(-44.7769718892781,29.5583592071516,
-39.126492904595));
#254491=CARTESIAN_POINT('Ctrl Pts',(-44.8092469543588,29.5632772749199,
-39.1341985554971));
#254492=CARTESIAN_POINT('Ctrl Pts',(-44.8415220194395,29.5681953426883,
-39.1419042063993));
#254493=CARTESIAN_POINT('Ctrl Pts',(-44.873794287365,29.5739237069059,-39.1497713394166));
#254494=CARTESIAN_POINT('Ctrl Pts',(-44.9059258943645,29.580448064776,-39.1577677872645));
#254495=CARTESIAN_POINT('Ctrl Pts',(-44.938057501364,29.5869724226462,-39.1657642351124));
#254496=CARTESIAN_POINT('Ctrl Pts',(-44.9698454327154,29.5942479284801,
-39.1738387467903));
#254497=CARTESIAN_POINT('Ctrl Pts',(-45.0013540521658,29.6022690447016,
-39.1820030835632));
#254498=CARTESIAN_POINT('Ctrl Pts',(-45.0328626716162,29.6102901609231,
-39.1901674203362));
#254499=CARTESIAN_POINT('Ctrl Pts',(-45.0640728677801,29.6190530040921,
-39.1984168268269));
#254500=CARTESIAN_POINT('Ctrl Pts',(-45.0949895328334,29.6285456745752,
-39.2067494504582));
#254501=CARTESIAN_POINT('Ctrl Pts',(-45.0988345002,29.6297262355499,-39.207785741594));
#254502=CARTESIAN_POINT('Ctrl Pts',(-45.1026749334513,29.630918067705,-39.2088233175957));
#254503=CARTESIAN_POINT('Ctrl Pts',(-45.1065107582268,29.6321211388928,
-39.2098621557269));
#254504=CARTESIAN_POINT('Ctrl Pts',(-42.5264433853035,31.2691187985001,
-39.0141965709288));
#254505=CARTESIAN_POINT('Ctrl Pts',(-42.533975017942,31.2141173491589,-39.0171948856712));
#254506=CARTESIAN_POINT('Ctrl Pts',(-42.5438622229547,31.1589786372441,
-39.0202688264213));
#254507=CARTESIAN_POINT('Ctrl Pts',(-42.5561557287987,31.1040026525962,
-39.023404719375));
#254508=CARTESIAN_POINT('Ctrl Pts',(-42.5683599682557,31.0494258630668,
-39.0265178417832));
#254509=CARTESIAN_POINT('Ctrl Pts',(-42.5829359045809,30.9950101372705,
-39.0296919913082));
#254510=CARTESIAN_POINT('Ctrl Pts',(-42.5998833018802,30.9410609056468,
-39.0329117328335));
#254511=CARTESIAN_POINT('Ctrl Pts',(-42.6167409587158,30.8873973479218,
-39.0361144250685));
#254512=CARTESIAN_POINT('Ctrl Pts',(-42.6359450801664,30.834196084843,-39.0393621924919));
#254513=CARTESIAN_POINT('Ctrl Pts',(-42.6574438939907,30.7817589584099,
-39.0426382781429));
#254514=CARTESIAN_POINT('Ctrl Pts',(-42.6788724270608,30.7294932517034,
-39.0459036540975));
#254515=CARTESIAN_POINT('Ctrl Pts',(-42.7025805580132,30.6779874187089,
-39.0491971234277));
#254516=CARTESIAN_POINT('Ctrl Pts',(-42.7284661350043,30.6275306909273,
-39.0525010968636));
#254517=CARTESIAN_POINT('Ctrl Pts',(-42.7543356047292,30.5771053597781,
-39.0558030144063));
#254518=CARTESIAN_POINT('Ctrl Pts',(-42.7823795359021,30.5277285141059,
-39.0591153803188));
#254519=CARTESIAN_POINT('Ctrl Pts',(-42.8124479723331,30.4796685666064,
-39.0624202628221));
#254520=CARTESIAN_POINT('Ctrl Pts',(-42.8425499311369,30.4315550385532,
-39.065728829837));
#254521=CARTESIAN_POINT('Ctrl Pts',(-42.8746804827911,30.3847619516162,
-39.0690298536715));
#254522=CARTESIAN_POINT('Ctrl Pts',(-42.9086463432861,30.3395285449195,
-39.072305612684));
#254523=CARTESIAN_POINT('Ctrl Pts',(-42.9427092073028,30.2941659555764,
-39.0755907269772));
#254524=CARTESIAN_POINT('Ctrl Pts',(-42.978617320009,30.2503724567378,-39.0788503909572));
#254525=CARTESIAN_POINT('Ctrl Pts',(-43.0161401302784,30.2083508338029,
-39.0820676376815));
#254526=CARTESIAN_POINT('Ctrl Pts',(-43.0539958194939,30.1659564212647,
-39.0853134258101));
#254527=CARTESIAN_POINT('Ctrl Pts',(-43.0934943374488,30.1253658443146,
-39.088516002619));
#254528=CARTESIAN_POINT('Ctrl Pts',(-43.1343718380936,30.0867415073552,
-39.0916594701529));
#254529=CARTESIAN_POINT('Ctrl Pts',(-43.1754823554595,30.0478969975327,
-39.0948208566027));
#254530=CARTESIAN_POINT('Ctrl Pts',(-43.2179868945264,30.0110413889675,
-39.0979224276242));
#254531=CARTESIAN_POINT('Ctrl Pts',(-43.2616002290463,29.9762894859414,
-39.1009500664389));
#254532=CARTESIAN_POINT('Ctrl Pts',(-43.3057813273405,29.9410851783504,
-39.1040171194296));
#254533=CARTESIAN_POINT('Ctrl Pts',(-43.3510995292929,29.9080397621653,
-39.107008278067));
#254534=CARTESIAN_POINT('Ctrl Pts',(-43.3972523236822,29.8772191026902,
-39.109911393871));
#254535=CARTESIAN_POINT('Ctrl Pts',(-43.4336815722595,29.852891789898,-39.1122028765141));
#254536=CARTESIAN_POINT('Ctrl Pts',(-43.4706305620717,29.8299494375692,
-39.1144395560518));
#254537=CARTESIAN_POINT('Ctrl Pts',(-43.5079524583199,29.8084016307237,
-39.1166166666663));
#254538=CARTESIAN_POINT('Ctrl Pts',(-43.5553799427766,29.7810193598056,
-39.1193832699262));
#254539=CARTESIAN_POINT('Ctrl Pts',(-43.6044581995708,29.7552851959446,
-39.1222461913981));
#254540=CARTESIAN_POINT('Ctrl Pts',(-43.6550143791165,29.7314482427253,
-39.1251953413445));
#254541=CARTESIAN_POINT('Ctrl Pts',(-43.7050241825406,29.7078689027626,
-39.1281126189239));
#254542=CARTESIAN_POINT('Ctrl Pts',(-43.756479873319,29.6861466532943,-39.1311142558983));
#254543=CARTESIAN_POINT('Ctrl Pts',(-43.8091686689389,29.6664994960942,
-39.1341878331413));
#254544=CARTESIAN_POINT('Ctrl Pts',(-43.8612441375445,29.6470810427793,
-39.1372256322283));
#254545=CARTESIAN_POINT('Ctrl Pts',(-43.9145237443489,29.6296902265431,
-39.1403336816531));
#254546=CARTESIAN_POINT('Ctrl Pts',(-43.9687625207563,29.61450562165,-39.1434976847857));
#254547=CARTESIAN_POINT('Ctrl Pts',(-44.0226897493758,29.5994082371991,
-39.1466435138693));
#254548=CARTESIAN_POINT('Ctrl Pts',(-44.0775646322468,29.5864922846488,
-39.1498446249087));
#254549=CARTESIAN_POINT('Ctrl Pts',(-44.1331141493744,29.5758935484052,
-39.1530850848182));
#254550=CARTESIAN_POINT('Ctrl Pts',(-44.1884409379484,29.565337308322,-39.1563125519425));
#254551=CARTESIAN_POINT('Ctrl Pts',(-44.244436327736,29.5570801011644,-39.1595790160483));
#254552=CARTESIAN_POINT('Ctrl Pts',(-44.3008071787297,29.5512101408557,
-39.1628673702128));
#254553=CARTESIAN_POINT('Ctrl Pts',(-44.3570499030541,29.5453535225217,
-39.1661482501976));
#254554=CARTESIAN_POINT('Ctrl Pts',(-44.4136656784857,29.5418735174476,
-39.1694508797056));
#254555=CARTESIAN_POINT('Ctrl Pts',(-44.4703500735278,29.540807629945,-39.1727574929379));
#254556=CARTESIAN_POINT('Ctrl Pts',(-44.5270863560613,29.5397407667554,
-39.1760671329622));
#254557=CARTESIAN_POINT('Ctrl Pts',(-44.5838906443107,29.5410924924669,
-39.1793807208643));
#254558=CARTESIAN_POINT('Ctrl Pts',(-44.6404552194646,29.5448481851576,
-39.1826802988214));
#254559=CARTESIAN_POINT('Ctrl Pts',(-44.6970922205564,29.5486086866808,
-39.1859841015965));
#254560=CARTESIAN_POINT('Ctrl Pts',(-44.7534881638628,29.5547791795424,
-39.1892738159161));
#254561=CARTESIAN_POINT('Ctrl Pts',(-44.8093427863577,29.5632932892976,
-39.1925319186275));
#254562=CARTESIAN_POINT('Ctrl Pts',(-44.8655321438493,29.5718584238448,
-39.1958095470461));
#254563=CARTESIAN_POINT('Ctrl Pts',(-44.9211729794212,29.5827950700452,
-39.1990551433739));
#254564=CARTESIAN_POINT('Ctrl Pts',(-44.9759791375788,29.5959864507854,
-39.2022520070656));
#254565=CARTESIAN_POINT('Ctrl Pts',(-45.0200746694849,29.6065998739822,
-39.2048241159244));
#254566=CARTESIAN_POINT('Ctrl Pts',(-45.0636301540079,29.6186718150447,
-39.2073646941016));
#254567=CARTESIAN_POINT('Ctrl Pts',(-45.1065099250746,29.6321209281423,
-39.2098658234324));
#254568=CARTESIAN_POINT('Ctrl Pts',(-46.6981266849492,30.7091523375488,
-39.2904704603133));
#254569=CARTESIAN_POINT('Ctrl Pts',(-46.6689684123063,30.6404043382273,
-39.273452295095));
#254570=CARTESIAN_POINT('Ctrl Pts',(-46.6043681216411,30.5066861069553,
-39.238925705885));
#254571=CARTESIAN_POINT('Ctrl Pts',(-46.5083209189471,30.3487389562033,
-39.1945593129175));
#254572=CARTESIAN_POINT('Ctrl Pts',(-46.4437937583117,30.2581216171786,
-39.1673894861782));
#254573=CARTESIAN_POINT('Ctrl Pts',(-46.3992224148768,30.1986447451181,
-39.1491520227249));
#254574=CARTESIAN_POINT('Ctrl Pts',(-46.3761748773305,30.1693908446446,
-39.1399767764946));
#254575=CARTESIAN_POINT('Ctrl Pts',(-46.3284414024809,30.1117648114071,
-39.1214771434543));
#254576=CARTESIAN_POINT('Ctrl Pts',(-46.3038983378397,30.083571828401,-39.112209259666));
#254577=CARTESIAN_POINT('Ctrl Pts',(-46.253707387608,30.0286632749651,-39.0937226519629));
#254578=CARTESIAN_POINT('Ctrl Pts',(-46.2280147026909,30.001893564456,-39.0844865568113));
#254579=CARTESIAN_POINT('Ctrl Pts',(-46.1492148010453,29.9236586721517,
-39.0568159196779));
#254580=CARTESIAN_POINT('Ctrl Pts',(-46.0669347173688,29.8495134741745,
-39.0292038481275));
#254581=CARTESIAN_POINT('Ctrl Pts',(-45.9503410384262,29.7587889734315,
-38.9925114043613));
#254582=CARTESIAN_POINT('Ctrl Pts',(-45.8594191065401,29.6948377475824,
-38.9650526418885));
#254583=CARTESIAN_POINT('Ctrl Pts',(-45.7964751089327,29.6549785818455,
-38.9467936623891));
#254584=CARTESIAN_POINT('Ctrl Pts',(-45.748348603817,29.6261284949947,-38.9331097524421));
#254585=CARTESIAN_POINT('Ctrl Pts',(-45.7321473284057,29.616684052073,-38.9285487676403));
#254586=CARTESIAN_POINT('Ctrl Pts',(-45.6996106203311,29.5982459977232,
-38.9194791520014));
#254587=CARTESIAN_POINT('Ctrl Pts',(-45.683249044345,29.5892352448745,-38.9149628379356));
#254588=CARTESIAN_POINT('Ctrl Pts',(-45.6010439155842,29.5452684013657,
-38.8924942188443));
#254589=CARTESIAN_POINT('Ctrl Pts',(-45.4667739830181,29.4816584171599,
-38.8571935516581));
#254590=CARTESIAN_POINT('Ctrl Pts',(-45.2922645146651,29.4187721922835,
-38.8147007629208));
#254591=CARTESIAN_POINT('Ctrl Pts',(-45.184512437616,29.3885937253944,-38.7899522655792));
#254592=CARTESIAN_POINT('Ctrl Pts',(-45.1119891467798,29.3701842541612,
-38.7736235920333));
#254593=CARTESIAN_POINT('Ctrl Pts',(-45.0754052578815,29.3618381514785,
-38.7655490803555));
#254594=CARTESIAN_POINT('Ctrl Pts',(-45.0014447932705,29.3468760834356,
-38.7495561846596));
#254595=CARTESIAN_POINT('Ctrl Pts',(-44.964301863367,29.3403115562353,-38.7416890516424));
#254596=CARTESIAN_POINT('Ctrl Pts',(-44.8900079594565,29.3290481892184,
-38.726277749838));
#254597=CARTESIAN_POINT('Ctrl Pts',(-44.8527936282157,29.324336495618,-38.7187198739728));
#254598=CARTESIAN_POINT('Ctrl Pts',(-44.7410083373266,29.3129455735289,
-38.6964994820139));
#254599=CARTESIAN_POINT('Ctrl Pts',(-44.6662563757167,29.3089967422249,
-38.6822807693139));
#254600=CARTESIAN_POINT('Ctrl Pts',(-44.516312468428,29.3084067934202,-38.6550493453909));
#254601=CARTESIAN_POINT('Ctrl Pts',(-44.441103189525,29.3117700143417,-38.6420342479066));
#254602=CARTESIAN_POINT('Ctrl Pts',(-44.3468378615956,29.3206690055189,
-38.6265520162729));
#254603=CARTESIAN_POINT('Ctrl Pts',(-44.3279589148655,29.3226883315868,
-38.6234933649988));
#254604=CARTESIAN_POINT('Ctrl Pts',(-44.2901960653062,29.3271995080042,
-38.6174591262491));
#254605=CARTESIAN_POINT('Ctrl Pts',(-44.271274393292,29.329697893027,-38.614477863833));
#254606=CARTESIAN_POINT('Ctrl Pts',(-44.2146592782019,29.3378915995821,
-38.60568558559));
#254607=CARTESIAN_POINT('Ctrl Pts',(-44.1772069502033,29.344266758826,-38.6000392683017));
#254608=CARTESIAN_POINT('Ctrl Pts',(-44.0655444875092,29.3661148598052,
-38.5837127379559));
#254609=CARTESIAN_POINT('Ctrl Pts',(-43.9553791862171,29.3933792052515,
-38.5686255047386));
#254610=CARTESIAN_POINT('Ctrl Pts',(-43.8114622524781,29.4404829778103,
-38.5509833019505));
#254611=CARTESIAN_POINT('Ctrl Pts',(-43.705021834675,29.481230340464,-38.5390021142185));
#254612=CARTESIAN_POINT('Ctrl Pts',(-43.6350719757086,29.512061063653,-38.5318621614261));
#254613=CARTESIAN_POINT('Ctrl Pts',(-43.5656410085295,29.5447591316771,
-38.525155654825));
#254614=CARTESIAN_POINT('Ctrl Pts',(-43.5311320054746,29.5620794464364,
-38.5220163122062));
#254615=CARTESIAN_POINT('Ctrl Pts',(-43.4634866412134,29.5981758355574,
-38.5162526847879));
#254616=CARTESIAN_POINT('Ctrl Pts',(-43.4301834663392,29.6170276546,-38.5136117755133));
#254617=CARTESIAN_POINT('Ctrl Pts',(-43.3647025891651,29.6562685687332,
-38.5088155315793));
#254618=CARTESIAN_POINT('Ctrl Pts',(-43.2681192378476,29.7174608121974,
-38.5023448938576));
#254619=CARTESIAN_POINT('Ctrl Pts',(-43.1764049274077,29.7855824582168,
-38.4980286134812));
#254620=CARTESIAN_POINT('Ctrl Pts',(-43.0584774180437,29.8826126224142,
-38.4942050936184));
#254621=CARTESIAN_POINT('Ctrl Pts',(-43.001681818637,29.9342392650769,-38.4932590761897));
#254622=CARTESIAN_POINT('Ctrl Pts',(-42.8926599718677,30.0438904492243,
-38.4933742455196));
#254623=CARTESIAN_POINT('Ctrl Pts',(-42.8414047150844,30.1009342501745,
-38.4944336470273));
#254624=CARTESIAN_POINT('Ctrl Pts',(-42.7451036203247,30.2193471227021,
-38.498479276642));
#254625=CARTESIAN_POINT('Ctrl Pts',(-42.6550322643363,30.3420646399833,
-38.5044516702661));
#254626=CARTESIAN_POINT('Ctrl Pts',(-42.5773225406025,30.4733365238586,
-38.5142428327574));
#254627=CARTESIAN_POINT('Ctrl Pts',(-42.5326943378214,30.5580963840027,
-38.5215739479982));
#254628=CARTESIAN_POINT('Ctrl Pts',(-42.5239673850246,30.5751883092729,
-38.5231018165939));
#254629=CARTESIAN_POINT('Ctrl Pts',(-42.5069121510755,30.60964376351,-38.5262794637242));
#254630=CARTESIAN_POINT('Ctrl Pts',(-42.4985805781952,30.627019094627,-38.5279307934181));
#254631=CARTESIAN_POINT('Ctrl Pts',(-42.4743295471271,30.6792614198295,
-38.5330409224498));
#254632=CARTESIAN_POINT('Ctrl Pts',(-42.4438856226513,30.7493896366731,
-38.5402834483744));
#254633=CARTESIAN_POINT('Ctrl Pts',(-42.4037483179465,30.8560072598611,
-38.5524071291592));
#254634=CARTESIAN_POINT('Ctrl Pts',(-42.3690543371876,30.9640160484273,
-38.5657659376104));
#254635=CARTESIAN_POINT('Ctrl Pts',(-42.3397558527982,31.0734075527136,
-38.5803463747351));
#254636=CARTESIAN_POINT('Ctrl Pts',(-42.3238156343608,31.1472555030051,
-38.5908775753381));
#254637=CARTESIAN_POINT('Ctrl Pts',(-42.3096820427396,31.2215665449467,
-38.6018154236264));
#254638=CARTESIAN_POINT('Ctrl Pts',(-42.3035171869091,31.2589715314082,
-38.6074906718877));
#254639=CARTESIAN_POINT('Ctrl Pts',(-42.2930235524414,31.3341791410138,
-38.6192399292287));
#254640=CARTESIAN_POINT('Ctrl Pts',(-42.2886818075092,31.3721585359098,
-38.6253436316658));
#254641=CARTESIAN_POINT('Ctrl Pts',(-42.281930630611,31.4478003630713,-38.6378362101326));
#254642=CARTESIAN_POINT('Ctrl Pts',(-42.277074994566,31.5232809912004,-38.6506356205751));
#254643=CARTESIAN_POINT('Ctrl Pts',(-42.2747992363309,31.6735553614761,
-38.6774229397946));
#254644=CARTESIAN_POINT('Ctrl Pts',(-42.2834818483937,31.8228397562226,
-38.7059581415094));
#254645=CARTESIAN_POINT('Ctrl Pts',(-42.3030248127084,31.9711385758679,
-38.7362097844166));
#254646=CARTESIAN_POINT('Ctrl Pts',(-42.3164494406915,32.0449687602614,
-38.7519128032936));
#254647=CARTESIAN_POINT('Ctrl Pts',(-42.3317154579634,32.1186122141692,
-38.7679009120377));
#254648=CARTESIAN_POINT('Ctrl Pts',(-42.3402956643805,32.1554227583218,
-38.7760569897633));
#254649=CARTESIAN_POINT('Ctrl Pts',(-42.3591481714288,32.228169160774,-38.7925026060078));
#254650=CARTESIAN_POINT('Ctrl Pts',(-42.3694448348212,32.2642362896146,
-38.8008201507359));
#254651=CARTESIAN_POINT('Ctrl Pts',(-42.4028917825415,32.3714169561226,
-38.8260275044574));
#254652=CARTESIAN_POINT('Ctrl Pts',(-42.428602574983,32.4415633880281,-38.8431823298655));
#254653=CARTESIAN_POINT('Ctrl Pts',(-42.4722685042023,32.5448307979217,
-38.8694323201497));
#254654=CARTESIAN_POINT('Ctrl Pts',(-42.4876674804306,32.5789105800712,
-38.8782643966373));
#254655=CARTESIAN_POINT('Ctrl Pts',(-42.5202146590728,32.6464795812123,
-38.8961197808447));
#254656=CARTESIAN_POINT('Ctrl Pts',(-42.5373018269229,32.6798350022668,
-38.9051083126545));
#254657=CARTESIAN_POINT('Ctrl Pts',(-42.5906929412925,32.7780783962456,
-38.9321048428364));
#254658=CARTESIAN_POINT('Ctrl Pts',(-42.629225789877,32.8414173722334,-38.9502105255135));
#254659=CARTESIAN_POINT('Ctrl Pts',(-42.7120000069194,32.9638220552461,
-38.9866125955294));
#254660=CARTESIAN_POINT('Ctrl Pts',(-42.7783647966162,33.0524402968179,
-39.0140612314234));
#254661=CARTESIAN_POINT('Ctrl Pts',(-42.8754380724448,33.1642175243331,
-39.0509520337677));
#254662=CARTESIAN_POINT('Ctrl Pts',(-42.9268673384212,33.2179450225078,
-39.0694937486382));
#254663=CARTESIAN_POINT('Ctrl Pts',(-42.9797817061918,33.2705900457306,
-39.088089881442));
#254664=CARTESIAN_POINT('Ctrl Pts',(-43.0069972096607,33.2963736994336,
-39.097418269769));
#254665=CARTESIAN_POINT('Ctrl Pts',(-43.0622936398443,33.3462615369726,
-39.1159154063528));
#254666=CARTESIAN_POINT('Ctrl Pts',(-43.0904949946047,33.3704876748183,
-39.1251268688783));
#254667=CARTESIAN_POINT('Ctrl Pts',(-43.176562606447,33.4408730143712,-39.1525915568785));
#254668=CARTESIAN_POINT('Ctrl Pts',(-43.2360245534179,33.4848790444095,
-39.1707230137558));
#254669=CARTESIAN_POINT('Ctrl Pts',(-43.358992255749,33.5670176609587,-39.2066046432507));
#254670=CARTESIAN_POINT('Ctrl Pts',(-43.4542745623933,33.6242424638975,
-39.233238623837));
#254671=CARTESIAN_POINT('Ctrl Pts',(-43.5542222374601,33.6747516510336,
-39.2594493821381));
#254672=CARTESIAN_POINT('Ctrl Pts',(-43.6219256430316,33.7069073870393,
-39.2768314299875));
#254673=CARTESIAN_POINT('Ctrl Pts',(-43.6563381479934,33.7222286468184,
-39.2854811722856));
#254674=CARTESIAN_POINT('Ctrl Pts',(-43.7254519170511,33.7509934760635,
-39.3024907499371));
#254675=CARTESIAN_POINT('Ctrl Pts',(-43.7602995448845,33.7645084608315,
-39.3108885064059));
#254676=CARTESIAN_POINT('Ctrl Pts',(-43.8304781084082,33.789780836939,-39.3274499785309));
#254677=CARTESIAN_POINT('Ctrl Pts',(-43.9365171946568,33.8250735562425,
-39.3519527568515));
#254678=CARTESIAN_POINT('Ctrl Pts',(-44.0809642638621,33.8617420360433,
-39.3832806139221));
#254679=CARTESIAN_POINT('Ctrl Pts',(-44.1916183723467,33.8813683146414,
-39.4057679385072));
#254680=CARTESIAN_POINT('Ctrl Pts',(-44.2659122959159,33.8926702964892,
-39.4205323411483));
#254681=CARTESIAN_POINT('Ctrl Pts',(-44.3033049221432,33.8974288658374,
-39.4277978831022));
#254682=CARTESIAN_POINT('Ctrl Pts',(-44.3598453576919,33.9032050944765,
-39.4385322478049));
#254683=CARTESIAN_POINT('Ctrl Pts',(-44.3787527158677,33.9049006163346,
-39.4420799976889));
#254684=CARTESIAN_POINT('Ctrl Pts',(-44.4164967874688,33.9078161173588,
-39.4490791780208));
#254685=CARTESIAN_POINT('Ctrl Pts',(-44.4353708468856,33.9090400957878,
-39.4525377314439));
#254686=CARTESIAN_POINT('Ctrl Pts',(-44.4919347179527,33.9120095261765,
-39.462779235967));
#254687=CARTESIAN_POINT('Ctrl Pts',(-44.52962054914,33.9130584408517,-39.4694384189012));
#254688=CARTESIAN_POINT('Ctrl Pts',(-44.6425299001817,33.9134342925821,
-39.4889026473125));
#254689=CARTESIAN_POINT('Ctrl Pts',(-44.7176656228988,33.9100023852834,
-39.5012068570978));
#254690=CARTESIAN_POINT('Ctrl Pts',(-44.867623327666,33.8957625538083,-39.524471978366));
#254691=CARTESIAN_POINT('Ctrl Pts',(-44.9424659600731,33.8849485744664,
-39.5354353652432));
#254692=CARTESIAN_POINT('Ctrl Pts',(-45.0357885152669,33.8666999843662,
-39.5482785606344));
#254693=CARTESIAN_POINT('Ctrl Pts',(-45.0544546343785,33.8628074782943,
-39.5508053225112));
#254694=CARTESIAN_POINT('Ctrl Pts',(-45.091743102575,33.8545484160302,-39.5557691634051));
#254695=CARTESIAN_POINT('Ctrl Pts',(-45.1104022544846,33.850171655015,-39.5582107864407));
#254696=CARTESIAN_POINT('Ctrl Pts',(-45.1661672125598,33.8363538303533,
-39.5653802281989));
#254697=CARTESIAN_POINT('Ctrl Pts',(-45.2029511118778,33.8262578362557,
-39.5699395109212));
#254698=CARTESIAN_POINT('Ctrl Pts',(-45.312316831343,33.7933159380614,-39.582990524906));
#254699=CARTESIAN_POINT('Ctrl Pts',(-45.4195983160475,33.7551076509549,
-39.5947758536238));
#254700=CARTESIAN_POINT('Ctrl Pts',(-45.5585113890164,33.6937328563153,
-39.6079933748399));
#254701=CARTESIAN_POINT('Ctrl Pts',(-45.6606150024606,33.6424505696195,
-39.6166516297843));
#254702=CARTESIAN_POINT('Ctrl Pts',(-45.7272860947277,33.6047101271221,
-39.6215780075552));
#254703=CARTESIAN_POINT('Ctrl Pts',(-45.7932287365117,33.5651705839516,
-39.6260731428005));
#254704=CARTESIAN_POINT('Ctrl Pts',(-45.8259059249178,33.5444453395394,
-39.6281074988013));
#254705=CARTESIAN_POINT('Ctrl Pts',(-45.8897275017006,33.5016881508368,
-39.6316923737189));
#254706=CARTESIAN_POINT('Ctrl Pts',(-45.9210297733036,33.4795651380848,
-39.6332542688506));
#254707=CARTESIAN_POINT('Ctrl Pts',(-45.9823424846244,33.4339088874735,
-39.6359180193303));
#254708=CARTESIAN_POINT('Ctrl Pts',(-46.0724202597563,33.3632801300718,
-39.6392265347984));
#254709=CARTESIAN_POINT('Ctrl Pts',(-46.1850394564173,33.2606222983665,
-39.6409205727319));
#254710=CARTESIAN_POINT('Ctrl Pts',(-46.2638636333332,33.1772336958075,
-39.6401443034625));
#254711=CARTESIAN_POINT('Ctrl Pts',(-46.3151397511292,33.1201974856456,
-39.6391646017005));
#254712=CARTESIAN_POINT('Ctrl Pts',(-46.3401349353408,33.0909661742941,
-39.6384440851485));
#254713=CARTESIAN_POINT('Ctrl Pts',(-46.3888523044997,33.0309971480077,
-39.6365301000439));
#254714=CARTESIAN_POINT('Ctrl Pts',(-46.4123735341802,33.0005036828642,
-39.6353439924849));
#254715=CARTESIAN_POINT('Ctrl Pts',(-46.4576879006691,32.9386388625828,
-39.6325280276393));
#254716=CARTESIAN_POINT('Ctrl Pts',(-46.52311576659,32.8444620833496,-39.6276360146217));
#254717=CARTESIAN_POINT('Ctrl Pts',(-46.5810426872604,32.7462345994881,
-39.6207752343847));
#254718=CARTESIAN_POINT('Ctrl Pts',(-46.6516918187307,32.6117039458857,
-39.6098936921283));
#254719=CARTESIAN_POINT('Ctrl Pts',(-46.683723185051,32.5426422373878,-39.6035832967262));
#254720=CARTESIAN_POINT('Ctrl Pts',(-46.7195635412788,32.4540883209461,
-39.5945936116187));
#254721=CARTESIAN_POINT('Ctrl Pts',(-46.7265235775841,32.4362514419463,
-39.5927383889278));
#254722=CARTESIAN_POINT('Ctrl Pts',(-46.7400123459627,32.4003742100513,
-39.5889189813535));
#254723=CARTESIAN_POINT('Ctrl Pts',(-46.7465535157541,32.3822946053341,
-39.5869502184844));
#254724=CARTESIAN_POINT('Ctrl Pts',(-46.7654644360989,32.3279072933142,
-39.5808958427402));
#254725=CARTESIAN_POINT('Ctrl Pts',(-46.7770937339888,32.2915493874551,
-39.5766741707955));
#254726=CARTESIAN_POINT('Ctrl Pts',(-46.8091770518909,32.182013131159,-39.5634457571489));
#254727=CARTESIAN_POINT('Ctrl Pts',(-46.8444383818759,32.034891308334,-39.5443264312115));
#254728=CARTESIAN_POINT('Ctrl Pts',(-46.8650708643864,31.8856621776612,
-39.5223044891954));
#254729=CARTESIAN_POINT('Ctrl Pts',(-46.8750487417844,31.7729724844591,
-39.50469487268));
#254730=CARTESIAN_POINT('Ctrl Pts',(-46.8774570362353,31.7352651712118,
-39.4986397605723));
#254731=CARTESIAN_POINT('Ctrl Pts',(-46.8796767940079,31.6785286095959,
-39.4892824810203));
#254732=CARTESIAN_POINT('Ctrl Pts',(-46.8801843407089,31.6595724593507,
-39.4861150486293));
#254733=CARTESIAN_POINT('Ctrl Pts',(-46.8807312344332,31.6216180949417,
-39.479690628598));
#254734=CARTESIAN_POINT('Ctrl Pts',(-46.8807699646674,31.6025797052015,
-39.4764266299692));
#254735=CARTESIAN_POINT('Ctrl Pts',(-46.8801790388754,31.5455906639181,
-39.4665317368708));
#254736=CARTESIAN_POINT('Ctrl Pts',(-46.8788490796135,31.5078273383739,
-39.4598096545541));
#254737=CARTESIAN_POINT('Ctrl Pts',(-46.874360617844,31.4326451774338,-39.4461013696832));
#254738=CARTESIAN_POINT('Ctrl Pts',(-46.864884835636,31.320441459725,-39.4251517854185));
#254739=CARTESIAN_POINT('Ctrl Pts',(-46.8414902947658,31.1730719473388,
-39.3956936109857));
#254740=CARTESIAN_POINT('Ctrl Pts',(-46.8074810934279,31.0279105813681,
-39.364717848004));
#254741=CARTESIAN_POINT('Ctrl Pts',(-46.7869180083019,30.9560697433081,
-39.3487190247537));
#254742=CARTESIAN_POINT('Ctrl Pts',(-46.7645577771926,30.884604709384,-39.332461491893));
#254743=CARTESIAN_POINT('Ctrl Pts',(-46.7524740339114,30.8490466969583,
-39.3242001683612));
#254744=CARTESIAN_POINT('Ctrl Pts',(-46.7264943673172,30.7783632715819,
-39.3074248425479));
#254745=CARTESIAN_POINT('Ctrl Pts',(-46.7127058212706,30.7435263372096,
-39.2989795429224));
#254746=CARTESIAN_POINT('Ctrl Pts',(-46.6981266849492,30.7091523375488,
-39.2904704603133));
#254747=CARTESIAN_POINT('Ctrl Pts',(-45.0394875320819,30.9432190801919,
-41.190386719266));
#254748=CARTESIAN_POINT('Ctrl Pts',(-45.0282734427409,30.91723575627,-41.1733685540478));
#254749=CARTESIAN_POINT('Ctrl Pts',(-45.0034876660128,30.8666726764904,
-41.1388419648381));
#254750=CARTESIAN_POINT('Ctrl Pts',(-44.9667665375866,30.8068862988478,
-41.09447557187));
#254751=CARTESIAN_POINT('Ctrl Pts',(-44.9421458413835,30.7725558756156,
-41.0673057451311));
#254752=CARTESIAN_POINT('Ctrl Pts',(-44.9251493960809,30.7500159625169,
-41.0490682816776));
#254753=CARTESIAN_POINT('Ctrl Pts',(-44.9163654668634,30.7389260450349,
-41.0398930354472));
#254754=CARTESIAN_POINT('Ctrl Pts',(-44.8981827131164,30.7170729960788,
-41.0213934024069));
#254755=CARTESIAN_POINT('Ctrl Pts',(-44.888838333634,30.7063777841388,-41.0121255186188));
#254756=CARTESIAN_POINT('Ctrl Pts',(-44.8697378119757,30.6855401076749,
-40.9936389109155));
#254757=CARTESIAN_POINT('Ctrl Pts',(-44.8599646045333,30.6753771122426,
-40.984402815764));
#254758=CARTESIAN_POINT('Ctrl Pts',(-44.8300025766326,30.6456635434001,
-40.9567321786306));
#254759=CARTESIAN_POINT('Ctrl Pts',(-44.7987417882795,30.6174785558847,
-40.9291201070801));
#254760=CARTESIAN_POINT('Ctrl Pts',(-44.7544912812914,30.5829390177582,
-40.8924276633141));
#254761=CARTESIAN_POINT('Ctrl Pts',(-44.7200063674423,30.5585634922437,
-40.8649689008411));
#254762=CARTESIAN_POINT('Ctrl Pts',(-44.6961476159991,30.5433500948652,
-40.8467099213417));
#254763=CARTESIAN_POINT('Ctrl Pts',(-44.6779108400504,30.5323301088838,
-40.8330260113948));
#254764=CARTESIAN_POINT('Ctrl Pts',(-44.6717725199842,30.5287210947847,
-40.8284650265932));
#254765=CARTESIAN_POINT('Ctrl Pts',(-44.6594468286685,30.521672327511,-40.8193954109541));
#254766=CARTESIAN_POINT('Ctrl Pts',(-44.6532495459125,30.5182260348866,
-40.8148790968875));
#254767=CARTESIAN_POINT('Ctrl Pts',(-44.6221170703041,30.5014023919654,
-40.7924104777995));
#254768=CARTESIAN_POINT('Ctrl Pts',(-44.5712944462502,30.4770113822335,
-40.7571098106096));
#254769=CARTESIAN_POINT('Ctrl Pts',(-44.5053084694641,30.4527583886953,
-40.7146170218743));
#254770=CARTESIAN_POINT('Ctrl Pts',(-44.4645950315289,30.4410392847555,
-40.6898685245315));
#254771=CARTESIAN_POINT('Ctrl Pts',(-44.4371992237873,30.4338676574989,
-40.6735398509862));
#254772=CARTESIAN_POINT('Ctrl Pts',(-44.4233828828253,30.4306039319716,
-40.6654653393082));
#254773=CARTESIAN_POINT('Ctrl Pts',(-44.395457566773,30.4247250011004,-40.6494724436125));
#254774=CARTESIAN_POINT('Ctrl Pts',(-44.3814368244576,30.4221299378924,
-40.6416053105951));
#254775=CARTESIAN_POINT('Ctrl Pts',(-44.353398925472,30.4176419772095,-40.6261940087904));
#254776=CARTESIAN_POINT('Ctrl Pts',(-44.3393578467875,30.4157440298243,
-40.6186361329255));
#254777=CARTESIAN_POINT('Ctrl Pts',(-44.2971907773647,30.4110825461462,
-40.5964157409664));
#254778=CARTESIAN_POINT('Ctrl Pts',(-44.2690063197214,30.4093460565949,
-40.5821970282665));
#254779=CARTESIAN_POINT('Ctrl Pts',(-44.212497942469,30.4086221665927,-40.5549656043439));
#254780=CARTESIAN_POINT('Ctrl Pts',(-44.1841675064314,30.4096363406377,
-40.5419505068598));
#254781=CARTESIAN_POINT('Ctrl Pts',(-44.1486758957365,30.4126704859088,
-40.5264682752254));
#254782=CARTESIAN_POINT('Ctrl Pts',(-44.141568690144,30.4133673915631,-40.5234096239519));
#254783=CARTESIAN_POINT('Ctrl Pts',(-44.1273541295014,30.414939058346,-40.5173753852017));
#254784=CARTESIAN_POINT('Ctrl Pts',(-44.1202325648852,30.4158161528369,
-40.5143941227858));
#254785=CARTESIAN_POINT('Ctrl Pts',(-44.0989269046614,30.418710900521,-40.5056018445424));
#254786=CARTESIAN_POINT('Ctrl Pts',(-44.0848361489451,30.4209852789275,
-40.4999555272545));
#254787=CARTESIAN_POINT('Ctrl Pts',(-44.0428355440345,30.4288357011986,
-40.4836289969086));
#254788=CARTESIAN_POINT('Ctrl Pts',(-44.001418907738,30.4387301387603,-40.4685417636913));
#254789=CARTESIAN_POINT('Ctrl Pts',(-43.9473552852602,30.4559806561897,
-40.4508995609031));
#254790=CARTESIAN_POINT('Ctrl Pts',(-43.9073915907435,30.4709642266074,
-40.4389183731711));
#254791=CARTESIAN_POINT('Ctrl Pts',(-43.8811432548962,30.4823370897352,
-40.4317784203789));
#254792=CARTESIAN_POINT('Ctrl Pts',(-43.8550972458946,30.4944149327137,
-40.4250719137776));
#254793=CARTESIAN_POINT('Ctrl Pts',(-43.8421555815742,30.5008203273088,
-40.4219325711588));
#254794=CARTESIAN_POINT('Ctrl Pts',(-43.8167947927211,30.5141840584711,
-40.4161689437405));
#254795=CARTESIAN_POINT('Ctrl Pts',(-43.8043130802594,30.5211703528968,
-40.413528034466));
#254796=CARTESIAN_POINT('Ctrl Pts',(-43.7797793173031,30.5357258010655,
-40.4087317905317));
#254797=CARTESIAN_POINT('Ctrl Pts',(-43.7436043213473,30.5584424906522,
-40.4022611528103));
#254798=CARTESIAN_POINT('Ctrl Pts',(-43.7092889915882,30.583786036936,-40.397944872434));
#254799=CARTESIAN_POINT('Ctrl Pts',(-43.6651994519323,30.6199287507259,
-40.394121352571));
#254800=CARTESIAN_POINT('Ctrl Pts',(-43.6439827068456,30.6391798378995,
-40.3931753351425));
#254801=CARTESIAN_POINT('Ctrl Pts',(-43.6032932824946,30.680108587057,-40.3932905044721));
#254802=CARTESIAN_POINT('Ctrl Pts',(-43.5841829799745,30.7014201645355,
-40.3943499059801));
#254803=CARTESIAN_POINT('Ctrl Pts',(-43.5483166082379,30.7456951818503,
-40.3983955355947));
#254804=CARTESIAN_POINT('Ctrl Pts',(-43.5148120542517,30.7916143604394,
-40.4043679292189));
#254805=CARTESIAN_POINT('Ctrl Pts',(-43.4859931451963,30.8408014772341,
-40.4141590917094));
#254806=CARTESIAN_POINT('Ctrl Pts',(-43.469474574758,30.8725808034089,-40.4214902069511));
#254807=CARTESIAN_POINT('Ctrl Pts',(-43.4662461658165,30.8789901287051,
-40.4230180755467));
#254808=CARTESIAN_POINT('Ctrl Pts',(-43.4599404108544,30.8919125782622,
-40.4261957226772));
#254809=CARTESIAN_POINT('Ctrl Pts',(-43.4568618652692,30.8984301381776,
-40.4278470523708));
#254810=CARTESIAN_POINT('Ctrl Pts',(-43.4479066843131,30.9180293597941,
-40.4329571814025));
#254811=CARTESIAN_POINT('Ctrl Pts',(-43.4366800830858,30.9443463169446,
-40.440199707327));
#254812=CARTESIAN_POINT('Ctrl Pts',(-43.4219268251392,30.9843790154574,
-40.4523233881121));
#254813=CARTESIAN_POINT('Ctrl Pts',(-43.4092278315493,31.0249558361973,
-40.4656821965631));
#254814=CARTESIAN_POINT('Ctrl Pts',(-43.3985649158327,31.0660734353404,
-40.4802626336878));
#254815=CARTESIAN_POINT('Ctrl Pts',(-43.3928117504253,31.0938450909326,
-40.4907938342908));
#254816=CARTESIAN_POINT('Ctrl Pts',(-43.3877402558097,31.1217978520093,
-40.5017316825792));
#254817=CARTESIAN_POINT('Ctrl Pts',(-43.3855448869231,31.1358715333473,
-40.5074069308404));
#254818=CARTESIAN_POINT('Ctrl Pts',(-43.3818466485176,31.1641754295066,
-40.5191561881817));
#254819=CARTESIAN_POINT('Ctrl Pts',(-43.3803394900793,31.1784722137567,
-40.5252598906186));
#254820=CARTESIAN_POINT('Ctrl Pts',(-43.3780514709974,31.2069533499868,
-40.5377524690855));
#254821=CARTESIAN_POINT('Ctrl Pts',(-43.3764764291988,31.2353806198054,
-40.5505518795279));
#254822=CARTESIAN_POINT('Ctrl Pts',(-43.3761228002374,31.292003207243,-40.577339198747));
#254823=CARTESIAN_POINT('Ctrl Pts',(-43.3798904844517,31.3482922086547,
-40.6058744004623));
#254824=CARTESIAN_POINT('Ctrl Pts',(-43.3877424304871,31.4042485256067,
-40.6361260433691));
#254825=CARTESIAN_POINT('Ctrl Pts',(-43.393042276717,31.4321193306868,-40.6518290622461));
#254826=CARTESIAN_POINT('Ctrl Pts',(-43.3990345440792,31.4599262492628,
-40.6678171709904));
#254827=CARTESIAN_POINT('Ctrl Pts',(-43.4023871385948,31.4738288295879,
-40.6759732487162));
#254828=CARTESIAN_POINT('Ctrl Pts',(-43.4097262599636,31.5013102698765,
-40.6924188649606));
#254829=CARTESIAN_POINT('Ctrl Pts',(-43.4137223958007,31.5149386860624,
-40.7007364096885));
#254830=CARTESIAN_POINT('Ctrl Pts',(-43.4266697743275,31.5554481319482,
-40.7259437634106));
#254831=CARTESIAN_POINT('Ctrl Pts',(-43.4365815013438,31.5819735775504,
-40.743098588818));
#254832=CARTESIAN_POINT('Ctrl Pts',(-43.453362100664,31.6210434116697,-40.7693485791028));
#254833=CARTESIAN_POINT('Ctrl Pts',(-43.4592720436944,31.6339404199602,
-40.77818065559));
#254834=CARTESIAN_POINT('Ctrl Pts',(-43.471748387858,31.6595177912398,-40.7960360397975));
#254835=CARTESIAN_POINT('Ctrl Pts',(-43.4782913690647,31.6721475181291,
-40.8050245716083));
#254836=CARTESIAN_POINT('Ctrl Pts',(-43.4987158872668,31.7093568101663,
-40.832021101787));
#254837=CARTESIAN_POINT('Ctrl Pts',(-43.5134312848982,31.7333600460206,
-40.8501267844669));
#254838=CARTESIAN_POINT('Ctrl Pts',(-43.5449969636312,31.7797747067972,
-40.8865288544817));
#254839=CARTESIAN_POINT('Ctrl Pts',(-43.570273480101,31.8133992725601,-40.9139774903764));
#254840=CARTESIAN_POINT('Ctrl Pts',(-43.6071874842548,31.8558549470217,
-40.9508682927202));
#254841=CARTESIAN_POINT('Ctrl Pts',(-43.6267265436653,31.8762775041081,
-40.9694100075909));
#254842=CARTESIAN_POINT('Ctrl Pts',(-43.6468212761471,31.8962967826001,
-40.9880061403947));
#254843=CARTESIAN_POINT('Ctrl Pts',(-43.6571524242715,31.9061057307006,
-40.997334528722));
#254844=CARTESIAN_POINT('Ctrl Pts',(-43.6781351765956,31.9250932263188,
-41.0158316653051));
#254845=CARTESIAN_POINT('Ctrl Pts',(-43.6888325213991,31.9343181422645,
-41.0250431278314));
#254846=CARTESIAN_POINT('Ctrl Pts',(-43.7214683281725,31.961133026229,-41.0525078158304));
#254847=CARTESIAN_POINT('Ctrl Pts',(-43.744000771517,31.977916302359,-41.070639272709));
#254848=CARTESIAN_POINT('Ctrl Pts',(-43.7905699795511,32.0092811177654,
-41.106520902203));
#254849=CARTESIAN_POINT('Ctrl Pts',(-43.8266341229871,32.0311632771839,
-41.1331548827895));
#254850=CARTESIAN_POINT('Ctrl Pts',(-43.8644344365312,32.050527928199,-41.1593656410909));
#254851=CARTESIAN_POINT('Ctrl Pts',(-43.8900335656271,32.0628690313763,
-41.1767476889401));
#254852=CARTESIAN_POINT('Ctrl Pts',(-43.903042008964,32.0687560539784,-41.1853974312384));
#254853=CARTESIAN_POINT('Ctrl Pts',(-43.9291618902095,32.0798229381751,
-41.2024070088898));
#254854=CARTESIAN_POINT('Ctrl Pts',(-43.9423286751247,32.0850301956599,
-41.2108047653586));
#254855=CARTESIAN_POINT('Ctrl Pts',(-43.9688389276373,32.0947834481969,
-41.2273662374836));
#254856=CARTESIAN_POINT('Ctrl Pts',(-44.0088868242005,32.1084293286422,
-41.2518690158044));
#254857=CARTESIAN_POINT('Ctrl Pts',(-44.0634057706764,32.1227159830699,
-41.2831968728749));
#254858=CARTESIAN_POINT('Ctrl Pts',(-44.1051448739617,32.1304686073096,
-41.30568419746));
#254859=CARTESIAN_POINT('Ctrl Pts',(-44.1331632182567,32.1349666221674,
-41.3204486001008));
#254860=CARTESIAN_POINT('Ctrl Pts',(-44.1472622735965,32.1368798783668,
-41.3277141420552));
#254861=CARTESIAN_POINT('Ctrl Pts',(-44.1685768983456,32.1392377391899,
-41.3384485067576));
#254862=CARTESIAN_POINT('Ctrl Pts',(-44.1757038998442,32.1399371964,-41.3419962566417));
#254863=CARTESIAN_POINT('Ctrl Pts',(-44.1899298892594,32.1411565650423,
-41.3489954369734));
#254864=CARTESIAN_POINT('Ctrl Pts',(-44.1970429564213,32.1416781032566,
-41.3524539903966));
#254865=CARTESIAN_POINT('Ctrl Pts',(-44.2183581262916,32.1429776302475,
-41.3626954949199));
#254866=CARTESIAN_POINT('Ctrl Pts',(-44.232556678806,32.1434929542666,-41.3693546778539));
#254867=CARTESIAN_POINT('Ctrl Pts',(-44.2750884056492,32.1439936324359,
-41.3888189062651));
#254868=CARTESIAN_POINT('Ctrl Pts',(-44.3033804172497,32.1429384256622,
-41.4011231160504));
#254869=CARTESIAN_POINT('Ctrl Pts',(-44.3598247343314,32.13804594572,-41.4243882373187));
#254870=CARTESIAN_POINT('Ctrl Pts',(-44.3879848006206,32.1342064546963,
-41.4353516241949));
#254871=CARTESIAN_POINT('Ctrl Pts',(-44.4230841862873,32.1276226980045,
-41.4481948195873));
#254872=CARTESIAN_POINT('Ctrl Pts',(-44.4301039616143,32.126214419323,-41.4507215814638));
#254873=CARTESIAN_POINT('Ctrl Pts',(-44.4441256434231,32.1232190082407,
-41.455685422358));
#254874=CARTESIAN_POINT('Ctrl Pts',(-44.4511413829898,32.1216281453652,
-41.4581270453932));
#254875=CARTESIAN_POINT('Ctrl Pts',(-44.472106554004,32.1165956901708,-41.4652964871519));
#254876=CARTESIAN_POINT('Ctrl Pts',(-44.4859328208737,32.1129061786889,
-41.4698557698741));
#254877=CARTESIAN_POINT('Ctrl Pts',(-44.5270324780087,32.1008340938932,
-41.4829067838587));
#254878=CARTESIAN_POINT('Ctrl Pts',(-44.5673316800757,32.08677017453,-41.4946921125766));
#254879=CARTESIAN_POINT('Ctrl Pts',(-44.6194780799712,32.0640738471498,
-41.5079096337926));
#254880=CARTESIAN_POINT('Ctrl Pts',(-44.6577884739158,32.045065905176,-41.5165678887371));
#254881=CARTESIAN_POINT('Ctrl Pts',(-44.6827916371924,32.031050813041,-41.5214942665077));
#254882=CARTESIAN_POINT('Ctrl Pts',(-44.7075150580676,32.0163554529027,
-41.5259894017533));
#254883=CARTESIAN_POINT('Ctrl Pts',(-44.7197631353705,32.0086467826241,
-41.5280237577537));
#254884=CARTESIAN_POINT('Ctrl Pts',(-44.7436779765282,31.9927322821733,
-41.5316086326721));
#254885=CARTESIAN_POINT('Ctrl Pts',(-44.7554039451266,31.9844926239501,
-41.5331705278033));
#254886=CARTESIAN_POINT('Ctrl Pts',(-44.7783650010144,31.9674779303508,
-41.5358342782831));
#254887=CARTESIAN_POINT('Ctrl Pts',(-44.8120876763637,31.941142023486,-41.5391427937509));
#254888=CARTESIAN_POINT('Ctrl Pts',(-44.8542060542843,31.9028069711657,
-41.5408368316843));
#254889=CARTESIAN_POINT('Ctrl Pts',(-44.883650374082,31.8716290815775,-41.5400605624154));
#254890=CARTESIAN_POINT('Ctrl Pts',(-44.9027957424029,31.8502960261458,
-41.5390808606534));
#254891=CARTESIAN_POINT('Ctrl Pts',(-44.912124025092,31.8393588588263,-41.5383603441012));
#254892=CARTESIAN_POINT('Ctrl Pts',(-44.9302963003321,31.816913187918,-41.5364463589967));
#254893=CARTESIAN_POINT('Ctrl Pts',(-44.9390653236876,31.8054960967264,
-41.5352602514373));
#254894=CARTESIAN_POINT('Ctrl Pts',(-44.9559494861592,31.7823260274566,
-41.532444286592));
#254895=CARTESIAN_POINT('Ctrl Pts',(-44.9803129684955,31.7470436123751,
-41.5275522735743));
#254896=CARTESIAN_POINT('Ctrl Pts',(-45.00183725318,31.7102129370948,-41.5206914933375));
#254897=CARTESIAN_POINT('Ctrl Pts',(-45.0280427451288,31.6597446570548,
-41.5098099510806));
#254898=CARTESIAN_POINT('Ctrl Pts',(-45.0398987329805,31.6338241168053,
-41.5034995556801));
#254899=CARTESIAN_POINT('Ctrl Pts',(-45.0531290598229,31.6005723463994,
-41.4945098705711));
#254900=CARTESIAN_POINT('Ctrl Pts',(-45.0556963147994,31.5938738844661,
-41.4926546478805));
#254901=CARTESIAN_POINT('Ctrl Pts',(-45.0606676096559,31.5803990532317,
-41.4888352403062));
#254902=CARTESIAN_POINT('Ctrl Pts',(-45.0630762139805,31.5736079348959,
-41.4868664774371));
#254903=CARTESIAN_POINT('Ctrl Pts',(-45.0700329505347,31.5531765604049,
-41.4808121016924));
#254904=CARTESIAN_POINT('Ctrl Pts',(-45.0743018132827,31.5395152309552,
-41.4765904297482));
#254905=CARTESIAN_POINT('Ctrl Pts',(-45.0860497029301,31.4983488303989,
-41.4633620161014));
#254906=CARTESIAN_POINT('Ctrl Pts',(-45.0988767040151,31.4430340104486,
-41.4442426901641));
#254907=CARTESIAN_POINT('Ctrl Pts',(-45.1061818129997,31.386882792419,-41.4222207481485));
#254908=CARTESIAN_POINT('Ctrl Pts',(-45.1095857869151,31.3444641027996,
-41.4046111316328));
#254909=CARTESIAN_POINT('Ctrl Pts',(-45.1103739871937,31.3302675876129,
-41.3985560195248));
#254910=CARTESIAN_POINT('Ctrl Pts',(-45.1110306052012,31.30890259785,-41.3891987399731));
#254911=CARTESIAN_POINT('Ctrl Pts',(-45.1111617199316,31.3017636946428,
-41.3860313075819));
#254912=CARTESIAN_POINT('Ctrl Pts',(-45.1112472734604,31.2874686716035,
-41.3796068875509));
#254913=CARTESIAN_POINT('Ctrl Pts',(-45.111201351958,31.2802974166487,-41.3763428889219));
#254914=CARTESIAN_POINT('Ctrl Pts',(-45.1107973541963,31.25882908612,-41.3664479958234));
#254915=CARTESIAN_POINT('Ctrl Pts',(-45.11017580813,31.2446005169708,-41.3597259135069));
#254916=CARTESIAN_POINT('Ctrl Pts',(-45.1082442962718,31.2162677536902,
-41.3460176286356));
#254917=CARTESIAN_POINT('Ctrl Pts',(-45.104314463686,31.1739750543259,-41.3250680443717));
#254918=CARTESIAN_POINT('Ctrl Pts',(-45.0950241996196,31.1183949914011,
-41.295609869938));
#254919=CARTESIAN_POINT('Ctrl Pts',(-45.0817381040079,31.0636149263882,
-41.264634106957));
#254920=CARTESIAN_POINT('Ctrl Pts',(-45.0737554763462,31.0364928582332,
-41.2486352837062));
#254921=CARTESIAN_POINT('Ctrl Pts',(-45.0650963255467,31.0095068957897,
-41.2323777508457));
#254922=CARTESIAN_POINT('Ctrl Pts',(-45.0604265398991,30.996076905732,-41.224116427314));
#254923=CARTESIAN_POINT('Ctrl Pts',(-45.0504049610752,30.9693743366894,
-41.2073411015006));
#254924=CARTESIAN_POINT('Ctrl Pts',(-45.0450945767524,30.9562107421528,
-41.1988958018751));
#254925=CARTESIAN_POINT('Ctrl Pts',(-45.0394875320819,30.9432190801919,
-41.190386719266));
#254926=CARTESIAN_POINT('Ctrl Pts',(-45.3466072487201,32.9831474726814,
-40.3575667765884));
#254927=CARTESIAN_POINT('Ctrl Pts',(-45.4775804476444,32.9506416230843,
-40.3279308140717));
#254928=CARTESIAN_POINT('Ctrl Pts',(-45.6018489459591,32.8970303670972,
-40.3018706355002));
#254929=CARTESIAN_POINT('Ctrl Pts',(-45.7930510520033,32.7694772175728,
-40.2654024161569));
#254930=CARTESIAN_POINT('Ctrl Pts',(-45.8648371032935,32.7073974754499,
-40.2528314281289));
#254931=CARTESIAN_POINT('Ctrl Pts',(-45.9708819323183,32.5885937141489,
-40.236033098347));
#254932=CARTESIAN_POINT('Ctrl Pts',(-46.0094601394925,32.5369923640417,
-40.2304669096557));
#254933=CARTESIAN_POINT('Ctrl Pts',(-46.0443914997218,32.4808275965294,
-40.2259504969968));
#254934=CARTESIAN_POINT('Ctrl Pts',(-46.0453687463461,32.4792476132019,
-40.2258246312621));
#254935=CARTESIAN_POINT('Ctrl Pts',(-46.0482994498696,32.4744830235869,
-40.2254486323447));
#254936=CARTESIAN_POINT('Ctrl Pts',(-46.0502410390434,32.4712910039402,
-40.2252015084794));
#254937=CARTESIAN_POINT('Ctrl Pts',(-46.0560808750791,32.4615817586325,
-40.22446420935));
#254938=CARTESIAN_POINT('Ctrl Pts',(-46.0599292529414,32.455034611037,-40.2239865664018));
#254939=CARTESIAN_POINT('Ctrl Pts',(-46.0675639706264,32.4417408317884,
-40.2230555504732));
#254940=CARTESIAN_POINT('Ctrl Pts',(-46.0713470910329,32.4349941460753,
-40.222602877568));
#254941=CARTESIAN_POINT('Ctrl Pts',(-46.110523107097,32.3634224247021,-40.218006074707));
#254942=CARTESIAN_POINT('Ctrl Pts',(-46.1395815298695,32.2953942994941,
-40.2153865540286));
#254943=CARTESIAN_POINT('Ctrl Pts',(-46.2069461227329,32.0848150750412,
-40.2116780528921));
#254944=CARTESIAN_POINT('Ctrl Pts',(-46.2252178127257,31.9383772329122,
-40.2146552898855));
#254945=CARTESIAN_POINT('Ctrl Pts',(-46.2146419207919,31.6745946451145,
-40.2265788965334));
#254946=CARTESIAN_POINT('Ctrl Pts',(-46.1952499881773,31.576162819291,-40.2334689298899));
#254947=CARTESIAN_POINT('Ctrl Pts',(-46.1762418209585,31.5014470256211,
-40.2388224305403));
#254948=CARTESIAN_POINT('Ctrl Pts',(-46.6981266849492,30.7091523375488,
-39.2904704603133));
#254949=CARTESIAN_POINT('Ctrl Pts',(-46.6689684123063,30.6404043382273,
-39.273452295095));
#254950=CARTESIAN_POINT('Ctrl Pts',(-46.6043681216411,30.5066861069553,
-39.238925705885));
#254951=CARTESIAN_POINT('Ctrl Pts',(-46.5083209189471,30.3487389562033,
-39.1945593129175));
#254952=CARTESIAN_POINT('Ctrl Pts',(-46.4437937583117,30.2581216171786,
-39.1673894861782));
#254953=CARTESIAN_POINT('Ctrl Pts',(-46.3992224148768,30.1986447451181,
-39.1491520227249));
#254954=CARTESIAN_POINT('Ctrl Pts',(-46.3761748773305,30.1693908446446,
-39.1399767764946));
#254955=CARTESIAN_POINT('Ctrl Pts',(-46.3284414024809,30.1117648114071,
-39.1214771434543));
#254956=CARTESIAN_POINT('Ctrl Pts',(-46.3038983378397,30.083571828401,-39.112209259666));
#254957=CARTESIAN_POINT('Ctrl Pts',(-46.253707387608,30.0286632749651,-39.0937226519629));
#254958=CARTESIAN_POINT('Ctrl Pts',(-46.2280147026909,30.001893564456,-39.0844865568113));
#254959=CARTESIAN_POINT('Ctrl Pts',(-46.1492148010453,29.9236586721517,
-39.0568159196779));
#254960=CARTESIAN_POINT('Ctrl Pts',(-46.0669347173688,29.8495134741745,
-39.0292038481275));
#254961=CARTESIAN_POINT('Ctrl Pts',(-45.9503410384262,29.7587889734315,
-38.9925114043613));
#254962=CARTESIAN_POINT('Ctrl Pts',(-45.8594191065401,29.6948377475824,
-38.9650526418885));
#254963=CARTESIAN_POINT('Ctrl Pts',(-45.7964751089327,29.6549785818455,
-38.9467936623891));
#254964=CARTESIAN_POINT('Ctrl Pts',(-45.748348603817,29.6261284949947,-38.9331097524421));
#254965=CARTESIAN_POINT('Ctrl Pts',(-45.7321473284057,29.616684052073,-38.9285487676403));
#254966=CARTESIAN_POINT('Ctrl Pts',(-45.6996106203311,29.5982459977232,
-38.9194791520014));
#254967=CARTESIAN_POINT('Ctrl Pts',(-45.683249044345,29.5892352448745,-38.9149628379356));
#254968=CARTESIAN_POINT('Ctrl Pts',(-45.6010439155842,29.5452684013657,
-38.8924942188443));
#254969=CARTESIAN_POINT('Ctrl Pts',(-45.4667739830181,29.4816584171599,
-38.8571935516581));
#254970=CARTESIAN_POINT('Ctrl Pts',(-45.2922645146651,29.4187721922835,
-38.8147007629208));
#254971=CARTESIAN_POINT('Ctrl Pts',(-45.184512437616,29.3885937253944,-38.7899522655792));
#254972=CARTESIAN_POINT('Ctrl Pts',(-45.1119891467798,29.3701842541612,
-38.7736235920333));
#254973=CARTESIAN_POINT('Ctrl Pts',(-45.0754052578815,29.3618381514785,
-38.7655490803555));
#254974=CARTESIAN_POINT('Ctrl Pts',(-45.0014447932705,29.3468760834356,
-38.7495561846596));
#254975=CARTESIAN_POINT('Ctrl Pts',(-44.964301863367,29.3403115562353,-38.7416890516424));
#254976=CARTESIAN_POINT('Ctrl Pts',(-44.8900079594565,29.3290481892184,
-38.726277749838));
#254977=CARTESIAN_POINT('Ctrl Pts',(-44.8527936282157,29.324336495618,-38.7187198739728));
#254978=CARTESIAN_POINT('Ctrl Pts',(-44.7410083373266,29.3129455735289,
-38.6964994820139));
#254979=CARTESIAN_POINT('Ctrl Pts',(-44.6662563757167,29.3089967422249,
-38.6822807693139));
#254980=CARTESIAN_POINT('Ctrl Pts',(-44.516312468428,29.3084067934202,-38.6550493453909));
#254981=CARTESIAN_POINT('Ctrl Pts',(-44.441103189525,29.3117700143417,-38.6420342479066));
#254982=CARTESIAN_POINT('Ctrl Pts',(-44.3468378615956,29.3206690055189,
-38.6265520162729));
#254983=CARTESIAN_POINT('Ctrl Pts',(-44.3279589148655,29.3226883315868,
-38.6234933649988));
#254984=CARTESIAN_POINT('Ctrl Pts',(-44.2901960653062,29.3271995080042,
-38.6174591262491));
#254985=CARTESIAN_POINT('Ctrl Pts',(-44.271274393292,29.329697893027,-38.614477863833));
#254986=CARTESIAN_POINT('Ctrl Pts',(-44.2146592782019,29.3378915995821,
-38.60568558559));
#254987=CARTESIAN_POINT('Ctrl Pts',(-44.1772069502033,29.344266758826,-38.6000392683017));
#254988=CARTESIAN_POINT('Ctrl Pts',(-44.0655444875092,29.3661148598052,
-38.5837127379559));
#254989=CARTESIAN_POINT('Ctrl Pts',(-43.9553791862171,29.3933792052515,
-38.5686255047386));
#254990=CARTESIAN_POINT('Ctrl Pts',(-43.8114622524781,29.4404829778103,
-38.5509833019505));
#254991=CARTESIAN_POINT('Ctrl Pts',(-43.705021834675,29.481230340464,-38.5390021142185));
#254992=CARTESIAN_POINT('Ctrl Pts',(-43.6350719757086,29.512061063653,-38.5318621614261));
#254993=CARTESIAN_POINT('Ctrl Pts',(-43.5656410085295,29.5447591316771,
-38.525155654825));
#254994=CARTESIAN_POINT('Ctrl Pts',(-43.5311320054746,29.5620794464364,
-38.5220163122062));
#254995=CARTESIAN_POINT('Ctrl Pts',(-43.4634866412134,29.5981758355574,
-38.5162526847879));
#254996=CARTESIAN_POINT('Ctrl Pts',(-43.4301834663392,29.6170276546,-38.5136117755133));
#254997=CARTESIAN_POINT('Ctrl Pts',(-43.3647025891651,29.6562685687332,
-38.5088155315793));
#254998=CARTESIAN_POINT('Ctrl Pts',(-43.2681192378476,29.7174608121974,
-38.5023448938576));
#254999=CARTESIAN_POINT('Ctrl Pts',(-43.1764049274077,29.7855824582168,
-38.4980286134812));
#255000=CARTESIAN_POINT('Ctrl Pts',(-43.0584774180437,29.8826126224142,
-38.4942050936184));
#255001=CARTESIAN_POINT('Ctrl Pts',(-43.001681818637,29.9342392650769,-38.4932590761897));
#255002=CARTESIAN_POINT('Ctrl Pts',(-42.8926599718677,30.0438904492243,
-38.4933742455196));
#255003=CARTESIAN_POINT('Ctrl Pts',(-42.8414047150844,30.1009342501745,
-38.4944336470273));
#255004=CARTESIAN_POINT('Ctrl Pts',(-42.7451036203247,30.2193471227021,
-38.498479276642));
#255005=CARTESIAN_POINT('Ctrl Pts',(-42.6550322643363,30.3420646399833,
-38.5044516702661));
#255006=CARTESIAN_POINT('Ctrl Pts',(-42.5773225406025,30.4733365238586,
-38.5142428327574));
#255007=CARTESIAN_POINT('Ctrl Pts',(-42.5326943378214,30.5580963840027,
-38.5215739479982));
#255008=CARTESIAN_POINT('Ctrl Pts',(-42.5239673850246,30.5751883092729,
-38.5231018165939));
#255009=CARTESIAN_POINT('Ctrl Pts',(-42.5069121510755,30.60964376351,-38.5262794637242));
#255010=CARTESIAN_POINT('Ctrl Pts',(-42.4985805781952,30.627019094627,-38.5279307934181));
#255011=CARTESIAN_POINT('Ctrl Pts',(-42.4743295471271,30.6792614198295,
-38.5330409224498));
#255012=CARTESIAN_POINT('Ctrl Pts',(-42.4438856226513,30.7493896366731,
-38.5402834483744));
#255013=CARTESIAN_POINT('Ctrl Pts',(-42.4037483179465,30.8560072598611,
-38.5524071291592));
#255014=CARTESIAN_POINT('Ctrl Pts',(-42.3690543371876,30.9640160484273,
-38.5657659376104));
#255015=CARTESIAN_POINT('Ctrl Pts',(-42.3397558527982,31.0734075527136,
-38.5803463747351));
#255016=CARTESIAN_POINT('Ctrl Pts',(-42.3238156343608,31.1472555030051,
-38.5908775753381));
#255017=CARTESIAN_POINT('Ctrl Pts',(-42.3096820427396,31.2215665449467,
-38.6018154236264));
#255018=CARTESIAN_POINT('Ctrl Pts',(-42.3035171869091,31.2589715314082,
-38.6074906718877));
#255019=CARTESIAN_POINT('Ctrl Pts',(-42.2930235524414,31.3341791410138,
-38.6192399292287));
#255020=CARTESIAN_POINT('Ctrl Pts',(-42.2886818075092,31.3721585359098,
-38.6253436316658));
#255021=CARTESIAN_POINT('Ctrl Pts',(-42.281930630611,31.4478003630713,-38.6378362101326));
#255022=CARTESIAN_POINT('Ctrl Pts',(-42.277074994566,31.5232809912004,-38.6506356205751));
#255023=CARTESIAN_POINT('Ctrl Pts',(-42.2747992363309,31.6735553614761,
-38.6774229397946));
#255024=CARTESIAN_POINT('Ctrl Pts',(-42.2834818483937,31.8228397562226,
-38.7059581415094));
#255025=CARTESIAN_POINT('Ctrl Pts',(-42.3030248127084,31.9711385758679,
-38.7362097844166));
#255026=CARTESIAN_POINT('Ctrl Pts',(-42.3164494406915,32.0449687602614,
-38.7519128032936));
#255027=CARTESIAN_POINT('Ctrl Pts',(-42.3317154579634,32.1186122141692,
-38.7679009120377));
#255028=CARTESIAN_POINT('Ctrl Pts',(-42.3402956643805,32.1554227583218,
-38.7760569897633));
#255029=CARTESIAN_POINT('Ctrl Pts',(-42.3591481714288,32.228169160774,-38.7925026060078));
#255030=CARTESIAN_POINT('Ctrl Pts',(-42.3694448348212,32.2642362896146,
-38.8008201507359));
#255031=CARTESIAN_POINT('Ctrl Pts',(-42.4028917825415,32.3714169561226,
-38.8260275044574));
#255032=CARTESIAN_POINT('Ctrl Pts',(-42.428602574983,32.4415633880281,-38.8431823298655));
#255033=CARTESIAN_POINT('Ctrl Pts',(-42.4722685042023,32.5448307979217,
-38.8694323201497));
#255034=CARTESIAN_POINT('Ctrl Pts',(-42.4876674804306,32.5789105800712,
-38.8782643966373));
#255035=CARTESIAN_POINT('Ctrl Pts',(-42.5202146590728,32.6464795812123,
-38.8961197808447));
#255036=CARTESIAN_POINT('Ctrl Pts',(-42.5373018269229,32.6798350022668,
-38.9051083126545));
#255037=CARTESIAN_POINT('Ctrl Pts',(-42.5906929412925,32.7780783962456,
-38.9321048428364));
#255038=CARTESIAN_POINT('Ctrl Pts',(-42.629225789877,32.8414173722334,-38.9502105255135));
#255039=CARTESIAN_POINT('Ctrl Pts',(-42.7120000069194,32.9638220552461,
-38.9866125955294));
#255040=CARTESIAN_POINT('Ctrl Pts',(-42.7783647966162,33.0524402968179,
-39.0140612314234));
#255041=CARTESIAN_POINT('Ctrl Pts',(-42.8754380724448,33.1642175243331,
-39.0509520337677));
#255042=CARTESIAN_POINT('Ctrl Pts',(-42.9268673384212,33.2179450225078,
-39.0694937486382));
#255043=CARTESIAN_POINT('Ctrl Pts',(-42.9797817061918,33.2705900457306,
-39.088089881442));
#255044=CARTESIAN_POINT('Ctrl Pts',(-43.0069972096607,33.2963736994336,
-39.097418269769));
#255045=CARTESIAN_POINT('Ctrl Pts',(-43.0622936398443,33.3462615369726,
-39.1159154063528));
#255046=CARTESIAN_POINT('Ctrl Pts',(-43.0904949946047,33.3704876748183,
-39.1251268688783));
#255047=CARTESIAN_POINT('Ctrl Pts',(-43.176562606447,33.4408730143712,-39.1525915568785));
#255048=CARTESIAN_POINT('Ctrl Pts',(-43.2360245534179,33.4848790444095,
-39.1707230137558));
#255049=CARTESIAN_POINT('Ctrl Pts',(-43.358992255749,33.5670176609587,-39.2066046432507));
#255050=CARTESIAN_POINT('Ctrl Pts',(-43.4542745623933,33.6242424638975,
-39.233238623837));
#255051=CARTESIAN_POINT('Ctrl Pts',(-43.5542222374601,33.6747516510336,
-39.2594493821381));
#255052=CARTESIAN_POINT('Ctrl Pts',(-43.6219256430316,33.7069073870393,
-39.2768314299875));
#255053=CARTESIAN_POINT('Ctrl Pts',(-43.6563381479934,33.7222286468184,
-39.2854811722856));
#255054=CARTESIAN_POINT('Ctrl Pts',(-43.7254519170511,33.7509934760635,
-39.3024907499371));
#255055=CARTESIAN_POINT('Ctrl Pts',(-43.7602995448845,33.7645084608315,
-39.3108885064059));
#255056=CARTESIAN_POINT('Ctrl Pts',(-43.8304781084082,33.789780836939,-39.3274499785309));
#255057=CARTESIAN_POINT('Ctrl Pts',(-43.9365171946568,33.8250735562425,
-39.3519527568515));
#255058=CARTESIAN_POINT('Ctrl Pts',(-44.0809642638621,33.8617420360433,
-39.3832806139221));
#255059=CARTESIAN_POINT('Ctrl Pts',(-44.1916183723467,33.8813683146414,
-39.4057679385072));
#255060=CARTESIAN_POINT('Ctrl Pts',(-44.2659122959159,33.8926702964892,
-39.4205323411483));
#255061=CARTESIAN_POINT('Ctrl Pts',(-44.3033049221432,33.8974288658374,
-39.4277978831022));
#255062=CARTESIAN_POINT('Ctrl Pts',(-44.3598453576919,33.9032050944765,
-39.4385322478049));
#255063=CARTESIAN_POINT('Ctrl Pts',(-44.3787527158677,33.9049006163346,
-39.4420799976889));
#255064=CARTESIAN_POINT('Ctrl Pts',(-44.4164967874688,33.9078161173588,
-39.4490791780208));
#255065=CARTESIAN_POINT('Ctrl Pts',(-44.4353708468856,33.9090400957878,
-39.4525377314439));
#255066=CARTESIAN_POINT('Ctrl Pts',(-44.4919347179527,33.9120095261765,
-39.462779235967));
#255067=CARTESIAN_POINT('Ctrl Pts',(-44.52962054914,33.9130584408517,-39.4694384189012));
#255068=CARTESIAN_POINT('Ctrl Pts',(-44.6425299001817,33.9134342925821,
-39.4889026473125));
#255069=CARTESIAN_POINT('Ctrl Pts',(-44.7176656228988,33.9100023852834,
-39.5012068570978));
#255070=CARTESIAN_POINT('Ctrl Pts',(-44.867623327666,33.8957625538083,-39.524471978366));
#255071=CARTESIAN_POINT('Ctrl Pts',(-44.9424659600731,33.8849485744664,
-39.5354353652432));
#255072=CARTESIAN_POINT('Ctrl Pts',(-45.0357885152669,33.8666999843662,
-39.5482785606344));
#255073=CARTESIAN_POINT('Ctrl Pts',(-45.0544546343785,33.8628074782943,
-39.5508053225112));
#255074=CARTESIAN_POINT('Ctrl Pts',(-45.091743102575,33.8545484160302,-39.5557691634051));
#255075=CARTESIAN_POINT('Ctrl Pts',(-45.1104022544846,33.850171655015,-39.5582107864407));
#255076=CARTESIAN_POINT('Ctrl Pts',(-45.1661672125598,33.8363538303533,
-39.5653802281989));
#255077=CARTESIAN_POINT('Ctrl Pts',(-45.2029511118778,33.8262578362557,
-39.5699395109212));
#255078=CARTESIAN_POINT('Ctrl Pts',(-45.312316831343,33.7933159380614,-39.582990524906));
#255079=CARTESIAN_POINT('Ctrl Pts',(-45.4195983160475,33.7551076509549,
-39.5947758536238));
#255080=CARTESIAN_POINT('Ctrl Pts',(-45.5585113890164,33.6937328563153,
-39.6079933748399));
#255081=CARTESIAN_POINT('Ctrl Pts',(-45.6606150024606,33.6424505696195,
-39.6166516297843));
#255082=CARTESIAN_POINT('Ctrl Pts',(-45.7272860947277,33.6047101271221,
-39.6215780075552));
#255083=CARTESIAN_POINT('Ctrl Pts',(-45.7932287365117,33.5651705839516,
-39.6260731428005));
#255084=CARTESIAN_POINT('Ctrl Pts',(-45.8259059249178,33.5444453395394,
-39.6281074988013));
#255085=CARTESIAN_POINT('Ctrl Pts',(-45.8897275017006,33.5016881508368,
-39.6316923737189));
#255086=CARTESIAN_POINT('Ctrl Pts',(-45.9210297733036,33.4795651380848,
-39.6332542688506));
#255087=CARTESIAN_POINT('Ctrl Pts',(-45.9823424846244,33.4339088874735,
-39.6359180193303));
#255088=CARTESIAN_POINT('Ctrl Pts',(-46.0724202597563,33.3632801300718,
-39.6392265347984));
#255089=CARTESIAN_POINT('Ctrl Pts',(-46.1850394564173,33.2606222983665,
-39.6409205727319));
#255090=CARTESIAN_POINT('Ctrl Pts',(-46.2638636333332,33.1772336958075,
-39.6401443034625));
#255091=CARTESIAN_POINT('Ctrl Pts',(-46.3151397511292,33.1201974856456,
-39.6391646017005));
#255092=CARTESIAN_POINT('Ctrl Pts',(-46.3401349353408,33.0909661742941,
-39.6384440851485));
#255093=CARTESIAN_POINT('Ctrl Pts',(-46.3888523044997,33.0309971480077,
-39.6365301000439));
#255094=CARTESIAN_POINT('Ctrl Pts',(-46.4123735341802,33.0005036828642,
-39.6353439924849));
#255095=CARTESIAN_POINT('Ctrl Pts',(-46.4576879006691,32.9386388625828,
-39.6325280276393));
#255096=CARTESIAN_POINT('Ctrl Pts',(-46.52311576659,32.8444620833496,-39.6276360146217));
#255097=CARTESIAN_POINT('Ctrl Pts',(-46.5810426872604,32.7462345994881,
-39.6207752343847));
#255098=CARTESIAN_POINT('Ctrl Pts',(-46.6516918187307,32.6117039458857,
-39.6098936921283));
#255099=CARTESIAN_POINT('Ctrl Pts',(-46.683723185051,32.5426422373878,-39.6035832967262));
#255100=CARTESIAN_POINT('Ctrl Pts',(-46.7195635412788,32.4540883209461,
-39.5945936116187));
#255101=CARTESIAN_POINT('Ctrl Pts',(-46.7265235775841,32.4362514419463,
-39.5927383889278));
#255102=CARTESIAN_POINT('Ctrl Pts',(-46.7400123459627,32.4003742100513,
-39.5889189813535));
#255103=CARTESIAN_POINT('Ctrl Pts',(-46.7465535157541,32.3822946053341,
-39.5869502184844));
#255104=CARTESIAN_POINT('Ctrl Pts',(-46.7654644360989,32.3279072933142,
-39.5808958427402));
#255105=CARTESIAN_POINT('Ctrl Pts',(-46.7770937339888,32.2915493874551,
-39.5766741707955));
#255106=CARTESIAN_POINT('Ctrl Pts',(-46.8091770518909,32.182013131159,-39.5634457571489));
#255107=CARTESIAN_POINT('Ctrl Pts',(-46.8444383818759,32.034891308334,-39.5443264312115));
#255108=CARTESIAN_POINT('Ctrl Pts',(-46.8650708643864,31.8856621776612,
-39.5223044891954));
#255109=CARTESIAN_POINT('Ctrl Pts',(-46.8750487417844,31.7729724844591,
-39.50469487268));
#255110=CARTESIAN_POINT('Ctrl Pts',(-46.8774570362353,31.7352651712118,
-39.4986397605723));
#255111=CARTESIAN_POINT('Ctrl Pts',(-46.8796767940079,31.6785286095959,
-39.4892824810203));
#255112=CARTESIAN_POINT('Ctrl Pts',(-46.8801843407089,31.6595724593507,
-39.4861150486293));
#255113=CARTESIAN_POINT('Ctrl Pts',(-46.8807312344332,31.6216180949417,
-39.479690628598));
#255114=CARTESIAN_POINT('Ctrl Pts',(-46.8807699646674,31.6025797052015,
-39.4764266299692));
#255115=CARTESIAN_POINT('Ctrl Pts',(-46.8801790388754,31.5455906639181,
-39.4665317368708));
#255116=CARTESIAN_POINT('Ctrl Pts',(-46.8788490796135,31.5078273383739,
-39.4598096545541));
#255117=CARTESIAN_POINT('Ctrl Pts',(-46.874360617844,31.4326451774338,-39.4461013696832));
#255118=CARTESIAN_POINT('Ctrl Pts',(-46.864884835636,31.320441459725,-39.4251517854185));
#255119=CARTESIAN_POINT('Ctrl Pts',(-46.8414902947658,31.1730719473388,
-39.3956936109857));
#255120=CARTESIAN_POINT('Ctrl Pts',(-46.8074810934279,31.0279105813681,
-39.364717848004));
#255121=CARTESIAN_POINT('Ctrl Pts',(-46.7869180083019,30.9560697433081,
-39.3487190247537));
#255122=CARTESIAN_POINT('Ctrl Pts',(-46.7645577771926,30.884604709384,-39.332461491893));
#255123=CARTESIAN_POINT('Ctrl Pts',(-46.7524740339114,30.8490466969583,
-39.3242001683612));
#255124=CARTESIAN_POINT('Ctrl Pts',(-46.7264943673172,30.7783632715819,
-39.3074248425479));
#255125=CARTESIAN_POINT('Ctrl Pts',(-46.7127058212706,30.7435263372096,
-39.2989795429224));
#255126=CARTESIAN_POINT('Ctrl Pts',(-46.6981266849492,30.7091523375488,
-39.2904704603133));
#255127=CARTESIAN_POINT('Ctrl Pts',(-45.0394875320819,30.9432190801919,
-41.190386719266));
#255128=CARTESIAN_POINT('Ctrl Pts',(-45.0282734427409,30.91723575627,-41.1733685540478));
#255129=CARTESIAN_POINT('Ctrl Pts',(-45.0034876660128,30.8666726764904,
-41.1388419648381));
#255130=CARTESIAN_POINT('Ctrl Pts',(-44.9667665375866,30.8068862988478,
-41.09447557187));
#255131=CARTESIAN_POINT('Ctrl Pts',(-44.9421458413835,30.7725558756156,
-41.0673057451311));
#255132=CARTESIAN_POINT('Ctrl Pts',(-44.9251493960809,30.7500159625169,
-41.0490682816776));
#255133=CARTESIAN_POINT('Ctrl Pts',(-44.9163654668634,30.7389260450349,
-41.0398930354472));
#255134=CARTESIAN_POINT('Ctrl Pts',(-44.8981827131164,30.7170729960788,
-41.0213934024069));
#255135=CARTESIAN_POINT('Ctrl Pts',(-44.888838333634,30.7063777841388,-41.0121255186188));
#255136=CARTESIAN_POINT('Ctrl Pts',(-44.8697378119757,30.6855401076749,
-40.9936389109155));
#255137=CARTESIAN_POINT('Ctrl Pts',(-44.8599646045333,30.6753771122426,
-40.984402815764));
#255138=CARTESIAN_POINT('Ctrl Pts',(-44.8300025766326,30.6456635434001,
-40.9567321786306));
#255139=CARTESIAN_POINT('Ctrl Pts',(-44.7987417882795,30.6174785558847,
-40.9291201070801));
#255140=CARTESIAN_POINT('Ctrl Pts',(-44.7544912812914,30.5829390177582,
-40.8924276633141));
#255141=CARTESIAN_POINT('Ctrl Pts',(-44.7200063674423,30.5585634922437,
-40.8649689008411));
#255142=CARTESIAN_POINT('Ctrl Pts',(-44.6961476159991,30.5433500948652,
-40.8467099213417));
#255143=CARTESIAN_POINT('Ctrl Pts',(-44.6779108400504,30.5323301088838,
-40.8330260113948));
#255144=CARTESIAN_POINT('Ctrl Pts',(-44.6717725199842,30.5287210947847,
-40.8284650265932));
#255145=CARTESIAN_POINT('Ctrl Pts',(-44.6594468286685,30.521672327511,-40.8193954109541));
#255146=CARTESIAN_POINT('Ctrl Pts',(-44.6532495459125,30.5182260348866,
-40.8148790968875));
#255147=CARTESIAN_POINT('Ctrl Pts',(-44.6221170703041,30.5014023919654,
-40.7924104777995));
#255148=CARTESIAN_POINT('Ctrl Pts',(-44.5712944462502,30.4770113822335,
-40.7571098106096));
#255149=CARTESIAN_POINT('Ctrl Pts',(-44.5053084694641,30.4527583886953,
-40.7146170218743));
#255150=CARTESIAN_POINT('Ctrl Pts',(-44.4645950315289,30.4410392847555,
-40.6898685245315));
#255151=CARTESIAN_POINT('Ctrl Pts',(-44.4371992237873,30.4338676574989,
-40.6735398509862));
#255152=CARTESIAN_POINT('Ctrl Pts',(-44.4233828828253,30.4306039319716,
-40.6654653393082));
#255153=CARTESIAN_POINT('Ctrl Pts',(-44.395457566773,30.4247250011004,-40.6494724436125));
#255154=CARTESIAN_POINT('Ctrl Pts',(-44.3814368244576,30.4221299378924,
-40.6416053105951));
#255155=CARTESIAN_POINT('Ctrl Pts',(-44.353398925472,30.4176419772095,-40.6261940087904));
#255156=CARTESIAN_POINT('Ctrl Pts',(-44.3393578467875,30.4157440298243,
-40.6186361329255));
#255157=CARTESIAN_POINT('Ctrl Pts',(-44.2971907773647,30.4110825461462,
-40.5964157409664));
#255158=CARTESIAN_POINT('Ctrl Pts',(-44.2690063197214,30.4093460565949,
-40.5821970282665));
#255159=CARTESIAN_POINT('Ctrl Pts',(-44.212497942469,30.4086221665927,-40.5549656043439));
#255160=CARTESIAN_POINT('Ctrl Pts',(-44.1841675064314,30.4096363406377,
-40.5419505068598));
#255161=CARTESIAN_POINT('Ctrl Pts',(-44.1486758957365,30.4126704859088,
-40.5264682752254));
#255162=CARTESIAN_POINT('Ctrl Pts',(-44.141568690144,30.4133673915631,-40.5234096239519));
#255163=CARTESIAN_POINT('Ctrl Pts',(-44.1273541295014,30.414939058346,-40.5173753852017));
#255164=CARTESIAN_POINT('Ctrl Pts',(-44.1202325648852,30.4158161528369,
-40.5143941227858));
#255165=CARTESIAN_POINT('Ctrl Pts',(-44.0989269046614,30.418710900521,-40.5056018445424));
#255166=CARTESIAN_POINT('Ctrl Pts',(-44.0848361489451,30.4209852789275,
-40.4999555272545));
#255167=CARTESIAN_POINT('Ctrl Pts',(-44.0428355440345,30.4288357011986,
-40.4836289969086));
#255168=CARTESIAN_POINT('Ctrl Pts',(-44.001418907738,30.4387301387603,-40.4685417636913));
#255169=CARTESIAN_POINT('Ctrl Pts',(-43.9473552852602,30.4559806561897,
-40.4508995609031));
#255170=CARTESIAN_POINT('Ctrl Pts',(-43.9073915907435,30.4709642266074,
-40.4389183731711));
#255171=CARTESIAN_POINT('Ctrl Pts',(-43.8811432548962,30.4823370897352,
-40.4317784203789));
#255172=CARTESIAN_POINT('Ctrl Pts',(-43.8550972458946,30.4944149327137,
-40.4250719137776));
#255173=CARTESIAN_POINT('Ctrl Pts',(-43.8421555815742,30.5008203273088,
-40.4219325711588));
#255174=CARTESIAN_POINT('Ctrl Pts',(-43.8167947927211,30.5141840584711,
-40.4161689437405));
#255175=CARTESIAN_POINT('Ctrl Pts',(-43.8043130802594,30.5211703528968,
-40.413528034466));
#255176=CARTESIAN_POINT('Ctrl Pts',(-43.7797793173031,30.5357258010655,
-40.4087317905317));
#255177=CARTESIAN_POINT('Ctrl Pts',(-43.7436043213473,30.5584424906522,
-40.4022611528103));
#255178=CARTESIAN_POINT('Ctrl Pts',(-43.7092889915882,30.583786036936,-40.397944872434));
#255179=CARTESIAN_POINT('Ctrl Pts',(-43.6651994519323,30.6199287507259,
-40.394121352571));
#255180=CARTESIAN_POINT('Ctrl Pts',(-43.6439827068456,30.6391798378995,
-40.3931753351425));
#255181=CARTESIAN_POINT('Ctrl Pts',(-43.6032932824946,30.680108587057,-40.3932905044721));
#255182=CARTESIAN_POINT('Ctrl Pts',(-43.5841829799745,30.7014201645355,
-40.3943499059801));
#255183=CARTESIAN_POINT('Ctrl Pts',(-43.5483166082379,30.7456951818503,
-40.3983955355947));
#255184=CARTESIAN_POINT('Ctrl Pts',(-43.5148120542517,30.7916143604394,
-40.4043679292189));
#255185=CARTESIAN_POINT('Ctrl Pts',(-43.4859931451963,30.8408014772341,
-40.4141590917094));
#255186=CARTESIAN_POINT('Ctrl Pts',(-43.469474574758,30.8725808034089,-40.4214902069511));
#255187=CARTESIAN_POINT('Ctrl Pts',(-43.4662461658165,30.8789901287051,
-40.4230180755467));
#255188=CARTESIAN_POINT('Ctrl Pts',(-43.4599404108544,30.8919125782622,
-40.4261957226772));
#255189=CARTESIAN_POINT('Ctrl Pts',(-43.4568618652692,30.8984301381776,
-40.4278470523708));
#255190=CARTESIAN_POINT('Ctrl Pts',(-43.4479066843131,30.9180293597941,
-40.4329571814025));
#255191=CARTESIAN_POINT('Ctrl Pts',(-43.4366800830858,30.9443463169446,
-40.440199707327));
#255192=CARTESIAN_POINT('Ctrl Pts',(-43.4219268251392,30.9843790154574,
-40.4523233881121));
#255193=CARTESIAN_POINT('Ctrl Pts',(-43.4092278315493,31.0249558361973,
-40.4656821965631));
#255194=CARTESIAN_POINT('Ctrl Pts',(-43.3985649158327,31.0660734353404,
-40.4802626336878));
#255195=CARTESIAN_POINT('Ctrl Pts',(-43.3928117504253,31.0938450909326,
-40.4907938342908));
#255196=CARTESIAN_POINT('Ctrl Pts',(-43.3877402558097,31.1217978520093,
-40.5017316825792));
#255197=CARTESIAN_POINT('Ctrl Pts',(-43.3855448869231,31.1358715333473,
-40.5074069308404));
#255198=CARTESIAN_POINT('Ctrl Pts',(-43.3818466485176,31.1641754295066,
-40.5191561881817));
#255199=CARTESIAN_POINT('Ctrl Pts',(-43.3803394900793,31.1784722137567,
-40.5252598906186));
#255200=CARTESIAN_POINT('Ctrl Pts',(-43.3780514709974,31.2069533499868,
-40.5377524690855));
#255201=CARTESIAN_POINT('Ctrl Pts',(-43.3764764291988,31.2353806198054,
-40.5505518795279));
#255202=CARTESIAN_POINT('Ctrl Pts',(-43.3761228002374,31.292003207243,-40.577339198747));
#255203=CARTESIAN_POINT('Ctrl Pts',(-43.3798904844517,31.3482922086547,
-40.6058744004623));
#255204=CARTESIAN_POINT('Ctrl Pts',(-43.3877424304871,31.4042485256067,
-40.6361260433691));
#255205=CARTESIAN_POINT('Ctrl Pts',(-43.393042276717,31.4321193306868,-40.6518290622461));
#255206=CARTESIAN_POINT('Ctrl Pts',(-43.3990345440792,31.4599262492628,
-40.6678171709904));
#255207=CARTESIAN_POINT('Ctrl Pts',(-43.4023871385948,31.4738288295879,
-40.6759732487162));
#255208=CARTESIAN_POINT('Ctrl Pts',(-43.4097262599636,31.5013102698765,
-40.6924188649606));
#255209=CARTESIAN_POINT('Ctrl Pts',(-43.4137223958007,31.5149386860624,
-40.7007364096885));
#255210=CARTESIAN_POINT('Ctrl Pts',(-43.4266697743275,31.5554481319482,
-40.7259437634106));
#255211=CARTESIAN_POINT('Ctrl Pts',(-43.4365815013438,31.5819735775504,
-40.743098588818));
#255212=CARTESIAN_POINT('Ctrl Pts',(-43.453362100664,31.6210434116697,-40.7693485791028));
#255213=CARTESIAN_POINT('Ctrl Pts',(-43.4592720436944,31.6339404199602,
-40.77818065559));
#255214=CARTESIAN_POINT('Ctrl Pts',(-43.471748387858,31.6595177912398,-40.7960360397975));
#255215=CARTESIAN_POINT('Ctrl Pts',(-43.4782913690647,31.6721475181291,
-40.8050245716083));
#255216=CARTESIAN_POINT('Ctrl Pts',(-43.4987158872668,31.7093568101663,
-40.832021101787));
#255217=CARTESIAN_POINT('Ctrl Pts',(-43.5134312848982,31.7333600460206,
-40.8501267844669));
#255218=CARTESIAN_POINT('Ctrl Pts',(-43.5449969636312,31.7797747067972,
-40.8865288544817));
#255219=CARTESIAN_POINT('Ctrl Pts',(-43.570273480101,31.8133992725601,-40.9139774903764));
#255220=CARTESIAN_POINT('Ctrl Pts',(-43.6071874842548,31.8558549470217,
-40.9508682927202));
#255221=CARTESIAN_POINT('Ctrl Pts',(-43.6267265436653,31.8762775041081,
-40.9694100075909));
#255222=CARTESIAN_POINT('Ctrl Pts',(-43.6468212761471,31.8962967826001,
-40.9880061403947));
#255223=CARTESIAN_POINT('Ctrl Pts',(-43.6571524242715,31.9061057307006,
-40.997334528722));
#255224=CARTESIAN_POINT('Ctrl Pts',(-43.6781351765956,31.9250932263188,
-41.0158316653051));
#255225=CARTESIAN_POINT('Ctrl Pts',(-43.6888325213991,31.9343181422645,
-41.0250431278314));
#255226=CARTESIAN_POINT('Ctrl Pts',(-43.7214683281725,31.961133026229,-41.0525078158304));
#255227=CARTESIAN_POINT('Ctrl Pts',(-43.744000771517,31.977916302359,-41.070639272709));
#255228=CARTESIAN_POINT('Ctrl Pts',(-43.7905699795511,32.0092811177654,
-41.106520902203));
#255229=CARTESIAN_POINT('Ctrl Pts',(-43.8266341229871,32.0311632771839,
-41.1331548827895));
#255230=CARTESIAN_POINT('Ctrl Pts',(-43.8644344365312,32.050527928199,-41.1593656410909));
#255231=CARTESIAN_POINT('Ctrl Pts',(-43.8900335656271,32.0628690313763,
-41.1767476889401));
#255232=CARTESIAN_POINT('Ctrl Pts',(-43.903042008964,32.0687560539784,-41.1853974312384));
#255233=CARTESIAN_POINT('Ctrl Pts',(-43.9291618902095,32.0798229381751,
-41.2024070088898));
#255234=CARTESIAN_POINT('Ctrl Pts',(-43.9423286751247,32.0850301956599,
-41.2108047653586));
#255235=CARTESIAN_POINT('Ctrl Pts',(-43.9688389276373,32.0947834481969,
-41.2273662374836));
#255236=CARTESIAN_POINT('Ctrl Pts',(-44.0088868242005,32.1084293286422,
-41.2518690158044));
#255237=CARTESIAN_POINT('Ctrl Pts',(-44.0634057706764,32.1227159830699,
-41.2831968728749));
#255238=CARTESIAN_POINT('Ctrl Pts',(-44.1051448739617,32.1304686073096,
-41.30568419746));
#255239=CARTESIAN_POINT('Ctrl Pts',(-44.1331632182567,32.1349666221674,
-41.3204486001008));
#255240=CARTESIAN_POINT('Ctrl Pts',(-44.1472622735965,32.1368798783668,
-41.3277141420552));
#255241=CARTESIAN_POINT('Ctrl Pts',(-44.1685768983456,32.1392377391899,
-41.3384485067576));
#255242=CARTESIAN_POINT('Ctrl Pts',(-44.1757038998442,32.1399371964,-41.3419962566417));
#255243=CARTESIAN_POINT('Ctrl Pts',(-44.1899298892594,32.1411565650423,
-41.3489954369734));
#255244=CARTESIAN_POINT('Ctrl Pts',(-44.1970429564213,32.1416781032566,
-41.3524539903966));
#255245=CARTESIAN_POINT('Ctrl Pts',(-44.2183581262916,32.1429776302475,
-41.3626954949199));
#255246=CARTESIAN_POINT('Ctrl Pts',(-44.232556678806,32.1434929542666,-41.3693546778539));
#255247=CARTESIAN_POINT('Ctrl Pts',(-44.2750884056492,32.1439936324359,
-41.3888189062651));
#255248=CARTESIAN_POINT('Ctrl Pts',(-44.3033804172497,32.1429384256622,
-41.4011231160504));
#255249=CARTESIAN_POINT('Ctrl Pts',(-44.3598247343314,32.13804594572,-41.4243882373187));
#255250=CARTESIAN_POINT('Ctrl Pts',(-44.3879848006206,32.1342064546963,
-41.4353516241949));
#255251=CARTESIAN_POINT('Ctrl Pts',(-44.4230841862873,32.1276226980045,
-41.4481948195873));
#255252=CARTESIAN_POINT('Ctrl Pts',(-44.4301039616143,32.126214419323,-41.4507215814638));
#255253=CARTESIAN_POINT('Ctrl Pts',(-44.4441256434231,32.1232190082407,
-41.455685422358));
#255254=CARTESIAN_POINT('Ctrl Pts',(-44.4511413829898,32.1216281453652,
-41.4581270453932));
#255255=CARTESIAN_POINT('Ctrl Pts',(-44.472106554004,32.1165956901708,-41.4652964871519));
#255256=CARTESIAN_POINT('Ctrl Pts',(-44.4859328208737,32.1129061786889,
-41.4698557698741));
#255257=CARTESIAN_POINT('Ctrl Pts',(-44.5270324780087,32.1008340938932,
-41.4829067838587));
#255258=CARTESIAN_POINT('Ctrl Pts',(-44.5673316800757,32.08677017453,-41.4946921125766));
#255259=CARTESIAN_POINT('Ctrl Pts',(-44.6194780799712,32.0640738471498,
-41.5079096337926));
#255260=CARTESIAN_POINT('Ctrl Pts',(-44.6577884739158,32.045065905176,-41.5165678887371));
#255261=CARTESIAN_POINT('Ctrl Pts',(-44.6827916371924,32.031050813041,-41.5214942665077));
#255262=CARTESIAN_POINT('Ctrl Pts',(-44.7075150580676,32.0163554529027,
-41.5259894017533));
#255263=CARTESIAN_POINT('Ctrl Pts',(-44.7197631353705,32.0086467826241,
-41.5280237577537));
#255264=CARTESIAN_POINT('Ctrl Pts',(-44.7436779765282,31.9927322821733,
-41.5316086326721));
#255265=CARTESIAN_POINT('Ctrl Pts',(-44.7554039451266,31.9844926239501,
-41.5331705278033));
#255266=CARTESIAN_POINT('Ctrl Pts',(-44.7783650010144,31.9674779303508,
-41.5358342782831));
#255267=CARTESIAN_POINT('Ctrl Pts',(-44.8120876763637,31.941142023486,-41.5391427937509));
#255268=CARTESIAN_POINT('Ctrl Pts',(-44.8542060542843,31.9028069711657,
-41.5408368316843));
#255269=CARTESIAN_POINT('Ctrl Pts',(-44.883650374082,31.8716290815775,-41.5400605624154));
#255270=CARTESIAN_POINT('Ctrl Pts',(-44.9027957424029,31.8502960261458,
-41.5390808606534));
#255271=CARTESIAN_POINT('Ctrl Pts',(-44.912124025092,31.8393588588263,-41.5383603441012));
#255272=CARTESIAN_POINT('Ctrl Pts',(-44.9302963003321,31.816913187918,-41.5364463589967));
#255273=CARTESIAN_POINT('Ctrl Pts',(-44.9390653236876,31.8054960967264,
-41.5352602514373));
#255274=CARTESIAN_POINT('Ctrl Pts',(-44.9559494861592,31.7823260274566,
-41.532444286592));
#255275=CARTESIAN_POINT('Ctrl Pts',(-44.9803129684955,31.7470436123751,
-41.5275522735743));
#255276=CARTESIAN_POINT('Ctrl Pts',(-45.00183725318,31.7102129370948,-41.5206914933375));
#255277=CARTESIAN_POINT('Ctrl Pts',(-45.0280427451288,31.6597446570548,
-41.5098099510806));
#255278=CARTESIAN_POINT('Ctrl Pts',(-45.0398987329805,31.6338241168053,
-41.5034995556801));
#255279=CARTESIAN_POINT('Ctrl Pts',(-45.0531290598229,31.6005723463994,
-41.4945098705711));
#255280=CARTESIAN_POINT('Ctrl Pts',(-45.0556963147994,31.5938738844661,
-41.4926546478805));
#255281=CARTESIAN_POINT('Ctrl Pts',(-45.0606676096559,31.5803990532317,
-41.4888352403062));
#255282=CARTESIAN_POINT('Ctrl Pts',(-45.0630762139805,31.5736079348959,
-41.4868664774371));
#255283=CARTESIAN_POINT('Ctrl Pts',(-45.0700329505347,31.5531765604049,
-41.4808121016924));
#255284=CARTESIAN_POINT('Ctrl Pts',(-45.0743018132827,31.5395152309552,
-41.4765904297482));
#255285=CARTESIAN_POINT('Ctrl Pts',(-45.0860497029301,31.4983488303989,
-41.4633620161014));
#255286=CARTESIAN_POINT('Ctrl Pts',(-45.0988767040151,31.4430340104486,
-41.4442426901641));
#255287=CARTESIAN_POINT('Ctrl Pts',(-45.1061818129997,31.386882792419,-41.4222207481485));
#255288=CARTESIAN_POINT('Ctrl Pts',(-45.1095857869151,31.3444641027996,
-41.4046111316328));
#255289=CARTESIAN_POINT('Ctrl Pts',(-45.1103739871937,31.3302675876129,
-41.3985560195248));
#255290=CARTESIAN_POINT('Ctrl Pts',(-45.1110306052012,31.30890259785,-41.3891987399731));
#255291=CARTESIAN_POINT('Ctrl Pts',(-45.1111617199316,31.3017636946428,
-41.3860313075819));
#255292=CARTESIAN_POINT('Ctrl Pts',(-45.1112472734604,31.2874686716035,
-41.3796068875509));
#255293=CARTESIAN_POINT('Ctrl Pts',(-45.111201351958,31.2802974166487,-41.3763428889219));
#255294=CARTESIAN_POINT('Ctrl Pts',(-45.1107973541963,31.25882908612,-41.3664479958234));
#255295=CARTESIAN_POINT('Ctrl Pts',(-45.11017580813,31.2446005169708,-41.3597259135069));
#255296=CARTESIAN_POINT('Ctrl Pts',(-45.1082442962718,31.2162677536902,
-41.3460176286356));
#255297=CARTESIAN_POINT('Ctrl Pts',(-45.104314463686,31.1739750543259,-41.3250680443717));
#255298=CARTESIAN_POINT('Ctrl Pts',(-45.0950241996196,31.1183949914011,
-41.295609869938));
#255299=CARTESIAN_POINT('Ctrl Pts',(-45.0817381040079,31.0636149263882,
-41.264634106957));
#255300=CARTESIAN_POINT('Ctrl Pts',(-45.0737554763462,31.0364928582332,
-41.2486352837062));
#255301=CARTESIAN_POINT('Ctrl Pts',(-45.0650963255467,31.0095068957897,
-41.2323777508457));
#255302=CARTESIAN_POINT('Ctrl Pts',(-45.0604265398991,30.996076905732,-41.224116427314));
#255303=CARTESIAN_POINT('Ctrl Pts',(-45.0504049610752,30.9693743366894,
-41.2073411015006));
#255304=CARTESIAN_POINT('Ctrl Pts',(-45.0450945767524,30.9562107421528,
-41.1988958018751));
#255305=CARTESIAN_POINT('Ctrl Pts',(-45.0394875320819,30.9432190801919,
-41.190386719266));
#255306=CARTESIAN_POINT('',(-45.413889917786,33.3235045267141,-40.0133525317522));
#255307=CARTESIAN_POINT('Ctrl Pts',(-43.399376135545,33.205102110798,-39.5898551246884));
#255308=CARTESIAN_POINT('Ctrl Pts',(-43.4519070146144,33.2400854050083,
-39.607463913371));
#255309=CARTESIAN_POINT('Ctrl Pts',(-43.5337620388772,33.2891936594495,
-39.6337707491335));
#255310=CARTESIAN_POINT('Ctrl Pts',(-43.6195680771379,33.3326108090195,
-39.6596645368951));
#255311=CARTESIAN_POINT('Ctrl Pts',(-43.6784022657394,33.3605926156183,
-39.6770465847445));
#255312=CARTESIAN_POINT('Ctrl Pts',(-43.7083060299631,33.3739265642863,
-39.6856963270425));
#255313=CARTESIAN_POINT('Ctrl Pts',(-43.7683631864552,33.3989633419485,
-39.7027059046941));
#255314=CARTESIAN_POINT('Ctrl Pts',(-43.7986437698924,33.4107283136069,
-39.7111036611629));
#255315=CARTESIAN_POINT('Ctrl Pts',(-43.8596236543864,33.432731604347,-39.7276651332879));
#255316=CARTESIAN_POINT('Ctrl Pts',(-43.9517617731223,33.4634644421701,
-39.7521679116086));
#255317=CARTESIAN_POINT('Ctrl Pts',(-44.0772655876523,33.4954182164341,
-39.7834957686792));
#255318=CARTESIAN_POINT('Ctrl Pts',(-44.1734028302798,33.5125433235231,
-39.8059830932642));
#255319=CARTESIAN_POINT('Ctrl Pts',(-44.2379488567859,33.5224120576217,
-39.8207474959053));
#255320=CARTESIAN_POINT('Ctrl Pts',(-44.2704347193422,33.5265712650576,
-39.8280130378593));
#255321=CARTESIAN_POINT('Ctrl Pts',(-44.3195548787318,33.5316274184839,
-39.8387474025619));
#255322=CARTESIAN_POINT('Ctrl Pts',(-44.3359807184467,33.5331131204799,
-39.8422951524459));
#255323=CARTESIAN_POINT('Ctrl Pts',(-44.3687707333322,33.5356713331865,
-39.8492943327777));
#255324=CARTESIAN_POINT('Ctrl Pts',(-44.3851673533813,33.5367473433996,
-39.8527528862009));
#255325=CARTESIAN_POINT('Ctrl Pts',(-44.4343061264537,33.5393650105759,
-39.8629943907241));
#255326=CARTESIAN_POINT('Ctrl Pts',(-44.4670443896497,33.5403015249987,
-39.8696535736582));
#255327=CARTESIAN_POINT('Ctrl Pts',(-44.5651287758397,33.5407036712734,
-39.8891178020695));
#255328=CARTESIAN_POINT('Ctrl Pts',(-44.6303969251806,33.5377724131818,
-39.9014220118547));
#255329=CARTESIAN_POINT('Ctrl Pts',(-44.7606561433707,33.5255015904578,
-39.924687133123));
#255330=CARTESIAN_POINT('Ctrl Pts',(-44.8256651474086,33.516156778985,-39.93565052));
#255331=CARTESIAN_POINT('Ctrl Pts',(-44.9067230595199,33.5003653725032,
-39.9484937153914));
#255332=CARTESIAN_POINT('Ctrl Pts',(-44.9229358898309,33.4969961660477,
-39.9510204772682));
#255333=CARTESIAN_POINT('Ctrl Pts',(-44.9553232364802,33.4898458857957,
-39.9559843181622));
#255334=CARTESIAN_POINT('Ctrl Pts',(-44.9715297170939,33.48605597099,-39.9584259411976));
#255335=CARTESIAN_POINT('Ctrl Pts',(-45.0199641404161,33.4740887742096,
-39.965595382956));
#255336=CARTESIAN_POINT('Ctrl Pts',(-45.0519120411053,33.4653422982392,
-39.9701546656783));
#255337=CARTESIAN_POINT('Ctrl Pts',(-45.1468975937756,33.4367966020141,
-39.983205679663));
#255338=CARTESIAN_POINT('Ctrl Pts',(-45.2400693383874,33.4036742979489,
-39.9949910083808));
#255339=CARTESIAN_POINT('Ctrl Pts',(-45.3486712153738,33.3557567039275,
-40.0068900294228));
#255340=CARTESIAN_POINT('Ctrl Pts',(-45.3961814822964,33.332503308482,-40.0116442129886));
#255341=CARTESIAN_POINT('Ctrl Pts',(-45.4138896478391,33.3235054357711,
-40.0133501741483));
#255342=CARTESIAN_POINT('Ctrl Pts',(-45.4138896492504,33.3235039948814,
-40.0133529162944));
#255343=CARTESIAN_POINT('Ctrl Pts',(-45.220007869287,33.4018089092386,-40.0137878164737));
#255344=CARTESIAN_POINT('Ctrl Pts',(-45.0135121509523,33.4437912620812,
-40.0118840249176));
#255345=CARTESIAN_POINT('Ctrl Pts',(-44.6315114877946,33.4515951730344,
-40.0050871993533));
#255346=CARTESIAN_POINT('Ctrl Pts',(-44.4590991737821,33.4292864011566,
-40.0008095143876));
#255347=CARTESIAN_POINT('Ctrl Pts',(-44.0965692082188,33.3271748070394,
-39.9897581690022));
#255348=CARTESIAN_POINT('Ctrl Pts',(-43.9111554000927,33.2383845853547,
-39.9827536906167));
#255349=CARTESIAN_POINT('Ctrl Pts',(-43.5996400949778,33.0179220859889,
-39.9689626255907));
#255350=CARTESIAN_POINT('Ctrl Pts',(-43.4715347449999,32.8953861314864,
-39.962602231998));
#255351=CARTESIAN_POINT('Ctrl Pts',(-43.3633208282253,32.7547543987198,
-39.9581074212483));
#255352=CARTESIAN_POINT('Ctrl Pts',(-43.0534148594278,32.3583957084033,
-39.8341886583259));
#255353=CARTESIAN_POINT('Ctrl Pts',(-43.085178776931,32.5092364820398,-39.7972070934614));
#255354=CARTESIAN_POINT('Ctrl Pts',(-43.1311025668885,32.6568722937985,
-39.7575468725598));
#255355=CARTESIAN_POINT('Ctrl Pts',(-43.2471037313335,32.939586900846,-39.6756564072208));
#255356=CARTESIAN_POINT('Ctrl Pts',(-43.3174654472053,33.0756353558302,
-39.6331721875354));
#255357=CARTESIAN_POINT('Ctrl Pts',(-43.3993761267971,33.2051021146614,
-39.5898551195224));
#255358=CARTESIAN_POINT('Ctrl Pts',(-46.6981266849492,30.7091523375488,
-39.2904704603133));
#255359=CARTESIAN_POINT('Ctrl Pts',(-46.6689684123063,30.6404043382273,
-39.273452295095));
#255360=CARTESIAN_POINT('Ctrl Pts',(-46.6043681216411,30.5066861069553,
-39.238925705885));
#255361=CARTESIAN_POINT('Ctrl Pts',(-46.5083209189471,30.3487389562033,
-39.1945593129175));
#255362=CARTESIAN_POINT('Ctrl Pts',(-46.4437937583117,30.2581216171786,
-39.1673894861782));
#255363=CARTESIAN_POINT('Ctrl Pts',(-46.3992224148768,30.1986447451181,
-39.1491520227249));
#255364=CARTESIAN_POINT('Ctrl Pts',(-46.3761748773305,30.1693908446446,
-39.1399767764946));
#255365=CARTESIAN_POINT('Ctrl Pts',(-46.3284414024809,30.1117648114071,
-39.1214771434543));
#255366=CARTESIAN_POINT('Ctrl Pts',(-46.3038983378397,30.083571828401,-39.112209259666));
#255367=CARTESIAN_POINT('Ctrl Pts',(-46.253707387608,30.0286632749651,-39.0937226519629));
#255368=CARTESIAN_POINT('Ctrl Pts',(-46.2280147026909,30.001893564456,-39.0844865568113));
#255369=CARTESIAN_POINT('Ctrl Pts',(-46.1492148010453,29.9236586721517,
-39.0568159196779));
#255370=CARTESIAN_POINT('Ctrl Pts',(-46.0669347173688,29.8495134741745,
-39.0292038481275));
#255371=CARTESIAN_POINT('Ctrl Pts',(-45.9503410384262,29.7587889734315,
-38.9925114043613));
#255372=CARTESIAN_POINT('Ctrl Pts',(-45.8594191065401,29.6948377475824,
-38.9650526418885));
#255373=CARTESIAN_POINT('Ctrl Pts',(-45.7964751089327,29.6549785818455,
-38.9467936623891));
#255374=CARTESIAN_POINT('Ctrl Pts',(-45.748348603817,29.6261284949947,-38.9331097524421));
#255375=CARTESIAN_POINT('Ctrl Pts',(-45.7321473284057,29.616684052073,-38.9285487676403));
#255376=CARTESIAN_POINT('Ctrl Pts',(-45.6996106203311,29.5982459977232,
-38.9194791520014));
#255377=CARTESIAN_POINT('Ctrl Pts',(-45.683249044345,29.5892352448745,-38.9149628379356));
#255378=CARTESIAN_POINT('Ctrl Pts',(-45.6010439155842,29.5452684013657,
-38.8924942188443));
#255379=CARTESIAN_POINT('Ctrl Pts',(-45.4667739830181,29.4816584171599,
-38.8571935516581));
#255380=CARTESIAN_POINT('Ctrl Pts',(-45.2922645146651,29.4187721922835,
-38.8147007629208));
#255381=CARTESIAN_POINT('Ctrl Pts',(-45.184512437616,29.3885937253944,-38.7899522655792));
#255382=CARTESIAN_POINT('Ctrl Pts',(-45.1119891467798,29.3701842541612,
-38.7736235920333));
#255383=CARTESIAN_POINT('Ctrl Pts',(-45.0754052578815,29.3618381514785,
-38.7655490803555));
#255384=CARTESIAN_POINT('Ctrl Pts',(-45.0014447932705,29.3468760834356,
-38.7495561846596));
#255385=CARTESIAN_POINT('Ctrl Pts',(-44.964301863367,29.3403115562353,-38.7416890516424));
#255386=CARTESIAN_POINT('Ctrl Pts',(-44.8900079594565,29.3290481892184,
-38.726277749838));
#255387=CARTESIAN_POINT('Ctrl Pts',(-44.8527936282157,29.324336495618,-38.7187198739728));
#255388=CARTESIAN_POINT('Ctrl Pts',(-44.7410083373266,29.3129455735289,
-38.6964994820139));
#255389=CARTESIAN_POINT('Ctrl Pts',(-44.6662563757167,29.3089967422249,
-38.6822807693139));
#255390=CARTESIAN_POINT('Ctrl Pts',(-44.516312468428,29.3084067934202,-38.6550493453909));
#255391=CARTESIAN_POINT('Ctrl Pts',(-44.441103189525,29.3117700143417,-38.6420342479066));
#255392=CARTESIAN_POINT('Ctrl Pts',(-44.3468378615956,29.3206690055189,
-38.6265520162729));
#255393=CARTESIAN_POINT('Ctrl Pts',(-44.3279589148655,29.3226883315868,
-38.6234933649988));
#255394=CARTESIAN_POINT('Ctrl Pts',(-44.2901960653062,29.3271995080042,
-38.6174591262491));
#255395=CARTESIAN_POINT('Ctrl Pts',(-44.271274393292,29.329697893027,-38.614477863833));
#255396=CARTESIAN_POINT('Ctrl Pts',(-44.2146592782019,29.3378915995821,
-38.60568558559));
#255397=CARTESIAN_POINT('Ctrl Pts',(-44.1772069502033,29.344266758826,-38.6000392683017));
#255398=CARTESIAN_POINT('Ctrl Pts',(-44.0655444875092,29.3661148598052,
-38.5837127379559));
#255399=CARTESIAN_POINT('Ctrl Pts',(-43.9553791862171,29.3933792052515,
-38.5686255047386));
#255400=CARTESIAN_POINT('Ctrl Pts',(-43.8114622524781,29.4404829778103,
-38.5509833019505));
#255401=CARTESIAN_POINT('Ctrl Pts',(-43.705021834675,29.481230340464,-38.5390021142185));
#255402=CARTESIAN_POINT('Ctrl Pts',(-43.6350719757086,29.512061063653,-38.5318621614261));
#255403=CARTESIAN_POINT('Ctrl Pts',(-43.5656410085295,29.5447591316771,
-38.525155654825));
#255404=CARTESIAN_POINT('Ctrl Pts',(-43.5311320054746,29.5620794464364,
-38.5220163122062));
#255405=CARTESIAN_POINT('Ctrl Pts',(-43.4634866412134,29.5981758355574,
-38.5162526847879));
#255406=CARTESIAN_POINT('Ctrl Pts',(-43.4301834663392,29.6170276546,-38.5136117755133));
#255407=CARTESIAN_POINT('Ctrl Pts',(-43.3647025891651,29.6562685687332,
-38.5088155315793));
#255408=CARTESIAN_POINT('Ctrl Pts',(-43.2681192378476,29.7174608121974,
-38.5023448938576));
#255409=CARTESIAN_POINT('Ctrl Pts',(-43.1764049274077,29.7855824582168,
-38.4980286134812));
#255410=CARTESIAN_POINT('Ctrl Pts',(-43.0584774180437,29.8826126224142,
-38.4942050936184));
#255411=CARTESIAN_POINT('Ctrl Pts',(-43.001681818637,29.9342392650769,-38.4932590761897));
#255412=CARTESIAN_POINT('Ctrl Pts',(-42.8926599718677,30.0438904492243,
-38.4933742455196));
#255413=CARTESIAN_POINT('Ctrl Pts',(-42.8414047150844,30.1009342501745,
-38.4944336470273));
#255414=CARTESIAN_POINT('Ctrl Pts',(-42.7451036203247,30.2193471227021,
-38.498479276642));
#255415=CARTESIAN_POINT('Ctrl Pts',(-42.6550322643363,30.3420646399833,
-38.5044516702661));
#255416=CARTESIAN_POINT('Ctrl Pts',(-42.5773225406025,30.4733365238586,
-38.5142428327574));
#255417=CARTESIAN_POINT('Ctrl Pts',(-42.5326943378214,30.5580963840027,
-38.5215739479982));
#255418=CARTESIAN_POINT('Ctrl Pts',(-42.5239673850246,30.5751883092729,
-38.5231018165939));
#255419=CARTESIAN_POINT('Ctrl Pts',(-42.5069121510755,30.60964376351,-38.5262794637242));
#255420=CARTESIAN_POINT('Ctrl Pts',(-42.4985805781952,30.627019094627,-38.5279307934181));
#255421=CARTESIAN_POINT('Ctrl Pts',(-42.4743295471271,30.6792614198295,
-38.5330409224498));
#255422=CARTESIAN_POINT('Ctrl Pts',(-42.4438856226513,30.7493896366731,
-38.5402834483744));
#255423=CARTESIAN_POINT('Ctrl Pts',(-42.4037483179465,30.8560072598611,
-38.5524071291592));
#255424=CARTESIAN_POINT('Ctrl Pts',(-42.3690543371876,30.9640160484273,
-38.5657659376104));
#255425=CARTESIAN_POINT('Ctrl Pts',(-42.3397558527982,31.0734075527136,
-38.5803463747351));
#255426=CARTESIAN_POINT('Ctrl Pts',(-42.3238156343608,31.1472555030051,
-38.5908775753381));
#255427=CARTESIAN_POINT('Ctrl Pts',(-42.3096820427396,31.2215665449467,
-38.6018154236264));
#255428=CARTESIAN_POINT('Ctrl Pts',(-42.3035171869091,31.2589715314082,
-38.6074906718877));
#255429=CARTESIAN_POINT('Ctrl Pts',(-42.2930235524414,31.3341791410138,
-38.6192399292287));
#255430=CARTESIAN_POINT('Ctrl Pts',(-42.2886818075092,31.3721585359098,
-38.6253436316658));
#255431=CARTESIAN_POINT('Ctrl Pts',(-42.281930630611,31.4478003630713,-38.6378362101326));
#255432=CARTESIAN_POINT('Ctrl Pts',(-42.277074994566,31.5232809912004,-38.6506356205751));
#255433=CARTESIAN_POINT('Ctrl Pts',(-42.2747992363309,31.6735553614761,
-38.6774229397946));
#255434=CARTESIAN_POINT('Ctrl Pts',(-42.2834818483937,31.8228397562226,
-38.7059581415094));
#255435=CARTESIAN_POINT('Ctrl Pts',(-42.3030248127084,31.9711385758679,
-38.7362097844166));
#255436=CARTESIAN_POINT('Ctrl Pts',(-42.3164494406915,32.0449687602614,
-38.7519128032936));
#255437=CARTESIAN_POINT('Ctrl Pts',(-42.3317154579634,32.1186122141692,
-38.7679009120377));
#255438=CARTESIAN_POINT('Ctrl Pts',(-42.3402956643805,32.1554227583218,
-38.7760569897633));
#255439=CARTESIAN_POINT('Ctrl Pts',(-42.3591481714288,32.228169160774,-38.7925026060078));
#255440=CARTESIAN_POINT('Ctrl Pts',(-42.3694448348212,32.2642362896146,
-38.8008201507359));
#255441=CARTESIAN_POINT('Ctrl Pts',(-42.4028917825415,32.3714169561226,
-38.8260275044574));
#255442=CARTESIAN_POINT('Ctrl Pts',(-42.428602574983,32.4415633880281,-38.8431823298655));
#255443=CARTESIAN_POINT('Ctrl Pts',(-42.4722685042023,32.5448307979217,
-38.8694323201497));
#255444=CARTESIAN_POINT('Ctrl Pts',(-42.4876674804306,32.5789105800712,
-38.8782643966373));
#255445=CARTESIAN_POINT('Ctrl Pts',(-42.5202146590728,32.6464795812123,
-38.8961197808447));
#255446=CARTESIAN_POINT('Ctrl Pts',(-42.5373018269229,32.6798350022668,
-38.9051083126545));
#255447=CARTESIAN_POINT('Ctrl Pts',(-42.5906929412925,32.7780783962456,
-38.9321048428364));
#255448=CARTESIAN_POINT('Ctrl Pts',(-42.629225789877,32.8414173722334,-38.9502105255135));
#255449=CARTESIAN_POINT('Ctrl Pts',(-42.7120000069194,32.9638220552461,
-38.9866125955294));
#255450=CARTESIAN_POINT('Ctrl Pts',(-42.7783647966162,33.0524402968179,
-39.0140612314234));
#255451=CARTESIAN_POINT('Ctrl Pts',(-42.8754380724448,33.1642175243331,
-39.0509520337677));
#255452=CARTESIAN_POINT('Ctrl Pts',(-42.9268673384212,33.2179450225078,
-39.0694937486382));
#255453=CARTESIAN_POINT('Ctrl Pts',(-42.9797817061918,33.2705900457306,
-39.088089881442));
#255454=CARTESIAN_POINT('Ctrl Pts',(-43.0069972096607,33.2963736994336,
-39.097418269769));
#255455=CARTESIAN_POINT('Ctrl Pts',(-43.0622936398443,33.3462615369726,
-39.1159154063528));
#255456=CARTESIAN_POINT('Ctrl Pts',(-43.0904949946047,33.3704876748183,
-39.1251268688783));
#255457=CARTESIAN_POINT('Ctrl Pts',(-43.176562606447,33.4408730143712,-39.1525915568785));
#255458=CARTESIAN_POINT('Ctrl Pts',(-43.2360245534179,33.4848790444095,
-39.1707230137558));
#255459=CARTESIAN_POINT('Ctrl Pts',(-43.358992255749,33.5670176609587,-39.2066046432507));
#255460=CARTESIAN_POINT('Ctrl Pts',(-43.4542745623933,33.6242424638975,
-39.233238623837));
#255461=CARTESIAN_POINT('Ctrl Pts',(-43.5542222374601,33.6747516510336,
-39.2594493821381));
#255462=CARTESIAN_POINT('Ctrl Pts',(-43.6219256430316,33.7069073870393,
-39.2768314299875));
#255463=CARTESIAN_POINT('Ctrl Pts',(-43.6563381479934,33.7222286468184,
-39.2854811722856));
#255464=CARTESIAN_POINT('Ctrl Pts',(-43.7254519170511,33.7509934760635,
-39.3024907499371));
#255465=CARTESIAN_POINT('Ctrl Pts',(-43.7602995448845,33.7645084608315,
-39.3108885064059));
#255466=CARTESIAN_POINT('Ctrl Pts',(-43.8304781084082,33.789780836939,-39.3274499785309));
#255467=CARTESIAN_POINT('Ctrl Pts',(-43.9365171946568,33.8250735562425,
-39.3519527568515));
#255468=CARTESIAN_POINT('Ctrl Pts',(-44.0809642638621,33.8617420360433,
-39.3832806139221));
#255469=CARTESIAN_POINT('Ctrl Pts',(-44.1916183723467,33.8813683146414,
-39.4057679385072));
#255470=CARTESIAN_POINT('Ctrl Pts',(-44.2659122959159,33.8926702964892,
-39.4205323411483));
#255471=CARTESIAN_POINT('Ctrl Pts',(-44.3033049221432,33.8974288658374,
-39.4277978831022));
#255472=CARTESIAN_POINT('Ctrl Pts',(-44.3598453576919,33.9032050944765,
-39.4385322478049));
#255473=CARTESIAN_POINT('Ctrl Pts',(-44.3787527158677,33.9049006163346,
-39.4420799976889));
#255474=CARTESIAN_POINT('Ctrl Pts',(-44.4164967874688,33.9078161173588,
-39.4490791780208));
#255475=CARTESIAN_POINT('Ctrl Pts',(-44.4353708468856,33.9090400957878,
-39.4525377314439));
#255476=CARTESIAN_POINT('Ctrl Pts',(-44.4919347179527,33.9120095261765,
-39.462779235967));
#255477=CARTESIAN_POINT('Ctrl Pts',(-44.52962054914,33.9130584408517,-39.4694384189012));
#255478=CARTESIAN_POINT('Ctrl Pts',(-44.6425299001817,33.9134342925821,
-39.4889026473125));
#255479=CARTESIAN_POINT('Ctrl Pts',(-44.7176656228988,33.9100023852834,
-39.5012068570978));
#255480=CARTESIAN_POINT('Ctrl Pts',(-44.867623327666,33.8957625538083,-39.524471978366));
#255481=CARTESIAN_POINT('Ctrl Pts',(-44.9424659600731,33.8849485744664,
-39.5354353652432));
#255482=CARTESIAN_POINT('Ctrl Pts',(-45.0357885152669,33.8666999843662,
-39.5482785606344));
#255483=CARTESIAN_POINT('Ctrl Pts',(-45.0544546343785,33.8628074782943,
-39.5508053225112));
#255484=CARTESIAN_POINT('Ctrl Pts',(-45.091743102575,33.8545484160302,-39.5557691634051));
#255485=CARTESIAN_POINT('Ctrl Pts',(-45.1104022544846,33.850171655015,-39.5582107864407));
#255486=CARTESIAN_POINT('Ctrl Pts',(-45.1661672125598,33.8363538303533,
-39.5653802281989));
#255487=CARTESIAN_POINT('Ctrl Pts',(-45.2029511118778,33.8262578362557,
-39.5699395109212));
#255488=CARTESIAN_POINT('Ctrl Pts',(-45.312316831343,33.7933159380614,-39.582990524906));
#255489=CARTESIAN_POINT('Ctrl Pts',(-45.4195983160475,33.7551076509549,
-39.5947758536238));
#255490=CARTESIAN_POINT('Ctrl Pts',(-45.5585113890164,33.6937328563153,
-39.6079933748399));
#255491=CARTESIAN_POINT('Ctrl Pts',(-45.6606150024606,33.6424505696195,
-39.6166516297843));
#255492=CARTESIAN_POINT('Ctrl Pts',(-45.7272860947277,33.6047101271221,
-39.6215780075552));
#255493=CARTESIAN_POINT('Ctrl Pts',(-45.7932287365117,33.5651705839516,
-39.6260731428005));
#255494=CARTESIAN_POINT('Ctrl Pts',(-45.8259059249178,33.5444453395394,
-39.6281074988013));
#255495=CARTESIAN_POINT('Ctrl Pts',(-45.8897275017006,33.5016881508368,
-39.6316923737189));
#255496=CARTESIAN_POINT('Ctrl Pts',(-45.9210297733036,33.4795651380848,
-39.6332542688506));
#255497=CARTESIAN_POINT('Ctrl Pts',(-45.9823424846244,33.4339088874735,
-39.6359180193303));
#255498=CARTESIAN_POINT('Ctrl Pts',(-46.0724202597563,33.3632801300718,
-39.6392265347984));
#255499=CARTESIAN_POINT('Ctrl Pts',(-46.1850394564173,33.2606222983665,
-39.6409205727319));
#255500=CARTESIAN_POINT('Ctrl Pts',(-46.2638636333332,33.1772336958075,
-39.6401443034625));
#255501=CARTESIAN_POINT('Ctrl Pts',(-46.3151397511292,33.1201974856456,
-39.6391646017005));
#255502=CARTESIAN_POINT('Ctrl Pts',(-46.3401349353408,33.0909661742941,
-39.6384440851485));
#255503=CARTESIAN_POINT('Ctrl Pts',(-46.3888523044997,33.0309971480077,
-39.6365301000439));
#255504=CARTESIAN_POINT('Ctrl Pts',(-46.4123735341802,33.0005036828642,
-39.6353439924849));
#255505=CARTESIAN_POINT('Ctrl Pts',(-46.4576879006691,32.9386388625828,
-39.6325280276393));
#255506=CARTESIAN_POINT('Ctrl Pts',(-46.52311576659,32.8444620833496,-39.6276360146217));
#255507=CARTESIAN_POINT('Ctrl Pts',(-46.5810426872604,32.7462345994881,
-39.6207752343847));
#255508=CARTESIAN_POINT('Ctrl Pts',(-46.6516918187307,32.6117039458857,
-39.6098936921283));
#255509=CARTESIAN_POINT('Ctrl Pts',(-46.683723185051,32.5426422373878,-39.6035832967262));
#255510=CARTESIAN_POINT('Ctrl Pts',(-46.7195635412788,32.4540883209461,
-39.5945936116187));
#255511=CARTESIAN_POINT('Ctrl Pts',(-46.7265235775841,32.4362514419463,
-39.5927383889278));
#255512=CARTESIAN_POINT('Ctrl Pts',(-46.7400123459627,32.4003742100513,
-39.5889189813535));
#255513=CARTESIAN_POINT('Ctrl Pts',(-46.7465535157541,32.3822946053341,
-39.5869502184844));
#255514=CARTESIAN_POINT('Ctrl Pts',(-46.7654644360989,32.3279072933142,
-39.5808958427402));
#255515=CARTESIAN_POINT('Ctrl Pts',(-46.7770937339888,32.2915493874551,
-39.5766741707955));
#255516=CARTESIAN_POINT('Ctrl Pts',(-46.8091770518909,32.182013131159,-39.5634457571489));
#255517=CARTESIAN_POINT('Ctrl Pts',(-46.8444383818759,32.034891308334,-39.5443264312115));
#255518=CARTESIAN_POINT('Ctrl Pts',(-46.8650708643864,31.8856621776612,
-39.5223044891954));
#255519=CARTESIAN_POINT('Ctrl Pts',(-46.8750487417844,31.7729724844591,
-39.50469487268));
#255520=CARTESIAN_POINT('Ctrl Pts',(-46.8774570362353,31.7352651712118,
-39.4986397605723));
#255521=CARTESIAN_POINT('Ctrl Pts',(-46.8796767940079,31.6785286095959,
-39.4892824810203));
#255522=CARTESIAN_POINT('Ctrl Pts',(-46.8801843407089,31.6595724593507,
-39.4861150486293));
#255523=CARTESIAN_POINT('Ctrl Pts',(-46.8807312344332,31.6216180949417,
-39.479690628598));
#255524=CARTESIAN_POINT('Ctrl Pts',(-46.8807699646674,31.6025797052015,
-39.4764266299692));
#255525=CARTESIAN_POINT('Ctrl Pts',(-46.8801790388754,31.5455906639181,
-39.4665317368708));
#255526=CARTESIAN_POINT('Ctrl Pts',(-46.8788490796135,31.5078273383739,
-39.4598096545541));
#255527=CARTESIAN_POINT('Ctrl Pts',(-46.874360617844,31.4326451774338,-39.4461013696832));
#255528=CARTESIAN_POINT('Ctrl Pts',(-46.864884835636,31.320441459725,-39.4251517854185));
#255529=CARTESIAN_POINT('Ctrl Pts',(-46.8414902947658,31.1730719473388,
-39.3956936109857));
#255530=CARTESIAN_POINT('Ctrl Pts',(-46.8074810934279,31.0279105813681,
-39.364717848004));
#255531=CARTESIAN_POINT('Ctrl Pts',(-46.7869180083019,30.9560697433081,
-39.3487190247537));
#255532=CARTESIAN_POINT('Ctrl Pts',(-46.7645577771926,30.884604709384,-39.332461491893));
#255533=CARTESIAN_POINT('Ctrl Pts',(-46.7524740339114,30.8490466969583,
-39.3242001683612));
#255534=CARTESIAN_POINT('Ctrl Pts',(-46.7264943673172,30.7783632715819,
-39.3074248425479));
#255535=CARTESIAN_POINT('Ctrl Pts',(-46.7127058212706,30.7435263372096,
-39.2989795429224));
#255536=CARTESIAN_POINT('Ctrl Pts',(-46.6981266849492,30.7091523375488,
-39.2904704603133));
#255537=CARTESIAN_POINT('Ctrl Pts',(-45.0394875320819,30.9432190801919,
-41.190386719266));
#255538=CARTESIAN_POINT('Ctrl Pts',(-45.0282734427409,30.91723575627,-41.1733685540478));
#255539=CARTESIAN_POINT('Ctrl Pts',(-45.0034876660128,30.8666726764904,
-41.1388419648381));
#255540=CARTESIAN_POINT('Ctrl Pts',(-44.9667665375866,30.8068862988478,
-41.09447557187));
#255541=CARTESIAN_POINT('Ctrl Pts',(-44.9421458413835,30.7725558756156,
-41.0673057451311));
#255542=CARTESIAN_POINT('Ctrl Pts',(-44.9251493960809,30.7500159625169,
-41.0490682816776));
#255543=CARTESIAN_POINT('Ctrl Pts',(-44.9163654668634,30.7389260450349,
-41.0398930354472));
#255544=CARTESIAN_POINT('Ctrl Pts',(-44.8981827131164,30.7170729960788,
-41.0213934024069));
#255545=CARTESIAN_POINT('Ctrl Pts',(-44.888838333634,30.7063777841388,-41.0121255186188));
#255546=CARTESIAN_POINT('Ctrl Pts',(-44.8697378119757,30.6855401076749,
-40.9936389109155));
#255547=CARTESIAN_POINT('Ctrl Pts',(-44.8599646045333,30.6753771122426,
-40.984402815764));
#255548=CARTESIAN_POINT('Ctrl Pts',(-44.8300025766326,30.6456635434001,
-40.9567321786306));
#255549=CARTESIAN_POINT('Ctrl Pts',(-44.7987417882795,30.6174785558847,
-40.9291201070801));
#255550=CARTESIAN_POINT('Ctrl Pts',(-44.7544912812914,30.5829390177582,
-40.8924276633141));
#255551=CARTESIAN_POINT('Ctrl Pts',(-44.7200063674423,30.5585634922437,
-40.8649689008411));
#255552=CARTESIAN_POINT('Ctrl Pts',(-44.6961476159991,30.5433500948652,
-40.8467099213417));
#255553=CARTESIAN_POINT('Ctrl Pts',(-44.6779108400504,30.5323301088838,
-40.8330260113948));
#255554=CARTESIAN_POINT('Ctrl Pts',(-44.6717725199842,30.5287210947847,
-40.8284650265932));
#255555=CARTESIAN_POINT('Ctrl Pts',(-44.6594468286685,30.521672327511,-40.8193954109541));
#255556=CARTESIAN_POINT('Ctrl Pts',(-44.6532495459125,30.5182260348866,
-40.8148790968875));
#255557=CARTESIAN_POINT('Ctrl Pts',(-44.6221170703041,30.5014023919654,
-40.7924104777995));
#255558=CARTESIAN_POINT('Ctrl Pts',(-44.5712944462502,30.4770113822335,
-40.7571098106096));
#255559=CARTESIAN_POINT('Ctrl Pts',(-44.5053084694641,30.4527583886953,
-40.7146170218743));
#255560=CARTESIAN_POINT('Ctrl Pts',(-44.4645950315289,30.4410392847555,
-40.6898685245315));
#255561=CARTESIAN_POINT('Ctrl Pts',(-44.4371992237873,30.4338676574989,
-40.6735398509862));
#255562=CARTESIAN_POINT('Ctrl Pts',(-44.4233828828253,30.4306039319716,
-40.6654653393082));
#255563=CARTESIAN_POINT('Ctrl Pts',(-44.395457566773,30.4247250011004,-40.6494724436125));
#255564=CARTESIAN_POINT('Ctrl Pts',(-44.3814368244576,30.4221299378924,
-40.6416053105951));
#255565=CARTESIAN_POINT('Ctrl Pts',(-44.353398925472,30.4176419772095,-40.6261940087904));
#255566=CARTESIAN_POINT('Ctrl Pts',(-44.3393578467875,30.4157440298243,
-40.6186361329255));
#255567=CARTESIAN_POINT('Ctrl Pts',(-44.2971907773647,30.4110825461462,
-40.5964157409664));
#255568=CARTESIAN_POINT('Ctrl Pts',(-44.2690063197214,30.4093460565949,
-40.5821970282665));
#255569=CARTESIAN_POINT('Ctrl Pts',(-44.212497942469,30.4086221665927,-40.5549656043439));
#255570=CARTESIAN_POINT('Ctrl Pts',(-44.1841675064314,30.4096363406377,
-40.5419505068598));
#255571=CARTESIAN_POINT('Ctrl Pts',(-44.1486758957365,30.4126704859088,
-40.5264682752254));
#255572=CARTESIAN_POINT('Ctrl Pts',(-44.141568690144,30.4133673915631,-40.5234096239519));
#255573=CARTESIAN_POINT('Ctrl Pts',(-44.1273541295014,30.414939058346,-40.5173753852017));
#255574=CARTESIAN_POINT('Ctrl Pts',(-44.1202325648852,30.4158161528369,
-40.5143941227858));
#255575=CARTESIAN_POINT('Ctrl Pts',(-44.0989269046614,30.418710900521,-40.5056018445424));
#255576=CARTESIAN_POINT('Ctrl Pts',(-44.0848361489451,30.4209852789275,
-40.4999555272545));
#255577=CARTESIAN_POINT('Ctrl Pts',(-44.0428355440345,30.4288357011986,
-40.4836289969086));
#255578=CARTESIAN_POINT('Ctrl Pts',(-44.001418907738,30.4387301387603,-40.4685417636913));
#255579=CARTESIAN_POINT('Ctrl Pts',(-43.9473552852602,30.4559806561897,
-40.4508995609031));
#255580=CARTESIAN_POINT('Ctrl Pts',(-43.9073915907435,30.4709642266074,
-40.4389183731711));
#255581=CARTESIAN_POINT('Ctrl Pts',(-43.8811432548962,30.4823370897352,
-40.4317784203789));
#255582=CARTESIAN_POINT('Ctrl Pts',(-43.8550972458946,30.4944149327137,
-40.4250719137776));
#255583=CARTESIAN_POINT('Ctrl Pts',(-43.8421555815742,30.5008203273088,
-40.4219325711588));
#255584=CARTESIAN_POINT('Ctrl Pts',(-43.8167947927211,30.5141840584711,
-40.4161689437405));
#255585=CARTESIAN_POINT('Ctrl Pts',(-43.8043130802594,30.5211703528968,
-40.413528034466));
#255586=CARTESIAN_POINT('Ctrl Pts',(-43.7797793173031,30.5357258010655,
-40.4087317905317));
#255587=CARTESIAN_POINT('Ctrl Pts',(-43.7436043213473,30.5584424906522,
-40.4022611528103));
#255588=CARTESIAN_POINT('Ctrl Pts',(-43.7092889915882,30.583786036936,-40.397944872434));
#255589=CARTESIAN_POINT('Ctrl Pts',(-43.6651994519323,30.6199287507259,
-40.394121352571));
#255590=CARTESIAN_POINT('Ctrl Pts',(-43.6439827068456,30.6391798378995,
-40.3931753351425));
#255591=CARTESIAN_POINT('Ctrl Pts',(-43.6032932824946,30.680108587057,-40.3932905044721));
#255592=CARTESIAN_POINT('Ctrl Pts',(-43.5841829799745,30.7014201645355,
-40.3943499059801));
#255593=CARTESIAN_POINT('Ctrl Pts',(-43.5483166082379,30.7456951818503,
-40.3983955355947));
#255594=CARTESIAN_POINT('Ctrl Pts',(-43.5148120542517,30.7916143604394,
-40.4043679292189));
#255595=CARTESIAN_POINT('Ctrl Pts',(-43.4859931451963,30.8408014772341,
-40.4141590917094));
#255596=CARTESIAN_POINT('Ctrl Pts',(-43.469474574758,30.8725808034089,-40.4214902069511));
#255597=CARTESIAN_POINT('Ctrl Pts',(-43.4662461658165,30.8789901287051,
-40.4230180755467));
#255598=CARTESIAN_POINT('Ctrl Pts',(-43.4599404108544,30.8919125782622,
-40.4261957226772));
#255599=CARTESIAN_POINT('Ctrl Pts',(-43.4568618652692,30.8984301381776,
-40.4278470523708));
#255600=CARTESIAN_POINT('Ctrl Pts',(-43.4479066843131,30.9180293597941,
-40.4329571814025));
#255601=CARTESIAN_POINT('Ctrl Pts',(-43.4366800830858,30.9443463169446,
-40.440199707327));
#255602=CARTESIAN_POINT('Ctrl Pts',(-43.4219268251392,30.9843790154574,
-40.4523233881121));
#255603=CARTESIAN_POINT('Ctrl Pts',(-43.4092278315493,31.0249558361973,
-40.4656821965631));
#255604=CARTESIAN_POINT('Ctrl Pts',(-43.3985649158327,31.0660734353404,
-40.4802626336878));
#255605=CARTESIAN_POINT('Ctrl Pts',(-43.3928117504253,31.0938450909326,
-40.4907938342908));
#255606=CARTESIAN_POINT('Ctrl Pts',(-43.3877402558097,31.1217978520093,
-40.5017316825792));
#255607=CARTESIAN_POINT('Ctrl Pts',(-43.3855448869231,31.1358715333473,
-40.5074069308404));
#255608=CARTESIAN_POINT('Ctrl Pts',(-43.3818466485176,31.1641754295066,
-40.5191561881817));
#255609=CARTESIAN_POINT('Ctrl Pts',(-43.3803394900793,31.1784722137567,
-40.5252598906186));
#255610=CARTESIAN_POINT('Ctrl Pts',(-43.3780514709974,31.2069533499868,
-40.5377524690855));
#255611=CARTESIAN_POINT('Ctrl Pts',(-43.3764764291988,31.2353806198054,
-40.5505518795279));
#255612=CARTESIAN_POINT('Ctrl Pts',(-43.3761228002374,31.292003207243,-40.577339198747));
#255613=CARTESIAN_POINT('Ctrl Pts',(-43.3798904844517,31.3482922086547,
-40.6058744004623));
#255614=CARTESIAN_POINT('Ctrl Pts',(-43.3877424304871,31.4042485256067,
-40.6361260433691));
#255615=CARTESIAN_POINT('Ctrl Pts',(-43.393042276717,31.4321193306868,-40.6518290622461));
#255616=CARTESIAN_POINT('Ctrl Pts',(-43.3990345440792,31.4599262492628,
-40.6678171709904));
#255617=CARTESIAN_POINT('Ctrl Pts',(-43.4023871385948,31.4738288295879,
-40.6759732487162));
#255618=CARTESIAN_POINT('Ctrl Pts',(-43.4097262599636,31.5013102698765,
-40.6924188649606));
#255619=CARTESIAN_POINT('Ctrl Pts',(-43.4137223958007,31.5149386860624,
-40.7007364096885));
#255620=CARTESIAN_POINT('Ctrl Pts',(-43.4266697743275,31.5554481319482,
-40.7259437634106));
#255621=CARTESIAN_POINT('Ctrl Pts',(-43.4365815013438,31.5819735775504,
-40.743098588818));
#255622=CARTESIAN_POINT('Ctrl Pts',(-43.453362100664,31.6210434116697,-40.7693485791028));
#255623=CARTESIAN_POINT('Ctrl Pts',(-43.4592720436944,31.6339404199602,
-40.77818065559));
#255624=CARTESIAN_POINT('Ctrl Pts',(-43.471748387858,31.6595177912398,-40.7960360397975));
#255625=CARTESIAN_POINT('Ctrl Pts',(-43.4782913690647,31.6721475181291,
-40.8050245716083));
#255626=CARTESIAN_POINT('Ctrl Pts',(-43.4987158872668,31.7093568101663,
-40.832021101787));
#255627=CARTESIAN_POINT('Ctrl Pts',(-43.5134312848982,31.7333600460206,
-40.8501267844669));
#255628=CARTESIAN_POINT('Ctrl Pts',(-43.5449969636312,31.7797747067972,
-40.8865288544817));
#255629=CARTESIAN_POINT('Ctrl Pts',(-43.570273480101,31.8133992725601,-40.9139774903764));
#255630=CARTESIAN_POINT('Ctrl Pts',(-43.6071874842548,31.8558549470217,
-40.9508682927202));
#255631=CARTESIAN_POINT('Ctrl Pts',(-43.6267265436653,31.8762775041081,
-40.9694100075909));
#255632=CARTESIAN_POINT('Ctrl Pts',(-43.6468212761471,31.8962967826001,
-40.9880061403947));
#255633=CARTESIAN_POINT('Ctrl Pts',(-43.6571524242715,31.9061057307006,
-40.997334528722));
#255634=CARTESIAN_POINT('Ctrl Pts',(-43.6781351765956,31.9250932263188,
-41.0158316653051));
#255635=CARTESIAN_POINT('Ctrl Pts',(-43.6888325213991,31.9343181422645,
-41.0250431278314));
#255636=CARTESIAN_POINT('Ctrl Pts',(-43.7214683281725,31.961133026229,-41.0525078158304));
#255637=CARTESIAN_POINT('Ctrl Pts',(-43.744000771517,31.977916302359,-41.070639272709));
#255638=CARTESIAN_POINT('Ctrl Pts',(-43.7905699795511,32.0092811177654,
-41.106520902203));
#255639=CARTESIAN_POINT('Ctrl Pts',(-43.8266341229871,32.0311632771839,
-41.1331548827895));
#255640=CARTESIAN_POINT('Ctrl Pts',(-43.8644344365312,32.050527928199,-41.1593656410909));
#255641=CARTESIAN_POINT('Ctrl Pts',(-43.8900335656271,32.0628690313763,
-41.1767476889401));
#255642=CARTESIAN_POINT('Ctrl Pts',(-43.903042008964,32.0687560539784,-41.1853974312384));
#255643=CARTESIAN_POINT('Ctrl Pts',(-43.9291618902095,32.0798229381751,
-41.2024070088898));
#255644=CARTESIAN_POINT('Ctrl Pts',(-43.9423286751247,32.0850301956599,
-41.2108047653586));
#255645=CARTESIAN_POINT('Ctrl Pts',(-43.9688389276373,32.0947834481969,
-41.2273662374836));
#255646=CARTESIAN_POINT('Ctrl Pts',(-44.0088868242005,32.1084293286422,
-41.2518690158044));
#255647=CARTESIAN_POINT('Ctrl Pts',(-44.0634057706764,32.1227159830699,
-41.2831968728749));
#255648=CARTESIAN_POINT('Ctrl Pts',(-44.1051448739617,32.1304686073096,
-41.30568419746));
#255649=CARTESIAN_POINT('Ctrl Pts',(-44.1331632182567,32.1349666221674,
-41.3204486001008));
#255650=CARTESIAN_POINT('Ctrl Pts',(-44.1472622735965,32.1368798783668,
-41.3277141420552));
#255651=CARTESIAN_POINT('Ctrl Pts',(-44.1685768983456,32.1392377391899,
-41.3384485067576));
#255652=CARTESIAN_POINT('Ctrl Pts',(-44.1757038998442,32.1399371964,-41.3419962566417));
#255653=CARTESIAN_POINT('Ctrl Pts',(-44.1899298892594,32.1411565650423,
-41.3489954369734));
#255654=CARTESIAN_POINT('Ctrl Pts',(-44.1970429564213,32.1416781032566,
-41.3524539903966));
#255655=CARTESIAN_POINT('Ctrl Pts',(-44.2183581262916,32.1429776302475,
-41.3626954949199));
#255656=CARTESIAN_POINT('Ctrl Pts',(-44.232556678806,32.1434929542666,-41.3693546778539));
#255657=CARTESIAN_POINT('Ctrl Pts',(-44.2750884056492,32.1439936324359,
-41.3888189062651));
#255658=CARTESIAN_POINT('Ctrl Pts',(-44.3033804172497,32.1429384256622,
-41.4011231160504));
#255659=CARTESIAN_POINT('Ctrl Pts',(-44.3598247343314,32.13804594572,-41.4243882373187));
#255660=CARTESIAN_POINT('Ctrl Pts',(-44.3879848006206,32.1342064546963,
-41.4353516241949));
#255661=CARTESIAN_POINT('Ctrl Pts',(-44.4230841862873,32.1276226980045,
-41.4481948195873));
#255662=CARTESIAN_POINT('Ctrl Pts',(-44.4301039616143,32.126214419323,-41.4507215814638));
#255663=CARTESIAN_POINT('Ctrl Pts',(-44.4441256434231,32.1232190082407,
-41.455685422358));
#255664=CARTESIAN_POINT('Ctrl Pts',(-44.4511413829898,32.1216281453652,
-41.4581270453932));
#255665=CARTESIAN_POINT('Ctrl Pts',(-44.472106554004,32.1165956901708,-41.4652964871519));
#255666=CARTESIAN_POINT('Ctrl Pts',(-44.4859328208737,32.1129061786889,
-41.4698557698741));
#255667=CARTESIAN_POINT('Ctrl Pts',(-44.5270324780087,32.1008340938932,
-41.4829067838587));
#255668=CARTESIAN_POINT('Ctrl Pts',(-44.5673316800757,32.08677017453,-41.4946921125766));
#255669=CARTESIAN_POINT('Ctrl Pts',(-44.6194780799712,32.0640738471498,
-41.5079096337926));
#255670=CARTESIAN_POINT('Ctrl Pts',(-44.6577884739158,32.045065905176,-41.5165678887371));
#255671=CARTESIAN_POINT('Ctrl Pts',(-44.6827916371924,32.031050813041,-41.5214942665077));
#255672=CARTESIAN_POINT('Ctrl Pts',(-44.7075150580676,32.0163554529027,
-41.5259894017533));
#255673=CARTESIAN_POINT('Ctrl Pts',(-44.7197631353705,32.0086467826241,
-41.5280237577537));
#255674=CARTESIAN_POINT('Ctrl Pts',(-44.7436779765282,31.9927322821733,
-41.5316086326721));
#255675=CARTESIAN_POINT('Ctrl Pts',(-44.7554039451266,31.9844926239501,
-41.5331705278033));
#255676=CARTESIAN_POINT('Ctrl Pts',(-44.7783650010144,31.9674779303508,
-41.5358342782831));
#255677=CARTESIAN_POINT('Ctrl Pts',(-44.8120876763637,31.941142023486,-41.5391427937509));
#255678=CARTESIAN_POINT('Ctrl Pts',(-44.8542060542843,31.9028069711657,
-41.5408368316843));
#255679=CARTESIAN_POINT('Ctrl Pts',(-44.883650374082,31.8716290815775,-41.5400605624154));
#255680=CARTESIAN_POINT('Ctrl Pts',(-44.9027957424029,31.8502960261458,
-41.5390808606534));
#255681=CARTESIAN_POINT('Ctrl Pts',(-44.912124025092,31.8393588588263,-41.5383603441012));
#255682=CARTESIAN_POINT('Ctrl Pts',(-44.9302963003321,31.816913187918,-41.5364463589967));
#255683=CARTESIAN_POINT('Ctrl Pts',(-44.9390653236876,31.8054960967264,
-41.5352602514373));
#255684=CARTESIAN_POINT('Ctrl Pts',(-44.9559494861592,31.7823260274566,
-41.532444286592));
#255685=CARTESIAN_POINT('Ctrl Pts',(-44.9803129684955,31.7470436123751,
-41.5275522735743));
#255686=CARTESIAN_POINT('Ctrl Pts',(-45.00183725318,31.7102129370948,-41.5206914933375));
#255687=CARTESIAN_POINT('Ctrl Pts',(-45.0280427451288,31.6597446570548,
-41.5098099510806));
#255688=CARTESIAN_POINT('Ctrl Pts',(-45.0398987329805,31.6338241168053,
-41.5034995556801));
#255689=CARTESIAN_POINT('Ctrl Pts',(-45.0531290598229,31.6005723463994,
-41.4945098705711));
#255690=CARTESIAN_POINT('Ctrl Pts',(-45.0556963147994,31.5938738844661,
-41.4926546478805));
#255691=CARTESIAN_POINT('Ctrl Pts',(-45.0606676096559,31.5803990532317,
-41.4888352403062));
#255692=CARTESIAN_POINT('Ctrl Pts',(-45.0630762139805,31.5736079348959,
-41.4868664774371));
#255693=CARTESIAN_POINT('Ctrl Pts',(-45.0700329505347,31.5531765604049,
-41.4808121016924));
#255694=CARTESIAN_POINT('Ctrl Pts',(-45.0743018132827,31.5395152309552,
-41.4765904297482));
#255695=CARTESIAN_POINT('Ctrl Pts',(-45.0860497029301,31.4983488303989,
-41.4633620161014));
#255696=CARTESIAN_POINT('Ctrl Pts',(-45.0988767040151,31.4430340104486,
-41.4442426901641));
#255697=CARTESIAN_POINT('Ctrl Pts',(-45.1061818129997,31.386882792419,-41.4222207481485));
#255698=CARTESIAN_POINT('Ctrl Pts',(-45.1095857869151,31.3444641027996,
-41.4046111316328));
#255699=CARTESIAN_POINT('Ctrl Pts',(-45.1103739871937,31.3302675876129,
-41.3985560195248));
#255700=CARTESIAN_POINT('Ctrl Pts',(-45.1110306052012,31.30890259785,-41.3891987399731));
#255701=CARTESIAN_POINT('Ctrl Pts',(-45.1111617199316,31.3017636946428,
-41.3860313075819));
#255702=CARTESIAN_POINT('Ctrl Pts',(-45.1112472734604,31.2874686716035,
-41.3796068875509));
#255703=CARTESIAN_POINT('Ctrl Pts',(-45.111201351958,31.2802974166487,-41.3763428889219));
#255704=CARTESIAN_POINT('Ctrl Pts',(-45.1107973541963,31.25882908612,-41.3664479958234));
#255705=CARTESIAN_POINT('Ctrl Pts',(-45.11017580813,31.2446005169708,-41.3597259135069));
#255706=CARTESIAN_POINT('Ctrl Pts',(-45.1082442962718,31.2162677536902,
-41.3460176286356));
#255707=CARTESIAN_POINT('Ctrl Pts',(-45.104314463686,31.1739750543259,-41.3250680443717));
#255708=CARTESIAN_POINT('Ctrl Pts',(-45.0950241996196,31.1183949914011,
-41.295609869938));
#255709=CARTESIAN_POINT('Ctrl Pts',(-45.0817381040079,31.0636149263882,
-41.264634106957));
#255710=CARTESIAN_POINT('Ctrl Pts',(-45.0737554763462,31.0364928582332,
-41.2486352837062));
#255711=CARTESIAN_POINT('Ctrl Pts',(-45.0650963255467,31.0095068957897,
-41.2323777508457));
#255712=CARTESIAN_POINT('Ctrl Pts',(-45.0604265398991,30.996076905732,-41.224116427314));
#255713=CARTESIAN_POINT('Ctrl Pts',(-45.0504049610752,30.9693743366894,
-41.2073411015006));
#255714=CARTESIAN_POINT('Ctrl Pts',(-45.0450945767524,30.9562107421528,
-41.1988958018751));
#255715=CARTESIAN_POINT('Ctrl Pts',(-45.0394875320819,30.9432190801919,
-41.190386719266));
#255716=CARTESIAN_POINT('',(-42.6662672096693,32.3203213022045,-39.2608974781454));
#255717=CARTESIAN_POINT('',(-42.7562642394046,32.238293307241,-39.4336017780241));
#255718=CARTESIAN_POINT('',(-42.6662672096693,32.3203213022045,-39.2608974781454));
#255719=CARTESIAN_POINT('Origin',(-44.4753294917431,31.5614417668058,-39.4557296694497));
#255720=CARTESIAN_POINT('Ctrl Pts',(-43.0434008892766,32.902468814613,-39.4567761948493));
#255721=CARTESIAN_POINT('Ctrl Pts',(-42.9769841821306,32.8009549221958,
-39.4517406334174));
#255722=CARTESIAN_POINT('Ctrl Pts',(-42.919362741941,32.6938935737936,-39.4472380210389));
#255723=CARTESIAN_POINT('Ctrl Pts',(-42.8231628417698,32.4713594324972,
-39.4394681758366));
#255724=CARTESIAN_POINT('Ctrl Pts',(-42.7846681593587,32.3561866606744,
-39.4362084259695));
#255725=CARTESIAN_POINT('Ctrl Pts',(-42.7562642394046,32.2382933072411,
-39.4336017780242));
#255726=CARTESIAN_POINT('Ctrl Pts',(-42.4577131944625,32.5104083279569,
-38.8606823233882));
#255727=CARTESIAN_POINT('Ctrl Pts',(-42.4722685042022,32.5448307979214,
-38.8694323201496));
#255728=CARTESIAN_POINT('Ctrl Pts',(-42.4876674804305,32.5789105800709,
-38.8782643966372));
#255729=CARTESIAN_POINT('Ctrl Pts',(-42.5202146590728,32.6464795812123,
-38.8961197808447));
#255730=CARTESIAN_POINT('Ctrl Pts',(-42.5373018269229,32.6798350022668,
-38.9051083126545));
#255731=CARTESIAN_POINT('Ctrl Pts',(-42.5906929412925,32.7780783962456,
-38.9321048428364));
#255732=CARTESIAN_POINT('Ctrl Pts',(-42.629225789877,32.8414173722334,-38.9502105255134));
#255733=CARTESIAN_POINT('Ctrl Pts',(-42.7120000069194,32.9638220552461,
-38.9866125955295));
#255734=CARTESIAN_POINT('Ctrl Pts',(-42.7562439327448,33.0229003355902,
-39.0049117194725));
#255735=CARTESIAN_POINT('Ctrl Pts',(-42.8269002201102,33.1083282766067,
-39.0325063049612));
#255736=CARTESIAN_POINT('Ctrl Pts',(-42.851168481378,33.1362718559733,-39.0417288667405));
#255737=CARTESIAN_POINT('Ctrl Pts',(-42.9011535535061,33.1910821810744,
-39.0602232021637));
#255738=CARTESIAN_POINT('Ctrl Pts',(-42.9268673384213,33.2179450225078,
-39.0694937486382));
#255739=CARTESIAN_POINT('Ctrl Pts',(-42.9797817061917,33.2705900457306,
-39.088089881442));
#255740=CARTESIAN_POINT('Ctrl Pts',(-43.0069972096607,33.2963736994337,
-39.097418269769));
#255741=CARTESIAN_POINT('Ctrl Pts',(-43.0622936398443,33.3462615369725,
-39.1159154063528));
#255742=CARTESIAN_POINT('Ctrl Pts',(-43.0904949946047,33.3704876748183,
-39.1251268688782));
#255743=CARTESIAN_POINT('Ctrl Pts',(-43.176562606447,33.4408730143711,-39.1525915568785));
#255744=CARTESIAN_POINT('Ctrl Pts',(-43.2360245534179,33.4848790444095,
-39.1707230137558));
#255745=CARTESIAN_POINT('Ctrl Pts',(-43.3282503301662,33.5464830068215,
-39.1976342358769));
#255746=CARTESIAN_POINT('Ctrl Pts',(-43.3595022265301,33.5662859367769,
-39.2065582055264));
#255747=CARTESIAN_POINT('Ctrl Pts',(-43.423032399699,33.604418869649,-39.2243132114598));
#255748=CARTESIAN_POINT('Ctrl Pts',(-43.4553106319894,33.6227489368786,
-39.2331442507783));
#255749=CARTESIAN_POINT('Ctrl Pts',(-43.5209070247133,33.6579164232732,
-39.2507127863664));
#255750=CARTESIAN_POINT('Ctrl Pts',(-43.5542222374601,33.6747516510336,
-39.2594493821381));
#255751=CARTESIAN_POINT('Ctrl Pts',(-43.6219256430316,33.7069073870392,
-39.2768314299875));
#255752=CARTESIAN_POINT('Ctrl Pts',(-43.6563381479934,33.7222286468184,
-39.2854811722856));
#255753=CARTESIAN_POINT('Ctrl Pts',(-43.7254519170511,33.7509934760634,
-39.3024907499371));
#255754=CARTESIAN_POINT('Ctrl Pts',(-43.7602995448845,33.7645084608315,
-39.3108885064059));
#255755=CARTESIAN_POINT('Ctrl Pts',(-43.8304781084082,33.789780836939,-39.3274499785309));
#255756=CARTESIAN_POINT('Ctrl Pts',(-43.8658243285985,33.8015455603985,
-39.3356176307442));
#255757=CARTESIAN_POINT('Ctrl Pts',(-43.9726293607703,33.8342393174696,
-39.3597845530997));
#255758=CARTESIAN_POINT('Ctrl Pts',(-44.0448528416425,33.8525737420732,
-39.3754485022349));
#255759=CARTESIAN_POINT('Ctrl Pts',(-44.1547335161489,33.874826743562,-39.3982722291653));
#255760=CARTESIAN_POINT('Ctrl Pts',(-44.1916183723467,33.8813683146414,
-39.4057679385072));
#255761=CARTESIAN_POINT('Ctrl Pts',(-44.2659122959158,33.8926702964892,
-39.4205323411483));
#255762=CARTESIAN_POINT('Ctrl Pts',(-44.3033049221432,33.8974288658374,
-39.4277978831022));
#255763=CARTESIAN_POINT('Ctrl Pts',(-44.3598453576919,33.9032050944765,
-39.4385322478049));
#255764=CARTESIAN_POINT('Ctrl Pts',(-44.3787527158677,33.9049006163346,
-39.4420799976889));
#255765=CARTESIAN_POINT('Ctrl Pts',(-44.4164967874688,33.9078161173588,
-39.4490791780208));
#255766=CARTESIAN_POINT('Ctrl Pts',(-44.4353708468856,33.9090400957878,
-39.4525377314439));
#255767=CARTESIAN_POINT('Ctrl Pts',(-44.4919347179527,33.9120095261766,
-39.462779235967));
#255768=CARTESIAN_POINT('Ctrl Pts',(-44.52962054914,33.9130584408517,-39.4694384189012));
#255769=CARTESIAN_POINT('Ctrl Pts',(-44.6425299001817,33.9134342925821,
-39.4889026473125));
#255770=CARTESIAN_POINT('Ctrl Pts',(-44.7176656228988,33.9100023852834,
-39.5012068570978));
#255771=CARTESIAN_POINT('Ctrl Pts',(-44.867623327666,33.8957625538083,-39.524471978366));
#255772=CARTESIAN_POINT('Ctrl Pts',(-44.9424659600731,33.8849485744664,
-39.5354353652432));
#255773=CARTESIAN_POINT('Ctrl Pts',(-45.0357885152669,33.8666999843662,
-39.5482785606344));
#255774=CARTESIAN_POINT('Ctrl Pts',(-45.0544546343785,33.8628074782943,
-39.5508053225112));
#255775=CARTESIAN_POINT('Ctrl Pts',(-45.0917431025751,33.8545484160302,
-39.5557691634051));
#255776=CARTESIAN_POINT('Ctrl Pts',(-45.1104022544846,33.8501716550149,
-39.5582107864407));
#255777=CARTESIAN_POINT('Ctrl Pts',(-45.1661672125598,33.8363538303533,
-39.565380228199));
#255778=CARTESIAN_POINT('Ctrl Pts',(-45.2029511118778,33.8262578362557,
-39.5699395109212));
#255779=CARTESIAN_POINT('Ctrl Pts',(-45.2758615915212,33.8042965707928,
-39.578640186911));
#255780=CARTESIAN_POINT('Ctrl Pts',(-45.3119687135373,33.792436319941,-39.5827791123973));
#255781=CARTESIAN_POINT('Ctrl Pts',(-45.3834929078587,33.7669724252328,
-39.5906388675035));
#255782=CARTESIAN_POINT('Ctrl Pts',(-45.4189099726225,33.753368762151,-39.59435969177));
#255783=CARTESIAN_POINT('Ctrl Pts',(-45.4890551197469,33.7244209300036,
-39.6013847808703));
#255784=CARTESIAN_POINT('Ctrl Pts',(-45.5237832050323,33.7090767682036,
-39.60468904687));
#255785=CARTESIAN_POINT('Ctrl Pts',(-45.5925464188782,33.6766380670054,
-39.6108794240926));
#255786=CARTESIAN_POINT('Ctrl Pts',(-45.6265815610841,33.6595435620003,
-39.6137655431243));
#255787=CARTESIAN_POINT('Ctrl Pts',(-45.6939497262655,33.6235811757592,
-39.6191148199286));
#255788=CARTESIAN_POINT('Ctrl Pts',(-45.7272860947277,33.6047101271221,
-39.6215780075552));
#255789=CARTESIAN_POINT('Ctrl Pts',(-45.7932287365117,33.5651705839516,
-39.6260731428005));
#255790=CARTESIAN_POINT('Ctrl Pts',(-45.8259059249178,33.5444453395394,
-39.6281074988012));
#255791=CARTESIAN_POINT('Ctrl Pts',(-45.8897275017006,33.5016881508368,
-39.6316923737189));
#255792=CARTESIAN_POINT('Ctrl Pts',(-45.9210297733036,33.4795651380847,
-39.6332542688506));
#255793=CARTESIAN_POINT('Ctrl Pts',(-45.9823424846244,33.4339088874735,
-39.6359180193303));
#255794=CARTESIAN_POINT('Ctrl Pts',(-46.0123687620003,33.4103663679687,
-39.6370209899198));
#255795=CARTESIAN_POINT('Ctrl Pts',(-46.1005740569048,33.337614535667,-39.639649668426));
#255796=CARTESIAN_POINT('Ctrl Pts',(-46.1568837651934,33.2862857446323,
-39.6404967282823));
#255797=CARTESIAN_POINT('Ctrl Pts',(-46.2375893041651,33.2050303462875,
-39.6404032087595));
#255798=CARTESIAN_POINT('Ctrl Pts',(-46.2638636333332,33.1772336958076,
-39.6401443034625));
#255799=CARTESIAN_POINT('Ctrl Pts',(-46.3151397511292,33.1201974856456,
-39.6391646017005));
#255800=CARTESIAN_POINT('Ctrl Pts',(-46.3401349353408,33.0909661742941,
-39.6384440851485));
#255801=CARTESIAN_POINT('Ctrl Pts',(-46.3888523044997,33.0309971480077,
-39.6365301000439));
#255802=CARTESIAN_POINT('Ctrl Pts',(-46.4123735341802,33.0005036828642,
-39.6353439924849));
#255803=CARTESIAN_POINT('Ctrl Pts',(-46.4576879006691,32.9386388625828,
-39.6325280276392));
#255804=CARTESIAN_POINT('Ctrl Pts',(-46.4794979867991,32.9072463828166,
-39.6308974590955));
#255805=CARTESIAN_POINT('Ctrl Pts',(-46.5424231451674,32.8117200287728,
-39.625348882952));
#255806=CARTESIAN_POINT('Ctrl Pts',(-46.5810426872604,32.7462345994881,
-39.6207752343847));
#255807=CARTESIAN_POINT('Ctrl Pts',(-46.6516918187306,32.6117039458857,
-39.6098936921283));
#255808=CARTESIAN_POINT('Ctrl Pts',(-46.683723185051,32.5426422373878,-39.6035832967262));
#255809=CARTESIAN_POINT('Ctrl Pts',(-46.7195635412788,32.4540883209462,
-39.5945936116187));
#255810=CARTESIAN_POINT('Ctrl Pts',(-46.726523577584,32.4362514419463,-39.5927383889277));
#255811=CARTESIAN_POINT('Ctrl Pts',(-46.7400123459627,32.4003742100513,
-39.5889189813535));
#255812=CARTESIAN_POINT('Ctrl Pts',(-46.7465535157541,32.3822946053341,
-39.5869502184844));
#255813=CARTESIAN_POINT('Ctrl Pts',(-46.7654644360989,32.3279072933141,
-39.5808958427402));
#255814=CARTESIAN_POINT('Ctrl Pts',(-46.7770937339888,32.2915493874552,
-39.5766741707955));
#255815=CARTESIAN_POINT('Ctrl Pts',(-46.7984826125902,32.218525216591,-39.5678552283644));
#255816=CARTESIAN_POINT('Ctrl Pts',(-46.8082356969316,32.1818782626467,
-39.5632601453561));
#255817=CARTESIAN_POINT('Ctrl Pts',(-46.825891612219,32.1083194036329,-39.5537041764669));
#255818=CARTESIAN_POINT('Ctrl Pts',(-46.8337943341285,32.0714074828253,
-39.5487432700414));
#255819=CARTESIAN_POINT('Ctrl Pts',(-46.8547548417649,31.9602784784655,
-39.5333157914925));
#255820=CARTESIAN_POINT('Ctrl Pts',(-46.8650708643863,31.8856621776612,
-39.5223044891954));
#255821=CARTESIAN_POINT('Ctrl Pts',(-46.8750487417844,31.7729724844591,
-39.50469487268));
#255822=CARTESIAN_POINT('Ctrl Pts',(-46.8774570362353,31.7352651712118,
-39.4986397605722));
#255823=CARTESIAN_POINT('Ctrl Pts',(-46.8796767940079,31.6785286095959,
-39.4892824810203));
#255824=CARTESIAN_POINT('Ctrl Pts',(-46.8801843407089,31.6595724593507,
-39.4861150486293));
#255825=CARTESIAN_POINT('Ctrl Pts',(-46.8807312344333,31.6216180949417,
-39.479690628598));
#255826=CARTESIAN_POINT('Ctrl Pts',(-46.8807699646674,31.6025797052015,
-39.4764266299692));
#255827=CARTESIAN_POINT('Ctrl Pts',(-46.8801790388754,31.5455906639181,
-39.4665317368708));
#255828=CARTESIAN_POINT('Ctrl Pts',(-46.8788490796135,31.5078273383739,
-39.4598096545541));
#255829=CARTESIAN_POINT('Ctrl Pts',(-46.874360617844,31.4326451774337,-39.4461013696832));
#255830=CARTESIAN_POINT('Ctrl Pts',(-46.8712024719357,31.3952438451296,
-39.4391182381771));
#255831=CARTESIAN_POINT('Ctrl Pts',(-46.859034870425,31.2835993575687,-39.4177870553822));
#255832=CARTESIAN_POINT('Ctrl Pts',(-46.8473376289695,31.2099145948488,
-39.4030579748028));
#255833=CARTESIAN_POINT('Ctrl Pts',(-46.8244863951756,31.1004910081606,
-39.3802058074804));
#255834=CARTESIAN_POINT('Ctrl Pts',(-46.8159835780379,31.0642007181804,
-39.3724617858671));
#255835=CARTESIAN_POINT('Ctrl Pts',(-46.7971994280146,30.9919902987916,
-39.3567184383004));
#255836=CARTESIAN_POINT('Ctrl Pts',(-46.7869180083019,30.9560697433081,
-39.3487190247537));
#255837=CARTESIAN_POINT('Ctrl Pts',(-46.7645577771926,30.884604709384,-39.332461491893));
#255838=CARTESIAN_POINT('Ctrl Pts',(-46.7524740339114,30.8490466969583,
-39.3242001683612));
#255839=CARTESIAN_POINT('Ctrl Pts',(-46.7264943673172,30.778363271582,-39.3074248425479));
#255840=CARTESIAN_POINT('Ctrl Pts',(-46.7127058212706,30.7435263372096,
-39.2989795429224));
#255841=CARTESIAN_POINT('Ctrl Pts',(-46.6981266849492,30.7091523375488,
-39.2904704603133));
#255842=CARTESIAN_POINT('Ctrl Pts',(-42.6662678860477,32.3203206857175,
-39.2608987761157));
#255843=CARTESIAN_POINT('Ctrl Pts',(-42.678935401819,32.3502354261213,-39.2696487728771));
#255844=CARTESIAN_POINT('Ctrl Pts',(-42.6923355177353,32.3798530670723,
-39.2784808493646));
#255845=CARTESIAN_POINT('Ctrl Pts',(-42.7206547846785,32.4385765514345,
-39.2963362335721));
#255846=CARTESIAN_POINT('Ctrl Pts',(-42.7355208246471,32.4675661149098,
-39.3053247653821));
#255847=CARTESIAN_POINT('Ctrl Pts',(-42.7819675412757,32.5529527044587,
-39.3323212955634));
#255848=CARTESIAN_POINT('Ctrl Pts',(-42.8154832551899,32.6080056255704,
-39.350426978241));
#255849=CARTESIAN_POINT('Ctrl Pts',(-42.8874704180899,32.7144030466848,
-39.3868290482568));
#255850=CARTESIAN_POINT('Ctrl Pts',(-42.9259440972401,32.7657584717183,
-39.4051281722));
#255851=CARTESIAN_POINT('Ctrl Pts',(-42.9873793042677,32.8400236828058,
-39.4327227576885));
#255852=CARTESIAN_POINT('Ctrl Pts',(-43.0084794421579,32.864316719619,-39.4419453194678));
#255853=CARTESIAN_POINT('Ctrl Pts',(-43.0519372785408,32.9119682754171,
-39.4604396548911));
#255854=CARTESIAN_POINT('Ctrl Pts',(-43.0742923458191,32.9353234004109,
-39.4697102013656));
#255855=CARTESIAN_POINT('Ctrl Pts',(-43.1202932730876,32.9810958260852,
-39.4883063341693));
#255856=CARTESIAN_POINT('Ctrl Pts',(-43.1439520951656,33.0035144156811,
-39.4976347224965));
#255857=CARTESIAN_POINT('Ctrl Pts',(-43.1920203654931,33.0468931109494,
-39.5161318590801));
#255858=CARTESIAN_POINT('Ctrl Pts',(-43.2165345089143,33.0679592485651,
-39.5253433216058));
#255859=CARTESIAN_POINT('Ctrl Pts',(-43.2913467365328,33.1291664924534,
-39.5528080096058));
#255860=CARTESIAN_POINT('Ctrl Pts',(-43.3430295011989,33.16743806238,-39.5709394664834));
#255861=CARTESIAN_POINT('Ctrl Pts',(-43.42318529819,33.2210204170675,-39.5978506886043));
#255862=CARTESIAN_POINT('Ctrl Pts',(-43.4503464116134,33.2382458390107,
-39.6067746582539));
#255863=CARTESIAN_POINT('Ctrl Pts',(-43.5055592644833,33.2714177212331,
-39.6245296641872));
#255864=CARTESIAN_POINT('Ctrl Pts',(-43.5336109652927,33.2873642373592,
-39.6333607035057));
#255865=CARTESIAN_POINT('Ctrl Pts',(-43.5906167586109,33.3179611793576,
-39.6509292390937));
#255866=CARTESIAN_POINT('Ctrl Pts',(-43.6195682890663,33.3326096993947,
-39.6596658348655));
#255867=CARTESIAN_POINT('Ctrl Pts',(-43.6784024489033,33.3605914924566,
-39.6770478827149));
#255868=CARTESIAN_POINT('Ctrl Pts',(-43.7083061985044,33.3739254346794,
-39.685697625013));
#255869=CARTESIAN_POINT('Ctrl Pts',(-43.7683633256242,33.3989622002509,
-39.7027072026645));
#255870=CARTESIAN_POINT('Ctrl Pts',(-43.7986438942497,33.4107271662336,
-39.7111049591333));
#255871=CARTESIAN_POINT('Ctrl Pts',(-43.8596237489107,33.4327304463716,
-39.7276664312583));
#255872=CARTESIAN_POINT('Ctrl Pts',(-43.8903363171894,33.4429751408118,
-39.7358340834717));
#255873=CARTESIAN_POINT('Ctrl Pts',(-43.9831381063675,33.4714505290734,
-39.7600010058271));
#255874=CARTESIAN_POINT('Ctrl Pts',(-44.045889936343,33.4874275689807,-39.7756649549624));
#255875=CARTESIAN_POINT('Ctrl Pts',(-44.1413569064837,33.5068342142111,
-39.7984886818927));
#255876=CARTESIAN_POINT('Ctrl Pts',(-44.1734027712035,33.5125421273567,
-39.8059843912346));
#255877=CARTESIAN_POINT('Ctrl Pts',(-44.2379487660953,33.522410856807,-39.8207487938757));
#255878=CARTESIAN_POINT('Ctrl Pts',(-44.2704346127381,33.5265700622991,
-39.8280143358296));
#255879=CARTESIAN_POINT('Ctrl Pts',(-44.3195547480624,33.53162621339,-39.8387487005323));
#255880=CARTESIAN_POINT('Ctrl Pts',(-44.3359805797293,33.5331119147056,
-39.8422964504163));
#255881=CARTESIAN_POINT('Ctrl Pts',(-44.368770578548,33.5356701262535,-39.8492956307481));
#255882=CARTESIAN_POINT('Ctrl Pts',(-44.3851671905622,33.5367461359866,
-39.8527541841713));
#255883=CARTESIAN_POINT('Ctrl Pts',(-44.4343059395537,33.5393638020221,
-39.8629956886945));
#255884=CARTESIAN_POINT('Ctrl Pts',(-44.4670441867038,33.5403003160803,
-39.8696548716286));
#255885=CARTESIAN_POINT('Ctrl Pts',(-44.5651285248139,33.5407024624404,
-39.8891191000399));
#255886=CARTESIAN_POINT('Ctrl Pts',(-44.6303966421524,33.5377712059725,
-39.9014233098251));
#255887=CARTESIAN_POINT('Ctrl Pts',(-44.7606557964568,33.5255003896343,
-39.9246884310934));
#255888=CARTESIAN_POINT('Ctrl Pts',(-44.8256647686024,33.5161555829264,
-39.9356518179704));
#255889=CARTESIAN_POINT('Ctrl Pts',(-44.9067226409372,33.5003641844135,
-39.9484950133618));
#255890=CARTESIAN_POINT('Ctrl Pts',(-44.9229354632917,33.4969949796552,
-39.9510217752386));
#255891=CARTESIAN_POINT('Ctrl Pts',(-44.9553227940458,33.4898447029991,
-39.9559856161326));
#255892=CARTESIAN_POINT('Ctrl Pts',(-44.971529266705,33.4860547900967,-39.958427239168));
#255893=CARTESIAN_POINT('Ctrl Pts',(-45.019963666253,33.4740875993182,-39.9655966809264));
#255894=CARTESIAN_POINT('Ctrl Pts',(-45.0519115512582,33.4653411277245,
-39.9701559636487));
#255895=CARTESIAN_POINT('Ctrl Pts',(-45.1152352219466,33.4463106730797,
-39.9788566396385));
#255896=CARTESIAN_POINT('Ctrl Pts',(-45.1465941073248,33.436031038673,-39.9829955651248));
#255897=CARTESIAN_POINT('Ctrl Pts',(-45.2087113592473,33.4139567327306,
-39.9908553202309));
#255898=CARTESIAN_POINT('Ctrl Pts',(-45.2394697192292,33.4021620444808,
-39.9945761444974));
#255899=CARTESIAN_POINT('Ctrl Pts',(-45.3003868460925,33.3770601489593,
-40.0016012335977));
#255900=CARTESIAN_POINT('Ctrl Pts',(-45.3305456155218,33.3637529479941,
-40.0049054995974));
#255901=CARTESIAN_POINT('Ctrl Pts',(-45.3902600985989,33.3356174580523,
-40.01109587682));
#255902=CARTESIAN_POINT('Ctrl Pts',(-45.4198158241265,33.3207891989555,
-40.0139819958517));
#255903=CARTESIAN_POINT('Ctrl Pts',(-45.4783162406983,33.289591616671,-40.0193312726561));
#255904=CARTESIAN_POINT('Ctrl Pts',(-45.5072638360001,33.2732195440424,
-40.0217944602826));
#255905=CARTESIAN_POINT('Ctrl Pts',(-45.5645236685819,33.2389134161644,
-40.0262895955279));
#255906=CARTESIAN_POINT('Ctrl Pts',(-45.5928974744892,33.2209301068779,
-40.0283239515286));
#255907=CARTESIAN_POINT('Ctrl Pts',(-45.6483127164684,33.183827317638,-40.0319088264464));
#255908=CARTESIAN_POINT('Ctrl Pts',(-45.6754912491912,33.164628826888,-40.033470721578));
#255909=CARTESIAN_POINT('Ctrl Pts',(-45.7287252026082,33.1250059065848,
-40.0361344720577));
#255910=CARTESIAN_POINT('Ctrl Pts',(-45.7547943757217,33.1045734241173,
-40.0372374426473));
#255911=CARTESIAN_POINT('Ctrl Pts',(-45.8313729898423,33.0414293618193,
-40.0398661211534));
#255912=CARTESIAN_POINT('Ctrl Pts',(-45.8802572019016,32.996875335828,-40.0407131810096));
#255913=CARTESIAN_POINT('Ctrl Pts',(-45.9503152695219,32.9263392450608,
-40.0406196614869));
#255914=CARTESIAN_POINT('Ctrl Pts',(-45.9731223693318,32.9022087072537,
-40.04036075619));
#255915=CARTESIAN_POINT('Ctrl Pts',(-46.0176301600934,32.8526933495872,
-40.0393810544279));
#255916=CARTESIAN_POINT('Ctrl Pts',(-46.0393251189803,32.8273156909405,
-40.0386605378759));
#255917=CARTESIAN_POINT('Ctrl Pts',(-46.0816081786906,32.7752509415469,
-40.0367465527713));
#255918=CARTESIAN_POINT('Ctrl Pts',(-46.1020218631531,32.7487759054673,
-40.0355604452122));
#255919=CARTESIAN_POINT('Ctrl Pts',(-46.1413474207414,32.6950621160095,
-40.0327444803666));
#255920=CARTESIAN_POINT('Ctrl Pts',(-46.1602740044506,32.6678050222156,
-40.0311139118228));
#255921=CARTESIAN_POINT('Ctrl Pts',(-46.2148766161292,32.5848603625352,
-40.0255653356794));
#255922=CARTESIAN_POINT('Ctrl Pts',(-46.2483838166511,32.5279971310113,
-40.0209916871121));
#255923=CARTESIAN_POINT('Ctrl Pts',(-46.3096709166782,32.4111741762596,
-40.0101101448556));
#255924=CARTESIAN_POINT('Ctrl Pts',(-46.337452349158,32.351200134253,-40.0037997494539));
#255925=CARTESIAN_POINT('Ctrl Pts',(-46.3685299134922,32.2742955884667,
-39.9948100643461));
#255926=CARTESIAN_POINT('Ctrl Pts',(-46.3745646125082,32.2588050117033,
-39.9929548416551));
#255927=CARTESIAN_POINT('Ctrl Pts',(-46.3862591791565,32.2276468348101,
-39.9891354340809));
#255928=CARTESIAN_POINT('Ctrl Pts',(-46.3919298260057,32.2119451443588,
-39.9871666712118));
#255929=CARTESIAN_POINT('Ctrl Pts',(-46.4083226032432,32.1647106343652,
-39.9811122954676));
#255930=CARTESIAN_POINT('Ctrl Pts',(-46.418401428985,32.1331337514891,-39.9768906235228));
#255931=CARTESIAN_POINT('Ctrl Pts',(-46.4369345420855,32.0697109656014,
-39.9680716810918));
#255932=CARTESIAN_POINT('Ctrl Pts',(-46.4453831985413,32.0378818340676,
-39.9634765980836));
#255933=CARTESIAN_POINT('Ctrl Pts',(-46.4606729029267,31.9739922725109,
-39.9539206291942));
#255934=CARTESIAN_POINT('Ctrl Pts',(-46.4675138561323,31.9419318287439,
-39.9489597227689));
#255935=CARTESIAN_POINT('Ctrl Pts',(-46.4856493778314,31.8454072024775,
-39.9335322442199));
#255936=CARTESIAN_POINT('Ctrl Pts',(-46.4945617255914,31.78059453833,-39.9225209419229));
#255937=CARTESIAN_POINT('Ctrl Pts',(-46.50315481336,31.6827073984777,-39.9049113254075));
#255938=CARTESIAN_POINT('Ctrl Pts',(-46.5052218357471,31.6499526236153,
-39.8988562132996));
#255939=CARTESIAN_POINT('Ctrl Pts',(-46.5071123188746,31.6006670667202,
-39.8894989337477));
#255940=CARTESIAN_POINT('Ctrl Pts',(-46.5075405703607,31.5842002139207,
-39.8863315013567));
#255941=CARTESIAN_POINT('Ctrl Pts',(-46.5079902829931,31.5512296784738,
-39.8799070813255));
#255942=CARTESIAN_POINT('Ctrl Pts',(-46.5080111813793,31.5346910950095,
-39.8766430826966));
#255943=CARTESIAN_POINT('Ctrl Pts',(-46.5074596318877,31.4851844744852,
-39.8667481895982));
#255944=CARTESIAN_POINT('Ctrl Pts',(-46.5062788995272,31.4523787341376,
-39.8600261072815));
#255945=CARTESIAN_POINT('Ctrl Pts',(-46.5023290580356,31.3870653764436,
-39.8463178224105));
#255946=CARTESIAN_POINT('Ctrl Pts',(-46.4995602704424,31.3545729642139,
-39.8393346909045));
#255947=CARTESIAN_POINT('Ctrl Pts',(-46.4889145018408,31.2575800929905,
-39.8180035081097));
#255948=CARTESIAN_POINT('Ctrl Pts',(-46.4787027861653,31.1935630330159,
-39.8032744275302));
#255949=CARTESIAN_POINT('Ctrl Pts',(-46.4587767101283,31.0984927565591,
-39.7804222602078));
#255950=CARTESIAN_POINT('Ctrl Pts',(-46.4513652889539,31.0669621539425,
-39.7726782385945));
#255951=CARTESIAN_POINT('Ctrl Pts',(-46.4349975412466,31.0042213777813,
-39.7569348910278));
#255952=CARTESIAN_POINT('Ctrl Pts',(-46.4260411389904,30.9730108340646,
-39.7489354774811));
#255953=CARTESIAN_POINT('Ctrl Pts',(-46.4065670339061,30.9109152953089,
-39.7326779446204));
#255954=CARTESIAN_POINT('Ctrl Pts',(-46.3960450372602,30.8800185402287,
-39.7244166210886));
#255955=CARTESIAN_POINT('Ctrl Pts',(-46.3734269342347,30.8185996612379,
-39.7076412952753));
#255956=CARTESIAN_POINT('Ctrl Pts',(-46.3614243089069,30.7883282055528,
-39.6991959956498));
#255957=CARTESIAN_POINT('Ctrl Pts',(-46.3487351394075,30.7584583851184,
-39.6906869130407));
#255958=CARTESIAN_POINT('',(-42.4577131917459,32.5104083291869,-38.8606823230689));
#255959=CARTESIAN_POINT('',(-42.4577131944625,32.5104083279569,-38.8606823233882));
#255960=CARTESIAN_POINT('',(-46.6981266849484,30.7091523375492,-39.2904704603132));
#255961=CARTESIAN_POINT('Ctrl Pts',(-42.4577131904514,32.5104083297438,
-38.8606823230314));
#255962=CARTESIAN_POINT('Ctrl Pts',(-42.4722685042036,32.5448307979246,
-38.8694323201505));
#255963=CARTESIAN_POINT('Ctrl Pts',(-42.4876674804313,32.5789105800726,
-38.8782643966377));
#255964=CARTESIAN_POINT('Ctrl Pts',(-42.5202146590728,32.6464795812123,
-38.8961197808447));
#255965=CARTESIAN_POINT('Ctrl Pts',(-42.5373018269229,32.6798350022668,
-38.9051083126545));
#255966=CARTESIAN_POINT('Ctrl Pts',(-42.5906929412925,32.7780783962456,
-38.9321048428364));
#255967=CARTESIAN_POINT('Ctrl Pts',(-42.629225789877,32.8414173722334,-38.9502105255134));
#255968=CARTESIAN_POINT('Ctrl Pts',(-42.7120000069194,32.9638220552461,
-38.9866125955295));
#255969=CARTESIAN_POINT('Ctrl Pts',(-42.7562439327448,33.0229003355902,
-39.0049117194725));
#255970=CARTESIAN_POINT('Ctrl Pts',(-42.8269002201102,33.1083282766067,
-39.0325063049612));
#255971=CARTESIAN_POINT('Ctrl Pts',(-42.851168481378,33.1362718559733,-39.0417288667405));
#255972=CARTESIAN_POINT('Ctrl Pts',(-42.9011535535061,33.1910821810744,
-39.0602232021637));
#255973=CARTESIAN_POINT('Ctrl Pts',(-42.9268673384213,33.2179450225078,
-39.0694937486382));
#255974=CARTESIAN_POINT('Ctrl Pts',(-42.9797817061917,33.2705900457306,
-39.088089881442));
#255975=CARTESIAN_POINT('Ctrl Pts',(-43.0069972096607,33.2963736994337,
-39.097418269769));
#255976=CARTESIAN_POINT('Ctrl Pts',(-43.0622936398443,33.3462615369725,
-39.1159154063528));
#255977=CARTESIAN_POINT('Ctrl Pts',(-43.0904949946047,33.3704876748183,
-39.1251268688782));
#255978=CARTESIAN_POINT('Ctrl Pts',(-43.176562606447,33.4408730143711,-39.1525915568785));
#255979=CARTESIAN_POINT('Ctrl Pts',(-43.2360245534179,33.4848790444095,
-39.1707230137558));
#255980=CARTESIAN_POINT('Ctrl Pts',(-43.3282503301662,33.5464830068215,
-39.1976342358769));
#255981=CARTESIAN_POINT('Ctrl Pts',(-43.3595022265301,33.5662859367769,
-39.2065582055264));
#255982=CARTESIAN_POINT('Ctrl Pts',(-43.423032399699,33.604418869649,-39.2243132114598));
#255983=CARTESIAN_POINT('Ctrl Pts',(-43.4553106319894,33.6227489368786,
-39.2331442507783));
#255984=CARTESIAN_POINT('Ctrl Pts',(-43.5209070247133,33.6579164232732,
-39.2507127863664));
#255985=CARTESIAN_POINT('Ctrl Pts',(-43.5542222374601,33.6747516510336,
-39.2594493821381));
#255986=CARTESIAN_POINT('Ctrl Pts',(-43.6219256430316,33.7069073870392,
-39.2768314299875));
#255987=CARTESIAN_POINT('Ctrl Pts',(-43.6563381479934,33.7222286468184,
-39.2854811722856));
#255988=CARTESIAN_POINT('Ctrl Pts',(-43.7254519170511,33.7509934760634,
-39.3024907499371));
#255989=CARTESIAN_POINT('Ctrl Pts',(-43.7602995448845,33.7645084608315,
-39.3108885064059));
#255990=CARTESIAN_POINT('Ctrl Pts',(-43.8304781084082,33.789780836939,-39.3274499785309));
#255991=CARTESIAN_POINT('Ctrl Pts',(-43.8658243285985,33.8015455603985,
-39.3356176307442));
#255992=CARTESIAN_POINT('Ctrl Pts',(-43.9726293607703,33.8342393174696,
-39.3597845530997));
#255993=CARTESIAN_POINT('Ctrl Pts',(-44.0448528416425,33.8525737420732,
-39.3754485022349));
#255994=CARTESIAN_POINT('Ctrl Pts',(-44.1547335161489,33.874826743562,-39.3982722291653));
#255995=CARTESIAN_POINT('Ctrl Pts',(-44.1916183723467,33.8813683146414,
-39.4057679385072));
#255996=CARTESIAN_POINT('Ctrl Pts',(-44.2659122959158,33.8926702964892,
-39.4205323411483));
#255997=CARTESIAN_POINT('Ctrl Pts',(-44.3033049221432,33.8974288658374,
-39.4277978831022));
#255998=CARTESIAN_POINT('Ctrl Pts',(-44.3598453576919,33.9032050944765,
-39.4385322478049));
#255999=CARTESIAN_POINT('Ctrl Pts',(-44.3787527158677,33.9049006163346,
-39.4420799976889));
#256000=CARTESIAN_POINT('Ctrl Pts',(-44.4164967874688,33.9078161173588,
-39.4490791780208));
#256001=CARTESIAN_POINT('Ctrl Pts',(-44.4353708468856,33.9090400957878,
-39.4525377314439));
#256002=CARTESIAN_POINT('Ctrl Pts',(-44.4919347179527,33.9120095261766,
-39.462779235967));
#256003=CARTESIAN_POINT('Ctrl Pts',(-44.52962054914,33.9130584408517,-39.4694384189012));
#256004=CARTESIAN_POINT('Ctrl Pts',(-44.6425299001817,33.9134342925821,
-39.4889026473125));
#256005=CARTESIAN_POINT('Ctrl Pts',(-44.7176656228988,33.9100023852834,
-39.5012068570978));
#256006=CARTESIAN_POINT('Ctrl Pts',(-44.867623327666,33.8957625538083,-39.524471978366));
#256007=CARTESIAN_POINT('Ctrl Pts',(-44.9424659600731,33.8849485744664,
-39.5354353652432));
#256008=CARTESIAN_POINT('Ctrl Pts',(-45.0357885152669,33.8666999843662,
-39.5482785606344));
#256009=CARTESIAN_POINT('Ctrl Pts',(-45.0544546343785,33.8628074782943,
-39.5508053225112));
#256010=CARTESIAN_POINT('Ctrl Pts',(-45.0917431025751,33.8545484160302,
-39.5557691634051));
#256011=CARTESIAN_POINT('Ctrl Pts',(-45.1104022544846,33.8501716550149,
-39.5582107864407));
#256012=CARTESIAN_POINT('Ctrl Pts',(-45.1661672125598,33.8363538303533,
-39.565380228199));
#256013=CARTESIAN_POINT('Ctrl Pts',(-45.2029511118778,33.8262578362557,
-39.5699395109212));
#256014=CARTESIAN_POINT('Ctrl Pts',(-45.2758615915212,33.8042965707928,
-39.578640186911));
#256015=CARTESIAN_POINT('Ctrl Pts',(-45.3119687135373,33.792436319941,-39.5827791123973));
#256016=CARTESIAN_POINT('Ctrl Pts',(-45.3834929078587,33.7669724252328,
-39.5906388675035));
#256017=CARTESIAN_POINT('Ctrl Pts',(-45.4189099726225,33.753368762151,-39.59435969177));
#256018=CARTESIAN_POINT('Ctrl Pts',(-45.4890551197469,33.7244209300036,
-39.6013847808703));
#256019=CARTESIAN_POINT('Ctrl Pts',(-45.5237832050323,33.7090767682036,
-39.60468904687));
#256020=CARTESIAN_POINT('Ctrl Pts',(-45.5925464188782,33.6766380670054,
-39.6108794240926));
#256021=CARTESIAN_POINT('Ctrl Pts',(-45.6265815610841,33.6595435620003,
-39.6137655431243));
#256022=CARTESIAN_POINT('Ctrl Pts',(-45.6939497262655,33.6235811757592,
-39.6191148199286));
#256023=CARTESIAN_POINT('Ctrl Pts',(-45.7272860947277,33.6047101271221,
-39.6215780075552));
#256024=CARTESIAN_POINT('Ctrl Pts',(-45.7932287365117,33.5651705839516,
-39.6260731428005));
#256025=CARTESIAN_POINT('Ctrl Pts',(-45.8259059249178,33.5444453395394,
-39.6281074988012));
#256026=CARTESIAN_POINT('Ctrl Pts',(-45.8897275017006,33.5016881508368,
-39.6316923737189));
#256027=CARTESIAN_POINT('Ctrl Pts',(-45.9210297733036,33.4795651380847,
-39.6332542688506));
#256028=CARTESIAN_POINT('Ctrl Pts',(-45.9823424846244,33.4339088874735,
-39.6359180193303));
#256029=CARTESIAN_POINT('Ctrl Pts',(-46.0123687620003,33.4103663679687,
-39.6370209899198));
#256030=CARTESIAN_POINT('Ctrl Pts',(-46.1005740569048,33.337614535667,-39.639649668426));
#256031=CARTESIAN_POINT('Ctrl Pts',(-46.1568837651934,33.2862857446323,
-39.6404967282823));
#256032=CARTESIAN_POINT('Ctrl Pts',(-46.2375893041651,33.2050303462875,
-39.6404032087595));
#256033=CARTESIAN_POINT('Ctrl Pts',(-46.2638636333332,33.1772336958076,
-39.6401443034625));
#256034=CARTESIAN_POINT('Ctrl Pts',(-46.3151397511292,33.1201974856456,
-39.6391646017005));
#256035=CARTESIAN_POINT('Ctrl Pts',(-46.3401349353408,33.0909661742941,
-39.6384440851485));
#256036=CARTESIAN_POINT('Ctrl Pts',(-46.3888523044997,33.0309971480077,
-39.6365301000439));
#256037=CARTESIAN_POINT('Ctrl Pts',(-46.4123735341802,33.0005036828642,
-39.6353439924849));
#256038=CARTESIAN_POINT('Ctrl Pts',(-46.4576879006691,32.9386388625828,
-39.6325280276392));
#256039=CARTESIAN_POINT('Ctrl Pts',(-46.4794979867991,32.9072463828166,
-39.6308974590955));
#256040=CARTESIAN_POINT('Ctrl Pts',(-46.5424231451674,32.8117200287728,
-39.625348882952));
#256041=CARTESIAN_POINT('Ctrl Pts',(-46.5810426872604,32.7462345994881,
-39.6207752343847));
#256042=CARTESIAN_POINT('Ctrl Pts',(-46.6516918187306,32.6117039458857,
-39.6098936921283));
#256043=CARTESIAN_POINT('Ctrl Pts',(-46.683723185051,32.5426422373878,-39.6035832967262));
#256044=CARTESIAN_POINT('Ctrl Pts',(-46.7195635412788,32.4540883209462,
-39.5945936116187));
#256045=CARTESIAN_POINT('Ctrl Pts',(-46.726523577584,32.4362514419463,-39.5927383889277));
#256046=CARTESIAN_POINT('Ctrl Pts',(-46.7400123459627,32.4003742100513,
-39.5889189813535));
#256047=CARTESIAN_POINT('Ctrl Pts',(-46.7465535157541,32.3822946053341,
-39.5869502184844));
#256048=CARTESIAN_POINT('Ctrl Pts',(-46.7654644360989,32.3279072933141,
-39.5808958427402));
#256049=CARTESIAN_POINT('Ctrl Pts',(-46.7770937339888,32.2915493874552,
-39.5766741707955));
#256050=CARTESIAN_POINT('Ctrl Pts',(-46.7984826125902,32.218525216591,-39.5678552283644));
#256051=CARTESIAN_POINT('Ctrl Pts',(-46.8082356969316,32.1818782626467,
-39.5632601453561));
#256052=CARTESIAN_POINT('Ctrl Pts',(-46.825891612219,32.1083194036329,-39.5537041764669));
#256053=CARTESIAN_POINT('Ctrl Pts',(-46.8337943341285,32.0714074828253,
-39.5487432700414));
#256054=CARTESIAN_POINT('Ctrl Pts',(-46.8547548417649,31.9602784784655,
-39.5333157914925));
#256055=CARTESIAN_POINT('Ctrl Pts',(-46.8650708643863,31.8856621776612,
-39.5223044891954));
#256056=CARTESIAN_POINT('Ctrl Pts',(-46.8750487417844,31.7729724844591,
-39.50469487268));
#256057=CARTESIAN_POINT('Ctrl Pts',(-46.8774570362353,31.7352651712118,
-39.4986397605722));
#256058=CARTESIAN_POINT('Ctrl Pts',(-46.8796767940079,31.6785286095959,
-39.4892824810203));
#256059=CARTESIAN_POINT('Ctrl Pts',(-46.8801843407089,31.6595724593507,
-39.4861150486293));
#256060=CARTESIAN_POINT('Ctrl Pts',(-46.8807312344333,31.6216180949417,
-39.479690628598));
#256061=CARTESIAN_POINT('Ctrl Pts',(-46.8807699646674,31.6025797052015,
-39.4764266299692));
#256062=CARTESIAN_POINT('Ctrl Pts',(-46.8801790388754,31.5455906639181,
-39.4665317368708));
#256063=CARTESIAN_POINT('Ctrl Pts',(-46.8788490796135,31.5078273383739,
-39.4598096545541));
#256064=CARTESIAN_POINT('Ctrl Pts',(-46.874360617844,31.4326451774337,-39.4461013696832));
#256065=CARTESIAN_POINT('Ctrl Pts',(-46.8712024719357,31.3952438451296,
-39.4391182381771));
#256066=CARTESIAN_POINT('Ctrl Pts',(-46.859034870425,31.2835993575687,-39.4177870553822));
#256067=CARTESIAN_POINT('Ctrl Pts',(-46.8473376289695,31.2099145948488,
-39.4030579748028));
#256068=CARTESIAN_POINT('Ctrl Pts',(-46.8244863951756,31.1004910081606,
-39.3802058074804));
#256069=CARTESIAN_POINT('Ctrl Pts',(-46.8159835780379,31.0642007181804,
-39.3724617858671));
#256070=CARTESIAN_POINT('Ctrl Pts',(-46.7971994280146,30.9919902987916,
-39.3567184383004));
#256071=CARTESIAN_POINT('Ctrl Pts',(-46.7869180083019,30.9560697433081,
-39.3487190247537));
#256072=CARTESIAN_POINT('Ctrl Pts',(-46.7645577771926,30.884604709384,-39.332461491893));
#256073=CARTESIAN_POINT('Ctrl Pts',(-46.7524740339114,30.8490466969583,
-39.3242001683612));
#256074=CARTESIAN_POINT('Ctrl Pts',(-46.7264943673172,30.778363271582,-39.3074248425479));
#256075=CARTESIAN_POINT('Ctrl Pts',(-46.7127058212706,30.7435263372096,
-39.2989795429224));
#256076=CARTESIAN_POINT('Ctrl Pts',(-46.6981266849484,30.7091523375492,
-39.2904704603132));
#256077=CARTESIAN_POINT('',(-46.348736272544,30.7584582252104,-39.6906856150703));
#256078=CARTESIAN_POINT('',(-46.6981266849484,30.7091523375492,-39.2904704603132));
#256079=CARTESIAN_POINT('',(-46.5057017799105,31.6353141775361,-39.8960581789586));
#256080=CARTESIAN_POINT('Ctrl Pts',(-46.5057014676852,31.6353142217915,
-39.89605787487));
#256081=CARTESIAN_POINT('Ctrl Pts',(-46.5059898391685,31.6292400867244,
-39.8949168219445));
#256082=CARTESIAN_POINT('Ctrl Pts',(-46.5062503858504,31.6231697137711,
-39.8937699034812));
#256083=CARTESIAN_POINT('Ctrl Pts',(-46.5071135271648,31.6006673192385,
-39.8894976357773));
#256084=CARTESIAN_POINT('Ctrl Pts',(-46.5075417789082,31.5842004583658,
-39.8863302033863));
#256085=CARTESIAN_POINT('Ctrl Pts',(-46.5079914918558,31.5512299067555,
-39.8799057833551));
#256086=CARTESIAN_POINT('Ctrl Pts',(-46.5080123902999,31.5346913151838,
-39.8766417847262));
#256087=CARTESIAN_POINT('Ctrl Pts',(-46.5074608406805,31.4851846703929,
-39.8667468916278));
#256088=CARTESIAN_POINT('Ctrl Pts',(-46.506280107836,31.4523789139669,-39.8600248093111));
#256089=CARTESIAN_POINT('Ctrl Pts',(-46.5023302645975,31.3870655242667,
-39.8463165244401));
#256090=CARTESIAN_POINT('Ctrl Pts',(-46.4940227302404,31.289588481428,-39.8253669401756));
#256091=CARTESIAN_POINT('Ctrl Pts',(-46.4735992389084,31.1615543100329,
-39.7959087657426));
#256092=CARTESIAN_POINT('Ctrl Pts',(-46.4439553357389,31.0354316602054,
-39.764933002761));
#256093=CARTESIAN_POINT('Ctrl Pts',(-46.4260423093758,30.9730107791217,
-39.7489341795107));
#256094=CARTESIAN_POINT('Ctrl Pts',(-46.4065681949313,30.9109152099792,
-39.7326766466501));
#256095=CARTESIAN_POINT('Ctrl Pts',(-46.3960461932204,30.8800184397817,
-39.7244153231182));
#256096=CARTESIAN_POINT('Ctrl Pts',(-46.3734280792928,30.8185995307444,
-39.7076399973049));
#256097=CARTESIAN_POINT('Ctrl Pts',(-46.3614254481729,30.7883280602527,
-39.6991946976795));
#256098=CARTESIAN_POINT('Ctrl Pts',(-46.348736272544,30.7584582252104,-39.6906856150703));
#256099=CARTESIAN_POINT('Ctrl Pts',(-46.5057014676852,31.6353142217915,
-39.89605787487));
#256100=CARTESIAN_POINT('Ctrl Pts',(-46.504431262165,31.6620633341882,-39.9010881326463));
#256101=CARTESIAN_POINT('Ctrl Pts',(-46.5026263105811,31.688741807057,-39.9059955470865));
#256102=CARTESIAN_POINT('Ctrl Pts',(-46.4945629272159,31.7805948790823,
-39.9225196439524));
#256103=CARTESIAN_POINT('Ctrl Pts',(-46.4856505749035,31.8454075750247,
-39.9335309462494));
#256104=CARTESIAN_POINT('Ctrl Pts',(-46.4675150440425,31.9419322486556,
-39.9489584247984));
#256105=CARTESIAN_POINT('Ctrl Pts',(-46.4606740873934,31.9739927081568,
-39.9539193312238));
#256106=CARTESIAN_POINT('Ctrl Pts',(-46.445384375334,32.0378823010726,-39.9634753001132));
#256107=CARTESIAN_POINT('Ctrl Pts',(-46.4369357146477,32.0697114482314,
-39.9680703831214));
#256108=CARTESIAN_POINT('Ctrl Pts',(-46.4184025922855,32.1331342652581,
-39.9768893255524));
#256109=CARTESIAN_POINT('Ctrl Pts',(-46.4083237615152,32.1647111636399,
-39.9811109974971));
#256110=CARTESIAN_POINT('Ctrl Pts',(-46.391930976111,32.2119456968313,-39.9871653732414));
#256111=CARTESIAN_POINT('Ctrl Pts',(-46.3862603264385,32.2276473949945,
-39.9891341361105));
#256112=CARTESIAN_POINT('Ctrl Pts',(-46.3745657539713,32.2588055871924,
-39.9929535436847));
#256113=CARTESIAN_POINT('Ctrl Pts',(-46.3685310519543,32.2742961715653,
-39.9948087663756));
#256114=CARTESIAN_POINT('Ctrl Pts',(-46.3374534721736,32.3512007551325,
-40.0037984514834));
#256115=CARTESIAN_POINT('Ctrl Pts',(-46.3096720259105,32.4111748266119,
-40.0101088468852));
#256116=CARTESIAN_POINT('Ctrl Pts',(-46.2483848955207,32.5279978387927,
-40.0209903891417));
#256117=CARTESIAN_POINT('Ctrl Pts',(-46.2148776784186,32.58486109828,-40.025564037709));
#256118=CARTESIAN_POINT('Ctrl Pts',(-46.1602750397486,32.6678057987649,
-40.0311126138524));
#256119=CARTESIAN_POINT('Ctrl Pts',(-46.1413484466877,32.6950629059706,
-40.0327431823962));
#256120=CARTESIAN_POINT('Ctrl Pts',(-46.1020228696767,32.7487767218636,
-40.0355591472418));
#256121=CARTESIAN_POINT('Ctrl Pts',(-46.0816091751359,32.7752517709756,
-40.0367452548009));
#256122=CARTESIAN_POINT('Ctrl Pts',(-46.039326094558,32.8273165460041,-40.0386592399055));
#256123=CARTESIAN_POINT('Ctrl Pts',(-46.0176311249679,32.8526942171489,
-40.0393797564574));
#256124=CARTESIAN_POINT('Ctrl Pts',(-45.9731233122554,32.9022095992068,
-40.0403594582195));
#256125=CARTESIAN_POINT('Ctrl Pts',(-45.9503162012007,32.9263401489037,
-40.0406183635165));
#256126=CARTESIAN_POINT('Ctrl Pts',(-45.8802580990489,32.9968762744355,
-40.0407118830392));
#256127=CARTESIAN_POINT('Ctrl Pts',(-45.8313738629074,33.0414303223986,
-40.039864823183));
#256128=CARTESIAN_POINT('Ctrl Pts',(-45.7547952110795,33.1045744158562,
-40.0372361446768));
#256129=CARTESIAN_POINT('Ctrl Pts',(-45.7287260251324,33.1250069084101,
-40.0361331740873));
#256130=CARTESIAN_POINT('Ctrl Pts',(-45.6754920455146,33.1646298482803,
-40.0334694236076));
#256131=CARTESIAN_POINT('Ctrl Pts',(-45.6483134994178,33.1838283485151,
-40.0319075284759));
#256132=CARTESIAN_POINT('Ctrl Pts',(-45.5928982301755,33.2209311560931,
-40.0283226535581));
#256133=CARTESIAN_POINT('Ctrl Pts',(-45.5645244103116,33.2389144742721,
-40.0262882975575));
#256134=CARTESIAN_POINT('Ctrl Pts',(-45.5072645495699,33.2732206191231,
-40.0217931623121));
#256135=CARTESIAN_POINT('Ctrl Pts',(-45.4783169400346,33.2895926998564,
-40.0193299746856));
#256136=CARTESIAN_POINT('Ctrl Pts',(-45.4373898222728,33.3114186492017,
-40.0155876017777));
#256137=CARTESIAN_POINT('Ctrl Pts',(-45.4256642380104,33.3175230028014,
-40.0144861643931));
#256138=CARTESIAN_POINT('Ctrl Pts',(-45.4138902706673,33.3235051193248,
-40.0133502342376));
#256139=CARTESIAN_POINT('Origin',(-44.5079524583202,31.5404524382932,-52.920575));
#256140=CARTESIAN_POINT('Ctrl Pts',(-42.8392071752677,31.5404524382931,
-52.4912));
#256141=CARTESIAN_POINT('Ctrl Pts',(-42.8392071752677,32.5039029766724,
-52.4328666666667));
#256142=CARTESIAN_POINT('Ctrl Pts',(-43.6735798167939,32.985628245862,-52.3745333333334));
#256143=CARTESIAN_POINT('Ctrl Pts',(-44.5079524583201,33.4673535150516,
-52.3162000000001));
#256144=CARTESIAN_POINT('Ctrl Pts',(-45.3423250998464,32.985628245862,-52.2578666666667));
#256145=CARTESIAN_POINT('Ctrl Pts',(-46.1766977413726,32.5039029766724,
-52.1995333333334));
#256146=CARTESIAN_POINT('Ctrl Pts',(-46.1766977413726,31.5404524382932,
-52.1412));
#256147=CARTESIAN_POINT('Ctrl Pts',(-46.1766977413726,30.5770018999139,
-52.0828666666667));
#256148=CARTESIAN_POINT('Ctrl Pts',(-45.3423250998464,30.0952766307242,
-52.0245333333333));
#256149=CARTESIAN_POINT('Ctrl Pts',(-44.5079524583202,29.6135513615346,
-51.9662));
#256150=CARTESIAN_POINT('Ctrl Pts',(-43.6735798167939,30.0952766307242,
-51.9078666666667));
#256151=CARTESIAN_POINT('Ctrl Pts',(-42.8392071752677,30.5770018999139,
-51.8495333333334));
#256152=CARTESIAN_POINT('Ctrl Pts',(-42.8392071752677,31.5404524382931,
-51.7912));
#256153=CARTESIAN_POINT('Ctrl Pts',(-42.8392071752677,31.5404524382931,
-52.64995));
#256154=CARTESIAN_POINT('Ctrl Pts',(-42.8392071752677,32.5039029766724,
-52.5916166666667));
#256155=CARTESIAN_POINT('Ctrl Pts',(-43.6735798167939,32.985628245862,-52.5332833333334));
#256156=CARTESIAN_POINT('Ctrl Pts',(-44.5079524583201,33.4673535150516,
-52.47495));
#256157=CARTESIAN_POINT('Ctrl Pts',(-45.3423250998464,32.985628245862,-52.4166166666667));
#256158=CARTESIAN_POINT('Ctrl Pts',(-46.1766977413726,32.5039029766724,
-52.3582833333334));
#256159=CARTESIAN_POINT('Ctrl Pts',(-46.1766977413726,31.5404524382932,
-52.29995));
#256160=CARTESIAN_POINT('Ctrl Pts',(-46.1766977413726,30.5770018999139,
-52.2416166666667));
#256161=CARTESIAN_POINT('Ctrl Pts',(-45.3423250998464,30.0952766307242,
-52.1832833333333));
#256162=CARTESIAN_POINT('Ctrl Pts',(-44.5079524583202,29.6135513615346,
-52.12495));
#256163=CARTESIAN_POINT('Ctrl Pts',(-43.6735798167939,30.0952766307242,
-52.0666166666667));
#256164=CARTESIAN_POINT('Ctrl Pts',(-42.8392071752677,30.5770018999139,
-52.0082833333333));
#256165=CARTESIAN_POINT('Ctrl Pts',(-42.8392071752677,31.5404524382931,
-51.94995));
#256166=CARTESIAN_POINT('Ctrl Pts',(-46.5766932247455,31.5404524382932,
-52.6102625));
#256167=CARTESIAN_POINT('Ctrl Pts',(-46.5766932247455,30.3460643999139,
-52.5519291666666));
#256168=CARTESIAN_POINT('Ctrl Pts',(-45.5423228415329,29.7488703807243,
-52.4935958333333));
#256169=CARTESIAN_POINT('Ctrl Pts',(-44.5079524583202,29.1516763615346,
-52.4352625));
#256170=CARTESIAN_POINT('Ctrl Pts',(-43.4735820751074,29.7488703807243,
-52.3769291666667));
#256171=CARTESIAN_POINT('Ctrl Pts',(-42.4392116918948,30.3460643999138,
-52.3185958333334));
#256172=CARTESIAN_POINT('Ctrl Pts',(-42.4392116918948,31.5404524382931,
-52.2602625));
#256173=CARTESIAN_POINT('Ctrl Pts',(-42.4392116918947,32.7348404766723,
-52.2019291666667));
#256174=CARTESIAN_POINT('Ctrl Pts',(-43.4735820751074,33.332034495862,-52.1435958333333));
#256175=CARTESIAN_POINT('Ctrl Pts',(-44.5079524583201,33.9292285150516,
-52.0852625));
#256176=CARTESIAN_POINT('Ctrl Pts',(-45.5423228415328,33.332034495862,-52.0269291666667));
#256177=CARTESIAN_POINT('Ctrl Pts',(-46.5766932247455,32.7348404766724,
-51.9685958333333));
#256178=CARTESIAN_POINT('Ctrl Pts',(-46.5766932247455,31.5404524382932,
-51.9102625));
#256179=CARTESIAN_POINT('Ctrl Pts',(-46.5766932247455,30.3460643999139,
-51.8519291666667));
#256180=CARTESIAN_POINT('Ctrl Pts',(-45.5423228415329,29.7488703807243,
-51.7935958333333));
#256181=CARTESIAN_POINT('Ctrl Pts',(-44.5079524583202,29.1516763615346,
-51.7352625));
#256182=CARTESIAN_POINT('Ctrl Pts',(-43.4735820751074,29.7488703807243,
-51.6769291666667));
#256183=CARTESIAN_POINT('Ctrl Pts',(-42.4392116918948,30.3460643999138,
-51.6185958333333));
#256184=CARTESIAN_POINT('Ctrl Pts',(-42.4392116918948,31.5404524382931,
-51.5602625));
#256185=CARTESIAN_POINT('Ctrl Pts',(-42.4392116918947,32.7348404766723,
-51.5019291666666));
#256186=CARTESIAN_POINT('Ctrl Pts',(-43.4735820751074,33.332034495862,-51.4435958333333));
#256187=CARTESIAN_POINT('Ctrl Pts',(-44.5079524583201,33.9292285150516,
-51.3852625));
#256188=CARTESIAN_POINT('Ctrl Pts',(-45.5423228415328,33.332034495862,-51.3269291666667));
#256189=CARTESIAN_POINT('Ctrl Pts',(-46.5766932247455,32.7348404766724,
-51.2685958333333));
#256190=CARTESIAN_POINT('Ctrl Pts',(-46.5766932247455,31.5404524382932,
-51.2102625));
#256191=CARTESIAN_POINT('Ctrl Pts',(-46.5766932247455,30.3460643999139,
-51.1519291666666));
#256192=CARTESIAN_POINT('Ctrl Pts',(-45.5423228415329,29.7488703807243,
-51.0935958333334));
#256193=CARTESIAN_POINT('Ctrl Pts',(-44.5079524583202,29.1516763615346,
-51.0352625));
#256194=CARTESIAN_POINT('Ctrl Pts',(-43.4735820751074,29.7488703807243,
-50.9769291666667));
#256195=CARTESIAN_POINT('Ctrl Pts',(-42.4392116918948,30.3460643999138,
-50.9185958333333));
#256196=CARTESIAN_POINT('Ctrl Pts',(-42.4392116918948,31.5404524382931,
-50.8602625));
#256197=CARTESIAN_POINT('Ctrl Pts',(-42.4392116918947,32.7348404766723,
-50.8019291666667));
#256198=CARTESIAN_POINT('Ctrl Pts',(-43.4735820751074,33.332034495862,-50.7435958333333));
#256199=CARTESIAN_POINT('Ctrl Pts',(-44.5079524583201,33.9292285150516,
-50.6852625));
#256200=CARTESIAN_POINT('Ctrl Pts',(-45.5423228415328,33.332034495862,-50.6269291666667));
#256201=CARTESIAN_POINT('Ctrl Pts',(-46.5766932247455,32.7348404766724,
-50.5685958333333));
#256202=CARTESIAN_POINT('Ctrl Pts',(-46.5766932247455,31.5404524382932,
-50.5102625));
#256203=CARTESIAN_POINT('Ctrl Pts',(-46.5766932247455,30.3460643999139,
-50.4519291666667));
#256204=CARTESIAN_POINT('Ctrl Pts',(-45.5423228415329,29.7488703807243,
-50.3935958333333));
#256205=CARTESIAN_POINT('Ctrl Pts',(-44.5079524583202,29.1516763615346,
-50.3352625));
#256206=CARTESIAN_POINT('Ctrl Pts',(-43.4735820751074,29.7488703807243,
-50.2769291666667));
#256207=CARTESIAN_POINT('Ctrl Pts',(-42.4392116918948,30.3460643999138,
-50.2185958333333));
#256208=CARTESIAN_POINT('Ctrl Pts',(-42.4392116918948,31.5404524382931,
-50.1602625));
#256209=CARTESIAN_POINT('Ctrl Pts',(-42.4392116918947,32.7348404766723,
-50.1019291666667));
#256210=CARTESIAN_POINT('Ctrl Pts',(-43.4735820751074,33.332034495862,-50.0435958333333));
#256211=CARTESIAN_POINT('Ctrl Pts',(-44.5079524583201,33.9292285150516,
-49.9852625));
#256212=CARTESIAN_POINT('Ctrl Pts',(-45.5423228415328,33.332034495862,-49.9269291666667));
#256213=CARTESIAN_POINT('Ctrl Pts',(-46.5766932247455,32.7348404766724,
-49.8685958333333));
#256214=CARTESIAN_POINT('Ctrl Pts',(-46.5766932247455,31.5404524382932,
-49.8102625));
#256215=CARTESIAN_POINT('Ctrl Pts',(-46.5766932247455,30.3460643999139,
-49.7519291666667));
#256216=CARTESIAN_POINT('Ctrl Pts',(-45.5423228415329,29.7488703807243,
-49.6935958333334));
#256217=CARTESIAN_POINT('Ctrl Pts',(-44.5079524583202,29.1516763615346,
-49.6352625));
#256218=CARTESIAN_POINT('Ctrl Pts',(-43.4735820751074,29.7488703807243,
-49.5769291666667));
#256219=CARTESIAN_POINT('Ctrl Pts',(-42.4392116918948,30.3460643999138,
-49.5185958333334));
#256220=CARTESIAN_POINT('Ctrl Pts',(-42.4392116918948,31.5404524382931,
-49.4602625));
#256221=CARTESIAN_POINT('Ctrl Pts',(-42.4392116918947,32.7348404766723,
-49.4019291666667));
#256222=CARTESIAN_POINT('Ctrl Pts',(-43.4735820751074,33.332034495862,-49.3435958333333));
#256223=CARTESIAN_POINT('Ctrl Pts',(-44.5079524583201,33.9292285150516,
-49.2852625));
#256224=CARTESIAN_POINT('Ctrl Pts',(-45.5423228415328,33.332034495862,-49.2269291666667));
#256225=CARTESIAN_POINT('Ctrl Pts',(-46.5766932247455,32.7348404766724,
-49.1685958333334));
#256226=CARTESIAN_POINT('Ctrl Pts',(-46.5766932247455,31.5404524382932,
-49.1102625));
#256227=CARTESIAN_POINT('Ctrl Pts',(-46.5766932247455,30.3460643999139,
-49.0519291666667));
#256228=CARTESIAN_POINT('Ctrl Pts',(-45.5423228415329,29.7488703807243,
-48.9935958333333));
#256229=CARTESIAN_POINT('Ctrl Pts',(-44.5079524583202,29.1516763615346,
-48.9352625));
#256230=CARTESIAN_POINT('Ctrl Pts',(-43.4735820751074,29.7488703807243,
-48.8769291666667));
#256231=CARTESIAN_POINT('Ctrl Pts',(-42.4392116918948,30.3460643999138,
-48.8185958333333));
#256232=CARTESIAN_POINT('Ctrl Pts',(-42.4392116918948,31.5404524382931,
-48.7602625));
#256233=CARTESIAN_POINT('Ctrl Pts',(-42.4392116918947,32.7348404766723,
-48.7019291666667));
#256234=CARTESIAN_POINT('Ctrl Pts',(-43.4735820751074,33.332034495862,-48.6435958333333));
#256235=CARTESIAN_POINT('Ctrl Pts',(-44.5079524583201,33.9292285150516,
-48.5852625));
#256236=CARTESIAN_POINT('Ctrl Pts',(-45.5423228415328,33.332034495862,-48.5269291666667));
#256237=CARTESIAN_POINT('Ctrl Pts',(-46.5766932247455,32.7348404766724,
-48.4685958333333));
#256238=CARTESIAN_POINT('Ctrl Pts',(-46.5766932247455,31.5404524382932,
-48.4102625));
#256239=CARTESIAN_POINT('Ctrl Pts',(-46.5766932247455,30.3460643999139,
-48.3519291666667));
#256240=CARTESIAN_POINT('Ctrl Pts',(-45.5423228415329,29.7488703807243,
-48.2935958333333));
#256241=CARTESIAN_POINT('Ctrl Pts',(-44.5079524583202,29.1516763615346,
-48.2352625));
#256242=CARTESIAN_POINT('Ctrl Pts',(-43.4735820751074,29.7488703807243,
-48.1769291666667));
#256243=CARTESIAN_POINT('Ctrl Pts',(-42.4392116918948,30.3460643999138,
-48.1185958333334));
#256244=CARTESIAN_POINT('Ctrl Pts',(-42.4392116918948,31.5404524382931,
-48.0602625));
#256245=CARTESIAN_POINT('Ctrl Pts',(-42.4392116918947,32.7348404766723,
-48.0019291666667));
#256246=CARTESIAN_POINT('Ctrl Pts',(-43.4735820751074,33.332034495862,-47.9435958333334));
#256247=CARTESIAN_POINT('Ctrl Pts',(-44.5079524583201,33.9292285150516,
-47.8852625));
#256248=CARTESIAN_POINT('Ctrl Pts',(-45.5423228415328,33.332034495862,-47.8269291666667));
#256249=CARTESIAN_POINT('Ctrl Pts',(-46.5766932247455,32.7348404766724,
-47.7685958333333));
#256250=CARTESIAN_POINT('Ctrl Pts',(-46.5766932247455,31.5404524382932,
-47.7102625));
#256251=CARTESIAN_POINT('Ctrl Pts',(-46.5766932247455,30.3460643999139,
-47.6519291666667));
#256252=CARTESIAN_POINT('Ctrl Pts',(-45.5423228415329,29.7488703807243,
-47.5935958333333));
#256253=CARTESIAN_POINT('Ctrl Pts',(-44.5079524583202,29.1516763615346,
-47.5352625));
#256254=CARTESIAN_POINT('Ctrl Pts',(-43.4735820751074,29.7488703807243,
-47.4769291666667));
#256255=CARTESIAN_POINT('Ctrl Pts',(-42.4392116918948,30.3460643999138,
-47.4185958333333));
#256256=CARTESIAN_POINT('Ctrl Pts',(-42.4392116918948,31.5404524382931,
-47.3602625));
#256257=CARTESIAN_POINT('Ctrl Pts',(-42.4392116918947,32.7348404766723,
-47.3019291666666));
#256258=CARTESIAN_POINT('Ctrl Pts',(-43.4735820751074,33.332034495862,-47.2435958333333));
#256259=CARTESIAN_POINT('Ctrl Pts',(-44.5079524583201,33.9292285150516,
-47.1852625));
#256260=CARTESIAN_POINT('Ctrl Pts',(-45.5423228415328,33.332034495862,-47.1269291666667));
#256261=CARTESIAN_POINT('Ctrl Pts',(-46.5766932247455,32.7348404766724,
-47.0685958333333));
#256262=CARTESIAN_POINT('Ctrl Pts',(-46.5766932247455,31.5404524382932,
-47.0102625));
#256263=CARTESIAN_POINT('Ctrl Pts',(-46.5766932247455,30.3460643999139,
-46.9519291666667));
#256264=CARTESIAN_POINT('Ctrl Pts',(-45.5423228415329,29.7488703807243,
-46.8935958333333));
#256265=CARTESIAN_POINT('Ctrl Pts',(-44.5079524583202,29.1516763615346,
-46.8352625));
#256266=CARTESIAN_POINT('Ctrl Pts',(-43.4735820751074,29.7488703807243,
-46.7769291666667));
#256267=CARTESIAN_POINT('Ctrl Pts',(-42.4392116918948,30.3460643999138,
-46.7185958333333));
#256268=CARTESIAN_POINT('Ctrl Pts',(-42.4392116918948,31.5404524382931,
-46.6602625));
#256269=CARTESIAN_POINT('Ctrl Pts',(-42.4392116918948,32.7348404766723,
-46.6019291666667));
#256270=CARTESIAN_POINT('Ctrl Pts',(-43.4735820751074,33.332034495862,-46.5435958333334));
#256271=CARTESIAN_POINT('Ctrl Pts',(-44.5079524583201,33.9292285150516,
-46.4852625));
#256272=CARTESIAN_POINT('Ctrl Pts',(-45.5423228415328,33.332034495862,-46.4269291666667));
#256273=CARTESIAN_POINT('Ctrl Pts',(-46.5766932247455,32.7348404766724,
-46.3685958333333));
#256274=CARTESIAN_POINT('Ctrl Pts',(-46.5766932247455,31.5404524382932,
-46.3102625));
#256275=CARTESIAN_POINT('Ctrl Pts',(-46.5766932247455,30.3460643999139,
-46.2519291666667));
#256276=CARTESIAN_POINT('Ctrl Pts',(-45.5423228415329,29.7488703807243,
-46.1935958333333));
#256277=CARTESIAN_POINT('Ctrl Pts',(-44.5079524583202,29.1516763615346,
-46.1352625));
#256278=CARTESIAN_POINT('Ctrl Pts',(-43.4735820751074,29.7488703807243,
-46.0769291666667));
#256279=CARTESIAN_POINT('Ctrl Pts',(-42.4392116918948,30.3460643999138,
-46.0185958333334));
#256280=CARTESIAN_POINT('Ctrl Pts',(-42.4392116918948,31.5404524382931,
-45.9602625));
#256281=CARTESIAN_POINT('Ctrl Pts',(-42.4392116918948,32.7348404766723,
-45.9019291666667));
#256282=CARTESIAN_POINT('Ctrl Pts',(-43.4735820751074,33.332034495862,-45.8435958333333));
#256283=CARTESIAN_POINT('Ctrl Pts',(-44.5079524583201,33.9292285150516,
-45.7852625));
#256284=CARTESIAN_POINT('Ctrl Pts',(-45.5423228415328,33.332034495862,-45.7269291666667));
#256285=CARTESIAN_POINT('Ctrl Pts',(-46.5766932247455,32.7348404766724,
-45.6685958333334));
#256286=CARTESIAN_POINT('Ctrl Pts',(-46.5766932247455,31.5404524382932,
-45.6102625));
#256287=CARTESIAN_POINT('Ctrl Pts',(-46.5766932247455,30.3460643999139,
-45.5519291666667));
#256288=CARTESIAN_POINT('Ctrl Pts',(-45.5423228415329,29.7488703807243,
-45.4935958333333));
#256289=CARTESIAN_POINT('Ctrl Pts',(-44.5079524583202,29.1516763615346,
-45.4352625));
#256290=CARTESIAN_POINT('Ctrl Pts',(-43.4735820751074,29.7488703807243,
-45.3769291666667));
#256291=CARTESIAN_POINT('Ctrl Pts',(-42.4392116918948,30.3460643999138,
-45.3185958333333));
#256292=CARTESIAN_POINT('Ctrl Pts',(-42.4392116918948,31.5404524382931,
-45.2602625));
#256293=CARTESIAN_POINT('Ctrl Pts',(-42.4392116918948,32.7348404766723,
-45.2019291666667));
#256294=CARTESIAN_POINT('Ctrl Pts',(-43.4735820751074,33.332034495862,-45.1435958333333));
#256295=CARTESIAN_POINT('Ctrl Pts',(-44.5079524583201,33.9292285150516,
-45.0852625));
#256296=CARTESIAN_POINT('Ctrl Pts',(-45.5423228415328,33.332034495862,-45.0269291666667));
#256297=CARTESIAN_POINT('Ctrl Pts',(-46.5766932247455,32.7348404766724,
-44.9685958333334));
#256298=CARTESIAN_POINT('Ctrl Pts',(-46.5766932247455,31.5404524382932,
-44.9102625));
#256299=CARTESIAN_POINT('Ctrl Pts',(-46.5766932247455,30.3460643999139,
-44.8519291666667));
#256300=CARTESIAN_POINT('Ctrl Pts',(-45.5423228415329,29.7488703807243,
-44.7935958333333));
#256301=CARTESIAN_POINT('Ctrl Pts',(-44.5079524583202,29.1516763615346,
-44.7352625));
#256302=CARTESIAN_POINT('Ctrl Pts',(-43.4735820751074,29.7488703807243,
-44.6769291666667));
#256303=CARTESIAN_POINT('Ctrl Pts',(-42.4392116918948,30.3460643999138,
-44.6185958333334));
#256304=CARTESIAN_POINT('Ctrl Pts',(-42.4392116918948,31.5404524382931,
-44.5602625));
#256305=CARTESIAN_POINT('Ctrl Pts',(-42.4392116918948,32.7348404766723,
-44.5019291666667));
#256306=CARTESIAN_POINT('Ctrl Pts',(-43.4735820751074,33.332034495862,-44.4435958333333));
#256307=CARTESIAN_POINT('Ctrl Pts',(-44.5079524583201,33.9292285150516,
-44.3852625));
#256308=CARTESIAN_POINT('Ctrl Pts',(-45.5423228415328,33.332034495862,-44.3269291666667));
#256309=CARTESIAN_POINT('Ctrl Pts',(-46.5766932247455,32.7348404766724,
-44.2685958333334));
#256310=CARTESIAN_POINT('Ctrl Pts',(-46.5766932247455,31.5404524382932,
-44.2102625));
#256311=CARTESIAN_POINT('Ctrl Pts',(-46.5766932247455,30.3460643999139,
-44.1519291666667));
#256312=CARTESIAN_POINT('Ctrl Pts',(-45.5423228415329,29.7488703807243,
-44.0935958333334));
#256313=CARTESIAN_POINT('Ctrl Pts',(-44.5079524583202,29.1516763615346,
-44.0352625));
#256314=CARTESIAN_POINT('Ctrl Pts',(-43.4735820751074,29.7488703807243,
-43.9769291666667));
#256315=CARTESIAN_POINT('Ctrl Pts',(-42.4392116918948,30.3460643999138,
-43.9185958333333));
#256316=CARTESIAN_POINT('Ctrl Pts',(-42.4392116918948,31.5404524382931,
-43.8602625));
#256317=CARTESIAN_POINT('Ctrl Pts',(-42.4392116918948,32.7348404766723,
-43.8019291666667));
#256318=CARTESIAN_POINT('Ctrl Pts',(-43.4735820751074,33.332034495862,-43.7435958333334));
#256319=CARTESIAN_POINT('Ctrl Pts',(-44.5079524583201,33.9292285150516,
-43.6852625));
#256320=CARTESIAN_POINT('Ctrl Pts',(-45.5423228415328,33.332034495862,-43.6269291666667));
#256321=CARTESIAN_POINT('Ctrl Pts',(-46.5766932247455,32.7348404766724,
-43.5685958333333));
#256322=CARTESIAN_POINT('Ctrl Pts',(-46.5766932247455,31.5404524382932,
-43.5102625));
#256323=CARTESIAN_POINT('Ctrl Pts',(-46.5766932247455,30.3460643999139,
-43.4519291666667));
#256324=CARTESIAN_POINT('Ctrl Pts',(-45.5423228415329,29.7488703807243,
-43.3935958333334));
#256325=CARTESIAN_POINT('Ctrl Pts',(-44.5079524583202,29.1516763615346,
-43.3352625));
#256326=CARTESIAN_POINT('Ctrl Pts',(-43.4735820751074,29.7488703807243,
-43.2769291666667));
#256327=CARTESIAN_POINT('Ctrl Pts',(-42.4392116918948,30.3460643999138,
-43.2185958333333));
#256328=CARTESIAN_POINT('Ctrl Pts',(-42.4392116918948,31.5404524382931,
-43.1602625));
#256329=CARTESIAN_POINT('Ctrl Pts',(-42.4392116918948,32.7348404766723,
-43.1019291666667));
#256330=CARTESIAN_POINT('Ctrl Pts',(-43.4735820751074,33.332034495862,-43.0435958333334));
#256331=CARTESIAN_POINT('Ctrl Pts',(-44.5079524583201,33.9292285150516,
-42.9852625));
#256332=CARTESIAN_POINT('Ctrl Pts',(-45.5423228415328,33.332034495862,-42.9269291666667));
#256333=CARTESIAN_POINT('Ctrl Pts',(-46.5766932247455,32.7348404766724,
-42.8685958333333));
#256334=CARTESIAN_POINT('Ctrl Pts',(-46.5766932247455,31.5404524382932,
-42.8102625));
#256335=CARTESIAN_POINT('Ctrl Pts',(-46.5766932247455,30.3460643999139,
-42.7519291666666));
#256336=CARTESIAN_POINT('Ctrl Pts',(-45.5423228415329,29.7488703807243,
-42.6935958333333));
#256337=CARTESIAN_POINT('Ctrl Pts',(-44.5079524583202,29.1516763615346,
-42.6352625));
#256338=CARTESIAN_POINT('Ctrl Pts',(-43.4735820751074,29.7488703807243,
-42.5769291666667));
#256339=CARTESIAN_POINT('Ctrl Pts',(-42.4392116918948,30.3460643999138,
-42.5185958333333));
#256340=CARTESIAN_POINT('Ctrl Pts',(-42.4392116918948,31.5404524382931,
-42.4602625));
#256341=CARTESIAN_POINT('Ctrl Pts',(-42.4392116918948,32.7348404766723,
-42.4019291666666));
#256342=CARTESIAN_POINT('Ctrl Pts',(-43.4735820751074,33.332034495862,-42.3435958333334));
#256343=CARTESIAN_POINT('Ctrl Pts',(-44.5079524583201,33.9292285150516,
-42.2852625));
#256344=CARTESIAN_POINT('Ctrl Pts',(-45.5423228415328,33.332034495862,-42.2269291666667));
#256345=CARTESIAN_POINT('Ctrl Pts',(-46.5766932247455,32.7348404766724,
-42.1685958333333));
#256346=CARTESIAN_POINT('Ctrl Pts',(-46.5766932247455,31.5404524382932,
-42.1102625));
#256347=CARTESIAN_POINT('Ctrl Pts',(-46.5766932247455,30.3460643999139,
-42.0519291666666));
#256348=CARTESIAN_POINT('Ctrl Pts',(-45.5423228415329,29.7488703807243,
-41.9935958333334));
#256349=CARTESIAN_POINT('Ctrl Pts',(-44.5079524583202,29.1516763615346,
-41.9352625));
#256350=CARTESIAN_POINT('Ctrl Pts',(-43.4735820751074,29.7488703807243,
-41.8769291666667));
#256351=CARTESIAN_POINT('Ctrl Pts',(-42.4392116918948,30.3460643999138,
-41.8185958333333));
#256352=CARTESIAN_POINT('Ctrl Pts',(-42.4392116918948,31.5404524382931,
-41.7602625));
#256353=CARTESIAN_POINT('Ctrl Pts',(-42.4392116918948,32.7348404766723,
-41.7019291666666));
#256354=CARTESIAN_POINT('Ctrl Pts',(-43.4735820751074,33.332034495862,-41.6435958333334));
#256355=CARTESIAN_POINT('Ctrl Pts',(-44.5079524583201,33.9292285150516,
-41.5852625));
#256356=CARTESIAN_POINT('Ctrl Pts',(-45.5423228415328,33.332034495862,-41.5269291666667));
#256357=CARTESIAN_POINT('Ctrl Pts',(-46.5766932247455,32.7348404766724,
-41.4685958333333));
#256358=CARTESIAN_POINT('Ctrl Pts',(-46.5766932247455,31.5404524382932,
-41.4102625));
#256359=CARTESIAN_POINT('Ctrl Pts',(-46.5766932247455,30.3460643999139,
-41.3519291666666));
#256360=CARTESIAN_POINT('Ctrl Pts',(-45.5423228415329,29.7488703807243,
-41.2935958333334));
#256361=CARTESIAN_POINT('Ctrl Pts',(-44.5079524583202,29.1516763615346,
-41.2352625));
#256362=CARTESIAN_POINT('Ctrl Pts',(-43.4735820751074,29.7488703807243,
-41.1769291666667));
#256363=CARTESIAN_POINT('Ctrl Pts',(-42.4392116918948,30.3460643999138,
-41.1185958333333));
#256364=CARTESIAN_POINT('Ctrl Pts',(-42.4392116918948,31.5404524382931,
-41.0602625));
#256365=CARTESIAN_POINT('Ctrl Pts',(-42.4392116918948,32.7348404766723,
-41.0019291666666));
#256366=CARTESIAN_POINT('Ctrl Pts',(-43.4735820751074,33.332034495862,-40.9435958333334));
#256367=CARTESIAN_POINT('Ctrl Pts',(-44.5079524583201,33.9292285150516,
-40.8852625));
#256368=CARTESIAN_POINT('Ctrl Pts',(-45.5423228415328,33.332034495862,-40.8269291666667));
#256369=CARTESIAN_POINT('Ctrl Pts',(-46.5766932247455,32.7348404766724,
-40.7685958333333));
#256370=CARTESIAN_POINT('Ctrl Pts',(-46.5766932247455,31.5404524382932,
-40.7102625));
#256371=CARTESIAN_POINT('Ctrl Pts',(-46.5766932247455,30.3460643999139,
-40.6519291666667));
#256372=CARTESIAN_POINT('Ctrl Pts',(-45.5423228415329,29.7488703807243,
-40.5935958333334));
#256373=CARTESIAN_POINT('Ctrl Pts',(-44.5079524583202,29.1516763615346,
-40.5352625));
#256374=CARTESIAN_POINT('Ctrl Pts',(-43.4735820751074,29.7488703807243,
-40.4769291666667));
#256375=CARTESIAN_POINT('Ctrl Pts',(-42.4392116918948,30.3460643999138,
-40.4185958333333));
#256376=CARTESIAN_POINT('Ctrl Pts',(-42.4392116918948,31.5404524382931,
-40.3602625));
#256377=CARTESIAN_POINT('Ctrl Pts',(-42.4392116918948,32.7348404766723,
-40.3019291666667));
#256378=CARTESIAN_POINT('Ctrl Pts',(-43.4735820751074,33.332034495862,-40.2435958333334));
#256379=CARTESIAN_POINT('Ctrl Pts',(-44.5079524583201,33.9292285150516,
-40.1852625));
#256380=CARTESIAN_POINT('Ctrl Pts',(-45.5423228415328,33.332034495862,-40.1269291666666));
#256381=CARTESIAN_POINT('Ctrl Pts',(-46.5766932247455,32.7348404766724,
-40.0685958333333));
#256382=CARTESIAN_POINT('Ctrl Pts',(-46.5766932247455,31.5404524382932,
-40.0102625));
#256383=CARTESIAN_POINT('Ctrl Pts',(-46.5766932247455,30.3460643999139,
-39.9519291666667));
#256384=CARTESIAN_POINT('Ctrl Pts',(-45.5423228415329,29.7488703807243,
-39.8935958333334));
#256385=CARTESIAN_POINT('Ctrl Pts',(-44.5079524583202,29.1516763615346,
-39.8352625));
#256386=CARTESIAN_POINT('Ctrl Pts',(-43.4735820751074,29.7488703807243,
-39.7769291666666));
#256387=CARTESIAN_POINT('Ctrl Pts',(-42.4392116918948,30.3460643999138,
-39.7185958333334));
#256388=CARTESIAN_POINT('Ctrl Pts',(-42.4392116918948,31.5404524382931,
-39.6602625));
#256389=CARTESIAN_POINT('Ctrl Pts',(-42.4392116918948,32.7348404766723,
-39.6019291666667));
#256390=CARTESIAN_POINT('Ctrl Pts',(-43.4735820751074,33.332034495862,-39.5435958333333));
#256391=CARTESIAN_POINT('Ctrl Pts',(-44.5079524583201,33.9292285150516,
-39.4852625));
#256392=CARTESIAN_POINT('Ctrl Pts',(-45.5423228415328,33.332034495862,-39.4269291666667));
#256393=CARTESIAN_POINT('Ctrl Pts',(-46.5766932247455,32.7348404766724,
-39.3685958333334));
#256394=CARTESIAN_POINT('Ctrl Pts',(-46.5766932247455,31.5404524382932,
-39.3102625));
#256395=CARTESIAN_POINT('Ctrl Pts',(-46.5766932247455,30.3460643999139,
-39.2519291666667));
#256396=CARTESIAN_POINT('Ctrl Pts',(-45.5423228415329,29.7488703807243,
-39.1935958333334));
#256397=CARTESIAN_POINT('Ctrl Pts',(-44.5079524583202,29.1516763615346,
-39.1352625));
#256398=CARTESIAN_POINT('Ctrl Pts',(-43.4735820751074,29.7488703807243,
-39.0769291666667));
#256399=CARTESIAN_POINT('Ctrl Pts',(-42.4392116918948,30.3460643999138,
-39.0185958333333));
#256400=CARTESIAN_POINT('Ctrl Pts',(-42.4392116918948,31.5404524382931,
-38.9602625));
#256401=CARTESIAN_POINT('Ctrl Pts',(-42.4392116918948,32.7348404766723,
-38.9019291666667));
#256402=CARTESIAN_POINT('Ctrl Pts',(-43.4735820751074,33.332034495862,-38.8435958333333));
#256403=CARTESIAN_POINT('Ctrl Pts',(-44.5079524583201,33.9292285150516,
-38.7852625));
#256404=CARTESIAN_POINT('Ctrl Pts',(-45.5423228415328,33.332034495862,-38.7269291666667));
#256405=CARTESIAN_POINT('Ctrl Pts',(-46.5766932247455,32.7348404766724,
-38.6685958333334));
#256406=CARTESIAN_POINT('Ctrl Pts',(-46.5766932247455,31.5404524382932,
-38.6102625));
#256407=CARTESIAN_POINT('Ctrl Pts',(-46.5766932247455,30.3460643999139,
-38.5519291666667));
#256408=CARTESIAN_POINT('Ctrl Pts',(-45.5423228415329,29.7488703807243,
-38.4935958333334));
#256409=CARTESIAN_POINT('Ctrl Pts',(-44.5079524583202,29.1516763615346,
-38.4352625));
#256410=CARTESIAN_POINT('Ctrl Pts',(-43.4735820751074,29.7488703807243,
-38.3769291666666));
#256411=CARTESIAN_POINT('Ctrl Pts',(-42.4392116918948,30.3460643999138,
-38.3185958333333));
#256412=CARTESIAN_POINT('Ctrl Pts',(-42.4392116918948,31.5404524382931,
-38.2602625));
#256413=CARTESIAN_POINT('Ctrl Pts',(-42.4392116918948,32.7348404766723,
-38.2019291666667));
#256414=CARTESIAN_POINT('Ctrl Pts',(-43.4735820751074,33.332034495862,-38.1435958333334));
#256415=CARTESIAN_POINT('Ctrl Pts',(-44.5079524583201,33.9292285150516,
-38.0852625));
#256416=CARTESIAN_POINT('Ctrl Pts',(-45.5423228415328,33.332034495862,-38.0269291666667));
#256417=CARTESIAN_POINT('Ctrl Pts',(-46.5766932247455,32.7348404766724,
-37.9685958333333));
#256418=CARTESIAN_POINT('Ctrl Pts',(-46.5766932247455,31.5404524382932,
-37.9102625));
#256419=CARTESIAN_POINT('Ctrl Pts',(-46.5766932247455,30.3460643999139,
-37.8519291666667));
#256420=CARTESIAN_POINT('Ctrl Pts',(-45.5423228415329,29.7488703807243,
-37.7935958333334));
#256421=CARTESIAN_POINT('Ctrl Pts',(-44.5079524583202,29.1516763615346,
-37.7352625));
#256422=CARTESIAN_POINT('Ctrl Pts',(-43.4735820751074,29.7488703807243,
-37.6769291666667));
#256423=CARTESIAN_POINT('Ctrl Pts',(-42.4392116918948,30.3460643999138,
-37.6185958333333));
#256424=CARTESIAN_POINT('Ctrl Pts',(-42.4392116918948,31.5404524382931,
-37.5602625));
#256425=CARTESIAN_POINT('Ctrl Pts',(-42.4392116918948,32.7348404766723,
-37.5019291666666));
#256426=CARTESIAN_POINT('Ctrl Pts',(-43.4735820751074,33.332034495862,-37.4435958333333));
#256427=CARTESIAN_POINT('Ctrl Pts',(-44.5079524583201,33.9292285150516,
-37.3852625));
#256428=CARTESIAN_POINT('Ctrl Pts',(-45.5423228415328,33.332034495862,-37.3269291666667));
#256429=CARTESIAN_POINT('Ctrl Pts',(-46.5766932247455,32.7348404766724,
-37.2685958333333));
#256430=CARTESIAN_POINT('Ctrl Pts',(-46.5766932247455,31.5404524382932,
-37.2102625));
#256431=CARTESIAN_POINT('Ctrl Pts',(-46.5766932247455,30.3460643999139,
-37.1519291666667));
#256432=CARTESIAN_POINT('Ctrl Pts',(-45.5423228415329,29.7488703807243,
-37.0935958333333));
#256433=CARTESIAN_POINT('Ctrl Pts',(-44.5079524583202,29.1516763615346,
-37.0352625));
#256434=CARTESIAN_POINT('Ctrl Pts',(-43.4735820751074,29.7488703807243,
-36.9769291666667));
#256435=CARTESIAN_POINT('Ctrl Pts',(-42.4392116918948,30.3460643999138,
-36.9185958333333));
#256436=CARTESIAN_POINT('Ctrl Pts',(-42.4392116918948,31.5404524382931,
-36.8602625));
#256437=CARTESIAN_POINT('Ctrl Pts',(-42.4392116918948,32.7348404766723,
-36.8019291666666));
#256438=CARTESIAN_POINT('Ctrl Pts',(-43.4735820751074,33.332034495862,-36.7435958333334));
#256439=CARTESIAN_POINT('Ctrl Pts',(-44.5079524583201,33.9292285150516,
-36.6852625));
#256440=CARTESIAN_POINT('Ctrl Pts',(-45.5423228415328,33.332034495862,-36.6269291666666));
#256441=CARTESIAN_POINT('Ctrl Pts',(-45.6766051604214,33.2545065629043,
-36.6193563132714));
#256442=CARTESIAN_POINT('Ctrl Pts',(-45.7978303778612,33.1578278775004,
-36.611216324118));
#256443=CARTESIAN_POINT('Ctrl Pts',(-46.1766977413726,31.5404524382932,
-52.8412));
#256444=CARTESIAN_POINT('Ctrl Pts',(-46.1766977413726,30.5770018999139,
-52.7828666666667));
#256445=CARTESIAN_POINT('Ctrl Pts',(-45.3423250998464,30.0952766307242,
-52.7245333333334));
#256446=CARTESIAN_POINT('Ctrl Pts',(-44.5079524583202,29.6135513615346,
-52.6662));
#256447=CARTESIAN_POINT('Ctrl Pts',(-43.6735798167939,30.0952766307242,
-52.6078666666667));
#256448=CARTESIAN_POINT('Ctrl Pts',(-42.8392071752677,30.5770018999139,
-52.5495333333333));
#256449=CARTESIAN_POINT('Ctrl Pts',(-42.8392071752677,31.5404524382931,
-52.4912));
#256450=CARTESIAN_POINT('Ctrl Pts',(-42.8392071752677,32.5039029766724,
-52.4328666666667));
#256451=CARTESIAN_POINT('Ctrl Pts',(-43.6735798167939,32.985628245862,-52.3745333333334));
#256452=CARTESIAN_POINT('Ctrl Pts',(-44.5079524583201,33.4673535150516,
-52.3162000000001));
#256453=CARTESIAN_POINT('Ctrl Pts',(-45.3423250998464,32.985628245862,-52.2578666666667));
#256454=CARTESIAN_POINT('Ctrl Pts',(-46.1766977413726,32.5039029766724,
-52.1995333333334));
#256455=CARTESIAN_POINT('Ctrl Pts',(-46.1766977413726,31.5404524382932,
-52.1412));
#256456=CARTESIAN_POINT('Ctrl Pts',(-46.1766977413726,30.5770018999139,
-52.0828666666667));
#256457=CARTESIAN_POINT('Ctrl Pts',(-45.3423250998464,30.0952766307242,
-52.0245333333333));
#256458=CARTESIAN_POINT('Ctrl Pts',(-44.5079524583202,29.6135513615346,
-51.9662));
#256459=CARTESIAN_POINT('Ctrl Pts',(-43.6735798167939,30.0952766307242,
-51.9078666666667));
#256460=CARTESIAN_POINT('Ctrl Pts',(-42.8392071752677,30.5770018999139,
-51.8495333333334));
#256461=CARTESIAN_POINT('Ctrl Pts',(-42.8392071752677,31.5404524382931,
-51.7912));
#256462=CARTESIAN_POINT('Ctrl Pts',(-42.8392071752677,32.5039029766724,
-51.7328666666667));
#256463=CARTESIAN_POINT('Ctrl Pts',(-43.6735798167939,32.985628245862,-51.6745333333333));
#256464=CARTESIAN_POINT('Ctrl Pts',(-44.5079524583201,33.4673535150516,
-51.6162));
#256465=CARTESIAN_POINT('Ctrl Pts',(-45.3423250998464,32.985628245862,-51.5578666666667));
#256466=CARTESIAN_POINT('Ctrl Pts',(-46.1766977413726,32.5039029766724,
-51.4995333333333));
#256467=CARTESIAN_POINT('Ctrl Pts',(-46.1766977413726,31.5404524382932,
-51.4412));
#256468=CARTESIAN_POINT('Ctrl Pts',(-46.1766977413726,30.5770018999139,
-51.3828666666667));
#256469=CARTESIAN_POINT('Ctrl Pts',(-45.3423250998464,30.0952766307242,
-51.3245333333334));
#256470=CARTESIAN_POINT('Ctrl Pts',(-44.5079524583202,29.6135513615346,
-51.2662));
#256471=CARTESIAN_POINT('Ctrl Pts',(-43.6735798167939,30.0952766307242,
-51.2078666666667));
#256472=CARTESIAN_POINT('Ctrl Pts',(-42.8392071752677,30.5770018999139,
-51.1495333333333));
#256473=CARTESIAN_POINT('Ctrl Pts',(-42.8392071752677,31.5404524382931,
-51.0912));
#256474=CARTESIAN_POINT('Ctrl Pts',(-42.8392071752677,32.5039029766724,
-51.0328666666667));
#256475=CARTESIAN_POINT('Ctrl Pts',(-43.6735798167939,32.985628245862,-50.9745333333333));
#256476=CARTESIAN_POINT('Ctrl Pts',(-44.5079524583201,33.4673535150516,
-50.9162));
#256477=CARTESIAN_POINT('Ctrl Pts',(-45.3423250998464,32.985628245862,-50.8578666666667));
#256478=CARTESIAN_POINT('Ctrl Pts',(-46.1766977413726,32.5039029766724,
-50.7995333333333));
#256479=CARTESIAN_POINT('Ctrl Pts',(-46.1766977413726,31.5404524382932,
-50.7412));
#256480=CARTESIAN_POINT('Ctrl Pts',(-46.1766977413726,30.5770018999139,
-50.6828666666667));
#256481=CARTESIAN_POINT('Ctrl Pts',(-45.3423250998464,30.0952766307242,
-50.6245333333333));
#256482=CARTESIAN_POINT('Ctrl Pts',(-44.5079524583202,29.6135513615346,
-50.5662));
#256483=CARTESIAN_POINT('Ctrl Pts',(-43.6735798167939,30.0952766307242,
-50.5078666666667));
#256484=CARTESIAN_POINT('Ctrl Pts',(-42.8392071752677,30.5770018999139,
-50.4495333333333));
#256485=CARTESIAN_POINT('Ctrl Pts',(-42.8392071752677,31.5404524382931,
-50.3912));
#256486=CARTESIAN_POINT('Ctrl Pts',(-42.8392071752677,32.5039029766724,
-50.3328666666666));
#256487=CARTESIAN_POINT('Ctrl Pts',(-43.6735798167939,32.985628245862,-50.2745333333333));
#256488=CARTESIAN_POINT('Ctrl Pts',(-44.5079524583201,33.4673535150516,
-50.2162));
#256489=CARTESIAN_POINT('Ctrl Pts',(-45.3423250998464,32.985628245862,-50.1578666666667));
#256490=CARTESIAN_POINT('Ctrl Pts',(-46.1766977413726,32.5039029766724,
-50.0995333333333));
#256491=CARTESIAN_POINT('Ctrl Pts',(-46.1766977413726,31.5404524382932,
-50.0412));
#256492=CARTESIAN_POINT('Ctrl Pts',(-46.1766977413726,30.5770018999139,
-49.9828666666667));
#256493=CARTESIAN_POINT('Ctrl Pts',(-45.3423250998464,30.0952766307242,
-49.9245333333334));
#256494=CARTESIAN_POINT('Ctrl Pts',(-44.5079524583202,29.6135513615346,
-49.8662));
#256495=CARTESIAN_POINT('Ctrl Pts',(-43.6735798167939,30.0952766307242,
-49.8078666666667));
#256496=CARTESIAN_POINT('Ctrl Pts',(-42.8392071752677,30.5770018999139,
-49.7495333333333));
#256497=CARTESIAN_POINT('Ctrl Pts',(-42.8392071752677,31.5404524382931,
-49.6912));
#256498=CARTESIAN_POINT('Ctrl Pts',(-42.8392071752677,32.5039029766724,
-49.6328666666667));
#256499=CARTESIAN_POINT('Ctrl Pts',(-43.6735798167939,32.985628245862,-49.5745333333333));
#256500=CARTESIAN_POINT('Ctrl Pts',(-44.5079524583201,33.4673535150516,
-49.5162));
#256501=CARTESIAN_POINT('Ctrl Pts',(-45.3423250998464,32.985628245862,-49.4578666666667));
#256502=CARTESIAN_POINT('Ctrl Pts',(-46.1766977413726,32.5039029766724,
-49.3995333333333));
#256503=CARTESIAN_POINT('Ctrl Pts',(-46.1766977413726,31.5404524382932,
-49.3412));
#256504=CARTESIAN_POINT('Ctrl Pts',(-46.1766977413726,30.5770018999139,
-49.2828666666666));
#256505=CARTESIAN_POINT('Ctrl Pts',(-45.3423250998464,30.0952766307242,
-49.2245333333333));
#256506=CARTESIAN_POINT('Ctrl Pts',(-44.5079524583202,29.6135513615346,
-49.1662));
#256507=CARTESIAN_POINT('Ctrl Pts',(-43.6735798167939,30.0952766307242,
-49.1078666666667));
#256508=CARTESIAN_POINT('Ctrl Pts',(-42.8392071752677,30.5770018999139,
-49.0495333333334));
#256509=CARTESIAN_POINT('Ctrl Pts',(-42.8392071752677,31.5404524382931,
-48.9912));
#256510=CARTESIAN_POINT('Ctrl Pts',(-42.8392071752677,32.5039029766724,
-48.9328666666667));
#256511=CARTESIAN_POINT('Ctrl Pts',(-43.6735798167939,32.985628245862,-48.8745333333333));
#256512=CARTESIAN_POINT('Ctrl Pts',(-44.5079524583201,33.4673535150516,
-48.8162));
#256513=CARTESIAN_POINT('Ctrl Pts',(-45.3423250998464,32.985628245862,-48.7578666666667));
#256514=CARTESIAN_POINT('Ctrl Pts',(-46.1766977413726,32.5039029766724,
-48.6995333333334));
#256515=CARTESIAN_POINT('Ctrl Pts',(-46.1766977413726,31.5404524382932,
-48.6412));
#256516=CARTESIAN_POINT('Ctrl Pts',(-46.1766977413726,30.5770018999139,
-48.5828666666667));
#256517=CARTESIAN_POINT('Ctrl Pts',(-45.3423250998464,30.0952766307242,
-48.5245333333333));
#256518=CARTESIAN_POINT('Ctrl Pts',(-44.5079524583202,29.6135513615346,
-48.4662));
#256519=CARTESIAN_POINT('Ctrl Pts',(-43.6735798167939,30.0952766307242,
-48.4078666666667));
#256520=CARTESIAN_POINT('Ctrl Pts',(-42.8392071752677,30.5770018999139,
-48.3495333333333));
#256521=CARTESIAN_POINT('Ctrl Pts',(-42.8392071752677,31.5404524382931,
-48.2912));
#256522=CARTESIAN_POINT('Ctrl Pts',(-42.8392071752677,32.5039029766724,
-48.2328666666667));
#256523=CARTESIAN_POINT('Ctrl Pts',(-43.6735798167939,32.985628245862,-48.1745333333334));
#256524=CARTESIAN_POINT('Ctrl Pts',(-44.5079524583201,33.4673535150516,
-48.1162));
#256525=CARTESIAN_POINT('Ctrl Pts',(-45.3423250998464,32.985628245862,-48.0578666666667));
#256526=CARTESIAN_POINT('Ctrl Pts',(-46.1766977413726,32.5039029766724,
-47.9995333333334));
#256527=CARTESIAN_POINT('Ctrl Pts',(-46.1766977413726,31.5404524382932,
-47.9412));
#256528=CARTESIAN_POINT('Ctrl Pts',(-46.1766977413726,30.5770018999139,
-47.8828666666667));
#256529=CARTESIAN_POINT('Ctrl Pts',(-45.3423250998464,30.0952766307242,
-47.8245333333333));
#256530=CARTESIAN_POINT('Ctrl Pts',(-44.5079524583202,29.6135513615346,
-47.7662));
#256531=CARTESIAN_POINT('Ctrl Pts',(-43.6735798167939,30.0952766307242,
-47.7078666666667));
#256532=CARTESIAN_POINT('Ctrl Pts',(-42.8392071752677,30.5770018999139,
-47.6495333333334));
#256533=CARTESIAN_POINT('Ctrl Pts',(-42.8392071752677,31.5404524382931,
-47.5912));
#256534=CARTESIAN_POINT('Ctrl Pts',(-42.8392071752677,32.5039029766724,
-47.5328666666667));
#256535=CARTESIAN_POINT('Ctrl Pts',(-43.6735798167939,32.985628245862,-47.4745333333334));
#256536=CARTESIAN_POINT('Ctrl Pts',(-44.5079524583201,33.4673535150516,
-47.4162));
#256537=CARTESIAN_POINT('Ctrl Pts',(-45.3423250998464,32.985628245862,-47.3578666666667));
#256538=CARTESIAN_POINT('Ctrl Pts',(-46.1766977413726,32.5039029766724,
-47.2995333333334));
#256539=CARTESIAN_POINT('Ctrl Pts',(-46.1766977413726,31.5404524382932,
-47.2412));
#256540=CARTESIAN_POINT('Ctrl Pts',(-46.1766977413726,30.5770018999139,
-47.1828666666667));
#256541=CARTESIAN_POINT('Ctrl Pts',(-45.3423250998464,30.0952766307242,
-47.1245333333333));
#256542=CARTESIAN_POINT('Ctrl Pts',(-44.5079524583202,29.6135513615346,
-47.0662));
#256543=CARTESIAN_POINT('Ctrl Pts',(-43.6735798167939,30.0952766307242,
-47.0078666666667));
#256544=CARTESIAN_POINT('Ctrl Pts',(-42.8392071752677,30.5770018999139,
-46.9495333333334));
#256545=CARTESIAN_POINT('Ctrl Pts',(-42.8392071752677,31.5404524382931,
-46.8912));
#256546=CARTESIAN_POINT('Ctrl Pts',(-42.8392071752677,32.5039029766724,
-46.8328666666667));
#256547=CARTESIAN_POINT('Ctrl Pts',(-43.6735798167939,32.985628245862,-46.7745333333333));
#256548=CARTESIAN_POINT('Ctrl Pts',(-44.5079524583201,33.4673535150516,
-46.7162));
#256549=CARTESIAN_POINT('Ctrl Pts',(-45.3423250998464,32.985628245862,-46.6578666666667));
#256550=CARTESIAN_POINT('Ctrl Pts',(-46.1766977413726,32.5039029766724,
-46.5995333333333));
#256551=CARTESIAN_POINT('Ctrl Pts',(-46.1766977413726,31.5404524382932,
-46.5412));
#256552=CARTESIAN_POINT('Ctrl Pts',(-46.1766977413726,30.5770018999139,
-46.4828666666667));
#256553=CARTESIAN_POINT('Ctrl Pts',(-45.3423250998464,30.0952766307242,
-46.4245333333333));
#256554=CARTESIAN_POINT('Ctrl Pts',(-44.5079524583202,29.6135513615346,
-46.3662));
#256555=CARTESIAN_POINT('Ctrl Pts',(-43.6735798167939,30.0952766307242,
-46.3078666666667));
#256556=CARTESIAN_POINT('Ctrl Pts',(-42.8392071752677,30.5770018999139,
-46.2495333333334));
#256557=CARTESIAN_POINT('Ctrl Pts',(-42.8392071752677,31.5404524382931,
-46.1912));
#256558=CARTESIAN_POINT('Ctrl Pts',(-42.8392071752677,32.5039029766724,
-46.1328666666667));
#256559=CARTESIAN_POINT('Ctrl Pts',(-43.6735798167939,32.985628245862,-46.0745333333334));
#256560=CARTESIAN_POINT('Ctrl Pts',(-44.5079524583201,33.4673535150516,
-46.0162));
#256561=CARTESIAN_POINT('Ctrl Pts',(-45.3423250998464,32.985628245862,-45.9578666666667));
#256562=CARTESIAN_POINT('Ctrl Pts',(-46.1766977413726,32.5039029766724,
-45.8995333333333));
#256563=CARTESIAN_POINT('Ctrl Pts',(-46.1766977413726,31.5404524382932,
-45.8412));
#256564=CARTESIAN_POINT('Ctrl Pts',(-46.1766977413726,30.5770018999139,
-45.7828666666667));
#256565=CARTESIAN_POINT('Ctrl Pts',(-45.3423250998464,30.0952766307242,
-45.7245333333333));
#256566=CARTESIAN_POINT('Ctrl Pts',(-44.5079524583202,29.6135513615346,
-45.6662));
#256567=CARTESIAN_POINT('Ctrl Pts',(-43.6735798167939,30.0952766307242,
-45.6078666666667));
#256568=CARTESIAN_POINT('Ctrl Pts',(-42.8392071752677,30.5770018999139,
-45.5495333333333));
#256569=CARTESIAN_POINT('Ctrl Pts',(-42.8392071752677,31.5404524382931,
-45.4912));
#256570=CARTESIAN_POINT('Ctrl Pts',(-42.8392071752677,32.5039029766724,
-45.4328666666666));
#256571=CARTESIAN_POINT('Ctrl Pts',(-43.6735798167939,32.985628245862,-45.3745333333333));
#256572=CARTESIAN_POINT('Ctrl Pts',(-44.5079524583201,33.4673535150516,
-45.3162));
#256573=CARTESIAN_POINT('Ctrl Pts',(-45.3423250998464,32.985628245862,-45.2578666666667));
#256574=CARTESIAN_POINT('Ctrl Pts',(-46.1766977413726,32.5039029766724,
-45.1995333333333));
#256575=CARTESIAN_POINT('Ctrl Pts',(-46.1766977413726,31.5404524382932,
-45.1412));
#256576=CARTESIAN_POINT('Ctrl Pts',(-46.1766977413726,30.5770018999139,
-45.0828666666667));
#256577=CARTESIAN_POINT('Ctrl Pts',(-45.3423250998464,30.0952766307242,
-45.0245333333333));
#256578=CARTESIAN_POINT('Ctrl Pts',(-44.5079524583202,29.6135513615346,
-44.9662));
#256579=CARTESIAN_POINT('Ctrl Pts',(-43.6735798167939,30.0952766307242,
-44.9078666666666));
#256580=CARTESIAN_POINT('Ctrl Pts',(-42.8392071752677,30.5770018999139,
-44.8495333333333));
#256581=CARTESIAN_POINT('Ctrl Pts',(-42.8392071752677,31.5404524382931,
-44.7912));
#256582=CARTESIAN_POINT('Ctrl Pts',(-42.8392071752677,32.5039029766724,
-44.7328666666666));
#256583=CARTESIAN_POINT('Ctrl Pts',(-43.6735798167939,32.985628245862,-44.6745333333334));
#256584=CARTESIAN_POINT('Ctrl Pts',(-44.5079524583201,33.4673535150516,
-44.6162));
#256585=CARTESIAN_POINT('Ctrl Pts',(-45.3423250998464,32.985628245862,-44.5578666666667));
#256586=CARTESIAN_POINT('Ctrl Pts',(-46.1766977413726,32.5039029766724,
-44.4995333333333));
#256587=CARTESIAN_POINT('Ctrl Pts',(-46.1766977413726,31.5404524382932,
-44.4412));
#256588=CARTESIAN_POINT('Ctrl Pts',(-46.1766977413726,30.5770018999139,
-44.3828666666667));
#256589=CARTESIAN_POINT('Ctrl Pts',(-45.3423250998464,30.0952766307242,
-44.3245333333334));
#256590=CARTESIAN_POINT('Ctrl Pts',(-44.5079524583202,29.6135513615346,
-44.2662));
#256591=CARTESIAN_POINT('Ctrl Pts',(-43.6735798167939,30.0952766307242,
-44.2078666666667));
#256592=CARTESIAN_POINT('Ctrl Pts',(-42.8392071752677,30.5770018999139,
-44.1495333333334));
#256593=CARTESIAN_POINT('Ctrl Pts',(-42.8392071752677,31.5404524382931,
-44.0912));
#256594=CARTESIAN_POINT('Ctrl Pts',(-42.8392071752677,32.5039029766724,
-44.0328666666667));
#256595=CARTESIAN_POINT('Ctrl Pts',(-43.6735798167939,32.985628245862,-43.9745333333333));
#256596=CARTESIAN_POINT('Ctrl Pts',(-44.5079524583201,33.4673535150516,
-43.9162));
#256597=CARTESIAN_POINT('Ctrl Pts',(-45.3423250998464,32.985628245862,-43.8578666666667));
#256598=CARTESIAN_POINT('Ctrl Pts',(-46.1766977413726,32.5039029766724,
-43.7995333333334));
#256599=CARTESIAN_POINT('Ctrl Pts',(-46.1766977413726,31.5404524382932,
-43.7412));
#256600=CARTESIAN_POINT('Ctrl Pts',(-46.1766977413726,30.5770018999139,
-43.6828666666667));
#256601=CARTESIAN_POINT('Ctrl Pts',(-45.3423250998464,30.0952766307242,
-43.6245333333333));
#256602=CARTESIAN_POINT('Ctrl Pts',(-44.5079524583202,29.6135513615346,
-43.5662));
#256603=CARTESIAN_POINT('Ctrl Pts',(-43.6735798167939,30.0952766307242,
-43.5078666666667));
#256604=CARTESIAN_POINT('Ctrl Pts',(-42.8392071752677,30.5770018999139,
-43.4495333333334));
#256605=CARTESIAN_POINT('Ctrl Pts',(-42.8392071752677,31.5404524382931,
-43.3912));
#256606=CARTESIAN_POINT('Ctrl Pts',(-42.8392071752677,32.5039029766724,
-43.3328666666667));
#256607=CARTESIAN_POINT('Ctrl Pts',(-43.6735798167939,32.985628245862,-43.2745333333334));
#256608=CARTESIAN_POINT('Ctrl Pts',(-44.5079524583201,33.4673535150516,
-43.2162));
#256609=CARTESIAN_POINT('Ctrl Pts',(-45.3423250998464,32.985628245862,-43.1578666666667));
#256610=CARTESIAN_POINT('Ctrl Pts',(-46.1766977413726,32.5039029766724,
-43.0995333333334));
#256611=CARTESIAN_POINT('Ctrl Pts',(-46.1766977413726,31.5404524382932,
-43.0412));
#256612=CARTESIAN_POINT('Ctrl Pts',(-46.1766977413726,30.5770018999139,
-42.9828666666667));
#256613=CARTESIAN_POINT('Ctrl Pts',(-45.3423250998464,30.0952766307242,
-42.9245333333334));
#256614=CARTESIAN_POINT('Ctrl Pts',(-44.5079524583202,29.6135513615346,
-42.8662));
#256615=CARTESIAN_POINT('Ctrl Pts',(-43.6735798167939,30.0952766307242,
-42.8078666666667));
#256616=CARTESIAN_POINT('Ctrl Pts',(-42.8392071752677,30.5770018999139,
-42.7495333333334));
#256617=CARTESIAN_POINT('Ctrl Pts',(-42.8392071752677,31.5404524382931,
-42.6912));
#256618=CARTESIAN_POINT('Ctrl Pts',(-42.8392071752677,32.5039029766724,
-42.6328666666667));
#256619=CARTESIAN_POINT('Ctrl Pts',(-43.6735798167939,32.985628245862,-42.5745333333333));
#256620=CARTESIAN_POINT('Ctrl Pts',(-44.5079524583201,33.4673535150516,
-42.5162));
#256621=CARTESIAN_POINT('Ctrl Pts',(-45.3423250998464,32.985628245862,-42.4578666666667));
#256622=CARTESIAN_POINT('Ctrl Pts',(-46.1766977413726,32.5039029766724,
-42.3995333333334));
#256623=CARTESIAN_POINT('Ctrl Pts',(-46.1766977413726,31.5404524382932,
-42.3412));
#256624=CARTESIAN_POINT('Ctrl Pts',(-46.1766977413726,30.5770018999139,
-42.2828666666667));
#256625=CARTESIAN_POINT('Ctrl Pts',(-45.3423250998464,30.0952766307242,
-42.2245333333333));
#256626=CARTESIAN_POINT('Ctrl Pts',(-44.5079524583202,29.6135513615346,
-42.1662));
#256627=CARTESIAN_POINT('Ctrl Pts',(-43.6735798167939,30.0952766307242,
-42.1078666666667));
#256628=CARTESIAN_POINT('Ctrl Pts',(-42.8392071752677,30.5770018999139,
-42.0495333333334));
#256629=CARTESIAN_POINT('Ctrl Pts',(-42.8392071752677,31.5404524382931,
-41.9912));
#256630=CARTESIAN_POINT('Ctrl Pts',(-42.8392071752677,32.5039029766724,
-41.9328666666667));
#256631=CARTESIAN_POINT('Ctrl Pts',(-43.6735798167939,32.985628245862,-41.8745333333334));
#256632=CARTESIAN_POINT('Ctrl Pts',(-44.5079524583201,33.4673535150516,
-41.8162));
#256633=CARTESIAN_POINT('Ctrl Pts',(-45.3423250998464,32.985628245862,-41.7578666666667));
#256634=CARTESIAN_POINT('Ctrl Pts',(-46.1766977413726,32.5039029766724,
-41.6995333333333));
#256635=CARTESIAN_POINT('Ctrl Pts',(-46.1766977413726,31.5404524382932,
-41.6412));
#256636=CARTESIAN_POINT('Ctrl Pts',(-46.1766977413726,30.5770018999139,
-41.5828666666667));
#256637=CARTESIAN_POINT('Ctrl Pts',(-45.3423250998464,30.0952766307242,
-41.5245333333334));
#256638=CARTESIAN_POINT('Ctrl Pts',(-44.5079524583202,29.6135513615346,
-41.4662));
#256639=CARTESIAN_POINT('Ctrl Pts',(-43.6735798167939,30.0952766307242,
-41.4078666666667));
#256640=CARTESIAN_POINT('Ctrl Pts',(-42.8392071752677,30.5770018999139,
-41.3495333333333));
#256641=CARTESIAN_POINT('Ctrl Pts',(-42.8392071752677,31.5404524382931,
-41.2912));
#256642=CARTESIAN_POINT('Ctrl Pts',(-42.8392071752677,32.5039029766724,
-41.2328666666667));
#256643=CARTESIAN_POINT('Ctrl Pts',(-43.6735798167939,32.985628245862,-41.1745333333334));
#256644=CARTESIAN_POINT('Ctrl Pts',(-44.5079524583201,33.4673535150516,
-41.1162));
#256645=CARTESIAN_POINT('Ctrl Pts',(-45.3423250998464,32.985628245862,-41.0578666666667));
#256646=CARTESIAN_POINT('Ctrl Pts',(-46.1766977413726,32.5039029766724,
-40.9995333333333));
#256647=CARTESIAN_POINT('Ctrl Pts',(-46.1766977413726,31.5404524382932,
-40.9412));
#256648=CARTESIAN_POINT('Ctrl Pts',(-46.1766977413726,30.5770018999139,
-40.8828666666667));
#256649=CARTESIAN_POINT('Ctrl Pts',(-45.3423250998464,30.0952766307242,
-40.8245333333333));
#256650=CARTESIAN_POINT('Ctrl Pts',(-44.5079524583202,29.6135513615346,
-40.7662));
#256651=CARTESIAN_POINT('Ctrl Pts',(-43.6735798167939,30.0952766307242,
-40.7078666666667));
#256652=CARTESIAN_POINT('Ctrl Pts',(-42.8392071752677,30.5770018999139,
-40.6495333333333));
#256653=CARTESIAN_POINT('Ctrl Pts',(-42.8392071752677,31.5404524382931,
-40.5912));
#256654=CARTESIAN_POINT('Ctrl Pts',(-42.8392071752677,32.5039029766724,
-40.5328666666667));
#256655=CARTESIAN_POINT('Ctrl Pts',(-43.6735798167939,32.985628245862,-40.4745333333334));
#256656=CARTESIAN_POINT('Ctrl Pts',(-44.5079524583201,33.4673535150516,
-40.4162));
#256657=CARTESIAN_POINT('Ctrl Pts',(-45.3423250998464,32.985628245862,-40.3578666666667));
#256658=CARTESIAN_POINT('Ctrl Pts',(-46.1766977413726,32.5039029766724,
-40.2995333333333));
#256659=CARTESIAN_POINT('Ctrl Pts',(-46.1766977413726,31.5404524382932,
-40.2412));
#256660=CARTESIAN_POINT('Ctrl Pts',(-46.1766977413726,30.5770018999139,
-40.1828666666667));
#256661=CARTESIAN_POINT('Ctrl Pts',(-45.3423250998464,30.0952766307242,
-40.1245333333334));
#256662=CARTESIAN_POINT('Ctrl Pts',(-44.5079524583202,29.6135513615346,
-40.0662));
#256663=CARTESIAN_POINT('Ctrl Pts',(-43.6735798167939,30.0952766307242,
-40.0078666666667));
#256664=CARTESIAN_POINT('Ctrl Pts',(-42.8392071752677,30.5770018999139,
-39.9495333333333));
#256665=CARTESIAN_POINT('Ctrl Pts',(-42.8392071752677,31.5404524382931,
-39.8912));
#256666=CARTESIAN_POINT('Ctrl Pts',(-42.8392071752677,32.5039029766724,
-39.8328666666666));
#256667=CARTESIAN_POINT('Ctrl Pts',(-43.6735798167939,32.985628245862,-39.7745333333334));
#256668=CARTESIAN_POINT('Ctrl Pts',(-44.5079524583201,33.4673535150516,
-39.7162));
#256669=CARTESIAN_POINT('Ctrl Pts',(-45.3423250998464,32.985628245862,-39.6578666666667));
#256670=CARTESIAN_POINT('Ctrl Pts',(-46.1766977413726,32.5039029766724,
-39.5995333333333));
#256671=CARTESIAN_POINT('Ctrl Pts',(-46.1766977413726,31.5404524382932,
-39.5412));
#256672=CARTESIAN_POINT('Ctrl Pts',(-46.1766977413726,30.5770018999139,
-39.4828666666666));
#256673=CARTESIAN_POINT('Ctrl Pts',(-45.3423250998464,30.0952766307242,
-39.4245333333334));
#256674=CARTESIAN_POINT('Ctrl Pts',(-44.5079524583202,29.6135513615346,
-39.3662));
#256675=CARTESIAN_POINT('Ctrl Pts',(-43.6735798167939,30.0952766307242,
-39.3078666666666));
#256676=CARTESIAN_POINT('Ctrl Pts',(-42.8392071752677,30.5770018999139,
-39.2495333333333));
#256677=CARTESIAN_POINT('Ctrl Pts',(-42.8392071752677,31.5404524382931,
-39.1912));
#256678=CARTESIAN_POINT('Ctrl Pts',(-42.8392071752677,32.5039029766724,
-39.1328666666667));
#256679=CARTESIAN_POINT('Ctrl Pts',(-43.6735798167939,32.985628245862,-39.0745333333333));
#256680=CARTESIAN_POINT('Ctrl Pts',(-44.5079524583201,33.4673535150516,
-39.0162));
#256681=CARTESIAN_POINT('Ctrl Pts',(-45.3423250998464,32.985628245862,-38.9578666666667));
#256682=CARTESIAN_POINT('Ctrl Pts',(-46.1766977413726,32.5039029766724,
-38.8995333333334));
#256683=CARTESIAN_POINT('Ctrl Pts',(-46.1766977413726,31.5404524382932,
-38.8412));
#256684=CARTESIAN_POINT('Ctrl Pts',(-46.1766977413726,30.5770018999139,
-38.7828666666667));
#256685=CARTESIAN_POINT('Ctrl Pts',(-45.3423250998464,30.0952766307242,
-38.7245333333334));
#256686=CARTESIAN_POINT('Ctrl Pts',(-44.5079524583202,29.6135513615346,
-38.6662));
#256687=CARTESIAN_POINT('Ctrl Pts',(-43.6735798167939,30.0952766307242,
-38.6078666666667));
#256688=CARTESIAN_POINT('Ctrl Pts',(-42.8392071752677,30.5770018999139,
-38.5495333333334));
#256689=CARTESIAN_POINT('Ctrl Pts',(-42.8392071752677,31.5404524382931,
-38.4912));
#256690=CARTESIAN_POINT('Ctrl Pts',(-42.8392071752677,32.5039029766724,
-38.4328666666667));
#256691=CARTESIAN_POINT('Ctrl Pts',(-43.6735798167939,32.985628245862,-38.3745333333333));
#256692=CARTESIAN_POINT('Ctrl Pts',(-44.5079524583201,33.4673535150516,
-38.3162));
#256693=CARTESIAN_POINT('Ctrl Pts',(-45.3423250998464,32.985628245862,-38.2578666666667));
#256694=CARTESIAN_POINT('Ctrl Pts',(-46.1766977413726,32.5039029766724,
-38.1995333333333));
#256695=CARTESIAN_POINT('Ctrl Pts',(-46.1766977413726,31.5404524382932,
-38.1412));
#256696=CARTESIAN_POINT('Ctrl Pts',(-46.1766977413726,30.5770018999139,
-38.0828666666667));
#256697=CARTESIAN_POINT('Ctrl Pts',(-45.3423250998464,30.0952766307242,
-38.0245333333334));
#256698=CARTESIAN_POINT('Ctrl Pts',(-44.5079524583202,29.6135513615346,
-37.9662));
#256699=CARTESIAN_POINT('Ctrl Pts',(-43.6735798167939,30.0952766307242,
-37.9078666666667));
#256700=CARTESIAN_POINT('Ctrl Pts',(-42.8392071752677,30.5770018999139,
-37.8495333333334));
#256701=CARTESIAN_POINT('Ctrl Pts',(-42.8392071752677,31.5404524382931,
-37.7912));
#256702=CARTESIAN_POINT('Ctrl Pts',(-42.8392071752677,32.5039029766724,
-37.7328666666667));
#256703=CARTESIAN_POINT('Ctrl Pts',(-43.6735798167939,32.985628245862,-37.6745333333334));
#256704=CARTESIAN_POINT('Ctrl Pts',(-44.5079524583201,33.4673535150516,
-37.6162));
#256705=CARTESIAN_POINT('Ctrl Pts',(-45.3423250998464,32.985628245862,-37.5578666666667));
#256706=CARTESIAN_POINT('Ctrl Pts',(-46.1766977413726,32.5039029766724,
-37.4995333333334));
#256707=CARTESIAN_POINT('Ctrl Pts',(-46.1766977413726,31.5404524382932,
-37.4412));
#256708=CARTESIAN_POINT('Ctrl Pts',(-46.1766977413726,30.5770018999139,
-37.3828666666667));
#256709=CARTESIAN_POINT('Ctrl Pts',(-45.3423250998464,30.0952766307242,
-37.3245333333333));
#256710=CARTESIAN_POINT('Ctrl Pts',(-44.5079524583202,29.6135513615346,
-37.2662));
#256711=CARTESIAN_POINT('Ctrl Pts',(-43.6735798167939,30.0952766307242,
-37.2078666666667));
#256712=CARTESIAN_POINT('Ctrl Pts',(-42.8392071752677,30.5770018999139,
-37.1495333333334));
#256713=CARTESIAN_POINT('Ctrl Pts',(-42.8392071752677,31.5404524382931,
-37.0912));
#256714=CARTESIAN_POINT('Ctrl Pts',(-42.8392071752677,32.5039029766724,
-37.0328666666667));
#256715=CARTESIAN_POINT('Ctrl Pts',(-43.6735798167939,32.985628245862,-36.9745333333333));
#256716=CARTESIAN_POINT('Ctrl Pts',(-44.5079524583201,33.4673535150516,
-36.9162));
#256717=CARTESIAN_POINT('Ctrl Pts',(-45.3423250998464,32.985628245862,-36.8578666666667));
#256718=CARTESIAN_POINT('Ctrl Pts',(-45.4506436431261,32.9230905057412,
-36.8502938132714));
#256719=CARTESIAN_POINT('Ctrl Pts',(-45.548429703648,32.8451048524115,-36.8421538241181));
#256720=CARTESIAN_POINT('Ctrl Pts',(-45.1065105640991,29.6321241563178,
-39.2098675790904));
#256721=CARTESIAN_POINT('Ctrl Pts',(-44.8761803077342,29.6051666105646,
-39.2221339827541));
#256722=CARTESIAN_POINT('Ctrl Pts',(-44.6436379954239,29.607165620836,-39.2270640528163));
#256723=CARTESIAN_POINT('Ctrl Pts',(-44.2077922427375,29.6727869442853,
-39.22565455626));
#256724=CARTESIAN_POINT('Ctrl Pts',(-44.0062031944438,29.7300950035031,
-39.220445337313));
#256725=CARTESIAN_POINT('Ctrl Pts',(-43.7098713630896,29.86081135322,-39.2079104317569));
#256726=CARTESIAN_POINT('Ctrl Pts',(-43.60926248355,29.9148659151021,-39.2029328369672));
#256727=CARTESIAN_POINT('Ctrl Pts',(-43.4947753987298,29.9878345433764,
-39.1954110293585));
#256728=CARTESIAN_POINT('Ctrl Pts',(-43.4770495704002,29.9994758178606,
-39.1941827039815));
#256729=CARTESIAN_POINT('Ctrl Pts',(-43.4573679760584,30.0127891661798,
-39.1927474179514));
#256730=CARTESIAN_POINT('Ctrl Pts',(-43.455236241125,30.0142363143022,-39.1925910112225));
#256731=CARTESIAN_POINT('Ctrl Pts',(-43.4509772683043,30.0171379110115,
-39.1922766338915));
#256732=CARTESIAN_POINT('Ctrl Pts',(-43.448850057475,30.0185923429967,-39.1921186649498));
#256733=CARTESIAN_POINT('Ctrl Pts',(-43.3720581307162,30.0712848254434,
-39.1863818256824));
#256734=CARTESIAN_POINT('Ctrl Pts',(-43.3005780774843,30.1267697410433,
-39.1798786632206));
#256735=CARTESIAN_POINT('Ctrl Pts',(-43.1313005315916,30.2748214743608,
-39.1616036912891));
#256736=CARTESIAN_POINT('Ctrl Pts',(-43.038186711969,30.3718329559061,-39.1488638155419));
#256737=CARTESIAN_POINT('Ctrl Pts',(-42.7806050039729,30.6908099865963,
-39.104922208377));
#256738=CARTESIAN_POINT('Ctrl Pts',(-42.6474050756438,30.9323003143339,
-39.0690165286225));
#256739=CARTESIAN_POINT('Ctrl Pts',(-42.5442998877123,31.2160759566304,
-39.0229211248878));
#256740=CARTESIAN_POINT('Ctrl Pts',(-42.5351088114909,31.2426960773276,
-39.0185610256159));
#256741=CARTESIAN_POINT('Ctrl Pts',(-42.5264442257536,31.2691195439559,
-39.0141970763358));
#256742=CARTESIAN_POINT('Ctrl Pts',(-46.5766932247455,31.5404524382932,
-52.6102625));
#256743=CARTESIAN_POINT('Ctrl Pts',(-46.5766932247455,30.3460643999139,
-52.5519291666666));
#256744=CARTESIAN_POINT('Ctrl Pts',(-45.5423228415329,29.7488703807243,
-52.4935958333333));
#256745=CARTESIAN_POINT('Ctrl Pts',(-44.5079524583202,29.1516763615346,
-52.4352625));
#256746=CARTESIAN_POINT('Ctrl Pts',(-43.4735820751074,29.7488703807243,
-52.3769291666667));
#256747=CARTESIAN_POINT('Ctrl Pts',(-42.4392116918948,30.3460643999138,
-52.3185958333334));
#256748=CARTESIAN_POINT('Ctrl Pts',(-42.4392116918948,31.5404524382931,
-52.2602625));
#256749=CARTESIAN_POINT('Ctrl Pts',(-42.4392116918947,32.7348404766723,
-52.2019291666667));
#256750=CARTESIAN_POINT('Ctrl Pts',(-43.4735820751074,33.332034495862,-52.1435958333333));
#256751=CARTESIAN_POINT('Ctrl Pts',(-44.5079524583201,33.9292285150516,
-52.0852625));
#256752=CARTESIAN_POINT('Ctrl Pts',(-45.5423228415328,33.332034495862,-52.0269291666667));
#256753=CARTESIAN_POINT('Ctrl Pts',(-46.5766932247455,32.7348404766724,
-51.9685958333333));
#256754=CARTESIAN_POINT('Ctrl Pts',(-46.5766932247455,31.5404524382932,
-51.9102625));
#256755=CARTESIAN_POINT('Ctrl Pts',(-46.5766932247455,30.3460643999139,
-51.8519291666667));
#256756=CARTESIAN_POINT('Ctrl Pts',(-45.5423228415329,29.7488703807243,
-51.7935958333333));
#256757=CARTESIAN_POINT('Ctrl Pts',(-44.5079524583202,29.1516763615346,
-51.7352625));
#256758=CARTESIAN_POINT('Ctrl Pts',(-43.4735820751074,29.7488703807243,
-51.6769291666667));
#256759=CARTESIAN_POINT('Ctrl Pts',(-42.4392116918948,30.3460643999138,
-51.6185958333333));
#256760=CARTESIAN_POINT('Ctrl Pts',(-42.4392116918948,31.5404524382931,
-51.5602625));
#256761=CARTESIAN_POINT('Ctrl Pts',(-42.4392116918947,32.7348404766723,
-51.5019291666666));
#256762=CARTESIAN_POINT('Ctrl Pts',(-43.4735820751074,33.332034495862,-51.4435958333333));
#256763=CARTESIAN_POINT('Ctrl Pts',(-44.5079524583201,33.9292285150516,
-51.3852625));
#256764=CARTESIAN_POINT('Ctrl Pts',(-45.5423228415328,33.332034495862,-51.3269291666667));
#256765=CARTESIAN_POINT('Ctrl Pts',(-46.5766932247455,32.7348404766724,
-51.2685958333333));
#256766=CARTESIAN_POINT('Ctrl Pts',(-46.5766932247455,31.5404524382932,
-51.2102625));
#256767=CARTESIAN_POINT('Ctrl Pts',(-46.5766932247455,30.3460643999139,
-51.1519291666666));
#256768=CARTESIAN_POINT('Ctrl Pts',(-45.5423228415329,29.7488703807243,
-51.0935958333334));
#256769=CARTESIAN_POINT('Ctrl Pts',(-44.5079524583202,29.1516763615346,
-51.0352625));
#256770=CARTESIAN_POINT('Ctrl Pts',(-43.4735820751074,29.7488703807243,
-50.9769291666667));
#256771=CARTESIAN_POINT('Ctrl Pts',(-42.4392116918948,30.3460643999138,
-50.9185958333333));
#256772=CARTESIAN_POINT('Ctrl Pts',(-42.4392116918948,31.5404524382931,
-50.8602625));
#256773=CARTESIAN_POINT('Ctrl Pts',(-42.4392116918947,32.7348404766723,
-50.8019291666667));
#256774=CARTESIAN_POINT('Ctrl Pts',(-43.4735820751074,33.332034495862,-50.7435958333333));
#256775=CARTESIAN_POINT('Ctrl Pts',(-44.5079524583201,33.9292285150516,
-50.6852625));
#256776=CARTESIAN_POINT('Ctrl Pts',(-45.5423228415328,33.332034495862,-50.6269291666667));
#256777=CARTESIAN_POINT('Ctrl Pts',(-46.5766932247455,32.7348404766724,
-50.5685958333333));
#256778=CARTESIAN_POINT('Ctrl Pts',(-46.5766932247455,31.5404524382932,
-50.5102625));
#256779=CARTESIAN_POINT('Ctrl Pts',(-46.5766932247455,30.3460643999139,
-50.4519291666667));
#256780=CARTESIAN_POINT('Ctrl Pts',(-45.5423228415329,29.7488703807243,
-50.3935958333333));
#256781=CARTESIAN_POINT('Ctrl Pts',(-44.5079524583202,29.1516763615346,
-50.3352625));
#256782=CARTESIAN_POINT('Ctrl Pts',(-43.4735820751074,29.7488703807243,
-50.2769291666667));
#256783=CARTESIAN_POINT('Ctrl Pts',(-42.4392116918948,30.3460643999138,
-50.2185958333333));
#256784=CARTESIAN_POINT('Ctrl Pts',(-42.4392116918948,31.5404524382931,
-50.1602625));
#256785=CARTESIAN_POINT('Ctrl Pts',(-42.4392116918947,32.7348404766723,
-50.1019291666667));
#256786=CARTESIAN_POINT('Ctrl Pts',(-43.4735820751074,33.332034495862,-50.0435958333333));
#256787=CARTESIAN_POINT('Ctrl Pts',(-44.5079524583201,33.9292285150516,
-49.9852625));
#256788=CARTESIAN_POINT('Ctrl Pts',(-45.5423228415328,33.332034495862,-49.9269291666667));
#256789=CARTESIAN_POINT('Ctrl Pts',(-46.5766932247455,32.7348404766724,
-49.8685958333333));
#256790=CARTESIAN_POINT('Ctrl Pts',(-46.5766932247455,31.5404524382932,
-49.8102625));
#256791=CARTESIAN_POINT('Ctrl Pts',(-46.5766932247455,30.3460643999139,
-49.7519291666667));
#256792=CARTESIAN_POINT('Ctrl Pts',(-45.5423228415329,29.7488703807243,
-49.6935958333334));
#256793=CARTESIAN_POINT('Ctrl Pts',(-44.5079524583202,29.1516763615346,
-49.6352625));
#256794=CARTESIAN_POINT('Ctrl Pts',(-43.4735820751074,29.7488703807243,
-49.5769291666667));
#256795=CARTESIAN_POINT('Ctrl Pts',(-42.4392116918948,30.3460643999138,
-49.5185958333334));
#256796=CARTESIAN_POINT('Ctrl Pts',(-42.4392116918948,31.5404524382931,
-49.4602625));
#256797=CARTESIAN_POINT('Ctrl Pts',(-42.4392116918947,32.7348404766723,
-49.4019291666667));
#256798=CARTESIAN_POINT('Ctrl Pts',(-43.4735820751074,33.332034495862,-49.3435958333333));
#256799=CARTESIAN_POINT('Ctrl Pts',(-44.5079524583201,33.9292285150516,
-49.2852625));
#256800=CARTESIAN_POINT('Ctrl Pts',(-45.5423228415328,33.332034495862,-49.2269291666667));
#256801=CARTESIAN_POINT('Ctrl Pts',(-46.5766932247455,32.7348404766724,
-49.1685958333334));
#256802=CARTESIAN_POINT('Ctrl Pts',(-46.5766932247455,31.5404524382932,
-49.1102625));
#256803=CARTESIAN_POINT('Ctrl Pts',(-46.5766932247455,30.3460643999139,
-49.0519291666667));
#256804=CARTESIAN_POINT('Ctrl Pts',(-45.5423228415329,29.7488703807243,
-48.9935958333333));
#256805=CARTESIAN_POINT('Ctrl Pts',(-44.5079524583202,29.1516763615346,
-48.9352625));
#256806=CARTESIAN_POINT('Ctrl Pts',(-43.4735820751074,29.7488703807243,
-48.8769291666667));
#256807=CARTESIAN_POINT('Ctrl Pts',(-42.4392116918948,30.3460643999138,
-48.8185958333333));
#256808=CARTESIAN_POINT('Ctrl Pts',(-42.4392116918948,31.5404524382931,
-48.7602625));
#256809=CARTESIAN_POINT('Ctrl Pts',(-42.4392116918947,32.7348404766723,
-48.7019291666667));
#256810=CARTESIAN_POINT('Ctrl Pts',(-43.4735820751074,33.332034495862,-48.6435958333333));
#256811=CARTESIAN_POINT('Ctrl Pts',(-44.5079524583201,33.9292285150516,
-48.5852625));
#256812=CARTESIAN_POINT('Ctrl Pts',(-45.5423228415328,33.332034495862,-48.5269291666667));
#256813=CARTESIAN_POINT('Ctrl Pts',(-46.5766932247455,32.7348404766724,
-48.4685958333333));
#256814=CARTESIAN_POINT('Ctrl Pts',(-46.5766932247455,31.5404524382932,
-48.4102625));
#256815=CARTESIAN_POINT('Ctrl Pts',(-46.5766932247455,30.3460643999139,
-48.3519291666667));
#256816=CARTESIAN_POINT('Ctrl Pts',(-45.5423228415329,29.7488703807243,
-48.2935958333333));
#256817=CARTESIAN_POINT('Ctrl Pts',(-44.5079524583202,29.1516763615346,
-48.2352625));
#256818=CARTESIAN_POINT('Ctrl Pts',(-43.4735820751074,29.7488703807243,
-48.1769291666667));
#256819=CARTESIAN_POINT('Ctrl Pts',(-42.4392116918948,30.3460643999138,
-48.1185958333334));
#256820=CARTESIAN_POINT('Ctrl Pts',(-42.4392116918948,31.5404524382931,
-48.0602625));
#256821=CARTESIAN_POINT('Ctrl Pts',(-42.4392116918947,32.7348404766723,
-48.0019291666667));
#256822=CARTESIAN_POINT('Ctrl Pts',(-43.4735820751074,33.332034495862,-47.9435958333334));
#256823=CARTESIAN_POINT('Ctrl Pts',(-44.5079524583201,33.9292285150516,
-47.8852625));
#256824=CARTESIAN_POINT('Ctrl Pts',(-45.5423228415328,33.332034495862,-47.8269291666667));
#256825=CARTESIAN_POINT('Ctrl Pts',(-46.5766932247455,32.7348404766724,
-47.7685958333333));
#256826=CARTESIAN_POINT('Ctrl Pts',(-46.5766932247455,31.5404524382932,
-47.7102625));
#256827=CARTESIAN_POINT('Ctrl Pts',(-46.5766932247455,30.3460643999139,
-47.6519291666667));
#256828=CARTESIAN_POINT('Ctrl Pts',(-45.5423228415329,29.7488703807243,
-47.5935958333333));
#256829=CARTESIAN_POINT('Ctrl Pts',(-44.5079524583202,29.1516763615346,
-47.5352625));
#256830=CARTESIAN_POINT('Ctrl Pts',(-43.4735820751074,29.7488703807243,
-47.4769291666667));
#256831=CARTESIAN_POINT('Ctrl Pts',(-42.4392116918948,30.3460643999138,
-47.4185958333333));
#256832=CARTESIAN_POINT('Ctrl Pts',(-42.4392116918948,31.5404524382931,
-47.3602625));
#256833=CARTESIAN_POINT('Ctrl Pts',(-42.4392116918947,32.7348404766723,
-47.3019291666666));
#256834=CARTESIAN_POINT('Ctrl Pts',(-43.4735820751074,33.332034495862,-47.2435958333333));
#256835=CARTESIAN_POINT('Ctrl Pts',(-44.5079524583201,33.9292285150516,
-47.1852625));
#256836=CARTESIAN_POINT('Ctrl Pts',(-45.5423228415328,33.332034495862,-47.1269291666667));
#256837=CARTESIAN_POINT('Ctrl Pts',(-46.5766932247455,32.7348404766724,
-47.0685958333333));
#256838=CARTESIAN_POINT('Ctrl Pts',(-46.5766932247455,31.5404524382932,
-47.0102625));
#256839=CARTESIAN_POINT('Ctrl Pts',(-46.5766932247455,30.3460643999139,
-46.9519291666667));
#256840=CARTESIAN_POINT('Ctrl Pts',(-45.5423228415329,29.7488703807243,
-46.8935958333333));
#256841=CARTESIAN_POINT('Ctrl Pts',(-44.5079524583202,29.1516763615346,
-46.8352625));
#256842=CARTESIAN_POINT('Ctrl Pts',(-43.4735820751074,29.7488703807243,
-46.7769291666667));
#256843=CARTESIAN_POINT('Ctrl Pts',(-42.4392116918948,30.3460643999138,
-46.7185958333333));
#256844=CARTESIAN_POINT('Ctrl Pts',(-42.4392116918948,31.5404524382931,
-46.6602625));
#256845=CARTESIAN_POINT('Ctrl Pts',(-42.4392116918948,32.7348404766723,
-46.6019291666667));
#256846=CARTESIAN_POINT('Ctrl Pts',(-43.4735820751074,33.332034495862,-46.5435958333334));
#256847=CARTESIAN_POINT('Ctrl Pts',(-44.5079524583201,33.9292285150516,
-46.4852625));
#256848=CARTESIAN_POINT('Ctrl Pts',(-45.5423228415328,33.332034495862,-46.4269291666667));
#256849=CARTESIAN_POINT('Ctrl Pts',(-46.5766932247455,32.7348404766724,
-46.3685958333333));
#256850=CARTESIAN_POINT('Ctrl Pts',(-46.5766932247455,31.5404524382932,
-46.3102625));
#256851=CARTESIAN_POINT('Ctrl Pts',(-46.5766932247455,30.3460643999139,
-46.2519291666667));
#256852=CARTESIAN_POINT('Ctrl Pts',(-45.5423228415329,29.7488703807243,
-46.1935958333333));
#256853=CARTESIAN_POINT('Ctrl Pts',(-44.5079524583202,29.1516763615346,
-46.1352625));
#256854=CARTESIAN_POINT('Ctrl Pts',(-43.4735820751074,29.7488703807243,
-46.0769291666667));
#256855=CARTESIAN_POINT('Ctrl Pts',(-42.4392116918948,30.3460643999138,
-46.0185958333334));
#256856=CARTESIAN_POINT('Ctrl Pts',(-42.4392116918948,31.5404524382931,
-45.9602625));
#256857=CARTESIAN_POINT('Ctrl Pts',(-42.4392116918948,32.7348404766723,
-45.9019291666667));
#256858=CARTESIAN_POINT('Ctrl Pts',(-43.4735820751074,33.332034495862,-45.8435958333333));
#256859=CARTESIAN_POINT('Ctrl Pts',(-44.5079524583201,33.9292285150516,
-45.7852625));
#256860=CARTESIAN_POINT('Ctrl Pts',(-45.5423228415328,33.332034495862,-45.7269291666667));
#256861=CARTESIAN_POINT('Ctrl Pts',(-46.5766932247455,32.7348404766724,
-45.6685958333334));
#256862=CARTESIAN_POINT('Ctrl Pts',(-46.5766932247455,31.5404524382932,
-45.6102625));
#256863=CARTESIAN_POINT('Ctrl Pts',(-46.5766932247455,30.3460643999139,
-45.5519291666667));
#256864=CARTESIAN_POINT('Ctrl Pts',(-45.5423228415329,29.7488703807243,
-45.4935958333333));
#256865=CARTESIAN_POINT('Ctrl Pts',(-44.5079524583202,29.1516763615346,
-45.4352625));
#256866=CARTESIAN_POINT('Ctrl Pts',(-43.4735820751074,29.7488703807243,
-45.3769291666667));
#256867=CARTESIAN_POINT('Ctrl Pts',(-42.4392116918948,30.3460643999138,
-45.3185958333333));
#256868=CARTESIAN_POINT('Ctrl Pts',(-42.4392116918948,31.5404524382931,
-45.2602625));
#256869=CARTESIAN_POINT('Ctrl Pts',(-42.4392116918948,32.7348404766723,
-45.2019291666667));
#256870=CARTESIAN_POINT('Ctrl Pts',(-43.4735820751074,33.332034495862,-45.1435958333333));
#256871=CARTESIAN_POINT('Ctrl Pts',(-44.5079524583201,33.9292285150516,
-45.0852625));
#256872=CARTESIAN_POINT('Ctrl Pts',(-45.5423228415328,33.332034495862,-45.0269291666667));
#256873=CARTESIAN_POINT('Ctrl Pts',(-46.5766932247455,32.7348404766724,
-44.9685958333334));
#256874=CARTESIAN_POINT('Ctrl Pts',(-46.5766932247455,31.5404524382932,
-44.9102625));
#256875=CARTESIAN_POINT('Ctrl Pts',(-46.5766932247455,30.3460643999139,
-44.8519291666667));
#256876=CARTESIAN_POINT('Ctrl Pts',(-45.5423228415329,29.7488703807243,
-44.7935958333333));
#256877=CARTESIAN_POINT('Ctrl Pts',(-44.5079524583202,29.1516763615346,
-44.7352625));
#256878=CARTESIAN_POINT('Ctrl Pts',(-43.4735820751074,29.7488703807243,
-44.6769291666667));
#256879=CARTESIAN_POINT('Ctrl Pts',(-42.4392116918948,30.3460643999138,
-44.6185958333334));
#256880=CARTESIAN_POINT('Ctrl Pts',(-42.4392116918948,31.5404524382931,
-44.5602625));
#256881=CARTESIAN_POINT('Ctrl Pts',(-42.4392116918948,32.7348404766723,
-44.5019291666667));
#256882=CARTESIAN_POINT('Ctrl Pts',(-43.4735820751074,33.332034495862,-44.4435958333333));
#256883=CARTESIAN_POINT('Ctrl Pts',(-44.5079524583201,33.9292285150516,
-44.3852625));
#256884=CARTESIAN_POINT('Ctrl Pts',(-45.5423228415328,33.332034495862,-44.3269291666667));
#256885=CARTESIAN_POINT('Ctrl Pts',(-46.5766932247455,32.7348404766724,
-44.2685958333334));
#256886=CARTESIAN_POINT('Ctrl Pts',(-46.5766932247455,31.5404524382932,
-44.2102625));
#256887=CARTESIAN_POINT('Ctrl Pts',(-46.5766932247455,30.3460643999139,
-44.1519291666667));
#256888=CARTESIAN_POINT('Ctrl Pts',(-45.5423228415329,29.7488703807243,
-44.0935958333334));
#256889=CARTESIAN_POINT('Ctrl Pts',(-44.5079524583202,29.1516763615346,
-44.0352625));
#256890=CARTESIAN_POINT('Ctrl Pts',(-43.4735820751074,29.7488703807243,
-43.9769291666667));
#256891=CARTESIAN_POINT('Ctrl Pts',(-42.4392116918948,30.3460643999138,
-43.9185958333333));
#256892=CARTESIAN_POINT('Ctrl Pts',(-42.4392116918948,31.5404524382931,
-43.8602625));
#256893=CARTESIAN_POINT('Ctrl Pts',(-42.4392116918948,32.7348404766723,
-43.8019291666667));
#256894=CARTESIAN_POINT('Ctrl Pts',(-43.4735820751074,33.332034495862,-43.7435958333334));
#256895=CARTESIAN_POINT('Ctrl Pts',(-44.5079524583201,33.9292285150516,
-43.6852625));
#256896=CARTESIAN_POINT('Ctrl Pts',(-45.5423228415328,33.332034495862,-43.6269291666667));
#256897=CARTESIAN_POINT('Ctrl Pts',(-46.5766932247455,32.7348404766724,
-43.5685958333333));
#256898=CARTESIAN_POINT('Ctrl Pts',(-46.5766932247455,31.5404524382932,
-43.5102625));
#256899=CARTESIAN_POINT('Ctrl Pts',(-46.5766932247455,30.3460643999139,
-43.4519291666667));
#256900=CARTESIAN_POINT('Ctrl Pts',(-45.5423228415329,29.7488703807243,
-43.3935958333334));
#256901=CARTESIAN_POINT('Ctrl Pts',(-44.5079524583202,29.1516763615346,
-43.3352625));
#256902=CARTESIAN_POINT('Ctrl Pts',(-43.4735820751074,29.7488703807243,
-43.2769291666667));
#256903=CARTESIAN_POINT('Ctrl Pts',(-42.4392116918948,30.3460643999138,
-43.2185958333333));
#256904=CARTESIAN_POINT('Ctrl Pts',(-42.4392116918948,31.5404524382931,
-43.1602625));
#256905=CARTESIAN_POINT('Ctrl Pts',(-42.4392116918948,32.7348404766723,
-43.1019291666667));
#256906=CARTESIAN_POINT('Ctrl Pts',(-43.4735820751074,33.332034495862,-43.0435958333334));
#256907=CARTESIAN_POINT('Ctrl Pts',(-44.5079524583201,33.9292285150516,
-42.9852625));
#256908=CARTESIAN_POINT('Ctrl Pts',(-45.5423228415328,33.332034495862,-42.9269291666667));
#256909=CARTESIAN_POINT('Ctrl Pts',(-46.5766932247455,32.7348404766724,
-42.8685958333333));
#256910=CARTESIAN_POINT('Ctrl Pts',(-46.5766932247455,31.5404524382932,
-42.8102625));
#256911=CARTESIAN_POINT('Ctrl Pts',(-46.5766932247455,30.3460643999139,
-42.7519291666666));
#256912=CARTESIAN_POINT('Ctrl Pts',(-45.5423228415329,29.7488703807243,
-42.6935958333333));
#256913=CARTESIAN_POINT('Ctrl Pts',(-44.5079524583202,29.1516763615346,
-42.6352625));
#256914=CARTESIAN_POINT('Ctrl Pts',(-43.4735820751074,29.7488703807243,
-42.5769291666667));
#256915=CARTESIAN_POINT('Ctrl Pts',(-42.4392116918948,30.3460643999138,
-42.5185958333333));
#256916=CARTESIAN_POINT('Ctrl Pts',(-42.4392116918948,31.5404524382931,
-42.4602625));
#256917=CARTESIAN_POINT('Ctrl Pts',(-42.4392116918948,32.7348404766723,
-42.4019291666666));
#256918=CARTESIAN_POINT('Ctrl Pts',(-43.4735820751074,33.332034495862,-42.3435958333334));
#256919=CARTESIAN_POINT('Ctrl Pts',(-44.5079524583201,33.9292285150516,
-42.2852625));
#256920=CARTESIAN_POINT('Ctrl Pts',(-45.5423228415328,33.332034495862,-42.2269291666667));
#256921=CARTESIAN_POINT('Ctrl Pts',(-46.5766932247455,32.7348404766724,
-42.1685958333333));
#256922=CARTESIAN_POINT('Ctrl Pts',(-46.5766932247455,31.5404524382932,
-42.1102625));
#256923=CARTESIAN_POINT('Ctrl Pts',(-46.5766932247455,30.3460643999139,
-42.0519291666666));
#256924=CARTESIAN_POINT('Ctrl Pts',(-45.5423228415329,29.7488703807243,
-41.9935958333334));
#256925=CARTESIAN_POINT('Ctrl Pts',(-44.5079524583202,29.1516763615346,
-41.9352625));
#256926=CARTESIAN_POINT('Ctrl Pts',(-43.4735820751074,29.7488703807243,
-41.8769291666667));
#256927=CARTESIAN_POINT('Ctrl Pts',(-42.4392116918948,30.3460643999138,
-41.8185958333333));
#256928=CARTESIAN_POINT('Ctrl Pts',(-42.4392116918948,31.5404524382931,
-41.7602625));
#256929=CARTESIAN_POINT('Ctrl Pts',(-42.4392116918948,32.7348404766723,
-41.7019291666666));
#256930=CARTESIAN_POINT('Ctrl Pts',(-43.4735820751074,33.332034495862,-41.6435958333334));
#256931=CARTESIAN_POINT('Ctrl Pts',(-44.5079524583201,33.9292285150516,
-41.5852625));
#256932=CARTESIAN_POINT('Ctrl Pts',(-45.5423228415328,33.332034495862,-41.5269291666667));
#256933=CARTESIAN_POINT('Ctrl Pts',(-46.5766932247455,32.7348404766724,
-41.4685958333333));
#256934=CARTESIAN_POINT('Ctrl Pts',(-46.5766932247455,31.5404524382932,
-41.4102625));
#256935=CARTESIAN_POINT('Ctrl Pts',(-46.5766932247455,30.3460643999139,
-41.3519291666666));
#256936=CARTESIAN_POINT('Ctrl Pts',(-45.5423228415329,29.7488703807243,
-41.2935958333334));
#256937=CARTESIAN_POINT('Ctrl Pts',(-44.5079524583202,29.1516763615346,
-41.2352625));
#256938=CARTESIAN_POINT('Ctrl Pts',(-43.4735820751074,29.7488703807243,
-41.1769291666667));
#256939=CARTESIAN_POINT('Ctrl Pts',(-42.4392116918948,30.3460643999138,
-41.1185958333333));
#256940=CARTESIAN_POINT('Ctrl Pts',(-42.4392116918948,31.5404524382931,
-41.0602625));
#256941=CARTESIAN_POINT('Ctrl Pts',(-42.4392116918948,32.7348404766723,
-41.0019291666666));
#256942=CARTESIAN_POINT('Ctrl Pts',(-43.4735820751074,33.332034495862,-40.9435958333334));
#256943=CARTESIAN_POINT('Ctrl Pts',(-44.5079524583201,33.9292285150516,
-40.8852625));
#256944=CARTESIAN_POINT('Ctrl Pts',(-45.5423228415328,33.332034495862,-40.8269291666667));
#256945=CARTESIAN_POINT('Ctrl Pts',(-46.5766932247455,32.7348404766724,
-40.7685958333333));
#256946=CARTESIAN_POINT('Ctrl Pts',(-46.5766932247455,31.5404524382932,
-40.7102625));
#256947=CARTESIAN_POINT('Ctrl Pts',(-46.5766932247455,30.3460643999139,
-40.6519291666667));
#256948=CARTESIAN_POINT('Ctrl Pts',(-45.5423228415329,29.7488703807243,
-40.5935958333334));
#256949=CARTESIAN_POINT('Ctrl Pts',(-44.5079524583202,29.1516763615346,
-40.5352625));
#256950=CARTESIAN_POINT('Ctrl Pts',(-43.4735820751074,29.7488703807243,
-40.4769291666667));
#256951=CARTESIAN_POINT('Ctrl Pts',(-42.4392116918948,30.3460643999138,
-40.4185958333333));
#256952=CARTESIAN_POINT('Ctrl Pts',(-42.4392116918948,31.5404524382931,
-40.3602625));
#256953=CARTESIAN_POINT('Ctrl Pts',(-42.4392116918948,32.7348404766723,
-40.3019291666667));
#256954=CARTESIAN_POINT('Ctrl Pts',(-43.4735820751074,33.332034495862,-40.2435958333334));
#256955=CARTESIAN_POINT('Ctrl Pts',(-44.5079524583201,33.9292285150516,
-40.1852625));
#256956=CARTESIAN_POINT('Ctrl Pts',(-45.5423228415328,33.332034495862,-40.1269291666666));
#256957=CARTESIAN_POINT('Ctrl Pts',(-46.5766932247455,32.7348404766724,
-40.0685958333333));
#256958=CARTESIAN_POINT('Ctrl Pts',(-46.5766932247455,31.5404524382932,
-40.0102625));
#256959=CARTESIAN_POINT('Ctrl Pts',(-46.5766932247455,30.3460643999139,
-39.9519291666667));
#256960=CARTESIAN_POINT('Ctrl Pts',(-45.5423228415329,29.7488703807243,
-39.8935958333334));
#256961=CARTESIAN_POINT('Ctrl Pts',(-44.5079524583202,29.1516763615346,
-39.8352625));
#256962=CARTESIAN_POINT('Ctrl Pts',(-43.4735820751074,29.7488703807243,
-39.7769291666666));
#256963=CARTESIAN_POINT('Ctrl Pts',(-42.4392116918948,30.3460643999138,
-39.7185958333334));
#256964=CARTESIAN_POINT('Ctrl Pts',(-42.4392116918948,31.5404524382931,
-39.6602625));
#256965=CARTESIAN_POINT('Ctrl Pts',(-42.4392116918948,32.7348404766723,
-39.6019291666667));
#256966=CARTESIAN_POINT('Ctrl Pts',(-43.4735820751074,33.332034495862,-39.5435958333333));
#256967=CARTESIAN_POINT('Ctrl Pts',(-44.5079524583201,33.9292285150516,
-39.4852625));
#256968=CARTESIAN_POINT('Ctrl Pts',(-45.5423228415328,33.332034495862,-39.4269291666667));
#256969=CARTESIAN_POINT('Ctrl Pts',(-46.5766932247455,32.7348404766724,
-39.3685958333334));
#256970=CARTESIAN_POINT('Ctrl Pts',(-46.5766932247455,31.5404524382932,
-39.3102625));
#256971=CARTESIAN_POINT('Ctrl Pts',(-46.5766932247455,30.3460643999139,
-39.2519291666667));
#256972=CARTESIAN_POINT('Ctrl Pts',(-45.5423228415329,29.7488703807243,
-39.1935958333334));
#256973=CARTESIAN_POINT('Ctrl Pts',(-44.5079524583202,29.1516763615346,
-39.1352625));
#256974=CARTESIAN_POINT('Ctrl Pts',(-43.4735820751074,29.7488703807243,
-39.0769291666667));
#256975=CARTESIAN_POINT('Ctrl Pts',(-42.4392116918948,30.3460643999138,
-39.0185958333333));
#256976=CARTESIAN_POINT('Ctrl Pts',(-42.4392116918948,31.5404524382931,
-38.9602625));
#256977=CARTESIAN_POINT('Ctrl Pts',(-42.4392116918948,32.7348404766723,
-38.9019291666667));
#256978=CARTESIAN_POINT('Ctrl Pts',(-43.4735820751074,33.332034495862,-38.8435958333333));
#256979=CARTESIAN_POINT('Ctrl Pts',(-44.5079524583201,33.9292285150516,
-38.7852625));
#256980=CARTESIAN_POINT('Ctrl Pts',(-45.5423228415328,33.332034495862,-38.7269291666667));
#256981=CARTESIAN_POINT('Ctrl Pts',(-46.5766932247455,32.7348404766724,
-38.6685958333334));
#256982=CARTESIAN_POINT('Ctrl Pts',(-46.5766932247455,31.5404524382932,
-38.6102625));
#256983=CARTESIAN_POINT('Ctrl Pts',(-46.5766932247455,30.3460643999139,
-38.5519291666667));
#256984=CARTESIAN_POINT('Ctrl Pts',(-45.5423228415329,29.7488703807243,
-38.4935958333334));
#256985=CARTESIAN_POINT('Ctrl Pts',(-44.5079524583202,29.1516763615346,
-38.4352625));
#256986=CARTESIAN_POINT('Ctrl Pts',(-43.4735820751074,29.7488703807243,
-38.3769291666666));
#256987=CARTESIAN_POINT('Ctrl Pts',(-42.4392116918948,30.3460643999138,
-38.3185958333333));
#256988=CARTESIAN_POINT('Ctrl Pts',(-42.4392116918948,31.5404524382931,
-38.2602625));
#256989=CARTESIAN_POINT('Ctrl Pts',(-42.4392116918948,32.7348404766723,
-38.2019291666667));
#256990=CARTESIAN_POINT('Ctrl Pts',(-43.4735820751074,33.332034495862,-38.1435958333334));
#256991=CARTESIAN_POINT('Ctrl Pts',(-44.5079524583201,33.9292285150516,
-38.0852625));
#256992=CARTESIAN_POINT('Ctrl Pts',(-45.5423228415328,33.332034495862,-38.0269291666667));
#256993=CARTESIAN_POINT('Ctrl Pts',(-46.5766932247455,32.7348404766724,
-37.9685958333333));
#256994=CARTESIAN_POINT('Ctrl Pts',(-46.5766932247455,31.5404524382932,
-37.9102625));
#256995=CARTESIAN_POINT('Ctrl Pts',(-46.5766932247455,30.3460643999139,
-37.8519291666667));
#256996=CARTESIAN_POINT('Ctrl Pts',(-45.5423228415329,29.7488703807243,
-37.7935958333334));
#256997=CARTESIAN_POINT('Ctrl Pts',(-44.5079524583202,29.1516763615346,
-37.7352625));
#256998=CARTESIAN_POINT('Ctrl Pts',(-43.4735820751074,29.7488703807243,
-37.6769291666667));
#256999=CARTESIAN_POINT('Ctrl Pts',(-42.4392116918948,30.3460643999138,
-37.6185958333333));
#257000=CARTESIAN_POINT('Ctrl Pts',(-42.4392116918948,31.5404524382931,
-37.5602625));
#257001=CARTESIAN_POINT('Ctrl Pts',(-42.4392116918948,32.7348404766723,
-37.5019291666666));
#257002=CARTESIAN_POINT('Ctrl Pts',(-43.4735820751074,33.332034495862,-37.4435958333333));
#257003=CARTESIAN_POINT('Ctrl Pts',(-44.5079524583201,33.9292285150516,
-37.3852625));
#257004=CARTESIAN_POINT('Ctrl Pts',(-45.5423228415328,33.332034495862,-37.3269291666667));
#257005=CARTESIAN_POINT('Ctrl Pts',(-46.5766932247455,32.7348404766724,
-37.2685958333333));
#257006=CARTESIAN_POINT('Ctrl Pts',(-46.5766932247455,31.5404524382932,
-37.2102625));
#257007=CARTESIAN_POINT('Ctrl Pts',(-46.5766932247455,30.3460643999139,
-37.1519291666667));
#257008=CARTESIAN_POINT('Ctrl Pts',(-45.5423228415329,29.7488703807243,
-37.0935958333333));
#257009=CARTESIAN_POINT('Ctrl Pts',(-44.5079524583202,29.1516763615346,
-37.0352625));
#257010=CARTESIAN_POINT('Ctrl Pts',(-43.4735820751074,29.7488703807243,
-36.9769291666667));
#257011=CARTESIAN_POINT('Ctrl Pts',(-42.4392116918948,30.3460643999138,
-36.9185958333333));
#257012=CARTESIAN_POINT('Ctrl Pts',(-42.4392116918948,31.5404524382931,
-36.8602625));
#257013=CARTESIAN_POINT('Ctrl Pts',(-42.4392116918948,32.7348404766723,
-36.8019291666666));
#257014=CARTESIAN_POINT('Ctrl Pts',(-43.4735820751074,33.332034495862,-36.7435958333334));
#257015=CARTESIAN_POINT('Ctrl Pts',(-44.5079524583201,33.9292285150516,
-36.6852625));
#257016=CARTESIAN_POINT('Ctrl Pts',(-45.5423228415328,33.332034495862,-36.6269291666666));
#257017=CARTESIAN_POINT('Ctrl Pts',(-45.6766051604214,33.2545065629043,
-36.6193563132714));
#257018=CARTESIAN_POINT('Ctrl Pts',(-45.7978303778612,33.1578278775004,
-36.611216324118));
#257019=CARTESIAN_POINT('Ctrl Pts',(-46.1766975859751,31.5404524382932,
-52.8412000897188));
#257020=CARTESIAN_POINT('Ctrl Pts',(-46.1766975859751,30.5770019896326,
-52.7828667563854));
#257021=CARTESIAN_POINT('Ctrl Pts',(-45.3423250221477,30.0952767653024,
-52.7245334230522));
#257022=CARTESIAN_POINT('Ctrl Pts',(-44.5079524583202,29.6135515409722,
-52.6662000897188));
#257023=CARTESIAN_POINT('Ctrl Pts',(-43.6735798944927,30.0952767653024,
-52.6078667563855));
#257024=CARTESIAN_POINT('Ctrl Pts',(-42.8392073306652,30.5770019896326,
-52.5495334230521));
#257025=CARTESIAN_POINT('Ctrl Pts',(-42.8392073306652,31.5404524382931,
-52.4912000897188));
#257026=CARTESIAN_POINT('Ctrl Pts',(-42.8392073306652,32.5039028869536,
-52.4328667563855));
#257027=CARTESIAN_POINT('Ctrl Pts',(-43.6735798944926,32.9856281112839,
-52.3745334230522));
#257028=CARTESIAN_POINT('Ctrl Pts',(-44.5079524583201,33.4673533356141,
-52.3162000897188));
#257029=CARTESIAN_POINT('Ctrl Pts',(-45.3423250221477,32.9856281112839,
-52.2578667563855));
#257030=CARTESIAN_POINT('Ctrl Pts',(-46.1766975859751,32.5039028869536,
-52.1995334230521));
#257031=CARTESIAN_POINT('Ctrl Pts',(-46.1766975859751,31.5404524382932,
-52.1412000897188));
#257032=CARTESIAN_POINT('Ctrl Pts',(-46.1766975859751,30.5770019896326,
-52.0828667563854));
#257033=CARTESIAN_POINT('Ctrl Pts',(-45.3423250221477,30.0952767653024,
-52.0245334230521));
#257034=CARTESIAN_POINT('Ctrl Pts',(-44.5079524583202,29.6135515409722,
-51.9662000897188));
#257035=CARTESIAN_POINT('Ctrl Pts',(-43.6735798944927,30.0952767653024,
-51.9078667563855));
#257036=CARTESIAN_POINT('Ctrl Pts',(-42.8392073306652,30.5770019896326,
-51.8495334230521));
#257037=CARTESIAN_POINT('Ctrl Pts',(-42.8392073306652,31.5404524382931,
-51.7912000897188));
#257038=CARTESIAN_POINT('Ctrl Pts',(-42.8392073306652,32.5039028869536,
-51.7328667563854));
#257039=CARTESIAN_POINT('Ctrl Pts',(-43.6735798944926,32.9856281112839,
-51.6745334230521));
#257040=CARTESIAN_POINT('Ctrl Pts',(-44.5079524583201,33.4673533356141,
-51.6162000897188));
#257041=CARTESIAN_POINT('Ctrl Pts',(-45.3423250221477,32.9856281112839,
-51.5578667563855));
#257042=CARTESIAN_POINT('Ctrl Pts',(-46.1766975859751,32.5039028869536,
-51.4995334230521));
#257043=CARTESIAN_POINT('Ctrl Pts',(-46.1766975859751,31.5404524382932,
-51.4412000897188));
#257044=CARTESIAN_POINT('Ctrl Pts',(-46.1766975859751,30.5770019896326,
-51.3828667563855));
#257045=CARTESIAN_POINT('Ctrl Pts',(-45.3423250221477,30.0952767653024,
-51.3245334230522));
#257046=CARTESIAN_POINT('Ctrl Pts',(-44.5079524583202,29.6135515409722,
-51.2662000897188));
#257047=CARTESIAN_POINT('Ctrl Pts',(-43.6735798944927,30.0952767653024,
-51.2078667563855));
#257048=CARTESIAN_POINT('Ctrl Pts',(-42.8392073306652,30.5770019896326,
-51.1495334230521));
#257049=CARTESIAN_POINT('Ctrl Pts',(-42.8392073306652,31.5404524382931,
-51.0912000897188));
#257050=CARTESIAN_POINT('Ctrl Pts',(-42.8392073306652,32.5039028869536,
-51.0328667563854));
#257051=CARTESIAN_POINT('Ctrl Pts',(-43.6735798944926,32.9856281112839,
-50.9745334230521));
#257052=CARTESIAN_POINT('Ctrl Pts',(-44.5079524583201,33.4673533356141,
-50.9162000897188));
#257053=CARTESIAN_POINT('Ctrl Pts',(-45.3423250221477,32.9856281112839,
-50.8578667563855));
#257054=CARTESIAN_POINT('Ctrl Pts',(-46.1766975859751,32.5039028869536,
-50.7995334230521));
#257055=CARTESIAN_POINT('Ctrl Pts',(-46.1766975859751,31.5404524382932,
-50.7412000897188));
#257056=CARTESIAN_POINT('Ctrl Pts',(-46.1766975859751,30.5770019896326,
-50.6828667563855));
#257057=CARTESIAN_POINT('Ctrl Pts',(-45.3423250221477,30.0952767653024,
-50.6245334230521));
#257058=CARTESIAN_POINT('Ctrl Pts',(-44.5079524583202,29.6135515409722,
-50.5662000897188));
#257059=CARTESIAN_POINT('Ctrl Pts',(-43.6735798944927,30.0952767653024,
-50.5078667563855));
#257060=CARTESIAN_POINT('Ctrl Pts',(-42.8392073306652,30.5770019896326,
-50.4495334230521));
#257061=CARTESIAN_POINT('Ctrl Pts',(-42.8392073306652,31.5404524382931,
-50.3912000897188));
#257062=CARTESIAN_POINT('Ctrl Pts',(-42.8392073306652,32.5039028869536,
-50.3328667563854));
#257063=CARTESIAN_POINT('Ctrl Pts',(-43.6735798944926,32.9856281112839,
-50.2745334230521));
#257064=CARTESIAN_POINT('Ctrl Pts',(-44.5079524583201,33.4673533356141,
-50.2162000897188));
#257065=CARTESIAN_POINT('Ctrl Pts',(-45.3423250221477,32.9856281112839,
-50.1578667563855));
#257066=CARTESIAN_POINT('Ctrl Pts',(-46.1766975859751,32.5039028869536,
-50.0995334230521));
#257067=CARTESIAN_POINT('Ctrl Pts',(-46.1766975859751,31.5404524382932,
-50.0412000897188));
#257068=CARTESIAN_POINT('Ctrl Pts',(-46.1766975859751,30.5770019896326,
-49.9828667563855));
#257069=CARTESIAN_POINT('Ctrl Pts',(-45.3423250221477,30.0952767653024,
-49.9245334230522));
#257070=CARTESIAN_POINT('Ctrl Pts',(-44.5079524583202,29.6135515409722,
-49.8662000897188));
#257071=CARTESIAN_POINT('Ctrl Pts',(-43.6735798944927,30.0952767653024,
-49.8078667563855));
#257072=CARTESIAN_POINT('Ctrl Pts',(-42.8392073306652,30.5770019896326,
-49.7495334230521));
#257073=CARTESIAN_POINT('Ctrl Pts',(-42.8392073306652,31.5404524382931,
-49.6912000897188));
#257074=CARTESIAN_POINT('Ctrl Pts',(-42.8392073306652,32.5039028869536,
-49.6328667563854));
#257075=CARTESIAN_POINT('Ctrl Pts',(-43.6735798944926,32.9856281112839,
-49.5745334230521));
#257076=CARTESIAN_POINT('Ctrl Pts',(-44.5079524583201,33.4673533356141,
-49.5162000897188));
#257077=CARTESIAN_POINT('Ctrl Pts',(-45.3423250221477,32.9856281112839,
-49.4578667563855));
#257078=CARTESIAN_POINT('Ctrl Pts',(-46.1766975859751,32.5039028869536,
-49.3995334230521));
#257079=CARTESIAN_POINT('Ctrl Pts',(-46.1766975859751,31.5404524382932,
-49.3412000897188));
#257080=CARTESIAN_POINT('Ctrl Pts',(-46.1766975859751,30.5770019896326,
-49.2828667563854));
#257081=CARTESIAN_POINT('Ctrl Pts',(-45.3423250221477,30.0952767653024,
-49.2245334230521));
#257082=CARTESIAN_POINT('Ctrl Pts',(-44.5079524583202,29.6135515409722,
-49.1662000897188));
#257083=CARTESIAN_POINT('Ctrl Pts',(-43.6735798944927,30.0952767653024,
-49.1078667563855));
#257084=CARTESIAN_POINT('Ctrl Pts',(-42.8392073306652,30.5770019896326,
-49.0495334230521));
#257085=CARTESIAN_POINT('Ctrl Pts',(-42.8392073306652,31.5404524382931,
-48.9912000897188));
#257086=CARTESIAN_POINT('Ctrl Pts',(-42.8392073306652,32.5039028869536,
-48.9328667563854));
#257087=CARTESIAN_POINT('Ctrl Pts',(-43.6735798944926,32.9856281112839,
-48.8745334230521));
#257088=CARTESIAN_POINT('Ctrl Pts',(-44.5079524583201,33.4673533356141,
-48.8162000897187));
#257089=CARTESIAN_POINT('Ctrl Pts',(-45.3423250221477,32.9856281112839,
-48.7578667563855));
#257090=CARTESIAN_POINT('Ctrl Pts',(-46.1766975859751,32.5039028869536,
-48.6995334230521));
#257091=CARTESIAN_POINT('Ctrl Pts',(-46.1766975859751,31.5404524382932,
-48.6412000897188));
#257092=CARTESIAN_POINT('Ctrl Pts',(-46.1766975859751,30.5770019896326,
-48.5828667563854));
#257093=CARTESIAN_POINT('Ctrl Pts',(-45.3423250221477,30.0952767653024,
-48.5245334230521));
#257094=CARTESIAN_POINT('Ctrl Pts',(-44.5079524583202,29.6135515409722,
-48.4662000897187));
#257095=CARTESIAN_POINT('Ctrl Pts',(-43.6735798944927,30.0952767653024,
-48.4078667563855));
#257096=CARTESIAN_POINT('Ctrl Pts',(-42.8392073306652,30.5770019896326,
-48.3495334230521));
#257097=CARTESIAN_POINT('Ctrl Pts',(-42.8392073306652,31.5404524382931,
-48.2912000897188));
#257098=CARTESIAN_POINT('Ctrl Pts',(-42.8392073306652,32.5039028869536,
-48.2328667563854));
#257099=CARTESIAN_POINT('Ctrl Pts',(-43.6735798944926,32.9856281112839,
-48.1745334230522));
#257100=CARTESIAN_POINT('Ctrl Pts',(-44.5079524583201,33.4673533356141,
-48.1162000897187));
#257101=CARTESIAN_POINT('Ctrl Pts',(-45.3423250221477,32.9856281112839,
-48.0578667563855));
#257102=CARTESIAN_POINT('Ctrl Pts',(-46.1766975859751,32.5039028869536,
-47.9995334230521));
#257103=CARTESIAN_POINT('Ctrl Pts',(-46.1766975859751,31.5404524382932,
-47.9412000897188));
#257104=CARTESIAN_POINT('Ctrl Pts',(-46.1766975859751,30.5770019896326,
-47.8828667563854));
#257105=CARTESIAN_POINT('Ctrl Pts',(-45.3423250221477,30.0952767653024,
-47.8245334230521));
#257106=CARTESIAN_POINT('Ctrl Pts',(-44.5079524583202,29.6135515409722,
-47.7662000897188));
#257107=CARTESIAN_POINT('Ctrl Pts',(-43.6735798944927,30.0952767653024,
-47.7078667563855));
#257108=CARTESIAN_POINT('Ctrl Pts',(-42.8392073306652,30.5770019896326,
-47.6495334230521));
#257109=CARTESIAN_POINT('Ctrl Pts',(-42.8392073306652,31.5404524382931,
-47.5912000897188));
#257110=CARTESIAN_POINT('Ctrl Pts',(-42.8392073306652,32.5039028869536,
-47.5328667563854));
#257111=CARTESIAN_POINT('Ctrl Pts',(-43.6735798944926,32.9856281112839,
-47.4745334230522));
#257112=CARTESIAN_POINT('Ctrl Pts',(-44.5079524583201,33.4673533356141,
-47.4162000897188));
#257113=CARTESIAN_POINT('Ctrl Pts',(-45.3423250221477,32.9856281112839,
-47.3578667563855));
#257114=CARTESIAN_POINT('Ctrl Pts',(-46.1766975859751,32.5039028869536,
-47.2995334230521));
#257115=CARTESIAN_POINT('Ctrl Pts',(-46.1766975859751,31.5404524382932,
-47.2412000897188));
#257116=CARTESIAN_POINT('Ctrl Pts',(-46.1766975859751,30.5770019896326,
-47.1828667563854));
#257117=CARTESIAN_POINT('Ctrl Pts',(-45.3423250221477,30.0952767653024,
-47.1245334230521));
#257118=CARTESIAN_POINT('Ctrl Pts',(-44.5079524583202,29.6135515409722,
-47.0662000897188));
#257119=CARTESIAN_POINT('Ctrl Pts',(-43.6735798944927,30.0952767653024,
-47.0078667563855));
#257120=CARTESIAN_POINT('Ctrl Pts',(-42.8392073306652,30.5770019896326,
-46.9495334230521));
#257121=CARTESIAN_POINT('Ctrl Pts',(-42.8392073306652,31.5404524382931,
-46.8912000897188));
#257122=CARTESIAN_POINT('Ctrl Pts',(-42.8392073306652,32.5039028869536,
-46.8328667563854));
#257123=CARTESIAN_POINT('Ctrl Pts',(-43.6735798944926,32.9856281112839,
-46.7745334230521));
#257124=CARTESIAN_POINT('Ctrl Pts',(-44.5079524583201,33.4673533356141,
-46.7162000897188));
#257125=CARTESIAN_POINT('Ctrl Pts',(-45.3423250221477,32.9856281112839,
-46.6578667563855));
#257126=CARTESIAN_POINT('Ctrl Pts',(-46.1766975859751,32.5039028869536,
-46.5995334230521));
#257127=CARTESIAN_POINT('Ctrl Pts',(-46.1766975859751,31.5404524382932,
-46.5412000897188));
#257128=CARTESIAN_POINT('Ctrl Pts',(-46.1766975859751,30.5770019896326,
-46.4828667563854));
#257129=CARTESIAN_POINT('Ctrl Pts',(-45.3423250221477,30.0952767653024,
-46.4245334230521));
#257130=CARTESIAN_POINT('Ctrl Pts',(-44.5079524583202,29.6135515409722,
-46.3662000897188));
#257131=CARTESIAN_POINT('Ctrl Pts',(-43.6735798944927,30.0952767653024,
-46.3078667563855));
#257132=CARTESIAN_POINT('Ctrl Pts',(-42.8392073306652,30.5770019896326,
-46.2495334230521));
#257133=CARTESIAN_POINT('Ctrl Pts',(-42.8392073306652,31.5404524382931,
-46.1912000897188));
#257134=CARTESIAN_POINT('Ctrl Pts',(-42.8392073306652,32.5039028869536,
-46.1328667563855));
#257135=CARTESIAN_POINT('Ctrl Pts',(-43.6735798944926,32.9856281112839,
-46.0745334230522));
#257136=CARTESIAN_POINT('Ctrl Pts',(-44.5079524583201,33.4673533356141,
-46.0162000897188));
#257137=CARTESIAN_POINT('Ctrl Pts',(-45.3423250221477,32.9856281112839,
-45.9578667563855));
#257138=CARTESIAN_POINT('Ctrl Pts',(-46.1766975859751,32.5039028869536,
-45.8995334230521));
#257139=CARTESIAN_POINT('Ctrl Pts',(-46.1766975859751,31.5404524382932,
-45.8412000897188));
#257140=CARTESIAN_POINT('Ctrl Pts',(-46.1766975859751,30.5770019896326,
-45.7828667563855));
#257141=CARTESIAN_POINT('Ctrl Pts',(-45.3423250221477,30.0952767653024,
-45.7245334230521));
#257142=CARTESIAN_POINT('Ctrl Pts',(-44.5079524583202,29.6135515409722,
-45.6662000897188));
#257143=CARTESIAN_POINT('Ctrl Pts',(-43.6735798944927,30.0952767653024,
-45.6078667563855));
#257144=CARTESIAN_POINT('Ctrl Pts',(-42.8392073306652,30.5770019896326,
-45.5495334230521));
#257145=CARTESIAN_POINT('Ctrl Pts',(-42.8392073306652,31.5404524382931,
-45.4912000897188));
#257146=CARTESIAN_POINT('Ctrl Pts',(-42.8392073306652,32.5039028869536,
-45.4328667563854));
#257147=CARTESIAN_POINT('Ctrl Pts',(-43.6735798944926,32.9856281112839,
-45.3745334230521));
#257148=CARTESIAN_POINT('Ctrl Pts',(-44.5079524583201,33.4673533356141,
-45.3162000897188));
#257149=CARTESIAN_POINT('Ctrl Pts',(-45.3423250221477,32.9856281112839,
-45.2578667563855));
#257150=CARTESIAN_POINT('Ctrl Pts',(-46.1766975859751,32.5039028869536,
-45.1995334230521));
#257151=CARTESIAN_POINT('Ctrl Pts',(-46.1766975859751,31.5404524382932,
-45.1412000897188));
#257152=CARTESIAN_POINT('Ctrl Pts',(-46.1766975859751,30.5770019896326,
-45.0828667563855));
#257153=CARTESIAN_POINT('Ctrl Pts',(-45.3423250221477,30.0952767653024,
-45.0245334230521));
#257154=CARTESIAN_POINT('Ctrl Pts',(-44.5079524583202,29.6135515409722,
-44.9662000897188));
#257155=CARTESIAN_POINT('Ctrl Pts',(-43.6735798944927,30.0952767653024,
-44.9078667563854));
#257156=CARTESIAN_POINT('Ctrl Pts',(-42.8392073306652,30.5770019896326,
-44.8495334230521));
#257157=CARTESIAN_POINT('Ctrl Pts',(-42.8392073306652,31.5404524382931,
-44.7912000897188));
#257158=CARTESIAN_POINT('Ctrl Pts',(-42.8392073306652,32.5039028869536,
-44.7328667563854));
#257159=CARTESIAN_POINT('Ctrl Pts',(-43.6735798944926,32.9856281112839,
-44.6745334230521));
#257160=CARTESIAN_POINT('Ctrl Pts',(-44.5079524583201,33.4673533356141,
-44.6162000897188));
#257161=CARTESIAN_POINT('Ctrl Pts',(-45.3423250221477,32.9856281112839,
-44.5578667563855));
#257162=CARTESIAN_POINT('Ctrl Pts',(-46.1766975859751,32.5039028869536,
-44.4995334230521));
#257163=CARTESIAN_POINT('Ctrl Pts',(-46.1766975859751,31.5404524382932,
-44.4412000897188));
#257164=CARTESIAN_POINT('Ctrl Pts',(-46.1766975859751,30.5770019896326,
-44.3828667563854));
#257165=CARTESIAN_POINT('Ctrl Pts',(-45.3423250221477,30.0952767653024,
-44.3245334230521));
#257166=CARTESIAN_POINT('Ctrl Pts',(-44.5079524583202,29.6135515409722,
-44.2662000897188));
#257167=CARTESIAN_POINT('Ctrl Pts',(-43.6735798944927,30.0952767653024,
-44.2078667563855));
#257168=CARTESIAN_POINT('Ctrl Pts',(-42.8392073306652,30.5770019896326,
-44.1495334230521));
#257169=CARTESIAN_POINT('Ctrl Pts',(-42.8392073306652,31.5404524382931,
-44.0912000897188));
#257170=CARTESIAN_POINT('Ctrl Pts',(-42.8392073306652,32.5039028869536,
-44.0328667563854));
#257171=CARTESIAN_POINT('Ctrl Pts',(-43.6735798944926,32.9856281112839,
-43.9745334230521));
#257172=CARTESIAN_POINT('Ctrl Pts',(-44.5079524583201,33.4673533356141,
-43.9162000897188));
#257173=CARTESIAN_POINT('Ctrl Pts',(-45.3423250221477,32.9856281112839,
-43.8578667563855));
#257174=CARTESIAN_POINT('Ctrl Pts',(-46.1766975859751,32.5039028869536,
-43.7995334230521));
#257175=CARTESIAN_POINT('Ctrl Pts',(-46.1766975859751,31.5404524382932,
-43.7412000897188));
#257176=CARTESIAN_POINT('Ctrl Pts',(-46.1766975859751,30.5770019896326,
-43.6828667563854));
#257177=CARTESIAN_POINT('Ctrl Pts',(-45.3423250221477,30.0952767653024,
-43.6245334230521));
#257178=CARTESIAN_POINT('Ctrl Pts',(-44.5079524583202,29.6135515409722,
-43.5662000897188));
#257179=CARTESIAN_POINT('Ctrl Pts',(-43.6735798944927,30.0952767653024,
-43.5078667563854));
#257180=CARTESIAN_POINT('Ctrl Pts',(-42.8392073306652,30.5770019896326,
-43.4495334230521));
#257181=CARTESIAN_POINT('Ctrl Pts',(-42.8392073306652,31.5404524382931,
-43.3912000897188));
#257182=CARTESIAN_POINT('Ctrl Pts',(-42.8392073306652,32.5039028869536,
-43.3328667563854));
#257183=CARTESIAN_POINT('Ctrl Pts',(-43.6735798944926,32.9856281112839,
-43.2745334230521));
#257184=CARTESIAN_POINT('Ctrl Pts',(-44.5079524583201,33.4673533356141,
-43.2162000897188));
#257185=CARTESIAN_POINT('Ctrl Pts',(-45.3423250221477,32.9856281112839,
-43.1578667563855));
#257186=CARTESIAN_POINT('Ctrl Pts',(-46.1766975859751,32.5039028869536,
-43.0995334230521));
#257187=CARTESIAN_POINT('Ctrl Pts',(-46.1766975859751,31.5404524382932,
-43.0412000897188));
#257188=CARTESIAN_POINT('Ctrl Pts',(-46.1766975859751,30.5770019896326,
-42.9828667563854));
#257189=CARTESIAN_POINT('Ctrl Pts',(-45.3423250221477,30.0952767653024,
-42.9245334230521));
#257190=CARTESIAN_POINT('Ctrl Pts',(-44.5079524583202,29.6135515409722,
-42.8662000897187));
#257191=CARTESIAN_POINT('Ctrl Pts',(-43.6735798944927,30.0952767653024,
-42.8078667563855));
#257192=CARTESIAN_POINT('Ctrl Pts',(-42.8392073306652,30.5770019896326,
-42.7495334230521));
#257193=CARTESIAN_POINT('Ctrl Pts',(-42.8392073306652,31.5404524382931,
-42.6912000897188));
#257194=CARTESIAN_POINT('Ctrl Pts',(-42.8392073306652,32.5039028869536,
-42.6328667563855));
#257195=CARTESIAN_POINT('Ctrl Pts',(-43.6735798944926,32.9856281112839,
-42.5745334230521));
#257196=CARTESIAN_POINT('Ctrl Pts',(-44.5079524583201,33.4673533356141,
-42.5162000897188));
#257197=CARTESIAN_POINT('Ctrl Pts',(-45.3423250221477,32.9856281112839,
-42.4578667563855));
#257198=CARTESIAN_POINT('Ctrl Pts',(-46.1766975859751,32.5039028869536,
-42.3995334230521));
#257199=CARTESIAN_POINT('Ctrl Pts',(-46.1766975859751,31.5404524382932,
-42.3412000897188));
#257200=CARTESIAN_POINT('Ctrl Pts',(-46.1766975859751,30.5770019896326,
-42.2828667563854));
#257201=CARTESIAN_POINT('Ctrl Pts',(-45.3423250221477,30.0952767653024,
-42.2245334230521));
#257202=CARTESIAN_POINT('Ctrl Pts',(-44.5079524583202,29.6135515409722,
-42.1662000897188));
#257203=CARTESIAN_POINT('Ctrl Pts',(-43.6735798944927,30.0952767653024,
-42.1078667563855));
#257204=CARTESIAN_POINT('Ctrl Pts',(-42.8392073306652,30.5770019896326,
-42.0495334230521));
#257205=CARTESIAN_POINT('Ctrl Pts',(-42.8392073306652,31.5404524382931,
-41.9912000897188));
#257206=CARTESIAN_POINT('Ctrl Pts',(-42.8392073306652,32.5039028869536,
-41.9328667563855));
#257207=CARTESIAN_POINT('Ctrl Pts',(-43.6735798944926,32.9856281112839,
-41.8745334230521));
#257208=CARTESIAN_POINT('Ctrl Pts',(-44.5079524583201,33.4673533356141,
-41.8162000897188));
#257209=CARTESIAN_POINT('Ctrl Pts',(-45.3423250221477,32.9856281112839,
-41.7578667563855));
#257210=CARTESIAN_POINT('Ctrl Pts',(-46.1766975859751,32.5039028869536,
-41.6995334230521));
#257211=CARTESIAN_POINT('Ctrl Pts',(-46.1766975859751,31.5404524382932,
-41.6412000897188));
#257212=CARTESIAN_POINT('Ctrl Pts',(-46.1766975859751,30.5770019896326,
-41.5828667563854));
#257213=CARTESIAN_POINT('Ctrl Pts',(-45.3423250221477,30.0952767653024,
-41.5245334230521));
#257214=CARTESIAN_POINT('Ctrl Pts',(-44.5079524583202,29.6135515409722,
-41.4662000897188));
#257215=CARTESIAN_POINT('Ctrl Pts',(-43.6735798944927,30.0952767653024,
-41.4078667563855));
#257216=CARTESIAN_POINT('Ctrl Pts',(-42.8392073306652,30.5770019896326,
-41.3495334230521));
#257217=CARTESIAN_POINT('Ctrl Pts',(-42.8392073306652,31.5404524382931,
-41.2912000897188));
#257218=CARTESIAN_POINT('Ctrl Pts',(-42.8392073306652,32.5039028869536,
-41.2328667563855));
#257219=CARTESIAN_POINT('Ctrl Pts',(-43.6735798944926,32.9856281112839,
-41.1745334230521));
#257220=CARTESIAN_POINT('Ctrl Pts',(-44.5079524583201,33.4673533356141,
-41.1162000897188));
#257221=CARTESIAN_POINT('Ctrl Pts',(-45.3423250221477,32.9856281112839,
-41.0578667563855));
#257222=CARTESIAN_POINT('Ctrl Pts',(-46.1766975859751,32.5039028869536,
-40.9995334230521));
#257223=CARTESIAN_POINT('Ctrl Pts',(-46.1766975859751,31.5404524382932,
-40.9412000897188));
#257224=CARTESIAN_POINT('Ctrl Pts',(-46.1766975859751,30.5770019896326,
-40.8828667563855));
#257225=CARTESIAN_POINT('Ctrl Pts',(-45.3423250221477,30.0952767653024,
-40.8245334230521));
#257226=CARTESIAN_POINT('Ctrl Pts',(-44.5079524583202,29.6135515409722,
-40.7662000897188));
#257227=CARTESIAN_POINT('Ctrl Pts',(-43.6735798944927,30.0952767653024,
-40.7078667563855));
#257228=CARTESIAN_POINT('Ctrl Pts',(-42.8392073306652,30.5770019896326,
-40.6495334230521));
#257229=CARTESIAN_POINT('Ctrl Pts',(-42.8392073306652,31.5404524382931,
-40.5912000897188));
#257230=CARTESIAN_POINT('Ctrl Pts',(-42.8392073306652,32.5039028869536,
-40.5328667563855));
#257231=CARTESIAN_POINT('Ctrl Pts',(-43.6735798944926,32.9856281112839,
-40.4745334230521));
#257232=CARTESIAN_POINT('Ctrl Pts',(-44.5079524583201,33.4673533356141,
-40.4162000897188));
#257233=CARTESIAN_POINT('Ctrl Pts',(-45.3423250221477,32.9856281112839,
-40.3578667563855));
#257234=CARTESIAN_POINT('Ctrl Pts',(-46.1766975859751,32.5039028869536,
-40.2995334230521));
#257235=CARTESIAN_POINT('Ctrl Pts',(-46.1766975859751,31.5404524382932,
-40.2412000897188));
#257236=CARTESIAN_POINT('Ctrl Pts',(-46.1766975859751,30.5770019896326,
-40.1828667563855));
#257237=CARTESIAN_POINT('Ctrl Pts',(-45.3423250221477,30.0952767653024,
-40.1245334230521));
#257238=CARTESIAN_POINT('Ctrl Pts',(-44.5079524583202,29.6135515409722,
-40.0662000897188));
#257239=CARTESIAN_POINT('Ctrl Pts',(-43.6735798944927,30.0952767653024,
-40.0078667563855));
#257240=CARTESIAN_POINT('Ctrl Pts',(-42.8392073306652,30.5770019896326,
-39.9495334230521));
#257241=CARTESIAN_POINT('Ctrl Pts',(-42.8392073306652,31.5404524382931,
-39.8912000897188));
#257242=CARTESIAN_POINT('Ctrl Pts',(-42.8392073306652,32.5039028869536,
-39.8328667563854));
#257243=CARTESIAN_POINT('Ctrl Pts',(-43.6735798944926,32.9856281112839,
-39.7745334230521));
#257244=CARTESIAN_POINT('Ctrl Pts',(-44.5079524583201,33.4673533356141,
-39.7162000897188));
#257245=CARTESIAN_POINT('Ctrl Pts',(-45.3423250221477,32.9856281112839,
-39.6578667563855));
#257246=CARTESIAN_POINT('Ctrl Pts',(-46.1766975859751,32.5039028869536,
-39.5995334230521));
#257247=CARTESIAN_POINT('Ctrl Pts',(-46.1766975859751,31.5404524382932,
-39.5412000897188));
#257248=CARTESIAN_POINT('Ctrl Pts',(-46.1766975859751,30.5770019896326,
-39.4828667563854));
#257249=CARTESIAN_POINT('Ctrl Pts',(-45.3423250221477,30.0952767653024,
-39.4245334230521));
#257250=CARTESIAN_POINT('Ctrl Pts',(-44.5079524583202,29.6135515409722,
-39.3662000897187));
#257251=CARTESIAN_POINT('Ctrl Pts',(-43.6735798944927,30.0952767653024,
-39.3078667563854));
#257252=CARTESIAN_POINT('Ctrl Pts',(-42.8392073306652,30.5770019896326,
-39.2495334230521));
#257253=CARTESIAN_POINT('Ctrl Pts',(-42.8392073306652,31.5404524382931,
-39.1912000897188));
#257254=CARTESIAN_POINT('Ctrl Pts',(-42.8392073306652,32.5039028869536,
-39.1328667563854));
#257255=CARTESIAN_POINT('Ctrl Pts',(-43.6735798944926,32.9856281112839,
-39.0745334230521));
#257256=CARTESIAN_POINT('Ctrl Pts',(-44.5079524583201,33.4673533356141,
-39.0162000897188));
#257257=CARTESIAN_POINT('Ctrl Pts',(-45.3423250221477,32.9856281112839,
-38.9578667563855));
#257258=CARTESIAN_POINT('Ctrl Pts',(-46.1766975859751,32.5039028869536,
-38.8995334230521));
#257259=CARTESIAN_POINT('Ctrl Pts',(-46.1766975859751,31.5404524382932,
-38.8412000897188));
#257260=CARTESIAN_POINT('Ctrl Pts',(-46.1766975859751,30.5770019896326,
-38.7828667563854));
#257261=CARTESIAN_POINT('Ctrl Pts',(-45.3423250221477,30.0952767653024,
-38.7245334230521));
#257262=CARTESIAN_POINT('Ctrl Pts',(-44.5079524583202,29.6135515409722,
-38.6662000897187));
#257263=CARTESIAN_POINT('Ctrl Pts',(-43.6735798944927,30.0952767653024,
-38.6078667563855));
#257264=CARTESIAN_POINT('Ctrl Pts',(-42.8392073306652,30.5770019896326,
-38.5495334230521));
#257265=CARTESIAN_POINT('Ctrl Pts',(-42.8392073306652,31.5404524382931,
-38.4912000897188));
#257266=CARTESIAN_POINT('Ctrl Pts',(-42.8392073306652,32.5039028869536,
-38.4328667563854));
#257267=CARTESIAN_POINT('Ctrl Pts',(-43.6735798944926,32.9856281112839,
-38.3745334230521));
#257268=CARTESIAN_POINT('Ctrl Pts',(-44.5079524583201,33.4673533356141,
-38.3162000897187));
#257269=CARTESIAN_POINT('Ctrl Pts',(-45.3423250221477,32.9856281112839,
-38.2578667563855));
#257270=CARTESIAN_POINT('Ctrl Pts',(-46.1766975859751,32.5039028869536,
-38.1995334230521));
#257271=CARTESIAN_POINT('Ctrl Pts',(-46.1766975859751,31.5404524382932,
-38.1412000897188));
#257272=CARTESIAN_POINT('Ctrl Pts',(-46.1766975859751,30.5770019896326,
-38.0828667563854));
#257273=CARTESIAN_POINT('Ctrl Pts',(-45.3423250221477,30.0952767653024,
-38.0245334230521));
#257274=CARTESIAN_POINT('Ctrl Pts',(-44.5079524583202,29.6135515409722,
-37.9662000897188));
#257275=CARTESIAN_POINT('Ctrl Pts',(-43.6735798944927,30.0952767653024,
-37.9078667563855));
#257276=CARTESIAN_POINT('Ctrl Pts',(-42.8392073306652,30.5770019896326,
-37.8495334230521));
#257277=CARTESIAN_POINT('Ctrl Pts',(-42.8392073306652,31.5404524382931,
-37.7912000897188));
#257278=CARTESIAN_POINT('Ctrl Pts',(-42.8392073306652,32.5039028869536,
-37.7328667563854));
#257279=CARTESIAN_POINT('Ctrl Pts',(-43.6735798944926,32.9856281112839,
-37.6745334230521));
#257280=CARTESIAN_POINT('Ctrl Pts',(-44.5079524583201,33.4673533356141,
-37.6162000897188));
#257281=CARTESIAN_POINT('Ctrl Pts',(-45.3423250221477,32.9856281112839,
-37.5578667563855));
#257282=CARTESIAN_POINT('Ctrl Pts',(-46.1766975859751,32.5039028869536,
-37.4995334230521));
#257283=CARTESIAN_POINT('Ctrl Pts',(-46.1766975859751,31.5404524382932,
-37.4412000897188));
#257284=CARTESIAN_POINT('Ctrl Pts',(-46.1766975859751,30.5770019896326,
-37.3828667563855));
#257285=CARTESIAN_POINT('Ctrl Pts',(-45.3423250221477,30.0952767653024,
-37.3245334230521));
#257286=CARTESIAN_POINT('Ctrl Pts',(-44.5079524583202,29.6135515409722,
-37.2662000897188));
#257287=CARTESIAN_POINT('Ctrl Pts',(-43.6735798944927,30.0952767653024,
-37.2078667563855));
#257288=CARTESIAN_POINT('Ctrl Pts',(-42.8392073306652,30.5770019896326,
-37.1495334230521));
#257289=CARTESIAN_POINT('Ctrl Pts',(-42.8392073306652,31.5404524382931,
-37.0912000897188));
#257290=CARTESIAN_POINT('Ctrl Pts',(-42.8392073306652,32.5039028869536,
-37.0328667563855));
#257291=CARTESIAN_POINT('Ctrl Pts',(-43.6735798944926,32.9856281112839,
-36.9745334230521));
#257292=CARTESIAN_POINT('Ctrl Pts',(-44.5079524583201,33.4673533356141,
-36.9162000897188));
#257293=CARTESIAN_POINT('Ctrl Pts',(-45.3423250221477,32.9856281112839,
-36.8578667563855));
#257294=CARTESIAN_POINT('Ctrl Pts',(-45.4506435553405,32.9230903769867,
-36.8502939029902));
#257295=CARTESIAN_POINT('Ctrl Pts',(-45.5484296067563,32.8451047309192,
-36.8421539138368));
#257296=CARTESIAN_POINT('Ctrl Pts',(-46.5079524583201,31.5404524382926,
-52.64995));
#257297=CARTESIAN_POINT('Ctrl Pts',(-46.4950120245211,31.3925617663045,
-52.64995));
#257298=CARTESIAN_POINT('Ctrl Pts',(-46.4647658835106,31.2467042332267,
-52.64995));
#257299=CARTESIAN_POINT('Ctrl Pts',(-46.374803322878,30.9770256287474,-52.64995));
#257300=CARTESIAN_POINT('Ctrl Pts',(-46.318075281921,30.8531799156226,-52.64995));
#257301=CARTESIAN_POINT('Ctrl Pts',(-46.1241199408216,30.5276040394677,
-52.64995));
#257302=CARTESIAN_POINT('Ctrl Pts',(-45.9605617229685,30.3447545989436,
-52.6499500000001));
#257303=CARTESIAN_POINT('Ctrl Pts',(-45.6181630929711,30.0852600117117,
-52.6499500000001));
#257304=CARTESIAN_POINT('Ctrl Pts',(-45.4037244819514,29.9562168938456,
-52.6499500000282));
#257305=CARTESIAN_POINT('Ctrl Pts',(-44.9862869603902,29.8483847666303,
-52.6499500000282));
#257306=CARTESIAN_POINT('Ctrl Pts',(-44.8386017522404,29.8303377940401,
-52.64995));
#257307=CARTESIAN_POINT('Ctrl Pts',(-44.5503390053885,29.8332193714484,
-52.64995));
#257308=CARTESIAN_POINT('Ctrl Pts',(-44.4109642294216,29.8520756782854,
-52.64995));
#257309=CARTESIAN_POINT('Ctrl Pts',(-44.2755200796091,29.8879736913688,
-52.64995));
#257310=CARTESIAN_POINT('Ctrl Pts',(-44.5079524583208,29.5404524382925,
-40.5749499999997));
#257311=CARTESIAN_POINT('Ctrl Pts',(-44.3968299128524,29.5404524382925,
-40.568467851514));
#257312=CARTESIAN_POINT('Ctrl Pts',(-44.2856405135298,29.5497134444641,
-40.5619818032202));
#257313=CARTESIAN_POINT('Ctrl Pts',(-43.9253649275659,29.6104363327409,
-40.5409657273724));
#257314=CARTESIAN_POINT('Ctrl Pts',(-43.6855666100239,29.6998090325789,
-40.5272829764295));
#257315=CARTESIAN_POINT('Ctrl Pts',(-43.2423657182469,29.9692774273866,
-40.5007432393533));
#257316=CARTESIAN_POINT('Ctrl Pts',(-43.0454921814785,30.1506824820443,
-40.4858368470313));
#257317=CARTESIAN_POINT('Ctrl Pts',(-42.7368235400766,30.5756684261979,
-40.4553645085971));
#257318=CARTESIAN_POINT('Ctrl Pts',(-42.6264497148207,30.8140446972255,
-40.4401029441556));
#257319=CARTESIAN_POINT('Ctrl Pts',(-42.5046488178855,31.3138038931373,
-40.4113035086948));
#257320=CARTESIAN_POINT('Ctrl Pts',(-42.4920854562892,31.5698862113898,
-40.3989258478379));
#257321=CARTESIAN_POINT('Ctrl Pts',(-42.5653797870039,32.0862857493079,
-40.3707005479556));
#257322=CARTESIAN_POINT('Ctrl Pts',(-42.6556867547492,32.3408286617681,
-40.3552075580647));
#257323=CARTESIAN_POINT('Ctrl Pts',(-42.9257217377094,32.7905245969834,
-40.324613731669));
#257324=CARTESIAN_POINT('Ctrl Pts',(-43.0994167252046,32.9834335181717,
-40.309802226329));
#257325=CARTESIAN_POINT('Ctrl Pts',(-43.5123894580008,33.2943941768154,
-40.2820480315413));
#257326=CARTESIAN_POINT('Ctrl Pts',(-43.7482931115836,33.4087109993068,
-40.2692634618935));
#257327=CARTESIAN_POINT('Ctrl Pts',(-44.2549423409082,33.5418863052154,
-40.2397089235162));
#257328=CARTESIAN_POINT('Ctrl Pts',(-44.5211480844148,33.5577692603707,
-40.2241802551449));
#257329=CARTESIAN_POINT('Ctrl Pts',(-45.034518162743,33.4865628518253,-40.1942336672423));
#257330=CARTESIAN_POINT('Ctrl Pts',(-45.2774019700598,33.4039470825283,
-40.1800654451487));
#257331=CARTESIAN_POINT('Ctrl Pts',(-45.7285228007267,33.1468187134193,
-40.1537500633597));
#257332=CARTESIAN_POINT('Ctrl Pts',(-45.9304658971415,32.9711079469821,
-40.1390674255521));
#257333=CARTESIAN_POINT('Ctrl Pts',(-46.2515389935812,32.5543478314764,
-40.1086488441459));
#257334=CARTESIAN_POINT('Ctrl Pts',(-46.3688060858683,32.3184704964571,
-40.0933124677031));
#257335=CARTESIAN_POINT('Ctrl Pts',(-46.5042019275048,31.8220614198178,
-40.0642857548446));
#257336=CARTESIAN_POINT('Ctrl Pts',(-46.5237882527671,31.5669899543883,
-40.051752503518));
#257337=CARTESIAN_POINT('Ctrl Pts',(-46.4653120508861,31.0514704111867,
-40.0240038547637));
#257338=CARTESIAN_POINT('Ctrl Pts',(-46.3832833125564,30.7965049593682,
-40.0087309673246));
#257339=CARTESIAN_POINT('Ctrl Pts',(-46.1281397073777,30.3398162423274,
-39.9782182103898));
#257340=CARTESIAN_POINT('Ctrl Pts',(-45.9599378712318,30.141059404952,-39.9632714960655));
#257341=CARTESIAN_POINT('Ctrl Pts',(-45.5574367799837,29.8185237628238,
-39.9352379774211));
#257342=CARTESIAN_POINT('Ctrl Pts',(-45.3270340049066,29.6977457571994,
-39.9227297568837));
#257343=CARTESIAN_POINT('Ctrl Pts',(-44.8940104176252,29.5684904717941,
-39.8974700476257));
#257344=CARTESIAN_POINT('Ctrl Pts',(-44.7012947640528,29.5404524382925,
-39.8862283011673));
#257345=CARTESIAN_POINT('Ctrl Pts',(-44.5079524583208,29.5404524382925,
-39.8749499999996));
#257346=CARTESIAN_POINT('Ctrl Pts',(-46.1766977413726,31.5404524382932,
-52.99995));
#257347=CARTESIAN_POINT('Ctrl Pts',(-46.1766977413726,30.5770018999139,
-52.9416166666667));
#257348=CARTESIAN_POINT('Ctrl Pts',(-45.3423250998464,30.0952766307242,
-52.8832833333334));
#257349=CARTESIAN_POINT('Ctrl Pts',(-44.5079524583202,29.6135513615346,
-52.82495));
#257350=CARTESIAN_POINT('Ctrl Pts',(-43.6735798167939,30.0952766307242,
-52.7666166666667));
#257351=CARTESIAN_POINT('Ctrl Pts',(-42.8392071752677,30.5770018999139,
-52.7082833333333));
#257352=CARTESIAN_POINT('Ctrl Pts',(-42.8392071752677,31.5404524382931,
-52.64995));
#257353=CARTESIAN_POINT('Ctrl Pts',(-42.8392071752677,32.5039029766724,
-52.5916166666666));
#257354=CARTESIAN_POINT('Ctrl Pts',(-43.6735798167939,32.985628245862,-52.5332833333334));
#257355=CARTESIAN_POINT('Ctrl Pts',(-44.5079524583201,33.4673535150516,
-52.4749500000001));
#257356=CARTESIAN_POINT('Ctrl Pts',(-45.3423250998464,32.985628245862,-52.4166166666667));
#257357=CARTESIAN_POINT('Ctrl Pts',(-46.1766977413726,32.5039029766724,
-52.3582833333334));
#257358=CARTESIAN_POINT('Ctrl Pts',(-46.1766977413726,31.5404524382932,
-52.29995));
#257359=CARTESIAN_POINT('Ctrl Pts',(-46.1766977413726,30.5770018999139,
-52.2416166666667));
#257360=CARTESIAN_POINT('Ctrl Pts',(-45.3423250998464,30.0952766307242,
-52.1832833333333));
#257361=CARTESIAN_POINT('Ctrl Pts',(-44.5079524583202,29.6135513615346,
-52.12495));
#257362=CARTESIAN_POINT('Ctrl Pts',(-43.6735798167939,30.0952766307242,
-52.0666166666667));
#257363=CARTESIAN_POINT('Ctrl Pts',(-42.8392071752677,30.5770018999139,
-52.0082833333333));
#257364=CARTESIAN_POINT('Ctrl Pts',(-42.8392071752677,31.5404524382931,
-51.94995));
#257365=CARTESIAN_POINT('Ctrl Pts',(-42.8392071752677,32.5039029766724,
-51.8916166666667));
#257366=CARTESIAN_POINT('Ctrl Pts',(-43.6735798167939,32.985628245862,-51.8332833333333));
#257367=CARTESIAN_POINT('Ctrl Pts',(-44.5079524583201,33.4673535150516,
-51.77495));
#257368=CARTESIAN_POINT('Ctrl Pts',(-45.3423250998464,32.985628245862,-51.7166166666667));
#257369=CARTESIAN_POINT('Ctrl Pts',(-46.1766977413726,32.5039029766724,
-51.6582833333333));
#257370=CARTESIAN_POINT('Ctrl Pts',(-46.1766977413726,31.5404524382932,
-51.59995));
#257371=CARTESIAN_POINT('Ctrl Pts',(-46.1766977413726,30.5770018999139,
-51.5416166666667));
#257372=CARTESIAN_POINT('Ctrl Pts',(-45.3423250998464,30.0952766307242,
-51.4832833333333));
#257373=CARTESIAN_POINT('Ctrl Pts',(-44.5079524583202,29.6135513615346,
-51.42495));
#257374=CARTESIAN_POINT('Ctrl Pts',(-43.6735798167939,30.0952766307242,
-51.3666166666667));
#257375=CARTESIAN_POINT('Ctrl Pts',(-42.8392071752677,30.5770018999139,
-51.3082833333333));
#257376=CARTESIAN_POINT('Ctrl Pts',(-42.8392071752677,31.5404524382931,
-51.24995));
#257377=CARTESIAN_POINT('Ctrl Pts',(-42.8392071752677,32.5039029766724,
-51.1916166666667));
#257378=CARTESIAN_POINT('Ctrl Pts',(-43.6735798167939,32.985628245862,-51.1332833333333));
#257379=CARTESIAN_POINT('Ctrl Pts',(-44.5079524583201,33.4673535150516,
-51.07495));
#257380=CARTESIAN_POINT('Ctrl Pts',(-45.3423250998464,32.985628245862,-51.0166166666667));
#257381=CARTESIAN_POINT('Ctrl Pts',(-46.1766977413726,32.5039029766724,
-50.9582833333334));
#257382=CARTESIAN_POINT('Ctrl Pts',(-46.1766977413726,31.5404524382932,
-50.89995));
#257383=CARTESIAN_POINT('Ctrl Pts',(-46.1766977413726,30.5770018999139,
-50.8416166666667));
#257384=CARTESIAN_POINT('Ctrl Pts',(-45.3423250998464,30.0952766307242,
-50.7832833333333));
#257385=CARTESIAN_POINT('Ctrl Pts',(-44.5079524583202,29.6135513615346,
-50.72495));
#257386=CARTESIAN_POINT('Ctrl Pts',(-43.6735798167939,30.0952766307242,
-50.6666166666667));
#257387=CARTESIAN_POINT('Ctrl Pts',(-42.8392071752677,30.5770018999139,
-50.6082833333334));
#257388=CARTESIAN_POINT('Ctrl Pts',(-42.8392071752677,31.5404524382931,
-50.54995));
#257389=CARTESIAN_POINT('Ctrl Pts',(-42.8392071752677,32.5039029766724,
-50.4916166666667));
#257390=CARTESIAN_POINT('Ctrl Pts',(-43.6735798167939,32.985628245862,-50.4332833333333));
#257391=CARTESIAN_POINT('Ctrl Pts',(-44.5079524583201,33.4673535150516,
-50.37495));
#257392=CARTESIAN_POINT('Ctrl Pts',(-45.3423250998464,32.985628245862,-50.3166166666667));
#257393=CARTESIAN_POINT('Ctrl Pts',(-46.1766977413726,32.5039029766724,
-50.2582833333334));
#257394=CARTESIAN_POINT('Ctrl Pts',(-46.1766977413726,31.5404524382932,
-50.19995));
#257395=CARTESIAN_POINT('Ctrl Pts',(-46.1766977413726,30.5770018999139,
-50.1416166666667));
#257396=CARTESIAN_POINT('Ctrl Pts',(-45.3423250998464,30.0952766307242,
-50.0832833333333));
#257397=CARTESIAN_POINT('Ctrl Pts',(-44.5079524583202,29.6135513615346,
-50.02495));
#257398=CARTESIAN_POINT('Ctrl Pts',(-43.6735798167939,30.0952766307242,
-49.9666166666667));
#257399=CARTESIAN_POINT('Ctrl Pts',(-42.8392071752677,30.5770018999139,
-49.9082833333334));
#257400=CARTESIAN_POINT('Ctrl Pts',(-42.8392071752677,31.5404524382931,
-49.84995));
#257401=CARTESIAN_POINT('Ctrl Pts',(-42.8392071752677,32.5039029766724,
-49.7916166666667));
#257402=CARTESIAN_POINT('Ctrl Pts',(-43.6735798167939,32.985628245862,-49.7332833333333));
#257403=CARTESIAN_POINT('Ctrl Pts',(-44.5079524583201,33.4673535150516,
-49.67495));
#257404=CARTESIAN_POINT('Ctrl Pts',(-45.3423250998464,32.985628245862,-49.6166166666667));
#257405=CARTESIAN_POINT('Ctrl Pts',(-46.1766977413726,32.5039029766724,
-49.5582833333334));
#257406=CARTESIAN_POINT('Ctrl Pts',(-46.1766977413726,31.5404524382932,
-49.49995));
#257407=CARTESIAN_POINT('Ctrl Pts',(-46.1766977413726,30.5770018999139,
-49.4416166666667));
#257408=CARTESIAN_POINT('Ctrl Pts',(-45.3423250998464,30.0952766307242,
-49.3832833333334));
#257409=CARTESIAN_POINT('Ctrl Pts',(-44.5079524583202,29.6135513615346,
-49.32495));
#257410=CARTESIAN_POINT('Ctrl Pts',(-43.6735798167939,30.0952766307242,
-49.2666166666667));
#257411=CARTESIAN_POINT('Ctrl Pts',(-42.8392071752677,30.5770018999139,
-49.2082833333334));
#257412=CARTESIAN_POINT('Ctrl Pts',(-42.8392071752677,31.5404524382931,
-49.14995));
#257413=CARTESIAN_POINT('Ctrl Pts',(-42.8392071752677,32.5039029766724,
-49.0916166666667));
#257414=CARTESIAN_POINT('Ctrl Pts',(-43.6735798167939,32.985628245862,-49.0332833333333));
#257415=CARTESIAN_POINT('Ctrl Pts',(-44.5079524583201,33.4673535150516,
-48.97495));
#257416=CARTESIAN_POINT('Ctrl Pts',(-45.3423250998464,32.985628245862,-48.9166166666667));
#257417=CARTESIAN_POINT('Ctrl Pts',(-46.1766977413726,32.5039029766724,
-48.8582833333333));
#257418=CARTESIAN_POINT('Ctrl Pts',(-46.1766977413726,31.5404524382932,
-48.79995));
#257419=CARTESIAN_POINT('Ctrl Pts',(-46.1766977413726,30.5770018999139,
-48.7416166666667));
#257420=CARTESIAN_POINT('Ctrl Pts',(-45.3423250998464,30.0952766307242,
-48.6832833333333));
#257421=CARTESIAN_POINT('Ctrl Pts',(-44.5079524583202,29.6135513615346,
-48.62495));
#257422=CARTESIAN_POINT('Ctrl Pts',(-43.6735798167939,30.0952766307242,
-48.5666166666667));
#257423=CARTESIAN_POINT('Ctrl Pts',(-42.8392071752677,30.5770018999139,
-48.5082833333333));
#257424=CARTESIAN_POINT('Ctrl Pts',(-42.8392071752677,31.5404524382931,
-48.44995));
#257425=CARTESIAN_POINT('Ctrl Pts',(-42.8392071752677,32.5039029766724,
-48.3916166666667));
#257426=CARTESIAN_POINT('Ctrl Pts',(-43.6735798167939,32.985628245862,-48.3332833333333));
#257427=CARTESIAN_POINT('Ctrl Pts',(-44.5079524583201,33.4673535150516,
-48.27495));
#257428=CARTESIAN_POINT('Ctrl Pts',(-45.3423250998464,32.985628245862,-48.2166166666667));
#257429=CARTESIAN_POINT('Ctrl Pts',(-46.1766977413726,32.5039029766724,
-48.1582833333333));
#257430=CARTESIAN_POINT('Ctrl Pts',(-46.1766977413726,31.5404524382932,
-48.09995));
#257431=CARTESIAN_POINT('Ctrl Pts',(-46.1766977413726,30.5770018999139,
-48.0416166666667));
#257432=CARTESIAN_POINT('Ctrl Pts',(-45.3423250998464,30.0952766307242,
-47.9832833333334));
#257433=CARTESIAN_POINT('Ctrl Pts',(-44.5079524583202,29.6135513615346,
-47.92495));
#257434=CARTESIAN_POINT('Ctrl Pts',(-43.6735798167939,30.0952766307242,
-47.8666166666667));
#257435=CARTESIAN_POINT('Ctrl Pts',(-42.8392071752677,30.5770018999139,
-47.8082833333333));
#257436=CARTESIAN_POINT('Ctrl Pts',(-42.8392071752677,31.5404524382931,
-47.74995));
#257437=CARTESIAN_POINT('Ctrl Pts',(-42.8392071752677,32.5039029766724,
-47.6916166666667));
#257438=CARTESIAN_POINT('Ctrl Pts',(-43.6735798167939,32.985628245862,-47.6332833333333));
#257439=CARTESIAN_POINT('Ctrl Pts',(-44.5079524583201,33.4673535150516,
-47.57495));
#257440=CARTESIAN_POINT('Ctrl Pts',(-45.3423250998464,32.985628245862,-47.5166166666667));
#257441=CARTESIAN_POINT('Ctrl Pts',(-46.1766977413726,32.5039029766724,
-47.4582833333333));
#257442=CARTESIAN_POINT('Ctrl Pts',(-46.1766977413726,31.5404524382932,
-47.39995));
#257443=CARTESIAN_POINT('Ctrl Pts',(-46.1766977413726,30.5770018999139,
-47.3416166666666));
#257444=CARTESIAN_POINT('Ctrl Pts',(-45.3423250998464,30.0952766307242,
-47.2832833333333));
#257445=CARTESIAN_POINT('Ctrl Pts',(-44.5079524583202,29.6135513615346,
-47.22495));
#257446=CARTESIAN_POINT('Ctrl Pts',(-43.6735798167939,30.0952766307242,
-47.1666166666667));
#257447=CARTESIAN_POINT('Ctrl Pts',(-42.8392071752677,30.5770018999139,
-47.1082833333333));
#257448=CARTESIAN_POINT('Ctrl Pts',(-42.8392071752677,31.5404524382931,
-47.04995));
#257449=CARTESIAN_POINT('Ctrl Pts',(-42.8392071752677,32.5039029766724,
-46.9916166666667));
#257450=CARTESIAN_POINT('Ctrl Pts',(-43.6735798167939,32.985628245862,-46.9332833333333));
#257451=CARTESIAN_POINT('Ctrl Pts',(-44.5079524583201,33.4673535150516,
-46.87495));
#257452=CARTESIAN_POINT('Ctrl Pts',(-45.3423250998464,32.985628245862,-46.8166166666667));
#257453=CARTESIAN_POINT('Ctrl Pts',(-46.1766977413726,32.5039029766724,
-46.7582833333333));
#257454=CARTESIAN_POINT('Ctrl Pts',(-46.1766977413726,31.5404524382932,
-46.69995));
#257455=CARTESIAN_POINT('Ctrl Pts',(-46.1766977413726,30.5770018999139,
-46.6416166666666));
#257456=CARTESIAN_POINT('Ctrl Pts',(-45.3423250998464,30.0952766307242,
-46.5832833333334));
#257457=CARTESIAN_POINT('Ctrl Pts',(-44.5079524583202,29.6135513615346,
-46.52495));
#257458=CARTESIAN_POINT('Ctrl Pts',(-43.6735798167939,30.0952766307242,
-46.4666166666667));
#257459=CARTESIAN_POINT('Ctrl Pts',(-42.8392071752677,30.5770018999139,
-46.4082833333333));
#257460=CARTESIAN_POINT('Ctrl Pts',(-42.8392071752677,31.5404524382931,
-46.34995));
#257461=CARTESIAN_POINT('Ctrl Pts',(-42.8392071752677,32.5039029766724,
-46.2916166666667));
#257462=CARTESIAN_POINT('Ctrl Pts',(-43.6735798167939,32.985628245862,-46.2332833333334));
#257463=CARTESIAN_POINT('Ctrl Pts',(-44.5079524583201,33.4673535150516,
-46.17495));
#257464=CARTESIAN_POINT('Ctrl Pts',(-45.3423250998464,32.985628245862,-46.1166166666667));
#257465=CARTESIAN_POINT('Ctrl Pts',(-46.1766977413726,32.5039029766724,
-46.0582833333333));
#257466=CARTESIAN_POINT('Ctrl Pts',(-46.1766977413726,31.5404524382932,
-45.99995));
#257467=CARTESIAN_POINT('Ctrl Pts',(-46.1766977413726,30.5770018999139,
-45.9416166666667));
#257468=CARTESIAN_POINT('Ctrl Pts',(-45.3423250998464,30.0952766307242,
-45.8832833333333));
#257469=CARTESIAN_POINT('Ctrl Pts',(-44.5079524583202,29.6135513615346,
-45.82495));
#257470=CARTESIAN_POINT('Ctrl Pts',(-43.6735798167939,30.0952766307242,
-45.7666166666667));
#257471=CARTESIAN_POINT('Ctrl Pts',(-42.8392071752677,30.5770018999139,
-45.7082833333333));
#257472=CARTESIAN_POINT('Ctrl Pts',(-42.8392071752677,31.5404524382931,
-45.64995));
#257473=CARTESIAN_POINT('Ctrl Pts',(-42.8392071752677,32.5039029766724,
-45.5916166666667));
#257474=CARTESIAN_POINT('Ctrl Pts',(-43.6735798167939,32.985628245862,-45.5332833333333));
#257475=CARTESIAN_POINT('Ctrl Pts',(-44.5079524583201,33.4673535150516,
-45.47495));
#257476=CARTESIAN_POINT('Ctrl Pts',(-45.3423250998464,32.985628245862,-45.4166166666667));
#257477=CARTESIAN_POINT('Ctrl Pts',(-46.1766977413726,32.5039029766724,
-45.3582833333333));
#257478=CARTESIAN_POINT('Ctrl Pts',(-46.1766977413726,31.5404524382932,
-45.29995));
#257479=CARTESIAN_POINT('Ctrl Pts',(-46.1766977413726,30.5770018999139,
-45.2416166666667));
#257480=CARTESIAN_POINT('Ctrl Pts',(-45.3423250998464,30.0952766307242,
-45.1832833333333));
#257481=CARTESIAN_POINT('Ctrl Pts',(-44.5079524583202,29.6135513615346,
-45.12495));
#257482=CARTESIAN_POINT('Ctrl Pts',(-43.6735798167939,30.0952766307242,
-45.0666166666667));
#257483=CARTESIAN_POINT('Ctrl Pts',(-42.8392071752677,30.5770018999139,
-45.0082833333334));
#257484=CARTESIAN_POINT('Ctrl Pts',(-42.8392071752677,31.5404524382931,
-44.94995));
#257485=CARTESIAN_POINT('Ctrl Pts',(-42.8392071752677,32.5039029766724,
-44.8916166666667));
#257486=CARTESIAN_POINT('Ctrl Pts',(-43.6735798167939,32.985628245862,-44.8332833333334));
#257487=CARTESIAN_POINT('Ctrl Pts',(-44.5079524583201,33.4673535150516,
-44.77495));
#257488=CARTESIAN_POINT('Ctrl Pts',(-45.3423250998464,32.985628245862,-44.7166166666667));
#257489=CARTESIAN_POINT('Ctrl Pts',(-46.1766977413726,32.5039029766724,
-44.6582833333333));
#257490=CARTESIAN_POINT('Ctrl Pts',(-46.1766977413726,31.5404524382932,
-44.59995));
#257491=CARTESIAN_POINT('Ctrl Pts',(-46.1766977413726,30.5770018999139,
-44.5416166666667));
#257492=CARTESIAN_POINT('Ctrl Pts',(-45.3423250998464,30.0952766307242,
-44.4832833333334));
#257493=CARTESIAN_POINT('Ctrl Pts',(-44.5079524583202,29.6135513615346,
-44.42495));
#257494=CARTESIAN_POINT('Ctrl Pts',(-43.6735798167939,30.0952766307242,
-44.3666166666667));
#257495=CARTESIAN_POINT('Ctrl Pts',(-42.8392071752677,30.5770018999139,
-44.3082833333334));
#257496=CARTESIAN_POINT('Ctrl Pts',(-42.8392071752677,31.5404524382931,
-44.24995));
#257497=CARTESIAN_POINT('Ctrl Pts',(-42.8392071752677,32.5039029766724,
-44.1916166666667));
#257498=CARTESIAN_POINT('Ctrl Pts',(-43.6735798167939,32.985628245862,-44.1332833333334));
#257499=CARTESIAN_POINT('Ctrl Pts',(-44.5079524583201,33.4673535150516,
-44.07495));
#257500=CARTESIAN_POINT('Ctrl Pts',(-45.3423250998464,32.985628245862,-44.0166166666667));
#257501=CARTESIAN_POINT('Ctrl Pts',(-46.1766977413726,32.5039029766724,
-43.9582833333334));
#257502=CARTESIAN_POINT('Ctrl Pts',(-46.1766977413726,31.5404524382932,
-43.89995));
#257503=CARTESIAN_POINT('Ctrl Pts',(-46.1766977413726,30.5770018999139,
-43.8416166666667));
#257504=CARTESIAN_POINT('Ctrl Pts',(-45.3423250998464,30.0952766307242,
-43.7832833333334));
#257505=CARTESIAN_POINT('Ctrl Pts',(-44.5079524583202,29.6135513615346,
-43.72495));
#257506=CARTESIAN_POINT('Ctrl Pts',(-43.6735798167939,30.0952766307242,
-43.6666166666667));
#257507=CARTESIAN_POINT('Ctrl Pts',(-42.8392071752677,30.5770018999139,
-43.6082833333333));
#257508=CARTESIAN_POINT('Ctrl Pts',(-42.8392071752677,31.5404524382931,
-43.54995));
#257509=CARTESIAN_POINT('Ctrl Pts',(-42.8392071752677,32.5039029766724,
-43.4916166666667));
#257510=CARTESIAN_POINT('Ctrl Pts',(-43.6735798167939,32.985628245862,-43.4332833333333));
#257511=CARTESIAN_POINT('Ctrl Pts',(-44.5079524583201,33.4673535150516,
-43.37495));
#257512=CARTESIAN_POINT('Ctrl Pts',(-45.3423250998464,32.985628245862,-43.3166166666667));
#257513=CARTESIAN_POINT('Ctrl Pts',(-46.1766977413726,32.5039029766724,
-43.2582833333333));
#257514=CARTESIAN_POINT('Ctrl Pts',(-46.1766977413726,31.5404524382932,
-43.19995));
#257515=CARTESIAN_POINT('Ctrl Pts',(-46.1766977413726,30.5770018999139,
-43.1416166666666));
#257516=CARTESIAN_POINT('Ctrl Pts',(-45.3423250998464,30.0952766307242,
-43.0832833333333));
#257517=CARTESIAN_POINT('Ctrl Pts',(-44.5079524583202,29.6135513615346,
-43.02495));
#257518=CARTESIAN_POINT('Ctrl Pts',(-43.6735798167939,30.0952766307242,
-42.9666166666667));
#257519=CARTESIAN_POINT('Ctrl Pts',(-42.8392071752677,30.5770018999139,
-42.9082833333333));
#257520=CARTESIAN_POINT('Ctrl Pts',(-42.8392071752677,31.5404524382931,
-42.84995));
#257521=CARTESIAN_POINT('Ctrl Pts',(-42.8392071752677,32.5039029766724,
-42.7916166666667));
#257522=CARTESIAN_POINT('Ctrl Pts',(-43.6735798167939,32.985628245862,-42.7332833333334));
#257523=CARTESIAN_POINT('Ctrl Pts',(-44.5079524583201,33.4673535150516,
-42.67495));
#257524=CARTESIAN_POINT('Ctrl Pts',(-45.3423250998464,32.985628245862,-42.6166166666667));
#257525=CARTESIAN_POINT('Ctrl Pts',(-46.1766977413726,32.5039029766724,
-42.5582833333333));
#257526=CARTESIAN_POINT('Ctrl Pts',(-46.1766977413726,31.5404524382932,
-42.49995));
#257527=CARTESIAN_POINT('Ctrl Pts',(-46.1766977413726,30.5770018999139,
-42.4416166666667));
#257528=CARTESIAN_POINT('Ctrl Pts',(-45.3423250998464,30.0952766307242,
-42.3832833333333));
#257529=CARTESIAN_POINT('Ctrl Pts',(-44.5079524583202,29.6135513615346,
-42.32495));
#257530=CARTESIAN_POINT('Ctrl Pts',(-43.6735798167939,30.0952766307242,
-42.2666166666667));
#257531=CARTESIAN_POINT('Ctrl Pts',(-42.8392071752677,30.5770018999139,
-42.2082833333333));
#257532=CARTESIAN_POINT('Ctrl Pts',(-42.8392071752677,31.5404524382931,
-42.14995));
#257533=CARTESIAN_POINT('Ctrl Pts',(-42.8392071752677,32.5039029766724,
-42.0916166666667));
#257534=CARTESIAN_POINT('Ctrl Pts',(-43.6735798167939,32.985628245862,-42.0332833333334));
#257535=CARTESIAN_POINT('Ctrl Pts',(-44.5079524583201,33.4673535150516,
-41.97495));
#257536=CARTESIAN_POINT('Ctrl Pts',(-45.3423250998464,32.985628245862,-41.9166166666666));
#257537=CARTESIAN_POINT('Ctrl Pts',(-46.1766977413726,32.5039029766724,
-41.8582833333333));
#257538=CARTESIAN_POINT('Ctrl Pts',(-46.1766977413726,31.5404524382932,
-41.79995));
#257539=CARTESIAN_POINT('Ctrl Pts',(-46.1766977413726,30.5770018999139,
-41.7416166666667));
#257540=CARTESIAN_POINT('Ctrl Pts',(-45.3423250998464,30.0952766307242,
-41.6832833333333));
#257541=CARTESIAN_POINT('Ctrl Pts',(-44.5079524583202,29.6135513615346,
-41.62495));
#257542=CARTESIAN_POINT('Ctrl Pts',(-43.6735798167939,30.0952766307242,
-41.5666166666667));
#257543=CARTESIAN_POINT('Ctrl Pts',(-42.8392071752677,30.5770018999139,
-41.5082833333334));
#257544=CARTESIAN_POINT('Ctrl Pts',(-42.8392071752677,31.5404524382931,
-41.44995));
#257545=CARTESIAN_POINT('Ctrl Pts',(-42.8392071752677,32.5039029766724,
-41.3916166666667));
#257546=CARTESIAN_POINT('Ctrl Pts',(-43.6735798167939,32.985628245862,-41.3332833333334));
#257547=CARTESIAN_POINT('Ctrl Pts',(-44.5079524583201,33.4673535150516,
-41.27495));
#257548=CARTESIAN_POINT('Ctrl Pts',(-45.3423250998464,32.985628245862,-41.2166166666667));
#257549=CARTESIAN_POINT('Ctrl Pts',(-46.1766977413726,32.5039029766724,
-41.1582833333333));
#257550=CARTESIAN_POINT('Ctrl Pts',(-46.1766977413726,31.5404524382932,
-41.09995));
#257551=CARTESIAN_POINT('Ctrl Pts',(-46.1766977413726,30.5770018999139,
-41.0416166666667));
#257552=CARTESIAN_POINT('Ctrl Pts',(-45.3423250998464,30.0952766307242,
-40.9832833333333));
#257553=CARTESIAN_POINT('Ctrl Pts',(-44.5079524583202,29.6135513615346,
-40.92495));
#257554=CARTESIAN_POINT('Ctrl Pts',(-43.6735798167939,30.0952766307242,
-40.8666166666667));
#257555=CARTESIAN_POINT('Ctrl Pts',(-42.8392071752677,30.5770018999139,
-40.8082833333334));
#257556=CARTESIAN_POINT('Ctrl Pts',(-42.8392071752677,31.5404524382931,
-40.74995));
#257557=CARTESIAN_POINT('Ctrl Pts',(-42.8392071752677,32.5039029766724,
-40.6916166666667));
#257558=CARTESIAN_POINT('Ctrl Pts',(-43.6735798167939,32.985628245862,-40.6332833333334));
#257559=CARTESIAN_POINT('Ctrl Pts',(-44.5079524583201,33.4673535150516,
-40.57495));
#257560=CARTESIAN_POINT('Ctrl Pts',(-45.3423250998464,32.985628245862,-40.5166166666666));
#257561=CARTESIAN_POINT('Ctrl Pts',(-46.1766977413726,32.5039029766724,
-40.4582833333333));
#257562=CARTESIAN_POINT('Ctrl Pts',(-46.1766977413726,31.5404524382932,
-40.39995));
#257563=CARTESIAN_POINT('Ctrl Pts',(-46.1766977413726,30.5770018999139,
-40.3416166666667));
#257564=CARTESIAN_POINT('Ctrl Pts',(-45.3423250998464,30.0952766307242,
-40.2832833333334));
#257565=CARTESIAN_POINT('Ctrl Pts',(-44.5079524583202,29.6135513615346,
-40.22495));
#257566=CARTESIAN_POINT('Ctrl Pts',(-43.6735798167939,30.0952766307242,
-40.1666166666667));
#257567=CARTESIAN_POINT('Ctrl Pts',(-42.8392071752677,30.5770018999139,
-40.1082833333334));
#257568=CARTESIAN_POINT('Ctrl Pts',(-42.8392071752677,31.5404524382931,
-40.04995));
#257569=CARTESIAN_POINT('Ctrl Pts',(-42.8392071752677,32.5039029766724,
-39.9916166666667));
#257570=CARTESIAN_POINT('Ctrl Pts',(-43.6735798167939,32.985628245862,-39.9332833333333));
#257571=CARTESIAN_POINT('Ctrl Pts',(-44.5079524583201,33.4673535150516,
-39.87495));
#257572=CARTESIAN_POINT('Ctrl Pts',(-45.3423250998464,32.985628245862,-39.8166166666667));
#257573=CARTESIAN_POINT('Ctrl Pts',(-46.1766977413726,32.5039029766724,
-39.7582833333334));
#257574=CARTESIAN_POINT('Ctrl Pts',(-46.1766977413726,31.5404524382932,
-39.69995));
#257575=CARTESIAN_POINT('Ctrl Pts',(-46.1766977413726,30.5770018999139,
-39.6416166666667));
#257576=CARTESIAN_POINT('Ctrl Pts',(-45.3423250998464,30.0952766307242,
-39.5832833333333));
#257577=CARTESIAN_POINT('Ctrl Pts',(-44.5079524583202,29.6135513615346,
-39.52495));
#257578=CARTESIAN_POINT('Ctrl Pts',(-43.6735798167939,30.0952766307242,
-39.4666166666667));
#257579=CARTESIAN_POINT('Ctrl Pts',(-42.8392071752677,30.5770018999139,
-39.4082833333333));
#257580=CARTESIAN_POINT('Ctrl Pts',(-42.8392071752677,31.5404524382931,
-39.34995));
#257581=CARTESIAN_POINT('Ctrl Pts',(-42.8392071752677,32.5039029766724,
-39.2916166666667));
#257582=CARTESIAN_POINT('Ctrl Pts',(-43.6735798167939,32.985628245862,-39.2332833333333));
#257583=CARTESIAN_POINT('Ctrl Pts',(-44.5079524583201,33.4673535150516,
-39.17495));
#257584=CARTESIAN_POINT('Ctrl Pts',(-45.3423250998464,32.985628245862,-39.1166166666667));
#257585=CARTESIAN_POINT('Ctrl Pts',(-46.1766977413726,32.5039029766724,
-39.0582833333333));
#257586=CARTESIAN_POINT('Ctrl Pts',(-46.1766977413726,31.5404524382932,
-38.99995));
#257587=CARTESIAN_POINT('Ctrl Pts',(-46.1766977413726,30.5770018999139,
-38.9416166666667));
#257588=CARTESIAN_POINT('Ctrl Pts',(-45.3423250998464,30.0952766307242,
-38.8832833333334));
#257589=CARTESIAN_POINT('Ctrl Pts',(-44.5079524583202,29.6135513615346,
-38.82495));
#257590=CARTESIAN_POINT('Ctrl Pts',(-43.6735798167939,30.0952766307242,
-38.7666166666667));
#257591=CARTESIAN_POINT('Ctrl Pts',(-42.8392071752677,30.5770018999139,
-38.7082833333333));
#257592=CARTESIAN_POINT('Ctrl Pts',(-42.8392071752677,31.5404524382931,
-38.64995));
#257593=CARTESIAN_POINT('Ctrl Pts',(-42.8392071752677,32.5039029766724,
-38.5916166666667));
#257594=CARTESIAN_POINT('Ctrl Pts',(-43.6735798167939,32.985628245862,-38.5332833333334));
#257595=CARTESIAN_POINT('Ctrl Pts',(-44.5079524583201,33.4673535150516,
-38.47495));
#257596=CARTESIAN_POINT('Ctrl Pts',(-45.3423250998464,32.985628245862,-38.4166166666667));
#257597=CARTESIAN_POINT('Ctrl Pts',(-46.1766977413726,32.5039029766724,
-38.3582833333333));
#257598=CARTESIAN_POINT('Ctrl Pts',(-46.1766977413726,31.5404524382932,
-38.29995));
#257599=CARTESIAN_POINT('Ctrl Pts',(-46.1766977413726,30.5770018999139,
-38.2416166666667));
#257600=CARTESIAN_POINT('Ctrl Pts',(-45.3423250998464,30.0952766307242,
-38.1832833333333));
#257601=CARTESIAN_POINT('Ctrl Pts',(-44.5079524583202,29.6135513615346,
-38.12495));
#257602=CARTESIAN_POINT('Ctrl Pts',(-43.6735798167939,30.0952766307242,
-38.0666166666667));
#257603=CARTESIAN_POINT('Ctrl Pts',(-42.8392071752677,30.5770018999139,
-38.0082833333333));
#257604=CARTESIAN_POINT('Ctrl Pts',(-42.8392071752677,31.5404524382931,
-37.94995));
#257605=CARTESIAN_POINT('Ctrl Pts',(-42.8392071752677,32.5039029766724,
-37.8916166666667));
#257606=CARTESIAN_POINT('Ctrl Pts',(-43.6735798167939,32.985628245862,-37.8332833333334));
#257607=CARTESIAN_POINT('Ctrl Pts',(-44.5079524583201,33.4673535150516,
-37.77495));
#257608=CARTESIAN_POINT('Ctrl Pts',(-45.3423250998464,32.985628245862,-37.7166166666667));
#257609=CARTESIAN_POINT('Ctrl Pts',(-46.1766977413726,32.5039029766724,
-37.6582833333333));
#257610=CARTESIAN_POINT('Ctrl Pts',(-46.1766977413726,31.5404524382932,
-37.59995));
#257611=CARTESIAN_POINT('Ctrl Pts',(-46.1766977413726,30.5770018999139,
-37.5416166666667));
#257612=CARTESIAN_POINT('Ctrl Pts',(-45.3423250998464,30.0952766307242,
-37.4832833333334));
#257613=CARTESIAN_POINT('Ctrl Pts',(-44.5079524583202,29.6135513615346,
-37.42495));
#257614=CARTESIAN_POINT('Ctrl Pts',(-43.6735798167939,30.0952766307242,
-37.3666166666667));
#257615=CARTESIAN_POINT('Ctrl Pts',(-42.8392071752677,30.5770018999139,
-37.3082833333333));
#257616=CARTESIAN_POINT('Ctrl Pts',(-42.8392071752677,31.5404524382931,
-37.24995));
#257617=CARTESIAN_POINT('Ctrl Pts',(-42.8392071752677,32.5039029766724,
-37.1916166666667));
#257618=CARTESIAN_POINT('Ctrl Pts',(-43.6735798167939,32.985628245862,-37.1332833333334));
#257619=CARTESIAN_POINT('Ctrl Pts',(-44.5079524583201,33.4673535150516,
-37.07495));
#257620=CARTESIAN_POINT('Ctrl Pts',(-45.3423250998464,32.985628245862,-37.0166166666667));
#257621=CARTESIAN_POINT('Ctrl Pts',(-45.4506530446704,32.9230850777571,
-37.0090431559831));
#257622=CARTESIAN_POINT('Ctrl Pts',(-45.5484465834729,32.8450913903532,
-37.0009024189827));
#257623=CARTESIAN_POINT('Ctrl Pts',(-46.5766932247455,31.5404524382932,
-53.2308875));
#257624=CARTESIAN_POINT('Ctrl Pts',(-46.5766932247455,30.3460643999139,
-53.1725541666667));
#257625=CARTESIAN_POINT('Ctrl Pts',(-45.5423228415329,29.7488703807243,
-53.1142208333334));
#257626=CARTESIAN_POINT('Ctrl Pts',(-44.5079524583202,29.1516763615346,
-53.0558875000001));
#257627=CARTESIAN_POINT('Ctrl Pts',(-43.4735820751074,29.7488703807243,
-52.9975541666667));
#257628=CARTESIAN_POINT('Ctrl Pts',(-42.4392116918948,30.3460643999138,
-52.9392208333334));
#257629=CARTESIAN_POINT('Ctrl Pts',(-42.4392116918948,31.5404524382931,
-52.8808875));
#257630=CARTESIAN_POINT('Ctrl Pts',(-42.4392116918947,32.7348404766723,
-52.8225541666667));
#257631=CARTESIAN_POINT('Ctrl Pts',(-43.4735820751074,33.332034495862,-52.7642208333334));
#257632=CARTESIAN_POINT('Ctrl Pts',(-44.5079524583201,33.9292285150516,
-52.7058875));
#257633=CARTESIAN_POINT('Ctrl Pts',(-45.5423228415328,33.332034495862,-52.6475541666667));
#257634=CARTESIAN_POINT('Ctrl Pts',(-46.5766932247455,32.7348404766724,
-52.5892208333333));
#257635=CARTESIAN_POINT('Ctrl Pts',(-46.5766932247455,31.5404524382932,
-52.5308875));
#257636=CARTESIAN_POINT('Ctrl Pts',(-46.5766932247455,30.3460643999139,
-52.4725541666667));
#257637=CARTESIAN_POINT('Ctrl Pts',(-45.5423228415329,29.7488703807243,
-52.4142208333333));
#257638=CARTESIAN_POINT('Ctrl Pts',(-44.5079524583202,29.1516763615346,
-52.3558875000001));
#257639=CARTESIAN_POINT('Ctrl Pts',(-43.4735820751074,29.7488703807243,
-52.2975541666667));
#257640=CARTESIAN_POINT('Ctrl Pts',(-42.4392116918948,30.3460643999138,
-52.2392208333334));
#257641=CARTESIAN_POINT('Ctrl Pts',(-42.4392116918948,31.5404524382931,
-52.1808875));
#257642=CARTESIAN_POINT('Ctrl Pts',(-42.4392116918947,32.7348404766723,
-52.1225541666667));
#257643=CARTESIAN_POINT('Ctrl Pts',(-43.4735820751074,33.332034495862,-52.0642208333334));
#257644=CARTESIAN_POINT('Ctrl Pts',(-44.5079524583201,33.9292285150516,
-52.0058875));
#257645=CARTESIAN_POINT('Ctrl Pts',(-45.5423228415328,33.332034495862,-51.9475541666667));
#257646=CARTESIAN_POINT('Ctrl Pts',(-46.5766932247455,32.7348404766724,
-51.8892208333334));
#257647=CARTESIAN_POINT('Ctrl Pts',(-46.5766932247455,31.5404524382932,
-51.8308875));
#257648=CARTESIAN_POINT('Ctrl Pts',(-46.5766932247455,30.3460643999139,
-51.7725541666667));
#257649=CARTESIAN_POINT('Ctrl Pts',(-45.5423228415329,29.7488703807243,
-51.7142208333334));
#257650=CARTESIAN_POINT('Ctrl Pts',(-44.5079524583202,29.1516763615346,
-51.6558875));
#257651=CARTESIAN_POINT('Ctrl Pts',(-43.4735820751074,29.7488703807243,
-51.5975541666667));
#257652=CARTESIAN_POINT('Ctrl Pts',(-42.4392116918948,30.3460643999138,
-51.5392208333333));
#257653=CARTESIAN_POINT('Ctrl Pts',(-42.4392116918948,31.5404524382931,
-51.4808875));
#257654=CARTESIAN_POINT('Ctrl Pts',(-42.4392116918947,32.7348404766723,
-51.4225541666667));
#257655=CARTESIAN_POINT('Ctrl Pts',(-43.4735820751074,33.332034495862,-51.3642208333334));
#257656=CARTESIAN_POINT('Ctrl Pts',(-44.5079524583201,33.9292285150516,
-51.3058875));
#257657=CARTESIAN_POINT('Ctrl Pts',(-45.5423228415328,33.332034495862,-51.2475541666667));
#257658=CARTESIAN_POINT('Ctrl Pts',(-46.5766932247455,32.7348404766724,
-51.1892208333333));
#257659=CARTESIAN_POINT('Ctrl Pts',(-46.5766932247455,31.5404524382932,
-51.1308875));
#257660=CARTESIAN_POINT('Ctrl Pts',(-46.5766932247455,30.3460643999139,
-51.0725541666667));
#257661=CARTESIAN_POINT('Ctrl Pts',(-45.5423228415329,29.7488703807243,
-51.0142208333334));
#257662=CARTESIAN_POINT('Ctrl Pts',(-44.5079524583202,29.1516763615346,
-50.9558875));
#257663=CARTESIAN_POINT('Ctrl Pts',(-43.4735820751074,29.7488703807243,
-50.8975541666667));
#257664=CARTESIAN_POINT('Ctrl Pts',(-42.4392116918948,30.3460643999138,
-50.8392208333333));
#257665=CARTESIAN_POINT('Ctrl Pts',(-42.4392116918948,31.5404524382931,
-50.7808875));
#257666=CARTESIAN_POINT('Ctrl Pts',(-42.4392116918947,32.7348404766723,
-50.7225541666666));
#257667=CARTESIAN_POINT('Ctrl Pts',(-43.4735820751074,33.332034495862,-50.6642208333333));
#257668=CARTESIAN_POINT('Ctrl Pts',(-44.5079524583201,33.9292285150516,
-50.6058875));
#257669=CARTESIAN_POINT('Ctrl Pts',(-45.5423228415328,33.332034495862,-50.5475541666667));
#257670=CARTESIAN_POINT('Ctrl Pts',(-46.5766932247455,32.7348404766724,
-50.4892208333333));
#257671=CARTESIAN_POINT('Ctrl Pts',(-46.5766932247455,31.5404524382932,
-50.4308875));
#257672=CARTESIAN_POINT('Ctrl Pts',(-46.5766932247455,30.3460643999139,
-50.3725541666667));
#257673=CARTESIAN_POINT('Ctrl Pts',(-45.5423228415329,29.7488703807243,
-50.3142208333334));
#257674=CARTESIAN_POINT('Ctrl Pts',(-44.5079524583202,29.1516763615346,
-50.2558875));
#257675=CARTESIAN_POINT('Ctrl Pts',(-43.4735820751074,29.7488703807243,
-50.1975541666667));
#257676=CARTESIAN_POINT('Ctrl Pts',(-42.4392116918948,30.3460643999138,
-50.1392208333333));
#257677=CARTESIAN_POINT('Ctrl Pts',(-42.4392116918948,31.5404524382931,
-50.0808875));
#257678=CARTESIAN_POINT('Ctrl Pts',(-42.4392116918947,32.7348404766723,
-50.0225541666667));
#257679=CARTESIAN_POINT('Ctrl Pts',(-43.4735820751074,33.332034495862,-49.9642208333334));
#257680=CARTESIAN_POINT('Ctrl Pts',(-44.5079524583201,33.9292285150516,
-49.9058875));
#257681=CARTESIAN_POINT('Ctrl Pts',(-45.5423228415328,33.332034495862,-49.8475541666667));
#257682=CARTESIAN_POINT('Ctrl Pts',(-46.5766932247455,32.7348404766724,
-49.7892208333333));
#257683=CARTESIAN_POINT('Ctrl Pts',(-46.5766932247455,31.5404524382932,
-49.7308875));
#257684=CARTESIAN_POINT('Ctrl Pts',(-46.5766932247455,30.3460643999139,
-49.6725541666667));
#257685=CARTESIAN_POINT('Ctrl Pts',(-45.5423228415329,29.7488703807243,
-49.6142208333334));
#257686=CARTESIAN_POINT('Ctrl Pts',(-44.5079524583202,29.1516763615346,
-49.5558875));
#257687=CARTESIAN_POINT('Ctrl Pts',(-43.4735820751074,29.7488703807243,
-49.4975541666667));
#257688=CARTESIAN_POINT('Ctrl Pts',(-42.4392116918948,30.3460643999138,
-49.4392208333333));
#257689=CARTESIAN_POINT('Ctrl Pts',(-42.4392116918948,31.5404524382931,
-49.3808875));
#257690=CARTESIAN_POINT('Ctrl Pts',(-42.4392116918947,32.7348404766723,
-49.3225541666667));
#257691=CARTESIAN_POINT('Ctrl Pts',(-43.4735820751074,33.332034495862,-49.2642208333334));
#257692=CARTESIAN_POINT('Ctrl Pts',(-44.5079524583201,33.9292285150516,
-49.2058875));
#257693=CARTESIAN_POINT('Ctrl Pts',(-45.5423228415328,33.332034495862,-49.1475541666667));
#257694=CARTESIAN_POINT('Ctrl Pts',(-46.5766932247455,32.7348404766724,
-49.0892208333333));
#257695=CARTESIAN_POINT('Ctrl Pts',(-46.5766932247455,31.5404524382932,
-49.0308875));
#257696=CARTESIAN_POINT('Ctrl Pts',(-46.5766932247455,30.3460643999139,
-48.9725541666667));
#257697=CARTESIAN_POINT('Ctrl Pts',(-45.5423228415329,29.7488703807243,
-48.9142208333333));
#257698=CARTESIAN_POINT('Ctrl Pts',(-44.5079524583202,29.1516763615346,
-48.8558875));
#257699=CARTESIAN_POINT('Ctrl Pts',(-43.4735820751074,29.7488703807243,
-48.7975541666667));
#257700=CARTESIAN_POINT('Ctrl Pts',(-42.4392116918948,30.3460643999138,
-48.7392208333334));
#257701=CARTESIAN_POINT('Ctrl Pts',(-42.4392116918948,31.5404524382931,
-48.6808875));
#257702=CARTESIAN_POINT('Ctrl Pts',(-42.4392116918947,32.7348404766723,
-48.6225541666667));
#257703=CARTESIAN_POINT('Ctrl Pts',(-43.4735820751074,33.332034495862,-48.5642208333334));
#257704=CARTESIAN_POINT('Ctrl Pts',(-44.5079524583201,33.9292285150516,
-48.5058875));
#257705=CARTESIAN_POINT('Ctrl Pts',(-45.5423228415328,33.332034495862,-48.4475541666667));
#257706=CARTESIAN_POINT('Ctrl Pts',(-46.5766932247455,32.7348404766724,
-48.3892208333334));
#257707=CARTESIAN_POINT('Ctrl Pts',(-46.5766932247455,31.5404524382932,
-48.3308875));
#257708=CARTESIAN_POINT('Ctrl Pts',(-46.5766932247455,30.3460643999139,
-48.2725541666667));
#257709=CARTESIAN_POINT('Ctrl Pts',(-45.5423228415329,29.7488703807243,
-48.2142208333334));
#257710=CARTESIAN_POINT('Ctrl Pts',(-44.5079524583202,29.1516763615346,
-48.1558875));
#257711=CARTESIAN_POINT('Ctrl Pts',(-43.4735820751074,29.7488703807243,
-48.0975541666667));
#257712=CARTESIAN_POINT('Ctrl Pts',(-42.4392116918948,30.3460643999138,
-48.0392208333334));
#257713=CARTESIAN_POINT('Ctrl Pts',(-42.4392116918948,31.5404524382931,
-47.9808875));
#257714=CARTESIAN_POINT('Ctrl Pts',(-42.4392116918947,32.7348404766723,
-47.9225541666667));
#257715=CARTESIAN_POINT('Ctrl Pts',(-43.4735820751074,33.332034495862,-47.8642208333334));
#257716=CARTESIAN_POINT('Ctrl Pts',(-44.5079524583201,33.9292285150516,
-47.8058875000001));
#257717=CARTESIAN_POINT('Ctrl Pts',(-45.5423228415328,33.332034495862,-47.7475541666667));
#257718=CARTESIAN_POINT('Ctrl Pts',(-46.5766932247455,32.7348404766724,
-47.6892208333334));
#257719=CARTESIAN_POINT('Ctrl Pts',(-46.5766932247455,31.5404524382932,
-47.6308875));
#257720=CARTESIAN_POINT('Ctrl Pts',(-46.5766932247455,30.3460643999139,
-47.5725541666667));
#257721=CARTESIAN_POINT('Ctrl Pts',(-45.5423228415329,29.7488703807243,
-47.5142208333333));
#257722=CARTESIAN_POINT('Ctrl Pts',(-44.5079524583202,29.1516763615346,
-47.4558875));
#257723=CARTESIAN_POINT('Ctrl Pts',(-43.4735820751074,29.7488703807243,
-47.3975541666667));
#257724=CARTESIAN_POINT('Ctrl Pts',(-42.4392116918948,30.3460643999138,
-47.3392208333333));
#257725=CARTESIAN_POINT('Ctrl Pts',(-42.4392116918948,31.5404524382931,
-47.2808875));
#257726=CARTESIAN_POINT('Ctrl Pts',(-42.4392116918947,32.7348404766723,
-47.2225541666667));
#257727=CARTESIAN_POINT('Ctrl Pts',(-43.4735820751074,33.332034495862,-47.1642208333334));
#257728=CARTESIAN_POINT('Ctrl Pts',(-44.5079524583201,33.9292285150516,
-47.1058875));
#257729=CARTESIAN_POINT('Ctrl Pts',(-45.5423228415328,33.332034495862,-47.0475541666667));
#257730=CARTESIAN_POINT('Ctrl Pts',(-46.5766932247455,32.7348404766724,
-46.9892208333334));
#257731=CARTESIAN_POINT('Ctrl Pts',(-46.5766932247455,31.5404524382932,
-46.9308875));
#257732=CARTESIAN_POINT('Ctrl Pts',(-46.5766932247455,30.3460643999139,
-46.8725541666667));
#257733=CARTESIAN_POINT('Ctrl Pts',(-45.5423228415329,29.7488703807243,
-46.8142208333334));
#257734=CARTESIAN_POINT('Ctrl Pts',(-44.5079524583202,29.1516763615346,
-46.7558875));
#257735=CARTESIAN_POINT('Ctrl Pts',(-43.4735820751074,29.7488703807243,
-46.6975541666667));
#257736=CARTESIAN_POINT('Ctrl Pts',(-42.4392116918948,30.3460643999138,
-46.6392208333333));
#257737=CARTESIAN_POINT('Ctrl Pts',(-42.4392116918948,31.5404524382931,
-46.5808875));
#257738=CARTESIAN_POINT('Ctrl Pts',(-42.4392116918948,32.7348404766723,
-46.5225541666667));
#257739=CARTESIAN_POINT('Ctrl Pts',(-43.4735820751074,33.332034495862,-46.4642208333334));
#257740=CARTESIAN_POINT('Ctrl Pts',(-44.5079524583201,33.9292285150516,
-46.4058875));
#257741=CARTESIAN_POINT('Ctrl Pts',(-45.5423228415328,33.332034495862,-46.3475541666667));
#257742=CARTESIAN_POINT('Ctrl Pts',(-46.5766932247455,32.7348404766724,
-46.2892208333334));
#257743=CARTESIAN_POINT('Ctrl Pts',(-46.5766932247455,31.5404524382932,
-46.2308875));
#257744=CARTESIAN_POINT('Ctrl Pts',(-46.5766932247455,30.3460643999139,
-46.1725541666667));
#257745=CARTESIAN_POINT('Ctrl Pts',(-45.5423228415329,29.7488703807243,
-46.1142208333334));
#257746=CARTESIAN_POINT('Ctrl Pts',(-44.5079524583202,29.1516763615346,
-46.0558875));
#257747=CARTESIAN_POINT('Ctrl Pts',(-43.4735820751074,29.7488703807243,
-45.9975541666667));
#257748=CARTESIAN_POINT('Ctrl Pts',(-42.4392116918948,30.3460643999138,
-45.9392208333333));
#257749=CARTESIAN_POINT('Ctrl Pts',(-42.4392116918948,31.5404524382931,
-45.8808875));
#257750=CARTESIAN_POINT('Ctrl Pts',(-42.4392116918948,32.7348404766723,
-45.8225541666667));
#257751=CARTESIAN_POINT('Ctrl Pts',(-43.4735820751074,33.332034495862,-45.7642208333334));
#257752=CARTESIAN_POINT('Ctrl Pts',(-44.5079524583201,33.9292285150516,
-45.7058875));
#257753=CARTESIAN_POINT('Ctrl Pts',(-45.5423228415328,33.332034495862,-45.6475541666667));
#257754=CARTESIAN_POINT('Ctrl Pts',(-46.5766932247455,32.7348404766724,
-45.5892208333333));
#257755=CARTESIAN_POINT('Ctrl Pts',(-46.5766932247455,31.5404524382932,
-45.5308875));
#257756=CARTESIAN_POINT('Ctrl Pts',(-46.5766932247455,30.3460643999139,
-45.4725541666667));
#257757=CARTESIAN_POINT('Ctrl Pts',(-45.5423228415329,29.7488703807243,
-45.4142208333334));
#257758=CARTESIAN_POINT('Ctrl Pts',(-44.5079524583202,29.1516763615346,
-45.3558875));
#257759=CARTESIAN_POINT('Ctrl Pts',(-43.4735820751074,29.7488703807243,
-45.2975541666667));
#257760=CARTESIAN_POINT('Ctrl Pts',(-42.4392116918948,30.3460643999138,
-45.2392208333333));
#257761=CARTESIAN_POINT('Ctrl Pts',(-42.4392116918948,31.5404524382931,
-45.1808875));
#257762=CARTESIAN_POINT('Ctrl Pts',(-42.4392116918948,32.7348404766723,
-45.1225541666667));
#257763=CARTESIAN_POINT('Ctrl Pts',(-43.4735820751074,33.332034495862,-45.0642208333334));
#257764=CARTESIAN_POINT('Ctrl Pts',(-44.5079524583201,33.9292285150516,
-45.0058875));
#257765=CARTESIAN_POINT('Ctrl Pts',(-45.5423228415328,33.332034495862,-44.9475541666667));
#257766=CARTESIAN_POINT('Ctrl Pts',(-46.5766932247455,32.7348404766724,
-44.8892208333333));
#257767=CARTESIAN_POINT('Ctrl Pts',(-46.5766932247455,31.5404524382932,
-44.8308875));
#257768=CARTESIAN_POINT('Ctrl Pts',(-46.5766932247455,30.3460643999139,
-44.7725541666666));
#257769=CARTESIAN_POINT('Ctrl Pts',(-45.5423228415329,29.7488703807243,
-44.7142208333334));
#257770=CARTESIAN_POINT('Ctrl Pts',(-44.5079524583202,29.1516763615346,
-44.6558875));
#257771=CARTESIAN_POINT('Ctrl Pts',(-43.4735820751074,29.7488703807243,
-44.5975541666667));
#257772=CARTESIAN_POINT('Ctrl Pts',(-42.4392116918948,30.3460643999138,
-44.5392208333333));
#257773=CARTESIAN_POINT('Ctrl Pts',(-42.4392116918948,31.5404524382931,
-44.4808875));
#257774=CARTESIAN_POINT('Ctrl Pts',(-42.4392116918948,32.7348404766723,
-44.4225541666667));
#257775=CARTESIAN_POINT('Ctrl Pts',(-43.4735820751074,33.332034495862,-44.3642208333333));
#257776=CARTESIAN_POINT('Ctrl Pts',(-44.5079524583201,33.9292285150516,
-44.3058875));
#257777=CARTESIAN_POINT('Ctrl Pts',(-45.5423228415328,33.332034495862,-44.2475541666667));
#257778=CARTESIAN_POINT('Ctrl Pts',(-46.5766932247455,32.7348404766724,
-44.1892208333334));
#257779=CARTESIAN_POINT('Ctrl Pts',(-46.5766932247455,31.5404524382932,
-44.1308875));
#257780=CARTESIAN_POINT('Ctrl Pts',(-46.5766932247455,30.3460643999139,
-44.0725541666667));
#257781=CARTESIAN_POINT('Ctrl Pts',(-45.5423228415329,29.7488703807243,
-44.0142208333334));
#257782=CARTESIAN_POINT('Ctrl Pts',(-44.5079524583202,29.1516763615346,
-43.9558875));
#257783=CARTESIAN_POINT('Ctrl Pts',(-43.4735820751074,29.7488703807243,
-43.8975541666667));
#257784=CARTESIAN_POINT('Ctrl Pts',(-42.4392116918948,30.3460643999138,
-43.8392208333333));
#257785=CARTESIAN_POINT('Ctrl Pts',(-42.4392116918948,31.5404524382931,
-43.7808875));
#257786=CARTESIAN_POINT('Ctrl Pts',(-42.4392116918948,32.7348404766723,
-43.7225541666667));
#257787=CARTESIAN_POINT('Ctrl Pts',(-43.4735820751074,33.332034495862,-43.6642208333334));
#257788=CARTESIAN_POINT('Ctrl Pts',(-44.5079524583201,33.9292285150516,
-43.6058875));
#257789=CARTESIAN_POINT('Ctrl Pts',(-45.5423228415328,33.332034495862,-43.5475541666667));
#257790=CARTESIAN_POINT('Ctrl Pts',(-46.5766932247455,32.7348404766724,
-43.4892208333333));
#257791=CARTESIAN_POINT('Ctrl Pts',(-46.5766932247455,31.5404524382932,
-43.4308875));
#257792=CARTESIAN_POINT('Ctrl Pts',(-46.5766932247455,30.3460643999139,
-43.3725541666667));
#257793=CARTESIAN_POINT('Ctrl Pts',(-45.5423228415329,29.7488703807243,
-43.3142208333334));
#257794=CARTESIAN_POINT('Ctrl Pts',(-44.5079524583202,29.1516763615346,
-43.2558875));
#257795=CARTESIAN_POINT('Ctrl Pts',(-43.4735820751074,29.7488703807243,
-43.1975541666667));
#257796=CARTESIAN_POINT('Ctrl Pts',(-42.4392116918948,30.3460643999138,
-43.1392208333334));
#257797=CARTESIAN_POINT('Ctrl Pts',(-42.4392116918948,31.5404524382931,
-43.0808875));
#257798=CARTESIAN_POINT('Ctrl Pts',(-42.4392116918948,32.7348404766723,
-43.0225541666667));
#257799=CARTESIAN_POINT('Ctrl Pts',(-43.4735820751074,33.332034495862,-42.9642208333334));
#257800=CARTESIAN_POINT('Ctrl Pts',(-44.5079524583201,33.9292285150516,
-42.9058875));
#257801=CARTESIAN_POINT('Ctrl Pts',(-45.5423228415328,33.332034495862,-42.8475541666667));
#257802=CARTESIAN_POINT('Ctrl Pts',(-46.5766932247455,32.7348404766724,
-42.7892208333334));
#257803=CARTESIAN_POINT('Ctrl Pts',(-46.5766932247455,31.5404524382932,
-42.7308875));
#257804=CARTESIAN_POINT('Ctrl Pts',(-46.5766932247455,30.3460643999139,
-42.6725541666667));
#257805=CARTESIAN_POINT('Ctrl Pts',(-45.5423228415329,29.7488703807243,
-42.6142208333334));
#257806=CARTESIAN_POINT('Ctrl Pts',(-44.5079524583202,29.1516763615346,
-42.5558875));
#257807=CARTESIAN_POINT('Ctrl Pts',(-43.4735820751074,29.7488703807243,
-42.4975541666667));
#257808=CARTESIAN_POINT('Ctrl Pts',(-42.4392116918948,30.3460643999138,
-42.4392208333334));
#257809=CARTESIAN_POINT('Ctrl Pts',(-42.4392116918948,31.5404524382931,
-42.3808875));
#257810=CARTESIAN_POINT('Ctrl Pts',(-42.4392116918948,32.7348404766723,
-42.3225541666667));
#257811=CARTESIAN_POINT('Ctrl Pts',(-43.4735820751074,33.332034495862,-42.2642208333334));
#257812=CARTESIAN_POINT('Ctrl Pts',(-44.5079524583201,33.9292285150516,
-42.2058875));
#257813=CARTESIAN_POINT('Ctrl Pts',(-45.5423228415328,33.332034495862,-42.1475541666667));
#257814=CARTESIAN_POINT('Ctrl Pts',(-46.5766932247455,32.7348404766724,
-42.0892208333333));
#257815=CARTESIAN_POINT('Ctrl Pts',(-46.5766932247455,31.5404524382932,
-42.0308875));
#257816=CARTESIAN_POINT('Ctrl Pts',(-46.5766932247455,30.3460643999139,
-41.9725541666667));
#257817=CARTESIAN_POINT('Ctrl Pts',(-45.5423228415329,29.7488703807243,
-41.9142208333334));
#257818=CARTESIAN_POINT('Ctrl Pts',(-44.5079524583202,29.1516763615346,
-41.8558875));
#257819=CARTESIAN_POINT('Ctrl Pts',(-43.4735820751074,29.7488703807243,
-41.7975541666667));
#257820=CARTESIAN_POINT('Ctrl Pts',(-42.4392116918948,30.3460643999138,
-41.7392208333333));
#257821=CARTESIAN_POINT('Ctrl Pts',(-42.4392116918948,31.5404524382931,
-41.6808875));
#257822=CARTESIAN_POINT('Ctrl Pts',(-42.4392116918948,32.7348404766723,
-41.6225541666667));
#257823=CARTESIAN_POINT('Ctrl Pts',(-43.4735820751074,33.332034495862,-41.5642208333334));
#257824=CARTESIAN_POINT('Ctrl Pts',(-44.5079524583201,33.9292285150516,
-41.5058875));
#257825=CARTESIAN_POINT('Ctrl Pts',(-45.5423228415328,33.332034495862,-41.4475541666667));
#257826=CARTESIAN_POINT('Ctrl Pts',(-46.5766932247455,32.7348404766724,
-41.3892208333333));
#257827=CARTESIAN_POINT('Ctrl Pts',(-46.5766932247455,31.5404524382932,
-41.3308875));
#257828=CARTESIAN_POINT('Ctrl Pts',(-46.5766932247455,30.3460643999139,
-41.2725541666667));
#257829=CARTESIAN_POINT('Ctrl Pts',(-45.5423228415329,29.7488703807243,
-41.2142208333333));
#257830=CARTESIAN_POINT('Ctrl Pts',(-44.5079524583202,29.1516763615346,
-41.1558875));
#257831=CARTESIAN_POINT('Ctrl Pts',(-43.4735820751074,29.7488703807243,
-41.0975541666667));
#257832=CARTESIAN_POINT('Ctrl Pts',(-42.4392116918948,30.3460643999138,
-41.0392208333333));
#257833=CARTESIAN_POINT('Ctrl Pts',(-42.4392116918948,31.5404524382931,
-40.9808875));
#257834=CARTESIAN_POINT('Ctrl Pts',(-42.4392116918948,32.7348404766723,
-40.9225541666667));
#257835=CARTESIAN_POINT('Ctrl Pts',(-43.4735820751074,33.332034495862,-40.8642208333334));
#257836=CARTESIAN_POINT('Ctrl Pts',(-44.5079524583201,33.9292285150516,
-40.8058875));
#257837=CARTESIAN_POINT('Ctrl Pts',(-45.5423228415328,33.332034495862,-40.7475541666667));
#257838=CARTESIAN_POINT('Ctrl Pts',(-46.5766932247455,32.7348404766724,
-40.6892208333333));
#257839=CARTESIAN_POINT('Ctrl Pts',(-46.5766932247455,31.5404524382932,
-40.6308875));
#257840=CARTESIAN_POINT('Ctrl Pts',(-46.5766932247455,30.3460643999139,
-40.5725541666667));
#257841=CARTESIAN_POINT('Ctrl Pts',(-45.5423228415329,29.7488703807243,
-40.5142208333333));
#257842=CARTESIAN_POINT('Ctrl Pts',(-44.5079524583202,29.1516763615346,
-40.4558875));
#257843=CARTESIAN_POINT('Ctrl Pts',(-43.4735820751074,29.7488703807243,
-40.3975541666667));
#257844=CARTESIAN_POINT('Ctrl Pts',(-42.4392116918948,30.3460643999138,
-40.3392208333333));
#257845=CARTESIAN_POINT('Ctrl Pts',(-42.4392116918948,31.5404524382931,
-40.2808875));
#257846=CARTESIAN_POINT('Ctrl Pts',(-42.4392116918948,32.7348404766723,
-40.2225541666667));
#257847=CARTESIAN_POINT('Ctrl Pts',(-43.4735820751074,33.332034495862,-40.1642208333333));
#257848=CARTESIAN_POINT('Ctrl Pts',(-44.5079524583201,33.9292285150516,
-40.1058875));
#257849=CARTESIAN_POINT('Ctrl Pts',(-45.5423228415328,33.332034495862,-40.0475541666667));
#257850=CARTESIAN_POINT('Ctrl Pts',(-46.5766932247455,32.7348404766724,
-39.9892208333333));
#257851=CARTESIAN_POINT('Ctrl Pts',(-46.5766932247455,31.5404524382932,
-39.9308875));
#257852=CARTESIAN_POINT('Ctrl Pts',(-46.5766932247455,30.3460643999139,
-39.8725541666667));
#257853=CARTESIAN_POINT('Ctrl Pts',(-45.5423228415329,29.7488703807243,
-39.8142208333334));
#257854=CARTESIAN_POINT('Ctrl Pts',(-44.5079524583202,29.1516763615346,
-39.7558875));
#257855=CARTESIAN_POINT('Ctrl Pts',(-43.4735820751074,29.7488703807243,
-39.6975541666667));
#257856=CARTESIAN_POINT('Ctrl Pts',(-42.4392116918948,30.3460643999138,
-39.6392208333334));
#257857=CARTESIAN_POINT('Ctrl Pts',(-42.4392116918948,31.5404524382931,
-39.5808875));
#257858=CARTESIAN_POINT('Ctrl Pts',(-42.4392116918948,32.7348404766723,
-39.5225541666667));
#257859=CARTESIAN_POINT('Ctrl Pts',(-43.4735820751074,33.332034495862,-39.4642208333333));
#257860=CARTESIAN_POINT('Ctrl Pts',(-44.5079524583201,33.9292285150516,
-39.4058875));
#257861=CARTESIAN_POINT('Ctrl Pts',(-45.5423228415328,33.332034495862,-39.3475541666667));
#257862=CARTESIAN_POINT('Ctrl Pts',(-46.5766932247455,32.7348404766724,
-39.2892208333334));
#257863=CARTESIAN_POINT('Ctrl Pts',(-46.5766932247455,31.5404524382932,
-39.2308875));
#257864=CARTESIAN_POINT('Ctrl Pts',(-46.5766932247455,30.3460643999139,
-39.1725541666667));
#257865=CARTESIAN_POINT('Ctrl Pts',(-45.5423228415329,29.7488703807243,
-39.1142208333333));
#257866=CARTESIAN_POINT('Ctrl Pts',(-44.5079524583202,29.1516763615346,
-39.0558875));
#257867=CARTESIAN_POINT('Ctrl Pts',(-43.4735820751074,29.7488703807243,
-38.9975541666667));
#257868=CARTESIAN_POINT('Ctrl Pts',(-42.4392116918948,30.3460643999138,
-38.9392208333334));
#257869=CARTESIAN_POINT('Ctrl Pts',(-42.4392116918948,31.5404524382931,
-38.8808875));
#257870=CARTESIAN_POINT('Ctrl Pts',(-42.4392116918948,32.7348404766723,
-38.8225541666667));
#257871=CARTESIAN_POINT('Ctrl Pts',(-43.4735820751074,33.332034495862,-38.7642208333333));
#257872=CARTESIAN_POINT('Ctrl Pts',(-44.5079524583201,33.9292285150516,
-38.7058875));
#257873=CARTESIAN_POINT('Ctrl Pts',(-45.5423228415328,33.332034495862,-38.6475541666667));
#257874=CARTESIAN_POINT('Ctrl Pts',(-46.5766932247455,32.7348404766724,
-38.5892208333334));
#257875=CARTESIAN_POINT('Ctrl Pts',(-46.5766932247455,31.5404524382932,
-38.5308875));
#257876=CARTESIAN_POINT('Ctrl Pts',(-46.5766932247455,30.3460643999139,
-38.4725541666667));
#257877=CARTESIAN_POINT('Ctrl Pts',(-45.5423228415329,29.7488703807243,
-38.4142208333334));
#257878=CARTESIAN_POINT('Ctrl Pts',(-44.5079524583202,29.1516763615346,
-38.3558875));
#257879=CARTESIAN_POINT('Ctrl Pts',(-43.4735820751074,29.7488703807243,
-38.2975541666667));
#257880=CARTESIAN_POINT('Ctrl Pts',(-42.4392116918948,30.3460643999138,
-38.2392208333333));
#257881=CARTESIAN_POINT('Ctrl Pts',(-42.4392116918948,31.5404524382931,
-38.1808875));
#257882=CARTESIAN_POINT('Ctrl Pts',(-42.4392116918948,32.7348404766723,
-38.1225541666667));
#257883=CARTESIAN_POINT('Ctrl Pts',(-43.4735820751074,33.332034495862,-38.0642208333334));
#257884=CARTESIAN_POINT('Ctrl Pts',(-44.5079524583201,33.9292285150516,
-38.0058875));
#257885=CARTESIAN_POINT('Ctrl Pts',(-45.5423228415328,33.332034495862,-37.9475541666667));
#257886=CARTESIAN_POINT('Ctrl Pts',(-46.5766932247455,32.7348404766724,
-37.8892208333334));
#257887=CARTESIAN_POINT('Ctrl Pts',(-46.5766932247455,31.5404524382932,
-37.8308875));
#257888=CARTESIAN_POINT('Ctrl Pts',(-46.5766932247455,30.3460643999139,
-37.7725541666667));
#257889=CARTESIAN_POINT('Ctrl Pts',(-45.5423228415329,29.7488703807243,
-37.7142208333333));
#257890=CARTESIAN_POINT('Ctrl Pts',(-44.5079524583202,29.1516763615346,
-37.6558875));
#257891=CARTESIAN_POINT('Ctrl Pts',(-43.4735820751074,29.7488703807243,
-37.5975541666667));
#257892=CARTESIAN_POINT('Ctrl Pts',(-42.4392116918948,30.3460643999138,
-37.5392208333334));
#257893=CARTESIAN_POINT('Ctrl Pts',(-42.4392116918948,31.5404524382931,
-37.4808875));
#257894=CARTESIAN_POINT('Ctrl Pts',(-42.4392116918948,32.7348404766723,
-37.4225541666667));
#257895=CARTESIAN_POINT('Ctrl Pts',(-43.4735820751074,33.332034495862,-37.3642208333333));
#257896=CARTESIAN_POINT('Ctrl Pts',(-44.5079524583201,33.9292285150516,
-37.3058875));
#257897=CARTESIAN_POINT('Ctrl Pts',(-45.5423228415328,33.332034495862,-37.2475541666667));
#257898=CARTESIAN_POINT('Ctrl Pts',(-45.6766168155003,33.2544998338414,
-37.239980655983));
#257899=CARTESIAN_POINT('Ctrl Pts',(-45.7978513037523,33.1578111886089,
-37.2318399189827));
#257900=CARTESIAN_POINT('Ctrl Pts',(-46.5057015041446,31.6353141793171,
-39.8960578923557));
#257901=CARTESIAN_POINT('Ctrl Pts',(-46.5119689182291,31.50332502993,-39.889207245322));
#257902=CARTESIAN_POINT('Ctrl Pts',(-46.5051456084936,31.3710593016932,
-39.8825607059083));
#257903=CARTESIAN_POINT('Ctrl Pts',(-46.4647767050806,31.1050578555559,
-39.8679453789873));
#257904=CARTESIAN_POINT('Ctrl Pts',(-46.4304101376052,30.9722276023654,
-39.8602326823062));
#257905=CARTESIAN_POINT('Ctrl Pts',(-46.2910712917496,30.5971572052441,
-39.8372207705955));
#257906=CARTESIAN_POINT('Ctrl Pts',(-46.1515432444974,30.3708657627987,
-39.8217193778446));
#257907=CARTESIAN_POINT('Ctrl Pts',(-45.7937945447006,29.986360537189,-39.7918605486601));
#257908=CARTESIAN_POINT('Ctrl Pts',(-45.5795141212975,29.83155817775,-39.7787077636743));
#257909=CARTESIAN_POINT('Ctrl Pts',(-45.1083142701796,29.6155194738802,
-39.7512211056924));
#257910=CARTESIAN_POINT('Ctrl Pts',(-44.8567670881079,29.5544784081473,
-39.7365475200715));
#257911=CARTESIAN_POINT('Ctrl Pts',(-44.5697046391987,29.5411668093911,
-39.7198022105518));
#257912=CARTESIAN_POINT('Ctrl Pts',(-44.5388151356,29.5404524382925,-39.7180003228417));
#257913=CARTESIAN_POINT('Ctrl Pts',(-44.5079524583208,29.5404524382925,
-39.7162000000005));
#257914=CARTESIAN_POINT('',(-46.2580162608798,30.7712606105792,-39.7946023861626));
#257915=CARTESIAN_POINT('Ctrl Pts',(-46.2580162608798,30.7712606105792,
-39.7946023861626));
#257916=CARTESIAN_POINT('Ctrl Pts',(-46.3359857239729,30.9069849161725,
-39.8137239675819));
#257917=CARTESIAN_POINT('Ctrl Pts',(-46.396731144117,31.0517787814577,-39.8323019201559));
#257918=CARTESIAN_POINT('Ctrl Pts',(-46.4779237668435,31.3431553140667,
-39.8662996885231));
#257919=CARTESIAN_POINT('Ctrl Pts',(-46.5007939700139,31.4890814765333,
-39.8816624604009));
#257920=CARTESIAN_POINT('Ctrl Pts',(-46.5057020315789,31.6353141675789,
-39.896058194301));
#257921=CARTESIAN_POINT('Ctrl Pts',(-42.7562642394046,32.2382933072411,
-39.4336017780242));
#257922=CARTESIAN_POINT('Ctrl Pts',(-42.7061752771237,32.0303939840906,
-39.4290050783144));
#257923=CARTESIAN_POINT('Ctrl Pts',(-42.6879554887345,31.8161871839669,
-39.4265147261078));
#257924=CARTESIAN_POINT('Ctrl Pts',(-42.722826451042,31.3151915282915,-39.4248348087752));
#257925=CARTESIAN_POINT('Ctrl Pts',(-42.7978352817771,31.0971672163081,
-39.4293776397756));
#257926=CARTESIAN_POINT('Ctrl Pts',(-42.9440228306321,30.7609930563022,
-39.4392856099245));
#257927=CARTESIAN_POINT('Ctrl Pts',(-43.0567852873963,30.5852973811317,
-39.4475010921534));
#257928=CARTESIAN_POINT('Ctrl Pts',(-43.2774600503745,30.3411850111334,
-39.4631783255256));
#257929=CARTESIAN_POINT('Ctrl Pts',(-43.3671859662176,30.2593637739806,
-39.4694819317037));
#257930=CARTESIAN_POINT('Ctrl Pts',(-43.4669086721409,30.1846213999269,
-39.4763662142424));
#257931=CARTESIAN_POINT('Ctrl Pts',(-43.4696440671836,30.1825827861219,
-39.4765549614359));
#257932=CARTESIAN_POINT('Ctrl Pts',(-43.4751302568142,30.1785171929352,
-39.476933339386));
#257933=CARTESIAN_POINT('Ctrl Pts',(-43.4778810222449,30.1764902718028,
-39.477122967848));
#257934=CARTESIAN_POINT('Ctrl Pts',(-43.486189072521,30.1704031945995,-39.4776954266054));
#257935=CARTESIAN_POINT('Ctrl Pts',(-43.4917628814586,30.1663661255867,
-39.478079121429));
#257936=CARTESIAN_POINT('Ctrl Pts',(-43.6119452918925,30.0803173607471,
-39.486344690909));
#257937=CARTESIAN_POINT('Ctrl Pts',(-43.7365211293469,30.0105461443142,
-39.4945972457688));
#257938=CARTESIAN_POINT('Ctrl Pts',(-44.1000414214535,29.8596150599266,
-39.5217363802476));
#257939=CARTESIAN_POINT('Ctrl Pts',(-44.348728581181,29.8115394459938,-39.5427431282814));
#257940=CARTESIAN_POINT('Ctrl Pts',(-44.8440271149477,29.8137267466852,
-39.5899036033774));
#257941=CARTESIAN_POINT('Ctrl Pts',(-45.0860786710093,29.861506312415,-39.6155008436718));
#257942=CARTESIAN_POINT('Ctrl Pts',(-45.5020085767912,30.0282049213117,
-39.6643839318259));
#257943=CARTESIAN_POINT('Ctrl Pts',(-45.6748667889198,30.1313751697612,
-39.6873672741751));
#257944=CARTESIAN_POINT('Ctrl Pts',(-46.0013454707669,30.4043598575736,
-39.7391811305329));
#257945=CARTESIAN_POINT('Ctrl Pts',(-46.1464934812618,30.5771288156309,
-39.767252038655));
#257946=CARTESIAN_POINT('Ctrl Pts',(-46.2580162608798,30.7712606105792,
-39.7946023861626));
#257947=CARTESIAN_POINT('Ctrl Pts',(-46.1766977413726,31.5404524382932,
-52.99995));
#257948=CARTESIAN_POINT('Ctrl Pts',(-46.1766977413726,30.5770018999139,
-52.9416166666667));
#257949=CARTESIAN_POINT('Ctrl Pts',(-45.3423250998464,30.0952766307242,
-52.8832833333334));
#257950=CARTESIAN_POINT('Ctrl Pts',(-44.5079524583202,29.6135513615346,
-52.82495));
#257951=CARTESIAN_POINT('Ctrl Pts',(-43.6735798167939,30.0952766307242,
-52.7666166666667));
#257952=CARTESIAN_POINT('Ctrl Pts',(-42.8392071752677,30.5770018999139,
-52.7082833333333));
#257953=CARTESIAN_POINT('Ctrl Pts',(-42.8392071752677,31.5404524382931,
-52.64995));
#257954=CARTESIAN_POINT('Ctrl Pts',(-42.8392071752677,32.5039029766724,
-52.5916166666666));
#257955=CARTESIAN_POINT('Ctrl Pts',(-43.6735798167939,32.985628245862,-52.5332833333334));
#257956=CARTESIAN_POINT('Ctrl Pts',(-44.5079524583201,33.4673535150516,
-52.4749500000001));
#257957=CARTESIAN_POINT('Ctrl Pts',(-45.3423250998464,32.985628245862,-52.4166166666667));
#257958=CARTESIAN_POINT('Ctrl Pts',(-46.1766977413726,32.5039029766724,
-52.3582833333334));
#257959=CARTESIAN_POINT('Ctrl Pts',(-46.1766977413726,31.5404524382932,
-52.29995));
#257960=CARTESIAN_POINT('Ctrl Pts',(-46.1766977413726,30.5770018999139,
-52.2416166666667));
#257961=CARTESIAN_POINT('Ctrl Pts',(-45.3423250998464,30.0952766307242,
-52.1832833333333));
#257962=CARTESIAN_POINT('Ctrl Pts',(-44.5079524583202,29.6135513615346,
-52.12495));
#257963=CARTESIAN_POINT('Ctrl Pts',(-43.6735798167939,30.0952766307242,
-52.0666166666667));
#257964=CARTESIAN_POINT('Ctrl Pts',(-42.8392071752677,30.5770018999139,
-52.0082833333333));
#257965=CARTESIAN_POINT('Ctrl Pts',(-42.8392071752677,31.5404524382931,
-51.94995));
#257966=CARTESIAN_POINT('Ctrl Pts',(-42.8392071752677,32.5039029766724,
-51.8916166666667));
#257967=CARTESIAN_POINT('Ctrl Pts',(-43.6735798167939,32.985628245862,-51.8332833333333));
#257968=CARTESIAN_POINT('Ctrl Pts',(-44.5079524583201,33.4673535150516,
-51.77495));
#257969=CARTESIAN_POINT('Ctrl Pts',(-45.3423250998464,32.985628245862,-51.7166166666667));
#257970=CARTESIAN_POINT('Ctrl Pts',(-46.1766977413726,32.5039029766724,
-51.6582833333333));
#257971=CARTESIAN_POINT('Ctrl Pts',(-46.1766977413726,31.5404524382932,
-51.59995));
#257972=CARTESIAN_POINT('Ctrl Pts',(-46.1766977413726,30.5770018999139,
-51.5416166666667));
#257973=CARTESIAN_POINT('Ctrl Pts',(-45.3423250998464,30.0952766307242,
-51.4832833333333));
#257974=CARTESIAN_POINT('Ctrl Pts',(-44.5079524583202,29.6135513615346,
-51.42495));
#257975=CARTESIAN_POINT('Ctrl Pts',(-43.6735798167939,30.0952766307242,
-51.3666166666667));
#257976=CARTESIAN_POINT('Ctrl Pts',(-42.8392071752677,30.5770018999139,
-51.3082833333333));
#257977=CARTESIAN_POINT('Ctrl Pts',(-42.8392071752677,31.5404524382931,
-51.24995));
#257978=CARTESIAN_POINT('Ctrl Pts',(-42.8392071752677,32.5039029766724,
-51.1916166666666));
#257979=CARTESIAN_POINT('Ctrl Pts',(-43.6735798167939,32.985628245862,-51.1332833333333));
#257980=CARTESIAN_POINT('Ctrl Pts',(-44.5079524583201,33.4673535150516,
-51.07495));
#257981=CARTESIAN_POINT('Ctrl Pts',(-45.3423250998464,32.985628245862,-51.0166166666667));
#257982=CARTESIAN_POINT('Ctrl Pts',(-46.1766977413726,32.5039029766724,
-50.9582833333334));
#257983=CARTESIAN_POINT('Ctrl Pts',(-46.1766977413726,31.5404524382932,
-50.89995));
#257984=CARTESIAN_POINT('Ctrl Pts',(-46.1766977413726,30.5770018999139,
-50.8416166666667));
#257985=CARTESIAN_POINT('Ctrl Pts',(-45.3423250998464,30.0952766307242,
-50.7832833333333));
#257986=CARTESIAN_POINT('Ctrl Pts',(-44.5079524583202,29.6135513615346,
-50.72495));
#257987=CARTESIAN_POINT('Ctrl Pts',(-43.6735798167939,30.0952766307242,
-50.6666166666667));
#257988=CARTESIAN_POINT('Ctrl Pts',(-42.8392071752677,30.5770018999139,
-50.6082833333334));
#257989=CARTESIAN_POINT('Ctrl Pts',(-42.8392071752677,31.5404524382931,
-50.54995));
#257990=CARTESIAN_POINT('Ctrl Pts',(-42.8392071752677,32.5039029766724,
-50.4916166666667));
#257991=CARTESIAN_POINT('Ctrl Pts',(-43.6735798167939,32.985628245862,-50.4332833333333));
#257992=CARTESIAN_POINT('Ctrl Pts',(-44.5079524583201,33.4673535150516,
-50.37495));
#257993=CARTESIAN_POINT('Ctrl Pts',(-45.3423250998464,32.985628245862,-50.3166166666667));
#257994=CARTESIAN_POINT('Ctrl Pts',(-46.1766977413726,32.5039029766724,
-50.2582833333334));
#257995=CARTESIAN_POINT('Ctrl Pts',(-46.1766977413726,31.5404524382932,
-50.19995));
#257996=CARTESIAN_POINT('Ctrl Pts',(-46.1766977413726,30.5770018999139,
-50.1416166666667));
#257997=CARTESIAN_POINT('Ctrl Pts',(-45.3423250998464,30.0952766307242,
-50.0832833333333));
#257998=CARTESIAN_POINT('Ctrl Pts',(-44.5079524583202,29.6135513615346,
-50.02495));
#257999=CARTESIAN_POINT('Ctrl Pts',(-43.6735798167939,30.0952766307242,
-49.9666166666667));
#258000=CARTESIAN_POINT('Ctrl Pts',(-42.8392071752677,30.5770018999139,
-49.9082833333334));
#258001=CARTESIAN_POINT('Ctrl Pts',(-42.8392071752677,31.5404524382931,
-49.84995));
#258002=CARTESIAN_POINT('Ctrl Pts',(-42.8392071752677,32.5039029766724,
-49.7916166666667));
#258003=CARTESIAN_POINT('Ctrl Pts',(-43.6735798167939,32.985628245862,-49.7332833333333));
#258004=CARTESIAN_POINT('Ctrl Pts',(-44.5079524583201,33.4673535150516,
-49.67495));
#258005=CARTESIAN_POINT('Ctrl Pts',(-45.3423250998464,32.985628245862,-49.6166166666667));
#258006=CARTESIAN_POINT('Ctrl Pts',(-46.1766977413726,32.5039029766724,
-49.5582833333334));
#258007=CARTESIAN_POINT('Ctrl Pts',(-46.1766977413726,31.5404524382932,
-49.49995));
#258008=CARTESIAN_POINT('Ctrl Pts',(-46.1766977413726,30.5770018999139,
-49.4416166666667));
#258009=CARTESIAN_POINT('Ctrl Pts',(-45.3423250998464,30.0952766307242,
-49.3832833333334));
#258010=CARTESIAN_POINT('Ctrl Pts',(-44.5079524583202,29.6135513615346,
-49.32495));
#258011=CARTESIAN_POINT('Ctrl Pts',(-43.6735798167939,30.0952766307242,
-49.2666166666667));
#258012=CARTESIAN_POINT('Ctrl Pts',(-42.8392071752677,30.5770018999139,
-49.2082833333334));
#258013=CARTESIAN_POINT('Ctrl Pts',(-42.8392071752677,31.5404524382931,
-49.14995));
#258014=CARTESIAN_POINT('Ctrl Pts',(-42.8392071752677,32.5039029766724,
-49.0916166666667));
#258015=CARTESIAN_POINT('Ctrl Pts',(-43.6735798167939,32.985628245862,-49.0332833333333));
#258016=CARTESIAN_POINT('Ctrl Pts',(-44.5079524583201,33.4673535150516,
-48.97495));
#258017=CARTESIAN_POINT('Ctrl Pts',(-45.3423250998464,32.985628245862,-48.9166166666667));
#258018=CARTESIAN_POINT('Ctrl Pts',(-46.1766977413726,32.5039029766724,
-48.8582833333333));
#258019=CARTESIAN_POINT('Ctrl Pts',(-46.1766977413726,31.5404524382932,
-48.79995));
#258020=CARTESIAN_POINT('Ctrl Pts',(-46.1766977413726,30.5770018999139,
-48.7416166666667));
#258021=CARTESIAN_POINT('Ctrl Pts',(-45.3423250998464,30.0952766307242,
-48.6832833333333));
#258022=CARTESIAN_POINT('Ctrl Pts',(-44.5079524583202,29.6135513615346,
-48.62495));
#258023=CARTESIAN_POINT('Ctrl Pts',(-43.6735798167939,30.0952766307242,
-48.5666166666667));
#258024=CARTESIAN_POINT('Ctrl Pts',(-42.8392071752677,30.5770018999139,
-48.5082833333333));
#258025=CARTESIAN_POINT('Ctrl Pts',(-42.8392071752677,31.5404524382931,
-48.44995));
#258026=CARTESIAN_POINT('Ctrl Pts',(-42.8392071752677,32.5039029766724,
-48.3916166666667));
#258027=CARTESIAN_POINT('Ctrl Pts',(-43.6735798167939,32.985628245862,-48.3332833333333));
#258028=CARTESIAN_POINT('Ctrl Pts',(-44.5079524583201,33.4673535150516,
-48.27495));
#258029=CARTESIAN_POINT('Ctrl Pts',(-45.3423250998464,32.985628245862,-48.2166166666667));
#258030=CARTESIAN_POINT('Ctrl Pts',(-46.1766977413726,32.5039029766724,
-48.1582833333333));
#258031=CARTESIAN_POINT('Ctrl Pts',(-46.1766977413726,31.5404524382932,
-48.09995));
#258032=CARTESIAN_POINT('Ctrl Pts',(-46.1766977413726,30.5770018999139,
-48.0416166666667));
#258033=CARTESIAN_POINT('Ctrl Pts',(-45.3423250998464,30.0952766307242,
-47.9832833333334));
#258034=CARTESIAN_POINT('Ctrl Pts',(-44.5079524583202,29.6135513615346,
-47.92495));
#258035=CARTESIAN_POINT('Ctrl Pts',(-43.6735798167939,30.0952766307242,
-47.8666166666667));
#258036=CARTESIAN_POINT('Ctrl Pts',(-42.8392071752677,30.5770018999139,
-47.8082833333333));
#258037=CARTESIAN_POINT('Ctrl Pts',(-42.8392071752677,31.5404524382931,
-47.74995));
#258038=CARTESIAN_POINT('Ctrl Pts',(-42.8392071752677,32.5039029766724,
-47.6916166666667));
#258039=CARTESIAN_POINT('Ctrl Pts',(-43.6735798167939,32.985628245862,-47.6332833333333));
#258040=CARTESIAN_POINT('Ctrl Pts',(-44.5079524583201,33.4673535150516,
-47.57495));
#258041=CARTESIAN_POINT('Ctrl Pts',(-45.3423250998464,32.985628245862,-47.5166166666667));
#258042=CARTESIAN_POINT('Ctrl Pts',(-46.1766977413726,32.5039029766724,
-47.4582833333333));
#258043=CARTESIAN_POINT('Ctrl Pts',(-46.1766977413726,31.5404524382932,
-47.39995));
#258044=CARTESIAN_POINT('Ctrl Pts',(-46.1766977413726,30.5770018999139,
-47.3416166666666));
#258045=CARTESIAN_POINT('Ctrl Pts',(-45.3423250998464,30.0952766307242,
-47.2832833333333));
#258046=CARTESIAN_POINT('Ctrl Pts',(-44.5079524583202,29.6135513615346,
-47.22495));
#258047=CARTESIAN_POINT('Ctrl Pts',(-43.6735798167939,30.0952766307242,
-47.1666166666667));
#258048=CARTESIAN_POINT('Ctrl Pts',(-42.8392071752677,30.5770018999139,
-47.1082833333333));
#258049=CARTESIAN_POINT('Ctrl Pts',(-42.8392071752677,31.5404524382931,
-47.04995));
#258050=CARTESIAN_POINT('Ctrl Pts',(-42.8392071752677,32.5039029766724,
-46.9916166666667));
#258051=CARTESIAN_POINT('Ctrl Pts',(-43.6735798167939,32.985628245862,-46.9332833333333));
#258052=CARTESIAN_POINT('Ctrl Pts',(-44.5079524583201,33.4673535150516,
-46.87495));
#258053=CARTESIAN_POINT('Ctrl Pts',(-45.3423250998464,32.985628245862,-46.8166166666667));
#258054=CARTESIAN_POINT('Ctrl Pts',(-46.1766977413726,32.5039029766724,
-46.7582833333333));
#258055=CARTESIAN_POINT('Ctrl Pts',(-46.1766977413726,31.5404524382932,
-46.69995));
#258056=CARTESIAN_POINT('Ctrl Pts',(-46.1766977413726,30.5770018999139,
-46.6416166666666));
#258057=CARTESIAN_POINT('Ctrl Pts',(-45.3423250998464,30.0952766307242,
-46.5832833333334));
#258058=CARTESIAN_POINT('Ctrl Pts',(-44.5079524583202,29.6135513615346,
-46.52495));
#258059=CARTESIAN_POINT('Ctrl Pts',(-43.6735798167939,30.0952766307242,
-46.4666166666667));
#258060=CARTESIAN_POINT('Ctrl Pts',(-42.8392071752677,30.5770018999139,
-46.4082833333334));
#258061=CARTESIAN_POINT('Ctrl Pts',(-42.8392071752677,31.5404524382931,
-46.34995));
#258062=CARTESIAN_POINT('Ctrl Pts',(-42.8392071752677,32.5039029766724,
-46.2916166666667));
#258063=CARTESIAN_POINT('Ctrl Pts',(-43.6735798167939,32.985628245862,-46.2332833333334));
#258064=CARTESIAN_POINT('Ctrl Pts',(-44.5079524583201,33.4673535150516,
-46.17495));
#258065=CARTESIAN_POINT('Ctrl Pts',(-45.3423250998464,32.985628245862,-46.1166166666667));
#258066=CARTESIAN_POINT('Ctrl Pts',(-46.1766977413726,32.5039029766724,
-46.0582833333333));
#258067=CARTESIAN_POINT('Ctrl Pts',(-46.1766977413726,31.5404524382932,
-45.99995));
#258068=CARTESIAN_POINT('Ctrl Pts',(-46.1766977413726,30.5770018999139,
-45.9416166666667));
#258069=CARTESIAN_POINT('Ctrl Pts',(-45.3423250998464,30.0952766307242,
-45.8832833333333));
#258070=CARTESIAN_POINT('Ctrl Pts',(-44.5079524583202,29.6135513615346,
-45.82495));
#258071=CARTESIAN_POINT('Ctrl Pts',(-43.6735798167939,30.0952766307242,
-45.7666166666667));
#258072=CARTESIAN_POINT('Ctrl Pts',(-42.8392071752677,30.5770018999139,
-45.7082833333333));
#258073=CARTESIAN_POINT('Ctrl Pts',(-42.8392071752677,31.5404524382931,
-45.64995));
#258074=CARTESIAN_POINT('Ctrl Pts',(-42.8392071752677,32.5039029766724,
-45.5916166666667));
#258075=CARTESIAN_POINT('Ctrl Pts',(-43.6735798167939,32.985628245862,-45.5332833333333));
#258076=CARTESIAN_POINT('Ctrl Pts',(-44.5079524583201,33.4673535150516,
-45.47495));
#258077=CARTESIAN_POINT('Ctrl Pts',(-45.3423250998464,32.985628245862,-45.4166166666667));
#258078=CARTESIAN_POINT('Ctrl Pts',(-46.1766977413726,32.5039029766724,
-45.3582833333333));
#258079=CARTESIAN_POINT('Ctrl Pts',(-46.1766977413726,31.5404524382932,
-45.29995));
#258080=CARTESIAN_POINT('Ctrl Pts',(-46.1766977413726,30.5770018999139,
-45.2416166666667));
#258081=CARTESIAN_POINT('Ctrl Pts',(-45.3423250998464,30.0952766307242,
-45.1832833333333));
#258082=CARTESIAN_POINT('Ctrl Pts',(-44.5079524583202,29.6135513615346,
-45.12495));
#258083=CARTESIAN_POINT('Ctrl Pts',(-43.6735798167939,30.0952766307242,
-45.0666166666667));
#258084=CARTESIAN_POINT('Ctrl Pts',(-42.8392071752677,30.5770018999139,
-45.0082833333334));
#258085=CARTESIAN_POINT('Ctrl Pts',(-42.8392071752677,31.5404524382931,
-44.94995));
#258086=CARTESIAN_POINT('Ctrl Pts',(-42.8392071752677,32.5039029766724,
-44.8916166666667));
#258087=CARTESIAN_POINT('Ctrl Pts',(-43.6735798167939,32.985628245862,-44.8332833333334));
#258088=CARTESIAN_POINT('Ctrl Pts',(-44.5079524583201,33.4673535150516,
-44.77495));
#258089=CARTESIAN_POINT('Ctrl Pts',(-45.3423250998464,32.985628245862,-44.7166166666667));
#258090=CARTESIAN_POINT('Ctrl Pts',(-46.1766977413726,32.5039029766724,
-44.6582833333333));
#258091=CARTESIAN_POINT('Ctrl Pts',(-46.1766977413726,31.5404524382932,
-44.59995));
#258092=CARTESIAN_POINT('Ctrl Pts',(-46.1766977413726,30.5770018999139,
-44.5416166666667));
#258093=CARTESIAN_POINT('Ctrl Pts',(-45.3423250998464,30.0952766307242,
-44.4832833333334));
#258094=CARTESIAN_POINT('Ctrl Pts',(-44.5079524583202,29.6135513615346,
-44.42495));
#258095=CARTESIAN_POINT('Ctrl Pts',(-43.6735798167939,30.0952766307242,
-44.3666166666667));
#258096=CARTESIAN_POINT('Ctrl Pts',(-42.8392071752677,30.5770018999139,
-44.3082833333334));
#258097=CARTESIAN_POINT('Ctrl Pts',(-42.8392071752677,31.5404524382931,
-44.24995));
#258098=CARTESIAN_POINT('Ctrl Pts',(-42.8392071752677,32.5039029766724,
-44.1916166666667));
#258099=CARTESIAN_POINT('Ctrl Pts',(-43.6735798167939,32.985628245862,-44.1332833333334));
#258100=CARTESIAN_POINT('Ctrl Pts',(-44.5079524583201,33.4673535150516,
-44.07495));
#258101=CARTESIAN_POINT('Ctrl Pts',(-45.3423250998464,32.985628245862,-44.0166166666667));
#258102=CARTESIAN_POINT('Ctrl Pts',(-46.1766977413726,32.5039029766724,
-43.9582833333334));
#258103=CARTESIAN_POINT('Ctrl Pts',(-46.1766977413726,31.5404524382932,
-43.89995));
#258104=CARTESIAN_POINT('Ctrl Pts',(-46.1766977413726,30.5770018999139,
-43.8416166666667));
#258105=CARTESIAN_POINT('Ctrl Pts',(-45.3423250998464,30.0952766307242,
-43.7832833333334));
#258106=CARTESIAN_POINT('Ctrl Pts',(-44.5079524583202,29.6135513615346,
-43.72495));
#258107=CARTESIAN_POINT('Ctrl Pts',(-43.6735798167939,30.0952766307242,
-43.6666166666667));
#258108=CARTESIAN_POINT('Ctrl Pts',(-42.8392071752677,30.5770018999139,
-43.6082833333333));
#258109=CARTESIAN_POINT('Ctrl Pts',(-42.8392071752677,31.5404524382931,
-43.54995));
#258110=CARTESIAN_POINT('Ctrl Pts',(-42.8392071752677,32.5039029766724,
-43.4916166666667));
#258111=CARTESIAN_POINT('Ctrl Pts',(-43.6735798167939,32.985628245862,-43.4332833333333));
#258112=CARTESIAN_POINT('Ctrl Pts',(-44.5079524583201,33.4673535150516,
-43.37495));
#258113=CARTESIAN_POINT('Ctrl Pts',(-45.3423250998464,32.985628245862,-43.3166166666667));
#258114=CARTESIAN_POINT('Ctrl Pts',(-46.1766977413726,32.5039029766724,
-43.2582833333333));
#258115=CARTESIAN_POINT('Ctrl Pts',(-46.1766977413726,31.5404524382932,
-43.19995));
#258116=CARTESIAN_POINT('Ctrl Pts',(-46.1766977413726,30.5770018999139,
-43.1416166666666));
#258117=CARTESIAN_POINT('Ctrl Pts',(-45.3423250998464,30.0952766307242,
-43.0832833333333));
#258118=CARTESIAN_POINT('Ctrl Pts',(-44.5079524583202,29.6135513615346,
-43.02495));
#258119=CARTESIAN_POINT('Ctrl Pts',(-43.6735798167939,30.0952766307242,
-42.9666166666667));
#258120=CARTESIAN_POINT('Ctrl Pts',(-42.8392071752677,30.5770018999139,
-42.9082833333333));
#258121=CARTESIAN_POINT('Ctrl Pts',(-42.8392071752677,31.5404524382931,
-42.84995));
#258122=CARTESIAN_POINT('Ctrl Pts',(-42.8392071752677,32.5039029766724,
-42.7916166666667));
#258123=CARTESIAN_POINT('Ctrl Pts',(-43.6735798167939,32.985628245862,-42.7332833333334));
#258124=CARTESIAN_POINT('Ctrl Pts',(-44.5079524583201,33.4673535150516,
-42.67495));
#258125=CARTESIAN_POINT('Ctrl Pts',(-45.3423250998464,32.985628245862,-42.6166166666667));
#258126=CARTESIAN_POINT('Ctrl Pts',(-46.1766977413726,32.5039029766724,
-42.5582833333333));
#258127=CARTESIAN_POINT('Ctrl Pts',(-46.1766977413726,31.5404524382932,
-42.49995));
#258128=CARTESIAN_POINT('Ctrl Pts',(-46.1766977413726,30.5770018999139,
-42.4416166666667));
#258129=CARTESIAN_POINT('Ctrl Pts',(-45.3423250998464,30.0952766307242,
-42.3832833333333));
#258130=CARTESIAN_POINT('Ctrl Pts',(-44.5079524583202,29.6135513615346,
-42.32495));
#258131=CARTESIAN_POINT('Ctrl Pts',(-43.6735798167939,30.0952766307242,
-42.2666166666667));
#258132=CARTESIAN_POINT('Ctrl Pts',(-42.8392071752677,30.5770018999139,
-42.2082833333333));
#258133=CARTESIAN_POINT('Ctrl Pts',(-42.8392071752677,31.5404524382931,
-42.14995));
#258134=CARTESIAN_POINT('Ctrl Pts',(-42.8392071752677,32.5039029766724,
-42.0916166666667));
#258135=CARTESIAN_POINT('Ctrl Pts',(-43.6735798167939,32.985628245862,-42.0332833333334));
#258136=CARTESIAN_POINT('Ctrl Pts',(-44.5079524583201,33.4673535150516,
-41.97495));
#258137=CARTESIAN_POINT('Ctrl Pts',(-45.3423250998464,32.985628245862,-41.9166166666666));
#258138=CARTESIAN_POINT('Ctrl Pts',(-46.1766977413726,32.5039029766724,
-41.8582833333333));
#258139=CARTESIAN_POINT('Ctrl Pts',(-46.1766977413726,31.5404524382932,
-41.79995));
#258140=CARTESIAN_POINT('Ctrl Pts',(-46.1766977413726,30.5770018999139,
-41.7416166666667));
#258141=CARTESIAN_POINT('Ctrl Pts',(-45.3423250998464,30.0952766307242,
-41.6832833333333));
#258142=CARTESIAN_POINT('Ctrl Pts',(-44.5079524583202,29.6135513615346,
-41.62495));
#258143=CARTESIAN_POINT('Ctrl Pts',(-43.6735798167939,30.0952766307242,
-41.5666166666667));
#258144=CARTESIAN_POINT('Ctrl Pts',(-42.8392071752677,30.5770018999139,
-41.5082833333334));
#258145=CARTESIAN_POINT('Ctrl Pts',(-42.8392071752677,31.5404524382931,
-41.44995));
#258146=CARTESIAN_POINT('Ctrl Pts',(-42.8392071752677,32.5039029766724,
-41.3916166666667));
#258147=CARTESIAN_POINT('Ctrl Pts',(-43.6735798167939,32.985628245862,-41.3332833333334));
#258148=CARTESIAN_POINT('Ctrl Pts',(-44.5079524583201,33.4673535150516,
-41.27495));
#258149=CARTESIAN_POINT('Ctrl Pts',(-45.3423250998464,32.985628245862,-41.2166166666667));
#258150=CARTESIAN_POINT('Ctrl Pts',(-46.1766977413726,32.5039029766724,
-41.1582833333333));
#258151=CARTESIAN_POINT('Ctrl Pts',(-46.1766977413726,31.5404524382932,
-41.09995));
#258152=CARTESIAN_POINT('Ctrl Pts',(-46.1766977413726,30.5770018999139,
-41.0416166666667));
#258153=CARTESIAN_POINT('Ctrl Pts',(-45.3423250998464,30.0952766307242,
-40.9832833333333));
#258154=CARTESIAN_POINT('Ctrl Pts',(-44.5079524583202,29.6135513615346,
-40.92495));
#258155=CARTESIAN_POINT('Ctrl Pts',(-43.6735798167939,30.0952766307242,
-40.8666166666667));
#258156=CARTESIAN_POINT('Ctrl Pts',(-42.8392071752677,30.5770018999139,
-40.8082833333334));
#258157=CARTESIAN_POINT('Ctrl Pts',(-42.8392071752677,31.5404524382931,
-40.74995));
#258158=CARTESIAN_POINT('Ctrl Pts',(-42.8392071752677,32.5039029766724,
-40.6916166666667));
#258159=CARTESIAN_POINT('Ctrl Pts',(-43.6735798167939,32.985628245862,-40.6332833333334));
#258160=CARTESIAN_POINT('Ctrl Pts',(-44.5079524583201,33.4673535150516,
-40.57495));
#258161=CARTESIAN_POINT('Ctrl Pts',(-45.3423250998464,32.985628245862,-40.5166166666666));
#258162=CARTESIAN_POINT('Ctrl Pts',(-46.1766977413726,32.5039029766724,
-40.4582833333333));
#258163=CARTESIAN_POINT('Ctrl Pts',(-46.1766977413726,31.5404524382932,
-40.39995));
#258164=CARTESIAN_POINT('Ctrl Pts',(-46.1766977413726,30.5770018999139,
-40.3416166666667));
#258165=CARTESIAN_POINT('Ctrl Pts',(-45.3423250998464,30.0952766307242,
-40.2832833333334));
#258166=CARTESIAN_POINT('Ctrl Pts',(-44.5079524583202,29.6135513615346,
-40.22495));
#258167=CARTESIAN_POINT('Ctrl Pts',(-43.6735798167939,30.0952766307242,
-40.1666166666667));
#258168=CARTESIAN_POINT('Ctrl Pts',(-42.8392071752677,30.5770018999139,
-40.1082833333334));
#258169=CARTESIAN_POINT('Ctrl Pts',(-42.8392071752677,31.5404524382931,
-40.04995));
#258170=CARTESIAN_POINT('Ctrl Pts',(-42.8392071752677,32.5039029766724,
-39.9916166666667));
#258171=CARTESIAN_POINT('Ctrl Pts',(-43.6735798167939,32.985628245862,-39.9332833333333));
#258172=CARTESIAN_POINT('Ctrl Pts',(-44.5079524583201,33.4673535150516,
-39.87495));
#258173=CARTESIAN_POINT('Ctrl Pts',(-45.3423250998464,32.985628245862,-39.8166166666667));
#258174=CARTESIAN_POINT('Ctrl Pts',(-46.1766977413726,32.5039029766724,
-39.7582833333334));
#258175=CARTESIAN_POINT('Ctrl Pts',(-46.1766977413726,31.5404524382932,
-39.69995));
#258176=CARTESIAN_POINT('Ctrl Pts',(-46.1766977413726,30.5770018999139,
-39.6416166666667));
#258177=CARTESIAN_POINT('Ctrl Pts',(-45.3423250998464,30.0952766307242,
-39.5832833333333));
#258178=CARTESIAN_POINT('Ctrl Pts',(-44.5079524583202,29.6135513615346,
-39.52495));
#258179=CARTESIAN_POINT('Ctrl Pts',(-43.6735798167939,30.0952766307242,
-39.4666166666667));
#258180=CARTESIAN_POINT('Ctrl Pts',(-42.8392071752677,30.5770018999139,
-39.4082833333333));
#258181=CARTESIAN_POINT('Ctrl Pts',(-42.8392071752677,31.5404524382931,
-39.34995));
#258182=CARTESIAN_POINT('Ctrl Pts',(-42.8392071752677,32.5039029766724,
-39.2916166666667));
#258183=CARTESIAN_POINT('Ctrl Pts',(-43.6735798167939,32.985628245862,-39.2332833333333));
#258184=CARTESIAN_POINT('Ctrl Pts',(-44.5079524583201,33.4673535150516,
-39.17495));
#258185=CARTESIAN_POINT('Ctrl Pts',(-45.3423250998464,32.985628245862,-39.1166166666667));
#258186=CARTESIAN_POINT('Ctrl Pts',(-46.1766977413726,32.5039029766724,
-39.0582833333333));
#258187=CARTESIAN_POINT('Ctrl Pts',(-46.1766977413726,31.5404524382932,
-38.99995));
#258188=CARTESIAN_POINT('Ctrl Pts',(-46.1766977413726,30.5770018999139,
-38.9416166666667));
#258189=CARTESIAN_POINT('Ctrl Pts',(-45.3423250998464,30.0952766307242,
-38.8832833333334));
#258190=CARTESIAN_POINT('Ctrl Pts',(-44.5079524583202,29.6135513615346,
-38.82495));
#258191=CARTESIAN_POINT('Ctrl Pts',(-43.6735798167939,30.0952766307242,
-38.7666166666667));
#258192=CARTESIAN_POINT('Ctrl Pts',(-42.8392071752677,30.5770018999139,
-38.7082833333333));
#258193=CARTESIAN_POINT('Ctrl Pts',(-42.8392071752677,31.5404524382931,
-38.64995));
#258194=CARTESIAN_POINT('Ctrl Pts',(-42.8392071752677,32.5039029766724,
-38.5916166666667));
#258195=CARTESIAN_POINT('Ctrl Pts',(-43.6735798167939,32.985628245862,-38.5332833333334));
#258196=CARTESIAN_POINT('Ctrl Pts',(-44.5079524583201,33.4673535150516,
-38.47495));
#258197=CARTESIAN_POINT('Ctrl Pts',(-45.3423250998464,32.985628245862,-38.4166166666667));
#258198=CARTESIAN_POINT('Ctrl Pts',(-46.1766977413726,32.5039029766724,
-38.3582833333333));
#258199=CARTESIAN_POINT('Ctrl Pts',(-46.1766977413726,31.5404524382932,
-38.29995));
#258200=CARTESIAN_POINT('Ctrl Pts',(-46.1766977413726,30.5770018999139,
-38.2416166666667));
#258201=CARTESIAN_POINT('Ctrl Pts',(-45.3423250998464,30.0952766307242,
-38.1832833333333));
#258202=CARTESIAN_POINT('Ctrl Pts',(-44.5079524583202,29.6135513615346,
-38.12495));
#258203=CARTESIAN_POINT('Ctrl Pts',(-43.6735798167939,30.0952766307242,
-38.0666166666667));
#258204=CARTESIAN_POINT('Ctrl Pts',(-42.8392071752677,30.5770018999139,
-38.0082833333333));
#258205=CARTESIAN_POINT('Ctrl Pts',(-42.8392071752677,31.5404524382931,
-37.94995));
#258206=CARTESIAN_POINT('Ctrl Pts',(-42.8392071752677,32.5039029766724,
-37.8916166666667));
#258207=CARTESIAN_POINT('Ctrl Pts',(-43.6735798167939,32.985628245862,-37.8332833333334));
#258208=CARTESIAN_POINT('Ctrl Pts',(-44.5079524583201,33.4673535150516,
-37.77495));
#258209=CARTESIAN_POINT('Ctrl Pts',(-45.3423250998464,32.985628245862,-37.7166166666667));
#258210=CARTESIAN_POINT('Ctrl Pts',(-46.1766977413726,32.5039029766724,
-37.6582833333333));
#258211=CARTESIAN_POINT('Ctrl Pts',(-46.1766977413726,31.5404524382932,
-37.59995));
#258212=CARTESIAN_POINT('Ctrl Pts',(-46.1766977413726,30.5770018999139,
-37.5416166666667));
#258213=CARTESIAN_POINT('Ctrl Pts',(-45.3423250998464,30.0952766307242,
-37.4832833333334));
#258214=CARTESIAN_POINT('Ctrl Pts',(-44.5079524583202,29.6135513615346,
-37.42495));
#258215=CARTESIAN_POINT('Ctrl Pts',(-43.6735798167939,30.0952766307242,
-37.3666166666667));
#258216=CARTESIAN_POINT('Ctrl Pts',(-42.8392071752677,30.5770018999139,
-37.3082833333333));
#258217=CARTESIAN_POINT('Ctrl Pts',(-42.8392071752677,31.5404524382931,
-37.24995));
#258218=CARTESIAN_POINT('Ctrl Pts',(-42.8392071752677,32.5039029766724,
-37.1916166666667));
#258219=CARTESIAN_POINT('Ctrl Pts',(-43.6735798167939,32.985628245862,-37.1332833333334));
#258220=CARTESIAN_POINT('Ctrl Pts',(-44.5079524583201,33.4673535150516,
-37.07495));
#258221=CARTESIAN_POINT('Ctrl Pts',(-45.3423250998464,32.985628245862,-37.0166166666667));
#258222=CARTESIAN_POINT('Ctrl Pts',(-45.4506530446704,32.9230850777571,
-37.0090431559831));
#258223=CARTESIAN_POINT('Ctrl Pts',(-45.5484465834729,32.8450913903532,
-37.0009024189827));
#258224=CARTESIAN_POINT('Ctrl Pts',(-46.5766932247455,31.5404524382932,
-53.2308875));
#258225=CARTESIAN_POINT('Ctrl Pts',(-46.5766932247455,30.3460643999139,
-53.1725541666667));
#258226=CARTESIAN_POINT('Ctrl Pts',(-45.5423228415329,29.7488703807243,
-53.1142208333334));
#258227=CARTESIAN_POINT('Ctrl Pts',(-44.5079524583202,29.1516763615346,
-53.0558875000001));
#258228=CARTESIAN_POINT('Ctrl Pts',(-43.4735820751074,29.7488703807243,
-52.9975541666667));
#258229=CARTESIAN_POINT('Ctrl Pts',(-42.4392116918948,30.3460643999138,
-52.9392208333334));
#258230=CARTESIAN_POINT('Ctrl Pts',(-42.4392116918948,31.5404524382931,
-52.8808875));
#258231=CARTESIAN_POINT('Ctrl Pts',(-42.4392116918947,32.7348404766723,
-52.8225541666667));
#258232=CARTESIAN_POINT('Ctrl Pts',(-43.4735820751074,33.332034495862,-52.7642208333334));
#258233=CARTESIAN_POINT('Ctrl Pts',(-44.5079524583201,33.9292285150516,
-52.7058875));
#258234=CARTESIAN_POINT('Ctrl Pts',(-45.5423228415328,33.332034495862,-52.6475541666667));
#258235=CARTESIAN_POINT('Ctrl Pts',(-46.5766932247455,32.7348404766724,
-52.5892208333333));
#258236=CARTESIAN_POINT('Ctrl Pts',(-46.5766932247455,31.5404524382932,
-52.5308875));
#258237=CARTESIAN_POINT('Ctrl Pts',(-46.5766932247455,30.3460643999139,
-52.4725541666667));
#258238=CARTESIAN_POINT('Ctrl Pts',(-45.5423228415329,29.7488703807243,
-52.4142208333333));
#258239=CARTESIAN_POINT('Ctrl Pts',(-44.5079524583202,29.1516763615346,
-52.3558875000001));
#258240=CARTESIAN_POINT('Ctrl Pts',(-43.4735820751074,29.7488703807243,
-52.2975541666667));
#258241=CARTESIAN_POINT('Ctrl Pts',(-42.4392116918948,30.3460643999138,
-52.2392208333334));
#258242=CARTESIAN_POINT('Ctrl Pts',(-42.4392116918948,31.5404524382931,
-52.1808875));
#258243=CARTESIAN_POINT('Ctrl Pts',(-42.4392116918947,32.7348404766723,
-52.1225541666667));
#258244=CARTESIAN_POINT('Ctrl Pts',(-43.4735820751074,33.332034495862,-52.0642208333334));
#258245=CARTESIAN_POINT('Ctrl Pts',(-44.5079524583201,33.9292285150516,
-52.0058875));
#258246=CARTESIAN_POINT('Ctrl Pts',(-45.5423228415328,33.332034495862,-51.9475541666667));
#258247=CARTESIAN_POINT('Ctrl Pts',(-46.5766932247455,32.7348404766724,
-51.8892208333334));
#258248=CARTESIAN_POINT('Ctrl Pts',(-46.5766932247455,31.5404524382932,
-51.8308875));
#258249=CARTESIAN_POINT('Ctrl Pts',(-46.5766932247455,30.3460643999139,
-51.7725541666667));
#258250=CARTESIAN_POINT('Ctrl Pts',(-45.5423228415329,29.7488703807243,
-51.7142208333334));
#258251=CARTESIAN_POINT('Ctrl Pts',(-44.5079524583202,29.1516763615346,
-51.6558875));
#258252=CARTESIAN_POINT('Ctrl Pts',(-43.4735820751074,29.7488703807243,
-51.5975541666667));
#258253=CARTESIAN_POINT('Ctrl Pts',(-42.4392116918948,30.3460643999138,
-51.5392208333333));
#258254=CARTESIAN_POINT('Ctrl Pts',(-42.4392116918948,31.5404524382931,
-51.4808875));
#258255=CARTESIAN_POINT('Ctrl Pts',(-42.4392116918947,32.7348404766723,
-51.4225541666667));
#258256=CARTESIAN_POINT('Ctrl Pts',(-43.4735820751074,33.332034495862,-51.3642208333334));
#258257=CARTESIAN_POINT('Ctrl Pts',(-44.5079524583201,33.9292285150516,
-51.3058875));
#258258=CARTESIAN_POINT('Ctrl Pts',(-45.5423228415328,33.332034495862,-51.2475541666667));
#258259=CARTESIAN_POINT('Ctrl Pts',(-46.5766932247455,32.7348404766724,
-51.1892208333333));
#258260=CARTESIAN_POINT('Ctrl Pts',(-46.5766932247455,31.5404524382932,
-51.1308875));
#258261=CARTESIAN_POINT('Ctrl Pts',(-46.5766932247455,30.3460643999139,
-51.0725541666667));
#258262=CARTESIAN_POINT('Ctrl Pts',(-45.5423228415329,29.7488703807243,
-51.0142208333334));
#258263=CARTESIAN_POINT('Ctrl Pts',(-44.5079524583202,29.1516763615346,
-50.9558875));
#258264=CARTESIAN_POINT('Ctrl Pts',(-43.4735820751074,29.7488703807243,
-50.8975541666667));
#258265=CARTESIAN_POINT('Ctrl Pts',(-42.4392116918948,30.3460643999138,
-50.8392208333333));
#258266=CARTESIAN_POINT('Ctrl Pts',(-42.4392116918948,31.5404524382931,
-50.7808875));
#258267=CARTESIAN_POINT('Ctrl Pts',(-42.4392116918947,32.7348404766723,
-50.7225541666666));
#258268=CARTESIAN_POINT('Ctrl Pts',(-43.4735820751074,33.332034495862,-50.6642208333333));
#258269=CARTESIAN_POINT('Ctrl Pts',(-44.5079524583201,33.9292285150516,
-50.6058875));
#258270=CARTESIAN_POINT('Ctrl Pts',(-45.5423228415328,33.332034495862,-50.5475541666667));
#258271=CARTESIAN_POINT('Ctrl Pts',(-46.5766932247455,32.7348404766724,
-50.4892208333333));
#258272=CARTESIAN_POINT('Ctrl Pts',(-46.5766932247455,31.5404524382932,
-50.4308875));
#258273=CARTESIAN_POINT('Ctrl Pts',(-46.5766932247455,30.3460643999139,
-50.3725541666667));
#258274=CARTESIAN_POINT('Ctrl Pts',(-45.5423228415329,29.7488703807243,
-50.3142208333334));
#258275=CARTESIAN_POINT('Ctrl Pts',(-44.5079524583202,29.1516763615346,
-50.2558875));
#258276=CARTESIAN_POINT('Ctrl Pts',(-43.4735820751074,29.7488703807243,
-50.1975541666667));
#258277=CARTESIAN_POINT('Ctrl Pts',(-42.4392116918948,30.3460643999138,
-50.1392208333333));
#258278=CARTESIAN_POINT('Ctrl Pts',(-42.4392116918948,31.5404524382931,
-50.0808875));
#258279=CARTESIAN_POINT('Ctrl Pts',(-42.4392116918947,32.7348404766723,
-50.0225541666667));
#258280=CARTESIAN_POINT('Ctrl Pts',(-43.4735820751074,33.332034495862,-49.9642208333334));
#258281=CARTESIAN_POINT('Ctrl Pts',(-44.5079524583201,33.9292285150516,
-49.9058875));
#258282=CARTESIAN_POINT('Ctrl Pts',(-45.5423228415328,33.332034495862,-49.8475541666667));
#258283=CARTESIAN_POINT('Ctrl Pts',(-46.5766932247455,32.7348404766724,
-49.7892208333333));
#258284=CARTESIAN_POINT('Ctrl Pts',(-46.5766932247455,31.5404524382932,
-49.7308875));
#258285=CARTESIAN_POINT('Ctrl Pts',(-46.5766932247455,30.3460643999139,
-49.6725541666667));
#258286=CARTESIAN_POINT('Ctrl Pts',(-45.5423228415329,29.7488703807243,
-49.6142208333334));
#258287=CARTESIAN_POINT('Ctrl Pts',(-44.5079524583202,29.1516763615346,
-49.5558875));
#258288=CARTESIAN_POINT('Ctrl Pts',(-43.4735820751074,29.7488703807243,
-49.4975541666667));
#258289=CARTESIAN_POINT('Ctrl Pts',(-42.4392116918948,30.3460643999138,
-49.4392208333333));
#258290=CARTESIAN_POINT('Ctrl Pts',(-42.4392116918948,31.5404524382931,
-49.3808875));
#258291=CARTESIAN_POINT('Ctrl Pts',(-42.4392116918947,32.7348404766723,
-49.3225541666667));
#258292=CARTESIAN_POINT('Ctrl Pts',(-43.4735820751074,33.332034495862,-49.2642208333334));
#258293=CARTESIAN_POINT('Ctrl Pts',(-44.5079524583201,33.9292285150516,
-49.2058875));
#258294=CARTESIAN_POINT('Ctrl Pts',(-45.5423228415328,33.332034495862,-49.1475541666667));
#258295=CARTESIAN_POINT('Ctrl Pts',(-46.5766932247455,32.7348404766724,
-49.0892208333333));
#258296=CARTESIAN_POINT('Ctrl Pts',(-46.5766932247455,31.5404524382932,
-49.0308875));
#258297=CARTESIAN_POINT('Ctrl Pts',(-46.5766932247455,30.3460643999139,
-48.9725541666667));
#258298=CARTESIAN_POINT('Ctrl Pts',(-45.5423228415329,29.7488703807243,
-48.9142208333333));
#258299=CARTESIAN_POINT('Ctrl Pts',(-44.5079524583202,29.1516763615346,
-48.8558875));
#258300=CARTESIAN_POINT('Ctrl Pts',(-43.4735820751074,29.7488703807243,
-48.7975541666667));
#258301=CARTESIAN_POINT('Ctrl Pts',(-42.4392116918948,30.3460643999138,
-48.7392208333334));
#258302=CARTESIAN_POINT('Ctrl Pts',(-42.4392116918948,31.5404524382931,
-48.6808875));
#258303=CARTESIAN_POINT('Ctrl Pts',(-42.4392116918947,32.7348404766723,
-48.6225541666667));
#258304=CARTESIAN_POINT('Ctrl Pts',(-43.4735820751074,33.332034495862,-48.5642208333334));
#258305=CARTESIAN_POINT('Ctrl Pts',(-44.5079524583201,33.9292285150516,
-48.5058875));
#258306=CARTESIAN_POINT('Ctrl Pts',(-45.5423228415328,33.332034495862,-48.4475541666667));
#258307=CARTESIAN_POINT('Ctrl Pts',(-46.5766932247455,32.7348404766724,
-48.3892208333334));
#258308=CARTESIAN_POINT('Ctrl Pts',(-46.5766932247455,31.5404524382932,
-48.3308875));
#258309=CARTESIAN_POINT('Ctrl Pts',(-46.5766932247455,30.3460643999139,
-48.2725541666667));
#258310=CARTESIAN_POINT('Ctrl Pts',(-45.5423228415329,29.7488703807243,
-48.2142208333334));
#258311=CARTESIAN_POINT('Ctrl Pts',(-44.5079524583202,29.1516763615346,
-48.1558875));
#258312=CARTESIAN_POINT('Ctrl Pts',(-43.4735820751074,29.7488703807243,
-48.0975541666667));
#258313=CARTESIAN_POINT('Ctrl Pts',(-42.4392116918948,30.3460643999138,
-48.0392208333334));
#258314=CARTESIAN_POINT('Ctrl Pts',(-42.4392116918948,31.5404524382931,
-47.9808875));
#258315=CARTESIAN_POINT('Ctrl Pts',(-42.4392116918947,32.7348404766723,
-47.9225541666667));
#258316=CARTESIAN_POINT('Ctrl Pts',(-43.4735820751074,33.332034495862,-47.8642208333334));
#258317=CARTESIAN_POINT('Ctrl Pts',(-44.5079524583201,33.9292285150516,
-47.8058875000001));
#258318=CARTESIAN_POINT('Ctrl Pts',(-45.5423228415328,33.332034495862,-47.7475541666667));
#258319=CARTESIAN_POINT('Ctrl Pts',(-46.5766932247455,32.7348404766724,
-47.6892208333334));
#258320=CARTESIAN_POINT('Ctrl Pts',(-46.5766932247455,31.5404524382932,
-47.6308875));
#258321=CARTESIAN_POINT('Ctrl Pts',(-46.5766932247455,30.3460643999139,
-47.5725541666667));
#258322=CARTESIAN_POINT('Ctrl Pts',(-45.5423228415329,29.7488703807243,
-47.5142208333333));
#258323=CARTESIAN_POINT('Ctrl Pts',(-44.5079524583202,29.1516763615346,
-47.4558875));
#258324=CARTESIAN_POINT('Ctrl Pts',(-43.4735820751074,29.7488703807243,
-47.3975541666667));
#258325=CARTESIAN_POINT('Ctrl Pts',(-42.4392116918948,30.3460643999138,
-47.3392208333333));
#258326=CARTESIAN_POINT('Ctrl Pts',(-42.4392116918948,31.5404524382931,
-47.2808875));
#258327=CARTESIAN_POINT('Ctrl Pts',(-42.4392116918947,32.7348404766723,
-47.2225541666667));
#258328=CARTESIAN_POINT('Ctrl Pts',(-43.4735820751074,33.332034495862,-47.1642208333334));
#258329=CARTESIAN_POINT('Ctrl Pts',(-44.5079524583201,33.9292285150516,
-47.1058875));
#258330=CARTESIAN_POINT('Ctrl Pts',(-45.5423228415328,33.332034495862,-47.0475541666667));
#258331=CARTESIAN_POINT('Ctrl Pts',(-46.5766932247455,32.7348404766724,
-46.9892208333334));
#258332=CARTESIAN_POINT('Ctrl Pts',(-46.5766932247455,31.5404524382932,
-46.9308875));
#258333=CARTESIAN_POINT('Ctrl Pts',(-46.5766932247455,30.3460643999139,
-46.8725541666667));
#258334=CARTESIAN_POINT('Ctrl Pts',(-45.5423228415329,29.7488703807243,
-46.8142208333334));
#258335=CARTESIAN_POINT('Ctrl Pts',(-44.5079524583202,29.1516763615346,
-46.7558875));
#258336=CARTESIAN_POINT('Ctrl Pts',(-43.4735820751074,29.7488703807243,
-46.6975541666667));
#258337=CARTESIAN_POINT('Ctrl Pts',(-42.4392116918948,30.3460643999138,
-46.6392208333333));
#258338=CARTESIAN_POINT('Ctrl Pts',(-42.4392116918948,31.5404524382931,
-46.5808875));
#258339=CARTESIAN_POINT('Ctrl Pts',(-42.4392116918948,32.7348404766723,
-46.5225541666667));
#258340=CARTESIAN_POINT('Ctrl Pts',(-43.4735820751074,33.332034495862,-46.4642208333334));
#258341=CARTESIAN_POINT('Ctrl Pts',(-44.5079524583201,33.9292285150516,
-46.4058875));
#258342=CARTESIAN_POINT('Ctrl Pts',(-45.5423228415328,33.332034495862,-46.3475541666667));
#258343=CARTESIAN_POINT('Ctrl Pts',(-46.5766932247455,32.7348404766724,
-46.2892208333334));
#258344=CARTESIAN_POINT('Ctrl Pts',(-46.5766932247455,31.5404524382932,
-46.2308875));
#258345=CARTESIAN_POINT('Ctrl Pts',(-46.5766932247455,30.3460643999139,
-46.1725541666667));
#258346=CARTESIAN_POINT('Ctrl Pts',(-45.5423228415329,29.7488703807243,
-46.1142208333334));
#258347=CARTESIAN_POINT('Ctrl Pts',(-44.5079524583202,29.1516763615346,
-46.0558875));
#258348=CARTESIAN_POINT('Ctrl Pts',(-43.4735820751074,29.7488703807243,
-45.9975541666667));
#258349=CARTESIAN_POINT('Ctrl Pts',(-42.4392116918948,30.3460643999138,
-45.9392208333333));
#258350=CARTESIAN_POINT('Ctrl Pts',(-42.4392116918948,31.5404524382931,
-45.8808875));
#258351=CARTESIAN_POINT('Ctrl Pts',(-42.4392116918948,32.7348404766723,
-45.8225541666667));
#258352=CARTESIAN_POINT('Ctrl Pts',(-43.4735820751074,33.332034495862,-45.7642208333334));
#258353=CARTESIAN_POINT('Ctrl Pts',(-44.5079524583201,33.9292285150516,
-45.7058875));
#258354=CARTESIAN_POINT('Ctrl Pts',(-45.5423228415328,33.332034495862,-45.6475541666667));
#258355=CARTESIAN_POINT('Ctrl Pts',(-46.5766932247455,32.7348404766724,
-45.5892208333333));
#258356=CARTESIAN_POINT('Ctrl Pts',(-46.5766932247455,31.5404524382932,
-45.5308875));
#258357=CARTESIAN_POINT('Ctrl Pts',(-46.5766932247455,30.3460643999139,
-45.4725541666667));
#258358=CARTESIAN_POINT('Ctrl Pts',(-45.5423228415329,29.7488703807243,
-45.4142208333334));
#258359=CARTESIAN_POINT('Ctrl Pts',(-44.5079524583202,29.1516763615346,
-45.3558875));
#258360=CARTESIAN_POINT('Ctrl Pts',(-43.4735820751074,29.7488703807243,
-45.2975541666667));
#258361=CARTESIAN_POINT('Ctrl Pts',(-42.4392116918948,30.3460643999138,
-45.2392208333333));
#258362=CARTESIAN_POINT('Ctrl Pts',(-42.4392116918948,31.5404524382931,
-45.1808875));
#258363=CARTESIAN_POINT('Ctrl Pts',(-42.4392116918948,32.7348404766723,
-45.1225541666667));
#258364=CARTESIAN_POINT('Ctrl Pts',(-43.4735820751074,33.332034495862,-45.0642208333334));
#258365=CARTESIAN_POINT('Ctrl Pts',(-44.5079524583201,33.9292285150516,
-45.0058875));
#258366=CARTESIAN_POINT('Ctrl Pts',(-45.5423228415328,33.332034495862,-44.9475541666667));
#258367=CARTESIAN_POINT('Ctrl Pts',(-46.5766932247455,32.7348404766724,
-44.8892208333333));
#258368=CARTESIAN_POINT('Ctrl Pts',(-46.5766932247455,31.5404524382932,
-44.8308875));
#258369=CARTESIAN_POINT('Ctrl Pts',(-46.5766932247455,30.3460643999139,
-44.7725541666666));
#258370=CARTESIAN_POINT('Ctrl Pts',(-45.5423228415329,29.7488703807243,
-44.7142208333334));
#258371=CARTESIAN_POINT('Ctrl Pts',(-44.5079524583202,29.1516763615346,
-44.6558875));
#258372=CARTESIAN_POINT('Ctrl Pts',(-43.4735820751074,29.7488703807243,
-44.5975541666667));
#258373=CARTESIAN_POINT('Ctrl Pts',(-42.4392116918948,30.3460643999138,
-44.5392208333333));
#258374=CARTESIAN_POINT('Ctrl Pts',(-42.4392116918948,31.5404524382931,
-44.4808875));
#258375=CARTESIAN_POINT('Ctrl Pts',(-42.4392116918948,32.7348404766723,
-44.4225541666667));
#258376=CARTESIAN_POINT('Ctrl Pts',(-43.4735820751074,33.332034495862,-44.3642208333333));
#258377=CARTESIAN_POINT('Ctrl Pts',(-44.5079524583201,33.9292285150516,
-44.3058875));
#258378=CARTESIAN_POINT('Ctrl Pts',(-45.5423228415328,33.332034495862,-44.2475541666667));
#258379=CARTESIAN_POINT('Ctrl Pts',(-46.5766932247455,32.7348404766724,
-44.1892208333334));
#258380=CARTESIAN_POINT('Ctrl Pts',(-46.5766932247455,31.5404524382932,
-44.1308875));
#258381=CARTESIAN_POINT('Ctrl Pts',(-46.5766932247455,30.3460643999139,
-44.0725541666667));
#258382=CARTESIAN_POINT('Ctrl Pts',(-45.5423228415329,29.7488703807243,
-44.0142208333334));
#258383=CARTESIAN_POINT('Ctrl Pts',(-44.5079524583202,29.1516763615346,
-43.9558875));
#258384=CARTESIAN_POINT('Ctrl Pts',(-43.4735820751074,29.7488703807243,
-43.8975541666667));
#258385=CARTESIAN_POINT('Ctrl Pts',(-42.4392116918948,30.3460643999138,
-43.8392208333333));
#258386=CARTESIAN_POINT('Ctrl Pts',(-42.4392116918948,31.5404524382931,
-43.7808875));
#258387=CARTESIAN_POINT('Ctrl Pts',(-42.4392116918948,32.7348404766723,
-43.7225541666667));
#258388=CARTESIAN_POINT('Ctrl Pts',(-43.4735820751074,33.332034495862,-43.6642208333334));
#258389=CARTESIAN_POINT('Ctrl Pts',(-44.5079524583201,33.9292285150516,
-43.6058875));
#258390=CARTESIAN_POINT('Ctrl Pts',(-45.5423228415328,33.332034495862,-43.5475541666667));
#258391=CARTESIAN_POINT('Ctrl Pts',(-46.5766932247455,32.7348404766724,
-43.4892208333333));
#258392=CARTESIAN_POINT('Ctrl Pts',(-46.5766932247455,31.5404524382932,
-43.4308875));
#258393=CARTESIAN_POINT('Ctrl Pts',(-46.5766932247455,30.3460643999139,
-43.3725541666667));
#258394=CARTESIAN_POINT('Ctrl Pts',(-45.5423228415329,29.7488703807243,
-43.3142208333334));
#258395=CARTESIAN_POINT('Ctrl Pts',(-44.5079524583202,29.1516763615346,
-43.2558875));
#258396=CARTESIAN_POINT('Ctrl Pts',(-43.4735820751074,29.7488703807243,
-43.1975541666667));
#258397=CARTESIAN_POINT('Ctrl Pts',(-42.4392116918948,30.3460643999138,
-43.1392208333334));
#258398=CARTESIAN_POINT('Ctrl Pts',(-42.4392116918948,31.5404524382931,
-43.0808875));
#258399=CARTESIAN_POINT('Ctrl Pts',(-42.4392116918948,32.7348404766723,
-43.0225541666667));
#258400=CARTESIAN_POINT('Ctrl Pts',(-43.4735820751074,33.332034495862,-42.9642208333334));
#258401=CARTESIAN_POINT('Ctrl Pts',(-44.5079524583201,33.9292285150516,
-42.9058875));
#258402=CARTESIAN_POINT('Ctrl Pts',(-45.5423228415328,33.332034495862,-42.8475541666667));
#258403=CARTESIAN_POINT('Ctrl Pts',(-46.5766932247455,32.7348404766724,
-42.7892208333334));
#258404=CARTESIAN_POINT('Ctrl Pts',(-46.5766932247455,31.5404524382932,
-42.7308875));
#258405=CARTESIAN_POINT('Ctrl Pts',(-46.5766932247455,30.3460643999139,
-42.6725541666667));
#258406=CARTESIAN_POINT('Ctrl Pts',(-45.5423228415329,29.7488703807243,
-42.6142208333334));
#258407=CARTESIAN_POINT('Ctrl Pts',(-44.5079524583202,29.1516763615346,
-42.5558875));
#258408=CARTESIAN_POINT('Ctrl Pts',(-43.4735820751074,29.7488703807243,
-42.4975541666667));
#258409=CARTESIAN_POINT('Ctrl Pts',(-42.4392116918948,30.3460643999138,
-42.4392208333334));
#258410=CARTESIAN_POINT('Ctrl Pts',(-42.4392116918948,31.5404524382931,
-42.3808875));
#258411=CARTESIAN_POINT('Ctrl Pts',(-42.4392116918948,32.7348404766723,
-42.3225541666667));
#258412=CARTESIAN_POINT('Ctrl Pts',(-43.4735820751074,33.332034495862,-42.2642208333334));
#258413=CARTESIAN_POINT('Ctrl Pts',(-44.5079524583201,33.9292285150516,
-42.2058875));
#258414=CARTESIAN_POINT('Ctrl Pts',(-45.5423228415328,33.332034495862,-42.1475541666667));
#258415=CARTESIAN_POINT('Ctrl Pts',(-46.5766932247455,32.7348404766724,
-42.0892208333333));
#258416=CARTESIAN_POINT('Ctrl Pts',(-46.5766932247455,31.5404524382932,
-42.0308875));
#258417=CARTESIAN_POINT('Ctrl Pts',(-46.5766932247455,30.3460643999139,
-41.9725541666667));
#258418=CARTESIAN_POINT('Ctrl Pts',(-45.5423228415329,29.7488703807243,
-41.9142208333334));
#258419=CARTESIAN_POINT('Ctrl Pts',(-44.5079524583202,29.1516763615346,
-41.8558875));
#258420=CARTESIAN_POINT('Ctrl Pts',(-43.4735820751074,29.7488703807243,
-41.7975541666667));
#258421=CARTESIAN_POINT('Ctrl Pts',(-42.4392116918948,30.3460643999138,
-41.7392208333333));
#258422=CARTESIAN_POINT('Ctrl Pts',(-42.4392116918948,31.5404524382931,
-41.6808875));
#258423=CARTESIAN_POINT('Ctrl Pts',(-42.4392116918948,32.7348404766723,
-41.6225541666667));
#258424=CARTESIAN_POINT('Ctrl Pts',(-43.4735820751074,33.332034495862,-41.5642208333334));
#258425=CARTESIAN_POINT('Ctrl Pts',(-44.5079524583201,33.9292285150516,
-41.5058875));
#258426=CARTESIAN_POINT('Ctrl Pts',(-45.5423228415328,33.332034495862,-41.4475541666667));
#258427=CARTESIAN_POINT('Ctrl Pts',(-46.5766932247455,32.7348404766724,
-41.3892208333333));
#258428=CARTESIAN_POINT('Ctrl Pts',(-46.5766932247455,31.5404524382932,
-41.3308875));
#258429=CARTESIAN_POINT('Ctrl Pts',(-46.5766932247455,30.3460643999139,
-41.2725541666667));
#258430=CARTESIAN_POINT('Ctrl Pts',(-45.5423228415329,29.7488703807243,
-41.2142208333333));
#258431=CARTESIAN_POINT('Ctrl Pts',(-44.5079524583202,29.1516763615346,
-41.1558875));
#258432=CARTESIAN_POINT('Ctrl Pts',(-43.4735820751074,29.7488703807243,
-41.0975541666667));
#258433=CARTESIAN_POINT('Ctrl Pts',(-42.4392116918948,30.3460643999138,
-41.0392208333333));
#258434=CARTESIAN_POINT('Ctrl Pts',(-42.4392116918948,31.5404524382931,
-40.9808875));
#258435=CARTESIAN_POINT('Ctrl Pts',(-42.4392116918948,32.7348404766723,
-40.9225541666667));
#258436=CARTESIAN_POINT('Ctrl Pts',(-43.4735820751074,33.332034495862,-40.8642208333334));
#258437=CARTESIAN_POINT('Ctrl Pts',(-44.5079524583201,33.9292285150516,
-40.8058875));
#258438=CARTESIAN_POINT('Ctrl Pts',(-45.5423228415328,33.332034495862,-40.7475541666667));
#258439=CARTESIAN_POINT('Ctrl Pts',(-46.5766932247455,32.7348404766724,
-40.6892208333333));
#258440=CARTESIAN_POINT('Ctrl Pts',(-46.5766932247455,31.5404524382932,
-40.6308875));
#258441=CARTESIAN_POINT('Ctrl Pts',(-46.5766932247455,30.3460643999139,
-40.5725541666667));
#258442=CARTESIAN_POINT('Ctrl Pts',(-45.5423228415329,29.7488703807243,
-40.5142208333333));
#258443=CARTESIAN_POINT('Ctrl Pts',(-44.5079524583202,29.1516763615346,
-40.4558875));
#258444=CARTESIAN_POINT('Ctrl Pts',(-43.4735820751074,29.7488703807243,
-40.3975541666667));
#258445=CARTESIAN_POINT('Ctrl Pts',(-42.4392116918948,30.3460643999138,
-40.3392208333333));
#258446=CARTESIAN_POINT('Ctrl Pts',(-42.4392116918948,31.5404524382931,
-40.2808875));
#258447=CARTESIAN_POINT('Ctrl Pts',(-42.4392116918948,32.7348404766723,
-40.2225541666667));
#258448=CARTESIAN_POINT('Ctrl Pts',(-43.4735820751074,33.332034495862,-40.1642208333333));
#258449=CARTESIAN_POINT('Ctrl Pts',(-44.5079524583201,33.9292285150516,
-40.1058875));
#258450=CARTESIAN_POINT('Ctrl Pts',(-45.5423228415328,33.332034495862,-40.0475541666667));
#258451=CARTESIAN_POINT('Ctrl Pts',(-46.5766932247455,32.7348404766724,
-39.9892208333333));
#258452=CARTESIAN_POINT('Ctrl Pts',(-46.5766932247455,31.5404524382932,
-39.9308875));
#258453=CARTESIAN_POINT('Ctrl Pts',(-46.5766932247455,30.3460643999139,
-39.8725541666667));
#258454=CARTESIAN_POINT('Ctrl Pts',(-45.5423228415329,29.7488703807243,
-39.8142208333334));
#258455=CARTESIAN_POINT('Ctrl Pts',(-44.5079524583202,29.1516763615346,
-39.7558875));
#258456=CARTESIAN_POINT('Ctrl Pts',(-43.4735820751074,29.7488703807243,
-39.6975541666667));
#258457=CARTESIAN_POINT('Ctrl Pts',(-42.4392116918948,30.3460643999138,
-39.6392208333334));
#258458=CARTESIAN_POINT('Ctrl Pts',(-42.4392116918948,31.5404524382931,
-39.5808875));
#258459=CARTESIAN_POINT('Ctrl Pts',(-42.4392116918948,32.7348404766723,
-39.5225541666667));
#258460=CARTESIAN_POINT('Ctrl Pts',(-43.4735820751074,33.332034495862,-39.4642208333333));
#258461=CARTESIAN_POINT('Ctrl Pts',(-44.5079524583201,33.9292285150516,
-39.4058875));
#258462=CARTESIAN_POINT('Ctrl Pts',(-45.5423228415328,33.332034495862,-39.3475541666667));
#258463=CARTESIAN_POINT('Ctrl Pts',(-46.5766932247455,32.7348404766724,
-39.2892208333334));
#258464=CARTESIAN_POINT('Ctrl Pts',(-46.5766932247455,31.5404524382932,
-39.2308875));
#258465=CARTESIAN_POINT('Ctrl Pts',(-46.5766932247455,30.3460643999139,
-39.1725541666667));
#258466=CARTESIAN_POINT('Ctrl Pts',(-45.5423228415329,29.7488703807243,
-39.1142208333333));
#258467=CARTESIAN_POINT('Ctrl Pts',(-44.5079524583202,29.1516763615346,
-39.0558875));
#258468=CARTESIAN_POINT('Ctrl Pts',(-43.4735820751074,29.7488703807243,
-38.9975541666667));
#258469=CARTESIAN_POINT('Ctrl Pts',(-42.4392116918948,30.3460643999138,
-38.9392208333334));
#258470=CARTESIAN_POINT('Ctrl Pts',(-42.4392116918948,31.5404524382931,
-38.8808875));
#258471=CARTESIAN_POINT('Ctrl Pts',(-42.4392116918948,32.7348404766723,
-38.8225541666667));
#258472=CARTESIAN_POINT('Ctrl Pts',(-43.4735820751074,33.332034495862,-38.7642208333333));
#258473=CARTESIAN_POINT('Ctrl Pts',(-44.5079524583201,33.9292285150516,
-38.7058875));
#258474=CARTESIAN_POINT('Ctrl Pts',(-45.5423228415328,33.332034495862,-38.6475541666667));
#258475=CARTESIAN_POINT('Ctrl Pts',(-46.5766932247455,32.7348404766724,
-38.5892208333334));
#258476=CARTESIAN_POINT('Ctrl Pts',(-46.5766932247455,31.5404524382932,
-38.5308875));
#258477=CARTESIAN_POINT('Ctrl Pts',(-46.5766932247455,30.3460643999139,
-38.4725541666667));
#258478=CARTESIAN_POINT('Ctrl Pts',(-45.5423228415329,29.7488703807243,
-38.4142208333334));
#258479=CARTESIAN_POINT('Ctrl Pts',(-44.5079524583202,29.1516763615346,
-38.3558875));
#258480=CARTESIAN_POINT('Ctrl Pts',(-43.4735820751074,29.7488703807243,
-38.2975541666667));
#258481=CARTESIAN_POINT('Ctrl Pts',(-42.4392116918948,30.3460643999138,
-38.2392208333333));
#258482=CARTESIAN_POINT('Ctrl Pts',(-42.4392116918948,31.5404524382931,
-38.1808875));
#258483=CARTESIAN_POINT('Ctrl Pts',(-42.4392116918948,32.7348404766723,
-38.1225541666667));
#258484=CARTESIAN_POINT('Ctrl Pts',(-43.4735820751074,33.332034495862,-38.0642208333334));
#258485=CARTESIAN_POINT('Ctrl Pts',(-44.5079524583201,33.9292285150516,
-38.0058875));
#258486=CARTESIAN_POINT('Ctrl Pts',(-45.5423228415328,33.332034495862,-37.9475541666667));
#258487=CARTESIAN_POINT('Ctrl Pts',(-46.5766932247455,32.7348404766724,
-37.8892208333334));
#258488=CARTESIAN_POINT('Ctrl Pts',(-46.5766932247455,31.5404524382932,
-37.8308875));
#258489=CARTESIAN_POINT('Ctrl Pts',(-46.5766932247455,30.3460643999139,
-37.7725541666667));
#258490=CARTESIAN_POINT('Ctrl Pts',(-45.5423228415329,29.7488703807243,
-37.7142208333333));
#258491=CARTESIAN_POINT('Ctrl Pts',(-44.5079524583202,29.1516763615346,
-37.6558875));
#258492=CARTESIAN_POINT('Ctrl Pts',(-43.4735820751074,29.7488703807243,
-37.5975541666667));
#258493=CARTESIAN_POINT('Ctrl Pts',(-42.4392116918948,30.3460643999138,
-37.5392208333334));
#258494=CARTESIAN_POINT('Ctrl Pts',(-42.4392116918948,31.5404524382931,
-37.4808875));
#258495=CARTESIAN_POINT('Ctrl Pts',(-42.4392116918948,32.7348404766723,
-37.4225541666667));
#258496=CARTESIAN_POINT('Ctrl Pts',(-43.4735820751074,33.332034495862,-37.3642208333333));
#258497=CARTESIAN_POINT('Ctrl Pts',(-44.5079524583201,33.9292285150516,
-37.3058875));
#258498=CARTESIAN_POINT('Ctrl Pts',(-45.5423228415328,33.332034495862,-37.2475541666667));
#258499=CARTESIAN_POINT('Ctrl Pts',(-45.6766168155003,33.2544998338414,
-37.239980655983));
#258500=CARTESIAN_POINT('Ctrl Pts',(-45.7978513037523,33.1578111886089,
-37.2318399189827));
#258501=CARTESIAN_POINT('Ctrl Pts',(-42.8392071752677,31.5404524382931,
-52.64995));
#258502=CARTESIAN_POINT('Ctrl Pts',(-42.8226659458705,31.698184429907,-52.64995));
#258503=CARTESIAN_POINT('Ctrl Pts',(-42.8274712764285,31.857393032193,-52.64995));
#258504=CARTESIAN_POINT('Ctrl Pts',(-42.8786574174946,32.1643235021153,
-52.64995));
#258505=CARTESIAN_POINT('Ctrl Pts',(-42.9232286878865,32.3108921662114,
-52.64995));
#258506=CARTESIAN_POINT('Ctrl Pts',(-43.0750368173286,32.6461601401754,
-52.64995));
#258507=CARTESIAN_POINT('Ctrl Pts',(-43.199204951854,32.8244027472953,-52.64995));
#258508=CARTESIAN_POINT('Ctrl Pts',(-43.5542933457999,33.1754582937784,
-52.64995));
#258509=CARTESIAN_POINT('Ctrl Pts',(-43.7742269286882,33.2962963987312,
-52.64995));
#258510=CARTESIAN_POINT('Ctrl Pts',(-44.079508833452,33.4246330791964,-52.64995));
#258511=CARTESIAN_POINT('Ctrl Pts',(-44.2169771822674,33.4654712631672,
-52.64995));
#258512=CARTESIAN_POINT('Ctrl Pts',(-44.4991010430727,33.5166685395148,
-52.64995));
#258513=CARTESIAN_POINT('Ctrl Pts',(-44.6429009445464,33.526707841618,-52.64995));
#258514=CARTESIAN_POINT('Ctrl Pts',(-44.7865238868864,33.5209569091753,
-52.64995));
#258515=CARTESIAN_POINT('Ctrl Pts',(-45.4138902596022,33.323505073581,-40.0133536282584));
#258516=CARTESIAN_POINT('Ctrl Pts',(-45.2343960628182,33.4147029298636,
-40.0238241230707));
#258517=CARTESIAN_POINT('Ctrl Pts',(-45.0421833621338,33.4782627639555,
-40.0350365306106));
#258518=CARTESIAN_POINT('Ctrl Pts',(-44.6401461563769,33.546739741288,-40.0584887009463));
#258519=CARTESIAN_POINT('Ctrl Pts',(-44.4323784874203,33.5496690225212,
-40.0706084816355));
#258520=CARTESIAN_POINT('Ctrl Pts',(-43.965283865819,33.4836041701764,-40.0978556678955));
#258521=CARTESIAN_POINT('Ctrl Pts',(-43.7127963349201,33.3946236208596,
-40.1123894250198));
#258522=CARTESIAN_POINT('Ctrl Pts',(-43.2663921378172,33.1289396202989,
-40.1388314112441));
#258523=CARTESIAN_POINT('Ctrl Pts',(-43.0745867349475,32.9582604222257,
-40.1530481325778));
#258524=CARTESIAN_POINT('Ctrl Pts',(-42.7592677610395,32.5464128492502,
-40.1830507128567));
#258525=CARTESIAN_POINT('Ctrl Pts',(-42.6417717032953,32.3067654968633,
-40.1985842217561));
#258526=CARTESIAN_POINT('Ctrl Pts',(-42.5080675690629,31.8005712300943,
-40.2280559228371));
#258527=CARTESIAN_POINT('Ctrl Pts',(-42.491225438116,31.539507602342,-40.24075985994));
#258528=CARTESIAN_POINT('Ctrl Pts',(-42.5578673808582,31.0271940342069,
-40.2685847162115));
#258529=CARTESIAN_POINT('Ctrl Pts',(-42.6400423036273,30.7807512666597,
-40.2834313171333));
#258530=CARTESIAN_POINT('Ctrl Pts',(-42.8982610531121,30.3236941111856,
-40.3140523786047));
#258531=CARTESIAN_POINT('Ctrl Pts',(-43.0753335831877,30.1194513548329,
-40.3295349599719));
#258532=CARTESIAN_POINT('Ctrl Pts',(-43.4885359770171,29.801119579637,-40.3576682283675));
#258533=CARTESIAN_POINT('Ctrl Pts',(-43.7173503770357,29.6858775233593,
-40.3700815452588));
#258534=CARTESIAN_POINT('Ctrl Pts',(-44.1397209055691,29.5659481498849,
-40.39471982609));
#258535=CARTESIAN_POINT('Ctrl Pts',(-44.3235830214837,29.5404524382925,
-40.4054451161849));
#258536=CARTESIAN_POINT('Ctrl Pts',(-44.5079524583208,29.5404524382925,
-40.4162000000005));
#258537=CARTESIAN_POINT('Origin',(-44.5079524583206,-57.475452478349,235.35105));
#258538=CARTESIAN_POINT('',(-44.2366247616132,-55.4939425958135,-39.0141962777036));
#258539=CARTESIAN_POINT('Ctrl Pts',(-44.2366247583656,-55.4939426255002,
-39.0141963182746));
#258540=CARTESIAN_POINT('Ctrl Pts',(-44.2338595158803,-55.4943212705074,
-39.0136979066985));
#258541=CARTESIAN_POINT('Ctrl Pts',(-44.2310952123238,-55.494705686492,
-39.0132009363795));
#258542=CARTESIAN_POINT('Ctrl Pts',(-44.1959512291589,-55.4996679139964,
-39.0068980480834));
#258543=CARTESIAN_POINT('Ctrl Pts',(-44.1637009035284,-55.5050310901567,
-39.0012798595208));
#258544=CARTESIAN_POINT('Ctrl Pts',(-44.0994607677182,-55.5173400934252,
-38.9904230184279));
#258545=CARTESIAN_POINT('Ctrl Pts',(-44.0674709555852,-55.5242859080952,
-38.9851843621813));
#258546=CARTESIAN_POINT('Ctrl Pts',(-44.0037536572564,-55.5397721100658,
-38.9750906394313));
#258547=CARTESIAN_POINT('Ctrl Pts',(-43.9720261650696,-55.5483124604321,
-38.9702355633813));
#258548=CARTESIAN_POINT('Ctrl Pts',(-43.9088372843841,-55.5670115927043,
-38.9609158992096));
#258549=CARTESIAN_POINT('Ctrl Pts',(-43.877363149692,-55.5771759127617,
-38.9564497975263));
#258550=CARTESIAN_POINT('Ctrl Pts',(-43.8147378173409,-55.5991372642861,
-38.9479240409952));
#258551=CARTESIAN_POINT('Ctrl Pts',(-43.783451665776,-55.6109933882688,
-38.943848461355));
#258552=CARTESIAN_POINT('Ctrl Pts',(-43.7218906736911,-55.6361026235129,
-38.9361997181442));
#258553=CARTESIAN_POINT('Ctrl Pts',(-43.6915050002909,-55.6493890121587,
-38.9326103047847));
#258554=CARTESIAN_POINT('Ctrl Pts',(-43.631563048157,-55.6773880028563,
-38.9259028928878));
#258555=CARTESIAN_POINT('Ctrl Pts',(-43.601998052992,-55.6921031576597,
-38.9227836015923));
#258556=CARTESIAN_POINT('Ctrl Pts',(-43.5179303005816,-55.7365693660334,
-38.914462897476));
#258557=CARTESIAN_POINT('Ctrl Pts',(-43.4644496898179,-55.7681223775077,
-38.909852823657));
#258558=CARTESIAN_POINT('Ctrl Pts',(-43.412401760938,-55.8022014933363,
-38.9060754072981));
#258559=CARTESIAN_POINT('',(-42.599626743264,-58.0740282963067,-39.2098669215977));
#258560=CARTESIAN_POINT('Ctrl Pts',(-44.2366247692744,-55.4939426503596,
-39.0141962812275));
#258561=CARTESIAN_POINT('Ctrl Pts',(-44.1816234426521,-55.5014739795454,
-39.0171945157568));
#258562=CARTESIAN_POINT('Ctrl Pts',(-44.1264848220931,-55.511360891976,
-39.0202683895418));
#258563=CARTESIAN_POINT('Ctrl Pts',(-44.0715088992886,-55.5236541187052,
-39.0234042273537));
#258564=CARTESIAN_POINT('Ctrl Pts',(-44.016932191927,-55.5358580764289,
-39.0265172938357));
#258565=CARTESIAN_POINT('Ctrl Pts',(-43.9625165190864,-55.550433742495,
-39.0296913990414));
#258566=CARTESIAN_POINT('Ctrl Pts',(-43.9085673130736,-55.567380883633,
-39.0329111064327));
#258567=CARTESIAN_POINT('Ctrl Pts',(-43.8549038016002,-55.5842382791373,
-39.0361137634745));
#258568=CARTESIAN_POINT('Ctrl Pts',(-43.801702557357,-55.6034421513973,
-39.0393615057487));
#258569=CARTESIAN_POINT('Ctrl Pts',(-43.749265424276,-55.6249407308052,
-39.0426375748536));
#258570=CARTESIAN_POINT('Ctrl Pts',(-43.6969997422626,-55.6463690173848,
-39.0459029323596));
#258571=CARTESIAN_POINT('Ctrl Pts',(-43.645493907733,-55.6700769138001,
-39.0491963917554));
#258572=CARTESIAN_POINT('Ctrl Pts',(-43.5950371540441,-55.6959622708899,
-39.0525003623023));
#258573=CARTESIAN_POINT('Ctrl Pts',(-43.5446118156451,-55.7218315112868,
-39.0558022757373));
#258574=CARTESIAN_POINT('Ctrl Pts',(-43.4952349376079,-55.7498752261513,
-39.0591146445718));
#258575=CARTESIAN_POINT('Ctrl Pts',(-43.4471749346482,-55.7799434619491,
-39.0624195354973));
#258576=CARTESIAN_POINT('Ctrl Pts',(-43.3990613691433,-55.8100452085905,
-39.0657281097011));
#258577=CARTESIAN_POINT('Ctrl Pts',(-43.3522682206211,-55.8421755622777,
-39.069029146243));
#258578=CARTESIAN_POINT('Ctrl Pts',(-43.3070347303892,-55.8761412415753,
-39.0723049218769));
#258579=CARTESIAN_POINT('Ctrl Pts',(-43.2616720745725,-55.9102039108864,
-39.0755900515862));
#258580=CARTESIAN_POINT('Ctrl Pts',(-43.2178784859956,-55.9461118443527,
-39.0788497349381));
#258581=CARTESIAN_POINT('Ctrl Pts',(-43.1758567523826,-55.983634493292,
-39.0820670033003));
#258582=CARTESIAN_POINT('Ctrl Pts',(-43.1334622507125,-56.0214899996301,
-39.0853128115339));
#258583=CARTESIAN_POINT('Ctrl Pts',(-43.0928715614086,-56.0609883511961,
-39.0885154107999));
#258584=CARTESIAN_POINT('Ctrl Pts',(-43.0542470912624,-56.1018657043628,
-39.0916589013438));
#258585=CARTESIAN_POINT('Ctrl Pts',(-43.0154024605019,-56.1429760596432,
-39.0948203098761));
#258586=CARTESIAN_POINT('Ctrl Pts',(-42.9785467086067,-56.1854804548215,
-39.0979219035787));
#258587=CARTESIAN_POINT('Ctrl Pts',(-42.9437946423332,-56.2290936658421,
-39.1009495637756));
#258588=CARTESIAN_POINT('Ctrl Pts',(-42.9085901815573,-56.273274623734,
-39.104016637365));
#258589=CARTESIAN_POINT('Ctrl Pts',(-42.8755445902652,-56.318592705421,
-39.1070078153198));
#258590=CARTESIAN_POINT('Ctrl Pts',(-42.8447237362775,-56.3647454016771,
-39.10991094713));
#258591=CARTESIAN_POINT('Ctrl Pts',(-42.8203947202628,-56.4011768933802,
-39.1122025883782));
#258592=CARTESIAN_POINT('Ctrl Pts',(-42.7974508292817,-56.4381282062735,
-39.1144394174622));
#258593=CARTESIAN_POINT('Ctrl Pts',(-42.7759016507517,-56.4754524783487,
-39.1166166666666));
#258594=CARTESIAN_POINT('Ctrl Pts',(-42.7485194349713,-56.5228798673043,
-39.1193832643557));
#258595=CARTESIAN_POINT('Ctrl Pts',(-42.7227853156708,-56.5719579455147,
-39.1222461525621));
#258596=CARTESIAN_POINT('Ctrl Pts',(-42.6989483896267,-56.6225138678289,
-39.1251952485667));
#258597=CARTESIAN_POINT('Ctrl Pts',(-42.6753690419702,-56.6725234901324,
-39.128112477065));
#258598=CARTESIAN_POINT('Ctrl Pts',(-42.6536467732358,-56.7239789270653,
-39.1311140449706));
#258599=CARTESIAN_POINT('Ctrl Pts',(-42.6339995794796,-56.7766673996404,
-39.134187540091));
#258600=CARTESIAN_POINT('Ctrl Pts',(-42.6145810488471,-56.828742659414,
-39.1372252644543));
#258601=CARTESIAN_POINT('Ctrl Pts',(-42.597190147,-56.8820219948949,-39.1403332266998));
#258602=CARTESIAN_POINT('Ctrl Pts',(-42.5820054437861,-56.9362604394896,
-39.1434971370248));
#258603=CARTESIAN_POINT('Ctrl Pts',(-42.5669079416121,-56.9901874095233,
-39.1466428779944));
#258604=CARTESIAN_POINT('Ctrl Pts',(-42.5539918645355,-57.0450619765139,
-39.1498438955004));
#258605=CARTESIAN_POINT('Ctrl Pts',(-42.543392993098,-57.1006111214144,
-39.1530842633456));
#258606=CARTESIAN_POINT('Ctrl Pts',(-42.532836604651,-57.155937611119,-39.1563116429668));
#258607=CARTESIAN_POINT('Ctrl Pts',(-42.5245792445104,-57.2119326478768,
-39.1595780211275));
#258608=CARTESIAN_POINT('Ctrl Pts',(-42.518709123124,-57.2683030915222,
-39.1628662978962));
#258609=CARTESIAN_POINT('Ctrl Pts',(-42.5128523366118,-57.3245454811242,
-39.1661471048438));
#258610=CARTESIAN_POINT('Ctrl Pts',(-42.509372161352,-57.3811608687148,
-39.1694496698809));
#258611=CARTESIAN_POINT('Ctrl Pts',(-42.5083060983997,-57.4378448214745,
-39.1727562343354));
#258612=CARTESIAN_POINT('Ctrl Pts',(-42.5072390574213,-57.4945807771591,
-39.1760658322944));
#258613=CARTESIAN_POINT('Ctrl Pts',(-42.5085906099458,-57.5513846843009,
-39.1793793938705));
#258614=CARTESIAN_POINT('Ctrl Pts',(-42.5123461307596,-57.6079488207989,
-39.1826789685134));
#258615=CARTESIAN_POINT('Ctrl Pts',(-42.5161064641788,-57.6645854428161,
-39.1859827714784));
#258616=CARTESIAN_POINT('Ctrl Pts',(-42.5222767953613,-57.7209809488454,
-39.1892725090309));
#258617=CARTESIAN_POINT('Ctrl Pts',(-42.5307907462682,-57.7768350714559,
-39.1925306654734));
#258618=CARTESIAN_POINT('Ctrl Pts',(-42.5393557389353,-57.8330240436285,
-39.1958083548028));
#258619=CARTESIAN_POINT('Ctrl Pts',(-42.5502922560484,-57.8886644282291,
-39.1990540427749));
#258620=CARTESIAN_POINT('Ctrl Pts',(-42.5634835159962,-57.9434700632674,
-39.202251036505));
#258621=CARTESIAN_POINT('Ctrl Pts',(-42.5740992219077,-57.9875750620441,
-39.2048238267748));
#258622=CARTESIAN_POINT('Ctrl Pts',(-42.5861741058487,-58.0311397239746,
-39.2073650970601));
#258623=CARTESIAN_POINT('Ctrl Pts',(-42.5996267629089,-58.0740282897704,
-39.2098669280151));
#258624=CARTESIAN_POINT('Ctrl Pts',(-42.5465468229071,-57.0844434842294,
-38.9933892973418));
#258625=CARTESIAN_POINT('Ctrl Pts',(-42.5456036161884,-57.089174404209,
-38.9941812935483));
#258626=CARTESIAN_POINT('Ctrl Pts',(-42.5446783779407,-57.0939047795968,
-38.9949768713224));
#258627=CARTESIAN_POINT('Ctrl Pts',(-42.543771399786,-57.0986331989938,
-38.9957757940657));
#258628=CARTESIAN_POINT('Ctrl Pts',(-42.5375451994903,-57.131092730784,
-39.0012602183534));
#258629=CARTESIAN_POINT('Ctrl Pts',(-42.5321429006105,-57.163596155606,
-39.0069231082391));
#258630=CARTESIAN_POINT('Ctrl Pts',(-42.5275574313231,-57.1961040632046,
-39.0127541622176));
#258631=CARTESIAN_POINT('Ctrl Pts',(-42.5229719620357,-57.2286119708033,
-39.018585216196));
#258632=CARTESIAN_POINT('Ctrl Pts',(-42.5191999190634,-57.2611374049919,
-39.0245864537587));
#258633=CARTESIAN_POINT('Ctrl Pts',(-42.5162298763662,-57.2936802127718,
-39.0307548596727));
#258634=CARTESIAN_POINT('Ctrl Pts',(-42.5102897909718,-57.3587658283315,
-39.0430916715007));
#258635=CARTESIAN_POINT('Ctrl Pts',(-42.5075526709299,-57.4239208272887,
-39.0560961189448));
#258636=CARTESIAN_POINT('Ctrl Pts',(-42.507999333869,-57.4891455421591,
-39.0697591885565));
#258637=CARTESIAN_POINT('Ctrl Pts',(-42.5082226653386,-57.5217578995943,
-39.0765907233624));
#258638=CARTESIAN_POINT('Ctrl Pts',(-42.5092432682604,-57.5543877143394,
-39.0835871924588));
#258639=CARTESIAN_POINT('Ctrl Pts',(-42.5110675613762,-57.5870352205429,
-39.0907492962697));
#258640=CARTESIAN_POINT('Ctrl Pts',(-42.512891854492,-57.6196827267464,
-39.0979114000806));
#258641=CARTESIAN_POINT('Ctrl Pts',(-42.5155178619726,-57.6523290916439,
-39.1052348221532));
#258642=CARTESIAN_POINT('Ctrl Pts',(-42.5189635766488,-57.6850311714121,
-39.1127343794571));
#258643=CARTESIAN_POINT('Ctrl Pts',(-42.5224092913251,-57.7177332511804,
-39.1202339367609));
#258644=CARTESIAN_POINT('Ctrl Pts',(-42.5266542176424,-57.7502677264705,
-39.1278590184786));
#258645=CARTESIAN_POINT('Ctrl Pts',(-42.5316660996073,-57.7825228747794,
-39.1355792827514));
#258646=CARTESIAN_POINT('Ctrl Pts',(-42.5366779815723,-57.8147780230883,
-39.1432995470241));
#258647=CARTESIAN_POINT('Ctrl Pts',(-42.5424617625837,-57.8468004016288,
-39.1511256797657));
#258648=CARTESIAN_POINT('Ctrl Pts',(-42.5490019659384,-57.8785814507583,
-39.159052225872));
#258649=CARTESIAN_POINT('Ctrl Pts',(-42.5626174009892,-57.9447434317856,
-39.1755537576797));
#258650=CARTESIAN_POINT('Ctrl Pts',(-42.5795086601173,-58.0098893460482,
-39.1924961709041));
#258651=CARTESIAN_POINT('Ctrl Pts',(-42.5996267529072,-58.0740282937004,
-39.2098669200529));
#258652=CARTESIAN_POINT('Origin',(-44.5079524583206,-57.475452478349,235.35105));
#258653=CARTESIAN_POINT('Ctrl Pts',(-44.5079524583204,-59.475452478349,
-40.0499499999999));
#258654=CARTESIAN_POINT('Ctrl Pts',(-44.6760170471088,-59.475452478349,
-40.058440311863));
#258655=CARTESIAN_POINT('Ctrl Pts',(-44.8437184416945,-59.454274826314,
-40.067529957345));
#258656=CARTESIAN_POINT('Ctrl Pts',(-45.2594552607162,-59.3471207622369,
-40.0916575385967));
#258657=CARTESIAN_POINT('Ctrl Pts',(-45.496644407017,-59.2333984614142,
-40.1069567955656));
#258658=CARTESIAN_POINT('Ctrl Pts',(-45.9176156971467,-58.9187425694116,
-40.1374009492541));
#258659=CARTESIAN_POINT('Ctrl Pts',(-46.0962927130596,-58.7194235547151,
-40.1522408525492));
#258660=CARTESIAN_POINT('Ctrl Pts',(-46.3597901723978,-58.2723890083923,
-40.1785907639449));
#258661=CARTESIAN_POINT('Ctrl Pts',(-46.4459283624828,-58.0311157161805,
-40.1925363111265));
#258662=CARTESIAN_POINT('Ctrl Pts',(-46.5247792217884,-57.5194806295679,
-40.2223816911789));
#258663=CARTESIAN_POINT('Ctrl Pts',(-46.5130120601188,-57.25347877823,-40.2378984658403));
#258664=CARTESIAN_POINT('Ctrl Pts',(-46.3876509989154,-56.7441882232003,
-40.2676070815504));
#258665=CARTESIAN_POINT('Ctrl Pts',(-46.2764125732784,-56.5056369266457,
-40.280563622792));
#258666=CARTESIAN_POINT('Ctrl Pts',(-45.9709302364628,-56.0877642162817,
-40.3081839789162));
#258667=CARTESIAN_POINT('Ctrl Pts',(-45.7808172794246,-55.9115589358159,
-40.3229274542022));
#258668=CARTESIAN_POINT('Ctrl Pts',(-45.3357905484516,-55.6353556244966,
-40.3534653106215));
#258669=CARTESIAN_POINT('Ctrl Pts',(-45.0830257677249,-55.541391309908,
-40.3689751452056));
#258670=CARTESIAN_POINT('Ctrl Pts',(-44.5678032257904,-55.4602065065838,
-40.3973711242144));
#258671=CARTESIAN_POINT('Ctrl Pts',(-44.3111368282405,-55.4689461400547,
-40.409702993038));
#258672=CARTESIAN_POINT('Ctrl Pts',(-43.8096122890819,-55.5834047199034,
-40.4383774594563));
#258673=CARTESIAN_POINT('Ctrl Pts',(-43.5699698324844,-55.6900407660986,
-40.4535939706926));
#258674=CARTESIAN_POINT('Ctrl Pts',(-43.1406185437216,-55.991989266126,
-40.4840908341309));
#258675=CARTESIAN_POINT('Ctrl Pts',(-42.9562192264815,-56.1860972069512,
-40.4990678278399));
#258676=CARTESIAN_POINT('Ctrl Pts',(-42.6801324996151,-56.6250040775835,
-40.525816668515));
#258677=CARTESIAN_POINT('Ctrl Pts',(-42.5871730365578,-56.8631930866537,
-40.5392348688177));
#258678=CARTESIAN_POINT('Ctrl Pts',(-42.4934537579717,-57.3710008542222,
-40.5688569885925));
#258679=CARTESIAN_POINT('Ctrl Pts',(-42.4971800063187,-57.6364236424564,
-40.5843399845728));
#258680=CARTESIAN_POINT('Ctrl Pts',(-42.6071199604835,-58.1507508500168,
-40.6143424050137));
#258681=CARTESIAN_POINT('Ctrl Pts',(-42.7122907149391,-58.3945581559768,
-40.6277104088922));
#258682=CARTESIAN_POINT('Ctrl Pts',(-43.0070601563209,-58.8219102326021,
-40.6550660508894));
#258683=CARTESIAN_POINT('Ctrl Pts',(-43.1916614582763,-59.0028573575633,
-40.6696693913629));
#258684=CARTESIAN_POINT('Ctrl Pts',(-43.6274028185405,-59.2907998889782,
-40.7000805619648));
#258685=CARTESIAN_POINT('Ctrl Pts',(-43.8765775868587,-59.3917624882435,
-40.7156131524052));
#258686=CARTESIAN_POINT('Ctrl Pts',(-44.2604122311971,-59.4639653632714,
-40.7371096851764));
#258687=CARTESIAN_POINT('Ctrl Pts',(-44.3841812462878,-59.475452478349,
-40.7436973075237));
#258688=CARTESIAN_POINT('Ctrl Pts',(-44.5079524583206,-59.475452478349,
-40.7499499999999));
#258689=CARTESIAN_POINT('',(-46.2909969405137,-58.3814064003432,-40.0133527207719));
#258690=CARTESIAN_POINT('Ctrl Pts',(-44.5079524583206,-59.475452478349,
-40.5912000000001));
#258691=CARTESIAN_POINT('Ctrl Pts',(-44.3712894750723,-59.475452478349,
-40.5842960391105));
#258692=CARTESIAN_POINT('Ctrl Pts',(-44.2346952893026,-59.4614482703518,
-40.5769870976757));
#258693=CARTESIAN_POINT('Ctrl Pts',(-43.8401496223421,-59.3793023154099,
-40.5546594573751));
#258694=CARTESIAN_POINT('Ctrl Pts',(-43.5934164424196,-59.2738427846152,
-40.539119050957));
#258695=CARTESIAN_POINT('Ctrl Pts',(-43.1638937079193,-58.978402858688,
-40.5088033598087));
#258696=CARTESIAN_POINT('Ctrl Pts',(-42.9829501165407,-58.7944530350421,
-40.4942972213898));
#258697=CARTESIAN_POINT('Ctrl Pts',(-42.6952377625678,-58.3609299758541,
-40.4671181033913));
#258698=CARTESIAN_POINT('Ctrl Pts',(-42.5941044680215,-58.1136062477262,
-40.4534256365473));
#258699=CARTESIAN_POINT('Ctrl Pts',(-42.4944238939425,-57.5960599864837,
-40.4232354379748));
#258700=CARTESIAN_POINT('Ctrl Pts',(-42.4959830199083,-57.331149200749,
-40.4077823088069));
#258701=CARTESIAN_POINT('Ctrl Pts',(-42.599471521949,-56.8259352812586,
-40.3783114968366));
#258702=CARTESIAN_POINT('Ctrl Pts',(-42.6969737399032,-56.5897443279571,
-40.3651874708724));
#258703=CARTESIAN_POINT('Ctrl Pts',(-42.9814317908889,-56.1563383945309,
-40.3381761704037));
#258704=CARTESIAN_POINT('Ctrl Pts',(-43.1695715019011,-55.9658105643254,
-40.3231146388194));
#258705=CARTESIAN_POINT('Ctrl Pts',(-43.6043129843349,-55.6724854920117,
-40.292596989418));
#258706=CARTESIAN_POINT('Ctrl Pts',(-43.8454807836701,-55.5706149980718,
-40.2774424159648));
#258707=CARTESIAN_POINT('Ctrl Pts',(-44.3492069523885,-55.4654949802471,
-40.248929102023));
#258708=CARTESIAN_POINT('Ctrl Pts',(-44.6066546508642,-55.461653859112,
-40.2366162077022));
#258709=CARTESIAN_POINT('Ctrl Pts',(-45.120303738751,-55.5529418352898,
-40.2080050408038));
#258710=CARTESIAN_POINT('Ctrl Pts',(-45.3707162471246,-55.6515462973986,
-40.1924787010278));
#258711=CARTESIAN_POINT('Ctrl Pts',(-45.8096388792983,-55.935542744414,
-40.1620219125873));
#258712=CARTESIAN_POINT('Ctrl Pts',(-45.9961215501845,-56.1149012768774,
-40.1473698627865));
#258713=CARTESIAN_POINT('Ctrl Pts',(-46.2945361068356,-56.5390431049575,
-40.1199237085639));
#258714=CARTESIAN_POINT('Ctrl Pts',(-46.4017791757504,-56.7810506455932,
-40.1067067735774));
#258715=CARTESIAN_POINT('Ctrl Pts',(-46.5104850354038,-57.2647523638798,
-40.0784908400107));
#258716=CARTESIAN_POINT('Ctrl Pts',(-46.5213905146943,-57.4997997300255,
-40.0647797436521));
#258717=CARTESIAN_POINT('Ctrl Pts',(-46.462284513203,-57.9578859173332,
-40.0380580493925));
#258718=CARTESIAN_POINT('Ctrl Pts',(-46.394478244912,-58.1777405942362,
-40.0252331932399));
#258719=CARTESIAN_POINT('Ctrl Pts',(-46.2909969103393,-58.3814063856342,
-40.0133526887417));
#258720=CARTESIAN_POINT('',(-44.6028144957888,-59.4732020054856,-39.8960583336497));
#258721=CARTESIAN_POINT('Ctrl Pts',(-44.6028145367817,-59.4732017575571,
-39.896058052999));
#258722=CARTESIAN_POINT('Ctrl Pts',(-44.6309237118345,-59.4718673393062,
-39.9013440349211));
#258723=CARTESIAN_POINT('Ctrl Pts',(-44.6590015032546,-59.4699391376493,
-39.9065030818641));
#258724=CARTESIAN_POINT('Ctrl Pts',(-44.7195562226364,-59.4644947877976,
-39.9173708456776));
#258725=CARTESIAN_POINT('Ctrl Pts',(-44.7520254641284,-59.4607736709145,
-39.9230368121193));
#258726=CARTESIAN_POINT('Ctrl Pts',(-44.8168752155214,-59.4517213309666,
-39.9340284833551));
#258727=CARTESIAN_POINT('Ctrl Pts',(-44.8492557303708,-59.4463901948908,
-39.9393542053395));
#258728=CARTESIAN_POINT('Ctrl Pts',(-44.9139264543873,-59.4340919253905,
-39.9496609938934));
#258729=CARTESIAN_POINT('Ctrl Pts',(-44.946215463264,-59.4271242954454,
-39.9546417246475));
#258730=CARTESIAN_POINT('Ctrl Pts',(-45.0107056952338,-59.411516304601,
-39.9642527707462));
#258731=CARTESIAN_POINT('Ctrl Pts',(-45.0429448249416,-59.4028563587456,
-39.9688866673414));
#258732=CARTESIAN_POINT('Ctrl Pts',(-45.1065152212723,-59.3840690317117,
-39.9776842198647));
#258733=CARTESIAN_POINT('Ctrl Pts',(-45.1380045334646,-59.373905450928,
-39.981871837324));
#258734=CARTESIAN_POINT('Ctrl Pts',(-45.200302444735,-59.3520826555279,
-39.9898169453504));
#258735=CARTESIAN_POINT('Ctrl Pts',(-45.2311273685557,-59.3404195858245,
-39.9935768864381));
#258736=CARTESIAN_POINT('Ctrl Pts',(-45.32263664318,-59.3031909081966,-40.0042245496825));
#258737=CARTESIAN_POINT('Ctrl Pts',(-45.3823576994497,-59.2753909454431,
-40.0104815827663));
#258738=CARTESIAN_POINT('Ctrl Pts',(-45.4699947035294,-59.2291813824217,
-40.0185985839041));
#258739=CARTESIAN_POINT('Ctrl Pts',(-45.4988824306035,-59.2130254047437,
-40.0210924810235));
#258740=CARTESIAN_POINT('Ctrl Pts',(-45.5559983886489,-59.1791841401258,
-40.0256506619548));
#258741=CARTESIAN_POINT('Ctrl Pts',(-45.5842159038049,-59.161505654346,
-40.0277141794724));
#258742=CARTESIAN_POINT('Ctrl Pts',(-45.6260683484526,-59.1337942848195,
-40.0304825527898));
#258743=CARTESIAN_POINT('Ctrl Pts',(-45.639937085558,-59.1243584137232,
-40.0313502886864));
#258744=CARTESIAN_POINT('Ctrl Pts',(-45.6673408070756,-59.1052063125898,
-40.0329654356527));
#258745=CARTESIAN_POINT('Ctrl Pts',(-45.6809062118534,-59.0954702890689,
-40.0337149272658));
#258746=CARTESIAN_POINT('Ctrl Pts',(-45.721141509693,-59.0658238467719,
-40.0357872710599));
#258747=CARTESIAN_POINT('Ctrl Pts',(-45.7474017250148,-59.0454416887883,
-40.0369374935097));
#258748=CARTESIAN_POINT('Ctrl Pts',(-45.8244369758231,-58.9825233897898,
-40.0396997359252));
#258749=CARTESIAN_POINT('Ctrl Pts',(-45.8735338613848,-58.9381770793581,
-40.0406290361817));
#258750=CARTESIAN_POINT('Ctrl Pts',(-45.9672017588149,-58.844746856131,
-40.0406755331895));
#258751=CARTESIAN_POINT('Ctrl Pts',(-46.0117880585293,-58.7956402330911,
-40.0397912781262));
#258752=CARTESIAN_POINT('Ctrl Pts',(-46.0751829525158,-58.7183959597934,
-40.03708141461));
#258753=CARTESIAN_POINT('Ctrl Pts',(-46.0957687894685,-58.6919898183277,
-40.0359425033221));
#258754=CARTESIAN_POINT('Ctrl Pts',(-46.1356388662634,-58.6381045244638,
-40.0331996147473));
#258755=CARTESIAN_POINT('Ctrl Pts',(-46.1547846879949,-58.6108153057907,
-40.0316057182764));
#258756=CARTESIAN_POINT('Ctrl Pts',(-46.191608467482,-58.5554560068352,
-40.0279771039652));
#258757=CARTESIAN_POINT('Ctrl Pts',(-46.209273608015,-58.5274033537027,
-40.025943288199));
#258758=CARTESIAN_POINT('Ctrl Pts',(-46.2431323556178,-58.4705630466323,
-40.0214426044335));
#258759=CARTESIAN_POINT('Ctrl Pts',(-46.2593259282838,-58.441775375496,
-40.0189757265311));
#258760=CARTESIAN_POINT('Ctrl Pts',(-46.2802839458637,-58.4022634681017,
-40.0153404975323));
#258761=CARTESIAN_POINT('Ctrl Pts',(-46.2856865831931,-58.3918579776286,
-40.0143602145261));
#258762=CARTESIAN_POINT('Ctrl Pts',(-46.2909969450817,-58.3814064047113,
-40.0133526947335));
#258763=CARTESIAN_POINT('Ctrl Pts',(-44.6028144943784,-59.4732015101633,
-39.8960579076686));
#258764=CARTESIAN_POINT('Ctrl Pts',(-44.5712018647696,-59.4747026188422,
-39.8944171138134));
#258765=CARTESIAN_POINT('Ctrl Pts',(-44.539572771046,-59.475452478349,-39.8927973996557));
#258766=CARTESIAN_POINT('Ctrl Pts',(-44.5079524583206,-59.475452478349,
-39.8912000000002));
#258767=CARTESIAN_POINT('Ctrl Pts',(-43.4805771074156,-59.5712767529309,
-39.2399080357013));
#258768=CARTESIAN_POINT('Ctrl Pts',(-43.4150727209207,-59.5358440364426,
-39.2223070534893));
#258769=CARTESIAN_POINT('Ctrl Pts',(-43.2883193276586,-59.4590682572254,
-39.1867578392588));
#258770=CARTESIAN_POINT('Ctrl Pts',(-43.1106712693135,-59.32658002426,-39.1324031814995));
#258771=CARTESIAN_POINT('Ctrl Pts',(-43.0005921597408,-59.2266373021163,
-39.0954660506179));
#258772=CARTESIAN_POINT('Ctrl Pts',(-42.8948534568781,-59.1207134074407,
-39.0581733199915));
#258773=CARTESIAN_POINT('Ctrl Pts',(-42.7951360401793,-59.0104958554849,
-39.0211184761739));
#258774=CARTESIAN_POINT('Ctrl Pts',(-42.6850011896347,-58.8622904152127,
-38.9753582681256));
#258775=CARTESIAN_POINT('Ctrl Pts',(-42.6055727997797,-58.7375004045667,
-38.939089851323));
#258776=CARTESIAN_POINT('Ctrl Pts',(-42.5503788594446,-58.6407591922129,
-38.9120596161462));
#258777=CARTESIAN_POINT('Ctrl Pts',(-42.5165536369311,-58.5741539171446,
-38.8941613358138));
#258778=CARTESIAN_POINT('Ctrl Pts',(-42.4842288567228,-58.5064298632496,
-38.8763157156907));
#258779=CARTESIAN_POINT('Ctrl Pts',(-42.4689425396028,-58.4722695523732,
-38.8674882509199));
#258780=CARTESIAN_POINT('Ctrl Pts',(-42.4257123024776,-58.3690064948315,
-38.8413136266604));
#258781=CARTESIAN_POINT('Ctrl Pts',(-42.3750272156063,-58.229152189777,
-38.8072100415055));
#258782=CARTESIAN_POINT('Ctrl Pts',(-42.3380647902547,-58.0850119200902,
-38.7746901633276));
#258783=CARTESIAN_POINT('Ctrl Pts',(-42.3155659796374,-57.9752818499468,
-38.7509105250088));
#258784=CARTESIAN_POINT('Ctrl Pts',(-42.3089374211558,-57.9384266221928,
-38.7430843922672));
#258785=CARTESIAN_POINT('Ctrl Pts',(-42.297458012674,-57.864178756387,-38.7276438637217));
#258786=CARTESIAN_POINT('Ctrl Pts',(-42.292601515188,-57.8267325312259,
-38.720018782004));
#258787=CARTESIAN_POINT('Ctrl Pts',(-42.2847289916893,-57.7514526301959,
-38.7050196673963));
#258788=CARTESIAN_POINT('Ctrl Pts',(-42.2817363521424,-57.7138759968928,
-38.6976962453237));
#258789=CARTESIAN_POINT('Ctrl Pts',(-42.277596992864,-57.6387184974263,
-38.6833720377019));
#258790=CARTESIAN_POINT('Ctrl Pts',(-42.2741651307842,-57.5260409596698,
-38.6623829091612));
#258791=CARTESIAN_POINT('Ctrl Pts',(-42.2805893100654,-57.3760354719141,
-38.6363740800325));
#258792=CARTESIAN_POINT('Ctrl Pts',(-42.2937061680812,-57.2637038035873,
-38.618370061439));
#258793=CARTESIAN_POINT('Ctrl Pts',(-42.3043247017591,-57.1888547452426,
-38.6067079534822));
#258794=CARTESIAN_POINT('Ctrl Pts',(-42.3105743117123,-57.1514345461221,
-38.6010450635964));
#258795=CARTESIAN_POINT('Ctrl Pts',(-42.3249704170347,-57.0766935209607,
-38.590076215021));
#258796=CARTESIAN_POINT('Ctrl Pts',(-42.3331592025312,-57.0392159768686,
-38.5847494243559));
#258797=CARTESIAN_POINT('Ctrl Pts',(-42.3512949844302,-56.9651221381903,
-38.5745673038812));
#258798=CARTESIAN_POINT('Ctrl Pts',(-42.3712216906218,-56.8916587034686,
-38.564820665347));
#258799=CARTESIAN_POINT('Ctrl Pts',(-42.4063979707918,-56.7834465224234,
-38.5515118436));
#258800=CARTESIAN_POINT('Ctrl Pts',(-42.4468320479729,-56.6771725078319,
-38.5395042677724));
#258801=CARTESIAN_POINT('Ctrl Pts',(-42.4925290654744,-56.5728473165674,
-38.5288039137004));
#258802=CARTESIAN_POINT('Ctrl Pts',(-42.5265325119253,-56.5046058456765,
-38.5225509073062));
#258803=CARTESIAN_POINT('Ctrl Pts',(-42.5623338475306,-56.4370293947697,
-38.5167461666044));
#258804=CARTESIAN_POINT('Ctrl Pts',(-42.5811223641794,-56.4035923099625,
-38.5140693065785));
#258805=CARTESIAN_POINT('Ctrl Pts',(-42.620584523009,-56.3373241998654,
-38.5091697400817));
#258806=CARTESIAN_POINT('Ctrl Pts',(-42.6411082254821,-56.3047465904101,
-38.5069659500128));
#258807=CARTESIAN_POINT('Ctrl Pts',(-42.7048067991197,-56.2090283357163,
-38.501110858935));
#258808=CARTESIAN_POINT('Ctrl Pts',(-42.7502234543428,-56.1476408662828,
-38.4981890389281));
#258809=CARTESIAN_POINT('Ctrl Pts',(-42.8467942323831,-56.0297655581676,
-38.4942910511033));
#258810=CARTESIAN_POINT('Ctrl Pts',(-42.8979715413934,-55.9732420482176,
-38.4933125989996));
#258811=CARTESIAN_POINT('Ctrl Pts',(-42.9790570553347,-55.8921695883033,
-38.4933149859729));
#258812=CARTESIAN_POINT('Ctrl Pts',(-43.0068374106561,-55.8657400908868,
-38.4935622007431));
#258813=CARTESIAN_POINT('Ctrl Pts',(-43.0495800649421,-55.8270637749536,
-38.4943063068789));
#258814=CARTESIAN_POINT('Ctrl Pts',(-43.0640222060113,-55.8143203511958,
-38.494617152342));
#258815=CARTESIAN_POINT('Ctrl Pts',(-43.0932714774893,-55.7891564261061,
-38.4953646906773));
#258816=CARTESIAN_POINT('Ctrl Pts',(-43.1080901283632,-55.7767277938553,
-38.4958020036096));
#258817=CARTESIAN_POINT('Ctrl Pts',(-43.1528523310046,-55.7401327167866,
-38.4972962980169));
#258818=CARTESIAN_POINT('Ctrl Pts',(-43.2134913856688,-55.6930468850421,
-38.4997758707861));
#258819=CARTESIAN_POINT('Ctrl Pts',(-43.3385569247743,-55.6055389451161,
-38.5066450244003));
#258820=CARTESIAN_POINT('Ctrl Pts',(-43.4691986576013,-55.5278792007279,
-38.5163302992824));
#258821=CARTESIAN_POINT('Ctrl Pts',(-43.5713395927684,-55.4769743237494,
-38.5256877381308));
#258822=CARTESIAN_POINT('Ctrl Pts',(-43.6403672861995,-55.4446857735354,
-38.5323951500278));
#258823=CARTESIAN_POINT('Ctrl Pts',(-43.6753577685123,-55.4293620157832,
-38.5359845633874));
#258824=CARTESIAN_POINT('Ctrl Pts',(-43.7462462065788,-55.4003985583156,
-38.5436333065981));
#258825=CARTESIAN_POINT('Ctrl Pts',(-43.7822717759725,-55.3867204456352,
-38.5477088862383));
#258826=CARTESIAN_POINT('Ctrl Pts',(-43.8543821738219,-55.3613797848081,
-38.5562346427694));
#258827=CARTESIAN_POINT('Ctrl Pts',(-43.890622407919,-55.349649082917,-38.5607007444526));
#258828=CARTESIAN_POINT('Ctrl Pts',(-43.9997560709039,-55.3172704656441,
-38.5746802407103));
#258829=CARTESIAN_POINT('Ctrl Pts',(-44.1098017310836,-55.290468361793,
-38.5898286859852));
#258830=CARTESIAN_POINT('Ctrl Pts',(-44.2583166685835,-55.2656490138239,
-38.612301023075));
#258831=CARTESIAN_POINT('Ctrl Pts',(-44.3705972700495,-55.2524997368729,
-38.6302900391873));
#258832=CARTESIAN_POINT('Ctrl Pts',(-44.446056048267,-55.2474029004138,
-38.6430428201589));
#258833=CARTESIAN_POINT('Ctrl Pts',(-44.5218128020516,-55.2441636366351,
-38.65617756452));
#258834=CARTESIAN_POINT('Ctrl Pts',(-44.5599089424743,-55.2434808562086,
-38.6629497802385));
#258835=CARTESIAN_POINT('Ctrl Pts',(-44.6354869543582,-55.2439911084578,
-38.6767130108817));
#258836=CARTESIAN_POINT('Ctrl Pts',(-44.6731456892459,-55.2451740103824,
-38.6837342374529));
#258837=CARTESIAN_POINT('Ctrl Pts',(-44.7481014788608,-55.2493620066237,
-38.6980304684339));
#258838=CARTESIAN_POINT('Ctrl Pts',(-44.860046548974,-55.2583760573225,
-38.7198650218829));
#258839=CARTESIAN_POINT('Ctrl Pts',(-45.0073845433675,-55.2811507310277,
-38.7505067688753));
#258840=CARTESIAN_POINT('Ctrl Pts',(-45.1528189888476,-55.3146135839333,
-38.7826550300594));
#258841=CARTESIAN_POINT('Ctrl Pts',(-45.2248832056965,-55.3349380951144,
-38.7992310848652));
#258842=CARTESIAN_POINT('Ctrl Pts',(-45.2966462681613,-55.3570913336823,
-38.8160672125853));
#258843=CARTESIAN_POINT('Ctrl Pts',(-45.3323638946335,-55.3690863290504,
-38.8246135819642));
#258844=CARTESIAN_POINT('Ctrl Pts',(-45.4027951436545,-55.3946744461232,
-38.841798196801));
#258845=CARTESIAN_POINT('Ctrl Pts',(-45.4376370321487,-55.4083060218429,
-38.85046633842));
#258846=CARTESIAN_POINT('Ctrl Pts',(-45.5409345111852,-55.4516493275196,
-38.8766665754573));
#258847=CARTESIAN_POINT('Ctrl Pts',(-45.6082182891413,-55.4838201174091,
-38.8944064774514));
#258848=CARTESIAN_POINT('Ctrl Pts',(-45.7067749877369,-55.5369855856676,
-38.9214216121435));
#258849=CARTESIAN_POINT('Ctrl Pts',(-45.7392219877795,-55.5555212114618,
-38.9304915704334));
#258850=CARTESIAN_POINT('Ctrl Pts',(-45.8033556832395,-55.5942722159849,
-38.9487787872477));
#258851=CARTESIAN_POINT('Ctrl Pts',(-45.8348443691401,-55.6143675312756,
-38.9579395118015));
#258852=CARTESIAN_POINT('Ctrl Pts',(-45.9274099842789,-55.6766589025306,
-38.9854159162723));
#258853=CARTESIAN_POINT('Ctrl Pts',(-45.9867610865919,-55.7209353156014,
-39.0037703637879));
#258854=CARTESIAN_POINT('Ctrl Pts',(-46.1007337830098,-55.8148102393793,
-39.0405190865864));
#258855=CARTESIAN_POINT('Ctrl Pts',(-46.1826971388658,-55.889219933262,
-39.0681181728269));
#258856=CARTESIAN_POINT('Ctrl Pts',(-46.259356574729,-55.9696687352924,
-39.0957737179551));
#258857=CARTESIAN_POINT('Ctrl Pts',(-46.309266807939,-56.024663053365,-39.1142236413887));
#258858=CARTESIAN_POINT('Ctrl Pts',(-46.3336138177017,-56.0528284109483,
-39.1234510495426));
#258859=CARTESIAN_POINT('Ctrl Pts',(-46.3692509284248,-56.0961546965833,
-39.1373141736981));
#258860=CARTESIAN_POINT('Ctrl Pts',(-46.3809719555493,-56.1107655250657,
-39.14193505412));
#258861=CARTESIAN_POINT('Ctrl Pts',(-46.4039850968433,-56.1401806715041,
-39.1511314768264));
#258862=CARTESIAN_POINT('Ctrl Pts',(-46.4153001903629,-56.1550126624776,
-39.1557159133813));
#258863=CARTESIAN_POINT('Ctrl Pts',(-46.4486370096885,-56.1998310060263,
-39.1694131182659));
#258864=CARTESIAN_POINT('Ctrl Pts',(-46.4700835091466,-56.2301795317326,
-39.1784826054425));
#258865=CARTESIAN_POINT('Ctrl Pts',(-46.532071913686,-56.3225583984772,
-39.2054898733524));
#258866=CARTESIAN_POINT('Ctrl Pts',(-46.5894197348374,-56.4176636744323,
-39.23211607576));
#258867=CARTESIAN_POINT('Ctrl Pts',(-46.6566074362748,-56.5498680842415,
-39.2668544229849));
#258868=CARTESIAN_POINT('Ctrl Pts',(-46.6870820302515,-56.617790568625,
-39.2839693714534));
#258869=CARTESIAN_POINT('Ctrl Pts',(-46.7159729830272,-56.6866360545619,
-39.3009558869148));
#258870=CARTESIAN_POINT('Ctrl Pts',(-46.7296188023799,-56.7214992889704,
-39.3093799218186));
#258871=CARTESIAN_POINT('Ctrl Pts',(-46.7553216997643,-56.7922546384013,
-39.3261176641085));
#258872=CARTESIAN_POINT('Ctrl Pts',(-46.7672996943011,-56.8279354881579,
-39.3343809787628));
#258873=CARTESIAN_POINT('Ctrl Pts',(-46.8004530502947,-56.9353633959568,
-39.358737163018));
#258874=CARTESIAN_POINT('Ctrl Pts',(-46.8189795501832,-57.0077635587999,
-39.3744658121213));
#258875=CARTESIAN_POINT('Ctrl Pts',(-46.848916211803,-57.1540080946302,
-39.4048998290393));
#258876=CARTESIAN_POINT('Ctrl Pts',(-46.866048617508,-57.2647966217996,
-39.4269646939479));
#258877=CARTESIAN_POINT('Ctrl Pts',(-46.875074749658,-57.3772756893033,
-39.4478819384746));
#258878=CARTESIAN_POINT('Ctrl Pts',(-46.8792542953452,-57.4526370309597,
-39.4615663943076));
#258879=CARTESIAN_POINT('Ctrl Pts',(-46.8804258736835,-57.4905390832845,
-39.4682843608713));
#258880=CARTESIAN_POINT('Ctrl Pts',(-46.8808837743635,-57.566610437341,
-39.4814341960201));
#258881=CARTESIAN_POINT('Ctrl Pts',(-46.8801708637706,-57.604491394965,
-39.4878166677226));
#258882=CARTESIAN_POINT('Ctrl Pts',(-46.8768913879562,-57.6800597985945,
-39.5002231148134));
#258883=CARTESIAN_POINT('Ctrl Pts',(-46.8691896925243,-57.7930657109158,
-39.5182849936093));
#258884=CARTESIAN_POINT('Ctrl Pts',(-46.8479069711518,-57.9423669591112,
-39.540205996752));
#258885=CARTESIAN_POINT('Ctrl Pts',(-46.8236459543104,-58.053306681129,
-39.5550278422771));
#258886=CARTESIAN_POINT('Ctrl Pts',(-46.8055990109883,-58.1270324939452,
-39.5645447403379));
#258887=CARTESIAN_POINT('Ctrl Pts',(-46.7956339676918,-58.1637938532181,
-39.5691227921436));
#258888=CARTESIAN_POINT('Ctrl Pts',(-46.7738161327052,-58.2370162077019,
-39.5779016468881));
#258889=CARTESIAN_POINT('Ctrl Pts',(-46.7619036278491,-58.2736352268715,
-39.5821192203466));
#258890=CARTESIAN_POINT('Ctrl Pts',(-46.7364059718256,-58.3458255995332,
-39.5900871854462));
#258891=CARTESIAN_POINT('Ctrl Pts',(-46.7091836493705,-58.4171862986019,
-39.5976163356366));
#258892=CARTESIAN_POINT('Ctrl Pts',(-46.663274408039,-58.5216699086648,
-39.6076014242402));
#258893=CARTESIAN_POINT('Ctrl Pts',(-46.6123207377325,-58.6236436013082,
-39.616293729045));
#258894=CARTESIAN_POINT('Ctrl Pts',(-46.5563244858032,-58.7230996041114,
-39.6236943138341));
#258895=CARTESIAN_POINT('Ctrl Pts',(-46.515607032986,-58.7877140896312,
-39.6277619492082));
#258896=CARTESIAN_POINT('Ctrl Pts',(-46.4731710833873,-58.8514710047945,
-39.6313905635194));
#258897=CARTESIAN_POINT('Ctrl Pts',(-46.4511086137465,-58.8829006319494,
-39.6329844599904));
#258898=CARTESIAN_POINT('Ctrl Pts',(-46.4051673201274,-58.9449633016888,
-39.6357273485653));
#258899=CARTESIAN_POINT('Ctrl Pts',(-46.381447994276,-58.975377588932,-39.6368662598532));
#258900=CARTESIAN_POINT('Ctrl Pts',(-46.3084068909562,-59.0643493136614,
-39.6395761233691));
#258901=CARTESIAN_POINT('Ctrl Pts',(-46.2570407846102,-59.1209150453974,
-39.6404603784325));
#258902=CARTESIAN_POINT('Ctrl Pts',(-46.1491379755941,-59.228544463199,
-39.6404138814247));
#258903=CARTESIAN_POINT('Ctrl Pts',(-46.0925836555155,-59.2796343044913,
-39.6394845811684));
#258904=CARTESIAN_POINT('Ctrl Pts',(-46.0038529437629,-59.3521266125547,
-39.6367223387528));
#258905=CARTESIAN_POINT('Ctrl Pts',(-45.9736068078661,-59.3756113554055,
-39.6355721163029));
#258906=CARTESIAN_POINT('Ctrl Pts',(-45.9272656961273,-59.4097723546528,
-39.6334997725088));
#258907=CARTESIAN_POINT('Ctrl Pts',(-45.9116419215573,-59.4209912820171,
-39.6327502808957));
#258908=CARTESIAN_POINT('Ctrl Pts',(-45.8800804794677,-59.4430610802669,
-39.6311351339295));
#258909=CARTESIAN_POINT('Ctrl Pts',(-45.8321587971618,-59.4756823489919,
-39.628531354857));
#258910=CARTESIAN_POINT('Ctrl Pts',(-45.7834097108732,-59.5062438963941,
-39.6254355071979));
#258911=CARTESIAN_POINT('Ctrl Pts',(-45.717633106262,-59.5452481912826,
-39.6208773262667));
#258912=CARTESIAN_POINT('Ctrl Pts',(-45.6178307490054,-59.601113548897,
-39.6133952897297));
#258913=CARTESIAN_POINT('Ctrl Pts',(-45.4802897643185,-59.6652183443042,
-39.6008811885904));
#258914=CARTESIAN_POINT('Ctrl Pts',(-45.3738098009101,-59.7055766782111,
-39.5896017905935));
#258915=CARTESIAN_POINT('Ctrl Pts',(-45.3020778813705,-59.7307512119865,
-39.5816566825671));
#258916=CARTESIAN_POINT('Ctrl Pts',(-45.2658207311094,-59.7424779859237,
-39.5774690651077));
#258917=CARTESIAN_POINT('Ctrl Pts',(-45.1926264675053,-59.7641596016776,
-39.5686715125846));
#258918=CARTESIAN_POINT('Ctrl Pts',(-45.1555073907618,-59.7741562512684,
-39.5640376159893));
#258919=CARTESIAN_POINT('Ctrl Pts',(-45.0441315765335,-59.8011904590316,
-39.5496210468413));
#258920=CARTESIAN_POINT('Ctrl Pts',(-44.9324484012679,-59.8224577850013,
-39.5341534065747));
#258921=CARTESIAN_POINT('Ctrl Pts',(-44.8203079610257,-59.8353953605365,
-39.5171556909205));
#258922=CARTESIAN_POINT('Ctrl Pts',(-44.7080184564226,-59.8455760612675,
-39.4996502778008));
#258923=CARTESIAN_POINT('Ctrl Pts',(-44.6329372249224,-59.8486931621852,
-39.4873001861445));
#258924=CARTESIAN_POINT('Ctrl Pts',(-44.5200834441659,-59.8478515133141,
-39.4677634802869));
#258925=CARTESIAN_POINT('Ctrl Pts',(-44.4823810871712,-59.8466449718289,
-39.4610736497974));
#258926=CARTESIAN_POINT('Ctrl Pts',(-44.4258051079382,-59.8434394706745,
-39.4507883432074));
#258927=CARTESIAN_POINT('Ctrl Pts',(-44.4069254589855,-59.8421361346926,
-39.4473147915973));
#258928=CARTESIAN_POINT('Ctrl Pts',(-44.3691376542581,-59.8390581625153,
-39.4402793331445));
#258929=CARTESIAN_POINT('Ctrl Pts',(-44.3502459350849,-59.8372838734483,
-39.4367203104461));
#258930=CARTESIAN_POINT('Ctrl Pts',(-44.2562487381671,-59.8272835659938,
-39.4188041728073));
#258931=CARTESIAN_POINT('Ctrl Pts',(-44.1080045765469,-59.8040393501646,
-39.3892226636159));
#258932=CARTESIAN_POINT('Ctrl Pts',(-43.9639303529155,-59.7668593120831,
-39.3578670379715));
#258933=CARTESIAN_POINT('Ctrl Pts',(-43.8219159040518,-59.7227861654643,
-39.3256251231267));
#258934=CARTESIAN_POINT('Ctrl Pts',(-43.7519290534068,-59.6972943066161,
-39.3090578287531));
#258935=CARTESIAN_POINT('Ctrl Pts',(-43.665783177736,-59.6610675807531,
-39.2877890488175));
#258936=CARTESIAN_POINT('Ctrl Pts',(-43.6486106666635,-59.653596197985,
-39.2835041280971));
#258937=CARTESIAN_POINT('Ctrl Pts',(-43.6144193015916,-59.6382222359849,
-39.2748825183767));
#258938=CARTESIAN_POINT('Ctrl Pts',(-43.597366582891,-59.6303022352814,
-39.2705368924251));
#258939=CARTESIAN_POINT('Ctrl Pts',(-43.5465994182959,-59.605961903298,
-39.2574616452183));
#258940=CARTESIAN_POINT('Ctrl Pts',(-43.513329300663,-59.588993111175,-39.2487085268073));
#258941=CARTESIAN_POINT('Ctrl Pts',(-43.4805771074156,-59.5712767529309,
-39.2399080357013));
#258942=CARTESIAN_POINT('Ctrl Pts',(-43.8341420587998,-57.9817357678076,
-41.1268248734572));
#258943=CARTESIAN_POINT('Ctrl Pts',(-43.8090823387197,-57.9680163597508,
-41.1092238912453));
#258944=CARTESIAN_POINT('Ctrl Pts',(-43.7605654269547,-57.9383371077444,
-41.0736746770147));
#258945=CARTESIAN_POINT('Ctrl Pts',(-43.6924895655639,-57.8872515755908,
-41.019320019256));
#258946=CARTESIAN_POINT('Ctrl Pts',(-43.6502497090231,-57.8487916199066,
-40.9823828883729));
#258947=CARTESIAN_POINT('Ctrl Pts',(-43.6096433745973,-57.8080652293815,
-40.945090157748));
#258948=CARTESIAN_POINT('Ctrl Pts',(-43.5713160673933,-57.7657212262301,
-40.9080353139296));
#258949=CARTESIAN_POINT('Ctrl Pts',(-43.5288984657655,-57.7088609123343,
-40.8622751058818));
#258950=CARTESIAN_POINT('Ctrl Pts',(-43.4982484100127,-57.6610280687967,
-40.826006689079));
#258951=CARTESIAN_POINT('Ctrl Pts',(-43.4769169762936,-57.6239677344727,
-40.798976453902));
#258952=CARTESIAN_POINT('Ctrl Pts',(-43.4638199758968,-57.5984660781933,
-40.7810781735695));
#258953=CARTESIAN_POINT('Ctrl Pts',(-43.4512904535732,-57.5725430453748,
-40.7632325534464));
#258954=CARTESIAN_POINT('Ctrl Pts',(-43.4453582046716,-57.5594707895743,
-40.7544050886758));
#258955=CARTESIAN_POINT('Ctrl Pts',(-43.4285595200757,-57.5199648485381,
-40.7282304644163));
#258956=CARTESIAN_POINT('Ctrl Pts',(-43.4088016745783,-57.4664867157472,
-40.6941268792613));
#258957=CARTESIAN_POINT('Ctrl Pts',(-43.3942530508608,-57.4114223976644,
-40.6616070010832));
#258958=CARTESIAN_POINT('Ctrl Pts',(-43.3853242538269,-57.3695231591805,
-40.6378273627645));
#258959=CARTESIAN_POINT('Ctrl Pts',(-43.3826786150667,-57.3554536366825,
-40.630001230023));
#258960=CARTESIAN_POINT('Ctrl Pts',(-43.378062215599,-57.3271160344971,
-40.6145607014775));
#258961=CARTESIAN_POINT('Ctrl Pts',(-43.3760891270041,-57.3128275119467,
-40.60693561976));
#258962=CARTESIAN_POINT('Ctrl Pts',(-43.3728422231051,-57.2841093232557,
-40.5919365051523));
#258963=CARTESIAN_POINT('Ctrl Pts',(-43.3715781643254,-57.2697777029377,
-40.5846130830795));
#258964=CARTESIAN_POINT('Ctrl Pts',(-43.3697526802575,-57.2411194243864,
-40.5702888754578));
#258965=CARTESIAN_POINT('Ctrl Pts',(-43.3680717796799,-57.1981642741791,
-40.5492997469169));
#258966=CARTESIAN_POINT('Ctrl Pts',(-43.3700185838812,-57.1410182421193,
-40.5232909177883));
#258967=CARTESIAN_POINT('Ctrl Pts',(-43.3746384661022,-57.0982543712987,
-40.505286899195));
#258968=CARTESIAN_POINT('Ctrl Pts',(-43.3784319419536,-57.0697666559562,
-40.4936247912381));
#258969=CARTESIAN_POINT('Ctrl Pts',(-43.3806866868643,-57.0555278483981,
-40.4879619013523));
#258970=CARTESIAN_POINT('Ctrl Pts',(-43.3859186984709,-57.0270949764048,
-40.476993052777));
#258971=CARTESIAN_POINT('Ctrl Pts',(-43.3889115442249,-57.0128413374093,
-40.4716662621118));
#258972=CARTESIAN_POINT('Ctrl Pts',(-43.3955695423488,-56.984668670318,
-40.4614841416371));
#258973=CARTESIAN_POINT('Ctrl Pts',(-43.4029115329907,-56.9567427536229,
-40.4517375031029));
#258974=CARTESIAN_POINT('Ctrl Pts',(-43.4159439893498,-56.915628788467,
-40.4384286813559));
#258975=CARTESIAN_POINT('Ctrl Pts',(-43.4309850942545,-56.8752725380991,
-40.4264211055283));
#258976=CARTESIAN_POINT('Ctrl Pts',(-43.4480370013178,-56.8356780486645,
-40.4157207514563));
#258977=CARTESIAN_POINT('Ctrl Pts',(-43.4607570961379,-56.8097932355363,
-40.409467745062));
#258978=CARTESIAN_POINT('Ctrl Pts',(-43.4741642201056,-56.7841683331057,
-40.4036630043601));
#258979=CARTESIAN_POINT('Ctrl Pts',(-43.4812071336048,-56.7714928975767,
-40.4009861443346));
#258980=CARTESIAN_POINT('Ctrl Pts',(-43.4960130774609,-56.7463797512019,
-40.3960865778375));
#258981=CARTESIAN_POINT('Ctrl Pts',(-43.5037198572985,-56.7340380787953,
-40.3938827877695));
#258982=CARTESIAN_POINT('Ctrl Pts',(-43.527657505214,-56.6977883833479,
-40.3880276966888));
#258983=CARTESIAN_POINT('Ctrl Pts',(-43.5447483375558,-56.6745564757614,
-40.3851058766842));
#258984=CARTESIAN_POINT('Ctrl Pts',(-43.5811328114983,-56.629979998045,
-40.3812078888591));
#258985=CARTESIAN_POINT('Ctrl Pts',(-43.6004351631962,-56.6086219171049,
-40.3802294367552));
#258986=CARTESIAN_POINT('Ctrl Pts',(-43.6310475296952,-56.578014570072,
-40.3802318237287));
#258987=CARTESIAN_POINT('Ctrl Pts',(-43.6415402048873,-56.5680413281089,
-40.3804790384992));
#258988=CARTESIAN_POINT('Ctrl Pts',(-43.6576911458811,-56.5534539772523,
-40.3812231446347));
#258989=CARTESIAN_POINT('Ctrl Pts',(-43.6631494628181,-56.5486488515781,
-40.3815339900979));
#258990=CARTESIAN_POINT('Ctrl Pts',(-43.6742063152013,-56.5391628964206,
-40.3822815284329));
#258991=CARTESIAN_POINT('Ctrl Pts',(-43.6798092119243,-56.534479009001,
-40.3827188413654));
#258992=CARTESIAN_POINT('Ctrl Pts',(-43.6967370434146,-56.5206915949946,
-40.3842131357726));
#258993=CARTESIAN_POINT('Ctrl Pts',(-43.7196778600618,-56.5029622466235,
-40.386692708542));
#258994=CARTESIAN_POINT('Ctrl Pts',(-43.7670264629127,-56.4700551612604,
-40.3935618621563));
#258995=CARTESIAN_POINT('Ctrl Pts',(-43.8165352419067,-56.4409186299576,
-40.4032471370382));
#258996=CARTESIAN_POINT('Ctrl Pts',(-43.8552784957563,-56.4218759376155,
-40.4126045758866));
#258997=CARTESIAN_POINT('Ctrl Pts',(-43.8814691350842,-56.4098116142502,
-40.4193119877837));
#258998=CARTESIAN_POINT('Ctrl Pts',(-43.8947490665381,-56.4040935548973,
-40.4229014011429));
#258999=CARTESIAN_POINT('Ctrl Pts',(-43.9216608718689,-56.3933018151258,
-40.430550144354));
#259000=CARTESIAN_POINT('Ctrl Pts',(-43.9353412421961,-56.3882139347518,
-40.434625723994));
#259001=CARTESIAN_POINT('Ctrl Pts',(-43.9627318697344,-56.3788058930362,
-40.4431514805252));
#259002=CARTESIAN_POINT('Ctrl Pts',(-43.9765011076412,-56.3744602994329,
-40.4476175822086));
#259003=CARTESIAN_POINT('Ctrl Pts',(-44.0179764085085,-56.3624961934912,
-40.4615970784657));
#259004=CARTESIAN_POINT('Ctrl Pts',(-44.0598195105868,-56.3526585058303,
-40.4767455237411));
#259005=CARTESIAN_POINT('Ctrl Pts',(-44.1163310625808,-56.3437038269143,
-40.4992178608308));
#259006=CARTESIAN_POINT('Ctrl Pts',(-44.1590753545772,-56.3390714325247,
-40.5172068769433));
#259007=CARTESIAN_POINT('Ctrl Pts',(-44.1878153726385,-56.337382052278,
-40.5299596579145));
#259008=CARTESIAN_POINT('Ctrl Pts',(-44.2166756293141,-56.3364007867548,
-40.5430944022758));
#259009=CARTESIAN_POINT('Ctrl Pts',(-44.2311921171808,-56.3362675100036,
-40.5498666179945));
#259010=CARTESIAN_POINT('Ctrl Pts',(-44.2599977007373,-56.3367129587916,
-40.5636298486377));
#259011=CARTESIAN_POINT('Ctrl Pts',(-44.2743541649932,-56.3372884158027,
-40.5706510752088));
#259012=CARTESIAN_POINT('Ctrl Pts',(-44.3029357424357,-56.3391317429585,
-40.5849473061899));
#259013=CARTESIAN_POINT('Ctrl Pts',(-44.3456316213443,-56.3429350642169,
-40.6067818596389));
#259014=CARTESIAN_POINT('Ctrl Pts',(-44.4018650235691,-56.3520939287388,
-40.6374236066311));
#259015=CARTESIAN_POINT('Ctrl Pts',(-44.4574103376146,-56.3653147883305,
-40.6695718678152));
#259016=CARTESIAN_POINT('Ctrl Pts',(-44.4849466005937,-56.3732907222196,
-40.686147922621));
#259017=CARTESIAN_POINT('Ctrl Pts',(-44.512374392093,-56.3819617528141,
-40.7029840503412));
#259018=CARTESIAN_POINT('Ctrl Pts',(-44.5260289861432,-56.3866462995878,
-40.7115304197201));
#259019=CARTESIAN_POINT('Ctrl Pts',(-44.5529609776699,-56.3966203919845,
-40.7287150345567));
#259020=CARTESIAN_POINT('Ctrl Pts',(-44.5662873943758,-56.4019250012471,
-40.737383176176));
#259021=CARTESIAN_POINT('Ctrl Pts',(-44.6058068395674,-56.4187668411382,
-40.7635834132132));
#259022=CARTESIAN_POINT('Ctrl Pts',(-44.6315615859976,-56.4312362585519,
-40.7813233152079));
#259023=CARTESIAN_POINT('Ctrl Pts',(-44.6693071486035,-56.4518014713652,
-40.8083384498991));
#259024=CARTESIAN_POINT('Ctrl Pts',(-44.6817372625133,-56.458965010373,
-40.8174084081892));
#259025=CARTESIAN_POINT('Ctrl Pts',(-44.7063132537473,-56.473929075182,
-40.8356956250034));
#259026=CARTESIAN_POINT('Ctrl Pts',(-44.7183832523531,-56.4816832398284,
-40.8448563495594));
#259027=CARTESIAN_POINT('Ctrl Pts',(-44.7538754102704,-56.505703003501,
-40.8723327540241));
#259028=CARTESIAN_POINT('Ctrl Pts',(-44.7766465418209,-56.5227549736834,
-40.8906872015444));
#259029=CARTESIAN_POINT('Ctrl Pts',(-44.8204030914552,-56.5588699415109,
-40.9274359243417));
#259030=CARTESIAN_POINT('Ctrl Pts',(-44.851893062885,-56.5874690797881,
-40.9550350105826));
#259031=CARTESIAN_POINT('Ctrl Pts',(-44.8813802932551,-56.6183507815631,
-40.982690555711));
#259032=CARTESIAN_POINT('Ctrl Pts',(-44.9005867815582,-56.6394533348067,
-41.0011404791447));
#259033=CARTESIAN_POINT('Ctrl Pts',(-44.9099603095753,-56.6502571213647,
-41.0103678872986));
#259034=CARTESIAN_POINT('Ctrl Pts',(-44.9236872082217,-56.6668706184025,
-41.0242310114538));
#259035=CARTESIAN_POINT('Ctrl Pts',(-44.9282031316495,-56.6724722064122,
-41.0288518918758));
#259036=CARTESIAN_POINT('Ctrl Pts',(-44.9370720489983,-56.6837477093971,
-41.038048314582));
#259037=CARTESIAN_POINT('Ctrl Pts',(-44.9414338933841,-56.6894322363092,
-41.0426327511372));
#259038=CARTESIAN_POINT('Ctrl Pts',(-44.9542884395491,-56.7066066663578,
-41.0563299560217));
#259039=CARTESIAN_POINT('Ctrl Pts',(-44.9625629539304,-56.7182326826763,
-41.0653994431984));
#259040=CARTESIAN_POINT('Ctrl Pts',(-44.9864941991718,-56.7536111473724,
-41.0924067111081));
#259041=CARTESIAN_POINT('Ctrl Pts',(-45.0086645271567,-56.7900134244028,
-41.1190329135161));
#259042=CARTESIAN_POINT('Ctrl Pts',(-45.034704630644,-56.8405768845403,
-41.1537712607408));
#259043=CARTESIAN_POINT('Ctrl Pts',(-45.0465408860903,-56.8665423758261,
-41.1708862092094));
#259044=CARTESIAN_POINT('Ctrl Pts',(-45.0577761134165,-56.8928546179869,
-41.1878727246706));
#259045=CARTESIAN_POINT('Ctrl Pts',(-45.0630901582258,-56.906176087846,
-41.1962967595746));
#259046=CARTESIAN_POINT('Ctrl Pts',(-45.0731156002939,-56.9332061371524,
-41.2130345018643));
#259047=CARTESIAN_POINT('Ctrl Pts',(-45.0777961712447,-56.9468340019015,
-41.2212978165198));
#259048=CARTESIAN_POINT('Ctrl Pts',(-45.0907786540592,-56.9878560258786,
-41.2456540007716));
#259049=CARTESIAN_POINT('Ctrl Pts',(-45.0980724298404,-57.0154910056487,
-41.2613826498774));
#259050=CARTESIAN_POINT('Ctrl Pts',(-45.1099506000897,-57.0712899900431,
-41.2918166667949));
#259051=CARTESIAN_POINT('Ctrl Pts',(-45.1168338059478,-57.11354441615,-41.3138815317038));
#259052=CARTESIAN_POINT('Ctrl Pts',(-45.1206309792415,-57.1564190282566,
-41.3347987762303));
#259053=CARTESIAN_POINT('Ctrl Pts',(-45.1224627479043,-57.1851396939165,
-41.3484832320635));
#259054=CARTESIAN_POINT('Ctrl Pts',(-45.1230291819396,-57.199581674993,
-41.3552011986272));
#259055=CARTESIAN_POINT('Ctrl Pts',(-45.1234439819388,-57.2285619504273,
-41.3683510337761));
#259056=CARTESIAN_POINT('Ctrl Pts',(-45.1232917301137,-57.2429904040975,
-41.3747335054784));
#259057=CARTESIAN_POINT('Ctrl Pts',(-45.122279779691,-57.2717682086368,
-41.3871399525693));
#259058=CARTESIAN_POINT('Ctrl Pts',(-45.1196997436484,-57.3147947598186,
-41.4052018313649));
#259059=CARTESIAN_POINT('Ctrl Pts',(-45.1120557453653,-57.3716084168758,
-41.4271228345082));
#259060=CARTESIAN_POINT('Ctrl Pts',(-45.1031553338884,-57.4137999065974,
-41.4419446800329));
#259061=CARTESIAN_POINT('Ctrl Pts',(-45.09650693546,-57.4418330021969,-41.4514615780937));
#259062=CARTESIAN_POINT('Ctrl Pts',(-45.092823442876,-57.4558081403435,
-41.4560396298995));
#259063=CARTESIAN_POINT('Ctrl Pts',(-45.08473584999,-57.4836385233421,-41.464818484644));
#259064=CARTESIAN_POINT('Ctrl Pts',(-45.0803094818206,-57.4975537933777,
-41.4690360581021));
#259065=CARTESIAN_POINT('Ctrl Pts',(-45.0708158371377,-57.5249803724867,
-41.4770040232021));
#259066=CARTESIAN_POINT('Ctrl Pts',(-45.060662137239,-57.5520858826269,
-41.4845331733926));
#259067=CARTESIAN_POINT('Ctrl Pts',(-45.0434887903859,-57.591755117417,
-41.4945182619959));
#259068=CARTESIAN_POINT('Ctrl Pts',(-45.0243848727922,-57.6304534586566,
-41.5032105668009));
#259069=CARTESIAN_POINT('Ctrl Pts',(-45.0033512023575,-57.6681778817651,
-41.51061115159));
#259070=CARTESIAN_POINT('Ctrl Pts',(-44.9880328234845,-57.692673879575,
-41.5146787869643));
#259071=CARTESIAN_POINT('Ctrl Pts',(-44.9720568870916,-57.7168380825906,
-41.5183074012753));
#259072=CARTESIAN_POINT('Ctrl Pts',(-44.9637457009402,-57.7287466936453,
-41.5199012977462));
#259073=CARTESIAN_POINT('Ctrl Pts',(-44.9464287138105,-57.7522550306847,
-41.5226441863212));
#259074=CARTESIAN_POINT('Ctrl Pts',(-44.9374830238235,-57.7637718882179,
-41.5237830976086));
#259075=CARTESIAN_POINT('Ctrl Pts',(-44.9099214446927,-57.7974515399035,
-41.5264929611258));
#259076=CARTESIAN_POINT('Ctrl Pts',(-44.8905204729439,-57.8188493934961,
-41.5273772161885));
#259077=CARTESIAN_POINT('Ctrl Pts',(-44.8497318000032,-57.8595330722204,
-41.5273307191807));
#259078=CARTESIAN_POINT('Ctrl Pts',(-44.8283374647208,-57.878828810327,
-41.5264014189239));
#259079=CARTESIAN_POINT('Ctrl Pts',(-44.7947479986672,-57.9061820008563,
-41.5236391765087));
#259080=CARTESIAN_POINT('Ctrl Pts',(-44.7832945060713,-57.9150388128137,
-41.5224889540588));
#259081=CARTESIAN_POINT('Ctrl Pts',(-44.7657408175914,-57.9279147771907,
-41.5204166102647));
#259082=CARTESIAN_POINT('Ctrl Pts',(-44.7598217545323,-57.9321421746299,
-41.5196671186517));
#259083=CARTESIAN_POINT('Ctrl Pts',(-44.7478629508254,-57.9404557426351,
-41.5180519716851));
#259084=CARTESIAN_POINT('Ctrl Pts',(-44.7297025277655,-57.9527400844071,
-41.5154481926132));
#259085=CARTESIAN_POINT('Ctrl Pts',(-44.711220794734,-57.9642369190977,
-41.5123523449538));
#259086=CARTESIAN_POINT('Ctrl Pts',(-44.6862770262529,-57.9788987855805,
-41.5077941640223));
#259087=CARTESIAN_POINT('Ctrl Pts',(-44.6484202704456,-57.9998814948776,
-41.5003121274858));
#259088=CARTESIAN_POINT('Ctrl Pts',(-44.5962108390282,-58.0238874022289,
-41.4877980263462));
#259089=CARTESIAN_POINT('Ctrl Pts',(-44.5557649369164,-58.0389385823793,
-41.4765186283493));
#259090=CARTESIAN_POINT('Ctrl Pts',(-44.5285120653069,-58.048310487242,
-41.4685735203231));
#259091=CARTESIAN_POINT('Ctrl Pts',(-44.5147341086114,-58.0526671867402,
-41.4643859028639));
#259092=CARTESIAN_POINT('Ctrl Pts',(-44.4869140318333,-58.0607029371288,
-41.4555883503401));
#259093=CARTESIAN_POINT('Ctrl Pts',(-44.4728027150897,-58.0643973546439,
-41.4509544537452));
#259094=CARTESIAN_POINT('Ctrl Pts',(-44.4304531283686,-58.0743536715507,
-41.4365378845966));
#259095=CARTESIAN_POINT('Ctrl Pts',(-44.3879697631396,-58.0821103913619,
-41.4210702443308));
#259096=CARTESIAN_POINT('Ctrl Pts',(-44.3452880889881,-58.0866896268435,
-41.4040725286766));
#259097=CARTESIAN_POINT('Ctrl Pts',(-44.3025416355467,-58.090217180745,
-41.3865671155567));
#259098=CARTESIAN_POINT('Ctrl Pts',(-44.2739489581488,-58.0911687787978,
-41.3742170239002));
#259099=CARTESIAN_POINT('Ctrl Pts',(-44.2309555122234,-58.090491506171,
-41.3546803180427));
#259100=CARTESIAN_POINT('Ctrl Pts',(-44.2165895018292,-58.0899123697243,
-41.347990487553));
#259101=CARTESIAN_POINT('Ctrl Pts',(-44.1950278537333,-58.0885113544661,
-41.337705180963));
#259102=CARTESIAN_POINT('Ctrl Pts',(-44.1878319550126,-58.0879547296283,
-41.3342316293533));
#259103=CARTESIAN_POINT('Ctrl Pts',(-44.1734279164018,-58.0866616594573,
-41.3271961709002));
#259104=CARTESIAN_POINT('Ctrl Pts',(-44.1662260389348,-58.0859253983809,
-41.3236371482021));
#259105=CARTESIAN_POINT('Ctrl Pts',(-44.130389101081,-58.0818150523559,
-41.3057210105631));
#259106=CARTESIAN_POINT('Ctrl Pts',(-44.073848260417,-58.0724828543971,
-41.2761395013722));
#259107=CARTESIAN_POINT('Ctrl Pts',(-44.0188545174212,-58.0578491440998,
-41.2447838757269));
#259108=CARTESIAN_POINT('Ctrl Pts',(-43.9646246641704,-58.0405931079736,
-41.2125419608827));
#259109=CARTESIAN_POINT('Ctrl Pts',(-43.9378880325505,-58.0306505669816,
-41.1959746665064));
#259110=CARTESIAN_POINT('Ctrl Pts',(-43.9049634769563,-58.0165631445999,
-41.174705886574));
#259111=CARTESIAN_POINT('Ctrl Pts',(-43.898399460067,-58.0136596367661,
-41.1704209658528));
#259112=CARTESIAN_POINT('Ctrl Pts',(-43.8853286348063,-58.0076886655405,
-41.1617993561325));
#259113=CARTESIAN_POINT('Ctrl Pts',(-43.8788088737381,-58.0046144513738,
-41.157453730181));
#259114=CARTESIAN_POINT('Ctrl Pts',(-43.8593967360427,-57.9951717320096,
-41.1443784829743));
#259115=CARTESIAN_POINT('Ctrl Pts',(-43.8466719188398,-57.9885954718361,
-41.1356253645631));
#259116=CARTESIAN_POINT('Ctrl Pts',(-43.8341420587998,-57.9817357678076,
-41.1268248734572));
#259117=CARTESIAN_POINT('Ctrl Pts',(-45.9506478428458,-58.3141066664263,
-40.3575668188428));
#259118=CARTESIAN_POINT('Ctrl Pts',(-45.9187159875041,-58.4427318713764,
-40.3284662798477));
#259119=CARTESIAN_POINT('Ctrl Pts',(-45.8662597178432,-58.5652908169572,
-40.3027297091841));
#259120=CARTESIAN_POINT('Ctrl Pts',(-45.7408073320632,-58.7557683566169,
-40.2662627946592));
#259121=CARTESIAN_POINT('Ctrl Pts',(-45.6790009363265,-58.8279963011486,
-40.2535679867602));
#259122=CARTESIAN_POINT('Ctrl Pts',(-45.5604868254795,-58.9348862510393,
-40.2365559979816));
#259123=CARTESIAN_POINT('Ctrl Pts',(-45.5089640560027,-58.9738218628677,
-40.2309032397059));
#259124=CARTESIAN_POINT('Ctrl Pts',(-45.4511612750621,-59.0101321417087,
-40.2261786038362));
#259125=CARTESIAN_POINT('Ctrl Pts',(-45.4480371162561,-59.0120733533552,
-40.225927923055));
#259126=CARTESIAN_POINT('Ctrl Pts',(-45.4417466121093,-59.015939425046,
-40.2254324787861));
#259127=CARTESIAN_POINT('Ctrl Pts',(-45.4385803758859,-59.0178639115207,
-40.2251877908802));
#259128=CARTESIAN_POINT('Ctrl Pts',(-45.4289273025488,-59.0236663554915,
-40.2244558904502));
#259129=CARTESIAN_POINT('Ctrl Pts',(-45.4224008854538,-59.0275005455267,
-40.2239803627221));
#259130=CARTESIAN_POINT('Ctrl Pts',(-45.4091894470304,-59.0350866163115,
-40.2230553863648));
#259131=CARTESIAN_POINT('Ctrl Pts',(-45.4024735404165,-59.0388524512952,
-40.2226046964558));
#259132=CARTESIAN_POINT('Ctrl Pts',(-45.3308213216707,-59.0780782303883,
-40.2180000493414));
#259133=CARTESIAN_POINT('Ctrl Pts',(-45.2626750700944,-59.1071890367889,
-40.2153702456219));
#259134=CARTESIAN_POINT('Ctrl Pts',(-45.0546969823245,-59.1736287470141,
-40.2117346205805));
#259135=CARTESIAN_POINT('Ctrl Pts',(-44.910874640258,-59.192104560712,-40.2145478148852));
#259136=CARTESIAN_POINT('Ctrl Pts',(-44.6409196303305,-59.1827735438882,
-40.2265311750986));
#259137=CARTESIAN_POINT('Ctrl Pts',(-44.5382095666334,-59.1613643120583,
-40.233858657804));
#259138=CARTESIAN_POINT('Ctrl Pts',(-44.4689492302736,-59.1437418920634,
-40.2388225645965));
#259139=CARTESIAN_POINT('Ctrl Pts',(-43.4805771074156,-59.5712767529309,
-39.2399080357013));
#259140=CARTESIAN_POINT('Ctrl Pts',(-43.4150727209207,-59.5358440364426,
-39.2223070534893));
#259141=CARTESIAN_POINT('Ctrl Pts',(-43.2883193276586,-59.4590682572254,
-39.1867578392588));
#259142=CARTESIAN_POINT('Ctrl Pts',(-43.1106712693135,-59.32658002426,-39.1324031814995));
#259143=CARTESIAN_POINT('Ctrl Pts',(-43.0005921597408,-59.2266373021163,
-39.0954660506179));
#259144=CARTESIAN_POINT('Ctrl Pts',(-42.8948534568781,-59.1207134074407,
-39.0581733199915));
#259145=CARTESIAN_POINT('Ctrl Pts',(-42.7951360401793,-59.0104958554849,
-39.0211184761739));
#259146=CARTESIAN_POINT('Ctrl Pts',(-42.6850011896347,-58.8622904152127,
-38.9753582681256));
#259147=CARTESIAN_POINT('Ctrl Pts',(-42.6055727997797,-58.7375004045667,
-38.939089851323));
#259148=CARTESIAN_POINT('Ctrl Pts',(-42.5503788594446,-58.6407591922129,
-38.9120596161462));
#259149=CARTESIAN_POINT('Ctrl Pts',(-42.5165536369311,-58.5741539171446,
-38.8941613358138));
#259150=CARTESIAN_POINT('Ctrl Pts',(-42.4842288567228,-58.5064298632496,
-38.8763157156907));
#259151=CARTESIAN_POINT('Ctrl Pts',(-42.4689425396028,-58.4722695523732,
-38.8674882509199));
#259152=CARTESIAN_POINT('Ctrl Pts',(-42.4257123024776,-58.3690064948315,
-38.8413136266604));
#259153=CARTESIAN_POINT('Ctrl Pts',(-42.3750272156063,-58.229152189777,
-38.8072100415055));
#259154=CARTESIAN_POINT('Ctrl Pts',(-42.3380647902547,-58.0850119200902,
-38.7746901633276));
#259155=CARTESIAN_POINT('Ctrl Pts',(-42.3155659796374,-57.9752818499468,
-38.7509105250088));
#259156=CARTESIAN_POINT('Ctrl Pts',(-42.3089374211558,-57.9384266221928,
-38.7430843922672));
#259157=CARTESIAN_POINT('Ctrl Pts',(-42.297458012674,-57.864178756387,-38.7276438637217));
#259158=CARTESIAN_POINT('Ctrl Pts',(-42.292601515188,-57.8267325312259,
-38.720018782004));
#259159=CARTESIAN_POINT('Ctrl Pts',(-42.2847289916893,-57.7514526301959,
-38.7050196673963));
#259160=CARTESIAN_POINT('Ctrl Pts',(-42.2817363521424,-57.7138759968928,
-38.6976962453237));
#259161=CARTESIAN_POINT('Ctrl Pts',(-42.277596992864,-57.6387184974263,
-38.6833720377019));
#259162=CARTESIAN_POINT('Ctrl Pts',(-42.2741651307842,-57.5260409596698,
-38.6623829091612));
#259163=CARTESIAN_POINT('Ctrl Pts',(-42.2805893100654,-57.3760354719141,
-38.6363740800325));
#259164=CARTESIAN_POINT('Ctrl Pts',(-42.2937061680812,-57.2637038035873,
-38.618370061439));
#259165=CARTESIAN_POINT('Ctrl Pts',(-42.3043247017591,-57.1888547452426,
-38.6067079534822));
#259166=CARTESIAN_POINT('Ctrl Pts',(-42.3105743117123,-57.1514345461221,
-38.6010450635964));
#259167=CARTESIAN_POINT('Ctrl Pts',(-42.3249704170347,-57.0766935209607,
-38.590076215021));
#259168=CARTESIAN_POINT('Ctrl Pts',(-42.3331592025312,-57.0392159768686,
-38.5847494243559));
#259169=CARTESIAN_POINT('Ctrl Pts',(-42.3512949844302,-56.9651221381903,
-38.5745673038812));
#259170=CARTESIAN_POINT('Ctrl Pts',(-42.3712216906218,-56.8916587034686,
-38.564820665347));
#259171=CARTESIAN_POINT('Ctrl Pts',(-42.4063979707918,-56.7834465224234,
-38.5515118436));
#259172=CARTESIAN_POINT('Ctrl Pts',(-42.4468320479729,-56.6771725078319,
-38.5395042677724));
#259173=CARTESIAN_POINT('Ctrl Pts',(-42.4925290654744,-56.5728473165674,
-38.5288039137004));
#259174=CARTESIAN_POINT('Ctrl Pts',(-42.5265325119253,-56.5046058456765,
-38.5225509073062));
#259175=CARTESIAN_POINT('Ctrl Pts',(-42.5623338475306,-56.4370293947697,
-38.5167461666044));
#259176=CARTESIAN_POINT('Ctrl Pts',(-42.5811223641794,-56.4035923099625,
-38.5140693065785));
#259177=CARTESIAN_POINT('Ctrl Pts',(-42.620584523009,-56.3373241998654,
-38.5091697400817));
#259178=CARTESIAN_POINT('Ctrl Pts',(-42.6411082254821,-56.3047465904101,
-38.5069659500128));
#259179=CARTESIAN_POINT('Ctrl Pts',(-42.7048067991197,-56.2090283357163,
-38.501110858935));
#259180=CARTESIAN_POINT('Ctrl Pts',(-42.7502234543428,-56.1476408662828,
-38.4981890389281));
#259181=CARTESIAN_POINT('Ctrl Pts',(-42.8467942323831,-56.0297655581676,
-38.4942910511033));
#259182=CARTESIAN_POINT('Ctrl Pts',(-42.8979715413934,-55.9732420482176,
-38.4933125989996));
#259183=CARTESIAN_POINT('Ctrl Pts',(-42.9790570553347,-55.8921695883033,
-38.4933149859729));
#259184=CARTESIAN_POINT('Ctrl Pts',(-43.0068374106561,-55.8657400908868,
-38.4935622007431));
#259185=CARTESIAN_POINT('Ctrl Pts',(-43.0495800649421,-55.8270637749536,
-38.4943063068789));
#259186=CARTESIAN_POINT('Ctrl Pts',(-43.0640222060113,-55.8143203511958,
-38.494617152342));
#259187=CARTESIAN_POINT('Ctrl Pts',(-43.0932714774893,-55.7891564261061,
-38.4953646906773));
#259188=CARTESIAN_POINT('Ctrl Pts',(-43.1080901283632,-55.7767277938553,
-38.4958020036096));
#259189=CARTESIAN_POINT('Ctrl Pts',(-43.1528523310046,-55.7401327167866,
-38.4972962980169));
#259190=CARTESIAN_POINT('Ctrl Pts',(-43.2134913856688,-55.6930468850421,
-38.4997758707861));
#259191=CARTESIAN_POINT('Ctrl Pts',(-43.3385569247743,-55.6055389451161,
-38.5066450244003));
#259192=CARTESIAN_POINT('Ctrl Pts',(-43.4691986576013,-55.5278792007279,
-38.5163302992824));
#259193=CARTESIAN_POINT('Ctrl Pts',(-43.5713395927684,-55.4769743237494,
-38.5256877381308));
#259194=CARTESIAN_POINT('Ctrl Pts',(-43.6403672861995,-55.4446857735354,
-38.5323951500278));
#259195=CARTESIAN_POINT('Ctrl Pts',(-43.6753577685123,-55.4293620157832,
-38.5359845633874));
#259196=CARTESIAN_POINT('Ctrl Pts',(-43.7462462065788,-55.4003985583156,
-38.5436333065981));
#259197=CARTESIAN_POINT('Ctrl Pts',(-43.7822717759725,-55.3867204456352,
-38.5477088862383));
#259198=CARTESIAN_POINT('Ctrl Pts',(-43.8543821738219,-55.3613797848081,
-38.5562346427694));
#259199=CARTESIAN_POINT('Ctrl Pts',(-43.890622407919,-55.349649082917,-38.5607007444526));
#259200=CARTESIAN_POINT('Ctrl Pts',(-43.9997560709039,-55.3172704656441,
-38.5746802407103));
#259201=CARTESIAN_POINT('Ctrl Pts',(-44.1098017310836,-55.290468361793,
-38.5898286859852));
#259202=CARTESIAN_POINT('Ctrl Pts',(-44.2583166685835,-55.2656490138239,
-38.612301023075));
#259203=CARTESIAN_POINT('Ctrl Pts',(-44.3705972700495,-55.2524997368729,
-38.6302900391873));
#259204=CARTESIAN_POINT('Ctrl Pts',(-44.446056048267,-55.2474029004138,
-38.6430428201589));
#259205=CARTESIAN_POINT('Ctrl Pts',(-44.5218128020516,-55.2441636366351,
-38.65617756452));
#259206=CARTESIAN_POINT('Ctrl Pts',(-44.5599089424743,-55.2434808562086,
-38.6629497802385));
#259207=CARTESIAN_POINT('Ctrl Pts',(-44.6354869543582,-55.2439911084578,
-38.6767130108817));
#259208=CARTESIAN_POINT('Ctrl Pts',(-44.6731456892459,-55.2451740103824,
-38.6837342374529));
#259209=CARTESIAN_POINT('Ctrl Pts',(-44.7481014788608,-55.2493620066237,
-38.6980304684339));
#259210=CARTESIAN_POINT('Ctrl Pts',(-44.860046548974,-55.2583760573225,
-38.7198650218829));
#259211=CARTESIAN_POINT('Ctrl Pts',(-45.0073845433675,-55.2811507310277,
-38.7505067688753));
#259212=CARTESIAN_POINT('Ctrl Pts',(-45.1528189888476,-55.3146135839333,
-38.7826550300594));
#259213=CARTESIAN_POINT('Ctrl Pts',(-45.2248832056965,-55.3349380951144,
-38.7992310848652));
#259214=CARTESIAN_POINT('Ctrl Pts',(-45.2966462681613,-55.3570913336823,
-38.8160672125853));
#259215=CARTESIAN_POINT('Ctrl Pts',(-45.3323638946335,-55.3690863290504,
-38.8246135819642));
#259216=CARTESIAN_POINT('Ctrl Pts',(-45.4027951436545,-55.3946744461232,
-38.841798196801));
#259217=CARTESIAN_POINT('Ctrl Pts',(-45.4376370321487,-55.4083060218429,
-38.85046633842));
#259218=CARTESIAN_POINT('Ctrl Pts',(-45.5409345111852,-55.4516493275196,
-38.8766665754573));
#259219=CARTESIAN_POINT('Ctrl Pts',(-45.6082182891413,-55.4838201174091,
-38.8944064774514));
#259220=CARTESIAN_POINT('Ctrl Pts',(-45.7067749877369,-55.5369855856676,
-38.9214216121435));
#259221=CARTESIAN_POINT('Ctrl Pts',(-45.7392219877795,-55.5555212114618,
-38.9304915704334));
#259222=CARTESIAN_POINT('Ctrl Pts',(-45.8033556832395,-55.5942722159849,
-38.9487787872477));
#259223=CARTESIAN_POINT('Ctrl Pts',(-45.8348443691401,-55.6143675312756,
-38.9579395118015));
#259224=CARTESIAN_POINT('Ctrl Pts',(-45.9274099842789,-55.6766589025306,
-38.9854159162723));
#259225=CARTESIAN_POINT('Ctrl Pts',(-45.9867610865919,-55.7209353156014,
-39.0037703637879));
#259226=CARTESIAN_POINT('Ctrl Pts',(-46.1007337830098,-55.8148102393793,
-39.0405190865864));
#259227=CARTESIAN_POINT('Ctrl Pts',(-46.1826971388658,-55.889219933262,
-39.0681181728269));
#259228=CARTESIAN_POINT('Ctrl Pts',(-46.259356574729,-55.9696687352924,
-39.0957737179551));
#259229=CARTESIAN_POINT('Ctrl Pts',(-46.309266807939,-56.024663053365,-39.1142236413887));
#259230=CARTESIAN_POINT('Ctrl Pts',(-46.3336138177017,-56.0528284109483,
-39.1234510495426));
#259231=CARTESIAN_POINT('Ctrl Pts',(-46.3692509284248,-56.0961546965833,
-39.1373141736981));
#259232=CARTESIAN_POINT('Ctrl Pts',(-46.3809719555493,-56.1107655250657,
-39.14193505412));
#259233=CARTESIAN_POINT('Ctrl Pts',(-46.4039850968433,-56.1401806715041,
-39.1511314768264));
#259234=CARTESIAN_POINT('Ctrl Pts',(-46.4153001903629,-56.1550126624776,
-39.1557159133813));
#259235=CARTESIAN_POINT('Ctrl Pts',(-46.4486370096885,-56.1998310060263,
-39.1694131182659));
#259236=CARTESIAN_POINT('Ctrl Pts',(-46.4700835091466,-56.2301795317326,
-39.1784826054425));
#259237=CARTESIAN_POINT('Ctrl Pts',(-46.532071913686,-56.3225583984772,
-39.2054898733524));
#259238=CARTESIAN_POINT('Ctrl Pts',(-46.5894197348374,-56.4176636744323,
-39.23211607576));
#259239=CARTESIAN_POINT('Ctrl Pts',(-46.6566074362748,-56.5498680842415,
-39.2668544229849));
#259240=CARTESIAN_POINT('Ctrl Pts',(-46.6870820302515,-56.617790568625,
-39.2839693714534));
#259241=CARTESIAN_POINT('Ctrl Pts',(-46.7159729830272,-56.6866360545619,
-39.3009558869148));
#259242=CARTESIAN_POINT('Ctrl Pts',(-46.7296188023799,-56.7214992889704,
-39.3093799218186));
#259243=CARTESIAN_POINT('Ctrl Pts',(-46.7553216997643,-56.7922546384013,
-39.3261176641085));
#259244=CARTESIAN_POINT('Ctrl Pts',(-46.7672996943011,-56.8279354881579,
-39.3343809787628));
#259245=CARTESIAN_POINT('Ctrl Pts',(-46.8004530502947,-56.9353633959568,
-39.358737163018));
#259246=CARTESIAN_POINT('Ctrl Pts',(-46.8189795501832,-57.0077635587999,
-39.3744658121213));
#259247=CARTESIAN_POINT('Ctrl Pts',(-46.848916211803,-57.1540080946302,
-39.4048998290393));
#259248=CARTESIAN_POINT('Ctrl Pts',(-46.866048617508,-57.2647966217996,
-39.4269646939479));
#259249=CARTESIAN_POINT('Ctrl Pts',(-46.875074749658,-57.3772756893033,
-39.4478819384746));
#259250=CARTESIAN_POINT('Ctrl Pts',(-46.8792542953452,-57.4526370309597,
-39.4615663943076));
#259251=CARTESIAN_POINT('Ctrl Pts',(-46.8804258736835,-57.4905390832845,
-39.4682843608713));
#259252=CARTESIAN_POINT('Ctrl Pts',(-46.8808837743635,-57.566610437341,
-39.4814341960201));
#259253=CARTESIAN_POINT('Ctrl Pts',(-46.8801708637706,-57.604491394965,
-39.4878166677226));
#259254=CARTESIAN_POINT('Ctrl Pts',(-46.8768913879562,-57.6800597985945,
-39.5002231148134));
#259255=CARTESIAN_POINT('Ctrl Pts',(-46.8691896925243,-57.7930657109158,
-39.5182849936093));
#259256=CARTESIAN_POINT('Ctrl Pts',(-46.8479069711518,-57.9423669591112,
-39.540205996752));
#259257=CARTESIAN_POINT('Ctrl Pts',(-46.8236459543104,-58.053306681129,
-39.5550278422771));
#259258=CARTESIAN_POINT('Ctrl Pts',(-46.8055990109883,-58.1270324939452,
-39.5645447403379));
#259259=CARTESIAN_POINT('Ctrl Pts',(-46.7956339676918,-58.1637938532181,
-39.5691227921436));
#259260=CARTESIAN_POINT('Ctrl Pts',(-46.7738161327052,-58.2370162077019,
-39.5779016468881));
#259261=CARTESIAN_POINT('Ctrl Pts',(-46.7619036278491,-58.2736352268715,
-39.5821192203466));
#259262=CARTESIAN_POINT('Ctrl Pts',(-46.7364059718256,-58.3458255995332,
-39.5900871854462));
#259263=CARTESIAN_POINT('Ctrl Pts',(-46.7091836493705,-58.4171862986019,
-39.5976163356366));
#259264=CARTESIAN_POINT('Ctrl Pts',(-46.663274408039,-58.5216699086648,
-39.6076014242402));
#259265=CARTESIAN_POINT('Ctrl Pts',(-46.6123207377325,-58.6236436013082,
-39.616293729045));
#259266=CARTESIAN_POINT('Ctrl Pts',(-46.5563244858032,-58.7230996041114,
-39.6236943138341));
#259267=CARTESIAN_POINT('Ctrl Pts',(-46.515607032986,-58.7877140896312,
-39.6277619492082));
#259268=CARTESIAN_POINT('Ctrl Pts',(-46.4731710833873,-58.8514710047945,
-39.6313905635194));
#259269=CARTESIAN_POINT('Ctrl Pts',(-46.4511086137465,-58.8829006319494,
-39.6329844599904));
#259270=CARTESIAN_POINT('Ctrl Pts',(-46.4051673201274,-58.9449633016888,
-39.6357273485653));
#259271=CARTESIAN_POINT('Ctrl Pts',(-46.381447994276,-58.975377588932,-39.6368662598532));
#259272=CARTESIAN_POINT('Ctrl Pts',(-46.3084068909562,-59.0643493136614,
-39.6395761233691));
#259273=CARTESIAN_POINT('Ctrl Pts',(-46.2570407846102,-59.1209150453974,
-39.6404603784325));
#259274=CARTESIAN_POINT('Ctrl Pts',(-46.1491379755941,-59.228544463199,
-39.6404138814247));
#259275=CARTESIAN_POINT('Ctrl Pts',(-46.0925836555155,-59.2796343044913,
-39.6394845811684));
#259276=CARTESIAN_POINT('Ctrl Pts',(-46.0038529437629,-59.3521266125547,
-39.6367223387528));
#259277=CARTESIAN_POINT('Ctrl Pts',(-45.9736068078661,-59.3756113554055,
-39.6355721163029));
#259278=CARTESIAN_POINT('Ctrl Pts',(-45.9272656961273,-59.4097723546528,
-39.6334997725088));
#259279=CARTESIAN_POINT('Ctrl Pts',(-45.9116419215573,-59.4209912820171,
-39.6327502808957));
#259280=CARTESIAN_POINT('Ctrl Pts',(-45.8800804794677,-59.4430610802669,
-39.6311351339295));
#259281=CARTESIAN_POINT('Ctrl Pts',(-45.8321587971618,-59.4756823489919,
-39.628531354857));
#259282=CARTESIAN_POINT('Ctrl Pts',(-45.7834097108732,-59.5062438963941,
-39.6254355071979));
#259283=CARTESIAN_POINT('Ctrl Pts',(-45.717633106262,-59.5452481912826,
-39.6208773262667));
#259284=CARTESIAN_POINT('Ctrl Pts',(-45.6178307490054,-59.601113548897,
-39.6133952897297));
#259285=CARTESIAN_POINT('Ctrl Pts',(-45.4802897643185,-59.6652183443042,
-39.6008811885904));
#259286=CARTESIAN_POINT('Ctrl Pts',(-45.3738098009101,-59.7055766782111,
-39.5896017905935));
#259287=CARTESIAN_POINT('Ctrl Pts',(-45.3020778813705,-59.7307512119865,
-39.5816566825671));
#259288=CARTESIAN_POINT('Ctrl Pts',(-45.2658207311094,-59.7424779859237,
-39.5774690651077));
#259289=CARTESIAN_POINT('Ctrl Pts',(-45.1926264675053,-59.7641596016776,
-39.5686715125846));
#259290=CARTESIAN_POINT('Ctrl Pts',(-45.1555073907618,-59.7741562512684,
-39.5640376159893));
#259291=CARTESIAN_POINT('Ctrl Pts',(-45.0441315765335,-59.8011904590316,
-39.5496210468413));
#259292=CARTESIAN_POINT('Ctrl Pts',(-44.9324484012679,-59.8224577850013,
-39.5341534065747));
#259293=CARTESIAN_POINT('Ctrl Pts',(-44.8203079610257,-59.8353953605365,
-39.5171556909205));
#259294=CARTESIAN_POINT('Ctrl Pts',(-44.7080184564226,-59.8455760612675,
-39.4996502778008));
#259295=CARTESIAN_POINT('Ctrl Pts',(-44.6329372249224,-59.8486931621852,
-39.4873001861445));
#259296=CARTESIAN_POINT('Ctrl Pts',(-44.5200834441659,-59.8478515133141,
-39.4677634802869));
#259297=CARTESIAN_POINT('Ctrl Pts',(-44.4823810871712,-59.8466449718289,
-39.4610736497974));
#259298=CARTESIAN_POINT('Ctrl Pts',(-44.4258051079382,-59.8434394706745,
-39.4507883432074));
#259299=CARTESIAN_POINT('Ctrl Pts',(-44.4069254589855,-59.8421361346926,
-39.4473147915973));
#259300=CARTESIAN_POINT('Ctrl Pts',(-44.3691376542581,-59.8390581625153,
-39.4402793331445));
#259301=CARTESIAN_POINT('Ctrl Pts',(-44.3502459350849,-59.8372838734483,
-39.4367203104461));
#259302=CARTESIAN_POINT('Ctrl Pts',(-44.2562487381671,-59.8272835659938,
-39.4188041728073));
#259303=CARTESIAN_POINT('Ctrl Pts',(-44.1080045765469,-59.8040393501646,
-39.3892226636159));
#259304=CARTESIAN_POINT('Ctrl Pts',(-43.9639303529155,-59.7668593120831,
-39.3578670379715));
#259305=CARTESIAN_POINT('Ctrl Pts',(-43.8219159040518,-59.7227861654643,
-39.3256251231267));
#259306=CARTESIAN_POINT('Ctrl Pts',(-43.7519290534068,-59.6972943066161,
-39.3090578287531));
#259307=CARTESIAN_POINT('Ctrl Pts',(-43.665783177736,-59.6610675807531,
-39.2877890488175));
#259308=CARTESIAN_POINT('Ctrl Pts',(-43.6486106666635,-59.653596197985,
-39.2835041280971));
#259309=CARTESIAN_POINT('Ctrl Pts',(-43.6144193015916,-59.6382222359849,
-39.2748825183767));
#259310=CARTESIAN_POINT('Ctrl Pts',(-43.597366582891,-59.6303022352814,
-39.2705368924251));
#259311=CARTESIAN_POINT('Ctrl Pts',(-43.5465994182959,-59.605961903298,
-39.2574616452183));
#259312=CARTESIAN_POINT('Ctrl Pts',(-43.513329300663,-59.588993111175,-39.2487085268073));
#259313=CARTESIAN_POINT('Ctrl Pts',(-43.4805771074156,-59.5712767529309,
-39.2399080357013));
#259314=CARTESIAN_POINT('Ctrl Pts',(-43.8341420587998,-57.9817357678076,
-41.1268248734572));
#259315=CARTESIAN_POINT('Ctrl Pts',(-43.8090823387197,-57.9680163597508,
-41.1092238912453));
#259316=CARTESIAN_POINT('Ctrl Pts',(-43.7605654269547,-57.9383371077444,
-41.0736746770147));
#259317=CARTESIAN_POINT('Ctrl Pts',(-43.6924895655639,-57.8872515755908,
-41.019320019256));
#259318=CARTESIAN_POINT('Ctrl Pts',(-43.6502497090231,-57.8487916199066,
-40.9823828883729));
#259319=CARTESIAN_POINT('Ctrl Pts',(-43.6096433745973,-57.8080652293815,
-40.945090157748));
#259320=CARTESIAN_POINT('Ctrl Pts',(-43.5713160673933,-57.7657212262301,
-40.9080353139296));
#259321=CARTESIAN_POINT('Ctrl Pts',(-43.5288984657655,-57.7088609123343,
-40.8622751058818));
#259322=CARTESIAN_POINT('Ctrl Pts',(-43.4982484100127,-57.6610280687967,
-40.826006689079));
#259323=CARTESIAN_POINT('Ctrl Pts',(-43.4769169762936,-57.6239677344727,
-40.798976453902));
#259324=CARTESIAN_POINT('Ctrl Pts',(-43.4638199758968,-57.5984660781933,
-40.7810781735695));
#259325=CARTESIAN_POINT('Ctrl Pts',(-43.4512904535732,-57.5725430453748,
-40.7632325534464));
#259326=CARTESIAN_POINT('Ctrl Pts',(-43.4453582046716,-57.5594707895743,
-40.7544050886758));
#259327=CARTESIAN_POINT('Ctrl Pts',(-43.4285595200757,-57.5199648485381,
-40.7282304644163));
#259328=CARTESIAN_POINT('Ctrl Pts',(-43.4088016745783,-57.4664867157472,
-40.6941268792613));
#259329=CARTESIAN_POINT('Ctrl Pts',(-43.3942530508608,-57.4114223976644,
-40.6616070010832));
#259330=CARTESIAN_POINT('Ctrl Pts',(-43.3853242538269,-57.3695231591805,
-40.6378273627645));
#259331=CARTESIAN_POINT('Ctrl Pts',(-43.3826786150667,-57.3554536366825,
-40.630001230023));
#259332=CARTESIAN_POINT('Ctrl Pts',(-43.378062215599,-57.3271160344971,
-40.6145607014775));
#259333=CARTESIAN_POINT('Ctrl Pts',(-43.3760891270041,-57.3128275119467,
-40.60693561976));
#259334=CARTESIAN_POINT('Ctrl Pts',(-43.3728422231051,-57.2841093232557,
-40.5919365051523));
#259335=CARTESIAN_POINT('Ctrl Pts',(-43.3715781643254,-57.2697777029377,
-40.5846130830795));
#259336=CARTESIAN_POINT('Ctrl Pts',(-43.3697526802575,-57.2411194243864,
-40.5702888754578));
#259337=CARTESIAN_POINT('Ctrl Pts',(-43.3680717796799,-57.1981642741791,
-40.5492997469169));
#259338=CARTESIAN_POINT('Ctrl Pts',(-43.3700185838812,-57.1410182421193,
-40.5232909177883));
#259339=CARTESIAN_POINT('Ctrl Pts',(-43.3746384661022,-57.0982543712987,
-40.505286899195));
#259340=CARTESIAN_POINT('Ctrl Pts',(-43.3784319419536,-57.0697666559562,
-40.4936247912381));
#259341=CARTESIAN_POINT('Ctrl Pts',(-43.3806866868643,-57.0555278483981,
-40.4879619013523));
#259342=CARTESIAN_POINT('Ctrl Pts',(-43.3859186984709,-57.0270949764048,
-40.476993052777));
#259343=CARTESIAN_POINT('Ctrl Pts',(-43.3889115442249,-57.0128413374093,
-40.4716662621118));
#259344=CARTESIAN_POINT('Ctrl Pts',(-43.3955695423488,-56.984668670318,
-40.4614841416371));
#259345=CARTESIAN_POINT('Ctrl Pts',(-43.4029115329907,-56.9567427536229,
-40.4517375031029));
#259346=CARTESIAN_POINT('Ctrl Pts',(-43.4159439893498,-56.915628788467,
-40.4384286813559));
#259347=CARTESIAN_POINT('Ctrl Pts',(-43.4309850942545,-56.8752725380991,
-40.4264211055283));
#259348=CARTESIAN_POINT('Ctrl Pts',(-43.4480370013178,-56.8356780486645,
-40.4157207514563));
#259349=CARTESIAN_POINT('Ctrl Pts',(-43.4607570961379,-56.8097932355363,
-40.409467745062));
#259350=CARTESIAN_POINT('Ctrl Pts',(-43.4741642201056,-56.7841683331057,
-40.4036630043601));
#259351=CARTESIAN_POINT('Ctrl Pts',(-43.4812071336048,-56.7714928975767,
-40.4009861443346));
#259352=CARTESIAN_POINT('Ctrl Pts',(-43.4960130774609,-56.7463797512019,
-40.3960865778375));
#259353=CARTESIAN_POINT('Ctrl Pts',(-43.5037198572985,-56.7340380787953,
-40.3938827877695));
#259354=CARTESIAN_POINT('Ctrl Pts',(-43.527657505214,-56.6977883833479,
-40.3880276966888));
#259355=CARTESIAN_POINT('Ctrl Pts',(-43.5447483375558,-56.6745564757614,
-40.3851058766842));
#259356=CARTESIAN_POINT('Ctrl Pts',(-43.5811328114983,-56.629979998045,
-40.3812078888591));
#259357=CARTESIAN_POINT('Ctrl Pts',(-43.6004351631962,-56.6086219171049,
-40.3802294367552));
#259358=CARTESIAN_POINT('Ctrl Pts',(-43.6310475296952,-56.578014570072,
-40.3802318237287));
#259359=CARTESIAN_POINT('Ctrl Pts',(-43.6415402048873,-56.5680413281089,
-40.3804790384992));
#259360=CARTESIAN_POINT('Ctrl Pts',(-43.6576911458811,-56.5534539772523,
-40.3812231446347));
#259361=CARTESIAN_POINT('Ctrl Pts',(-43.6631494628181,-56.5486488515781,
-40.3815339900979));
#259362=CARTESIAN_POINT('Ctrl Pts',(-43.6742063152013,-56.5391628964206,
-40.3822815284329));
#259363=CARTESIAN_POINT('Ctrl Pts',(-43.6798092119243,-56.534479009001,
-40.3827188413654));
#259364=CARTESIAN_POINT('Ctrl Pts',(-43.6967370434146,-56.5206915949946,
-40.3842131357726));
#259365=CARTESIAN_POINT('Ctrl Pts',(-43.7196778600618,-56.5029622466235,
-40.386692708542));
#259366=CARTESIAN_POINT('Ctrl Pts',(-43.7670264629127,-56.4700551612604,
-40.3935618621563));
#259367=CARTESIAN_POINT('Ctrl Pts',(-43.8165352419067,-56.4409186299576,
-40.4032471370382));
#259368=CARTESIAN_POINT('Ctrl Pts',(-43.8552784957563,-56.4218759376155,
-40.4126045758866));
#259369=CARTESIAN_POINT('Ctrl Pts',(-43.8814691350842,-56.4098116142502,
-40.4193119877837));
#259370=CARTESIAN_POINT('Ctrl Pts',(-43.8947490665381,-56.4040935548973,
-40.4229014011429));
#259371=CARTESIAN_POINT('Ctrl Pts',(-43.9216608718689,-56.3933018151258,
-40.430550144354));
#259372=CARTESIAN_POINT('Ctrl Pts',(-43.9353412421961,-56.3882139347518,
-40.434625723994));
#259373=CARTESIAN_POINT('Ctrl Pts',(-43.9627318697344,-56.3788058930362,
-40.4431514805252));
#259374=CARTESIAN_POINT('Ctrl Pts',(-43.9765011076412,-56.3744602994329,
-40.4476175822086));
#259375=CARTESIAN_POINT('Ctrl Pts',(-44.0179764085085,-56.3624961934912,
-40.4615970784657));
#259376=CARTESIAN_POINT('Ctrl Pts',(-44.0598195105868,-56.3526585058303,
-40.4767455237411));
#259377=CARTESIAN_POINT('Ctrl Pts',(-44.1163310625808,-56.3437038269143,
-40.4992178608308));
#259378=CARTESIAN_POINT('Ctrl Pts',(-44.1590753545772,-56.3390714325247,
-40.5172068769433));
#259379=CARTESIAN_POINT('Ctrl Pts',(-44.1878153726385,-56.337382052278,
-40.5299596579145));
#259380=CARTESIAN_POINT('Ctrl Pts',(-44.2166756293141,-56.3364007867548,
-40.5430944022758));
#259381=CARTESIAN_POINT('Ctrl Pts',(-44.2311921171808,-56.3362675100036,
-40.5498666179945));
#259382=CARTESIAN_POINT('Ctrl Pts',(-44.2599977007373,-56.3367129587916,
-40.5636298486377));
#259383=CARTESIAN_POINT('Ctrl Pts',(-44.2743541649932,-56.3372884158027,
-40.5706510752088));
#259384=CARTESIAN_POINT('Ctrl Pts',(-44.3029357424357,-56.3391317429585,
-40.5849473061899));
#259385=CARTESIAN_POINT('Ctrl Pts',(-44.3456316213443,-56.3429350642169,
-40.6067818596389));
#259386=CARTESIAN_POINT('Ctrl Pts',(-44.4018650235691,-56.3520939287388,
-40.6374236066311));
#259387=CARTESIAN_POINT('Ctrl Pts',(-44.4574103376146,-56.3653147883305,
-40.6695718678152));
#259388=CARTESIAN_POINT('Ctrl Pts',(-44.4849466005937,-56.3732907222196,
-40.686147922621));
#259389=CARTESIAN_POINT('Ctrl Pts',(-44.512374392093,-56.3819617528141,
-40.7029840503412));
#259390=CARTESIAN_POINT('Ctrl Pts',(-44.5260289861432,-56.3866462995878,
-40.7115304197201));
#259391=CARTESIAN_POINT('Ctrl Pts',(-44.5529609776699,-56.3966203919845,
-40.7287150345567));
#259392=CARTESIAN_POINT('Ctrl Pts',(-44.5662873943758,-56.4019250012471,
-40.737383176176));
#259393=CARTESIAN_POINT('Ctrl Pts',(-44.6058068395674,-56.4187668411382,
-40.7635834132132));
#259394=CARTESIAN_POINT('Ctrl Pts',(-44.6315615859976,-56.4312362585519,
-40.7813233152079));
#259395=CARTESIAN_POINT('Ctrl Pts',(-44.6693071486035,-56.4518014713652,
-40.8083384498991));
#259396=CARTESIAN_POINT('Ctrl Pts',(-44.6817372625133,-56.458965010373,
-40.8174084081892));
#259397=CARTESIAN_POINT('Ctrl Pts',(-44.7063132537473,-56.473929075182,
-40.8356956250034));
#259398=CARTESIAN_POINT('Ctrl Pts',(-44.7183832523531,-56.4816832398284,
-40.8448563495594));
#259399=CARTESIAN_POINT('Ctrl Pts',(-44.7538754102704,-56.505703003501,
-40.8723327540241));
#259400=CARTESIAN_POINT('Ctrl Pts',(-44.7766465418209,-56.5227549736834,
-40.8906872015444));
#259401=CARTESIAN_POINT('Ctrl Pts',(-44.8204030914552,-56.5588699415109,
-40.9274359243417));
#259402=CARTESIAN_POINT('Ctrl Pts',(-44.851893062885,-56.5874690797881,
-40.9550350105826));
#259403=CARTESIAN_POINT('Ctrl Pts',(-44.8813802932551,-56.6183507815631,
-40.982690555711));
#259404=CARTESIAN_POINT('Ctrl Pts',(-44.9005867815582,-56.6394533348067,
-41.0011404791447));
#259405=CARTESIAN_POINT('Ctrl Pts',(-44.9099603095753,-56.6502571213647,
-41.0103678872986));
#259406=CARTESIAN_POINT('Ctrl Pts',(-44.9236872082217,-56.6668706184025,
-41.0242310114538));
#259407=CARTESIAN_POINT('Ctrl Pts',(-44.9282031316495,-56.6724722064122,
-41.0288518918758));
#259408=CARTESIAN_POINT('Ctrl Pts',(-44.9370720489983,-56.6837477093971,
-41.038048314582));
#259409=CARTESIAN_POINT('Ctrl Pts',(-44.9414338933841,-56.6894322363092,
-41.0426327511372));
#259410=CARTESIAN_POINT('Ctrl Pts',(-44.9542884395491,-56.7066066663578,
-41.0563299560217));
#259411=CARTESIAN_POINT('Ctrl Pts',(-44.9625629539304,-56.7182326826763,
-41.0653994431984));
#259412=CARTESIAN_POINT('Ctrl Pts',(-44.9864941991718,-56.7536111473724,
-41.0924067111081));
#259413=CARTESIAN_POINT('Ctrl Pts',(-45.0086645271567,-56.7900134244028,
-41.1190329135161));
#259414=CARTESIAN_POINT('Ctrl Pts',(-45.034704630644,-56.8405768845403,
-41.1537712607408));
#259415=CARTESIAN_POINT('Ctrl Pts',(-45.0465408860903,-56.8665423758261,
-41.1708862092094));
#259416=CARTESIAN_POINT('Ctrl Pts',(-45.0577761134165,-56.8928546179869,
-41.1878727246706));
#259417=CARTESIAN_POINT('Ctrl Pts',(-45.0630901582258,-56.906176087846,
-41.1962967595746));
#259418=CARTESIAN_POINT('Ctrl Pts',(-45.0731156002939,-56.9332061371524,
-41.2130345018643));
#259419=CARTESIAN_POINT('Ctrl Pts',(-45.0777961712447,-56.9468340019015,
-41.2212978165198));
#259420=CARTESIAN_POINT('Ctrl Pts',(-45.0907786540592,-56.9878560258786,
-41.2456540007716));
#259421=CARTESIAN_POINT('Ctrl Pts',(-45.0980724298404,-57.0154910056487,
-41.2613826498774));
#259422=CARTESIAN_POINT('Ctrl Pts',(-45.1099506000897,-57.0712899900431,
-41.2918166667949));
#259423=CARTESIAN_POINT('Ctrl Pts',(-45.1168338059478,-57.11354441615,-41.3138815317038));
#259424=CARTESIAN_POINT('Ctrl Pts',(-45.1206309792415,-57.1564190282566,
-41.3347987762303));
#259425=CARTESIAN_POINT('Ctrl Pts',(-45.1224627479043,-57.1851396939165,
-41.3484832320635));
#259426=CARTESIAN_POINT('Ctrl Pts',(-45.1230291819396,-57.199581674993,
-41.3552011986272));
#259427=CARTESIAN_POINT('Ctrl Pts',(-45.1234439819388,-57.2285619504273,
-41.3683510337761));
#259428=CARTESIAN_POINT('Ctrl Pts',(-45.1232917301137,-57.2429904040975,
-41.3747335054784));
#259429=CARTESIAN_POINT('Ctrl Pts',(-45.122279779691,-57.2717682086368,
-41.3871399525693));
#259430=CARTESIAN_POINT('Ctrl Pts',(-45.1196997436484,-57.3147947598186,
-41.4052018313649));
#259431=CARTESIAN_POINT('Ctrl Pts',(-45.1120557453653,-57.3716084168758,
-41.4271228345082));
#259432=CARTESIAN_POINT('Ctrl Pts',(-45.1031553338884,-57.4137999065974,
-41.4419446800329));
#259433=CARTESIAN_POINT('Ctrl Pts',(-45.09650693546,-57.4418330021969,-41.4514615780937));
#259434=CARTESIAN_POINT('Ctrl Pts',(-45.092823442876,-57.4558081403435,
-41.4560396298995));
#259435=CARTESIAN_POINT('Ctrl Pts',(-45.08473584999,-57.4836385233421,-41.464818484644));
#259436=CARTESIAN_POINT('Ctrl Pts',(-45.0803094818206,-57.4975537933777,
-41.4690360581021));
#259437=CARTESIAN_POINT('Ctrl Pts',(-45.0708158371377,-57.5249803724867,
-41.4770040232021));
#259438=CARTESIAN_POINT('Ctrl Pts',(-45.060662137239,-57.5520858826269,
-41.4845331733926));
#259439=CARTESIAN_POINT('Ctrl Pts',(-45.0434887903859,-57.591755117417,
-41.4945182619959));
#259440=CARTESIAN_POINT('Ctrl Pts',(-45.0243848727922,-57.6304534586566,
-41.5032105668009));
#259441=CARTESIAN_POINT('Ctrl Pts',(-45.0033512023575,-57.6681778817651,
-41.51061115159));
#259442=CARTESIAN_POINT('Ctrl Pts',(-44.9880328234845,-57.692673879575,
-41.5146787869643));
#259443=CARTESIAN_POINT('Ctrl Pts',(-44.9720568870916,-57.7168380825906,
-41.5183074012753));
#259444=CARTESIAN_POINT('Ctrl Pts',(-44.9637457009402,-57.7287466936453,
-41.5199012977462));
#259445=CARTESIAN_POINT('Ctrl Pts',(-44.9464287138105,-57.7522550306847,
-41.5226441863212));
#259446=CARTESIAN_POINT('Ctrl Pts',(-44.9374830238235,-57.7637718882179,
-41.5237830976086));
#259447=CARTESIAN_POINT('Ctrl Pts',(-44.9099214446927,-57.7974515399035,
-41.5264929611258));
#259448=CARTESIAN_POINT('Ctrl Pts',(-44.8905204729439,-57.8188493934961,
-41.5273772161885));
#259449=CARTESIAN_POINT('Ctrl Pts',(-44.8497318000032,-57.8595330722204,
-41.5273307191807));
#259450=CARTESIAN_POINT('Ctrl Pts',(-44.8283374647208,-57.878828810327,
-41.5264014189239));
#259451=CARTESIAN_POINT('Ctrl Pts',(-44.7947479986672,-57.9061820008563,
-41.5236391765087));
#259452=CARTESIAN_POINT('Ctrl Pts',(-44.7832945060713,-57.9150388128137,
-41.5224889540588));
#259453=CARTESIAN_POINT('Ctrl Pts',(-44.7657408175914,-57.9279147771907,
-41.5204166102647));
#259454=CARTESIAN_POINT('Ctrl Pts',(-44.7598217545323,-57.9321421746299,
-41.5196671186517));
#259455=CARTESIAN_POINT('Ctrl Pts',(-44.7478629508254,-57.9404557426351,
-41.5180519716851));
#259456=CARTESIAN_POINT('Ctrl Pts',(-44.7297025277655,-57.9527400844071,
-41.5154481926132));
#259457=CARTESIAN_POINT('Ctrl Pts',(-44.711220794734,-57.9642369190977,
-41.5123523449538));
#259458=CARTESIAN_POINT('Ctrl Pts',(-44.6862770262529,-57.9788987855805,
-41.5077941640223));
#259459=CARTESIAN_POINT('Ctrl Pts',(-44.6484202704456,-57.9998814948776,
-41.5003121274858));
#259460=CARTESIAN_POINT('Ctrl Pts',(-44.5962108390282,-58.0238874022289,
-41.4877980263462));
#259461=CARTESIAN_POINT('Ctrl Pts',(-44.5557649369164,-58.0389385823793,
-41.4765186283493));
#259462=CARTESIAN_POINT('Ctrl Pts',(-44.5285120653069,-58.048310487242,
-41.4685735203231));
#259463=CARTESIAN_POINT('Ctrl Pts',(-44.5147341086114,-58.0526671867402,
-41.4643859028639));
#259464=CARTESIAN_POINT('Ctrl Pts',(-44.4869140318333,-58.0607029371288,
-41.4555883503401));
#259465=CARTESIAN_POINT('Ctrl Pts',(-44.4728027150897,-58.0643973546439,
-41.4509544537452));
#259466=CARTESIAN_POINT('Ctrl Pts',(-44.4304531283686,-58.0743536715507,
-41.4365378845966));
#259467=CARTESIAN_POINT('Ctrl Pts',(-44.3879697631396,-58.0821103913619,
-41.4210702443308));
#259468=CARTESIAN_POINT('Ctrl Pts',(-44.3452880889881,-58.0866896268435,
-41.4040725286766));
#259469=CARTESIAN_POINT('Ctrl Pts',(-44.3025416355467,-58.090217180745,
-41.3865671155567));
#259470=CARTESIAN_POINT('Ctrl Pts',(-44.2739489581488,-58.0911687787978,
-41.3742170239002));
#259471=CARTESIAN_POINT('Ctrl Pts',(-44.2309555122234,-58.090491506171,
-41.3546803180427));
#259472=CARTESIAN_POINT('Ctrl Pts',(-44.2165895018292,-58.0899123697243,
-41.347990487553));
#259473=CARTESIAN_POINT('Ctrl Pts',(-44.1950278537333,-58.0885113544661,
-41.337705180963));
#259474=CARTESIAN_POINT('Ctrl Pts',(-44.1878319550126,-58.0879547296283,
-41.3342316293533));
#259475=CARTESIAN_POINT('Ctrl Pts',(-44.1734279164018,-58.0866616594573,
-41.3271961709002));
#259476=CARTESIAN_POINT('Ctrl Pts',(-44.1662260389348,-58.0859253983809,
-41.3236371482021));
#259477=CARTESIAN_POINT('Ctrl Pts',(-44.130389101081,-58.0818150523559,
-41.3057210105631));
#259478=CARTESIAN_POINT('Ctrl Pts',(-44.073848260417,-58.0724828543971,
-41.2761395013722));
#259479=CARTESIAN_POINT('Ctrl Pts',(-44.0188545174212,-58.0578491440998,
-41.2447838757269));
#259480=CARTESIAN_POINT('Ctrl Pts',(-43.9646246641704,-58.0405931079736,
-41.2125419608827));
#259481=CARTESIAN_POINT('Ctrl Pts',(-43.9378880325505,-58.0306505669816,
-41.1959746665064));
#259482=CARTESIAN_POINT('Ctrl Pts',(-43.9049634769563,-58.0165631445999,
-41.174705886574));
#259483=CARTESIAN_POINT('Ctrl Pts',(-43.898399460067,-58.0136596367661,
-41.1704209658528));
#259484=CARTESIAN_POINT('Ctrl Pts',(-43.8853286348063,-58.0076886655405,
-41.1617993561325));
#259485=CARTESIAN_POINT('Ctrl Pts',(-43.8788088737381,-58.0046144513738,
-41.157453730181));
#259486=CARTESIAN_POINT('Ctrl Pts',(-43.8593967360427,-57.9951717320096,
-41.1443784829743));
#259487=CARTESIAN_POINT('Ctrl Pts',(-43.8466719188398,-57.9885954718361,
-41.1356253645631));
#259488=CARTESIAN_POINT('Ctrl Pts',(-43.8341420587998,-57.9817357678076,
-41.1268248734572));
#259489=CARTESIAN_POINT('Ctrl Pts',(-46.1726021405987,-56.3668761797815,
-39.5898551158851));
#259490=CARTESIAN_POINT('Ctrl Pts',(-46.2069057047429,-56.4183864095348,
-39.607121781657));
#259491=CARTESIAN_POINT('Ctrl Pts',(-46.2553082908951,-56.4989321412679,
-39.6330245761036));
#259492=CARTESIAN_POINT('Ctrl Pts',(-46.3126017708591,-56.6115274351852,
-39.6670695777419));
#259493=CARTESIAN_POINT('Ctrl Pts',(-46.3391231723103,-56.6705508392544,
-39.6841845262104));
#259494=CARTESIAN_POINT('Ctrl Pts',(-46.3642693448436,-56.7303750220794,
-39.7011710416717));
#259495=CARTESIAN_POINT('Ctrl Pts',(-46.3761479944029,-56.76066924716,-39.7095950765756));
#259496=CARTESIAN_POINT('Ctrl Pts',(-46.3985257027381,-56.8221504582685,
-39.7263328188654));
#259497=CARTESIAN_POINT('Ctrl Pts',(-46.4089559133708,-56.8531538688126,
-39.73459613352));
#259498=CARTESIAN_POINT('Ctrl Pts',(-46.437831026164,-56.9464970853635,
-39.7589523177745));
#259499=CARTESIAN_POINT('Ctrl Pts',(-46.4539750647129,-57.0094025506593,
-39.7746809668783));
#259500=CARTESIAN_POINT('Ctrl Pts',(-46.4800815194185,-57.1364635805498,
-39.8051149837962));
#259501=CARTESIAN_POINT('Ctrl Pts',(-46.4950400693282,-57.232716021489,
-39.8271798487049));
#259502=CARTESIAN_POINT('Ctrl Pts',(-46.5029571390459,-57.3304319805551,
-39.8480970932315));
#259503=CARTESIAN_POINT('Ctrl Pts',(-46.5066387211099,-57.3959008325223,
-39.8617815490646));
#259504=CARTESIAN_POINT('Ctrl Pts',(-46.5076819483115,-57.4288270025733,
-39.8684995156283));
#259505=CARTESIAN_POINT('Ctrl Pts',(-46.508130707335,-57.4949103365212,
-39.8816493507771));
#259506=CARTESIAN_POINT('Ctrl Pts',(-46.5075367124945,-57.527817016895,
-39.8880318224796));
#259507=CARTESIAN_POINT('Ctrl Pts',(-46.504738178928,-57.5934611321397,
-39.9004382695704));
#259508=CARTESIAN_POINT('Ctrl Pts',(-46.4981227877063,-57.6916244184968,
-39.9185001483662));
#259509=CARTESIAN_POINT('Ctrl Pts',(-46.4797328401766,-57.8213090440304,
-39.940421151509));
#259510=CARTESIAN_POINT('Ctrl Pts',(-46.4587298084939,-57.9176672625727,
-39.9552429970341));
#259511=CARTESIAN_POINT('Ctrl Pts',(-46.4431004971084,-57.9817016478038,
-39.9647598950948));
#259512=CARTESIAN_POINT('Ctrl Pts',(-46.4344677710292,-58.0136300484471,
-39.9693379469006));
#259513=CARTESIAN_POINT('Ctrl Pts',(-46.4155621210723,-58.0772247635304,
-39.9781168016451));
#259514=CARTESIAN_POINT('Ctrl Pts',(-46.4052374261782,-58.109028316384,
-39.9823343751034));
#259515=CARTESIAN_POINT('Ctrl Pts',(-46.3831342217529,-58.1717242862158,
-39.9903023402032));
#259516=CARTESIAN_POINT('Ctrl Pts',(-46.3595321549874,-58.2336984575206,
-39.9978314903936));
#259517=CARTESIAN_POINT('Ctrl Pts',(-46.3244338236407,-58.3136871658631,
-40.0066338415421));
#259518=CARTESIAN_POINT('Ctrl Pts',(-46.3006305954557,-58.3624460386648,
-40.0115250278133));
#259519=CARTESIAN_POINT('Ctrl Pts',(-46.2909969450817,-58.3814064047113,
-40.0133526947335));
#259520=CARTESIAN_POINT('Ctrl Pts',(-46.2909969422729,-58.3814064027011,
-40.013352709603));
#259521=CARTESIAN_POINT('Ctrl Pts',(-46.3693097501125,-58.1875098833917,
-40.0137875322504));
#259522=CARTESIAN_POINT('Ctrl Pts',(-46.411278999678,-57.9809289977677,
-40.0118819906088));
#259523=CARTESIAN_POINT('Ctrl Pts',(-46.4191068837893,-57.5991845865335,
-40.0050928659256));
#259524=CARTESIAN_POINT('Ctrl Pts',(-46.3968688023029,-57.4268964497847,
-40.0008179121686));
#259525=CARTESIAN_POINT('Ctrl Pts',(-46.2946092803027,-57.0638316879311,
-39.9897515821211));
#259526=CARTESIAN_POINT('Ctrl Pts',(-46.2056470788626,-56.8783069534362,
-39.9827369701668));
#259527=CARTESIAN_POINT('Ctrl Pts',(-45.9855349754196,-56.5673096976623,
-39.9689716167871));
#259528=CARTESIAN_POINT('Ctrl Pts',(-45.8629979265771,-56.4391204389221,
-39.9626060055202));
#259529=CARTESIAN_POINT('Ctrl Pts',(-45.7222549758842,-56.3308214393021,
-39.9581073668549));
#259530=CARTESIAN_POINT('Ctrl Pts',(-45.3258935545055,-56.0209136569754,
-39.8341888326825));
#259531=CARTESIAN_POINT('Ctrl Pts',(-45.4764270023181,-56.0526141472619,
-39.797283341326));
#259532=CARTESIAN_POINT('Ctrl Pts',(-45.6236924541279,-56.098325931019,
-39.7577446198746));
#259533=CARTESIAN_POINT('Ctrl Pts',(-45.9074046606253,-56.214732273663,
-39.6755637187821));
#259534=CARTESIAN_POINT('Ctrl Pts',(-46.0434656100389,-56.2851743761681,
-39.6330616925565));
#259535=CARTESIAN_POINT('Ctrl Pts',(-46.1726021442766,-56.3668761803699,
-39.5898551239125));
#259536=CARTESIAN_POINT('Ctrl Pts',(-43.4805771074156,-59.5712767529309,
-39.2399080357013));
#259537=CARTESIAN_POINT('Ctrl Pts',(-43.4150727209207,-59.5358440364426,
-39.2223070534893));
#259538=CARTESIAN_POINT('Ctrl Pts',(-43.2883193276586,-59.4590682572254,
-39.1867578392588));
#259539=CARTESIAN_POINT('Ctrl Pts',(-43.1106712693135,-59.32658002426,-39.1324031814995));
#259540=CARTESIAN_POINT('Ctrl Pts',(-43.0005921597408,-59.2266373021163,
-39.0954660506179));
#259541=CARTESIAN_POINT('Ctrl Pts',(-42.8948534568781,-59.1207134074407,
-39.0581733199915));
#259542=CARTESIAN_POINT('Ctrl Pts',(-42.7951360401793,-59.0104958554849,
-39.0211184761739));
#259543=CARTESIAN_POINT('Ctrl Pts',(-42.6850011896347,-58.8622904152127,
-38.9753582681256));
#259544=CARTESIAN_POINT('Ctrl Pts',(-42.6055727997797,-58.7375004045667,
-38.939089851323));
#259545=CARTESIAN_POINT('Ctrl Pts',(-42.5503788594446,-58.6407591922129,
-38.9120596161462));
#259546=CARTESIAN_POINT('Ctrl Pts',(-42.5165536369311,-58.5741539171446,
-38.8941613358138));
#259547=CARTESIAN_POINT('Ctrl Pts',(-42.4842288567228,-58.5064298632496,
-38.8763157156907));
#259548=CARTESIAN_POINT('Ctrl Pts',(-42.4689425396028,-58.4722695523732,
-38.8674882509199));
#259549=CARTESIAN_POINT('Ctrl Pts',(-42.4257123024776,-58.3690064948315,
-38.8413136266604));
#259550=CARTESIAN_POINT('Ctrl Pts',(-42.3750272156063,-58.229152189777,
-38.8072100415055));
#259551=CARTESIAN_POINT('Ctrl Pts',(-42.3380647902547,-58.0850119200902,
-38.7746901633276));
#259552=CARTESIAN_POINT('Ctrl Pts',(-42.3155659796374,-57.9752818499468,
-38.7509105250088));
#259553=CARTESIAN_POINT('Ctrl Pts',(-42.3089374211558,-57.9384266221928,
-38.7430843922672));
#259554=CARTESIAN_POINT('Ctrl Pts',(-42.297458012674,-57.864178756387,-38.7276438637217));
#259555=CARTESIAN_POINT('Ctrl Pts',(-42.292601515188,-57.8267325312259,
-38.720018782004));
#259556=CARTESIAN_POINT('Ctrl Pts',(-42.2847289916893,-57.7514526301959,
-38.7050196673963));
#259557=CARTESIAN_POINT('Ctrl Pts',(-42.2817363521424,-57.7138759968928,
-38.6976962453237));
#259558=CARTESIAN_POINT('Ctrl Pts',(-42.277596992864,-57.6387184974263,
-38.6833720377019));
#259559=CARTESIAN_POINT('Ctrl Pts',(-42.2741651307842,-57.5260409596698,
-38.6623829091612));
#259560=CARTESIAN_POINT('Ctrl Pts',(-42.2805893100654,-57.3760354719141,
-38.6363740800325));
#259561=CARTESIAN_POINT('Ctrl Pts',(-42.2937061680812,-57.2637038035873,
-38.618370061439));
#259562=CARTESIAN_POINT('Ctrl Pts',(-42.3043247017591,-57.1888547452426,
-38.6067079534822));
#259563=CARTESIAN_POINT('Ctrl Pts',(-42.3105743117123,-57.1514345461221,
-38.6010450635964));
#259564=CARTESIAN_POINT('Ctrl Pts',(-42.3249704170347,-57.0766935209607,
-38.590076215021));
#259565=CARTESIAN_POINT('Ctrl Pts',(-42.3331592025312,-57.0392159768686,
-38.5847494243559));
#259566=CARTESIAN_POINT('Ctrl Pts',(-42.3512949844302,-56.9651221381903,
-38.5745673038812));
#259567=CARTESIAN_POINT('Ctrl Pts',(-42.3712216906218,-56.8916587034686,
-38.564820665347));
#259568=CARTESIAN_POINT('Ctrl Pts',(-42.4063979707918,-56.7834465224234,
-38.5515118436));
#259569=CARTESIAN_POINT('Ctrl Pts',(-42.4468320479729,-56.6771725078319,
-38.5395042677724));
#259570=CARTESIAN_POINT('Ctrl Pts',(-42.4925290654744,-56.5728473165674,
-38.5288039137004));
#259571=CARTESIAN_POINT('Ctrl Pts',(-42.5265325119253,-56.5046058456765,
-38.5225509073062));
#259572=CARTESIAN_POINT('Ctrl Pts',(-42.5623338475306,-56.4370293947697,
-38.5167461666044));
#259573=CARTESIAN_POINT('Ctrl Pts',(-42.5811223641794,-56.4035923099625,
-38.5140693065785));
#259574=CARTESIAN_POINT('Ctrl Pts',(-42.620584523009,-56.3373241998654,
-38.5091697400817));
#259575=CARTESIAN_POINT('Ctrl Pts',(-42.6411082254821,-56.3047465904101,
-38.5069659500128));
#259576=CARTESIAN_POINT('Ctrl Pts',(-42.7048067991197,-56.2090283357163,
-38.501110858935));
#259577=CARTESIAN_POINT('Ctrl Pts',(-42.7502234543428,-56.1476408662828,
-38.4981890389281));
#259578=CARTESIAN_POINT('Ctrl Pts',(-42.8467942323831,-56.0297655581676,
-38.4942910511033));
#259579=CARTESIAN_POINT('Ctrl Pts',(-42.8979715413934,-55.9732420482176,
-38.4933125989996));
#259580=CARTESIAN_POINT('Ctrl Pts',(-42.9790570553347,-55.8921695883033,
-38.4933149859729));
#259581=CARTESIAN_POINT('Ctrl Pts',(-43.0068374106561,-55.8657400908868,
-38.4935622007431));
#259582=CARTESIAN_POINT('Ctrl Pts',(-43.0495800649421,-55.8270637749536,
-38.4943063068789));
#259583=CARTESIAN_POINT('Ctrl Pts',(-43.0640222060113,-55.8143203511958,
-38.494617152342));
#259584=CARTESIAN_POINT('Ctrl Pts',(-43.0932714774893,-55.7891564261061,
-38.4953646906773));
#259585=CARTESIAN_POINT('Ctrl Pts',(-43.1080901283632,-55.7767277938553,
-38.4958020036096));
#259586=CARTESIAN_POINT('Ctrl Pts',(-43.1528523310046,-55.7401327167866,
-38.4972962980169));
#259587=CARTESIAN_POINT('Ctrl Pts',(-43.2134913856688,-55.6930468850421,
-38.4997758707861));
#259588=CARTESIAN_POINT('Ctrl Pts',(-43.3385569247743,-55.6055389451161,
-38.5066450244003));
#259589=CARTESIAN_POINT('Ctrl Pts',(-43.4691986576013,-55.5278792007279,
-38.5163302992824));
#259590=CARTESIAN_POINT('Ctrl Pts',(-43.5713395927684,-55.4769743237494,
-38.5256877381308));
#259591=CARTESIAN_POINT('Ctrl Pts',(-43.6403672861995,-55.4446857735354,
-38.5323951500278));
#259592=CARTESIAN_POINT('Ctrl Pts',(-43.6753577685123,-55.4293620157832,
-38.5359845633874));
#259593=CARTESIAN_POINT('Ctrl Pts',(-43.7462462065788,-55.4003985583156,
-38.5436333065981));
#259594=CARTESIAN_POINT('Ctrl Pts',(-43.7822717759725,-55.3867204456352,
-38.5477088862383));
#259595=CARTESIAN_POINT('Ctrl Pts',(-43.8543821738219,-55.3613797848081,
-38.5562346427694));
#259596=CARTESIAN_POINT('Ctrl Pts',(-43.890622407919,-55.349649082917,-38.5607007444526));
#259597=CARTESIAN_POINT('Ctrl Pts',(-43.9997560709039,-55.3172704656441,
-38.5746802407103));
#259598=CARTESIAN_POINT('Ctrl Pts',(-44.1098017310836,-55.290468361793,
-38.5898286859852));
#259599=CARTESIAN_POINT('Ctrl Pts',(-44.2583166685835,-55.2656490138239,
-38.612301023075));
#259600=CARTESIAN_POINT('Ctrl Pts',(-44.3705972700495,-55.2524997368729,
-38.6302900391873));
#259601=CARTESIAN_POINT('Ctrl Pts',(-44.446056048267,-55.2474029004138,
-38.6430428201589));
#259602=CARTESIAN_POINT('Ctrl Pts',(-44.5218128020516,-55.2441636366351,
-38.65617756452));
#259603=CARTESIAN_POINT('Ctrl Pts',(-44.5599089424743,-55.2434808562086,
-38.6629497802385));
#259604=CARTESIAN_POINT('Ctrl Pts',(-44.6354869543582,-55.2439911084578,
-38.6767130108817));
#259605=CARTESIAN_POINT('Ctrl Pts',(-44.6731456892459,-55.2451740103824,
-38.6837342374529));
#259606=CARTESIAN_POINT('Ctrl Pts',(-44.7481014788608,-55.2493620066237,
-38.6980304684339));
#259607=CARTESIAN_POINT('Ctrl Pts',(-44.860046548974,-55.2583760573225,
-38.7198650218829));
#259608=CARTESIAN_POINT('Ctrl Pts',(-45.0073845433675,-55.2811507310277,
-38.7505067688753));
#259609=CARTESIAN_POINT('Ctrl Pts',(-45.1528189888476,-55.3146135839333,
-38.7826550300594));
#259610=CARTESIAN_POINT('Ctrl Pts',(-45.2248832056965,-55.3349380951144,
-38.7992310848652));
#259611=CARTESIAN_POINT('Ctrl Pts',(-45.2966462681613,-55.3570913336823,
-38.8160672125853));
#259612=CARTESIAN_POINT('Ctrl Pts',(-45.3323638946335,-55.3690863290504,
-38.8246135819642));
#259613=CARTESIAN_POINT('Ctrl Pts',(-45.4027951436545,-55.3946744461232,
-38.841798196801));
#259614=CARTESIAN_POINT('Ctrl Pts',(-45.4376370321487,-55.4083060218429,
-38.85046633842));
#259615=CARTESIAN_POINT('Ctrl Pts',(-45.5409345111852,-55.4516493275196,
-38.8766665754573));
#259616=CARTESIAN_POINT('Ctrl Pts',(-45.6082182891413,-55.4838201174091,
-38.8944064774514));
#259617=CARTESIAN_POINT('Ctrl Pts',(-45.7067749877369,-55.5369855856676,
-38.9214216121435));
#259618=CARTESIAN_POINT('Ctrl Pts',(-45.7392219877795,-55.5555212114618,
-38.9304915704334));
#259619=CARTESIAN_POINT('Ctrl Pts',(-45.8033556832395,-55.5942722159849,
-38.9487787872477));
#259620=CARTESIAN_POINT('Ctrl Pts',(-45.8348443691401,-55.6143675312756,
-38.9579395118015));
#259621=CARTESIAN_POINT('Ctrl Pts',(-45.9274099842789,-55.6766589025306,
-38.9854159162723));
#259622=CARTESIAN_POINT('Ctrl Pts',(-45.9867610865919,-55.7209353156014,
-39.0037703637879));
#259623=CARTESIAN_POINT('Ctrl Pts',(-46.1007337830098,-55.8148102393793,
-39.0405190865864));
#259624=CARTESIAN_POINT('Ctrl Pts',(-46.1826971388658,-55.889219933262,
-39.0681181728269));
#259625=CARTESIAN_POINT('Ctrl Pts',(-46.259356574729,-55.9696687352924,
-39.0957737179551));
#259626=CARTESIAN_POINT('Ctrl Pts',(-46.309266807939,-56.024663053365,-39.1142236413887));
#259627=CARTESIAN_POINT('Ctrl Pts',(-46.3336138177017,-56.0528284109483,
-39.1234510495426));
#259628=CARTESIAN_POINT('Ctrl Pts',(-46.3692509284248,-56.0961546965833,
-39.1373141736981));
#259629=CARTESIAN_POINT('Ctrl Pts',(-46.3809719555493,-56.1107655250657,
-39.14193505412));
#259630=CARTESIAN_POINT('Ctrl Pts',(-46.4039850968433,-56.1401806715041,
-39.1511314768264));
#259631=CARTESIAN_POINT('Ctrl Pts',(-46.4153001903629,-56.1550126624776,
-39.1557159133813));
#259632=CARTESIAN_POINT('Ctrl Pts',(-46.4486370096885,-56.1998310060263,
-39.1694131182659));
#259633=CARTESIAN_POINT('Ctrl Pts',(-46.4700835091466,-56.2301795317326,
-39.1784826054425));
#259634=CARTESIAN_POINT('Ctrl Pts',(-46.532071913686,-56.3225583984772,
-39.2054898733524));
#259635=CARTESIAN_POINT('Ctrl Pts',(-46.5894197348374,-56.4176636744323,
-39.23211607576));
#259636=CARTESIAN_POINT('Ctrl Pts',(-46.6566074362748,-56.5498680842415,
-39.2668544229849));
#259637=CARTESIAN_POINT('Ctrl Pts',(-46.6870820302515,-56.617790568625,
-39.2839693714534));
#259638=CARTESIAN_POINT('Ctrl Pts',(-46.7159729830272,-56.6866360545619,
-39.3009558869148));
#259639=CARTESIAN_POINT('Ctrl Pts',(-46.7296188023799,-56.7214992889704,
-39.3093799218186));
#259640=CARTESIAN_POINT('Ctrl Pts',(-46.7553216997643,-56.7922546384013,
-39.3261176641085));
#259641=CARTESIAN_POINT('Ctrl Pts',(-46.7672996943011,-56.8279354881579,
-39.3343809787628));
#259642=CARTESIAN_POINT('Ctrl Pts',(-46.8004530502947,-56.9353633959568,
-39.358737163018));
#259643=CARTESIAN_POINT('Ctrl Pts',(-46.8189795501832,-57.0077635587999,
-39.3744658121213));
#259644=CARTESIAN_POINT('Ctrl Pts',(-46.848916211803,-57.1540080946302,
-39.4048998290393));
#259645=CARTESIAN_POINT('Ctrl Pts',(-46.866048617508,-57.2647966217996,
-39.4269646939479));
#259646=CARTESIAN_POINT('Ctrl Pts',(-46.875074749658,-57.3772756893033,
-39.4478819384746));
#259647=CARTESIAN_POINT('Ctrl Pts',(-46.8792542953452,-57.4526370309597,
-39.4615663943076));
#259648=CARTESIAN_POINT('Ctrl Pts',(-46.8804258736835,-57.4905390832845,
-39.4682843608713));
#259649=CARTESIAN_POINT('Ctrl Pts',(-46.8808837743635,-57.566610437341,
-39.4814341960201));
#259650=CARTESIAN_POINT('Ctrl Pts',(-46.8801708637706,-57.604491394965,
-39.4878166677226));
#259651=CARTESIAN_POINT('Ctrl Pts',(-46.8768913879562,-57.6800597985945,
-39.5002231148134));
#259652=CARTESIAN_POINT('Ctrl Pts',(-46.8691896925243,-57.7930657109158,
-39.5182849936093));
#259653=CARTESIAN_POINT('Ctrl Pts',(-46.8479069711518,-57.9423669591112,
-39.540205996752));
#259654=CARTESIAN_POINT('Ctrl Pts',(-46.8236459543104,-58.053306681129,
-39.5550278422771));
#259655=CARTESIAN_POINT('Ctrl Pts',(-46.8055990109883,-58.1270324939452,
-39.5645447403379));
#259656=CARTESIAN_POINT('Ctrl Pts',(-46.7956339676918,-58.1637938532181,
-39.5691227921436));
#259657=CARTESIAN_POINT('Ctrl Pts',(-46.7738161327052,-58.2370162077019,
-39.5779016468881));
#259658=CARTESIAN_POINT('Ctrl Pts',(-46.7619036278491,-58.2736352268715,
-39.5821192203466));
#259659=CARTESIAN_POINT('Ctrl Pts',(-46.7364059718256,-58.3458255995332,
-39.5900871854462));
#259660=CARTESIAN_POINT('Ctrl Pts',(-46.7091836493705,-58.4171862986019,
-39.5976163356366));
#259661=CARTESIAN_POINT('Ctrl Pts',(-46.663274408039,-58.5216699086648,
-39.6076014242402));
#259662=CARTESIAN_POINT('Ctrl Pts',(-46.6123207377325,-58.6236436013082,
-39.616293729045));
#259663=CARTESIAN_POINT('Ctrl Pts',(-46.5563244858032,-58.7230996041114,
-39.6236943138341));
#259664=CARTESIAN_POINT('Ctrl Pts',(-46.515607032986,-58.7877140896312,
-39.6277619492082));
#259665=CARTESIAN_POINT('Ctrl Pts',(-46.4731710833873,-58.8514710047945,
-39.6313905635194));
#259666=CARTESIAN_POINT('Ctrl Pts',(-46.4511086137465,-58.8829006319494,
-39.6329844599904));
#259667=CARTESIAN_POINT('Ctrl Pts',(-46.4051673201274,-58.9449633016888,
-39.6357273485653));
#259668=CARTESIAN_POINT('Ctrl Pts',(-46.381447994276,-58.975377588932,-39.6368662598532));
#259669=CARTESIAN_POINT('Ctrl Pts',(-46.3084068909562,-59.0643493136614,
-39.6395761233691));
#259670=CARTESIAN_POINT('Ctrl Pts',(-46.2570407846102,-59.1209150453974,
-39.6404603784325));
#259671=CARTESIAN_POINT('Ctrl Pts',(-46.1491379755941,-59.228544463199,
-39.6404138814247));
#259672=CARTESIAN_POINT('Ctrl Pts',(-46.0925836555155,-59.2796343044913,
-39.6394845811684));
#259673=CARTESIAN_POINT('Ctrl Pts',(-46.0038529437629,-59.3521266125547,
-39.6367223387528));
#259674=CARTESIAN_POINT('Ctrl Pts',(-45.9736068078661,-59.3756113554055,
-39.6355721163029));
#259675=CARTESIAN_POINT('Ctrl Pts',(-45.9272656961273,-59.4097723546528,
-39.6334997725088));
#259676=CARTESIAN_POINT('Ctrl Pts',(-45.9116419215573,-59.4209912820171,
-39.6327502808957));
#259677=CARTESIAN_POINT('Ctrl Pts',(-45.8800804794677,-59.4430610802669,
-39.6311351339295));
#259678=CARTESIAN_POINT('Ctrl Pts',(-45.8321587971618,-59.4756823489919,
-39.628531354857));
#259679=CARTESIAN_POINT('Ctrl Pts',(-45.7834097108732,-59.5062438963941,
-39.6254355071979));
#259680=CARTESIAN_POINT('Ctrl Pts',(-45.717633106262,-59.5452481912826,
-39.6208773262667));
#259681=CARTESIAN_POINT('Ctrl Pts',(-45.6178307490054,-59.601113548897,
-39.6133952897297));
#259682=CARTESIAN_POINT('Ctrl Pts',(-45.4802897643185,-59.6652183443042,
-39.6008811885904));
#259683=CARTESIAN_POINT('Ctrl Pts',(-45.3738098009101,-59.7055766782111,
-39.5896017905935));
#259684=CARTESIAN_POINT('Ctrl Pts',(-45.3020778813705,-59.7307512119865,
-39.5816566825671));
#259685=CARTESIAN_POINT('Ctrl Pts',(-45.2658207311094,-59.7424779859237,
-39.5774690651077));
#259686=CARTESIAN_POINT('Ctrl Pts',(-45.1926264675053,-59.7641596016776,
-39.5686715125846));
#259687=CARTESIAN_POINT('Ctrl Pts',(-45.1555073907618,-59.7741562512684,
-39.5640376159893));
#259688=CARTESIAN_POINT('Ctrl Pts',(-45.0441315765335,-59.8011904590316,
-39.5496210468413));
#259689=CARTESIAN_POINT('Ctrl Pts',(-44.9324484012679,-59.8224577850013,
-39.5341534065747));
#259690=CARTESIAN_POINT('Ctrl Pts',(-44.8203079610257,-59.8353953605365,
-39.5171556909205));
#259691=CARTESIAN_POINT('Ctrl Pts',(-44.7080184564226,-59.8455760612675,
-39.4996502778008));
#259692=CARTESIAN_POINT('Ctrl Pts',(-44.6329372249224,-59.8486931621852,
-39.4873001861445));
#259693=CARTESIAN_POINT('Ctrl Pts',(-44.5200834441659,-59.8478515133141,
-39.4677634802869));
#259694=CARTESIAN_POINT('Ctrl Pts',(-44.4823810871712,-59.8466449718289,
-39.4610736497974));
#259695=CARTESIAN_POINT('Ctrl Pts',(-44.4258051079382,-59.8434394706745,
-39.4507883432074));
#259696=CARTESIAN_POINT('Ctrl Pts',(-44.4069254589855,-59.8421361346926,
-39.4473147915973));
#259697=CARTESIAN_POINT('Ctrl Pts',(-44.3691376542581,-59.8390581625153,
-39.4402793331445));
#259698=CARTESIAN_POINT('Ctrl Pts',(-44.3502459350849,-59.8372838734483,
-39.4367203104461));
#259699=CARTESIAN_POINT('Ctrl Pts',(-44.2562487381671,-59.8272835659938,
-39.4188041728073));
#259700=CARTESIAN_POINT('Ctrl Pts',(-44.1080045765469,-59.8040393501646,
-39.3892226636159));
#259701=CARTESIAN_POINT('Ctrl Pts',(-43.9639303529155,-59.7668593120831,
-39.3578670379715));
#259702=CARTESIAN_POINT('Ctrl Pts',(-43.8219159040518,-59.7227861654643,
-39.3256251231267));
#259703=CARTESIAN_POINT('Ctrl Pts',(-43.7519290534068,-59.6972943066161,
-39.3090578287531));
#259704=CARTESIAN_POINT('Ctrl Pts',(-43.665783177736,-59.6610675807531,
-39.2877890488175));
#259705=CARTESIAN_POINT('Ctrl Pts',(-43.6486106666635,-59.653596197985,
-39.2835041280971));
#259706=CARTESIAN_POINT('Ctrl Pts',(-43.6144193015916,-59.6382222359849,
-39.2748825183767));
#259707=CARTESIAN_POINT('Ctrl Pts',(-43.597366582891,-59.6303022352814,
-39.2705368924251));
#259708=CARTESIAN_POINT('Ctrl Pts',(-43.5465994182959,-59.605961903298,
-39.2574616452183));
#259709=CARTESIAN_POINT('Ctrl Pts',(-43.513329300663,-59.588993111175,-39.2487085268073));
#259710=CARTESIAN_POINT('Ctrl Pts',(-43.4805771074156,-59.5712767529309,
-39.2399080357013));
#259711=CARTESIAN_POINT('Ctrl Pts',(-43.8341420587998,-57.9817357678076,
-41.1268248734572));
#259712=CARTESIAN_POINT('Ctrl Pts',(-43.8090823387197,-57.9680163597508,
-41.1092238912453));
#259713=CARTESIAN_POINT('Ctrl Pts',(-43.7605654269547,-57.9383371077444,
-41.0736746770147));
#259714=CARTESIAN_POINT('Ctrl Pts',(-43.6924895655639,-57.8872515755908,
-41.019320019256));
#259715=CARTESIAN_POINT('Ctrl Pts',(-43.6502497090231,-57.8487916199066,
-40.9823828883729));
#259716=CARTESIAN_POINT('Ctrl Pts',(-43.6096433745973,-57.8080652293815,
-40.945090157748));
#259717=CARTESIAN_POINT('Ctrl Pts',(-43.5713160673933,-57.7657212262301,
-40.9080353139296));
#259718=CARTESIAN_POINT('Ctrl Pts',(-43.5288984657655,-57.7088609123343,
-40.8622751058818));
#259719=CARTESIAN_POINT('Ctrl Pts',(-43.4982484100127,-57.6610280687967,
-40.826006689079));
#259720=CARTESIAN_POINT('Ctrl Pts',(-43.4769169762936,-57.6239677344727,
-40.798976453902));
#259721=CARTESIAN_POINT('Ctrl Pts',(-43.4638199758968,-57.5984660781933,
-40.7810781735695));
#259722=CARTESIAN_POINT('Ctrl Pts',(-43.4512904535732,-57.5725430453748,
-40.7632325534464));
#259723=CARTESIAN_POINT('Ctrl Pts',(-43.4453582046716,-57.5594707895743,
-40.7544050886758));
#259724=CARTESIAN_POINT('Ctrl Pts',(-43.4285595200757,-57.5199648485381,
-40.7282304644163));
#259725=CARTESIAN_POINT('Ctrl Pts',(-43.4088016745783,-57.4664867157472,
-40.6941268792613));
#259726=CARTESIAN_POINT('Ctrl Pts',(-43.3942530508608,-57.4114223976644,
-40.6616070010832));
#259727=CARTESIAN_POINT('Ctrl Pts',(-43.3853242538269,-57.3695231591805,
-40.6378273627645));
#259728=CARTESIAN_POINT('Ctrl Pts',(-43.3826786150667,-57.3554536366825,
-40.630001230023));
#259729=CARTESIAN_POINT('Ctrl Pts',(-43.378062215599,-57.3271160344971,
-40.6145607014775));
#259730=CARTESIAN_POINT('Ctrl Pts',(-43.3760891270041,-57.3128275119467,
-40.60693561976));
#259731=CARTESIAN_POINT('Ctrl Pts',(-43.3728422231051,-57.2841093232557,
-40.5919365051523));
#259732=CARTESIAN_POINT('Ctrl Pts',(-43.3715781643254,-57.2697777029377,
-40.5846130830795));
#259733=CARTESIAN_POINT('Ctrl Pts',(-43.3697526802575,-57.2411194243864,
-40.5702888754578));
#259734=CARTESIAN_POINT('Ctrl Pts',(-43.3680717796799,-57.1981642741791,
-40.5492997469169));
#259735=CARTESIAN_POINT('Ctrl Pts',(-43.3700185838812,-57.1410182421193,
-40.5232909177883));
#259736=CARTESIAN_POINT('Ctrl Pts',(-43.3746384661022,-57.0982543712987,
-40.505286899195));
#259737=CARTESIAN_POINT('Ctrl Pts',(-43.3784319419536,-57.0697666559562,
-40.4936247912381));
#259738=CARTESIAN_POINT('Ctrl Pts',(-43.3806866868643,-57.0555278483981,
-40.4879619013523));
#259739=CARTESIAN_POINT('Ctrl Pts',(-43.3859186984709,-57.0270949764048,
-40.476993052777));
#259740=CARTESIAN_POINT('Ctrl Pts',(-43.3889115442249,-57.0128413374093,
-40.4716662621118));
#259741=CARTESIAN_POINT('Ctrl Pts',(-43.3955695423488,-56.984668670318,
-40.4614841416371));
#259742=CARTESIAN_POINT('Ctrl Pts',(-43.4029115329907,-56.9567427536229,
-40.4517375031029));
#259743=CARTESIAN_POINT('Ctrl Pts',(-43.4159439893498,-56.915628788467,
-40.4384286813559));
#259744=CARTESIAN_POINT('Ctrl Pts',(-43.4309850942545,-56.8752725380991,
-40.4264211055283));
#259745=CARTESIAN_POINT('Ctrl Pts',(-43.4480370013178,-56.8356780486645,
-40.4157207514563));
#259746=CARTESIAN_POINT('Ctrl Pts',(-43.4607570961379,-56.8097932355363,
-40.409467745062));
#259747=CARTESIAN_POINT('Ctrl Pts',(-43.4741642201056,-56.7841683331057,
-40.4036630043601));
#259748=CARTESIAN_POINT('Ctrl Pts',(-43.4812071336048,-56.7714928975767,
-40.4009861443346));
#259749=CARTESIAN_POINT('Ctrl Pts',(-43.4960130774609,-56.7463797512019,
-40.3960865778375));
#259750=CARTESIAN_POINT('Ctrl Pts',(-43.5037198572985,-56.7340380787953,
-40.3938827877695));
#259751=CARTESIAN_POINT('Ctrl Pts',(-43.527657505214,-56.6977883833479,
-40.3880276966888));
#259752=CARTESIAN_POINT('Ctrl Pts',(-43.5447483375558,-56.6745564757614,
-40.3851058766842));
#259753=CARTESIAN_POINT('Ctrl Pts',(-43.5811328114983,-56.629979998045,
-40.3812078888591));
#259754=CARTESIAN_POINT('Ctrl Pts',(-43.6004351631962,-56.6086219171049,
-40.3802294367552));
#259755=CARTESIAN_POINT('Ctrl Pts',(-43.6310475296952,-56.578014570072,
-40.3802318237287));
#259756=CARTESIAN_POINT('Ctrl Pts',(-43.6415402048873,-56.5680413281089,
-40.3804790384992));
#259757=CARTESIAN_POINT('Ctrl Pts',(-43.6576911458811,-56.5534539772523,
-40.3812231446347));
#259758=CARTESIAN_POINT('Ctrl Pts',(-43.6631494628181,-56.5486488515781,
-40.3815339900979));
#259759=CARTESIAN_POINT('Ctrl Pts',(-43.6742063152013,-56.5391628964206,
-40.3822815284329));
#259760=CARTESIAN_POINT('Ctrl Pts',(-43.6798092119243,-56.534479009001,
-40.3827188413654));
#259761=CARTESIAN_POINT('Ctrl Pts',(-43.6967370434146,-56.5206915949946,
-40.3842131357726));
#259762=CARTESIAN_POINT('Ctrl Pts',(-43.7196778600618,-56.5029622466235,
-40.386692708542));
#259763=CARTESIAN_POINT('Ctrl Pts',(-43.7670264629127,-56.4700551612604,
-40.3935618621563));
#259764=CARTESIAN_POINT('Ctrl Pts',(-43.8165352419067,-56.4409186299576,
-40.4032471370382));
#259765=CARTESIAN_POINT('Ctrl Pts',(-43.8552784957563,-56.4218759376155,
-40.4126045758866));
#259766=CARTESIAN_POINT('Ctrl Pts',(-43.8814691350842,-56.4098116142502,
-40.4193119877837));
#259767=CARTESIAN_POINT('Ctrl Pts',(-43.8947490665381,-56.4040935548973,
-40.4229014011429));
#259768=CARTESIAN_POINT('Ctrl Pts',(-43.9216608718689,-56.3933018151258,
-40.430550144354));
#259769=CARTESIAN_POINT('Ctrl Pts',(-43.9353412421961,-56.3882139347518,
-40.434625723994));
#259770=CARTESIAN_POINT('Ctrl Pts',(-43.9627318697344,-56.3788058930362,
-40.4431514805252));
#259771=CARTESIAN_POINT('Ctrl Pts',(-43.9765011076412,-56.3744602994329,
-40.4476175822086));
#259772=CARTESIAN_POINT('Ctrl Pts',(-44.0179764085085,-56.3624961934912,
-40.4615970784657));
#259773=CARTESIAN_POINT('Ctrl Pts',(-44.0598195105868,-56.3526585058303,
-40.4767455237411));
#259774=CARTESIAN_POINT('Ctrl Pts',(-44.1163310625808,-56.3437038269143,
-40.4992178608308));
#259775=CARTESIAN_POINT('Ctrl Pts',(-44.1590753545772,-56.3390714325247,
-40.5172068769433));
#259776=CARTESIAN_POINT('Ctrl Pts',(-44.1878153726385,-56.337382052278,
-40.5299596579145));
#259777=CARTESIAN_POINT('Ctrl Pts',(-44.2166756293141,-56.3364007867548,
-40.5430944022758));
#259778=CARTESIAN_POINT('Ctrl Pts',(-44.2311921171808,-56.3362675100036,
-40.5498666179945));
#259779=CARTESIAN_POINT('Ctrl Pts',(-44.2599977007373,-56.3367129587916,
-40.5636298486377));
#259780=CARTESIAN_POINT('Ctrl Pts',(-44.2743541649932,-56.3372884158027,
-40.5706510752088));
#259781=CARTESIAN_POINT('Ctrl Pts',(-44.3029357424357,-56.3391317429585,
-40.5849473061899));
#259782=CARTESIAN_POINT('Ctrl Pts',(-44.3456316213443,-56.3429350642169,
-40.6067818596389));
#259783=CARTESIAN_POINT('Ctrl Pts',(-44.4018650235691,-56.3520939287388,
-40.6374236066311));
#259784=CARTESIAN_POINT('Ctrl Pts',(-44.4574103376146,-56.3653147883305,
-40.6695718678152));
#259785=CARTESIAN_POINT('Ctrl Pts',(-44.4849466005937,-56.3732907222196,
-40.686147922621));
#259786=CARTESIAN_POINT('Ctrl Pts',(-44.512374392093,-56.3819617528141,
-40.7029840503412));
#259787=CARTESIAN_POINT('Ctrl Pts',(-44.5260289861432,-56.3866462995878,
-40.7115304197201));
#259788=CARTESIAN_POINT('Ctrl Pts',(-44.5529609776699,-56.3966203919845,
-40.7287150345567));
#259789=CARTESIAN_POINT('Ctrl Pts',(-44.5662873943758,-56.4019250012471,
-40.737383176176));
#259790=CARTESIAN_POINT('Ctrl Pts',(-44.6058068395674,-56.4187668411382,
-40.7635834132132));
#259791=CARTESIAN_POINT('Ctrl Pts',(-44.6315615859976,-56.4312362585519,
-40.7813233152079));
#259792=CARTESIAN_POINT('Ctrl Pts',(-44.6693071486035,-56.4518014713652,
-40.8083384498991));
#259793=CARTESIAN_POINT('Ctrl Pts',(-44.6817372625133,-56.458965010373,
-40.8174084081892));
#259794=CARTESIAN_POINT('Ctrl Pts',(-44.7063132537473,-56.473929075182,
-40.8356956250034));
#259795=CARTESIAN_POINT('Ctrl Pts',(-44.7183832523531,-56.4816832398284,
-40.8448563495594));
#259796=CARTESIAN_POINT('Ctrl Pts',(-44.7538754102704,-56.505703003501,
-40.8723327540241));
#259797=CARTESIAN_POINT('Ctrl Pts',(-44.7766465418209,-56.5227549736834,
-40.8906872015444));
#259798=CARTESIAN_POINT('Ctrl Pts',(-44.8204030914552,-56.5588699415109,
-40.9274359243417));
#259799=CARTESIAN_POINT('Ctrl Pts',(-44.851893062885,-56.5874690797881,
-40.9550350105826));
#259800=CARTESIAN_POINT('Ctrl Pts',(-44.8813802932551,-56.6183507815631,
-40.982690555711));
#259801=CARTESIAN_POINT('Ctrl Pts',(-44.9005867815582,-56.6394533348067,
-41.0011404791447));
#259802=CARTESIAN_POINT('Ctrl Pts',(-44.9099603095753,-56.6502571213647,
-41.0103678872986));
#259803=CARTESIAN_POINT('Ctrl Pts',(-44.9236872082217,-56.6668706184025,
-41.0242310114538));
#259804=CARTESIAN_POINT('Ctrl Pts',(-44.9282031316495,-56.6724722064122,
-41.0288518918758));
#259805=CARTESIAN_POINT('Ctrl Pts',(-44.9370720489983,-56.6837477093971,
-41.038048314582));
#259806=CARTESIAN_POINT('Ctrl Pts',(-44.9414338933841,-56.6894322363092,
-41.0426327511372));
#259807=CARTESIAN_POINT('Ctrl Pts',(-44.9542884395491,-56.7066066663578,
-41.0563299560217));
#259808=CARTESIAN_POINT('Ctrl Pts',(-44.9625629539304,-56.7182326826763,
-41.0653994431984));
#259809=CARTESIAN_POINT('Ctrl Pts',(-44.9864941991718,-56.7536111473724,
-41.0924067111081));
#259810=CARTESIAN_POINT('Ctrl Pts',(-45.0086645271567,-56.7900134244028,
-41.1190329135161));
#259811=CARTESIAN_POINT('Ctrl Pts',(-45.034704630644,-56.8405768845403,
-41.1537712607408));
#259812=CARTESIAN_POINT('Ctrl Pts',(-45.0465408860903,-56.8665423758261,
-41.1708862092094));
#259813=CARTESIAN_POINT('Ctrl Pts',(-45.0577761134165,-56.8928546179869,
-41.1878727246706));
#259814=CARTESIAN_POINT('Ctrl Pts',(-45.0630901582258,-56.906176087846,
-41.1962967595746));
#259815=CARTESIAN_POINT('Ctrl Pts',(-45.0731156002939,-56.9332061371524,
-41.2130345018643));
#259816=CARTESIAN_POINT('Ctrl Pts',(-45.0777961712447,-56.9468340019015,
-41.2212978165198));
#259817=CARTESIAN_POINT('Ctrl Pts',(-45.0907786540592,-56.9878560258786,
-41.2456540007716));
#259818=CARTESIAN_POINT('Ctrl Pts',(-45.0980724298404,-57.0154910056487,
-41.2613826498774));
#259819=CARTESIAN_POINT('Ctrl Pts',(-45.1099506000897,-57.0712899900431,
-41.2918166667949));
#259820=CARTESIAN_POINT('Ctrl Pts',(-45.1168338059478,-57.11354441615,-41.3138815317038));
#259821=CARTESIAN_POINT('Ctrl Pts',(-45.1206309792415,-57.1564190282566,
-41.3347987762303));
#259822=CARTESIAN_POINT('Ctrl Pts',(-45.1224627479043,-57.1851396939165,
-41.3484832320635));
#259823=CARTESIAN_POINT('Ctrl Pts',(-45.1230291819396,-57.199581674993,
-41.3552011986272));
#259824=CARTESIAN_POINT('Ctrl Pts',(-45.1234439819388,-57.2285619504273,
-41.3683510337761));
#259825=CARTESIAN_POINT('Ctrl Pts',(-45.1232917301137,-57.2429904040975,
-41.3747335054784));
#259826=CARTESIAN_POINT('Ctrl Pts',(-45.122279779691,-57.2717682086368,
-41.3871399525693));
#259827=CARTESIAN_POINT('Ctrl Pts',(-45.1196997436484,-57.3147947598186,
-41.4052018313649));
#259828=CARTESIAN_POINT('Ctrl Pts',(-45.1120557453653,-57.3716084168758,
-41.4271228345082));
#259829=CARTESIAN_POINT('Ctrl Pts',(-45.1031553338884,-57.4137999065974,
-41.4419446800329));
#259830=CARTESIAN_POINT('Ctrl Pts',(-45.09650693546,-57.4418330021969,-41.4514615780937));
#259831=CARTESIAN_POINT('Ctrl Pts',(-45.092823442876,-57.4558081403435,
-41.4560396298995));
#259832=CARTESIAN_POINT('Ctrl Pts',(-45.08473584999,-57.4836385233421,-41.464818484644));
#259833=CARTESIAN_POINT('Ctrl Pts',(-45.0803094818206,-57.4975537933777,
-41.4690360581021));
#259834=CARTESIAN_POINT('Ctrl Pts',(-45.0708158371377,-57.5249803724867,
-41.4770040232021));
#259835=CARTESIAN_POINT('Ctrl Pts',(-45.060662137239,-57.5520858826269,
-41.4845331733926));
#259836=CARTESIAN_POINT('Ctrl Pts',(-45.0434887903859,-57.591755117417,
-41.4945182619959));
#259837=CARTESIAN_POINT('Ctrl Pts',(-45.0243848727922,-57.6304534586566,
-41.5032105668009));
#259838=CARTESIAN_POINT('Ctrl Pts',(-45.0033512023575,-57.6681778817651,
-41.51061115159));
#259839=CARTESIAN_POINT('Ctrl Pts',(-44.9880328234845,-57.692673879575,
-41.5146787869643));
#259840=CARTESIAN_POINT('Ctrl Pts',(-44.9720568870916,-57.7168380825906,
-41.5183074012753));
#259841=CARTESIAN_POINT('Ctrl Pts',(-44.9637457009402,-57.7287466936453,
-41.5199012977462));
#259842=CARTESIAN_POINT('Ctrl Pts',(-44.9464287138105,-57.7522550306847,
-41.5226441863212));
#259843=CARTESIAN_POINT('Ctrl Pts',(-44.9374830238235,-57.7637718882179,
-41.5237830976086));
#259844=CARTESIAN_POINT('Ctrl Pts',(-44.9099214446927,-57.7974515399035,
-41.5264929611258));
#259845=CARTESIAN_POINT('Ctrl Pts',(-44.8905204729439,-57.8188493934961,
-41.5273772161885));
#259846=CARTESIAN_POINT('Ctrl Pts',(-44.8497318000032,-57.8595330722204,
-41.5273307191807));
#259847=CARTESIAN_POINT('Ctrl Pts',(-44.8283374647208,-57.878828810327,
-41.5264014189239));
#259848=CARTESIAN_POINT('Ctrl Pts',(-44.7947479986672,-57.9061820008563,
-41.5236391765087));
#259849=CARTESIAN_POINT('Ctrl Pts',(-44.7832945060713,-57.9150388128137,
-41.5224889540588));
#259850=CARTESIAN_POINT('Ctrl Pts',(-44.7657408175914,-57.9279147771907,
-41.5204166102647));
#259851=CARTESIAN_POINT('Ctrl Pts',(-44.7598217545323,-57.9321421746299,
-41.5196671186517));
#259852=CARTESIAN_POINT('Ctrl Pts',(-44.7478629508254,-57.9404557426351,
-41.5180519716851));
#259853=CARTESIAN_POINT('Ctrl Pts',(-44.7297025277655,-57.9527400844071,
-41.5154481926132));
#259854=CARTESIAN_POINT('Ctrl Pts',(-44.711220794734,-57.9642369190977,
-41.5123523449538));
#259855=CARTESIAN_POINT('Ctrl Pts',(-44.6862770262529,-57.9788987855805,
-41.5077941640223));
#259856=CARTESIAN_POINT('Ctrl Pts',(-44.6484202704456,-57.9998814948776,
-41.5003121274858));
#259857=CARTESIAN_POINT('Ctrl Pts',(-44.5962108390282,-58.0238874022289,
-41.4877980263462));
#259858=CARTESIAN_POINT('Ctrl Pts',(-44.5557649369164,-58.0389385823793,
-41.4765186283493));
#259859=CARTESIAN_POINT('Ctrl Pts',(-44.5285120653069,-58.048310487242,
-41.4685735203231));
#259860=CARTESIAN_POINT('Ctrl Pts',(-44.5147341086114,-58.0526671867402,
-41.4643859028639));
#259861=CARTESIAN_POINT('Ctrl Pts',(-44.4869140318333,-58.0607029371288,
-41.4555883503401));
#259862=CARTESIAN_POINT('Ctrl Pts',(-44.4728027150897,-58.0643973546439,
-41.4509544537452));
#259863=CARTESIAN_POINT('Ctrl Pts',(-44.4304531283686,-58.0743536715507,
-41.4365378845966));
#259864=CARTESIAN_POINT('Ctrl Pts',(-44.3879697631396,-58.0821103913619,
-41.4210702443308));
#259865=CARTESIAN_POINT('Ctrl Pts',(-44.3452880889881,-58.0866896268435,
-41.4040725286766));
#259866=CARTESIAN_POINT('Ctrl Pts',(-44.3025416355467,-58.090217180745,
-41.3865671155567));
#259867=CARTESIAN_POINT('Ctrl Pts',(-44.2739489581488,-58.0911687787978,
-41.3742170239002));
#259868=CARTESIAN_POINT('Ctrl Pts',(-44.2309555122234,-58.090491506171,
-41.3546803180427));
#259869=CARTESIAN_POINT('Ctrl Pts',(-44.2165895018292,-58.0899123697243,
-41.347990487553));
#259870=CARTESIAN_POINT('Ctrl Pts',(-44.1950278537333,-58.0885113544661,
-41.337705180963));
#259871=CARTESIAN_POINT('Ctrl Pts',(-44.1878319550126,-58.0879547296283,
-41.3342316293533));
#259872=CARTESIAN_POINT('Ctrl Pts',(-44.1734279164018,-58.0866616594573,
-41.3271961709002));
#259873=CARTESIAN_POINT('Ctrl Pts',(-44.1662260389348,-58.0859253983809,
-41.3236371482021));
#259874=CARTESIAN_POINT('Ctrl Pts',(-44.130389101081,-58.0818150523559,
-41.3057210105631));
#259875=CARTESIAN_POINT('Ctrl Pts',(-44.073848260417,-58.0724828543971,
-41.2761395013722));
#259876=CARTESIAN_POINT('Ctrl Pts',(-44.0188545174212,-58.0578491440998,
-41.2447838757269));
#259877=CARTESIAN_POINT('Ctrl Pts',(-43.9646246641704,-58.0405931079736,
-41.2125419608827));
#259878=CARTESIAN_POINT('Ctrl Pts',(-43.9378880325505,-58.0306505669816,
-41.1959746665064));
#259879=CARTESIAN_POINT('Ctrl Pts',(-43.9049634769563,-58.0165631445999,
-41.174705886574));
#259880=CARTESIAN_POINT('Ctrl Pts',(-43.898399460067,-58.0136596367661,
-41.1704209658528));
#259881=CARTESIAN_POINT('Ctrl Pts',(-43.8853286348063,-58.0076886655405,
-41.1617993561325));
#259882=CARTESIAN_POINT('Ctrl Pts',(-43.8788088737381,-58.0046144513738,
-41.157453730181));
#259883=CARTESIAN_POINT('Ctrl Pts',(-43.8593967360427,-57.9951717320096,
-41.1443784829743));
#259884=CARTESIAN_POINT('Ctrl Pts',(-43.8466719188398,-57.9885954718361,
-41.1356253645631));
#259885=CARTESIAN_POINT('Ctrl Pts',(-43.8341420587998,-57.9817357678076,
-41.1268248734572));
#259886=CARTESIAN_POINT('',(-45.4581751231188,-55.7156010961851,-39.3126317220031));
#259887=CARTESIAN_POINT('',(-45.3904396609892,-55.7772425608068,-39.4382820396906));
#259888=CARTESIAN_POINT('',(-45.4581751231188,-55.7156010961851,-39.3126317220031));
#259889=CARTESIAN_POINT('Origin',(-44.3987054398481,-57.592449415963,-39.4571364862761));
#259890=CARTESIAN_POINT('Ctrl Pts',(-45.8699710781849,-56.0109010507348,
-39.4567769182892));
#259891=CARTESIAN_POINT('Ctrl Pts',(-45.8053259834915,-55.968605507759,
-39.4535705001808));
#259892=CARTESIAN_POINT('Ctrl Pts',(-45.7383889969054,-55.9298524990358,
-39.4505766434469));
#259893=CARTESIAN_POINT('Ctrl Pts',(-45.5794955533779,-55.8490954403259,
-39.4442200262513));
#259894=CARTESIAN_POINT('Ctrl Pts',(-45.4862186035378,-55.809766049426,
-39.4410295384064));
#259895=CARTESIAN_POINT('Ctrl Pts',(-45.3904396609892,-55.7772425608068,
-39.4382820396906));
#259896=CARTESIAN_POINT('Ctrl Pts',(-45.6739227548714,-55.5192637629146,
-38.912416567246));
#259897=CARTESIAN_POINT('Ctrl Pts',(-45.7067749877366,-55.5369855856674,
-38.9214216121434));
#259898=CARTESIAN_POINT('Ctrl Pts',(-45.7392219877792,-55.5555212114617,
-38.9304915704333));
#259899=CARTESIAN_POINT('Ctrl Pts',(-45.8033556832395,-55.5942722159849,
-38.9487787872477));
#259900=CARTESIAN_POINT('Ctrl Pts',(-45.8348443691401,-55.6143675312756,
-38.9579395118016));
#259901=CARTESIAN_POINT('Ctrl Pts',(-45.9274099842789,-55.6766589025305,
-38.9854159162722));
#259902=CARTESIAN_POINT('Ctrl Pts',(-45.9867610865919,-55.7209353156014,
-39.0037703637879));
#259903=CARTESIAN_POINT('Ctrl Pts',(-46.1007337830098,-55.8148102393793,
-39.0405190865864));
#259904=CARTESIAN_POINT('Ctrl Pts',(-46.155375425224,-55.8644173763685,
-39.0589184916404));
#259905=CARTESIAN_POINT('Ctrl Pts',(-46.2338037269528,-55.9428521307486,
-39.0865551957989));
#259906=CARTESIAN_POINT('Ctrl Pts',(-46.259356574729,-55.9696687352924,
-39.0957737179551));
#259907=CARTESIAN_POINT('Ctrl Pts',(-46.309266807939,-56.024663053365,-39.1142236413887));
#259908=CARTESIAN_POINT('Ctrl Pts',(-46.3336138177017,-56.0528284109483,
-39.1234510495426));
#259909=CARTESIAN_POINT('Ctrl Pts',(-46.3692509284248,-56.0961546965834,
-39.1373141736981));
#259910=CARTESIAN_POINT('Ctrl Pts',(-46.3809719555493,-56.1107655250657,
-39.14193505412));
#259911=CARTESIAN_POINT('Ctrl Pts',(-46.4039850968433,-56.1401806715041,
-39.1511314768264));
#259912=CARTESIAN_POINT('Ctrl Pts',(-46.4153001903629,-56.1550126624777,
-39.1557159133814));
#259913=CARTESIAN_POINT('Ctrl Pts',(-46.4486370096884,-56.1998310060262,
-39.1694131182658));
#259914=CARTESIAN_POINT('Ctrl Pts',(-46.4700835091466,-56.2301795317326,
-39.1784826054425));
#259915=CARTESIAN_POINT('Ctrl Pts',(-46.5320719136859,-56.3225583984772,
-39.2054898733524));
#259916=CARTESIAN_POINT('Ctrl Pts',(-46.5703035947222,-56.3859631579321,
-39.2232408562602));
#259917=CARTESIAN_POINT('Ctrl Pts',(-46.6230137301682,-56.4837650915426,
-39.2494851373609));
#259918=CARTESIAN_POINT('Ctrl Pts',(-46.6398105780351,-56.5168167317113,
-39.2581698041384));
#259919=CARTESIAN_POINT('Ctrl Pts',(-46.6718446885168,-56.5838294931519,
-39.2754119185794));
#259920=CARTESIAN_POINT('Ctrl Pts',(-46.6870820302515,-56.617790568625,
-39.2839693714534));
#259921=CARTESIAN_POINT('Ctrl Pts',(-46.7159729830272,-56.6866360545619,
-39.3009558869148));
#259922=CARTESIAN_POINT('Ctrl Pts',(-46.7296188023799,-56.7214992889704,
-39.3093799218186));
#259923=CARTESIAN_POINT('Ctrl Pts',(-46.7553216997642,-56.7922546384013,
-39.3261176641085));
#259924=CARTESIAN_POINT('Ctrl Pts',(-46.7672996943011,-56.8279354881579,
-39.3343809787628));
#259925=CARTESIAN_POINT('Ctrl Pts',(-46.8004530502947,-56.9353633959568,
-39.358737163018));
#259926=CARTESIAN_POINT('Ctrl Pts',(-46.8189795501832,-57.0077635587999,
-39.3744658121213));
#259927=CARTESIAN_POINT('Ctrl Pts',(-46.848916211803,-57.1540080946302,
-39.4048998290393));
#259928=CARTESIAN_POINT('Ctrl Pts',(-46.8603369445408,-57.2278698672909,
-39.4196100581687));
#259929=CARTESIAN_POINT('Ctrl Pts',(-46.8720664744741,-57.3397812895282,
-39.4409093640372));
#259930=CARTESIAN_POINT('Ctrl Pts',(-46.875074749658,-57.3772756893033,
-39.4478819384746));
#259931=CARTESIAN_POINT('Ctrl Pts',(-46.8792542953452,-57.4526370309597,
-39.4615663943076));
#259932=CARTESIAN_POINT('Ctrl Pts',(-46.8804258736835,-57.4905390832846,
-39.4682843608713));
#259933=CARTESIAN_POINT('Ctrl Pts',(-46.8808837743635,-57.5666104373409,
-39.4814341960201));
#259934=CARTESIAN_POINT('Ctrl Pts',(-46.8801708637706,-57.604491394965,
-39.4878166677226));
#259935=CARTESIAN_POINT('Ctrl Pts',(-46.8768913879562,-57.6800597985945,
-39.5002231148134));
#259936=CARTESIAN_POINT('Ctrl Pts',(-46.8743246637802,-57.7177284992744,
-39.5062438407196));
#259937=CARTESIAN_POINT('Ctrl Pts',(-46.863867568228,-57.8303908432586,
-39.5237649596504));
#259938=CARTESIAN_POINT('Ctrl Pts',(-46.8532263654434,-57.9050414873811,
-39.5347254895779));
#259939=CARTESIAN_POINT('Ctrl Pts',(-46.8317335315027,-58.0163268447592,
-39.5500873410526));
#259940=CARTESIAN_POINT('Ctrl Pts',(-46.8236459543104,-58.0533066811291,
-39.5550278422771));
#259941=CARTESIAN_POINT('Ctrl Pts',(-46.8055990109883,-58.1270324939451,
-39.5645447403379));
#259942=CARTESIAN_POINT('Ctrl Pts',(-46.7956339676918,-58.1637938532181,
-39.5691227921436));
#259943=CARTESIAN_POINT('Ctrl Pts',(-46.7738161327052,-58.2370162077018,
-39.5779016468881));
#259944=CARTESIAN_POINT('Ctrl Pts',(-46.7619036278491,-58.2736352268715,
-39.5821192203466));
#259945=CARTESIAN_POINT('Ctrl Pts',(-46.7364059718256,-58.3458255995332,
-39.5900871854462));
#259946=CARTESIAN_POINT('Ctrl Pts',(-46.7227943874693,-58.3815079294473,
-39.593852026583));
#259947=CARTESIAN_POINT('Ctrl Pts',(-46.6938810604275,-58.4520118571144,
-39.6009443874688));
#259948=CARTESIAN_POINT('Ctrl Pts',(-46.6785776252269,-58.4868413763864,
-39.6042729713841));
#259949=CARTESIAN_POINT('Ctrl Pts',(-46.6462897337504,-58.5556617200885,
-39.6104989383907));
#259950=CARTESIAN_POINT('Ctrl Pts',(-46.629305264578,-58.5896525381261,
-39.6133963175589));
#259951=CARTESIAN_POINT('Ctrl Pts',(-46.5936553532051,-58.6567954587996,
-39.6187605717742));
#259952=CARTESIAN_POINT('Ctrl Pts',(-46.5749899237926,-58.6899475678396,
-39.6212274496765));
#259953=CARTESIAN_POINT('Ctrl Pts',(-46.5359657438849,-58.7554068733743,
-39.6257281334421));
#259954=CARTESIAN_POINT('Ctrl Pts',(-46.515607032986,-58.7877140896313,
-39.6277619492082));
#259955=CARTESIAN_POINT('Ctrl Pts',(-46.4731710833873,-58.8514710047945,
-39.6313905635194));
#259956=CARTESIAN_POINT('Ctrl Pts',(-46.4511086137466,-58.8829006319494,
-39.6329844599904));
#259957=CARTESIAN_POINT('Ctrl Pts',(-46.4051673201273,-58.9449633016888,
-39.6357273485653));
#259958=CARTESIAN_POINT('Ctrl Pts',(-46.381447994276,-58.975377588932,-39.6368662598532));
#259959=CARTESIAN_POINT('Ctrl Pts',(-46.3084068909562,-59.0643493136613,
-39.639576123369));
#259960=CARTESIAN_POINT('Ctrl Pts',(-46.2570407846103,-59.1209150453975,
-39.6404603784326));
#259961=CARTESIAN_POINT('Ctrl Pts',(-46.1491379755941,-59.228544463199,
-39.6404138814247));
#259962=CARTESIAN_POINT('Ctrl Pts',(-46.0925836555154,-59.2796343044913,
-39.6394845811683));
#259963=CARTESIAN_POINT('Ctrl Pts',(-46.003852943763,-59.3521266125548,
-39.6367223387528));
#259964=CARTESIAN_POINT('Ctrl Pts',(-45.9736068078661,-59.3756113554054,
-39.6355721163029));
#259965=CARTESIAN_POINT('Ctrl Pts',(-45.9272656961273,-59.4097723546528,
-39.6334997725088));
#259966=CARTESIAN_POINT('Ctrl Pts',(-45.9116419215573,-59.4209912820171,
-39.6327502808957));
#259967=CARTESIAN_POINT('Ctrl Pts',(-45.8800804794677,-59.4430610802668,
-39.6311351339295));
#259968=CARTESIAN_POINT('Ctrl Pts',(-45.8641077773929,-59.4539347618601,
-39.6302673980329));
#259969=CARTESIAN_POINT('Ctrl Pts',(-45.8159067176779,-59.4858696807562,
-39.6274990247155));
#259970=CARTESIAN_POINT('Ctrl Pts',(-45.7834097108732,-59.5062438963941,
-39.6254355071979));
#259971=CARTESIAN_POINT('Ctrl Pts',(-45.717633106262,-59.5452481912826,
-39.6208773262667));
#259972=CARTESIAN_POINT('Ctrl Pts',(-45.6843658495255,-59.5638704323978,
-39.6183834291471));
#259973=CARTESIAN_POINT('Ctrl Pts',(-45.5834449288538,-59.6171384125673,
-39.6102664280093));
#259974=CARTESIAN_POINT('Ctrl Pts',(-45.5146744626452,-59.6491908713697,
-39.6040093949256));
#259975=CARTESIAN_POINT('Ctrl Pts',(-45.409303365533,-59.6921244665012,
-39.5933617316812));
#259976=CARTESIAN_POINT('Ctrl Pts',(-45.3738098009101,-59.7055766782111,
-39.5896017905935));
#259977=CARTESIAN_POINT('Ctrl Pts',(-45.3020778813705,-59.7307512119864,
-39.5816566825671));
#259978=CARTESIAN_POINT('Ctrl Pts',(-45.2658207311094,-59.7424779859238,
-39.5774690651077));
#259979=CARTESIAN_POINT('Ctrl Pts',(-45.1926264675053,-59.7641596016776,
-39.5686715125846));
#259980=CARTESIAN_POINT('Ctrl Pts',(-45.1555073907618,-59.7741562512685,
-39.5640376159893));
#259981=CARTESIAN_POINT('Ctrl Pts',(-45.0812568479429,-59.7921790564438,
-39.5544265698906));
#259982=CARTESIAN_POINT('Ctrl Pts',(-45.04408172978,-59.8002277891036,-39.5494458391365));
#259983=CARTESIAN_POINT('Ctrl Pts',(-44.9696261062542,-59.8144410677077,
-39.5391390505826));
#259984=CARTESIAN_POINT('Ctrl Pts',(-44.9323469822025,-59.8206061841119,
-39.5338133285981));
#259985=CARTESIAN_POINT('Ctrl Pts',(-44.8576879123993,-59.8310833805954,
-39.5228216573624));
#259986=CARTESIAN_POINT('Ctrl Pts',(-44.8203079610257,-59.8353953605365,
-39.5171556909205));
#259987=CARTESIAN_POINT('Ctrl Pts',(-44.7080184564225,-59.8455760612674,
-39.4996502778007));
#259988=CARTESIAN_POINT('Ctrl Pts',(-44.6329372249224,-59.8486931621852,
-39.4873001861445));
#259989=CARTESIAN_POINT('Ctrl Pts',(-44.5200834441659,-59.8478515133141,
-39.4677634802869));
#259990=CARTESIAN_POINT('Ctrl Pts',(-44.4823810871712,-59.8466449718289,
-39.4610736497973));
#259991=CARTESIAN_POINT('Ctrl Pts',(-44.4258051079382,-59.8434394706745,
-39.4507883432074));
#259992=CARTESIAN_POINT('Ctrl Pts',(-44.4069254589855,-59.8421361346926,
-39.4473147915973));
#259993=CARTESIAN_POINT('Ctrl Pts',(-44.3691376542581,-59.8390581625153,
-39.4402793331445));
#259994=CARTESIAN_POINT('Ctrl Pts',(-44.3502459350849,-59.8372838734483,
-39.4367203104461));
#259995=CARTESIAN_POINT('Ctrl Pts',(-44.2938476169342,-59.8312836889756,
-39.4259706278629));
#259996=CARTESIAN_POINT('Ctrl Pts',(-44.2565162762141,-59.8263768596807,
-39.4186892629542));
#259997=CARTESIAN_POINT('Ctrl Pts',(-44.1823865424055,-59.8147890207299,
-39.4039021619013));
#259998=CARTESIAN_POINT('Ctrl Pts',(-44.14558648486,-59.8081083758143,-39.3963962058824));
#259999=CARTESIAN_POINT('Ctrl Pts',(-44.0359682134124,-59.785449432176,
-39.3735449917432));
#260000=CARTESIAN_POINT('Ctrl Pts',(-43.9639303529155,-59.7668593120831,
-39.3578670379715));
#260001=CARTESIAN_POINT('Ctrl Pts',(-43.8219159040518,-59.7227861654644,
-39.3256251231267));
#260002=CARTESIAN_POINT('Ctrl Pts',(-43.7519290534068,-59.6972943066161,
-39.3090578287532));
#260003=CARTESIAN_POINT('Ctrl Pts',(-43.665783177736,-59.6610675807532,
-39.2877890488175));
#260004=CARTESIAN_POINT('Ctrl Pts',(-43.6486106666635,-59.653596197985,
-39.2835041280971));
#260005=CARTESIAN_POINT('Ctrl Pts',(-43.6144193015917,-59.6382222359849,
-39.2748825183767));
#260006=CARTESIAN_POINT('Ctrl Pts',(-43.597366582891,-59.6303022352814,
-39.2705368924251));
#260007=CARTESIAN_POINT('Ctrl Pts',(-43.5465994182958,-59.6059619032979,
-39.2574616452183));
#260008=CARTESIAN_POINT('Ctrl Pts',(-43.5133293006631,-59.588993111175,
-39.2487085268073));
#260009=CARTESIAN_POINT('Ctrl Pts',(-43.4805771074156,-59.5712767529309,
-39.2399080357013));
#260010=CARTESIAN_POINT('Ctrl Pts',(-45.4581748301254,-55.7156013628182,
-39.3126322655097));
#260011=CARTESIAN_POINT('Ctrl Pts',(-45.4867277088334,-55.7310183438428,
-39.321637310407));
#260012=CARTESIAN_POINT('Ctrl Pts',(-45.51492912057,-55.7471419461907,-39.330707268697));
#260013=CARTESIAN_POINT('Ctrl Pts',(-45.5706726136103,-55.7808477327706,
-39.3489944855113));
#260014=CARTESIAN_POINT('Ctrl Pts',(-45.5980425893803,-55.7983254858436,
-39.3581552100656));
#260015=CARTESIAN_POINT('Ctrl Pts',(-45.6785029049759,-55.8524994362108,
-39.3856316145351));
#260016=CARTESIAN_POINT('Ctrl Pts',(-45.7300953831417,-55.8910015357548,
-39.4039860620517));
#260017=CARTESIAN_POINT('Ctrl Pts',(-45.8291752111236,-55.9726255533772,
-39.4407347848499));
#260018=CARTESIAN_POINT('Ctrl Pts',(-45.876679984022,-56.0157549785288,
-39.459134189904));
#260019=CARTESIAN_POINT('Ctrl Pts',(-45.9448695334179,-56.0839422557895,
-39.4867708940624));
#260020=CARTESIAN_POINT('Ctrl Pts',(-45.9670873402583,-56.1072544162851,
-39.4959894162187));
#260021=CARTESIAN_POINT('Ctrl Pts',(-46.0104852988087,-56.1550602795965,
-39.5144393396524));
#260022=CARTESIAN_POINT('Ctrl Pts',(-46.0316564280385,-56.1795432421045,
-39.5236667478063));
#260023=CARTESIAN_POINT('Ctrl Pts',(-46.0626463753838,-56.2172037362606,
-39.5375298719617));
#260024=CARTESIAN_POINT('Ctrl Pts',(-46.072839197582,-56.2299037017973,
-39.5421507523836));
#260025=CARTESIAN_POINT('Ctrl Pts',(-46.0928523442025,-56.2554714237357,
-39.55134717509));
#260026=CARTESIAN_POINT('Ctrl Pts',(-46.1026926512335,-56.268363234494,
-39.555931611645));
#260027=CARTESIAN_POINT('Ctrl Pts',(-46.1316851735074,-56.3073182946572,
-39.5696288165295));
#260028=CARTESIAN_POINT('Ctrl Pts',(-46.1503378904843,-56.3336957698022,
-39.5786983037061));
#260029=CARTESIAN_POINT('Ctrl Pts',(-46.2042543586894,-56.4139848320304,
-39.605705571616));
#260030=CARTESIAN_POINT('Ctrl Pts',(-46.2375119613918,-56.4690888109481,
-39.6234565545238));
#260031=CARTESIAN_POINT('Ctrl Pts',(-46.2833712877372,-56.5540826662774,
-39.6497008356246));
#260032=CARTESIAN_POINT('Ctrl Pts',(-46.2979862913122,-56.5828052175225,
-39.658385502402));
#260033=CARTESIAN_POINT('Ctrl Pts',(-46.3258619629745,-56.6410393597078,
-39.6756276168431));
#260034=CARTESIAN_POINT('Ctrl Pts',(-46.3391226997695,-56.6705509109048,
-39.684185069717));
#260035=CARTESIAN_POINT('Ctrl Pts',(-46.3642688672173,-56.7303750814786,
-39.7011715851784));
#260036=CARTESIAN_POINT('Ctrl Pts',(-46.3761475143767,-56.7606693003541,
-39.7095956200823));
#260037=CARTESIAN_POINT('Ctrl Pts',(-46.3985252181961,-56.8221504988681,
-39.7263333623721));
#260038=CARTESIAN_POINT('Ctrl Pts',(-46.408955426727,-56.8531539030601,
-39.7345966770267));
#260039=CARTESIAN_POINT('Ctrl Pts',(-46.43783053371,-56.9464971004833,-39.7589528612811));
#260040=CARTESIAN_POINT('Ctrl Pts',(-46.4539745690236,-57.0094025528851,
-39.774681510385));
#260041=CARTESIAN_POINT('Ctrl Pts',(-46.4800810185276,-57.1364635567237,
-39.8051155273028));
#260042=CARTESIAN_POINT('Ctrl Pts',(-46.4900526283019,-57.200634229788,
-39.8198257564322));
#260043=CARTESIAN_POINT('Ctrl Pts',(-46.5003179883916,-57.2978587411347,
-39.8411250623009));
#260044=CARTESIAN_POINT('Ctrl Pts',(-46.5029566336967,-57.3304319169396,
-39.8480976367382));
#260045=CARTESIAN_POINT('Ctrl Pts',(-46.5066382150844,-57.3959007554725,
-39.8617820925713));
#260046=CARTESIAN_POINT('Ctrl Pts',(-46.5076814421117,-57.4288269187661,
-39.8685000591349));
#260047=CARTESIAN_POINT('Ctrl Pts',(-46.5081302011228,-57.4949102391499,
-39.8816498942838));
#260048=CARTESIAN_POINT('Ctrl Pts',(-46.5075362064438,-57.5278169127684,
-39.8880323659863));
#260049=CARTESIAN_POINT('Ctrl Pts',(-46.5047376735305,-57.5934610145355,
-39.900438813077));
#260050=CARTESIAN_POINT('Ctrl Pts',(-46.5025329846453,-57.6261821585506,
-39.9064595389832));
#260051=CARTESIAN_POINT('Ctrl Pts',(-46.4935235433768,-57.7240452733633,
-39.923980657914));
#260052=CARTESIAN_POINT('Ctrl Pts',(-46.4843287087445,-57.788887590308,
-39.9349411878415));
#260053=CARTESIAN_POINT('Ctrl Pts',(-46.4657308186056,-57.885547740833,
-39.9503030393162));
#260054=CARTESIAN_POINT('Ctrl Pts',(-46.4587293129245,-57.9176670783696,
-39.9552435405408));
#260055=CARTESIAN_POINT('Ctrl Pts',(-46.4431000048223,-57.9817014504392,
-39.9647604386015));
#260056=CARTESIAN_POINT('Ctrl Pts',(-46.4344672805524,-58.0136298445192,
-39.9693384904073));
#260057=CARTESIAN_POINT('Ctrl Pts',(-46.4155616345504,-58.0772245465278,
-39.9781173451517));
#260058=CARTESIAN_POINT('Ctrl Pts',(-46.4052369418127,-58.1090280928419,
-39.9823349186101));
#260059=CARTESIAN_POINT('Ctrl Pts',(-46.383133741997,-58.1717240497799,
-39.9903028837099));
#260060=CARTESIAN_POINT('Ctrl Pts',(-46.3713323447936,-58.2027128491507,
-39.9940677248466));
#260061=CARTESIAN_POINT('Ctrl Pts',(-46.3462606561336,-58.263941687033,
-40.0011600857324));
#260062=CARTESIAN_POINT('Ctrl Pts',(-46.3329888995612,-58.2941886059125,
-40.0044886696476));
#260063=CARTESIAN_POINT('Ctrl Pts',(-46.3049844543585,-58.3539528281862,
-40.0107146366544));
#260064=CARTESIAN_POINT('Ctrl Pts',(-46.2902517545131,-58.3834701260217,
-40.0136120158225));
#260065=CARTESIAN_POINT('Ctrl Pts',(-46.2593254742523,-58.4417750834909,
-40.0189762700378));
#260066=CARTESIAN_POINT('Ctrl Pts',(-46.2431319049432,-58.4705627487002,
-40.0214431479402));
#260067=CARTESIAN_POINT('Ctrl Pts',(-46.2092731643552,-58.5274030440657,
-40.0259438317057));
#260068=CARTESIAN_POINT('Ctrl Pts',(-46.1916080274801,-58.5554556914203,
-40.0279776474719));
#260069=CARTESIAN_POINT('Ctrl Pts',(-46.1547842556146,-58.6108149789715,
-40.0316062617831));
#260070=CARTESIAN_POINT('Ctrl Pts',(-46.1356384378441,-58.6381041920218,
-40.033200158254));
#260071=CARTESIAN_POINT('Ctrl Pts',(-46.0957683692941,-58.6919894747804,
-40.0359430468289));
#260072=CARTESIAN_POINT('Ctrl Pts',(-46.0751825365968,-58.718395610803,
-40.0370819581167));
#260073=CARTESIAN_POINT('Ctrl Pts',(-46.0117876557102,-58.7956398681744,
-40.0397918216329));
#260074=CARTESIAN_POINT('Ctrl Pts',(-45.967201365203,-58.8447464810846,
-40.0406760766962));
#260075=CARTESIAN_POINT('Ctrl Pts',(-45.8735334871044,-58.9381766850286,
-40.0406295796883));
#260076=CARTESIAN_POINT('Ctrl Pts',(-45.8244366116702,-58.9825229863024,
-40.0397002794319));
#260077=CARTESIAN_POINT('Ctrl Pts',(-45.7474013767448,-59.045441272299,
-40.0369380370164));
#260078=CARTESIAN_POINT('Ctrl Pts',(-45.721141166836,-59.0658234260692,
-40.0357878145665));
#260079=CARTESIAN_POINT('Ctrl Pts',(-45.6809058772882,-59.0954698622353,
-40.0337154707725));
#260080=CARTESIAN_POINT('Ctrl Pts',(-45.6673404753058,-59.1052058837424,
-40.0329659791594));
#260081=CARTESIAN_POINT('Ctrl Pts',(-45.6399367594346,-59.1243579809134,
-40.0313508321932));
#260082=CARTESIAN_POINT('Ctrl Pts',(-45.6260680251864,-59.1337938500571,
-40.0304830962965));
#260083=CARTESIAN_POINT('Ctrl Pts',(-45.5842155891604,-59.1615052138478,
-40.0277147229792));
#260084=CARTESIAN_POINT('Ctrl Pts',(-45.5559980798161,-59.1791836959668,
-40.0256512054615));
#260085=CARTESIAN_POINT('Ctrl Pts',(-45.4988821335321,-59.2130249535731,
-40.0210930245302));
#260086=CARTESIAN_POINT('Ctrl Pts',(-45.4699944124056,-59.2291809279018,
-40.0185991274108));
#260087=CARTESIAN_POINT('Ctrl Pts',(-45.382357426366,-59.2753904813377,
-40.010482126273));
#260088=CARTESIAN_POINT('Ctrl Pts',(-45.3226363823857,-59.3031904383161,
-40.0042250931893));
#260089=CARTESIAN_POINT('Ctrl Pts',(-45.2311271265862,-59.3404191081965,
-39.9935774299448));
#260090=CARTESIAN_POINT('Ctrl Pts',(-45.2003022091057,-59.3520821754701,
-39.9898174888571));
#260091=CARTESIAN_POINT('Ctrl Pts',(-45.1380043106471,-59.3739049663185,
-39.9818723808308));
#260092=CARTESIAN_POINT('Ctrl Pts',(-45.1065150049296,-59.3840685449793,
-39.9776847633714));
#260093=CARTESIAN_POINT('Ctrl Pts',(-45.0429446216685,-59.4028558680827,
-39.9688872108481));
#260094=CARTESIAN_POINT('Ctrl Pts',(-45.0107054985878,-59.4115158121228,
-39.9642533142529));
#260095=CARTESIAN_POINT('Ctrl Pts',(-44.9462152798728,-59.4271237996878,
-39.9546422681542));
#260096=CARTESIAN_POINT('Ctrl Pts',(-44.9139262776317,-59.4340914281647,
-39.9496615374001));
#260097=CARTESIAN_POINT('Ctrl Pts',(-44.8492555669035,-59.4463896950644,
-39.9393547488463));
#260098=CARTESIAN_POINT('Ctrl Pts',(-44.8168750587066,-59.4517208300076,
-39.9340290268618));
#260099=CARTESIAN_POINT('Ctrl Pts',(-44.7520253206349,-59.4607731680205,
-39.923037355626));
#260100=CARTESIAN_POINT('Ctrl Pts',(-44.7195560858118,-59.4644942841012,
-39.9173713891842));
#260101=CARTESIAN_POINT('Ctrl Pts',(-44.6220166858359,-59.4732638501436,
-39.8998659760644));
#260102=CARTESIAN_POINT('Ctrl Pts',(-44.5567956923543,-59.4759216471728,
-39.8875158844081));
#260103=CARTESIAN_POINT('Ctrl Pts',(-44.4587593121986,-59.4751148625585,
-39.8679791785505));
#260104=CARTESIAN_POINT('Ctrl Pts',(-44.4260066021956,-59.4740413938938,
-39.861289348061));
#260105=CARTESIAN_POINT('Ctrl Pts',(-44.3768571744168,-59.4712186248072,
-39.8510040414711));
#260106=CARTESIAN_POINT('Ctrl Pts',(-44.3604556528324,-59.470073666511,
-39.8475304898609));
#260107=CARTESIAN_POINT('Ctrl Pts',(-44.3276275527921,-59.4673742726518,
-39.8404950314082));
#260108=CARTESIAN_POINT('Ctrl Pts',(-44.3112152529909,-59.465820149672,
-39.8369360087098));
#260109=CARTESIAN_POINT('Ctrl Pts',(-44.2622184211888,-59.4605695228838,
-39.8261863261265));
#260110=CARTESIAN_POINT('Ctrl Pts',(-44.2297857112555,-59.4562815511248,
-39.8189049612177));
#260111=CARTESIAN_POINT('Ctrl Pts',(-44.1653821501578,-59.4461645800485,
-39.804117860165));
#260112=CARTESIAN_POINT('Ctrl Pts',(-44.1334098533119,-59.4403358965057,
-39.796611904146));
#260113=CARTESIAN_POINT('Ctrl Pts',(-44.0381705489761,-59.4205767439822,
-39.7737606900069));
#260114=CARTESIAN_POINT('Ctrl Pts',(-43.9755797867482,-59.404377678535,
-39.758082736235));
#260115=CARTESIAN_POINT('Ctrl Pts',(-43.8521844802478,-59.3659924501046,
-39.7258408213904));
#260116=CARTESIAN_POINT('Ctrl Pts',(-43.7913710156582,-59.3437986068227,
-39.7092735270162));
#260117=CARTESIAN_POINT('Ctrl Pts',(-43.7165133999419,-59.3122676347018,
-39.6880047470813));
#260118=CARTESIAN_POINT('Ctrl Pts',(-43.7015909540668,-59.3057650997492,
-39.6837198263607));
#260119=CARTESIAN_POINT('Ctrl Pts',(-43.6718792626187,-59.2923855152665,
-39.6750982166404));
#260120=CARTESIAN_POINT('Ctrl Pts',(-43.6570605877876,-59.2854933075233,
-39.6707525906888));
#260121=CARTESIAN_POINT('Ctrl Pts',(-43.6129438349825,-59.2643127642054,
-39.657677343482));
#260122=CARTESIAN_POINT('Ctrl Pts',(-43.5840313825064,-59.2495482316173,
-39.6489242250709));
#260123=CARTESIAN_POINT('Ctrl Pts',(-43.5555683529588,-59.2341345733972,
-39.6401237339649));
#260124=CARTESIAN_POINT('',(-45.6739227569384,-55.519263759503,-38.9124165664198));
#260125=CARTESIAN_POINT('',(-45.6739227548714,-55.5192637629146,-38.912416567246));
#260126=CARTESIAN_POINT('',(-43.4805771074159,-59.5712767529304,-39.2399080357012));
#260127=CARTESIAN_POINT('Ctrl Pts',(-45.6739227574752,-55.5192637582493,
-38.9124165669282));
#260128=CARTESIAN_POINT('Ctrl Pts',(-45.7067749877369,-55.5369855856676,
-38.9214216121435));
#260129=CARTESIAN_POINT('Ctrl Pts',(-45.7392219877795,-55.5555212114618,
-38.9304915704334));
#260130=CARTESIAN_POINT('Ctrl Pts',(-45.8033556832395,-55.5942722159849,
-38.9487787872477));
#260131=CARTESIAN_POINT('Ctrl Pts',(-45.8348443691401,-55.6143675312756,
-38.9579395118016));
#260132=CARTESIAN_POINT('Ctrl Pts',(-45.9274099842789,-55.6766589025305,
-38.9854159162722));
#260133=CARTESIAN_POINT('Ctrl Pts',(-45.9867610865919,-55.7209353156014,
-39.0037703637879));
#260134=CARTESIAN_POINT('Ctrl Pts',(-46.1007337830098,-55.8148102393793,
-39.0405190865864));
#260135=CARTESIAN_POINT('Ctrl Pts',(-46.155375425224,-55.8644173763685,
-39.0589184916404));
#260136=CARTESIAN_POINT('Ctrl Pts',(-46.2338037269528,-55.9428521307486,
-39.0865551957989));
#260137=CARTESIAN_POINT('Ctrl Pts',(-46.259356574729,-55.9696687352924,
-39.0957737179551));
#260138=CARTESIAN_POINT('Ctrl Pts',(-46.309266807939,-56.024663053365,-39.1142236413887));
#260139=CARTESIAN_POINT('Ctrl Pts',(-46.3336138177017,-56.0528284109483,
-39.1234510495426));
#260140=CARTESIAN_POINT('Ctrl Pts',(-46.3692509284248,-56.0961546965834,
-39.1373141736981));
#260141=CARTESIAN_POINT('Ctrl Pts',(-46.3809719555493,-56.1107655250657,
-39.14193505412));
#260142=CARTESIAN_POINT('Ctrl Pts',(-46.4039850968433,-56.1401806715041,
-39.1511314768264));
#260143=CARTESIAN_POINT('Ctrl Pts',(-46.4153001903629,-56.1550126624777,
-39.1557159133814));
#260144=CARTESIAN_POINT('Ctrl Pts',(-46.4486370096884,-56.1998310060262,
-39.1694131182658));
#260145=CARTESIAN_POINT('Ctrl Pts',(-46.4700835091466,-56.2301795317326,
-39.1784826054425));
#260146=CARTESIAN_POINT('Ctrl Pts',(-46.5320719136859,-56.3225583984772,
-39.2054898733524));
#260147=CARTESIAN_POINT('Ctrl Pts',(-46.5703035947222,-56.3859631579321,
-39.2232408562602));
#260148=CARTESIAN_POINT('Ctrl Pts',(-46.6230137301682,-56.4837650915426,
-39.2494851373609));
#260149=CARTESIAN_POINT('Ctrl Pts',(-46.6398105780351,-56.5168167317113,
-39.2581698041384));
#260150=CARTESIAN_POINT('Ctrl Pts',(-46.6718446885168,-56.5838294931519,
-39.2754119185794));
#260151=CARTESIAN_POINT('Ctrl Pts',(-46.6870820302515,-56.617790568625,
-39.2839693714534));
#260152=CARTESIAN_POINT('Ctrl Pts',(-46.7159729830272,-56.6866360545619,
-39.3009558869148));
#260153=CARTESIAN_POINT('Ctrl Pts',(-46.7296188023799,-56.7214992889704,
-39.3093799218186));
#260154=CARTESIAN_POINT('Ctrl Pts',(-46.7553216997642,-56.7922546384013,
-39.3261176641085));
#260155=CARTESIAN_POINT('Ctrl Pts',(-46.7672996943011,-56.8279354881579,
-39.3343809787628));
#260156=CARTESIAN_POINT('Ctrl Pts',(-46.8004530502947,-56.9353633959568,
-39.358737163018));
#260157=CARTESIAN_POINT('Ctrl Pts',(-46.8189795501832,-57.0077635587999,
-39.3744658121213));
#260158=CARTESIAN_POINT('Ctrl Pts',(-46.848916211803,-57.1540080946302,
-39.4048998290393));
#260159=CARTESIAN_POINT('Ctrl Pts',(-46.8603369445408,-57.2278698672909,
-39.4196100581687));
#260160=CARTESIAN_POINT('Ctrl Pts',(-46.8720664744741,-57.3397812895282,
-39.4409093640372));
#260161=CARTESIAN_POINT('Ctrl Pts',(-46.875074749658,-57.3772756893033,
-39.4478819384746));
#260162=CARTESIAN_POINT('Ctrl Pts',(-46.8792542953452,-57.4526370309597,
-39.4615663943076));
#260163=CARTESIAN_POINT('Ctrl Pts',(-46.8804258736835,-57.4905390832846,
-39.4682843608713));
#260164=CARTESIAN_POINT('Ctrl Pts',(-46.8808837743635,-57.5666104373409,
-39.4814341960201));
#260165=CARTESIAN_POINT('Ctrl Pts',(-46.8801708637706,-57.604491394965,
-39.4878166677226));
#260166=CARTESIAN_POINT('Ctrl Pts',(-46.8768913879562,-57.6800597985945,
-39.5002231148134));
#260167=CARTESIAN_POINT('Ctrl Pts',(-46.8743246637802,-57.7177284992744,
-39.5062438407196));
#260168=CARTESIAN_POINT('Ctrl Pts',(-46.863867568228,-57.8303908432586,
-39.5237649596504));
#260169=CARTESIAN_POINT('Ctrl Pts',(-46.8532263654434,-57.9050414873811,
-39.5347254895779));
#260170=CARTESIAN_POINT('Ctrl Pts',(-46.8317335315027,-58.0163268447592,
-39.5500873410526));
#260171=CARTESIAN_POINT('Ctrl Pts',(-46.8236459543104,-58.0533066811291,
-39.5550278422771));
#260172=CARTESIAN_POINT('Ctrl Pts',(-46.8055990109883,-58.1270324939451,
-39.5645447403379));
#260173=CARTESIAN_POINT('Ctrl Pts',(-46.7956339676918,-58.1637938532181,
-39.5691227921436));
#260174=CARTESIAN_POINT('Ctrl Pts',(-46.7738161327052,-58.2370162077018,
-39.5779016468881));
#260175=CARTESIAN_POINT('Ctrl Pts',(-46.7619036278491,-58.2736352268715,
-39.5821192203466));
#260176=CARTESIAN_POINT('Ctrl Pts',(-46.7364059718256,-58.3458255995332,
-39.5900871854462));
#260177=CARTESIAN_POINT('Ctrl Pts',(-46.7227943874693,-58.3815079294473,
-39.593852026583));
#260178=CARTESIAN_POINT('Ctrl Pts',(-46.6938810604275,-58.4520118571144,
-39.6009443874688));
#260179=CARTESIAN_POINT('Ctrl Pts',(-46.6785776252269,-58.4868413763864,
-39.6042729713841));
#260180=CARTESIAN_POINT('Ctrl Pts',(-46.6462897337504,-58.5556617200885,
-39.6104989383907));
#260181=CARTESIAN_POINT('Ctrl Pts',(-46.629305264578,-58.5896525381261,
-39.6133963175589));
#260182=CARTESIAN_POINT('Ctrl Pts',(-46.5936553532051,-58.6567954587996,
-39.6187605717742));
#260183=CARTESIAN_POINT('Ctrl Pts',(-46.5749899237926,-58.6899475678396,
-39.6212274496765));
#260184=CARTESIAN_POINT('Ctrl Pts',(-46.5359657438849,-58.7554068733743,
-39.6257281334421));
#260185=CARTESIAN_POINT('Ctrl Pts',(-46.515607032986,-58.7877140896313,
-39.6277619492082));
#260186=CARTESIAN_POINT('Ctrl Pts',(-46.4731710833873,-58.8514710047945,
-39.6313905635194));
#260187=CARTESIAN_POINT('Ctrl Pts',(-46.4511086137466,-58.8829006319494,
-39.6329844599904));
#260188=CARTESIAN_POINT('Ctrl Pts',(-46.4051673201273,-58.9449633016888,
-39.6357273485653));
#260189=CARTESIAN_POINT('Ctrl Pts',(-46.381447994276,-58.975377588932,-39.6368662598532));
#260190=CARTESIAN_POINT('Ctrl Pts',(-46.3084068909562,-59.0643493136613,
-39.639576123369));
#260191=CARTESIAN_POINT('Ctrl Pts',(-46.2570407846103,-59.1209150453975,
-39.6404603784326));
#260192=CARTESIAN_POINT('Ctrl Pts',(-46.1491379755941,-59.228544463199,
-39.6404138814247));
#260193=CARTESIAN_POINT('Ctrl Pts',(-46.0925836555154,-59.2796343044913,
-39.6394845811683));
#260194=CARTESIAN_POINT('Ctrl Pts',(-46.003852943763,-59.3521266125548,
-39.6367223387528));
#260195=CARTESIAN_POINT('Ctrl Pts',(-45.9736068078661,-59.3756113554054,
-39.6355721163029));
#260196=CARTESIAN_POINT('Ctrl Pts',(-45.9272656961273,-59.4097723546528,
-39.6334997725088));
#260197=CARTESIAN_POINT('Ctrl Pts',(-45.9116419215573,-59.4209912820171,
-39.6327502808957));
#260198=CARTESIAN_POINT('Ctrl Pts',(-45.8800804794677,-59.4430610802668,
-39.6311351339295));
#260199=CARTESIAN_POINT('Ctrl Pts',(-45.8641077773929,-59.4539347618601,
-39.6302673980329));
#260200=CARTESIAN_POINT('Ctrl Pts',(-45.8159067176779,-59.4858696807562,
-39.6274990247155));
#260201=CARTESIAN_POINT('Ctrl Pts',(-45.7834097108732,-59.5062438963941,
-39.6254355071979));
#260202=CARTESIAN_POINT('Ctrl Pts',(-45.717633106262,-59.5452481912826,
-39.6208773262667));
#260203=CARTESIAN_POINT('Ctrl Pts',(-45.6843658495255,-59.5638704323978,
-39.6183834291471));
#260204=CARTESIAN_POINT('Ctrl Pts',(-45.5834449288538,-59.6171384125673,
-39.6102664280093));
#260205=CARTESIAN_POINT('Ctrl Pts',(-45.5146744626452,-59.6491908713697,
-39.6040093949256));
#260206=CARTESIAN_POINT('Ctrl Pts',(-45.409303365533,-59.6921244665012,
-39.5933617316812));
#260207=CARTESIAN_POINT('Ctrl Pts',(-45.3738098009101,-59.7055766782111,
-39.5896017905935));
#260208=CARTESIAN_POINT('Ctrl Pts',(-45.3020778813705,-59.7307512119864,
-39.5816566825671));
#260209=CARTESIAN_POINT('Ctrl Pts',(-45.2658207311094,-59.7424779859238,
-39.5774690651077));
#260210=CARTESIAN_POINT('Ctrl Pts',(-45.1926264675053,-59.7641596016776,
-39.5686715125846));
#260211=CARTESIAN_POINT('Ctrl Pts',(-45.1555073907618,-59.7741562512685,
-39.5640376159893));
#260212=CARTESIAN_POINT('Ctrl Pts',(-45.0812568479429,-59.7921790564438,
-39.5544265698906));
#260213=CARTESIAN_POINT('Ctrl Pts',(-45.04408172978,-59.8002277891036,-39.5494458391365));
#260214=CARTESIAN_POINT('Ctrl Pts',(-44.9696261062542,-59.8144410677077,
-39.5391390505826));
#260215=CARTESIAN_POINT('Ctrl Pts',(-44.9323469822025,-59.8206061841119,
-39.5338133285981));
#260216=CARTESIAN_POINT('Ctrl Pts',(-44.8576879123993,-59.8310833805954,
-39.5228216573624));
#260217=CARTESIAN_POINT('Ctrl Pts',(-44.8203079610257,-59.8353953605365,
-39.5171556909205));
#260218=CARTESIAN_POINT('Ctrl Pts',(-44.7080184564225,-59.8455760612674,
-39.4996502778007));
#260219=CARTESIAN_POINT('Ctrl Pts',(-44.6329372249224,-59.8486931621852,
-39.4873001861445));
#260220=CARTESIAN_POINT('Ctrl Pts',(-44.5200834441659,-59.8478515133141,
-39.4677634802869));
#260221=CARTESIAN_POINT('Ctrl Pts',(-44.4823810871712,-59.8466449718289,
-39.4610736497973));
#260222=CARTESIAN_POINT('Ctrl Pts',(-44.4258051079382,-59.8434394706745,
-39.4507883432074));
#260223=CARTESIAN_POINT('Ctrl Pts',(-44.4069254589855,-59.8421361346926,
-39.4473147915973));
#260224=CARTESIAN_POINT('Ctrl Pts',(-44.3691376542581,-59.8390581625153,
-39.4402793331445));
#260225=CARTESIAN_POINT('Ctrl Pts',(-44.3502459350849,-59.8372838734483,
-39.4367203104461));
#260226=CARTESIAN_POINT('Ctrl Pts',(-44.2938476169342,-59.8312836889756,
-39.4259706278629));
#260227=CARTESIAN_POINT('Ctrl Pts',(-44.2565162762141,-59.8263768596807,
-39.4186892629542));
#260228=CARTESIAN_POINT('Ctrl Pts',(-44.1823865424055,-59.8147890207299,
-39.4039021619013));
#260229=CARTESIAN_POINT('Ctrl Pts',(-44.14558648486,-59.8081083758143,-39.3963962058824));
#260230=CARTESIAN_POINT('Ctrl Pts',(-44.0359682134124,-59.785449432176,
-39.3735449917432));
#260231=CARTESIAN_POINT('Ctrl Pts',(-43.9639303529155,-59.7668593120831,
-39.3578670379715));
#260232=CARTESIAN_POINT('Ctrl Pts',(-43.8219159040518,-59.7227861654644,
-39.3256251231267));
#260233=CARTESIAN_POINT('Ctrl Pts',(-43.7519290534068,-59.6972943066161,
-39.3090578287532));
#260234=CARTESIAN_POINT('Ctrl Pts',(-43.665783177736,-59.6610675807532,
-39.2877890488175));
#260235=CARTESIAN_POINT('Ctrl Pts',(-43.6486106666635,-59.653596197985,
-39.2835041280971));
#260236=CARTESIAN_POINT('Ctrl Pts',(-43.6144193015917,-59.6382222359849,
-39.2748825183767));
#260237=CARTESIAN_POINT('Ctrl Pts',(-43.597366582891,-59.6303022352814,
-39.2705368924251));
#260238=CARTESIAN_POINT('Ctrl Pts',(-43.5465994182958,-59.6059619032979,
-39.2574616452183));
#260239=CARTESIAN_POINT('Ctrl Pts',(-43.5133293006631,-59.588993111175,
-39.2487085268073));
#260240=CARTESIAN_POINT('Ctrl Pts',(-43.4805771074159,-59.5712767529304,
-39.2399080357012));
#260241=CARTESIAN_POINT('',(-43.5555682511181,-59.2341350312479,-39.6401231904583));
#260242=CARTESIAN_POINT('',(-43.4805771074159,-59.5712767529304,-39.2399080357012));
#260243=CARTESIAN_POINT('Ctrl Pts',(-44.6028144607067,-59.4732023778567,
-39.8960586142665));
#260244=CARTESIAN_POINT('Ctrl Pts',(-44.5657362830796,-59.4749625407307,
-39.8890876965807));
#260245=CARTESIAN_POINT('Ctrl Pts',(-44.5286093371808,-59.4756901946432,
-39.8818983399833));
#260246=CARTESIAN_POINT('Ctrl Pts',(-44.4914381955716,-59.4753842969682,
-39.8744908703297));
#260247=CARTESIAN_POINT('Ctrl Pts',(-44.4587593954789,-59.4751153687477,
-39.8679786350438));
#260248=CARTESIAN_POINT('Ctrl Pts',(-44.4260066787541,-59.4740418999023,
-39.8612888045543));
#260249=CARTESIAN_POINT('Ctrl Pts',(-44.3932403868445,-59.4721600534981,
-39.8544319334943));
#260250=CARTESIAN_POINT('Ctrl Pts',(-44.3768572408897,-59.4712191302959,
-39.8510034979643));
#260251=CARTESIAN_POINT('Ctrl Pts',(-44.36045571594,-59.4700741717846,-39.8475299463542));
#260252=CARTESIAN_POINT('Ctrl Pts',(-44.3440416625521,-59.468724474598,
-39.8440122171279));
#260253=CARTESIAN_POINT('Ctrl Pts',(-44.3276276091642,-59.4673747774113,
-39.8404944879015));
#260254=CARTESIAN_POINT('Ctrl Pts',(-44.3112153059959,-59.4658206541325,
-39.8369354652031));
#260255=CARTESIAN_POINT('Ctrl Pts',(-44.2948830253781,-59.4640704448638,
-39.8333522376753));
#260256=CARTESIAN_POINT('Ctrl Pts',(-44.2622183820993,-59.4605700175345,
-39.8261857646199));
#260257=CARTESIAN_POINT('Ctrl Pts',(-44.2297857475685,-59.4562820537288,
-39.8189044177111));
#260258=CARTESIAN_POINT('Ctrl Pts',(-44.1975839604555,-59.4512235680695,
-39.8115108662318));
#260259=CARTESIAN_POINT('Ctrl Pts',(-44.1653823351036,-59.4461651078207,
-39.804117351893));
#260260=CARTESIAN_POINT('Ctrl Pts',(-44.1334101092193,-59.4403364490933,
-39.7966114142227));
#260261=CARTESIAN_POINT('Ctrl Pts',(-44.1016634287012,-59.4337500174524,
-39.7889942816371));
#260262=CARTESIAN_POINT('Ctrl Pts',(-44.0381699081893,-59.4205771210844,
-39.7737599782022));
#260263=CARTESIAN_POINT('Ctrl Pts',(-43.9755797709279,-59.4043781707976,
-39.7580821927283));
#260264=CARTESIAN_POINT('Ctrl Pts',(-43.913882105035,-59.3851855527201,
-39.741961235306));
#260265=CARTESIAN_POINT('Ctrl Pts',(-43.8521844391421,-59.3659929346427,
-39.7258402778837));
#260266=CARTESIAN_POINT('Ctrl Pts',(-43.7913709620947,-59.343799086882,
-39.7092729835095));
#260267=CARTESIAN_POINT('Ctrl Pts',(-43.7314848572577,-59.3185743040837,
-39.6922579595616));
#260268=CARTESIAN_POINT('Ctrl Pts',(-43.7165133310485,-59.3122681083841,
-39.6880042035746));
#260269=CARTESIAN_POINT('Ctrl Pts',(-43.7015908821177,-59.3057655721158,
-39.6837192828541));
#260270=CARTESIAN_POINT('Ctrl Pts',(-43.6867350333519,-59.2990757785203,
-39.6794084779939));
#260271=CARTESIAN_POINT('Ctrl Pts',(-43.671879184586,-59.2923859849247,
-39.6750976731337));
#260272=CARTESIAN_POINT('Ctrl Pts',(-43.657060506721,-59.2854937757857,
-39.6707520471821));
#260273=CARTESIAN_POINT('Ctrl Pts',(-43.6423549194422,-59.2784335932494,
-39.6663936314465));
#260274=CARTESIAN_POINT('Ctrl Pts',(-43.6129437448845,-59.2643132281768,
-39.6576767999753));
#260275=CARTESIAN_POINT('Ctrl Pts',(-43.5840312864905,-59.2495486925951,
-39.6489236815642));
#260276=CARTESIAN_POINT('Ctrl Pts',(-43.5555682511181,-59.2341350312479,
-39.6401231904583));
#260277=CARTESIAN_POINT('Origin',(-44.5079524583207,-57.4754524783487,-52.920575));
#260278=CARTESIAN_POINT('Ctrl Pts',(-44.5079524583208,-55.8067071952963,
-52.4912));
#260279=CARTESIAN_POINT('Ctrl Pts',(-45.4714029967,-55.8067071952963,-52.4328666666667));
#260280=CARTESIAN_POINT('Ctrl Pts',(-45.9531282658897,-56.6410798368225,
-52.3745333333334));
#260281=CARTESIAN_POINT('Ctrl Pts',(-46.4348535350793,-57.4754524783487,
-52.3162000000001));
#260282=CARTESIAN_POINT('Ctrl Pts',(-45.9531282658897,-58.309825119875,
-52.2578666666667));
#260283=CARTESIAN_POINT('Ctrl Pts',(-45.4714029967,-59.1441977614012,-52.1995333333334));
#260284=CARTESIAN_POINT('Ctrl Pts',(-44.5079524583208,-59.1441977614012,
-52.1412));
#260285=CARTESIAN_POINT('Ctrl Pts',(-43.5445019199415,-59.1441977614012,
-52.0828666666667));
#260286=CARTESIAN_POINT('Ctrl Pts',(-43.0627766507519,-58.309825119875,
-52.0245333333333));
#260287=CARTESIAN_POINT('Ctrl Pts',(-42.5810513815623,-57.4754524783487,
-51.9662));
#260288=CARTESIAN_POINT('Ctrl Pts',(-43.0627766507519,-56.6410798368225,
-51.9078666666667));
#260289=CARTESIAN_POINT('Ctrl Pts',(-43.5445019199415,-55.8067071952963,
-51.8495333333334));
#260290=CARTESIAN_POINT('Ctrl Pts',(-44.5079524583208,-55.8067071952963,
-51.7912));
#260291=CARTESIAN_POINT('Ctrl Pts',(-44.5079524583208,-55.8067071952963,
-52.64995));
#260292=CARTESIAN_POINT('Ctrl Pts',(-45.4714029967001,-55.8067071952964,
-52.5916166666668));
#260293=CARTESIAN_POINT('Ctrl Pts',(-45.9531282658897,-56.6410798368225,
-52.5332833333334));
#260294=CARTESIAN_POINT('Ctrl Pts',(-46.4348535350793,-57.4754524783487,
-52.4749500000001));
#260295=CARTESIAN_POINT('Ctrl Pts',(-45.9531282658897,-58.309825119875,
-52.4166166666667));
#260296=CARTESIAN_POINT('Ctrl Pts',(-45.4714029967,-59.1441977614012,-52.3582833333334));
#260297=CARTESIAN_POINT('Ctrl Pts',(-44.5079524583208,-59.1441977614012,
-52.29995));
#260298=CARTESIAN_POINT('Ctrl Pts',(-43.5445019199415,-59.1441977614012,
-52.2416166666667));
#260299=CARTESIAN_POINT('Ctrl Pts',(-43.0627766507519,-58.309825119875,
-52.1832833333333));
#260300=CARTESIAN_POINT('Ctrl Pts',(-42.5810513815623,-57.4754524783487,
-52.12495));
#260301=CARTESIAN_POINT('Ctrl Pts',(-43.0627766507519,-56.6410798368225,
-52.0666166666667));
#260302=CARTESIAN_POINT('Ctrl Pts',(-43.5445019199415,-55.8067071952963,
-52.0082833333333));
#260303=CARTESIAN_POINT('Ctrl Pts',(-44.5079524583208,-55.8067071952963,
-51.94995));
#260304=CARTESIAN_POINT('Ctrl Pts',(-44.5079524583208,-59.5441932447742,
-52.6102625));
#260305=CARTESIAN_POINT('Ctrl Pts',(-43.3135644199415,-59.5441932447742,
-52.5519291666666));
#260306=CARTESIAN_POINT('Ctrl Pts',(-42.7163704007519,-58.5098228615615,
-52.4935958333333));
#260307=CARTESIAN_POINT('Ctrl Pts',(-42.1191763815623,-57.4754524783487,
-52.4352625000001));
#260308=CARTESIAN_POINT('Ctrl Pts',(-42.7163704007519,-56.4410820951361,
-52.3769291666667));
#260309=CARTESIAN_POINT('Ctrl Pts',(-43.3135644199415,-55.4067117119233,
-52.3185958333334));
#260310=CARTESIAN_POINT('Ctrl Pts',(-44.5079524583208,-55.4067117119234,
-52.2602625));
#260311=CARTESIAN_POINT('Ctrl Pts',(-45.7023404967,-55.4067117119233,-52.2019291666667));
#260312=CARTESIAN_POINT('Ctrl Pts',(-46.2995345158897,-56.4410820951361,
-52.1435958333333));
#260313=CARTESIAN_POINT('Ctrl Pts',(-46.8967285350793,-57.4754524783487,
-52.0852625));
#260314=CARTESIAN_POINT('Ctrl Pts',(-46.2995345158897,-58.5098228615615,
-52.0269291666667));
#260315=CARTESIAN_POINT('Ctrl Pts',(-45.7023404967,-59.5441932447742,-51.9685958333333));
#260316=CARTESIAN_POINT('Ctrl Pts',(-44.5079524583208,-59.5441932447742,
-51.9102625));
#260317=CARTESIAN_POINT('Ctrl Pts',(-43.3135644199415,-59.5441932447742,
-51.8519291666667));
#260318=CARTESIAN_POINT('Ctrl Pts',(-42.7163704007519,-58.5098228615615,
-51.7935958333333));
#260319=CARTESIAN_POINT('Ctrl Pts',(-42.1191763815623,-57.4754524783487,
-51.7352625));
#260320=CARTESIAN_POINT('Ctrl Pts',(-42.7163704007519,-56.4410820951361,
-51.6769291666667));
#260321=CARTESIAN_POINT('Ctrl Pts',(-43.3135644199415,-55.4067117119233,
-51.6185958333333));
#260322=CARTESIAN_POINT('Ctrl Pts',(-44.5079524583208,-55.4067117119234,
-51.5602625));
#260323=CARTESIAN_POINT('Ctrl Pts',(-45.7023404967,-55.4067117119233,-51.5019291666666));
#260324=CARTESIAN_POINT('Ctrl Pts',(-46.2995345158897,-56.4410820951361,
-51.4435958333333));
#260325=CARTESIAN_POINT('Ctrl Pts',(-46.8967285350793,-57.4754524783487,
-51.3852625));
#260326=CARTESIAN_POINT('Ctrl Pts',(-46.2995345158897,-58.5098228615615,
-51.3269291666667));
#260327=CARTESIAN_POINT('Ctrl Pts',(-45.7023404967,-59.5441932447742,-51.2685958333333));
#260328=CARTESIAN_POINT('Ctrl Pts',(-44.5079524583208,-59.5441932447742,
-51.2102625));
#260329=CARTESIAN_POINT('Ctrl Pts',(-43.3135644199415,-59.5441932447742,
-51.1519291666666));
#260330=CARTESIAN_POINT('Ctrl Pts',(-42.7163704007519,-58.5098228615615,
-51.0935958333334));
#260331=CARTESIAN_POINT('Ctrl Pts',(-42.1191763815623,-57.4754524783487,
-51.0352625));
#260332=CARTESIAN_POINT('Ctrl Pts',(-42.7163704007519,-56.4410820951361,
-50.9769291666667));
#260333=CARTESIAN_POINT('Ctrl Pts',(-43.3135644199415,-55.4067117119233,
-50.9185958333333));
#260334=CARTESIAN_POINT('Ctrl Pts',(-44.5079524583208,-55.4067117119234,
-50.8602625));
#260335=CARTESIAN_POINT('Ctrl Pts',(-45.7023404967,-55.4067117119233,-50.8019291666667));
#260336=CARTESIAN_POINT('Ctrl Pts',(-46.2995345158897,-56.4410820951361,
-50.7435958333333));
#260337=CARTESIAN_POINT('Ctrl Pts',(-46.8967285350793,-57.4754524783487,
-50.6852625));
#260338=CARTESIAN_POINT('Ctrl Pts',(-46.2995345158897,-58.5098228615615,
-50.6269291666667));
#260339=CARTESIAN_POINT('Ctrl Pts',(-45.7023404967,-59.5441932447742,-50.5685958333333));
#260340=CARTESIAN_POINT('Ctrl Pts',(-44.5079524583208,-59.5441932447742,
-50.5102625));
#260341=CARTESIAN_POINT('Ctrl Pts',(-43.3135644199415,-59.5441932447742,
-50.4519291666667));
#260342=CARTESIAN_POINT('Ctrl Pts',(-42.7163704007519,-58.5098228615615,
-50.3935958333333));
#260343=CARTESIAN_POINT('Ctrl Pts',(-42.1191763815623,-57.4754524783487,
-50.3352625));
#260344=CARTESIAN_POINT('Ctrl Pts',(-42.7163704007519,-56.4410820951361,
-50.2769291666667));
#260345=CARTESIAN_POINT('Ctrl Pts',(-43.3135644199415,-55.4067117119233,
-50.2185958333333));
#260346=CARTESIAN_POINT('Ctrl Pts',(-44.5079524583208,-55.4067117119234,
-50.1602625));
#260347=CARTESIAN_POINT('Ctrl Pts',(-45.7023404967,-55.4067117119233,-50.1019291666667));
#260348=CARTESIAN_POINT('Ctrl Pts',(-46.2995345158897,-56.4410820951361,
-50.0435958333333));
#260349=CARTESIAN_POINT('Ctrl Pts',(-46.8967285350793,-57.4754524783487,
-49.9852625));
#260350=CARTESIAN_POINT('Ctrl Pts',(-46.2995345158897,-58.5098228615615,
-49.9269291666667));
#260351=CARTESIAN_POINT('Ctrl Pts',(-45.7023404967,-59.5441932447742,-49.8685958333333));
#260352=CARTESIAN_POINT('Ctrl Pts',(-44.5079524583208,-59.5441932447742,
-49.8102625));
#260353=CARTESIAN_POINT('Ctrl Pts',(-43.3135644199415,-59.5441932447742,
-49.7519291666667));
#260354=CARTESIAN_POINT('Ctrl Pts',(-42.7163704007519,-58.5098228615615,
-49.6935958333334));
#260355=CARTESIAN_POINT('Ctrl Pts',(-42.1191763815623,-57.4754524783487,
-49.6352625));
#260356=CARTESIAN_POINT('Ctrl Pts',(-42.7163704007519,-56.4410820951361,
-49.5769291666667));
#260357=CARTESIAN_POINT('Ctrl Pts',(-43.3135644199415,-55.4067117119233,
-49.5185958333334));
#260358=CARTESIAN_POINT('Ctrl Pts',(-44.5079524583208,-55.4067117119234,
-49.4602625));
#260359=CARTESIAN_POINT('Ctrl Pts',(-45.7023404967,-55.4067117119233,-49.4019291666667));
#260360=CARTESIAN_POINT('Ctrl Pts',(-46.2995345158897,-56.4410820951361,
-49.3435958333333));
#260361=CARTESIAN_POINT('Ctrl Pts',(-46.8967285350793,-57.4754524783487,
-49.2852625));
#260362=CARTESIAN_POINT('Ctrl Pts',(-46.2995345158897,-58.5098228615615,
-49.2269291666667));
#260363=CARTESIAN_POINT('Ctrl Pts',(-45.7023404967,-59.5441932447742,-49.1685958333334));
#260364=CARTESIAN_POINT('Ctrl Pts',(-44.5079524583208,-59.5441932447742,
-49.1102625));
#260365=CARTESIAN_POINT('Ctrl Pts',(-43.3135644199415,-59.5441932447742,
-49.0519291666667));
#260366=CARTESIAN_POINT('Ctrl Pts',(-42.7163704007519,-58.5098228615615,
-48.9935958333333));
#260367=CARTESIAN_POINT('Ctrl Pts',(-42.1191763815623,-57.4754524783487,
-48.9352625));
#260368=CARTESIAN_POINT('Ctrl Pts',(-42.7163704007519,-56.4410820951361,
-48.8769291666667));
#260369=CARTESIAN_POINT('Ctrl Pts',(-43.3135644199415,-55.4067117119233,
-48.8185958333334));
#260370=CARTESIAN_POINT('Ctrl Pts',(-44.5079524583208,-55.4067117119234,
-48.7602625));
#260371=CARTESIAN_POINT('Ctrl Pts',(-45.7023404967,-55.4067117119233,-48.7019291666667));
#260372=CARTESIAN_POINT('Ctrl Pts',(-46.2995345158897,-56.4410820951361,
-48.6435958333333));
#260373=CARTESIAN_POINT('Ctrl Pts',(-46.8967285350793,-57.4754524783487,
-48.5852625));
#260374=CARTESIAN_POINT('Ctrl Pts',(-46.2995345158897,-58.5098228615615,
-48.5269291666667));
#260375=CARTESIAN_POINT('Ctrl Pts',(-45.7023404967,-59.5441932447742,-48.4685958333333));
#260376=CARTESIAN_POINT('Ctrl Pts',(-44.5079524583208,-59.5441932447742,
-48.4102625));
#260377=CARTESIAN_POINT('Ctrl Pts',(-43.3135644199415,-59.5441932447742,
-48.3519291666667));
#260378=CARTESIAN_POINT('Ctrl Pts',(-42.7163704007519,-58.5098228615615,
-48.2935958333334));
#260379=CARTESIAN_POINT('Ctrl Pts',(-42.1191763815623,-57.4754524783487,
-48.2352625));
#260380=CARTESIAN_POINT('Ctrl Pts',(-42.7163704007519,-56.4410820951361,
-48.1769291666667));
#260381=CARTESIAN_POINT('Ctrl Pts',(-43.3135644199415,-55.4067117119233,
-48.1185958333334));
#260382=CARTESIAN_POINT('Ctrl Pts',(-44.5079524583208,-55.4067117119234,
-48.0602625));
#260383=CARTESIAN_POINT('Ctrl Pts',(-45.7023404967,-55.4067117119233,-48.0019291666667));
#260384=CARTESIAN_POINT('Ctrl Pts',(-46.2995345158897,-56.4410820951361,
-47.9435958333334));
#260385=CARTESIAN_POINT('Ctrl Pts',(-46.8967285350793,-57.4754524783487,
-47.8852625));
#260386=CARTESIAN_POINT('Ctrl Pts',(-46.2995345158897,-58.5098228615615,
-47.8269291666667));
#260387=CARTESIAN_POINT('Ctrl Pts',(-45.7023404967,-59.5441932447742,-47.7685958333333));
#260388=CARTESIAN_POINT('Ctrl Pts',(-44.5079524583208,-59.5441932447742,
-47.7102625));
#260389=CARTESIAN_POINT('Ctrl Pts',(-43.3135644199415,-59.5441932447742,
-47.6519291666667));
#260390=CARTESIAN_POINT('Ctrl Pts',(-42.7163704007519,-58.5098228615615,
-47.5935958333333));
#260391=CARTESIAN_POINT('Ctrl Pts',(-42.1191763815623,-57.4754524783487,
-47.5352625));
#260392=CARTESIAN_POINT('Ctrl Pts',(-42.7163704007519,-56.4410820951361,
-47.4769291666667));
#260393=CARTESIAN_POINT('Ctrl Pts',(-43.3135644199415,-55.4067117119233,
-47.4185958333333));
#260394=CARTESIAN_POINT('Ctrl Pts',(-44.5079524583208,-55.4067117119234,
-47.3602625));
#260395=CARTESIAN_POINT('Ctrl Pts',(-45.7023404967,-55.4067117119233,-47.3019291666666));
#260396=CARTESIAN_POINT('Ctrl Pts',(-46.2995345158897,-56.4410820951361,
-47.2435958333334));
#260397=CARTESIAN_POINT('Ctrl Pts',(-46.8967285350793,-57.4754524783487,
-47.1852625));
#260398=CARTESIAN_POINT('Ctrl Pts',(-46.2995345158897,-58.5098228615615,
-47.1269291666667));
#260399=CARTESIAN_POINT('Ctrl Pts',(-45.7023404967,-59.5441932447742,-47.0685958333333));
#260400=CARTESIAN_POINT('Ctrl Pts',(-44.5079524583208,-59.5441932447742,
-47.0102625));
#260401=CARTESIAN_POINT('Ctrl Pts',(-43.3135644199415,-59.5441932447742,
-46.9519291666667));
#260402=CARTESIAN_POINT('Ctrl Pts',(-42.7163704007519,-58.5098228615615,
-46.8935958333333));
#260403=CARTESIAN_POINT('Ctrl Pts',(-42.1191763815623,-57.4754524783487,
-46.8352625));
#260404=CARTESIAN_POINT('Ctrl Pts',(-42.7163704007519,-56.4410820951361,
-46.7769291666667));
#260405=CARTESIAN_POINT('Ctrl Pts',(-43.3135644199415,-55.4067117119233,
-46.7185958333333));
#260406=CARTESIAN_POINT('Ctrl Pts',(-44.5079524583208,-55.4067117119234,
-46.6602625));
#260407=CARTESIAN_POINT('Ctrl Pts',(-45.7023404967,-55.4067117119233,-46.6019291666667));
#260408=CARTESIAN_POINT('Ctrl Pts',(-46.2995345158897,-56.4410820951361,
-46.5435958333334));
#260409=CARTESIAN_POINT('Ctrl Pts',(-46.8967285350793,-57.4754524783487,
-46.4852625));
#260410=CARTESIAN_POINT('Ctrl Pts',(-46.2995345158897,-58.5098228615615,
-46.4269291666667));
#260411=CARTESIAN_POINT('Ctrl Pts',(-45.7023404967,-59.5441932447742,-46.3685958333333));
#260412=CARTESIAN_POINT('Ctrl Pts',(-44.5079524583208,-59.5441932447742,
-46.3102625));
#260413=CARTESIAN_POINT('Ctrl Pts',(-43.3135644199415,-59.5441932447742,
-46.2519291666667));
#260414=CARTESIAN_POINT('Ctrl Pts',(-42.7163704007519,-58.5098228615615,
-46.1935958333333));
#260415=CARTESIAN_POINT('Ctrl Pts',(-42.1191763815623,-57.4754524783487,
-46.1352625));
#260416=CARTESIAN_POINT('Ctrl Pts',(-42.7163704007519,-56.4410820951361,
-46.0769291666667));
#260417=CARTESIAN_POINT('Ctrl Pts',(-43.3135644199415,-55.4067117119233,
-46.0185958333334));
#260418=CARTESIAN_POINT('Ctrl Pts',(-44.5079524583208,-55.4067117119234,
-45.9602625));
#260419=CARTESIAN_POINT('Ctrl Pts',(-45.7023404967,-55.4067117119233,-45.9019291666667));
#260420=CARTESIAN_POINT('Ctrl Pts',(-46.2995345158897,-56.4410820951361,
-45.8435958333333));
#260421=CARTESIAN_POINT('Ctrl Pts',(-46.8967285350793,-57.4754524783487,
-45.7852625));
#260422=CARTESIAN_POINT('Ctrl Pts',(-46.2995345158897,-58.5098228615615,
-45.7269291666667));
#260423=CARTESIAN_POINT('Ctrl Pts',(-45.7023404967,-59.5441932447742,-45.6685958333334));
#260424=CARTESIAN_POINT('Ctrl Pts',(-44.5079524583208,-59.5441932447742,
-45.6102625));
#260425=CARTESIAN_POINT('Ctrl Pts',(-43.3135644199415,-59.5441932447742,
-45.5519291666667));
#260426=CARTESIAN_POINT('Ctrl Pts',(-42.7163704007519,-58.5098228615615,
-45.4935958333333));
#260427=CARTESIAN_POINT('Ctrl Pts',(-42.1191763815623,-57.4754524783487,
-45.4352625));
#260428=CARTESIAN_POINT('Ctrl Pts',(-42.7163704007519,-56.4410820951361,
-45.3769291666667));
#260429=CARTESIAN_POINT('Ctrl Pts',(-43.3135644199415,-55.4067117119233,
-45.3185958333333));
#260430=CARTESIAN_POINT('Ctrl Pts',(-44.5079524583208,-55.4067117119234,
-45.2602625));
#260431=CARTESIAN_POINT('Ctrl Pts',(-45.7023404967,-55.4067117119233,-45.2019291666667));
#260432=CARTESIAN_POINT('Ctrl Pts',(-46.2995345158897,-56.4410820951361,
-45.1435958333334));
#260433=CARTESIAN_POINT('Ctrl Pts',(-46.8967285350793,-57.4754524783487,
-45.0852625));
#260434=CARTESIAN_POINT('Ctrl Pts',(-46.2995345158897,-58.5098228615615,
-45.0269291666667));
#260435=CARTESIAN_POINT('Ctrl Pts',(-45.7023404967,-59.5441932447742,-44.9685958333334));
#260436=CARTESIAN_POINT('Ctrl Pts',(-44.5079524583208,-59.5441932447742,
-44.9102625));
#260437=CARTESIAN_POINT('Ctrl Pts',(-43.3135644199415,-59.5441932447742,
-44.8519291666667));
#260438=CARTESIAN_POINT('Ctrl Pts',(-42.7163704007519,-58.5098228615615,
-44.7935958333333));
#260439=CARTESIAN_POINT('Ctrl Pts',(-42.1191763815623,-57.4754524783487,
-44.7352625));
#260440=CARTESIAN_POINT('Ctrl Pts',(-42.7163704007519,-56.4410820951361,
-44.6769291666667));
#260441=CARTESIAN_POINT('Ctrl Pts',(-43.3135644199415,-55.4067117119233,
-44.6185958333334));
#260442=CARTESIAN_POINT('Ctrl Pts',(-44.5079524583208,-55.4067117119234,
-44.5602625));
#260443=CARTESIAN_POINT('Ctrl Pts',(-45.7023404967,-55.4067117119233,-44.5019291666667));
#260444=CARTESIAN_POINT('Ctrl Pts',(-46.2995345158897,-56.4410820951361,
-44.4435958333333));
#260445=CARTESIAN_POINT('Ctrl Pts',(-46.8967285350793,-57.4754524783487,
-44.3852625));
#260446=CARTESIAN_POINT('Ctrl Pts',(-46.2995345158897,-58.5098228615615,
-44.3269291666667));
#260447=CARTESIAN_POINT('Ctrl Pts',(-45.7023404967,-59.5441932447742,-44.2685958333334));
#260448=CARTESIAN_POINT('Ctrl Pts',(-44.5079524583208,-59.5441932447742,
-44.2102625));
#260449=CARTESIAN_POINT('Ctrl Pts',(-43.3135644199415,-59.5441932447742,
-44.1519291666667));
#260450=CARTESIAN_POINT('Ctrl Pts',(-42.7163704007519,-58.5098228615615,
-44.0935958333334));
#260451=CARTESIAN_POINT('Ctrl Pts',(-42.1191763815623,-57.4754524783487,
-44.0352625));
#260452=CARTESIAN_POINT('Ctrl Pts',(-42.7163704007519,-56.4410820951361,
-43.9769291666667));
#260453=CARTESIAN_POINT('Ctrl Pts',(-43.3135644199415,-55.4067117119233,
-43.9185958333334));
#260454=CARTESIAN_POINT('Ctrl Pts',(-44.5079524583208,-55.4067117119234,
-43.8602625));
#260455=CARTESIAN_POINT('Ctrl Pts',(-45.7023404967,-55.4067117119233,-43.8019291666667));
#260456=CARTESIAN_POINT('Ctrl Pts',(-46.2995345158897,-56.4410820951361,
-43.7435958333334));
#260457=CARTESIAN_POINT('Ctrl Pts',(-46.8967285350793,-57.4754524783487,
-43.6852625));
#260458=CARTESIAN_POINT('Ctrl Pts',(-46.2995345158897,-58.5098228615615,
-43.6269291666667));
#260459=CARTESIAN_POINT('Ctrl Pts',(-45.7023404967,-59.5441932447742,-43.5685958333334));
#260460=CARTESIAN_POINT('Ctrl Pts',(-44.5079524583208,-59.5441932447742,
-43.5102625));
#260461=CARTESIAN_POINT('Ctrl Pts',(-43.3135644199415,-59.5441932447742,
-43.4519291666667));
#260462=CARTESIAN_POINT('Ctrl Pts',(-42.7163704007519,-58.5098228615615,
-43.3935958333334));
#260463=CARTESIAN_POINT('Ctrl Pts',(-42.1191763815623,-57.4754524783487,
-43.3352625));
#260464=CARTESIAN_POINT('Ctrl Pts',(-42.7163704007519,-56.4410820951361,
-43.2769291666667));
#260465=CARTESIAN_POINT('Ctrl Pts',(-43.3135644199415,-55.4067117119233,
-43.2185958333334));
#260466=CARTESIAN_POINT('Ctrl Pts',(-44.5079524583208,-55.4067117119234,
-43.1602625));
#260467=CARTESIAN_POINT('Ctrl Pts',(-45.7023404967,-55.4067117119233,-43.1019291666667));
#260468=CARTESIAN_POINT('Ctrl Pts',(-46.2995345158897,-56.4410820951361,
-43.0435958333334));
#260469=CARTESIAN_POINT('Ctrl Pts',(-46.8967285350793,-57.4754524783487,
-42.9852625));
#260470=CARTESIAN_POINT('Ctrl Pts',(-46.2995345158897,-58.5098228615615,
-42.9269291666667));
#260471=CARTESIAN_POINT('Ctrl Pts',(-45.7023404967,-59.5441932447742,-42.8685958333333));
#260472=CARTESIAN_POINT('Ctrl Pts',(-44.5079524583208,-59.5441932447742,
-42.8102625));
#260473=CARTESIAN_POINT('Ctrl Pts',(-43.3135644199415,-59.5441932447742,
-42.7519291666667));
#260474=CARTESIAN_POINT('Ctrl Pts',(-42.7163704007519,-58.5098228615615,
-42.6935958333333));
#260475=CARTESIAN_POINT('Ctrl Pts',(-42.1191763815623,-57.4754524783487,
-42.6352625));
#260476=CARTESIAN_POINT('Ctrl Pts',(-42.7163704007519,-56.4410820951361,
-42.5769291666667));
#260477=CARTESIAN_POINT('Ctrl Pts',(-43.3135644199415,-55.4067117119233,
-42.5185958333333));
#260478=CARTESIAN_POINT('Ctrl Pts',(-44.5079524583208,-55.4067117119234,
-42.4602625));
#260479=CARTESIAN_POINT('Ctrl Pts',(-45.7023404967,-55.4067117119233,-42.4019291666666));
#260480=CARTESIAN_POINT('Ctrl Pts',(-46.2995345158897,-56.4410820951361,
-42.3435958333334));
#260481=CARTESIAN_POINT('Ctrl Pts',(-46.8967285350793,-57.4754524783487,
-42.2852625));
#260482=CARTESIAN_POINT('Ctrl Pts',(-46.2995345158897,-58.5098228615615,
-42.2269291666667));
#260483=CARTESIAN_POINT('Ctrl Pts',(-45.7023404967,-59.5441932447742,-42.1685958333333));
#260484=CARTESIAN_POINT('Ctrl Pts',(-44.5079524583208,-59.5441932447742,
-42.1102625));
#260485=CARTESIAN_POINT('Ctrl Pts',(-43.3135644199415,-59.5441932447742,
-42.0519291666667));
#260486=CARTESIAN_POINT('Ctrl Pts',(-42.7163704007519,-58.5098228615615,
-41.9935958333334));
#260487=CARTESIAN_POINT('Ctrl Pts',(-42.1191763815623,-57.4754524783487,
-41.9352625));
#260488=CARTESIAN_POINT('Ctrl Pts',(-42.7163704007519,-56.4410820951361,
-41.8769291666667));
#260489=CARTESIAN_POINT('Ctrl Pts',(-43.3135644199415,-55.4067117119233,
-41.8185958333333));
#260490=CARTESIAN_POINT('Ctrl Pts',(-44.5079524583208,-55.4067117119234,
-41.7602625));
#260491=CARTESIAN_POINT('Ctrl Pts',(-45.7023404967,-55.4067117119233,-41.7019291666667));
#260492=CARTESIAN_POINT('Ctrl Pts',(-46.2995345158897,-56.4410820951361,
-41.6435958333334));
#260493=CARTESIAN_POINT('Ctrl Pts',(-46.8967285350793,-57.4754524783487,
-41.5852625));
#260494=CARTESIAN_POINT('Ctrl Pts',(-46.2995345158897,-58.5098228615615,
-41.5269291666667));
#260495=CARTESIAN_POINT('Ctrl Pts',(-45.7023404967,-59.5441932447742,-41.4685958333333));
#260496=CARTESIAN_POINT('Ctrl Pts',(-44.5079524583208,-59.5441932447742,
-41.4102625));
#260497=CARTESIAN_POINT('Ctrl Pts',(-43.3135644199415,-59.5441932447742,
-41.3519291666666));
#260498=CARTESIAN_POINT('Ctrl Pts',(-42.7163704007519,-58.5098228615615,
-41.2935958333334));
#260499=CARTESIAN_POINT('Ctrl Pts',(-42.1191763815623,-57.4754524783487,
-41.2352625));
#260500=CARTESIAN_POINT('Ctrl Pts',(-42.7163704007519,-56.4410820951361,
-41.1769291666667));
#260501=CARTESIAN_POINT('Ctrl Pts',(-43.3135644199415,-55.4067117119233,
-41.1185958333333));
#260502=CARTESIAN_POINT('Ctrl Pts',(-44.5079524583208,-55.4067117119234,
-41.0602625));
#260503=CARTESIAN_POINT('Ctrl Pts',(-45.7023404967,-55.4067117119233,-41.0019291666666));
#260504=CARTESIAN_POINT('Ctrl Pts',(-46.2995345158897,-56.4410820951361,
-40.9435958333334));
#260505=CARTESIAN_POINT('Ctrl Pts',(-46.8967285350793,-57.4754524783487,
-40.8852625));
#260506=CARTESIAN_POINT('Ctrl Pts',(-46.2995345158897,-58.5098228615615,
-40.8269291666667));
#260507=CARTESIAN_POINT('Ctrl Pts',(-45.7023404967,-59.5441932447742,-40.7685958333333));
#260508=CARTESIAN_POINT('Ctrl Pts',(-44.5079524583208,-59.5441932447742,
-40.7102625));
#260509=CARTESIAN_POINT('Ctrl Pts',(-43.3135644199415,-59.5441932447742,
-40.6519291666667));
#260510=CARTESIAN_POINT('Ctrl Pts',(-42.7163704007519,-58.5098228615615,
-40.5935958333334));
#260511=CARTESIAN_POINT('Ctrl Pts',(-42.1191763815623,-57.4754524783487,
-40.5352625));
#260512=CARTESIAN_POINT('Ctrl Pts',(-42.7163704007519,-56.4410820951361,
-40.4769291666667));
#260513=CARTESIAN_POINT('Ctrl Pts',(-43.3135644199415,-55.4067117119233,
-40.4185958333333));
#260514=CARTESIAN_POINT('Ctrl Pts',(-44.5079524583208,-55.4067117119234,
-40.3602625));
#260515=CARTESIAN_POINT('Ctrl Pts',(-45.7023404967,-55.4067117119233,-40.3019291666667));
#260516=CARTESIAN_POINT('Ctrl Pts',(-46.2995345158897,-56.4410820951361,
-40.2435958333334));
#260517=CARTESIAN_POINT('Ctrl Pts',(-46.8967285350793,-57.4754524783487,
-40.1852625));
#260518=CARTESIAN_POINT('Ctrl Pts',(-46.2995345158897,-58.5098228615615,
-40.1269291666666));
#260519=CARTESIAN_POINT('Ctrl Pts',(-45.7023404967,-59.5441932447742,-40.0685958333333));
#260520=CARTESIAN_POINT('Ctrl Pts',(-44.5079524583208,-59.5441932447742,
-40.0102625));
#260521=CARTESIAN_POINT('Ctrl Pts',(-43.3135644199415,-59.5441932447742,
-39.9519291666667));
#260522=CARTESIAN_POINT('Ctrl Pts',(-42.7163704007519,-58.5098228615615,
-39.8935958333334));
#260523=CARTESIAN_POINT('Ctrl Pts',(-42.1191763815623,-57.4754524783487,
-39.8352625));
#260524=CARTESIAN_POINT('Ctrl Pts',(-42.7163704007519,-56.4410820951361,
-39.7769291666667));
#260525=CARTESIAN_POINT('Ctrl Pts',(-43.3135644199415,-55.4067117119233,
-39.7185958333334));
#260526=CARTESIAN_POINT('Ctrl Pts',(-44.5079524583208,-55.4067117119234,
-39.6602625));
#260527=CARTESIAN_POINT('Ctrl Pts',(-45.7023404967,-55.4067117119233,-39.6019291666667));
#260528=CARTESIAN_POINT('Ctrl Pts',(-46.2995345158897,-56.4410820951361,
-39.5435958333333));
#260529=CARTESIAN_POINT('Ctrl Pts',(-46.8967285350793,-57.4754524783487,
-39.4852625));
#260530=CARTESIAN_POINT('Ctrl Pts',(-46.2995345158897,-58.5098228615615,
-39.4269291666667));
#260531=CARTESIAN_POINT('Ctrl Pts',(-45.7023404967,-59.5441932447742,-39.3685958333334));
#260532=CARTESIAN_POINT('Ctrl Pts',(-44.5079524583208,-59.5441932447742,
-39.3102625));
#260533=CARTESIAN_POINT('Ctrl Pts',(-43.3135644199415,-59.5441932447742,
-39.2519291666667));
#260534=CARTESIAN_POINT('Ctrl Pts',(-42.7163704007519,-58.5098228615615,
-39.1935958333334));
#260535=CARTESIAN_POINT('Ctrl Pts',(-42.1191763815623,-57.4754524783487,
-39.1352625));
#260536=CARTESIAN_POINT('Ctrl Pts',(-42.7163704007519,-56.4410820951361,
-39.0769291666667));
#260537=CARTESIAN_POINT('Ctrl Pts',(-43.3135644199415,-55.4067117119233,
-39.0185958333334));
#260538=CARTESIAN_POINT('Ctrl Pts',(-44.5079524583208,-55.4067117119234,
-38.9602625));
#260539=CARTESIAN_POINT('Ctrl Pts',(-45.7023404967,-55.4067117119233,-38.9019291666667));
#260540=CARTESIAN_POINT('Ctrl Pts',(-46.2995345158897,-56.4410820951361,
-38.8435958333333));
#260541=CARTESIAN_POINT('Ctrl Pts',(-46.8967285350793,-57.4754524783487,
-38.7852625));
#260542=CARTESIAN_POINT('Ctrl Pts',(-46.2995345158897,-58.5098228615615,
-38.7269291666667));
#260543=CARTESIAN_POINT('Ctrl Pts',(-45.7023404967,-59.5441932447742,-38.6685958333334));
#260544=CARTESIAN_POINT('Ctrl Pts',(-44.5079524583208,-59.5441932447742,
-38.6102625));
#260545=CARTESIAN_POINT('Ctrl Pts',(-43.3135644199415,-59.5441932447742,
-38.5519291666667));
#260546=CARTESIAN_POINT('Ctrl Pts',(-42.7163704007519,-58.5098228615615,
-38.4935958333334));
#260547=CARTESIAN_POINT('Ctrl Pts',(-42.1191763815623,-57.4754524783487,
-38.4352625));
#260548=CARTESIAN_POINT('Ctrl Pts',(-42.7163704007519,-56.4410820951361,
-38.3769291666667));
#260549=CARTESIAN_POINT('Ctrl Pts',(-43.3135644199415,-55.4067117119233,
-38.3185958333333));
#260550=CARTESIAN_POINT('Ctrl Pts',(-44.5079524583208,-55.4067117119234,
-38.2602625));
#260551=CARTESIAN_POINT('Ctrl Pts',(-45.7023404967,-55.4067117119233,-38.2019291666667));
#260552=CARTESIAN_POINT('Ctrl Pts',(-46.2995345158897,-56.4410820951361,
-38.1435958333334));
#260553=CARTESIAN_POINT('Ctrl Pts',(-46.8967285350793,-57.4754524783487,
-38.0852625));
#260554=CARTESIAN_POINT('Ctrl Pts',(-46.2995345158897,-58.5098228615615,
-38.0269291666667));
#260555=CARTESIAN_POINT('Ctrl Pts',(-45.7023404967,-59.5441932447742,-37.9685958333333));
#260556=CARTESIAN_POINT('Ctrl Pts',(-44.5079524583208,-59.5441932447742,
-37.9102625));
#260557=CARTESIAN_POINT('Ctrl Pts',(-43.3135644199415,-59.5441932447742,
-37.8519291666667));
#260558=CARTESIAN_POINT('Ctrl Pts',(-42.7163704007519,-58.5098228615615,
-37.7935958333334));
#260559=CARTESIAN_POINT('Ctrl Pts',(-42.1191763815623,-57.4754524783487,
-37.7352625));
#260560=CARTESIAN_POINT('Ctrl Pts',(-42.7163704007519,-56.4410820951361,
-37.6769291666667));
#260561=CARTESIAN_POINT('Ctrl Pts',(-43.3135644199415,-55.4067117119233,
-37.6185958333333));
#260562=CARTESIAN_POINT('Ctrl Pts',(-44.5079524583208,-55.4067117119234,
-37.5602625));
#260563=CARTESIAN_POINT('Ctrl Pts',(-45.7023404967,-55.4067117119233,-37.5019291666667));
#260564=CARTESIAN_POINT('Ctrl Pts',(-46.2995345158897,-56.4410820951361,
-37.4435958333333));
#260565=CARTESIAN_POINT('Ctrl Pts',(-46.8967285350793,-57.4754524783487,
-37.3852625));
#260566=CARTESIAN_POINT('Ctrl Pts',(-46.2995345158897,-58.5098228615615,
-37.3269291666667));
#260567=CARTESIAN_POINT('Ctrl Pts',(-45.7023404967,-59.5441932447742,-37.2685958333333));
#260568=CARTESIAN_POINT('Ctrl Pts',(-44.5079524583208,-59.5441932447742,
-37.2102625));
#260569=CARTESIAN_POINT('Ctrl Pts',(-43.3135644199415,-59.5441932447742,
-37.1519291666667));
#260570=CARTESIAN_POINT('Ctrl Pts',(-42.7163704007519,-58.5098228615615,
-37.0935958333333));
#260571=CARTESIAN_POINT('Ctrl Pts',(-42.1191763815623,-57.4754524783487,
-37.0352625));
#260572=CARTESIAN_POINT('Ctrl Pts',(-42.7163704007519,-56.4410820951361,
-36.9769291666667));
#260573=CARTESIAN_POINT('Ctrl Pts',(-43.3135644199415,-55.4067117119233,
-36.9185958333333));
#260574=CARTESIAN_POINT('Ctrl Pts',(-44.5079524583208,-55.4067117119234,
-36.8602625));
#260575=CARTESIAN_POINT('Ctrl Pts',(-45.7023404967,-55.4067117119233,-36.8019291666666));
#260576=CARTESIAN_POINT('Ctrl Pts',(-46.2995345158897,-56.4410820951361,
-36.7435958333334));
#260577=CARTESIAN_POINT('Ctrl Pts',(-46.8967285350793,-57.4754524783487,
-36.6852625));
#260578=CARTESIAN_POINT('Ctrl Pts',(-46.2995345158897,-58.5098228615615,
-36.6269291666667));
#260579=CARTESIAN_POINT('Ctrl Pts',(-46.222006582932,-58.64410518045,-36.6193563132714));
#260580=CARTESIAN_POINT('Ctrl Pts',(-46.1253278975281,-58.7653303978899,
-36.611216324118));
#260581=CARTESIAN_POINT('Ctrl Pts',(-44.5079524583208,-59.1441977614012,
-52.8412));
#260582=CARTESIAN_POINT('Ctrl Pts',(-43.5445019199415,-59.1441977614012,
-52.7828666666667));
#260583=CARTESIAN_POINT('Ctrl Pts',(-43.0627766507519,-58.309825119875,
-52.7245333333334));
#260584=CARTESIAN_POINT('Ctrl Pts',(-42.5810513815623,-57.4754524783487,
-52.6662));
#260585=CARTESIAN_POINT('Ctrl Pts',(-43.0627766507519,-56.6410798368225,
-52.6078666666667));
#260586=CARTESIAN_POINT('Ctrl Pts',(-43.5445019199415,-55.8067071952963,
-52.5495333333333));
#260587=CARTESIAN_POINT('Ctrl Pts',(-44.5079524583208,-55.8067071952963,
-52.4912));
#260588=CARTESIAN_POINT('Ctrl Pts',(-45.4714029967,-55.8067071952963,-52.4328666666667));
#260589=CARTESIAN_POINT('Ctrl Pts',(-45.9531282658897,-56.6410798368225,
-52.3745333333334));
#260590=CARTESIAN_POINT('Ctrl Pts',(-46.4348535350793,-57.4754524783487,
-52.3162000000001));
#260591=CARTESIAN_POINT('Ctrl Pts',(-45.9531282658897,-58.309825119875,
-52.2578666666667));
#260592=CARTESIAN_POINT('Ctrl Pts',(-45.4714029967,-59.1441977614012,-52.1995333333334));
#260593=CARTESIAN_POINT('Ctrl Pts',(-44.5079524583208,-59.1441977614012,
-52.1412));
#260594=CARTESIAN_POINT('Ctrl Pts',(-43.5445019199415,-59.1441977614012,
-52.0828666666667));
#260595=CARTESIAN_POINT('Ctrl Pts',(-43.0627766507519,-58.309825119875,
-52.0245333333333));
#260596=CARTESIAN_POINT('Ctrl Pts',(-42.5810513815623,-57.4754524783487,
-51.9662));
#260597=CARTESIAN_POINT('Ctrl Pts',(-43.0627766507519,-56.6410798368225,
-51.9078666666667));
#260598=CARTESIAN_POINT('Ctrl Pts',(-43.5445019199415,-55.8067071952963,
-51.8495333333334));
#260599=CARTESIAN_POINT('Ctrl Pts',(-44.5079524583208,-55.8067071952963,
-51.7912));
#260600=CARTESIAN_POINT('Ctrl Pts',(-45.4714029967,-55.8067071952963,-51.7328666666667));
#260601=CARTESIAN_POINT('Ctrl Pts',(-45.9531282658897,-56.6410798368225,
-51.6745333333334));
#260602=CARTESIAN_POINT('Ctrl Pts',(-46.4348535350793,-57.4754524783487,
-51.6162));
#260603=CARTESIAN_POINT('Ctrl Pts',(-45.9531282658897,-58.309825119875,
-51.5578666666667));
#260604=CARTESIAN_POINT('Ctrl Pts',(-45.4714029967,-59.1441977614012,-51.4995333333334));
#260605=CARTESIAN_POINT('Ctrl Pts',(-44.5079524583208,-59.1441977614012,
-51.4412));
#260606=CARTESIAN_POINT('Ctrl Pts',(-43.5445019199415,-59.1441977614012,
-51.3828666666667));
#260607=CARTESIAN_POINT('Ctrl Pts',(-43.0627766507519,-58.309825119875,
-51.3245333333334));
#260608=CARTESIAN_POINT('Ctrl Pts',(-42.5810513815623,-57.4754524783487,
-51.2662));
#260609=CARTESIAN_POINT('Ctrl Pts',(-43.0627766507519,-56.6410798368225,
-51.2078666666667));
#260610=CARTESIAN_POINT('Ctrl Pts',(-43.5445019199415,-55.8067071952963,
-51.1495333333334));
#260611=CARTESIAN_POINT('Ctrl Pts',(-44.5079524583208,-55.8067071952963,
-51.0912));
#260612=CARTESIAN_POINT('Ctrl Pts',(-45.4714029967,-55.8067071952963,-51.0328666666667));
#260613=CARTESIAN_POINT('Ctrl Pts',(-45.9531282658897,-56.6410798368225,
-50.9745333333333));
#260614=CARTESIAN_POINT('Ctrl Pts',(-46.4348535350793,-57.4754524783487,
-50.9162));
#260615=CARTESIAN_POINT('Ctrl Pts',(-45.9531282658897,-58.309825119875,
-50.8578666666667));
#260616=CARTESIAN_POINT('Ctrl Pts',(-45.4714029967,-59.1441977614012,-50.7995333333334));
#260617=CARTESIAN_POINT('Ctrl Pts',(-44.5079524583208,-59.1441977614012,
-50.7412));
#260618=CARTESIAN_POINT('Ctrl Pts',(-43.5445019199415,-59.1441977614012,
-50.6828666666667));
#260619=CARTESIAN_POINT('Ctrl Pts',(-43.0627766507519,-58.309825119875,
-50.6245333333333));
#260620=CARTESIAN_POINT('Ctrl Pts',(-42.5810513815623,-57.4754524783487,
-50.5662));
#260621=CARTESIAN_POINT('Ctrl Pts',(-43.0627766507519,-56.6410798368225,
-50.5078666666667));
#260622=CARTESIAN_POINT('Ctrl Pts',(-43.5445019199415,-55.8067071952963,
-50.4495333333333));
#260623=CARTESIAN_POINT('Ctrl Pts',(-44.5079524583208,-55.8067071952963,
-50.3912));
#260624=CARTESIAN_POINT('Ctrl Pts',(-45.4714029967,-55.8067071952963,-50.3328666666667));
#260625=CARTESIAN_POINT('Ctrl Pts',(-45.9531282658897,-56.6410798368225,
-50.2745333333334));
#260626=CARTESIAN_POINT('Ctrl Pts',(-46.4348535350793,-57.4754524783487,
-50.2162));
#260627=CARTESIAN_POINT('Ctrl Pts',(-45.9531282658897,-58.309825119875,
-50.1578666666667));
#260628=CARTESIAN_POINT('Ctrl Pts',(-45.4714029967,-59.1441977614012,-50.0995333333333));
#260629=CARTESIAN_POINT('Ctrl Pts',(-44.5079524583208,-59.1441977614012,
-50.0412));
#260630=CARTESIAN_POINT('Ctrl Pts',(-43.5445019199415,-59.1441977614012,
-49.9828666666667));
#260631=CARTESIAN_POINT('Ctrl Pts',(-43.0627766507519,-58.309825119875,
-49.9245333333334));
#260632=CARTESIAN_POINT('Ctrl Pts',(-42.5810513815623,-57.4754524783487,
-49.8662));
#260633=CARTESIAN_POINT('Ctrl Pts',(-43.0627766507519,-56.6410798368225,
-49.8078666666667));
#260634=CARTESIAN_POINT('Ctrl Pts',(-43.5445019199415,-55.8067071952963,
-49.7495333333333));
#260635=CARTESIAN_POINT('Ctrl Pts',(-44.5079524583208,-55.8067071952963,
-49.6912));
#260636=CARTESIAN_POINT('Ctrl Pts',(-45.4714029967,-55.8067071952963,-49.6328666666667));
#260637=CARTESIAN_POINT('Ctrl Pts',(-45.9531282658897,-56.6410798368225,
-49.5745333333334));
#260638=CARTESIAN_POINT('Ctrl Pts',(-46.4348535350793,-57.4754524783487,
-49.5162));
#260639=CARTESIAN_POINT('Ctrl Pts',(-45.9531282658897,-58.309825119875,
-49.4578666666667));
#260640=CARTESIAN_POINT('Ctrl Pts',(-45.4714029967,-59.1441977614012,-49.3995333333333));
#260641=CARTESIAN_POINT('Ctrl Pts',(-44.5079524583208,-59.1441977614012,
-49.3412));
#260642=CARTESIAN_POINT('Ctrl Pts',(-43.5445019199415,-59.1441977614012,
-49.2828666666666));
#260643=CARTESIAN_POINT('Ctrl Pts',(-43.0627766507519,-58.309825119875,
-49.2245333333334));
#260644=CARTESIAN_POINT('Ctrl Pts',(-42.5810513815623,-57.4754524783487,
-49.1662));
#260645=CARTESIAN_POINT('Ctrl Pts',(-43.0627766507519,-56.6410798368225,
-49.1078666666667));
#260646=CARTESIAN_POINT('Ctrl Pts',(-43.5445019199415,-55.8067071952963,
-49.0495333333334));
#260647=CARTESIAN_POINT('Ctrl Pts',(-44.5079524583208,-55.8067071952963,
-48.9912));
#260648=CARTESIAN_POINT('Ctrl Pts',(-45.4714029967,-55.8067071952963,-48.9328666666667));
#260649=CARTESIAN_POINT('Ctrl Pts',(-45.9531282658897,-56.6410798368225,
-48.8745333333334));
#260650=CARTESIAN_POINT('Ctrl Pts',(-46.4348535350793,-57.4754524783487,
-48.8162));
#260651=CARTESIAN_POINT('Ctrl Pts',(-45.9531282658897,-58.309825119875,
-48.7578666666667));
#260652=CARTESIAN_POINT('Ctrl Pts',(-45.4714029967,-59.1441977614012,-48.6995333333334));
#260653=CARTESIAN_POINT('Ctrl Pts',(-44.5079524583208,-59.1441977614012,
-48.6412));
#260654=CARTESIAN_POINT('Ctrl Pts',(-43.5445019199415,-59.1441977614012,
-48.5828666666667));
#260655=CARTESIAN_POINT('Ctrl Pts',(-43.0627766507519,-58.309825119875,
-48.5245333333334));
#260656=CARTESIAN_POINT('Ctrl Pts',(-42.5810513815623,-57.4754524783487,
-48.4662));
#260657=CARTESIAN_POINT('Ctrl Pts',(-43.0627766507519,-56.6410798368225,
-48.4078666666667));
#260658=CARTESIAN_POINT('Ctrl Pts',(-43.5445019199415,-55.8067071952963,
-48.3495333333333));
#260659=CARTESIAN_POINT('Ctrl Pts',(-44.5079524583208,-55.8067071952963,
-48.2912));
#260660=CARTESIAN_POINT('Ctrl Pts',(-45.4714029967,-55.8067071952963,-48.2328666666667));
#260661=CARTESIAN_POINT('Ctrl Pts',(-45.9531282658897,-56.6410798368225,
-48.1745333333334));
#260662=CARTESIAN_POINT('Ctrl Pts',(-46.4348535350793,-57.4754524783487,
-48.1162));
#260663=CARTESIAN_POINT('Ctrl Pts',(-45.9531282658897,-58.309825119875,
-48.0578666666667));
#260664=CARTESIAN_POINT('Ctrl Pts',(-45.4714029967,-59.1441977614012,-47.9995333333334));
#260665=CARTESIAN_POINT('Ctrl Pts',(-44.5079524583208,-59.1441977614012,
-47.9412));
#260666=CARTESIAN_POINT('Ctrl Pts',(-43.5445019199415,-59.1441977614012,
-47.8828666666667));
#260667=CARTESIAN_POINT('Ctrl Pts',(-43.0627766507519,-58.309825119875,
-47.8245333333333));
#260668=CARTESIAN_POINT('Ctrl Pts',(-42.5810513815623,-57.4754524783487,
-47.7662));
#260669=CARTESIAN_POINT('Ctrl Pts',(-43.0627766507519,-56.6410798368225,
-47.7078666666667));
#260670=CARTESIAN_POINT('Ctrl Pts',(-43.5445019199415,-55.8067071952963,
-47.6495333333334));
#260671=CARTESIAN_POINT('Ctrl Pts',(-44.5079524583208,-55.8067071952963,
-47.5912));
#260672=CARTESIAN_POINT('Ctrl Pts',(-45.4714029967,-55.8067071952963,-47.5328666666667));
#260673=CARTESIAN_POINT('Ctrl Pts',(-45.9531282658897,-56.6410798368225,
-47.4745333333334));
#260674=CARTESIAN_POINT('Ctrl Pts',(-46.4348535350793,-57.4754524783487,
-47.4162));
#260675=CARTESIAN_POINT('Ctrl Pts',(-45.9531282658897,-58.309825119875,
-47.3578666666667));
#260676=CARTESIAN_POINT('Ctrl Pts',(-45.4714029967,-59.1441977614012,-47.2995333333334));
#260677=CARTESIAN_POINT('Ctrl Pts',(-44.5079524583208,-59.1441977614012,
-47.2412));
#260678=CARTESIAN_POINT('Ctrl Pts',(-43.5445019199415,-59.1441977614012,
-47.1828666666667));
#260679=CARTESIAN_POINT('Ctrl Pts',(-43.0627766507519,-58.309825119875,
-47.1245333333333));
#260680=CARTESIAN_POINT('Ctrl Pts',(-42.5810513815623,-57.4754524783487,
-47.0662));
#260681=CARTESIAN_POINT('Ctrl Pts',(-43.0627766507519,-56.6410798368225,
-47.0078666666667));
#260682=CARTESIAN_POINT('Ctrl Pts',(-43.5445019199415,-55.8067071952963,
-46.9495333333334));
#260683=CARTESIAN_POINT('Ctrl Pts',(-44.5079524583208,-55.8067071952963,
-46.8912));
#260684=CARTESIAN_POINT('Ctrl Pts',(-45.4714029967,-55.8067071952963,-46.8328666666667));
#260685=CARTESIAN_POINT('Ctrl Pts',(-45.9531282658897,-56.6410798368225,
-46.7745333333334));
#260686=CARTESIAN_POINT('Ctrl Pts',(-46.4348535350793,-57.4754524783487,
-46.7162));
#260687=CARTESIAN_POINT('Ctrl Pts',(-45.9531282658897,-58.309825119875,
-46.6578666666667));
#260688=CARTESIAN_POINT('Ctrl Pts',(-45.4714029967,-59.1441977614012,-46.5995333333334));
#260689=CARTESIAN_POINT('Ctrl Pts',(-44.5079524583208,-59.1441977614012,
-46.5412));
#260690=CARTESIAN_POINT('Ctrl Pts',(-43.5445019199415,-59.1441977614012,
-46.4828666666667));
#260691=CARTESIAN_POINT('Ctrl Pts',(-43.0627766507519,-58.309825119875,
-46.4245333333334));
#260692=CARTESIAN_POINT('Ctrl Pts',(-42.5810513815623,-57.4754524783487,
-46.3662));
#260693=CARTESIAN_POINT('Ctrl Pts',(-43.0627766507519,-56.6410798368225,
-46.3078666666667));
#260694=CARTESIAN_POINT('Ctrl Pts',(-43.5445019199415,-55.8067071952963,
-46.2495333333334));
#260695=CARTESIAN_POINT('Ctrl Pts',(-44.5079524583208,-55.8067071952963,
-46.1912));
#260696=CARTESIAN_POINT('Ctrl Pts',(-45.4714029967,-55.8067071952963,-46.1328666666667));
#260697=CARTESIAN_POINT('Ctrl Pts',(-45.9531282658897,-56.6410798368225,
-46.0745333333334));
#260698=CARTESIAN_POINT('Ctrl Pts',(-46.4348535350793,-57.4754524783487,
-46.0162));
#260699=CARTESIAN_POINT('Ctrl Pts',(-45.9531282658897,-58.309825119875,
-45.9578666666667));
#260700=CARTESIAN_POINT('Ctrl Pts',(-45.4714029967,-59.1441977614012,-45.8995333333333));
#260701=CARTESIAN_POINT('Ctrl Pts',(-44.5079524583208,-59.1441977614012,
-45.8412));
#260702=CARTESIAN_POINT('Ctrl Pts',(-43.5445019199415,-59.1441977614012,
-45.7828666666667));
#260703=CARTESIAN_POINT('Ctrl Pts',(-43.0627766507519,-58.309825119875,
-45.7245333333333));
#260704=CARTESIAN_POINT('Ctrl Pts',(-42.5810513815623,-57.4754524783487,
-45.6662));
#260705=CARTESIAN_POINT('Ctrl Pts',(-43.0627766507519,-56.6410798368225,
-45.6078666666667));
#260706=CARTESIAN_POINT('Ctrl Pts',(-43.5445019199415,-55.8067071952963,
-45.5495333333333));
#260707=CARTESIAN_POINT('Ctrl Pts',(-44.5079524583208,-55.8067071952963,
-45.4912));
#260708=CARTESIAN_POINT('Ctrl Pts',(-45.4714029967,-55.8067071952963,-45.4328666666666));
#260709=CARTESIAN_POINT('Ctrl Pts',(-45.9531282658897,-56.6410798368225,
-45.3745333333334));
#260710=CARTESIAN_POINT('Ctrl Pts',(-46.4348535350793,-57.4754524783487,
-45.3162));
#260711=CARTESIAN_POINT('Ctrl Pts',(-45.9531282658897,-58.309825119875,
-45.2578666666667));
#260712=CARTESIAN_POINT('Ctrl Pts',(-45.4714029967,-59.1441977614012,-45.1995333333333));
#260713=CARTESIAN_POINT('Ctrl Pts',(-44.5079524583208,-59.1441977614012,
-45.1412));
#260714=CARTESIAN_POINT('Ctrl Pts',(-43.5445019199415,-59.1441977614012,
-45.0828666666667));
#260715=CARTESIAN_POINT('Ctrl Pts',(-43.0627766507519,-58.309825119875,
-45.0245333333334));
#260716=CARTESIAN_POINT('Ctrl Pts',(-42.5810513815623,-57.4754524783487,
-44.9662));
#260717=CARTESIAN_POINT('Ctrl Pts',(-43.0627766507519,-56.6410798368225,
-44.9078666666667));
#260718=CARTESIAN_POINT('Ctrl Pts',(-43.5445019199415,-55.8067071952963,
-44.8495333333333));
#260719=CARTESIAN_POINT('Ctrl Pts',(-44.5079524583208,-55.8067071952963,
-44.7912));
#260720=CARTESIAN_POINT('Ctrl Pts',(-45.4714029967,-55.8067071952963,-44.7328666666667));
#260721=CARTESIAN_POINT('Ctrl Pts',(-45.9531282658897,-56.6410798368225,
-44.6745333333334));
#260722=CARTESIAN_POINT('Ctrl Pts',(-46.4348535350793,-57.4754524783487,
-44.6162));
#260723=CARTESIAN_POINT('Ctrl Pts',(-45.9531282658897,-58.309825119875,
-44.5578666666667));
#260724=CARTESIAN_POINT('Ctrl Pts',(-45.4714029967,-59.1441977614012,-44.4995333333333));
#260725=CARTESIAN_POINT('Ctrl Pts',(-44.5079524583208,-59.1441977614012,
-44.4412));
#260726=CARTESIAN_POINT('Ctrl Pts',(-43.5445019199415,-59.1441977614012,
-44.3828666666667));
#260727=CARTESIAN_POINT('Ctrl Pts',(-43.0627766507519,-58.309825119875,
-44.3245333333334));
#260728=CARTESIAN_POINT('Ctrl Pts',(-42.5810513815623,-57.4754524783487,
-44.2662));
#260729=CARTESIAN_POINT('Ctrl Pts',(-43.0627766507519,-56.6410798368225,
-44.2078666666667));
#260730=CARTESIAN_POINT('Ctrl Pts',(-43.5445019199415,-55.8067071952963,
-44.1495333333334));
#260731=CARTESIAN_POINT('Ctrl Pts',(-44.5079524583208,-55.8067071952963,
-44.0912));
#260732=CARTESIAN_POINT('Ctrl Pts',(-45.4714029967,-55.8067071952963,-44.0328666666667));
#260733=CARTESIAN_POINT('Ctrl Pts',(-45.9531282658897,-56.6410798368225,
-43.9745333333333));
#260734=CARTESIAN_POINT('Ctrl Pts',(-46.4348535350793,-57.4754524783487,
-43.9162));
#260735=CARTESIAN_POINT('Ctrl Pts',(-45.9531282658897,-58.309825119875,
-43.8578666666667));
#260736=CARTESIAN_POINT('Ctrl Pts',(-45.4714029967,-59.1441977614012,-43.7995333333334));
#260737=CARTESIAN_POINT('Ctrl Pts',(-44.5079524583208,-59.1441977614012,
-43.7412));
#260738=CARTESIAN_POINT('Ctrl Pts',(-43.5445019199415,-59.1441977614012,
-43.6828666666667));
#260739=CARTESIAN_POINT('Ctrl Pts',(-43.0627766507519,-58.309825119875,
-43.6245333333333));
#260740=CARTESIAN_POINT('Ctrl Pts',(-42.5810513815623,-57.4754524783487,
-43.5662));
#260741=CARTESIAN_POINT('Ctrl Pts',(-43.0627766507519,-56.6410798368225,
-43.5078666666667));
#260742=CARTESIAN_POINT('Ctrl Pts',(-43.5445019199415,-55.8067071952963,
-43.4495333333334));
#260743=CARTESIAN_POINT('Ctrl Pts',(-44.5079524583208,-55.8067071952963,
-43.3912));
#260744=CARTESIAN_POINT('Ctrl Pts',(-45.4714029967,-55.8067071952963,-43.3328666666667));
#260745=CARTESIAN_POINT('Ctrl Pts',(-45.9531282658897,-56.6410798368225,
-43.2745333333334));
#260746=CARTESIAN_POINT('Ctrl Pts',(-46.4348535350793,-57.4754524783487,
-43.2162));
#260747=CARTESIAN_POINT('Ctrl Pts',(-45.9531282658897,-58.309825119875,
-43.1578666666667));
#260748=CARTESIAN_POINT('Ctrl Pts',(-45.4714029967,-59.1441977614012,-43.0995333333334));
#260749=CARTESIAN_POINT('Ctrl Pts',(-44.5079524583208,-59.1441977614012,
-43.0412));
#260750=CARTESIAN_POINT('Ctrl Pts',(-43.5445019199415,-59.1441977614012,
-42.9828666666667));
#260751=CARTESIAN_POINT('Ctrl Pts',(-43.0627766507519,-58.309825119875,
-42.9245333333334));
#260752=CARTESIAN_POINT('Ctrl Pts',(-42.5810513815623,-57.4754524783487,
-42.8662));
#260753=CARTESIAN_POINT('Ctrl Pts',(-43.0627766507519,-56.6410798368225,
-42.8078666666667));
#260754=CARTESIAN_POINT('Ctrl Pts',(-43.5445019199415,-55.8067071952963,
-42.7495333333334));
#260755=CARTESIAN_POINT('Ctrl Pts',(-44.5079524583208,-55.8067071952963,
-42.6912));
#260756=CARTESIAN_POINT('Ctrl Pts',(-45.4714029967,-55.8067071952963,-42.6328666666667));
#260757=CARTESIAN_POINT('Ctrl Pts',(-45.9531282658897,-56.6410798368225,
-42.5745333333333));
#260758=CARTESIAN_POINT('Ctrl Pts',(-46.4348535350793,-57.4754524783487,
-42.5162));
#260759=CARTESIAN_POINT('Ctrl Pts',(-45.9531282658897,-58.309825119875,
-42.4578666666667));
#260760=CARTESIAN_POINT('Ctrl Pts',(-45.4714029967,-59.1441977614012,-42.3995333333334));
#260761=CARTESIAN_POINT('Ctrl Pts',(-44.5079524583208,-59.1441977614012,
-42.3412));
#260762=CARTESIAN_POINT('Ctrl Pts',(-43.5445019199415,-59.1441977614012,
-42.2828666666667));
#260763=CARTESIAN_POINT('Ctrl Pts',(-43.0627766507519,-58.309825119875,
-42.2245333333333));
#260764=CARTESIAN_POINT('Ctrl Pts',(-42.5810513815623,-57.4754524783487,
-42.1662));
#260765=CARTESIAN_POINT('Ctrl Pts',(-43.0627766507519,-56.6410798368225,
-42.1078666666667));
#260766=CARTESIAN_POINT('Ctrl Pts',(-43.5445019199415,-55.8067071952963,
-42.0495333333334));
#260767=CARTESIAN_POINT('Ctrl Pts',(-44.5079524583208,-55.8067071952963,
-41.9912));
#260768=CARTESIAN_POINT('Ctrl Pts',(-45.4714029967,-55.8067071952963,-41.9328666666667));
#260769=CARTESIAN_POINT('Ctrl Pts',(-45.9531282658897,-56.6410798368225,
-41.8745333333334));
#260770=CARTESIAN_POINT('Ctrl Pts',(-46.4348535350793,-57.4754524783487,
-41.8162));
#260771=CARTESIAN_POINT('Ctrl Pts',(-45.9531282658897,-58.309825119875,
-41.7578666666667));
#260772=CARTESIAN_POINT('Ctrl Pts',(-45.4714029967,-59.1441977614012,-41.6995333333334));
#260773=CARTESIAN_POINT('Ctrl Pts',(-44.5079524583208,-59.1441977614012,
-41.6412));
#260774=CARTESIAN_POINT('Ctrl Pts',(-43.5445019199415,-59.1441977614012,
-41.5828666666667));
#260775=CARTESIAN_POINT('Ctrl Pts',(-43.0627766507519,-58.309825119875,
-41.5245333333334));
#260776=CARTESIAN_POINT('Ctrl Pts',(-42.5810513815623,-57.4754524783487,
-41.4662));
#260777=CARTESIAN_POINT('Ctrl Pts',(-43.0627766507519,-56.6410798368225,
-41.4078666666667));
#260778=CARTESIAN_POINT('Ctrl Pts',(-43.5445019199415,-55.8067071952963,
-41.3495333333333));
#260779=CARTESIAN_POINT('Ctrl Pts',(-44.5079524583208,-55.8067071952963,
-41.2912));
#260780=CARTESIAN_POINT('Ctrl Pts',(-45.4714029967,-55.8067071952963,-41.2328666666667));
#260781=CARTESIAN_POINT('Ctrl Pts',(-45.9531282658897,-56.6410798368225,
-41.1745333333334));
#260782=CARTESIAN_POINT('Ctrl Pts',(-46.4348535350793,-57.4754524783487,
-41.1162));
#260783=CARTESIAN_POINT('Ctrl Pts',(-45.9531282658897,-58.309825119875,
-41.0578666666667));
#260784=CARTESIAN_POINT('Ctrl Pts',(-45.4714029967,-59.1441977614012,-40.9995333333333));
#260785=CARTESIAN_POINT('Ctrl Pts',(-44.5079524583208,-59.1441977614012,
-40.9412));
#260786=CARTESIAN_POINT('Ctrl Pts',(-43.5445019199415,-59.1441977614012,
-40.8828666666667));
#260787=CARTESIAN_POINT('Ctrl Pts',(-43.0627766507519,-58.309825119875,
-40.8245333333333));
#260788=CARTESIAN_POINT('Ctrl Pts',(-42.5810513815623,-57.4754524783487,
-40.7662));
#260789=CARTESIAN_POINT('Ctrl Pts',(-43.0627766507519,-56.6410798368225,
-40.7078666666667));
#260790=CARTESIAN_POINT('Ctrl Pts',(-43.5445019199415,-55.8067071952963,
-40.6495333333334));
#260791=CARTESIAN_POINT('Ctrl Pts',(-44.5079524583208,-55.8067071952963,
-40.5912));
#260792=CARTESIAN_POINT('Ctrl Pts',(-45.4714029967,-55.8067071952963,-40.5328666666667));
#260793=CARTESIAN_POINT('Ctrl Pts',(-45.9531282658897,-56.6410798368225,
-40.4745333333334));
#260794=CARTESIAN_POINT('Ctrl Pts',(-46.4348535350793,-57.4754524783487,
-40.4162));
#260795=CARTESIAN_POINT('Ctrl Pts',(-45.9531282658897,-58.309825119875,
-40.3578666666667));
#260796=CARTESIAN_POINT('Ctrl Pts',(-45.4714029967,-59.1441977614012,-40.2995333333333));
#260797=CARTESIAN_POINT('Ctrl Pts',(-44.5079524583208,-59.1441977614012,
-40.2412));
#260798=CARTESIAN_POINT('Ctrl Pts',(-43.5445019199415,-59.1441977614012,
-40.1828666666667));
#260799=CARTESIAN_POINT('Ctrl Pts',(-43.0627766507519,-58.309825119875,
-40.1245333333334));
#260800=CARTESIAN_POINT('Ctrl Pts',(-42.5810513815623,-57.4754524783487,
-40.0662));
#260801=CARTESIAN_POINT('Ctrl Pts',(-43.0627766507519,-56.6410798368225,
-40.0078666666667));
#260802=CARTESIAN_POINT('Ctrl Pts',(-43.5445019199415,-55.8067071952963,
-39.9495333333333));
#260803=CARTESIAN_POINT('Ctrl Pts',(-44.5079524583208,-55.8067071952963,
-39.8912));
#260804=CARTESIAN_POINT('Ctrl Pts',(-45.4714029967,-55.8067071952963,-39.8328666666666));
#260805=CARTESIAN_POINT('Ctrl Pts',(-45.9531282658897,-56.6410798368225,
-39.7745333333334));
#260806=CARTESIAN_POINT('Ctrl Pts',(-46.4348535350793,-57.4754524783487,
-39.7162));
#260807=CARTESIAN_POINT('Ctrl Pts',(-45.9531282658897,-58.309825119875,
-39.6578666666667));
#260808=CARTESIAN_POINT('Ctrl Pts',(-45.4714029967,-59.1441977614012,-39.5995333333333));
#260809=CARTESIAN_POINT('Ctrl Pts',(-44.5079524583208,-59.1441977614012,
-39.5412));
#260810=CARTESIAN_POINT('Ctrl Pts',(-43.5445019199415,-59.1441977614012,
-39.4828666666666));
#260811=CARTESIAN_POINT('Ctrl Pts',(-43.0627766507519,-58.309825119875,
-39.4245333333334));
#260812=CARTESIAN_POINT('Ctrl Pts',(-42.5810513815623,-57.4754524783487,
-39.3662));
#260813=CARTESIAN_POINT('Ctrl Pts',(-43.0627766507519,-56.6410798368225,
-39.3078666666667));
#260814=CARTESIAN_POINT('Ctrl Pts',(-43.5445019199415,-55.8067071952963,
-39.2495333333333));
#260815=CARTESIAN_POINT('Ctrl Pts',(-44.5079524583208,-55.8067071952963,
-39.1912));
#260816=CARTESIAN_POINT('Ctrl Pts',(-45.4714029967,-55.8067071952963,-39.1328666666667));
#260817=CARTESIAN_POINT('Ctrl Pts',(-45.9531282658897,-56.6410798368225,
-39.0745333333333));
#260818=CARTESIAN_POINT('Ctrl Pts',(-46.4348535350793,-57.4754524783487,
-39.0162));
#260819=CARTESIAN_POINT('Ctrl Pts',(-45.9531282658897,-58.309825119875,
-38.9578666666667));
#260820=CARTESIAN_POINT('Ctrl Pts',(-45.4714029967,-59.1441977614012,-38.8995333333334));
#260821=CARTESIAN_POINT('Ctrl Pts',(-44.5079524583208,-59.1441977614012,
-38.8412));
#260822=CARTESIAN_POINT('Ctrl Pts',(-43.5445019199415,-59.1441977614012,
-38.7828666666667));
#260823=CARTESIAN_POINT('Ctrl Pts',(-43.0627766507519,-58.309825119875,
-38.7245333333334));
#260824=CARTESIAN_POINT('Ctrl Pts',(-42.5810513815623,-57.4754524783487,
-38.6662));
#260825=CARTESIAN_POINT('Ctrl Pts',(-43.0627766507519,-56.6410798368225,
-38.6078666666667));
#260826=CARTESIAN_POINT('Ctrl Pts',(-43.5445019199415,-55.8067071952963,
-38.5495333333334));
#260827=CARTESIAN_POINT('Ctrl Pts',(-44.5079524583208,-55.8067071952963,
-38.4912));
#260828=CARTESIAN_POINT('Ctrl Pts',(-45.4714029967,-55.8067071952963,-38.4328666666667));
#260829=CARTESIAN_POINT('Ctrl Pts',(-45.9531282658897,-56.6410798368225,
-38.3745333333333));
#260830=CARTESIAN_POINT('Ctrl Pts',(-46.4348535350793,-57.4754524783487,
-38.3162));
#260831=CARTESIAN_POINT('Ctrl Pts',(-45.9531282658897,-58.309825119875,
-38.2578666666667));
#260832=CARTESIAN_POINT('Ctrl Pts',(-45.4714029967,-59.1441977614012,-38.1995333333333));
#260833=CARTESIAN_POINT('Ctrl Pts',(-44.5079524583208,-59.1441977614012,
-38.1412));
#260834=CARTESIAN_POINT('Ctrl Pts',(-43.5445019199415,-59.1441977614012,
-38.0828666666667));
#260835=CARTESIAN_POINT('Ctrl Pts',(-43.0627766507519,-58.309825119875,
-38.0245333333334));
#260836=CARTESIAN_POINT('Ctrl Pts',(-42.5810513815623,-57.4754524783487,
-37.9662));
#260837=CARTESIAN_POINT('Ctrl Pts',(-43.0627766507519,-56.6410798368225,
-37.9078666666667));
#260838=CARTESIAN_POINT('Ctrl Pts',(-43.5445019199415,-55.8067071952963,
-37.8495333333334));
#260839=CARTESIAN_POINT('Ctrl Pts',(-44.5079524583208,-55.8067071952963,
-37.7912));
#260840=CARTESIAN_POINT('Ctrl Pts',(-45.4714029967,-55.8067071952963,-37.7328666666667));
#260841=CARTESIAN_POINT('Ctrl Pts',(-45.9531282658897,-56.6410798368225,
-37.6745333333334));
#260842=CARTESIAN_POINT('Ctrl Pts',(-46.4348535350793,-57.4754524783487,
-37.6162));
#260843=CARTESIAN_POINT('Ctrl Pts',(-45.9531282658897,-58.309825119875,
-37.5578666666667));
#260844=CARTESIAN_POINT('Ctrl Pts',(-45.4714029967,-59.1441977614012,-37.4995333333334));
#260845=CARTESIAN_POINT('Ctrl Pts',(-44.5079524583208,-59.1441977614012,
-37.4412));
#260846=CARTESIAN_POINT('Ctrl Pts',(-43.5445019199415,-59.1441977614012,
-37.3828666666667));
#260847=CARTESIAN_POINT('Ctrl Pts',(-43.0627766507519,-58.309825119875,
-37.3245333333333));
#260848=CARTESIAN_POINT('Ctrl Pts',(-42.5810513815623,-57.4754524783487,
-37.2662));
#260849=CARTESIAN_POINT('Ctrl Pts',(-43.0627766507519,-56.6410798368225,
-37.2078666666667));
#260850=CARTESIAN_POINT('Ctrl Pts',(-43.5445019199415,-55.8067071952963,
-37.1495333333334));
#260851=CARTESIAN_POINT('Ctrl Pts',(-44.5079524583208,-55.8067071952963,
-37.0912));
#260852=CARTESIAN_POINT('Ctrl Pts',(-45.4714029967,-55.8067071952963,-37.0328666666667));
#260853=CARTESIAN_POINT('Ctrl Pts',(-45.9531282658897,-56.6410798368225,
-36.9745333333333));
#260854=CARTESIAN_POINT('Ctrl Pts',(-46.4348535350793,-57.4754524783487,
-36.9162));
#260855=CARTESIAN_POINT('Ctrl Pts',(-45.9531282658897,-58.309825119875,
-36.8578666666667));
#260856=CARTESIAN_POINT('Ctrl Pts',(-45.8905905257689,-58.4181436631548,
-36.8502938132714));
#260857=CARTESIAN_POINT('Ctrl Pts',(-45.8126048724392,-58.5159297236766,
-36.8421538241181));
#260858=CARTESIAN_POINT('Ctrl Pts',(-42.5996267014623,-58.0740282996226,
-39.2098668919623));
#260859=CARTESIAN_POINT('Ctrl Pts',(-42.5725778614496,-57.8429829953309,
-39.2221682992926));
#260860=CARTESIAN_POINT('Ctrl Pts',(-42.5746974198402,-57.610126621336,
-39.227083277036));
#260861=CARTESIAN_POINT('Ctrl Pts',(-42.6405003904691,-57.1745640350164,
-39.2256289192332));
#260862=CARTESIAN_POINT('Ctrl Pts',(-42.6977550170523,-56.9733387116817,
-39.2204303507015));
#260863=CARTESIAN_POINT('Ctrl Pts',(-42.8283324794819,-56.6773258608037,
-39.2079085695582));
#260864=CARTESIAN_POINT('Ctrl Pts',(-42.8824025719944,-56.5767100388546,
-39.2029307320589));
#260865=CARTESIAN_POINT('Ctrl Pts',(-42.9551055667509,-56.4626324221248,
-39.1954338390341));
#260866=CARTESIAN_POINT('Ctrl Pts',(-42.9664620034791,-56.4453286852025,
-39.1942364504284));
#260867=CARTESIAN_POINT('Ctrl Pts',(-42.9795523961031,-56.4259574076604,
-39.1928277088137));
#260868=CARTESIAN_POINT('Ctrl Pts',(-42.9809760143693,-56.4238580974341,
-39.192674110711));
#260869=CARTESIAN_POINT('Ctrl Pts',(-42.9838312438709,-56.419662423705,
-39.1923652757117));
#260870=CARTESIAN_POINT('Ctrl Pts',(-42.9852628470618,-56.4175660843538,
-39.1922100390342));
#260871=CARTESIAN_POINT('Ctrl Pts',(-43.0379271161551,-56.3407179277042,
-39.1864853162508));
#260872=CARTESIAN_POINT('Ctrl Pts',(-43.093260109904,-56.269324547675,-39.1800000400795));
#260873=CARTESIAN_POINT('Ctrl Pts',(-43.2395455298464,-56.1018453733189,
-39.1619525260045));
#260874=CARTESIAN_POINT('Ctrl Pts',(-43.334446313922,-56.0103462780516,
-39.1495099323279));
#260875=CARTESIAN_POINT('Ctrl Pts',(-43.6658508016362,-55.7405007337001,
-39.103943047775));
#260876=CARTESIAN_POINT('Ctrl Pts',(-43.9263559243168,-55.5998720026574,
-39.0651121378969));
#260877=CARTESIAN_POINT('Ctrl Pts',(-44.2150213622831,-55.5011028009662,
-39.0177579842635));
#260878=CARTESIAN_POINT('Ctrl Pts',(-44.225814020228,-55.4974873478956,
-39.0159815752866));
#260879=CARTESIAN_POINT('Ctrl Pts',(-44.236624711623,-55.4939424893001,
-39.0141961864886));
#260880=CARTESIAN_POINT('Ctrl Pts',(-44.5079524583208,-59.5441932447742,
-52.6102625));
#260881=CARTESIAN_POINT('Ctrl Pts',(-43.3135644199415,-59.5441932447742,
-52.5519291666666));
#260882=CARTESIAN_POINT('Ctrl Pts',(-42.7163704007519,-58.5098228615615,
-52.4935958333333));
#260883=CARTESIAN_POINT('Ctrl Pts',(-42.1191763815623,-57.4754524783487,
-52.4352625000001));
#260884=CARTESIAN_POINT('Ctrl Pts',(-42.7163704007519,-56.4410820951361,
-52.3769291666667));
#260885=CARTESIAN_POINT('Ctrl Pts',(-43.3135644199415,-55.4067117119233,
-52.3185958333334));
#260886=CARTESIAN_POINT('Ctrl Pts',(-44.5079524583208,-55.4067117119234,
-52.2602625));
#260887=CARTESIAN_POINT('Ctrl Pts',(-45.7023404967,-55.4067117119233,-52.2019291666667));
#260888=CARTESIAN_POINT('Ctrl Pts',(-46.2995345158897,-56.4410820951361,
-52.1435958333333));
#260889=CARTESIAN_POINT('Ctrl Pts',(-46.8967285350793,-57.4754524783487,
-52.0852625));
#260890=CARTESIAN_POINT('Ctrl Pts',(-46.2995345158897,-58.5098228615615,
-52.0269291666667));
#260891=CARTESIAN_POINT('Ctrl Pts',(-45.7023404967,-59.5441932447742,-51.9685958333333));
#260892=CARTESIAN_POINT('Ctrl Pts',(-44.5079524583208,-59.5441932447742,
-51.9102625));
#260893=CARTESIAN_POINT('Ctrl Pts',(-43.3135644199415,-59.5441932447742,
-51.8519291666667));
#260894=CARTESIAN_POINT('Ctrl Pts',(-42.7163704007519,-58.5098228615615,
-51.7935958333333));
#260895=CARTESIAN_POINT('Ctrl Pts',(-42.1191763815623,-57.4754524783487,
-51.7352625));
#260896=CARTESIAN_POINT('Ctrl Pts',(-42.7163704007519,-56.4410820951361,
-51.6769291666667));
#260897=CARTESIAN_POINT('Ctrl Pts',(-43.3135644199415,-55.4067117119233,
-51.6185958333333));
#260898=CARTESIAN_POINT('Ctrl Pts',(-44.5079524583208,-55.4067117119234,
-51.5602625));
#260899=CARTESIAN_POINT('Ctrl Pts',(-45.7023404967,-55.4067117119233,-51.5019291666666));
#260900=CARTESIAN_POINT('Ctrl Pts',(-46.2995345158897,-56.4410820951361,
-51.4435958333333));
#260901=CARTESIAN_POINT('Ctrl Pts',(-46.8967285350793,-57.4754524783487,
-51.3852625));
#260902=CARTESIAN_POINT('Ctrl Pts',(-46.2995345158897,-58.5098228615615,
-51.3269291666667));
#260903=CARTESIAN_POINT('Ctrl Pts',(-45.7023404967,-59.5441932447742,-51.2685958333333));
#260904=CARTESIAN_POINT('Ctrl Pts',(-44.5079524583208,-59.5441932447742,
-51.2102625));
#260905=CARTESIAN_POINT('Ctrl Pts',(-43.3135644199415,-59.5441932447742,
-51.1519291666666));
#260906=CARTESIAN_POINT('Ctrl Pts',(-42.7163704007519,-58.5098228615615,
-51.0935958333334));
#260907=CARTESIAN_POINT('Ctrl Pts',(-42.1191763815623,-57.4754524783487,
-51.0352625));
#260908=CARTESIAN_POINT('Ctrl Pts',(-42.7163704007519,-56.4410820951361,
-50.9769291666667));
#260909=CARTESIAN_POINT('Ctrl Pts',(-43.3135644199415,-55.4067117119233,
-50.9185958333333));
#260910=CARTESIAN_POINT('Ctrl Pts',(-44.5079524583208,-55.4067117119234,
-50.8602625));
#260911=CARTESIAN_POINT('Ctrl Pts',(-45.7023404967,-55.4067117119233,-50.8019291666667));
#260912=CARTESIAN_POINT('Ctrl Pts',(-46.2995345158897,-56.4410820951361,
-50.7435958333333));
#260913=CARTESIAN_POINT('Ctrl Pts',(-46.8967285350793,-57.4754524783487,
-50.6852625));
#260914=CARTESIAN_POINT('Ctrl Pts',(-46.2995345158897,-58.5098228615615,
-50.6269291666667));
#260915=CARTESIAN_POINT('Ctrl Pts',(-45.7023404967,-59.5441932447742,-50.5685958333333));
#260916=CARTESIAN_POINT('Ctrl Pts',(-44.5079524583208,-59.5441932447742,
-50.5102625));
#260917=CARTESIAN_POINT('Ctrl Pts',(-43.3135644199415,-59.5441932447742,
-50.4519291666667));
#260918=CARTESIAN_POINT('Ctrl Pts',(-42.7163704007519,-58.5098228615615,
-50.3935958333333));
#260919=CARTESIAN_POINT('Ctrl Pts',(-42.1191763815623,-57.4754524783487,
-50.3352625));
#260920=CARTESIAN_POINT('Ctrl Pts',(-42.7163704007519,-56.4410820951361,
-50.2769291666667));
#260921=CARTESIAN_POINT('Ctrl Pts',(-43.3135644199415,-55.4067117119233,
-50.2185958333333));
#260922=CARTESIAN_POINT('Ctrl Pts',(-44.5079524583208,-55.4067117119234,
-50.1602625));
#260923=CARTESIAN_POINT('Ctrl Pts',(-45.7023404967,-55.4067117119233,-50.1019291666667));
#260924=CARTESIAN_POINT('Ctrl Pts',(-46.2995345158897,-56.4410820951361,
-50.0435958333333));
#260925=CARTESIAN_POINT('Ctrl Pts',(-46.8967285350793,-57.4754524783487,
-49.9852625));
#260926=CARTESIAN_POINT('Ctrl Pts',(-46.2995345158897,-58.5098228615615,
-49.9269291666667));
#260927=CARTESIAN_POINT('Ctrl Pts',(-45.7023404967,-59.5441932447742,-49.8685958333333));
#260928=CARTESIAN_POINT('Ctrl Pts',(-44.5079524583208,-59.5441932447742,
-49.8102625));
#260929=CARTESIAN_POINT('Ctrl Pts',(-43.3135644199415,-59.5441932447742,
-49.7519291666667));
#260930=CARTESIAN_POINT('Ctrl Pts',(-42.7163704007519,-58.5098228615615,
-49.6935958333334));
#260931=CARTESIAN_POINT('Ctrl Pts',(-42.1191763815623,-57.4754524783487,
-49.6352625));
#260932=CARTESIAN_POINT('Ctrl Pts',(-42.7163704007519,-56.4410820951361,
-49.5769291666667));
#260933=CARTESIAN_POINT('Ctrl Pts',(-43.3135644199415,-55.4067117119233,
-49.5185958333334));
#260934=CARTESIAN_POINT('Ctrl Pts',(-44.5079524583208,-55.4067117119234,
-49.4602625));
#260935=CARTESIAN_POINT('Ctrl Pts',(-45.7023404967,-55.4067117119233,-49.4019291666667));
#260936=CARTESIAN_POINT('Ctrl Pts',(-46.2995345158897,-56.4410820951361,
-49.3435958333333));
#260937=CARTESIAN_POINT('Ctrl Pts',(-46.8967285350793,-57.4754524783487,
-49.2852625));
#260938=CARTESIAN_POINT('Ctrl Pts',(-46.2995345158897,-58.5098228615615,
-49.2269291666667));
#260939=CARTESIAN_POINT('Ctrl Pts',(-45.7023404967,-59.5441932447742,-49.1685958333334));
#260940=CARTESIAN_POINT('Ctrl Pts',(-44.5079524583208,-59.5441932447742,
-49.1102625));
#260941=CARTESIAN_POINT('Ctrl Pts',(-43.3135644199415,-59.5441932447742,
-49.0519291666667));
#260942=CARTESIAN_POINT('Ctrl Pts',(-42.7163704007519,-58.5098228615615,
-48.9935958333333));
#260943=CARTESIAN_POINT('Ctrl Pts',(-42.1191763815623,-57.4754524783487,
-48.9352625));
#260944=CARTESIAN_POINT('Ctrl Pts',(-42.7163704007519,-56.4410820951361,
-48.8769291666667));
#260945=CARTESIAN_POINT('Ctrl Pts',(-43.3135644199415,-55.4067117119233,
-48.8185958333334));
#260946=CARTESIAN_POINT('Ctrl Pts',(-44.5079524583208,-55.4067117119234,
-48.7602625));
#260947=CARTESIAN_POINT('Ctrl Pts',(-45.7023404967,-55.4067117119233,-48.7019291666667));
#260948=CARTESIAN_POINT('Ctrl Pts',(-46.2995345158897,-56.4410820951361,
-48.6435958333333));
#260949=CARTESIAN_POINT('Ctrl Pts',(-46.8967285350793,-57.4754524783487,
-48.5852625));
#260950=CARTESIAN_POINT('Ctrl Pts',(-46.2995345158897,-58.5098228615615,
-48.5269291666667));
#260951=CARTESIAN_POINT('Ctrl Pts',(-45.7023404967,-59.5441932447742,-48.4685958333333));
#260952=CARTESIAN_POINT('Ctrl Pts',(-44.5079524583208,-59.5441932447742,
-48.4102625));
#260953=CARTESIAN_POINT('Ctrl Pts',(-43.3135644199415,-59.5441932447742,
-48.3519291666667));
#260954=CARTESIAN_POINT('Ctrl Pts',(-42.7163704007519,-58.5098228615615,
-48.2935958333334));
#260955=CARTESIAN_POINT('Ctrl Pts',(-42.1191763815623,-57.4754524783487,
-48.2352625));
#260956=CARTESIAN_POINT('Ctrl Pts',(-42.7163704007519,-56.4410820951361,
-48.1769291666667));
#260957=CARTESIAN_POINT('Ctrl Pts',(-43.3135644199415,-55.4067117119233,
-48.1185958333334));
#260958=CARTESIAN_POINT('Ctrl Pts',(-44.5079524583208,-55.4067117119234,
-48.0602625));
#260959=CARTESIAN_POINT('Ctrl Pts',(-45.7023404967,-55.4067117119233,-48.0019291666667));
#260960=CARTESIAN_POINT('Ctrl Pts',(-46.2995345158897,-56.4410820951361,
-47.9435958333334));
#260961=CARTESIAN_POINT('Ctrl Pts',(-46.8967285350793,-57.4754524783487,
-47.8852625));
#260962=CARTESIAN_POINT('Ctrl Pts',(-46.2995345158897,-58.5098228615615,
-47.8269291666667));
#260963=CARTESIAN_POINT('Ctrl Pts',(-45.7023404967,-59.5441932447742,-47.7685958333333));
#260964=CARTESIAN_POINT('Ctrl Pts',(-44.5079524583208,-59.5441932447742,
-47.7102625));
#260965=CARTESIAN_POINT('Ctrl Pts',(-43.3135644199415,-59.5441932447742,
-47.6519291666667));
#260966=CARTESIAN_POINT('Ctrl Pts',(-42.7163704007519,-58.5098228615615,
-47.5935958333333));
#260967=CARTESIAN_POINT('Ctrl Pts',(-42.1191763815623,-57.4754524783487,
-47.5352625));
#260968=CARTESIAN_POINT('Ctrl Pts',(-42.7163704007519,-56.4410820951361,
-47.4769291666667));
#260969=CARTESIAN_POINT('Ctrl Pts',(-43.3135644199415,-55.4067117119233,
-47.4185958333333));
#260970=CARTESIAN_POINT('Ctrl Pts',(-44.5079524583208,-55.4067117119234,
-47.3602625));
#260971=CARTESIAN_POINT('Ctrl Pts',(-45.7023404967,-55.4067117119233,-47.3019291666666));
#260972=CARTESIAN_POINT('Ctrl Pts',(-46.2995345158897,-56.4410820951361,
-47.2435958333334));
#260973=CARTESIAN_POINT('Ctrl Pts',(-46.8967285350793,-57.4754524783487,
-47.1852625));
#260974=CARTESIAN_POINT('Ctrl Pts',(-46.2995345158897,-58.5098228615615,
-47.1269291666667));
#260975=CARTESIAN_POINT('Ctrl Pts',(-45.7023404967,-59.5441932447742,-47.0685958333333));
#260976=CARTESIAN_POINT('Ctrl Pts',(-44.5079524583208,-59.5441932447742,
-47.0102625));
#260977=CARTESIAN_POINT('Ctrl Pts',(-43.3135644199415,-59.5441932447742,
-46.9519291666667));
#260978=CARTESIAN_POINT('Ctrl Pts',(-42.7163704007519,-58.5098228615615,
-46.8935958333333));
#260979=CARTESIAN_POINT('Ctrl Pts',(-42.1191763815623,-57.4754524783487,
-46.8352625));
#260980=CARTESIAN_POINT('Ctrl Pts',(-42.7163704007519,-56.4410820951361,
-46.7769291666667));
#260981=CARTESIAN_POINT('Ctrl Pts',(-43.3135644199415,-55.4067117119233,
-46.7185958333333));
#260982=CARTESIAN_POINT('Ctrl Pts',(-44.5079524583208,-55.4067117119234,
-46.6602625));
#260983=CARTESIAN_POINT('Ctrl Pts',(-45.7023404967,-55.4067117119233,-46.6019291666667));
#260984=CARTESIAN_POINT('Ctrl Pts',(-46.2995345158897,-56.4410820951361,
-46.5435958333334));
#260985=CARTESIAN_POINT('Ctrl Pts',(-46.8967285350793,-57.4754524783487,
-46.4852625));
#260986=CARTESIAN_POINT('Ctrl Pts',(-46.2995345158897,-58.5098228615615,
-46.4269291666667));
#260987=CARTESIAN_POINT('Ctrl Pts',(-45.7023404967,-59.5441932447742,-46.3685958333333));
#260988=CARTESIAN_POINT('Ctrl Pts',(-44.5079524583208,-59.5441932447742,
-46.3102625));
#260989=CARTESIAN_POINT('Ctrl Pts',(-43.3135644199415,-59.5441932447742,
-46.2519291666667));
#260990=CARTESIAN_POINT('Ctrl Pts',(-42.7163704007519,-58.5098228615615,
-46.1935958333333));
#260991=CARTESIAN_POINT('Ctrl Pts',(-42.1191763815623,-57.4754524783487,
-46.1352625));
#260992=CARTESIAN_POINT('Ctrl Pts',(-42.7163704007519,-56.4410820951361,
-46.0769291666667));
#260993=CARTESIAN_POINT('Ctrl Pts',(-43.3135644199415,-55.4067117119233,
-46.0185958333334));
#260994=CARTESIAN_POINT('Ctrl Pts',(-44.5079524583208,-55.4067117119234,
-45.9602625));
#260995=CARTESIAN_POINT('Ctrl Pts',(-45.7023404967,-55.4067117119233,-45.9019291666667));
#260996=CARTESIAN_POINT('Ctrl Pts',(-46.2995345158897,-56.4410820951361,
-45.8435958333333));
#260997=CARTESIAN_POINT('Ctrl Pts',(-46.8967285350793,-57.4754524783487,
-45.7852625));
#260998=CARTESIAN_POINT('Ctrl Pts',(-46.2995345158897,-58.5098228615615,
-45.7269291666667));
#260999=CARTESIAN_POINT('Ctrl Pts',(-45.7023404967,-59.5441932447742,-45.6685958333334));
#261000=CARTESIAN_POINT('Ctrl Pts',(-44.5079524583208,-59.5441932447742,
-45.6102625));
#261001=CARTESIAN_POINT('Ctrl Pts',(-43.3135644199415,-59.5441932447742,
-45.5519291666667));
#261002=CARTESIAN_POINT('Ctrl Pts',(-42.7163704007519,-58.5098228615615,
-45.4935958333333));
#261003=CARTESIAN_POINT('Ctrl Pts',(-42.1191763815623,-57.4754524783487,
-45.4352625));
#261004=CARTESIAN_POINT('Ctrl Pts',(-42.7163704007519,-56.4410820951361,
-45.3769291666667));
#261005=CARTESIAN_POINT('Ctrl Pts',(-43.3135644199415,-55.4067117119233,
-45.3185958333333));
#261006=CARTESIAN_POINT('Ctrl Pts',(-44.5079524583208,-55.4067117119234,
-45.2602625));
#261007=CARTESIAN_POINT('Ctrl Pts',(-45.7023404967,-55.4067117119233,-45.2019291666667));
#261008=CARTESIAN_POINT('Ctrl Pts',(-46.2995345158897,-56.4410820951361,
-45.1435958333334));
#261009=CARTESIAN_POINT('Ctrl Pts',(-46.8967285350793,-57.4754524783487,
-45.0852625));
#261010=CARTESIAN_POINT('Ctrl Pts',(-46.2995345158897,-58.5098228615615,
-45.0269291666667));
#261011=CARTESIAN_POINT('Ctrl Pts',(-45.7023404967,-59.5441932447742,-44.9685958333334));
#261012=CARTESIAN_POINT('Ctrl Pts',(-44.5079524583208,-59.5441932447742,
-44.9102625));
#261013=CARTESIAN_POINT('Ctrl Pts',(-43.3135644199415,-59.5441932447742,
-44.8519291666667));
#261014=CARTESIAN_POINT('Ctrl Pts',(-42.7163704007519,-58.5098228615615,
-44.7935958333333));
#261015=CARTESIAN_POINT('Ctrl Pts',(-42.1191763815623,-57.4754524783487,
-44.7352625));
#261016=CARTESIAN_POINT('Ctrl Pts',(-42.7163704007519,-56.4410820951361,
-44.6769291666667));
#261017=CARTESIAN_POINT('Ctrl Pts',(-43.3135644199415,-55.4067117119233,
-44.6185958333334));
#261018=CARTESIAN_POINT('Ctrl Pts',(-44.5079524583208,-55.4067117119234,
-44.5602625));
#261019=CARTESIAN_POINT('Ctrl Pts',(-45.7023404967,-55.4067117119233,-44.5019291666667));
#261020=CARTESIAN_POINT('Ctrl Pts',(-46.2995345158897,-56.4410820951361,
-44.4435958333333));
#261021=CARTESIAN_POINT('Ctrl Pts',(-46.8967285350793,-57.4754524783487,
-44.3852625));
#261022=CARTESIAN_POINT('Ctrl Pts',(-46.2995345158897,-58.5098228615615,
-44.3269291666667));
#261023=CARTESIAN_POINT('Ctrl Pts',(-45.7023404967,-59.5441932447742,-44.2685958333334));
#261024=CARTESIAN_POINT('Ctrl Pts',(-44.5079524583208,-59.5441932447742,
-44.2102625));
#261025=CARTESIAN_POINT('Ctrl Pts',(-43.3135644199415,-59.5441932447742,
-44.1519291666667));
#261026=CARTESIAN_POINT('Ctrl Pts',(-42.7163704007519,-58.5098228615615,
-44.0935958333334));
#261027=CARTESIAN_POINT('Ctrl Pts',(-42.1191763815623,-57.4754524783487,
-44.0352625));
#261028=CARTESIAN_POINT('Ctrl Pts',(-42.7163704007519,-56.4410820951361,
-43.9769291666667));
#261029=CARTESIAN_POINT('Ctrl Pts',(-43.3135644199415,-55.4067117119233,
-43.9185958333334));
#261030=CARTESIAN_POINT('Ctrl Pts',(-44.5079524583208,-55.4067117119234,
-43.8602625));
#261031=CARTESIAN_POINT('Ctrl Pts',(-45.7023404967,-55.4067117119233,-43.8019291666667));
#261032=CARTESIAN_POINT('Ctrl Pts',(-46.2995345158897,-56.4410820951361,
-43.7435958333334));
#261033=CARTESIAN_POINT('Ctrl Pts',(-46.8967285350793,-57.4754524783487,
-43.6852625));
#261034=CARTESIAN_POINT('Ctrl Pts',(-46.2995345158897,-58.5098228615615,
-43.6269291666667));
#261035=CARTESIAN_POINT('Ctrl Pts',(-45.7023404967,-59.5441932447742,-43.5685958333334));
#261036=CARTESIAN_POINT('Ctrl Pts',(-44.5079524583208,-59.5441932447742,
-43.5102625));
#261037=CARTESIAN_POINT('Ctrl Pts',(-43.3135644199415,-59.5441932447742,
-43.4519291666667));
#261038=CARTESIAN_POINT('Ctrl Pts',(-42.7163704007519,-58.5098228615615,
-43.3935958333334));
#261039=CARTESIAN_POINT('Ctrl Pts',(-42.1191763815623,-57.4754524783487,
-43.3352625));
#261040=CARTESIAN_POINT('Ctrl Pts',(-42.7163704007519,-56.4410820951361,
-43.2769291666667));
#261041=CARTESIAN_POINT('Ctrl Pts',(-43.3135644199415,-55.4067117119233,
-43.2185958333334));
#261042=CARTESIAN_POINT('Ctrl Pts',(-44.5079524583208,-55.4067117119234,
-43.1602625));
#261043=CARTESIAN_POINT('Ctrl Pts',(-45.7023404967,-55.4067117119233,-43.1019291666667));
#261044=CARTESIAN_POINT('Ctrl Pts',(-46.2995345158897,-56.4410820951361,
-43.0435958333334));
#261045=CARTESIAN_POINT('Ctrl Pts',(-46.8967285350793,-57.4754524783487,
-42.9852625));
#261046=CARTESIAN_POINT('Ctrl Pts',(-46.2995345158897,-58.5098228615615,
-42.9269291666667));
#261047=CARTESIAN_POINT('Ctrl Pts',(-45.7023404967,-59.5441932447742,-42.8685958333333));
#261048=CARTESIAN_POINT('Ctrl Pts',(-44.5079524583208,-59.5441932447742,
-42.8102625));
#261049=CARTESIAN_POINT('Ctrl Pts',(-43.3135644199415,-59.5441932447742,
-42.7519291666667));
#261050=CARTESIAN_POINT('Ctrl Pts',(-42.7163704007519,-58.5098228615615,
-42.6935958333333));
#261051=CARTESIAN_POINT('Ctrl Pts',(-42.1191763815623,-57.4754524783487,
-42.6352625));
#261052=CARTESIAN_POINT('Ctrl Pts',(-42.7163704007519,-56.4410820951361,
-42.5769291666667));
#261053=CARTESIAN_POINT('Ctrl Pts',(-43.3135644199415,-55.4067117119233,
-42.5185958333333));
#261054=CARTESIAN_POINT('Ctrl Pts',(-44.5079524583208,-55.4067117119234,
-42.4602625));
#261055=CARTESIAN_POINT('Ctrl Pts',(-45.7023404967,-55.4067117119233,-42.4019291666666));
#261056=CARTESIAN_POINT('Ctrl Pts',(-46.2995345158897,-56.4410820951361,
-42.3435958333334));
#261057=CARTESIAN_POINT('Ctrl Pts',(-46.8967285350793,-57.4754524783487,
-42.2852625));
#261058=CARTESIAN_POINT('Ctrl Pts',(-46.2995345158897,-58.5098228615615,
-42.2269291666667));
#261059=CARTESIAN_POINT('Ctrl Pts',(-45.7023404967,-59.5441932447742,-42.1685958333333));
#261060=CARTESIAN_POINT('Ctrl Pts',(-44.5079524583208,-59.5441932447742,
-42.1102625));
#261061=CARTESIAN_POINT('Ctrl Pts',(-43.3135644199415,-59.5441932447742,
-42.0519291666667));
#261062=CARTESIAN_POINT('Ctrl Pts',(-42.7163704007519,-58.5098228615615,
-41.9935958333334));
#261063=CARTESIAN_POINT('Ctrl Pts',(-42.1191763815623,-57.4754524783487,
-41.9352625));
#261064=CARTESIAN_POINT('Ctrl Pts',(-42.7163704007519,-56.4410820951361,
-41.8769291666667));
#261065=CARTESIAN_POINT('Ctrl Pts',(-43.3135644199415,-55.4067117119233,
-41.8185958333333));
#261066=CARTESIAN_POINT('Ctrl Pts',(-44.5079524583208,-55.4067117119234,
-41.7602625));
#261067=CARTESIAN_POINT('Ctrl Pts',(-45.7023404967,-55.4067117119233,-41.7019291666667));
#261068=CARTESIAN_POINT('Ctrl Pts',(-46.2995345158897,-56.4410820951361,
-41.6435958333334));
#261069=CARTESIAN_POINT('Ctrl Pts',(-46.8967285350793,-57.4754524783487,
-41.5852625));
#261070=CARTESIAN_POINT('Ctrl Pts',(-46.2995345158897,-58.5098228615615,
-41.5269291666667));
#261071=CARTESIAN_POINT('Ctrl Pts',(-45.7023404967,-59.5441932447742,-41.4685958333333));
#261072=CARTESIAN_POINT('Ctrl Pts',(-44.5079524583208,-59.5441932447742,
-41.4102625));
#261073=CARTESIAN_POINT('Ctrl Pts',(-43.3135644199415,-59.5441932447742,
-41.3519291666666));
#261074=CARTESIAN_POINT('Ctrl Pts',(-42.7163704007519,-58.5098228615615,
-41.2935958333334));
#261075=CARTESIAN_POINT('Ctrl Pts',(-42.1191763815623,-57.4754524783487,
-41.2352625));
#261076=CARTESIAN_POINT('Ctrl Pts',(-42.7163704007519,-56.4410820951361,
-41.1769291666667));
#261077=CARTESIAN_POINT('Ctrl Pts',(-43.3135644199415,-55.4067117119233,
-41.1185958333333));
#261078=CARTESIAN_POINT('Ctrl Pts',(-44.5079524583208,-55.4067117119234,
-41.0602625));
#261079=CARTESIAN_POINT('Ctrl Pts',(-45.7023404967,-55.4067117119233,-41.0019291666666));
#261080=CARTESIAN_POINT('Ctrl Pts',(-46.2995345158897,-56.4410820951361,
-40.9435958333334));
#261081=CARTESIAN_POINT('Ctrl Pts',(-46.8967285350793,-57.4754524783487,
-40.8852625));
#261082=CARTESIAN_POINT('Ctrl Pts',(-46.2995345158897,-58.5098228615615,
-40.8269291666667));
#261083=CARTESIAN_POINT('Ctrl Pts',(-45.7023404967,-59.5441932447742,-40.7685958333333));
#261084=CARTESIAN_POINT('Ctrl Pts',(-44.5079524583208,-59.5441932447742,
-40.7102625));
#261085=CARTESIAN_POINT('Ctrl Pts',(-43.3135644199415,-59.5441932447742,
-40.6519291666667));
#261086=CARTESIAN_POINT('Ctrl Pts',(-42.7163704007519,-58.5098228615615,
-40.5935958333334));
#261087=CARTESIAN_POINT('Ctrl Pts',(-42.1191763815623,-57.4754524783487,
-40.5352625));
#261088=CARTESIAN_POINT('Ctrl Pts',(-42.7163704007519,-56.4410820951361,
-40.4769291666667));
#261089=CARTESIAN_POINT('Ctrl Pts',(-43.3135644199415,-55.4067117119233,
-40.4185958333333));
#261090=CARTESIAN_POINT('Ctrl Pts',(-44.5079524583208,-55.4067117119234,
-40.3602625));
#261091=CARTESIAN_POINT('Ctrl Pts',(-45.7023404967,-55.4067117119233,-40.3019291666667));
#261092=CARTESIAN_POINT('Ctrl Pts',(-46.2995345158897,-56.4410820951361,
-40.2435958333334));
#261093=CARTESIAN_POINT('Ctrl Pts',(-46.8967285350793,-57.4754524783487,
-40.1852625));
#261094=CARTESIAN_POINT('Ctrl Pts',(-46.2995345158897,-58.5098228615615,
-40.1269291666666));
#261095=CARTESIAN_POINT('Ctrl Pts',(-45.7023404967,-59.5441932447742,-40.0685958333333));
#261096=CARTESIAN_POINT('Ctrl Pts',(-44.5079524583208,-59.5441932447742,
-40.0102625));
#261097=CARTESIAN_POINT('Ctrl Pts',(-43.3135644199415,-59.5441932447742,
-39.9519291666667));
#261098=CARTESIAN_POINT('Ctrl Pts',(-42.7163704007519,-58.5098228615615,
-39.8935958333334));
#261099=CARTESIAN_POINT('Ctrl Pts',(-42.1191763815623,-57.4754524783487,
-39.8352625));
#261100=CARTESIAN_POINT('Ctrl Pts',(-42.7163704007519,-56.4410820951361,
-39.7769291666667));
#261101=CARTESIAN_POINT('Ctrl Pts',(-43.3135644199415,-55.4067117119233,
-39.7185958333334));
#261102=CARTESIAN_POINT('Ctrl Pts',(-44.5079524583208,-55.4067117119234,
-39.6602625));
#261103=CARTESIAN_POINT('Ctrl Pts',(-45.7023404967,-55.4067117119233,-39.6019291666667));
#261104=CARTESIAN_POINT('Ctrl Pts',(-46.2995345158897,-56.4410820951361,
-39.5435958333333));
#261105=CARTESIAN_POINT('Ctrl Pts',(-46.8967285350793,-57.4754524783487,
-39.4852625));
#261106=CARTESIAN_POINT('Ctrl Pts',(-46.2995345158897,-58.5098228615615,
-39.4269291666667));
#261107=CARTESIAN_POINT('Ctrl Pts',(-45.7023404967,-59.5441932447742,-39.3685958333334));
#261108=CARTESIAN_POINT('Ctrl Pts',(-44.5079524583208,-59.5441932447742,
-39.3102625));
#261109=CARTESIAN_POINT('Ctrl Pts',(-43.3135644199415,-59.5441932447742,
-39.2519291666667));
#261110=CARTESIAN_POINT('Ctrl Pts',(-42.7163704007519,-58.5098228615615,
-39.1935958333334));
#261111=CARTESIAN_POINT('Ctrl Pts',(-42.1191763815623,-57.4754524783487,
-39.1352625));
#261112=CARTESIAN_POINT('Ctrl Pts',(-42.7163704007519,-56.4410820951361,
-39.0769291666667));
#261113=CARTESIAN_POINT('Ctrl Pts',(-43.3135644199415,-55.4067117119233,
-39.0185958333334));
#261114=CARTESIAN_POINT('Ctrl Pts',(-44.5079524583208,-55.4067117119234,
-38.9602625));
#261115=CARTESIAN_POINT('Ctrl Pts',(-45.7023404967,-55.4067117119233,-38.9019291666667));
#261116=CARTESIAN_POINT('Ctrl Pts',(-46.2995345158897,-56.4410820951361,
-38.8435958333333));
#261117=CARTESIAN_POINT('Ctrl Pts',(-46.8967285350793,-57.4754524783487,
-38.7852625));
#261118=CARTESIAN_POINT('Ctrl Pts',(-46.2995345158897,-58.5098228615615,
-38.7269291666667));
#261119=CARTESIAN_POINT('Ctrl Pts',(-45.7023404967,-59.5441932447742,-38.6685958333334));
#261120=CARTESIAN_POINT('Ctrl Pts',(-44.5079524583208,-59.5441932447742,
-38.6102625));
#261121=CARTESIAN_POINT('Ctrl Pts',(-43.3135644199415,-59.5441932447742,
-38.5519291666667));
#261122=CARTESIAN_POINT('Ctrl Pts',(-42.7163704007519,-58.5098228615615,
-38.4935958333334));
#261123=CARTESIAN_POINT('Ctrl Pts',(-42.1191763815623,-57.4754524783487,
-38.4352625));
#261124=CARTESIAN_POINT('Ctrl Pts',(-42.7163704007519,-56.4410820951361,
-38.3769291666667));
#261125=CARTESIAN_POINT('Ctrl Pts',(-43.3135644199415,-55.4067117119233,
-38.3185958333333));
#261126=CARTESIAN_POINT('Ctrl Pts',(-44.5079524583208,-55.4067117119234,
-38.2602625));
#261127=CARTESIAN_POINT('Ctrl Pts',(-45.7023404967,-55.4067117119233,-38.2019291666667));
#261128=CARTESIAN_POINT('Ctrl Pts',(-46.2995345158897,-56.4410820951361,
-38.1435958333334));
#261129=CARTESIAN_POINT('Ctrl Pts',(-46.8967285350793,-57.4754524783487,
-38.0852625));
#261130=CARTESIAN_POINT('Ctrl Pts',(-46.2995345158897,-58.5098228615615,
-38.0269291666667));
#261131=CARTESIAN_POINT('Ctrl Pts',(-45.7023404967,-59.5441932447742,-37.9685958333333));
#261132=CARTESIAN_POINT('Ctrl Pts',(-44.5079524583208,-59.5441932447742,
-37.9102625));
#261133=CARTESIAN_POINT('Ctrl Pts',(-43.3135644199415,-59.5441932447742,
-37.8519291666667));
#261134=CARTESIAN_POINT('Ctrl Pts',(-42.7163704007519,-58.5098228615615,
-37.7935958333334));
#261135=CARTESIAN_POINT('Ctrl Pts',(-42.1191763815623,-57.4754524783487,
-37.7352625));
#261136=CARTESIAN_POINT('Ctrl Pts',(-42.7163704007519,-56.4410820951361,
-37.6769291666667));
#261137=CARTESIAN_POINT('Ctrl Pts',(-43.3135644199415,-55.4067117119233,
-37.6185958333333));
#261138=CARTESIAN_POINT('Ctrl Pts',(-44.5079524583208,-55.4067117119234,
-37.5602625));
#261139=CARTESIAN_POINT('Ctrl Pts',(-45.7023404967,-55.4067117119233,-37.5019291666667));
#261140=CARTESIAN_POINT('Ctrl Pts',(-46.2995345158897,-56.4410820951361,
-37.4435958333333));
#261141=CARTESIAN_POINT('Ctrl Pts',(-46.8967285350793,-57.4754524783487,
-37.3852625));
#261142=CARTESIAN_POINT('Ctrl Pts',(-46.2995345158897,-58.5098228615615,
-37.3269291666667));
#261143=CARTESIAN_POINT('Ctrl Pts',(-45.7023404967,-59.5441932447742,-37.2685958333333));
#261144=CARTESIAN_POINT('Ctrl Pts',(-44.5079524583208,-59.5441932447742,
-37.2102625));
#261145=CARTESIAN_POINT('Ctrl Pts',(-43.3135644199415,-59.5441932447742,
-37.1519291666667));
#261146=CARTESIAN_POINT('Ctrl Pts',(-42.7163704007519,-58.5098228615615,
-37.0935958333333));
#261147=CARTESIAN_POINT('Ctrl Pts',(-42.1191763815623,-57.4754524783487,
-37.0352625));
#261148=CARTESIAN_POINT('Ctrl Pts',(-42.7163704007519,-56.4410820951361,
-36.9769291666667));
#261149=CARTESIAN_POINT('Ctrl Pts',(-43.3135644199415,-55.4067117119233,
-36.9185958333333));
#261150=CARTESIAN_POINT('Ctrl Pts',(-44.5079524583208,-55.4067117119234,
-36.8602625));
#261151=CARTESIAN_POINT('Ctrl Pts',(-45.7023404967,-55.4067117119233,-36.8019291666666));
#261152=CARTESIAN_POINT('Ctrl Pts',(-46.2995345158897,-56.4410820951361,
-36.7435958333334));
#261153=CARTESIAN_POINT('Ctrl Pts',(-46.8967285350793,-57.4754524783487,
-36.6852625));
#261154=CARTESIAN_POINT('Ctrl Pts',(-46.2995345158897,-58.5098228615615,
-36.6269291666667));
#261155=CARTESIAN_POINT('Ctrl Pts',(-46.222006582932,-58.64410518045,-36.6193563132714));
#261156=CARTESIAN_POINT('Ctrl Pts',(-46.1253278975281,-58.7653303978899,
-36.611216324118));
#261157=CARTESIAN_POINT('Ctrl Pts',(-44.5079524583208,-59.1441976086192,
-52.8412000882087));
#261158=CARTESIAN_POINT('Ctrl Pts',(-43.5445020081503,-59.1441976086192,
-52.7828667548754));
#261159=CARTESIAN_POINT('Ctrl Pts',(-43.062776783065,-58.309825043484,-52.7245334215421));
#261160=CARTESIAN_POINT('Ctrl Pts',(-42.5810515579797,-57.4754524783487,
-52.6662000882087));
#261161=CARTESIAN_POINT('Ctrl Pts',(-43.062776783065,-56.6410799132135,
-52.6078667548754));
#261162=CARTESIAN_POINT('Ctrl Pts',(-43.5445020081503,-55.8067073480783,
-52.549533421542));
#261163=CARTESIAN_POINT('Ctrl Pts',(-44.5079524583208,-55.8067073480783,
-52.4912000882087));
#261164=CARTESIAN_POINT('Ctrl Pts',(-45.4714029084913,-55.8067073480783,
-52.4328667548755));
#261165=CARTESIAN_POINT('Ctrl Pts',(-45.9531281335766,-56.6410799132135,
-52.3745334215421));
#261166=CARTESIAN_POINT('Ctrl Pts',(-46.4348533586618,-57.4754524783487,
-52.3162000882088));
#261167=CARTESIAN_POINT('Ctrl Pts',(-45.9531281335766,-58.309825043484,
-52.2578667548754));
#261168=CARTESIAN_POINT('Ctrl Pts',(-45.4714029084913,-59.1441976086192,
-52.1995334215421));
#261169=CARTESIAN_POINT('Ctrl Pts',(-44.5079524583208,-59.1441976086192,
-52.1412000882087));
#261170=CARTESIAN_POINT('Ctrl Pts',(-43.5445020081503,-59.1441976086192,
-52.0828667548754));
#261171=CARTESIAN_POINT('Ctrl Pts',(-43.062776783065,-58.309825043484,-52.024533421542));
#261172=CARTESIAN_POINT('Ctrl Pts',(-42.5810515579797,-57.4754524783487,
-51.9662000882087));
#261173=CARTESIAN_POINT('Ctrl Pts',(-43.062776783065,-56.6410799132135,
-51.9078667548754));
#261174=CARTESIAN_POINT('Ctrl Pts',(-43.5445020081503,-55.8067073480783,
-51.8495334215421));
#261175=CARTESIAN_POINT('Ctrl Pts',(-44.5079524583208,-55.8067073480783,
-51.7912000882087));
#261176=CARTESIAN_POINT('Ctrl Pts',(-45.4714029084913,-55.8067073480783,
-51.7328667548754));
#261177=CARTESIAN_POINT('Ctrl Pts',(-45.9531281335766,-56.6410799132135,
-51.6745334215421));
#261178=CARTESIAN_POINT('Ctrl Pts',(-46.4348533586618,-57.4754524783487,
-51.6162000882087));
#261179=CARTESIAN_POINT('Ctrl Pts',(-45.9531281335766,-58.309825043484,
-51.5578667548754));
#261180=CARTESIAN_POINT('Ctrl Pts',(-45.4714029084913,-59.1441976086192,
-51.4995334215421));
#261181=CARTESIAN_POINT('Ctrl Pts',(-44.5079524583208,-59.1441976086192,
-51.4412000882087));
#261182=CARTESIAN_POINT('Ctrl Pts',(-43.5445020081503,-59.1441976086192,
-51.3828667548754));
#261183=CARTESIAN_POINT('Ctrl Pts',(-43.062776783065,-58.309825043484,-51.3245334215421));
#261184=CARTESIAN_POINT('Ctrl Pts',(-42.5810515579797,-57.4754524783487,
-51.2662000882087));
#261185=CARTESIAN_POINT('Ctrl Pts',(-43.062776783065,-56.6410799132135,
-51.2078667548754));
#261186=CARTESIAN_POINT('Ctrl Pts',(-43.5445020081503,-55.8067073480783,
-51.1495334215421));
#261187=CARTESIAN_POINT('Ctrl Pts',(-44.5079524583208,-55.8067073480783,
-51.0912000882087));
#261188=CARTESIAN_POINT('Ctrl Pts',(-45.4714029084913,-55.8067073480783,
-51.0328667548754));
#261189=CARTESIAN_POINT('Ctrl Pts',(-45.9531281335766,-56.6410799132135,
-50.974533421542));
#261190=CARTESIAN_POINT('Ctrl Pts',(-46.4348533586618,-57.4754524783487,
-50.9162000882087));
#261191=CARTESIAN_POINT('Ctrl Pts',(-45.9531281335766,-58.309825043484,
-50.8578667548754));
#261192=CARTESIAN_POINT('Ctrl Pts',(-45.4714029084913,-59.1441976086192,
-50.7995334215421));
#261193=CARTESIAN_POINT('Ctrl Pts',(-44.5079524583208,-59.1441976086192,
-50.7412000882087));
#261194=CARTESIAN_POINT('Ctrl Pts',(-43.5445020081503,-59.1441976086192,
-50.6828667548754));
#261195=CARTESIAN_POINT('Ctrl Pts',(-43.062776783065,-58.309825043484,-50.624533421542));
#261196=CARTESIAN_POINT('Ctrl Pts',(-42.5810515579797,-57.4754524783487,
-50.5662000882087));
#261197=CARTESIAN_POINT('Ctrl Pts',(-43.062776783065,-56.6410799132135,
-50.5078667548754));
#261198=CARTESIAN_POINT('Ctrl Pts',(-43.5445020081503,-55.8067073480783,
-50.4495334215421));
#261199=CARTESIAN_POINT('Ctrl Pts',(-44.5079524583208,-55.8067073480783,
-50.3912000882087));
#261200=CARTESIAN_POINT('Ctrl Pts',(-45.4714029084913,-55.8067073480783,
-50.3328667548754));
#261201=CARTESIAN_POINT('Ctrl Pts',(-45.9531281335766,-56.6410799132135,
-50.2745334215421));
#261202=CARTESIAN_POINT('Ctrl Pts',(-46.4348533586618,-57.4754524783487,
-50.2162000882088));
#261203=CARTESIAN_POINT('Ctrl Pts',(-45.9531281335766,-58.309825043484,
-50.1578667548754));
#261204=CARTESIAN_POINT('Ctrl Pts',(-45.4714029084913,-59.1441976086192,
-50.0995334215421));
#261205=CARTESIAN_POINT('Ctrl Pts',(-44.5079524583208,-59.1441976086192,
-50.0412000882087));
#261206=CARTESIAN_POINT('Ctrl Pts',(-43.5445020081503,-59.1441976086192,
-49.9828667548755));
#261207=CARTESIAN_POINT('Ctrl Pts',(-43.062776783065,-58.309825043484,-49.9245334215421));
#261208=CARTESIAN_POINT('Ctrl Pts',(-42.5810515579797,-57.4754524783487,
-49.8662000882087));
#261209=CARTESIAN_POINT('Ctrl Pts',(-43.062776783065,-56.6410799132135,
-49.8078667548754));
#261210=CARTESIAN_POINT('Ctrl Pts',(-43.5445020081503,-55.8067073480783,
-49.7495334215421));
#261211=CARTESIAN_POINT('Ctrl Pts',(-44.5079524583208,-55.8067073480783,
-49.6912000882087));
#261212=CARTESIAN_POINT('Ctrl Pts',(-45.4714029084913,-55.8067073480783,
-49.6328667548754));
#261213=CARTESIAN_POINT('Ctrl Pts',(-45.9531281335766,-56.6410799132135,
-49.5745334215421));
#261214=CARTESIAN_POINT('Ctrl Pts',(-46.4348533586618,-57.4754524783487,
-49.5162000882088));
#261215=CARTESIAN_POINT('Ctrl Pts',(-45.9531281335766,-58.309825043484,
-49.4578667548754));
#261216=CARTESIAN_POINT('Ctrl Pts',(-45.4714029084913,-59.1441976086192,
-49.3995334215421));
#261217=CARTESIAN_POINT('Ctrl Pts',(-44.5079524583208,-59.1441976086192,
-49.3412000882087));
#261218=CARTESIAN_POINT('Ctrl Pts',(-43.5445020081503,-59.1441976086192,
-49.2828667548754));
#261219=CARTESIAN_POINT('Ctrl Pts',(-43.062776783065,-58.309825043484,-49.2245334215421));
#261220=CARTESIAN_POINT('Ctrl Pts',(-42.5810515579797,-57.4754524783487,
-49.1662000882087));
#261221=CARTESIAN_POINT('Ctrl Pts',(-43.062776783065,-56.6410799132135,
-49.1078667548754));
#261222=CARTESIAN_POINT('Ctrl Pts',(-43.5445020081503,-55.8067073480783,
-49.0495334215421));
#261223=CARTESIAN_POINT('Ctrl Pts',(-44.5079524583208,-55.8067073480783,
-48.9912000882087));
#261224=CARTESIAN_POINT('Ctrl Pts',(-45.4714029084913,-55.8067073480783,
-48.9328667548754));
#261225=CARTESIAN_POINT('Ctrl Pts',(-45.9531281335766,-56.6410799132135,
-48.8745334215421));
#261226=CARTESIAN_POINT('Ctrl Pts',(-46.4348533586618,-57.4754524783487,
-48.8162000882088));
#261227=CARTESIAN_POINT('Ctrl Pts',(-45.9531281335766,-58.309825043484,
-48.7578667548754));
#261228=CARTESIAN_POINT('Ctrl Pts',(-45.4714029084913,-59.1441976086192,
-48.6995334215421));
#261229=CARTESIAN_POINT('Ctrl Pts',(-44.5079524583208,-59.1441976086192,
-48.6412000882087));
#261230=CARTESIAN_POINT('Ctrl Pts',(-43.5445020081503,-59.1441976086192,
-48.5828667548754));
#261231=CARTESIAN_POINT('Ctrl Pts',(-43.062776783065,-58.309825043484,-48.5245334215421));
#261232=CARTESIAN_POINT('Ctrl Pts',(-42.5810515579797,-57.4754524783487,
-48.4662000882088));
#261233=CARTESIAN_POINT('Ctrl Pts',(-43.062776783065,-56.6410799132135,
-48.4078667548754));
#261234=CARTESIAN_POINT('Ctrl Pts',(-43.5445020081503,-55.8067073480783,
-48.3495334215421));
#261235=CARTESIAN_POINT('Ctrl Pts',(-44.5079524583208,-55.8067073480783,
-48.2912000882087));
#261236=CARTESIAN_POINT('Ctrl Pts',(-45.4714029084913,-55.8067073480783,
-48.2328667548754));
#261237=CARTESIAN_POINT('Ctrl Pts',(-45.9531281335766,-56.6410799132135,
-48.1745334215421));
#261238=CARTESIAN_POINT('Ctrl Pts',(-46.4348533586618,-57.4754524783487,
-48.1162000882087));
#261239=CARTESIAN_POINT('Ctrl Pts',(-45.9531281335766,-58.309825043484,
-48.0578667548754));
#261240=CARTESIAN_POINT('Ctrl Pts',(-45.4714029084913,-59.1441976086192,
-47.9995334215421));
#261241=CARTESIAN_POINT('Ctrl Pts',(-44.5079524583208,-59.1441976086192,
-47.9412000882087));
#261242=CARTESIAN_POINT('Ctrl Pts',(-43.5445020081503,-59.1441976086192,
-47.8828667548754));
#261243=CARTESIAN_POINT('Ctrl Pts',(-43.062776783065,-58.309825043484,-47.824533421542));
#261244=CARTESIAN_POINT('Ctrl Pts',(-42.5810515579797,-57.4754524783487,
-47.7662000882088));
#261245=CARTESIAN_POINT('Ctrl Pts',(-43.062776783065,-56.6410799132135,
-47.7078667548754));
#261246=CARTESIAN_POINT('Ctrl Pts',(-43.5445020081503,-55.8067073480783,
-47.6495334215421));
#261247=CARTESIAN_POINT('Ctrl Pts',(-44.5079524583208,-55.8067073480783,
-47.5912000882087));
#261248=CARTESIAN_POINT('Ctrl Pts',(-45.4714029084913,-55.8067073480783,
-47.5328667548754));
#261249=CARTESIAN_POINT('Ctrl Pts',(-45.9531281335766,-56.6410799132135,
-47.4745334215421));
#261250=CARTESIAN_POINT('Ctrl Pts',(-46.4348533586618,-57.4754524783487,
-47.4162000882087));
#261251=CARTESIAN_POINT('Ctrl Pts',(-45.9531281335766,-58.309825043484,
-47.3578667548754));
#261252=CARTESIAN_POINT('Ctrl Pts',(-45.4714029084913,-59.1441976086192,
-47.2995334215421));
#261253=CARTESIAN_POINT('Ctrl Pts',(-44.5079524583208,-59.1441976086192,
-47.2412000882087));
#261254=CARTESIAN_POINT('Ctrl Pts',(-43.5445020081503,-59.1441976086192,
-47.1828667548754));
#261255=CARTESIAN_POINT('Ctrl Pts',(-43.062776783065,-58.309825043484,-47.124533421542));
#261256=CARTESIAN_POINT('Ctrl Pts',(-42.5810515579797,-57.4754524783487,
-47.0662000882087));
#261257=CARTESIAN_POINT('Ctrl Pts',(-43.062776783065,-56.6410799132135,
-47.0078667548754));
#261258=CARTESIAN_POINT('Ctrl Pts',(-43.5445020081503,-55.8067073480783,
-46.9495334215421));
#261259=CARTESIAN_POINT('Ctrl Pts',(-44.5079524583208,-55.8067073480783,
-46.8912000882087));
#261260=CARTESIAN_POINT('Ctrl Pts',(-45.4714029084913,-55.8067073480783,
-46.8328667548754));
#261261=CARTESIAN_POINT('Ctrl Pts',(-45.9531281335766,-56.6410799132135,
-46.7745334215421));
#261262=CARTESIAN_POINT('Ctrl Pts',(-46.4348533586618,-57.4754524783487,
-46.7162000882087));
#261263=CARTESIAN_POINT('Ctrl Pts',(-45.9531281335766,-58.309825043484,
-46.6578667548754));
#261264=CARTESIAN_POINT('Ctrl Pts',(-45.4714029084913,-59.1441976086192,
-46.5995334215421));
#261265=CARTESIAN_POINT('Ctrl Pts',(-44.5079524583208,-59.1441976086192,
-46.5412000882087));
#261266=CARTESIAN_POINT('Ctrl Pts',(-43.5445020081503,-59.1441976086192,
-46.4828667548754));
#261267=CARTESIAN_POINT('Ctrl Pts',(-43.062776783065,-58.309825043484,-46.4245334215421));
#261268=CARTESIAN_POINT('Ctrl Pts',(-42.5810515579797,-57.4754524783487,
-46.3662000882087));
#261269=CARTESIAN_POINT('Ctrl Pts',(-43.062776783065,-56.6410799132135,
-46.3078667548754));
#261270=CARTESIAN_POINT('Ctrl Pts',(-43.5445020081503,-55.8067073480783,
-46.2495334215421));
#261271=CARTESIAN_POINT('Ctrl Pts',(-44.5079524583208,-55.8067073480783,
-46.1912000882087));
#261272=CARTESIAN_POINT('Ctrl Pts',(-45.4714029084913,-55.8067073480783,
-46.1328667548754));
#261273=CARTESIAN_POINT('Ctrl Pts',(-45.9531281335766,-56.6410799132135,
-46.0745334215421));
#261274=CARTESIAN_POINT('Ctrl Pts',(-46.4348533586618,-57.4754524783487,
-46.0162000882087));
#261275=CARTESIAN_POINT('Ctrl Pts',(-45.9531281335766,-58.309825043484,
-45.9578667548754));
#261276=CARTESIAN_POINT('Ctrl Pts',(-45.4714029084913,-59.1441976086192,
-45.8995334215421));
#261277=CARTESIAN_POINT('Ctrl Pts',(-44.5079524583208,-59.1441976086192,
-45.8412000882087));
#261278=CARTESIAN_POINT('Ctrl Pts',(-43.5445020081503,-59.1441976086192,
-45.7828667548754));
#261279=CARTESIAN_POINT('Ctrl Pts',(-43.062776783065,-58.309825043484,-45.724533421542));
#261280=CARTESIAN_POINT('Ctrl Pts',(-42.5810515579797,-57.4754524783487,
-45.6662000882087));
#261281=CARTESIAN_POINT('Ctrl Pts',(-43.062776783065,-56.6410799132135,
-45.6078667548754));
#261282=CARTESIAN_POINT('Ctrl Pts',(-43.5445020081503,-55.8067073480783,
-45.5495334215421));
#261283=CARTESIAN_POINT('Ctrl Pts',(-44.5079524583208,-55.8067073480783,
-45.4912000882087));
#261284=CARTESIAN_POINT('Ctrl Pts',(-45.4714029084913,-55.8067073480783,
-45.4328667548754));
#261285=CARTESIAN_POINT('Ctrl Pts',(-45.9531281335766,-56.6410799132135,
-45.3745334215421));
#261286=CARTESIAN_POINT('Ctrl Pts',(-46.4348533586618,-57.4754524783487,
-45.3162000882088));
#261287=CARTESIAN_POINT('Ctrl Pts',(-45.9531281335766,-58.309825043484,
-45.2578667548754));
#261288=CARTESIAN_POINT('Ctrl Pts',(-45.4714029084913,-59.1441976086192,
-45.1995334215421));
#261289=CARTESIAN_POINT('Ctrl Pts',(-44.5079524583208,-59.1441976086192,
-45.1412000882087));
#261290=CARTESIAN_POINT('Ctrl Pts',(-43.5445020081503,-59.1441976086192,
-45.0828667548754));
#261291=CARTESIAN_POINT('Ctrl Pts',(-43.062776783065,-58.309825043484,-45.0245334215421));
#261292=CARTESIAN_POINT('Ctrl Pts',(-42.5810515579797,-57.4754524783487,
-44.9662000882088));
#261293=CARTESIAN_POINT('Ctrl Pts',(-43.062776783065,-56.6410799132135,
-44.9078667548754));
#261294=CARTESIAN_POINT('Ctrl Pts',(-43.5445020081503,-55.8067073480783,
-44.8495334215421));
#261295=CARTESIAN_POINT('Ctrl Pts',(-44.5079524583208,-55.8067073480783,
-44.7912000882087));
#261296=CARTESIAN_POINT('Ctrl Pts',(-45.4714029084913,-55.8067073480783,
-44.7328667548754));
#261297=CARTESIAN_POINT('Ctrl Pts',(-45.9531281335766,-56.6410799132135,
-44.6745334215421));
#261298=CARTESIAN_POINT('Ctrl Pts',(-46.4348533586618,-57.4754524783487,
-44.6162000882088));
#261299=CARTESIAN_POINT('Ctrl Pts',(-45.9531281335766,-58.309825043484,
-44.5578667548754));
#261300=CARTESIAN_POINT('Ctrl Pts',(-45.4714029084913,-59.1441976086192,
-44.4995334215421));
#261301=CARTESIAN_POINT('Ctrl Pts',(-44.5079524583208,-59.1441976086192,
-44.4412000882087));
#261302=CARTESIAN_POINT('Ctrl Pts',(-43.5445020081503,-59.1441976086192,
-44.3828667548754));
#261303=CARTESIAN_POINT('Ctrl Pts',(-43.062776783065,-58.309825043484,-44.3245334215421));
#261304=CARTESIAN_POINT('Ctrl Pts',(-42.5810515579797,-57.4754524783487,
-44.2662000882088));
#261305=CARTESIAN_POINT('Ctrl Pts',(-43.062776783065,-56.6410799132135,
-44.2078667548754));
#261306=CARTESIAN_POINT('Ctrl Pts',(-43.5445020081503,-55.8067073480783,
-44.1495334215421));
#261307=CARTESIAN_POINT('Ctrl Pts',(-44.5079524583208,-55.8067073480783,
-44.0912000882087));
#261308=CARTESIAN_POINT('Ctrl Pts',(-45.4714029084913,-55.8067073480783,
-44.0328667548754));
#261309=CARTESIAN_POINT('Ctrl Pts',(-45.9531281335766,-56.6410799132135,
-43.9745334215421));
#261310=CARTESIAN_POINT('Ctrl Pts',(-46.4348533586618,-57.4754524783487,
-43.9162000882088));
#261311=CARTESIAN_POINT('Ctrl Pts',(-45.9531281335766,-58.309825043484,
-43.8578667548754));
#261312=CARTESIAN_POINT('Ctrl Pts',(-45.4714029084913,-59.1441976086192,
-43.7995334215421));
#261313=CARTESIAN_POINT('Ctrl Pts',(-44.5079524583208,-59.1441976086192,
-43.7412000882087));
#261314=CARTESIAN_POINT('Ctrl Pts',(-43.5445020081503,-59.1441976086192,
-43.6828667548754));
#261315=CARTESIAN_POINT('Ctrl Pts',(-43.062776783065,-58.309825043484,-43.6245334215421));
#261316=CARTESIAN_POINT('Ctrl Pts',(-42.5810515579797,-57.4754524783487,
-43.5662000882088));
#261317=CARTESIAN_POINT('Ctrl Pts',(-43.062776783065,-56.6410799132135,
-43.5078667548754));
#261318=CARTESIAN_POINT('Ctrl Pts',(-43.5445020081503,-55.8067073480783,
-43.4495334215421));
#261319=CARTESIAN_POINT('Ctrl Pts',(-44.5079524583208,-55.8067073480783,
-43.3912000882087));
#261320=CARTESIAN_POINT('Ctrl Pts',(-45.4714029084913,-55.8067073480783,
-43.3328667548754));
#261321=CARTESIAN_POINT('Ctrl Pts',(-45.9531281335766,-56.6410799132135,
-43.2745334215421));
#261322=CARTESIAN_POINT('Ctrl Pts',(-46.4348533586618,-57.4754524783487,
-43.2162000882088));
#261323=CARTESIAN_POINT('Ctrl Pts',(-45.9531281335766,-58.309825043484,
-43.1578667548754));
#261324=CARTESIAN_POINT('Ctrl Pts',(-45.4714029084913,-59.1441976086192,
-43.0995334215421));
#261325=CARTESIAN_POINT('Ctrl Pts',(-44.5079524583208,-59.1441976086192,
-43.0412000882087));
#261326=CARTESIAN_POINT('Ctrl Pts',(-43.5445020081503,-59.1441976086192,
-42.9828667548754));
#261327=CARTESIAN_POINT('Ctrl Pts',(-43.062776783065,-58.309825043484,-42.9245334215421));
#261328=CARTESIAN_POINT('Ctrl Pts',(-42.5810515579797,-57.4754524783487,
-42.8662000882087));
#261329=CARTESIAN_POINT('Ctrl Pts',(-43.062776783065,-56.6410799132135,
-42.8078667548754));
#261330=CARTESIAN_POINT('Ctrl Pts',(-43.5445020081503,-55.8067073480783,
-42.7495334215421));
#261331=CARTESIAN_POINT('Ctrl Pts',(-44.5079524583208,-55.8067073480783,
-42.6912000882087));
#261332=CARTESIAN_POINT('Ctrl Pts',(-45.4714029084913,-55.8067073480783,
-42.6328667548754));
#261333=CARTESIAN_POINT('Ctrl Pts',(-45.9531281335766,-56.6410799132135,
-42.5745334215421));
#261334=CARTESIAN_POINT('Ctrl Pts',(-46.4348533586618,-57.4754524783487,
-42.5162000882087));
#261335=CARTESIAN_POINT('Ctrl Pts',(-45.9531281335766,-58.309825043484,
-42.4578667548754));
#261336=CARTESIAN_POINT('Ctrl Pts',(-45.4714029084913,-59.1441976086192,
-42.3995334215421));
#261337=CARTESIAN_POINT('Ctrl Pts',(-44.5079524583208,-59.1441976086192,
-42.3412000882087));
#261338=CARTESIAN_POINT('Ctrl Pts',(-43.5445020081503,-59.1441976086192,
-42.2828667548754));
#261339=CARTESIAN_POINT('Ctrl Pts',(-43.062776783065,-58.309825043484,-42.2245334215421));
#261340=CARTESIAN_POINT('Ctrl Pts',(-42.5810515579797,-57.4754524783487,
-42.1662000882087));
#261341=CARTESIAN_POINT('Ctrl Pts',(-43.062776783065,-56.6410799132135,
-42.1078667548754));
#261342=CARTESIAN_POINT('Ctrl Pts',(-43.5445020081503,-55.8067073480783,
-42.0495334215421));
#261343=CARTESIAN_POINT('Ctrl Pts',(-44.5079524583208,-55.8067073480783,
-41.9912000882087));
#261344=CARTESIAN_POINT('Ctrl Pts',(-45.4714029084913,-55.8067073480783,
-41.9328667548754));
#261345=CARTESIAN_POINT('Ctrl Pts',(-45.9531281335766,-56.6410799132135,
-41.8745334215421));
#261346=CARTESIAN_POINT('Ctrl Pts',(-46.4348533586618,-57.4754524783487,
-41.8162000882087));
#261347=CARTESIAN_POINT('Ctrl Pts',(-45.9531281335766,-58.309825043484,
-41.7578667548754));
#261348=CARTESIAN_POINT('Ctrl Pts',(-45.4714029084913,-59.1441976086192,
-41.6995334215421));
#261349=CARTESIAN_POINT('Ctrl Pts',(-44.5079524583208,-59.1441976086192,
-41.6412000882087));
#261350=CARTESIAN_POINT('Ctrl Pts',(-43.5445020081503,-59.1441976086192,
-41.5828667548754));
#261351=CARTESIAN_POINT('Ctrl Pts',(-43.062776783065,-58.309825043484,-41.5245334215421));
#261352=CARTESIAN_POINT('Ctrl Pts',(-42.5810515579797,-57.4754524783487,
-41.4662000882087));
#261353=CARTESIAN_POINT('Ctrl Pts',(-43.062776783065,-56.6410799132135,
-41.4078667548754));
#261354=CARTESIAN_POINT('Ctrl Pts',(-43.5445020081503,-55.8067073480783,
-41.349533421542));
#261355=CARTESIAN_POINT('Ctrl Pts',(-44.5079524583208,-55.8067073480783,
-41.2912000882087));
#261356=CARTESIAN_POINT('Ctrl Pts',(-45.4714029084913,-55.8067073480783,
-41.2328667548754));
#261357=CARTESIAN_POINT('Ctrl Pts',(-45.9531281335766,-56.6410799132135,
-41.1745334215421));
#261358=CARTESIAN_POINT('Ctrl Pts',(-46.4348533586618,-57.4754524783487,
-41.1162000882087));
#261359=CARTESIAN_POINT('Ctrl Pts',(-45.9531281335766,-58.309825043484,
-41.0578667548754));
#261360=CARTESIAN_POINT('Ctrl Pts',(-45.4714029084913,-59.1441976086192,
-40.9995334215421));
#261361=CARTESIAN_POINT('Ctrl Pts',(-44.5079524583208,-59.1441976086192,
-40.9412000882087));
#261362=CARTESIAN_POINT('Ctrl Pts',(-43.5445020081503,-59.1441976086192,
-40.8828667548755));
#261363=CARTESIAN_POINT('Ctrl Pts',(-43.062776783065,-58.309825043484,-40.8245334215421));
#261364=CARTESIAN_POINT('Ctrl Pts',(-42.5810515579797,-57.4754524783487,
-40.7662000882087));
#261365=CARTESIAN_POINT('Ctrl Pts',(-43.062776783065,-56.6410799132135,
-40.7078667548754));
#261366=CARTESIAN_POINT('Ctrl Pts',(-43.5445020081503,-55.8067073480783,
-40.6495334215421));
#261367=CARTESIAN_POINT('Ctrl Pts',(-44.5079524583208,-55.8067073480783,
-40.5912000882087));
#261368=CARTESIAN_POINT('Ctrl Pts',(-45.4714029084913,-55.8067073480783,
-40.5328667548754));
#261369=CARTESIAN_POINT('Ctrl Pts',(-45.9531281335766,-56.6410799132135,
-40.4745334215421));
#261370=CARTESIAN_POINT('Ctrl Pts',(-46.4348533586618,-57.4754524783487,
-40.4162000882087));
#261371=CARTESIAN_POINT('Ctrl Pts',(-45.9531281335766,-58.309825043484,
-40.3578667548754));
#261372=CARTESIAN_POINT('Ctrl Pts',(-45.4714029084913,-59.1441976086192,
-40.2995334215421));
#261373=CARTESIAN_POINT('Ctrl Pts',(-44.5079524583208,-59.1441976086192,
-40.2412000882087));
#261374=CARTESIAN_POINT('Ctrl Pts',(-43.5445020081503,-59.1441976086192,
-40.1828667548754));
#261375=CARTESIAN_POINT('Ctrl Pts',(-43.062776783065,-58.309825043484,-40.1245334215421));
#261376=CARTESIAN_POINT('Ctrl Pts',(-42.5810515579797,-57.4754524783487,
-40.0662000882088));
#261377=CARTESIAN_POINT('Ctrl Pts',(-43.062776783065,-56.6410799132135,
-40.0078667548754));
#261378=CARTESIAN_POINT('Ctrl Pts',(-43.5445020081503,-55.8067073480783,
-39.9495334215421));
#261379=CARTESIAN_POINT('Ctrl Pts',(-44.5079524583208,-55.8067073480783,
-39.8912000882087));
#261380=CARTESIAN_POINT('Ctrl Pts',(-45.4714029084913,-55.8067073480783,
-39.8328667548754));
#261381=CARTESIAN_POINT('Ctrl Pts',(-45.9531281335766,-56.6410799132135,
-39.7745334215421));
#261382=CARTESIAN_POINT('Ctrl Pts',(-46.4348533586618,-57.4754524783487,
-39.7162000882088));
#261383=CARTESIAN_POINT('Ctrl Pts',(-45.9531281335766,-58.309825043484,
-39.6578667548754));
#261384=CARTESIAN_POINT('Ctrl Pts',(-45.4714029084913,-59.1441976086192,
-39.5995334215421));
#261385=CARTESIAN_POINT('Ctrl Pts',(-44.5079524583208,-59.1441976086192,
-39.5412000882087));
#261386=CARTESIAN_POINT('Ctrl Pts',(-43.5445020081503,-59.1441976086192,
-39.4828667548754));
#261387=CARTESIAN_POINT('Ctrl Pts',(-43.062776783065,-58.309825043484,-39.4245334215421));
#261388=CARTESIAN_POINT('Ctrl Pts',(-42.5810515579797,-57.4754524783487,
-39.3662000882088));
#261389=CARTESIAN_POINT('Ctrl Pts',(-43.062776783065,-56.6410799132135,
-39.3078667548754));
#261390=CARTESIAN_POINT('Ctrl Pts',(-43.5445020081503,-55.8067073480783,
-39.2495334215421));
#261391=CARTESIAN_POINT('Ctrl Pts',(-44.5079524583208,-55.8067073480783,
-39.1912000882087));
#261392=CARTESIAN_POINT('Ctrl Pts',(-45.4714029084913,-55.8067073480783,
-39.1328667548754));
#261393=CARTESIAN_POINT('Ctrl Pts',(-45.9531281335766,-56.6410799132135,
-39.0745334215421));
#261394=CARTESIAN_POINT('Ctrl Pts',(-46.4348533586618,-57.4754524783487,
-39.0162000882088));
#261395=CARTESIAN_POINT('Ctrl Pts',(-45.9531281335766,-58.309825043484,
-38.9578667548754));
#261396=CARTESIAN_POINT('Ctrl Pts',(-45.4714029084913,-59.1441976086192,
-38.8995334215421));
#261397=CARTESIAN_POINT('Ctrl Pts',(-44.5079524583208,-59.1441976086192,
-38.8412000882087));
#261398=CARTESIAN_POINT('Ctrl Pts',(-43.5445020081503,-59.1441976086192,
-38.7828667548754));
#261399=CARTESIAN_POINT('Ctrl Pts',(-43.062776783065,-58.309825043484,-38.7245334215421));
#261400=CARTESIAN_POINT('Ctrl Pts',(-42.5810515579797,-57.4754524783487,
-38.6662000882088));
#261401=CARTESIAN_POINT('Ctrl Pts',(-43.062776783065,-56.6410799132135,
-38.6078667548754));
#261402=CARTESIAN_POINT('Ctrl Pts',(-43.5445020081503,-55.8067073480783,
-38.5495334215421));
#261403=CARTESIAN_POINT('Ctrl Pts',(-44.5079524583208,-55.8067073480783,
-38.4912000882087));
#261404=CARTESIAN_POINT('Ctrl Pts',(-45.4714029084913,-55.8067073480783,
-38.4328667548754));
#261405=CARTESIAN_POINT('Ctrl Pts',(-45.9531281335766,-56.6410799132135,
-38.3745334215421));
#261406=CARTESIAN_POINT('Ctrl Pts',(-46.4348533586618,-57.4754524783487,
-38.3162000882087));
#261407=CARTESIAN_POINT('Ctrl Pts',(-45.9531281335766,-58.309825043484,
-38.2578667548754));
#261408=CARTESIAN_POINT('Ctrl Pts',(-45.4714029084913,-59.1441976086192,
-38.1995334215421));
#261409=CARTESIAN_POINT('Ctrl Pts',(-44.5079524583208,-59.1441976086192,
-38.1412000882087));
#261410=CARTESIAN_POINT('Ctrl Pts',(-43.5445020081503,-59.1441976086192,
-38.0828667548754));
#261411=CARTESIAN_POINT('Ctrl Pts',(-43.062776783065,-58.309825043484,-38.0245334215421));
#261412=CARTESIAN_POINT('Ctrl Pts',(-42.5810515579797,-57.4754524783487,
-37.9662000882088));
#261413=CARTESIAN_POINT('Ctrl Pts',(-43.062776783065,-56.6410799132135,
-37.9078667548754));
#261414=CARTESIAN_POINT('Ctrl Pts',(-43.5445020081503,-55.8067073480783,
-37.8495334215421));
#261415=CARTESIAN_POINT('Ctrl Pts',(-44.5079524583208,-55.8067073480783,
-37.7912000882087));
#261416=CARTESIAN_POINT('Ctrl Pts',(-45.4714029084913,-55.8067073480783,
-37.7328667548754));
#261417=CARTESIAN_POINT('Ctrl Pts',(-45.9531281335766,-56.6410799132135,
-37.6745334215421));
#261418=CARTESIAN_POINT('Ctrl Pts',(-46.4348533586618,-57.4754524783487,
-37.6162000882088));
#261419=CARTESIAN_POINT('Ctrl Pts',(-45.9531281335766,-58.309825043484,
-37.5578667548754));
#261420=CARTESIAN_POINT('Ctrl Pts',(-45.4714029084913,-59.1441976086192,
-37.4995334215421));
#261421=CARTESIAN_POINT('Ctrl Pts',(-44.5079524583208,-59.1441976086192,
-37.4412000882087));
#261422=CARTESIAN_POINT('Ctrl Pts',(-43.5445020081503,-59.1441976086192,
-37.3828667548754));
#261423=CARTESIAN_POINT('Ctrl Pts',(-43.062776783065,-58.309825043484,-37.3245334215421));
#261424=CARTESIAN_POINT('Ctrl Pts',(-42.5810515579797,-57.4754524783487,
-37.2662000882087));
#261425=CARTESIAN_POINT('Ctrl Pts',(-43.062776783065,-56.6410799132135,
-37.2078667548754));
#261426=CARTESIAN_POINT('Ctrl Pts',(-43.5445020081503,-55.8067073480783,
-37.1495334215421));
#261427=CARTESIAN_POINT('Ctrl Pts',(-44.5079524583208,-55.8067073480783,
-37.0912000882087));
#261428=CARTESIAN_POINT('Ctrl Pts',(-45.4714029084913,-55.8067073480783,
-37.0328667548754));
#261429=CARTESIAN_POINT('Ctrl Pts',(-45.9531281335766,-56.6410799132135,
-36.9745334215421));
#261430=CARTESIAN_POINT('Ctrl Pts',(-46.4348533586618,-57.4754524783487,
-36.9162000882087));
#261431=CARTESIAN_POINT('Ctrl Pts',(-45.9531281335766,-58.309825043484,
-36.8578667548754));
#261432=CARTESIAN_POINT('Ctrl Pts',(-45.8905903991815,-58.4181435768467,
-36.8502939014801));
#261433=CARTESIAN_POINT('Ctrl Pts',(-45.8126047529917,-58.5159296284157,
-36.8421539123268));
#261434=CARTESIAN_POINT('Ctrl Pts',(-44.5079524583208,-59.4754524783488,
-52.64995));
#261435=CARTESIAN_POINT('Ctrl Pts',(-44.3600617863357,-59.4625120445501,
-52.64995));
#261436=CARTESIAN_POINT('Ctrl Pts',(-44.2142042532552,-59.4322659035397,
-52.64995));
#261437=CARTESIAN_POINT('Ctrl Pts',(-43.9445256487742,-59.3423033429062,
-52.64995));
#261438=CARTESIAN_POINT('Ctrl Pts',(-43.8206799356501,-59.2855753019495,
-52.64995));
#261439=CARTESIAN_POINT('Ctrl Pts',(-43.4951040594959,-59.0916199608506,
-52.64995));
#261440=CARTESIAN_POINT('Ctrl Pts',(-43.3122546189713,-58.9280617429974,
-52.6499500000001));
#261441=CARTESIAN_POINT('Ctrl Pts',(-43.0527600317383,-58.5856631129985,
-52.6499500000001));
#261442=CARTESIAN_POINT('Ctrl Pts',(-42.923716913873,-58.371224501979,-52.6499500000282));
#261443=CARTESIAN_POINT('Ctrl Pts',(-42.815884786658,-57.953786980419,-52.6499500000282));
#261444=CARTESIAN_POINT('Ctrl Pts',(-42.7978378140676,-57.8061017722689,
-52.64995));
#261445=CARTESIAN_POINT('Ctrl Pts',(-42.8007193914761,-57.5178390254165,
-52.64995));
#261446=CARTESIAN_POINT('Ctrl Pts',(-42.8195756983132,-57.3784642494499,
-52.64995));
#261447=CARTESIAN_POINT('Ctrl Pts',(-42.8554737113965,-57.2430200996376,
-52.64995));
#261448=CARTESIAN_POINT('Ctrl Pts',(-44.5079524583208,-59.1441977614012,
-52.99995));
#261449=CARTESIAN_POINT('Ctrl Pts',(-43.5445019199415,-59.1441977614012,
-52.9416166666667));
#261450=CARTESIAN_POINT('Ctrl Pts',(-43.0627766507519,-58.309825119875,
-52.8832833333334));
#261451=CARTESIAN_POINT('Ctrl Pts',(-42.5810513815623,-57.4754524783487,
-52.82495));
#261452=CARTESIAN_POINT('Ctrl Pts',(-43.0627766507519,-56.6410798368225,
-52.7666166666667));
#261453=CARTESIAN_POINT('Ctrl Pts',(-43.5445019199415,-55.8067071952963,
-52.7082833333333));
#261454=CARTESIAN_POINT('Ctrl Pts',(-44.5079524583208,-55.8067071952963,
-52.64995));
#261455=CARTESIAN_POINT('Ctrl Pts',(-45.4714029967,-55.8067071952963,-52.5916166666666));
#261456=CARTESIAN_POINT('Ctrl Pts',(-45.9531282658897,-56.6410798368225,
-52.5332833333334));
#261457=CARTESIAN_POINT('Ctrl Pts',(-46.4348535350793,-57.4754524783487,
-52.4749500000001));
#261458=CARTESIAN_POINT('Ctrl Pts',(-45.9531282658897,-58.309825119875,
-52.4166166666667));
#261459=CARTESIAN_POINT('Ctrl Pts',(-45.4714029967,-59.1441977614012,-52.3582833333334));
#261460=CARTESIAN_POINT('Ctrl Pts',(-44.5079524583208,-59.1441977614012,
-52.29995));
#261461=CARTESIAN_POINT('Ctrl Pts',(-43.5445019199415,-59.1441977614012,
-52.2416166666667));
#261462=CARTESIAN_POINT('Ctrl Pts',(-43.0627766507519,-58.309825119875,
-52.1832833333333));
#261463=CARTESIAN_POINT('Ctrl Pts',(-42.5810513815623,-57.4754524783487,
-52.12495));
#261464=CARTESIAN_POINT('Ctrl Pts',(-43.0627766507519,-56.6410798368225,
-52.0666166666667));
#261465=CARTESIAN_POINT('Ctrl Pts',(-43.5445019199415,-55.8067071952963,
-52.0082833333333));
#261466=CARTESIAN_POINT('Ctrl Pts',(-44.5079524583208,-55.8067071952963,
-51.94995));
#261467=CARTESIAN_POINT('Ctrl Pts',(-45.4714029967,-55.8067071952963,-51.8916166666667));
#261468=CARTESIAN_POINT('Ctrl Pts',(-45.9531282658897,-56.6410798368225,
-51.8332833333334));
#261469=CARTESIAN_POINT('Ctrl Pts',(-46.4348535350793,-57.4754524783487,
-51.77495));
#261470=CARTESIAN_POINT('Ctrl Pts',(-45.9531282658897,-58.309825119875,
-51.7166166666667));
#261471=CARTESIAN_POINT('Ctrl Pts',(-45.4714029967,-59.1441977614012,-51.6582833333333));
#261472=CARTESIAN_POINT('Ctrl Pts',(-44.5079524583208,-59.1441977614012,
-51.59995));
#261473=CARTESIAN_POINT('Ctrl Pts',(-43.5445019199415,-59.1441977614012,
-51.5416166666667));
#261474=CARTESIAN_POINT('Ctrl Pts',(-43.0627766507519,-58.309825119875,
-51.4832833333334));
#261475=CARTESIAN_POINT('Ctrl Pts',(-42.5810513815623,-57.4754524783487,
-51.42495));
#261476=CARTESIAN_POINT('Ctrl Pts',(-43.0627766507519,-56.6410798368225,
-51.3666166666667));
#261477=CARTESIAN_POINT('Ctrl Pts',(-43.5445019199415,-55.8067071952963,
-51.3082833333333));
#261478=CARTESIAN_POINT('Ctrl Pts',(-44.5079524583208,-55.8067071952963,
-51.24995));
#261479=CARTESIAN_POINT('Ctrl Pts',(-45.4714029967,-55.8067071952963,-51.1916166666667));
#261480=CARTESIAN_POINT('Ctrl Pts',(-45.9531282658897,-56.6410798368225,
-51.1332833333334));
#261481=CARTESIAN_POINT('Ctrl Pts',(-46.4348535350793,-57.4754524783487,
-51.07495));
#261482=CARTESIAN_POINT('Ctrl Pts',(-45.9531282658897,-58.309825119875,
-51.0166166666667));
#261483=CARTESIAN_POINT('Ctrl Pts',(-45.4714029967,-59.1441977614012,-50.9582833333334));
#261484=CARTESIAN_POINT('Ctrl Pts',(-44.5079524583208,-59.1441977614012,
-50.89995));
#261485=CARTESIAN_POINT('Ctrl Pts',(-43.5445019199415,-59.1441977614012,
-50.8416166666667));
#261486=CARTESIAN_POINT('Ctrl Pts',(-43.0627766507519,-58.309825119875,
-50.7832833333333));
#261487=CARTESIAN_POINT('Ctrl Pts',(-42.5810513815623,-57.4754524783487,
-50.72495));
#261488=CARTESIAN_POINT('Ctrl Pts',(-43.0627766507519,-56.6410798368225,
-50.6666166666667));
#261489=CARTESIAN_POINT('Ctrl Pts',(-43.5445019199415,-55.8067071952963,
-50.6082833333334));
#261490=CARTESIAN_POINT('Ctrl Pts',(-44.5079524583208,-55.8067071952963,
-50.54995));
#261491=CARTESIAN_POINT('Ctrl Pts',(-45.4714029967,-55.8067071952963,-50.4916166666667));
#261492=CARTESIAN_POINT('Ctrl Pts',(-45.9531282658897,-56.6410798368225,
-50.4332833333333));
#261493=CARTESIAN_POINT('Ctrl Pts',(-46.4348535350793,-57.4754524783487,
-50.37495));
#261494=CARTESIAN_POINT('Ctrl Pts',(-45.9531282658897,-58.309825119875,
-50.3166166666667));
#261495=CARTESIAN_POINT('Ctrl Pts',(-45.4714029967,-59.1441977614012,-50.2582833333334));
#261496=CARTESIAN_POINT('Ctrl Pts',(-44.5079524583208,-59.1441977614012,
-50.19995));
#261497=CARTESIAN_POINT('Ctrl Pts',(-43.5445019199415,-59.1441977614012,
-50.1416166666667));
#261498=CARTESIAN_POINT('Ctrl Pts',(-43.0627766507519,-58.309825119875,
-50.0832833333334));
#261499=CARTESIAN_POINT('Ctrl Pts',(-42.5810513815623,-57.4754524783487,
-50.02495));
#261500=CARTESIAN_POINT('Ctrl Pts',(-43.0627766507519,-56.6410798368225,
-49.9666166666667));
#261501=CARTESIAN_POINT('Ctrl Pts',(-43.5445019199415,-55.8067071952963,
-49.9082833333334));
#261502=CARTESIAN_POINT('Ctrl Pts',(-44.5079524583208,-55.8067071952963,
-49.84995));
#261503=CARTESIAN_POINT('Ctrl Pts',(-45.4714029967,-55.8067071952963,-49.7916166666667));
#261504=CARTESIAN_POINT('Ctrl Pts',(-45.9531282658897,-56.6410798368225,
-49.7332833333334));
#261505=CARTESIAN_POINT('Ctrl Pts',(-46.4348535350793,-57.4754524783487,
-49.67495));
#261506=CARTESIAN_POINT('Ctrl Pts',(-45.9531282658897,-58.309825119875,
-49.6166166666667));
#261507=CARTESIAN_POINT('Ctrl Pts',(-45.4714029967,-59.1441977614012,-49.5582833333334));
#261508=CARTESIAN_POINT('Ctrl Pts',(-44.5079524583208,-59.1441977614012,
-49.49995));
#261509=CARTESIAN_POINT('Ctrl Pts',(-43.5445019199415,-59.1441977614012,
-49.4416166666667));
#261510=CARTESIAN_POINT('Ctrl Pts',(-43.0627766507519,-58.309825119875,
-49.3832833333334));
#261511=CARTESIAN_POINT('Ctrl Pts',(-42.5810513815623,-57.4754524783487,
-49.32495));
#261512=CARTESIAN_POINT('Ctrl Pts',(-43.0627766507519,-56.6410798368225,
-49.2666166666667));
#261513=CARTESIAN_POINT('Ctrl Pts',(-43.5445019199415,-55.8067071952963,
-49.2082833333334));
#261514=CARTESIAN_POINT('Ctrl Pts',(-44.5079524583208,-55.8067071952963,
-49.14995));
#261515=CARTESIAN_POINT('Ctrl Pts',(-45.4714029967,-55.8067071952963,-49.0916166666667));
#261516=CARTESIAN_POINT('Ctrl Pts',(-45.9531282658897,-56.6410798368225,
-49.0332833333333));
#261517=CARTESIAN_POINT('Ctrl Pts',(-46.4348535350793,-57.4754524783487,
-48.97495));
#261518=CARTESIAN_POINT('Ctrl Pts',(-45.9531282658897,-58.309825119875,
-48.9166166666667));
#261519=CARTESIAN_POINT('Ctrl Pts',(-45.4714029967,-59.1441977614012,-48.8582833333333));
#261520=CARTESIAN_POINT('Ctrl Pts',(-44.5079524583208,-59.1441977614012,
-48.79995));
#261521=CARTESIAN_POINT('Ctrl Pts',(-43.5445019199415,-59.1441977614012,
-48.7416166666667));
#261522=CARTESIAN_POINT('Ctrl Pts',(-43.0627766507519,-58.309825119875,
-48.6832833333334));
#261523=CARTESIAN_POINT('Ctrl Pts',(-42.5810513815623,-57.4754524783487,
-48.62495));
#261524=CARTESIAN_POINT('Ctrl Pts',(-43.0627766507519,-56.6410798368225,
-48.5666166666667));
#261525=CARTESIAN_POINT('Ctrl Pts',(-43.5445019199415,-55.8067071952963,
-48.5082833333334));
#261526=CARTESIAN_POINT('Ctrl Pts',(-44.5079524583208,-55.8067071952963,
-48.44995));
#261527=CARTESIAN_POINT('Ctrl Pts',(-45.4714029967,-55.8067071952963,-48.3916166666667));
#261528=CARTESIAN_POINT('Ctrl Pts',(-45.9531282658897,-56.6410798368225,
-48.3332833333334));
#261529=CARTESIAN_POINT('Ctrl Pts',(-46.4348535350793,-57.4754524783487,
-48.27495));
#261530=CARTESIAN_POINT('Ctrl Pts',(-45.9531282658897,-58.309825119875,
-48.2166166666667));
#261531=CARTESIAN_POINT('Ctrl Pts',(-45.4714029967,-59.1441977614012,-48.1582833333334));
#261532=CARTESIAN_POINT('Ctrl Pts',(-44.5079524583208,-59.1441977614012,
-48.09995));
#261533=CARTESIAN_POINT('Ctrl Pts',(-43.5445019199415,-59.1441977614012,
-48.0416166666667));
#261534=CARTESIAN_POINT('Ctrl Pts',(-43.0627766507519,-58.309825119875,
-47.9832833333334));
#261535=CARTESIAN_POINT('Ctrl Pts',(-42.5810513815623,-57.4754524783487,
-47.92495));
#261536=CARTESIAN_POINT('Ctrl Pts',(-43.0627766507519,-56.6410798368225,
-47.8666166666667));
#261537=CARTESIAN_POINT('Ctrl Pts',(-43.5445019199415,-55.8067071952963,
-47.8082833333333));
#261538=CARTESIAN_POINT('Ctrl Pts',(-44.5079524583208,-55.8067071952963,
-47.74995));
#261539=CARTESIAN_POINT('Ctrl Pts',(-45.4714029967,-55.8067071952963,-47.6916166666667));
#261540=CARTESIAN_POINT('Ctrl Pts',(-45.9531282658897,-56.6410798368225,
-47.6332833333333));
#261541=CARTESIAN_POINT('Ctrl Pts',(-46.4348535350793,-57.4754524783487,
-47.57495));
#261542=CARTESIAN_POINT('Ctrl Pts',(-45.9531282658897,-58.309825119875,
-47.5166166666667));
#261543=CARTESIAN_POINT('Ctrl Pts',(-45.4714029967,-59.1441977614012,-47.4582833333333));
#261544=CARTESIAN_POINT('Ctrl Pts',(-44.5079524583208,-59.1441977614012,
-47.39995));
#261545=CARTESIAN_POINT('Ctrl Pts',(-43.5445019199415,-59.1441977614012,
-47.3416166666666));
#261546=CARTESIAN_POINT('Ctrl Pts',(-43.0627766507519,-58.309825119875,
-47.2832833333333));
#261547=CARTESIAN_POINT('Ctrl Pts',(-42.5810513815623,-57.4754524783487,
-47.22495));
#261548=CARTESIAN_POINT('Ctrl Pts',(-43.0627766507519,-56.6410798368225,
-47.1666166666667));
#261549=CARTESIAN_POINT('Ctrl Pts',(-43.5445019199415,-55.8067071952963,
-47.1082833333333));
#261550=CARTESIAN_POINT('Ctrl Pts',(-44.5079524583208,-55.8067071952963,
-47.04995));
#261551=CARTESIAN_POINT('Ctrl Pts',(-45.4714029967,-55.8067071952963,-46.9916166666667));
#261552=CARTESIAN_POINT('Ctrl Pts',(-45.9531282658897,-56.6410798368225,
-46.9332833333334));
#261553=CARTESIAN_POINT('Ctrl Pts',(-46.4348535350793,-57.4754524783487,
-46.87495));
#261554=CARTESIAN_POINT('Ctrl Pts',(-45.9531282658897,-58.309825119875,
-46.8166166666667));
#261555=CARTESIAN_POINT('Ctrl Pts',(-45.4714029967,-59.1441977614012,-46.7582833333333));
#261556=CARTESIAN_POINT('Ctrl Pts',(-44.5079524583208,-59.1441977614012,
-46.69995));
#261557=CARTESIAN_POINT('Ctrl Pts',(-43.5445019199415,-59.1441977614012,
-46.6416166666666));
#261558=CARTESIAN_POINT('Ctrl Pts',(-43.0627766507519,-58.309825119875,
-46.5832833333334));
#261559=CARTESIAN_POINT('Ctrl Pts',(-42.5810513815623,-57.4754524783487,
-46.52495));
#261560=CARTESIAN_POINT('Ctrl Pts',(-43.0627766507519,-56.6410798368225,
-46.4666166666667));
#261561=CARTESIAN_POINT('Ctrl Pts',(-43.5445019199415,-55.8067071952963,
-46.4082833333333));
#261562=CARTESIAN_POINT('Ctrl Pts',(-44.5079524583208,-55.8067071952963,
-46.34995));
#261563=CARTESIAN_POINT('Ctrl Pts',(-45.4714029967,-55.8067071952963,-46.2916166666667));
#261564=CARTESIAN_POINT('Ctrl Pts',(-45.9531282658897,-56.6410798368225,
-46.2332833333334));
#261565=CARTESIAN_POINT('Ctrl Pts',(-46.4348535350793,-57.4754524783487,
-46.17495));
#261566=CARTESIAN_POINT('Ctrl Pts',(-45.9531282658897,-58.309825119875,
-46.1166166666667));
#261567=CARTESIAN_POINT('Ctrl Pts',(-45.4714029967,-59.1441977614012,-46.0582833333333));
#261568=CARTESIAN_POINT('Ctrl Pts',(-44.5079524583208,-59.1441977614012,
-45.99995));
#261569=CARTESIAN_POINT('Ctrl Pts',(-43.5445019199415,-59.1441977614012,
-45.9416166666667));
#261570=CARTESIAN_POINT('Ctrl Pts',(-43.0627766507519,-58.309825119875,
-45.8832833333333));
#261571=CARTESIAN_POINT('Ctrl Pts',(-42.5810513815623,-57.4754524783487,
-45.82495));
#261572=CARTESIAN_POINT('Ctrl Pts',(-43.0627766507519,-56.6410798368225,
-45.7666166666667));
#261573=CARTESIAN_POINT('Ctrl Pts',(-43.5445019199415,-55.8067071952963,
-45.7082833333333));
#261574=CARTESIAN_POINT('Ctrl Pts',(-44.5079524583208,-55.8067071952963,
-45.64995));
#261575=CARTESIAN_POINT('Ctrl Pts',(-45.4714029967,-55.8067071952963,-45.5916166666667));
#261576=CARTESIAN_POINT('Ctrl Pts',(-45.9531282658897,-56.6410798368225,
-45.5332833333333));
#261577=CARTESIAN_POINT('Ctrl Pts',(-46.4348535350793,-57.4754524783487,
-45.47495));
#261578=CARTESIAN_POINT('Ctrl Pts',(-45.9531282658897,-58.309825119875,
-45.4166166666667));
#261579=CARTESIAN_POINT('Ctrl Pts',(-45.4714029967,-59.1441977614012,-45.3582833333333));
#261580=CARTESIAN_POINT('Ctrl Pts',(-44.5079524583208,-59.1441977614012,
-45.29995));
#261581=CARTESIAN_POINT('Ctrl Pts',(-43.5445019199415,-59.1441977614012,
-45.2416166666667));
#261582=CARTESIAN_POINT('Ctrl Pts',(-43.0627766507519,-58.309825119875,
-45.1832833333334));
#261583=CARTESIAN_POINT('Ctrl Pts',(-42.5810513815623,-57.4754524783487,
-45.12495));
#261584=CARTESIAN_POINT('Ctrl Pts',(-43.0627766507519,-56.6410798368225,
-45.0666166666667));
#261585=CARTESIAN_POINT('Ctrl Pts',(-43.5445019199415,-55.8067071952963,
-45.0082833333334));
#261586=CARTESIAN_POINT('Ctrl Pts',(-44.5079524583208,-55.8067071952963,
-44.94995));
#261587=CARTESIAN_POINT('Ctrl Pts',(-45.4714029967,-55.8067071952963,-44.8916166666667));
#261588=CARTESIAN_POINT('Ctrl Pts',(-45.9531282658897,-56.6410798368225,
-44.8332833333334));
#261589=CARTESIAN_POINT('Ctrl Pts',(-46.4348535350793,-57.4754524783487,
-44.77495));
#261590=CARTESIAN_POINT('Ctrl Pts',(-45.9531282658897,-58.309825119875,
-44.7166166666667));
#261591=CARTESIAN_POINT('Ctrl Pts',(-45.4714029967,-59.1441977614012,-44.6582833333334));
#261592=CARTESIAN_POINT('Ctrl Pts',(-44.5079524583208,-59.1441977614012,
-44.59995));
#261593=CARTESIAN_POINT('Ctrl Pts',(-43.5445019199415,-59.1441977614012,
-44.5416166666667));
#261594=CARTESIAN_POINT('Ctrl Pts',(-43.0627766507519,-58.309825119875,
-44.4832833333334));
#261595=CARTESIAN_POINT('Ctrl Pts',(-42.5810513815623,-57.4754524783487,
-44.42495));
#261596=CARTESIAN_POINT('Ctrl Pts',(-43.0627766507519,-56.6410798368225,
-44.3666166666667));
#261597=CARTESIAN_POINT('Ctrl Pts',(-43.5445019199415,-55.8067071952963,
-44.3082833333334));
#261598=CARTESIAN_POINT('Ctrl Pts',(-44.5079524583208,-55.8067071952963,
-44.24995));
#261599=CARTESIAN_POINT('Ctrl Pts',(-45.4714029967,-55.8067071952963,-44.1916166666667));
#261600=CARTESIAN_POINT('Ctrl Pts',(-45.9531282658897,-56.6410798368225,
-44.1332833333334));
#261601=CARTESIAN_POINT('Ctrl Pts',(-46.4348535350793,-57.4754524783487,
-44.07495));
#261602=CARTESIAN_POINT('Ctrl Pts',(-45.9531282658897,-58.309825119875,
-44.0166166666667));
#261603=CARTESIAN_POINT('Ctrl Pts',(-45.4714029967,-59.1441977614012,-43.9582833333334));
#261604=CARTESIAN_POINT('Ctrl Pts',(-44.5079524583208,-59.1441977614012,
-43.89995));
#261605=CARTESIAN_POINT('Ctrl Pts',(-43.5445019199415,-59.1441977614012,
-43.8416166666667));
#261606=CARTESIAN_POINT('Ctrl Pts',(-43.0627766507519,-58.309825119875,
-43.7832833333334));
#261607=CARTESIAN_POINT('Ctrl Pts',(-42.5810513815623,-57.4754524783487,
-43.72495));
#261608=CARTESIAN_POINT('Ctrl Pts',(-43.0627766507519,-56.6410798368225,
-43.6666166666667));
#261609=CARTESIAN_POINT('Ctrl Pts',(-43.5445019199415,-55.8067071952963,
-43.6082833333333));
#261610=CARTESIAN_POINT('Ctrl Pts',(-44.5079524583208,-55.8067071952963,
-43.54995));
#261611=CARTESIAN_POINT('Ctrl Pts',(-45.4714029967,-55.8067071952963,-43.4916166666667));
#261612=CARTESIAN_POINT('Ctrl Pts',(-45.9531282658897,-56.6410798368225,
-43.4332833333333));
#261613=CARTESIAN_POINT('Ctrl Pts',(-46.4348535350793,-57.4754524783487,
-43.37495));
#261614=CARTESIAN_POINT('Ctrl Pts',(-45.9531282658897,-58.309825119875,
-43.3166166666667));
#261615=CARTESIAN_POINT('Ctrl Pts',(-45.4714029967,-59.1441977614012,-43.2582833333333));
#261616=CARTESIAN_POINT('Ctrl Pts',(-44.5079524583208,-59.1441977614012,
-43.19995));
#261617=CARTESIAN_POINT('Ctrl Pts',(-43.5445019199415,-59.1441977614012,
-43.1416166666667));
#261618=CARTESIAN_POINT('Ctrl Pts',(-43.0627766507519,-58.309825119875,
-43.0832833333333));
#261619=CARTESIAN_POINT('Ctrl Pts',(-42.5810513815623,-57.4754524783487,
-43.02495));
#261620=CARTESIAN_POINT('Ctrl Pts',(-43.0627766507519,-56.6410798368225,
-42.9666166666667));
#261621=CARTESIAN_POINT('Ctrl Pts',(-43.5445019199415,-55.8067071952963,
-42.9082833333333));
#261622=CARTESIAN_POINT('Ctrl Pts',(-44.5079524583208,-55.8067071952963,
-42.84995));
#261623=CARTESIAN_POINT('Ctrl Pts',(-45.4714029967,-55.8067071952963,-42.7916166666667));
#261624=CARTESIAN_POINT('Ctrl Pts',(-45.9531282658897,-56.6410798368225,
-42.7332833333334));
#261625=CARTESIAN_POINT('Ctrl Pts',(-46.4348535350793,-57.4754524783487,
-42.67495));
#261626=CARTESIAN_POINT('Ctrl Pts',(-45.9531282658897,-58.309825119875,
-42.6166166666667));
#261627=CARTESIAN_POINT('Ctrl Pts',(-45.4714029967,-59.1441977614012,-42.5582833333333));
#261628=CARTESIAN_POINT('Ctrl Pts',(-44.5079524583208,-59.1441977614012,
-42.49995));
#261629=CARTESIAN_POINT('Ctrl Pts',(-43.5445019199415,-59.1441977614012,
-42.4416166666667));
#261630=CARTESIAN_POINT('Ctrl Pts',(-43.0627766507519,-58.309825119875,
-42.3832833333333));
#261631=CARTESIAN_POINT('Ctrl Pts',(-42.5810513815623,-57.4754524783487,
-42.32495));
#261632=CARTESIAN_POINT('Ctrl Pts',(-43.0627766507519,-56.6410798368225,
-42.2666166666667));
#261633=CARTESIAN_POINT('Ctrl Pts',(-43.5445019199415,-55.8067071952963,
-42.2082833333333));
#261634=CARTESIAN_POINT('Ctrl Pts',(-44.5079524583208,-55.8067071952963,
-42.14995));
#261635=CARTESIAN_POINT('Ctrl Pts',(-45.4714029967,-55.8067071952963,-42.0916166666667));
#261636=CARTESIAN_POINT('Ctrl Pts',(-45.9531282658897,-56.6410798368225,
-42.0332833333334));
#261637=CARTESIAN_POINT('Ctrl Pts',(-46.4348535350793,-57.4754524783487,
-41.97495));
#261638=CARTESIAN_POINT('Ctrl Pts',(-45.9531282658897,-58.309825119875,
-41.9166166666667));
#261639=CARTESIAN_POINT('Ctrl Pts',(-45.4714029967,-59.1441977614012,-41.8582833333333));
#261640=CARTESIAN_POINT('Ctrl Pts',(-44.5079524583208,-59.1441977614012,
-41.79995));
#261641=CARTESIAN_POINT('Ctrl Pts',(-43.5445019199415,-59.1441977614012,
-41.7416166666667));
#261642=CARTESIAN_POINT('Ctrl Pts',(-43.0627766507519,-58.309825119875,
-41.6832833333333));
#261643=CARTESIAN_POINT('Ctrl Pts',(-42.5810513815623,-57.4754524783487,
-41.62495));
#261644=CARTESIAN_POINT('Ctrl Pts',(-43.0627766507519,-56.6410798368225,
-41.5666166666667));
#261645=CARTESIAN_POINT('Ctrl Pts',(-43.5445019199415,-55.8067071952963,
-41.5082833333334));
#261646=CARTESIAN_POINT('Ctrl Pts',(-44.5079524583208,-55.8067071952963,
-41.44995));
#261647=CARTESIAN_POINT('Ctrl Pts',(-45.4714029967,-55.8067071952963,-41.3916166666667));
#261648=CARTESIAN_POINT('Ctrl Pts',(-45.9531282658897,-56.6410798368225,
-41.3332833333334));
#261649=CARTESIAN_POINT('Ctrl Pts',(-46.4348535350793,-57.4754524783487,
-41.27495));
#261650=CARTESIAN_POINT('Ctrl Pts',(-45.9531282658897,-58.309825119875,
-41.2166166666667));
#261651=CARTESIAN_POINT('Ctrl Pts',(-45.4714029967,-59.1441977614012,-41.1582833333333));
#261652=CARTESIAN_POINT('Ctrl Pts',(-44.5079524583208,-59.1441977614012,
-41.09995));
#261653=CARTESIAN_POINT('Ctrl Pts',(-43.5445019199415,-59.1441977614012,
-41.0416166666667));
#261654=CARTESIAN_POINT('Ctrl Pts',(-43.0627766507519,-58.309825119875,
-40.9832833333333));
#261655=CARTESIAN_POINT('Ctrl Pts',(-42.5810513815623,-57.4754524783487,
-40.92495));
#261656=CARTESIAN_POINT('Ctrl Pts',(-43.0627766507519,-56.6410798368225,
-40.8666166666667));
#261657=CARTESIAN_POINT('Ctrl Pts',(-43.5445019199415,-55.8067071952963,
-40.8082833333334));
#261658=CARTESIAN_POINT('Ctrl Pts',(-44.5079524583208,-55.8067071952963,
-40.74995));
#261659=CARTESIAN_POINT('Ctrl Pts',(-45.4714029967,-55.8067071952963,-40.6916166666667));
#261660=CARTESIAN_POINT('Ctrl Pts',(-45.9531282658897,-56.6410798368225,
-40.6332833333334));
#261661=CARTESIAN_POINT('Ctrl Pts',(-46.4348535350793,-57.4754524783487,
-40.57495));
#261662=CARTESIAN_POINT('Ctrl Pts',(-45.9531282658897,-58.309825119875,
-40.5166166666667));
#261663=CARTESIAN_POINT('Ctrl Pts',(-45.4714029967,-59.1441977614012,-40.4582833333333));
#261664=CARTESIAN_POINT('Ctrl Pts',(-44.5079524583208,-59.1441977614012,
-40.39995));
#261665=CARTESIAN_POINT('Ctrl Pts',(-43.5445019199415,-59.1441977614012,
-40.3416166666667));
#261666=CARTESIAN_POINT('Ctrl Pts',(-43.0627766507519,-58.309825119875,
-40.2832833333334));
#261667=CARTESIAN_POINT('Ctrl Pts',(-42.5810513815623,-57.4754524783487,
-40.22495));
#261668=CARTESIAN_POINT('Ctrl Pts',(-43.0627766507519,-56.6410798368225,
-40.1666166666667));
#261669=CARTESIAN_POINT('Ctrl Pts',(-43.5445019199415,-55.8067071952963,
-40.1082833333334));
#261670=CARTESIAN_POINT('Ctrl Pts',(-44.5079524583208,-55.8067071952963,
-40.04995));
#261671=CARTESIAN_POINT('Ctrl Pts',(-45.4714029967,-55.8067071952963,-39.9916166666667));
#261672=CARTESIAN_POINT('Ctrl Pts',(-45.9531282658897,-56.6410798368225,
-39.9332833333333));
#261673=CARTESIAN_POINT('Ctrl Pts',(-46.4348535350793,-57.4754524783487,
-39.87495));
#261674=CARTESIAN_POINT('Ctrl Pts',(-45.9531282658897,-58.309825119875,
-39.8166166666667));
#261675=CARTESIAN_POINT('Ctrl Pts',(-45.4714029967,-59.1441977614012,-39.7582833333334));
#261676=CARTESIAN_POINT('Ctrl Pts',(-44.5079524583208,-59.1441977614012,
-39.69995));
#261677=CARTESIAN_POINT('Ctrl Pts',(-43.5445019199415,-59.1441977614012,
-39.6416166666667));
#261678=CARTESIAN_POINT('Ctrl Pts',(-43.0627766507519,-58.309825119875,
-39.5832833333333));
#261679=CARTESIAN_POINT('Ctrl Pts',(-42.5810513815623,-57.4754524783487,
-39.52495));
#261680=CARTESIAN_POINT('Ctrl Pts',(-43.0627766507519,-56.6410798368225,
-39.4666166666667));
#261681=CARTESIAN_POINT('Ctrl Pts',(-43.5445019199415,-55.8067071952963,
-39.4082833333334));
#261682=CARTESIAN_POINT('Ctrl Pts',(-44.5079524583208,-55.8067071952963,
-39.34995));
#261683=CARTESIAN_POINT('Ctrl Pts',(-45.4714029967,-55.8067071952963,-39.2916166666667));
#261684=CARTESIAN_POINT('Ctrl Pts',(-45.9531282658897,-56.6410798368225,
-39.2332833333333));
#261685=CARTESIAN_POINT('Ctrl Pts',(-46.4348535350793,-57.4754524783487,
-39.17495));
#261686=CARTESIAN_POINT('Ctrl Pts',(-45.9531282658897,-58.309825119875,
-39.1166166666667));
#261687=CARTESIAN_POINT('Ctrl Pts',(-45.4714029967,-59.1441977614012,-39.0582833333334));
#261688=CARTESIAN_POINT('Ctrl Pts',(-44.5079524583208,-59.1441977614012,
-38.99995));
#261689=CARTESIAN_POINT('Ctrl Pts',(-43.5445019199415,-59.1441977614012,
-38.9416166666667));
#261690=CARTESIAN_POINT('Ctrl Pts',(-43.0627766507519,-58.309825119875,
-38.8832833333334));
#261691=CARTESIAN_POINT('Ctrl Pts',(-42.5810513815623,-57.4754524783487,
-38.82495));
#261692=CARTESIAN_POINT('Ctrl Pts',(-43.0627766507519,-56.6410798368225,
-38.7666166666667));
#261693=CARTESIAN_POINT('Ctrl Pts',(-43.5445019199415,-55.8067071952963,
-38.7082833333334));
#261694=CARTESIAN_POINT('Ctrl Pts',(-44.5079524583208,-55.8067071952963,
-38.64995));
#261695=CARTESIAN_POINT('Ctrl Pts',(-45.4714029967,-55.8067071952963,-38.5916166666667));
#261696=CARTESIAN_POINT('Ctrl Pts',(-45.9531282658897,-56.6410798368225,
-38.5332833333334));
#261697=CARTESIAN_POINT('Ctrl Pts',(-46.4348535350793,-57.4754524783487,
-38.47495));
#261698=CARTESIAN_POINT('Ctrl Pts',(-45.9531282658897,-58.309825119875,
-38.4166166666667));
#261699=CARTESIAN_POINT('Ctrl Pts',(-45.4714029967,-59.1441977614012,-38.3582833333333));
#261700=CARTESIAN_POINT('Ctrl Pts',(-44.5079524583208,-59.1441977614012,
-38.29995));
#261701=CARTESIAN_POINT('Ctrl Pts',(-43.5445019199415,-59.1441977614012,
-38.2416166666667));
#261702=CARTESIAN_POINT('Ctrl Pts',(-43.0627766507519,-58.309825119875,
-38.1832833333333));
#261703=CARTESIAN_POINT('Ctrl Pts',(-42.5810513815623,-57.4754524783487,
-38.12495));
#261704=CARTESIAN_POINT('Ctrl Pts',(-43.0627766507519,-56.6410798368225,
-38.0666166666667));
#261705=CARTESIAN_POINT('Ctrl Pts',(-43.5445019199415,-55.8067071952963,
-38.0082833333333));
#261706=CARTESIAN_POINT('Ctrl Pts',(-44.5079524583208,-55.8067071952963,
-37.94995));
#261707=CARTESIAN_POINT('Ctrl Pts',(-45.4714029967,-55.8067071952963,-37.8916166666667));
#261708=CARTESIAN_POINT('Ctrl Pts',(-45.9531282658897,-56.6410798368225,
-37.8332833333334));
#261709=CARTESIAN_POINT('Ctrl Pts',(-46.4348535350793,-57.4754524783487,
-37.77495));
#261710=CARTESIAN_POINT('Ctrl Pts',(-45.9531282658897,-58.309825119875,
-37.7166166666667));
#261711=CARTESIAN_POINT('Ctrl Pts',(-45.4714029967,-59.1441977614012,-37.6582833333333));
#261712=CARTESIAN_POINT('Ctrl Pts',(-44.5079524583208,-59.1441977614012,
-37.59995));
#261713=CARTESIAN_POINT('Ctrl Pts',(-43.5445019199415,-59.1441977614012,
-37.5416166666667));
#261714=CARTESIAN_POINT('Ctrl Pts',(-43.0627766507519,-58.309825119875,
-37.4832833333334));
#261715=CARTESIAN_POINT('Ctrl Pts',(-42.5810513815623,-57.4754524783487,
-37.42495));
#261716=CARTESIAN_POINT('Ctrl Pts',(-43.0627766507519,-56.6410798368225,
-37.3666166666667));
#261717=CARTESIAN_POINT('Ctrl Pts',(-43.5445019199415,-55.8067071952963,
-37.3082833333333));
#261718=CARTESIAN_POINT('Ctrl Pts',(-44.5079524583208,-55.8067071952963,
-37.24995));
#261719=CARTESIAN_POINT('Ctrl Pts',(-45.4714029967,-55.8067071952963,-37.1916166666667));
#261720=CARTESIAN_POINT('Ctrl Pts',(-45.9531282658897,-56.6410798368225,
-37.1332833333334));
#261721=CARTESIAN_POINT('Ctrl Pts',(-46.4348535350793,-57.4754524783487,
-37.07495));
#261722=CARTESIAN_POINT('Ctrl Pts',(-45.9531282658897,-58.309825119875,
-37.0166166666667));
#261723=CARTESIAN_POINT('Ctrl Pts',(-45.8905850977848,-58.418153064699,
-37.0090431559831));
#261724=CARTESIAN_POINT('Ctrl Pts',(-45.8125914103809,-58.5159466035015,
-37.0009024189827));
#261725=CARTESIAN_POINT('Ctrl Pts',(-44.5079524583208,-59.5441932447742,
-53.2308875));
#261726=CARTESIAN_POINT('Ctrl Pts',(-43.3135644199415,-59.5441932447742,
-53.1725541666667));
#261727=CARTESIAN_POINT('Ctrl Pts',(-42.7163704007519,-58.5098228615615,
-53.1142208333334));
#261728=CARTESIAN_POINT('Ctrl Pts',(-42.1191763815623,-57.4754524783487,
-53.0558875000001));
#261729=CARTESIAN_POINT('Ctrl Pts',(-42.7163704007519,-56.4410820951361,
-52.9975541666667));
#261730=CARTESIAN_POINT('Ctrl Pts',(-43.3135644199415,-55.4067117119233,
-52.9392208333334));
#261731=CARTESIAN_POINT('Ctrl Pts',(-44.5079524583208,-55.4067117119234,
-52.8808875));
#261732=CARTESIAN_POINT('Ctrl Pts',(-45.7023404967,-55.4067117119233,-52.8225541666667));
#261733=CARTESIAN_POINT('Ctrl Pts',(-46.2995345158897,-56.4410820951361,
-52.7642208333334));
#261734=CARTESIAN_POINT('Ctrl Pts',(-46.8967285350793,-57.4754524783487,
-52.7058875));
#261735=CARTESIAN_POINT('Ctrl Pts',(-46.2995345158897,-58.5098228615615,
-52.6475541666667));
#261736=CARTESIAN_POINT('Ctrl Pts',(-45.7023404967,-59.5441932447742,-52.5892208333333));
#261737=CARTESIAN_POINT('Ctrl Pts',(-44.5079524583208,-59.5441932447742,
-52.5308875));
#261738=CARTESIAN_POINT('Ctrl Pts',(-43.3135644199415,-59.5441932447742,
-52.4725541666667));
#261739=CARTESIAN_POINT('Ctrl Pts',(-42.7163704007519,-58.5098228615615,
-52.4142208333334));
#261740=CARTESIAN_POINT('Ctrl Pts',(-42.1191763815623,-57.4754524783487,
-52.3558875000001));
#261741=CARTESIAN_POINT('Ctrl Pts',(-42.7163704007519,-56.4410820951361,
-52.2975541666667));
#261742=CARTESIAN_POINT('Ctrl Pts',(-43.3135644199415,-55.4067117119233,
-52.2392208333334));
#261743=CARTESIAN_POINT('Ctrl Pts',(-44.5079524583208,-55.4067117119234,
-52.1808875));
#261744=CARTESIAN_POINT('Ctrl Pts',(-45.7023404967,-55.4067117119233,-52.1225541666667));
#261745=CARTESIAN_POINT('Ctrl Pts',(-46.2995345158897,-56.4410820951361,
-52.0642208333334));
#261746=CARTESIAN_POINT('Ctrl Pts',(-46.8967285350793,-57.4754524783487,
-52.0058875));
#261747=CARTESIAN_POINT('Ctrl Pts',(-46.2995345158897,-58.5098228615615,
-51.9475541666667));
#261748=CARTESIAN_POINT('Ctrl Pts',(-45.7023404967,-59.5441932447742,-51.8892208333334));
#261749=CARTESIAN_POINT('Ctrl Pts',(-44.5079524583208,-59.5441932447742,
-51.8308875));
#261750=CARTESIAN_POINT('Ctrl Pts',(-43.3135644199415,-59.5441932447742,
-51.7725541666667));
#261751=CARTESIAN_POINT('Ctrl Pts',(-42.7163704007519,-58.5098228615615,
-51.7142208333334));
#261752=CARTESIAN_POINT('Ctrl Pts',(-42.1191763815623,-57.4754524783487,
-51.6558875));
#261753=CARTESIAN_POINT('Ctrl Pts',(-42.7163704007519,-56.4410820951361,
-51.5975541666667));
#261754=CARTESIAN_POINT('Ctrl Pts',(-43.3135644199415,-55.4067117119233,
-51.5392208333333));
#261755=CARTESIAN_POINT('Ctrl Pts',(-44.5079524583208,-55.4067117119234,
-51.4808875));
#261756=CARTESIAN_POINT('Ctrl Pts',(-45.7023404967,-55.4067117119233,-51.4225541666667));
#261757=CARTESIAN_POINT('Ctrl Pts',(-46.2995345158897,-56.4410820951361,
-51.3642208333334));
#261758=CARTESIAN_POINT('Ctrl Pts',(-46.8967285350793,-57.4754524783487,
-51.3058875));
#261759=CARTESIAN_POINT('Ctrl Pts',(-46.2995345158897,-58.5098228615615,
-51.2475541666667));
#261760=CARTESIAN_POINT('Ctrl Pts',(-45.7023404967,-59.5441932447742,-51.1892208333334));
#261761=CARTESIAN_POINT('Ctrl Pts',(-44.5079524583208,-59.5441932447742,
-51.1308875));
#261762=CARTESIAN_POINT('Ctrl Pts',(-43.3135644199415,-59.5441932447742,
-51.0725541666667));
#261763=CARTESIAN_POINT('Ctrl Pts',(-42.7163704007519,-58.5098228615615,
-51.0142208333334));
#261764=CARTESIAN_POINT('Ctrl Pts',(-42.1191763815623,-57.4754524783487,
-50.9558875));
#261765=CARTESIAN_POINT('Ctrl Pts',(-42.7163704007519,-56.4410820951361,
-50.8975541666667));
#261766=CARTESIAN_POINT('Ctrl Pts',(-43.3135644199415,-55.4067117119233,
-50.8392208333333));
#261767=CARTESIAN_POINT('Ctrl Pts',(-44.5079524583208,-55.4067117119234,
-50.7808875));
#261768=CARTESIAN_POINT('Ctrl Pts',(-45.7023404967,-55.4067117119233,-50.7225541666667));
#261769=CARTESIAN_POINT('Ctrl Pts',(-46.2995345158897,-56.4410820951361,
-50.6642208333333));
#261770=CARTESIAN_POINT('Ctrl Pts',(-46.8967285350793,-57.4754524783487,
-50.6058875));
#261771=CARTESIAN_POINT('Ctrl Pts',(-46.2995345158897,-58.5098228615615,
-50.5475541666667));
#261772=CARTESIAN_POINT('Ctrl Pts',(-45.7023404967,-59.5441932447742,-50.4892208333333));
#261773=CARTESIAN_POINT('Ctrl Pts',(-44.5079524583208,-59.5441932447742,
-50.4308875));
#261774=CARTESIAN_POINT('Ctrl Pts',(-43.3135644199415,-59.5441932447742,
-50.3725541666667));
#261775=CARTESIAN_POINT('Ctrl Pts',(-42.7163704007519,-58.5098228615615,
-50.3142208333334));
#261776=CARTESIAN_POINT('Ctrl Pts',(-42.1191763815623,-57.4754524783487,
-50.2558875));
#261777=CARTESIAN_POINT('Ctrl Pts',(-42.7163704007519,-56.4410820951361,
-50.1975541666667));
#261778=CARTESIAN_POINT('Ctrl Pts',(-43.3135644199415,-55.4067117119233,
-50.1392208333333));
#261779=CARTESIAN_POINT('Ctrl Pts',(-44.5079524583208,-55.4067117119234,
-50.0808875));
#261780=CARTESIAN_POINT('Ctrl Pts',(-45.7023404967,-55.4067117119233,-50.0225541666667));
#261781=CARTESIAN_POINT('Ctrl Pts',(-46.2995345158897,-56.4410820951361,
-49.9642208333334));
#261782=CARTESIAN_POINT('Ctrl Pts',(-46.8967285350793,-57.4754524783487,
-49.9058875));
#261783=CARTESIAN_POINT('Ctrl Pts',(-46.2995345158897,-58.5098228615615,
-49.8475541666667));
#261784=CARTESIAN_POINT('Ctrl Pts',(-45.7023404967,-59.5441932447742,-49.7892208333333));
#261785=CARTESIAN_POINT('Ctrl Pts',(-44.5079524583208,-59.5441932447742,
-49.7308875));
#261786=CARTESIAN_POINT('Ctrl Pts',(-43.3135644199415,-59.5441932447742,
-49.6725541666667));
#261787=CARTESIAN_POINT('Ctrl Pts',(-42.7163704007519,-58.5098228615615,
-49.6142208333334));
#261788=CARTESIAN_POINT('Ctrl Pts',(-42.1191763815623,-57.4754524783487,
-49.5558875));
#261789=CARTESIAN_POINT('Ctrl Pts',(-42.7163704007519,-56.4410820951361,
-49.4975541666667));
#261790=CARTESIAN_POINT('Ctrl Pts',(-43.3135644199415,-55.4067117119233,
-49.4392208333333));
#261791=CARTESIAN_POINT('Ctrl Pts',(-44.5079524583208,-55.4067117119234,
-49.3808875));
#261792=CARTESIAN_POINT('Ctrl Pts',(-45.7023404967,-55.4067117119233,-49.3225541666667));
#261793=CARTESIAN_POINT('Ctrl Pts',(-46.2995345158897,-56.4410820951361,
-49.2642208333334));
#261794=CARTESIAN_POINT('Ctrl Pts',(-46.8967285350793,-57.4754524783487,
-49.2058875));
#261795=CARTESIAN_POINT('Ctrl Pts',(-46.2995345158897,-58.5098228615615,
-49.1475541666667));
#261796=CARTESIAN_POINT('Ctrl Pts',(-45.7023404967,-59.5441932447742,-49.0892208333333));
#261797=CARTESIAN_POINT('Ctrl Pts',(-44.5079524583208,-59.5441932447742,
-49.0308875));
#261798=CARTESIAN_POINT('Ctrl Pts',(-43.3135644199415,-59.5441932447742,
-48.9725541666667));
#261799=CARTESIAN_POINT('Ctrl Pts',(-42.7163704007519,-58.5098228615615,
-48.9142208333334));
#261800=CARTESIAN_POINT('Ctrl Pts',(-42.1191763815623,-57.4754524783487,
-48.8558875));
#261801=CARTESIAN_POINT('Ctrl Pts',(-42.7163704007519,-56.4410820951361,
-48.7975541666667));
#261802=CARTESIAN_POINT('Ctrl Pts',(-43.3135644199415,-55.4067117119233,
-48.7392208333334));
#261803=CARTESIAN_POINT('Ctrl Pts',(-44.5079524583208,-55.4067117119234,
-48.6808875));
#261804=CARTESIAN_POINT('Ctrl Pts',(-45.7023404967,-55.4067117119233,-48.6225541666667));
#261805=CARTESIAN_POINT('Ctrl Pts',(-46.2995345158897,-56.4410820951361,
-48.5642208333334));
#261806=CARTESIAN_POINT('Ctrl Pts',(-46.8967285350793,-57.4754524783487,
-48.5058875));
#261807=CARTESIAN_POINT('Ctrl Pts',(-46.2995345158897,-58.5098228615615,
-48.4475541666667));
#261808=CARTESIAN_POINT('Ctrl Pts',(-45.7023404967,-59.5441932447742,-48.3892208333334));
#261809=CARTESIAN_POINT('Ctrl Pts',(-44.5079524583208,-59.5441932447742,
-48.3308875));
#261810=CARTESIAN_POINT('Ctrl Pts',(-43.3135644199415,-59.5441932447742,
-48.2725541666667));
#261811=CARTESIAN_POINT('Ctrl Pts',(-42.7163704007519,-58.5098228615615,
-48.2142208333334));
#261812=CARTESIAN_POINT('Ctrl Pts',(-42.1191763815623,-57.4754524783487,
-48.1558875));
#261813=CARTESIAN_POINT('Ctrl Pts',(-42.7163704007519,-56.4410820951361,
-48.0975541666667));
#261814=CARTESIAN_POINT('Ctrl Pts',(-43.3135644199415,-55.4067117119233,
-48.0392208333334));
#261815=CARTESIAN_POINT('Ctrl Pts',(-44.5079524583208,-55.4067117119234,
-47.9808875));
#261816=CARTESIAN_POINT('Ctrl Pts',(-45.7023404967,-55.4067117119233,-47.9225541666667));
#261817=CARTESIAN_POINT('Ctrl Pts',(-46.2995345158897,-56.4410820951361,
-47.8642208333334));
#261818=CARTESIAN_POINT('Ctrl Pts',(-46.8967285350793,-57.4754524783487,
-47.8058875000001));
#261819=CARTESIAN_POINT('Ctrl Pts',(-46.2995345158897,-58.5098228615615,
-47.7475541666667));
#261820=CARTESIAN_POINT('Ctrl Pts',(-45.7023404967,-59.5441932447742,-47.6892208333334));
#261821=CARTESIAN_POINT('Ctrl Pts',(-44.5079524583208,-59.5441932447742,
-47.6308875));
#261822=CARTESIAN_POINT('Ctrl Pts',(-43.3135644199415,-59.5441932447742,
-47.5725541666667));
#261823=CARTESIAN_POINT('Ctrl Pts',(-42.7163704007519,-58.5098228615615,
-47.5142208333333));
#261824=CARTESIAN_POINT('Ctrl Pts',(-42.1191763815623,-57.4754524783487,
-47.4558875));
#261825=CARTESIAN_POINT('Ctrl Pts',(-42.7163704007519,-56.4410820951361,
-47.3975541666667));
#261826=CARTESIAN_POINT('Ctrl Pts',(-43.3135644199415,-55.4067117119233,
-47.3392208333334));
#261827=CARTESIAN_POINT('Ctrl Pts',(-44.5079524583208,-55.4067117119234,
-47.2808875));
#261828=CARTESIAN_POINT('Ctrl Pts',(-45.7023404967,-55.4067117119233,-47.2225541666667));
#261829=CARTESIAN_POINT('Ctrl Pts',(-46.2995345158897,-56.4410820951361,
-47.1642208333334));
#261830=CARTESIAN_POINT('Ctrl Pts',(-46.8967285350793,-57.4754524783487,
-47.1058875));
#261831=CARTESIAN_POINT('Ctrl Pts',(-46.2995345158897,-58.5098228615615,
-47.0475541666667));
#261832=CARTESIAN_POINT('Ctrl Pts',(-45.7023404967,-59.5441932447742,-46.9892208333334));
#261833=CARTESIAN_POINT('Ctrl Pts',(-44.5079524583208,-59.5441932447742,
-46.9308875));
#261834=CARTESIAN_POINT('Ctrl Pts',(-43.3135644199415,-59.5441932447742,
-46.8725541666667));
#261835=CARTESIAN_POINT('Ctrl Pts',(-42.7163704007519,-58.5098228615615,
-46.8142208333334));
#261836=CARTESIAN_POINT('Ctrl Pts',(-42.1191763815623,-57.4754524783487,
-46.7558875));
#261837=CARTESIAN_POINT('Ctrl Pts',(-42.7163704007519,-56.4410820951361,
-46.6975541666667));
#261838=CARTESIAN_POINT('Ctrl Pts',(-43.3135644199415,-55.4067117119233,
-46.6392208333334));
#261839=CARTESIAN_POINT('Ctrl Pts',(-44.5079524583208,-55.4067117119234,
-46.5808875));
#261840=CARTESIAN_POINT('Ctrl Pts',(-45.7023404967,-55.4067117119233,-46.5225541666667));
#261841=CARTESIAN_POINT('Ctrl Pts',(-46.2995345158897,-56.4410820951361,
-46.4642208333334));
#261842=CARTESIAN_POINT('Ctrl Pts',(-46.8967285350793,-57.4754524783487,
-46.4058875));
#261843=CARTESIAN_POINT('Ctrl Pts',(-46.2995345158897,-58.5098228615615,
-46.3475541666667));
#261844=CARTESIAN_POINT('Ctrl Pts',(-45.7023404967,-59.5441932447742,-46.2892208333334));
#261845=CARTESIAN_POINT('Ctrl Pts',(-44.5079524583208,-59.5441932447742,
-46.2308875));
#261846=CARTESIAN_POINT('Ctrl Pts',(-43.3135644199415,-59.5441932447742,
-46.1725541666667));
#261847=CARTESIAN_POINT('Ctrl Pts',(-42.7163704007519,-58.5098228615615,
-46.1142208333334));
#261848=CARTESIAN_POINT('Ctrl Pts',(-42.1191763815623,-57.4754524783487,
-46.0558875));
#261849=CARTESIAN_POINT('Ctrl Pts',(-42.7163704007519,-56.4410820951361,
-45.9975541666667));
#261850=CARTESIAN_POINT('Ctrl Pts',(-43.3135644199415,-55.4067117119233,
-45.9392208333333));
#261851=CARTESIAN_POINT('Ctrl Pts',(-44.5079524583208,-55.4067117119234,
-45.8808875));
#261852=CARTESIAN_POINT('Ctrl Pts',(-45.7023404967,-55.4067117119233,-45.8225541666667));
#261853=CARTESIAN_POINT('Ctrl Pts',(-46.2995345158897,-56.4410820951361,
-45.7642208333334));
#261854=CARTESIAN_POINT('Ctrl Pts',(-46.8967285350793,-57.4754524783487,
-45.7058875));
#261855=CARTESIAN_POINT('Ctrl Pts',(-46.2995345158897,-58.5098228615615,
-45.6475541666667));
#261856=CARTESIAN_POINT('Ctrl Pts',(-45.7023404967,-59.5441932447742,-45.5892208333334));
#261857=CARTESIAN_POINT('Ctrl Pts',(-44.5079524583208,-59.5441932447742,
-45.5308875));
#261858=CARTESIAN_POINT('Ctrl Pts',(-43.3135644199415,-59.5441932447742,
-45.4725541666667));
#261859=CARTESIAN_POINT('Ctrl Pts',(-42.7163704007519,-58.5098228615615,
-45.4142208333334));
#261860=CARTESIAN_POINT('Ctrl Pts',(-42.1191763815623,-57.4754524783487,
-45.3558875));
#261861=CARTESIAN_POINT('Ctrl Pts',(-42.7163704007519,-56.4410820951361,
-45.2975541666667));
#261862=CARTESIAN_POINT('Ctrl Pts',(-43.3135644199415,-55.4067117119233,
-45.2392208333333));
#261863=CARTESIAN_POINT('Ctrl Pts',(-44.5079524583208,-55.4067117119234,
-45.1808875));
#261864=CARTESIAN_POINT('Ctrl Pts',(-45.7023404967,-55.4067117119233,-45.1225541666667));
#261865=CARTESIAN_POINT('Ctrl Pts',(-46.2995345158897,-56.4410820951361,
-45.0642208333334));
#261866=CARTESIAN_POINT('Ctrl Pts',(-46.8967285350793,-57.4754524783487,
-45.0058875));
#261867=CARTESIAN_POINT('Ctrl Pts',(-46.2995345158897,-58.5098228615615,
-44.9475541666667));
#261868=CARTESIAN_POINT('Ctrl Pts',(-45.7023404967,-59.5441932447742,-44.8892208333333));
#261869=CARTESIAN_POINT('Ctrl Pts',(-44.5079524583208,-59.5441932447742,
-44.8308875));
#261870=CARTESIAN_POINT('Ctrl Pts',(-43.3135644199415,-59.5441932447742,
-44.7725541666667));
#261871=CARTESIAN_POINT('Ctrl Pts',(-42.7163704007519,-58.5098228615615,
-44.7142208333334));
#261872=CARTESIAN_POINT('Ctrl Pts',(-42.1191763815623,-57.4754524783487,
-44.6558875));
#261873=CARTESIAN_POINT('Ctrl Pts',(-42.7163704007519,-56.4410820951361,
-44.5975541666667));
#261874=CARTESIAN_POINT('Ctrl Pts',(-43.3135644199415,-55.4067117119233,
-44.5392208333333));
#261875=CARTESIAN_POINT('Ctrl Pts',(-44.5079524583208,-55.4067117119234,
-44.4808875000001));
#261876=CARTESIAN_POINT('Ctrl Pts',(-45.7023404967,-55.4067117119233,-44.4225541666667));
#261877=CARTESIAN_POINT('Ctrl Pts',(-46.2995345158897,-56.4410820951361,
-44.3642208333333));
#261878=CARTESIAN_POINT('Ctrl Pts',(-46.8967285350793,-57.4754524783487,
-44.3058875));
#261879=CARTESIAN_POINT('Ctrl Pts',(-46.2995345158897,-58.5098228615615,
-44.2475541666667));
#261880=CARTESIAN_POINT('Ctrl Pts',(-45.7023404967,-59.5441932447742,-44.1892208333334));
#261881=CARTESIAN_POINT('Ctrl Pts',(-44.5079524583208,-59.5441932447742,
-44.1308875000001));
#261882=CARTESIAN_POINT('Ctrl Pts',(-43.3135644199415,-59.5441932447742,
-44.0725541666667));
#261883=CARTESIAN_POINT('Ctrl Pts',(-42.7163704007519,-58.5098228615615,
-44.0142208333334));
#261884=CARTESIAN_POINT('Ctrl Pts',(-42.1191763815623,-57.4754524783487,
-43.9558875));
#261885=CARTESIAN_POINT('Ctrl Pts',(-42.7163704007519,-56.4410820951361,
-43.8975541666667));
#261886=CARTESIAN_POINT('Ctrl Pts',(-43.3135644199415,-55.4067117119233,
-43.8392208333333));
#261887=CARTESIAN_POINT('Ctrl Pts',(-44.5079524583208,-55.4067117119234,
-43.7808875));
#261888=CARTESIAN_POINT('Ctrl Pts',(-45.7023404967,-55.4067117119233,-43.7225541666667));
#261889=CARTESIAN_POINT('Ctrl Pts',(-46.2995345158897,-56.4410820951361,
-43.6642208333334));
#261890=CARTESIAN_POINT('Ctrl Pts',(-46.8967285350793,-57.4754524783487,
-43.6058875));
#261891=CARTESIAN_POINT('Ctrl Pts',(-46.2995345158897,-58.5098228615615,
-43.5475541666667));
#261892=CARTESIAN_POINT('Ctrl Pts',(-45.7023404967,-59.5441932447742,-43.4892208333333));
#261893=CARTESIAN_POINT('Ctrl Pts',(-44.5079524583208,-59.5441932447742,
-43.4308875));
#261894=CARTESIAN_POINT('Ctrl Pts',(-43.3135644199415,-59.5441932447742,
-43.3725541666667));
#261895=CARTESIAN_POINT('Ctrl Pts',(-42.7163704007519,-58.5098228615615,
-43.3142208333334));
#261896=CARTESIAN_POINT('Ctrl Pts',(-42.1191763815623,-57.4754524783487,
-43.2558875));
#261897=CARTESIAN_POINT('Ctrl Pts',(-42.7163704007519,-56.4410820951361,
-43.1975541666667));
#261898=CARTESIAN_POINT('Ctrl Pts',(-43.3135644199415,-55.4067117119233,
-43.1392208333334));
#261899=CARTESIAN_POINT('Ctrl Pts',(-44.5079524583208,-55.4067117119234,
-43.0808875));
#261900=CARTESIAN_POINT('Ctrl Pts',(-45.7023404967,-55.4067117119233,-43.0225541666667));
#261901=CARTESIAN_POINT('Ctrl Pts',(-46.2995345158897,-56.4410820951361,
-42.9642208333334));
#261902=CARTESIAN_POINT('Ctrl Pts',(-46.8967285350793,-57.4754524783487,
-42.9058875));
#261903=CARTESIAN_POINT('Ctrl Pts',(-46.2995345158897,-58.5098228615615,
-42.8475541666667));
#261904=CARTESIAN_POINT('Ctrl Pts',(-45.7023404967,-59.5441932447742,-42.7892208333334));
#261905=CARTESIAN_POINT('Ctrl Pts',(-44.5079524583208,-59.5441932447742,
-42.7308875000001));
#261906=CARTESIAN_POINT('Ctrl Pts',(-43.3135644199415,-59.5441932447742,
-42.6725541666667));
#261907=CARTESIAN_POINT('Ctrl Pts',(-42.7163704007519,-58.5098228615615,
-42.6142208333334));
#261908=CARTESIAN_POINT('Ctrl Pts',(-42.1191763815623,-57.4754524783487,
-42.5558875));
#261909=CARTESIAN_POINT('Ctrl Pts',(-42.7163704007519,-56.4410820951361,
-42.4975541666667));
#261910=CARTESIAN_POINT('Ctrl Pts',(-43.3135644199415,-55.4067117119233,
-42.4392208333334));
#261911=CARTESIAN_POINT('Ctrl Pts',(-44.5079524583208,-55.4067117119234,
-42.3808875000001));
#261912=CARTESIAN_POINT('Ctrl Pts',(-45.7023404967,-55.4067117119233,-42.3225541666667));
#261913=CARTESIAN_POINT('Ctrl Pts',(-46.2995345158897,-56.4410820951361,
-42.2642208333334));
#261914=CARTESIAN_POINT('Ctrl Pts',(-46.8967285350793,-57.4754524783487,
-42.2058875));
#261915=CARTESIAN_POINT('Ctrl Pts',(-46.2995345158897,-58.5098228615615,
-42.1475541666667));
#261916=CARTESIAN_POINT('Ctrl Pts',(-45.7023404967,-59.5441932447742,-42.0892208333334));
#261917=CARTESIAN_POINT('Ctrl Pts',(-44.5079524583208,-59.5441932447742,
-42.0308875000001));
#261918=CARTESIAN_POINT('Ctrl Pts',(-43.3135644199415,-59.5441932447742,
-41.9725541666667));
#261919=CARTESIAN_POINT('Ctrl Pts',(-42.7163704007519,-58.5098228615615,
-41.9142208333334));
#261920=CARTESIAN_POINT('Ctrl Pts',(-42.1191763815623,-57.4754524783487,
-41.8558875));
#261921=CARTESIAN_POINT('Ctrl Pts',(-42.7163704007519,-56.4410820951361,
-41.7975541666667));
#261922=CARTESIAN_POINT('Ctrl Pts',(-43.3135644199415,-55.4067117119233,
-41.7392208333334));
#261923=CARTESIAN_POINT('Ctrl Pts',(-44.5079524583208,-55.4067117119234,
-41.6808875000001));
#261924=CARTESIAN_POINT('Ctrl Pts',(-45.7023404967,-55.4067117119233,-41.6225541666667));
#261925=CARTESIAN_POINT('Ctrl Pts',(-46.2995345158897,-56.4410820951361,
-41.5642208333334));
#261926=CARTESIAN_POINT('Ctrl Pts',(-46.8967285350793,-57.4754524783487,
-41.5058875));
#261927=CARTESIAN_POINT('Ctrl Pts',(-46.2995345158897,-58.5098228615615,
-41.4475541666667));
#261928=CARTESIAN_POINT('Ctrl Pts',(-45.7023404967,-59.5441932447742,-41.3892208333334));
#261929=CARTESIAN_POINT('Ctrl Pts',(-44.5079524583208,-59.5441932447742,
-41.3308875000001));
#261930=CARTESIAN_POINT('Ctrl Pts',(-43.3135644199415,-59.5441932447742,
-41.2725541666667));
#261931=CARTESIAN_POINT('Ctrl Pts',(-42.7163704007519,-58.5098228615615,
-41.2142208333333));
#261932=CARTESIAN_POINT('Ctrl Pts',(-42.1191763815623,-57.4754524783487,
-41.1558875));
#261933=CARTESIAN_POINT('Ctrl Pts',(-42.7163704007519,-56.4410820951361,
-41.0975541666667));
#261934=CARTESIAN_POINT('Ctrl Pts',(-43.3135644199415,-55.4067117119233,
-41.0392208333333));
#261935=CARTESIAN_POINT('Ctrl Pts',(-44.5079524583208,-55.4067117119234,
-40.9808875000001));
#261936=CARTESIAN_POINT('Ctrl Pts',(-45.7023404967,-55.4067117119233,-40.9225541666667));
#261937=CARTESIAN_POINT('Ctrl Pts',(-46.2995345158897,-56.4410820951361,
-40.8642208333334));
#261938=CARTESIAN_POINT('Ctrl Pts',(-46.8967285350793,-57.4754524783487,
-40.8058875));
#261939=CARTESIAN_POINT('Ctrl Pts',(-46.2995345158897,-58.5098228615615,
-40.7475541666667));
#261940=CARTESIAN_POINT('Ctrl Pts',(-45.7023404967,-59.5441932447742,-40.6892208333333));
#261941=CARTESIAN_POINT('Ctrl Pts',(-44.5079524583208,-59.5441932447742,
-40.6308875));
#261942=CARTESIAN_POINT('Ctrl Pts',(-43.3135644199415,-59.5441932447742,
-40.5725541666667));
#261943=CARTESIAN_POINT('Ctrl Pts',(-42.7163704007519,-58.5098228615615,
-40.5142208333333));
#261944=CARTESIAN_POINT('Ctrl Pts',(-42.1191763815623,-57.4754524783487,
-40.4558875));
#261945=CARTESIAN_POINT('Ctrl Pts',(-42.7163704007519,-56.4410820951361,
-40.3975541666667));
#261946=CARTESIAN_POINT('Ctrl Pts',(-43.3135644199415,-55.4067117119233,
-40.3392208333333));
#261947=CARTESIAN_POINT('Ctrl Pts',(-44.5079524583208,-55.4067117119234,
-40.2808875));
#261948=CARTESIAN_POINT('Ctrl Pts',(-45.7023404967,-55.4067117119233,-40.2225541666667));
#261949=CARTESIAN_POINT('Ctrl Pts',(-46.2995345158897,-56.4410820951361,
-40.1642208333333));
#261950=CARTESIAN_POINT('Ctrl Pts',(-46.8967285350793,-57.4754524783487,
-40.1058875));
#261951=CARTESIAN_POINT('Ctrl Pts',(-46.2995345158897,-58.5098228615615,
-40.0475541666667));
#261952=CARTESIAN_POINT('Ctrl Pts',(-45.7023404967,-59.5441932447742,-39.9892208333333));
#261953=CARTESIAN_POINT('Ctrl Pts',(-44.5079524583208,-59.5441932447742,
-39.9308875));
#261954=CARTESIAN_POINT('Ctrl Pts',(-43.3135644199415,-59.5441932447742,
-39.8725541666667));
#261955=CARTESIAN_POINT('Ctrl Pts',(-42.7163704007519,-58.5098228615615,
-39.8142208333334));
#261956=CARTESIAN_POINT('Ctrl Pts',(-42.1191763815623,-57.4754524783487,
-39.7558875));
#261957=CARTESIAN_POINT('Ctrl Pts',(-42.7163704007519,-56.4410820951361,
-39.6975541666667));
#261958=CARTESIAN_POINT('Ctrl Pts',(-43.3135644199415,-55.4067117119233,
-39.6392208333334));
#261959=CARTESIAN_POINT('Ctrl Pts',(-44.5079524583208,-55.4067117119234,
-39.5808875000001));
#261960=CARTESIAN_POINT('Ctrl Pts',(-45.7023404967,-55.4067117119233,-39.5225541666667));
#261961=CARTESIAN_POINT('Ctrl Pts',(-46.2995345158897,-56.4410820951361,
-39.4642208333333));
#261962=CARTESIAN_POINT('Ctrl Pts',(-46.8967285350793,-57.4754524783487,
-39.4058875));
#261963=CARTESIAN_POINT('Ctrl Pts',(-46.2995345158897,-58.5098228615615,
-39.3475541666667));
#261964=CARTESIAN_POINT('Ctrl Pts',(-45.7023404967,-59.5441932447742,-39.2892208333334));
#261965=CARTESIAN_POINT('Ctrl Pts',(-44.5079524583208,-59.5441932447742,
-39.2308875));
#261966=CARTESIAN_POINT('Ctrl Pts',(-43.3135644199415,-59.5441932447742,
-39.1725541666667));
#261967=CARTESIAN_POINT('Ctrl Pts',(-42.7163704007519,-58.5098228615615,
-39.1142208333333));
#261968=CARTESIAN_POINT('Ctrl Pts',(-42.1191763815623,-57.4754524783487,
-39.0558875));
#261969=CARTESIAN_POINT('Ctrl Pts',(-42.7163704007519,-56.4410820951361,
-38.9975541666667));
#261970=CARTESIAN_POINT('Ctrl Pts',(-43.3135644199415,-55.4067117119233,
-38.9392208333334));
#261971=CARTESIAN_POINT('Ctrl Pts',(-44.5079524583208,-55.4067117119234,
-38.8808875));
#261972=CARTESIAN_POINT('Ctrl Pts',(-45.7023404967,-55.4067117119233,-38.8225541666667));
#261973=CARTESIAN_POINT('Ctrl Pts',(-46.2995345158897,-56.4410820951361,
-38.7642208333333));
#261974=CARTESIAN_POINT('Ctrl Pts',(-46.8967285350793,-57.4754524783487,
-38.7058875));
#261975=CARTESIAN_POINT('Ctrl Pts',(-46.2995345158897,-58.5098228615615,
-38.6475541666667));
#261976=CARTESIAN_POINT('Ctrl Pts',(-45.7023404967,-59.5441932447742,-38.5892208333334));
#261977=CARTESIAN_POINT('Ctrl Pts',(-44.5079524583208,-59.5441932447742,
-38.5308875));
#261978=CARTESIAN_POINT('Ctrl Pts',(-43.3135644199415,-59.5441932447742,
-38.4725541666667));
#261979=CARTESIAN_POINT('Ctrl Pts',(-42.7163704007519,-58.5098228615615,
-38.4142208333334));
#261980=CARTESIAN_POINT('Ctrl Pts',(-42.1191763815623,-57.4754524783487,
-38.3558875));
#261981=CARTESIAN_POINT('Ctrl Pts',(-42.7163704007519,-56.4410820951361,
-38.2975541666667));
#261982=CARTESIAN_POINT('Ctrl Pts',(-43.3135644199415,-55.4067117119233,
-38.2392208333333));
#261983=CARTESIAN_POINT('Ctrl Pts',(-44.5079524583208,-55.4067117119234,
-38.1808875000001));
#261984=CARTESIAN_POINT('Ctrl Pts',(-45.7023404967,-55.4067117119233,-38.1225541666667));
#261985=CARTESIAN_POINT('Ctrl Pts',(-46.2995345158897,-56.4410820951361,
-38.0642208333334));
#261986=CARTESIAN_POINT('Ctrl Pts',(-46.8967285350793,-57.4754524783487,
-38.0058875));
#261987=CARTESIAN_POINT('Ctrl Pts',(-46.2995345158897,-58.5098228615615,
-37.9475541666667));
#261988=CARTESIAN_POINT('Ctrl Pts',(-45.7023404967,-59.5441932447742,-37.8892208333334));
#261989=CARTESIAN_POINT('Ctrl Pts',(-44.5079524583208,-59.5441932447742,
-37.8308875));
#261990=CARTESIAN_POINT('Ctrl Pts',(-43.3135644199415,-59.5441932447742,
-37.7725541666667));
#261991=CARTESIAN_POINT('Ctrl Pts',(-42.7163704007519,-58.5098228615615,
-37.7142208333333));
#261992=CARTESIAN_POINT('Ctrl Pts',(-42.1191763815623,-57.4754524783487,
-37.6558875));
#261993=CARTESIAN_POINT('Ctrl Pts',(-42.7163704007519,-56.4410820951361,
-37.5975541666667));
#261994=CARTESIAN_POINT('Ctrl Pts',(-43.3135644199415,-55.4067117119233,
-37.5392208333334));
#261995=CARTESIAN_POINT('Ctrl Pts',(-44.5079524583208,-55.4067117119234,
-37.4808875));
#261996=CARTESIAN_POINT('Ctrl Pts',(-45.7023404967,-55.4067117119233,-37.4225541666667));
#261997=CARTESIAN_POINT('Ctrl Pts',(-46.2995345158897,-56.4410820951361,
-37.3642208333333));
#261998=CARTESIAN_POINT('Ctrl Pts',(-46.8967285350793,-57.4754524783487,
-37.3058875));
#261999=CARTESIAN_POINT('Ctrl Pts',(-46.2995345158897,-58.5098228615615,
-37.2475541666667));
#262000=CARTESIAN_POINT('Ctrl Pts',(-46.2219998538691,-58.6441168355289,
-37.239980655983));
#262001=CARTESIAN_POINT('Ctrl Pts',(-46.1253112086366,-58.7653513237809,
-37.2318399189827));
#262002=CARTESIAN_POINT('',(-43.5801633933645,-59.1235613262403,-39.7713833389821));
#262003=CARTESIAN_POINT('Ctrl Pts',(-43.5801633933644,-59.1235613262403,
-39.7713833389821));
#262004=CARTESIAN_POINT('Ctrl Pts',(-43.7343054498627,-59.2338784870309,
-39.7948518398299));
#262005=CARTESIAN_POINT('Ctrl Pts',(-43.9040124134241,-59.3204101936929,
-39.8178912026959));
#262006=CARTESIAN_POINT('Ctrl Pts',(-44.2515556962439,-59.4355123678575,
-39.8599414219136));
#262007=CARTESIAN_POINT('Ctrl Pts',(-44.4268269797126,-59.467295367295,
-39.8787333172327));
#262008=CARTESIAN_POINT('Ctrl Pts',(-44.6028144650695,-59.4732025036409,
-39.8960584758442));
#262009=CARTESIAN_POINT('Ctrl Pts',(-45.3904396609892,-55.7772425608068,
-39.4382820396906));
#262010=CARTESIAN_POINT('Ctrl Pts',(-45.127863070379,-55.6880798854926,
-39.4307498115588));
#262011=CARTESIAN_POINT('Ctrl Pts',(-44.8501824314513,-55.65124567929,-39.4267602137955));
#262012=CARTESIAN_POINT('Ctrl Pts',(-44.272714170611,-55.6905726318167,
-39.4247756080659));
#262013=CARTESIAN_POINT('Ctrl Pts',(-44.0459076609694,-55.7713412684499,
-39.429749730603));
#262014=CARTESIAN_POINT('Ctrl Pts',(-43.7113885810197,-55.9220046278699,
-39.4400449959408));
#262015=CARTESIAN_POINT('Ctrl Pts',(-43.5414996037919,-56.0332426275574,
-39.4481441882684));
#262016=CARTESIAN_POINT('Ctrl Pts',(-43.3043122263345,-56.2496978707112,
-39.463510471409));
#262017=CARTESIAN_POINT('Ctrl Pts',(-43.2243163532729,-56.3378976358391,
-39.4697052531975));
#262018=CARTESIAN_POINT('Ctrl Pts',(-43.1510722028329,-56.4358173812626,
-39.4764626542922));
#262019=CARTESIAN_POINT('Ctrl Pts',(-43.1490501437171,-56.4385358974063,
-39.4766501743115));
#262020=CARTESIAN_POINT('Ctrl Pts',(-43.1429859160015,-56.4467348329594,
-39.477215478004));
#262021=CARTESIAN_POINT('Ctrl Pts',(-43.1389661987681,-56.4522315327458,
-39.4775941325867));
#262022=CARTESIAN_POINT('Ctrl Pts',(-43.1268675096469,-56.4689648450911,
-39.4787458758348));
#262023=CARTESIAN_POINT('Ctrl Pts',(-43.1188830933565,-56.4802673936354,
-39.4795224926569));
#262024=CARTESIAN_POINT('Ctrl Pts',(-43.0947203700718,-56.5152795267588,
-39.4819247606914));
#262025=CARTESIAN_POINT('Ctrl Pts',(-43.0789875520127,-56.5392273724946,
-39.4835617361158));
#262026=CARTESIAN_POINT('Ctrl Pts',(-43.0434745327861,-56.5960535881947,
-39.4874324719544));
#262027=CARTESIAN_POINT('Ctrl Pts',(-43.0238940213821,-56.6295843258748,
-39.489685078298));
#262028=CARTESIAN_POINT('Ctrl Pts',(-42.8971332874247,-56.8634741974343,
-39.505873075687));
#262029=CARTESIAN_POINT('Ctrl Pts',(-42.8269092740029,-57.0813286464389,
-39.5229511009414));
#262030=CARTESIAN_POINT('Ctrl Pts',(-42.7655858512823,-57.540255899092,
-39.5633280588462));
#262031=CARTESIAN_POINT('Ctrl Pts',(-42.7783791664303,-57.7782929357622,
-39.5865645306336));
#262032=CARTESIAN_POINT('Ctrl Pts',(-42.8697928172135,-58.1607402986936,
-39.6279729382228));
#262033=CARTESIAN_POINT('Ctrl Pts',(-42.9407328612678,-58.3782873632772,
-39.6516656052854));
#262034=CARTESIAN_POINT('Ctrl Pts',(-43.2188700913275,-58.8092261000328,
-39.7119082485011));
#262035=CARTESIAN_POINT('Ctrl Pts',(-43.3855231146887,-58.9842601944999,
-39.741748885875));
#262036=CARTESIAN_POINT('Ctrl Pts',(-43.5801633933645,-59.1235613262403,
-39.7713833389821));
#262037=CARTESIAN_POINT('Ctrl Pts',(-44.5079524583208,-59.1441977614012,
-52.99995));
#262038=CARTESIAN_POINT('Ctrl Pts',(-43.5445019199415,-59.1441977614012,
-52.9416166666667));
#262039=CARTESIAN_POINT('Ctrl Pts',(-43.0627766507519,-58.309825119875,
-52.8832833333334));
#262040=CARTESIAN_POINT('Ctrl Pts',(-42.5810513815623,-57.4754524783487,
-52.82495));
#262041=CARTESIAN_POINT('Ctrl Pts',(-43.0627766507519,-56.6410798368225,
-52.7666166666667));
#262042=CARTESIAN_POINT('Ctrl Pts',(-43.5445019199415,-55.8067071952963,
-52.7082833333333));
#262043=CARTESIAN_POINT('Ctrl Pts',(-44.5079524583208,-55.8067071952963,
-52.64995));
#262044=CARTESIAN_POINT('Ctrl Pts',(-45.4714029967,-55.8067071952963,-52.5916166666666));
#262045=CARTESIAN_POINT('Ctrl Pts',(-45.9531282658897,-56.6410798368225,
-52.5332833333334));
#262046=CARTESIAN_POINT('Ctrl Pts',(-46.4348535350793,-57.4754524783487,
-52.4749500000001));
#262047=CARTESIAN_POINT('Ctrl Pts',(-45.9531282658897,-58.309825119875,
-52.4166166666667));
#262048=CARTESIAN_POINT('Ctrl Pts',(-45.4714029967,-59.1441977614012,-52.3582833333334));
#262049=CARTESIAN_POINT('Ctrl Pts',(-44.5079524583208,-59.1441977614012,
-52.29995));
#262050=CARTESIAN_POINT('Ctrl Pts',(-43.5445019199415,-59.1441977614012,
-52.2416166666667));
#262051=CARTESIAN_POINT('Ctrl Pts',(-43.0627766507519,-58.309825119875,
-52.1832833333333));
#262052=CARTESIAN_POINT('Ctrl Pts',(-42.5810513815623,-57.4754524783487,
-52.12495));
#262053=CARTESIAN_POINT('Ctrl Pts',(-43.0627766507519,-56.6410798368225,
-52.0666166666667));
#262054=CARTESIAN_POINT('Ctrl Pts',(-43.5445019199415,-55.8067071952963,
-52.0082833333333));
#262055=CARTESIAN_POINT('Ctrl Pts',(-44.5079524583208,-55.8067071952963,
-51.94995));
#262056=CARTESIAN_POINT('Ctrl Pts',(-45.4714029967,-55.8067071952963,-51.8916166666667));
#262057=CARTESIAN_POINT('Ctrl Pts',(-45.9531282658897,-56.6410798368225,
-51.8332833333334));
#262058=CARTESIAN_POINT('Ctrl Pts',(-46.4348535350793,-57.4754524783487,
-51.77495));
#262059=CARTESIAN_POINT('Ctrl Pts',(-45.9531282658897,-58.309825119875,
-51.7166166666667));
#262060=CARTESIAN_POINT('Ctrl Pts',(-45.4714029967,-59.1441977614012,-51.6582833333333));
#262061=CARTESIAN_POINT('Ctrl Pts',(-44.5079524583208,-59.1441977614012,
-51.59995));
#262062=CARTESIAN_POINT('Ctrl Pts',(-43.5445019199415,-59.1441977614012,
-51.5416166666667));
#262063=CARTESIAN_POINT('Ctrl Pts',(-43.0627766507519,-58.309825119875,
-51.4832833333334));
#262064=CARTESIAN_POINT('Ctrl Pts',(-42.5810513815623,-57.4754524783487,
-51.42495));
#262065=CARTESIAN_POINT('Ctrl Pts',(-43.0627766507519,-56.6410798368225,
-51.3666166666667));
#262066=CARTESIAN_POINT('Ctrl Pts',(-43.5445019199415,-55.8067071952963,
-51.3082833333333));
#262067=CARTESIAN_POINT('Ctrl Pts',(-44.5079524583208,-55.8067071952963,
-51.24995));
#262068=CARTESIAN_POINT('Ctrl Pts',(-45.4714029967,-55.8067071952963,-51.1916166666667));
#262069=CARTESIAN_POINT('Ctrl Pts',(-45.9531282658897,-56.6410798368225,
-51.1332833333334));
#262070=CARTESIAN_POINT('Ctrl Pts',(-46.4348535350793,-57.4754524783487,
-51.07495));
#262071=CARTESIAN_POINT('Ctrl Pts',(-45.9531282658897,-58.309825119875,
-51.0166166666667));
#262072=CARTESIAN_POINT('Ctrl Pts',(-45.4714029967,-59.1441977614012,-50.9582833333334));
#262073=CARTESIAN_POINT('Ctrl Pts',(-44.5079524583208,-59.1441977614012,
-50.89995));
#262074=CARTESIAN_POINT('Ctrl Pts',(-43.5445019199415,-59.1441977614012,
-50.8416166666667));
#262075=CARTESIAN_POINT('Ctrl Pts',(-43.0627766507519,-58.309825119875,
-50.7832833333333));
#262076=CARTESIAN_POINT('Ctrl Pts',(-42.5810513815623,-57.4754524783487,
-50.72495));
#262077=CARTESIAN_POINT('Ctrl Pts',(-43.0627766507519,-56.6410798368225,
-50.6666166666667));
#262078=CARTESIAN_POINT('Ctrl Pts',(-43.5445019199415,-55.8067071952963,
-50.6082833333334));
#262079=CARTESIAN_POINT('Ctrl Pts',(-44.5079524583208,-55.8067071952963,
-50.54995));
#262080=CARTESIAN_POINT('Ctrl Pts',(-45.4714029967,-55.8067071952963,-50.4916166666667));
#262081=CARTESIAN_POINT('Ctrl Pts',(-45.9531282658897,-56.6410798368225,
-50.4332833333333));
#262082=CARTESIAN_POINT('Ctrl Pts',(-46.4348535350793,-57.4754524783487,
-50.37495));
#262083=CARTESIAN_POINT('Ctrl Pts',(-45.9531282658897,-58.309825119875,
-50.3166166666667));
#262084=CARTESIAN_POINT('Ctrl Pts',(-45.4714029967,-59.1441977614012,-50.2582833333334));
#262085=CARTESIAN_POINT('Ctrl Pts',(-44.5079524583208,-59.1441977614012,
-50.19995));
#262086=CARTESIAN_POINT('Ctrl Pts',(-43.5445019199415,-59.1441977614012,
-50.1416166666667));
#262087=CARTESIAN_POINT('Ctrl Pts',(-43.0627766507519,-58.309825119875,
-50.0832833333334));
#262088=CARTESIAN_POINT('Ctrl Pts',(-42.5810513815623,-57.4754524783487,
-50.02495));
#262089=CARTESIAN_POINT('Ctrl Pts',(-43.0627766507519,-56.6410798368225,
-49.9666166666667));
#262090=CARTESIAN_POINT('Ctrl Pts',(-43.5445019199415,-55.8067071952963,
-49.9082833333334));
#262091=CARTESIAN_POINT('Ctrl Pts',(-44.5079524583208,-55.8067071952963,
-49.84995));
#262092=CARTESIAN_POINT('Ctrl Pts',(-45.4714029967,-55.8067071952963,-49.7916166666667));
#262093=CARTESIAN_POINT('Ctrl Pts',(-45.9531282658897,-56.6410798368225,
-49.7332833333334));
#262094=CARTESIAN_POINT('Ctrl Pts',(-46.4348535350793,-57.4754524783487,
-49.67495));
#262095=CARTESIAN_POINT('Ctrl Pts',(-45.9531282658897,-58.309825119875,
-49.6166166666667));
#262096=CARTESIAN_POINT('Ctrl Pts',(-45.4714029967,-59.1441977614012,-49.5582833333334));
#262097=CARTESIAN_POINT('Ctrl Pts',(-44.5079524583208,-59.1441977614012,
-49.49995));
#262098=CARTESIAN_POINT('Ctrl Pts',(-43.5445019199415,-59.1441977614012,
-49.4416166666667));
#262099=CARTESIAN_POINT('Ctrl Pts',(-43.0627766507519,-58.309825119875,
-49.3832833333334));
#262100=CARTESIAN_POINT('Ctrl Pts',(-42.5810513815623,-57.4754524783487,
-49.32495));
#262101=CARTESIAN_POINT('Ctrl Pts',(-43.0627766507519,-56.6410798368225,
-49.2666166666667));
#262102=CARTESIAN_POINT('Ctrl Pts',(-43.5445019199415,-55.8067071952963,
-49.2082833333334));
#262103=CARTESIAN_POINT('Ctrl Pts',(-44.5079524583208,-55.8067071952963,
-49.14995));
#262104=CARTESIAN_POINT('Ctrl Pts',(-45.4714029967,-55.8067071952963,-49.0916166666667));
#262105=CARTESIAN_POINT('Ctrl Pts',(-45.9531282658897,-56.6410798368225,
-49.0332833333333));
#262106=CARTESIAN_POINT('Ctrl Pts',(-46.4348535350793,-57.4754524783487,
-48.97495));
#262107=CARTESIAN_POINT('Ctrl Pts',(-45.9531282658897,-58.309825119875,
-48.9166166666667));
#262108=CARTESIAN_POINT('Ctrl Pts',(-45.4714029967,-59.1441977614012,-48.8582833333333));
#262109=CARTESIAN_POINT('Ctrl Pts',(-44.5079524583208,-59.1441977614012,
-48.79995));
#262110=CARTESIAN_POINT('Ctrl Pts',(-43.5445019199415,-59.1441977614012,
-48.7416166666667));
#262111=CARTESIAN_POINT('Ctrl Pts',(-43.0627766507519,-58.309825119875,
-48.6832833333334));
#262112=CARTESIAN_POINT('Ctrl Pts',(-42.5810513815623,-57.4754524783487,
-48.62495));
#262113=CARTESIAN_POINT('Ctrl Pts',(-43.0627766507519,-56.6410798368225,
-48.5666166666667));
#262114=CARTESIAN_POINT('Ctrl Pts',(-43.5445019199415,-55.8067071952963,
-48.5082833333334));
#262115=CARTESIAN_POINT('Ctrl Pts',(-44.5079524583208,-55.8067071952963,
-48.44995));
#262116=CARTESIAN_POINT('Ctrl Pts',(-45.4714029967,-55.8067071952963,-48.3916166666667));
#262117=CARTESIAN_POINT('Ctrl Pts',(-45.9531282658897,-56.6410798368225,
-48.3332833333334));
#262118=CARTESIAN_POINT('Ctrl Pts',(-46.4348535350793,-57.4754524783487,
-48.27495));
#262119=CARTESIAN_POINT('Ctrl Pts',(-45.9531282658897,-58.309825119875,
-48.2166166666667));
#262120=CARTESIAN_POINT('Ctrl Pts',(-45.4714029967,-59.1441977614012,-48.1582833333334));
#262121=CARTESIAN_POINT('Ctrl Pts',(-44.5079524583208,-59.1441977614012,
-48.09995));
#262122=CARTESIAN_POINT('Ctrl Pts',(-43.5445019199415,-59.1441977614012,
-48.0416166666667));
#262123=CARTESIAN_POINT('Ctrl Pts',(-43.0627766507519,-58.309825119875,
-47.9832833333334));
#262124=CARTESIAN_POINT('Ctrl Pts',(-42.5810513815623,-57.4754524783487,
-47.92495));
#262125=CARTESIAN_POINT('Ctrl Pts',(-43.0627766507519,-56.6410798368225,
-47.8666166666667));
#262126=CARTESIAN_POINT('Ctrl Pts',(-43.5445019199415,-55.8067071952963,
-47.8082833333333));
#262127=CARTESIAN_POINT('Ctrl Pts',(-44.5079524583208,-55.8067071952963,
-47.74995));
#262128=CARTESIAN_POINT('Ctrl Pts',(-45.4714029967,-55.8067071952963,-47.6916166666667));
#262129=CARTESIAN_POINT('Ctrl Pts',(-45.9531282658897,-56.6410798368225,
-47.6332833333333));
#262130=CARTESIAN_POINT('Ctrl Pts',(-46.4348535350793,-57.4754524783487,
-47.57495));
#262131=CARTESIAN_POINT('Ctrl Pts',(-45.9531282658897,-58.309825119875,
-47.5166166666667));
#262132=CARTESIAN_POINT('Ctrl Pts',(-45.4714029967,-59.1441977614012,-47.4582833333333));
#262133=CARTESIAN_POINT('Ctrl Pts',(-44.5079524583208,-59.1441977614012,
-47.39995));
#262134=CARTESIAN_POINT('Ctrl Pts',(-43.5445019199415,-59.1441977614012,
-47.3416166666666));
#262135=CARTESIAN_POINT('Ctrl Pts',(-43.0627766507519,-58.309825119875,
-47.2832833333333));
#262136=CARTESIAN_POINT('Ctrl Pts',(-42.5810513815623,-57.4754524783487,
-47.22495));
#262137=CARTESIAN_POINT('Ctrl Pts',(-43.0627766507519,-56.6410798368225,
-47.1666166666667));
#262138=CARTESIAN_POINT('Ctrl Pts',(-43.5445019199415,-55.8067071952963,
-47.1082833333333));
#262139=CARTESIAN_POINT('Ctrl Pts',(-44.5079524583208,-55.8067071952963,
-47.04995));
#262140=CARTESIAN_POINT('Ctrl Pts',(-45.4714029967,-55.8067071952963,-46.9916166666667));
#262141=CARTESIAN_POINT('Ctrl Pts',(-45.9531282658897,-56.6410798368225,
-46.9332833333334));
#262142=CARTESIAN_POINT('Ctrl Pts',(-46.4348535350793,-57.4754524783487,
-46.87495));
#262143=CARTESIAN_POINT('Ctrl Pts',(-45.9531282658897,-58.309825119875,
-46.8166166666667));
#262144=CARTESIAN_POINT('Ctrl Pts',(-45.4714029967,-59.1441977614012,-46.7582833333333));
#262145=CARTESIAN_POINT('Ctrl Pts',(-44.5079524583208,-59.1441977614012,
-46.69995));
#262146=CARTESIAN_POINT('Ctrl Pts',(-43.5445019199415,-59.1441977614012,
-46.6416166666666));
#262147=CARTESIAN_POINT('Ctrl Pts',(-43.0627766507519,-58.309825119875,
-46.5832833333334));
#262148=CARTESIAN_POINT('Ctrl Pts',(-42.5810513815623,-57.4754524783487,
-46.52495));
#262149=CARTESIAN_POINT('Ctrl Pts',(-43.0627766507519,-56.6410798368225,
-46.4666166666667));
#262150=CARTESIAN_POINT('Ctrl Pts',(-43.5445019199415,-55.8067071952963,
-46.4082833333333));
#262151=CARTESIAN_POINT('Ctrl Pts',(-44.5079524583208,-55.8067071952963,
-46.34995));
#262152=CARTESIAN_POINT('Ctrl Pts',(-45.4714029967,-55.8067071952963,-46.2916166666667));
#262153=CARTESIAN_POINT('Ctrl Pts',(-45.9531282658897,-56.6410798368225,
-46.2332833333334));
#262154=CARTESIAN_POINT('Ctrl Pts',(-46.4348535350793,-57.4754524783487,
-46.17495));
#262155=CARTESIAN_POINT('Ctrl Pts',(-45.9531282658897,-58.309825119875,
-46.1166166666667));
#262156=CARTESIAN_POINT('Ctrl Pts',(-45.4714029967,-59.1441977614012,-46.0582833333333));
#262157=CARTESIAN_POINT('Ctrl Pts',(-44.5079524583208,-59.1441977614012,
-45.99995));
#262158=CARTESIAN_POINT('Ctrl Pts',(-43.5445019199415,-59.1441977614012,
-45.9416166666667));
#262159=CARTESIAN_POINT('Ctrl Pts',(-43.0627766507519,-58.309825119875,
-45.8832833333333));
#262160=CARTESIAN_POINT('Ctrl Pts',(-42.5810513815623,-57.4754524783487,
-45.82495));
#262161=CARTESIAN_POINT('Ctrl Pts',(-43.0627766507519,-56.6410798368225,
-45.7666166666667));
#262162=CARTESIAN_POINT('Ctrl Pts',(-43.5445019199415,-55.8067071952963,
-45.7082833333333));
#262163=CARTESIAN_POINT('Ctrl Pts',(-44.5079524583208,-55.8067071952963,
-45.64995));
#262164=CARTESIAN_POINT('Ctrl Pts',(-45.4714029967,-55.8067071952963,-45.5916166666667));
#262165=CARTESIAN_POINT('Ctrl Pts',(-45.9531282658897,-56.6410798368225,
-45.5332833333333));
#262166=CARTESIAN_POINT('Ctrl Pts',(-46.4348535350793,-57.4754524783487,
-45.47495));
#262167=CARTESIAN_POINT('Ctrl Pts',(-45.9531282658897,-58.309825119875,
-45.4166166666667));
#262168=CARTESIAN_POINT('Ctrl Pts',(-45.4714029967,-59.1441977614012,-45.3582833333333));
#262169=CARTESIAN_POINT('Ctrl Pts',(-44.5079524583208,-59.1441977614012,
-45.29995));
#262170=CARTESIAN_POINT('Ctrl Pts',(-43.5445019199415,-59.1441977614012,
-45.2416166666667));
#262171=CARTESIAN_POINT('Ctrl Pts',(-43.0627766507519,-58.309825119875,
-45.1832833333334));
#262172=CARTESIAN_POINT('Ctrl Pts',(-42.5810513815623,-57.4754524783487,
-45.12495));
#262173=CARTESIAN_POINT('Ctrl Pts',(-43.0627766507519,-56.6410798368225,
-45.0666166666667));
#262174=CARTESIAN_POINT('Ctrl Pts',(-43.5445019199415,-55.8067071952963,
-45.0082833333334));
#262175=CARTESIAN_POINT('Ctrl Pts',(-44.5079524583208,-55.8067071952963,
-44.94995));
#262176=CARTESIAN_POINT('Ctrl Pts',(-45.4714029967,-55.8067071952963,-44.8916166666667));
#262177=CARTESIAN_POINT('Ctrl Pts',(-45.9531282658897,-56.6410798368225,
-44.8332833333334));
#262178=CARTESIAN_POINT('Ctrl Pts',(-46.4348535350793,-57.4754524783487,
-44.77495));
#262179=CARTESIAN_POINT('Ctrl Pts',(-45.9531282658897,-58.309825119875,
-44.7166166666667));
#262180=CARTESIAN_POINT('Ctrl Pts',(-45.4714029967,-59.1441977614012,-44.6582833333334));
#262181=CARTESIAN_POINT('Ctrl Pts',(-44.5079524583208,-59.1441977614012,
-44.59995));
#262182=CARTESIAN_POINT('Ctrl Pts',(-43.5445019199415,-59.1441977614012,
-44.5416166666667));
#262183=CARTESIAN_POINT('Ctrl Pts',(-43.0627766507519,-58.309825119875,
-44.4832833333334));
#262184=CARTESIAN_POINT('Ctrl Pts',(-42.5810513815623,-57.4754524783487,
-44.42495));
#262185=CARTESIAN_POINT('Ctrl Pts',(-43.0627766507519,-56.6410798368225,
-44.3666166666667));
#262186=CARTESIAN_POINT('Ctrl Pts',(-43.5445019199415,-55.8067071952963,
-44.3082833333334));
#262187=CARTESIAN_POINT('Ctrl Pts',(-44.5079524583208,-55.8067071952963,
-44.24995));
#262188=CARTESIAN_POINT('Ctrl Pts',(-45.4714029967,-55.8067071952963,-44.1916166666667));
#262189=CARTESIAN_POINT('Ctrl Pts',(-45.9531282658897,-56.6410798368225,
-44.1332833333334));
#262190=CARTESIAN_POINT('Ctrl Pts',(-46.4348535350793,-57.4754524783487,
-44.07495));
#262191=CARTESIAN_POINT('Ctrl Pts',(-45.9531282658897,-58.309825119875,
-44.0166166666667));
#262192=CARTESIAN_POINT('Ctrl Pts',(-45.4714029967,-59.1441977614012,-43.9582833333334));
#262193=CARTESIAN_POINT('Ctrl Pts',(-44.5079524583208,-59.1441977614012,
-43.89995));
#262194=CARTESIAN_POINT('Ctrl Pts',(-43.5445019199415,-59.1441977614012,
-43.8416166666667));
#262195=CARTESIAN_POINT('Ctrl Pts',(-43.0627766507519,-58.309825119875,
-43.7832833333334));
#262196=CARTESIAN_POINT('Ctrl Pts',(-42.5810513815623,-57.4754524783487,
-43.72495));
#262197=CARTESIAN_POINT('Ctrl Pts',(-43.0627766507519,-56.6410798368225,
-43.6666166666667));
#262198=CARTESIAN_POINT('Ctrl Pts',(-43.5445019199415,-55.8067071952963,
-43.6082833333333));
#262199=CARTESIAN_POINT('Ctrl Pts',(-44.5079524583208,-55.8067071952963,
-43.54995));
#262200=CARTESIAN_POINT('Ctrl Pts',(-45.4714029967,-55.8067071952963,-43.4916166666667));
#262201=CARTESIAN_POINT('Ctrl Pts',(-45.9531282658897,-56.6410798368225,
-43.4332833333333));
#262202=CARTESIAN_POINT('Ctrl Pts',(-46.4348535350793,-57.4754524783487,
-43.37495));
#262203=CARTESIAN_POINT('Ctrl Pts',(-45.9531282658897,-58.309825119875,
-43.3166166666667));
#262204=CARTESIAN_POINT('Ctrl Pts',(-45.4714029967,-59.1441977614012,-43.2582833333333));
#262205=CARTESIAN_POINT('Ctrl Pts',(-44.5079524583208,-59.1441977614012,
-43.19995));
#262206=CARTESIAN_POINT('Ctrl Pts',(-43.5445019199415,-59.1441977614012,
-43.1416166666667));
#262207=CARTESIAN_POINT('Ctrl Pts',(-43.0627766507519,-58.309825119875,
-43.0832833333333));
#262208=CARTESIAN_POINT('Ctrl Pts',(-42.5810513815623,-57.4754524783487,
-43.02495));
#262209=CARTESIAN_POINT('Ctrl Pts',(-43.0627766507519,-56.6410798368225,
-42.9666166666667));
#262210=CARTESIAN_POINT('Ctrl Pts',(-43.5445019199415,-55.8067071952963,
-42.9082833333333));
#262211=CARTESIAN_POINT('Ctrl Pts',(-44.5079524583208,-55.8067071952963,
-42.84995));
#262212=CARTESIAN_POINT('Ctrl Pts',(-45.4714029967,-55.8067071952963,-42.7916166666667));
#262213=CARTESIAN_POINT('Ctrl Pts',(-45.9531282658897,-56.6410798368225,
-42.7332833333334));
#262214=CARTESIAN_POINT('Ctrl Pts',(-46.4348535350793,-57.4754524783487,
-42.67495));
#262215=CARTESIAN_POINT('Ctrl Pts',(-45.9531282658897,-58.309825119875,
-42.6166166666667));
#262216=CARTESIAN_POINT('Ctrl Pts',(-45.4714029967,-59.1441977614012,-42.5582833333333));
#262217=CARTESIAN_POINT('Ctrl Pts',(-44.5079524583208,-59.1441977614012,
-42.49995));
#262218=CARTESIAN_POINT('Ctrl Pts',(-43.5445019199415,-59.1441977614012,
-42.4416166666667));
#262219=CARTESIAN_POINT('Ctrl Pts',(-43.0627766507519,-58.309825119875,
-42.3832833333333));
#262220=CARTESIAN_POINT('Ctrl Pts',(-42.5810513815623,-57.4754524783487,
-42.32495));
#262221=CARTESIAN_POINT('Ctrl Pts',(-43.0627766507519,-56.6410798368225,
-42.2666166666667));
#262222=CARTESIAN_POINT('Ctrl Pts',(-43.5445019199415,-55.8067071952963,
-42.2082833333333));
#262223=CARTESIAN_POINT('Ctrl Pts',(-44.5079524583208,-55.8067071952963,
-42.14995));
#262224=CARTESIAN_POINT('Ctrl Pts',(-45.4714029967,-55.8067071952963,-42.0916166666667));
#262225=CARTESIAN_POINT('Ctrl Pts',(-45.9531282658897,-56.6410798368225,
-42.0332833333334));
#262226=CARTESIAN_POINT('Ctrl Pts',(-46.4348535350793,-57.4754524783487,
-41.97495));
#262227=CARTESIAN_POINT('Ctrl Pts',(-45.9531282658897,-58.309825119875,
-41.9166166666667));
#262228=CARTESIAN_POINT('Ctrl Pts',(-45.4714029967,-59.1441977614012,-41.8582833333333));
#262229=CARTESIAN_POINT('Ctrl Pts',(-44.5079524583208,-59.1441977614012,
-41.79995));
#262230=CARTESIAN_POINT('Ctrl Pts',(-43.5445019199415,-59.1441977614012,
-41.7416166666667));
#262231=CARTESIAN_POINT('Ctrl Pts',(-43.0627766507519,-58.309825119875,
-41.6832833333333));
#262232=CARTESIAN_POINT('Ctrl Pts',(-42.5810513815623,-57.4754524783487,
-41.62495));
#262233=CARTESIAN_POINT('Ctrl Pts',(-43.0627766507519,-56.6410798368225,
-41.5666166666667));
#262234=CARTESIAN_POINT('Ctrl Pts',(-43.5445019199415,-55.8067071952963,
-41.5082833333334));
#262235=CARTESIAN_POINT('Ctrl Pts',(-44.5079524583208,-55.8067071952963,
-41.44995));
#262236=CARTESIAN_POINT('Ctrl Pts',(-45.4714029967,-55.8067071952963,-41.3916166666667));
#262237=CARTESIAN_POINT('Ctrl Pts',(-45.9531282658897,-56.6410798368225,
-41.3332833333334));
#262238=CARTESIAN_POINT('Ctrl Pts',(-46.4348535350793,-57.4754524783487,
-41.27495));
#262239=CARTESIAN_POINT('Ctrl Pts',(-45.9531282658897,-58.309825119875,
-41.2166166666667));
#262240=CARTESIAN_POINT('Ctrl Pts',(-45.4714029967,-59.1441977614012,-41.1582833333333));
#262241=CARTESIAN_POINT('Ctrl Pts',(-44.5079524583208,-59.1441977614012,
-41.09995));
#262242=CARTESIAN_POINT('Ctrl Pts',(-43.5445019199415,-59.1441977614012,
-41.0416166666667));
#262243=CARTESIAN_POINT('Ctrl Pts',(-43.0627766507519,-58.309825119875,
-40.9832833333333));
#262244=CARTESIAN_POINT('Ctrl Pts',(-42.5810513815623,-57.4754524783487,
-40.92495));
#262245=CARTESIAN_POINT('Ctrl Pts',(-43.0627766507519,-56.6410798368225,
-40.8666166666667));
#262246=CARTESIAN_POINT('Ctrl Pts',(-43.5445019199415,-55.8067071952963,
-40.8082833333334));
#262247=CARTESIAN_POINT('Ctrl Pts',(-44.5079524583208,-55.8067071952963,
-40.74995));
#262248=CARTESIAN_POINT('Ctrl Pts',(-45.4714029967,-55.8067071952963,-40.6916166666667));
#262249=CARTESIAN_POINT('Ctrl Pts',(-45.9531282658897,-56.6410798368225,
-40.6332833333334));
#262250=CARTESIAN_POINT('Ctrl Pts',(-46.4348535350793,-57.4754524783487,
-40.57495));
#262251=CARTESIAN_POINT('Ctrl Pts',(-45.9531282658897,-58.309825119875,
-40.5166166666667));
#262252=CARTESIAN_POINT('Ctrl Pts',(-45.4714029967,-59.1441977614012,-40.4582833333333));
#262253=CARTESIAN_POINT('Ctrl Pts',(-44.5079524583208,-59.1441977614012,
-40.39995));
#262254=CARTESIAN_POINT('Ctrl Pts',(-43.5445019199415,-59.1441977614012,
-40.3416166666667));
#262255=CARTESIAN_POINT('Ctrl Pts',(-43.0627766507519,-58.309825119875,
-40.2832833333334));
#262256=CARTESIAN_POINT('Ctrl Pts',(-42.5810513815623,-57.4754524783487,
-40.22495));
#262257=CARTESIAN_POINT('Ctrl Pts',(-43.0627766507519,-56.6410798368225,
-40.1666166666667));
#262258=CARTESIAN_POINT('Ctrl Pts',(-43.5445019199415,-55.8067071952963,
-40.1082833333334));
#262259=CARTESIAN_POINT('Ctrl Pts',(-44.5079524583208,-55.8067071952963,
-40.04995));
#262260=CARTESIAN_POINT('Ctrl Pts',(-45.4714029967,-55.8067071952963,-39.9916166666667));
#262261=CARTESIAN_POINT('Ctrl Pts',(-45.9531282658897,-56.6410798368225,
-39.9332833333333));
#262262=CARTESIAN_POINT('Ctrl Pts',(-46.4348535350793,-57.4754524783487,
-39.87495));
#262263=CARTESIAN_POINT('Ctrl Pts',(-45.9531282658897,-58.309825119875,
-39.8166166666667));
#262264=CARTESIAN_POINT('Ctrl Pts',(-45.4714029967,-59.1441977614012,-39.7582833333334));
#262265=CARTESIAN_POINT('Ctrl Pts',(-44.5079524583208,-59.1441977614012,
-39.69995));
#262266=CARTESIAN_POINT('Ctrl Pts',(-43.5445019199415,-59.1441977614012,
-39.6416166666667));
#262267=CARTESIAN_POINT('Ctrl Pts',(-43.0627766507519,-58.309825119875,
-39.5832833333333));
#262268=CARTESIAN_POINT('Ctrl Pts',(-42.5810513815623,-57.4754524783487,
-39.52495));
#262269=CARTESIAN_POINT('Ctrl Pts',(-43.0627766507519,-56.6410798368225,
-39.4666166666667));
#262270=CARTESIAN_POINT('Ctrl Pts',(-43.5445019199415,-55.8067071952963,
-39.4082833333334));
#262271=CARTESIAN_POINT('Ctrl Pts',(-44.5079524583208,-55.8067071952963,
-39.34995));
#262272=CARTESIAN_POINT('Ctrl Pts',(-45.4714029967,-55.8067071952963,-39.2916166666667));
#262273=CARTESIAN_POINT('Ctrl Pts',(-45.9531282658897,-56.6410798368225,
-39.2332833333333));
#262274=CARTESIAN_POINT('Ctrl Pts',(-46.4348535350793,-57.4754524783487,
-39.17495));
#262275=CARTESIAN_POINT('Ctrl Pts',(-45.9531282658897,-58.309825119875,
-39.1166166666667));
#262276=CARTESIAN_POINT('Ctrl Pts',(-45.4714029967,-59.1441977614012,-39.0582833333334));
#262277=CARTESIAN_POINT('Ctrl Pts',(-44.5079524583208,-59.1441977614012,
-38.99995));
#262278=CARTESIAN_POINT('Ctrl Pts',(-43.5445019199415,-59.1441977614012,
-38.9416166666667));
#262279=CARTESIAN_POINT('Ctrl Pts',(-43.0627766507519,-58.309825119875,
-38.8832833333334));
#262280=CARTESIAN_POINT('Ctrl Pts',(-42.5810513815623,-57.4754524783487,
-38.82495));
#262281=CARTESIAN_POINT('Ctrl Pts',(-43.0627766507519,-56.6410798368225,
-38.7666166666667));
#262282=CARTESIAN_POINT('Ctrl Pts',(-43.5445019199415,-55.8067071952963,
-38.7082833333334));
#262283=CARTESIAN_POINT('Ctrl Pts',(-44.5079524583208,-55.8067071952963,
-38.64995));
#262284=CARTESIAN_POINT('Ctrl Pts',(-45.4714029967,-55.8067071952963,-38.5916166666667));
#262285=CARTESIAN_POINT('Ctrl Pts',(-45.9531282658897,-56.6410798368225,
-38.5332833333334));
#262286=CARTESIAN_POINT('Ctrl Pts',(-46.4348535350793,-57.4754524783487,
-38.47495));
#262287=CARTESIAN_POINT('Ctrl Pts',(-45.9531282658897,-58.309825119875,
-38.4166166666667));
#262288=CARTESIAN_POINT('Ctrl Pts',(-45.4714029967,-59.1441977614012,-38.3582833333333));
#262289=CARTESIAN_POINT('Ctrl Pts',(-44.5079524583208,-59.1441977614012,
-38.29995));
#262290=CARTESIAN_POINT('Ctrl Pts',(-43.5445019199415,-59.1441977614012,
-38.2416166666667));
#262291=CARTESIAN_POINT('Ctrl Pts',(-43.0627766507519,-58.309825119875,
-38.1832833333333));
#262292=CARTESIAN_POINT('Ctrl Pts',(-42.5810513815623,-57.4754524783487,
-38.12495));
#262293=CARTESIAN_POINT('Ctrl Pts',(-43.0627766507519,-56.6410798368225,
-38.0666166666667));
#262294=CARTESIAN_POINT('Ctrl Pts',(-43.5445019199415,-55.8067071952963,
-38.0082833333333));
#262295=CARTESIAN_POINT('Ctrl Pts',(-44.5079524583208,-55.8067071952963,
-37.94995));
#262296=CARTESIAN_POINT('Ctrl Pts',(-45.4714029967,-55.8067071952963,-37.8916166666667));
#262297=CARTESIAN_POINT('Ctrl Pts',(-45.9531282658897,-56.6410798368225,
-37.8332833333334));
#262298=CARTESIAN_POINT('Ctrl Pts',(-46.4348535350793,-57.4754524783487,
-37.77495));
#262299=CARTESIAN_POINT('Ctrl Pts',(-45.9531282658897,-58.309825119875,
-37.7166166666667));
#262300=CARTESIAN_POINT('Ctrl Pts',(-45.4714029967,-59.1441977614012,-37.6582833333333));
#262301=CARTESIAN_POINT('Ctrl Pts',(-44.5079524583208,-59.1441977614012,
-37.59995));
#262302=CARTESIAN_POINT('Ctrl Pts',(-43.5445019199415,-59.1441977614012,
-37.5416166666667));
#262303=CARTESIAN_POINT('Ctrl Pts',(-43.0627766507519,-58.309825119875,
-37.4832833333334));
#262304=CARTESIAN_POINT('Ctrl Pts',(-42.5810513815623,-57.4754524783487,
-37.42495));
#262305=CARTESIAN_POINT('Ctrl Pts',(-43.0627766507519,-56.6410798368225,
-37.3666166666667));
#262306=CARTESIAN_POINT('Ctrl Pts',(-43.5445019199415,-55.8067071952963,
-37.3082833333333));
#262307=CARTESIAN_POINT('Ctrl Pts',(-44.5079524583208,-55.8067071952963,
-37.24995));
#262308=CARTESIAN_POINT('Ctrl Pts',(-45.4714029967,-55.8067071952963,-37.1916166666667));
#262309=CARTESIAN_POINT('Ctrl Pts',(-45.9531282658897,-56.6410798368225,
-37.1332833333334));
#262310=CARTESIAN_POINT('Ctrl Pts',(-46.4348535350793,-57.4754524783487,
-37.07495));
#262311=CARTESIAN_POINT('Ctrl Pts',(-45.9531282658897,-58.309825119875,
-37.0166166666667));
#262312=CARTESIAN_POINT('Ctrl Pts',(-45.8905850977848,-58.418153064699,
-37.0090431559831));
#262313=CARTESIAN_POINT('Ctrl Pts',(-45.8125914103809,-58.5159466035015,
-37.0009024189827));
#262314=CARTESIAN_POINT('Ctrl Pts',(-44.5079524583208,-59.5441932447742,
-53.2308875));
#262315=CARTESIAN_POINT('Ctrl Pts',(-43.3135644199415,-59.5441932447742,
-53.1725541666667));
#262316=CARTESIAN_POINT('Ctrl Pts',(-42.7163704007519,-58.5098228615615,
-53.1142208333334));
#262317=CARTESIAN_POINT('Ctrl Pts',(-42.1191763815623,-57.4754524783487,
-53.0558875000001));
#262318=CARTESIAN_POINT('Ctrl Pts',(-42.7163704007519,-56.4410820951361,
-52.9975541666667));
#262319=CARTESIAN_POINT('Ctrl Pts',(-43.3135644199415,-55.4067117119233,
-52.9392208333334));
#262320=CARTESIAN_POINT('Ctrl Pts',(-44.5079524583208,-55.4067117119234,
-52.8808875));
#262321=CARTESIAN_POINT('Ctrl Pts',(-45.7023404967,-55.4067117119233,-52.8225541666667));
#262322=CARTESIAN_POINT('Ctrl Pts',(-46.2995345158897,-56.4410820951361,
-52.7642208333334));
#262323=CARTESIAN_POINT('Ctrl Pts',(-46.8967285350793,-57.4754524783487,
-52.7058875));
#262324=CARTESIAN_POINT('Ctrl Pts',(-46.2995345158897,-58.5098228615615,
-52.6475541666667));
#262325=CARTESIAN_POINT('Ctrl Pts',(-45.7023404967,-59.5441932447742,-52.5892208333333));
#262326=CARTESIAN_POINT('Ctrl Pts',(-44.5079524583208,-59.5441932447742,
-52.5308875));
#262327=CARTESIAN_POINT('Ctrl Pts',(-43.3135644199415,-59.5441932447742,
-52.4725541666667));
#262328=CARTESIAN_POINT('Ctrl Pts',(-42.7163704007519,-58.5098228615615,
-52.4142208333334));
#262329=CARTESIAN_POINT('Ctrl Pts',(-42.1191763815623,-57.4754524783487,
-52.3558875000001));
#262330=CARTESIAN_POINT('Ctrl Pts',(-42.7163704007519,-56.4410820951361,
-52.2975541666667));
#262331=CARTESIAN_POINT('Ctrl Pts',(-43.3135644199415,-55.4067117119233,
-52.2392208333334));
#262332=CARTESIAN_POINT('Ctrl Pts',(-44.5079524583208,-55.4067117119234,
-52.1808875));
#262333=CARTESIAN_POINT('Ctrl Pts',(-45.7023404967,-55.4067117119233,-52.1225541666667));
#262334=CARTESIAN_POINT('Ctrl Pts',(-46.2995345158897,-56.4410820951361,
-52.0642208333334));
#262335=CARTESIAN_POINT('Ctrl Pts',(-46.8967285350793,-57.4754524783487,
-52.0058875));
#262336=CARTESIAN_POINT('Ctrl Pts',(-46.2995345158897,-58.5098228615615,
-51.9475541666667));
#262337=CARTESIAN_POINT('Ctrl Pts',(-45.7023404967,-59.5441932447742,-51.8892208333334));
#262338=CARTESIAN_POINT('Ctrl Pts',(-44.5079524583208,-59.5441932447742,
-51.8308875));
#262339=CARTESIAN_POINT('Ctrl Pts',(-43.3135644199415,-59.5441932447742,
-51.7725541666667));
#262340=CARTESIAN_POINT('Ctrl Pts',(-42.7163704007519,-58.5098228615615,
-51.7142208333334));
#262341=CARTESIAN_POINT('Ctrl Pts',(-42.1191763815623,-57.4754524783487,
-51.6558875));
#262342=CARTESIAN_POINT('Ctrl Pts',(-42.7163704007519,-56.4410820951361,
-51.5975541666667));
#262343=CARTESIAN_POINT('Ctrl Pts',(-43.3135644199415,-55.4067117119233,
-51.5392208333333));
#262344=CARTESIAN_POINT('Ctrl Pts',(-44.5079524583208,-55.4067117119234,
-51.4808875));
#262345=CARTESIAN_POINT('Ctrl Pts',(-45.7023404967,-55.4067117119233,-51.4225541666667));
#262346=CARTESIAN_POINT('Ctrl Pts',(-46.2995345158897,-56.4410820951361,
-51.3642208333334));
#262347=CARTESIAN_POINT('Ctrl Pts',(-46.8967285350793,-57.4754524783487,
-51.3058875));
#262348=CARTESIAN_POINT('Ctrl Pts',(-46.2995345158897,-58.5098228615615,
-51.2475541666667));
#262349=CARTESIAN_POINT('Ctrl Pts',(-45.7023404967,-59.5441932447742,-51.1892208333334));
#262350=CARTESIAN_POINT('Ctrl Pts',(-44.5079524583208,-59.5441932447742,
-51.1308875));
#262351=CARTESIAN_POINT('Ctrl Pts',(-43.3135644199415,-59.5441932447742,
-51.0725541666667));
#262352=CARTESIAN_POINT('Ctrl Pts',(-42.7163704007519,-58.5098228615615,
-51.0142208333334));
#262353=CARTESIAN_POINT('Ctrl Pts',(-42.1191763815623,-57.4754524783487,
-50.9558875));
#262354=CARTESIAN_POINT('Ctrl Pts',(-42.7163704007519,-56.4410820951361,
-50.8975541666667));
#262355=CARTESIAN_POINT('Ctrl Pts',(-43.3135644199415,-55.4067117119233,
-50.8392208333333));
#262356=CARTESIAN_POINT('Ctrl Pts',(-44.5079524583208,-55.4067117119234,
-50.7808875));
#262357=CARTESIAN_POINT('Ctrl Pts',(-45.7023404967,-55.4067117119233,-50.7225541666667));
#262358=CARTESIAN_POINT('Ctrl Pts',(-46.2995345158897,-56.4410820951361,
-50.6642208333333));
#262359=CARTESIAN_POINT('Ctrl Pts',(-46.8967285350793,-57.4754524783487,
-50.6058875));
#262360=CARTESIAN_POINT('Ctrl Pts',(-46.2995345158897,-58.5098228615615,
-50.5475541666667));
#262361=CARTESIAN_POINT('Ctrl Pts',(-45.7023404967,-59.5441932447742,-50.4892208333333));
#262362=CARTESIAN_POINT('Ctrl Pts',(-44.5079524583208,-59.5441932447742,
-50.4308875));
#262363=CARTESIAN_POINT('Ctrl Pts',(-43.3135644199415,-59.5441932447742,
-50.3725541666667));
#262364=CARTESIAN_POINT('Ctrl Pts',(-42.7163704007519,-58.5098228615615,
-50.3142208333334));
#262365=CARTESIAN_POINT('Ctrl Pts',(-42.1191763815623,-57.4754524783487,
-50.2558875));
#262366=CARTESIAN_POINT('Ctrl Pts',(-42.7163704007519,-56.4410820951361,
-50.1975541666667));
#262367=CARTESIAN_POINT('Ctrl Pts',(-43.3135644199415,-55.4067117119233,
-50.1392208333333));
#262368=CARTESIAN_POINT('Ctrl Pts',(-44.5079524583208,-55.4067117119234,
-50.0808875));
#262369=CARTESIAN_POINT('Ctrl Pts',(-45.7023404967,-55.4067117119233,-50.0225541666667));
#262370=CARTESIAN_POINT('Ctrl Pts',(-46.2995345158897,-56.4410820951361,
-49.9642208333334));
#262371=CARTESIAN_POINT('Ctrl Pts',(-46.8967285350793,-57.4754524783487,
-49.9058875));
#262372=CARTESIAN_POINT('Ctrl Pts',(-46.2995345158897,-58.5098228615615,
-49.8475541666667));
#262373=CARTESIAN_POINT('Ctrl Pts',(-45.7023404967,-59.5441932447742,-49.7892208333333));
#262374=CARTESIAN_POINT('Ctrl Pts',(-44.5079524583208,-59.5441932447742,
-49.7308875));
#262375=CARTESIAN_POINT('Ctrl Pts',(-43.3135644199415,-59.5441932447742,
-49.6725541666667));
#262376=CARTESIAN_POINT('Ctrl Pts',(-42.7163704007519,-58.5098228615615,
-49.6142208333334));
#262377=CARTESIAN_POINT('Ctrl Pts',(-42.1191763815623,-57.4754524783487,
-49.5558875));
#262378=CARTESIAN_POINT('Ctrl Pts',(-42.7163704007519,-56.4410820951361,
-49.4975541666667));
#262379=CARTESIAN_POINT('Ctrl Pts',(-43.3135644199415,-55.4067117119233,
-49.4392208333333));
#262380=CARTESIAN_POINT('Ctrl Pts',(-44.5079524583208,-55.4067117119234,
-49.3808875));
#262381=CARTESIAN_POINT('Ctrl Pts',(-45.7023404967,-55.4067117119233,-49.3225541666667));
#262382=CARTESIAN_POINT('Ctrl Pts',(-46.2995345158897,-56.4410820951361,
-49.2642208333334));
#262383=CARTESIAN_POINT('Ctrl Pts',(-46.8967285350793,-57.4754524783487,
-49.2058875));
#262384=CARTESIAN_POINT('Ctrl Pts',(-46.2995345158897,-58.5098228615615,
-49.1475541666667));
#262385=CARTESIAN_POINT('Ctrl Pts',(-45.7023404967,-59.5441932447742,-49.0892208333333));
#262386=CARTESIAN_POINT('Ctrl Pts',(-44.5079524583208,-59.5441932447742,
-49.0308875));
#262387=CARTESIAN_POINT('Ctrl Pts',(-43.3135644199415,-59.5441932447742,
-48.9725541666667));
#262388=CARTESIAN_POINT('Ctrl Pts',(-42.7163704007519,-58.5098228615615,
-48.9142208333334));
#262389=CARTESIAN_POINT('Ctrl Pts',(-42.1191763815623,-57.4754524783487,
-48.8558875));
#262390=CARTESIAN_POINT('Ctrl Pts',(-42.7163704007519,-56.4410820951361,
-48.7975541666667));
#262391=CARTESIAN_POINT('Ctrl Pts',(-43.3135644199415,-55.4067117119233,
-48.7392208333334));
#262392=CARTESIAN_POINT('Ctrl Pts',(-44.5079524583208,-55.4067117119234,
-48.6808875));
#262393=CARTESIAN_POINT('Ctrl Pts',(-45.7023404967,-55.4067117119233,-48.6225541666667));
#262394=CARTESIAN_POINT('Ctrl Pts',(-46.2995345158897,-56.4410820951361,
-48.5642208333334));
#262395=CARTESIAN_POINT('Ctrl Pts',(-46.8967285350793,-57.4754524783487,
-48.5058875));
#262396=CARTESIAN_POINT('Ctrl Pts',(-46.2995345158897,-58.5098228615615,
-48.4475541666667));
#262397=CARTESIAN_POINT('Ctrl Pts',(-45.7023404967,-59.5441932447742,-48.3892208333334));
#262398=CARTESIAN_POINT('Ctrl Pts',(-44.5079524583208,-59.5441932447742,
-48.3308875));
#262399=CARTESIAN_POINT('Ctrl Pts',(-43.3135644199415,-59.5441932447742,
-48.2725541666667));
#262400=CARTESIAN_POINT('Ctrl Pts',(-42.7163704007519,-58.5098228615615,
-48.2142208333334));
#262401=CARTESIAN_POINT('Ctrl Pts',(-42.1191763815623,-57.4754524783487,
-48.1558875));
#262402=CARTESIAN_POINT('Ctrl Pts',(-42.7163704007519,-56.4410820951361,
-48.0975541666667));
#262403=CARTESIAN_POINT('Ctrl Pts',(-43.3135644199415,-55.4067117119233,
-48.0392208333334));
#262404=CARTESIAN_POINT('Ctrl Pts',(-44.5079524583208,-55.4067117119234,
-47.9808875));
#262405=CARTESIAN_POINT('Ctrl Pts',(-45.7023404967,-55.4067117119233,-47.9225541666667));
#262406=CARTESIAN_POINT('Ctrl Pts',(-46.2995345158897,-56.4410820951361,
-47.8642208333334));
#262407=CARTESIAN_POINT('Ctrl Pts',(-46.8967285350793,-57.4754524783487,
-47.8058875000001));
#262408=CARTESIAN_POINT('Ctrl Pts',(-46.2995345158897,-58.5098228615615,
-47.7475541666667));
#262409=CARTESIAN_POINT('Ctrl Pts',(-45.7023404967,-59.5441932447742,-47.6892208333334));
#262410=CARTESIAN_POINT('Ctrl Pts',(-44.5079524583208,-59.5441932447742,
-47.6308875));
#262411=CARTESIAN_POINT('Ctrl Pts',(-43.3135644199415,-59.5441932447742,
-47.5725541666667));
#262412=CARTESIAN_POINT('Ctrl Pts',(-42.7163704007519,-58.5098228615615,
-47.5142208333333));
#262413=CARTESIAN_POINT('Ctrl Pts',(-42.1191763815623,-57.4754524783487,
-47.4558875));
#262414=CARTESIAN_POINT('Ctrl Pts',(-42.7163704007519,-56.4410820951361,
-47.3975541666667));
#262415=CARTESIAN_POINT('Ctrl Pts',(-43.3135644199415,-55.4067117119233,
-47.3392208333334));
#262416=CARTESIAN_POINT('Ctrl Pts',(-44.5079524583208,-55.4067117119234,
-47.2808875));
#262417=CARTESIAN_POINT('Ctrl Pts',(-45.7023404967,-55.4067117119233,-47.2225541666667));
#262418=CARTESIAN_POINT('Ctrl Pts',(-46.2995345158897,-56.4410820951361,
-47.1642208333334));
#262419=CARTESIAN_POINT('Ctrl Pts',(-46.8967285350793,-57.4754524783487,
-47.1058875));
#262420=CARTESIAN_POINT('Ctrl Pts',(-46.2995345158897,-58.5098228615615,
-47.0475541666667));
#262421=CARTESIAN_POINT('Ctrl Pts',(-45.7023404967,-59.5441932447742,-46.9892208333334));
#262422=CARTESIAN_POINT('Ctrl Pts',(-44.5079524583208,-59.5441932447742,
-46.9308875));
#262423=CARTESIAN_POINT('Ctrl Pts',(-43.3135644199415,-59.5441932447742,
-46.8725541666667));
#262424=CARTESIAN_POINT('Ctrl Pts',(-42.7163704007519,-58.5098228615615,
-46.8142208333334));
#262425=CARTESIAN_POINT('Ctrl Pts',(-42.1191763815623,-57.4754524783487,
-46.7558875));
#262426=CARTESIAN_POINT('Ctrl Pts',(-42.7163704007519,-56.4410820951361,
-46.6975541666667));
#262427=CARTESIAN_POINT('Ctrl Pts',(-43.3135644199415,-55.4067117119233,
-46.6392208333334));
#262428=CARTESIAN_POINT('Ctrl Pts',(-44.5079524583208,-55.4067117119234,
-46.5808875));
#262429=CARTESIAN_POINT('Ctrl Pts',(-45.7023404967,-55.4067117119233,-46.5225541666667));
#262430=CARTESIAN_POINT('Ctrl Pts',(-46.2995345158897,-56.4410820951361,
-46.4642208333334));
#262431=CARTESIAN_POINT('Ctrl Pts',(-46.8967285350793,-57.4754524783487,
-46.4058875));
#262432=CARTESIAN_POINT('Ctrl Pts',(-46.2995345158897,-58.5098228615615,
-46.3475541666667));
#262433=CARTESIAN_POINT('Ctrl Pts',(-45.7023404967,-59.5441932447742,-46.2892208333334));
#262434=CARTESIAN_POINT('Ctrl Pts',(-44.5079524583208,-59.5441932447742,
-46.2308875));
#262435=CARTESIAN_POINT('Ctrl Pts',(-43.3135644199415,-59.5441932447742,
-46.1725541666667));
#262436=CARTESIAN_POINT('Ctrl Pts',(-42.7163704007519,-58.5098228615615,
-46.1142208333334));
#262437=CARTESIAN_POINT('Ctrl Pts',(-42.1191763815623,-57.4754524783487,
-46.0558875));
#262438=CARTESIAN_POINT('Ctrl Pts',(-42.7163704007519,-56.4410820951361,
-45.9975541666667));
#262439=CARTESIAN_POINT('Ctrl Pts',(-43.3135644199415,-55.4067117119233,
-45.9392208333333));
#262440=CARTESIAN_POINT('Ctrl Pts',(-44.5079524583208,-55.4067117119234,
-45.8808875));
#262441=CARTESIAN_POINT('Ctrl Pts',(-45.7023404967,-55.4067117119233,-45.8225541666667));
#262442=CARTESIAN_POINT('Ctrl Pts',(-46.2995345158897,-56.4410820951361,
-45.7642208333334));
#262443=CARTESIAN_POINT('Ctrl Pts',(-46.8967285350793,-57.4754524783487,
-45.7058875));
#262444=CARTESIAN_POINT('Ctrl Pts',(-46.2995345158897,-58.5098228615615,
-45.6475541666667));
#262445=CARTESIAN_POINT('Ctrl Pts',(-45.7023404967,-59.5441932447742,-45.5892208333334));
#262446=CARTESIAN_POINT('Ctrl Pts',(-44.5079524583208,-59.5441932447742,
-45.5308875));
#262447=CARTESIAN_POINT('Ctrl Pts',(-43.3135644199415,-59.5441932447742,
-45.4725541666667));
#262448=CARTESIAN_POINT('Ctrl Pts',(-42.7163704007519,-58.5098228615615,
-45.4142208333334));
#262449=CARTESIAN_POINT('Ctrl Pts',(-42.1191763815623,-57.4754524783487,
-45.3558875));
#262450=CARTESIAN_POINT('Ctrl Pts',(-42.7163704007519,-56.4410820951361,
-45.2975541666667));
#262451=CARTESIAN_POINT('Ctrl Pts',(-43.3135644199415,-55.4067117119233,
-45.2392208333333));
#262452=CARTESIAN_POINT('Ctrl Pts',(-44.5079524583208,-55.4067117119234,
-45.1808875));
#262453=CARTESIAN_POINT('Ctrl Pts',(-45.7023404967,-55.4067117119233,-45.1225541666667));
#262454=CARTESIAN_POINT('Ctrl Pts',(-46.2995345158897,-56.4410820951361,
-45.0642208333334));
#262455=CARTESIAN_POINT('Ctrl Pts',(-46.8967285350793,-57.4754524783487,
-45.0058875));
#262456=CARTESIAN_POINT('Ctrl Pts',(-46.2995345158897,-58.5098228615615,
-44.9475541666667));
#262457=CARTESIAN_POINT('Ctrl Pts',(-45.7023404967,-59.5441932447742,-44.8892208333333));
#262458=CARTESIAN_POINT('Ctrl Pts',(-44.5079524583208,-59.5441932447742,
-44.8308875));
#262459=CARTESIAN_POINT('Ctrl Pts',(-43.3135644199415,-59.5441932447742,
-44.7725541666667));
#262460=CARTESIAN_POINT('Ctrl Pts',(-42.7163704007519,-58.5098228615615,
-44.7142208333334));
#262461=CARTESIAN_POINT('Ctrl Pts',(-42.1191763815623,-57.4754524783487,
-44.6558875));
#262462=CARTESIAN_POINT('Ctrl Pts',(-42.7163704007519,-56.4410820951361,
-44.5975541666667));
#262463=CARTESIAN_POINT('Ctrl Pts',(-43.3135644199415,-55.4067117119233,
-44.5392208333333));
#262464=CARTESIAN_POINT('Ctrl Pts',(-44.5079524583208,-55.4067117119234,
-44.4808875000001));
#262465=CARTESIAN_POINT('Ctrl Pts',(-45.7023404967,-55.4067117119233,-44.4225541666667));
#262466=CARTESIAN_POINT('Ctrl Pts',(-46.2995345158897,-56.4410820951361,
-44.3642208333333));
#262467=CARTESIAN_POINT('Ctrl Pts',(-46.8967285350793,-57.4754524783487,
-44.3058875));
#262468=CARTESIAN_POINT('Ctrl Pts',(-46.2995345158897,-58.5098228615615,
-44.2475541666667));
#262469=CARTESIAN_POINT('Ctrl Pts',(-45.7023404967,-59.5441932447742,-44.1892208333334));
#262470=CARTESIAN_POINT('Ctrl Pts',(-44.5079524583208,-59.5441932447742,
-44.1308875000001));
#262471=CARTESIAN_POINT('Ctrl Pts',(-43.3135644199415,-59.5441932447742,
-44.0725541666667));
#262472=CARTESIAN_POINT('Ctrl Pts',(-42.7163704007519,-58.5098228615615,
-44.0142208333334));
#262473=CARTESIAN_POINT('Ctrl Pts',(-42.1191763815623,-57.4754524783487,
-43.9558875));
#262474=CARTESIAN_POINT('Ctrl Pts',(-42.7163704007519,-56.4410820951361,
-43.8975541666667));
#262475=CARTESIAN_POINT('Ctrl Pts',(-43.3135644199415,-55.4067117119233,
-43.8392208333333));
#262476=CARTESIAN_POINT('Ctrl Pts',(-44.5079524583208,-55.4067117119234,
-43.7808875));
#262477=CARTESIAN_POINT('Ctrl Pts',(-45.7023404967,-55.4067117119233,-43.7225541666667));
#262478=CARTESIAN_POINT('Ctrl Pts',(-46.2995345158897,-56.4410820951361,
-43.6642208333334));
#262479=CARTESIAN_POINT('Ctrl Pts',(-46.8967285350793,-57.4754524783487,
-43.6058875));
#262480=CARTESIAN_POINT('Ctrl Pts',(-46.2995345158897,-58.5098228615615,
-43.5475541666667));
#262481=CARTESIAN_POINT('Ctrl Pts',(-45.7023404967,-59.5441932447742,-43.4892208333333));
#262482=CARTESIAN_POINT('Ctrl Pts',(-44.5079524583208,-59.5441932447742,
-43.4308875));
#262483=CARTESIAN_POINT('Ctrl Pts',(-43.3135644199415,-59.5441932447742,
-43.3725541666667));
#262484=CARTESIAN_POINT('Ctrl Pts',(-42.7163704007519,-58.5098228615615,
-43.3142208333334));
#262485=CARTESIAN_POINT('Ctrl Pts',(-42.1191763815623,-57.4754524783487,
-43.2558875));
#262486=CARTESIAN_POINT('Ctrl Pts',(-42.7163704007519,-56.4410820951361,
-43.1975541666667));
#262487=CARTESIAN_POINT('Ctrl Pts',(-43.3135644199415,-55.4067117119233,
-43.1392208333334));
#262488=CARTESIAN_POINT('Ctrl Pts',(-44.5079524583208,-55.4067117119234,
-43.0808875));
#262489=CARTESIAN_POINT('Ctrl Pts',(-45.7023404967,-55.4067117119233,-43.0225541666667));
#262490=CARTESIAN_POINT('Ctrl Pts',(-46.2995345158897,-56.4410820951361,
-42.9642208333334));
#262491=CARTESIAN_POINT('Ctrl Pts',(-46.8967285350793,-57.4754524783487,
-42.9058875));
#262492=CARTESIAN_POINT('Ctrl Pts',(-46.2995345158897,-58.5098228615615,
-42.8475541666667));
#262493=CARTESIAN_POINT('Ctrl Pts',(-45.7023404967,-59.5441932447742,-42.7892208333334));
#262494=CARTESIAN_POINT('Ctrl Pts',(-44.5079524583208,-59.5441932447742,
-42.7308875000001));
#262495=CARTESIAN_POINT('Ctrl Pts',(-43.3135644199415,-59.5441932447742,
-42.6725541666667));
#262496=CARTESIAN_POINT('Ctrl Pts',(-42.7163704007519,-58.5098228615615,
-42.6142208333334));
#262497=CARTESIAN_POINT('Ctrl Pts',(-42.1191763815623,-57.4754524783487,
-42.5558875));
#262498=CARTESIAN_POINT('Ctrl Pts',(-42.7163704007519,-56.4410820951361,
-42.4975541666667));
#262499=CARTESIAN_POINT('Ctrl Pts',(-43.3135644199415,-55.4067117119233,
-42.4392208333334));
#262500=CARTESIAN_POINT('Ctrl Pts',(-44.5079524583208,-55.4067117119234,
-42.3808875000001));
#262501=CARTESIAN_POINT('Ctrl Pts',(-45.7023404967,-55.4067117119233,-42.3225541666667));
#262502=CARTESIAN_POINT('Ctrl Pts',(-46.2995345158897,-56.4410820951361,
-42.2642208333334));
#262503=CARTESIAN_POINT('Ctrl Pts',(-46.8967285350793,-57.4754524783487,
-42.2058875));
#262504=CARTESIAN_POINT('Ctrl Pts',(-46.2995345158897,-58.5098228615615,
-42.1475541666667));
#262505=CARTESIAN_POINT('Ctrl Pts',(-45.7023404967,-59.5441932447742,-42.0892208333334));
#262506=CARTESIAN_POINT('Ctrl Pts',(-44.5079524583208,-59.5441932447742,
-42.0308875000001));
#262507=CARTESIAN_POINT('Ctrl Pts',(-43.3135644199415,-59.5441932447742,
-41.9725541666667));
#262508=CARTESIAN_POINT('Ctrl Pts',(-42.7163704007519,-58.5098228615615,
-41.9142208333334));
#262509=CARTESIAN_POINT('Ctrl Pts',(-42.1191763815623,-57.4754524783487,
-41.8558875));
#262510=CARTESIAN_POINT('Ctrl Pts',(-42.7163704007519,-56.4410820951361,
-41.7975541666667));
#262511=CARTESIAN_POINT('Ctrl Pts',(-43.3135644199415,-55.4067117119233,
-41.7392208333334));
#262512=CARTESIAN_POINT('Ctrl Pts',(-44.5079524583208,-55.4067117119234,
-41.6808875000001));
#262513=CARTESIAN_POINT('Ctrl Pts',(-45.7023404967,-55.4067117119233,-41.6225541666667));
#262514=CARTESIAN_POINT('Ctrl Pts',(-46.2995345158897,-56.4410820951361,
-41.5642208333334));
#262515=CARTESIAN_POINT('Ctrl Pts',(-46.8967285350793,-57.4754524783487,
-41.5058875));
#262516=CARTESIAN_POINT('Ctrl Pts',(-46.2995345158897,-58.5098228615615,
-41.4475541666667));
#262517=CARTESIAN_POINT('Ctrl Pts',(-45.7023404967,-59.5441932447742,-41.3892208333334));
#262518=CARTESIAN_POINT('Ctrl Pts',(-44.5079524583208,-59.5441932447742,
-41.3308875000001));
#262519=CARTESIAN_POINT('Ctrl Pts',(-43.3135644199415,-59.5441932447742,
-41.2725541666667));
#262520=CARTESIAN_POINT('Ctrl Pts',(-42.7163704007519,-58.5098228615615,
-41.2142208333333));
#262521=CARTESIAN_POINT('Ctrl Pts',(-42.1191763815623,-57.4754524783487,
-41.1558875));
#262522=CARTESIAN_POINT('Ctrl Pts',(-42.7163704007519,-56.4410820951361,
-41.0975541666667));
#262523=CARTESIAN_POINT('Ctrl Pts',(-43.3135644199415,-55.4067117119233,
-41.0392208333333));
#262524=CARTESIAN_POINT('Ctrl Pts',(-44.5079524583208,-55.4067117119234,
-40.9808875000001));
#262525=CARTESIAN_POINT('Ctrl Pts',(-45.7023404967,-55.4067117119233,-40.9225541666667));
#262526=CARTESIAN_POINT('Ctrl Pts',(-46.2995345158897,-56.4410820951361,
-40.8642208333334));
#262527=CARTESIAN_POINT('Ctrl Pts',(-46.8967285350793,-57.4754524783487,
-40.8058875));
#262528=CARTESIAN_POINT('Ctrl Pts',(-46.2995345158897,-58.5098228615615,
-40.7475541666667));
#262529=CARTESIAN_POINT('Ctrl Pts',(-45.7023404967,-59.5441932447742,-40.6892208333333));
#262530=CARTESIAN_POINT('Ctrl Pts',(-44.5079524583208,-59.5441932447742,
-40.6308875));
#262531=CARTESIAN_POINT('Ctrl Pts',(-43.3135644199415,-59.5441932447742,
-40.5725541666667));
#262532=CARTESIAN_POINT('Ctrl Pts',(-42.7163704007519,-58.5098228615615,
-40.5142208333333));
#262533=CARTESIAN_POINT('Ctrl Pts',(-42.1191763815623,-57.4754524783487,
-40.4558875));
#262534=CARTESIAN_POINT('Ctrl Pts',(-42.7163704007519,-56.4410820951361,
-40.3975541666667));
#262535=CARTESIAN_POINT('Ctrl Pts',(-43.3135644199415,-55.4067117119233,
-40.3392208333333));
#262536=CARTESIAN_POINT('Ctrl Pts',(-44.5079524583208,-55.4067117119234,
-40.2808875));
#262537=CARTESIAN_POINT('Ctrl Pts',(-45.7023404967,-55.4067117119233,-40.2225541666667));
#262538=CARTESIAN_POINT('Ctrl Pts',(-46.2995345158897,-56.4410820951361,
-40.1642208333333));
#262539=CARTESIAN_POINT('Ctrl Pts',(-46.8967285350793,-57.4754524783487,
-40.1058875));
#262540=CARTESIAN_POINT('Ctrl Pts',(-46.2995345158897,-58.5098228615615,
-40.0475541666667));
#262541=CARTESIAN_POINT('Ctrl Pts',(-45.7023404967,-59.5441932447742,-39.9892208333333));
#262542=CARTESIAN_POINT('Ctrl Pts',(-44.5079524583208,-59.5441932447742,
-39.9308875));
#262543=CARTESIAN_POINT('Ctrl Pts',(-43.3135644199415,-59.5441932447742,
-39.8725541666667));
#262544=CARTESIAN_POINT('Ctrl Pts',(-42.7163704007519,-58.5098228615615,
-39.8142208333334));
#262545=CARTESIAN_POINT('Ctrl Pts',(-42.1191763815623,-57.4754524783487,
-39.7558875));
#262546=CARTESIAN_POINT('Ctrl Pts',(-42.7163704007519,-56.4410820951361,
-39.6975541666667));
#262547=CARTESIAN_POINT('Ctrl Pts',(-43.3135644199415,-55.4067117119233,
-39.6392208333334));
#262548=CARTESIAN_POINT('Ctrl Pts',(-44.5079524583208,-55.4067117119234,
-39.5808875000001));
#262549=CARTESIAN_POINT('Ctrl Pts',(-45.7023404967,-55.4067117119233,-39.5225541666667));
#262550=CARTESIAN_POINT('Ctrl Pts',(-46.2995345158897,-56.4410820951361,
-39.4642208333333));
#262551=CARTESIAN_POINT('Ctrl Pts',(-46.8967285350793,-57.4754524783487,
-39.4058875));
#262552=CARTESIAN_POINT('Ctrl Pts',(-46.2995345158897,-58.5098228615615,
-39.3475541666667));
#262553=CARTESIAN_POINT('Ctrl Pts',(-45.7023404967,-59.5441932447742,-39.2892208333334));
#262554=CARTESIAN_POINT('Ctrl Pts',(-44.5079524583208,-59.5441932447742,
-39.2308875));
#262555=CARTESIAN_POINT('Ctrl Pts',(-43.3135644199415,-59.5441932447742,
-39.1725541666667));
#262556=CARTESIAN_POINT('Ctrl Pts',(-42.7163704007519,-58.5098228615615,
-39.1142208333333));
#262557=CARTESIAN_POINT('Ctrl Pts',(-42.1191763815623,-57.4754524783487,
-39.0558875));
#262558=CARTESIAN_POINT('Ctrl Pts',(-42.7163704007519,-56.4410820951361,
-38.9975541666667));
#262559=CARTESIAN_POINT('Ctrl Pts',(-43.3135644199415,-55.4067117119233,
-38.9392208333334));
#262560=CARTESIAN_POINT('Ctrl Pts',(-44.5079524583208,-55.4067117119234,
-38.8808875));
#262561=CARTESIAN_POINT('Ctrl Pts',(-45.7023404967,-55.4067117119233,-38.8225541666667));
#262562=CARTESIAN_POINT('Ctrl Pts',(-46.2995345158897,-56.4410820951361,
-38.7642208333333));
#262563=CARTESIAN_POINT('Ctrl Pts',(-46.8967285350793,-57.4754524783487,
-38.7058875));
#262564=CARTESIAN_POINT('Ctrl Pts',(-46.2995345158897,-58.5098228615615,
-38.6475541666667));
#262565=CARTESIAN_POINT('Ctrl Pts',(-45.7023404967,-59.5441932447742,-38.5892208333334));
#262566=CARTESIAN_POINT('Ctrl Pts',(-44.5079524583208,-59.5441932447742,
-38.5308875));
#262567=CARTESIAN_POINT('Ctrl Pts',(-43.3135644199415,-59.5441932447742,
-38.4725541666667));
#262568=CARTESIAN_POINT('Ctrl Pts',(-42.7163704007519,-58.5098228615615,
-38.4142208333334));
#262569=CARTESIAN_POINT('Ctrl Pts',(-42.1191763815623,-57.4754524783487,
-38.3558875));
#262570=CARTESIAN_POINT('Ctrl Pts',(-42.7163704007519,-56.4410820951361,
-38.2975541666667));
#262571=CARTESIAN_POINT('Ctrl Pts',(-43.3135644199415,-55.4067117119233,
-38.2392208333333));
#262572=CARTESIAN_POINT('Ctrl Pts',(-44.5079524583208,-55.4067117119234,
-38.1808875000001));
#262573=CARTESIAN_POINT('Ctrl Pts',(-45.7023404967,-55.4067117119233,-38.1225541666667));
#262574=CARTESIAN_POINT('Ctrl Pts',(-46.2995345158897,-56.4410820951361,
-38.0642208333334));
#262575=CARTESIAN_POINT('Ctrl Pts',(-46.8967285350793,-57.4754524783487,
-38.0058875));
#262576=CARTESIAN_POINT('Ctrl Pts',(-46.2995345158897,-58.5098228615615,
-37.9475541666667));
#262577=CARTESIAN_POINT('Ctrl Pts',(-45.7023404967,-59.5441932447742,-37.8892208333334));
#262578=CARTESIAN_POINT('Ctrl Pts',(-44.5079524583208,-59.5441932447742,
-37.8308875));
#262579=CARTESIAN_POINT('Ctrl Pts',(-43.3135644199415,-59.5441932447742,
-37.7725541666667));
#262580=CARTESIAN_POINT('Ctrl Pts',(-42.7163704007519,-58.5098228615615,
-37.7142208333333));
#262581=CARTESIAN_POINT('Ctrl Pts',(-42.1191763815623,-57.4754524783487,
-37.6558875));
#262582=CARTESIAN_POINT('Ctrl Pts',(-42.7163704007519,-56.4410820951361,
-37.5975541666667));
#262583=CARTESIAN_POINT('Ctrl Pts',(-43.3135644199415,-55.4067117119233,
-37.5392208333334));
#262584=CARTESIAN_POINT('Ctrl Pts',(-44.5079524583208,-55.4067117119234,
-37.4808875));
#262585=CARTESIAN_POINT('Ctrl Pts',(-45.7023404967,-55.4067117119233,-37.4225541666667));
#262586=CARTESIAN_POINT('Ctrl Pts',(-46.2995345158897,-56.4410820951361,
-37.3642208333333));
#262587=CARTESIAN_POINT('Ctrl Pts',(-46.8967285350793,-57.4754524783487,
-37.3058875));
#262588=CARTESIAN_POINT('Ctrl Pts',(-46.2995345158897,-58.5098228615615,
-37.2475541666667));
#262589=CARTESIAN_POINT('Ctrl Pts',(-46.2219998538691,-58.6441168355289,
-37.239980655983));
#262590=CARTESIAN_POINT('Ctrl Pts',(-46.1253112086366,-58.7653513237809,
-37.2318399189827));
#262591=CARTESIAN_POINT('Ctrl Pts',(-44.5079524583208,-55.8067071952963,
-52.64995));
#262592=CARTESIAN_POINT('Ctrl Pts',(-44.6656844499352,-55.7901659658991,
-52.64995));
#262593=CARTESIAN_POINT('Ctrl Pts',(-44.8248930522219,-55.7949712964571,
-52.64995));
#262594=CARTESIAN_POINT('Ctrl Pts',(-45.1318235221455,-55.8461574375238,
-52.64995));
#262595=CARTESIAN_POINT('Ctrl Pts',(-45.2783921862421,-55.8907287079161,
-52.64995));
#262596=CARTESIAN_POINT('Ctrl Pts',(-45.613660160206,-56.0425368373591,
-52.64995));
#262597=CARTESIAN_POINT('Ctrl Pts',(-45.7919027673255,-56.1667049718845,
-52.64995));
#262598=CARTESIAN_POINT('Ctrl Pts',(-46.1429583138082,-56.5217933658313,
-52.64995));
#262599=CARTESIAN_POINT('Ctrl Pts',(-46.2637964187606,-56.7417269487201,
-52.64995));
#262600=CARTESIAN_POINT('Ctrl Pts',(-46.392133099223,-57.0470088534789,
-52.64995));
#262601=CARTESIAN_POINT('Ctrl Pts',(-46.4329712831928,-57.1844772022895,
-52.64995));
#262602=CARTESIAN_POINT('Ctrl Pts',(-46.4841685595404,-57.4666010630848,
-52.64995));
#262603=CARTESIAN_POINT('Ctrl Pts',(-46.4942078616446,-57.6104009645534,
-52.64995));
#262604=CARTESIAN_POINT('Ctrl Pts',(-46.4884569292041,-57.7540239068882,
-52.64995));
#262605=CARTESIAN_POINT('Origin',(44.5079524583206,-57.475452478349,235.35105));
#262606=CARTESIAN_POINT('',(45.1065281918136,-55.5671267379762,-39.2098669225693));
#262607=CARTESIAN_POINT('Ctrl Pts',(44.1169605019967,-55.5140434720247,
-38.9933921946761));
#262608=CARTESIAN_POINT('Ctrl Pts',(44.2022887299052,-55.4970339392592,
-39.0076769808271));
#262609=CARTESIAN_POINT('Ctrl Pts',(44.2884091944078,-55.4856555995933,
-39.023286029138));
#262610=CARTESIAN_POINT('Ctrl Pts',(44.4991063316471,-55.4715934716373,
-39.0642737523148));
#262611=CARTESIAN_POINT('Ctrl Pts',(44.6234934076874,-55.4749641540851,
-39.0908460389324));
#262612=CARTESIAN_POINT('Ctrl Pts',(44.8688808688308,-55.504420058799,-39.1478511670598));
#262613=CARTESIAN_POINT('Ctrl Pts',(44.9894084334508,-55.5303903344848,
-39.1781481007446));
#262614=CARTESIAN_POINT('Ctrl Pts',(45.106528182368,-55.567126745519,-39.2098669533806));
#262615=CARTESIAN_POINT('',(42.5264426591671,-57.204124658128,-39.0141963127215));
#262616=CARTESIAN_POINT('Ctrl Pts',(42.8346993804887,-56.3799036982206,
-38.9060738903536));
#262617=CARTESIAN_POINT('Ctrl Pts',(42.8191079311706,-56.4037152169138,
-38.9078025937102));
#262618=CARTESIAN_POINT('Ctrl Pts',(42.8039043779996,-56.4280492827628,
-38.9097224693021));
#262619=CARTESIAN_POINT('Ctrl Pts',(42.7891466755666,-56.4528544726931,
-38.9118346780871));
#262620=CARTESIAN_POINT('Ctrl Pts',(42.7721187707309,-56.4814754870741,
-38.9142718115331));
#262621=CARTESIAN_POINT('Ctrl Pts',(42.7558136628821,-56.5105053677241,
-38.9169462637683));
#262622=CARTESIAN_POINT('Ctrl Pts',(42.7402073536177,-56.5399968434849,
-38.9198636917123));
#262623=CARTESIAN_POINT('Ctrl Pts',(42.7247612337211,-56.5691856070041,
-38.922751174015));
#262624=CARTESIAN_POINT('Ctrl Pts',(42.7100090032885,-56.5988107367616,
-38.9258753161839));
#262625=CARTESIAN_POINT('Ctrl Pts',(42.6959610908403,-56.6288786279515,
-38.9292392096901));
#262626=CARTESIAN_POINT('Ctrl Pts',(42.6820564045184,-56.6586399605976,
-38.932568806468));
#262627=CARTESIAN_POINT('Ctrl Pts',(42.6688417582775,-56.688835076219,-38.9361332943689));
#262628=CARTESIAN_POINT('Ctrl Pts',(42.6563331490267,-56.719472363895,-38.9399372898989));
#262629=CARTESIAN_POINT('Ctrl Pts',(42.6439511930279,-56.7497994402564,
-38.9437027688844));
#262630=CARTESIAN_POINT('Ctrl Pts',(42.6322610361143,-56.7805597750077,
-38.9477029270453));
#262631=CARTESIAN_POINT('Ctrl Pts',(42.6212841673493,-56.8117637261139,
-38.9519438796553));
#262632=CARTESIAN_POINT('Ctrl Pts',(42.610417657956,-56.8426539585708,-38.9561421945263));
#262633=CARTESIAN_POINT('Ctrl Pts',(42.6002501306032,-56.8739789188314,
-38.9605764771568));
#262634=CARTESIAN_POINT('Ctrl Pts',(42.5908086952621,-56.9057509847877,
-38.9652543723165));
#262635=CARTESIAN_POINT('Ctrl Pts',(42.5814614976865,-56.9372059243332,
-38.9698855760176));
#262636=CARTESIAN_POINT('Ctrl Pts',(42.5728249837433,-56.9691068258,-38.9747569641089));
#262637=CARTESIAN_POINT('Ctrl Pts',(42.5649349981973,-57.0014449365778,
-38.9798735188755));
#262638=CARTESIAN_POINT('Ctrl Pts',(42.5571231858622,-57.0334626444927,
-38.9849393793142));
#262639=CARTESIAN_POINT('Ctrl Pts',(42.5500285451438,-57.0660123389163,
-38.9902641114435));
#262640=CARTESIAN_POINT('Ctrl Pts',(42.543771399786,-57.0986331989938,-38.9957757940657));
#262641=CARTESIAN_POINT('Ctrl Pts',(42.5370689667629,-57.1335755117135,
-39.001679713746));
#262642=CARTESIAN_POINT('Ctrl Pts',(42.5312861876561,-57.1687524789562,
-39.007821532343));
#262643=CARTESIAN_POINT('Ctrl Pts',(42.5264426092999,-57.2041247208502,
-39.0141962424421));
#262644=CARTESIAN_POINT('Ctrl Pts',(42.5264426283417,-57.2041246439921,
-39.0141962764686));
#262645=CARTESIAN_POINT('Ctrl Pts',(42.5450760563286,-57.0680445370257,
-39.0216142665105));
#262646=CARTESIAN_POINT('Ctrl Pts',(42.5776734710537,-56.9342676048075,
-39.0293231873749));
#262647=CARTESIAN_POINT('Ctrl Pts',(42.6706416925213,-56.6730323503409,
-39.0452318818938));
#262648=CARTESIAN_POINT('Ctrl Pts',(42.7312783272647,-56.5464660127888,
-39.0533943474495));
#262649=CARTESIAN_POINT('Ctrl Pts',(42.9435983774129,-56.201438833693,-39.0770171498676));
#262650=CARTESIAN_POINT('Ctrl Pts',(43.1261253028118,-56.0054501928792,
-39.0922418351299));
#262651=CARTESIAN_POINT('Ctrl Pts',(43.5474287173053,-55.7029969267937,
-39.1198092304128));
#262652=CARTESIAN_POINT('Ctrl Pts',(43.7794584498512,-55.5956854299055,
-39.1324545161726));
#262653=CARTESIAN_POINT('Ctrl Pts',(44.278976126795,-55.4714954972292,-39.1615930473276));
#262654=CARTESIAN_POINT('Ctrl Pts',(44.5424550156973,-55.4587534023231,
-39.1769626491803));
#262655=CARTESIAN_POINT('Ctrl Pts',(44.904456701214,-55.5123578192425,-39.1980794141687));
#262656=CARTESIAN_POINT('Ctrl Pts',(45.0066424797803,-55.5357960578388,
-39.2040402512518));
#262657=CARTESIAN_POINT('Ctrl Pts',(45.1065281894683,-55.5671267477461,
-39.2098669176502));
#262658=CARTESIAN_POINT('Origin',(44.5079524583206,-57.475452478349,235.35105));
#262659=CARTESIAN_POINT('Ctrl Pts',(44.5079524583206,-59.475452478349,-40.22495));
#262660=CARTESIAN_POINT('Ctrl Pts',(44.3134064919888,-59.475452478349,-40.2362985147027));
#262661=CARTESIAN_POINT('Ctrl Pts',(44.1195072893019,-59.4470642229361,
-40.2476093015263));
#262662=CARTESIAN_POINT('Ctrl Pts',(43.6856583461661,-59.3167143014365,
-40.2729171565426));
#262663=CARTESIAN_POINT('Ctrl Pts',(43.4555514926831,-59.1955857510714,
-40.2854137466271));
#262664=CARTESIAN_POINT('Ctrl Pts',(43.0536254671757,-58.8724196322647,
-40.3134623430353));
#262665=CARTESIAN_POINT('Ctrl Pts',(42.8857301827636,-58.6733468203936,
-40.3284160787138));
#262666=CARTESIAN_POINT('Ctrl Pts',(42.6313500986315,-58.2161860031401,
-40.3589304159134));
#262667=CARTESIAN_POINT('Ctrl Pts',(42.5497586678929,-57.961082232183,-40.3741975361746));
#262668=CARTESIAN_POINT('Ctrl Pts',(42.4921679449883,-57.4454909452804,
-40.4019239828176));
#262669=CARTESIAN_POINT('Ctrl Pts',(42.5121837301983,-57.1904786222485,
-40.4144697636932));
#262670=CARTESIAN_POINT('Ctrl Pts',(42.6484151609807,-56.6942789617644,
-40.4435102685851));
#262671=CARTESIAN_POINT('Ctrl Pts',(42.7661045739579,-56.4585617254506,
-40.4588508748245));
#262672=CARTESIAN_POINT('Ctrl Pts',(43.0879308195211,-56.042323041325,-40.489265081332));
#262673=CARTESIAN_POINT('Ctrl Pts',(43.2901830524831,-55.8669604384183,
-40.5039134513263));
#262674=CARTESIAN_POINT('Ctrl Pts',(43.7417978374699,-55.6105947638857,
-40.5302576471172));
#262675=CARTESIAN_POINT('Ctrl Pts',(43.9848712519941,-55.5283968064006,
-40.5444369296311));
#262676=CARTESIAN_POINT('Ctrl Pts',(44.4984615764082,-55.4581084733143,
-40.5743963652219));
#262677=CARTESIAN_POINT('Ctrl Pts',(44.7646876495702,-55.4744865525067,
-40.5899262194896));
#262678=CARTESIAN_POINT('Ctrl Pts',(45.2710162925252,-55.6085985558055,
-40.6194620569953));
#262679=CARTESIAN_POINT('Ctrl Pts',(45.5066033452955,-55.7232847031097,
-40.6322277122423));
#262680=CARTESIAN_POINT('Ctrl Pts',(45.918984247136,-56.034904349389,-40.659997936129));
#262681=CARTESIAN_POINT('Ctrl Pts',(46.0923733852973,-56.2281484516539,
-40.6748174535908));
#262682=CARTESIAN_POINT('Ctrl Pts',(46.361658910303,-56.6784022072892,-40.705417600851));
#262683=CARTESIAN_POINT('Ctrl Pts',(46.4515224045839,-56.9331562661353,
-40.7209083228238));
#262684=CARTESIAN_POINT('Ctrl Pts',(46.5238640803581,-57.4496948924172,
-40.7491128634236));
#262685=CARTESIAN_POINT('Ctrl Pts',(46.5108390657226,-57.705708271998,-40.7614979036731));
#262686=CARTESIAN_POINT('Ctrl Pts',(46.3881487371309,-58.2052515427372,
-40.7903123727508));
#262687=CARTESIAN_POINT('Ctrl Pts',(46.2773227653104,-58.4434704448938,
-40.8055791748165));
#262688=CARTESIAN_POINT('Ctrl Pts',(45.9678438328221,-58.8679200514476,
-40.8360480519584));
#262689=CARTESIAN_POINT('Ctrl Pts',(45.7706383033074,-59.0489592653161,
-40.8509456458029));
#262690=CARTESIAN_POINT('Ctrl Pts',(45.3269190694736,-59.3176237716168,
-40.8774598902303));
#262691=CARTESIAN_POINT('Ctrl Pts',(45.0869234570947,-59.4065609629546,
-40.8911766917383));
#262692=CARTESIAN_POINT('Ctrl Pts',(44.7277496182526,-59.4664001015449,
-40.9121284990041));
#262693=CARTESIAN_POINT('Ctrl Pts',(44.6178162529024,-59.475452478349,-40.9185412786495));
#262694=CARTESIAN_POINT('Ctrl Pts',(44.5079524583206,-59.475452478349,-40.9249500000001));
#262695=CARTESIAN_POINT('Ctrl Pts',(44.5079524583207,-59.475452478349,-40.7662));
#262696=CARTESIAN_POINT('Ctrl Pts',(44.5083775298429,-59.475452478349,-40.7661752041612));
#262697=CARTESIAN_POINT('Ctrl Pts',(44.5088026080816,-59.4754523428346,
-40.7661504079305));
#262698=CARTESIAN_POINT('Ctrl Pts',(44.7668034260579,-59.4752878370093,
-40.7511003602152));
#262699=CARTESIAN_POINT('Ctrl Pts',(45.0219684864269,-59.4253661652626,
-40.7362157316937));
#262700=CARTESIAN_POINT('Ctrl Pts',(45.500302270728,-59.2310567042668,-40.7083129276095));
#262701=CARTESIAN_POINT('Ctrl Pts',(45.7187606546021,-59.0881700738478,
-40.6956896013403));
#262702=CARTESIAN_POINT('Ctrl Pts',(46.0934420241406,-58.7229365286537,
-40.6663104722357));
#262703=CARTESIAN_POINT('Ctrl Pts',(46.2443678867435,-58.5025073402031,
-40.650772793422));
#262704=CARTESIAN_POINT('Ctrl Pts',(46.4477890250889,-58.0248714647437,
-40.6207103967757));
#262705=CARTESIAN_POINT('Ctrl Pts',(46.5019285880958,-57.7736673579108,
-40.6064409598016));
#262706=CARTESIAN_POINT('Ctrl Pts',(46.5132520993636,-57.2540501555927,
-40.579860591705));
#262707=CARTESIAN_POINT('Ctrl Pts',(46.4663000604843,-56.9904652730994,
-40.5654844827148));
#262708=CARTESIAN_POINT('Ctrl Pts',(46.273636796699,-56.5004392710753,-40.5351099311555));
#262709=CARTESIAN_POINT('Ctrl Pts',(46.1312667756054,-56.2783098828283,
-40.5197359067732));
#262710=CARTESIAN_POINT('Ctrl Pts',(45.7746433882416,-55.9071055070085,
-40.4905818335068));
#262711=CARTESIAN_POINT('Ctrl Pts',(45.5659936742326,-55.7594271642448,
-40.4779190709282));
#262712=CARTESIAN_POINT('Ctrl Pts',(45.093845544046,-55.5448874669513,-40.4503770966673));
#262713=CARTESIAN_POINT('Ctrl Pts',(44.8329702931349,-55.4843029305355,
-40.4351593736975));
#262714=CARTESIAN_POINT('Ctrl Pts',(44.3097029112295,-55.4686054722672,
-40.4046354430863));
#262715=CARTESIAN_POINT('Ctrl Pts',(44.0523852487196,-55.51096207822,-40.3896252461066));
#262716=CARTESIAN_POINT('Ctrl Pts',(43.5694318290431,-55.6907401383014,
-40.3614529632921));
#262717=CARTESIAN_POINT('Ctrl Pts',(43.3481921407017,-55.8259134639983,
-40.3490386477088));
#262718=CARTESIAN_POINT('Ctrl Pts',(42.9626483577539,-56.1783496732344,
-40.3199891959321));
#262719=CARTESIAN_POINT('Ctrl Pts',(42.8043598248836,-56.39462241756,-40.3044467484306));
#262720=CARTESIAN_POINT('Ctrl Pts',(42.585649810967,-56.8672048416347,-40.2741937172546));
#262721=CARTESIAN_POINT('Ctrl Pts',(42.5237503418946,-57.1174066419007,
-40.259748584359));
#262722=CARTESIAN_POINT('Ctrl Pts',(42.4969324210317,-57.6377858849942,
-40.2326777990934));
#262723=CARTESIAN_POINT('Ctrl Pts',(42.5362357228956,-57.9031746362469,
-40.2187673399372));
#262724=CARTESIAN_POINT('Ctrl Pts',(42.7150872537481,-58.3997422547582,
-40.1884651602349));
#262725=CARTESIAN_POINT('Ctrl Pts',(42.8514932711515,-58.6264621509445,
-40.1730331819982));
#262726=CARTESIAN_POINT('Ctrl Pts',(43.1980642286301,-59.007884642095,-40.1436561043353));
#262727=CARTESIAN_POINT('Ctrl Pts',(43.4024115098283,-59.1612444110393,
-40.1306898886619));
#262728=CARTESIAN_POINT('Ctrl Pts',(43.868198574263,-59.3888396055522,-40.1035189765699));
#262729=CARTESIAN_POINT('Ctrl Pts',(44.127238048215,-59.4567017443637,-40.0884083405893));
#262730=CARTESIAN_POINT('Ctrl Pts',(44.4305845724308,-59.4743307533407,
-40.0707131266768));
#262731=CARTESIAN_POINT('Ctrl Pts',(44.4692789444141,-59.475452478349,-40.0684559549778));
#262732=CARTESIAN_POINT('Ctrl Pts',(44.5079524583206,-59.475452478349,-40.0662));
#262733=CARTESIAN_POINT('Ctrl Pts',(43.4805771074156,-59.5712767529309,
-39.2399080357013));
#262734=CARTESIAN_POINT('Ctrl Pts',(43.4150727209207,-59.5358440364426,
-39.2223070534893));
#262735=CARTESIAN_POINT('Ctrl Pts',(43.2883193276586,-59.4590682572254,
-39.1867578392588));
#262736=CARTESIAN_POINT('Ctrl Pts',(43.1106712693135,-59.32658002426,-39.1324031814995));
#262737=CARTESIAN_POINT('Ctrl Pts',(43.0005921597408,-59.2266373021163,
-39.0954660506179));
#262738=CARTESIAN_POINT('Ctrl Pts',(42.8948534568781,-59.1207134074407,
-39.0581733199915));
#262739=CARTESIAN_POINT('Ctrl Pts',(42.7951360401793,-59.0104958554849,
-39.0211184761739));
#262740=CARTESIAN_POINT('Ctrl Pts',(42.6850011896347,-58.8622904152127,
-38.9753582681256));
#262741=CARTESIAN_POINT('Ctrl Pts',(42.6055727997797,-58.7375004045667,
-38.939089851323));
#262742=CARTESIAN_POINT('Ctrl Pts',(42.5503788594446,-58.6407591922129,
-38.9120596161462));
#262743=CARTESIAN_POINT('Ctrl Pts',(42.5165536369311,-58.5741539171446,
-38.8941613358138));
#262744=CARTESIAN_POINT('Ctrl Pts',(42.4842288567228,-58.5064298632496,
-38.8763157156907));
#262745=CARTESIAN_POINT('Ctrl Pts',(42.4689425396028,-58.4722695523732,
-38.8674882509199));
#262746=CARTESIAN_POINT('Ctrl Pts',(42.4257123024776,-58.3690064948315,
-38.8413136266604));
#262747=CARTESIAN_POINT('Ctrl Pts',(42.3750272156063,-58.229152189777,-38.8072100415055));
#262748=CARTESIAN_POINT('Ctrl Pts',(42.3380647902547,-58.0850119200902,
-38.7746901633276));
#262749=CARTESIAN_POINT('Ctrl Pts',(42.3155659796374,-57.9752818499468,
-38.7509105250088));
#262750=CARTESIAN_POINT('Ctrl Pts',(42.3089374211558,-57.9384266221928,
-38.7430843922672));
#262751=CARTESIAN_POINT('Ctrl Pts',(42.297458012674,-57.864178756387,-38.7276438637217));
#262752=CARTESIAN_POINT('Ctrl Pts',(42.292601515188,-57.8267325312259,-38.720018782004));
#262753=CARTESIAN_POINT('Ctrl Pts',(42.2847289916893,-57.7514526301959,
-38.7050196673963));
#262754=CARTESIAN_POINT('Ctrl Pts',(42.2817363521424,-57.7138759968928,
-38.6976962453237));
#262755=CARTESIAN_POINT('Ctrl Pts',(42.277596992864,-57.6387184974263,-38.6833720377019));
#262756=CARTESIAN_POINT('Ctrl Pts',(42.2741651307842,-57.5260409596698,
-38.6623829091612));
#262757=CARTESIAN_POINT('Ctrl Pts',(42.2805893100654,-57.3760354719141,
-38.6363740800325));
#262758=CARTESIAN_POINT('Ctrl Pts',(42.2937061680812,-57.2637038035873,
-38.618370061439));
#262759=CARTESIAN_POINT('Ctrl Pts',(42.3043247017591,-57.1888547452426,
-38.6067079534822));
#262760=CARTESIAN_POINT('Ctrl Pts',(42.3105743117123,-57.1514345461221,
-38.6010450635964));
#262761=CARTESIAN_POINT('Ctrl Pts',(42.3249704170347,-57.0766935209607,
-38.590076215021));
#262762=CARTESIAN_POINT('Ctrl Pts',(42.3331592025312,-57.0392159768686,
-38.5847494243559));
#262763=CARTESIAN_POINT('Ctrl Pts',(42.3512949844302,-56.9651221381903,
-38.5745673038812));
#262764=CARTESIAN_POINT('Ctrl Pts',(42.3712216906218,-56.8916587034686,
-38.564820665347));
#262765=CARTESIAN_POINT('Ctrl Pts',(42.4063979707918,-56.7834465224234,
-38.5515118436));
#262766=CARTESIAN_POINT('Ctrl Pts',(42.4468320479729,-56.6771725078319,
-38.5395042677724));
#262767=CARTESIAN_POINT('Ctrl Pts',(42.4925290654744,-56.5728473165674,
-38.5288039137004));
#262768=CARTESIAN_POINT('Ctrl Pts',(42.5265325119253,-56.5046058456765,
-38.5225509073062));
#262769=CARTESIAN_POINT('Ctrl Pts',(42.5623338475306,-56.4370293947697,
-38.5167461666044));
#262770=CARTESIAN_POINT('Ctrl Pts',(42.5811223641794,-56.4035923099625,
-38.5140693065785));
#262771=CARTESIAN_POINT('Ctrl Pts',(42.620584523009,-56.3373241998654,-38.5091697400817));
#262772=CARTESIAN_POINT('Ctrl Pts',(42.6411082254821,-56.3047465904101,
-38.5069659500128));
#262773=CARTESIAN_POINT('Ctrl Pts',(42.7048067991197,-56.2090283357163,
-38.501110858935));
#262774=CARTESIAN_POINT('Ctrl Pts',(42.7502234543428,-56.1476408662828,
-38.4981890389281));
#262775=CARTESIAN_POINT('Ctrl Pts',(42.8467942323831,-56.0297655581676,
-38.4942910511033));
#262776=CARTESIAN_POINT('Ctrl Pts',(42.8979715413934,-55.9732420482176,
-38.4933125989996));
#262777=CARTESIAN_POINT('Ctrl Pts',(42.9790570553347,-55.8921695883033,
-38.4933149859729));
#262778=CARTESIAN_POINT('Ctrl Pts',(43.0068374106561,-55.8657400908868,
-38.4935622007431));
#262779=CARTESIAN_POINT('Ctrl Pts',(43.0495800649421,-55.8270637749536,
-38.4943063068789));
#262780=CARTESIAN_POINT('Ctrl Pts',(43.0640222060113,-55.8143203511958,
-38.494617152342));
#262781=CARTESIAN_POINT('Ctrl Pts',(43.0932714774893,-55.7891564261061,
-38.4953646906773));
#262782=CARTESIAN_POINT('Ctrl Pts',(43.1080901283632,-55.7767277938553,
-38.4958020036096));
#262783=CARTESIAN_POINT('Ctrl Pts',(43.1528523310046,-55.7401327167866,
-38.4972962980169));
#262784=CARTESIAN_POINT('Ctrl Pts',(43.2134913856688,-55.6930468850421,
-38.4997758707861));
#262785=CARTESIAN_POINT('Ctrl Pts',(43.3385569247743,-55.6055389451161,
-38.5066450244003));
#262786=CARTESIAN_POINT('Ctrl Pts',(43.4691986576013,-55.5278792007279,
-38.5163302992824));
#262787=CARTESIAN_POINT('Ctrl Pts',(43.5713395927684,-55.4769743237494,
-38.5256877381308));
#262788=CARTESIAN_POINT('Ctrl Pts',(43.6403672861995,-55.4446857735354,
-38.5323951500278));
#262789=CARTESIAN_POINT('Ctrl Pts',(43.6753577685123,-55.4293620157832,
-38.5359845633874));
#262790=CARTESIAN_POINT('Ctrl Pts',(43.7462462065788,-55.4003985583156,
-38.5436333065981));
#262791=CARTESIAN_POINT('Ctrl Pts',(43.7822717759725,-55.3867204456352,
-38.5477088862383));
#262792=CARTESIAN_POINT('Ctrl Pts',(43.8543821738219,-55.3613797848081,
-38.5562346427694));
#262793=CARTESIAN_POINT('Ctrl Pts',(43.890622407919,-55.349649082917,-38.5607007444526));
#262794=CARTESIAN_POINT('Ctrl Pts',(43.9997560709039,-55.3172704656441,
-38.5746802407103));
#262795=CARTESIAN_POINT('Ctrl Pts',(44.1098017310836,-55.290468361793,-38.5898286859852));
#262796=CARTESIAN_POINT('Ctrl Pts',(44.2583166685835,-55.2656490138239,
-38.612301023075));
#262797=CARTESIAN_POINT('Ctrl Pts',(44.3705972700495,-55.2524997368729,
-38.6302900391873));
#262798=CARTESIAN_POINT('Ctrl Pts',(44.446056048267,-55.2474029004138,-38.6430428201589));
#262799=CARTESIAN_POINT('Ctrl Pts',(44.5218128020516,-55.2441636366351,
-38.65617756452));
#262800=CARTESIAN_POINT('Ctrl Pts',(44.5599089424743,-55.2434808562086,
-38.6629497802385));
#262801=CARTESIAN_POINT('Ctrl Pts',(44.6354869543582,-55.2439911084578,
-38.6767130108817));
#262802=CARTESIAN_POINT('Ctrl Pts',(44.6731456892459,-55.2451740103824,
-38.6837342374529));
#262803=CARTESIAN_POINT('Ctrl Pts',(44.7481014788608,-55.2493620066237,
-38.6980304684339));
#262804=CARTESIAN_POINT('Ctrl Pts',(44.860046548974,-55.2583760573225,-38.7198650218829));
#262805=CARTESIAN_POINT('Ctrl Pts',(45.0073845433675,-55.2811507310277,
-38.7505067688753));
#262806=CARTESIAN_POINT('Ctrl Pts',(45.1528189888476,-55.3146135839333,
-38.7826550300594));
#262807=CARTESIAN_POINT('Ctrl Pts',(45.2248832056965,-55.3349380951144,
-38.7992310848652));
#262808=CARTESIAN_POINT('Ctrl Pts',(45.2966462681613,-55.3570913336823,
-38.8160672125853));
#262809=CARTESIAN_POINT('Ctrl Pts',(45.3323638946335,-55.3690863290504,
-38.8246135819642));
#262810=CARTESIAN_POINT('Ctrl Pts',(45.4027951436545,-55.3946744461232,
-38.841798196801));
#262811=CARTESIAN_POINT('Ctrl Pts',(45.4376370321487,-55.4083060218429,
-38.85046633842));
#262812=CARTESIAN_POINT('Ctrl Pts',(45.5409345111852,-55.4516493275196,
-38.8766665754573));
#262813=CARTESIAN_POINT('Ctrl Pts',(45.6082182891413,-55.4838201174091,
-38.8944064774514));
#262814=CARTESIAN_POINT('Ctrl Pts',(45.7067749877369,-55.5369855856676,
-38.9214216121435));
#262815=CARTESIAN_POINT('Ctrl Pts',(45.7392219877795,-55.5555212114618,
-38.9304915704334));
#262816=CARTESIAN_POINT('Ctrl Pts',(45.8033556832395,-55.5942722159849,
-38.9487787872477));
#262817=CARTESIAN_POINT('Ctrl Pts',(45.8348443691401,-55.6143675312756,
-38.9579395118015));
#262818=CARTESIAN_POINT('Ctrl Pts',(45.9274099842789,-55.6766589025306,
-38.9854159162723));
#262819=CARTESIAN_POINT('Ctrl Pts',(45.9867610865919,-55.7209353156014,
-39.0037703637879));
#262820=CARTESIAN_POINT('Ctrl Pts',(46.1007337830098,-55.8148102393793,
-39.0405190865864));
#262821=CARTESIAN_POINT('Ctrl Pts',(46.1826971388658,-55.889219933262,-39.0681181728269));
#262822=CARTESIAN_POINT('Ctrl Pts',(46.259356574729,-55.9696687352924,-39.0957737179551));
#262823=CARTESIAN_POINT('Ctrl Pts',(46.309266807939,-56.024663053365,-39.1142236413887));
#262824=CARTESIAN_POINT('Ctrl Pts',(46.3336138177017,-56.0528284109483,
-39.1234510495426));
#262825=CARTESIAN_POINT('Ctrl Pts',(46.3692509284248,-56.0961546965833,
-39.1373141736981));
#262826=CARTESIAN_POINT('Ctrl Pts',(46.3809719555493,-56.1107655250657,
-39.14193505412));
#262827=CARTESIAN_POINT('Ctrl Pts',(46.4039850968433,-56.1401806715041,
-39.1511314768264));
#262828=CARTESIAN_POINT('Ctrl Pts',(46.4153001903629,-56.1550126624776,
-39.1557159133813));
#262829=CARTESIAN_POINT('Ctrl Pts',(46.4486370096885,-56.1998310060263,
-39.1694131182659));
#262830=CARTESIAN_POINT('Ctrl Pts',(46.4700835091466,-56.2301795317326,
-39.1784826054425));
#262831=CARTESIAN_POINT('Ctrl Pts',(46.532071913686,-56.3225583984772,-39.2054898733524));
#262832=CARTESIAN_POINT('Ctrl Pts',(46.5894197348374,-56.4176636744323,
-39.23211607576));
#262833=CARTESIAN_POINT('Ctrl Pts',(46.6566074362748,-56.5498680842415,
-39.2668544229849));
#262834=CARTESIAN_POINT('Ctrl Pts',(46.6870820302515,-56.617790568625,-39.2839693714534));
#262835=CARTESIAN_POINT('Ctrl Pts',(46.7159729830272,-56.6866360545619,
-39.3009558869148));
#262836=CARTESIAN_POINT('Ctrl Pts',(46.7296188023799,-56.7214992889704,
-39.3093799218186));
#262837=CARTESIAN_POINT('Ctrl Pts',(46.7553216997643,-56.7922546384013,
-39.3261176641085));
#262838=CARTESIAN_POINT('Ctrl Pts',(46.7672996943011,-56.8279354881579,
-39.3343809787628));
#262839=CARTESIAN_POINT('Ctrl Pts',(46.8004530502947,-56.9353633959568,
-39.358737163018));
#262840=CARTESIAN_POINT('Ctrl Pts',(46.8189795501832,-57.0077635587999,
-39.3744658121213));
#262841=CARTESIAN_POINT('Ctrl Pts',(46.848916211803,-57.1540080946302,-39.4048998290393));
#262842=CARTESIAN_POINT('Ctrl Pts',(46.866048617508,-57.2647966217996,-39.4269646939479));
#262843=CARTESIAN_POINT('Ctrl Pts',(46.875074749658,-57.3772756893033,-39.4478819384746));
#262844=CARTESIAN_POINT('Ctrl Pts',(46.8792542953452,-57.4526370309597,
-39.4615663943076));
#262845=CARTESIAN_POINT('Ctrl Pts',(46.8804258736835,-57.4905390832845,
-39.4682843608713));
#262846=CARTESIAN_POINT('Ctrl Pts',(46.8808837743635,-57.566610437341,-39.4814341960201));
#262847=CARTESIAN_POINT('Ctrl Pts',(46.8801708637706,-57.604491394965,-39.4878166677226));
#262848=CARTESIAN_POINT('Ctrl Pts',(46.8768913879562,-57.6800597985945,
-39.5002231148134));
#262849=CARTESIAN_POINT('Ctrl Pts',(46.8691896925243,-57.7930657109158,
-39.5182849936093));
#262850=CARTESIAN_POINT('Ctrl Pts',(46.8479069711518,-57.9423669591112,
-39.540205996752));
#262851=CARTESIAN_POINT('Ctrl Pts',(46.8236459543104,-58.053306681129,-39.5550278422771));
#262852=CARTESIAN_POINT('Ctrl Pts',(46.8055990109883,-58.1270324939452,
-39.5645447403379));
#262853=CARTESIAN_POINT('Ctrl Pts',(46.7956339676918,-58.1637938532181,
-39.5691227921436));
#262854=CARTESIAN_POINT('Ctrl Pts',(46.7738161327052,-58.2370162077019,
-39.5779016468881));
#262855=CARTESIAN_POINT('Ctrl Pts',(46.7619036278491,-58.2736352268715,
-39.5821192203466));
#262856=CARTESIAN_POINT('Ctrl Pts',(46.7364059718256,-58.3458255995332,
-39.5900871854462));
#262857=CARTESIAN_POINT('Ctrl Pts',(46.7091836493705,-58.4171862986019,
-39.5976163356366));
#262858=CARTESIAN_POINT('Ctrl Pts',(46.663274408039,-58.5216699086648,-39.6076014242402));
#262859=CARTESIAN_POINT('Ctrl Pts',(46.6123207377325,-58.6236436013082,
-39.616293729045));
#262860=CARTESIAN_POINT('Ctrl Pts',(46.5563244858032,-58.7230996041114,
-39.6236943138341));
#262861=CARTESIAN_POINT('Ctrl Pts',(46.515607032986,-58.7877140896312,-39.6277619492082));
#262862=CARTESIAN_POINT('Ctrl Pts',(46.4731710833873,-58.8514710047945,
-39.6313905635194));
#262863=CARTESIAN_POINT('Ctrl Pts',(46.4511086137465,-58.8829006319494,
-39.6329844599904));
#262864=CARTESIAN_POINT('Ctrl Pts',(46.4051673201274,-58.9449633016888,
-39.6357273485653));
#262865=CARTESIAN_POINT('Ctrl Pts',(46.381447994276,-58.975377588932,-39.6368662598532));
#262866=CARTESIAN_POINT('Ctrl Pts',(46.3084068909562,-59.0643493136614,
-39.6395761233691));
#262867=CARTESIAN_POINT('Ctrl Pts',(46.2570407846102,-59.1209150453974,
-39.6404603784325));
#262868=CARTESIAN_POINT('Ctrl Pts',(46.1491379755941,-59.228544463199,-39.6404138814247));
#262869=CARTESIAN_POINT('Ctrl Pts',(46.0925836555155,-59.2796343044913,
-39.6394845811684));
#262870=CARTESIAN_POINT('Ctrl Pts',(46.0038529437629,-59.3521266125547,
-39.6367223387528));
#262871=CARTESIAN_POINT('Ctrl Pts',(45.9736068078661,-59.3756113554055,
-39.6355721163029));
#262872=CARTESIAN_POINT('Ctrl Pts',(45.9272656961273,-59.4097723546528,
-39.6334997725088));
#262873=CARTESIAN_POINT('Ctrl Pts',(45.9116419215573,-59.4209912820171,
-39.6327502808957));
#262874=CARTESIAN_POINT('Ctrl Pts',(45.8800804794677,-59.4430610802669,
-39.6311351339295));
#262875=CARTESIAN_POINT('Ctrl Pts',(45.8321587971618,-59.4756823489919,
-39.628531354857));
#262876=CARTESIAN_POINT('Ctrl Pts',(45.7834097108732,-59.5062438963941,
-39.6254355071979));
#262877=CARTESIAN_POINT('Ctrl Pts',(45.717633106262,-59.5452481912826,-39.6208773262667));
#262878=CARTESIAN_POINT('Ctrl Pts',(45.6178307490054,-59.601113548897,-39.6133952897297));
#262879=CARTESIAN_POINT('Ctrl Pts',(45.4802897643185,-59.6652183443042,
-39.6008811885904));
#262880=CARTESIAN_POINT('Ctrl Pts',(45.3738098009101,-59.7055766782111,
-39.5896017905935));
#262881=CARTESIAN_POINT('Ctrl Pts',(45.3020778813705,-59.7307512119865,
-39.5816566825671));
#262882=CARTESIAN_POINT('Ctrl Pts',(45.2658207311094,-59.7424779859237,
-39.5774690651077));
#262883=CARTESIAN_POINT('Ctrl Pts',(45.1926264675053,-59.7641596016776,
-39.5686715125846));
#262884=CARTESIAN_POINT('Ctrl Pts',(45.1555073907618,-59.7741562512684,
-39.5640376159893));
#262885=CARTESIAN_POINT('Ctrl Pts',(45.0441315765335,-59.8011904590316,
-39.5496210468413));
#262886=CARTESIAN_POINT('Ctrl Pts',(44.9324484012679,-59.8224577850013,
-39.5341534065747));
#262887=CARTESIAN_POINT('Ctrl Pts',(44.8203079610257,-59.8353953605365,
-39.5171556909205));
#262888=CARTESIAN_POINT('Ctrl Pts',(44.7080184564226,-59.8455760612675,
-39.4996502778008));
#262889=CARTESIAN_POINT('Ctrl Pts',(44.6329372249224,-59.8486931621852,
-39.4873001861445));
#262890=CARTESIAN_POINT('Ctrl Pts',(44.5200834441659,-59.8478515133141,
-39.4677634802869));
#262891=CARTESIAN_POINT('Ctrl Pts',(44.4823810871712,-59.8466449718289,
-39.4610736497974));
#262892=CARTESIAN_POINT('Ctrl Pts',(44.4258051079382,-59.8434394706745,
-39.4507883432074));
#262893=CARTESIAN_POINT('Ctrl Pts',(44.4069254589855,-59.8421361346926,
-39.4473147915973));
#262894=CARTESIAN_POINT('Ctrl Pts',(44.3691376542581,-59.8390581625153,
-39.4402793331445));
#262895=CARTESIAN_POINT('Ctrl Pts',(44.3502459350849,-59.8372838734483,
-39.4367203104461));
#262896=CARTESIAN_POINT('Ctrl Pts',(44.2562487381671,-59.8272835659938,
-39.4188041728073));
#262897=CARTESIAN_POINT('Ctrl Pts',(44.1080045765469,-59.8040393501646,
-39.3892226636159));
#262898=CARTESIAN_POINT('Ctrl Pts',(43.9639303529155,-59.7668593120831,
-39.3578670379715));
#262899=CARTESIAN_POINT('Ctrl Pts',(43.8219159040518,-59.7227861654643,
-39.3256251231267));
#262900=CARTESIAN_POINT('Ctrl Pts',(43.7519290534068,-59.6972943066161,
-39.3090578287531));
#262901=CARTESIAN_POINT('Ctrl Pts',(43.665783177736,-59.6610675807531,-39.2877890488175));
#262902=CARTESIAN_POINT('Ctrl Pts',(43.6486106666635,-59.653596197985,-39.2835041280971));
#262903=CARTESIAN_POINT('Ctrl Pts',(43.6144193015916,-59.6382222359849,
-39.2748825183767));
#262904=CARTESIAN_POINT('Ctrl Pts',(43.597366582891,-59.6303022352814,-39.2705368924251));
#262905=CARTESIAN_POINT('Ctrl Pts',(43.5465994182959,-59.605961903298,-39.2574616452183));
#262906=CARTESIAN_POINT('Ctrl Pts',(43.513329300663,-59.588993111175,-39.2487085268073));
#262907=CARTESIAN_POINT('Ctrl Pts',(43.4805771074156,-59.5712767529309,
-39.2399080357013));
#262908=CARTESIAN_POINT('Ctrl Pts',(43.8903154257419,-57.7291941381088,
-41.4266127101804));
#262909=CARTESIAN_POINT('Ctrl Pts',(43.8716814361492,-57.7189244770852,
-41.4090117279687));
#262910=CARTESIAN_POINT('Ctrl Pts',(43.8355945080866,-57.6967277837834,
-41.3734625137379));
#262911=CARTESIAN_POINT('Ctrl Pts',(43.7849271573585,-57.6585752750105,
-41.3191078559793));
#262912=CARTESIAN_POINT('Ctrl Pts',(43.753465403225,-57.62988352171,-41.2821707250961));
#262913=CARTESIAN_POINT('Ctrl Pts',(43.7232071092872,-57.5995155202448,
-41.2448779944712));
#262914=CARTESIAN_POINT('Ctrl Pts',(43.694633283399,-57.5679550683129,-41.2078231506529));
#262915=CARTESIAN_POINT('Ctrl Pts',(43.6629744005209,-57.5256074013359,
-41.162062942605));
#262916=CARTESIAN_POINT('Ctrl Pts',(43.6400741040405,-57.4900012877665,
-41.1257945258022));
#262917=CARTESIAN_POINT('Ctrl Pts',(43.624122646482,-57.4624228770549,-41.0987642906252));
#262918=CARTESIAN_POINT('Ctrl Pts',(43.6143188854815,-57.4434516436916,
-41.0808660102928));
#262919=CARTESIAN_POINT('Ctrl Pts',(43.6049343759216,-57.4241698350281,
-41.0630203901697));
#262920=CARTESIAN_POINT('Ctrl Pts',(43.6004882740613,-57.4144479878336,
-41.054192925399));
#262921=CARTESIAN_POINT('Ctrl Pts',(43.5878889573419,-57.3850715912746,
-41.0280183011396));
#262922=CARTESIAN_POINT('Ctrl Pts',(43.5730447416356,-57.3453166524842,
-40.9939147159844));
#262923=CARTESIAN_POINT('Ctrl Pts',(43.5620571572655,-57.3044044614592,
-40.9613948378065));
#262924=CARTESIAN_POINT('Ctrl Pts',(43.5552843243605,-57.2732819874194,
-40.9376151994878));
#262925=CARTESIAN_POINT('Ctrl Pts',(43.5532714802541,-57.2628325912303,
-40.9297890667463));
#262926=CARTESIAN_POINT('Ctrl Pts',(43.5497454556161,-57.2417890776549,
-40.9143485382007));
#262927=CARTESIAN_POINT('Ctrl Pts',(43.5482304746054,-57.2311797832666,
-40.9067234564832));
#262928=CARTESIAN_POINT('Ctrl Pts',(43.5457184756399,-57.2098591834555,
-40.8917243418755));
#262929=CARTESIAN_POINT('Ctrl Pts',(43.5447290487245,-57.199220662917,-40.8844009198028));
#262930=CARTESIAN_POINT('Ctrl Pts',(43.5432711863927,-57.1779500447907,
-40.8700767121812));
#262931=CARTESIAN_POINT('Ctrl Pts',(43.5418684734652,-57.1460721839032,
-40.8490875836402));
#262932=CARTESIAN_POINT('Ctrl Pts',(43.5431039253892,-57.1036793909824,
-40.8230787545116));
#262933=CARTESIAN_POINT('Ctrl Pts',(43.5463738329101,-57.0719682486671,
-40.8050747359183));
#262934=CARTESIAN_POINT('Ctrl Pts',(43.5490829635055,-57.0508462881094,
-40.7934126279614));
#262935=CARTESIAN_POINT('Ctrl Pts',(43.5507030159248,-57.0402904723448,
-40.7877497380755));
#262936=CARTESIAN_POINT('Ctrl Pts',(43.5544790630841,-57.019214904491,-40.7767808895002));
#262937=CARTESIAN_POINT('Ctrl Pts',(43.5566463931059,-57.0086510117152,
-40.7714540988351));
#262938=CARTESIAN_POINT('Ctrl Pts',(43.5614808344627,-56.9877741662596,
-40.7612719783604));
#262939=CARTESIAN_POINT('Ctrl Pts',(43.5668234022498,-56.9670831174431,
-40.7515253398262));
#262940=CARTESIAN_POINT('Ctrl Pts',(43.5763377125496,-56.9366295208774,
-40.7382165180791));
#262941=CARTESIAN_POINT('Ctrl Pts',(43.5873444561754,-56.9067460923864,
-40.7262089422516));
#262942=CARTESIAN_POINT('Ctrl Pts',(43.5998453117462,-56.8774358278222,
-40.7155085881795));
#262943=CARTESIAN_POINT('Ctrl Pts',(43.6091839698139,-56.8582805167828,
-40.7092555817853));
#262944=CARTESIAN_POINT('Ctrl Pts',(43.6190331668358,-56.8393207538612,
-40.7034508410834));
#262945=CARTESIAN_POINT('Ctrl Pts',(43.6242099732076,-56.8299438685379,
-40.7007739810578));
#262946=CARTESIAN_POINT('Ctrl Pts',(43.6350986096338,-56.8113693026126,
-40.6958744145609));
#262947=CARTESIAN_POINT('Ctrl Pts',(43.6407690742328,-56.8022426567881,
-40.6936706244929));
#262948=CARTESIAN_POINT('Ctrl Pts',(43.6583896223854,-56.7754411523649,
-40.6878155334118));
#262949=CARTESIAN_POINT('Ctrl Pts',(43.6709801307092,-56.7582712890167,
-40.6848937134075));
#262950=CARTESIAN_POINT('Ctrl Pts',(43.6978023804218,-56.725340315416,-40.6809957255822));
#262951=CARTESIAN_POINT('Ctrl Pts',(43.7120405319879,-56.7095692151415,
-40.6800172734785));
#262952=CARTESIAN_POINT('Ctrl Pts',(43.7346338722206,-56.6869796178674,
-40.680019660452));
#262953=CARTESIAN_POINT('Ctrl Pts',(43.7423799312797,-56.6796208977126,
-40.6802668752224));
#262954=CARTESIAN_POINT('Ctrl Pts',(43.7543060585229,-56.6688607312791,
-40.681010981358));
#262955=CARTESIAN_POINT('Ctrl Pts',(43.7583370517177,-56.6653168192219,
-40.6813218268212));
#262956=CARTESIAN_POINT('Ctrl Pts',(43.7665035456834,-56.6583217341419,
-40.6820693651562));
#262957=CARTESIAN_POINT('Ctrl Pts',(43.7706422703,-56.6548683091639,-40.6825066780886));
#262958=CARTESIAN_POINT('Ctrl Pts',(43.7831478581881,-56.6447045100584,
-40.6840009724959));
#262959=CARTESIAN_POINT('Ctrl Pts',(43.8000992888712,-56.6316392340345,
-40.6864805452653));
#262960=CARTESIAN_POINT('Ctrl Pts',(43.8351004518507,-56.6074069729907,
-40.6933496988796));
#262961=CARTESIAN_POINT('Ctrl Pts',(43.8717190640765,-56.5859796680779,
-40.7030349737613));
#262962=CARTESIAN_POINT('Ctrl Pts',(43.9003898794618,-56.5719991465823,
-40.7123924126099));
#262963=CARTESIAN_POINT('Ctrl Pts',(43.919774692733,-56.5631479893168,-40.719099824507));
#262964=CARTESIAN_POINT('Ctrl Pts',(43.9296053152689,-56.5589560552736,
-40.722689237866));
#262965=CARTESIAN_POINT('Ctrl Pts',(43.9495302416178,-56.551051384942,-40.7303379810773));
#262966=CARTESIAN_POINT('Ctrl Pts',(43.959660471973,-56.5473282955902,-40.7344135607172));
#262967=CARTESIAN_POINT('Ctrl Pts',(43.9799461530017,-56.5404515818703,
-40.7429393172485));
#262968=CARTESIAN_POINT('Ctrl Pts',(43.9901452646573,-56.5372793127045,
-40.7474054189318));
#262969=CARTESIAN_POINT('Ctrl Pts',(44.0208712025373,-56.5285586047056,
-40.7613849151889));
#262970=CARTESIAN_POINT('Ctrl Pts',(44.0518784813599,-56.521416173947,-40.7765333604643));
#262971=CARTESIAN_POINT('Ctrl Pts',(44.0937728041468,-56.5149820273198,
-40.799005697554));
#262972=CARTESIAN_POINT('Ctrl Pts',(44.1254693703652,-56.5117027703592,
-40.8169947136667));
#262973=CARTESIAN_POINT('Ctrl Pts',(44.1467868482481,-56.5105547568045,
-40.8297474946377));
#262974=CARTESIAN_POINT('Ctrl Pts',(44.1681963264173,-56.50993223545,-40.842882238999));
#262975=CARTESIAN_POINT('Ctrl Pts',(44.1789665479467,-56.509886262238,-40.8496544547178));
#262976=CARTESIAN_POINT('Ctrl Pts',(44.2003410646824,-56.5103214152413,
-40.8634176853611));
#262977=CARTESIAN_POINT('Ctrl Pts',(44.2109953322312,-56.5108003631786,
-40.8704389119319));
#262978=CARTESIAN_POINT('Ctrl Pts',(44.2322091102727,-56.5122711761573,
-40.8847351429132));
#262979=CARTESIAN_POINT('Ctrl Pts',(44.2639028799147,-56.5152466319394,
-40.9065696963621));
#262980=CARTESIAN_POINT('Ctrl Pts',(44.305661850593,-56.5222422564611,-40.9372114433545));
#262981=CARTESIAN_POINT('Ctrl Pts',(44.346925841944,-56.532247127269,-40.9693597045385));
#262982=CARTESIAN_POINT('Ctrl Pts',(44.3673876336497,-56.53826115526,-40.9859357593442));
#262983=CARTESIAN_POINT('Ctrl Pts',(44.3877715667723,-56.5447901720246,
-41.0027718870644));
#262984=CARTESIAN_POINT('Ctrl Pts',(44.3979208506631,-56.5483132560745,
-41.0113182564434));
#262985=CARTESIAN_POINT('Ctrl Pts',(44.4179418071922,-56.5558066378292,
-41.02850287128));
#262986=CARTESIAN_POINT('Ctrl Pts',(44.4278499085732,-56.5597882829787,
-41.0371710128992));
#262987=CARTESIAN_POINT('Ctrl Pts',(44.4572364860018,-56.5724196473794,
-41.0633712499365));
#262988=CARTESIAN_POINT('Ctrl Pts',(44.4763932211824,-56.581758968269,-41.0811111519311));
#262989=CARTESIAN_POINT('Ctrl Pts',(44.5044772880921,-56.5971447477014,
-41.1081262866225));
#262990=CARTESIAN_POINT('Ctrl Pts',(44.5137271775895,-56.6025015227711,
-41.1171962449124));
#262991=CARTESIAN_POINT('Ctrl Pts',(44.5320183562985,-56.6136863880645,
-41.1354834617267));
#262992=CARTESIAN_POINT('Ctrl Pts',(44.5410031705763,-56.6194798267371,
-41.144644186283));
#262993=CARTESIAN_POINT('Ctrl Pts',(44.5674276642847,-56.6374191091633,
-41.1721205907467));
#262994=CARTESIAN_POINT('Ctrl Pts',(44.5843870769067,-56.6501457393646,
-41.1904750382678));
#262995=CARTESIAN_POINT('Ctrl Pts',(44.616987890196,-56.6770839740703,-41.2272237610649));
#262996=CARTESIAN_POINT('Ctrl Pts',(44.640458797708,-56.6984048650555,-41.2548228473058));
#262997=CARTESIAN_POINT('Ctrl Pts',(44.6624514458289,-56.7214114906953,
-41.2824783924342));
#262998=CARTESIAN_POINT('Ctrl Pts',(44.6767798128067,-56.7371294193188,
-41.3009283158679));
#262999=CARTESIAN_POINT('Ctrl Pts',(44.683774397772,-56.7451748501741,-41.3101557240219));
#263000=CARTESIAN_POINT('Ctrl Pts',(44.6940202659092,-56.7575442973705,
-41.324018848177));
#263001=CARTESIAN_POINT('Ctrl Pts',(44.6973914635031,-56.7617145235639,
-41.328639728599));
#263002=CARTESIAN_POINT('Ctrl Pts',(44.7040131878578,-56.770108052971,-41.3378361513053));
#263003=CARTESIAN_POINT('Ctrl Pts',(44.7072703203268,-56.7743392575068,
-41.3424205878605));
#263004=CARTESIAN_POINT('Ctrl Pts',(44.7168707027477,-56.7871217033085,
-41.3561177927451));
#263005=CARTESIAN_POINT('Ctrl Pts',(44.7230524906066,-56.7957731420119,
-41.3651872799216));
#263006=CARTESIAN_POINT('Ctrl Pts',(44.7409373255192,-56.8220955492914,
-41.3921945478314));
#263007=CARTESIAN_POINT('Ctrl Pts',(44.7575187561203,-56.8491712652862,
-41.4188207502394));
#263008=CARTESIAN_POINT('Ctrl Pts',(44.7770214494108,-56.88676384976,-41.453559097464));
#263009=CARTESIAN_POINT('Ctrl Pts',(44.7858965000619,-56.9060633365117,
-41.4706740459328));
#263010=CARTESIAN_POINT('Ctrl Pts',(44.7943266372896,-56.9256180211132,
-41.4876605613939));
#263011=CARTESIAN_POINT('Ctrl Pts',(44.7983169540911,-56.9355169983302,
-41.4960845962979));
#263012=CARTESIAN_POINT('Ctrl Pts',(44.8058516078422,-56.9556000996462,
-41.5128223385875));
#263013=CARTESIAN_POINT('Ctrl Pts',(44.8093727854448,-56.9657242505397,
-41.5210856532432));
#263014=CARTESIAN_POINT('Ctrl Pts',(44.8191505788346,-56.9961959016236,
-41.5454418374945));
#263015=CARTESIAN_POINT('Ctrl Pts',(44.8246597322132,-57.0167187198372,
-41.5611704866007));
#263016=CARTESIAN_POINT('Ctrl Pts',(44.8336688220904,-57.0581479791523,
-41.5916045035181));
#263017=CARTESIAN_POINT('Ctrl Pts',(44.8389236650083,-57.0895139074259,
-41.613669368427));
#263018=CARTESIAN_POINT('Ctrl Pts',(44.8418900765893,-57.1213299669285,
-41.6345866129535));
#263019=CARTESIAN_POINT('Ctrl Pts',(44.8433488372948,-57.142640498193,-41.6482710687869));
#263020=CARTESIAN_POINT('Ctrl Pts',(44.8438191277705,-57.1533552116615,
-41.6549890353504));
#263021=CARTESIAN_POINT('Ctrl Pts',(44.8442270800594,-57.1748537940466,
-41.6681388704993));
#263022=CARTESIAN_POINT('Ctrl Pts',(44.8441639040618,-57.1855561823783,
-41.6745213422017));
#263023=CARTESIAN_POINT('Ctrl Pts',(44.8435122114514,-57.2069000331791,
-41.6869277892926));
#263024=CARTESIAN_POINT('Ctrl Pts',(44.8417458896958,-57.2388084678274,
-41.7049896680882));
#263025=CARTESIAN_POINT('Ctrl Pts',(44.8362687719071,-57.2809279665006,
-41.7269106712316));
#263026=CARTESIAN_POINT('Ctrl Pts',(44.8298088085522,-57.3121969378441,
-41.7417325167562));
#263027=CARTESIAN_POINT('Ctrl Pts',(44.8249713776488,-57.3329705079708,
-41.751249414817));
#263028=CARTESIAN_POINT('Ctrl Pts',(44.8222858794974,-57.3433254378487,
-41.7558274666229));
#263029=CARTESIAN_POINT('Ctrl Pts',(44.8163797073795,-57.3639440769784,
-41.7646063213672));
#263030=CARTESIAN_POINT('Ctrl Pts',(44.8131427147447,-57.3742522416544,
-41.7688238948253));
#263031=CARTESIAN_POINT('Ctrl Pts',(44.8061917406462,-57.3945668799698,
-41.7767918599254));
#263032=CARTESIAN_POINT('Ctrl Pts',(44.7987498536529,-57.4146412549335,
-41.7843210101159));
#263033=CARTESIAN_POINT('Ctrl Pts',(44.7861419817956,-57.4440129710611,
-41.7943060987191));
#263034=CARTESIAN_POINT('Ctrl Pts',(44.7720982599006,-57.4726583092559,
-41.8029984035242));
#263035=CARTESIAN_POINT('Ctrl Pts',(44.7566193423106,-57.5005749992605,
-41.8103989883131));
#263036=CARTESIAN_POINT('Ctrl Pts',(44.7453362941317,-57.518697088903,-41.8144666236875));
#263037=CARTESIAN_POINT('Ctrl Pts',(44.7335642473644,-57.5365709174371,
-41.8180952379985));
#263038=CARTESIAN_POINT('Ctrl Pts',(44.7274378249752,-57.5453780864623,
-41.8196891344695));
#263039=CARTESIAN_POINT('Ctrl Pts',(44.7146685840676,-57.5627610237142,
-41.8224320230444));
#263040=CARTESIAN_POINT('Ctrl Pts',(44.7080700862024,-57.5712755128024,
-41.8235709343319));
#263041=CARTESIAN_POINT('Ctrl Pts',(44.6877341610586,-57.5961705213949,
-41.8262807978491));
#263042=CARTESIAN_POINT('Ctrl Pts',(44.6734117165454,-57.6119810052107,
-41.8271650529119));
#263043=CARTESIAN_POINT('Ctrl Pts',(44.6432859415473,-57.6420285404153,
-41.827118555904));
#263044=CARTESIAN_POINT('Ctrl Pts',(44.6274777219699,-57.6562729242579,
-41.8261892556471));
#263045=CARTESIAN_POINT('Ctrl Pts',(44.6026489360012,-57.6764545436153,
-41.823427013232));
#263046=CARTESIAN_POINT('Ctrl Pts',(44.5941811636919,-57.6829873126311,
-41.8222767907821));
#263047=CARTESIAN_POINT('Ctrl Pts',(44.5812011369499,-57.6924815728277,
-41.820204446988));
#263048=CARTESIAN_POINT('Ctrl Pts',(44.5768239301145,-57.6955981764101,
-41.8194549553751));
#263049=CARTESIAN_POINT('Ctrl Pts',(44.5679795363474,-57.7017261947271,
-41.8178398084084));
#263050=CARTESIAN_POINT('Ctrl Pts',(44.554547495243,-57.7107794649358,-41.8152360293365));
#263051=CARTESIAN_POINT('Ctrl Pts',(44.5408745509057,-57.7192473537464,
-41.812140181677));
#263052=CARTESIAN_POINT('Ctrl Pts',(44.5224181841827,-57.7300417662926,
-41.8075820007456));
#263053=CARTESIAN_POINT('Ctrl Pts',(44.494403164631,-57.7454824222945,-41.8000999642091));
#263054=CARTESIAN_POINT('Ctrl Pts',(44.4557509611988,-57.7631175354143,
-41.7875858630695));
#263055=CARTESIAN_POINT('Ctrl Pts',(44.4257963579031,-57.7741479888816,
-41.7763064650726));
#263056=CARTESIAN_POINT('Ctrl Pts',(44.4056101875344,-57.781009218212,-41.7683613570464));
#263057=CARTESIAN_POINT('Ctrl Pts',(44.3954036594654,-57.7841949818065,
-41.7641737395871));
#263058=CARTESIAN_POINT('Ctrl Pts',(44.3747925009816,-57.7900627169564,
-41.7553761870634));
#263059=CARTESIAN_POINT('Ctrl Pts',(44.3643365899562,-57.7927558542442,
-41.7507422904685));
#263060=CARTESIAN_POINT('Ctrl Pts',(44.3329536886806,-57.7999988857253,
-41.7363257213199));
#263061=CARTESIAN_POINT('Ctrl Pts',(44.3014645871824,-57.8056090798854,
-41.7208580810542));
#263062=CARTESIAN_POINT('Ctrl Pts',(44.2698183189435,-57.8088603667088,
-41.7038603653999));
#263063=CARTESIAN_POINT('Ctrl Pts',(44.2381206623806,-57.8113308880715,
-41.6863549522799));
#263064=CARTESIAN_POINT('Ctrl Pts',(44.2169139506954,-57.8119384373532,
-41.6740048606234));
#263065=CARTESIAN_POINT('Ctrl Pts',(44.1850197107514,-57.811287280344,-41.6544681547659));
#263066=CARTESIAN_POINT('Ctrl Pts',(44.1743613109546,-57.8108078241776,
-41.6477783242763));
#263067=CARTESIAN_POINT('Ctrl Pts',(44.1583626375358,-57.8096935003687,
-41.6374930176863));
#263068=CARTESIAN_POINT('Ctrl Pts',(44.1530230189312,-57.809255510817,-41.6340194660765));
#263069=CARTESIAN_POINT('Ctrl Pts',(44.1423341247923,-57.8082460206643,
-41.6269840076234));
#263070=CARTESIAN_POINT('Ctrl Pts',(44.1369894952372,-57.8076746784434,
-41.6234249849254));
#263071=CARTESIAN_POINT('Ctrl Pts',(44.1103928894951,-57.8045001122898,
-41.6055088472864));
#263072=CARTESIAN_POINT('Ctrl Pts',(44.0684216046586,-57.7973782151022,
-41.5759273380954));
#263073=CARTESIAN_POINT('Ctrl Pts',(44.0275807082801,-57.78632659952,-41.5445717124501));
#263074=CARTESIAN_POINT('Ctrl Pts',(43.9872978152183,-57.7733311875938,
-41.5123297976061));
#263075=CARTESIAN_POINT('Ctrl Pts',(43.9674326520914,-57.7658590768128,
-41.4957625032292));
#263076=CARTESIAN_POINT('Ctrl Pts',(43.942963744406,-57.7552890823142,-41.4744937232973));
#263077=CARTESIAN_POINT('Ctrl Pts',(43.938085174092,-57.7531113051098,-41.4702088025761));
#263078=CARTESIAN_POINT('Ctrl Pts',(43.9283699185172,-57.7486342535987,
-41.4615871928557));
#263079=CARTESIAN_POINT('Ctrl Pts',(43.9235236029976,-57.7463299238453,
-41.4572415669043));
#263080=CARTESIAN_POINT('Ctrl Pts',(43.9090930604083,-57.739254093668,-41.4441663196977));
#263081=CARTESIAN_POINT('Ctrl Pts',(43.8996324205383,-57.7343289686206,
-41.4354132012863));
#263082=CARTESIAN_POINT('Ctrl Pts',(43.8903154257419,-57.7291941381088,
-41.4266127101804));
#263083=CARTESIAN_POINT('Ctrl Pts',(45.3466064770396,-58.9181479613239,
-40.3575668307238));
#263084=CARTESIAN_POINT('Ctrl Pts',(45.4516646101692,-58.8920684645362,
-40.3337973782014));
#263085=CARTESIAN_POINT('Ctrl Pts',(45.552602293926,-58.8523392629073,-40.3122779577289));
#263086=CARTESIAN_POINT('Ctrl Pts',(45.770110848815,-58.7283580826205,-40.2690841502618));
#263087=CARTESIAN_POINT('Ctrl Pts',(45.8536347036611,-58.6509076535168,
-40.2548720327848));
#263088=CARTESIAN_POINT('Ctrl Pts',(45.9570392315636,-58.5416230805558,
-40.2380576556195));
#263089=CARTESIAN_POINT('Ctrl Pts',(46.0024773285342,-58.4828736078693,
-40.2313880447387));
#263090=CARTESIAN_POINT('Ctrl Pts',(46.0430807877281,-58.4179319806454,
-40.2261213989136));
#263091=CARTESIAN_POINT('Ctrl Pts',(46.0442081473202,-58.4161174068685,
-40.2259758098144));
#263092=CARTESIAN_POINT('Ctrl Pts',(46.0464553681406,-58.4124772870063,
-40.2256868790796));
#263093=CARTESIAN_POINT('Ctrl Pts',(46.0475751858796,-58.4106517551719,
-40.2255435461549));
#263094=CARTESIAN_POINT('Ctrl Pts',(46.0509385616361,-58.4051335817647,
-40.2251149869642));
#263095=CARTESIAN_POINT('Ctrl Pts',(46.0531661919851,-58.4014311118043,
-40.2248337748911));
#263096=CARTESIAN_POINT('Ctrl Pts',(46.057596560155,-58.3939710903869,-40.2242797496958));
#263097=CARTESIAN_POINT('Ctrl Pts',(46.0597989224255,-58.3902134067562,
-40.2240070251327));
#263098=CARTESIAN_POINT('Ctrl Pts',(46.0664273169517,-58.3787531619006,
-40.2231943218832));
#263099=CARTESIAN_POINT('Ctrl Pts',(46.0707848097754,-58.3710107097114,
-40.2226712692112));
#263100=CARTESIAN_POINT('Ctrl Pts',(46.11569824585,-58.2889710726676,-40.2173984115144));
#263101=CARTESIAN_POINT('Ctrl Pts',(46.1479046651237,-58.2104747759277,
-40.2146562982938));
#263102=CARTESIAN_POINT('Ctrl Pts',(46.2182188782769,-57.9683633912216,
-40.2117772978026));
#263103=CARTESIAN_POINT('Ctrl Pts',(46.2306353135395,-57.7999976154122,
-40.2167399225082));
#263104=CARTESIAN_POINT('Ctrl Pts',(46.2049800979504,-57.5666578926161,
-40.2296961597013));
#263105=CARTESIAN_POINT('Ctrl Pts',(46.1928858033625,-57.5018627715142,
-40.234134296036));
#263106=CARTESIAN_POINT('Ctrl Pts',(46.1762417771239,-57.4364451908711,
-40.2388223154954));
#263107=CARTESIAN_POINT('Ctrl Pts',(43.4805771074156,-59.5712767529309,
-39.2399080357013));
#263108=CARTESIAN_POINT('Ctrl Pts',(43.4150727209207,-59.5358440364426,
-39.2223070534893));
#263109=CARTESIAN_POINT('Ctrl Pts',(43.2883193276586,-59.4590682572254,
-39.1867578392588));
#263110=CARTESIAN_POINT('Ctrl Pts',(43.1106712693135,-59.32658002426,-39.1324031814995));
#263111=CARTESIAN_POINT('Ctrl Pts',(43.0005921597408,-59.2266373021163,
-39.0954660506179));
#263112=CARTESIAN_POINT('Ctrl Pts',(42.8948534568781,-59.1207134074407,
-39.0581733199915));
#263113=CARTESIAN_POINT('Ctrl Pts',(42.7951360401793,-59.0104958554849,
-39.0211184761739));
#263114=CARTESIAN_POINT('Ctrl Pts',(42.6850011896347,-58.8622904152127,
-38.9753582681256));
#263115=CARTESIAN_POINT('Ctrl Pts',(42.6055727997797,-58.7375004045667,
-38.939089851323));
#263116=CARTESIAN_POINT('Ctrl Pts',(42.5503788594446,-58.6407591922129,
-38.9120596161462));
#263117=CARTESIAN_POINT('Ctrl Pts',(42.5165536369311,-58.5741539171446,
-38.8941613358138));
#263118=CARTESIAN_POINT('Ctrl Pts',(42.4842288567228,-58.5064298632496,
-38.8763157156907));
#263119=CARTESIAN_POINT('Ctrl Pts',(42.4689425396028,-58.4722695523732,
-38.8674882509199));
#263120=CARTESIAN_POINT('Ctrl Pts',(42.4257123024776,-58.3690064948315,
-38.8413136266604));
#263121=CARTESIAN_POINT('Ctrl Pts',(42.3750272156063,-58.229152189777,-38.8072100415055));
#263122=CARTESIAN_POINT('Ctrl Pts',(42.3380647902547,-58.0850119200902,
-38.7746901633276));
#263123=CARTESIAN_POINT('Ctrl Pts',(42.3155659796374,-57.9752818499468,
-38.7509105250088));
#263124=CARTESIAN_POINT('Ctrl Pts',(42.3089374211558,-57.9384266221928,
-38.7430843922672));
#263125=CARTESIAN_POINT('Ctrl Pts',(42.297458012674,-57.864178756387,-38.7276438637217));
#263126=CARTESIAN_POINT('Ctrl Pts',(42.292601515188,-57.8267325312259,-38.720018782004));
#263127=CARTESIAN_POINT('Ctrl Pts',(42.2847289916893,-57.7514526301959,
-38.7050196673963));
#263128=CARTESIAN_POINT('Ctrl Pts',(42.2817363521424,-57.7138759968928,
-38.6976962453237));
#263129=CARTESIAN_POINT('Ctrl Pts',(42.277596992864,-57.6387184974263,-38.6833720377019));
#263130=CARTESIAN_POINT('Ctrl Pts',(42.2741651307842,-57.5260409596698,
-38.6623829091612));
#263131=CARTESIAN_POINT('Ctrl Pts',(42.2805893100654,-57.3760354719141,
-38.6363740800325));
#263132=CARTESIAN_POINT('Ctrl Pts',(42.2937061680812,-57.2637038035873,
-38.618370061439));
#263133=CARTESIAN_POINT('Ctrl Pts',(42.3043247017591,-57.1888547452426,
-38.6067079534822));
#263134=CARTESIAN_POINT('Ctrl Pts',(42.3105743117123,-57.1514345461221,
-38.6010450635964));
#263135=CARTESIAN_POINT('Ctrl Pts',(42.3249704170347,-57.0766935209607,
-38.590076215021));
#263136=CARTESIAN_POINT('Ctrl Pts',(42.3331592025312,-57.0392159768686,
-38.5847494243559));
#263137=CARTESIAN_POINT('Ctrl Pts',(42.3512949844302,-56.9651221381903,
-38.5745673038812));
#263138=CARTESIAN_POINT('Ctrl Pts',(42.3712216906218,-56.8916587034686,
-38.564820665347));
#263139=CARTESIAN_POINT('Ctrl Pts',(42.4063979707918,-56.7834465224234,
-38.5515118436));
#263140=CARTESIAN_POINT('Ctrl Pts',(42.4468320479729,-56.6771725078319,
-38.5395042677724));
#263141=CARTESIAN_POINT('Ctrl Pts',(42.4925290654744,-56.5728473165674,
-38.5288039137004));
#263142=CARTESIAN_POINT('Ctrl Pts',(42.5265325119253,-56.5046058456765,
-38.5225509073062));
#263143=CARTESIAN_POINT('Ctrl Pts',(42.5623338475306,-56.4370293947697,
-38.5167461666044));
#263144=CARTESIAN_POINT('Ctrl Pts',(42.5811223641794,-56.4035923099625,
-38.5140693065785));
#263145=CARTESIAN_POINT('Ctrl Pts',(42.620584523009,-56.3373241998654,-38.5091697400817));
#263146=CARTESIAN_POINT('Ctrl Pts',(42.6411082254821,-56.3047465904101,
-38.5069659500128));
#263147=CARTESIAN_POINT('Ctrl Pts',(42.7048067991197,-56.2090283357163,
-38.501110858935));
#263148=CARTESIAN_POINT('Ctrl Pts',(42.7502234543428,-56.1476408662828,
-38.4981890389281));
#263149=CARTESIAN_POINT('Ctrl Pts',(42.8467942323831,-56.0297655581676,
-38.4942910511033));
#263150=CARTESIAN_POINT('Ctrl Pts',(42.8979715413934,-55.9732420482176,
-38.4933125989996));
#263151=CARTESIAN_POINT('Ctrl Pts',(42.9790570553347,-55.8921695883033,
-38.4933149859729));
#263152=CARTESIAN_POINT('Ctrl Pts',(43.0068374106561,-55.8657400908868,
-38.4935622007431));
#263153=CARTESIAN_POINT('Ctrl Pts',(43.0495800649421,-55.8270637749536,
-38.4943063068789));
#263154=CARTESIAN_POINT('Ctrl Pts',(43.0640222060113,-55.8143203511958,
-38.494617152342));
#263155=CARTESIAN_POINT('Ctrl Pts',(43.0932714774893,-55.7891564261061,
-38.4953646906773));
#263156=CARTESIAN_POINT('Ctrl Pts',(43.1080901283632,-55.7767277938553,
-38.4958020036096));
#263157=CARTESIAN_POINT('Ctrl Pts',(43.1528523310046,-55.7401327167866,
-38.4972962980169));
#263158=CARTESIAN_POINT('Ctrl Pts',(43.2134913856688,-55.6930468850421,
-38.4997758707861));
#263159=CARTESIAN_POINT('Ctrl Pts',(43.3385569247743,-55.6055389451161,
-38.5066450244003));
#263160=CARTESIAN_POINT('Ctrl Pts',(43.4691986576013,-55.5278792007279,
-38.5163302992824));
#263161=CARTESIAN_POINT('Ctrl Pts',(43.5713395927684,-55.4769743237494,
-38.5256877381308));
#263162=CARTESIAN_POINT('Ctrl Pts',(43.6403672861995,-55.4446857735354,
-38.5323951500278));
#263163=CARTESIAN_POINT('Ctrl Pts',(43.6753577685123,-55.4293620157832,
-38.5359845633874));
#263164=CARTESIAN_POINT('Ctrl Pts',(43.7462462065788,-55.4003985583156,
-38.5436333065981));
#263165=CARTESIAN_POINT('Ctrl Pts',(43.7822717759725,-55.3867204456352,
-38.5477088862383));
#263166=CARTESIAN_POINT('Ctrl Pts',(43.8543821738219,-55.3613797848081,
-38.5562346427694));
#263167=CARTESIAN_POINT('Ctrl Pts',(43.890622407919,-55.349649082917,-38.5607007444526));
#263168=CARTESIAN_POINT('Ctrl Pts',(43.9997560709039,-55.3172704656441,
-38.5746802407103));
#263169=CARTESIAN_POINT('Ctrl Pts',(44.1098017310836,-55.290468361793,-38.5898286859852));
#263170=CARTESIAN_POINT('Ctrl Pts',(44.2583166685835,-55.2656490138239,
-38.612301023075));
#263171=CARTESIAN_POINT('Ctrl Pts',(44.3705972700495,-55.2524997368729,
-38.6302900391873));
#263172=CARTESIAN_POINT('Ctrl Pts',(44.446056048267,-55.2474029004138,-38.6430428201589));
#263173=CARTESIAN_POINT('Ctrl Pts',(44.5218128020516,-55.2441636366351,
-38.65617756452));
#263174=CARTESIAN_POINT('Ctrl Pts',(44.5599089424743,-55.2434808562086,
-38.6629497802385));
#263175=CARTESIAN_POINT('Ctrl Pts',(44.6354869543582,-55.2439911084578,
-38.6767130108817));
#263176=CARTESIAN_POINT('Ctrl Pts',(44.6731456892459,-55.2451740103824,
-38.6837342374529));
#263177=CARTESIAN_POINT('Ctrl Pts',(44.7481014788608,-55.2493620066237,
-38.6980304684339));
#263178=CARTESIAN_POINT('Ctrl Pts',(44.860046548974,-55.2583760573225,-38.7198650218829));
#263179=CARTESIAN_POINT('Ctrl Pts',(45.0073845433675,-55.2811507310277,
-38.7505067688753));
#263180=CARTESIAN_POINT('Ctrl Pts',(45.1528189888476,-55.3146135839333,
-38.7826550300594));
#263181=CARTESIAN_POINT('Ctrl Pts',(45.2248832056965,-55.3349380951144,
-38.7992310848652));
#263182=CARTESIAN_POINT('Ctrl Pts',(45.2966462681613,-55.3570913336823,
-38.8160672125853));
#263183=CARTESIAN_POINT('Ctrl Pts',(45.3323638946335,-55.3690863290504,
-38.8246135819642));
#263184=CARTESIAN_POINT('Ctrl Pts',(45.4027951436545,-55.3946744461232,
-38.841798196801));
#263185=CARTESIAN_POINT('Ctrl Pts',(45.4376370321487,-55.4083060218429,
-38.85046633842));
#263186=CARTESIAN_POINT('Ctrl Pts',(45.5409345111852,-55.4516493275196,
-38.8766665754573));
#263187=CARTESIAN_POINT('Ctrl Pts',(45.6082182891413,-55.4838201174091,
-38.8944064774514));
#263188=CARTESIAN_POINT('Ctrl Pts',(45.7067749877369,-55.5369855856676,
-38.9214216121435));
#263189=CARTESIAN_POINT('Ctrl Pts',(45.7392219877795,-55.5555212114618,
-38.9304915704334));
#263190=CARTESIAN_POINT('Ctrl Pts',(45.8033556832395,-55.5942722159849,
-38.9487787872477));
#263191=CARTESIAN_POINT('Ctrl Pts',(45.8348443691401,-55.6143675312756,
-38.9579395118015));
#263192=CARTESIAN_POINT('Ctrl Pts',(45.9274099842789,-55.6766589025306,
-38.9854159162723));
#263193=CARTESIAN_POINT('Ctrl Pts',(45.9867610865919,-55.7209353156014,
-39.0037703637879));
#263194=CARTESIAN_POINT('Ctrl Pts',(46.1007337830098,-55.8148102393793,
-39.0405190865864));
#263195=CARTESIAN_POINT('Ctrl Pts',(46.1826971388658,-55.889219933262,-39.0681181728269));
#263196=CARTESIAN_POINT('Ctrl Pts',(46.259356574729,-55.9696687352924,-39.0957737179551));
#263197=CARTESIAN_POINT('Ctrl Pts',(46.309266807939,-56.024663053365,-39.1142236413887));
#263198=CARTESIAN_POINT('Ctrl Pts',(46.3336138177017,-56.0528284109483,
-39.1234510495426));
#263199=CARTESIAN_POINT('Ctrl Pts',(46.3692509284248,-56.0961546965833,
-39.1373141736981));
#263200=CARTESIAN_POINT('Ctrl Pts',(46.3809719555493,-56.1107655250657,
-39.14193505412));
#263201=CARTESIAN_POINT('Ctrl Pts',(46.4039850968433,-56.1401806715041,
-39.1511314768264));
#263202=CARTESIAN_POINT('Ctrl Pts',(46.4153001903629,-56.1550126624776,
-39.1557159133813));
#263203=CARTESIAN_POINT('Ctrl Pts',(46.4486370096885,-56.1998310060263,
-39.1694131182659));
#263204=CARTESIAN_POINT('Ctrl Pts',(46.4700835091466,-56.2301795317326,
-39.1784826054425));
#263205=CARTESIAN_POINT('Ctrl Pts',(46.532071913686,-56.3225583984772,-39.2054898733524));
#263206=CARTESIAN_POINT('Ctrl Pts',(46.5894197348374,-56.4176636744323,
-39.23211607576));
#263207=CARTESIAN_POINT('Ctrl Pts',(46.6566074362748,-56.5498680842415,
-39.2668544229849));
#263208=CARTESIAN_POINT('Ctrl Pts',(46.6870820302515,-56.617790568625,-39.2839693714534));
#263209=CARTESIAN_POINT('Ctrl Pts',(46.7159729830272,-56.6866360545619,
-39.3009558869148));
#263210=CARTESIAN_POINT('Ctrl Pts',(46.7296188023799,-56.7214992889704,
-39.3093799218186));
#263211=CARTESIAN_POINT('Ctrl Pts',(46.7553216997643,-56.7922546384013,
-39.3261176641085));
#263212=CARTESIAN_POINT('Ctrl Pts',(46.7672996943011,-56.8279354881579,
-39.3343809787628));
#263213=CARTESIAN_POINT('Ctrl Pts',(46.8004530502947,-56.9353633959568,
-39.358737163018));
#263214=CARTESIAN_POINT('Ctrl Pts',(46.8189795501832,-57.0077635587999,
-39.3744658121213));
#263215=CARTESIAN_POINT('Ctrl Pts',(46.848916211803,-57.1540080946302,-39.4048998290393));
#263216=CARTESIAN_POINT('Ctrl Pts',(46.866048617508,-57.2647966217996,-39.4269646939479));
#263217=CARTESIAN_POINT('Ctrl Pts',(46.875074749658,-57.3772756893033,-39.4478819384746));
#263218=CARTESIAN_POINT('Ctrl Pts',(46.8792542953452,-57.4526370309597,
-39.4615663943076));
#263219=CARTESIAN_POINT('Ctrl Pts',(46.8804258736835,-57.4905390832845,
-39.4682843608713));
#263220=CARTESIAN_POINT('Ctrl Pts',(46.8808837743635,-57.566610437341,-39.4814341960201));
#263221=CARTESIAN_POINT('Ctrl Pts',(46.8801708637706,-57.604491394965,-39.4878166677226));
#263222=CARTESIAN_POINT('Ctrl Pts',(46.8768913879562,-57.6800597985945,
-39.5002231148134));
#263223=CARTESIAN_POINT('Ctrl Pts',(46.8691896925243,-57.7930657109158,
-39.5182849936093));
#263224=CARTESIAN_POINT('Ctrl Pts',(46.8479069711518,-57.9423669591112,
-39.540205996752));
#263225=CARTESIAN_POINT('Ctrl Pts',(46.8236459543104,-58.053306681129,-39.5550278422771));
#263226=CARTESIAN_POINT('Ctrl Pts',(46.8055990109883,-58.1270324939452,
-39.5645447403379));
#263227=CARTESIAN_POINT('Ctrl Pts',(46.7956339676918,-58.1637938532181,
-39.5691227921436));
#263228=CARTESIAN_POINT('Ctrl Pts',(46.7738161327052,-58.2370162077019,
-39.5779016468881));
#263229=CARTESIAN_POINT('Ctrl Pts',(46.7619036278491,-58.2736352268715,
-39.5821192203466));
#263230=CARTESIAN_POINT('Ctrl Pts',(46.7364059718256,-58.3458255995332,
-39.5900871854462));
#263231=CARTESIAN_POINT('Ctrl Pts',(46.7091836493705,-58.4171862986019,
-39.5976163356366));
#263232=CARTESIAN_POINT('Ctrl Pts',(46.663274408039,-58.5216699086648,-39.6076014242402));
#263233=CARTESIAN_POINT('Ctrl Pts',(46.6123207377325,-58.6236436013082,
-39.616293729045));
#263234=CARTESIAN_POINT('Ctrl Pts',(46.5563244858032,-58.7230996041114,
-39.6236943138341));
#263235=CARTESIAN_POINT('Ctrl Pts',(46.515607032986,-58.7877140896312,-39.6277619492082));
#263236=CARTESIAN_POINT('Ctrl Pts',(46.4731710833873,-58.8514710047945,
-39.6313905635194));
#263237=CARTESIAN_POINT('Ctrl Pts',(46.4511086137465,-58.8829006319494,
-39.6329844599904));
#263238=CARTESIAN_POINT('Ctrl Pts',(46.4051673201274,-58.9449633016888,
-39.6357273485653));
#263239=CARTESIAN_POINT('Ctrl Pts',(46.381447994276,-58.975377588932,-39.6368662598532));
#263240=CARTESIAN_POINT('Ctrl Pts',(46.3084068909562,-59.0643493136614,
-39.6395761233691));
#263241=CARTESIAN_POINT('Ctrl Pts',(46.2570407846102,-59.1209150453974,
-39.6404603784325));
#263242=CARTESIAN_POINT('Ctrl Pts',(46.1491379755941,-59.228544463199,-39.6404138814247));
#263243=CARTESIAN_POINT('Ctrl Pts',(46.0925836555155,-59.2796343044913,
-39.6394845811684));
#263244=CARTESIAN_POINT('Ctrl Pts',(46.0038529437629,-59.3521266125547,
-39.6367223387528));
#263245=CARTESIAN_POINT('Ctrl Pts',(45.9736068078661,-59.3756113554055,
-39.6355721163029));
#263246=CARTESIAN_POINT('Ctrl Pts',(45.9272656961273,-59.4097723546528,
-39.6334997725088));
#263247=CARTESIAN_POINT('Ctrl Pts',(45.9116419215573,-59.4209912820171,
-39.6327502808957));
#263248=CARTESIAN_POINT('Ctrl Pts',(45.8800804794677,-59.4430610802669,
-39.6311351339295));
#263249=CARTESIAN_POINT('Ctrl Pts',(45.8321587971618,-59.4756823489919,
-39.628531354857));
#263250=CARTESIAN_POINT('Ctrl Pts',(45.7834097108732,-59.5062438963941,
-39.6254355071979));
#263251=CARTESIAN_POINT('Ctrl Pts',(45.717633106262,-59.5452481912826,-39.6208773262667));
#263252=CARTESIAN_POINT('Ctrl Pts',(45.6178307490054,-59.601113548897,-39.6133952897297));
#263253=CARTESIAN_POINT('Ctrl Pts',(45.4802897643185,-59.6652183443042,
-39.6008811885904));
#263254=CARTESIAN_POINT('Ctrl Pts',(45.3738098009101,-59.7055766782111,
-39.5896017905935));
#263255=CARTESIAN_POINT('Ctrl Pts',(45.3020778813705,-59.7307512119865,
-39.5816566825671));
#263256=CARTESIAN_POINT('Ctrl Pts',(45.2658207311094,-59.7424779859237,
-39.5774690651077));
#263257=CARTESIAN_POINT('Ctrl Pts',(45.1926264675053,-59.7641596016776,
-39.5686715125846));
#263258=CARTESIAN_POINT('Ctrl Pts',(45.1555073907618,-59.7741562512684,
-39.5640376159893));
#263259=CARTESIAN_POINT('Ctrl Pts',(45.0441315765335,-59.8011904590316,
-39.5496210468413));
#263260=CARTESIAN_POINT('Ctrl Pts',(44.9324484012679,-59.8224577850013,
-39.5341534065747));
#263261=CARTESIAN_POINT('Ctrl Pts',(44.8203079610257,-59.8353953605365,
-39.5171556909205));
#263262=CARTESIAN_POINT('Ctrl Pts',(44.7080184564226,-59.8455760612675,
-39.4996502778008));
#263263=CARTESIAN_POINT('Ctrl Pts',(44.6329372249224,-59.8486931621852,
-39.4873001861445));
#263264=CARTESIAN_POINT('Ctrl Pts',(44.5200834441659,-59.8478515133141,
-39.4677634802869));
#263265=CARTESIAN_POINT('Ctrl Pts',(44.4823810871712,-59.8466449718289,
-39.4610736497974));
#263266=CARTESIAN_POINT('Ctrl Pts',(44.4258051079382,-59.8434394706745,
-39.4507883432074));
#263267=CARTESIAN_POINT('Ctrl Pts',(44.4069254589855,-59.8421361346926,
-39.4473147915973));
#263268=CARTESIAN_POINT('Ctrl Pts',(44.3691376542581,-59.8390581625153,
-39.4402793331445));
#263269=CARTESIAN_POINT('Ctrl Pts',(44.3502459350849,-59.8372838734483,
-39.4367203104461));
#263270=CARTESIAN_POINT('Ctrl Pts',(44.2562487381671,-59.8272835659938,
-39.4188041728073));
#263271=CARTESIAN_POINT('Ctrl Pts',(44.1080045765469,-59.8040393501646,
-39.3892226636159));
#263272=CARTESIAN_POINT('Ctrl Pts',(43.9639303529155,-59.7668593120831,
-39.3578670379715));
#263273=CARTESIAN_POINT('Ctrl Pts',(43.8219159040518,-59.7227861654643,
-39.3256251231267));
#263274=CARTESIAN_POINT('Ctrl Pts',(43.7519290534068,-59.6972943066161,
-39.3090578287531));
#263275=CARTESIAN_POINT('Ctrl Pts',(43.665783177736,-59.6610675807531,-39.2877890488175));
#263276=CARTESIAN_POINT('Ctrl Pts',(43.6486106666635,-59.653596197985,-39.2835041280971));
#263277=CARTESIAN_POINT('Ctrl Pts',(43.6144193015916,-59.6382222359849,
-39.2748825183767));
#263278=CARTESIAN_POINT('Ctrl Pts',(43.597366582891,-59.6303022352814,-39.2705368924251));
#263279=CARTESIAN_POINT('Ctrl Pts',(43.5465994182959,-59.605961903298,-39.2574616452183));
#263280=CARTESIAN_POINT('Ctrl Pts',(43.513329300663,-59.588993111175,-39.2487085268073));
#263281=CARTESIAN_POINT('Ctrl Pts',(43.4805771074156,-59.5712767529309,
-39.2399080357013));
#263282=CARTESIAN_POINT('Ctrl Pts',(43.8903154257419,-57.7291941381088,
-41.4266127101804));
#263283=CARTESIAN_POINT('Ctrl Pts',(43.8716814361492,-57.7189244770852,
-41.4090117279687));
#263284=CARTESIAN_POINT('Ctrl Pts',(43.8355945080866,-57.6967277837834,
-41.3734625137379));
#263285=CARTESIAN_POINT('Ctrl Pts',(43.7849271573585,-57.6585752750105,
-41.3191078559793));
#263286=CARTESIAN_POINT('Ctrl Pts',(43.753465403225,-57.62988352171,-41.2821707250961));
#263287=CARTESIAN_POINT('Ctrl Pts',(43.7232071092872,-57.5995155202448,
-41.2448779944712));
#263288=CARTESIAN_POINT('Ctrl Pts',(43.694633283399,-57.5679550683129,-41.2078231506529));
#263289=CARTESIAN_POINT('Ctrl Pts',(43.6629744005209,-57.5256074013359,
-41.162062942605));
#263290=CARTESIAN_POINT('Ctrl Pts',(43.6400741040405,-57.4900012877665,
-41.1257945258022));
#263291=CARTESIAN_POINT('Ctrl Pts',(43.624122646482,-57.4624228770549,-41.0987642906252));
#263292=CARTESIAN_POINT('Ctrl Pts',(43.6143188854815,-57.4434516436916,
-41.0808660102928));
#263293=CARTESIAN_POINT('Ctrl Pts',(43.6049343759216,-57.4241698350281,
-41.0630203901697));
#263294=CARTESIAN_POINT('Ctrl Pts',(43.6004882740613,-57.4144479878336,
-41.054192925399));
#263295=CARTESIAN_POINT('Ctrl Pts',(43.5878889573419,-57.3850715912746,
-41.0280183011396));
#263296=CARTESIAN_POINT('Ctrl Pts',(43.5730447416356,-57.3453166524842,
-40.9939147159844));
#263297=CARTESIAN_POINT('Ctrl Pts',(43.5620571572655,-57.3044044614592,
-40.9613948378065));
#263298=CARTESIAN_POINT('Ctrl Pts',(43.5552843243605,-57.2732819874194,
-40.9376151994878));
#263299=CARTESIAN_POINT('Ctrl Pts',(43.5532714802541,-57.2628325912303,
-40.9297890667463));
#263300=CARTESIAN_POINT('Ctrl Pts',(43.5497454556161,-57.2417890776549,
-40.9143485382007));
#263301=CARTESIAN_POINT('Ctrl Pts',(43.5482304746054,-57.2311797832666,
-40.9067234564832));
#263302=CARTESIAN_POINT('Ctrl Pts',(43.5457184756399,-57.2098591834555,
-40.8917243418755));
#263303=CARTESIAN_POINT('Ctrl Pts',(43.5447290487245,-57.199220662917,-40.8844009198028));
#263304=CARTESIAN_POINT('Ctrl Pts',(43.5432711863927,-57.1779500447907,
-40.8700767121812));
#263305=CARTESIAN_POINT('Ctrl Pts',(43.5418684734652,-57.1460721839032,
-40.8490875836402));
#263306=CARTESIAN_POINT('Ctrl Pts',(43.5431039253892,-57.1036793909824,
-40.8230787545116));
#263307=CARTESIAN_POINT('Ctrl Pts',(43.5463738329101,-57.0719682486671,
-40.8050747359183));
#263308=CARTESIAN_POINT('Ctrl Pts',(43.5490829635055,-57.0508462881094,
-40.7934126279614));
#263309=CARTESIAN_POINT('Ctrl Pts',(43.5507030159248,-57.0402904723448,
-40.7877497380755));
#263310=CARTESIAN_POINT('Ctrl Pts',(43.5544790630841,-57.019214904491,-40.7767808895002));
#263311=CARTESIAN_POINT('Ctrl Pts',(43.5566463931059,-57.0086510117152,
-40.7714540988351));
#263312=CARTESIAN_POINT('Ctrl Pts',(43.5614808344627,-56.9877741662596,
-40.7612719783604));
#263313=CARTESIAN_POINT('Ctrl Pts',(43.5668234022498,-56.9670831174431,
-40.7515253398262));
#263314=CARTESIAN_POINT('Ctrl Pts',(43.5763377125496,-56.9366295208774,
-40.7382165180791));
#263315=CARTESIAN_POINT('Ctrl Pts',(43.5873444561754,-56.9067460923864,
-40.7262089422516));
#263316=CARTESIAN_POINT('Ctrl Pts',(43.5998453117462,-56.8774358278222,
-40.7155085881795));
#263317=CARTESIAN_POINT('Ctrl Pts',(43.6091839698139,-56.8582805167828,
-40.7092555817853));
#263318=CARTESIAN_POINT('Ctrl Pts',(43.6190331668358,-56.8393207538612,
-40.7034508410834));
#263319=CARTESIAN_POINT('Ctrl Pts',(43.6242099732076,-56.8299438685379,
-40.7007739810578));
#263320=CARTESIAN_POINT('Ctrl Pts',(43.6350986096338,-56.8113693026126,
-40.6958744145609));
#263321=CARTESIAN_POINT('Ctrl Pts',(43.6407690742328,-56.8022426567881,
-40.6936706244929));
#263322=CARTESIAN_POINT('Ctrl Pts',(43.6583896223854,-56.7754411523649,
-40.6878155334118));
#263323=CARTESIAN_POINT('Ctrl Pts',(43.6709801307092,-56.7582712890167,
-40.6848937134075));
#263324=CARTESIAN_POINT('Ctrl Pts',(43.6978023804218,-56.725340315416,-40.6809957255822));
#263325=CARTESIAN_POINT('Ctrl Pts',(43.7120405319879,-56.7095692151415,
-40.6800172734785));
#263326=CARTESIAN_POINT('Ctrl Pts',(43.7346338722206,-56.6869796178674,
-40.680019660452));
#263327=CARTESIAN_POINT('Ctrl Pts',(43.7423799312797,-56.6796208977126,
-40.6802668752224));
#263328=CARTESIAN_POINT('Ctrl Pts',(43.7543060585229,-56.6688607312791,
-40.681010981358));
#263329=CARTESIAN_POINT('Ctrl Pts',(43.7583370517177,-56.6653168192219,
-40.6813218268212));
#263330=CARTESIAN_POINT('Ctrl Pts',(43.7665035456834,-56.6583217341419,
-40.6820693651562));
#263331=CARTESIAN_POINT('Ctrl Pts',(43.7706422703,-56.6548683091639,-40.6825066780886));
#263332=CARTESIAN_POINT('Ctrl Pts',(43.7831478581881,-56.6447045100584,
-40.6840009724959));
#263333=CARTESIAN_POINT('Ctrl Pts',(43.8000992888712,-56.6316392340345,
-40.6864805452653));
#263334=CARTESIAN_POINT('Ctrl Pts',(43.8351004518507,-56.6074069729907,
-40.6933496988796));
#263335=CARTESIAN_POINT('Ctrl Pts',(43.8717190640765,-56.5859796680779,
-40.7030349737613));
#263336=CARTESIAN_POINT('Ctrl Pts',(43.9003898794618,-56.5719991465823,
-40.7123924126099));
#263337=CARTESIAN_POINT('Ctrl Pts',(43.919774692733,-56.5631479893168,-40.719099824507));
#263338=CARTESIAN_POINT('Ctrl Pts',(43.9296053152689,-56.5589560552736,
-40.722689237866));
#263339=CARTESIAN_POINT('Ctrl Pts',(43.9495302416178,-56.551051384942,-40.7303379810773));
#263340=CARTESIAN_POINT('Ctrl Pts',(43.959660471973,-56.5473282955902,-40.7344135607172));
#263341=CARTESIAN_POINT('Ctrl Pts',(43.9799461530017,-56.5404515818703,
-40.7429393172485));
#263342=CARTESIAN_POINT('Ctrl Pts',(43.9901452646573,-56.5372793127045,
-40.7474054189318));
#263343=CARTESIAN_POINT('Ctrl Pts',(44.0208712025373,-56.5285586047056,
-40.7613849151889));
#263344=CARTESIAN_POINT('Ctrl Pts',(44.0518784813599,-56.521416173947,-40.7765333604643));
#263345=CARTESIAN_POINT('Ctrl Pts',(44.0937728041468,-56.5149820273198,
-40.799005697554));
#263346=CARTESIAN_POINT('Ctrl Pts',(44.1254693703652,-56.5117027703592,
-40.8169947136667));
#263347=CARTESIAN_POINT('Ctrl Pts',(44.1467868482481,-56.5105547568045,
-40.8297474946377));
#263348=CARTESIAN_POINT('Ctrl Pts',(44.1681963264173,-56.50993223545,-40.842882238999));
#263349=CARTESIAN_POINT('Ctrl Pts',(44.1789665479467,-56.509886262238,-40.8496544547178));
#263350=CARTESIAN_POINT('Ctrl Pts',(44.2003410646824,-56.5103214152413,
-40.8634176853611));
#263351=CARTESIAN_POINT('Ctrl Pts',(44.2109953322312,-56.5108003631786,
-40.8704389119319));
#263352=CARTESIAN_POINT('Ctrl Pts',(44.2322091102727,-56.5122711761573,
-40.8847351429132));
#263353=CARTESIAN_POINT('Ctrl Pts',(44.2639028799147,-56.5152466319394,
-40.9065696963621));
#263354=CARTESIAN_POINT('Ctrl Pts',(44.305661850593,-56.5222422564611,-40.9372114433545));
#263355=CARTESIAN_POINT('Ctrl Pts',(44.346925841944,-56.532247127269,-40.9693597045385));
#263356=CARTESIAN_POINT('Ctrl Pts',(44.3673876336497,-56.53826115526,-40.9859357593442));
#263357=CARTESIAN_POINT('Ctrl Pts',(44.3877715667723,-56.5447901720246,
-41.0027718870644));
#263358=CARTESIAN_POINT('Ctrl Pts',(44.3979208506631,-56.5483132560745,
-41.0113182564434));
#263359=CARTESIAN_POINT('Ctrl Pts',(44.4179418071922,-56.5558066378292,
-41.02850287128));
#263360=CARTESIAN_POINT('Ctrl Pts',(44.4278499085732,-56.5597882829787,
-41.0371710128992));
#263361=CARTESIAN_POINT('Ctrl Pts',(44.4572364860018,-56.5724196473794,
-41.0633712499365));
#263362=CARTESIAN_POINT('Ctrl Pts',(44.4763932211824,-56.581758968269,-41.0811111519311));
#263363=CARTESIAN_POINT('Ctrl Pts',(44.5044772880921,-56.5971447477014,
-41.1081262866225));
#263364=CARTESIAN_POINT('Ctrl Pts',(44.5137271775895,-56.6025015227711,
-41.1171962449124));
#263365=CARTESIAN_POINT('Ctrl Pts',(44.5320183562985,-56.6136863880645,
-41.1354834617267));
#263366=CARTESIAN_POINT('Ctrl Pts',(44.5410031705763,-56.6194798267371,
-41.144644186283));
#263367=CARTESIAN_POINT('Ctrl Pts',(44.5674276642847,-56.6374191091633,
-41.1721205907467));
#263368=CARTESIAN_POINT('Ctrl Pts',(44.5843870769067,-56.6501457393646,
-41.1904750382678));
#263369=CARTESIAN_POINT('Ctrl Pts',(44.616987890196,-56.6770839740703,-41.2272237610649));
#263370=CARTESIAN_POINT('Ctrl Pts',(44.640458797708,-56.6984048650555,-41.2548228473058));
#263371=CARTESIAN_POINT('Ctrl Pts',(44.6624514458289,-56.7214114906953,
-41.2824783924342));
#263372=CARTESIAN_POINT('Ctrl Pts',(44.6767798128067,-56.7371294193188,
-41.3009283158679));
#263373=CARTESIAN_POINT('Ctrl Pts',(44.683774397772,-56.7451748501741,-41.3101557240219));
#263374=CARTESIAN_POINT('Ctrl Pts',(44.6940202659092,-56.7575442973705,
-41.324018848177));
#263375=CARTESIAN_POINT('Ctrl Pts',(44.6973914635031,-56.7617145235639,
-41.328639728599));
#263376=CARTESIAN_POINT('Ctrl Pts',(44.7040131878578,-56.770108052971,-41.3378361513053));
#263377=CARTESIAN_POINT('Ctrl Pts',(44.7072703203268,-56.7743392575068,
-41.3424205878605));
#263378=CARTESIAN_POINT('Ctrl Pts',(44.7168707027477,-56.7871217033085,
-41.3561177927451));
#263379=CARTESIAN_POINT('Ctrl Pts',(44.7230524906066,-56.7957731420119,
-41.3651872799216));
#263380=CARTESIAN_POINT('Ctrl Pts',(44.7409373255192,-56.8220955492914,
-41.3921945478314));
#263381=CARTESIAN_POINT('Ctrl Pts',(44.7575187561203,-56.8491712652862,
-41.4188207502394));
#263382=CARTESIAN_POINT('Ctrl Pts',(44.7770214494108,-56.88676384976,-41.453559097464));
#263383=CARTESIAN_POINT('Ctrl Pts',(44.7858965000619,-56.9060633365117,
-41.4706740459328));
#263384=CARTESIAN_POINT('Ctrl Pts',(44.7943266372896,-56.9256180211132,
-41.4876605613939));
#263385=CARTESIAN_POINT('Ctrl Pts',(44.7983169540911,-56.9355169983302,
-41.4960845962979));
#263386=CARTESIAN_POINT('Ctrl Pts',(44.8058516078422,-56.9556000996462,
-41.5128223385875));
#263387=CARTESIAN_POINT('Ctrl Pts',(44.8093727854448,-56.9657242505397,
-41.5210856532432));
#263388=CARTESIAN_POINT('Ctrl Pts',(44.8191505788346,-56.9961959016236,
-41.5454418374945));
#263389=CARTESIAN_POINT('Ctrl Pts',(44.8246597322132,-57.0167187198372,
-41.5611704866007));
#263390=CARTESIAN_POINT('Ctrl Pts',(44.8336688220904,-57.0581479791523,
-41.5916045035181));
#263391=CARTESIAN_POINT('Ctrl Pts',(44.8389236650083,-57.0895139074259,
-41.613669368427));
#263392=CARTESIAN_POINT('Ctrl Pts',(44.8418900765893,-57.1213299669285,
-41.6345866129535));
#263393=CARTESIAN_POINT('Ctrl Pts',(44.8433488372948,-57.142640498193,-41.6482710687869));
#263394=CARTESIAN_POINT('Ctrl Pts',(44.8438191277705,-57.1533552116615,
-41.6549890353504));
#263395=CARTESIAN_POINT('Ctrl Pts',(44.8442270800594,-57.1748537940466,
-41.6681388704993));
#263396=CARTESIAN_POINT('Ctrl Pts',(44.8441639040618,-57.1855561823783,
-41.6745213422017));
#263397=CARTESIAN_POINT('Ctrl Pts',(44.8435122114514,-57.2069000331791,
-41.6869277892926));
#263398=CARTESIAN_POINT('Ctrl Pts',(44.8417458896958,-57.2388084678274,
-41.7049896680882));
#263399=CARTESIAN_POINT('Ctrl Pts',(44.8362687719071,-57.2809279665006,
-41.7269106712316));
#263400=CARTESIAN_POINT('Ctrl Pts',(44.8298088085522,-57.3121969378441,
-41.7417325167562));
#263401=CARTESIAN_POINT('Ctrl Pts',(44.8249713776488,-57.3329705079708,
-41.751249414817));
#263402=CARTESIAN_POINT('Ctrl Pts',(44.8222858794974,-57.3433254378487,
-41.7558274666229));
#263403=CARTESIAN_POINT('Ctrl Pts',(44.8163797073795,-57.3639440769784,
-41.7646063213672));
#263404=CARTESIAN_POINT('Ctrl Pts',(44.8131427147447,-57.3742522416544,
-41.7688238948253));
#263405=CARTESIAN_POINT('Ctrl Pts',(44.8061917406462,-57.3945668799698,
-41.7767918599254));
#263406=CARTESIAN_POINT('Ctrl Pts',(44.7987498536529,-57.4146412549335,
-41.7843210101159));
#263407=CARTESIAN_POINT('Ctrl Pts',(44.7861419817956,-57.4440129710611,
-41.7943060987191));
#263408=CARTESIAN_POINT('Ctrl Pts',(44.7720982599006,-57.4726583092559,
-41.8029984035242));
#263409=CARTESIAN_POINT('Ctrl Pts',(44.7566193423106,-57.5005749992605,
-41.8103989883131));
#263410=CARTESIAN_POINT('Ctrl Pts',(44.7453362941317,-57.518697088903,-41.8144666236875));
#263411=CARTESIAN_POINT('Ctrl Pts',(44.7335642473644,-57.5365709174371,
-41.8180952379985));
#263412=CARTESIAN_POINT('Ctrl Pts',(44.7274378249752,-57.5453780864623,
-41.8196891344695));
#263413=CARTESIAN_POINT('Ctrl Pts',(44.7146685840676,-57.5627610237142,
-41.8224320230444));
#263414=CARTESIAN_POINT('Ctrl Pts',(44.7080700862024,-57.5712755128024,
-41.8235709343319));
#263415=CARTESIAN_POINT('Ctrl Pts',(44.6877341610586,-57.5961705213949,
-41.8262807978491));
#263416=CARTESIAN_POINT('Ctrl Pts',(44.6734117165454,-57.6119810052107,
-41.8271650529119));
#263417=CARTESIAN_POINT('Ctrl Pts',(44.6432859415473,-57.6420285404153,
-41.827118555904));
#263418=CARTESIAN_POINT('Ctrl Pts',(44.6274777219699,-57.6562729242579,
-41.8261892556471));
#263419=CARTESIAN_POINT('Ctrl Pts',(44.6026489360012,-57.6764545436153,
-41.823427013232));
#263420=CARTESIAN_POINT('Ctrl Pts',(44.5941811636919,-57.6829873126311,
-41.8222767907821));
#263421=CARTESIAN_POINT('Ctrl Pts',(44.5812011369499,-57.6924815728277,
-41.820204446988));
#263422=CARTESIAN_POINT('Ctrl Pts',(44.5768239301145,-57.6955981764101,
-41.8194549553751));
#263423=CARTESIAN_POINT('Ctrl Pts',(44.5679795363474,-57.7017261947271,
-41.8178398084084));
#263424=CARTESIAN_POINT('Ctrl Pts',(44.554547495243,-57.7107794649358,-41.8152360293365));
#263425=CARTESIAN_POINT('Ctrl Pts',(44.5408745509057,-57.7192473537464,
-41.812140181677));
#263426=CARTESIAN_POINT('Ctrl Pts',(44.5224181841827,-57.7300417662926,
-41.8075820007456));
#263427=CARTESIAN_POINT('Ctrl Pts',(44.494403164631,-57.7454824222945,-41.8000999642091));
#263428=CARTESIAN_POINT('Ctrl Pts',(44.4557509611988,-57.7631175354143,
-41.7875858630695));
#263429=CARTESIAN_POINT('Ctrl Pts',(44.4257963579031,-57.7741479888816,
-41.7763064650726));
#263430=CARTESIAN_POINT('Ctrl Pts',(44.4056101875344,-57.781009218212,-41.7683613570464));
#263431=CARTESIAN_POINT('Ctrl Pts',(44.3954036594654,-57.7841949818065,
-41.7641737395871));
#263432=CARTESIAN_POINT('Ctrl Pts',(44.3747925009816,-57.7900627169564,
-41.7553761870634));
#263433=CARTESIAN_POINT('Ctrl Pts',(44.3643365899562,-57.7927558542442,
-41.7507422904685));
#263434=CARTESIAN_POINT('Ctrl Pts',(44.3329536886806,-57.7999988857253,
-41.7363257213199));
#263435=CARTESIAN_POINT('Ctrl Pts',(44.3014645871824,-57.8056090798854,
-41.7208580810542));
#263436=CARTESIAN_POINT('Ctrl Pts',(44.2698183189435,-57.8088603667088,
-41.7038603653999));
#263437=CARTESIAN_POINT('Ctrl Pts',(44.2381206623806,-57.8113308880715,
-41.6863549522799));
#263438=CARTESIAN_POINT('Ctrl Pts',(44.2169139506954,-57.8119384373532,
-41.6740048606234));
#263439=CARTESIAN_POINT('Ctrl Pts',(44.1850197107514,-57.811287280344,-41.6544681547659));
#263440=CARTESIAN_POINT('Ctrl Pts',(44.1743613109546,-57.8108078241776,
-41.6477783242763));
#263441=CARTESIAN_POINT('Ctrl Pts',(44.1583626375358,-57.8096935003687,
-41.6374930176863));
#263442=CARTESIAN_POINT('Ctrl Pts',(44.1530230189312,-57.809255510817,-41.6340194660765));
#263443=CARTESIAN_POINT('Ctrl Pts',(44.1423341247923,-57.8082460206643,
-41.6269840076234));
#263444=CARTESIAN_POINT('Ctrl Pts',(44.1369894952372,-57.8076746784434,
-41.6234249849254));
#263445=CARTESIAN_POINT('Ctrl Pts',(44.1103928894951,-57.8045001122898,
-41.6055088472864));
#263446=CARTESIAN_POINT('Ctrl Pts',(44.0684216046586,-57.7973782151022,
-41.5759273380954));
#263447=CARTESIAN_POINT('Ctrl Pts',(44.0275807082801,-57.78632659952,-41.5445717124501));
#263448=CARTESIAN_POINT('Ctrl Pts',(43.9872978152183,-57.7733311875938,
-41.5123297976061));
#263449=CARTESIAN_POINT('Ctrl Pts',(43.9674326520914,-57.7658590768128,
-41.4957625032292));
#263450=CARTESIAN_POINT('Ctrl Pts',(43.942963744406,-57.7552890823142,-41.4744937232973));
#263451=CARTESIAN_POINT('Ctrl Pts',(43.938085174092,-57.7531113051098,-41.4702088025761));
#263452=CARTESIAN_POINT('Ctrl Pts',(43.9283699185172,-57.7486342535987,
-41.4615871928557));
#263453=CARTESIAN_POINT('Ctrl Pts',(43.9235236029976,-57.7463299238453,
-41.4572415669043));
#263454=CARTESIAN_POINT('Ctrl Pts',(43.9090930604083,-57.739254093668,-41.4441663196977));
#263455=CARTESIAN_POINT('Ctrl Pts',(43.8996324205383,-57.7343289686206,
-41.4354132012863));
#263456=CARTESIAN_POINT('Ctrl Pts',(43.8903154257419,-57.7291941381088,
-41.4266127101804));
#263457=CARTESIAN_POINT('',(43.5555682511181,-59.2341350312479,-39.6401231904583));
#263458=CARTESIAN_POINT('',(43.6172881206076,-58.9566576914661,-39.9695117808943));
#263459=CARTESIAN_POINT('',(43.5555682511181,-59.2341350312479,-39.6401231904583));
#263460=CARTESIAN_POINT('Ctrl Pts',(43.5555682511181,-59.2341350312479,
-39.6401231904583));
#263461=CARTESIAN_POINT('Ctrl Pts',(43.5840312864905,-59.2495486925951,
-39.6489236815643));
#263462=CARTESIAN_POINT('Ctrl Pts',(43.6129437448844,-59.2643132281768,
-39.6576767999753));
#263463=CARTESIAN_POINT('Ctrl Pts',(43.657060506721,-59.2854937757857,-39.6707520471821));
#263464=CARTESIAN_POINT('Ctrl Pts',(43.6718791845861,-59.2923859849247,
-39.6750976731336));
#263465=CARTESIAN_POINT('Ctrl Pts',(43.7015908821177,-59.3057655721158,
-39.6837192828541));
#263466=CARTESIAN_POINT('Ctrl Pts',(43.7165133310485,-59.3122681083841,
-39.6880042035746));
#263467=CARTESIAN_POINT('Ctrl Pts',(43.7913709620947,-59.3437990868819,
-39.7092729835095));
#263468=CARTESIAN_POINT('Ctrl Pts',(43.8521844391421,-59.3659929346427,
-39.7258402778837));
#263469=CARTESIAN_POINT('Ctrl Pts',(43.9755797709279,-59.4043781707975,
-39.7580821927283));
#263470=CARTESIAN_POINT('Ctrl Pts',(44.1007600202038,-59.4367761316392,
-39.7894378183729));
#263471=CARTESIAN_POINT('Ctrl Pts',(44.2295539029067,-59.457069607789,-39.8190193275642));
#263472=CARTESIAN_POINT('Ctrl Pts',(44.3112153059959,-59.4658206541325,
-39.8369354652031));
#263473=CARTESIAN_POINT('Ctrl Pts',(44.3276276091643,-59.4673747774113,
-39.8404944879015));
#263474=CARTESIAN_POINT('Ctrl Pts',(44.36045571594,-59.4700741717846,-39.8475299463542));
#263475=CARTESIAN_POINT('Ctrl Pts',(44.3768572408897,-59.4712191302958,
-39.8510034979643));
#263476=CARTESIAN_POINT('Ctrl Pts',(44.426006678754,-59.4740418999023,-39.8612888045543));
#263477=CARTESIAN_POINT('Ctrl Pts',(44.4587593954789,-59.4751153687477,
-39.8679786350438));
#263478=CARTESIAN_POINT('Ctrl Pts',(44.5567957957571,-59.4759221534093,
-39.8875153409015));
#263479=CARTESIAN_POINT('Ctrl Pts',(44.6220168026294,-59.4732643557565,
-39.8998654325577));
#263480=CARTESIAN_POINT('Ctrl Pts',(44.7195562226364,-59.4644947877976,
-39.9173708456776));
#263481=CARTESIAN_POINT('Ctrl Pts',(44.8169644551499,-59.4533300166017,
-39.9343685613317));
#263482=CARTESIAN_POINT('Ctrl Pts',(44.913970347279,-59.4349282908675,-39.9498362015981));
#263483=CARTESIAN_POINT('Ctrl Pts',(45.0107056952338,-59.411516304601,-39.9642527707462));
#263484=CARTESIAN_POINT('Ctrl Pts',(45.0429448249416,-59.4028563587456,
-39.9688866673415));
#263485=CARTESIAN_POINT('Ctrl Pts',(45.1065152212723,-59.3840690317117,
-39.9776842198647));
#263486=CARTESIAN_POINT('Ctrl Pts',(45.1380045334646,-59.373905450928,-39.9818718373241));
#263487=CARTESIAN_POINT('Ctrl Pts',(45.200302444735,-59.3520826555278,-39.9898169453504));
#263488=CARTESIAN_POINT('Ctrl Pts',(45.2833557066068,-59.320656673229,-39.9999472459813));
#263489=CARTESIAN_POINT('Ctrl Pts',(45.364075785606,-59.2838188850366,-40.0085499382911));
#263490=CARTESIAN_POINT('Ctrl Pts',(45.4139072224687,-59.2584967483865,
-40.0133526723911));
#263491=CARTESIAN_POINT('Ctrl Pts',(45.4139074558404,-59.258497391876,-40.0133531717389));
#263492=CARTESIAN_POINT('Ctrl Pts',(45.2555531699078,-59.3224601009847,
-40.0137109606119));
#263493=CARTESIAN_POINT('Ctrl Pts',(45.0886088759217,-59.362243913815,-40.0125039011494));
#263494=CARTESIAN_POINT('Ctrl Pts',(44.7703416864287,-59.3897953534914,
-40.007848919862));
#263495=CARTESIAN_POINT('Ctrl Pts',(44.6212948829819,-59.383482606722,-40.0047256760571));
#263496=CARTESIAN_POINT('Ctrl Pts',(44.3078241746654,-59.3300095393333,
-39.9965299346065));
#263497=CARTESIAN_POINT('Ctrl Pts',(44.1460848365945,-59.2776316689425,
-39.9912944612456));
#263498=CARTESIAN_POINT('Ctrl Pts',(43.8182442761428,-59.1175558791083,
-39.9789555992433));
#263499=CARTESIAN_POINT('Ctrl Pts',(43.6926832053086,-59.0208412827663,
-39.9730690294287));
#263500=CARTESIAN_POINT('Ctrl Pts',(43.6172881206077,-58.9566576914661,
-39.9695117808943));
#263501=CARTESIAN_POINT('Ctrl Pts',(43.4805771074156,-59.5712767529309,
-39.2399080357013));
#263502=CARTESIAN_POINT('Ctrl Pts',(43.4150727209207,-59.5358440364426,
-39.2223070534893));
#263503=CARTESIAN_POINT('Ctrl Pts',(43.2883193276586,-59.4590682572254,
-39.1867578392588));
#263504=CARTESIAN_POINT('Ctrl Pts',(43.1106712693135,-59.32658002426,-39.1324031814995));
#263505=CARTESIAN_POINT('Ctrl Pts',(43.0005921597408,-59.2266373021163,
-39.0954660506179));
#263506=CARTESIAN_POINT('Ctrl Pts',(42.8948534568781,-59.1207134074407,
-39.0581733199915));
#263507=CARTESIAN_POINT('Ctrl Pts',(42.7951360401793,-59.0104958554849,
-39.0211184761739));
#263508=CARTESIAN_POINT('Ctrl Pts',(42.6850011896347,-58.8622904152127,
-38.9753582681256));
#263509=CARTESIAN_POINT('Ctrl Pts',(42.6055727997797,-58.7375004045667,
-38.939089851323));
#263510=CARTESIAN_POINT('Ctrl Pts',(42.5503788594446,-58.6407591922129,
-38.9120596161462));
#263511=CARTESIAN_POINT('Ctrl Pts',(42.5165536369311,-58.5741539171446,
-38.8941613358138));
#263512=CARTESIAN_POINT('Ctrl Pts',(42.4842288567228,-58.5064298632496,
-38.8763157156907));
#263513=CARTESIAN_POINT('Ctrl Pts',(42.4689425396028,-58.4722695523732,
-38.8674882509199));
#263514=CARTESIAN_POINT('Ctrl Pts',(42.4257123024776,-58.3690064948315,
-38.8413136266604));
#263515=CARTESIAN_POINT('Ctrl Pts',(42.3750272156063,-58.229152189777,-38.8072100415055));
#263516=CARTESIAN_POINT('Ctrl Pts',(42.3380647902547,-58.0850119200902,
-38.7746901633276));
#263517=CARTESIAN_POINT('Ctrl Pts',(42.3155659796374,-57.9752818499468,
-38.7509105250088));
#263518=CARTESIAN_POINT('Ctrl Pts',(42.3089374211558,-57.9384266221928,
-38.7430843922672));
#263519=CARTESIAN_POINT('Ctrl Pts',(42.297458012674,-57.864178756387,-38.7276438637217));
#263520=CARTESIAN_POINT('Ctrl Pts',(42.292601515188,-57.8267325312259,-38.720018782004));
#263521=CARTESIAN_POINT('Ctrl Pts',(42.2847289916893,-57.7514526301959,
-38.7050196673963));
#263522=CARTESIAN_POINT('Ctrl Pts',(42.2817363521424,-57.7138759968928,
-38.6976962453237));
#263523=CARTESIAN_POINT('Ctrl Pts',(42.277596992864,-57.6387184974263,-38.6833720377019));
#263524=CARTESIAN_POINT('Ctrl Pts',(42.2741651307842,-57.5260409596698,
-38.6623829091612));
#263525=CARTESIAN_POINT('Ctrl Pts',(42.2805893100654,-57.3760354719141,
-38.6363740800325));
#263526=CARTESIAN_POINT('Ctrl Pts',(42.2937061680812,-57.2637038035873,
-38.618370061439));
#263527=CARTESIAN_POINT('Ctrl Pts',(42.3043247017591,-57.1888547452426,
-38.6067079534822));
#263528=CARTESIAN_POINT('Ctrl Pts',(42.3105743117123,-57.1514345461221,
-38.6010450635964));
#263529=CARTESIAN_POINT('Ctrl Pts',(42.3249704170347,-57.0766935209607,
-38.590076215021));
#263530=CARTESIAN_POINT('Ctrl Pts',(42.3331592025312,-57.0392159768686,
-38.5847494243559));
#263531=CARTESIAN_POINT('Ctrl Pts',(42.3512949844302,-56.9651221381903,
-38.5745673038812));
#263532=CARTESIAN_POINT('Ctrl Pts',(42.3712216906218,-56.8916587034686,
-38.564820665347));
#263533=CARTESIAN_POINT('Ctrl Pts',(42.4063979707918,-56.7834465224234,
-38.5515118436));
#263534=CARTESIAN_POINT('Ctrl Pts',(42.4468320479729,-56.6771725078319,
-38.5395042677724));
#263535=CARTESIAN_POINT('Ctrl Pts',(42.4925290654744,-56.5728473165674,
-38.5288039137004));
#263536=CARTESIAN_POINT('Ctrl Pts',(42.5265325119253,-56.5046058456765,
-38.5225509073062));
#263537=CARTESIAN_POINT('Ctrl Pts',(42.5623338475306,-56.4370293947697,
-38.5167461666044));
#263538=CARTESIAN_POINT('Ctrl Pts',(42.5811223641794,-56.4035923099625,
-38.5140693065785));
#263539=CARTESIAN_POINT('Ctrl Pts',(42.620584523009,-56.3373241998654,-38.5091697400817));
#263540=CARTESIAN_POINT('Ctrl Pts',(42.6411082254821,-56.3047465904101,
-38.5069659500128));
#263541=CARTESIAN_POINT('Ctrl Pts',(42.7048067991197,-56.2090283357163,
-38.501110858935));
#263542=CARTESIAN_POINT('Ctrl Pts',(42.7502234543428,-56.1476408662828,
-38.4981890389281));
#263543=CARTESIAN_POINT('Ctrl Pts',(42.8467942323831,-56.0297655581676,
-38.4942910511033));
#263544=CARTESIAN_POINT('Ctrl Pts',(42.8979715413934,-55.9732420482176,
-38.4933125989996));
#263545=CARTESIAN_POINT('Ctrl Pts',(42.9790570553347,-55.8921695883033,
-38.4933149859729));
#263546=CARTESIAN_POINT('Ctrl Pts',(43.0068374106561,-55.8657400908868,
-38.4935622007431));
#263547=CARTESIAN_POINT('Ctrl Pts',(43.0495800649421,-55.8270637749536,
-38.4943063068789));
#263548=CARTESIAN_POINT('Ctrl Pts',(43.0640222060113,-55.8143203511958,
-38.494617152342));
#263549=CARTESIAN_POINT('Ctrl Pts',(43.0932714774893,-55.7891564261061,
-38.4953646906773));
#263550=CARTESIAN_POINT('Ctrl Pts',(43.1080901283632,-55.7767277938553,
-38.4958020036096));
#263551=CARTESIAN_POINT('Ctrl Pts',(43.1528523310046,-55.7401327167866,
-38.4972962980169));
#263552=CARTESIAN_POINT('Ctrl Pts',(43.2134913856688,-55.6930468850421,
-38.4997758707861));
#263553=CARTESIAN_POINT('Ctrl Pts',(43.3385569247743,-55.6055389451161,
-38.5066450244003));
#263554=CARTESIAN_POINT('Ctrl Pts',(43.4691986576013,-55.5278792007279,
-38.5163302992824));
#263555=CARTESIAN_POINT('Ctrl Pts',(43.5713395927684,-55.4769743237494,
-38.5256877381308));
#263556=CARTESIAN_POINT('Ctrl Pts',(43.6403672861995,-55.4446857735354,
-38.5323951500278));
#263557=CARTESIAN_POINT('Ctrl Pts',(43.6753577685123,-55.4293620157832,
-38.5359845633874));
#263558=CARTESIAN_POINT('Ctrl Pts',(43.7462462065788,-55.4003985583156,
-38.5436333065981));
#263559=CARTESIAN_POINT('Ctrl Pts',(43.7822717759725,-55.3867204456352,
-38.5477088862383));
#263560=CARTESIAN_POINT('Ctrl Pts',(43.8543821738219,-55.3613797848081,
-38.5562346427694));
#263561=CARTESIAN_POINT('Ctrl Pts',(43.890622407919,-55.349649082917,-38.5607007444526));
#263562=CARTESIAN_POINT('Ctrl Pts',(43.9997560709039,-55.3172704656441,
-38.5746802407103));
#263563=CARTESIAN_POINT('Ctrl Pts',(44.1098017310836,-55.290468361793,-38.5898286859852));
#263564=CARTESIAN_POINT('Ctrl Pts',(44.2583166685835,-55.2656490138239,
-38.612301023075));
#263565=CARTESIAN_POINT('Ctrl Pts',(44.3705972700495,-55.2524997368729,
-38.6302900391873));
#263566=CARTESIAN_POINT('Ctrl Pts',(44.446056048267,-55.2474029004138,-38.6430428201589));
#263567=CARTESIAN_POINT('Ctrl Pts',(44.5218128020516,-55.2441636366351,
-38.65617756452));
#263568=CARTESIAN_POINT('Ctrl Pts',(44.5599089424743,-55.2434808562086,
-38.6629497802385));
#263569=CARTESIAN_POINT('Ctrl Pts',(44.6354869543582,-55.2439911084578,
-38.6767130108817));
#263570=CARTESIAN_POINT('Ctrl Pts',(44.6731456892459,-55.2451740103824,
-38.6837342374529));
#263571=CARTESIAN_POINT('Ctrl Pts',(44.7481014788608,-55.2493620066237,
-38.6980304684339));
#263572=CARTESIAN_POINT('Ctrl Pts',(44.860046548974,-55.2583760573225,-38.7198650218829));
#263573=CARTESIAN_POINT('Ctrl Pts',(45.0073845433675,-55.2811507310277,
-38.7505067688753));
#263574=CARTESIAN_POINT('Ctrl Pts',(45.1528189888476,-55.3146135839333,
-38.7826550300594));
#263575=CARTESIAN_POINT('Ctrl Pts',(45.2248832056965,-55.3349380951144,
-38.7992310848652));
#263576=CARTESIAN_POINT('Ctrl Pts',(45.2966462681613,-55.3570913336823,
-38.8160672125853));
#263577=CARTESIAN_POINT('Ctrl Pts',(45.3323638946335,-55.3690863290504,
-38.8246135819642));
#263578=CARTESIAN_POINT('Ctrl Pts',(45.4027951436545,-55.3946744461232,
-38.841798196801));
#263579=CARTESIAN_POINT('Ctrl Pts',(45.4376370321487,-55.4083060218429,
-38.85046633842));
#263580=CARTESIAN_POINT('Ctrl Pts',(45.5409345111852,-55.4516493275196,
-38.8766665754573));
#263581=CARTESIAN_POINT('Ctrl Pts',(45.6082182891413,-55.4838201174091,
-38.8944064774514));
#263582=CARTESIAN_POINT('Ctrl Pts',(45.7067749877369,-55.5369855856676,
-38.9214216121435));
#263583=CARTESIAN_POINT('Ctrl Pts',(45.7392219877795,-55.5555212114618,
-38.9304915704334));
#263584=CARTESIAN_POINT('Ctrl Pts',(45.8033556832395,-55.5942722159849,
-38.9487787872477));
#263585=CARTESIAN_POINT('Ctrl Pts',(45.8348443691401,-55.6143675312756,
-38.9579395118015));
#263586=CARTESIAN_POINT('Ctrl Pts',(45.9274099842789,-55.6766589025306,
-38.9854159162723));
#263587=CARTESIAN_POINT('Ctrl Pts',(45.9867610865919,-55.7209353156014,
-39.0037703637879));
#263588=CARTESIAN_POINT('Ctrl Pts',(46.1007337830098,-55.8148102393793,
-39.0405190865864));
#263589=CARTESIAN_POINT('Ctrl Pts',(46.1826971388658,-55.889219933262,-39.0681181728269));
#263590=CARTESIAN_POINT('Ctrl Pts',(46.259356574729,-55.9696687352924,-39.0957737179551));
#263591=CARTESIAN_POINT('Ctrl Pts',(46.309266807939,-56.024663053365,-39.1142236413887));
#263592=CARTESIAN_POINT('Ctrl Pts',(46.3336138177017,-56.0528284109483,
-39.1234510495426));
#263593=CARTESIAN_POINT('Ctrl Pts',(46.3692509284248,-56.0961546965833,
-39.1373141736981));
#263594=CARTESIAN_POINT('Ctrl Pts',(46.3809719555493,-56.1107655250657,
-39.14193505412));
#263595=CARTESIAN_POINT('Ctrl Pts',(46.4039850968433,-56.1401806715041,
-39.1511314768264));
#263596=CARTESIAN_POINT('Ctrl Pts',(46.4153001903629,-56.1550126624776,
-39.1557159133813));
#263597=CARTESIAN_POINT('Ctrl Pts',(46.4486370096885,-56.1998310060263,
-39.1694131182659));
#263598=CARTESIAN_POINT('Ctrl Pts',(46.4700835091466,-56.2301795317326,
-39.1784826054425));
#263599=CARTESIAN_POINT('Ctrl Pts',(46.532071913686,-56.3225583984772,-39.2054898733524));
#263600=CARTESIAN_POINT('Ctrl Pts',(46.5894197348374,-56.4176636744323,
-39.23211607576));
#263601=CARTESIAN_POINT('Ctrl Pts',(46.6566074362748,-56.5498680842415,
-39.2668544229849));
#263602=CARTESIAN_POINT('Ctrl Pts',(46.6870820302515,-56.617790568625,-39.2839693714534));
#263603=CARTESIAN_POINT('Ctrl Pts',(46.7159729830272,-56.6866360545619,
-39.3009558869148));
#263604=CARTESIAN_POINT('Ctrl Pts',(46.7296188023799,-56.7214992889704,
-39.3093799218186));
#263605=CARTESIAN_POINT('Ctrl Pts',(46.7553216997643,-56.7922546384013,
-39.3261176641085));
#263606=CARTESIAN_POINT('Ctrl Pts',(46.7672996943011,-56.8279354881579,
-39.3343809787628));
#263607=CARTESIAN_POINT('Ctrl Pts',(46.8004530502947,-56.9353633959568,
-39.358737163018));
#263608=CARTESIAN_POINT('Ctrl Pts',(46.8189795501832,-57.0077635587999,
-39.3744658121213));
#263609=CARTESIAN_POINT('Ctrl Pts',(46.848916211803,-57.1540080946302,-39.4048998290393));
#263610=CARTESIAN_POINT('Ctrl Pts',(46.866048617508,-57.2647966217996,-39.4269646939479));
#263611=CARTESIAN_POINT('Ctrl Pts',(46.875074749658,-57.3772756893033,-39.4478819384746));
#263612=CARTESIAN_POINT('Ctrl Pts',(46.8792542953452,-57.4526370309597,
-39.4615663943076));
#263613=CARTESIAN_POINT('Ctrl Pts',(46.8804258736835,-57.4905390832845,
-39.4682843608713));
#263614=CARTESIAN_POINT('Ctrl Pts',(46.8808837743635,-57.566610437341,-39.4814341960201));
#263615=CARTESIAN_POINT('Ctrl Pts',(46.8801708637706,-57.604491394965,-39.4878166677226));
#263616=CARTESIAN_POINT('Ctrl Pts',(46.8768913879562,-57.6800597985945,
-39.5002231148134));
#263617=CARTESIAN_POINT('Ctrl Pts',(46.8691896925243,-57.7930657109158,
-39.5182849936093));
#263618=CARTESIAN_POINT('Ctrl Pts',(46.8479069711518,-57.9423669591112,
-39.540205996752));
#263619=CARTESIAN_POINT('Ctrl Pts',(46.8236459543104,-58.053306681129,-39.5550278422771));
#263620=CARTESIAN_POINT('Ctrl Pts',(46.8055990109883,-58.1270324939452,
-39.5645447403379));
#263621=CARTESIAN_POINT('Ctrl Pts',(46.7956339676918,-58.1637938532181,
-39.5691227921436));
#263622=CARTESIAN_POINT('Ctrl Pts',(46.7738161327052,-58.2370162077019,
-39.5779016468881));
#263623=CARTESIAN_POINT('Ctrl Pts',(46.7619036278491,-58.2736352268715,
-39.5821192203466));
#263624=CARTESIAN_POINT('Ctrl Pts',(46.7364059718256,-58.3458255995332,
-39.5900871854462));
#263625=CARTESIAN_POINT('Ctrl Pts',(46.7091836493705,-58.4171862986019,
-39.5976163356366));
#263626=CARTESIAN_POINT('Ctrl Pts',(46.663274408039,-58.5216699086648,-39.6076014242402));
#263627=CARTESIAN_POINT('Ctrl Pts',(46.6123207377325,-58.6236436013082,
-39.616293729045));
#263628=CARTESIAN_POINT('Ctrl Pts',(46.5563244858032,-58.7230996041114,
-39.6236943138341));
#263629=CARTESIAN_POINT('Ctrl Pts',(46.515607032986,-58.7877140896312,-39.6277619492082));
#263630=CARTESIAN_POINT('Ctrl Pts',(46.4731710833873,-58.8514710047945,
-39.6313905635194));
#263631=CARTESIAN_POINT('Ctrl Pts',(46.4511086137465,-58.8829006319494,
-39.6329844599904));
#263632=CARTESIAN_POINT('Ctrl Pts',(46.4051673201274,-58.9449633016888,
-39.6357273485653));
#263633=CARTESIAN_POINT('Ctrl Pts',(46.381447994276,-58.975377588932,-39.6368662598532));
#263634=CARTESIAN_POINT('Ctrl Pts',(46.3084068909562,-59.0643493136614,
-39.6395761233691));
#263635=CARTESIAN_POINT('Ctrl Pts',(46.2570407846102,-59.1209150453974,
-39.6404603784325));
#263636=CARTESIAN_POINT('Ctrl Pts',(46.1491379755941,-59.228544463199,-39.6404138814247));
#263637=CARTESIAN_POINT('Ctrl Pts',(46.0925836555155,-59.2796343044913,
-39.6394845811684));
#263638=CARTESIAN_POINT('Ctrl Pts',(46.0038529437629,-59.3521266125547,
-39.6367223387528));
#263639=CARTESIAN_POINT('Ctrl Pts',(45.9736068078661,-59.3756113554055,
-39.6355721163029));
#263640=CARTESIAN_POINT('Ctrl Pts',(45.9272656961273,-59.4097723546528,
-39.6334997725088));
#263641=CARTESIAN_POINT('Ctrl Pts',(45.9116419215573,-59.4209912820171,
-39.6327502808957));
#263642=CARTESIAN_POINT('Ctrl Pts',(45.8800804794677,-59.4430610802669,
-39.6311351339295));
#263643=CARTESIAN_POINT('Ctrl Pts',(45.8321587971618,-59.4756823489919,
-39.628531354857));
#263644=CARTESIAN_POINT('Ctrl Pts',(45.7834097108732,-59.5062438963941,
-39.6254355071979));
#263645=CARTESIAN_POINT('Ctrl Pts',(45.717633106262,-59.5452481912826,-39.6208773262667));
#263646=CARTESIAN_POINT('Ctrl Pts',(45.6178307490054,-59.601113548897,-39.6133952897297));
#263647=CARTESIAN_POINT('Ctrl Pts',(45.4802897643185,-59.6652183443042,
-39.6008811885904));
#263648=CARTESIAN_POINT('Ctrl Pts',(45.3738098009101,-59.7055766782111,
-39.5896017905935));
#263649=CARTESIAN_POINT('Ctrl Pts',(45.3020778813705,-59.7307512119865,
-39.5816566825671));
#263650=CARTESIAN_POINT('Ctrl Pts',(45.2658207311094,-59.7424779859237,
-39.5774690651077));
#263651=CARTESIAN_POINT('Ctrl Pts',(45.1926264675053,-59.7641596016776,
-39.5686715125846));
#263652=CARTESIAN_POINT('Ctrl Pts',(45.1555073907618,-59.7741562512684,
-39.5640376159893));
#263653=CARTESIAN_POINT('Ctrl Pts',(45.0441315765335,-59.8011904590316,
-39.5496210468413));
#263654=CARTESIAN_POINT('Ctrl Pts',(44.9324484012679,-59.8224577850013,
-39.5341534065747));
#263655=CARTESIAN_POINT('Ctrl Pts',(44.8203079610257,-59.8353953605365,
-39.5171556909205));
#263656=CARTESIAN_POINT('Ctrl Pts',(44.7080184564226,-59.8455760612675,
-39.4996502778008));
#263657=CARTESIAN_POINT('Ctrl Pts',(44.6329372249224,-59.8486931621852,
-39.4873001861445));
#263658=CARTESIAN_POINT('Ctrl Pts',(44.5200834441659,-59.8478515133141,
-39.4677634802869));
#263659=CARTESIAN_POINT('Ctrl Pts',(44.4823810871712,-59.8466449718289,
-39.4610736497974));
#263660=CARTESIAN_POINT('Ctrl Pts',(44.4258051079382,-59.8434394706745,
-39.4507883432074));
#263661=CARTESIAN_POINT('Ctrl Pts',(44.4069254589855,-59.8421361346926,
-39.4473147915973));
#263662=CARTESIAN_POINT('Ctrl Pts',(44.3691376542581,-59.8390581625153,
-39.4402793331445));
#263663=CARTESIAN_POINT('Ctrl Pts',(44.3502459350849,-59.8372838734483,
-39.4367203104461));
#263664=CARTESIAN_POINT('Ctrl Pts',(44.2562487381671,-59.8272835659938,
-39.4188041728073));
#263665=CARTESIAN_POINT('Ctrl Pts',(44.1080045765469,-59.8040393501646,
-39.3892226636159));
#263666=CARTESIAN_POINT('Ctrl Pts',(43.9639303529155,-59.7668593120831,
-39.3578670379715));
#263667=CARTESIAN_POINT('Ctrl Pts',(43.8219159040518,-59.7227861654643,
-39.3256251231267));
#263668=CARTESIAN_POINT('Ctrl Pts',(43.7519290534068,-59.6972943066161,
-39.3090578287531));
#263669=CARTESIAN_POINT('Ctrl Pts',(43.665783177736,-59.6610675807531,-39.2877890488175));
#263670=CARTESIAN_POINT('Ctrl Pts',(43.6486106666635,-59.653596197985,-39.2835041280971));
#263671=CARTESIAN_POINT('Ctrl Pts',(43.6144193015916,-59.6382222359849,
-39.2748825183767));
#263672=CARTESIAN_POINT('Ctrl Pts',(43.597366582891,-59.6303022352814,-39.2705368924251));
#263673=CARTESIAN_POINT('Ctrl Pts',(43.5465994182959,-59.605961903298,-39.2574616452183));
#263674=CARTESIAN_POINT('Ctrl Pts',(43.513329300663,-59.588993111175,-39.2487085268073));
#263675=CARTESIAN_POINT('Ctrl Pts',(43.4805771074156,-59.5712767529309,
-39.2399080357013));
#263676=CARTESIAN_POINT('Ctrl Pts',(43.8903154257419,-57.7291941381088,
-41.4266127101804));
#263677=CARTESIAN_POINT('Ctrl Pts',(43.8716814361492,-57.7189244770852,
-41.4090117279687));
#263678=CARTESIAN_POINT('Ctrl Pts',(43.8355945080866,-57.6967277837834,
-41.3734625137379));
#263679=CARTESIAN_POINT('Ctrl Pts',(43.7849271573585,-57.6585752750105,
-41.3191078559793));
#263680=CARTESIAN_POINT('Ctrl Pts',(43.753465403225,-57.62988352171,-41.2821707250961));
#263681=CARTESIAN_POINT('Ctrl Pts',(43.7232071092872,-57.5995155202448,
-41.2448779944712));
#263682=CARTESIAN_POINT('Ctrl Pts',(43.694633283399,-57.5679550683129,-41.2078231506529));
#263683=CARTESIAN_POINT('Ctrl Pts',(43.6629744005209,-57.5256074013359,
-41.162062942605));
#263684=CARTESIAN_POINT('Ctrl Pts',(43.6400741040405,-57.4900012877665,
-41.1257945258022));
#263685=CARTESIAN_POINT('Ctrl Pts',(43.624122646482,-57.4624228770549,-41.0987642906252));
#263686=CARTESIAN_POINT('Ctrl Pts',(43.6143188854815,-57.4434516436916,
-41.0808660102928));
#263687=CARTESIAN_POINT('Ctrl Pts',(43.6049343759216,-57.4241698350281,
-41.0630203901697));
#263688=CARTESIAN_POINT('Ctrl Pts',(43.6004882740613,-57.4144479878336,
-41.054192925399));
#263689=CARTESIAN_POINT('Ctrl Pts',(43.5878889573419,-57.3850715912746,
-41.0280183011396));
#263690=CARTESIAN_POINT('Ctrl Pts',(43.5730447416356,-57.3453166524842,
-40.9939147159844));
#263691=CARTESIAN_POINT('Ctrl Pts',(43.5620571572655,-57.3044044614592,
-40.9613948378065));
#263692=CARTESIAN_POINT('Ctrl Pts',(43.5552843243605,-57.2732819874194,
-40.9376151994878));
#263693=CARTESIAN_POINT('Ctrl Pts',(43.5532714802541,-57.2628325912303,
-40.9297890667463));
#263694=CARTESIAN_POINT('Ctrl Pts',(43.5497454556161,-57.2417890776549,
-40.9143485382007));
#263695=CARTESIAN_POINT('Ctrl Pts',(43.5482304746054,-57.2311797832666,
-40.9067234564832));
#263696=CARTESIAN_POINT('Ctrl Pts',(43.5457184756399,-57.2098591834555,
-40.8917243418755));
#263697=CARTESIAN_POINT('Ctrl Pts',(43.5447290487245,-57.199220662917,-40.8844009198028));
#263698=CARTESIAN_POINT('Ctrl Pts',(43.5432711863927,-57.1779500447907,
-40.8700767121812));
#263699=CARTESIAN_POINT('Ctrl Pts',(43.5418684734652,-57.1460721839032,
-40.8490875836402));
#263700=CARTESIAN_POINT('Ctrl Pts',(43.5431039253892,-57.1036793909824,
-40.8230787545116));
#263701=CARTESIAN_POINT('Ctrl Pts',(43.5463738329101,-57.0719682486671,
-40.8050747359183));
#263702=CARTESIAN_POINT('Ctrl Pts',(43.5490829635055,-57.0508462881094,
-40.7934126279614));
#263703=CARTESIAN_POINT('Ctrl Pts',(43.5507030159248,-57.0402904723448,
-40.7877497380755));
#263704=CARTESIAN_POINT('Ctrl Pts',(43.5544790630841,-57.019214904491,-40.7767808895002));
#263705=CARTESIAN_POINT('Ctrl Pts',(43.5566463931059,-57.0086510117152,
-40.7714540988351));
#263706=CARTESIAN_POINT('Ctrl Pts',(43.5614808344627,-56.9877741662596,
-40.7612719783604));
#263707=CARTESIAN_POINT('Ctrl Pts',(43.5668234022498,-56.9670831174431,
-40.7515253398262));
#263708=CARTESIAN_POINT('Ctrl Pts',(43.5763377125496,-56.9366295208774,
-40.7382165180791));
#263709=CARTESIAN_POINT('Ctrl Pts',(43.5873444561754,-56.9067460923864,
-40.7262089422516));
#263710=CARTESIAN_POINT('Ctrl Pts',(43.5998453117462,-56.8774358278222,
-40.7155085881795));
#263711=CARTESIAN_POINT('Ctrl Pts',(43.6091839698139,-56.8582805167828,
-40.7092555817853));
#263712=CARTESIAN_POINT('Ctrl Pts',(43.6190331668358,-56.8393207538612,
-40.7034508410834));
#263713=CARTESIAN_POINT('Ctrl Pts',(43.6242099732076,-56.8299438685379,
-40.7007739810578));
#263714=CARTESIAN_POINT('Ctrl Pts',(43.6350986096338,-56.8113693026126,
-40.6958744145609));
#263715=CARTESIAN_POINT('Ctrl Pts',(43.6407690742328,-56.8022426567881,
-40.6936706244929));
#263716=CARTESIAN_POINT('Ctrl Pts',(43.6583896223854,-56.7754411523649,
-40.6878155334118));
#263717=CARTESIAN_POINT('Ctrl Pts',(43.6709801307092,-56.7582712890167,
-40.6848937134075));
#263718=CARTESIAN_POINT('Ctrl Pts',(43.6978023804218,-56.725340315416,-40.6809957255822));
#263719=CARTESIAN_POINT('Ctrl Pts',(43.7120405319879,-56.7095692151415,
-40.6800172734785));
#263720=CARTESIAN_POINT('Ctrl Pts',(43.7346338722206,-56.6869796178674,
-40.680019660452));
#263721=CARTESIAN_POINT('Ctrl Pts',(43.7423799312797,-56.6796208977126,
-40.6802668752224));
#263722=CARTESIAN_POINT('Ctrl Pts',(43.7543060585229,-56.6688607312791,
-40.681010981358));
#263723=CARTESIAN_POINT('Ctrl Pts',(43.7583370517177,-56.6653168192219,
-40.6813218268212));
#263724=CARTESIAN_POINT('Ctrl Pts',(43.7665035456834,-56.6583217341419,
-40.6820693651562));
#263725=CARTESIAN_POINT('Ctrl Pts',(43.7706422703,-56.6548683091639,-40.6825066780886));
#263726=CARTESIAN_POINT('Ctrl Pts',(43.7831478581881,-56.6447045100584,
-40.6840009724959));
#263727=CARTESIAN_POINT('Ctrl Pts',(43.8000992888712,-56.6316392340345,
-40.6864805452653));
#263728=CARTESIAN_POINT('Ctrl Pts',(43.8351004518507,-56.6074069729907,
-40.6933496988796));
#263729=CARTESIAN_POINT('Ctrl Pts',(43.8717190640765,-56.5859796680779,
-40.7030349737613));
#263730=CARTESIAN_POINT('Ctrl Pts',(43.9003898794618,-56.5719991465823,
-40.7123924126099));
#263731=CARTESIAN_POINT('Ctrl Pts',(43.919774692733,-56.5631479893168,-40.719099824507));
#263732=CARTESIAN_POINT('Ctrl Pts',(43.9296053152689,-56.5589560552736,
-40.722689237866));
#263733=CARTESIAN_POINT('Ctrl Pts',(43.9495302416178,-56.551051384942,-40.7303379810773));
#263734=CARTESIAN_POINT('Ctrl Pts',(43.959660471973,-56.5473282955902,-40.7344135607172));
#263735=CARTESIAN_POINT('Ctrl Pts',(43.9799461530017,-56.5404515818703,
-40.7429393172485));
#263736=CARTESIAN_POINT('Ctrl Pts',(43.9901452646573,-56.5372793127045,
-40.7474054189318));
#263737=CARTESIAN_POINT('Ctrl Pts',(44.0208712025373,-56.5285586047056,
-40.7613849151889));
#263738=CARTESIAN_POINT('Ctrl Pts',(44.0518784813599,-56.521416173947,-40.7765333604643));
#263739=CARTESIAN_POINT('Ctrl Pts',(44.0937728041468,-56.5149820273198,
-40.799005697554));
#263740=CARTESIAN_POINT('Ctrl Pts',(44.1254693703652,-56.5117027703592,
-40.8169947136667));
#263741=CARTESIAN_POINT('Ctrl Pts',(44.1467868482481,-56.5105547568045,
-40.8297474946377));
#263742=CARTESIAN_POINT('Ctrl Pts',(44.1681963264173,-56.50993223545,-40.842882238999));
#263743=CARTESIAN_POINT('Ctrl Pts',(44.1789665479467,-56.509886262238,-40.8496544547178));
#263744=CARTESIAN_POINT('Ctrl Pts',(44.2003410646824,-56.5103214152413,
-40.8634176853611));
#263745=CARTESIAN_POINT('Ctrl Pts',(44.2109953322312,-56.5108003631786,
-40.8704389119319));
#263746=CARTESIAN_POINT('Ctrl Pts',(44.2322091102727,-56.5122711761573,
-40.8847351429132));
#263747=CARTESIAN_POINT('Ctrl Pts',(44.2639028799147,-56.5152466319394,
-40.9065696963621));
#263748=CARTESIAN_POINT('Ctrl Pts',(44.305661850593,-56.5222422564611,-40.9372114433545));
#263749=CARTESIAN_POINT('Ctrl Pts',(44.346925841944,-56.532247127269,-40.9693597045385));
#263750=CARTESIAN_POINT('Ctrl Pts',(44.3673876336497,-56.53826115526,-40.9859357593442));
#263751=CARTESIAN_POINT('Ctrl Pts',(44.3877715667723,-56.5447901720246,
-41.0027718870644));
#263752=CARTESIAN_POINT('Ctrl Pts',(44.3979208506631,-56.5483132560745,
-41.0113182564434));
#263753=CARTESIAN_POINT('Ctrl Pts',(44.4179418071922,-56.5558066378292,
-41.02850287128));
#263754=CARTESIAN_POINT('Ctrl Pts',(44.4278499085732,-56.5597882829787,
-41.0371710128992));
#263755=CARTESIAN_POINT('Ctrl Pts',(44.4572364860018,-56.5724196473794,
-41.0633712499365));
#263756=CARTESIAN_POINT('Ctrl Pts',(44.4763932211824,-56.581758968269,-41.0811111519311));
#263757=CARTESIAN_POINT('Ctrl Pts',(44.5044772880921,-56.5971447477014,
-41.1081262866225));
#263758=CARTESIAN_POINT('Ctrl Pts',(44.5137271775895,-56.6025015227711,
-41.1171962449124));
#263759=CARTESIAN_POINT('Ctrl Pts',(44.5320183562985,-56.6136863880645,
-41.1354834617267));
#263760=CARTESIAN_POINT('Ctrl Pts',(44.5410031705763,-56.6194798267371,
-41.144644186283));
#263761=CARTESIAN_POINT('Ctrl Pts',(44.5674276642847,-56.6374191091633,
-41.1721205907467));
#263762=CARTESIAN_POINT('Ctrl Pts',(44.5843870769067,-56.6501457393646,
-41.1904750382678));
#263763=CARTESIAN_POINT('Ctrl Pts',(44.616987890196,-56.6770839740703,-41.2272237610649));
#263764=CARTESIAN_POINT('Ctrl Pts',(44.640458797708,-56.6984048650555,-41.2548228473058));
#263765=CARTESIAN_POINT('Ctrl Pts',(44.6624514458289,-56.7214114906953,
-41.2824783924342));
#263766=CARTESIAN_POINT('Ctrl Pts',(44.6767798128067,-56.7371294193188,
-41.3009283158679));
#263767=CARTESIAN_POINT('Ctrl Pts',(44.683774397772,-56.7451748501741,-41.3101557240219));
#263768=CARTESIAN_POINT('Ctrl Pts',(44.6940202659092,-56.7575442973705,
-41.324018848177));
#263769=CARTESIAN_POINT('Ctrl Pts',(44.6973914635031,-56.7617145235639,
-41.328639728599));
#263770=CARTESIAN_POINT('Ctrl Pts',(44.7040131878578,-56.770108052971,-41.3378361513053));
#263771=CARTESIAN_POINT('Ctrl Pts',(44.7072703203268,-56.7743392575068,
-41.3424205878605));
#263772=CARTESIAN_POINT('Ctrl Pts',(44.7168707027477,-56.7871217033085,
-41.3561177927451));
#263773=CARTESIAN_POINT('Ctrl Pts',(44.7230524906066,-56.7957731420119,
-41.3651872799216));
#263774=CARTESIAN_POINT('Ctrl Pts',(44.7409373255192,-56.8220955492914,
-41.3921945478314));
#263775=CARTESIAN_POINT('Ctrl Pts',(44.7575187561203,-56.8491712652862,
-41.4188207502394));
#263776=CARTESIAN_POINT('Ctrl Pts',(44.7770214494108,-56.88676384976,-41.453559097464));
#263777=CARTESIAN_POINT('Ctrl Pts',(44.7858965000619,-56.9060633365117,
-41.4706740459328));
#263778=CARTESIAN_POINT('Ctrl Pts',(44.7943266372896,-56.9256180211132,
-41.4876605613939));
#263779=CARTESIAN_POINT('Ctrl Pts',(44.7983169540911,-56.9355169983302,
-41.4960845962979));
#263780=CARTESIAN_POINT('Ctrl Pts',(44.8058516078422,-56.9556000996462,
-41.5128223385875));
#263781=CARTESIAN_POINT('Ctrl Pts',(44.8093727854448,-56.9657242505397,
-41.5210856532432));
#263782=CARTESIAN_POINT('Ctrl Pts',(44.8191505788346,-56.9961959016236,
-41.5454418374945));
#263783=CARTESIAN_POINT('Ctrl Pts',(44.8246597322132,-57.0167187198372,
-41.5611704866007));
#263784=CARTESIAN_POINT('Ctrl Pts',(44.8336688220904,-57.0581479791523,
-41.5916045035181));
#263785=CARTESIAN_POINT('Ctrl Pts',(44.8389236650083,-57.0895139074259,
-41.613669368427));
#263786=CARTESIAN_POINT('Ctrl Pts',(44.8418900765893,-57.1213299669285,
-41.6345866129535));
#263787=CARTESIAN_POINT('Ctrl Pts',(44.8433488372948,-57.142640498193,-41.6482710687869));
#263788=CARTESIAN_POINT('Ctrl Pts',(44.8438191277705,-57.1533552116615,
-41.6549890353504));
#263789=CARTESIAN_POINT('Ctrl Pts',(44.8442270800594,-57.1748537940466,
-41.6681388704993));
#263790=CARTESIAN_POINT('Ctrl Pts',(44.8441639040618,-57.1855561823783,
-41.6745213422017));
#263791=CARTESIAN_POINT('Ctrl Pts',(44.8435122114514,-57.2069000331791,
-41.6869277892926));
#263792=CARTESIAN_POINT('Ctrl Pts',(44.8417458896958,-57.2388084678274,
-41.7049896680882));
#263793=CARTESIAN_POINT('Ctrl Pts',(44.8362687719071,-57.2809279665006,
-41.7269106712316));
#263794=CARTESIAN_POINT('Ctrl Pts',(44.8298088085522,-57.3121969378441,
-41.7417325167562));
#263795=CARTESIAN_POINT('Ctrl Pts',(44.8249713776488,-57.3329705079708,
-41.751249414817));
#263796=CARTESIAN_POINT('Ctrl Pts',(44.8222858794974,-57.3433254378487,
-41.7558274666229));
#263797=CARTESIAN_POINT('Ctrl Pts',(44.8163797073795,-57.3639440769784,
-41.7646063213672));
#263798=CARTESIAN_POINT('Ctrl Pts',(44.8131427147447,-57.3742522416544,
-41.7688238948253));
#263799=CARTESIAN_POINT('Ctrl Pts',(44.8061917406462,-57.3945668799698,
-41.7767918599254));
#263800=CARTESIAN_POINT('Ctrl Pts',(44.7987498536529,-57.4146412549335,
-41.7843210101159));
#263801=CARTESIAN_POINT('Ctrl Pts',(44.7861419817956,-57.4440129710611,
-41.7943060987191));
#263802=CARTESIAN_POINT('Ctrl Pts',(44.7720982599006,-57.4726583092559,
-41.8029984035242));
#263803=CARTESIAN_POINT('Ctrl Pts',(44.7566193423106,-57.5005749992605,
-41.8103989883131));
#263804=CARTESIAN_POINT('Ctrl Pts',(44.7453362941317,-57.518697088903,-41.8144666236875));
#263805=CARTESIAN_POINT('Ctrl Pts',(44.7335642473644,-57.5365709174371,
-41.8180952379985));
#263806=CARTESIAN_POINT('Ctrl Pts',(44.7274378249752,-57.5453780864623,
-41.8196891344695));
#263807=CARTESIAN_POINT('Ctrl Pts',(44.7146685840676,-57.5627610237142,
-41.8224320230444));
#263808=CARTESIAN_POINT('Ctrl Pts',(44.7080700862024,-57.5712755128024,
-41.8235709343319));
#263809=CARTESIAN_POINT('Ctrl Pts',(44.6877341610586,-57.5961705213949,
-41.8262807978491));
#263810=CARTESIAN_POINT('Ctrl Pts',(44.6734117165454,-57.6119810052107,
-41.8271650529119));
#263811=CARTESIAN_POINT('Ctrl Pts',(44.6432859415473,-57.6420285404153,
-41.827118555904));
#263812=CARTESIAN_POINT('Ctrl Pts',(44.6274777219699,-57.6562729242579,
-41.8261892556471));
#263813=CARTESIAN_POINT('Ctrl Pts',(44.6026489360012,-57.6764545436153,
-41.823427013232));
#263814=CARTESIAN_POINT('Ctrl Pts',(44.5941811636919,-57.6829873126311,
-41.8222767907821));
#263815=CARTESIAN_POINT('Ctrl Pts',(44.5812011369499,-57.6924815728277,
-41.820204446988));
#263816=CARTESIAN_POINT('Ctrl Pts',(44.5768239301145,-57.6955981764101,
-41.8194549553751));
#263817=CARTESIAN_POINT('Ctrl Pts',(44.5679795363474,-57.7017261947271,
-41.8178398084084));
#263818=CARTESIAN_POINT('Ctrl Pts',(44.554547495243,-57.7107794649358,-41.8152360293365));
#263819=CARTESIAN_POINT('Ctrl Pts',(44.5408745509057,-57.7192473537464,
-41.812140181677));
#263820=CARTESIAN_POINT('Ctrl Pts',(44.5224181841827,-57.7300417662926,
-41.8075820007456));
#263821=CARTESIAN_POINT('Ctrl Pts',(44.494403164631,-57.7454824222945,-41.8000999642091));
#263822=CARTESIAN_POINT('Ctrl Pts',(44.4557509611988,-57.7631175354143,
-41.7875858630695));
#263823=CARTESIAN_POINT('Ctrl Pts',(44.4257963579031,-57.7741479888816,
-41.7763064650726));
#263824=CARTESIAN_POINT('Ctrl Pts',(44.4056101875344,-57.781009218212,-41.7683613570464));
#263825=CARTESIAN_POINT('Ctrl Pts',(44.3954036594654,-57.7841949818065,
-41.7641737395871));
#263826=CARTESIAN_POINT('Ctrl Pts',(44.3747925009816,-57.7900627169564,
-41.7553761870634));
#263827=CARTESIAN_POINT('Ctrl Pts',(44.3643365899562,-57.7927558542442,
-41.7507422904685));
#263828=CARTESIAN_POINT('Ctrl Pts',(44.3329536886806,-57.7999988857253,
-41.7363257213199));
#263829=CARTESIAN_POINT('Ctrl Pts',(44.3014645871824,-57.8056090798854,
-41.7208580810542));
#263830=CARTESIAN_POINT('Ctrl Pts',(44.2698183189435,-57.8088603667088,
-41.7038603653999));
#263831=CARTESIAN_POINT('Ctrl Pts',(44.2381206623806,-57.8113308880715,
-41.6863549522799));
#263832=CARTESIAN_POINT('Ctrl Pts',(44.2169139506954,-57.8119384373532,
-41.6740048606234));
#263833=CARTESIAN_POINT('Ctrl Pts',(44.1850197107514,-57.811287280344,-41.6544681547659));
#263834=CARTESIAN_POINT('Ctrl Pts',(44.1743613109546,-57.8108078241776,
-41.6477783242763));
#263835=CARTESIAN_POINT('Ctrl Pts',(44.1583626375358,-57.8096935003687,
-41.6374930176863));
#263836=CARTESIAN_POINT('Ctrl Pts',(44.1530230189312,-57.809255510817,-41.6340194660765));
#263837=CARTESIAN_POINT('Ctrl Pts',(44.1423341247923,-57.8082460206643,
-41.6269840076234));
#263838=CARTESIAN_POINT('Ctrl Pts',(44.1369894952372,-57.8076746784434,
-41.6234249849254));
#263839=CARTESIAN_POINT('Ctrl Pts',(44.1103928894951,-57.8045001122898,
-41.6055088472864));
#263840=CARTESIAN_POINT('Ctrl Pts',(44.0684216046586,-57.7973782151022,
-41.5759273380954));
#263841=CARTESIAN_POINT('Ctrl Pts',(44.0275807082801,-57.78632659952,-41.5445717124501));
#263842=CARTESIAN_POINT('Ctrl Pts',(43.9872978152183,-57.7733311875938,
-41.5123297976061));
#263843=CARTESIAN_POINT('Ctrl Pts',(43.9674326520914,-57.7658590768128,
-41.4957625032292));
#263844=CARTESIAN_POINT('Ctrl Pts',(43.942963744406,-57.7552890823142,-41.4744937232973));
#263845=CARTESIAN_POINT('Ctrl Pts',(43.938085174092,-57.7531113051098,-41.4702088025761));
#263846=CARTESIAN_POINT('Ctrl Pts',(43.9283699185172,-57.7486342535987,
-41.4615871928557));
#263847=CARTESIAN_POINT('Ctrl Pts',(43.9235236029976,-57.7463299238453,
-41.4572415669043));
#263848=CARTESIAN_POINT('Ctrl Pts',(43.9090930604083,-57.739254093668,-41.4441663196977));
#263849=CARTESIAN_POINT('Ctrl Pts',(43.8996324205383,-57.7343289686206,
-41.4354132012863));
#263850=CARTESIAN_POINT('Ctrl Pts',(43.8903154257419,-57.7291941381088,
-41.4266127101804));
#263851=CARTESIAN_POINT('',(45.4581751231188,-55.7156010961851,-39.3126317220031));
#263852=CARTESIAN_POINT('',(45.2824537511366,-55.8755132365557,-39.638597553055));
#263853=CARTESIAN_POINT('',(45.4581751231188,-55.7156010961851,-39.3126317220031));
#263854=CARTESIAN_POINT('Origin',(44.4104395346295,-57.5698098586536,-39.4585973766342));
#263855=CARTESIAN_POINT('Ctrl Pts',(45.1065281945089,-55.5671267135029,
-39.2098668976124));
#263856=CARTESIAN_POINT('Ctrl Pts',(44.9196034855776,-55.5452400673183,
-39.2198174688805));
#263857=CARTESIAN_POINT('Ctrl Pts',(44.7296870412447,-55.5423799337785,
-39.2250112643947));
#263858=CARTESIAN_POINT('Ctrl Pts',(44.2390927302324,-55.5906252485044,
-39.2279787011603));
#263859=CARTESIAN_POINT('Ctrl Pts',(44.0090817791515,-55.6680747610649,
-39.2201085375079));
#263860=CARTESIAN_POINT('Ctrl Pts',(43.7382090165708,-55.7808826579177,
-39.2093719638497));
#263861=CARTESIAN_POINT('Ctrl Pts',(43.6231650567784,-55.840997752458,-39.2038428512868));
#263862=CARTESIAN_POINT('Ctrl Pts',(43.5024059980203,-55.917969348109,-39.1959115145055));
#263863=CARTESIAN_POINT('Ctrl Pts',(43.4922077364908,-55.9245826673839,
-39.1952208230375));
#263864=CARTESIAN_POINT('Ctrl Pts',(43.4720389115154,-55.9378870274315,
-39.1938132140166));
#263865=CARTESIAN_POINT('Ctrl Pts',(43.4620602401924,-55.9445806290796,
-39.1930961601356));
#263866=CARTESIAN_POINT('Ctrl Pts',(43.4496915434521,-55.9530170716417,
-39.1921817769743));
#263867=CARTESIAN_POINT('Ctrl Pts',(43.4472466873436,-55.954691516998,-39.1919997813558));
#263868=CARTESIAN_POINT('Ctrl Pts',(43.3583119868597,-56.0158518702413,
-39.1853338681724));
#263869=CARTESIAN_POINT('Ctrl Pts',(43.276069883232,-56.0810726814889,-39.1776023189702));
#263870=CARTESIAN_POINT('Ctrl Pts',(43.0861151222154,-56.2539000103423,
-39.1559361477625));
#263871=CARTESIAN_POINT('Ctrl Pts',(42.9842069097486,-56.3668846933458,
-39.1408381965094));
#263872=CARTESIAN_POINT('Ctrl Pts',(42.7323009654217,-56.7066866053067,
-39.0930140844855));
#263873=CARTESIAN_POINT('Ctrl Pts',(42.6102232298188,-56.9486116620658,
-39.0563926396021));
#263874=CARTESIAN_POINT('Ctrl Pts',(42.5264426781749,-57.2041246092115,
-39.0141963044759));
#263875=CARTESIAN_POINT('Ctrl Pts',(42.5264426236304,-57.2041246472958,
-39.0141972810499));
#263876=CARTESIAN_POINT('Ctrl Pts',(42.5223570304571,-57.2339619119713,
-39.0195734528566));
#263877=CARTESIAN_POINT('Ctrl Pts',(42.5115447559028,-57.3288674986212,
-39.0371239801764));
#263878=CARTESIAN_POINT('Ctrl Pts',(42.506182785202,-57.4564982984358,-39.0625980639181));
#263879=CARTESIAN_POINT('Ctrl Pts',(42.5092432682604,-57.5543877143394,
-39.0835871924589));
#263880=CARTESIAN_POINT('Ctrl Pts',(42.5128918544921,-57.6196827267464,
-39.0979114000806));
#263881=CARTESIAN_POINT('Ctrl Pts',(42.5155178619726,-57.6523290916439,
-39.1052348221532));
#263882=CARTESIAN_POINT('Ctrl Pts',(42.5224092913251,-57.7177332511804,
-39.120233936761));
#263883=CARTESIAN_POINT('Ctrl Pts',(42.5266542176424,-57.7502677264706,
-39.1278590184786));
#263884=CARTESIAN_POINT('Ctrl Pts',(42.5366779815724,-57.8147780230883,
-39.1432995470242));
#263885=CARTESIAN_POINT('Ctrl Pts',(42.5424617625838,-57.8468004016288,
-39.1511256797658));
#263886=CARTESIAN_POINT('Ctrl Pts',(42.5620823726479,-57.9421435490173,
-39.1749053180845));
#263887=CARTESIAN_POINT('Ctrl Pts',(42.5942908295626,-58.0673908049564,
-39.2074251962624));
#263888=CARTESIAN_POINT('Ctrl Pts',(42.6384162470065,-58.1889247195952,
-39.2415287814174));
#263889=CARTESIAN_POINT('Ctrl Pts',(42.676040350531,-58.2786648895678,-39.2677034056768));
#263890=CARTESIAN_POINT('Ctrl Pts',(42.6893426693184,-58.308352422918,-39.2765308704477));
#263891=CARTESIAN_POINT('Ctrl Pts',(42.7174688743488,-58.367210478172,-39.2943764905707));
#263892=CARTESIAN_POINT('Ctrl Pts',(42.7468976399245,-58.4250976736592,
-39.3122747709031));
#263893=CARTESIAN_POINT('Ctrl Pts',(42.7949093409291,-58.5091805688265,
-39.33930500608));
#263894=CARTESIAN_POINT('Ctrl Pts',(42.8639918437047,-58.6176479605168,
-39.3755734228826));
#263895=CARTESIAN_POINT('Ctrl Pts',(42.9458586003439,-58.7277739375476,
-39.4146896477163));
#263896=CARTESIAN_POINT('Ctrl Pts',(43.0153234518519,-58.8072809398543,
-39.4449530869582));
#263897=CARTESIAN_POINT('Ctrl Pts',(43.0434020223321,-58.8374710867404,
-39.4567766041471));
#263898=CARTESIAN_POINT('Ctrl Pts',(43.0434014360654,-58.8374714889306,
-39.456776868572));
#263899=CARTESIAN_POINT('Ctrl Pts',(42.9313536289255,-58.6662175819515,
-39.4482830419655));
#263900=CARTESIAN_POINT('Ctrl Pts',(42.844505428787,-58.4794048505646,-39.4413327045587));
#263901=CARTESIAN_POINT('Ctrl Pts',(42.7299233825216,-58.09580806204,-39.4313779831406));
#263902=CARTESIAN_POINT('Ctrl Pts',(42.7001443335031,-57.9014057226055,
-39.4282539321925));
#263903=CARTESIAN_POINT('Ctrl Pts',(42.6957518169554,-57.5153921394814,
-39.4252456428475));
#263904=CARTESIAN_POINT('Ctrl Pts',(42.7186804830506,-57.2657661474499,
-39.4244208737333));
#263905=CARTESIAN_POINT('Ctrl Pts',(42.881352952887,-56.8215446683501,-39.4348872407336));
#263906=CARTESIAN_POINT('Ctrl Pts',(42.9678495973224,-56.6600017061349,
-39.4410989978245));
#263907=CARTESIAN_POINT('Ctrl Pts',(43.165269885457,-56.3920180420655,-39.4552161772219));
#263908=CARTESIAN_POINT('Ctrl Pts',(43.2687938698745,-56.2817295804231,
-39.4625951676374));
#263909=CARTESIAN_POINT('Ctrl Pts',(43.4087045485911,-56.1645349417216,
-39.4723386928991));
#263910=CARTESIAN_POINT('Ctrl Pts',(43.4337474511219,-56.1446185810003,
-39.4740755133032));
#263911=CARTESIAN_POINT('Ctrl Pts',(43.4624070124288,-56.122993219963,-39.4760548803308));
#263912=CARTESIAN_POINT('Ctrl Pts',(43.4655267799061,-56.1206543087335,
-39.4762702364359));
#263913=CARTESIAN_POINT('Ctrl Pts',(43.4702206900142,-56.117157920804,-39.4765940904724));
#263914=CARTESIAN_POINT('Ctrl Pts',(43.4717893933871,-56.1159932120419,
-39.4767022949794));
#263915=CARTESIAN_POINT('Ctrl Pts',(43.5244120055323,-56.0770493035069,
-39.4803311343257));
#263916=CARTESIAN_POINT('Ctrl Pts',(43.5773300428345,-56.0418702026374,
-39.4839525622719));
#263917=CARTESIAN_POINT('Ctrl Pts',(43.6611219775383,-55.9920607689694,
-39.4896409291132));
#263918=CARTESIAN_POINT('Ctrl Pts',(43.6906998176424,-55.9755391894888,
-39.4916509259111));
#263919=CARTESIAN_POINT('Ctrl Pts',(43.9412200417594,-55.8446488555592,
-39.5091960926514));
#263920=CARTESIAN_POINT('Ctrl Pts',(44.1826052363169,-55.7754693918874,
-39.5285011629926));
#263921=CARTESIAN_POINT('Ctrl Pts',(44.5742546833041,-55.7421335552316,
-39.56393266636));
#263922=CARTESIAN_POINT('Ctrl Pts',(44.7207121507351,-55.7464909499098,
-39.5780619691923));
#263923=CARTESIAN_POINT('Ctrl Pts',(45.008007911895,-55.7878402235656,-39.6076254992843));
#263924=CARTESIAN_POINT('Ctrl Pts',(45.1478398540244,-55.8241870193201,
-39.6229270428342));
#263925=CARTESIAN_POINT('Ctrl Pts',(45.2824630401997,-55.8755167783063,
-39.6385986344006));
#263926=CARTESIAN_POINT('Ctrl Pts',(43.4805770970857,-59.5712767993712,
-39.2399079805728));
#263927=CARTESIAN_POINT('Ctrl Pts',(43.4478249032475,-59.5535604408099,
-39.2311074894668));
#263928=CARTESIAN_POINT('Ctrl Pts',(43.4156055925501,-59.5351039455316,
-39.2222635254953));
#263929=CARTESIAN_POINT('Ctrl Pts',(43.3522169314537,-59.4967329031118,
-39.2044893356988));
#263930=CARTESIAN_POINT('Ctrl Pts',(43.3210476326526,-59.4768182838717,
-39.195559106683));
#263931=CARTESIAN_POINT('Ctrl Pts',(43.22910224469,-59.4149049566893,-39.1686392736337));
#263932=CARTESIAN_POINT('Ctrl Pts',(43.1698853428616,-59.3707413470177,
-39.1505207493783));
#263933=CARTESIAN_POINT('Ctrl Pts',(43.0556331440142,-59.2766098026481,
-39.1139350081145));
#263934=CARTESIAN_POINT('Ctrl Pts',(43.0005921407603,-59.2266373423717,
-39.0954659954893));
#263935=CARTESIAN_POINT('Ctrl Pts',(42.8948534359946,-59.1207134457913,
-39.058173264863));
#263936=CARTESIAN_POINT('Ctrl Pts',(42.8449960335796,-59.065605688259,-39.0396462508422));
#263937=CARTESIAN_POINT('Ctrl Pts',(42.7510810974034,-58.9512122629159,
-39.0028139114377));
#263938=CARTESIAN_POINT('Ctrl Pts',(42.7070287909669,-58.8919306728536,
-38.9845102176061));
#263939=CARTESIAN_POINT('Ctrl Pts',(42.6452866096269,-58.7998959060405,
-38.9572240228595));
#263940=CARTESIAN_POINT('Ctrl Pts',(42.6254297416276,-58.7686980942012,
-38.9481569046653));
#263941=CARTESIAN_POINT('Ctrl Pts',(42.5871755865899,-58.7052547141791,
-38.9300801001639));
#263942=CARTESIAN_POINT('Ctrl Pts',(42.5687782262919,-58.6730091989553,
-38.9210704098267));
#263943=CARTESIAN_POINT('Ctrl Pts',(42.5334651607083,-58.6074544045328,
-38.9031098430389));
#263944=CARTESIAN_POINT('Ctrl Pts',(42.5165536092555,-58.5741539456505,
-38.8941612806853));
#263945=CARTESIAN_POINT('Ctrl Pts',(42.4842288284689,-58.5064298905342,
-38.8763156605622));
#263946=CARTESIAN_POINT('Ctrl Pts',(42.4689425110757,-58.4722695790417,
-38.8674881957913));
#263947=CARTESIAN_POINT('Ctrl Pts',(42.4401223524774,-58.4034275394388,
-38.850038446285));
#263948=CARTESIAN_POINT('Ctrl Pts',(42.4265830216104,-58.3687342215786,
-38.8414131147228));
#263949=CARTESIAN_POINT('Ctrl Pts',(42.4012287621092,-58.2988104506425,
-38.8243608135095));
#263950=CARTESIAN_POINT('Ctrl Pts',(42.3894137311741,-58.2635796417037,
-38.8159337609721));
#263951=CARTESIAN_POINT('Ctrl Pts',(42.3565460901882,-58.1570828792368,
-38.7909502174193));
#263952=CARTESIAN_POINT('Ctrl Pts',(42.3380647593969,-58.08501193977,-38.774690108199));
#263953=CARTESIAN_POINT('Ctrl Pts',(42.3155659483831,-57.9752818676448,
-38.7509104698803));
#263954=CARTESIAN_POINT('Ctrl Pts',(42.3089373897852,-57.9384266392251,
-38.7430843371387));
#263955=CARTESIAN_POINT('Ctrl Pts',(42.2974579811028,-57.8641787720779,
-38.7276438085931));
#263956=CARTESIAN_POINT('Ctrl Pts',(42.2926014835326,-57.8267325462403,
-38.7200187268755));
#263957=CARTESIAN_POINT('Ctrl Pts',(42.2847289598988,-57.7514526438499,
-38.7050196122677));
#263958=CARTESIAN_POINT('Ctrl Pts',(42.2817363203014,-57.7138760098677,
-38.6976961901952));
#263959=CARTESIAN_POINT('Ctrl Pts',(42.2775969609554,-57.6387185090426,
-38.6833719825733));
#263960=CARTESIAN_POINT('Ctrl Pts',(42.2764524982459,-57.601159318647,-38.6763755134769));
#263961=CARTESIAN_POINT('Ctrl Pts',(42.2757725868838,-57.4885396265684,
-38.6558809090593));
#263962=CARTESIAN_POINT('Ctrl Pts',(42.2789845110076,-57.4135368784203,
-38.6428764616153));
#263963=CARTESIAN_POINT('Ctrl Pts',(42.2893332825795,-57.3011476865308,
-38.6243712438732));
#263964=CARTESIAN_POINT('Ctrl Pts',(42.2937061365005,-57.2637038084211,
-38.6183700063105));
#263965=CARTESIAN_POINT('Ctrl Pts',(42.3043246703777,-57.1888547487219,
-38.6067078983536));
#263966=CARTESIAN_POINT('Ctrl Pts',(42.3105742804476,-57.1514345489241,
-38.6010450084679));
#263967=CARTESIAN_POINT('Ctrl Pts',(42.3249703860378,-57.0766935224097,
-38.5900761598925));
#263968=CARTESIAN_POINT('Ctrl Pts',(42.3331591716861,-57.0392159776392,
-38.5847493692274));
#263969=CARTESIAN_POINT('Ctrl Pts',(42.3512949539204,-56.9651221376192,
-38.5745672487527));
#263970=CARTESIAN_POINT('Ctrl Pts',(42.3612585832142,-56.9283882008754,
-38.5696935766092));
#263971=CARTESIAN_POINT('Ctrl Pts',(42.382946766925,-56.8555905629784,-38.5603847482528));
#263972=CARTESIAN_POINT('Ctrl Pts',(42.3946724253985,-56.8195179869541,
-38.5559481805345));
#263973=CARTESIAN_POINT('Ctrl Pts',(42.4198760421967,-56.7480211971863,
-38.5475091590052));
#263974=CARTESIAN_POINT('Ctrl Pts',(42.433354009658,-56.7125969868972,-38.5435067067598));
#263975=CARTESIAN_POINT('Ctrl Pts',(42.4620643367001,-56.6423975987555,
-38.5359374532668));
#263976=CARTESIAN_POINT('Ctrl Pts',(42.4772966787996,-56.6076224144876,
-38.53237064715));
#263977=CARTESIAN_POINT('Ctrl Pts',(42.5095307755788,-56.5387265419139,
-38.5256773524591));
#263978=CARTESIAN_POINT('Ctrl Pts',(42.5265324846308,-56.5046058367601,
-38.5225508521777));
#263979=CARTESIAN_POINT('Ctrl Pts',(42.5623338208904,-56.4370293846275,
-38.5167461114759));
#263980=CARTESIAN_POINT('Ctrl Pts',(42.5811223378823,-56.4035922992139,
-38.51406925145));
#263981=CARTESIAN_POINT('Ctrl Pts',(42.6205844974323,-56.3373241879144,
-38.5091696849532));
#263982=CARTESIAN_POINT('Ctrl Pts',(42.6411082002799,-56.3047465778678,
-38.5069658948843));
#263983=CARTESIAN_POINT('Ctrl Pts',(42.7048067750791,-56.2090283214366,
-38.5011108038064));
#263984=CARTESIAN_POINT('Ctrl Pts',(42.7502234311298,-56.1476408508883,
-38.4981889837996));
#263985=CARTESIAN_POINT('Ctrl Pts',(42.8467942109284,-56.0297655406316,
-38.4942909959747));
#263986=CARTESIAN_POINT('Ctrl Pts',(42.89797152087,-55.9732420296543,-38.493312543871));
#263987=CARTESIAN_POINT('Ctrl Pts',(42.9790570362859,-55.8921695682654,
-38.4933149308443));
#263988=CARTESIAN_POINT('Ctrl Pts',(43.0068373921125,-55.8657400703683,
-38.4935621456146));
#263989=CARTESIAN_POINT('Ctrl Pts',(43.0495800471754,-55.8270637537312,
-38.4943062517503));
#263990=CARTESIAN_POINT('Ctrl Pts',(43.0640221885071,-55.8143203297415,
-38.4946170972135));
#263991=CARTESIAN_POINT('Ctrl Pts',(43.0932714605165,-55.7891564041938,
-38.4953646355488));
#263992=CARTESIAN_POINT('Ctrl Pts',(43.1080901116598,-55.7767277717167,
-38.4958019484811));
#263993=CARTESIAN_POINT('Ctrl Pts',(43.1528523151143,-55.7401326939816,
-38.4972962428884));
#263994=CARTESIAN_POINT('Ctrl Pts',(43.1831712256444,-55.7165901141018,
-38.4985359777345));
#263995=CARTESIAN_POINT('Ctrl Pts',(43.244758341421,-55.671169126854,-38.501493078153));
#263996=CARTESIAN_POINT('Ctrl Pts',(43.2760240772567,-55.6492920651712,
-38.5032102375714));
#263997=CARTESIAN_POINT('Ctrl Pts',(43.3712176334144,-55.58612549871,-38.5090666032762));
#263998=CARTESIAN_POINT('Ctrl Pts',(43.4365388184857,-55.5472953546232,
-38.5139092517118));
#263999=CARTESIAN_POINT('Ctrl Pts',(43.5372923366523,-55.4939420358375,
-38.5225683917069));
#264000=CARTESIAN_POINT('Ctrl Pts',(43.5713395844727,-55.476974296143,-38.5256876830023));
#264001=CARTESIAN_POINT('Ctrl Pts',(43.6403672791554,-55.4446857453381,
-38.5323950948992));
#264002=CARTESIAN_POINT('Ctrl Pts',(43.6753577621025,-55.4293619873053,
-38.5359845082588));
#264003=CARTESIAN_POINT('Ctrl Pts',(43.7462462014538,-55.4003985293068,
-38.5436332514696));
#264004=CARTESIAN_POINT('Ctrl Pts',(43.7822717715004,-55.3867204163754,
-38.5477088311098));
#264005=CARTESIAN_POINT('Ctrl Pts',(43.8543821706563,-55.3613797550828,
-38.5562345876408));
#264006=CARTESIAN_POINT('Ctrl Pts',(43.8906224054099,-55.3496490529759,
-38.5607006893241));
#264007=CARTESIAN_POINT('Ctrl Pts',(43.963378182051,-55.3280633077297,-38.5700203534958));
#264008=CARTESIAN_POINT('Ctrl Pts',(43.9999084017295,-55.3182018771171,
-38.5748754295458));
#264009=CARTESIAN_POINT('Ctrl Pts',(44.0732691659691,-55.3003143634305,
-38.5849691522959));
#264010=CARTESIAN_POINT('Ctrl Pts',(44.1100997173916,-55.2922883228605,
-38.5902078085425));
#264011=CARTESIAN_POINT('Ctrl Pts',(44.1840590840081,-55.278057933328,-38.6010646496354));
#264012=CARTESIAN_POINT('Ctrl Pts',(44.2211879014379,-55.2718535986756,
-38.606682838198));
#264013=CARTESIAN_POINT('Ctrl Pts',(44.2957439119556,-55.261266200021,-38.6182974286047));
#264014=CARTESIAN_POINT('Ctrl Pts',(44.3331711028503,-55.2568831233685,
-38.6242938286285));
#264015=CARTESIAN_POINT('Ctrl Pts',(44.4083261451804,-55.2499510424672,
-38.6366662370891));
#264016=CARTESIAN_POINT('Ctrl Pts',(44.4460560558118,-55.2474028685688,
-38.6430427650303));
#264017=CARTESIAN_POINT('Ctrl Pts',(44.5218128109665,-55.2441636047241,
-38.6561775093914));
#264018=CARTESIAN_POINT('Ctrl Pts',(44.5599089520781,-55.2434808242815,
-38.66294972511));
#264019=CARTESIAN_POINT('Ctrl Pts',(44.6354869653286,-55.2439910765326,
-38.6767129557532));
#264020=CARTESIAN_POINT('Ctrl Pts',(44.6731457008971,-55.245173978475,-38.6837341823244));
#264021=CARTESIAN_POINT('Ctrl Pts',(44.7481014918668,-55.2493619747848,
-38.6980304133054));
#264022=CARTESIAN_POINT('Ctrl Pts',(44.7854165987361,-55.2523661957112,
-38.7053085311543));
#264023=CARTESIAN_POINT('Ctrl Pts',(44.8968808213,-55.2640710443033,-38.7275255991979));
#264024=CARTESIAN_POINT('Ctrl Pts',(44.970549832836,-55.2754583054948,-38.7428464642802));
#264025=CARTESIAN_POINT('Ctrl Pts',(45.0801002188279,-55.2978810234077,
-38.766580365083));
#264026=CARTESIAN_POINT('Ctrl Pts',(45.1164578950735,-55.3062470347631,
-38.7746173156054));
#264027=CARTESIAN_POINT('Ctrl Pts',(45.1888527862828,-55.324776345739,-38.7909433983534));
#264028=CARTESIAN_POINT('Ctrl Pts',(45.2248832273146,-55.3349380647777,
-38.7992310297367));
#264029=CARTESIAN_POINT('Ctrl Pts',(45.2966462910748,-55.3570913037395,
-38.8160671574568));
#264030=CARTESIAN_POINT('Ctrl Pts',(45.3323639181915,-55.3690862993212,
-38.8246135268356));
#264031=CARTESIAN_POINT('Ctrl Pts',(45.4027951684834,-55.3946744168502,
-38.8417981416725));
#264032=CARTESIAN_POINT('Ctrl Pts',(45.4376370576062,-55.4083059928131,
-38.8504662832915));
#264033=CARTESIAN_POINT('Ctrl Pts',(45.5065020448728,-55.4372015304471,
-38.8679331079831));
#264034=CARTESIAN_POINT('Ctrl Pts',(45.5405385294939,-55.4524695704278,
-38.8767349230064));
#264035=CARTESIAN_POINT('Ctrl Pts',(45.6078227830677,-55.4846397608258,
-38.8944741023142));
#264036=CARTESIAN_POINT('Ctrl Pts',(45.6410705511329,-55.5015419127995,
-38.9034114672202));
#264037=CARTESIAN_POINT('Ctrl Pts',(45.7067750180478,-55.5369855589402,
-38.9214215570149));
#264038=CARTESIAN_POINT('Ctrl Pts',(45.7392220186752,-55.5555211850666,
-38.9304915153049));
#264039=CARTESIAN_POINT('Ctrl Pts',(45.8033557152909,-55.5942721902847,
-38.9487787321192));
#264040=CARTESIAN_POINT('Ctrl Pts',(45.8348444017589,-55.6143675059359,
-38.9579394566731));
#264041=CARTESIAN_POINT('Ctrl Pts',(45.9274100185651,-55.676658878309,-38.9854158611437));
#264042=CARTESIAN_POINT('Ctrl Pts',(45.9867611219468,-55.7209352921753,
-39.0037703086594));
#264043=CARTESIAN_POINT('Ctrl Pts',(46.1007338204162,-55.8148102176407,
-39.0405190314579));
#264044=CARTESIAN_POINT('Ctrl Pts',(46.1553754636135,-55.8644173555222,
-39.0589184365119));
#264045=CARTESIAN_POINT('Ctrl Pts',(46.2338037667526,-55.9428521113138,
-39.0865551406703));
#264046=CARTESIAN_POINT('Ctrl Pts',(46.2593566149882,-55.9696687163404,
-39.0957736628265));
#264047=CARTESIAN_POINT('Ctrl Pts',(46.3092668490953,-56.0246630354032,
-39.1142235862602));
#264048=CARTESIAN_POINT('Ctrl Pts',(46.3336138592955,-56.0528283934937,
-39.1234509944141));
#264049=CARTESIAN_POINT('Ctrl Pts',(46.3692509706587,-56.0961546799093,
-39.1373141185695));
#264050=CARTESIAN_POINT('Ctrl Pts',(46.3809719979937,-56.1107655086548,
-39.1419349989914));
#264051=CARTESIAN_POINT('Ctrl Pts',(46.4039851397009,-56.1401806556231,
-39.1511314216979));
#264052=CARTESIAN_POINT('Ctrl Pts',(46.4153002334237,-56.155012646864,-39.1557158582529));
#264053=CARTESIAN_POINT('Ctrl Pts',(46.4486370533476,-56.1998309912202,
-39.1694130631373));
#264054=CARTESIAN_POINT('Ctrl Pts',(46.4700835531906,-56.2301795174735,
-39.1784825503139));
#264055=CARTESIAN_POINT('Ctrl Pts',(46.5320719588418,-56.3225583858835,
-39.2054898182239));
#264056=CARTESIAN_POINT('Ctrl Pts',(46.5703036405633,-56.3859631464818,
-39.2232408011316));
#264057=CARTESIAN_POINT('Ctrl Pts',(46.6230137769529,-56.4837650818566,
-39.2494850822324));
#264058=CARTESIAN_POINT('Ctrl Pts',(46.6398106251204,-56.5168167226216,
-39.2581697490099));
#264059=CARTESIAN_POINT('Ctrl Pts',(46.6718447361749,-56.5838294852714,
-39.2754118634509));
#264060=CARTESIAN_POINT('Ctrl Pts',(46.6870820781819,-56.6177905613574,
-39.2839693163248));
#264061=CARTESIAN_POINT('Ctrl Pts',(46.7159730314734,-56.686636048537,-39.3009558317863));
#264062=CARTESIAN_POINT('Ctrl Pts',(46.7296188510695,-56.7214992835749,
-39.3093798666901));
#264063=CARTESIAN_POINT('Ctrl Pts',(46.7553217489119,-56.7922546342832,
-39.3261176089799));
#264064=CARTESIAN_POINT('Ctrl Pts',(46.767299743662,-56.8279354846841,-39.3343809236343));
#264065=CARTESIAN_POINT('Ctrl Pts',(46.8004531002449,-56.9353633944232,
-39.3587371078895));
#264066=CARTESIAN_POINT('Ctrl Pts',(46.8189796004616,-57.0077635585741,
-39.3744657569928));
#264067=CARTESIAN_POINT('Ctrl Pts',(46.848916262609,-57.1540080970469,-39.4048997739107));
#264068=CARTESIAN_POINT('Ctrl Pts',(46.8603369955464,-57.2278698710425,
-39.4196100030402));
#264069=CARTESIAN_POINT('Ctrl Pts',(46.8720665256814,-57.3397812953029,
-39.4409093089087));
#264070=CARTESIAN_POINT('Ctrl Pts',(46.8750748009162,-57.3772756957559,
-39.4478818833461));
#264071=CARTESIAN_POINT('Ctrl Pts',(46.879254346672,-57.452637038775,-39.4615663391791));
#264072=CARTESIAN_POINT('Ctrl Pts',(46.880425925028,-57.4905390917853,-39.4682843057428));
#264073=CARTESIAN_POINT('Ctrl Pts',(46.8808838257092,-57.5666104472174,
-39.4814341408916));
#264074=CARTESIAN_POINT('Ctrl Pts',(46.8801709150999,-57.6044914055267,
-39.4878166125941));
#264075=CARTESIAN_POINT('Ctrl Pts',(46.8768914392193,-57.6800598105232,
-39.5002230596849));
#264076=CARTESIAN_POINT('Ctrl Pts',(46.8743247149934,-57.7177285118847,
-39.506243785591));
#264077=CARTESIAN_POINT('Ctrl Pts',(46.8638676192418,-57.8303908579074,
-39.5237649045219));
#264078=CARTESIAN_POINT('Ctrl Pts',(46.853226416258,-57.905041503381,-39.5347254344493));
#264079=CARTESIAN_POINT('Ctrl Pts',(46.8317335819185,-58.0163268627736,
-39.550087285924));
#264080=CARTESIAN_POINT('Ctrl Pts',(46.8236460045766,-58.0533066998131,
-39.5550277871486));
#264081=CARTESIAN_POINT('Ctrl Pts',(46.8055990609215,-58.127032513964,-39.5645446852094));
#264082=CARTESIAN_POINT('Ctrl Pts',(46.7956340174415,-58.1637938739027,
-39.5691227370151));
#264083=CARTESIAN_POINT('Ctrl Pts',(46.7738161820537,-58.2370162297126,
-39.5779015917596));
#264084=CARTESIAN_POINT('Ctrl Pts',(46.7619036769789,-58.2736352495457,
-39.582119165218));
#264085=CARTESIAN_POINT('Ctrl Pts',(46.7364060204878,-58.3458256235152,
-39.5900871303177));
#264086=CARTESIAN_POINT('Ctrl Pts',(46.7227944358822,-58.3815079540758,
-39.5938519714545));
#264087=CARTESIAN_POINT('Ctrl Pts',(46.6938811083112,-58.4520118830205,
-39.6009443323402));
#264088=CARTESIAN_POINT('Ctrl Pts',(46.6785776728307,-58.4868414029238,
-39.6042729162555));
#264089=CARTESIAN_POINT('Ctrl Pts',(46.6462897807642,-58.5556617478733,
-39.6104988832622));
#264090=CARTESIAN_POINT('Ctrl Pts',(46.6293053112816,-58.5896525665271,
-39.6133962624303));
#264091=CARTESIAN_POINT('Ctrl Pts',(46.5936553992581,-58.656795488418,-39.6187605166456));
#264092=CARTESIAN_POINT('Ctrl Pts',(46.5749899695051,-58.6899475980592,
-39.621227394548));
#264093=CARTESIAN_POINT('Ctrl Pts',(46.5359657888858,-58.7554069047812,
-39.6257280783136));
#264094=CARTESIAN_POINT('Ctrl Pts',(46.5156070776159,-58.7877141216242,
-39.6277618940797));
#264095=CARTESIAN_POINT('Ctrl Pts',(46.4731711272442,-58.8514710379442,
-39.6313905083909));
#264096=CARTESIAN_POINT('Ctrl Pts',(46.4511086572017,-58.8829006656694,
-39.6329844048618));
#264097=CARTESIAN_POINT('Ctrl Pts',(46.4051673627461,-58.9449633365352,
-39.6357272934367));
#264098=CARTESIAN_POINT('Ctrl Pts',(46.3814480364632,-58.9753776243305,
-39.6368662047246));
#264099=CARTESIAN_POINT('Ctrl Pts',(46.3084069318146,-59.0643493506752,
-39.6395760682405));
#264100=CARTESIAN_POINT('Ctrl Pts',(46.2570408245348,-59.1209150834389,
-39.640460323304));
#264101=CARTESIAN_POINT('Ctrl Pts',(46.1491380135578,-59.2285445031963,
-39.6404138262961));
#264102=CARTESIAN_POINT('Ctrl Pts',(46.0925836924519,-59.2796343454175,
-39.6394845260398));
#264103=CARTESIAN_POINT('Ctrl Pts',(46.0038529790884,-59.3521266547998,
-39.6367222836243));
#264104=CARTESIAN_POINT('Ctrl Pts',(45.9736068426425,-59.3756113980778,
-39.6355720611743));
#264105=CARTESIAN_POINT('Ctrl Pts',(45.9272657300626,-59.4097723979471,
-39.6334997173803));
#264106=CARTESIAN_POINT('Ctrl Pts',(45.9116419552091,-59.4209913255156,
-39.6327502257672));
#264107=CARTESIAN_POINT('Ctrl Pts',(45.8800805125468,-59.4430611241672,
-39.631135078801));
#264108=CARTESIAN_POINT('Ctrl Pts',(45.8641078101822,-59.4539348059586,
-39.6302673429044));
#264109=CARTESIAN_POINT('Ctrl Pts',(45.8159067495927,-59.4858697254365,
-39.627498969587));
#264110=CARTESIAN_POINT('Ctrl Pts',(45.7834097421985,-59.5062439414457,
-39.6254354520693));
#264111=CARTESIAN_POINT('Ctrl Pts',(45.7176331363943,-59.5452482370454,
-39.6208772711381));
#264112=CARTESIAN_POINT('Ctrl Pts',(45.6843658790545,-59.5638704785003,
-39.6183833740186));
#264113=CARTESIAN_POINT('Ctrl Pts',(45.583444956553,-59.6171384596421,-39.6102663728808));
#264114=CARTESIAN_POINT('Ctrl Pts',(45.5146744890979,-59.6491909190302,
-39.6040093397971));
#264115=CARTESIAN_POINT('Ctrl Pts',(45.4093033900763,-59.6921245149476,
-39.5933616765527));
#264116=CARTESIAN_POINT('Ctrl Pts',(45.3738098248103,-59.7055767269039,
-39.589601735465));
#264117=CARTESIAN_POINT('Ctrl Pts',(45.3020779039712,-59.7307512611409,
-39.5816566274386));
#264118=CARTESIAN_POINT('Ctrl Pts',(45.2658207530533,-59.7424780352937,
-39.5774690099792));
#264119=CARTESIAN_POINT('Ctrl Pts',(45.1926264881235,-59.7641596514461,
-39.568671457456));
#264120=CARTESIAN_POINT('Ctrl Pts',(45.1555074107078,-59.7741563012212,
-39.5640375608608));
#264121=CARTESIAN_POINT('Ctrl Pts',(45.0812568665445,-59.7921791067291,
-39.5544265147621));
#264122=CARTESIAN_POINT('Ctrl Pts',(45.0440817477085,-59.8002278395378,
-39.549445784008));
#264123=CARTESIAN_POINT('Ctrl Pts',(44.9696261228349,-59.8144411184057,
-39.5391389954541));
#264124=CARTESIAN_POINT('Ctrl Pts',(44.9323469981084,-59.8206062349248,
-39.5338132734696));
#264125=CARTESIAN_POINT('Ctrl Pts',(44.8576879269541,-59.8310834316045,
-39.5228216022339));
#264126=CARTESIAN_POINT('Ctrl Pts',(44.820307974904,-59.835395411627,-39.517155635792));
#264127=CARTESIAN_POINT('Ctrl Pts',(44.708018468269,-59.8455761125523,-39.4996502226722));
#264128=CARTESIAN_POINT('Ctrl Pts',(44.6329372354107,-59.8486932135334,
-39.487300131016));
#264129=CARTESIAN_POINT('Ctrl Pts',(44.5200834526131,-59.8478515646575,
-39.4677634251584));
#264130=CARTESIAN_POINT('Ctrl Pts',(44.4823810949366,-59.846645023154,-39.4610735946688));
#264131=CARTESIAN_POINT('Ctrl Pts',(44.4258051146807,-59.8434395219468,
-39.4507882880789));
#264132=CARTESIAN_POINT('Ctrl Pts',(44.4069254653865,-59.8421361859431,
-39.4473147364688));
#264133=CARTESIAN_POINT('Ctrl Pts',(44.369137659976,-59.8390582137137,-39.440279278016));
#264134=CARTESIAN_POINT('Ctrl Pts',(44.3502459404613,-59.8372839246163,
-39.4367202553176));
#264135=CARTESIAN_POINT('Ctrl Pts',(44.293847621291,-59.8312837400404,-39.4259705727343));
#264136=CARTESIAN_POINT('Ctrl Pts',(44.2565162798962,-59.8263769106602,
-39.4186892078256));
#264137=CARTESIAN_POINT('Ctrl Pts',(44.1823865447478,-59.8147890715068,
-39.4039021067728));
#264138=CARTESIAN_POINT('Ctrl Pts',(44.1455864865373,-59.8081084264739,
-39.3963961507539));
#264139=CARTESIAN_POINT('Ctrl Pts',(44.035968213109,-59.7854494824361,-39.3735449366146));
#264140=CARTESIAN_POINT('Ctrl Pts',(43.9639303513108,-59.7668593620139,
-39.3578669828429));
#264141=CARTESIAN_POINT('Ctrl Pts',(43.8219158998824,-59.7227862146117,
-39.3256250679982));
#264142=CARTESIAN_POINT('Ctrl Pts',(43.7519290479738,-59.6972943553091,
-39.3090577736246));
#264143=CARTESIAN_POINT('Ctrl Pts',(43.6657831707481,-59.6610676287994,
-39.287788993689));
#264144=CARTESIAN_POINT('Ctrl Pts',(43.6486106593656,-59.6535962458977,
-39.2835040729686));
#264145=CARTESIAN_POINT('Ctrl Pts',(43.6144192936767,-59.6382222836229,
-39.2748824632482));
#264146=CARTESIAN_POINT('Ctrl Pts',(43.5973665746684,-59.6303022827778,
-39.2705368372966));
#264147=CARTESIAN_POINT('Ctrl Pts',(43.5465994091571,-59.6059619503591,
-39.2574615900898));
#264148=CARTESIAN_POINT('Ctrl Pts',(43.513329290924,-59.5889931579325,-39.2487084716788));
#264149=CARTESIAN_POINT('Ctrl Pts',(43.4805770970857,-59.5712767993712,
-39.2399079805728));
#264150=CARTESIAN_POINT('Ctrl Pts',(43.5555688340535,-59.234132410514,-39.6401263014865));
#264151=CARTESIAN_POINT('Ctrl Pts',(43.5271058320223,-59.2187187670665,
-39.6313258103806));
#264152=CARTESIAN_POINT('Ctrl Pts',(43.4991052518144,-59.2026624632065,
-39.6224818464091));
#264153=CARTESIAN_POINT('Ctrl Pts',(43.4440152092532,-59.1692838342202,
-39.6047076566125));
#264154=CARTESIAN_POINT('Ctrl Pts',(43.4169257916853,-59.1519614464883,
-39.5957774275967));
#264155=CARTESIAN_POINT('Ctrl Pts',(43.3370134128483,-59.0981105486717,
-39.5688575945475));
#264156=CARTESIAN_POINT('Ctrl Pts',(43.285543443658,-59.0597022696331,-39.5507390702919));
#264157=CARTESIAN_POINT('Ctrl Pts',(43.1862320317398,-58.9778459096351,
-39.5141533290284));
#264158=CARTESIAN_POINT('Ctrl Pts',(43.1383856292385,-58.9343938929635,
-39.4956843164029));
#264159=CARTESIAN_POINT('Ctrl Pts',(43.0464616123337,-58.8422984996412,
-39.4583915857769));
#264160=CARTESIAN_POINT('Ctrl Pts',(43.0031145131512,-58.7943886576613,
-39.4398645717558));
#264161=CARTESIAN_POINT('Ctrl Pts',(42.9214555277954,-58.694943387258,-39.4030322323516));
#264162=CARTESIAN_POINT('Ctrl Pts',(42.8831481853276,-58.6434115048881,
-39.3847285385198));
#264163=CARTESIAN_POINT('Ctrl Pts',(42.8294517117175,-58.5634128288845,
-39.3574423437733));
#264164=CARTESIAN_POINT('Ctrl Pts',(42.8121813055727,-58.5362957447343,
-39.348375225579));
#264165=CARTESIAN_POINT('Ctrl Pts',(42.7789076210676,-58.4811523680481,
-39.3302984210776));
#264166=CARTESIAN_POINT('Ctrl Pts',(42.7629042791111,-58.453126121455,-39.3212887307404));
#264167=CARTESIAN_POINT('Ctrl Pts',(42.7321838794578,-58.3961505394088,
-39.3033281639527));
#264168=CARTESIAN_POINT('Ctrl Pts',(42.7174704361412,-58.3672088695202,
-39.294379601599));
#264169=CARTESIAN_POINT('Ctrl Pts',(42.689344263748,-58.3083508831849,-39.2765339814759));
#264170=CARTESIAN_POINT('Ctrl Pts',(42.6760419603829,-58.2786633846033,
-39.2677065167051));
#264171=CARTESIAN_POINT('Ctrl Pts',(42.6509592537523,-58.2188366747008,
-39.2502567671988));
#264172=CARTESIAN_POINT('Ctrl Pts',(42.6391740738076,-58.1886873909247,
-39.2416314356366));
#264173=CARTESIAN_POINT('Ctrl Pts',(42.6171012127209,-58.1279234454293,
-39.2245791344233));
#264174=CARTESIAN_POINT('Ctrl Pts',(42.6068134424726,-58.0973084744714,
-39.2161520818859));
#264175=CARTESIAN_POINT('Ctrl Pts',(42.5781884268765,-58.0047666909868,
-39.1911685383331));
#264176=CARTESIAN_POINT('Ctrl Pts',(42.5620841140238,-57.9421424384458,
-39.1749084291127));
#264177=CARTESIAN_POINT('Ctrl Pts',(42.542463526333,-57.8467994028925,-39.151128790794));
#264178=CARTESIAN_POINT('Ctrl Pts',(42.5366797518884,-57.8147770619196,
-39.1433026580524));
#264179=CARTESIAN_POINT('Ctrl Pts',(42.5266559992737,-57.7502668409957,
-39.1278621295069));
#264180=CARTESIAN_POINT('Ctrl Pts',(42.5224110777105,-57.7177324038865,
-39.1202370477892));
#264181=CARTESIAN_POINT('Ctrl Pts',(42.5155196559844,-57.652328321118,-39.1052379331815));
#264182=CARTESIAN_POINT('Ctrl Pts',(42.5128936513538,-57.6196819945454,
-39.0979145111089));
#264183=CARTESIAN_POINT('Ctrl Pts',(42.5092450689372,-57.5543870588034,
-39.0835903034871));
#264184=CARTESIAN_POINT('Ctrl Pts',(42.5082244669781,-57.5217572823762,
-39.0765938343906));
#264185=CARTESIAN_POINT('Ctrl Pts',(42.5075544726465,-57.4239203249817,
-39.0560992299731));
#264186=CARTESIAN_POINT('Ctrl Pts',(42.5102915889976,-57.3587654025749,
-39.043094782529));
#264187=CARTESIAN_POINT('Ctrl Pts',(42.5192017059061,-57.2611370939764,
-39.0245895647869));
#264188=CARTESIAN_POINT('Ctrl Pts',(42.522973744208,-57.2286116980208,-39.0185883272243));
#264189=CARTESIAN_POINT('Ctrl Pts',(42.5321446715301,-57.163595959261,-39.0069262192674));
#264190=CARTESIAN_POINT('Ctrl Pts',(42.5375469638235,-57.1310925726591,
-39.0012633293817));
#264191=CARTESIAN_POINT('Ctrl Pts',(42.5499993493055,-57.0661735854286,
-38.9902944808063));
#264192=CARTESIAN_POINT('Ctrl Pts',(42.5570860671587,-57.033621871048,-38.9849676901412));
#264193=CARTESIAN_POINT('Ctrl Pts',(42.5727873916265,-56.9692679908499,
-38.9747855696665));
#264194=CARTESIAN_POINT('Ctrl Pts',(42.5814163631431,-56.9373636386801,
-38.969911897523));
#264195=CARTESIAN_POINT('Ctrl Pts',(42.6002044275548,-56.8741385448439,
-38.9606030691666));
#264196=CARTESIAN_POINT('Ctrl Pts',(42.6103644732139,-56.8428100941247,
-38.9561665014482));
#264197=CARTESIAN_POINT('Ctrl Pts',(42.6322071886494,-56.7807177933216,
-38.947727479919));
#264198=CARTESIAN_POINT('Ctrl Pts',(42.6438898663583,-56.7499539462467,
-38.9437250276736));
#264199=CARTESIAN_POINT('Ctrl Pts',(42.6687796751254,-56.6889914341204,
-38.9361557741806));
#264200=CARTESIAN_POINT('Ctrl Pts',(42.6819867909859,-56.658792763486,-38.9325889680638));
#264201=CARTESIAN_POINT('Ctrl Pts',(42.7099385396534,-56.5989653584369,
-38.9258956733729));
#264202=CARTESIAN_POINT('Ctrl Pts',(42.7246831328038,-56.5693366093568,
-38.9227691730914));
#264203=CARTESIAN_POINT('Ctrl Pts',(42.7557346180894,-56.510658153127,-38.9169644323897));
#264204=CARTESIAN_POINT('Ctrl Pts',(42.7720318723629,-56.4816246493906,
-38.9142875723637));
#264205=CARTESIAN_POINT('Ctrl Pts',(42.8062644061236,-56.4240855769913,
-38.909388005867));
#264206=CARTESIAN_POINT('Ctrl Pts',(42.8240696175392,-56.3958000441502,
-38.9071842157982));
#264207=CARTESIAN_POINT('Ctrl Pts',(42.8793348313062,-56.3126951718662,
-38.9013291247197));
#264208=CARTESIAN_POINT('Ctrl Pts',(42.9187435313913,-56.259400561899,-38.8984073047134));
#264209=CARTESIAN_POINT('Ctrl Pts',(43.0025486921197,-56.1570720601927,
-38.8945093168885));
#264210=CARTESIAN_POINT('Ctrl Pts',(43.0469652685517,-56.1080071974563,
-38.8935308647847));
#264211=CARTESIAN_POINT('Ctrl Pts',(43.1173453422034,-56.0376384736874,
-38.8935332517581));
#264212=CARTESIAN_POINT('Ctrl Pts',(43.1414589512102,-56.0146993759999,
-38.8937804665284));
#264213=CARTESIAN_POINT('Ctrl Pts',(43.178561457947,-55.981132370469,-38.8945245726641));
#264214=CARTESIAN_POINT('Ctrl Pts',(43.1910981146608,-55.9700726732162,
-38.8948354181272));
#264215=CARTESIAN_POINT('Ctrl Pts',(43.2164887431531,-55.9482340721744,
-38.8955829564625));
#264216=CARTESIAN_POINT('Ctrl Pts',(43.2293527169208,-55.937448113455,-38.8960202693949));
#264217=CARTESIAN_POINT('Ctrl Pts',(43.2682112021707,-55.9056905804555,
-38.8975145638021));
#264218=CARTESIAN_POINT('Ctrl Pts',(43.2945322632909,-55.8852612363732,
-38.8987542986482));
#264219=CARTESIAN_POINT('Ctrl Pts',(43.3480003156045,-55.8458489068529,
-38.9017113990668));
#264220=CARTESIAN_POINT('Ctrl Pts',(43.3751451625608,-55.8268670886173,
-38.9034285584852));
#264221=CARTESIAN_POINT('Ctrl Pts',(43.457794616026,-55.772063647161,-38.90928492419));
#264222=CARTESIAN_POINT('Ctrl Pts',(43.5145115393775,-55.7383794675986,
-38.9141275726255));
#264223=CARTESIAN_POINT('Ctrl Pts',(43.6019985559746,-55.6921046980431,
-38.9227867126206));
#264224=CARTESIAN_POINT('Ctrl Pts',(43.6315635162974,-55.67738956075,-38.925906003916));
#264225=CARTESIAN_POINT('Ctrl Pts',(43.6915053978043,-55.6493906033967,
-38.932613415813));
#264226=CARTESIAN_POINT('Ctrl Pts',(43.7218910354095,-55.6361042305882,
-38.9362028291725));
#264227=CARTESIAN_POINT('Ctrl Pts',(43.7834519549885,-55.6109950253045,
-38.9438515723833));
#264228=CARTESIAN_POINT('Ctrl Pts',(43.8147380697121,-55.5991389154848,
-38.9479271520235));
#264229=CARTESIAN_POINT('Ctrl Pts',(43.8773633283321,-55.577177590229,-38.9564529085545));
#264230=CARTESIAN_POINT('Ctrl Pts',(43.9088374259754,-55.5670132823478,
-38.9609190102379));
#264231=CARTESIAN_POINT('Ctrl Pts',(43.9720262322937,-55.5483141725143,
-38.9702386744095));
#264232=CARTESIAN_POINT('Ctrl Pts',(44.003753687147,-55.5397738324173,-38.9750937504595));
#264233=CARTESIAN_POINT('Ctrl Pts',(44.0674709105135,-55.5242876491131,
-38.9851874732096));
#264234=CARTESIAN_POINT('Ctrl Pts',(44.0994606850175,-55.51734184284,-38.9904261294562));
#264235=CARTESIAN_POINT('Ctrl Pts',(44.1637007452764,-55.5050328545072,
-39.0012829705492));
#264236=CARTESIAN_POINT('Ctrl Pts',(44.1959510329844,-55.4996696848857,
-39.0069011591118));
#264237=CARTESIAN_POINT('Ctrl Pts',(44.2607122139946,-55.4905255962476,
-39.0185157495185));
#264238=CARTESIAN_POINT('Ctrl Pts',(44.2932231053838,-55.4867446662453,
-39.0245121495422));
#264239=CARTESIAN_POINT('Ctrl Pts',(44.358507484825,-55.4807761715604,-39.0368845580029));
#264240=CARTESIAN_POINT('Ctrl Pts',(44.3912827624034,-55.4785893296048,
-39.043261085944));
#264241=CARTESIAN_POINT('Ctrl Pts',(44.4570926895081,-55.4758289910908,
-39.0563958303051));
#264242=CARTESIAN_POINT('Ctrl Pts',(44.4901875455791,-55.475262761327,-39.0631680460238));
#264243=CARTESIAN_POINT('Ctrl Pts',(44.5558450459825,-55.4757592686521,
-39.076931276667));
#264244=CARTESIAN_POINT('Ctrl Pts',(44.5885613296957,-55.476813330479,-39.0839525032381));
#264245=CARTESIAN_POINT('Ctrl Pts',(44.6536810701527,-55.4805040184252,
-39.0982487342192));
#264246=CARTESIAN_POINT('Ctrl Pts',(44.6861002081385,-55.4831398985796,
-39.1055268520681));
#264247=CARTESIAN_POINT('Ctrl Pts',(44.7829416988568,-55.4933857216518,
-39.1277439201117));
#264248=CARTESIAN_POINT('Ctrl Pts',(44.8469489879605,-55.5033290244897,
-39.1430647851939));
#264249=CARTESIAN_POINT('Ctrl Pts',(44.9421358674272,-55.5228833885463,
-39.1667986859967));
#264250=CARTESIAN_POINT('Ctrl Pts',(44.9737272566983,-55.5301760197046,
-39.1748356365191));
#264251=CARTESIAN_POINT('Ctrl Pts',(45.0366329635135,-55.5463222396588,
-39.1911617192672));
#264252=CARTESIAN_POINT('Ctrl Pts',(45.0679413951409,-55.5551744507282,
-39.1994493506505));
#264253=CARTESIAN_POINT('Ctrl Pts',(45.1303008713406,-55.5744680900885,
-39.2162854783706));
#264254=CARTESIAN_POINT('Ctrl Pts',(45.1613388911671,-55.5849125268946,
-39.2248318477494));
#264255=CARTESIAN_POINT('Ctrl Pts',(45.2225438737999,-55.6071888828167,
-39.2420164625862));
#264256=CARTESIAN_POINT('Ctrl Pts',(45.2528222941887,-55.6190542948094,
-39.2506846042053));
#264257=CARTESIAN_POINT('Ctrl Pts',(45.3126689940191,-55.6442024946607,
-39.2681514288968));
#264258=CARTESIAN_POINT('Ctrl Pts',(45.3422489057867,-55.6574888345125,
-39.2769532439202));
#264259=CARTESIAN_POINT('Ctrl Pts',(45.4007247066096,-55.6854804145847,
-39.294692423228));
#264260=CARTESIAN_POINT('Ctrl Pts',(45.4296205949023,-55.7001856561536,
-39.303629788134));
#264261=CARTESIAN_POINT('Ctrl Pts',(45.4867262971545,-55.7310195886299,
-39.3216398779287));
#264262=CARTESIAN_POINT('Ctrl Pts',(45.5149276816543,-55.7471431755038,
-39.3307098362187));
#264263=CARTESIAN_POINT('Ctrl Pts',(45.5706711208682,-55.7808489297168,
-39.3489970530329));
#264264=CARTESIAN_POINT('Ctrl Pts',(45.5980410702153,-55.7983266659973,
-39.3581577775872));
#264265=CARTESIAN_POINT('Ctrl Pts',(45.6785013081512,-55.8525005642884,
-39.3856341820567));
#264266=CARTESIAN_POINT('Ctrl Pts',(45.7300937365428,-55.8910026267882,
-39.4039886295733));
#264267=CARTESIAN_POINT('Ctrl Pts',(45.8291734689818,-55.9726265658168,
-39.4407373523715));
#264268=CARTESIAN_POINT('Ctrl Pts',(45.8766781960947,-56.0157559494116,
-39.4591367574256));
#264269=CARTESIAN_POINT('Ctrl Pts',(45.9448676798055,-56.0839431609313,
-39.486773461584));
#264270=CARTESIAN_POINT('Ctrl Pts',(45.9670854652505,-56.1072552989447,
-39.4959919837403));
#264271=CARTESIAN_POINT('Ctrl Pts',(46.0104833820224,-56.1550611161397,
-39.514441907174));
#264272=CARTESIAN_POINT('Ctrl Pts',(46.0316544908778,-56.1795440550238,
-39.5236693153279));
#264273=CARTESIAN_POINT('Ctrl Pts',(46.0626444084099,-56.2172045128319,
-39.5375324394833));
#264274=CARTESIAN_POINT('Ctrl Pts',(46.0728372208042,-56.2299044661098,
-39.5421533199052));
#264275=CARTESIAN_POINT('Ctrl Pts',(46.0928503481787,-56.2554721633656,
-39.5513497426116));
#264276=CARTESIAN_POINT('Ctrl Pts',(46.1026906457484,-56.268363961677,-39.5559341791666));
#264277=CARTESIAN_POINT('Ctrl Pts',(46.1316831401522,-56.3073189842252,
-39.5696313840511));
#264278=CARTESIAN_POINT('Ctrl Pts',(46.150335839206,-56.3336964338945,-39.5787008712277));
#264279=CARTESIAN_POINT('Ctrl Pts',(46.2042522556268,-56.4139854185625,
-39.6057081391376));
#264280=CARTESIAN_POINT('Ctrl Pts',(46.2375098264188,-56.4690893442278,
-39.6234591220454));
#264281=CARTESIAN_POINT('Ctrl Pts',(46.2833691088139,-56.5540831173889,
-39.6497034031462));
#264282=CARTESIAN_POINT('Ctrl Pts',(46.2979840983916,-56.5828056408614,
-39.6583880699236));
#264283=CARTESIAN_POINT('Ctrl Pts',(46.3258597433761,-56.6410397267288,
-39.6756301843647));
#264284=CARTESIAN_POINT('Ctrl Pts',(46.3391204674906,-56.6705512493805,
-39.6841876372386));
#264285=CARTESIAN_POINT('Ctrl Pts',(46.3642666109142,-56.7303753620795,
-39.7011741527));
#264286=CARTESIAN_POINT('Ctrl Pts',(46.3761452467366,-56.7606695516432,
-39.7095981876039));
#264287=CARTESIAN_POINT('Ctrl Pts',(46.3985229292237,-56.8221506906604,
-39.7263359298937));
#264288=CARTESIAN_POINT('Ctrl Pts',(46.408953127825,-56.8531540648449,-39.7345992445483));
#264289=CARTESIAN_POINT('Ctrl Pts',(46.4378282073617,-56.9464971719099,
-39.7589554288027));
#264290=CARTESIAN_POINT('Ctrl Pts',(46.4539722273909,-57.0094025633998,
-39.7746840779066));
#264291=CARTESIAN_POINT('Ctrl Pts',(46.4800786523228,-57.1364634441695,
-39.8051180948244));
#264292=CARTESIAN_POINT('Ctrl Pts',(46.4900502528004,-57.200634055062,-39.8198283239538));
#264293=CARTESIAN_POINT('Ctrl Pts',(46.500315603497,-57.2978584721872,-39.8411276298225));
#264294=CARTESIAN_POINT('Ctrl Pts',(46.5029542464308,-57.3304316164207,
-39.8481002042598));
#264295=CARTESIAN_POINT('Ctrl Pts',(46.5066358246239,-57.3959003914897,
-39.8617846600929));
#264296=CARTESIAN_POINT('Ctrl Pts',(46.5076790508278,-57.4288265228613,
-39.8685026266565));
#264297=CARTESIAN_POINT('Ctrl Pts',(46.5081278097802,-57.4949097791684,
-39.8816524618054));
#264298=CARTESIAN_POINT('Ctrl Pts',(46.5075338158641,-57.5278164208752,
-39.8880349335079));
#264299=CARTESIAN_POINT('Ctrl Pts',(46.5047352860362,-57.5934604589744,
-39.9004413805986));
#264300=CARTESIAN_POINT('Ctrl Pts',(46.5025305994736,-57.6261815712493,
-39.9064621065048));
#264301=CARTESIAN_POINT('Ctrl Pts',(46.4935211674923,-57.7240445911198,
-39.9239832254356));
#264302=CARTESIAN_POINT('Ctrl Pts',(46.4843263421389,-57.7888868451408,
-39.9349437553631));
#264303=CARTESIAN_POINT('Ctrl Pts',(46.4657284705721,-57.88554690184,-39.9503056068378));
#264304=CARTESIAN_POINT('Ctrl Pts',(46.4587269718586,-57.9176662081948,
-39.9552461080624));
#264305=CARTESIAN_POINT('Ctrl Pts',(46.4430976792663,-57.9817005180905,
-39.9647630061231));
#264306=CARTESIAN_POINT('Ctrl Pts',(46.4344649635437,-58.0136288811654,
-39.9693410579289));
#264307=CARTESIAN_POINT('Ctrl Pts',(46.4155593362243,-58.0772235214093,
-39.9781199126733));
#264308=CARTESIAN_POINT('Ctrl Pts',(46.405234653673,-58.1090270368304,-39.9823374861317));
#264309=CARTESIAN_POINT('Ctrl Pts',(46.3831314756339,-58.1717229328585,
-39.9903054512315));
#264310=CARTESIAN_POINT('Ctrl Pts',(46.3713300900435,-58.2027117021187,
-39.9940702923682));
#264311=CARTESIAN_POINT('Ctrl Pts',(46.346258426029,-58.2639404804981,-40.001162653254));
#264312=CARTESIAN_POINT('Ctrl Pts',(46.3329866824905,-58.2941873699786,
-40.0044912371692));
#264313=CARTESIAN_POINT('Ctrl Pts',(46.3049822647675,-58.3539515341542,
-40.010717204176));
#264314=CARTESIAN_POINT('Ctrl Pts',(46.290249579368,-58.3834688032905,-40.0136145833441));
#264315=CARTESIAN_POINT('Ctrl Pts',(46.259323329411,-58.4417737040611,-40.0189788375594));
#264316=CARTESIAN_POINT('Ctrl Pts',(46.2431297759597,-58.470561341271,-40.0214457154618));
#264317=CARTESIAN_POINT('Ctrl Pts',(46.2092710685098,-58.5274015813425,
-40.0259463992273));
#264318=CARTESIAN_POINT('Ctrl Pts',(46.1916059489149,-58.5554542014027,
-40.0279802149935));
#264319=CARTESIAN_POINT('Ctrl Pts',(46.1547822130534,-58.6108134350802,
-40.0316088293047));
#264320=CARTESIAN_POINT('Ctrl Pts',(46.1356364139942,-58.6381026215683,
-40.0332027257756));
#264321=CARTESIAN_POINT('Ctrl Pts',(46.0957663843932,-58.6919878518662,
-40.0359456143505));
#264322=CARTESIAN_POINT('Ctrl Pts',(46.0751805717983,-58.7183939621751,
-40.0370845256383));
#264323=CARTESIAN_POINT('Ctrl Pts',(46.0117857527956,-58.7956381443108,
-40.0397943891545));
#264324=CARTESIAN_POINT('Ctrl Pts',(45.9671995057833,-58.8447447093681,
-40.0406786442178));
#264325=CARTESIAN_POINT('Ctrl Pts',(45.8735317190067,-58.9381748222192,
-40.0406321472099));
#264326=CARTESIAN_POINT('Ctrl Pts',(45.8244348914145,-58.9825210802309,
-40.0397028469535));
#264327=CARTESIAN_POINT('Ctrl Pts',(45.7473997315196,-59.0454393048068,
-40.036940604538));
#264328=CARTESIAN_POINT('Ctrl Pts',(45.7211395471819,-59.0658214386729,
-40.0357903820881));
#264329=CARTESIAN_POINT('Ctrl Pts',(45.6809042968051,-59.0954678458765,
-40.0337180382941));
#264330=CARTESIAN_POINT('Ctrl Pts',(45.6673389080279,-59.1052038578702,
-40.032968546681));
#264331=CARTESIAN_POINT('Ctrl Pts',(45.6399352188299,-59.1243559363232,
-40.0313533997148));
#264332=CARTESIAN_POINT('Ctrl Pts',(45.6260664980794,-59.1337917962429,
-40.0304856638181));
#264333=CARTESIAN_POINT('Ctrl Pts',(45.584214102782,-59.161503132938,-40.0277172905008));
#264334=CARTESIAN_POINT('Ctrl Pts',(45.5559966208921,-59.1791815977629,
-40.0256537729831));
#264335=CARTESIAN_POINT('Ctrl Pts',(45.4988807301693,-59.2130228222466,
-40.0210955920518));
#264336=CARTESIAN_POINT('Ctrl Pts',(45.469993037139,-59.2291787807534,-40.0186016949324));
#264337=CARTESIAN_POINT('Ctrl Pts',(45.3823561363204,-59.2753882889069,
-40.0104846937946));
#264338=CARTESIAN_POINT('Ctrl Pts',(45.3226351503952,-59.3031882186041,
-40.0042276607109));
#264339=CARTESIAN_POINT('Ctrl Pts',(45.2311259835243,-59.3404168518855,
-39.9935799974664));
#264340=CARTESIAN_POINT('Ctrl Pts',(45.2003010959947,-59.3520799076811,
-39.9898200563787));
#264341=CARTESIAN_POINT('Ctrl Pts',(45.1380032580586,-59.3739026770269,
-39.9818749483524));
#264342=CARTESIAN_POINT('Ctrl Pts',(45.1065139829285,-59.3840662456593,
-39.977687330893));
#264343=CARTESIAN_POINT('Ctrl Pts',(45.0429436614079,-59.4028535501948,
-39.9688897783697));
#264344=CARTESIAN_POINT('Ctrl Pts',(45.0107045696338,-59.4115134856595,
-39.9642558817745));
#264345=CARTESIAN_POINT('Ctrl Pts',(44.9462144135346,-59.4271214577326,
-39.9546448356758));
#264346=CARTESIAN_POINT('Ctrl Pts',(44.9139254426396,-59.4340890792738,
-39.9496641049217));
#264347=CARTESIAN_POINT('Ctrl Pts',(44.849254794685,-59.446387333888,-39.9393573163679));
#264348=CARTESIAN_POINT('Ctrl Pts',(44.8168743179144,-59.451718463481,-39.9340315943834));
#264349=CARTESIAN_POINT('Ctrl Pts',(44.752024642773,-59.4607707923529,-39.9230399231476));
#264350=CARTESIAN_POINT('Ctrl Pts',(44.7195554394538,-59.464491904643,-39.9173739567058));
#264351=CARTESIAN_POINT('Ctrl Pts',(44.622016134105,-59.4732614616325,-39.899868543586));
#264352=CARTESIAN_POINT('Ctrl Pts',(44.5567952038801,-59.4759192557151,
-39.8875184519297));
#264353=CARTESIAN_POINT('Ctrl Pts',(44.4587589187831,-59.4751124713245,
-39.8679817460721));
#264354=CARTESIAN_POINT('Ctrl Pts',(44.4260062405338,-59.4740390035135,
-39.8612919155826));
#264355=CARTESIAN_POINT('Ctrl Pts',(44.3768568603989,-59.4712162368822,
-39.8510066089926));
#264356=CARTESIAN_POINT('Ctrl Pts',(44.3604553547125,-59.470071279602,-39.8475330573825));
#264357=CARTESIAN_POINT('Ctrl Pts',(44.3276272864905,-59.4673718881716,
-39.8404975989298));
#264358=CARTESIAN_POINT('Ctrl Pts',(44.3112150025957,-59.4658177666042,
-39.8369385762314));
#264359=CARTESIAN_POINT('Ctrl Pts',(44.2622182182766,-59.4605671446247,
-39.8261888936481));
#264360=CARTESIAN_POINT('Ctrl Pts',(44.2297855397697,-59.4562791768359,
-39.8189075287393));
#264361=CARTESIAN_POINT('Ctrl Pts',(44.1653820410688,-59.4461622151957,
-39.8041204276866));
#264362=CARTESIAN_POINT('Ctrl Pts',(44.1334097751946,-59.4403335371186,
-39.7966144716676));
#264363=CARTESIAN_POINT('Ctrl Pts',(44.0381705631049,-59.4205744031982,
-39.7737632575285));
#264364=CARTESIAN_POINT('Ctrl Pts',(43.9755798614833,-59.4043753530904,
-39.7580853037566));
#264365=CARTESIAN_POINT('Ctrl Pts',(43.8521846744312,-59.36599016115,-39.725843388912));
#264366=CARTESIAN_POINT('Ctrl Pts',(43.791371268692,-59.343796339026,-39.7092760945378));
#264367=CARTESIAN_POINT('Ctrl Pts',(43.7165137253937,-59.3122653970299,
-39.6880073146029));
#264368=CARTESIAN_POINT('Ctrl Pts',(43.7015912939536,-59.3057628682929,
-39.6837223938823));
#264369=CARTESIAN_POINT('Ctrl Pts',(43.6718796312441,-59.2923832966048,
-39.675100784162));
#264370=CARTESIAN_POINT('Ctrl Pts',(43.6570609707452,-59.2854910954552,
-39.6707551582104));
#264371=CARTESIAN_POINT('Ctrl Pts',(43.6129442606048,-59.2643105724085,
-39.6576799110036));
#264372=CARTESIAN_POINT('Ctrl Pts',(43.5840318360846,-59.2495460539614,
-39.6489267925925));
#264373=CARTESIAN_POINT('Ctrl Pts',(43.5555688340535,-59.234132410514,-39.6401263014865));
#264374=CARTESIAN_POINT('',(45.673922755161,-55.5192637623964,-38.9124165672108));
#264375=CARTESIAN_POINT('',(45.6739227548708,-55.5192637629142,-38.9124165672458));
#264376=CARTESIAN_POINT('',(43.4805771074159,-59.5712767529304,-39.2399080357012));
#264377=CARTESIAN_POINT('Ctrl Pts',(43.4805771074156,-59.5712767529309,
-39.2399080357013));
#264378=CARTESIAN_POINT('Ctrl Pts',(43.2084983655955,-59.4241035716486,
-39.1668006710783));
#264379=CARTESIAN_POINT('Ctrl Pts',(42.9694351505993,-59.2238071870063,
-39.0896600468055));
#264380=CARTESIAN_POINT('Ctrl Pts',(42.5877499895759,-58.7449876099978,
-38.9374284505921));
#264381=CARTESIAN_POINT('Ctrl Pts',(42.4470026012736,-58.4716973584526,
-38.8636131689055));
#264382=CARTESIAN_POINT('Ctrl Pts',(42.2829188141298,-57.8937343216347,
-38.7304874981619));
#264383=CARTESIAN_POINT('Ctrl Pts',(42.2573533055641,-57.5951189999158,
-38.6719031562341));
#264384=CARTESIAN_POINT('Ctrl Pts',(42.3215651079466,-57.0104777473371,
-38.5774816051817));
#264385=CARTESIAN_POINT('Ctrl Pts',(42.4073752536078,-56.7295195546235,
-38.5418707047797));
#264386=CARTESIAN_POINT('Ctrl Pts',(42.6817387181495,-56.2116483083903,
-38.4973862220026));
#264387=CARTESIAN_POINT('Ctrl Pts',(42.8670639833424,-55.9810885822738,
-38.4890931163589));
#264388=CARTESIAN_POINT('Ctrl Pts',(43.3113300107118,-55.6043418037155,
-38.5014475290099));
#264389=CARTESIAN_POINT('Ctrl Pts',(43.563676465166,-55.4612112790788,-38.5214440607413));
#264390=CARTESIAN_POINT('Ctrl Pts',(44.1136708092855,-55.2727963636881,
-38.5873481888105));
#264391=CARTESIAN_POINT('Ctrl Pts',(44.4057389282975,-55.2321785575282,
-38.6330729320601));
#264392=CARTESIAN_POINT('Ctrl Pts',(44.8666382983243,-55.2549155285843,
-38.7204514563686));
#264393=CARTESIAN_POINT('Ctrl Pts',(45.0356772772846,-55.2823862237002,
-38.7558506821669));
#264394=CARTESIAN_POINT('Ctrl Pts',(45.364666265058,-55.3740467165804,-38.8313288315555));
#264395=CARTESIAN_POINT('Ctrl Pts',(45.5236259139144,-55.4381875697362,
-38.8712190690491));
#264396=CARTESIAN_POINT('Ctrl Pts',(45.6739227548708,-55.5192637629143,
-38.9124165672458));
#264397=CARTESIAN_POINT('',(43.4805771074159,-59.5712767529304,-39.2399080357012));
#264398=CARTESIAN_POINT('Origin',(44.615955334411,-57.3789268591943,-39.4599679236673));
#264399=CARTESIAN_POINT('Origin',(48.2118204350714,-55.8145579159494,-52.64995));
#264400=CARTESIAN_POINT('Ctrl Pts',(42.839207175268,-57.4754524783491,-52.64995));
#264401=CARTESIAN_POINT('Ctrl Pts',(42.8226659458708,-57.633184469963,-52.64995));
#264402=CARTESIAN_POINT('Ctrl Pts',(42.8274712764287,-57.792393072249,-52.64995));
#264403=CARTESIAN_POINT('Ctrl Pts',(42.8786574174949,-58.0993235421715,
-52.64995));
#264404=CARTESIAN_POINT('Ctrl Pts',(42.9232286878868,-58.2458922062675,
-52.64995));
#264405=CARTESIAN_POINT('Ctrl Pts',(43.075036817329,-58.5811601802315,-52.64995));
#264406=CARTESIAN_POINT('Ctrl Pts',(43.1992049518545,-58.7594027873514,
-52.64995));
#264407=CARTESIAN_POINT('Ctrl Pts',(43.5542933458002,-59.1104583338343,
-52.64995));
#264408=CARTESIAN_POINT('Ctrl Pts',(43.7742269286883,-59.2312964387871,
-52.64995));
#264409=CARTESIAN_POINT('Ctrl Pts',(44.0795088334533,-59.3596331192527,
-52.64995));
#264410=CARTESIAN_POINT('Ctrl Pts',(44.2169771822695,-59.4004713032236,
-52.64995));
#264411=CARTESIAN_POINT('Ctrl Pts',(44.4991010430761,-59.4516685795711,
-52.64995));
#264412=CARTESIAN_POINT('Ctrl Pts',(44.6429009445505,-59.4617078816742,
-52.64995));
#264413=CARTESIAN_POINT('Ctrl Pts',(44.7865238868913,-59.4559569492311,
-52.64995));
#264414=CARTESIAN_POINT('Ctrl Pts',(46.5079524583205,-57.4754524783491,
-52.64995));
#264415=CARTESIAN_POINT('Ctrl Pts',(46.4950120245218,-57.3275618063643,
-52.64995));
#264416=CARTESIAN_POINT('Ctrl Pts',(46.4647658835114,-57.1817042732835,
-52.64995));
#264417=CARTESIAN_POINT('Ctrl Pts',(46.3748033228779,-56.9120256688023,
-52.64995));
#264418=CARTESIAN_POINT('Ctrl Pts',(46.3180752819212,-56.7881799556783,
-52.64995));
#264419=CARTESIAN_POINT('Ctrl Pts',(46.1241199408223,-56.4626040795241,
-52.64995));
#264420=CARTESIAN_POINT('Ctrl Pts',(45.960561722969,-56.2797546389996,-52.64995));
#264421=CARTESIAN_POINT('Ctrl Pts',(45.6181630929699,-56.0202600517664,
-52.64995));
#264422=CARTESIAN_POINT('Ctrl Pts',(45.4037244819502,-55.8912169339011,
-52.6499500000282));
#264423=CARTESIAN_POINT('Ctrl Pts',(44.9862869603902,-55.7833848066862,
-52.6499500000282));
#264424=CARTESIAN_POINT('Ctrl Pts',(44.8386017522404,-55.7653378340959,
-52.64995));
#264425=CARTESIAN_POINT('Ctrl Pts',(44.5503390053884,-55.7682194115044,
-52.64995));
#264426=CARTESIAN_POINT('Ctrl Pts',(44.4109642294216,-55.7870757183414,
-52.64995));
#264427=CARTESIAN_POINT('Ctrl Pts',(44.2755200796093,-55.8229737314248,
-52.64995));
#264428=CARTESIAN_POINT('Origin',(44.5079524583205,-57.4754524783491,-52.920575));
#264429=CARTESIAN_POINT('Ctrl Pts',(42.839207175268,-57.4754524783491,-52.4912));
#264430=CARTESIAN_POINT('Ctrl Pts',(42.839207175268,-58.4389030167283,-52.4328666666667));
#264431=CARTESIAN_POINT('Ctrl Pts',(43.6735798167943,-58.920628285918,-52.3745333333334));
#264432=CARTESIAN_POINT('Ctrl Pts',(44.5079524583205,-59.4023535551075,
-52.3162000000001));
#264433=CARTESIAN_POINT('Ctrl Pts',(45.3423250998467,-58.920628285918,-52.2578666666667));
#264434=CARTESIAN_POINT('Ctrl Pts',(46.1766977413729,-58.4389030167283,
-52.1995333333334));
#264435=CARTESIAN_POINT('Ctrl Pts',(46.1766977413729,-57.4754524783491,
-52.1412));
#264436=CARTESIAN_POINT('Ctrl Pts',(46.1766977413729,-56.5120019399699,
-52.0828666666667));
#264437=CARTESIAN_POINT('Ctrl Pts',(45.3423250998467,-56.0302766707802,
-52.0245333333333));
#264438=CARTESIAN_POINT('Ctrl Pts',(44.5079524583205,-55.5485514015906,
-51.9662));
#264439=CARTESIAN_POINT('Ctrl Pts',(43.6735798167943,-56.0302766707802,
-51.9078666666667));
#264440=CARTESIAN_POINT('Ctrl Pts',(42.839207175268,-56.5120019399698,-51.8495333333334));
#264441=CARTESIAN_POINT('Ctrl Pts',(42.839207175268,-57.4754524783491,-51.7912));
#264442=CARTESIAN_POINT('Ctrl Pts',(42.839207175268,-57.4754524783491,-52.64995));
#264443=CARTESIAN_POINT('Ctrl Pts',(42.839207175268,-58.4389030167283,-52.5916166666667));
#264444=CARTESIAN_POINT('Ctrl Pts',(43.6735798167943,-58.920628285918,-52.5332833333334));
#264445=CARTESIAN_POINT('Ctrl Pts',(44.5079524583205,-59.4023535551075,
-52.4749500000001));
#264446=CARTESIAN_POINT('Ctrl Pts',(45.3423250998467,-58.920628285918,-52.4166166666667));
#264447=CARTESIAN_POINT('Ctrl Pts',(46.1766977413729,-58.4389030167283,
-52.3582833333334));
#264448=CARTESIAN_POINT('Ctrl Pts',(46.1766977413729,-57.4754524783491,
-52.29995));
#264449=CARTESIAN_POINT('Ctrl Pts',(46.1766977413729,-56.5120019399699,
-52.2416166666667));
#264450=CARTESIAN_POINT('Ctrl Pts',(45.3423250998467,-56.0302766707802,
-52.1832833333333));
#264451=CARTESIAN_POINT('Ctrl Pts',(44.5079524583205,-55.5485514015906,
-52.12495));
#264452=CARTESIAN_POINT('Ctrl Pts',(43.6735798167943,-56.0302766707802,
-52.0666166666667));
#264453=CARTESIAN_POINT('Ctrl Pts',(42.839207175268,-56.5120019399698,-52.0082833333333));
#264454=CARTESIAN_POINT('Ctrl Pts',(42.839207175268,-57.4754524783491,-51.94995));
#264455=CARTESIAN_POINT('Ctrl Pts',(46.5766932247459,-57.4754524783491,
-52.6102625));
#264456=CARTESIAN_POINT('Ctrl Pts',(46.5766932247459,-56.2810644399698,
-52.5519291666666));
#264457=CARTESIAN_POINT('Ctrl Pts',(45.5423228415332,-55.6838704207802,
-52.4935958333333));
#264458=CARTESIAN_POINT('Ctrl Pts',(44.5079524583205,-55.0866764015906,
-52.4352625000001));
#264459=CARTESIAN_POINT('Ctrl Pts',(43.4735820751078,-55.6838704207802,
-52.3769291666667));
#264460=CARTESIAN_POINT('Ctrl Pts',(42.4392116918951,-56.2810644399698,
-52.3185958333334));
#264461=CARTESIAN_POINT('Ctrl Pts',(42.439211691895,-57.4754524783491,-52.2602625));
#264462=CARTESIAN_POINT('Ctrl Pts',(42.4392116918951,-58.6698405167284,
-52.2019291666667));
#264463=CARTESIAN_POINT('Ctrl Pts',(43.4735820751078,-59.267034535918,-52.1435958333333));
#264464=CARTESIAN_POINT('Ctrl Pts',(44.5079524583205,-59.8642285551076,
-52.0852625));
#264465=CARTESIAN_POINT('Ctrl Pts',(45.5423228415332,-59.267034535918,-52.0269291666667));
#264466=CARTESIAN_POINT('Ctrl Pts',(46.5766932247459,-58.6698405167284,
-51.9685958333333));
#264467=CARTESIAN_POINT('Ctrl Pts',(46.5766932247459,-57.4754524783491,
-51.9102625));
#264468=CARTESIAN_POINT('Ctrl Pts',(46.5766932247459,-56.2810644399698,
-51.8519291666667));
#264469=CARTESIAN_POINT('Ctrl Pts',(45.5423228415332,-55.6838704207802,
-51.7935958333333));
#264470=CARTESIAN_POINT('Ctrl Pts',(44.5079524583205,-55.0866764015906,
-51.7352625));
#264471=CARTESIAN_POINT('Ctrl Pts',(43.4735820751078,-55.6838704207802,
-51.6769291666667));
#264472=CARTESIAN_POINT('Ctrl Pts',(42.4392116918951,-56.2810644399698,
-51.6185958333333));
#264473=CARTESIAN_POINT('Ctrl Pts',(42.439211691895,-57.4754524783491,-51.5602625));
#264474=CARTESIAN_POINT('Ctrl Pts',(42.4392116918951,-58.6698405167284,
-51.5019291666666));
#264475=CARTESIAN_POINT('Ctrl Pts',(43.4735820751078,-59.267034535918,-51.4435958333333));
#264476=CARTESIAN_POINT('Ctrl Pts',(44.5079524583205,-59.8642285551076,
-51.3852625));
#264477=CARTESIAN_POINT('Ctrl Pts',(45.5423228415332,-59.267034535918,-51.3269291666667));
#264478=CARTESIAN_POINT('Ctrl Pts',(46.5766932247459,-58.6698405167284,
-51.2685958333333));
#264479=CARTESIAN_POINT('Ctrl Pts',(46.5766932247459,-57.4754524783491,
-51.2102625));
#264480=CARTESIAN_POINT('Ctrl Pts',(46.5766932247459,-56.2810644399698,
-51.1519291666666));
#264481=CARTESIAN_POINT('Ctrl Pts',(45.5423228415332,-55.6838704207802,
-51.0935958333334));
#264482=CARTESIAN_POINT('Ctrl Pts',(44.5079524583205,-55.0866764015906,
-51.0352625));
#264483=CARTESIAN_POINT('Ctrl Pts',(43.4735820751078,-55.6838704207802,
-50.9769291666667));
#264484=CARTESIAN_POINT('Ctrl Pts',(42.4392116918951,-56.2810644399698,
-50.9185958333333));
#264485=CARTESIAN_POINT('Ctrl Pts',(42.439211691895,-57.4754524783491,-50.8602625));
#264486=CARTESIAN_POINT('Ctrl Pts',(42.4392116918951,-58.6698405167284,
-50.8019291666667));
#264487=CARTESIAN_POINT('Ctrl Pts',(43.4735820751078,-59.267034535918,-50.7435958333333));
#264488=CARTESIAN_POINT('Ctrl Pts',(44.5079524583205,-59.8642285551076,
-50.6852625));
#264489=CARTESIAN_POINT('Ctrl Pts',(45.5423228415332,-59.267034535918,-50.6269291666667));
#264490=CARTESIAN_POINT('Ctrl Pts',(46.5766932247459,-58.6698405167284,
-50.5685958333333));
#264491=CARTESIAN_POINT('Ctrl Pts',(46.5766932247459,-57.4754524783491,
-50.5102625));
#264492=CARTESIAN_POINT('Ctrl Pts',(46.5766932247459,-56.2810644399698,
-50.4519291666667));
#264493=CARTESIAN_POINT('Ctrl Pts',(45.5423228415332,-55.6838704207802,
-50.3935958333333));
#264494=CARTESIAN_POINT('Ctrl Pts',(44.5079524583205,-55.0866764015906,
-50.3352625));
#264495=CARTESIAN_POINT('Ctrl Pts',(43.4735820751078,-55.6838704207802,
-50.2769291666667));
#264496=CARTESIAN_POINT('Ctrl Pts',(42.4392116918951,-56.2810644399698,
-50.2185958333333));
#264497=CARTESIAN_POINT('Ctrl Pts',(42.439211691895,-57.4754524783491,-50.1602625));
#264498=CARTESIAN_POINT('Ctrl Pts',(42.4392116918951,-58.6698405167284,
-50.1019291666667));
#264499=CARTESIAN_POINT('Ctrl Pts',(43.4735820751078,-59.267034535918,-50.0435958333333));
#264500=CARTESIAN_POINT('Ctrl Pts',(44.5079524583205,-59.8642285551076,
-49.9852625));
#264501=CARTESIAN_POINT('Ctrl Pts',(45.5423228415332,-59.267034535918,-49.9269291666667));
#264502=CARTESIAN_POINT('Ctrl Pts',(46.5766932247459,-58.6698405167284,
-49.8685958333333));
#264503=CARTESIAN_POINT('Ctrl Pts',(46.5766932247459,-57.4754524783491,
-49.8102625));
#264504=CARTESIAN_POINT('Ctrl Pts',(46.5766932247459,-56.2810644399698,
-49.7519291666667));
#264505=CARTESIAN_POINT('Ctrl Pts',(45.5423228415332,-55.6838704207802,
-49.6935958333334));
#264506=CARTESIAN_POINT('Ctrl Pts',(44.5079524583205,-55.0866764015906,
-49.6352625));
#264507=CARTESIAN_POINT('Ctrl Pts',(43.4735820751078,-55.6838704207802,
-49.5769291666667));
#264508=CARTESIAN_POINT('Ctrl Pts',(42.4392116918951,-56.2810644399698,
-49.5185958333334));
#264509=CARTESIAN_POINT('Ctrl Pts',(42.439211691895,-57.4754524783491,-49.4602625));
#264510=CARTESIAN_POINT('Ctrl Pts',(42.4392116918951,-58.6698405167284,
-49.4019291666667));
#264511=CARTESIAN_POINT('Ctrl Pts',(43.4735820751078,-59.267034535918,-49.3435958333333));
#264512=CARTESIAN_POINT('Ctrl Pts',(44.5079524583205,-59.8642285551076,
-49.2852625));
#264513=CARTESIAN_POINT('Ctrl Pts',(45.5423228415332,-59.267034535918,-49.2269291666667));
#264514=CARTESIAN_POINT('Ctrl Pts',(46.5766932247459,-58.6698405167284,
-49.1685958333334));
#264515=CARTESIAN_POINT('Ctrl Pts',(46.5766932247459,-57.4754524783491,
-49.1102625));
#264516=CARTESIAN_POINT('Ctrl Pts',(46.5766932247459,-56.2810644399698,
-49.0519291666667));
#264517=CARTESIAN_POINT('Ctrl Pts',(45.5423228415332,-55.6838704207802,
-48.9935958333333));
#264518=CARTESIAN_POINT('Ctrl Pts',(44.5079524583205,-55.0866764015906,
-48.9352625));
#264519=CARTESIAN_POINT('Ctrl Pts',(43.4735820751078,-55.6838704207802,
-48.8769291666667));
#264520=CARTESIAN_POINT('Ctrl Pts',(42.4392116918951,-56.2810644399698,
-48.8185958333334));
#264521=CARTESIAN_POINT('Ctrl Pts',(42.439211691895,-57.4754524783491,-48.7602625));
#264522=CARTESIAN_POINT('Ctrl Pts',(42.4392116918951,-58.6698405167284,
-48.7019291666667));
#264523=CARTESIAN_POINT('Ctrl Pts',(43.4735820751078,-59.267034535918,-48.6435958333333));
#264524=CARTESIAN_POINT('Ctrl Pts',(44.5079524583205,-59.8642285551076,
-48.5852625));
#264525=CARTESIAN_POINT('Ctrl Pts',(45.5423228415332,-59.267034535918,-48.5269291666667));
#264526=CARTESIAN_POINT('Ctrl Pts',(46.5766932247459,-58.6698405167284,
-48.4685958333333));
#264527=CARTESIAN_POINT('Ctrl Pts',(46.5766932247459,-57.4754524783491,
-48.4102625));
#264528=CARTESIAN_POINT('Ctrl Pts',(46.5766932247459,-56.2810644399698,
-48.3519291666667));
#264529=CARTESIAN_POINT('Ctrl Pts',(45.5423228415332,-55.6838704207802,
-48.2935958333334));
#264530=CARTESIAN_POINT('Ctrl Pts',(44.5079524583205,-55.0866764015906,
-48.2352625));
#264531=CARTESIAN_POINT('Ctrl Pts',(43.4735820751078,-55.6838704207802,
-48.1769291666667));
#264532=CARTESIAN_POINT('Ctrl Pts',(42.4392116918951,-56.2810644399698,
-48.1185958333334));
#264533=CARTESIAN_POINT('Ctrl Pts',(42.439211691895,-57.4754524783491,-48.0602625));
#264534=CARTESIAN_POINT('Ctrl Pts',(42.4392116918951,-58.6698405167284,
-48.0019291666667));
#264535=CARTESIAN_POINT('Ctrl Pts',(43.4735820751078,-59.267034535918,-47.9435958333334));
#264536=CARTESIAN_POINT('Ctrl Pts',(44.5079524583205,-59.8642285551076,
-47.8852625));
#264537=CARTESIAN_POINT('Ctrl Pts',(45.5423228415332,-59.267034535918,-47.8269291666667));
#264538=CARTESIAN_POINT('Ctrl Pts',(46.5766932247459,-58.6698405167284,
-47.7685958333333));
#264539=CARTESIAN_POINT('Ctrl Pts',(46.5766932247459,-57.4754524783491,
-47.7102625));
#264540=CARTESIAN_POINT('Ctrl Pts',(46.5766932247459,-56.2810644399698,
-47.6519291666667));
#264541=CARTESIAN_POINT('Ctrl Pts',(45.5423228415332,-55.6838704207802,
-47.5935958333333));
#264542=CARTESIAN_POINT('Ctrl Pts',(44.5079524583205,-55.0866764015906,
-47.5352625));
#264543=CARTESIAN_POINT('Ctrl Pts',(43.4735820751078,-55.6838704207802,
-47.4769291666667));
#264544=CARTESIAN_POINT('Ctrl Pts',(42.4392116918951,-56.2810644399698,
-47.4185958333333));
#264545=CARTESIAN_POINT('Ctrl Pts',(42.439211691895,-57.4754524783491,-47.3602625));
#264546=CARTESIAN_POINT('Ctrl Pts',(42.4392116918951,-58.6698405167284,
-47.3019291666666));
#264547=CARTESIAN_POINT('Ctrl Pts',(43.4735820751078,-59.267034535918,-47.2435958333334));
#264548=CARTESIAN_POINT('Ctrl Pts',(44.5079524583205,-59.8642285551076,
-47.1852625));
#264549=CARTESIAN_POINT('Ctrl Pts',(45.5423228415332,-59.267034535918,-47.1269291666667));
#264550=CARTESIAN_POINT('Ctrl Pts',(46.5766932247459,-58.6698405167284,
-47.0685958333333));
#264551=CARTESIAN_POINT('Ctrl Pts',(46.5766932247459,-57.4754524783491,
-47.0102625));
#264552=CARTESIAN_POINT('Ctrl Pts',(46.5766932247459,-56.2810644399698,
-46.9519291666667));
#264553=CARTESIAN_POINT('Ctrl Pts',(45.5423228415332,-55.6838704207802,
-46.8935958333333));
#264554=CARTESIAN_POINT('Ctrl Pts',(44.5079524583205,-55.0866764015906,
-46.8352625));
#264555=CARTESIAN_POINT('Ctrl Pts',(43.4735820751078,-55.6838704207802,
-46.7769291666667));
#264556=CARTESIAN_POINT('Ctrl Pts',(42.4392116918951,-56.2810644399698,
-46.7185958333333));
#264557=CARTESIAN_POINT('Ctrl Pts',(42.439211691895,-57.4754524783491,-46.6602625));
#264558=CARTESIAN_POINT('Ctrl Pts',(42.4392116918951,-58.6698405167284,
-46.6019291666667));
#264559=CARTESIAN_POINT('Ctrl Pts',(43.4735820751078,-59.267034535918,-46.5435958333334));
#264560=CARTESIAN_POINT('Ctrl Pts',(44.5079524583205,-59.8642285551076,
-46.4852625));
#264561=CARTESIAN_POINT('Ctrl Pts',(45.5423228415332,-59.267034535918,-46.4269291666667));
#264562=CARTESIAN_POINT('Ctrl Pts',(46.5766932247459,-58.6698405167284,
-46.3685958333333));
#264563=CARTESIAN_POINT('Ctrl Pts',(46.5766932247459,-57.4754524783491,
-46.3102625));
#264564=CARTESIAN_POINT('Ctrl Pts',(46.5766932247459,-56.2810644399698,
-46.2519291666667));
#264565=CARTESIAN_POINT('Ctrl Pts',(45.5423228415332,-55.6838704207802,
-46.1935958333333));
#264566=CARTESIAN_POINT('Ctrl Pts',(44.5079524583205,-55.0866764015906,
-46.1352625));
#264567=CARTESIAN_POINT('Ctrl Pts',(43.4735820751078,-55.6838704207802,
-46.0769291666667));
#264568=CARTESIAN_POINT('Ctrl Pts',(42.4392116918951,-56.2810644399698,
-46.0185958333334));
#264569=CARTESIAN_POINT('Ctrl Pts',(42.439211691895,-57.4754524783491,-45.9602625));
#264570=CARTESIAN_POINT('Ctrl Pts',(42.4392116918951,-58.6698405167284,
-45.9019291666667));
#264571=CARTESIAN_POINT('Ctrl Pts',(43.4735820751078,-59.267034535918,-45.8435958333333));
#264572=CARTESIAN_POINT('Ctrl Pts',(44.5079524583205,-59.8642285551076,
-45.7852625));
#264573=CARTESIAN_POINT('Ctrl Pts',(45.5423228415332,-59.267034535918,-45.7269291666667));
#264574=CARTESIAN_POINT('Ctrl Pts',(46.5766932247459,-58.6698405167284,
-45.6685958333334));
#264575=CARTESIAN_POINT('Ctrl Pts',(46.5766932247459,-57.4754524783491,
-45.6102625));
#264576=CARTESIAN_POINT('Ctrl Pts',(46.5766932247459,-56.2810644399698,
-45.5519291666667));
#264577=CARTESIAN_POINT('Ctrl Pts',(45.5423228415332,-55.6838704207802,
-45.4935958333333));
#264578=CARTESIAN_POINT('Ctrl Pts',(44.5079524583205,-55.0866764015906,
-45.4352625));
#264579=CARTESIAN_POINT('Ctrl Pts',(43.4735820751078,-55.6838704207802,
-45.3769291666667));
#264580=CARTESIAN_POINT('Ctrl Pts',(42.4392116918951,-56.2810644399698,
-45.3185958333333));
#264581=CARTESIAN_POINT('Ctrl Pts',(42.439211691895,-57.4754524783491,-45.2602625));
#264582=CARTESIAN_POINT('Ctrl Pts',(42.4392116918951,-58.6698405167284,
-45.2019291666667));
#264583=CARTESIAN_POINT('Ctrl Pts',(43.4735820751078,-59.267034535918,-45.1435958333334));
#264584=CARTESIAN_POINT('Ctrl Pts',(44.5079524583205,-59.8642285551076,
-45.0852625));
#264585=CARTESIAN_POINT('Ctrl Pts',(45.5423228415332,-59.267034535918,-45.0269291666667));
#264586=CARTESIAN_POINT('Ctrl Pts',(46.5766932247459,-58.6698405167284,
-44.9685958333334));
#264587=CARTESIAN_POINT('Ctrl Pts',(46.5766932247459,-57.4754524783491,
-44.9102625));
#264588=CARTESIAN_POINT('Ctrl Pts',(46.5766932247459,-56.2810644399698,
-44.8519291666667));
#264589=CARTESIAN_POINT('Ctrl Pts',(45.5423228415332,-55.6838704207802,
-44.7935958333333));
#264590=CARTESIAN_POINT('Ctrl Pts',(44.5079524583205,-55.0866764015906,
-44.7352625));
#264591=CARTESIAN_POINT('Ctrl Pts',(43.4735820751078,-55.6838704207802,
-44.6769291666667));
#264592=CARTESIAN_POINT('Ctrl Pts',(42.4392116918951,-56.2810644399698,
-44.6185958333334));
#264593=CARTESIAN_POINT('Ctrl Pts',(42.439211691895,-57.4754524783491,-44.5602625));
#264594=CARTESIAN_POINT('Ctrl Pts',(42.4392116918951,-58.6698405167284,
-44.5019291666667));
#264595=CARTESIAN_POINT('Ctrl Pts',(43.4735820751078,-59.267034535918,-44.4435958333333));
#264596=CARTESIAN_POINT('Ctrl Pts',(44.5079524583205,-59.8642285551076,
-44.3852625));
#264597=CARTESIAN_POINT('Ctrl Pts',(45.5423228415332,-59.267034535918,-44.3269291666667));
#264598=CARTESIAN_POINT('Ctrl Pts',(46.5766932247459,-58.6698405167284,
-44.2685958333334));
#264599=CARTESIAN_POINT('Ctrl Pts',(46.5766932247459,-57.4754524783491,
-44.2102625));
#264600=CARTESIAN_POINT('Ctrl Pts',(46.5766932247459,-56.2810644399698,
-44.1519291666667));
#264601=CARTESIAN_POINT('Ctrl Pts',(45.5423228415332,-55.6838704207802,
-44.0935958333334));
#264602=CARTESIAN_POINT('Ctrl Pts',(44.5079524583205,-55.0866764015906,
-44.0352625));
#264603=CARTESIAN_POINT('Ctrl Pts',(43.4735820751078,-55.6838704207802,
-43.9769291666667));
#264604=CARTESIAN_POINT('Ctrl Pts',(42.4392116918951,-56.2810644399698,
-43.9185958333334));
#264605=CARTESIAN_POINT('Ctrl Pts',(42.439211691895,-57.4754524783491,-43.8602625));
#264606=CARTESIAN_POINT('Ctrl Pts',(42.4392116918951,-58.6698405167284,
-43.8019291666667));
#264607=CARTESIAN_POINT('Ctrl Pts',(43.4735820751078,-59.267034535918,-43.7435958333334));
#264608=CARTESIAN_POINT('Ctrl Pts',(44.5079524583205,-59.8642285551076,
-43.6852625));
#264609=CARTESIAN_POINT('Ctrl Pts',(45.5423228415332,-59.267034535918,-43.6269291666667));
#264610=CARTESIAN_POINT('Ctrl Pts',(46.5766932247459,-58.6698405167284,
-43.5685958333334));
#264611=CARTESIAN_POINT('Ctrl Pts',(46.5766932247459,-57.4754524783491,
-43.5102625));
#264612=CARTESIAN_POINT('Ctrl Pts',(46.5766932247459,-56.2810644399698,
-43.4519291666667));
#264613=CARTESIAN_POINT('Ctrl Pts',(45.5423228415332,-55.6838704207802,
-43.3935958333334));
#264614=CARTESIAN_POINT('Ctrl Pts',(44.5079524583205,-55.0866764015906,
-43.3352625));
#264615=CARTESIAN_POINT('Ctrl Pts',(43.4735820751078,-55.6838704207802,
-43.2769291666667));
#264616=CARTESIAN_POINT('Ctrl Pts',(42.4392116918951,-56.2810644399698,
-43.2185958333334));
#264617=CARTESIAN_POINT('Ctrl Pts',(42.439211691895,-57.4754524783491,-43.1602625));
#264618=CARTESIAN_POINT('Ctrl Pts',(42.4392116918951,-58.6698405167284,
-43.1019291666667));
#264619=CARTESIAN_POINT('Ctrl Pts',(43.4735820751078,-59.267034535918,-43.0435958333334));
#264620=CARTESIAN_POINT('Ctrl Pts',(44.5079524583205,-59.8642285551076,
-42.9852625));
#264621=CARTESIAN_POINT('Ctrl Pts',(45.5423228415332,-59.267034535918,-42.9269291666667));
#264622=CARTESIAN_POINT('Ctrl Pts',(46.5766932247459,-58.6698405167284,
-42.8685958333333));
#264623=CARTESIAN_POINT('Ctrl Pts',(46.5766932247459,-57.4754524783491,
-42.8102625));
#264624=CARTESIAN_POINT('Ctrl Pts',(46.5766932247459,-56.2810644399698,
-42.7519291666667));
#264625=CARTESIAN_POINT('Ctrl Pts',(45.5423228415332,-55.6838704207802,
-42.6935958333333));
#264626=CARTESIAN_POINT('Ctrl Pts',(44.5079524583205,-55.0866764015906,
-42.6352625));
#264627=CARTESIAN_POINT('Ctrl Pts',(43.4735820751078,-55.6838704207802,
-42.5769291666667));
#264628=CARTESIAN_POINT('Ctrl Pts',(42.4392116918951,-56.2810644399698,
-42.5185958333333));
#264629=CARTESIAN_POINT('Ctrl Pts',(42.439211691895,-57.4754524783491,-42.4602625));
#264630=CARTESIAN_POINT('Ctrl Pts',(42.4392116918951,-58.6698405167284,
-42.4019291666666));
#264631=CARTESIAN_POINT('Ctrl Pts',(43.4735820751078,-59.267034535918,-42.3435958333334));
#264632=CARTESIAN_POINT('Ctrl Pts',(44.5079524583205,-59.8642285551076,
-42.2852625));
#264633=CARTESIAN_POINT('Ctrl Pts',(45.5423228415332,-59.267034535918,-42.2269291666667));
#264634=CARTESIAN_POINT('Ctrl Pts',(46.5766932247459,-58.6698405167284,
-42.1685958333333));
#264635=CARTESIAN_POINT('Ctrl Pts',(46.5766932247459,-57.4754524783491,
-42.1102625));
#264636=CARTESIAN_POINT('Ctrl Pts',(46.5766932247459,-56.2810644399698,
-42.0519291666667));
#264637=CARTESIAN_POINT('Ctrl Pts',(45.5423228415332,-55.6838704207802,
-41.9935958333334));
#264638=CARTESIAN_POINT('Ctrl Pts',(44.5079524583205,-55.0866764015906,
-41.9352625));
#264639=CARTESIAN_POINT('Ctrl Pts',(43.4735820751078,-55.6838704207802,
-41.8769291666667));
#264640=CARTESIAN_POINT('Ctrl Pts',(42.4392116918951,-56.2810644399698,
-41.8185958333333));
#264641=CARTESIAN_POINT('Ctrl Pts',(42.439211691895,-57.4754524783491,-41.7602625));
#264642=CARTESIAN_POINT('Ctrl Pts',(42.4392116918951,-58.6698405167284,
-41.7019291666667));
#264643=CARTESIAN_POINT('Ctrl Pts',(43.4735820751078,-59.267034535918,-41.6435958333334));
#264644=CARTESIAN_POINT('Ctrl Pts',(44.5079524583205,-59.8642285551076,
-41.5852625));
#264645=CARTESIAN_POINT('Ctrl Pts',(45.5423228415332,-59.267034535918,-41.5269291666667));
#264646=CARTESIAN_POINT('Ctrl Pts',(46.5766932247459,-58.6698405167284,
-41.4685958333333));
#264647=CARTESIAN_POINT('Ctrl Pts',(46.5766932247459,-57.4754524783491,
-41.4102625));
#264648=CARTESIAN_POINT('Ctrl Pts',(46.5766932247459,-56.2810644399698,
-41.3519291666666));
#264649=CARTESIAN_POINT('Ctrl Pts',(45.5423228415332,-55.6838704207802,
-41.2935958333334));
#264650=CARTESIAN_POINT('Ctrl Pts',(44.5079524583205,-55.0866764015906,
-41.2352625));
#264651=CARTESIAN_POINT('Ctrl Pts',(43.4735820751078,-55.6838704207802,
-41.1769291666667));
#264652=CARTESIAN_POINT('Ctrl Pts',(42.4392116918951,-56.2810644399698,
-41.1185958333333));
#264653=CARTESIAN_POINT('Ctrl Pts',(42.439211691895,-57.4754524783491,-41.0602625));
#264654=CARTESIAN_POINT('Ctrl Pts',(42.4392116918951,-58.6698405167284,
-41.0019291666666));
#264655=CARTESIAN_POINT('Ctrl Pts',(43.4735820751078,-59.267034535918,-40.9435958333334));
#264656=CARTESIAN_POINT('Ctrl Pts',(44.5079524583205,-59.8642285551076,
-40.8852625));
#264657=CARTESIAN_POINT('Ctrl Pts',(45.5423228415332,-59.267034535918,-40.8269291666667));
#264658=CARTESIAN_POINT('Ctrl Pts',(46.5766932247459,-58.6698405167284,
-40.7685958333333));
#264659=CARTESIAN_POINT('Ctrl Pts',(46.5766932247459,-57.4754524783491,
-40.7102625));
#264660=CARTESIAN_POINT('Ctrl Pts',(46.5766932247459,-56.2810644399698,
-40.6519291666667));
#264661=CARTESIAN_POINT('Ctrl Pts',(45.5423228415332,-55.6838704207802,
-40.5935958333334));
#264662=CARTESIAN_POINT('Ctrl Pts',(44.5079524583205,-55.0866764015906,
-40.5352625));
#264663=CARTESIAN_POINT('Ctrl Pts',(43.4735820751078,-55.6838704207802,
-40.4769291666667));
#264664=CARTESIAN_POINT('Ctrl Pts',(42.4392116918951,-56.2810644399698,
-40.4185958333333));
#264665=CARTESIAN_POINT('Ctrl Pts',(42.439211691895,-57.4754524783491,-40.3602625));
#264666=CARTESIAN_POINT('Ctrl Pts',(42.4392116918951,-58.6698405167284,
-40.3019291666667));
#264667=CARTESIAN_POINT('Ctrl Pts',(43.4735820751078,-59.267034535918,-40.2435958333334));
#264668=CARTESIAN_POINT('Ctrl Pts',(44.5079524583205,-59.8642285551076,
-40.1852625));
#264669=CARTESIAN_POINT('Ctrl Pts',(45.5423228415332,-59.267034535918,-40.1269291666666));
#264670=CARTESIAN_POINT('Ctrl Pts',(46.5766932247459,-58.6698405167284,
-40.0685958333333));
#264671=CARTESIAN_POINT('Ctrl Pts',(46.5766932247459,-57.4754524783491,
-40.0102625));
#264672=CARTESIAN_POINT('Ctrl Pts',(46.5766932247459,-56.2810644399698,
-39.9519291666667));
#264673=CARTESIAN_POINT('Ctrl Pts',(45.5423228415332,-55.6838704207802,
-39.8935958333334));
#264674=CARTESIAN_POINT('Ctrl Pts',(44.5079524583205,-55.0866764015906,
-39.8352625));
#264675=CARTESIAN_POINT('Ctrl Pts',(43.4735820751078,-55.6838704207802,
-39.7769291666667));
#264676=CARTESIAN_POINT('Ctrl Pts',(42.4392116918951,-56.2810644399698,
-39.7185958333334));
#264677=CARTESIAN_POINT('Ctrl Pts',(42.439211691895,-57.4754524783491,-39.6602625));
#264678=CARTESIAN_POINT('Ctrl Pts',(42.4392116918951,-58.6698405167284,
-39.6019291666667));
#264679=CARTESIAN_POINT('Ctrl Pts',(43.4735820751078,-59.267034535918,-39.5435958333333));
#264680=CARTESIAN_POINT('Ctrl Pts',(44.5079524583205,-59.8642285551076,
-39.4852625));
#264681=CARTESIAN_POINT('Ctrl Pts',(45.5423228415332,-59.267034535918,-39.4269291666667));
#264682=CARTESIAN_POINT('Ctrl Pts',(46.5766932247459,-58.6698405167284,
-39.3685958333334));
#264683=CARTESIAN_POINT('Ctrl Pts',(46.5766932247459,-57.4754524783491,
-39.3102625));
#264684=CARTESIAN_POINT('Ctrl Pts',(46.5766932247459,-56.2810644399698,
-39.2519291666667));
#264685=CARTESIAN_POINT('Ctrl Pts',(45.5423228415332,-55.6838704207802,
-39.1935958333334));
#264686=CARTESIAN_POINT('Ctrl Pts',(44.5079524583205,-55.0866764015906,
-39.1352625));
#264687=CARTESIAN_POINT('Ctrl Pts',(43.4735820751078,-55.6838704207802,
-39.0769291666667));
#264688=CARTESIAN_POINT('Ctrl Pts',(42.4392116918951,-56.2810644399698,
-39.0185958333334));
#264689=CARTESIAN_POINT('Ctrl Pts',(42.439211691895,-57.4754524783491,-38.9602625));
#264690=CARTESIAN_POINT('Ctrl Pts',(42.4392116918951,-58.6698405167284,
-38.9019291666667));
#264691=CARTESIAN_POINT('Ctrl Pts',(43.4735820751078,-59.267034535918,-38.8435958333333));
#264692=CARTESIAN_POINT('Ctrl Pts',(44.5079524583205,-59.8642285551076,
-38.7852625));
#264693=CARTESIAN_POINT('Ctrl Pts',(45.5423228415332,-59.267034535918,-38.7269291666667));
#264694=CARTESIAN_POINT('Ctrl Pts',(46.5766932247459,-58.6698405167284,
-38.6685958333334));
#264695=CARTESIAN_POINT('Ctrl Pts',(46.5766932247459,-57.4754524783491,
-38.6102625));
#264696=CARTESIAN_POINT('Ctrl Pts',(46.5766932247459,-56.2810644399698,
-38.5519291666667));
#264697=CARTESIAN_POINT('Ctrl Pts',(45.5423228415332,-55.6838704207802,
-38.4935958333334));
#264698=CARTESIAN_POINT('Ctrl Pts',(44.5079524583205,-55.0866764015906,
-38.4352625));
#264699=CARTESIAN_POINT('Ctrl Pts',(43.4735820751078,-55.6838704207802,
-38.3769291666667));
#264700=CARTESIAN_POINT('Ctrl Pts',(42.4392116918951,-56.2810644399698,
-38.3185958333333));
#264701=CARTESIAN_POINT('Ctrl Pts',(42.439211691895,-57.4754524783491,-38.2602625));
#264702=CARTESIAN_POINT('Ctrl Pts',(42.4392116918951,-58.6698405167284,
-38.2019291666667));
#264703=CARTESIAN_POINT('Ctrl Pts',(43.4735820751078,-59.267034535918,-38.1435958333334));
#264704=CARTESIAN_POINT('Ctrl Pts',(44.5079524583205,-59.8642285551076,
-38.0852625));
#264705=CARTESIAN_POINT('Ctrl Pts',(45.5423228415332,-59.267034535918,-38.0269291666667));
#264706=CARTESIAN_POINT('Ctrl Pts',(46.5766932247459,-58.6698405167284,
-37.9685958333333));
#264707=CARTESIAN_POINT('Ctrl Pts',(46.5766932247459,-57.4754524783491,
-37.9102625));
#264708=CARTESIAN_POINT('Ctrl Pts',(46.5766932247459,-56.2810644399698,
-37.8519291666667));
#264709=CARTESIAN_POINT('Ctrl Pts',(45.5423228415332,-55.6838704207802,
-37.7935958333334));
#264710=CARTESIAN_POINT('Ctrl Pts',(44.5079524583205,-55.0866764015906,
-37.7352625));
#264711=CARTESIAN_POINT('Ctrl Pts',(43.4735820751078,-55.6838704207802,
-37.6769291666667));
#264712=CARTESIAN_POINT('Ctrl Pts',(42.4392116918951,-56.2810644399698,
-37.6185958333333));
#264713=CARTESIAN_POINT('Ctrl Pts',(42.439211691895,-57.4754524783491,-37.5602625));
#264714=CARTESIAN_POINT('Ctrl Pts',(42.4392116918951,-58.6698405167284,
-37.5019291666667));
#264715=CARTESIAN_POINT('Ctrl Pts',(43.4735820751078,-59.267034535918,-37.4435958333333));
#264716=CARTESIAN_POINT('Ctrl Pts',(44.5079524583205,-59.8642285551076,
-37.3852625));
#264717=CARTESIAN_POINT('Ctrl Pts',(45.5423228415332,-59.267034535918,-37.3269291666667));
#264718=CARTESIAN_POINT('Ctrl Pts',(46.5766932247459,-58.6698405167284,
-37.2685958333333));
#264719=CARTESIAN_POINT('Ctrl Pts',(46.5766932247459,-57.4754524783491,
-37.2102625));
#264720=CARTESIAN_POINT('Ctrl Pts',(46.5766932247459,-56.2810644399698,
-37.1519291666667));
#264721=CARTESIAN_POINT('Ctrl Pts',(45.5423228415332,-55.6838704207802,
-37.0935958333333));
#264722=CARTESIAN_POINT('Ctrl Pts',(44.5079524583205,-55.0866764015906,
-37.0352625));
#264723=CARTESIAN_POINT('Ctrl Pts',(43.4735820751078,-55.6838704207802,
-36.9769291666667));
#264724=CARTESIAN_POINT('Ctrl Pts',(42.4392116918951,-56.2810644399698,
-36.9185958333333));
#264725=CARTESIAN_POINT('Ctrl Pts',(42.439211691895,-57.4754524783491,-36.8602625));
#264726=CARTESIAN_POINT('Ctrl Pts',(42.4392116918951,-58.6698405167284,
-36.8019291666666));
#264727=CARTESIAN_POINT('Ctrl Pts',(43.4735820751078,-59.267034535918,-36.7435958333334));
#264728=CARTESIAN_POINT('Ctrl Pts',(44.5079524583205,-59.8642285551076,
-36.6852625));
#264729=CARTESIAN_POINT('Ctrl Pts',(45.5423228415332,-59.267034535918,-36.6269291666667));
#264730=CARTESIAN_POINT('Ctrl Pts',(45.6766051604217,-59.1895066029603,
-36.6193563132714));
#264731=CARTESIAN_POINT('Ctrl Pts',(45.7978303778615,-59.0928279175564,
-36.611216324118));
#264732=CARTESIAN_POINT('Ctrl Pts',(46.1766977413729,-57.4754524783491,
-52.8412));
#264733=CARTESIAN_POINT('Ctrl Pts',(46.1766977413729,-56.5120019399699,
-52.7828666666667));
#264734=CARTESIAN_POINT('Ctrl Pts',(45.3423250998467,-56.0302766707802,
-52.7245333333334));
#264735=CARTESIAN_POINT('Ctrl Pts',(44.5079524583205,-55.5485514015906,
-52.6662));
#264736=CARTESIAN_POINT('Ctrl Pts',(43.6735798167943,-56.0302766707802,
-52.6078666666667));
#264737=CARTESIAN_POINT('Ctrl Pts',(42.839207175268,-56.5120019399698,-52.5495333333333));
#264738=CARTESIAN_POINT('Ctrl Pts',(42.839207175268,-57.4754524783491,-52.4912));
#264739=CARTESIAN_POINT('Ctrl Pts',(42.839207175268,-58.4389030167283,-52.4328666666667));
#264740=CARTESIAN_POINT('Ctrl Pts',(43.6735798167943,-58.920628285918,-52.3745333333334));
#264741=CARTESIAN_POINT('Ctrl Pts',(44.5079524583205,-59.4023535551075,
-52.3162000000001));
#264742=CARTESIAN_POINT('Ctrl Pts',(45.3423250998467,-58.920628285918,-52.2578666666667));
#264743=CARTESIAN_POINT('Ctrl Pts',(46.1766977413729,-58.4389030167283,
-52.1995333333334));
#264744=CARTESIAN_POINT('Ctrl Pts',(46.1766977413729,-57.4754524783491,
-52.1412));
#264745=CARTESIAN_POINT('Ctrl Pts',(46.1766977413729,-56.5120019399699,
-52.0828666666667));
#264746=CARTESIAN_POINT('Ctrl Pts',(45.3423250998467,-56.0302766707802,
-52.0245333333333));
#264747=CARTESIAN_POINT('Ctrl Pts',(44.5079524583205,-55.5485514015906,
-51.9662));
#264748=CARTESIAN_POINT('Ctrl Pts',(43.6735798167943,-56.0302766707802,
-51.9078666666667));
#264749=CARTESIAN_POINT('Ctrl Pts',(42.839207175268,-56.5120019399698,-51.8495333333334));
#264750=CARTESIAN_POINT('Ctrl Pts',(42.839207175268,-57.4754524783491,-51.7912));
#264751=CARTESIAN_POINT('Ctrl Pts',(42.839207175268,-58.4389030167283,-51.7328666666667));
#264752=CARTESIAN_POINT('Ctrl Pts',(43.6735798167943,-58.920628285918,-51.6745333333334));
#264753=CARTESIAN_POINT('Ctrl Pts',(44.5079524583205,-59.4023535551075,
-51.6162));
#264754=CARTESIAN_POINT('Ctrl Pts',(45.3423250998467,-58.920628285918,-51.5578666666667));
#264755=CARTESIAN_POINT('Ctrl Pts',(46.1766977413729,-58.4389030167283,
-51.4995333333334));
#264756=CARTESIAN_POINT('Ctrl Pts',(46.1766977413729,-57.4754524783491,
-51.4412));
#264757=CARTESIAN_POINT('Ctrl Pts',(46.1766977413729,-56.5120019399699,
-51.3828666666667));
#264758=CARTESIAN_POINT('Ctrl Pts',(45.3423250998467,-56.0302766707802,
-51.3245333333334));
#264759=CARTESIAN_POINT('Ctrl Pts',(44.5079524583205,-55.5485514015906,
-51.2662));
#264760=CARTESIAN_POINT('Ctrl Pts',(43.6735798167943,-56.0302766707802,
-51.2078666666667));
#264761=CARTESIAN_POINT('Ctrl Pts',(42.839207175268,-56.5120019399698,-51.1495333333334));
#264762=CARTESIAN_POINT('Ctrl Pts',(42.839207175268,-57.4754524783491,-51.0912));
#264763=CARTESIAN_POINT('Ctrl Pts',(42.839207175268,-58.4389030167283,-51.0328666666667));
#264764=CARTESIAN_POINT('Ctrl Pts',(43.6735798167943,-58.920628285918,-50.9745333333333));
#264765=CARTESIAN_POINT('Ctrl Pts',(44.5079524583205,-59.4023535551075,
-50.9162));
#264766=CARTESIAN_POINT('Ctrl Pts',(45.3423250998467,-58.920628285918,-50.8578666666667));
#264767=CARTESIAN_POINT('Ctrl Pts',(46.1766977413729,-58.4389030167283,
-50.7995333333334));
#264768=CARTESIAN_POINT('Ctrl Pts',(46.1766977413729,-57.4754524783491,
-50.7412));
#264769=CARTESIAN_POINT('Ctrl Pts',(46.1766977413729,-56.5120019399699,
-50.6828666666667));
#264770=CARTESIAN_POINT('Ctrl Pts',(45.3423250998467,-56.0302766707802,
-50.6245333333333));
#264771=CARTESIAN_POINT('Ctrl Pts',(44.5079524583205,-55.5485514015906,
-50.5662));
#264772=CARTESIAN_POINT('Ctrl Pts',(43.6735798167943,-56.0302766707802,
-50.5078666666667));
#264773=CARTESIAN_POINT('Ctrl Pts',(42.839207175268,-56.5120019399698,-50.4495333333333));
#264774=CARTESIAN_POINT('Ctrl Pts',(42.839207175268,-57.4754524783491,-50.3912));
#264775=CARTESIAN_POINT('Ctrl Pts',(42.839207175268,-58.4389030167283,-50.3328666666667));
#264776=CARTESIAN_POINT('Ctrl Pts',(43.6735798167943,-58.920628285918,-50.2745333333334));
#264777=CARTESIAN_POINT('Ctrl Pts',(44.5079524583205,-59.4023535551075,
-50.2162));
#264778=CARTESIAN_POINT('Ctrl Pts',(45.3423250998467,-58.920628285918,-50.1578666666667));
#264779=CARTESIAN_POINT('Ctrl Pts',(46.1766977413729,-58.4389030167283,
-50.0995333333333));
#264780=CARTESIAN_POINT('Ctrl Pts',(46.1766977413729,-57.4754524783491,
-50.0412));
#264781=CARTESIAN_POINT('Ctrl Pts',(46.1766977413729,-56.5120019399699,
-49.9828666666667));
#264782=CARTESIAN_POINT('Ctrl Pts',(45.3423250998467,-56.0302766707802,
-49.9245333333334));
#264783=CARTESIAN_POINT('Ctrl Pts',(44.5079524583205,-55.5485514015906,
-49.8662));
#264784=CARTESIAN_POINT('Ctrl Pts',(43.6735798167943,-56.0302766707802,
-49.8078666666667));
#264785=CARTESIAN_POINT('Ctrl Pts',(42.839207175268,-56.5120019399698,-49.7495333333333));
#264786=CARTESIAN_POINT('Ctrl Pts',(42.839207175268,-57.4754524783491,-49.6912));
#264787=CARTESIAN_POINT('Ctrl Pts',(42.839207175268,-58.4389030167283,-49.6328666666667));
#264788=CARTESIAN_POINT('Ctrl Pts',(43.6735798167943,-58.920628285918,-49.5745333333334));
#264789=CARTESIAN_POINT('Ctrl Pts',(44.5079524583205,-59.4023535551075,
-49.5162));
#264790=CARTESIAN_POINT('Ctrl Pts',(45.3423250998467,-58.920628285918,-49.4578666666667));
#264791=CARTESIAN_POINT('Ctrl Pts',(46.1766977413729,-58.4389030167283,
-49.3995333333333));
#264792=CARTESIAN_POINT('Ctrl Pts',(46.1766977413729,-57.4754524783491,
-49.3412));
#264793=CARTESIAN_POINT('Ctrl Pts',(46.1766977413729,-56.5120019399699,
-49.2828666666666));
#264794=CARTESIAN_POINT('Ctrl Pts',(45.3423250998467,-56.0302766707802,
-49.2245333333334));
#264795=CARTESIAN_POINT('Ctrl Pts',(44.5079524583205,-55.5485514015906,
-49.1662));
#264796=CARTESIAN_POINT('Ctrl Pts',(43.6735798167943,-56.0302766707802,
-49.1078666666667));
#264797=CARTESIAN_POINT('Ctrl Pts',(42.839207175268,-56.5120019399698,-49.0495333333334));
#264798=CARTESIAN_POINT('Ctrl Pts',(42.839207175268,-57.4754524783491,-48.9912));
#264799=CARTESIAN_POINT('Ctrl Pts',(42.839207175268,-58.4389030167283,-48.9328666666667));
#264800=CARTESIAN_POINT('Ctrl Pts',(43.6735798167943,-58.920628285918,-48.8745333333334));
#264801=CARTESIAN_POINT('Ctrl Pts',(44.5079524583205,-59.4023535551075,
-48.8162));
#264802=CARTESIAN_POINT('Ctrl Pts',(45.3423250998467,-58.920628285918,-48.7578666666667));
#264803=CARTESIAN_POINT('Ctrl Pts',(46.1766977413729,-58.4389030167283,
-48.6995333333334));
#264804=CARTESIAN_POINT('Ctrl Pts',(46.1766977413729,-57.4754524783491,
-48.6412));
#264805=CARTESIAN_POINT('Ctrl Pts',(46.1766977413729,-56.5120019399699,
-48.5828666666667));
#264806=CARTESIAN_POINT('Ctrl Pts',(45.3423250998467,-56.0302766707802,
-48.5245333333334));
#264807=CARTESIAN_POINT('Ctrl Pts',(44.5079524583205,-55.5485514015906,
-48.4662));
#264808=CARTESIAN_POINT('Ctrl Pts',(43.6735798167943,-56.0302766707802,
-48.4078666666667));
#264809=CARTESIAN_POINT('Ctrl Pts',(42.839207175268,-56.5120019399698,-48.3495333333333));
#264810=CARTESIAN_POINT('Ctrl Pts',(42.839207175268,-57.4754524783491,-48.2912));
#264811=CARTESIAN_POINT('Ctrl Pts',(42.839207175268,-58.4389030167283,-48.2328666666667));
#264812=CARTESIAN_POINT('Ctrl Pts',(43.6735798167943,-58.920628285918,-48.1745333333334));
#264813=CARTESIAN_POINT('Ctrl Pts',(44.5079524583205,-59.4023535551075,
-48.1162));
#264814=CARTESIAN_POINT('Ctrl Pts',(45.3423250998467,-58.920628285918,-48.0578666666667));
#264815=CARTESIAN_POINT('Ctrl Pts',(46.1766977413729,-58.4389030167283,
-47.9995333333334));
#264816=CARTESIAN_POINT('Ctrl Pts',(46.1766977413729,-57.4754524783491,
-47.9412));
#264817=CARTESIAN_POINT('Ctrl Pts',(46.1766977413729,-56.5120019399699,
-47.8828666666667));
#264818=CARTESIAN_POINT('Ctrl Pts',(45.3423250998467,-56.0302766707802,
-47.8245333333333));
#264819=CARTESIAN_POINT('Ctrl Pts',(44.5079524583205,-55.5485514015906,
-47.7662));
#264820=CARTESIAN_POINT('Ctrl Pts',(43.6735798167943,-56.0302766707802,
-47.7078666666667));
#264821=CARTESIAN_POINT('Ctrl Pts',(42.839207175268,-56.5120019399698,-47.6495333333334));
#264822=CARTESIAN_POINT('Ctrl Pts',(42.839207175268,-57.4754524783491,-47.5912));
#264823=CARTESIAN_POINT('Ctrl Pts',(42.839207175268,-58.4389030167283,-47.5328666666667));
#264824=CARTESIAN_POINT('Ctrl Pts',(43.6735798167943,-58.920628285918,-47.4745333333334));
#264825=CARTESIAN_POINT('Ctrl Pts',(44.5079524583205,-59.4023535551075,
-47.4162));
#264826=CARTESIAN_POINT('Ctrl Pts',(45.3423250998467,-58.920628285918,-47.3578666666667));
#264827=CARTESIAN_POINT('Ctrl Pts',(46.1766977413729,-58.4389030167283,
-47.2995333333334));
#264828=CARTESIAN_POINT('Ctrl Pts',(46.1766977413729,-57.4754524783491,
-47.2412));
#264829=CARTESIAN_POINT('Ctrl Pts',(46.1766977413729,-56.5120019399699,
-47.1828666666667));
#264830=CARTESIAN_POINT('Ctrl Pts',(45.3423250998467,-56.0302766707802,
-47.1245333333333));
#264831=CARTESIAN_POINT('Ctrl Pts',(44.5079524583205,-55.5485514015906,
-47.0662));
#264832=CARTESIAN_POINT('Ctrl Pts',(43.6735798167943,-56.0302766707802,
-47.0078666666667));
#264833=CARTESIAN_POINT('Ctrl Pts',(42.839207175268,-56.5120019399698,-46.9495333333334));
#264834=CARTESIAN_POINT('Ctrl Pts',(42.839207175268,-57.4754524783491,-46.8912));
#264835=CARTESIAN_POINT('Ctrl Pts',(42.839207175268,-58.4389030167283,-46.8328666666667));
#264836=CARTESIAN_POINT('Ctrl Pts',(43.6735798167943,-58.920628285918,-46.7745333333334));
#264837=CARTESIAN_POINT('Ctrl Pts',(44.5079524583205,-59.4023535551075,
-46.7162));
#264838=CARTESIAN_POINT('Ctrl Pts',(45.3423250998467,-58.920628285918,-46.6578666666667));
#264839=CARTESIAN_POINT('Ctrl Pts',(46.1766977413729,-58.4389030167283,
-46.5995333333334));
#264840=CARTESIAN_POINT('Ctrl Pts',(46.1766977413729,-57.4754524783491,
-46.5412));
#264841=CARTESIAN_POINT('Ctrl Pts',(46.1766977413729,-56.5120019399699,
-46.4828666666667));
#264842=CARTESIAN_POINT('Ctrl Pts',(45.3423250998467,-56.0302766707802,
-46.4245333333334));
#264843=CARTESIAN_POINT('Ctrl Pts',(44.5079524583205,-55.5485514015906,
-46.3662));
#264844=CARTESIAN_POINT('Ctrl Pts',(43.6735798167943,-56.0302766707802,
-46.3078666666667));
#264845=CARTESIAN_POINT('Ctrl Pts',(42.839207175268,-56.5120019399698,-46.2495333333334));
#264846=CARTESIAN_POINT('Ctrl Pts',(42.839207175268,-57.4754524783491,-46.1912));
#264847=CARTESIAN_POINT('Ctrl Pts',(42.839207175268,-58.4389030167283,-46.1328666666667));
#264848=CARTESIAN_POINT('Ctrl Pts',(43.6735798167943,-58.920628285918,-46.0745333333334));
#264849=CARTESIAN_POINT('Ctrl Pts',(44.5079524583205,-59.4023535551075,
-46.0162));
#264850=CARTESIAN_POINT('Ctrl Pts',(45.3423250998467,-58.920628285918,-45.9578666666667));
#264851=CARTESIAN_POINT('Ctrl Pts',(46.1766977413729,-58.4389030167283,
-45.8995333333333));
#264852=CARTESIAN_POINT('Ctrl Pts',(46.1766977413729,-57.4754524783491,
-45.8412));
#264853=CARTESIAN_POINT('Ctrl Pts',(46.1766977413729,-56.5120019399699,
-45.7828666666667));
#264854=CARTESIAN_POINT('Ctrl Pts',(45.3423250998467,-56.0302766707802,
-45.7245333333333));
#264855=CARTESIAN_POINT('Ctrl Pts',(44.5079524583205,-55.5485514015906,
-45.6662));
#264856=CARTESIAN_POINT('Ctrl Pts',(43.6735798167943,-56.0302766707802,
-45.6078666666667));
#264857=CARTESIAN_POINT('Ctrl Pts',(42.839207175268,-56.5120019399698,-45.5495333333333));
#264858=CARTESIAN_POINT('Ctrl Pts',(42.839207175268,-57.4754524783491,-45.4912));
#264859=CARTESIAN_POINT('Ctrl Pts',(42.839207175268,-58.4389030167283,-45.4328666666666));
#264860=CARTESIAN_POINT('Ctrl Pts',(43.6735798167943,-58.920628285918,-45.3745333333334));
#264861=CARTESIAN_POINT('Ctrl Pts',(44.5079524583205,-59.4023535551075,
-45.3162));
#264862=CARTESIAN_POINT('Ctrl Pts',(45.3423250998467,-58.920628285918,-45.2578666666667));
#264863=CARTESIAN_POINT('Ctrl Pts',(46.1766977413729,-58.4389030167283,
-45.1995333333333));
#264864=CARTESIAN_POINT('Ctrl Pts',(46.1766977413729,-57.4754524783491,
-45.1412));
#264865=CARTESIAN_POINT('Ctrl Pts',(46.1766977413729,-56.5120019399699,
-45.0828666666667));
#264866=CARTESIAN_POINT('Ctrl Pts',(45.3423250998467,-56.0302766707802,
-45.0245333333334));
#264867=CARTESIAN_POINT('Ctrl Pts',(44.5079524583205,-55.5485514015906,
-44.9662));
#264868=CARTESIAN_POINT('Ctrl Pts',(43.6735798167943,-56.0302766707802,
-44.9078666666667));
#264869=CARTESIAN_POINT('Ctrl Pts',(42.839207175268,-56.5120019399698,-44.8495333333333));
#264870=CARTESIAN_POINT('Ctrl Pts',(42.839207175268,-57.4754524783491,-44.7912));
#264871=CARTESIAN_POINT('Ctrl Pts',(42.839207175268,-58.4389030167283,-44.7328666666667));
#264872=CARTESIAN_POINT('Ctrl Pts',(43.6735798167943,-58.920628285918,-44.6745333333334));
#264873=CARTESIAN_POINT('Ctrl Pts',(44.5079524583205,-59.4023535551075,
-44.6162));
#264874=CARTESIAN_POINT('Ctrl Pts',(45.3423250998467,-58.920628285918,-44.5578666666667));
#264875=CARTESIAN_POINT('Ctrl Pts',(46.1766977413729,-58.4389030167283,
-44.4995333333333));
#264876=CARTESIAN_POINT('Ctrl Pts',(46.1766977413729,-57.4754524783491,
-44.4412));
#264877=CARTESIAN_POINT('Ctrl Pts',(46.1766977413729,-56.5120019399699,
-44.3828666666667));
#264878=CARTESIAN_POINT('Ctrl Pts',(45.3423250998467,-56.0302766707802,
-44.3245333333334));
#264879=CARTESIAN_POINT('Ctrl Pts',(44.5079524583205,-55.5485514015906,
-44.2662));
#264880=CARTESIAN_POINT('Ctrl Pts',(43.6735798167943,-56.0302766707802,
-44.2078666666667));
#264881=CARTESIAN_POINT('Ctrl Pts',(42.839207175268,-56.5120019399698,-44.1495333333334));
#264882=CARTESIAN_POINT('Ctrl Pts',(42.839207175268,-57.4754524783491,-44.0912));
#264883=CARTESIAN_POINT('Ctrl Pts',(42.839207175268,-58.4389030167283,-44.0328666666667));
#264884=CARTESIAN_POINT('Ctrl Pts',(43.6735798167943,-58.920628285918,-43.9745333333333));
#264885=CARTESIAN_POINT('Ctrl Pts',(44.5079524583205,-59.4023535551075,
-43.9162));
#264886=CARTESIAN_POINT('Ctrl Pts',(45.3423250998467,-58.920628285918,-43.8578666666667));
#264887=CARTESIAN_POINT('Ctrl Pts',(46.1766977413729,-58.4389030167283,
-43.7995333333334));
#264888=CARTESIAN_POINT('Ctrl Pts',(46.1766977413729,-57.4754524783491,
-43.7412));
#264889=CARTESIAN_POINT('Ctrl Pts',(46.1766977413729,-56.5120019399699,
-43.6828666666667));
#264890=CARTESIAN_POINT('Ctrl Pts',(45.3423250998467,-56.0302766707802,
-43.6245333333333));
#264891=CARTESIAN_POINT('Ctrl Pts',(44.5079524583205,-55.5485514015906,
-43.5662));
#264892=CARTESIAN_POINT('Ctrl Pts',(43.6735798167943,-56.0302766707802,
-43.5078666666667));
#264893=CARTESIAN_POINT('Ctrl Pts',(42.839207175268,-56.5120019399698,-43.4495333333334));
#264894=CARTESIAN_POINT('Ctrl Pts',(42.839207175268,-57.4754524783491,-43.3912));
#264895=CARTESIAN_POINT('Ctrl Pts',(42.839207175268,-58.4389030167283,-43.3328666666667));
#264896=CARTESIAN_POINT('Ctrl Pts',(43.6735798167943,-58.920628285918,-43.2745333333334));
#264897=CARTESIAN_POINT('Ctrl Pts',(44.5079524583205,-59.4023535551075,
-43.2162));
#264898=CARTESIAN_POINT('Ctrl Pts',(45.3423250998467,-58.920628285918,-43.1578666666667));
#264899=CARTESIAN_POINT('Ctrl Pts',(46.1766977413729,-58.4389030167283,
-43.0995333333334));
#264900=CARTESIAN_POINT('Ctrl Pts',(46.1766977413729,-57.4754524783491,
-43.0412));
#264901=CARTESIAN_POINT('Ctrl Pts',(46.1766977413729,-56.5120019399699,
-42.9828666666667));
#264902=CARTESIAN_POINT('Ctrl Pts',(45.3423250998467,-56.0302766707802,
-42.9245333333334));
#264903=CARTESIAN_POINT('Ctrl Pts',(44.5079524583205,-55.5485514015906,
-42.8662));
#264904=CARTESIAN_POINT('Ctrl Pts',(43.6735798167943,-56.0302766707802,
-42.8078666666667));
#264905=CARTESIAN_POINT('Ctrl Pts',(42.839207175268,-56.5120019399698,-42.7495333333334));
#264906=CARTESIAN_POINT('Ctrl Pts',(42.839207175268,-57.4754524783491,-42.6912));
#264907=CARTESIAN_POINT('Ctrl Pts',(42.839207175268,-58.4389030167283,-42.6328666666667));
#264908=CARTESIAN_POINT('Ctrl Pts',(43.6735798167943,-58.920628285918,-42.5745333333333));
#264909=CARTESIAN_POINT('Ctrl Pts',(44.5079524583205,-59.4023535551075,
-42.5162));
#264910=CARTESIAN_POINT('Ctrl Pts',(45.3423250998467,-58.920628285918,-42.4578666666667));
#264911=CARTESIAN_POINT('Ctrl Pts',(46.1766977413729,-58.4389030167283,
-42.3995333333334));
#264912=CARTESIAN_POINT('Ctrl Pts',(46.1766977413729,-57.4754524783491,
-42.3412));
#264913=CARTESIAN_POINT('Ctrl Pts',(46.1766977413729,-56.5120019399699,
-42.2828666666667));
#264914=CARTESIAN_POINT('Ctrl Pts',(45.3423250998467,-56.0302766707802,
-42.2245333333333));
#264915=CARTESIAN_POINT('Ctrl Pts',(44.5079524583205,-55.5485514015906,
-42.1662));
#264916=CARTESIAN_POINT('Ctrl Pts',(43.6735798167943,-56.0302766707802,
-42.1078666666667));
#264917=CARTESIAN_POINT('Ctrl Pts',(42.839207175268,-56.5120019399698,-42.0495333333334));
#264918=CARTESIAN_POINT('Ctrl Pts',(42.839207175268,-57.4754524783491,-41.9912));
#264919=CARTESIAN_POINT('Ctrl Pts',(42.839207175268,-58.4389030167283,-41.9328666666667));
#264920=CARTESIAN_POINT('Ctrl Pts',(43.6735798167943,-58.920628285918,-41.8745333333334));
#264921=CARTESIAN_POINT('Ctrl Pts',(44.5079524583205,-59.4023535551075,
-41.8162));
#264922=CARTESIAN_POINT('Ctrl Pts',(45.3423250998467,-58.920628285918,-41.7578666666667));
#264923=CARTESIAN_POINT('Ctrl Pts',(46.1766977413729,-58.4389030167283,
-41.6995333333334));
#264924=CARTESIAN_POINT('Ctrl Pts',(46.1766977413729,-57.4754524783491,
-41.6412));
#264925=CARTESIAN_POINT('Ctrl Pts',(46.1766977413729,-56.5120019399699,
-41.5828666666667));
#264926=CARTESIAN_POINT('Ctrl Pts',(45.3423250998467,-56.0302766707802,
-41.5245333333334));
#264927=CARTESIAN_POINT('Ctrl Pts',(44.5079524583205,-55.5485514015906,
-41.4662));
#264928=CARTESIAN_POINT('Ctrl Pts',(43.6735798167943,-56.0302766707802,
-41.4078666666667));
#264929=CARTESIAN_POINT('Ctrl Pts',(42.839207175268,-56.5120019399698,-41.3495333333333));
#264930=CARTESIAN_POINT('Ctrl Pts',(42.839207175268,-57.4754524783491,-41.2912));
#264931=CARTESIAN_POINT('Ctrl Pts',(42.839207175268,-58.4389030167283,-41.2328666666667));
#264932=CARTESIAN_POINT('Ctrl Pts',(43.6735798167943,-58.920628285918,-41.1745333333334));
#264933=CARTESIAN_POINT('Ctrl Pts',(44.5079524583205,-59.4023535551075,
-41.1162));
#264934=CARTESIAN_POINT('Ctrl Pts',(45.3423250998467,-58.920628285918,-41.0578666666667));
#264935=CARTESIAN_POINT('Ctrl Pts',(46.1766977413729,-58.4389030167283,
-40.9995333333333));
#264936=CARTESIAN_POINT('Ctrl Pts',(46.1766977413729,-57.4754524783491,
-40.9412));
#264937=CARTESIAN_POINT('Ctrl Pts',(46.1766977413729,-56.5120019399699,
-40.8828666666667));
#264938=CARTESIAN_POINT('Ctrl Pts',(45.3423250998467,-56.0302766707802,
-40.8245333333333));
#264939=CARTESIAN_POINT('Ctrl Pts',(44.5079524583205,-55.5485514015906,
-40.7662));
#264940=CARTESIAN_POINT('Ctrl Pts',(43.6735798167943,-56.0302766707802,
-40.7078666666667));
#264941=CARTESIAN_POINT('Ctrl Pts',(42.839207175268,-56.5120019399698,-40.6495333333334));
#264942=CARTESIAN_POINT('Ctrl Pts',(42.839207175268,-57.4754524783491,-40.5912));
#264943=CARTESIAN_POINT('Ctrl Pts',(42.839207175268,-58.4389030167283,-40.5328666666667));
#264944=CARTESIAN_POINT('Ctrl Pts',(43.6735798167943,-58.920628285918,-40.4745333333334));
#264945=CARTESIAN_POINT('Ctrl Pts',(44.5079524583205,-59.4023535551075,
-40.4162));
#264946=CARTESIAN_POINT('Ctrl Pts',(45.3423250998467,-58.920628285918,-40.3578666666667));
#264947=CARTESIAN_POINT('Ctrl Pts',(46.1766977413729,-58.4389030167283,
-40.2995333333333));
#264948=CARTESIAN_POINT('Ctrl Pts',(46.1766977413729,-57.4754524783491,
-40.2412));
#264949=CARTESIAN_POINT('Ctrl Pts',(46.1766977413729,-56.5120019399699,
-40.1828666666667));
#264950=CARTESIAN_POINT('Ctrl Pts',(45.3423250998467,-56.0302766707802,
-40.1245333333334));
#264951=CARTESIAN_POINT('Ctrl Pts',(44.5079524583205,-55.5485514015906,
-40.0662));
#264952=CARTESIAN_POINT('Ctrl Pts',(43.6735798167943,-56.0302766707802,
-40.0078666666667));
#264953=CARTESIAN_POINT('Ctrl Pts',(42.839207175268,-56.5120019399698,-39.9495333333333));
#264954=CARTESIAN_POINT('Ctrl Pts',(42.839207175268,-57.4754524783491,-39.8912));
#264955=CARTESIAN_POINT('Ctrl Pts',(42.839207175268,-58.4389030167283,-39.8328666666666));
#264956=CARTESIAN_POINT('Ctrl Pts',(43.6735798167943,-58.920628285918,-39.7745333333334));
#264957=CARTESIAN_POINT('Ctrl Pts',(44.5079524583205,-59.4023535551075,
-39.7162));
#264958=CARTESIAN_POINT('Ctrl Pts',(45.3423250998467,-58.920628285918,-39.6578666666667));
#264959=CARTESIAN_POINT('Ctrl Pts',(46.1766977413729,-58.4389030167283,
-39.5995333333333));
#264960=CARTESIAN_POINT('Ctrl Pts',(46.1766977413729,-57.4754524783491,
-39.5412));
#264961=CARTESIAN_POINT('Ctrl Pts',(46.1766977413729,-56.5120019399699,
-39.4828666666666));
#264962=CARTESIAN_POINT('Ctrl Pts',(45.3423250998467,-56.0302766707802,
-39.4245333333334));
#264963=CARTESIAN_POINT('Ctrl Pts',(44.5079524583205,-55.5485514015906,
-39.3662));
#264964=CARTESIAN_POINT('Ctrl Pts',(43.6735798167943,-56.0302766707802,
-39.3078666666667));
#264965=CARTESIAN_POINT('Ctrl Pts',(42.839207175268,-56.5120019399698,-39.2495333333333));
#264966=CARTESIAN_POINT('Ctrl Pts',(42.839207175268,-57.4754524783491,-39.1912));
#264967=CARTESIAN_POINT('Ctrl Pts',(42.839207175268,-58.4389030167283,-39.1328666666667));
#264968=CARTESIAN_POINT('Ctrl Pts',(43.6735798167943,-58.920628285918,-39.0745333333333));
#264969=CARTESIAN_POINT('Ctrl Pts',(44.5079524583205,-59.4023535551075,
-39.0162));
#264970=CARTESIAN_POINT('Ctrl Pts',(45.3423250998467,-58.920628285918,-38.9578666666667));
#264971=CARTESIAN_POINT('Ctrl Pts',(46.1766977413729,-58.4389030167283,
-38.8995333333334));
#264972=CARTESIAN_POINT('Ctrl Pts',(46.1766977413729,-57.4754524783491,
-38.8412));
#264973=CARTESIAN_POINT('Ctrl Pts',(46.1766977413729,-56.5120019399699,
-38.7828666666667));
#264974=CARTESIAN_POINT('Ctrl Pts',(45.3423250998467,-56.0302766707802,
-38.7245333333334));
#264975=CARTESIAN_POINT('Ctrl Pts',(44.5079524583205,-55.5485514015906,
-38.6662));
#264976=CARTESIAN_POINT('Ctrl Pts',(43.6735798167943,-56.0302766707802,
-38.6078666666667));
#264977=CARTESIAN_POINT('Ctrl Pts',(42.839207175268,-56.5120019399698,-38.5495333333334));
#264978=CARTESIAN_POINT('Ctrl Pts',(42.839207175268,-57.4754524783491,-38.4912));
#264979=CARTESIAN_POINT('Ctrl Pts',(42.839207175268,-58.4389030167283,-38.4328666666667));
#264980=CARTESIAN_POINT('Ctrl Pts',(43.6735798167943,-58.920628285918,-38.3745333333333));
#264981=CARTESIAN_POINT('Ctrl Pts',(44.5079524583205,-59.4023535551075,
-38.3162));
#264982=CARTESIAN_POINT('Ctrl Pts',(45.3423250998467,-58.920628285918,-38.2578666666667));
#264983=CARTESIAN_POINT('Ctrl Pts',(46.1766977413729,-58.4389030167283,
-38.1995333333333));
#264984=CARTESIAN_POINT('Ctrl Pts',(46.1766977413729,-57.4754524783491,
-38.1412));
#264985=CARTESIAN_POINT('Ctrl Pts',(46.1766977413729,-56.5120019399699,
-38.0828666666667));
#264986=CARTESIAN_POINT('Ctrl Pts',(45.3423250998467,-56.0302766707802,
-38.0245333333334));
#264987=CARTESIAN_POINT('Ctrl Pts',(44.5079524583205,-55.5485514015906,
-37.9662));
#264988=CARTESIAN_POINT('Ctrl Pts',(43.6735798167943,-56.0302766707802,
-37.9078666666667));
#264989=CARTESIAN_POINT('Ctrl Pts',(42.839207175268,-56.5120019399698,-37.8495333333334));
#264990=CARTESIAN_POINT('Ctrl Pts',(42.839207175268,-57.4754524783491,-37.7912));
#264991=CARTESIAN_POINT('Ctrl Pts',(42.839207175268,-58.4389030167283,-37.7328666666667));
#264992=CARTESIAN_POINT('Ctrl Pts',(43.6735798167943,-58.920628285918,-37.6745333333334));
#264993=CARTESIAN_POINT('Ctrl Pts',(44.5079524583205,-59.4023535551075,
-37.6162));
#264994=CARTESIAN_POINT('Ctrl Pts',(45.3423250998467,-58.920628285918,-37.5578666666667));
#264995=CARTESIAN_POINT('Ctrl Pts',(46.1766977413729,-58.4389030167283,
-37.4995333333334));
#264996=CARTESIAN_POINT('Ctrl Pts',(46.1766977413729,-57.4754524783491,
-37.4412));
#264997=CARTESIAN_POINT('Ctrl Pts',(46.1766977413729,-56.5120019399699,
-37.3828666666667));
#264998=CARTESIAN_POINT('Ctrl Pts',(45.3423250998467,-56.0302766707802,
-37.3245333333333));
#264999=CARTESIAN_POINT('Ctrl Pts',(44.5079524583205,-55.5485514015906,
-37.2662));
#265000=CARTESIAN_POINT('Ctrl Pts',(43.6735798167943,-56.0302766707802,
-37.2078666666667));
#265001=CARTESIAN_POINT('Ctrl Pts',(42.839207175268,-56.5120019399698,-37.1495333333334));
#265002=CARTESIAN_POINT('Ctrl Pts',(42.839207175268,-57.4754524783491,-37.0912));
#265003=CARTESIAN_POINT('Ctrl Pts',(42.839207175268,-58.4389030167283,-37.0328666666667));
#265004=CARTESIAN_POINT('Ctrl Pts',(43.6735798167943,-58.920628285918,-36.9745333333333));
#265005=CARTESIAN_POINT('Ctrl Pts',(44.5079524583205,-59.4023535551075,
-36.9162));
#265006=CARTESIAN_POINT('Ctrl Pts',(45.3423250998467,-58.920628285918,-36.8578666666667));
#265007=CARTESIAN_POINT('Ctrl Pts',(45.4506436431264,-58.8580905457972,
-36.8502938132714));
#265008=CARTESIAN_POINT('Ctrl Pts',(45.5484297036483,-58.7801048924675,
-36.8421538241181));
#265009=CARTESIAN_POINT('Ctrl Pts',(46.5766932247459,-57.4754524783491,
-52.6102625));
#265010=CARTESIAN_POINT('Ctrl Pts',(46.5766932247459,-56.2810644399698,
-52.5519291666666));
#265011=CARTESIAN_POINT('Ctrl Pts',(45.5423228415332,-55.6838704207802,
-52.4935958333333));
#265012=CARTESIAN_POINT('Ctrl Pts',(44.5079524583205,-55.0866764015906,
-52.4352625000001));
#265013=CARTESIAN_POINT('Ctrl Pts',(43.4735820751078,-55.6838704207802,
-52.3769291666667));
#265014=CARTESIAN_POINT('Ctrl Pts',(42.4392116918951,-56.2810644399698,
-52.3185958333334));
#265015=CARTESIAN_POINT('Ctrl Pts',(42.439211691895,-57.4754524783491,-52.2602625));
#265016=CARTESIAN_POINT('Ctrl Pts',(42.4392116918951,-58.6698405167284,
-52.2019291666667));
#265017=CARTESIAN_POINT('Ctrl Pts',(43.4735820751078,-59.267034535918,-52.1435958333333));
#265018=CARTESIAN_POINT('Ctrl Pts',(44.5079524583205,-59.8642285551076,
-52.0852625));
#265019=CARTESIAN_POINT('Ctrl Pts',(45.5423228415332,-59.267034535918,-52.0269291666667));
#265020=CARTESIAN_POINT('Ctrl Pts',(46.5766932247459,-58.6698405167284,
-51.9685958333333));
#265021=CARTESIAN_POINT('Ctrl Pts',(46.5766932247459,-57.4754524783491,
-51.9102625));
#265022=CARTESIAN_POINT('Ctrl Pts',(46.5766932247459,-56.2810644399698,
-51.8519291666667));
#265023=CARTESIAN_POINT('Ctrl Pts',(45.5423228415332,-55.6838704207802,
-51.7935958333333));
#265024=CARTESIAN_POINT('Ctrl Pts',(44.5079524583205,-55.0866764015906,
-51.7352625));
#265025=CARTESIAN_POINT('Ctrl Pts',(43.4735820751078,-55.6838704207802,
-51.6769291666667));
#265026=CARTESIAN_POINT('Ctrl Pts',(42.4392116918951,-56.2810644399698,
-51.6185958333333));
#265027=CARTESIAN_POINT('Ctrl Pts',(42.439211691895,-57.4754524783491,-51.5602625));
#265028=CARTESIAN_POINT('Ctrl Pts',(42.4392116918951,-58.6698405167284,
-51.5019291666666));
#265029=CARTESIAN_POINT('Ctrl Pts',(43.4735820751078,-59.267034535918,-51.4435958333333));
#265030=CARTESIAN_POINT('Ctrl Pts',(44.5079524583205,-59.8642285551076,
-51.3852625));
#265031=CARTESIAN_POINT('Ctrl Pts',(45.5423228415332,-59.267034535918,-51.3269291666667));
#265032=CARTESIAN_POINT('Ctrl Pts',(46.5766932247459,-58.6698405167284,
-51.2685958333333));
#265033=CARTESIAN_POINT('Ctrl Pts',(46.5766932247459,-57.4754524783491,
-51.2102625));
#265034=CARTESIAN_POINT('Ctrl Pts',(46.5766932247459,-56.2810644399698,
-51.1519291666666));
#265035=CARTESIAN_POINT('Ctrl Pts',(45.5423228415332,-55.6838704207802,
-51.0935958333334));
#265036=CARTESIAN_POINT('Ctrl Pts',(44.5079524583205,-55.0866764015906,
-51.0352625));
#265037=CARTESIAN_POINT('Ctrl Pts',(43.4735820751078,-55.6838704207802,
-50.9769291666667));
#265038=CARTESIAN_POINT('Ctrl Pts',(42.4392116918951,-56.2810644399698,
-50.9185958333333));
#265039=CARTESIAN_POINT('Ctrl Pts',(42.439211691895,-57.4754524783491,-50.8602625));
#265040=CARTESIAN_POINT('Ctrl Pts',(42.4392116918951,-58.6698405167284,
-50.8019291666667));
#265041=CARTESIAN_POINT('Ctrl Pts',(43.4735820751078,-59.267034535918,-50.7435958333333));
#265042=CARTESIAN_POINT('Ctrl Pts',(44.5079524583205,-59.8642285551076,
-50.6852625));
#265043=CARTESIAN_POINT('Ctrl Pts',(45.5423228415332,-59.267034535918,-50.6269291666667));
#265044=CARTESIAN_POINT('Ctrl Pts',(46.5766932247459,-58.6698405167284,
-50.5685958333333));
#265045=CARTESIAN_POINT('Ctrl Pts',(46.5766932247459,-57.4754524783491,
-50.5102625));
#265046=CARTESIAN_POINT('Ctrl Pts',(46.5766932247459,-56.2810644399698,
-50.4519291666667));
#265047=CARTESIAN_POINT('Ctrl Pts',(45.5423228415332,-55.6838704207802,
-50.3935958333333));
#265048=CARTESIAN_POINT('Ctrl Pts',(44.5079524583205,-55.0866764015906,
-50.3352625));
#265049=CARTESIAN_POINT('Ctrl Pts',(43.4735820751078,-55.6838704207802,
-50.2769291666667));
#265050=CARTESIAN_POINT('Ctrl Pts',(42.4392116918951,-56.2810644399698,
-50.2185958333333));
#265051=CARTESIAN_POINT('Ctrl Pts',(42.439211691895,-57.4754524783491,-50.1602625));
#265052=CARTESIAN_POINT('Ctrl Pts',(42.4392116918951,-58.6698405167284,
-50.1019291666667));
#265053=CARTESIAN_POINT('Ctrl Pts',(43.4735820751078,-59.267034535918,-50.0435958333333));
#265054=CARTESIAN_POINT('Ctrl Pts',(44.5079524583205,-59.8642285551076,
-49.9852625));
#265055=CARTESIAN_POINT('Ctrl Pts',(45.5423228415332,-59.267034535918,-49.9269291666667));
#265056=CARTESIAN_POINT('Ctrl Pts',(46.5766932247459,-58.6698405167284,
-49.8685958333333));
#265057=CARTESIAN_POINT('Ctrl Pts',(46.5766932247459,-57.4754524783491,
-49.8102625));
#265058=CARTESIAN_POINT('Ctrl Pts',(46.5766932247459,-56.2810644399698,
-49.7519291666667));
#265059=CARTESIAN_POINT('Ctrl Pts',(45.5423228415332,-55.6838704207802,
-49.6935958333334));
#265060=CARTESIAN_POINT('Ctrl Pts',(44.5079524583205,-55.0866764015906,
-49.6352625));
#265061=CARTESIAN_POINT('Ctrl Pts',(43.4735820751078,-55.6838704207802,
-49.5769291666667));
#265062=CARTESIAN_POINT('Ctrl Pts',(42.4392116918951,-56.2810644399698,
-49.5185958333334));
#265063=CARTESIAN_POINT('Ctrl Pts',(42.439211691895,-57.4754524783491,-49.4602625));
#265064=CARTESIAN_POINT('Ctrl Pts',(42.4392116918951,-58.6698405167284,
-49.4019291666667));
#265065=CARTESIAN_POINT('Ctrl Pts',(43.4735820751078,-59.267034535918,-49.3435958333333));
#265066=CARTESIAN_POINT('Ctrl Pts',(44.5079524583205,-59.8642285551076,
-49.2852625));
#265067=CARTESIAN_POINT('Ctrl Pts',(45.5423228415332,-59.267034535918,-49.2269291666667));
#265068=CARTESIAN_POINT('Ctrl Pts',(46.5766932247459,-58.6698405167284,
-49.1685958333334));
#265069=CARTESIAN_POINT('Ctrl Pts',(46.5766932247459,-57.4754524783491,
-49.1102625));
#265070=CARTESIAN_POINT('Ctrl Pts',(46.5766932247459,-56.2810644399698,
-49.0519291666667));
#265071=CARTESIAN_POINT('Ctrl Pts',(45.5423228415332,-55.6838704207802,
-48.9935958333333));
#265072=CARTESIAN_POINT('Ctrl Pts',(44.5079524583205,-55.0866764015906,
-48.9352625));
#265073=CARTESIAN_POINT('Ctrl Pts',(43.4735820751078,-55.6838704207802,
-48.8769291666667));
#265074=CARTESIAN_POINT('Ctrl Pts',(42.4392116918951,-56.2810644399698,
-48.8185958333334));
#265075=CARTESIAN_POINT('Ctrl Pts',(42.439211691895,-57.4754524783491,-48.7602625));
#265076=CARTESIAN_POINT('Ctrl Pts',(42.4392116918951,-58.6698405167284,
-48.7019291666667));
#265077=CARTESIAN_POINT('Ctrl Pts',(43.4735820751078,-59.267034535918,-48.6435958333333));
#265078=CARTESIAN_POINT('Ctrl Pts',(44.5079524583205,-59.8642285551076,
-48.5852625));
#265079=CARTESIAN_POINT('Ctrl Pts',(45.5423228415332,-59.267034535918,-48.5269291666667));
#265080=CARTESIAN_POINT('Ctrl Pts',(46.5766932247459,-58.6698405167284,
-48.4685958333333));
#265081=CARTESIAN_POINT('Ctrl Pts',(46.5766932247459,-57.4754524783491,
-48.4102625));
#265082=CARTESIAN_POINT('Ctrl Pts',(46.5766932247459,-56.2810644399698,
-48.3519291666667));
#265083=CARTESIAN_POINT('Ctrl Pts',(45.5423228415332,-55.6838704207802,
-48.2935958333334));
#265084=CARTESIAN_POINT('Ctrl Pts',(44.5079524583205,-55.0866764015906,
-48.2352625));
#265085=CARTESIAN_POINT('Ctrl Pts',(43.4735820751078,-55.6838704207802,
-48.1769291666667));
#265086=CARTESIAN_POINT('Ctrl Pts',(42.4392116918951,-56.2810644399698,
-48.1185958333334));
#265087=CARTESIAN_POINT('Ctrl Pts',(42.439211691895,-57.4754524783491,-48.0602625));
#265088=CARTESIAN_POINT('Ctrl Pts',(42.4392116918951,-58.6698405167284,
-48.0019291666667));
#265089=CARTESIAN_POINT('Ctrl Pts',(43.4735820751078,-59.267034535918,-47.9435958333334));
#265090=CARTESIAN_POINT('Ctrl Pts',(44.5079524583205,-59.8642285551076,
-47.8852625));
#265091=CARTESIAN_POINT('Ctrl Pts',(45.5423228415332,-59.267034535918,-47.8269291666667));
#265092=CARTESIAN_POINT('Ctrl Pts',(46.5766932247459,-58.6698405167284,
-47.7685958333333));
#265093=CARTESIAN_POINT('Ctrl Pts',(46.5766932247459,-57.4754524783491,
-47.7102625));
#265094=CARTESIAN_POINT('Ctrl Pts',(46.5766932247459,-56.2810644399698,
-47.6519291666667));
#265095=CARTESIAN_POINT('Ctrl Pts',(45.5423228415332,-55.6838704207802,
-47.5935958333333));
#265096=CARTESIAN_POINT('Ctrl Pts',(44.5079524583205,-55.0866764015906,
-47.5352625));
#265097=CARTESIAN_POINT('Ctrl Pts',(43.4735820751078,-55.6838704207802,
-47.4769291666667));
#265098=CARTESIAN_POINT('Ctrl Pts',(42.4392116918951,-56.2810644399698,
-47.4185958333333));
#265099=CARTESIAN_POINT('Ctrl Pts',(42.439211691895,-57.4754524783491,-47.3602625));
#265100=CARTESIAN_POINT('Ctrl Pts',(42.4392116918951,-58.6698405167284,
-47.3019291666666));
#265101=CARTESIAN_POINT('Ctrl Pts',(43.4735820751078,-59.267034535918,-47.2435958333334));
#265102=CARTESIAN_POINT('Ctrl Pts',(44.5079524583205,-59.8642285551076,
-47.1852625));
#265103=CARTESIAN_POINT('Ctrl Pts',(45.5423228415332,-59.267034535918,-47.1269291666667));
#265104=CARTESIAN_POINT('Ctrl Pts',(46.5766932247459,-58.6698405167284,
-47.0685958333333));
#265105=CARTESIAN_POINT('Ctrl Pts',(46.5766932247459,-57.4754524783491,
-47.0102625));
#265106=CARTESIAN_POINT('Ctrl Pts',(46.5766932247459,-56.2810644399698,
-46.9519291666667));
#265107=CARTESIAN_POINT('Ctrl Pts',(45.5423228415332,-55.6838704207802,
-46.8935958333333));
#265108=CARTESIAN_POINT('Ctrl Pts',(44.5079524583205,-55.0866764015906,
-46.8352625));
#265109=CARTESIAN_POINT('Ctrl Pts',(43.4735820751078,-55.6838704207802,
-46.7769291666667));
#265110=CARTESIAN_POINT('Ctrl Pts',(42.4392116918951,-56.2810644399698,
-46.7185958333333));
#265111=CARTESIAN_POINT('Ctrl Pts',(42.439211691895,-57.4754524783491,-46.6602625));
#265112=CARTESIAN_POINT('Ctrl Pts',(42.4392116918951,-58.6698405167284,
-46.6019291666667));
#265113=CARTESIAN_POINT('Ctrl Pts',(43.4735820751078,-59.267034535918,-46.5435958333334));
#265114=CARTESIAN_POINT('Ctrl Pts',(44.5079524583205,-59.8642285551076,
-46.4852625));
#265115=CARTESIAN_POINT('Ctrl Pts',(45.5423228415332,-59.267034535918,-46.4269291666667));
#265116=CARTESIAN_POINT('Ctrl Pts',(46.5766932247459,-58.6698405167284,
-46.3685958333333));
#265117=CARTESIAN_POINT('Ctrl Pts',(46.5766932247459,-57.4754524783491,
-46.3102625));
#265118=CARTESIAN_POINT('Ctrl Pts',(46.5766932247459,-56.2810644399698,
-46.2519291666667));
#265119=CARTESIAN_POINT('Ctrl Pts',(45.5423228415332,-55.6838704207802,
-46.1935958333333));
#265120=CARTESIAN_POINT('Ctrl Pts',(44.5079524583205,-55.0866764015906,
-46.1352625));
#265121=CARTESIAN_POINT('Ctrl Pts',(43.4735820751078,-55.6838704207802,
-46.0769291666667));
#265122=CARTESIAN_POINT('Ctrl Pts',(42.4392116918951,-56.2810644399698,
-46.0185958333334));
#265123=CARTESIAN_POINT('Ctrl Pts',(42.439211691895,-57.4754524783491,-45.9602625));
#265124=CARTESIAN_POINT('Ctrl Pts',(42.4392116918951,-58.6698405167284,
-45.9019291666667));
#265125=CARTESIAN_POINT('Ctrl Pts',(43.4735820751078,-59.267034535918,-45.8435958333333));
#265126=CARTESIAN_POINT('Ctrl Pts',(44.5079524583205,-59.8642285551076,
-45.7852625));
#265127=CARTESIAN_POINT('Ctrl Pts',(45.5423228415332,-59.267034535918,-45.7269291666667));
#265128=CARTESIAN_POINT('Ctrl Pts',(46.5766932247459,-58.6698405167284,
-45.6685958333334));
#265129=CARTESIAN_POINT('Ctrl Pts',(46.5766932247459,-57.4754524783491,
-45.6102625));
#265130=CARTESIAN_POINT('Ctrl Pts',(46.5766932247459,-56.2810644399698,
-45.5519291666667));
#265131=CARTESIAN_POINT('Ctrl Pts',(45.5423228415332,-55.6838704207802,
-45.4935958333333));
#265132=CARTESIAN_POINT('Ctrl Pts',(44.5079524583205,-55.0866764015906,
-45.4352625));
#265133=CARTESIAN_POINT('Ctrl Pts',(43.4735820751078,-55.6838704207802,
-45.3769291666667));
#265134=CARTESIAN_POINT('Ctrl Pts',(42.4392116918951,-56.2810644399698,
-45.3185958333333));
#265135=CARTESIAN_POINT('Ctrl Pts',(42.439211691895,-57.4754524783491,-45.2602625));
#265136=CARTESIAN_POINT('Ctrl Pts',(42.4392116918951,-58.6698405167284,
-45.2019291666667));
#265137=CARTESIAN_POINT('Ctrl Pts',(43.4735820751078,-59.267034535918,-45.1435958333334));
#265138=CARTESIAN_POINT('Ctrl Pts',(44.5079524583205,-59.8642285551076,
-45.0852625));
#265139=CARTESIAN_POINT('Ctrl Pts',(45.5423228415332,-59.267034535918,-45.0269291666667));
#265140=CARTESIAN_POINT('Ctrl Pts',(46.5766932247459,-58.6698405167284,
-44.9685958333334));
#265141=CARTESIAN_POINT('Ctrl Pts',(46.5766932247459,-57.4754524783491,
-44.9102625));
#265142=CARTESIAN_POINT('Ctrl Pts',(46.5766932247459,-56.2810644399698,
-44.8519291666667));
#265143=CARTESIAN_POINT('Ctrl Pts',(45.5423228415332,-55.6838704207802,
-44.7935958333333));
#265144=CARTESIAN_POINT('Ctrl Pts',(44.5079524583205,-55.0866764015906,
-44.7352625));
#265145=CARTESIAN_POINT('Ctrl Pts',(43.4735820751078,-55.6838704207802,
-44.6769291666667));
#265146=CARTESIAN_POINT('Ctrl Pts',(42.4392116918951,-56.2810644399698,
-44.6185958333334));
#265147=CARTESIAN_POINT('Ctrl Pts',(42.439211691895,-57.4754524783491,-44.5602625));
#265148=CARTESIAN_POINT('Ctrl Pts',(42.4392116918951,-58.6698405167284,
-44.5019291666667));
#265149=CARTESIAN_POINT('Ctrl Pts',(43.4735820751078,-59.267034535918,-44.4435958333333));
#265150=CARTESIAN_POINT('Ctrl Pts',(44.5079524583205,-59.8642285551076,
-44.3852625));
#265151=CARTESIAN_POINT('Ctrl Pts',(45.5423228415332,-59.267034535918,-44.3269291666667));
#265152=CARTESIAN_POINT('Ctrl Pts',(46.5766932247459,-58.6698405167284,
-44.2685958333334));
#265153=CARTESIAN_POINT('Ctrl Pts',(46.5766932247459,-57.4754524783491,
-44.2102625));
#265154=CARTESIAN_POINT('Ctrl Pts',(46.5766932247459,-56.2810644399698,
-44.1519291666667));
#265155=CARTESIAN_POINT('Ctrl Pts',(45.5423228415332,-55.6838704207802,
-44.0935958333334));
#265156=CARTESIAN_POINT('Ctrl Pts',(44.5079524583205,-55.0866764015906,
-44.0352625));
#265157=CARTESIAN_POINT('Ctrl Pts',(43.4735820751078,-55.6838704207802,
-43.9769291666667));
#265158=CARTESIAN_POINT('Ctrl Pts',(42.4392116918951,-56.2810644399698,
-43.9185958333334));
#265159=CARTESIAN_POINT('Ctrl Pts',(42.439211691895,-57.4754524783491,-43.8602625));
#265160=CARTESIAN_POINT('Ctrl Pts',(42.4392116918951,-58.6698405167284,
-43.8019291666667));
#265161=CARTESIAN_POINT('Ctrl Pts',(43.4735820751078,-59.267034535918,-43.7435958333334));
#265162=CARTESIAN_POINT('Ctrl Pts',(44.5079524583205,-59.8642285551076,
-43.6852625));
#265163=CARTESIAN_POINT('Ctrl Pts',(45.5423228415332,-59.267034535918,-43.6269291666667));
#265164=CARTESIAN_POINT('Ctrl Pts',(46.5766932247459,-58.6698405167284,
-43.5685958333334));
#265165=CARTESIAN_POINT('Ctrl Pts',(46.5766932247459,-57.4754524783491,
-43.5102625));
#265166=CARTESIAN_POINT('Ctrl Pts',(46.5766932247459,-56.2810644399698,
-43.4519291666667));
#265167=CARTESIAN_POINT('Ctrl Pts',(45.5423228415332,-55.6838704207802,
-43.3935958333334));
#265168=CARTESIAN_POINT('Ctrl Pts',(44.5079524583205,-55.0866764015906,
-43.3352625));
#265169=CARTESIAN_POINT('Ctrl Pts',(43.4735820751078,-55.6838704207802,
-43.2769291666667));
#265170=CARTESIAN_POINT('Ctrl Pts',(42.4392116918951,-56.2810644399698,
-43.2185958333334));
#265171=CARTESIAN_POINT('Ctrl Pts',(42.439211691895,-57.4754524783491,-43.1602625));
#265172=CARTESIAN_POINT('Ctrl Pts',(42.4392116918951,-58.6698405167284,
-43.1019291666667));
#265173=CARTESIAN_POINT('Ctrl Pts',(43.4735820751078,-59.267034535918,-43.0435958333334));
#265174=CARTESIAN_POINT('Ctrl Pts',(44.5079524583205,-59.8642285551076,
-42.9852625));
#265175=CARTESIAN_POINT('Ctrl Pts',(45.5423228415332,-59.267034535918,-42.9269291666667));
#265176=CARTESIAN_POINT('Ctrl Pts',(46.5766932247459,-58.6698405167284,
-42.8685958333333));
#265177=CARTESIAN_POINT('Ctrl Pts',(46.5766932247459,-57.4754524783491,
-42.8102625));
#265178=CARTESIAN_POINT('Ctrl Pts',(46.5766932247459,-56.2810644399698,
-42.7519291666667));
#265179=CARTESIAN_POINT('Ctrl Pts',(45.5423228415332,-55.6838704207802,
-42.6935958333333));
#265180=CARTESIAN_POINT('Ctrl Pts',(44.5079524583205,-55.0866764015906,
-42.6352625));
#265181=CARTESIAN_POINT('Ctrl Pts',(43.4735820751078,-55.6838704207802,
-42.5769291666667));
#265182=CARTESIAN_POINT('Ctrl Pts',(42.4392116918951,-56.2810644399698,
-42.5185958333333));
#265183=CARTESIAN_POINT('Ctrl Pts',(42.439211691895,-57.4754524783491,-42.4602625));
#265184=CARTESIAN_POINT('Ctrl Pts',(42.4392116918951,-58.6698405167284,
-42.4019291666666));
#265185=CARTESIAN_POINT('Ctrl Pts',(43.4735820751078,-59.267034535918,-42.3435958333334));
#265186=CARTESIAN_POINT('Ctrl Pts',(44.5079524583205,-59.8642285551076,
-42.2852625));
#265187=CARTESIAN_POINT('Ctrl Pts',(45.5423228415332,-59.267034535918,-42.2269291666667));
#265188=CARTESIAN_POINT('Ctrl Pts',(46.5766932247459,-58.6698405167284,
-42.1685958333333));
#265189=CARTESIAN_POINT('Ctrl Pts',(46.5766932247459,-57.4754524783491,
-42.1102625));
#265190=CARTESIAN_POINT('Ctrl Pts',(46.5766932247459,-56.2810644399698,
-42.0519291666667));
#265191=CARTESIAN_POINT('Ctrl Pts',(45.5423228415332,-55.6838704207802,
-41.9935958333334));
#265192=CARTESIAN_POINT('Ctrl Pts',(44.5079524583205,-55.0866764015906,
-41.9352625));
#265193=CARTESIAN_POINT('Ctrl Pts',(43.4735820751078,-55.6838704207802,
-41.8769291666667));
#265194=CARTESIAN_POINT('Ctrl Pts',(42.4392116918951,-56.2810644399698,
-41.8185958333333));
#265195=CARTESIAN_POINT('Ctrl Pts',(42.439211691895,-57.4754524783491,-41.7602625));
#265196=CARTESIAN_POINT('Ctrl Pts',(42.4392116918951,-58.6698405167284,
-41.7019291666667));
#265197=CARTESIAN_POINT('Ctrl Pts',(43.4735820751078,-59.267034535918,-41.6435958333334));
#265198=CARTESIAN_POINT('Ctrl Pts',(44.5079524583205,-59.8642285551076,
-41.5852625));
#265199=CARTESIAN_POINT('Ctrl Pts',(45.5423228415332,-59.267034535918,-41.5269291666667));
#265200=CARTESIAN_POINT('Ctrl Pts',(46.5766932247459,-58.6698405167284,
-41.4685958333333));
#265201=CARTESIAN_POINT('Ctrl Pts',(46.5766932247459,-57.4754524783491,
-41.4102625));
#265202=CARTESIAN_POINT('Ctrl Pts',(46.5766932247459,-56.2810644399698,
-41.3519291666666));
#265203=CARTESIAN_POINT('Ctrl Pts',(45.5423228415332,-55.6838704207802,
-41.2935958333334));
#265204=CARTESIAN_POINT('Ctrl Pts',(44.5079524583205,-55.0866764015906,
-41.2352625));
#265205=CARTESIAN_POINT('Ctrl Pts',(43.4735820751078,-55.6838704207802,
-41.1769291666667));
#265206=CARTESIAN_POINT('Ctrl Pts',(42.4392116918951,-56.2810644399698,
-41.1185958333333));
#265207=CARTESIAN_POINT('Ctrl Pts',(42.439211691895,-57.4754524783491,-41.0602625));
#265208=CARTESIAN_POINT('Ctrl Pts',(42.4392116918951,-58.6698405167284,
-41.0019291666666));
#265209=CARTESIAN_POINT('Ctrl Pts',(43.4735820751078,-59.267034535918,-40.9435958333334));
#265210=CARTESIAN_POINT('Ctrl Pts',(44.5079524583205,-59.8642285551076,
-40.8852625));
#265211=CARTESIAN_POINT('Ctrl Pts',(45.5423228415332,-59.267034535918,-40.8269291666667));
#265212=CARTESIAN_POINT('Ctrl Pts',(46.5766932247459,-58.6698405167284,
-40.7685958333333));
#265213=CARTESIAN_POINT('Ctrl Pts',(46.5766932247459,-57.4754524783491,
-40.7102625));
#265214=CARTESIAN_POINT('Ctrl Pts',(46.5766932247459,-56.2810644399698,
-40.6519291666667));
#265215=CARTESIAN_POINT('Ctrl Pts',(45.5423228415332,-55.6838704207802,
-40.5935958333334));
#265216=CARTESIAN_POINT('Ctrl Pts',(44.5079524583205,-55.0866764015906,
-40.5352625));
#265217=CARTESIAN_POINT('Ctrl Pts',(43.4735820751078,-55.6838704207802,
-40.4769291666667));
#265218=CARTESIAN_POINT('Ctrl Pts',(42.4392116918951,-56.2810644399698,
-40.4185958333333));
#265219=CARTESIAN_POINT('Ctrl Pts',(42.439211691895,-57.4754524783491,-40.3602625));
#265220=CARTESIAN_POINT('Ctrl Pts',(42.4392116918951,-58.6698405167284,
-40.3019291666667));
#265221=CARTESIAN_POINT('Ctrl Pts',(43.4735820751078,-59.267034535918,-40.2435958333334));
#265222=CARTESIAN_POINT('Ctrl Pts',(44.5079524583205,-59.8642285551076,
-40.1852625));
#265223=CARTESIAN_POINT('Ctrl Pts',(45.5423228415332,-59.267034535918,-40.1269291666666));
#265224=CARTESIAN_POINT('Ctrl Pts',(46.5766932247459,-58.6698405167284,
-40.0685958333333));
#265225=CARTESIAN_POINT('Ctrl Pts',(46.5766932247459,-57.4754524783491,
-40.0102625));
#265226=CARTESIAN_POINT('Ctrl Pts',(46.5766932247459,-56.2810644399698,
-39.9519291666667));
#265227=CARTESIAN_POINT('Ctrl Pts',(45.5423228415332,-55.6838704207802,
-39.8935958333334));
#265228=CARTESIAN_POINT('Ctrl Pts',(44.5079524583205,-55.0866764015906,
-39.8352625));
#265229=CARTESIAN_POINT('Ctrl Pts',(43.4735820751078,-55.6838704207802,
-39.7769291666667));
#265230=CARTESIAN_POINT('Ctrl Pts',(42.4392116918951,-56.2810644399698,
-39.7185958333334));
#265231=CARTESIAN_POINT('Ctrl Pts',(42.439211691895,-57.4754524783491,-39.6602625));
#265232=CARTESIAN_POINT('Ctrl Pts',(42.4392116918951,-58.6698405167284,
-39.6019291666667));
#265233=CARTESIAN_POINT('Ctrl Pts',(43.4735820751078,-59.267034535918,-39.5435958333333));
#265234=CARTESIAN_POINT('Ctrl Pts',(44.5079524583205,-59.8642285551076,
-39.4852625));
#265235=CARTESIAN_POINT('Ctrl Pts',(45.5423228415332,-59.267034535918,-39.4269291666667));
#265236=CARTESIAN_POINT('Ctrl Pts',(46.5766932247459,-58.6698405167284,
-39.3685958333334));
#265237=CARTESIAN_POINT('Ctrl Pts',(46.5766932247459,-57.4754524783491,
-39.3102625));
#265238=CARTESIAN_POINT('Ctrl Pts',(46.5766932247459,-56.2810644399698,
-39.2519291666667));
#265239=CARTESIAN_POINT('Ctrl Pts',(45.5423228415332,-55.6838704207802,
-39.1935958333334));
#265240=CARTESIAN_POINT('Ctrl Pts',(44.5079524583205,-55.0866764015906,
-39.1352625));
#265241=CARTESIAN_POINT('Ctrl Pts',(43.4735820751078,-55.6838704207802,
-39.0769291666667));
#265242=CARTESIAN_POINT('Ctrl Pts',(42.4392116918951,-56.2810644399698,
-39.0185958333334));
#265243=CARTESIAN_POINT('Ctrl Pts',(42.439211691895,-57.4754524783491,-38.9602625));
#265244=CARTESIAN_POINT('Ctrl Pts',(42.4392116918951,-58.6698405167284,
-38.9019291666667));
#265245=CARTESIAN_POINT('Ctrl Pts',(43.4735820751078,-59.267034535918,-38.8435958333333));
#265246=CARTESIAN_POINT('Ctrl Pts',(44.5079524583205,-59.8642285551076,
-38.7852625));
#265247=CARTESIAN_POINT('Ctrl Pts',(45.5423228415332,-59.267034535918,-38.7269291666667));
#265248=CARTESIAN_POINT('Ctrl Pts',(46.5766932247459,-58.6698405167284,
-38.6685958333334));
#265249=CARTESIAN_POINT('Ctrl Pts',(46.5766932247459,-57.4754524783491,
-38.6102625));
#265250=CARTESIAN_POINT('Ctrl Pts',(46.5766932247459,-56.2810644399698,
-38.5519291666667));
#265251=CARTESIAN_POINT('Ctrl Pts',(45.5423228415332,-55.6838704207802,
-38.4935958333334));
#265252=CARTESIAN_POINT('Ctrl Pts',(44.5079524583205,-55.0866764015906,
-38.4352625));
#265253=CARTESIAN_POINT('Ctrl Pts',(43.4735820751078,-55.6838704207802,
-38.3769291666667));
#265254=CARTESIAN_POINT('Ctrl Pts',(42.4392116918951,-56.2810644399698,
-38.3185958333333));
#265255=CARTESIAN_POINT('Ctrl Pts',(42.439211691895,-57.4754524783491,-38.2602625));
#265256=CARTESIAN_POINT('Ctrl Pts',(42.4392116918951,-58.6698405167284,
-38.2019291666667));
#265257=CARTESIAN_POINT('Ctrl Pts',(43.4735820751078,-59.267034535918,-38.1435958333334));
#265258=CARTESIAN_POINT('Ctrl Pts',(44.5079524583205,-59.8642285551076,
-38.0852625));
#265259=CARTESIAN_POINT('Ctrl Pts',(45.5423228415332,-59.267034535918,-38.0269291666667));
#265260=CARTESIAN_POINT('Ctrl Pts',(46.5766932247459,-58.6698405167284,
-37.9685958333333));
#265261=CARTESIAN_POINT('Ctrl Pts',(46.5766932247459,-57.4754524783491,
-37.9102625));
#265262=CARTESIAN_POINT('Ctrl Pts',(46.5766932247459,-56.2810644399698,
-37.8519291666667));
#265263=CARTESIAN_POINT('Ctrl Pts',(45.5423228415332,-55.6838704207802,
-37.7935958333334));
#265264=CARTESIAN_POINT('Ctrl Pts',(44.5079524583205,-55.0866764015906,
-37.7352625));
#265265=CARTESIAN_POINT('Ctrl Pts',(43.4735820751078,-55.6838704207802,
-37.6769291666667));
#265266=CARTESIAN_POINT('Ctrl Pts',(42.4392116918951,-56.2810644399698,
-37.6185958333333));
#265267=CARTESIAN_POINT('Ctrl Pts',(42.439211691895,-57.4754524783491,-37.5602625));
#265268=CARTESIAN_POINT('Ctrl Pts',(42.4392116918951,-58.6698405167284,
-37.5019291666667));
#265269=CARTESIAN_POINT('Ctrl Pts',(43.4735820751078,-59.267034535918,-37.4435958333333));
#265270=CARTESIAN_POINT('Ctrl Pts',(44.5079524583205,-59.8642285551076,
-37.3852625));
#265271=CARTESIAN_POINT('Ctrl Pts',(45.5423228415332,-59.267034535918,-37.3269291666667));
#265272=CARTESIAN_POINT('Ctrl Pts',(46.5766932247459,-58.6698405167284,
-37.2685958333333));
#265273=CARTESIAN_POINT('Ctrl Pts',(46.5766932247459,-57.4754524783491,
-37.2102625));
#265274=CARTESIAN_POINT('Ctrl Pts',(46.5766932247459,-56.2810644399698,
-37.1519291666667));
#265275=CARTESIAN_POINT('Ctrl Pts',(45.5423228415332,-55.6838704207802,
-37.0935958333333));
#265276=CARTESIAN_POINT('Ctrl Pts',(44.5079524583205,-55.0866764015906,
-37.0352625));
#265277=CARTESIAN_POINT('Ctrl Pts',(43.4735820751078,-55.6838704207802,
-36.9769291666667));
#265278=CARTESIAN_POINT('Ctrl Pts',(42.4392116918951,-56.2810644399698,
-36.9185958333333));
#265279=CARTESIAN_POINT('Ctrl Pts',(42.439211691895,-57.4754524783491,-36.8602625));
#265280=CARTESIAN_POINT('Ctrl Pts',(42.4392116918951,-58.6698405167284,
-36.8019291666666));
#265281=CARTESIAN_POINT('Ctrl Pts',(43.4735820751078,-59.267034535918,-36.7435958333334));
#265282=CARTESIAN_POINT('Ctrl Pts',(44.5079524583205,-59.8642285551076,
-36.6852625));
#265283=CARTESIAN_POINT('Ctrl Pts',(45.5423228415332,-59.267034535918,-36.6269291666667));
#265284=CARTESIAN_POINT('Ctrl Pts',(45.6766051604217,-59.1895066029603,
-36.6193563132714));
#265285=CARTESIAN_POINT('Ctrl Pts',(45.7978303778615,-59.0928279175564,
-36.611216324118));
#265286=CARTESIAN_POINT('Ctrl Pts',(46.1766975979086,-57.4754524783491,
-52.8412000828291));
#265287=CARTESIAN_POINT('Ctrl Pts',(46.1766975979086,-56.512002022799,-52.7828667494958));
#265288=CARTESIAN_POINT('Ctrl Pts',(45.3423250281146,-56.0302767950239,
-52.7245334161625));
#265289=CARTESIAN_POINT('Ctrl Pts',(44.5079524583205,-55.5485515672488,
-52.6662000828291));
#265290=CARTESIAN_POINT('Ctrl Pts',(43.6735798885264,-56.0302767950239,
-52.6078667494958));
#265291=CARTESIAN_POINT('Ctrl Pts',(42.8392073187323,-56.5120020227989,
-52.5495334161624));
#265292=CARTESIAN_POINT('Ctrl Pts',(42.8392073187323,-57.4754524783491,
-52.4912000828291));
#265293=CARTESIAN_POINT('Ctrl Pts',(42.8392073187323,-58.4389029338992,
-52.4328667494959));
#265294=CARTESIAN_POINT('Ctrl Pts',(43.6735798885264,-58.9206281616743,
-52.3745334161625));
#265295=CARTESIAN_POINT('Ctrl Pts',(44.5079524583205,-59.4023533894493,
-52.3162000828292));
#265296=CARTESIAN_POINT('Ctrl Pts',(45.3423250281146,-58.9206281616743,
-52.2578667494958));
#265297=CARTESIAN_POINT('Ctrl Pts',(46.1766975979086,-58.4389029338992,
-52.1995334161625));
#265298=CARTESIAN_POINT('Ctrl Pts',(46.1766975979086,-57.4754524783491,
-52.1412000828291));
#265299=CARTESIAN_POINT('Ctrl Pts',(46.1766975979086,-56.512002022799,-52.0828667494958));
#265300=CARTESIAN_POINT('Ctrl Pts',(45.3423250281146,-56.0302767950239,
-52.0245334161624));
#265301=CARTESIAN_POINT('Ctrl Pts',(44.5079524583205,-55.5485515672488,
-51.9662000828291));
#265302=CARTESIAN_POINT('Ctrl Pts',(43.6735798885264,-56.0302767950239,
-51.9078667494958));
#265303=CARTESIAN_POINT('Ctrl Pts',(42.8392073187323,-56.5120020227989,
-51.8495334161625));
#265304=CARTESIAN_POINT('Ctrl Pts',(42.8392073187323,-57.4754524783491,
-51.7912000828291));
#265305=CARTESIAN_POINT('Ctrl Pts',(42.8392073187323,-58.4389029338992,
-51.7328667494958));
#265306=CARTESIAN_POINT('Ctrl Pts',(43.6735798885264,-58.9206281616743,
-51.6745334161625));
#265307=CARTESIAN_POINT('Ctrl Pts',(44.5079524583205,-59.4023533894493,
-51.6162000828291));
#265308=CARTESIAN_POINT('Ctrl Pts',(45.3423250281146,-58.9206281616743,
-51.5578667494958));
#265309=CARTESIAN_POINT('Ctrl Pts',(46.1766975979086,-58.4389029338992,
-51.4995334161625));
#265310=CARTESIAN_POINT('Ctrl Pts',(46.1766975979086,-57.4754524783491,
-51.4412000828291));
#265311=CARTESIAN_POINT('Ctrl Pts',(46.1766975979086,-56.512002022799,-51.3828667494958));
#265312=CARTESIAN_POINT('Ctrl Pts',(45.3423250281146,-56.0302767950239,
-51.3245334161625));
#265313=CARTESIAN_POINT('Ctrl Pts',(44.5079524583205,-55.5485515672488,
-51.2662000828291));
#265314=CARTESIAN_POINT('Ctrl Pts',(43.6735798885264,-56.0302767950239,
-51.2078667494958));
#265315=CARTESIAN_POINT('Ctrl Pts',(42.8392073187323,-56.5120020227989,
-51.1495334161625));
#265316=CARTESIAN_POINT('Ctrl Pts',(42.8392073187323,-57.4754524783491,
-51.0912000828291));
#265317=CARTESIAN_POINT('Ctrl Pts',(42.8392073187323,-58.4389029338992,
-51.0328667494958));
#265318=CARTESIAN_POINT('Ctrl Pts',(43.6735798885264,-58.9206281616743,
-50.9745334161624));
#265319=CARTESIAN_POINT('Ctrl Pts',(44.5079524583205,-59.4023533894493,
-50.9162000828291));
#265320=CARTESIAN_POINT('Ctrl Pts',(45.3423250281146,-58.9206281616743,
-50.8578667494958));
#265321=CARTESIAN_POINT('Ctrl Pts',(46.1766975979086,-58.4389029338992,
-50.7995334161625));
#265322=CARTESIAN_POINT('Ctrl Pts',(46.1766975979086,-57.4754524783491,
-50.7412000828291));
#265323=CARTESIAN_POINT('Ctrl Pts',(46.1766975979086,-56.512002022799,-50.6828667494958));
#265324=CARTESIAN_POINT('Ctrl Pts',(45.3423250281146,-56.0302767950239,
-50.6245334161624));
#265325=CARTESIAN_POINT('Ctrl Pts',(44.5079524583205,-55.5485515672488,
-50.5662000828291));
#265326=CARTESIAN_POINT('Ctrl Pts',(43.6735798885264,-56.0302767950239,
-50.5078667494958));
#265327=CARTESIAN_POINT('Ctrl Pts',(42.8392073187323,-56.5120020227989,
-50.4495334161625));
#265328=CARTESIAN_POINT('Ctrl Pts',(42.8392073187323,-57.4754524783491,
-50.3912000828291));
#265329=CARTESIAN_POINT('Ctrl Pts',(42.8392073187323,-58.4389029338992,
-50.3328667494958));
#265330=CARTESIAN_POINT('Ctrl Pts',(43.6735798885264,-58.9206281616743,
-50.2745334161625));
#265331=CARTESIAN_POINT('Ctrl Pts',(44.5079524583205,-59.4023533894493,
-50.2162000828292));
#265332=CARTESIAN_POINT('Ctrl Pts',(45.3423250281146,-58.9206281616743,
-50.1578667494958));
#265333=CARTESIAN_POINT('Ctrl Pts',(46.1766975979086,-58.4389029338992,
-50.0995334161625));
#265334=CARTESIAN_POINT('Ctrl Pts',(46.1766975979086,-57.4754524783491,
-50.0412000828291));
#265335=CARTESIAN_POINT('Ctrl Pts',(46.1766975979086,-56.512002022799,-49.9828667494958));
#265336=CARTESIAN_POINT('Ctrl Pts',(45.3423250281146,-56.0302767950239,
-49.9245334161625));
#265337=CARTESIAN_POINT('Ctrl Pts',(44.5079524583205,-55.5485515672488,
-49.8662000828292));
#265338=CARTESIAN_POINT('Ctrl Pts',(43.6735798885264,-56.0302767950239,
-49.8078667494958));
#265339=CARTESIAN_POINT('Ctrl Pts',(42.8392073187323,-56.5120020227989,
-49.7495334161624));
#265340=CARTESIAN_POINT('Ctrl Pts',(42.8392073187323,-57.4754524783491,
-49.6912000828291));
#265341=CARTESIAN_POINT('Ctrl Pts',(42.8392073187323,-58.4389029338992,
-49.6328667494958));
#265342=CARTESIAN_POINT('Ctrl Pts',(43.6735798885264,-58.9206281616743,
-49.5745334161625));
#265343=CARTESIAN_POINT('Ctrl Pts',(44.5079524583205,-59.4023533894493,
-49.5162000828292));
#265344=CARTESIAN_POINT('Ctrl Pts',(45.3423250281146,-58.9206281616743,
-49.4578667494958));
#265345=CARTESIAN_POINT('Ctrl Pts',(46.1766975979086,-58.4389029338992,
-49.3995334161625));
#265346=CARTESIAN_POINT('Ctrl Pts',(46.1766975979086,-57.4754524783491,
-49.3412000828291));
#265347=CARTESIAN_POINT('Ctrl Pts',(46.1766975979086,-56.512002022799,-49.2828667494958));
#265348=CARTESIAN_POINT('Ctrl Pts',(45.3423250281146,-56.0302767950239,
-49.2245334161625));
#265349=CARTESIAN_POINT('Ctrl Pts',(44.5079524583205,-55.5485515672488,
-49.1662000828291));
#265350=CARTESIAN_POINT('Ctrl Pts',(43.6735798885264,-56.0302767950239,
-49.1078667494958));
#265351=CARTESIAN_POINT('Ctrl Pts',(42.8392073187323,-56.5120020227989,
-49.0495334161625));
#265352=CARTESIAN_POINT('Ctrl Pts',(42.8392073187323,-57.4754524783491,
-48.9912000828291));
#265353=CARTESIAN_POINT('Ctrl Pts',(42.8392073187323,-58.4389029338992,
-48.9328667494958));
#265354=CARTESIAN_POINT('Ctrl Pts',(43.6735798885264,-58.9206281616743,
-48.8745334161625));
#265355=CARTESIAN_POINT('Ctrl Pts',(44.5079524583205,-59.4023533894493,
-48.8162000828292));
#265356=CARTESIAN_POINT('Ctrl Pts',(45.3423250281146,-58.9206281616743,
-48.7578667494958));
#265357=CARTESIAN_POINT('Ctrl Pts',(46.1766975979086,-58.4389029338992,
-48.6995334161625));
#265358=CARTESIAN_POINT('Ctrl Pts',(46.1766975979086,-57.4754524783491,
-48.6412000828291));
#265359=CARTESIAN_POINT('Ctrl Pts',(46.1766975979086,-56.512002022799,-48.5828667494958));
#265360=CARTESIAN_POINT('Ctrl Pts',(45.3423250281146,-56.0302767950239,
-48.5245334161625));
#265361=CARTESIAN_POINT('Ctrl Pts',(44.5079524583205,-55.5485515672488,
-48.4662000828292));
#265362=CARTESIAN_POINT('Ctrl Pts',(43.6735798885264,-56.0302767950239,
-48.4078667494958));
#265363=CARTESIAN_POINT('Ctrl Pts',(42.8392073187323,-56.5120020227989,
-48.3495334161625));
#265364=CARTESIAN_POINT('Ctrl Pts',(42.8392073187323,-57.4754524783491,
-48.2912000828291));
#265365=CARTESIAN_POINT('Ctrl Pts',(42.8392073187323,-58.4389029338992,
-48.2328667494958));
#265366=CARTESIAN_POINT('Ctrl Pts',(43.6735798885264,-58.9206281616743,
-48.1745334161625));
#265367=CARTESIAN_POINT('Ctrl Pts',(44.5079524583205,-59.4023533894493,
-48.1162000828291));
#265368=CARTESIAN_POINT('Ctrl Pts',(45.3423250281146,-58.9206281616743,
-48.0578667494958));
#265369=CARTESIAN_POINT('Ctrl Pts',(46.1766975979086,-58.4389029338992,
-47.9995334161625));
#265370=CARTESIAN_POINT('Ctrl Pts',(46.1766975979086,-57.4754524783491,
-47.9412000828291));
#265371=CARTESIAN_POINT('Ctrl Pts',(46.1766975979086,-56.512002022799,-47.8828667494958));
#265372=CARTESIAN_POINT('Ctrl Pts',(45.3423250281146,-56.0302767950239,
-47.8245334161624));
#265373=CARTESIAN_POINT('Ctrl Pts',(44.5079524583205,-55.5485515672488,
-47.7662000828292));
#265374=CARTESIAN_POINT('Ctrl Pts',(43.6735798885264,-56.0302767950239,
-47.7078667494958));
#265375=CARTESIAN_POINT('Ctrl Pts',(42.8392073187323,-56.5120020227989,
-47.6495334161625));
#265376=CARTESIAN_POINT('Ctrl Pts',(42.8392073187323,-57.4754524783491,
-47.5912000828291));
#265377=CARTESIAN_POINT('Ctrl Pts',(42.8392073187323,-58.4389029338992,
-47.5328667494958));
#265378=CARTESIAN_POINT('Ctrl Pts',(43.6735798885264,-58.9206281616743,
-47.4745334161625));
#265379=CARTESIAN_POINT('Ctrl Pts',(44.5079524583205,-59.4023533894493,
-47.4162000828291));
#265380=CARTESIAN_POINT('Ctrl Pts',(45.3423250281146,-58.9206281616743,
-47.3578667494958));
#265381=CARTESIAN_POINT('Ctrl Pts',(46.1766975979086,-58.4389029338992,
-47.2995334161625));
#265382=CARTESIAN_POINT('Ctrl Pts',(46.1766975979086,-57.4754524783491,
-47.2412000828291));
#265383=CARTESIAN_POINT('Ctrl Pts',(46.1766975979086,-56.512002022799,-47.1828667494958));
#265384=CARTESIAN_POINT('Ctrl Pts',(45.3423250281146,-56.0302767950239,
-47.1245334161624));
#265385=CARTESIAN_POINT('Ctrl Pts',(44.5079524583205,-55.5485515672488,
-47.0662000828291));
#265386=CARTESIAN_POINT('Ctrl Pts',(43.6735798885264,-56.0302767950239,
-47.0078667494958));
#265387=CARTESIAN_POINT('Ctrl Pts',(42.8392073187323,-56.5120020227989,
-46.9495334161625));
#265388=CARTESIAN_POINT('Ctrl Pts',(42.8392073187323,-57.4754524783491,
-46.8912000828291));
#265389=CARTESIAN_POINT('Ctrl Pts',(42.8392073187323,-58.4389029338992,
-46.8328667494958));
#265390=CARTESIAN_POINT('Ctrl Pts',(43.6735798885264,-58.9206281616743,
-46.7745334161625));
#265391=CARTESIAN_POINT('Ctrl Pts',(44.5079524583205,-59.4023533894493,
-46.7162000828291));
#265392=CARTESIAN_POINT('Ctrl Pts',(45.3423250281146,-58.9206281616743,
-46.6578667494958));
#265393=CARTESIAN_POINT('Ctrl Pts',(46.1766975979086,-58.4389029338992,
-46.5995334161625));
#265394=CARTESIAN_POINT('Ctrl Pts',(46.1766975979086,-57.4754524783491,
-46.5412000828291));
#265395=CARTESIAN_POINT('Ctrl Pts',(46.1766975979086,-56.512002022799,-46.4828667494958));
#265396=CARTESIAN_POINT('Ctrl Pts',(45.3423250281146,-56.0302767950239,
-46.4245334161625));
#265397=CARTESIAN_POINT('Ctrl Pts',(44.5079524583205,-55.5485515672488,
-46.3662000828291));
#265398=CARTESIAN_POINT('Ctrl Pts',(43.6735798885264,-56.0302767950239,
-46.3078667494958));
#265399=CARTESIAN_POINT('Ctrl Pts',(42.8392073187323,-56.5120020227989,
-46.2495334161625));
#265400=CARTESIAN_POINT('Ctrl Pts',(42.8392073187323,-57.4754524783491,
-46.1912000828291));
#265401=CARTESIAN_POINT('Ctrl Pts',(42.8392073187323,-58.4389029338992,
-46.1328667494958));
#265402=CARTESIAN_POINT('Ctrl Pts',(43.6735798885264,-58.9206281616743,
-46.0745334161625));
#265403=CARTESIAN_POINT('Ctrl Pts',(44.5079524583205,-59.4023533894493,
-46.0162000828291));
#265404=CARTESIAN_POINT('Ctrl Pts',(45.3423250281146,-58.9206281616743,
-45.9578667494958));
#265405=CARTESIAN_POINT('Ctrl Pts',(46.1766975979086,-58.4389029338992,
-45.8995334161624));
#265406=CARTESIAN_POINT('Ctrl Pts',(46.1766975979086,-57.4754524783491,
-45.8412000828291));
#265407=CARTESIAN_POINT('Ctrl Pts',(46.1766975979086,-56.512002022799,-45.7828667494958));
#265408=CARTESIAN_POINT('Ctrl Pts',(45.3423250281146,-56.0302767950239,
-45.7245334161624));
#265409=CARTESIAN_POINT('Ctrl Pts',(44.5079524583205,-55.5485515672488,
-45.6662000828291));
#265410=CARTESIAN_POINT('Ctrl Pts',(43.6735798885264,-56.0302767950239,
-45.6078667494958));
#265411=CARTESIAN_POINT('Ctrl Pts',(42.8392073187323,-56.5120020227989,
-45.5495334161625));
#265412=CARTESIAN_POINT('Ctrl Pts',(42.8392073187323,-57.4754524783491,
-45.4912000828291));
#265413=CARTESIAN_POINT('Ctrl Pts',(42.8392073187323,-58.4389029338992,
-45.4328667494958));
#265414=CARTESIAN_POINT('Ctrl Pts',(43.6735798885264,-58.9206281616743,
-45.3745334161625));
#265415=CARTESIAN_POINT('Ctrl Pts',(44.5079524583205,-59.4023533894493,
-45.3162000828292));
#265416=CARTESIAN_POINT('Ctrl Pts',(45.3423250281146,-58.9206281616743,
-45.2578667494958));
#265417=CARTESIAN_POINT('Ctrl Pts',(46.1766975979086,-58.4389029338992,
-45.1995334161625));
#265418=CARTESIAN_POINT('Ctrl Pts',(46.1766975979086,-57.4754524783491,
-45.1412000828291));
#265419=CARTESIAN_POINT('Ctrl Pts',(46.1766975979086,-56.512002022799,-45.0828667494958));
#265420=CARTESIAN_POINT('Ctrl Pts',(45.3423250281146,-56.0302767950239,
-45.0245334161625));
#265421=CARTESIAN_POINT('Ctrl Pts',(44.5079524583205,-55.5485515672488,
-44.9662000828292));
#265422=CARTESIAN_POINT('Ctrl Pts',(43.6735798885264,-56.0302767950239,
-44.9078667494958));
#265423=CARTESIAN_POINT('Ctrl Pts',(42.8392073187323,-56.5120020227989,
-44.8495334161625));
#265424=CARTESIAN_POINT('Ctrl Pts',(42.8392073187323,-57.4754524783491,
-44.7912000828291));
#265425=CARTESIAN_POINT('Ctrl Pts',(42.8392073187323,-58.4389029338992,
-44.7328667494958));
#265426=CARTESIAN_POINT('Ctrl Pts',(43.6735798885264,-58.9206281616743,
-44.6745334161625));
#265427=CARTESIAN_POINT('Ctrl Pts',(44.5079524583205,-59.4023533894493,
-44.6162000828292));
#265428=CARTESIAN_POINT('Ctrl Pts',(45.3423250281146,-58.9206281616743,
-44.5578667494959));
#265429=CARTESIAN_POINT('Ctrl Pts',(46.1766975979086,-58.4389029338992,
-44.4995334161625));
#265430=CARTESIAN_POINT('Ctrl Pts',(46.1766975979086,-57.4754524783491,
-44.4412000828291));
#265431=CARTESIAN_POINT('Ctrl Pts',(46.1766975979086,-56.512002022799,-44.3828667494958));
#265432=CARTESIAN_POINT('Ctrl Pts',(45.3423250281146,-56.0302767950239,
-44.3245334161625));
#265433=CARTESIAN_POINT('Ctrl Pts',(44.5079524583205,-55.5485515672488,
-44.2662000828292));
#265434=CARTESIAN_POINT('Ctrl Pts',(43.6735798885264,-56.0302767950239,
-44.2078667494958));
#265435=CARTESIAN_POINT('Ctrl Pts',(42.8392073187323,-56.5120020227989,
-44.1495334161625));
#265436=CARTESIAN_POINT('Ctrl Pts',(42.8392073187323,-57.4754524783491,
-44.0912000828291));
#265437=CARTESIAN_POINT('Ctrl Pts',(42.8392073187323,-58.4389029338992,
-44.0328667494958));
#265438=CARTESIAN_POINT('Ctrl Pts',(43.6735798885264,-58.9206281616743,
-43.9745334161625));
#265439=CARTESIAN_POINT('Ctrl Pts',(44.5079524583205,-59.4023533894493,
-43.9162000828292));
#265440=CARTESIAN_POINT('Ctrl Pts',(45.3423250281146,-58.9206281616743,
-43.8578667494958));
#265441=CARTESIAN_POINT('Ctrl Pts',(46.1766975979086,-58.4389029338992,
-43.7995334161625));
#265442=CARTESIAN_POINT('Ctrl Pts',(46.1766975979086,-57.4754524783491,
-43.7412000828291));
#265443=CARTESIAN_POINT('Ctrl Pts',(46.1766975979086,-56.512002022799,-43.6828667494958));
#265444=CARTESIAN_POINT('Ctrl Pts',(45.3423250281146,-56.0302767950239,
-43.6245334161625));
#265445=CARTESIAN_POINT('Ctrl Pts',(44.5079524583205,-55.5485515672488,
-43.5662000828292));
#265446=CARTESIAN_POINT('Ctrl Pts',(43.6735798885264,-56.0302767950239,
-43.5078667494958));
#265447=CARTESIAN_POINT('Ctrl Pts',(42.8392073187323,-56.5120020227989,
-43.4495334161625));
#265448=CARTESIAN_POINT('Ctrl Pts',(42.8392073187323,-57.4754524783491,
-43.3912000828291));
#265449=CARTESIAN_POINT('Ctrl Pts',(42.8392073187323,-58.4389029338992,
-43.3328667494958));
#265450=CARTESIAN_POINT('Ctrl Pts',(43.6735798885264,-58.9206281616743,
-43.2745334161625));
#265451=CARTESIAN_POINT('Ctrl Pts',(44.5079524583205,-59.4023533894493,
-43.2162000828292));
#265452=CARTESIAN_POINT('Ctrl Pts',(45.3423250281146,-58.9206281616743,
-43.1578667494958));
#265453=CARTESIAN_POINT('Ctrl Pts',(46.1766975979086,-58.4389029338992,
-43.0995334161625));
#265454=CARTESIAN_POINT('Ctrl Pts',(46.1766975979086,-57.4754524783491,
-43.0412000828291));
#265455=CARTESIAN_POINT('Ctrl Pts',(46.1766975979086,-56.512002022799,-42.9828667494958));
#265456=CARTESIAN_POINT('Ctrl Pts',(45.3423250281146,-56.0302767950239,
-42.9245334161625));
#265457=CARTESIAN_POINT('Ctrl Pts',(44.5079524583205,-55.5485515672488,
-42.8662000828291));
#265458=CARTESIAN_POINT('Ctrl Pts',(43.6735798885264,-56.0302767950239,
-42.8078667494958));
#265459=CARTESIAN_POINT('Ctrl Pts',(42.8392073187323,-56.5120020227989,
-42.7495334161625));
#265460=CARTESIAN_POINT('Ctrl Pts',(42.8392073187323,-57.4754524783491,
-42.6912000828291));
#265461=CARTESIAN_POINT('Ctrl Pts',(42.8392073187323,-58.4389029338992,
-42.6328667494958));
#265462=CARTESIAN_POINT('Ctrl Pts',(43.6735798885264,-58.9206281616743,
-42.5745334161625));
#265463=CARTESIAN_POINT('Ctrl Pts',(44.5079524583205,-59.4023533894493,
-42.5162000828291));
#265464=CARTESIAN_POINT('Ctrl Pts',(45.3423250281146,-58.9206281616743,
-42.4578667494958));
#265465=CARTESIAN_POINT('Ctrl Pts',(46.1766975979086,-58.4389029338992,
-42.3995334161625));
#265466=CARTESIAN_POINT('Ctrl Pts',(46.1766975979086,-57.4754524783491,
-42.3412000828291));
#265467=CARTESIAN_POINT('Ctrl Pts',(46.1766975979086,-56.512002022799,-42.2828667494958));
#265468=CARTESIAN_POINT('Ctrl Pts',(45.3423250281146,-56.0302767950239,
-42.2245334161625));
#265469=CARTESIAN_POINT('Ctrl Pts',(44.5079524583205,-55.5485515672488,
-42.1662000828291));
#265470=CARTESIAN_POINT('Ctrl Pts',(43.6735798885264,-56.0302767950239,
-42.1078667494958));
#265471=CARTESIAN_POINT('Ctrl Pts',(42.8392073187323,-56.5120020227989,
-42.0495334161625));
#265472=CARTESIAN_POINT('Ctrl Pts',(42.8392073187323,-57.4754524783491,
-41.9912000828291));
#265473=CARTESIAN_POINT('Ctrl Pts',(42.8392073187323,-58.4389029338992,
-41.9328667494958));
#265474=CARTESIAN_POINT('Ctrl Pts',(43.6735798885264,-58.9206281616743,
-41.8745334161625));
#265475=CARTESIAN_POINT('Ctrl Pts',(44.5079524583205,-59.4023533894493,
-41.8162000828291));
#265476=CARTESIAN_POINT('Ctrl Pts',(45.3423250281146,-58.9206281616743,
-41.7578667494958));
#265477=CARTESIAN_POINT('Ctrl Pts',(46.1766975979086,-58.4389029338992,
-41.6995334161625));
#265478=CARTESIAN_POINT('Ctrl Pts',(46.1766975979086,-57.4754524783491,
-41.6412000828291));
#265479=CARTESIAN_POINT('Ctrl Pts',(46.1766975979086,-56.512002022799,-41.5828667494958));
#265480=CARTESIAN_POINT('Ctrl Pts',(45.3423250281146,-56.0302767950239,
-41.5245334161625));
#265481=CARTESIAN_POINT('Ctrl Pts',(44.5079524583205,-55.5485515672488,
-41.4662000828291));
#265482=CARTESIAN_POINT('Ctrl Pts',(43.6735798885264,-56.0302767950239,
-41.4078667494958));
#265483=CARTESIAN_POINT('Ctrl Pts',(42.8392073187323,-56.5120020227989,
-41.3495334161625));
#265484=CARTESIAN_POINT('Ctrl Pts',(42.8392073187323,-57.4754524783491,
-41.2912000828291));
#265485=CARTESIAN_POINT('Ctrl Pts',(42.8392073187323,-58.4389029338992,
-41.2328667494958));
#265486=CARTESIAN_POINT('Ctrl Pts',(43.6735798885264,-58.9206281616743,
-41.1745334161625));
#265487=CARTESIAN_POINT('Ctrl Pts',(44.5079524583205,-59.4023533894493,
-41.1162000828291));
#265488=CARTESIAN_POINT('Ctrl Pts',(45.3423250281146,-58.9206281616743,
-41.0578667494958));
#265489=CARTESIAN_POINT('Ctrl Pts',(46.1766975979086,-58.4389029338992,
-40.9995334161624));
#265490=CARTESIAN_POINT('Ctrl Pts',(46.1766975979086,-57.4754524783491,
-40.9412000828291));
#265491=CARTESIAN_POINT('Ctrl Pts',(46.1766975979086,-56.512002022799,-40.8828667494959));
#265492=CARTESIAN_POINT('Ctrl Pts',(45.3423250281146,-56.0302767950239,
-40.8245334161625));
#265493=CARTESIAN_POINT('Ctrl Pts',(44.5079524583205,-55.5485515672488,
-40.7662000828291));
#265494=CARTESIAN_POINT('Ctrl Pts',(43.6735798885264,-56.0302767950239,
-40.7078667494958));
#265495=CARTESIAN_POINT('Ctrl Pts',(42.8392073187323,-56.5120020227989,
-40.6495334161625));
#265496=CARTESIAN_POINT('Ctrl Pts',(42.8392073187323,-57.4754524783491,
-40.5912000828291));
#265497=CARTESIAN_POINT('Ctrl Pts',(42.8392073187323,-58.4389029338992,
-40.5328667494958));
#265498=CARTESIAN_POINT('Ctrl Pts',(43.6735798885264,-58.9206281616743,
-40.4745334161625));
#265499=CARTESIAN_POINT('Ctrl Pts',(44.5079524583205,-59.4023533894493,
-40.4162000828291));
#265500=CARTESIAN_POINT('Ctrl Pts',(45.3423250281146,-58.9206281616743,
-40.3578667494958));
#265501=CARTESIAN_POINT('Ctrl Pts',(46.1766975979086,-58.4389029338992,
-40.2995334161625));
#265502=CARTESIAN_POINT('Ctrl Pts',(46.1766975979086,-57.4754524783491,
-40.2412000828291));
#265503=CARTESIAN_POINT('Ctrl Pts',(46.1766975979086,-56.512002022799,-40.1828667494958));
#265504=CARTESIAN_POINT('Ctrl Pts',(45.3423250281146,-56.0302767950239,
-40.1245334161625));
#265505=CARTESIAN_POINT('Ctrl Pts',(44.5079524583205,-55.5485515672488,
-40.0662000828292));
#265506=CARTESIAN_POINT('Ctrl Pts',(43.6735798885264,-56.0302767950239,
-40.0078667494958));
#265507=CARTESIAN_POINT('Ctrl Pts',(42.8392073187323,-56.5120020227989,
-39.9495334161625));
#265508=CARTESIAN_POINT('Ctrl Pts',(42.8392073187323,-57.4754524783491,
-39.8912000828291));
#265509=CARTESIAN_POINT('Ctrl Pts',(42.8392073187323,-58.4389029338992,
-39.8328667494958));
#265510=CARTESIAN_POINT('Ctrl Pts',(43.6735798885264,-58.9206281616743,
-39.7745334161625));
#265511=CARTESIAN_POINT('Ctrl Pts',(44.5079524583205,-59.4023533894493,
-39.7162000828292));
#265512=CARTESIAN_POINT('Ctrl Pts',(45.3423250281146,-58.9206281616743,
-39.6578667494958));
#265513=CARTESIAN_POINT('Ctrl Pts',(46.1766975979086,-58.4389029338992,
-39.5995334161625));
#265514=CARTESIAN_POINT('Ctrl Pts',(46.1766975979086,-57.4754524783491,
-39.5412000828291));
#265515=CARTESIAN_POINT('Ctrl Pts',(46.1766975979086,-56.512002022799,-39.4828667494958));
#265516=CARTESIAN_POINT('Ctrl Pts',(45.3423250281146,-56.0302767950239,
-39.4245334161625));
#265517=CARTESIAN_POINT('Ctrl Pts',(44.5079524583205,-55.5485515672488,
-39.3662000828292));
#265518=CARTESIAN_POINT('Ctrl Pts',(43.6735798885264,-56.0302767950239,
-39.3078667494958));
#265519=CARTESIAN_POINT('Ctrl Pts',(42.8392073187323,-56.5120020227989,
-39.2495334161625));
#265520=CARTESIAN_POINT('Ctrl Pts',(42.8392073187323,-57.4754524783491,
-39.1912000828291));
#265521=CARTESIAN_POINT('Ctrl Pts',(42.8392073187323,-58.4389029338992,
-39.1328667494958));
#265522=CARTESIAN_POINT('Ctrl Pts',(43.6735798885264,-58.9206281616743,
-39.0745334161625));
#265523=CARTESIAN_POINT('Ctrl Pts',(44.5079524583205,-59.4023533894493,
-39.0162000828292));
#265524=CARTESIAN_POINT('Ctrl Pts',(45.3423250281146,-58.9206281616743,
-38.9578667494958));
#265525=CARTESIAN_POINT('Ctrl Pts',(46.1766975979086,-58.4389029338992,
-38.8995334161625));
#265526=CARTESIAN_POINT('Ctrl Pts',(46.1766975979086,-57.4754524783491,
-38.8412000828291));
#265527=CARTESIAN_POINT('Ctrl Pts',(46.1766975979086,-56.512002022799,-38.7828667494958));
#265528=CARTESIAN_POINT('Ctrl Pts',(45.3423250281146,-56.0302767950239,
-38.7245334161625));
#265529=CARTESIAN_POINT('Ctrl Pts',(44.5079524583205,-55.5485515672488,
-38.6662000828292));
#265530=CARTESIAN_POINT('Ctrl Pts',(43.6735798885264,-56.0302767950239,
-38.6078667494958));
#265531=CARTESIAN_POINT('Ctrl Pts',(42.8392073187323,-56.5120020227989,
-38.5495334161625));
#265532=CARTESIAN_POINT('Ctrl Pts',(42.8392073187323,-57.4754524783491,
-38.4912000828291));
#265533=CARTESIAN_POINT('Ctrl Pts',(42.8392073187323,-58.4389029338992,
-38.4328667494958));
#265534=CARTESIAN_POINT('Ctrl Pts',(43.6735798885264,-58.9206281616743,
-38.3745334161625));
#265535=CARTESIAN_POINT('Ctrl Pts',(44.5079524583205,-59.4023533894493,
-38.3162000828291));
#265536=CARTESIAN_POINT('Ctrl Pts',(45.3423250281146,-58.9206281616743,
-38.2578667494958));
#265537=CARTESIAN_POINT('Ctrl Pts',(46.1766975979086,-58.4389029338992,
-38.1995334161625));
#265538=CARTESIAN_POINT('Ctrl Pts',(46.1766975979086,-57.4754524783491,
-38.1412000828291));
#265539=CARTESIAN_POINT('Ctrl Pts',(46.1766975979086,-56.512002022799,-38.0828667494958));
#265540=CARTESIAN_POINT('Ctrl Pts',(45.3423250281146,-56.0302767950239,
-38.0245334161625));
#265541=CARTESIAN_POINT('Ctrl Pts',(44.5079524583205,-55.5485515672488,
-37.9662000828292));
#265542=CARTESIAN_POINT('Ctrl Pts',(43.6735798885264,-56.0302767950239,
-37.9078667494958));
#265543=CARTESIAN_POINT('Ctrl Pts',(42.8392073187323,-56.5120020227989,
-37.8495334161625));
#265544=CARTESIAN_POINT('Ctrl Pts',(42.8392073187323,-57.4754524783491,
-37.7912000828291));
#265545=CARTESIAN_POINT('Ctrl Pts',(42.8392073187323,-58.4389029338992,
-37.7328667494958));
#265546=CARTESIAN_POINT('Ctrl Pts',(43.6735798885264,-58.9206281616743,
-37.6745334161625));
#265547=CARTESIAN_POINT('Ctrl Pts',(44.5079524583205,-59.4023533894493,
-37.6162000828292));
#265548=CARTESIAN_POINT('Ctrl Pts',(45.3423250281146,-58.9206281616743,
-37.5578667494958));
#265549=CARTESIAN_POINT('Ctrl Pts',(46.1766975979086,-58.4389029338992,
-37.4995334161625));
#265550=CARTESIAN_POINT('Ctrl Pts',(46.1766975979086,-57.4754524783491,
-37.4412000828291));
#265551=CARTESIAN_POINT('Ctrl Pts',(46.1766975979086,-56.512002022799,-37.3828667494958));
#265552=CARTESIAN_POINT('Ctrl Pts',(45.3423250281146,-56.0302767950239,
-37.3245334161625));
#265553=CARTESIAN_POINT('Ctrl Pts',(44.5079524583205,-55.5485515672488,
-37.2662000828291));
#265554=CARTESIAN_POINT('Ctrl Pts',(43.6735798885264,-56.0302767950239,
-37.2078667494958));
#265555=CARTESIAN_POINT('Ctrl Pts',(42.8392073187323,-56.5120020227989,
-37.1495334161625));
#265556=CARTESIAN_POINT('Ctrl Pts',(42.8392073187323,-57.4754524783491,
-37.0912000828291));
#265557=CARTESIAN_POINT('Ctrl Pts',(42.8392073187323,-58.4389029338992,
-37.0328667494958));
#265558=CARTESIAN_POINT('Ctrl Pts',(43.6735798885264,-58.9206281616743,
-36.9745334161625));
#265559=CARTESIAN_POINT('Ctrl Pts',(44.5079524583205,-59.4023533894493,
-36.9162000828291));
#265560=CARTESIAN_POINT('Ctrl Pts',(45.3423250281146,-58.9206281616743,
-36.8578667494958));
#265561=CARTESIAN_POINT('Ctrl Pts',(45.450643562082,-58.85809042693,-36.8502938961005));
#265562=CARTESIAN_POINT('Ctrl Pts',(45.5484296141971,-58.7801047803048,
-36.8421539069472));
#265563=CARTESIAN_POINT('Ctrl Pts',(43.0534153750531,-58.2933966653875,
-39.8341885847849));
#265564=CARTESIAN_POINT('Ctrl Pts',(43.0851788151522,-58.4442420125764,
-39.7972051715141));
#265565=CARTESIAN_POINT('Ctrl Pts',(43.1309616784702,-58.5915153842683,
-39.7576523687012));
#265566=CARTESIAN_POINT('Ctrl Pts',(43.247256036382,-58.8749728352147,-39.6755423546175));
#265567=CARTESIAN_POINT('Ctrl Pts',(43.3177680072758,-59.0111108306031,
-39.6330135942989));
#265568=CARTESIAN_POINT('Ctrl Pts',(43.3993758805278,-59.140102067276,-39.5898550959804));
#265569=CARTESIAN_POINT('Ctrl Pts',(46.1766977413729,-57.4754524783491,
-52.99995));
#265570=CARTESIAN_POINT('Ctrl Pts',(46.1766977413729,-56.5120019399699,
-52.9416166666667));
#265571=CARTESIAN_POINT('Ctrl Pts',(45.3423250998467,-56.0302766707802,
-52.8832833333334));
#265572=CARTESIAN_POINT('Ctrl Pts',(44.5079524583205,-55.5485514015906,
-52.82495));
#265573=CARTESIAN_POINT('Ctrl Pts',(43.6735798167943,-56.0302766707802,
-52.7666166666667));
#265574=CARTESIAN_POINT('Ctrl Pts',(42.839207175268,-56.5120019399698,-52.7082833333333));
#265575=CARTESIAN_POINT('Ctrl Pts',(42.839207175268,-57.4754524783491,-52.64995));
#265576=CARTESIAN_POINT('Ctrl Pts',(42.839207175268,-58.4389030167283,-52.5916166666666));
#265577=CARTESIAN_POINT('Ctrl Pts',(43.6735798167943,-58.920628285918,-52.5332833333334));
#265578=CARTESIAN_POINT('Ctrl Pts',(44.5079524583205,-59.4023535551075,
-52.4749500000001));
#265579=CARTESIAN_POINT('Ctrl Pts',(45.3423250998467,-58.920628285918,-52.4166166666667));
#265580=CARTESIAN_POINT('Ctrl Pts',(46.1766977413729,-58.4389030167283,
-52.3582833333334));
#265581=CARTESIAN_POINT('Ctrl Pts',(46.1766977413729,-57.4754524783491,
-52.29995));
#265582=CARTESIAN_POINT('Ctrl Pts',(46.1766977413729,-56.5120019399699,
-52.2416166666667));
#265583=CARTESIAN_POINT('Ctrl Pts',(45.3423250998467,-56.0302766707802,
-52.1832833333333));
#265584=CARTESIAN_POINT('Ctrl Pts',(44.5079524583205,-55.5485514015906,
-52.12495));
#265585=CARTESIAN_POINT('Ctrl Pts',(43.6735798167943,-56.0302766707802,
-52.0666166666667));
#265586=CARTESIAN_POINT('Ctrl Pts',(42.839207175268,-56.5120019399698,-52.0082833333333));
#265587=CARTESIAN_POINT('Ctrl Pts',(42.839207175268,-57.4754524783491,-51.94995));
#265588=CARTESIAN_POINT('Ctrl Pts',(42.839207175268,-58.4389030167283,-51.8916166666667));
#265589=CARTESIAN_POINT('Ctrl Pts',(43.6735798167943,-58.920628285918,-51.8332833333334));
#265590=CARTESIAN_POINT('Ctrl Pts',(44.5079524583205,-59.4023535551075,
-51.77495));
#265591=CARTESIAN_POINT('Ctrl Pts',(45.3423250998467,-58.920628285918,-51.7166166666667));
#265592=CARTESIAN_POINT('Ctrl Pts',(46.1766977413729,-58.4389030167283,
-51.6582833333333));
#265593=CARTESIAN_POINT('Ctrl Pts',(46.1766977413729,-57.4754524783491,
-51.59995));
#265594=CARTESIAN_POINT('Ctrl Pts',(46.1766977413729,-56.5120019399699,
-51.5416166666667));
#265595=CARTESIAN_POINT('Ctrl Pts',(45.3423250998467,-56.0302766707802,
-51.4832833333334));
#265596=CARTESIAN_POINT('Ctrl Pts',(44.5079524583205,-55.5485514015906,
-51.42495));
#265597=CARTESIAN_POINT('Ctrl Pts',(43.6735798167943,-56.0302766707802,
-51.3666166666667));
#265598=CARTESIAN_POINT('Ctrl Pts',(42.839207175268,-56.5120019399698,-51.3082833333333));
#265599=CARTESIAN_POINT('Ctrl Pts',(42.839207175268,-57.4754524783491,-51.24995));
#265600=CARTESIAN_POINT('Ctrl Pts',(42.839207175268,-58.4389030167283,-51.1916166666667));
#265601=CARTESIAN_POINT('Ctrl Pts',(43.6735798167943,-58.920628285918,-51.1332833333334));
#265602=CARTESIAN_POINT('Ctrl Pts',(44.5079524583205,-59.4023535551075,
-51.07495));
#265603=CARTESIAN_POINT('Ctrl Pts',(45.3423250998467,-58.920628285918,-51.0166166666667));
#265604=CARTESIAN_POINT('Ctrl Pts',(46.1766977413729,-58.4389030167283,
-50.9582833333334));
#265605=CARTESIAN_POINT('Ctrl Pts',(46.1766977413729,-57.4754524783491,
-50.89995));
#265606=CARTESIAN_POINT('Ctrl Pts',(46.1766977413729,-56.5120019399699,
-50.8416166666667));
#265607=CARTESIAN_POINT('Ctrl Pts',(45.3423250998467,-56.0302766707802,
-50.7832833333333));
#265608=CARTESIAN_POINT('Ctrl Pts',(44.5079524583205,-55.5485514015906,
-50.72495));
#265609=CARTESIAN_POINT('Ctrl Pts',(43.6735798167943,-56.0302766707802,
-50.6666166666667));
#265610=CARTESIAN_POINT('Ctrl Pts',(42.839207175268,-56.5120019399698,-50.6082833333334));
#265611=CARTESIAN_POINT('Ctrl Pts',(42.839207175268,-57.4754524783491,-50.54995));
#265612=CARTESIAN_POINT('Ctrl Pts',(42.839207175268,-58.4389030167283,-50.4916166666667));
#265613=CARTESIAN_POINT('Ctrl Pts',(43.6735798167943,-58.920628285918,-50.4332833333333));
#265614=CARTESIAN_POINT('Ctrl Pts',(44.5079524583205,-59.4023535551075,
-50.37495));
#265615=CARTESIAN_POINT('Ctrl Pts',(45.3423250998467,-58.920628285918,-50.3166166666667));
#265616=CARTESIAN_POINT('Ctrl Pts',(46.1766977413729,-58.4389030167283,
-50.2582833333334));
#265617=CARTESIAN_POINT('Ctrl Pts',(46.1766977413729,-57.4754524783491,
-50.19995));
#265618=CARTESIAN_POINT('Ctrl Pts',(46.1766977413729,-56.5120019399699,
-50.1416166666667));
#265619=CARTESIAN_POINT('Ctrl Pts',(45.3423250998467,-56.0302766707802,
-50.0832833333334));
#265620=CARTESIAN_POINT('Ctrl Pts',(44.5079524583205,-55.5485514015906,
-50.02495));
#265621=CARTESIAN_POINT('Ctrl Pts',(43.6735798167943,-56.0302766707802,
-49.9666166666667));
#265622=CARTESIAN_POINT('Ctrl Pts',(42.839207175268,-56.5120019399698,-49.9082833333334));
#265623=CARTESIAN_POINT('Ctrl Pts',(42.839207175268,-57.4754524783491,-49.84995));
#265624=CARTESIAN_POINT('Ctrl Pts',(42.839207175268,-58.4389030167283,-49.7916166666667));
#265625=CARTESIAN_POINT('Ctrl Pts',(43.6735798167943,-58.920628285918,-49.7332833333334));
#265626=CARTESIAN_POINT('Ctrl Pts',(44.5079524583205,-59.4023535551075,
-49.67495));
#265627=CARTESIAN_POINT('Ctrl Pts',(45.3423250998467,-58.920628285918,-49.6166166666667));
#265628=CARTESIAN_POINT('Ctrl Pts',(46.1766977413729,-58.4389030167283,
-49.5582833333334));
#265629=CARTESIAN_POINT('Ctrl Pts',(46.1766977413729,-57.4754524783491,
-49.49995));
#265630=CARTESIAN_POINT('Ctrl Pts',(46.1766977413729,-56.5120019399699,
-49.4416166666667));
#265631=CARTESIAN_POINT('Ctrl Pts',(45.3423250998467,-56.0302766707802,
-49.3832833333334));
#265632=CARTESIAN_POINT('Ctrl Pts',(44.5079524583205,-55.5485514015906,
-49.32495));
#265633=CARTESIAN_POINT('Ctrl Pts',(43.6735798167943,-56.0302766707802,
-49.2666166666667));
#265634=CARTESIAN_POINT('Ctrl Pts',(42.839207175268,-56.5120019399698,-49.2082833333334));
#265635=CARTESIAN_POINT('Ctrl Pts',(42.839207175268,-57.4754524783491,-49.14995));
#265636=CARTESIAN_POINT('Ctrl Pts',(42.839207175268,-58.4389030167283,-49.0916166666667));
#265637=CARTESIAN_POINT('Ctrl Pts',(43.6735798167943,-58.920628285918,-49.0332833333333));
#265638=CARTESIAN_POINT('Ctrl Pts',(44.5079524583205,-59.4023535551075,
-48.97495));
#265639=CARTESIAN_POINT('Ctrl Pts',(45.3423250998467,-58.920628285918,-48.9166166666667));
#265640=CARTESIAN_POINT('Ctrl Pts',(46.1766977413729,-58.4389030167283,
-48.8582833333333));
#265641=CARTESIAN_POINT('Ctrl Pts',(46.1766977413729,-57.4754524783491,
-48.79995));
#265642=CARTESIAN_POINT('Ctrl Pts',(46.1766977413729,-56.5120019399699,
-48.7416166666667));
#265643=CARTESIAN_POINT('Ctrl Pts',(45.3423250998467,-56.0302766707802,
-48.6832833333334));
#265644=CARTESIAN_POINT('Ctrl Pts',(44.5079524583205,-55.5485514015906,
-48.62495));
#265645=CARTESIAN_POINT('Ctrl Pts',(43.6735798167943,-56.0302766707802,
-48.5666166666667));
#265646=CARTESIAN_POINT('Ctrl Pts',(42.839207175268,-56.5120019399698,-48.5082833333334));
#265647=CARTESIAN_POINT('Ctrl Pts',(42.839207175268,-57.4754524783491,-48.44995));
#265648=CARTESIAN_POINT('Ctrl Pts',(42.839207175268,-58.4389030167283,-48.3916166666667));
#265649=CARTESIAN_POINT('Ctrl Pts',(43.6735798167943,-58.920628285918,-48.3332833333334));
#265650=CARTESIAN_POINT('Ctrl Pts',(44.5079524583205,-59.4023535551075,
-48.27495));
#265651=CARTESIAN_POINT('Ctrl Pts',(45.3423250998467,-58.920628285918,-48.2166166666667));
#265652=CARTESIAN_POINT('Ctrl Pts',(46.1766977413729,-58.4389030167283,
-48.1582833333334));
#265653=CARTESIAN_POINT('Ctrl Pts',(46.1766977413729,-57.4754524783491,
-48.09995));
#265654=CARTESIAN_POINT('Ctrl Pts',(46.1766977413729,-56.5120019399699,
-48.0416166666667));
#265655=CARTESIAN_POINT('Ctrl Pts',(45.3423250998467,-56.0302766707802,
-47.9832833333334));
#265656=CARTESIAN_POINT('Ctrl Pts',(44.5079524583205,-55.5485514015906,
-47.92495));
#265657=CARTESIAN_POINT('Ctrl Pts',(43.6735798167943,-56.0302766707802,
-47.8666166666667));
#265658=CARTESIAN_POINT('Ctrl Pts',(42.839207175268,-56.5120019399698,-47.8082833333333));
#265659=CARTESIAN_POINT('Ctrl Pts',(42.839207175268,-57.4754524783491,-47.74995));
#265660=CARTESIAN_POINT('Ctrl Pts',(42.839207175268,-58.4389030167283,-47.6916166666667));
#265661=CARTESIAN_POINT('Ctrl Pts',(43.6735798167943,-58.920628285918,-47.6332833333333));
#265662=CARTESIAN_POINT('Ctrl Pts',(44.5079524583205,-59.4023535551075,
-47.57495));
#265663=CARTESIAN_POINT('Ctrl Pts',(45.3423250998467,-58.920628285918,-47.5166166666667));
#265664=CARTESIAN_POINT('Ctrl Pts',(46.1766977413729,-58.4389030167283,
-47.4582833333333));
#265665=CARTESIAN_POINT('Ctrl Pts',(46.1766977413729,-57.4754524783491,
-47.39995));
#265666=CARTESIAN_POINT('Ctrl Pts',(46.1766977413729,-56.5120019399699,
-47.3416166666666));
#265667=CARTESIAN_POINT('Ctrl Pts',(45.3423250998467,-56.0302766707802,
-47.2832833333333));
#265668=CARTESIAN_POINT('Ctrl Pts',(44.5079524583205,-55.5485514015906,
-47.22495));
#265669=CARTESIAN_POINT('Ctrl Pts',(43.6735798167943,-56.0302766707802,
-47.1666166666667));
#265670=CARTESIAN_POINT('Ctrl Pts',(42.839207175268,-56.5120019399698,-47.1082833333333));
#265671=CARTESIAN_POINT('Ctrl Pts',(42.839207175268,-57.4754524783491,-47.04995));
#265672=CARTESIAN_POINT('Ctrl Pts',(42.839207175268,-58.4389030167283,-46.9916166666667));
#265673=CARTESIAN_POINT('Ctrl Pts',(43.6735798167943,-58.920628285918,-46.9332833333334));
#265674=CARTESIAN_POINT('Ctrl Pts',(44.5079524583205,-59.4023535551075,
-46.87495));
#265675=CARTESIAN_POINT('Ctrl Pts',(45.3423250998467,-58.920628285918,-46.8166166666667));
#265676=CARTESIAN_POINT('Ctrl Pts',(46.1766977413729,-58.4389030167283,
-46.7582833333333));
#265677=CARTESIAN_POINT('Ctrl Pts',(46.1766977413729,-57.4754524783491,
-46.69995));
#265678=CARTESIAN_POINT('Ctrl Pts',(46.1766977413729,-56.5120019399699,
-46.6416166666666));
#265679=CARTESIAN_POINT('Ctrl Pts',(45.3423250998467,-56.0302766707802,
-46.5832833333334));
#265680=CARTESIAN_POINT('Ctrl Pts',(44.5079524583205,-55.5485514015906,
-46.52495));
#265681=CARTESIAN_POINT('Ctrl Pts',(43.6735798167943,-56.0302766707802,
-46.4666166666667));
#265682=CARTESIAN_POINT('Ctrl Pts',(42.839207175268,-56.5120019399698,-46.4082833333333));
#265683=CARTESIAN_POINT('Ctrl Pts',(42.839207175268,-57.4754524783491,-46.34995));
#265684=CARTESIAN_POINT('Ctrl Pts',(42.839207175268,-58.4389030167283,-46.2916166666667));
#265685=CARTESIAN_POINT('Ctrl Pts',(43.6735798167943,-58.920628285918,-46.2332833333334));
#265686=CARTESIAN_POINT('Ctrl Pts',(44.5079524583205,-59.4023535551075,
-46.17495));
#265687=CARTESIAN_POINT('Ctrl Pts',(45.3423250998467,-58.920628285918,-46.1166166666667));
#265688=CARTESIAN_POINT('Ctrl Pts',(46.1766977413729,-58.4389030167283,
-46.0582833333333));
#265689=CARTESIAN_POINT('Ctrl Pts',(46.1766977413729,-57.4754524783491,
-45.99995));
#265690=CARTESIAN_POINT('Ctrl Pts',(46.1766977413729,-56.5120019399699,
-45.9416166666667));
#265691=CARTESIAN_POINT('Ctrl Pts',(45.3423250998467,-56.0302766707802,
-45.8832833333333));
#265692=CARTESIAN_POINT('Ctrl Pts',(44.5079524583205,-55.5485514015906,
-45.82495));
#265693=CARTESIAN_POINT('Ctrl Pts',(43.6735798167943,-56.0302766707802,
-45.7666166666667));
#265694=CARTESIAN_POINT('Ctrl Pts',(42.839207175268,-56.5120019399698,-45.7082833333333));
#265695=CARTESIAN_POINT('Ctrl Pts',(42.839207175268,-57.4754524783491,-45.64995));
#265696=CARTESIAN_POINT('Ctrl Pts',(42.839207175268,-58.4389030167283,-45.5916166666667));
#265697=CARTESIAN_POINT('Ctrl Pts',(43.6735798167943,-58.920628285918,-45.5332833333333));
#265698=CARTESIAN_POINT('Ctrl Pts',(44.5079524583205,-59.4023535551075,
-45.47495));
#265699=CARTESIAN_POINT('Ctrl Pts',(45.3423250998467,-58.920628285918,-45.4166166666667));
#265700=CARTESIAN_POINT('Ctrl Pts',(46.1766977413729,-58.4389030167283,
-45.3582833333333));
#265701=CARTESIAN_POINT('Ctrl Pts',(46.1766977413729,-57.4754524783491,
-45.29995));
#265702=CARTESIAN_POINT('Ctrl Pts',(46.1766977413729,-56.5120019399699,
-45.2416166666667));
#265703=CARTESIAN_POINT('Ctrl Pts',(45.3423250998467,-56.0302766707802,
-45.1832833333334));
#265704=CARTESIAN_POINT('Ctrl Pts',(44.5079524583205,-55.5485514015906,
-45.12495));
#265705=CARTESIAN_POINT('Ctrl Pts',(43.6735798167943,-56.0302766707802,
-45.0666166666667));
#265706=CARTESIAN_POINT('Ctrl Pts',(42.839207175268,-56.5120019399698,-45.0082833333334));
#265707=CARTESIAN_POINT('Ctrl Pts',(42.839207175268,-57.4754524783491,-44.94995));
#265708=CARTESIAN_POINT('Ctrl Pts',(42.839207175268,-58.4389030167283,-44.8916166666667));
#265709=CARTESIAN_POINT('Ctrl Pts',(43.6735798167943,-58.920628285918,-44.8332833333334));
#265710=CARTESIAN_POINT('Ctrl Pts',(44.5079524583205,-59.4023535551075,
-44.77495));
#265711=CARTESIAN_POINT('Ctrl Pts',(45.3423250998467,-58.920628285918,-44.7166166666667));
#265712=CARTESIAN_POINT('Ctrl Pts',(46.1766977413729,-58.4389030167283,
-44.6582833333334));
#265713=CARTESIAN_POINT('Ctrl Pts',(46.1766977413729,-57.4754524783491,
-44.59995));
#265714=CARTESIAN_POINT('Ctrl Pts',(46.1766977413729,-56.5120019399699,
-44.5416166666667));
#265715=CARTESIAN_POINT('Ctrl Pts',(45.3423250998467,-56.0302766707802,
-44.4832833333334));
#265716=CARTESIAN_POINT('Ctrl Pts',(44.5079524583205,-55.5485514015906,
-44.42495));
#265717=CARTESIAN_POINT('Ctrl Pts',(43.6735798167943,-56.0302766707802,
-44.3666166666667));
#265718=CARTESIAN_POINT('Ctrl Pts',(42.839207175268,-56.5120019399698,-44.3082833333334));
#265719=CARTESIAN_POINT('Ctrl Pts',(42.839207175268,-57.4754524783491,-44.24995));
#265720=CARTESIAN_POINT('Ctrl Pts',(42.839207175268,-58.4389030167283,-44.1916166666667));
#265721=CARTESIAN_POINT('Ctrl Pts',(43.6735798167943,-58.920628285918,-44.1332833333334));
#265722=CARTESIAN_POINT('Ctrl Pts',(44.5079524583205,-59.4023535551075,
-44.07495));
#265723=CARTESIAN_POINT('Ctrl Pts',(45.3423250998467,-58.920628285918,-44.0166166666667));
#265724=CARTESIAN_POINT('Ctrl Pts',(46.1766977413729,-58.4389030167283,
-43.9582833333334));
#265725=CARTESIAN_POINT('Ctrl Pts',(46.1766977413729,-57.4754524783491,
-43.89995));
#265726=CARTESIAN_POINT('Ctrl Pts',(46.1766977413729,-56.5120019399699,
-43.8416166666667));
#265727=CARTESIAN_POINT('Ctrl Pts',(45.3423250998467,-56.0302766707802,
-43.7832833333334));
#265728=CARTESIAN_POINT('Ctrl Pts',(44.5079524583205,-55.5485514015906,
-43.72495));
#265729=CARTESIAN_POINT('Ctrl Pts',(43.6735798167943,-56.0302766707802,
-43.6666166666667));
#265730=CARTESIAN_POINT('Ctrl Pts',(42.839207175268,-56.5120019399698,-43.6082833333333));
#265731=CARTESIAN_POINT('Ctrl Pts',(42.839207175268,-57.4754524783491,-43.54995));
#265732=CARTESIAN_POINT('Ctrl Pts',(42.839207175268,-58.4389030167283,-43.4916166666667));
#265733=CARTESIAN_POINT('Ctrl Pts',(43.6735798167943,-58.920628285918,-43.4332833333333));
#265734=CARTESIAN_POINT('Ctrl Pts',(44.5079524583205,-59.4023535551075,
-43.37495));
#265735=CARTESIAN_POINT('Ctrl Pts',(45.3423250998467,-58.920628285918,-43.3166166666667));
#265736=CARTESIAN_POINT('Ctrl Pts',(46.1766977413729,-58.4389030167283,
-43.2582833333333));
#265737=CARTESIAN_POINT('Ctrl Pts',(46.1766977413729,-57.4754524783491,
-43.19995));
#265738=CARTESIAN_POINT('Ctrl Pts',(46.1766977413729,-56.5120019399699,
-43.1416166666667));
#265739=CARTESIAN_POINT('Ctrl Pts',(45.3423250998467,-56.0302766707802,
-43.0832833333333));
#265740=CARTESIAN_POINT('Ctrl Pts',(44.5079524583205,-55.5485514015906,
-43.02495));
#265741=CARTESIAN_POINT('Ctrl Pts',(43.6735798167943,-56.0302766707802,
-42.9666166666667));
#265742=CARTESIAN_POINT('Ctrl Pts',(42.839207175268,-56.5120019399698,-42.9082833333333));
#265743=CARTESIAN_POINT('Ctrl Pts',(42.839207175268,-57.4754524783491,-42.84995));
#265744=CARTESIAN_POINT('Ctrl Pts',(42.839207175268,-58.4389030167283,-42.7916166666667));
#265745=CARTESIAN_POINT('Ctrl Pts',(43.6735798167943,-58.920628285918,-42.7332833333334));
#265746=CARTESIAN_POINT('Ctrl Pts',(44.5079524583205,-59.4023535551075,
-42.67495));
#265747=CARTESIAN_POINT('Ctrl Pts',(45.3423250998467,-58.920628285918,-42.6166166666667));
#265748=CARTESIAN_POINT('Ctrl Pts',(46.1766977413729,-58.4389030167283,
-42.5582833333333));
#265749=CARTESIAN_POINT('Ctrl Pts',(46.1766977413729,-57.4754524783491,
-42.49995));
#265750=CARTESIAN_POINT('Ctrl Pts',(46.1766977413729,-56.5120019399699,
-42.4416166666667));
#265751=CARTESIAN_POINT('Ctrl Pts',(45.3423250998467,-56.0302766707802,
-42.3832833333333));
#265752=CARTESIAN_POINT('Ctrl Pts',(44.5079524583205,-55.5485514015906,
-42.32495));
#265753=CARTESIAN_POINT('Ctrl Pts',(43.6735798167943,-56.0302766707802,
-42.2666166666667));
#265754=CARTESIAN_POINT('Ctrl Pts',(42.839207175268,-56.5120019399698,-42.2082833333333));
#265755=CARTESIAN_POINT('Ctrl Pts',(42.839207175268,-57.4754524783491,-42.14995));
#265756=CARTESIAN_POINT('Ctrl Pts',(42.839207175268,-58.4389030167283,-42.0916166666667));
#265757=CARTESIAN_POINT('Ctrl Pts',(43.6735798167943,-58.920628285918,-42.0332833333334));
#265758=CARTESIAN_POINT('Ctrl Pts',(44.5079524583205,-59.4023535551075,
-41.97495));
#265759=CARTESIAN_POINT('Ctrl Pts',(45.3423250998467,-58.920628285918,-41.9166166666667));
#265760=CARTESIAN_POINT('Ctrl Pts',(46.1766977413729,-58.4389030167283,
-41.8582833333333));
#265761=CARTESIAN_POINT('Ctrl Pts',(46.1766977413729,-57.4754524783491,
-41.79995));
#265762=CARTESIAN_POINT('Ctrl Pts',(46.1766977413729,-56.5120019399699,
-41.7416166666667));
#265763=CARTESIAN_POINT('Ctrl Pts',(45.3423250998467,-56.0302766707802,
-41.6832833333333));
#265764=CARTESIAN_POINT('Ctrl Pts',(44.5079524583205,-55.5485514015906,
-41.62495));
#265765=CARTESIAN_POINT('Ctrl Pts',(43.6735798167943,-56.0302766707802,
-41.5666166666667));
#265766=CARTESIAN_POINT('Ctrl Pts',(42.839207175268,-56.5120019399698,-41.5082833333334));
#265767=CARTESIAN_POINT('Ctrl Pts',(42.839207175268,-57.4754524783491,-41.44995));
#265768=CARTESIAN_POINT('Ctrl Pts',(42.839207175268,-58.4389030167283,-41.3916166666667));
#265769=CARTESIAN_POINT('Ctrl Pts',(43.6735798167943,-58.920628285918,-41.3332833333334));
#265770=CARTESIAN_POINT('Ctrl Pts',(44.5079524583205,-59.4023535551075,
-41.27495));
#265771=CARTESIAN_POINT('Ctrl Pts',(45.3423250998467,-58.920628285918,-41.2166166666667));
#265772=CARTESIAN_POINT('Ctrl Pts',(46.1766977413729,-58.4389030167283,
-41.1582833333333));
#265773=CARTESIAN_POINT('Ctrl Pts',(46.1766977413729,-57.4754524783491,
-41.09995));
#265774=CARTESIAN_POINT('Ctrl Pts',(46.1766977413729,-56.5120019399699,
-41.0416166666667));
#265775=CARTESIAN_POINT('Ctrl Pts',(45.3423250998467,-56.0302766707802,
-40.9832833333333));
#265776=CARTESIAN_POINT('Ctrl Pts',(44.5079524583205,-55.5485514015906,
-40.92495));
#265777=CARTESIAN_POINT('Ctrl Pts',(43.6735798167943,-56.0302766707802,
-40.8666166666667));
#265778=CARTESIAN_POINT('Ctrl Pts',(42.839207175268,-56.5120019399698,-40.8082833333334));
#265779=CARTESIAN_POINT('Ctrl Pts',(42.839207175268,-57.4754524783491,-40.74995));
#265780=CARTESIAN_POINT('Ctrl Pts',(42.839207175268,-58.4389030167283,-40.6916166666667));
#265781=CARTESIAN_POINT('Ctrl Pts',(43.6735798167943,-58.920628285918,-40.6332833333334));
#265782=CARTESIAN_POINT('Ctrl Pts',(44.5079524583205,-59.4023535551075,
-40.57495));
#265783=CARTESIAN_POINT('Ctrl Pts',(45.3423250998467,-58.920628285918,-40.5166166666667));
#265784=CARTESIAN_POINT('Ctrl Pts',(46.1766977413729,-58.4389030167283,
-40.4582833333333));
#265785=CARTESIAN_POINT('Ctrl Pts',(46.1766977413729,-57.4754524783491,
-40.39995));
#265786=CARTESIAN_POINT('Ctrl Pts',(46.1766977413729,-56.5120019399699,
-40.3416166666667));
#265787=CARTESIAN_POINT('Ctrl Pts',(45.3423250998467,-56.0302766707802,
-40.2832833333334));
#265788=CARTESIAN_POINT('Ctrl Pts',(44.5079524583205,-55.5485514015906,
-40.22495));
#265789=CARTESIAN_POINT('Ctrl Pts',(43.6735798167943,-56.0302766707802,
-40.1666166666667));
#265790=CARTESIAN_POINT('Ctrl Pts',(42.839207175268,-56.5120019399698,-40.1082833333334));
#265791=CARTESIAN_POINT('Ctrl Pts',(42.839207175268,-57.4754524783491,-40.04995));
#265792=CARTESIAN_POINT('Ctrl Pts',(42.839207175268,-58.4389030167283,-39.9916166666667));
#265793=CARTESIAN_POINT('Ctrl Pts',(43.6735798167943,-58.920628285918,-39.9332833333333));
#265794=CARTESIAN_POINT('Ctrl Pts',(44.5079524583205,-59.4023535551075,
-39.87495));
#265795=CARTESIAN_POINT('Ctrl Pts',(45.3423250998467,-58.920628285918,-39.8166166666667));
#265796=CARTESIAN_POINT('Ctrl Pts',(46.1766977413729,-58.4389030167283,
-39.7582833333334));
#265797=CARTESIAN_POINT('Ctrl Pts',(46.1766977413729,-57.4754524783491,
-39.69995));
#265798=CARTESIAN_POINT('Ctrl Pts',(46.1766977413729,-56.5120019399699,
-39.6416166666667));
#265799=CARTESIAN_POINT('Ctrl Pts',(45.3423250998467,-56.0302766707802,
-39.5832833333333));
#265800=CARTESIAN_POINT('Ctrl Pts',(44.5079524583205,-55.5485514015906,
-39.52495));
#265801=CARTESIAN_POINT('Ctrl Pts',(43.6735798167943,-56.0302766707802,
-39.4666166666667));
#265802=CARTESIAN_POINT('Ctrl Pts',(42.839207175268,-56.5120019399698,-39.4082833333334));
#265803=CARTESIAN_POINT('Ctrl Pts',(42.839207175268,-57.4754524783491,-39.34995));
#265804=CARTESIAN_POINT('Ctrl Pts',(42.839207175268,-58.4389030167283,-39.2916166666667));
#265805=CARTESIAN_POINT('Ctrl Pts',(43.6735798167943,-58.920628285918,-39.2332833333333));
#265806=CARTESIAN_POINT('Ctrl Pts',(44.5079524583205,-59.4023535551075,
-39.17495));
#265807=CARTESIAN_POINT('Ctrl Pts',(45.3423250998467,-58.920628285918,-39.1166166666667));
#265808=CARTESIAN_POINT('Ctrl Pts',(46.1766977413729,-58.4389030167283,
-39.0582833333334));
#265809=CARTESIAN_POINT('Ctrl Pts',(46.1766977413729,-57.4754524783491,
-38.99995));
#265810=CARTESIAN_POINT('Ctrl Pts',(46.1766977413729,-56.5120019399699,
-38.9416166666667));
#265811=CARTESIAN_POINT('Ctrl Pts',(45.3423250998467,-56.0302766707802,
-38.8832833333334));
#265812=CARTESIAN_POINT('Ctrl Pts',(44.5079524583205,-55.5485514015906,
-38.82495));
#265813=CARTESIAN_POINT('Ctrl Pts',(43.6735798167943,-56.0302766707802,
-38.7666166666667));
#265814=CARTESIAN_POINT('Ctrl Pts',(42.839207175268,-56.5120019399698,-38.7082833333334));
#265815=CARTESIAN_POINT('Ctrl Pts',(42.839207175268,-57.4754524783491,-38.64995));
#265816=CARTESIAN_POINT('Ctrl Pts',(42.839207175268,-58.4389030167283,-38.5916166666667));
#265817=CARTESIAN_POINT('Ctrl Pts',(43.6735798167943,-58.920628285918,-38.5332833333334));
#265818=CARTESIAN_POINT('Ctrl Pts',(44.5079524583205,-59.4023535551075,
-38.47495));
#265819=CARTESIAN_POINT('Ctrl Pts',(45.3423250998467,-58.920628285918,-38.4166166666667));
#265820=CARTESIAN_POINT('Ctrl Pts',(46.1766977413729,-58.4389030167283,
-38.3582833333333));
#265821=CARTESIAN_POINT('Ctrl Pts',(46.1766977413729,-57.4754524783491,
-38.29995));
#265822=CARTESIAN_POINT('Ctrl Pts',(46.1766977413729,-56.5120019399699,
-38.2416166666667));
#265823=CARTESIAN_POINT('Ctrl Pts',(45.3423250998467,-56.0302766707802,
-38.1832833333333));
#265824=CARTESIAN_POINT('Ctrl Pts',(44.5079524583205,-55.5485514015906,
-38.12495));
#265825=CARTESIAN_POINT('Ctrl Pts',(43.6735798167943,-56.0302766707802,
-38.0666166666667));
#265826=CARTESIAN_POINT('Ctrl Pts',(42.839207175268,-56.5120019399698,-38.0082833333333));
#265827=CARTESIAN_POINT('Ctrl Pts',(42.839207175268,-57.4754524783491,-37.94995));
#265828=CARTESIAN_POINT('Ctrl Pts',(42.839207175268,-58.4389030167283,-37.8916166666667));
#265829=CARTESIAN_POINT('Ctrl Pts',(43.6735798167943,-58.920628285918,-37.8332833333334));
#265830=CARTESIAN_POINT('Ctrl Pts',(44.5079524583205,-59.4023535551075,
-37.77495));
#265831=CARTESIAN_POINT('Ctrl Pts',(45.3423250998467,-58.920628285918,-37.7166166666667));
#265832=CARTESIAN_POINT('Ctrl Pts',(46.1766977413729,-58.4389030167283,
-37.6582833333333));
#265833=CARTESIAN_POINT('Ctrl Pts',(46.1766977413729,-57.4754524783491,
-37.59995));
#265834=CARTESIAN_POINT('Ctrl Pts',(46.1766977413729,-56.5120019399699,
-37.5416166666667));
#265835=CARTESIAN_POINT('Ctrl Pts',(45.3423250998467,-56.0302766707802,
-37.4832833333334));
#265836=CARTESIAN_POINT('Ctrl Pts',(44.5079524583205,-55.5485514015906,
-37.42495));
#265837=CARTESIAN_POINT('Ctrl Pts',(43.6735798167943,-56.0302766707802,
-37.3666166666667));
#265838=CARTESIAN_POINT('Ctrl Pts',(42.839207175268,-56.5120019399698,-37.3082833333333));
#265839=CARTESIAN_POINT('Ctrl Pts',(42.839207175268,-57.4754524783491,-37.24995));
#265840=CARTESIAN_POINT('Ctrl Pts',(42.839207175268,-58.4389030167283,-37.1916166666667));
#265841=CARTESIAN_POINT('Ctrl Pts',(43.6735798167943,-58.920628285918,-37.1332833333334));
#265842=CARTESIAN_POINT('Ctrl Pts',(44.5079524583205,-59.4023535551075,
-37.07495));
#265843=CARTESIAN_POINT('Ctrl Pts',(45.3423250998467,-58.920628285918,-37.0166166666667));
#265844=CARTESIAN_POINT('Ctrl Pts',(45.4506530446707,-58.8580851178131,
-37.0090431559831));
#265845=CARTESIAN_POINT('Ctrl Pts',(45.5484465834733,-58.7800914304091,
-37.0009024189827));
#265846=CARTESIAN_POINT('Ctrl Pts',(46.5766932247459,-57.4754524783491,
-53.2308875));
#265847=CARTESIAN_POINT('Ctrl Pts',(46.5766932247459,-56.2810644399698,
-53.1725541666667));
#265848=CARTESIAN_POINT('Ctrl Pts',(45.5423228415332,-55.6838704207802,
-53.1142208333334));
#265849=CARTESIAN_POINT('Ctrl Pts',(44.5079524583205,-55.0866764015906,
-53.0558875000001));
#265850=CARTESIAN_POINT('Ctrl Pts',(43.4735820751078,-55.6838704207802,
-52.9975541666667));
#265851=CARTESIAN_POINT('Ctrl Pts',(42.4392116918951,-56.2810644399698,
-52.9392208333334));
#265852=CARTESIAN_POINT('Ctrl Pts',(42.439211691895,-57.4754524783491,-52.8808875));
#265853=CARTESIAN_POINT('Ctrl Pts',(42.4392116918951,-58.6698405167284,
-52.8225541666667));
#265854=CARTESIAN_POINT('Ctrl Pts',(43.4735820751078,-59.267034535918,-52.7642208333334));
#265855=CARTESIAN_POINT('Ctrl Pts',(44.5079524583205,-59.8642285551076,
-52.7058875));
#265856=CARTESIAN_POINT('Ctrl Pts',(45.5423228415332,-59.267034535918,-52.6475541666667));
#265857=CARTESIAN_POINT('Ctrl Pts',(46.5766932247459,-58.6698405167284,
-52.5892208333333));
#265858=CARTESIAN_POINT('Ctrl Pts',(46.5766932247459,-57.4754524783491,
-52.5308875));
#265859=CARTESIAN_POINT('Ctrl Pts',(46.5766932247459,-56.2810644399698,
-52.4725541666667));
#265860=CARTESIAN_POINT('Ctrl Pts',(45.5423228415332,-55.6838704207802,
-52.4142208333334));
#265861=CARTESIAN_POINT('Ctrl Pts',(44.5079524583205,-55.0866764015906,
-52.3558875000001));
#265862=CARTESIAN_POINT('Ctrl Pts',(43.4735820751078,-55.6838704207802,
-52.2975541666667));
#265863=CARTESIAN_POINT('Ctrl Pts',(42.4392116918951,-56.2810644399698,
-52.2392208333334));
#265864=CARTESIAN_POINT('Ctrl Pts',(42.439211691895,-57.4754524783491,-52.1808875));
#265865=CARTESIAN_POINT('Ctrl Pts',(42.4392116918951,-58.6698405167284,
-52.1225541666667));
#265866=CARTESIAN_POINT('Ctrl Pts',(43.4735820751078,-59.267034535918,-52.0642208333334));
#265867=CARTESIAN_POINT('Ctrl Pts',(44.5079524583205,-59.8642285551076,
-52.0058875));
#265868=CARTESIAN_POINT('Ctrl Pts',(45.5423228415332,-59.267034535918,-51.9475541666667));
#265869=CARTESIAN_POINT('Ctrl Pts',(46.5766932247459,-58.6698405167284,
-51.8892208333334));
#265870=CARTESIAN_POINT('Ctrl Pts',(46.5766932247459,-57.4754524783491,
-51.8308875));
#265871=CARTESIAN_POINT('Ctrl Pts',(46.5766932247459,-56.2810644399698,
-51.7725541666667));
#265872=CARTESIAN_POINT('Ctrl Pts',(45.5423228415332,-55.6838704207802,
-51.7142208333334));
#265873=CARTESIAN_POINT('Ctrl Pts',(44.5079524583205,-55.0866764015906,
-51.6558875));
#265874=CARTESIAN_POINT('Ctrl Pts',(43.4735820751078,-55.6838704207802,
-51.5975541666667));
#265875=CARTESIAN_POINT('Ctrl Pts',(42.4392116918951,-56.2810644399698,
-51.5392208333333));
#265876=CARTESIAN_POINT('Ctrl Pts',(42.439211691895,-57.4754524783491,-51.4808875));
#265877=CARTESIAN_POINT('Ctrl Pts',(42.4392116918951,-58.6698405167284,
-51.4225541666667));
#265878=CARTESIAN_POINT('Ctrl Pts',(43.4735820751078,-59.267034535918,-51.3642208333334));
#265879=CARTESIAN_POINT('Ctrl Pts',(44.5079524583205,-59.8642285551076,
-51.3058875));
#265880=CARTESIAN_POINT('Ctrl Pts',(45.5423228415332,-59.267034535918,-51.2475541666667));
#265881=CARTESIAN_POINT('Ctrl Pts',(46.5766932247459,-58.6698405167284,
-51.1892208333334));
#265882=CARTESIAN_POINT('Ctrl Pts',(46.5766932247459,-57.4754524783491,
-51.1308875));
#265883=CARTESIAN_POINT('Ctrl Pts',(46.5766932247459,-56.2810644399698,
-51.0725541666667));
#265884=CARTESIAN_POINT('Ctrl Pts',(45.5423228415332,-55.6838704207802,
-51.0142208333334));
#265885=CARTESIAN_POINT('Ctrl Pts',(44.5079524583205,-55.0866764015906,
-50.9558875));
#265886=CARTESIAN_POINT('Ctrl Pts',(43.4735820751078,-55.6838704207802,
-50.8975541666667));
#265887=CARTESIAN_POINT('Ctrl Pts',(42.4392116918951,-56.2810644399698,
-50.8392208333333));
#265888=CARTESIAN_POINT('Ctrl Pts',(42.439211691895,-57.4754524783491,-50.7808875));
#265889=CARTESIAN_POINT('Ctrl Pts',(42.4392116918951,-58.6698405167284,
-50.7225541666667));
#265890=CARTESIAN_POINT('Ctrl Pts',(43.4735820751078,-59.267034535918,-50.6642208333333));
#265891=CARTESIAN_POINT('Ctrl Pts',(44.5079524583205,-59.8642285551076,
-50.6058875));
#265892=CARTESIAN_POINT('Ctrl Pts',(45.5423228415332,-59.267034535918,-50.5475541666667));
#265893=CARTESIAN_POINT('Ctrl Pts',(46.5766932247459,-58.6698405167284,
-50.4892208333333));
#265894=CARTESIAN_POINT('Ctrl Pts',(46.5766932247459,-57.4754524783491,
-50.4308875));
#265895=CARTESIAN_POINT('Ctrl Pts',(46.5766932247459,-56.2810644399698,
-50.3725541666667));
#265896=CARTESIAN_POINT('Ctrl Pts',(45.5423228415332,-55.6838704207802,
-50.3142208333334));
#265897=CARTESIAN_POINT('Ctrl Pts',(44.5079524583205,-55.0866764015906,
-50.2558875));
#265898=CARTESIAN_POINT('Ctrl Pts',(43.4735820751078,-55.6838704207802,
-50.1975541666667));
#265899=CARTESIAN_POINT('Ctrl Pts',(42.4392116918951,-56.2810644399698,
-50.1392208333333));
#265900=CARTESIAN_POINT('Ctrl Pts',(42.439211691895,-57.4754524783491,-50.0808875));
#265901=CARTESIAN_POINT('Ctrl Pts',(42.4392116918951,-58.6698405167284,
-50.0225541666667));
#265902=CARTESIAN_POINT('Ctrl Pts',(43.4735820751078,-59.267034535918,-49.9642208333334));
#265903=CARTESIAN_POINT('Ctrl Pts',(44.5079524583205,-59.8642285551076,
-49.9058875));
#265904=CARTESIAN_POINT('Ctrl Pts',(45.5423228415332,-59.267034535918,-49.8475541666667));
#265905=CARTESIAN_POINT('Ctrl Pts',(46.5766932247459,-58.6698405167284,
-49.7892208333333));
#265906=CARTESIAN_POINT('Ctrl Pts',(46.5766932247459,-57.4754524783491,
-49.7308875));
#265907=CARTESIAN_POINT('Ctrl Pts',(46.5766932247459,-56.2810644399698,
-49.6725541666667));
#265908=CARTESIAN_POINT('Ctrl Pts',(45.5423228415332,-55.6838704207802,
-49.6142208333334));
#265909=CARTESIAN_POINT('Ctrl Pts',(44.5079524583205,-55.0866764015906,
-49.5558875));
#265910=CARTESIAN_POINT('Ctrl Pts',(43.4735820751078,-55.6838704207802,
-49.4975541666667));
#265911=CARTESIAN_POINT('Ctrl Pts',(42.4392116918951,-56.2810644399698,
-49.4392208333333));
#265912=CARTESIAN_POINT('Ctrl Pts',(42.439211691895,-57.4754524783491,-49.3808875));
#265913=CARTESIAN_POINT('Ctrl Pts',(42.4392116918951,-58.6698405167284,
-49.3225541666667));
#265914=CARTESIAN_POINT('Ctrl Pts',(43.4735820751078,-59.267034535918,-49.2642208333334));
#265915=CARTESIAN_POINT('Ctrl Pts',(44.5079524583205,-59.8642285551076,
-49.2058875));
#265916=CARTESIAN_POINT('Ctrl Pts',(45.5423228415332,-59.267034535918,-49.1475541666667));
#265917=CARTESIAN_POINT('Ctrl Pts',(46.5766932247459,-58.6698405167284,
-49.0892208333333));
#265918=CARTESIAN_POINT('Ctrl Pts',(46.5766932247459,-57.4754524783491,
-49.0308875));
#265919=CARTESIAN_POINT('Ctrl Pts',(46.5766932247459,-56.2810644399698,
-48.9725541666667));
#265920=CARTESIAN_POINT('Ctrl Pts',(45.5423228415332,-55.6838704207802,
-48.9142208333334));
#265921=CARTESIAN_POINT('Ctrl Pts',(44.5079524583205,-55.0866764015906,
-48.8558875));
#265922=CARTESIAN_POINT('Ctrl Pts',(43.4735820751078,-55.6838704207802,
-48.7975541666667));
#265923=CARTESIAN_POINT('Ctrl Pts',(42.4392116918951,-56.2810644399698,
-48.7392208333334));
#265924=CARTESIAN_POINT('Ctrl Pts',(42.439211691895,-57.4754524783491,-48.6808875));
#265925=CARTESIAN_POINT('Ctrl Pts',(42.4392116918951,-58.6698405167284,
-48.6225541666667));
#265926=CARTESIAN_POINT('Ctrl Pts',(43.4735820751078,-59.267034535918,-48.5642208333334));
#265927=CARTESIAN_POINT('Ctrl Pts',(44.5079524583205,-59.8642285551076,
-48.5058875));
#265928=CARTESIAN_POINT('Ctrl Pts',(45.5423228415332,-59.267034535918,-48.4475541666667));
#265929=CARTESIAN_POINT('Ctrl Pts',(46.5766932247459,-58.6698405167284,
-48.3892208333334));
#265930=CARTESIAN_POINT('Ctrl Pts',(46.5766932247459,-57.4754524783491,
-48.3308875));
#265931=CARTESIAN_POINT('Ctrl Pts',(46.5766932247459,-56.2810644399698,
-48.2725541666667));
#265932=CARTESIAN_POINT('Ctrl Pts',(45.5423228415332,-55.6838704207802,
-48.2142208333334));
#265933=CARTESIAN_POINT('Ctrl Pts',(44.5079524583205,-55.0866764015906,
-48.1558875));
#265934=CARTESIAN_POINT('Ctrl Pts',(43.4735820751078,-55.6838704207802,
-48.0975541666667));
#265935=CARTESIAN_POINT('Ctrl Pts',(42.4392116918951,-56.2810644399698,
-48.0392208333334));
#265936=CARTESIAN_POINT('Ctrl Pts',(42.439211691895,-57.4754524783491,-47.9808875));
#265937=CARTESIAN_POINT('Ctrl Pts',(42.4392116918951,-58.6698405167284,
-47.9225541666667));
#265938=CARTESIAN_POINT('Ctrl Pts',(43.4735820751078,-59.267034535918,-47.8642208333334));
#265939=CARTESIAN_POINT('Ctrl Pts',(44.5079524583205,-59.8642285551076,
-47.8058875000001));
#265940=CARTESIAN_POINT('Ctrl Pts',(45.5423228415332,-59.267034535918,-47.7475541666667));
#265941=CARTESIAN_POINT('Ctrl Pts',(46.5766932247459,-58.6698405167284,
-47.6892208333334));
#265942=CARTESIAN_POINT('Ctrl Pts',(46.5766932247459,-57.4754524783491,
-47.6308875));
#265943=CARTESIAN_POINT('Ctrl Pts',(46.5766932247459,-56.2810644399698,
-47.5725541666667));
#265944=CARTESIAN_POINT('Ctrl Pts',(45.5423228415332,-55.6838704207802,
-47.5142208333333));
#265945=CARTESIAN_POINT('Ctrl Pts',(44.5079524583205,-55.0866764015906,
-47.4558875));
#265946=CARTESIAN_POINT('Ctrl Pts',(43.4735820751078,-55.6838704207802,
-47.3975541666667));
#265947=CARTESIAN_POINT('Ctrl Pts',(42.4392116918951,-56.2810644399698,
-47.3392208333334));
#265948=CARTESIAN_POINT('Ctrl Pts',(42.439211691895,-57.4754524783491,-47.2808875));
#265949=CARTESIAN_POINT('Ctrl Pts',(42.4392116918951,-58.6698405167284,
-47.2225541666667));
#265950=CARTESIAN_POINT('Ctrl Pts',(43.4735820751078,-59.267034535918,-47.1642208333334));
#265951=CARTESIAN_POINT('Ctrl Pts',(44.5079524583205,-59.8642285551076,
-47.1058875));
#265952=CARTESIAN_POINT('Ctrl Pts',(45.5423228415332,-59.267034535918,-47.0475541666667));
#265953=CARTESIAN_POINT('Ctrl Pts',(46.5766932247459,-58.6698405167284,
-46.9892208333334));
#265954=CARTESIAN_POINT('Ctrl Pts',(46.5766932247459,-57.4754524783491,
-46.9308875));
#265955=CARTESIAN_POINT('Ctrl Pts',(46.5766932247459,-56.2810644399698,
-46.8725541666667));
#265956=CARTESIAN_POINT('Ctrl Pts',(45.5423228415332,-55.6838704207802,
-46.8142208333334));
#265957=CARTESIAN_POINT('Ctrl Pts',(44.5079524583205,-55.0866764015906,
-46.7558875));
#265958=CARTESIAN_POINT('Ctrl Pts',(43.4735820751078,-55.6838704207802,
-46.6975541666667));
#265959=CARTESIAN_POINT('Ctrl Pts',(42.4392116918951,-56.2810644399698,
-46.6392208333334));
#265960=CARTESIAN_POINT('Ctrl Pts',(42.439211691895,-57.4754524783491,-46.5808875));
#265961=CARTESIAN_POINT('Ctrl Pts',(42.4392116918951,-58.6698405167284,
-46.5225541666667));
#265962=CARTESIAN_POINT('Ctrl Pts',(43.4735820751078,-59.267034535918,-46.4642208333334));
#265963=CARTESIAN_POINT('Ctrl Pts',(44.5079524583205,-59.8642285551076,
-46.4058875));
#265964=CARTESIAN_POINT('Ctrl Pts',(45.5423228415332,-59.267034535918,-46.3475541666667));
#265965=CARTESIAN_POINT('Ctrl Pts',(46.5766932247459,-58.6698405167284,
-46.2892208333334));
#265966=CARTESIAN_POINT('Ctrl Pts',(46.5766932247459,-57.4754524783491,
-46.2308875));
#265967=CARTESIAN_POINT('Ctrl Pts',(46.5766932247459,-56.2810644399698,
-46.1725541666667));
#265968=CARTESIAN_POINT('Ctrl Pts',(45.5423228415332,-55.6838704207802,
-46.1142208333334));
#265969=CARTESIAN_POINT('Ctrl Pts',(44.5079524583205,-55.0866764015906,
-46.0558875));
#265970=CARTESIAN_POINT('Ctrl Pts',(43.4735820751078,-55.6838704207802,
-45.9975541666667));
#265971=CARTESIAN_POINT('Ctrl Pts',(42.4392116918951,-56.2810644399698,
-45.9392208333333));
#265972=CARTESIAN_POINT('Ctrl Pts',(42.439211691895,-57.4754524783491,-45.8808875));
#265973=CARTESIAN_POINT('Ctrl Pts',(42.4392116918951,-58.6698405167284,
-45.8225541666667));
#265974=CARTESIAN_POINT('Ctrl Pts',(43.4735820751078,-59.267034535918,-45.7642208333334));
#265975=CARTESIAN_POINT('Ctrl Pts',(44.5079524583205,-59.8642285551076,
-45.7058875));
#265976=CARTESIAN_POINT('Ctrl Pts',(45.5423228415332,-59.267034535918,-45.6475541666667));
#265977=CARTESIAN_POINT('Ctrl Pts',(46.5766932247459,-58.6698405167284,
-45.5892208333334));
#265978=CARTESIAN_POINT('Ctrl Pts',(46.5766932247459,-57.4754524783491,
-45.5308875));
#265979=CARTESIAN_POINT('Ctrl Pts',(46.5766932247459,-56.2810644399698,
-45.4725541666667));
#265980=CARTESIAN_POINT('Ctrl Pts',(45.5423228415332,-55.6838704207802,
-45.4142208333334));
#265981=CARTESIAN_POINT('Ctrl Pts',(44.5079524583205,-55.0866764015906,
-45.3558875));
#265982=CARTESIAN_POINT('Ctrl Pts',(43.4735820751078,-55.6838704207802,
-45.2975541666667));
#265983=CARTESIAN_POINT('Ctrl Pts',(42.4392116918951,-56.2810644399698,
-45.2392208333333));
#265984=CARTESIAN_POINT('Ctrl Pts',(42.439211691895,-57.4754524783491,-45.1808875));
#265985=CARTESIAN_POINT('Ctrl Pts',(42.4392116918951,-58.6698405167284,
-45.1225541666667));
#265986=CARTESIAN_POINT('Ctrl Pts',(43.4735820751078,-59.267034535918,-45.0642208333334));
#265987=CARTESIAN_POINT('Ctrl Pts',(44.5079524583205,-59.8642285551076,
-45.0058875));
#265988=CARTESIAN_POINT('Ctrl Pts',(45.5423228415332,-59.267034535918,-44.9475541666667));
#265989=CARTESIAN_POINT('Ctrl Pts',(46.5766932247459,-58.6698405167284,
-44.8892208333333));
#265990=CARTESIAN_POINT('Ctrl Pts',(46.5766932247459,-57.4754524783491,
-44.8308875));
#265991=CARTESIAN_POINT('Ctrl Pts',(46.5766932247459,-56.2810644399698,
-44.7725541666667));
#265992=CARTESIAN_POINT('Ctrl Pts',(45.5423228415332,-55.6838704207802,
-44.7142208333334));
#265993=CARTESIAN_POINT('Ctrl Pts',(44.5079524583205,-55.0866764015906,
-44.6558875));
#265994=CARTESIAN_POINT('Ctrl Pts',(43.4735820751078,-55.6838704207802,
-44.5975541666667));
#265995=CARTESIAN_POINT('Ctrl Pts',(42.4392116918951,-56.2810644399698,
-44.5392208333333));
#265996=CARTESIAN_POINT('Ctrl Pts',(42.439211691895,-57.4754524783491,-44.4808875000001));
#265997=CARTESIAN_POINT('Ctrl Pts',(42.4392116918951,-58.6698405167284,
-44.4225541666667));
#265998=CARTESIAN_POINT('Ctrl Pts',(43.4735820751078,-59.267034535918,-44.3642208333333));
#265999=CARTESIAN_POINT('Ctrl Pts',(44.5079524583205,-59.8642285551076,
-44.3058875));
#266000=CARTESIAN_POINT('Ctrl Pts',(45.5423228415332,-59.267034535918,-44.2475541666667));
#266001=CARTESIAN_POINT('Ctrl Pts',(46.5766932247459,-58.6698405167284,
-44.1892208333334));
#266002=CARTESIAN_POINT('Ctrl Pts',(46.5766932247459,-57.4754524783491,
-44.1308875000001));
#266003=CARTESIAN_POINT('Ctrl Pts',(46.5766932247459,-56.2810644399698,
-44.0725541666667));
#266004=CARTESIAN_POINT('Ctrl Pts',(45.5423228415332,-55.6838704207802,
-44.0142208333334));
#266005=CARTESIAN_POINT('Ctrl Pts',(44.5079524583205,-55.0866764015906,
-43.9558875));
#266006=CARTESIAN_POINT('Ctrl Pts',(43.4735820751078,-55.6838704207802,
-43.8975541666667));
#266007=CARTESIAN_POINT('Ctrl Pts',(42.4392116918951,-56.2810644399698,
-43.8392208333333));
#266008=CARTESIAN_POINT('Ctrl Pts',(42.439211691895,-57.4754524783491,-43.7808875));
#266009=CARTESIAN_POINT('Ctrl Pts',(42.4392116918951,-58.6698405167284,
-43.7225541666667));
#266010=CARTESIAN_POINT('Ctrl Pts',(43.4735820751078,-59.267034535918,-43.6642208333334));
#266011=CARTESIAN_POINT('Ctrl Pts',(44.5079524583205,-59.8642285551076,
-43.6058875));
#266012=CARTESIAN_POINT('Ctrl Pts',(45.5423228415332,-59.267034535918,-43.5475541666667));
#266013=CARTESIAN_POINT('Ctrl Pts',(46.5766932247459,-58.6698405167284,
-43.4892208333333));
#266014=CARTESIAN_POINT('Ctrl Pts',(46.5766932247459,-57.4754524783491,
-43.4308875));
#266015=CARTESIAN_POINT('Ctrl Pts',(46.5766932247459,-56.2810644399698,
-43.3725541666667));
#266016=CARTESIAN_POINT('Ctrl Pts',(45.5423228415332,-55.6838704207802,
-43.3142208333334));
#266017=CARTESIAN_POINT('Ctrl Pts',(44.5079524583205,-55.0866764015906,
-43.2558875));
#266018=CARTESIAN_POINT('Ctrl Pts',(43.4735820751078,-55.6838704207802,
-43.1975541666667));
#266019=CARTESIAN_POINT('Ctrl Pts',(42.4392116918951,-56.2810644399698,
-43.1392208333334));
#266020=CARTESIAN_POINT('Ctrl Pts',(42.439211691895,-57.4754524783491,-43.0808875));
#266021=CARTESIAN_POINT('Ctrl Pts',(42.4392116918951,-58.6698405167284,
-43.0225541666667));
#266022=CARTESIAN_POINT('Ctrl Pts',(43.4735820751078,-59.267034535918,-42.9642208333334));
#266023=CARTESIAN_POINT('Ctrl Pts',(44.5079524583205,-59.8642285551076,
-42.9058875));
#266024=CARTESIAN_POINT('Ctrl Pts',(45.5423228415332,-59.267034535918,-42.8475541666667));
#266025=CARTESIAN_POINT('Ctrl Pts',(46.5766932247459,-58.6698405167284,
-42.7892208333334));
#266026=CARTESIAN_POINT('Ctrl Pts',(46.5766932247459,-57.4754524783491,
-42.7308875000001));
#266027=CARTESIAN_POINT('Ctrl Pts',(46.5766932247459,-56.2810644399698,
-42.6725541666667));
#266028=CARTESIAN_POINT('Ctrl Pts',(45.5423228415332,-55.6838704207802,
-42.6142208333334));
#266029=CARTESIAN_POINT('Ctrl Pts',(44.5079524583205,-55.0866764015906,
-42.5558875));
#266030=CARTESIAN_POINT('Ctrl Pts',(43.4735820751078,-55.6838704207802,
-42.4975541666667));
#266031=CARTESIAN_POINT('Ctrl Pts',(42.4392116918951,-56.2810644399698,
-42.4392208333334));
#266032=CARTESIAN_POINT('Ctrl Pts',(42.439211691895,-57.4754524783491,-42.3808875000001));
#266033=CARTESIAN_POINT('Ctrl Pts',(42.4392116918951,-58.6698405167284,
-42.3225541666667));
#266034=CARTESIAN_POINT('Ctrl Pts',(43.4735820751078,-59.267034535918,-42.2642208333334));
#266035=CARTESIAN_POINT('Ctrl Pts',(44.5079524583205,-59.8642285551076,
-42.2058875));
#266036=CARTESIAN_POINT('Ctrl Pts',(45.5423228415332,-59.267034535918,-42.1475541666667));
#266037=CARTESIAN_POINT('Ctrl Pts',(46.5766932247459,-58.6698405167284,
-42.0892208333334));
#266038=CARTESIAN_POINT('Ctrl Pts',(46.5766932247459,-57.4754524783491,
-42.0308875000001));
#266039=CARTESIAN_POINT('Ctrl Pts',(46.5766932247459,-56.2810644399698,
-41.9725541666667));
#266040=CARTESIAN_POINT('Ctrl Pts',(45.5423228415332,-55.6838704207802,
-41.9142208333334));
#266041=CARTESIAN_POINT('Ctrl Pts',(44.5079524583205,-55.0866764015906,
-41.8558875));
#266042=CARTESIAN_POINT('Ctrl Pts',(43.4735820751078,-55.6838704207802,
-41.7975541666667));
#266043=CARTESIAN_POINT('Ctrl Pts',(42.4392116918951,-56.2810644399698,
-41.7392208333334));
#266044=CARTESIAN_POINT('Ctrl Pts',(42.439211691895,-57.4754524783491,-41.6808875000001));
#266045=CARTESIAN_POINT('Ctrl Pts',(42.4392116918951,-58.6698405167284,
-41.6225541666667));
#266046=CARTESIAN_POINT('Ctrl Pts',(43.4735820751078,-59.267034535918,-41.5642208333334));
#266047=CARTESIAN_POINT('Ctrl Pts',(44.5079524583205,-59.8642285551076,
-41.5058875));
#266048=CARTESIAN_POINT('Ctrl Pts',(45.5423228415332,-59.267034535918,-41.4475541666667));
#266049=CARTESIAN_POINT('Ctrl Pts',(46.5766932247459,-58.6698405167284,
-41.3892208333334));
#266050=CARTESIAN_POINT('Ctrl Pts',(46.5766932247459,-57.4754524783491,
-41.3308875000001));
#266051=CARTESIAN_POINT('Ctrl Pts',(46.5766932247459,-56.2810644399698,
-41.2725541666667));
#266052=CARTESIAN_POINT('Ctrl Pts',(45.5423228415332,-55.6838704207802,
-41.2142208333333));
#266053=CARTESIAN_POINT('Ctrl Pts',(44.5079524583205,-55.0866764015906,
-41.1558875));
#266054=CARTESIAN_POINT('Ctrl Pts',(43.4735820751078,-55.6838704207802,
-41.0975541666667));
#266055=CARTESIAN_POINT('Ctrl Pts',(42.4392116918951,-56.2810644399698,
-41.0392208333333));
#266056=CARTESIAN_POINT('Ctrl Pts',(42.439211691895,-57.4754524783491,-40.9808875000001));
#266057=CARTESIAN_POINT('Ctrl Pts',(42.4392116918951,-58.6698405167284,
-40.9225541666667));
#266058=CARTESIAN_POINT('Ctrl Pts',(43.4735820751078,-59.267034535918,-40.8642208333334));
#266059=CARTESIAN_POINT('Ctrl Pts',(44.5079524583205,-59.8642285551076,
-40.8058875));
#266060=CARTESIAN_POINT('Ctrl Pts',(45.5423228415332,-59.267034535918,-40.7475541666667));
#266061=CARTESIAN_POINT('Ctrl Pts',(46.5766932247459,-58.6698405167284,
-40.6892208333333));
#266062=CARTESIAN_POINT('Ctrl Pts',(46.5766932247459,-57.4754524783491,
-40.6308875));
#266063=CARTESIAN_POINT('Ctrl Pts',(46.5766932247459,-56.2810644399698,
-40.5725541666667));
#266064=CARTESIAN_POINT('Ctrl Pts',(45.5423228415332,-55.6838704207802,
-40.5142208333333));
#266065=CARTESIAN_POINT('Ctrl Pts',(44.5079524583205,-55.0866764015906,
-40.4558875));
#266066=CARTESIAN_POINT('Ctrl Pts',(43.4735820751078,-55.6838704207802,
-40.3975541666667));
#266067=CARTESIAN_POINT('Ctrl Pts',(42.4392116918951,-56.2810644399698,
-40.3392208333333));
#266068=CARTESIAN_POINT('Ctrl Pts',(42.439211691895,-57.4754524783491,-40.2808875));
#266069=CARTESIAN_POINT('Ctrl Pts',(42.4392116918951,-58.6698405167284,
-40.2225541666667));
#266070=CARTESIAN_POINT('Ctrl Pts',(43.4735820751078,-59.267034535918,-40.1642208333333));
#266071=CARTESIAN_POINT('Ctrl Pts',(44.5079524583205,-59.8642285551076,
-40.1058875));
#266072=CARTESIAN_POINT('Ctrl Pts',(45.5423228415332,-59.267034535918,-40.0475541666667));
#266073=CARTESIAN_POINT('Ctrl Pts',(46.5766932247459,-58.6698405167284,
-39.9892208333333));
#266074=CARTESIAN_POINT('Ctrl Pts',(46.5766932247459,-57.4754524783491,
-39.9308875));
#266075=CARTESIAN_POINT('Ctrl Pts',(46.5766932247459,-56.2810644399698,
-39.8725541666667));
#266076=CARTESIAN_POINT('Ctrl Pts',(45.5423228415332,-55.6838704207802,
-39.8142208333334));
#266077=CARTESIAN_POINT('Ctrl Pts',(44.5079524583205,-55.0866764015906,
-39.7558875));
#266078=CARTESIAN_POINT('Ctrl Pts',(43.4735820751078,-55.6838704207802,
-39.6975541666667));
#266079=CARTESIAN_POINT('Ctrl Pts',(42.4392116918951,-56.2810644399698,
-39.6392208333334));
#266080=CARTESIAN_POINT('Ctrl Pts',(42.439211691895,-57.4754524783491,-39.5808875000001));
#266081=CARTESIAN_POINT('Ctrl Pts',(42.4392116918951,-58.6698405167284,
-39.5225541666667));
#266082=CARTESIAN_POINT('Ctrl Pts',(43.4735820751078,-59.267034535918,-39.4642208333333));
#266083=CARTESIAN_POINT('Ctrl Pts',(44.5079524583205,-59.8642285551076,
-39.4058875));
#266084=CARTESIAN_POINT('Ctrl Pts',(45.5423228415332,-59.267034535918,-39.3475541666667));
#266085=CARTESIAN_POINT('Ctrl Pts',(46.5766932247459,-58.6698405167284,
-39.2892208333334));
#266086=CARTESIAN_POINT('Ctrl Pts',(46.5766932247459,-57.4754524783491,
-39.2308875));
#266087=CARTESIAN_POINT('Ctrl Pts',(46.5766932247459,-56.2810644399698,
-39.1725541666667));
#266088=CARTESIAN_POINT('Ctrl Pts',(45.5423228415332,-55.6838704207802,
-39.1142208333333));
#266089=CARTESIAN_POINT('Ctrl Pts',(44.5079524583205,-55.0866764015906,
-39.0558875));
#266090=CARTESIAN_POINT('Ctrl Pts',(43.4735820751078,-55.6838704207802,
-38.9975541666667));
#266091=CARTESIAN_POINT('Ctrl Pts',(42.4392116918951,-56.2810644399698,
-38.9392208333334));
#266092=CARTESIAN_POINT('Ctrl Pts',(42.439211691895,-57.4754524783491,-38.8808875));
#266093=CARTESIAN_POINT('Ctrl Pts',(42.4392116918951,-58.6698405167284,
-38.8225541666667));
#266094=CARTESIAN_POINT('Ctrl Pts',(43.4735820751078,-59.267034535918,-38.7642208333333));
#266095=CARTESIAN_POINT('Ctrl Pts',(44.5079524583205,-59.8642285551076,
-38.7058875));
#266096=CARTESIAN_POINT('Ctrl Pts',(45.5423228415332,-59.267034535918,-38.6475541666667));
#266097=CARTESIAN_POINT('Ctrl Pts',(46.5766932247459,-58.6698405167284,
-38.5892208333334));
#266098=CARTESIAN_POINT('Ctrl Pts',(46.5766932247459,-57.4754524783491,
-38.5308875));
#266099=CARTESIAN_POINT('Ctrl Pts',(46.5766932247459,-56.2810644399698,
-38.4725541666667));
#266100=CARTESIAN_POINT('Ctrl Pts',(45.5423228415332,-55.6838704207802,
-38.4142208333334));
#266101=CARTESIAN_POINT('Ctrl Pts',(44.5079524583205,-55.0866764015906,
-38.3558875));
#266102=CARTESIAN_POINT('Ctrl Pts',(43.4735820751078,-55.6838704207802,
-38.2975541666667));
#266103=CARTESIAN_POINT('Ctrl Pts',(42.4392116918951,-56.2810644399698,
-38.2392208333333));
#266104=CARTESIAN_POINT('Ctrl Pts',(42.439211691895,-57.4754524783491,-38.1808875000001));
#266105=CARTESIAN_POINT('Ctrl Pts',(42.4392116918951,-58.6698405167284,
-38.1225541666667));
#266106=CARTESIAN_POINT('Ctrl Pts',(43.4735820751078,-59.267034535918,-38.0642208333334));
#266107=CARTESIAN_POINT('Ctrl Pts',(44.5079524583205,-59.8642285551076,
-38.0058875));
#266108=CARTESIAN_POINT('Ctrl Pts',(45.5423228415332,-59.267034535918,-37.9475541666667));
#266109=CARTESIAN_POINT('Ctrl Pts',(46.5766932247459,-58.6698405167284,
-37.8892208333334));
#266110=CARTESIAN_POINT('Ctrl Pts',(46.5766932247459,-57.4754524783491,
-37.8308875));
#266111=CARTESIAN_POINT('Ctrl Pts',(46.5766932247459,-56.2810644399698,
-37.7725541666667));
#266112=CARTESIAN_POINT('Ctrl Pts',(45.5423228415332,-55.6838704207802,
-37.7142208333333));
#266113=CARTESIAN_POINT('Ctrl Pts',(44.5079524583205,-55.0866764015906,
-37.6558875));
#266114=CARTESIAN_POINT('Ctrl Pts',(43.4735820751078,-55.6838704207802,
-37.5975541666667));
#266115=CARTESIAN_POINT('Ctrl Pts',(42.4392116918951,-56.2810644399698,
-37.5392208333334));
#266116=CARTESIAN_POINT('Ctrl Pts',(42.439211691895,-57.4754524783491,-37.4808875));
#266117=CARTESIAN_POINT('Ctrl Pts',(42.4392116918951,-58.6698405167284,
-37.4225541666667));
#266118=CARTESIAN_POINT('Ctrl Pts',(43.4735820751078,-59.267034535918,-37.3642208333333));
#266119=CARTESIAN_POINT('Ctrl Pts',(44.5079524583205,-59.8642285551076,
-37.3058875));
#266120=CARTESIAN_POINT('Ctrl Pts',(45.5423228415332,-59.267034535918,-37.2475541666667));
#266121=CARTESIAN_POINT('Ctrl Pts',(45.6766168155006,-59.1894998738974,
-37.239980655983));
#266122=CARTESIAN_POINT('Ctrl Pts',(45.7978513037526,-59.0928112286649,
-37.2318399189827));
#266123=CARTESIAN_POINT('Ctrl Pts',(45.2824537511366,-55.8755132365557,
-39.638597553055));
#266124=CARTESIAN_POINT('Ctrl Pts',(45.4486364499857,-55.938875190796,-39.6579429567418));
#266125=CARTESIAN_POINT('Ctrl Pts',(45.6046461036551,-56.0241879535461,
-39.6778552592192));
#266126=CARTESIAN_POINT('Ctrl Pts',(45.9008786079562,-56.2453730623026,
-39.7222494146269));
#266127=CARTESIAN_POINT('Ctrl Pts',(46.0363919947743,-56.3826287328891,
-39.7461336748472));
#266128=CARTESIAN_POINT('Ctrl Pts',(46.2521263249353,-56.6800261237718,
-39.7916412021743));
#266129=CARTESIAN_POINT('Ctrl Pts',(46.3350396458226,-56.8359257464262,
-39.8130825635204));
#266130=CARTESIAN_POINT('Ctrl Pts',(46.4613757977742,-57.1838034186047,
-39.8560922003017));
#266131=CARTESIAN_POINT('Ctrl Pts',(46.4991955457474,-57.3765422463827,
-39.8769823938147));
#266132=CARTESIAN_POINT('Ctrl Pts',(46.5057011933515,-57.57028764973,-39.8960556104567));
#266133=CARTESIAN_POINT('Ctrl Pts',(46.1766977413729,-57.4754524783491,
-52.99995));
#266134=CARTESIAN_POINT('Ctrl Pts',(46.1766977413729,-56.5120019399699,
-52.9416166666667));
#266135=CARTESIAN_POINT('Ctrl Pts',(45.3423250998467,-56.0302766707802,
-52.8832833333334));
#266136=CARTESIAN_POINT('Ctrl Pts',(44.5079524583205,-55.5485514015906,
-52.82495));
#266137=CARTESIAN_POINT('Ctrl Pts',(43.6735798167943,-56.0302766707802,
-52.7666166666667));
#266138=CARTESIAN_POINT('Ctrl Pts',(42.839207175268,-56.5120019399698,-52.7082833333333));
#266139=CARTESIAN_POINT('Ctrl Pts',(42.839207175268,-57.4754524783491,-52.64995));
#266140=CARTESIAN_POINT('Ctrl Pts',(42.839207175268,-58.4389030167283,-52.5916166666666));
#266141=CARTESIAN_POINT('Ctrl Pts',(43.6735798167943,-58.920628285918,-52.5332833333334));
#266142=CARTESIAN_POINT('Ctrl Pts',(44.5079524583205,-59.4023535551075,
-52.4749500000001));
#266143=CARTESIAN_POINT('Ctrl Pts',(45.3423250998467,-58.920628285918,-52.4166166666667));
#266144=CARTESIAN_POINT('Ctrl Pts',(46.1766977413729,-58.4389030167283,
-52.3582833333334));
#266145=CARTESIAN_POINT('Ctrl Pts',(46.1766977413729,-57.4754524783491,
-52.29995));
#266146=CARTESIAN_POINT('Ctrl Pts',(46.1766977413729,-56.5120019399699,
-52.2416166666667));
#266147=CARTESIAN_POINT('Ctrl Pts',(45.3423250998467,-56.0302766707802,
-52.1832833333333));
#266148=CARTESIAN_POINT('Ctrl Pts',(44.5079524583205,-55.5485514015906,
-52.12495));
#266149=CARTESIAN_POINT('Ctrl Pts',(43.6735798167943,-56.0302766707802,
-52.0666166666667));
#266150=CARTESIAN_POINT('Ctrl Pts',(42.839207175268,-56.5120019399698,-52.0082833333333));
#266151=CARTESIAN_POINT('Ctrl Pts',(42.839207175268,-57.4754524783491,-51.94995));
#266152=CARTESIAN_POINT('Ctrl Pts',(42.839207175268,-58.4389030167283,-51.8916166666667));
#266153=CARTESIAN_POINT('Ctrl Pts',(43.6735798167943,-58.920628285918,-51.8332833333334));
#266154=CARTESIAN_POINT('Ctrl Pts',(44.5079524583205,-59.4023535551075,
-51.77495));
#266155=CARTESIAN_POINT('Ctrl Pts',(45.3423250998467,-58.920628285918,-51.7166166666667));
#266156=CARTESIAN_POINT('Ctrl Pts',(46.1766977413729,-58.4389030167283,
-51.6582833333333));
#266157=CARTESIAN_POINT('Ctrl Pts',(46.1766977413729,-57.4754524783491,
-51.59995));
#266158=CARTESIAN_POINT('Ctrl Pts',(46.1766977413729,-56.5120019399699,
-51.5416166666667));
#266159=CARTESIAN_POINT('Ctrl Pts',(45.3423250998467,-56.0302766707802,
-51.4832833333334));
#266160=CARTESIAN_POINT('Ctrl Pts',(44.5079524583205,-55.5485514015906,
-51.42495));
#266161=CARTESIAN_POINT('Ctrl Pts',(43.6735798167943,-56.0302766707802,
-51.3666166666667));
#266162=CARTESIAN_POINT('Ctrl Pts',(42.839207175268,-56.5120019399698,-51.3082833333333));
#266163=CARTESIAN_POINT('Ctrl Pts',(42.839207175268,-57.4754524783491,-51.24995));
#266164=CARTESIAN_POINT('Ctrl Pts',(42.839207175268,-58.4389030167283,-51.1916166666667));
#266165=CARTESIAN_POINT('Ctrl Pts',(43.6735798167943,-58.920628285918,-51.1332833333334));
#266166=CARTESIAN_POINT('Ctrl Pts',(44.5079524583205,-59.4023535551075,
-51.07495));
#266167=CARTESIAN_POINT('Ctrl Pts',(45.3423250998467,-58.920628285918,-51.0166166666667));
#266168=CARTESIAN_POINT('Ctrl Pts',(46.1766977413729,-58.4389030167283,
-50.9582833333334));
#266169=CARTESIAN_POINT('Ctrl Pts',(46.1766977413729,-57.4754524783491,
-50.89995));
#266170=CARTESIAN_POINT('Ctrl Pts',(46.1766977413729,-56.5120019399699,
-50.8416166666667));
#266171=CARTESIAN_POINT('Ctrl Pts',(45.3423250998467,-56.0302766707802,
-50.7832833333333));
#266172=CARTESIAN_POINT('Ctrl Pts',(44.5079524583205,-55.5485514015906,
-50.72495));
#266173=CARTESIAN_POINT('Ctrl Pts',(43.6735798167943,-56.0302766707802,
-50.6666166666667));
#266174=CARTESIAN_POINT('Ctrl Pts',(42.839207175268,-56.5120019399698,-50.6082833333334));
#266175=CARTESIAN_POINT('Ctrl Pts',(42.839207175268,-57.4754524783491,-50.54995));
#266176=CARTESIAN_POINT('Ctrl Pts',(42.839207175268,-58.4389030167283,-50.4916166666667));
#266177=CARTESIAN_POINT('Ctrl Pts',(43.6735798167943,-58.920628285918,-50.4332833333333));
#266178=CARTESIAN_POINT('Ctrl Pts',(44.5079524583205,-59.4023535551075,
-50.37495));
#266179=CARTESIAN_POINT('Ctrl Pts',(45.3423250998467,-58.920628285918,-50.3166166666667));
#266180=CARTESIAN_POINT('Ctrl Pts',(46.1766977413729,-58.4389030167283,
-50.2582833333334));
#266181=CARTESIAN_POINT('Ctrl Pts',(46.1766977413729,-57.4754524783491,
-50.19995));
#266182=CARTESIAN_POINT('Ctrl Pts',(46.1766977413729,-56.5120019399699,
-50.1416166666667));
#266183=CARTESIAN_POINT('Ctrl Pts',(45.3423250998467,-56.0302766707802,
-50.0832833333334));
#266184=CARTESIAN_POINT('Ctrl Pts',(44.5079524583205,-55.5485514015906,
-50.02495));
#266185=CARTESIAN_POINT('Ctrl Pts',(43.6735798167943,-56.0302766707802,
-49.9666166666667));
#266186=CARTESIAN_POINT('Ctrl Pts',(42.839207175268,-56.5120019399698,-49.9082833333334));
#266187=CARTESIAN_POINT('Ctrl Pts',(42.839207175268,-57.4754524783491,-49.84995));
#266188=CARTESIAN_POINT('Ctrl Pts',(42.839207175268,-58.4389030167283,-49.7916166666667));
#266189=CARTESIAN_POINT('Ctrl Pts',(43.6735798167943,-58.920628285918,-49.7332833333334));
#266190=CARTESIAN_POINT('Ctrl Pts',(44.5079524583205,-59.4023535551075,
-49.67495));
#266191=CARTESIAN_POINT('Ctrl Pts',(45.3423250998467,-58.920628285918,-49.6166166666667));
#266192=CARTESIAN_POINT('Ctrl Pts',(46.1766977413729,-58.4389030167283,
-49.5582833333334));
#266193=CARTESIAN_POINT('Ctrl Pts',(46.1766977413729,-57.4754524783491,
-49.49995));
#266194=CARTESIAN_POINT('Ctrl Pts',(46.1766977413729,-56.5120019399699,
-49.4416166666667));
#266195=CARTESIAN_POINT('Ctrl Pts',(45.3423250998467,-56.0302766707802,
-49.3832833333334));
#266196=CARTESIAN_POINT('Ctrl Pts',(44.5079524583205,-55.5485514015906,
-49.32495));
#266197=CARTESIAN_POINT('Ctrl Pts',(43.6735798167943,-56.0302766707802,
-49.2666166666667));
#266198=CARTESIAN_POINT('Ctrl Pts',(42.839207175268,-56.5120019399698,-49.2082833333334));
#266199=CARTESIAN_POINT('Ctrl Pts',(42.839207175268,-57.4754524783491,-49.14995));
#266200=CARTESIAN_POINT('Ctrl Pts',(42.839207175268,-58.4389030167283,-49.0916166666667));
#266201=CARTESIAN_POINT('Ctrl Pts',(43.6735798167943,-58.920628285918,-49.0332833333333));
#266202=CARTESIAN_POINT('Ctrl Pts',(44.5079524583205,-59.4023535551075,
-48.97495));
#266203=CARTESIAN_POINT('Ctrl Pts',(45.3423250998467,-58.920628285918,-48.9166166666667));
#266204=CARTESIAN_POINT('Ctrl Pts',(46.1766977413729,-58.4389030167283,
-48.8582833333333));
#266205=CARTESIAN_POINT('Ctrl Pts',(46.1766977413729,-57.4754524783491,
-48.79995));
#266206=CARTESIAN_POINT('Ctrl Pts',(46.1766977413729,-56.5120019399699,
-48.7416166666667));
#266207=CARTESIAN_POINT('Ctrl Pts',(45.3423250998467,-56.0302766707802,
-48.6832833333334));
#266208=CARTESIAN_POINT('Ctrl Pts',(44.5079524583205,-55.5485514015906,
-48.62495));
#266209=CARTESIAN_POINT('Ctrl Pts',(43.6735798167943,-56.0302766707802,
-48.5666166666667));
#266210=CARTESIAN_POINT('Ctrl Pts',(42.839207175268,-56.5120019399698,-48.5082833333334));
#266211=CARTESIAN_POINT('Ctrl Pts',(42.839207175268,-57.4754524783491,-48.44995));
#266212=CARTESIAN_POINT('Ctrl Pts',(42.839207175268,-58.4389030167283,-48.3916166666667));
#266213=CARTESIAN_POINT('Ctrl Pts',(43.6735798167943,-58.920628285918,-48.3332833333334));
#266214=CARTESIAN_POINT('Ctrl Pts',(44.5079524583205,-59.4023535551075,
-48.27495));
#266215=CARTESIAN_POINT('Ctrl Pts',(45.3423250998467,-58.920628285918,-48.2166166666667));
#266216=CARTESIAN_POINT('Ctrl Pts',(46.1766977413729,-58.4389030167283,
-48.1582833333334));
#266217=CARTESIAN_POINT('Ctrl Pts',(46.1766977413729,-57.4754524783491,
-48.09995));
#266218=CARTESIAN_POINT('Ctrl Pts',(46.1766977413729,-56.5120019399699,
-48.0416166666667));
#266219=CARTESIAN_POINT('Ctrl Pts',(45.3423250998467,-56.0302766707802,
-47.9832833333334));
#266220=CARTESIAN_POINT('Ctrl Pts',(44.5079524583205,-55.5485514015906,
-47.92495));
#266221=CARTESIAN_POINT('Ctrl Pts',(43.6735798167943,-56.0302766707802,
-47.8666166666667));
#266222=CARTESIAN_POINT('Ctrl Pts',(42.839207175268,-56.5120019399698,-47.8082833333333));
#266223=CARTESIAN_POINT('Ctrl Pts',(42.839207175268,-57.4754524783491,-47.74995));
#266224=CARTESIAN_POINT('Ctrl Pts',(42.839207175268,-58.4389030167283,-47.6916166666667));
#266225=CARTESIAN_POINT('Ctrl Pts',(43.6735798167943,-58.920628285918,-47.6332833333333));
#266226=CARTESIAN_POINT('Ctrl Pts',(44.5079524583205,-59.4023535551075,
-47.57495));
#266227=CARTESIAN_POINT('Ctrl Pts',(45.3423250998467,-58.920628285918,-47.5166166666667));
#266228=CARTESIAN_POINT('Ctrl Pts',(46.1766977413729,-58.4389030167283,
-47.4582833333333));
#266229=CARTESIAN_POINT('Ctrl Pts',(46.1766977413729,-57.4754524783491,
-47.39995));
#266230=CARTESIAN_POINT('Ctrl Pts',(46.1766977413729,-56.5120019399699,
-47.3416166666666));
#266231=CARTESIAN_POINT('Ctrl Pts',(45.3423250998467,-56.0302766707802,
-47.2832833333333));
#266232=CARTESIAN_POINT('Ctrl Pts',(44.5079524583205,-55.5485514015906,
-47.22495));
#266233=CARTESIAN_POINT('Ctrl Pts',(43.6735798167943,-56.0302766707802,
-47.1666166666667));
#266234=CARTESIAN_POINT('Ctrl Pts',(42.839207175268,-56.5120019399698,-47.1082833333333));
#266235=CARTESIAN_POINT('Ctrl Pts',(42.839207175268,-57.4754524783491,-47.04995));
#266236=CARTESIAN_POINT('Ctrl Pts',(42.839207175268,-58.4389030167283,-46.9916166666667));
#266237=CARTESIAN_POINT('Ctrl Pts',(43.6735798167943,-58.920628285918,-46.9332833333334));
#266238=CARTESIAN_POINT('Ctrl Pts',(44.5079524583205,-59.4023535551075,
-46.87495));
#266239=CARTESIAN_POINT('Ctrl Pts',(45.3423250998467,-58.920628285918,-46.8166166666667));
#266240=CARTESIAN_POINT('Ctrl Pts',(46.1766977413729,-58.4389030167283,
-46.7582833333333));
#266241=CARTESIAN_POINT('Ctrl Pts',(46.1766977413729,-57.4754524783491,
-46.69995));
#266242=CARTESIAN_POINT('Ctrl Pts',(46.1766977413729,-56.5120019399699,
-46.6416166666666));
#266243=CARTESIAN_POINT('Ctrl Pts',(45.3423250998467,-56.0302766707802,
-46.5832833333334));
#266244=CARTESIAN_POINT('Ctrl Pts',(44.5079524583205,-55.5485514015906,
-46.52495));
#266245=CARTESIAN_POINT('Ctrl Pts',(43.6735798167943,-56.0302766707802,
-46.4666166666667));
#266246=CARTESIAN_POINT('Ctrl Pts',(42.839207175268,-56.5120019399698,-46.4082833333333));
#266247=CARTESIAN_POINT('Ctrl Pts',(42.839207175268,-57.4754524783491,-46.34995));
#266248=CARTESIAN_POINT('Ctrl Pts',(42.839207175268,-58.4389030167283,-46.2916166666667));
#266249=CARTESIAN_POINT('Ctrl Pts',(43.6735798167943,-58.920628285918,-46.2332833333334));
#266250=CARTESIAN_POINT('Ctrl Pts',(44.5079524583205,-59.4023535551075,
-46.17495));
#266251=CARTESIAN_POINT('Ctrl Pts',(45.3423250998467,-58.920628285918,-46.1166166666667));
#266252=CARTESIAN_POINT('Ctrl Pts',(46.1766977413729,-58.4389030167283,
-46.0582833333333));
#266253=CARTESIAN_POINT('Ctrl Pts',(46.1766977413729,-57.4754524783491,
-45.99995));
#266254=CARTESIAN_POINT('Ctrl Pts',(46.1766977413729,-56.5120019399699,
-45.9416166666667));
#266255=CARTESIAN_POINT('Ctrl Pts',(45.3423250998467,-56.0302766707802,
-45.8832833333333));
#266256=CARTESIAN_POINT('Ctrl Pts',(44.5079524583205,-55.5485514015906,
-45.82495));
#266257=CARTESIAN_POINT('Ctrl Pts',(43.6735798167943,-56.0302766707802,
-45.7666166666667));
#266258=CARTESIAN_POINT('Ctrl Pts',(42.839207175268,-56.5120019399698,-45.7082833333333));
#266259=CARTESIAN_POINT('Ctrl Pts',(42.839207175268,-57.4754524783491,-45.64995));
#266260=CARTESIAN_POINT('Ctrl Pts',(42.839207175268,-58.4389030167283,-45.5916166666667));
#266261=CARTESIAN_POINT('Ctrl Pts',(43.6735798167943,-58.920628285918,-45.5332833333333));
#266262=CARTESIAN_POINT('Ctrl Pts',(44.5079524583205,-59.4023535551075,
-45.47495));
#266263=CARTESIAN_POINT('Ctrl Pts',(45.3423250998467,-58.920628285918,-45.4166166666667));
#266264=CARTESIAN_POINT('Ctrl Pts',(46.1766977413729,-58.4389030167283,
-45.3582833333333));
#266265=CARTESIAN_POINT('Ctrl Pts',(46.1766977413729,-57.4754524783491,
-45.29995));
#266266=CARTESIAN_POINT('Ctrl Pts',(46.1766977413729,-56.5120019399699,
-45.2416166666667));
#266267=CARTESIAN_POINT('Ctrl Pts',(45.3423250998467,-56.0302766707802,
-45.1832833333334));
#266268=CARTESIAN_POINT('Ctrl Pts',(44.5079524583205,-55.5485514015906,
-45.12495));
#266269=CARTESIAN_POINT('Ctrl Pts',(43.6735798167943,-56.0302766707802,
-45.0666166666667));
#266270=CARTESIAN_POINT('Ctrl Pts',(42.839207175268,-56.5120019399698,-45.0082833333334));
#266271=CARTESIAN_POINT('Ctrl Pts',(42.839207175268,-57.4754524783491,-44.94995));
#266272=CARTESIAN_POINT('Ctrl Pts',(42.839207175268,-58.4389030167283,-44.8916166666667));
#266273=CARTESIAN_POINT('Ctrl Pts',(43.6735798167943,-58.920628285918,-44.8332833333334));
#266274=CARTESIAN_POINT('Ctrl Pts',(44.5079524583205,-59.4023535551075,
-44.77495));
#266275=CARTESIAN_POINT('Ctrl Pts',(45.3423250998467,-58.920628285918,-44.7166166666667));
#266276=CARTESIAN_POINT('Ctrl Pts',(46.1766977413729,-58.4389030167283,
-44.6582833333334));
#266277=CARTESIAN_POINT('Ctrl Pts',(46.1766977413729,-57.4754524783491,
-44.59995));
#266278=CARTESIAN_POINT('Ctrl Pts',(46.1766977413729,-56.5120019399699,
-44.5416166666667));
#266279=CARTESIAN_POINT('Ctrl Pts',(45.3423250998467,-56.0302766707802,
-44.4832833333334));
#266280=CARTESIAN_POINT('Ctrl Pts',(44.5079524583205,-55.5485514015906,
-44.42495));
#266281=CARTESIAN_POINT('Ctrl Pts',(43.6735798167943,-56.0302766707802,
-44.3666166666667));
#266282=CARTESIAN_POINT('Ctrl Pts',(42.839207175268,-56.5120019399698,-44.3082833333334));
#266283=CARTESIAN_POINT('Ctrl Pts',(42.839207175268,-57.4754524783491,-44.24995));
#266284=CARTESIAN_POINT('Ctrl Pts',(42.839207175268,-58.4389030167283,-44.1916166666667));
#266285=CARTESIAN_POINT('Ctrl Pts',(43.6735798167943,-58.920628285918,-44.1332833333334));
#266286=CARTESIAN_POINT('Ctrl Pts',(44.5079524583205,-59.4023535551075,
-44.07495));
#266287=CARTESIAN_POINT('Ctrl Pts',(45.3423250998467,-58.920628285918,-44.0166166666667));
#266288=CARTESIAN_POINT('Ctrl Pts',(46.1766977413729,-58.4389030167283,
-43.9582833333334));
#266289=CARTESIAN_POINT('Ctrl Pts',(46.1766977413729,-57.4754524783491,
-43.89995));
#266290=CARTESIAN_POINT('Ctrl Pts',(46.1766977413729,-56.5120019399699,
-43.8416166666667));
#266291=CARTESIAN_POINT('Ctrl Pts',(45.3423250998467,-56.0302766707802,
-43.7832833333334));
#266292=CARTESIAN_POINT('Ctrl Pts',(44.5079524583205,-55.5485514015906,
-43.72495));
#266293=CARTESIAN_POINT('Ctrl Pts',(43.6735798167943,-56.0302766707802,
-43.6666166666667));
#266294=CARTESIAN_POINT('Ctrl Pts',(42.839207175268,-56.5120019399698,-43.6082833333333));
#266295=CARTESIAN_POINT('Ctrl Pts',(42.839207175268,-57.4754524783491,-43.54995));
#266296=CARTESIAN_POINT('Ctrl Pts',(42.839207175268,-58.4389030167283,-43.4916166666667));
#266297=CARTESIAN_POINT('Ctrl Pts',(43.6735798167943,-58.920628285918,-43.4332833333333));
#266298=CARTESIAN_POINT('Ctrl Pts',(44.5079524583205,-59.4023535551075,
-43.37495));
#266299=CARTESIAN_POINT('Ctrl Pts',(45.3423250998467,-58.920628285918,-43.3166166666667));
#266300=CARTESIAN_POINT('Ctrl Pts',(46.1766977413729,-58.4389030167283,
-43.2582833333333));
#266301=CARTESIAN_POINT('Ctrl Pts',(46.1766977413729,-57.4754524783491,
-43.19995));
#266302=CARTESIAN_POINT('Ctrl Pts',(46.1766977413729,-56.5120019399699,
-43.1416166666667));
#266303=CARTESIAN_POINT('Ctrl Pts',(45.3423250998467,-56.0302766707802,
-43.0832833333333));
#266304=CARTESIAN_POINT('Ctrl Pts',(44.5079524583205,-55.5485514015906,
-43.02495));
#266305=CARTESIAN_POINT('Ctrl Pts',(43.6735798167943,-56.0302766707802,
-42.9666166666667));
#266306=CARTESIAN_POINT('Ctrl Pts',(42.839207175268,-56.5120019399698,-42.9082833333333));
#266307=CARTESIAN_POINT('Ctrl Pts',(42.839207175268,-57.4754524783491,-42.84995));
#266308=CARTESIAN_POINT('Ctrl Pts',(42.839207175268,-58.4389030167283,-42.7916166666667));
#266309=CARTESIAN_POINT('Ctrl Pts',(43.6735798167943,-58.920628285918,-42.7332833333334));
#266310=CARTESIAN_POINT('Ctrl Pts',(44.5079524583205,-59.4023535551075,
-42.67495));
#266311=CARTESIAN_POINT('Ctrl Pts',(45.3423250998467,-58.920628285918,-42.6166166666667));
#266312=CARTESIAN_POINT('Ctrl Pts',(46.1766977413729,-58.4389030167283,
-42.5582833333333));
#266313=CARTESIAN_POINT('Ctrl Pts',(46.1766977413729,-57.4754524783491,
-42.49995));
#266314=CARTESIAN_POINT('Ctrl Pts',(46.1766977413729,-56.5120019399699,
-42.4416166666667));
#266315=CARTESIAN_POINT('Ctrl Pts',(45.3423250998467,-56.0302766707802,
-42.3832833333333));
#266316=CARTESIAN_POINT('Ctrl Pts',(44.5079524583205,-55.5485514015906,
-42.32495));
#266317=CARTESIAN_POINT('Ctrl Pts',(43.6735798167943,-56.0302766707802,
-42.2666166666667));
#266318=CARTESIAN_POINT('Ctrl Pts',(42.839207175268,-56.5120019399698,-42.2082833333333));
#266319=CARTESIAN_POINT('Ctrl Pts',(42.839207175268,-57.4754524783491,-42.14995));
#266320=CARTESIAN_POINT('Ctrl Pts',(42.839207175268,-58.4389030167283,-42.0916166666667));
#266321=CARTESIAN_POINT('Ctrl Pts',(43.6735798167943,-58.920628285918,-42.0332833333334));
#266322=CARTESIAN_POINT('Ctrl Pts',(44.5079524583205,-59.4023535551075,
-41.97495));
#266323=CARTESIAN_POINT('Ctrl Pts',(45.3423250998467,-58.920628285918,-41.9166166666667));
#266324=CARTESIAN_POINT('Ctrl Pts',(46.1766977413729,-58.4389030167283,
-41.8582833333333));
#266325=CARTESIAN_POINT('Ctrl Pts',(46.1766977413729,-57.4754524783491,
-41.79995));
#266326=CARTESIAN_POINT('Ctrl Pts',(46.1766977413729,-56.5120019399699,
-41.7416166666667));
#266327=CARTESIAN_POINT('Ctrl Pts',(45.3423250998467,-56.0302766707802,
-41.6832833333333));
#266328=CARTESIAN_POINT('Ctrl Pts',(44.5079524583205,-55.5485514015906,
-41.62495));
#266329=CARTESIAN_POINT('Ctrl Pts',(43.6735798167943,-56.0302766707802,
-41.5666166666667));
#266330=CARTESIAN_POINT('Ctrl Pts',(42.839207175268,-56.5120019399698,-41.5082833333334));
#266331=CARTESIAN_POINT('Ctrl Pts',(42.839207175268,-57.4754524783491,-41.44995));
#266332=CARTESIAN_POINT('Ctrl Pts',(42.839207175268,-58.4389030167283,-41.3916166666667));
#266333=CARTESIAN_POINT('Ctrl Pts',(43.6735798167943,-58.920628285918,-41.3332833333334));
#266334=CARTESIAN_POINT('Ctrl Pts',(44.5079524583205,-59.4023535551075,
-41.27495));
#266335=CARTESIAN_POINT('Ctrl Pts',(45.3423250998467,-58.920628285918,-41.2166166666667));
#266336=CARTESIAN_POINT('Ctrl Pts',(46.1766977413729,-58.4389030167283,
-41.1582833333333));
#266337=CARTESIAN_POINT('Ctrl Pts',(46.1766977413729,-57.4754524783491,
-41.09995));
#266338=CARTESIAN_POINT('Ctrl Pts',(46.1766977413729,-56.5120019399699,
-41.0416166666667));
#266339=CARTESIAN_POINT('Ctrl Pts',(45.3423250998467,-56.0302766707802,
-40.9832833333333));
#266340=CARTESIAN_POINT('Ctrl Pts',(44.5079524583205,-55.5485514015906,
-40.92495));
#266341=CARTESIAN_POINT('Ctrl Pts',(43.6735798167943,-56.0302766707802,
-40.8666166666667));
#266342=CARTESIAN_POINT('Ctrl Pts',(42.839207175268,-56.5120019399698,-40.8082833333334));
#266343=CARTESIAN_POINT('Ctrl Pts',(42.839207175268,-57.4754524783491,-40.74995));
#266344=CARTESIAN_POINT('Ctrl Pts',(42.839207175268,-58.4389030167283,-40.6916166666667));
#266345=CARTESIAN_POINT('Ctrl Pts',(43.6735798167943,-58.920628285918,-40.6332833333334));
#266346=CARTESIAN_POINT('Ctrl Pts',(44.5079524583205,-59.4023535551075,
-40.57495));
#266347=CARTESIAN_POINT('Ctrl Pts',(45.3423250998467,-58.920628285918,-40.5166166666667));
#266348=CARTESIAN_POINT('Ctrl Pts',(46.1766977413729,-58.4389030167283,
-40.4582833333333));
#266349=CARTESIAN_POINT('Ctrl Pts',(46.1766977413729,-57.4754524783491,
-40.39995));
#266350=CARTESIAN_POINT('Ctrl Pts',(46.1766977413729,-56.5120019399699,
-40.3416166666667));
#266351=CARTESIAN_POINT('Ctrl Pts',(45.3423250998467,-56.0302766707802,
-40.2832833333334));
#266352=CARTESIAN_POINT('Ctrl Pts',(44.5079524583205,-55.5485514015906,
-40.22495));
#266353=CARTESIAN_POINT('Ctrl Pts',(43.6735798167943,-56.0302766707802,
-40.1666166666667));
#266354=CARTESIAN_POINT('Ctrl Pts',(42.839207175268,-56.5120019399698,-40.1082833333334));
#266355=CARTESIAN_POINT('Ctrl Pts',(42.839207175268,-57.4754524783491,-40.04995));
#266356=CARTESIAN_POINT('Ctrl Pts',(42.839207175268,-58.4389030167283,-39.9916166666667));
#266357=CARTESIAN_POINT('Ctrl Pts',(43.6735798167943,-58.920628285918,-39.9332833333333));
#266358=CARTESIAN_POINT('Ctrl Pts',(44.5079524583205,-59.4023535551075,
-39.87495));
#266359=CARTESIAN_POINT('Ctrl Pts',(45.3423250998467,-58.920628285918,-39.8166166666667));
#266360=CARTESIAN_POINT('Ctrl Pts',(46.1766977413729,-58.4389030167283,
-39.7582833333334));
#266361=CARTESIAN_POINT('Ctrl Pts',(46.1766977413729,-57.4754524783491,
-39.69995));
#266362=CARTESIAN_POINT('Ctrl Pts',(46.1766977413729,-56.5120019399699,
-39.6416166666667));
#266363=CARTESIAN_POINT('Ctrl Pts',(45.3423250998467,-56.0302766707802,
-39.5832833333333));
#266364=CARTESIAN_POINT('Ctrl Pts',(44.5079524583205,-55.5485514015906,
-39.52495));
#266365=CARTESIAN_POINT('Ctrl Pts',(43.6735798167943,-56.0302766707802,
-39.4666166666667));
#266366=CARTESIAN_POINT('Ctrl Pts',(42.839207175268,-56.5120019399698,-39.4082833333334));
#266367=CARTESIAN_POINT('Ctrl Pts',(42.839207175268,-57.4754524783491,-39.34995));
#266368=CARTESIAN_POINT('Ctrl Pts',(42.839207175268,-58.4389030167283,-39.2916166666667));
#266369=CARTESIAN_POINT('Ctrl Pts',(43.6735798167943,-58.920628285918,-39.2332833333333));
#266370=CARTESIAN_POINT('Ctrl Pts',(44.5079524583205,-59.4023535551075,
-39.17495));
#266371=CARTESIAN_POINT('Ctrl Pts',(45.3423250998467,-58.920628285918,-39.1166166666667));
#266372=CARTESIAN_POINT('Ctrl Pts',(46.1766977413729,-58.4389030167283,
-39.0582833333334));
#266373=CARTESIAN_POINT('Ctrl Pts',(46.1766977413729,-57.4754524783491,
-38.99995));
#266374=CARTESIAN_POINT('Ctrl Pts',(46.1766977413729,-56.5120019399699,
-38.9416166666667));
#266375=CARTESIAN_POINT('Ctrl Pts',(45.3423250998467,-56.0302766707802,
-38.8832833333334));
#266376=CARTESIAN_POINT('Ctrl Pts',(44.5079524583205,-55.5485514015906,
-38.82495));
#266377=CARTESIAN_POINT('Ctrl Pts',(43.6735798167943,-56.0302766707802,
-38.7666166666667));
#266378=CARTESIAN_POINT('Ctrl Pts',(42.839207175268,-56.5120019399698,-38.7082833333334));
#266379=CARTESIAN_POINT('Ctrl Pts',(42.839207175268,-57.4754524783491,-38.64995));
#266380=CARTESIAN_POINT('Ctrl Pts',(42.839207175268,-58.4389030167283,-38.5916166666667));
#266381=CARTESIAN_POINT('Ctrl Pts',(43.6735798167943,-58.920628285918,-38.5332833333334));
#266382=CARTESIAN_POINT('Ctrl Pts',(44.5079524583205,-59.4023535551075,
-38.47495));
#266383=CARTESIAN_POINT('Ctrl Pts',(45.3423250998467,-58.920628285918,-38.4166166666667));
#266384=CARTESIAN_POINT('Ctrl Pts',(46.1766977413729,-58.4389030167283,
-38.3582833333333));
#266385=CARTESIAN_POINT('Ctrl Pts',(46.1766977413729,-57.4754524783491,
-38.29995));
#266386=CARTESIAN_POINT('Ctrl Pts',(46.1766977413729,-56.5120019399699,
-38.2416166666667));
#266387=CARTESIAN_POINT('Ctrl Pts',(45.3423250998467,-56.0302766707802,
-38.1832833333333));
#266388=CARTESIAN_POINT('Ctrl Pts',(44.5079524583205,-55.5485514015906,
-38.12495));
#266389=CARTESIAN_POINT('Ctrl Pts',(43.6735798167943,-56.0302766707802,
-38.0666166666667));
#266390=CARTESIAN_POINT('Ctrl Pts',(42.839207175268,-56.5120019399698,-38.0082833333333));
#266391=CARTESIAN_POINT('Ctrl Pts',(42.839207175268,-57.4754524783491,-37.94995));
#266392=CARTESIAN_POINT('Ctrl Pts',(42.839207175268,-58.4389030167283,-37.8916166666667));
#266393=CARTESIAN_POINT('Ctrl Pts',(43.6735798167943,-58.920628285918,-37.8332833333334));
#266394=CARTESIAN_POINT('Ctrl Pts',(44.5079524583205,-59.4023535551075,
-37.77495));
#266395=CARTESIAN_POINT('Ctrl Pts',(45.3423250998467,-58.920628285918,-37.7166166666667));
#266396=CARTESIAN_POINT('Ctrl Pts',(46.1766977413729,-58.4389030167283,
-37.6582833333333));
#266397=CARTESIAN_POINT('Ctrl Pts',(46.1766977413729,-57.4754524783491,
-37.59995));
#266398=CARTESIAN_POINT('Ctrl Pts',(46.1766977413729,-56.5120019399699,
-37.5416166666667));
#266399=CARTESIAN_POINT('Ctrl Pts',(45.3423250998467,-56.0302766707802,
-37.4832833333334));
#266400=CARTESIAN_POINT('Ctrl Pts',(44.5079524583205,-55.5485514015906,
-37.42495));
#266401=CARTESIAN_POINT('Ctrl Pts',(43.6735798167943,-56.0302766707802,
-37.3666166666667));
#266402=CARTESIAN_POINT('Ctrl Pts',(42.839207175268,-56.5120019399698,-37.3082833333333));
#266403=CARTESIAN_POINT('Ctrl Pts',(42.839207175268,-57.4754524783491,-37.24995));
#266404=CARTESIAN_POINT('Ctrl Pts',(42.839207175268,-58.4389030167283,-37.1916166666667));
#266405=CARTESIAN_POINT('Ctrl Pts',(43.6735798167943,-58.920628285918,-37.1332833333334));
#266406=CARTESIAN_POINT('Ctrl Pts',(44.5079524583205,-59.4023535551075,
-37.07495));
#266407=CARTESIAN_POINT('Ctrl Pts',(45.3423250998467,-58.920628285918,-37.0166166666667));
#266408=CARTESIAN_POINT('Ctrl Pts',(45.4506530446707,-58.8580851178131,
-37.0090431559831));
#266409=CARTESIAN_POINT('Ctrl Pts',(45.5484465834733,-58.7800914304091,
-37.0009024189827));
#266410=CARTESIAN_POINT('Ctrl Pts',(46.5766932247459,-57.4754524783491,
-53.2308875));
#266411=CARTESIAN_POINT('Ctrl Pts',(46.5766932247459,-56.2810644399698,
-53.1725541666667));
#266412=CARTESIAN_POINT('Ctrl Pts',(45.5423228415332,-55.6838704207802,
-53.1142208333334));
#266413=CARTESIAN_POINT('Ctrl Pts',(44.5079524583205,-55.0866764015906,
-53.0558875000001));
#266414=CARTESIAN_POINT('Ctrl Pts',(43.4735820751078,-55.6838704207802,
-52.9975541666667));
#266415=CARTESIAN_POINT('Ctrl Pts',(42.4392116918951,-56.2810644399698,
-52.9392208333334));
#266416=CARTESIAN_POINT('Ctrl Pts',(42.439211691895,-57.4754524783491,-52.8808875));
#266417=CARTESIAN_POINT('Ctrl Pts',(42.4392116918951,-58.6698405167284,
-52.8225541666667));
#266418=CARTESIAN_POINT('Ctrl Pts',(43.4735820751078,-59.267034535918,-52.7642208333334));
#266419=CARTESIAN_POINT('Ctrl Pts',(44.5079524583205,-59.8642285551076,
-52.7058875));
#266420=CARTESIAN_POINT('Ctrl Pts',(45.5423228415332,-59.267034535918,-52.6475541666667));
#266421=CARTESIAN_POINT('Ctrl Pts',(46.5766932247459,-58.6698405167284,
-52.5892208333333));
#266422=CARTESIAN_POINT('Ctrl Pts',(46.5766932247459,-57.4754524783491,
-52.5308875));
#266423=CARTESIAN_POINT('Ctrl Pts',(46.5766932247459,-56.2810644399698,
-52.4725541666667));
#266424=CARTESIAN_POINT('Ctrl Pts',(45.5423228415332,-55.6838704207802,
-52.4142208333334));
#266425=CARTESIAN_POINT('Ctrl Pts',(44.5079524583205,-55.0866764015906,
-52.3558875000001));
#266426=CARTESIAN_POINT('Ctrl Pts',(43.4735820751078,-55.6838704207802,
-52.2975541666667));
#266427=CARTESIAN_POINT('Ctrl Pts',(42.4392116918951,-56.2810644399698,
-52.2392208333334));
#266428=CARTESIAN_POINT('Ctrl Pts',(42.439211691895,-57.4754524783491,-52.1808875));
#266429=CARTESIAN_POINT('Ctrl Pts',(42.4392116918951,-58.6698405167284,
-52.1225541666667));
#266430=CARTESIAN_POINT('Ctrl Pts',(43.4735820751078,-59.267034535918,-52.0642208333334));
#266431=CARTESIAN_POINT('Ctrl Pts',(44.5079524583205,-59.8642285551076,
-52.0058875));
#266432=CARTESIAN_POINT('Ctrl Pts',(45.5423228415332,-59.267034535918,-51.9475541666667));
#266433=CARTESIAN_POINT('Ctrl Pts',(46.5766932247459,-58.6698405167284,
-51.8892208333334));
#266434=CARTESIAN_POINT('Ctrl Pts',(46.5766932247459,-57.4754524783491,
-51.8308875));
#266435=CARTESIAN_POINT('Ctrl Pts',(46.5766932247459,-56.2810644399698,
-51.7725541666667));
#266436=CARTESIAN_POINT('Ctrl Pts',(45.5423228415332,-55.6838704207802,
-51.7142208333334));
#266437=CARTESIAN_POINT('Ctrl Pts',(44.5079524583205,-55.0866764015906,
-51.6558875));
#266438=CARTESIAN_POINT('Ctrl Pts',(43.4735820751078,-55.6838704207802,
-51.5975541666667));
#266439=CARTESIAN_POINT('Ctrl Pts',(42.4392116918951,-56.2810644399698,
-51.5392208333333));
#266440=CARTESIAN_POINT('Ctrl Pts',(42.439211691895,-57.4754524783491,-51.4808875));
#266441=CARTESIAN_POINT('Ctrl Pts',(42.4392116918951,-58.6698405167284,
-51.4225541666667));
#266442=CARTESIAN_POINT('Ctrl Pts',(43.4735820751078,-59.267034535918,-51.3642208333334));
#266443=CARTESIAN_POINT('Ctrl Pts',(44.5079524583205,-59.8642285551076,
-51.3058875));
#266444=CARTESIAN_POINT('Ctrl Pts',(45.5423228415332,-59.267034535918,-51.2475541666667));
#266445=CARTESIAN_POINT('Ctrl Pts',(46.5766932247459,-58.6698405167284,
-51.1892208333334));
#266446=CARTESIAN_POINT('Ctrl Pts',(46.5766932247459,-57.4754524783491,
-51.1308875));
#266447=CARTESIAN_POINT('Ctrl Pts',(46.5766932247459,-56.2810644399698,
-51.0725541666667));
#266448=CARTESIAN_POINT('Ctrl Pts',(45.5423228415332,-55.6838704207802,
-51.0142208333334));
#266449=CARTESIAN_POINT('Ctrl Pts',(44.5079524583205,-55.0866764015906,
-50.9558875));
#266450=CARTESIAN_POINT('Ctrl Pts',(43.4735820751078,-55.6838704207802,
-50.8975541666667));
#266451=CARTESIAN_POINT('Ctrl Pts',(42.4392116918951,-56.2810644399698,
-50.8392208333333));
#266452=CARTESIAN_POINT('Ctrl Pts',(42.439211691895,-57.4754524783491,-50.7808875));
#266453=CARTESIAN_POINT('Ctrl Pts',(42.4392116918951,-58.6698405167284,
-50.7225541666667));
#266454=CARTESIAN_POINT('Ctrl Pts',(43.4735820751078,-59.267034535918,-50.6642208333333));
#266455=CARTESIAN_POINT('Ctrl Pts',(44.5079524583205,-59.8642285551076,
-50.6058875));
#266456=CARTESIAN_POINT('Ctrl Pts',(45.5423228415332,-59.267034535918,-50.5475541666667));
#266457=CARTESIAN_POINT('Ctrl Pts',(46.5766932247459,-58.6698405167284,
-50.4892208333333));
#266458=CARTESIAN_POINT('Ctrl Pts',(46.5766932247459,-57.4754524783491,
-50.4308875));
#266459=CARTESIAN_POINT('Ctrl Pts',(46.5766932247459,-56.2810644399698,
-50.3725541666667));
#266460=CARTESIAN_POINT('Ctrl Pts',(45.5423228415332,-55.6838704207802,
-50.3142208333334));
#266461=CARTESIAN_POINT('Ctrl Pts',(44.5079524583205,-55.0866764015906,
-50.2558875));
#266462=CARTESIAN_POINT('Ctrl Pts',(43.4735820751078,-55.6838704207802,
-50.1975541666667));
#266463=CARTESIAN_POINT('Ctrl Pts',(42.4392116918951,-56.2810644399698,
-50.1392208333333));
#266464=CARTESIAN_POINT('Ctrl Pts',(42.439211691895,-57.4754524783491,-50.0808875));
#266465=CARTESIAN_POINT('Ctrl Pts',(42.4392116918951,-58.6698405167284,
-50.0225541666667));
#266466=CARTESIAN_POINT('Ctrl Pts',(43.4735820751078,-59.267034535918,-49.9642208333334));
#266467=CARTESIAN_POINT('Ctrl Pts',(44.5079524583205,-59.8642285551076,
-49.9058875));
#266468=CARTESIAN_POINT('Ctrl Pts',(45.5423228415332,-59.267034535918,-49.8475541666667));
#266469=CARTESIAN_POINT('Ctrl Pts',(46.5766932247459,-58.6698405167284,
-49.7892208333333));
#266470=CARTESIAN_POINT('Ctrl Pts',(46.5766932247459,-57.4754524783491,
-49.7308875));
#266471=CARTESIAN_POINT('Ctrl Pts',(46.5766932247459,-56.2810644399698,
-49.6725541666667));
#266472=CARTESIAN_POINT('Ctrl Pts',(45.5423228415332,-55.6838704207802,
-49.6142208333334));
#266473=CARTESIAN_POINT('Ctrl Pts',(44.5079524583205,-55.0866764015906,
-49.5558875));
#266474=CARTESIAN_POINT('Ctrl Pts',(43.4735820751078,-55.6838704207802,
-49.4975541666667));
#266475=CARTESIAN_POINT('Ctrl Pts',(42.4392116918951,-56.2810644399698,
-49.4392208333333));
#266476=CARTESIAN_POINT('Ctrl Pts',(42.439211691895,-57.4754524783491,-49.3808875));
#266477=CARTESIAN_POINT('Ctrl Pts',(42.4392116918951,-58.6698405167284,
-49.3225541666667));
#266478=CARTESIAN_POINT('Ctrl Pts',(43.4735820751078,-59.267034535918,-49.2642208333334));
#266479=CARTESIAN_POINT('Ctrl Pts',(44.5079524583205,-59.8642285551076,
-49.2058875));
#266480=CARTESIAN_POINT('Ctrl Pts',(45.5423228415332,-59.267034535918,-49.1475541666667));
#266481=CARTESIAN_POINT('Ctrl Pts',(46.5766932247459,-58.6698405167284,
-49.0892208333333));
#266482=CARTESIAN_POINT('Ctrl Pts',(46.5766932247459,-57.4754524783491,
-49.0308875));
#266483=CARTESIAN_POINT('Ctrl Pts',(46.5766932247459,-56.2810644399698,
-48.9725541666667));
#266484=CARTESIAN_POINT('Ctrl Pts',(45.5423228415332,-55.6838704207802,
-48.9142208333334));
#266485=CARTESIAN_POINT('Ctrl Pts',(44.5079524583205,-55.0866764015906,
-48.8558875));
#266486=CARTESIAN_POINT('Ctrl Pts',(43.4735820751078,-55.6838704207802,
-48.7975541666667));
#266487=CARTESIAN_POINT('Ctrl Pts',(42.4392116918951,-56.2810644399698,
-48.7392208333334));
#266488=CARTESIAN_POINT('Ctrl Pts',(42.439211691895,-57.4754524783491,-48.6808875));
#266489=CARTESIAN_POINT('Ctrl Pts',(42.4392116918951,-58.6698405167284,
-48.6225541666667));
#266490=CARTESIAN_POINT('Ctrl Pts',(43.4735820751078,-59.267034535918,-48.5642208333334));
#266491=CARTESIAN_POINT('Ctrl Pts',(44.5079524583205,-59.8642285551076,
-48.5058875));
#266492=CARTESIAN_POINT('Ctrl Pts',(45.5423228415332,-59.267034535918,-48.4475541666667));
#266493=CARTESIAN_POINT('Ctrl Pts',(46.5766932247459,-58.6698405167284,
-48.3892208333334));
#266494=CARTESIAN_POINT('Ctrl Pts',(46.5766932247459,-57.4754524783491,
-48.3308875));
#266495=CARTESIAN_POINT('Ctrl Pts',(46.5766932247459,-56.2810644399698,
-48.2725541666667));
#266496=CARTESIAN_POINT('Ctrl Pts',(45.5423228415332,-55.6838704207802,
-48.2142208333334));
#266497=CARTESIAN_POINT('Ctrl Pts',(44.5079524583205,-55.0866764015906,
-48.1558875));
#266498=CARTESIAN_POINT('Ctrl Pts',(43.4735820751078,-55.6838704207802,
-48.0975541666667));
#266499=CARTESIAN_POINT('Ctrl Pts',(42.4392116918951,-56.2810644399698,
-48.0392208333334));
#266500=CARTESIAN_POINT('Ctrl Pts',(42.439211691895,-57.4754524783491,-47.9808875));
#266501=CARTESIAN_POINT('Ctrl Pts',(42.4392116918951,-58.6698405167284,
-47.9225541666667));
#266502=CARTESIAN_POINT('Ctrl Pts',(43.4735820751078,-59.267034535918,-47.8642208333334));
#266503=CARTESIAN_POINT('Ctrl Pts',(44.5079524583205,-59.8642285551076,
-47.8058875000001));
#266504=CARTESIAN_POINT('Ctrl Pts',(45.5423228415332,-59.267034535918,-47.7475541666667));
#266505=CARTESIAN_POINT('Ctrl Pts',(46.5766932247459,-58.6698405167284,
-47.6892208333334));
#266506=CARTESIAN_POINT('Ctrl Pts',(46.5766932247459,-57.4754524783491,
-47.6308875));
#266507=CARTESIAN_POINT('Ctrl Pts',(46.5766932247459,-56.2810644399698,
-47.5725541666667));
#266508=CARTESIAN_POINT('Ctrl Pts',(45.5423228415332,-55.6838704207802,
-47.5142208333333));
#266509=CARTESIAN_POINT('Ctrl Pts',(44.5079524583205,-55.0866764015906,
-47.4558875));
#266510=CARTESIAN_POINT('Ctrl Pts',(43.4735820751078,-55.6838704207802,
-47.3975541666667));
#266511=CARTESIAN_POINT('Ctrl Pts',(42.4392116918951,-56.2810644399698,
-47.3392208333334));
#266512=CARTESIAN_POINT('Ctrl Pts',(42.439211691895,-57.4754524783491,-47.2808875));
#266513=CARTESIAN_POINT('Ctrl Pts',(42.4392116918951,-58.6698405167284,
-47.2225541666667));
#266514=CARTESIAN_POINT('Ctrl Pts',(43.4735820751078,-59.267034535918,-47.1642208333334));
#266515=CARTESIAN_POINT('Ctrl Pts',(44.5079524583205,-59.8642285551076,
-47.1058875));
#266516=CARTESIAN_POINT('Ctrl Pts',(45.5423228415332,-59.267034535918,-47.0475541666667));
#266517=CARTESIAN_POINT('Ctrl Pts',(46.5766932247459,-58.6698405167284,
-46.9892208333334));
#266518=CARTESIAN_POINT('Ctrl Pts',(46.5766932247459,-57.4754524783491,
-46.9308875));
#266519=CARTESIAN_POINT('Ctrl Pts',(46.5766932247459,-56.2810644399698,
-46.8725541666667));
#266520=CARTESIAN_POINT('Ctrl Pts',(45.5423228415332,-55.6838704207802,
-46.8142208333334));
#266521=CARTESIAN_POINT('Ctrl Pts',(44.5079524583205,-55.0866764015906,
-46.7558875));
#266522=CARTESIAN_POINT('Ctrl Pts',(43.4735820751078,-55.6838704207802,
-46.6975541666667));
#266523=CARTESIAN_POINT('Ctrl Pts',(42.4392116918951,-56.2810644399698,
-46.6392208333334));
#266524=CARTESIAN_POINT('Ctrl Pts',(42.439211691895,-57.4754524783491,-46.5808875));
#266525=CARTESIAN_POINT('Ctrl Pts',(42.4392116918951,-58.6698405167284,
-46.5225541666667));
#266526=CARTESIAN_POINT('Ctrl Pts',(43.4735820751078,-59.267034535918,-46.4642208333334));
#266527=CARTESIAN_POINT('Ctrl Pts',(44.5079524583205,-59.8642285551076,
-46.4058875));
#266528=CARTESIAN_POINT('Ctrl Pts',(45.5423228415332,-59.267034535918,-46.3475541666667));
#266529=CARTESIAN_POINT('Ctrl Pts',(46.5766932247459,-58.6698405167284,
-46.2892208333334));
#266530=CARTESIAN_POINT('Ctrl Pts',(46.5766932247459,-57.4754524783491,
-46.2308875));
#266531=CARTESIAN_POINT('Ctrl Pts',(46.5766932247459,-56.2810644399698,
-46.1725541666667));
#266532=CARTESIAN_POINT('Ctrl Pts',(45.5423228415332,-55.6838704207802,
-46.1142208333334));
#266533=CARTESIAN_POINT('Ctrl Pts',(44.5079524583205,-55.0866764015906,
-46.0558875));
#266534=CARTESIAN_POINT('Ctrl Pts',(43.4735820751078,-55.6838704207802,
-45.9975541666667));
#266535=CARTESIAN_POINT('Ctrl Pts',(42.4392116918951,-56.2810644399698,
-45.9392208333333));
#266536=CARTESIAN_POINT('Ctrl Pts',(42.439211691895,-57.4754524783491,-45.8808875));
#266537=CARTESIAN_POINT('Ctrl Pts',(42.4392116918951,-58.6698405167284,
-45.8225541666667));
#266538=CARTESIAN_POINT('Ctrl Pts',(43.4735820751078,-59.267034535918,-45.7642208333334));
#266539=CARTESIAN_POINT('Ctrl Pts',(44.5079524583205,-59.8642285551076,
-45.7058875));
#266540=CARTESIAN_POINT('Ctrl Pts',(45.5423228415332,-59.267034535918,-45.6475541666667));
#266541=CARTESIAN_POINT('Ctrl Pts',(46.5766932247459,-58.6698405167284,
-45.5892208333334));
#266542=CARTESIAN_POINT('Ctrl Pts',(46.5766932247459,-57.4754524783491,
-45.5308875));
#266543=CARTESIAN_POINT('Ctrl Pts',(46.5766932247459,-56.2810644399698,
-45.4725541666667));
#266544=CARTESIAN_POINT('Ctrl Pts',(45.5423228415332,-55.6838704207802,
-45.4142208333334));
#266545=CARTESIAN_POINT('Ctrl Pts',(44.5079524583205,-55.0866764015906,
-45.3558875));
#266546=CARTESIAN_POINT('Ctrl Pts',(43.4735820751078,-55.6838704207802,
-45.2975541666667));
#266547=CARTESIAN_POINT('Ctrl Pts',(42.4392116918951,-56.2810644399698,
-45.2392208333333));
#266548=CARTESIAN_POINT('Ctrl Pts',(42.439211691895,-57.4754524783491,-45.1808875));
#266549=CARTESIAN_POINT('Ctrl Pts',(42.4392116918951,-58.6698405167284,
-45.1225541666667));
#266550=CARTESIAN_POINT('Ctrl Pts',(43.4735820751078,-59.267034535918,-45.0642208333334));
#266551=CARTESIAN_POINT('Ctrl Pts',(44.5079524583205,-59.8642285551076,
-45.0058875));
#266552=CARTESIAN_POINT('Ctrl Pts',(45.5423228415332,-59.267034535918,-44.9475541666667));
#266553=CARTESIAN_POINT('Ctrl Pts',(46.5766932247459,-58.6698405167284,
-44.8892208333333));
#266554=CARTESIAN_POINT('Ctrl Pts',(46.5766932247459,-57.4754524783491,
-44.8308875));
#266555=CARTESIAN_POINT('Ctrl Pts',(46.5766932247459,-56.2810644399698,
-44.7725541666667));
#266556=CARTESIAN_POINT('Ctrl Pts',(45.5423228415332,-55.6838704207802,
-44.7142208333334));
#266557=CARTESIAN_POINT('Ctrl Pts',(44.5079524583205,-55.0866764015906,
-44.6558875));
#266558=CARTESIAN_POINT('Ctrl Pts',(43.4735820751078,-55.6838704207802,
-44.5975541666667));
#266559=CARTESIAN_POINT('Ctrl Pts',(42.4392116918951,-56.2810644399698,
-44.5392208333333));
#266560=CARTESIAN_POINT('Ctrl Pts',(42.439211691895,-57.4754524783491,-44.4808875000001));
#266561=CARTESIAN_POINT('Ctrl Pts',(42.4392116918951,-58.6698405167284,
-44.4225541666667));
#266562=CARTESIAN_POINT('Ctrl Pts',(43.4735820751078,-59.267034535918,-44.3642208333333));
#266563=CARTESIAN_POINT('Ctrl Pts',(44.5079524583205,-59.8642285551076,
-44.3058875));
#266564=CARTESIAN_POINT('Ctrl Pts',(45.5423228415332,-59.267034535918,-44.2475541666667));
#266565=CARTESIAN_POINT('Ctrl Pts',(46.5766932247459,-58.6698405167284,
-44.1892208333334));
#266566=CARTESIAN_POINT('Ctrl Pts',(46.5766932247459,-57.4754524783491,
-44.1308875000001));
#266567=CARTESIAN_POINT('Ctrl Pts',(46.5766932247459,-56.2810644399698,
-44.0725541666667));
#266568=CARTESIAN_POINT('Ctrl Pts',(45.5423228415332,-55.6838704207802,
-44.0142208333334));
#266569=CARTESIAN_POINT('Ctrl Pts',(44.5079524583205,-55.0866764015906,
-43.9558875));
#266570=CARTESIAN_POINT('Ctrl Pts',(43.4735820751078,-55.6838704207802,
-43.8975541666667));
#266571=CARTESIAN_POINT('Ctrl Pts',(42.4392116918951,-56.2810644399698,
-43.8392208333333));
#266572=CARTESIAN_POINT('Ctrl Pts',(42.439211691895,-57.4754524783491,-43.7808875));
#266573=CARTESIAN_POINT('Ctrl Pts',(42.4392116918951,-58.6698405167284,
-43.7225541666667));
#266574=CARTESIAN_POINT('Ctrl Pts',(43.4735820751078,-59.267034535918,-43.6642208333334));
#266575=CARTESIAN_POINT('Ctrl Pts',(44.5079524583205,-59.8642285551076,
-43.6058875));
#266576=CARTESIAN_POINT('Ctrl Pts',(45.5423228415332,-59.267034535918,-43.5475541666667));
#266577=CARTESIAN_POINT('Ctrl Pts',(46.5766932247459,-58.6698405167284,
-43.4892208333333));
#266578=CARTESIAN_POINT('Ctrl Pts',(46.5766932247459,-57.4754524783491,
-43.4308875));
#266579=CARTESIAN_POINT('Ctrl Pts',(46.5766932247459,-56.2810644399698,
-43.3725541666667));
#266580=CARTESIAN_POINT('Ctrl Pts',(45.5423228415332,-55.6838704207802,
-43.3142208333334));
#266581=CARTESIAN_POINT('Ctrl Pts',(44.5079524583205,-55.0866764015906,
-43.2558875));
#266582=CARTESIAN_POINT('Ctrl Pts',(43.4735820751078,-55.6838704207802,
-43.1975541666667));
#266583=CARTESIAN_POINT('Ctrl Pts',(42.4392116918951,-56.2810644399698,
-43.1392208333334));
#266584=CARTESIAN_POINT('Ctrl Pts',(42.439211691895,-57.4754524783491,-43.0808875));
#266585=CARTESIAN_POINT('Ctrl Pts',(42.4392116918951,-58.6698405167284,
-43.0225541666667));
#266586=CARTESIAN_POINT('Ctrl Pts',(43.4735820751078,-59.267034535918,-42.9642208333334));
#266587=CARTESIAN_POINT('Ctrl Pts',(44.5079524583205,-59.8642285551076,
-42.9058875));
#266588=CARTESIAN_POINT('Ctrl Pts',(45.5423228415332,-59.267034535918,-42.8475541666667));
#266589=CARTESIAN_POINT('Ctrl Pts',(46.5766932247459,-58.6698405167284,
-42.7892208333334));
#266590=CARTESIAN_POINT('Ctrl Pts',(46.5766932247459,-57.4754524783491,
-42.7308875000001));
#266591=CARTESIAN_POINT('Ctrl Pts',(46.5766932247459,-56.2810644399698,
-42.6725541666667));
#266592=CARTESIAN_POINT('Ctrl Pts',(45.5423228415332,-55.6838704207802,
-42.6142208333334));
#266593=CARTESIAN_POINT('Ctrl Pts',(44.5079524583205,-55.0866764015906,
-42.5558875));
#266594=CARTESIAN_POINT('Ctrl Pts',(43.4735820751078,-55.6838704207802,
-42.4975541666667));
#266595=CARTESIAN_POINT('Ctrl Pts',(42.4392116918951,-56.2810644399698,
-42.4392208333334));
#266596=CARTESIAN_POINT('Ctrl Pts',(42.439211691895,-57.4754524783491,-42.3808875000001));
#266597=CARTESIAN_POINT('Ctrl Pts',(42.4392116918951,-58.6698405167284,
-42.3225541666667));
#266598=CARTESIAN_POINT('Ctrl Pts',(43.4735820751078,-59.267034535918,-42.2642208333334));
#266599=CARTESIAN_POINT('Ctrl Pts',(44.5079524583205,-59.8642285551076,
-42.2058875));
#266600=CARTESIAN_POINT('Ctrl Pts',(45.5423228415332,-59.267034535918,-42.1475541666667));
#266601=CARTESIAN_POINT('Ctrl Pts',(46.5766932247459,-58.6698405167284,
-42.0892208333334));
#266602=CARTESIAN_POINT('Ctrl Pts',(46.5766932247459,-57.4754524783491,
-42.0308875000001));
#266603=CARTESIAN_POINT('Ctrl Pts',(46.5766932247459,-56.2810644399698,
-41.9725541666667));
#266604=CARTESIAN_POINT('Ctrl Pts',(45.5423228415332,-55.6838704207802,
-41.9142208333334));
#266605=CARTESIAN_POINT('Ctrl Pts',(44.5079524583205,-55.0866764015906,
-41.8558875));
#266606=CARTESIAN_POINT('Ctrl Pts',(43.4735820751078,-55.6838704207802,
-41.7975541666667));
#266607=CARTESIAN_POINT('Ctrl Pts',(42.4392116918951,-56.2810644399698,
-41.7392208333334));
#266608=CARTESIAN_POINT('Ctrl Pts',(42.439211691895,-57.4754524783491,-41.6808875000001));
#266609=CARTESIAN_POINT('Ctrl Pts',(42.4392116918951,-58.6698405167284,
-41.6225541666667));
#266610=CARTESIAN_POINT('Ctrl Pts',(43.4735820751078,-59.267034535918,-41.5642208333334));
#266611=CARTESIAN_POINT('Ctrl Pts',(44.5079524583205,-59.8642285551076,
-41.5058875));
#266612=CARTESIAN_POINT('Ctrl Pts',(45.5423228415332,-59.267034535918,-41.4475541666667));
#266613=CARTESIAN_POINT('Ctrl Pts',(46.5766932247459,-58.6698405167284,
-41.3892208333334));
#266614=CARTESIAN_POINT('Ctrl Pts',(46.5766932247459,-57.4754524783491,
-41.3308875000001));
#266615=CARTESIAN_POINT('Ctrl Pts',(46.5766932247459,-56.2810644399698,
-41.2725541666667));
#266616=CARTESIAN_POINT('Ctrl Pts',(45.5423228415332,-55.6838704207802,
-41.2142208333333));
#266617=CARTESIAN_POINT('Ctrl Pts',(44.5079524583205,-55.0866764015906,
-41.1558875));
#266618=CARTESIAN_POINT('Ctrl Pts',(43.4735820751078,-55.6838704207802,
-41.0975541666667));
#266619=CARTESIAN_POINT('Ctrl Pts',(42.4392116918951,-56.2810644399698,
-41.0392208333333));
#266620=CARTESIAN_POINT('Ctrl Pts',(42.439211691895,-57.4754524783491,-40.9808875000001));
#266621=CARTESIAN_POINT('Ctrl Pts',(42.4392116918951,-58.6698405167284,
-40.9225541666667));
#266622=CARTESIAN_POINT('Ctrl Pts',(43.4735820751078,-59.267034535918,-40.8642208333334));
#266623=CARTESIAN_POINT('Ctrl Pts',(44.5079524583205,-59.8642285551076,
-40.8058875));
#266624=CARTESIAN_POINT('Ctrl Pts',(45.5423228415332,-59.267034535918,-40.7475541666667));
#266625=CARTESIAN_POINT('Ctrl Pts',(46.5766932247459,-58.6698405167284,
-40.6892208333333));
#266626=CARTESIAN_POINT('Ctrl Pts',(46.5766932247459,-57.4754524783491,
-40.6308875));
#266627=CARTESIAN_POINT('Ctrl Pts',(46.5766932247459,-56.2810644399698,
-40.5725541666667));
#266628=CARTESIAN_POINT('Ctrl Pts',(45.5423228415332,-55.6838704207802,
-40.5142208333333));
#266629=CARTESIAN_POINT('Ctrl Pts',(44.5079524583205,-55.0866764015906,
-40.4558875));
#266630=CARTESIAN_POINT('Ctrl Pts',(43.4735820751078,-55.6838704207802,
-40.3975541666667));
#266631=CARTESIAN_POINT('Ctrl Pts',(42.4392116918951,-56.2810644399698,
-40.3392208333333));
#266632=CARTESIAN_POINT('Ctrl Pts',(42.439211691895,-57.4754524783491,-40.2808875));
#266633=CARTESIAN_POINT('Ctrl Pts',(42.4392116918951,-58.6698405167284,
-40.2225541666667));
#266634=CARTESIAN_POINT('Ctrl Pts',(43.4735820751078,-59.267034535918,-40.1642208333333));
#266635=CARTESIAN_POINT('Ctrl Pts',(44.5079524583205,-59.8642285551076,
-40.1058875));
#266636=CARTESIAN_POINT('Ctrl Pts',(45.5423228415332,-59.267034535918,-40.0475541666667));
#266637=CARTESIAN_POINT('Ctrl Pts',(46.5766932247459,-58.6698405167284,
-39.9892208333333));
#266638=CARTESIAN_POINT('Ctrl Pts',(46.5766932247459,-57.4754524783491,
-39.9308875));
#266639=CARTESIAN_POINT('Ctrl Pts',(46.5766932247459,-56.2810644399698,
-39.8725541666667));
#266640=CARTESIAN_POINT('Ctrl Pts',(45.5423228415332,-55.6838704207802,
-39.8142208333334));
#266641=CARTESIAN_POINT('Ctrl Pts',(44.5079524583205,-55.0866764015906,
-39.7558875));
#266642=CARTESIAN_POINT('Ctrl Pts',(43.4735820751078,-55.6838704207802,
-39.6975541666667));
#266643=CARTESIAN_POINT('Ctrl Pts',(42.4392116918951,-56.2810644399698,
-39.6392208333334));
#266644=CARTESIAN_POINT('Ctrl Pts',(42.439211691895,-57.4754524783491,-39.5808875000001));
#266645=CARTESIAN_POINT('Ctrl Pts',(42.4392116918951,-58.6698405167284,
-39.5225541666667));
#266646=CARTESIAN_POINT('Ctrl Pts',(43.4735820751078,-59.267034535918,-39.4642208333333));
#266647=CARTESIAN_POINT('Ctrl Pts',(44.5079524583205,-59.8642285551076,
-39.4058875));
#266648=CARTESIAN_POINT('Ctrl Pts',(45.5423228415332,-59.267034535918,-39.3475541666667));
#266649=CARTESIAN_POINT('Ctrl Pts',(46.5766932247459,-58.6698405167284,
-39.2892208333334));
#266650=CARTESIAN_POINT('Ctrl Pts',(46.5766932247459,-57.4754524783491,
-39.2308875));
#266651=CARTESIAN_POINT('Ctrl Pts',(46.5766932247459,-56.2810644399698,
-39.1725541666667));
#266652=CARTESIAN_POINT('Ctrl Pts',(45.5423228415332,-55.6838704207802,
-39.1142208333333));
#266653=CARTESIAN_POINT('Ctrl Pts',(44.5079524583205,-55.0866764015906,
-39.0558875));
#266654=CARTESIAN_POINT('Ctrl Pts',(43.4735820751078,-55.6838704207802,
-38.9975541666667));
#266655=CARTESIAN_POINT('Ctrl Pts',(42.4392116918951,-56.2810644399698,
-38.9392208333334));
#266656=CARTESIAN_POINT('Ctrl Pts',(42.439211691895,-57.4754524783491,-38.8808875));
#266657=CARTESIAN_POINT('Ctrl Pts',(42.4392116918951,-58.6698405167284,
-38.8225541666667));
#266658=CARTESIAN_POINT('Ctrl Pts',(43.4735820751078,-59.267034535918,-38.7642208333333));
#266659=CARTESIAN_POINT('Ctrl Pts',(44.5079524583205,-59.8642285551076,
-38.7058875));
#266660=CARTESIAN_POINT('Ctrl Pts',(45.5423228415332,-59.267034535918,-38.6475541666667));
#266661=CARTESIAN_POINT('Ctrl Pts',(46.5766932247459,-58.6698405167284,
-38.5892208333334));
#266662=CARTESIAN_POINT('Ctrl Pts',(46.5766932247459,-57.4754524783491,
-38.5308875));
#266663=CARTESIAN_POINT('Ctrl Pts',(46.5766932247459,-56.2810644399698,
-38.4725541666667));
#266664=CARTESIAN_POINT('Ctrl Pts',(45.5423228415332,-55.6838704207802,
-38.4142208333334));
#266665=CARTESIAN_POINT('Ctrl Pts',(44.5079524583205,-55.0866764015906,
-38.3558875));
#266666=CARTESIAN_POINT('Ctrl Pts',(43.4735820751078,-55.6838704207802,
-38.2975541666667));
#266667=CARTESIAN_POINT('Ctrl Pts',(42.4392116918951,-56.2810644399698,
-38.2392208333333));
#266668=CARTESIAN_POINT('Ctrl Pts',(42.439211691895,-57.4754524783491,-38.1808875000001));
#266669=CARTESIAN_POINT('Ctrl Pts',(42.4392116918951,-58.6698405167284,
-38.1225541666667));
#266670=CARTESIAN_POINT('Ctrl Pts',(43.4735820751078,-59.267034535918,-38.0642208333334));
#266671=CARTESIAN_POINT('Ctrl Pts',(44.5079524583205,-59.8642285551076,
-38.0058875));
#266672=CARTESIAN_POINT('Ctrl Pts',(45.5423228415332,-59.267034535918,-37.9475541666667));
#266673=CARTESIAN_POINT('Ctrl Pts',(46.5766932247459,-58.6698405167284,
-37.8892208333334));
#266674=CARTESIAN_POINT('Ctrl Pts',(46.5766932247459,-57.4754524783491,
-37.8308875));
#266675=CARTESIAN_POINT('Ctrl Pts',(46.5766932247459,-56.2810644399698,
-37.7725541666667));
#266676=CARTESIAN_POINT('Ctrl Pts',(45.5423228415332,-55.6838704207802,
-37.7142208333333));
#266677=CARTESIAN_POINT('Ctrl Pts',(44.5079524583205,-55.0866764015906,
-37.6558875));
#266678=CARTESIAN_POINT('Ctrl Pts',(43.4735820751078,-55.6838704207802,
-37.5975541666667));
#266679=CARTESIAN_POINT('Ctrl Pts',(42.4392116918951,-56.2810644399698,
-37.5392208333334));
#266680=CARTESIAN_POINT('Ctrl Pts',(42.439211691895,-57.4754524783491,-37.4808875));
#266681=CARTESIAN_POINT('Ctrl Pts',(42.4392116918951,-58.6698405167284,
-37.4225541666667));
#266682=CARTESIAN_POINT('Ctrl Pts',(43.4735820751078,-59.267034535918,-37.3642208333333));
#266683=CARTESIAN_POINT('Ctrl Pts',(44.5079524583205,-59.8642285551076,
-37.3058875));
#266684=CARTESIAN_POINT('Ctrl Pts',(45.5423228415332,-59.267034535918,-37.2475541666667));
#266685=CARTESIAN_POINT('Ctrl Pts',(45.6766168155006,-59.1894998738974,
-37.239980655983));
#266686=CARTESIAN_POINT('Ctrl Pts',(45.7978513037526,-59.0928112286649,
-37.2318399189827));
#266687=CARTESIAN_POINT('Ctrl Pts',(43.6172881206077,-58.9566576914661,
-39.9695117808943));
#266688=CARTESIAN_POINT('Ctrl Pts',(43.5704358934015,-58.9167725422626,
-39.9673012254286));
#266689=CARTESIAN_POINT('Ctrl Pts',(43.5257501710543,-58.8744832367377,
-39.9652307185737));
#266690=CARTESIAN_POINT('Ctrl Pts',(43.4408839869852,-58.7852840277194,
-39.9614099505568));
#266691=CARTESIAN_POINT('Ctrl Pts',(43.4008519842798,-58.7385284518944,
-39.9596661889691));
#266692=CARTESIAN_POINT('Ctrl Pts',(43.3633213057583,-58.68975488891,-39.9581073773016));
#266693=CARTESIAN_POINT('Origin',(-44.5079524583208,31.5404524382925,235.35105));
#266694=CARTESIAN_POINT('Origin',(44.5079524583208,31.5404524382925,235.35105));
#266695=CARTESIAN_POINT('Ctrl Pts',(46.2910031021108,32.4463941591995,-40.0133516425908));
#266696=CARTESIAN_POINT('Ctrl Pts',(46.2112828672414,32.6032974266246,-40.0284757239348));
#266697=CARTESIAN_POINT('Ctrl Pts',(46.1110474718835,32.7492894385726,-40.037425339261));
#266698=CARTESIAN_POINT('Ctrl Pts',(45.8745943899832,33.0112912763438,-40.042424287837));
#266699=CARTESIAN_POINT('Ctrl Pts',(45.7398389097727,33.1258434240995,-40.0384792740748));
#266700=CARTESIAN_POINT('Ctrl Pts',(45.443656638496,33.3168393914108,-40.0178747536464));
#266701=CARTESIAN_POINT('Ctrl Pts',(45.2839784166729,33.3920654111451,-40.0013399168391));
#266702=CARTESIAN_POINT('Ctrl Pts',(44.9497236580564,33.498953691193,-39.9566891255367));
#266703=CARTESIAN_POINT('Ctrl Pts',(44.7767592325017,33.5299421883571,-39.9287648350382));
#266704=CARTESIAN_POINT('Ctrl Pts',(44.6028100209088,33.538201682522,-39.8960596555963));
#266705=CARTESIAN_POINT('Origin',(0.,-12.9675000200281,-37.9059960127943));
#266706=CARTESIAN_POINT('Ctrl Pts',(-43.4805771074159,-59.5712767529304,
-39.2399080357012));
#266707=CARTESIAN_POINT('Ctrl Pts',(-43.4478249141681,-59.5535603946867,
-39.2311075445953));
#266708=CARTESIAN_POINT('Ctrl Pts',(-43.4156056040519,-59.5351038997391,
-39.2222635806238));
#266709=CARTESIAN_POINT('Ctrl Pts',(-43.3522169440986,-59.4967328580069,
-39.2044893908274));
#266710=CARTESIAN_POINT('Ctrl Pts',(-43.3210476458595,-59.4768182391239,
-39.1955591618115));
#266711=CARTESIAN_POINT('Ctrl Pts',(-43.2291022595543,-59.4149049130521,
-39.1686393287622));
#266712=CARTESIAN_POINT('Ctrl Pts',(-43.1698853587931,-59.3707413041733,
-39.1505208045068));
#266713=CARTESIAN_POINT('Ctrl Pts',(-43.0556331620037,-59.2766097614945,
-39.113935063243));
#266714=CARTESIAN_POINT('Ctrl Pts',(-43.0005921597408,-59.2266373021163,
-39.0954660506179));
#266715=CARTESIAN_POINT('Ctrl Pts',(-42.8948534568781,-59.1207134074407,
-39.0581733199915));
#266716=CARTESIAN_POINT('Ctrl Pts',(-42.8449960553599,-59.0656056508999,
-39.0396463059707));
#266717=CARTESIAN_POINT('Ctrl Pts',(-42.7510811208719,-58.9512122276158,
-39.0028139665663));
#266718=CARTESIAN_POINT('Ctrl Pts',(-42.7070288152267,-58.891930638621,
-38.9845102727346));
#266719=CARTESIAN_POINT('Ctrl Pts',(-42.6452866349949,-58.7998958734659,
-38.957224077988));
#266720=CARTESIAN_POINT('Ctrl Pts',(-42.625429767352,-58.7686980621887,
-38.9481569597938));
#266721=CARTESIAN_POINT('Ctrl Pts',(-42.5871756130002,-58.7052546833099,
-38.9300801552924));
#266722=CARTESIAN_POINT('Ctrl Pts',(-42.568778253032,-58.6730091686672,
-38.9210704649552));
#266723=CARTESIAN_POINT('Ctrl Pts',(-42.5334651880811,-58.6074543754265,
-38.9031098981675));
#266724=CARTESIAN_POINT('Ctrl Pts',(-42.5165536369311,-58.5741539171446,
-38.8941613358138));
#266725=CARTESIAN_POINT('Ctrl Pts',(-42.4842288567228,-58.5064298632496,
-38.8763157156907));
#266726=CARTESIAN_POINT('Ctrl Pts',(-42.4689425396028,-58.4722695523732,
-38.8674882509199));
#266727=CARTESIAN_POINT('Ctrl Pts',(-42.4401223815193,-58.4034275140121,
-38.8500385014136));
#266728=CARTESIAN_POINT('Ctrl Pts',(-42.426583050894,-58.3687341967778,
-38.8414131698514));
#266729=CARTESIAN_POINT('Ctrl Pts',(-42.4012287918448,-58.2988104271035,
-38.824360868638));
#266730=CARTESIAN_POINT('Ctrl Pts',(-42.3894137611201,-58.2635796188005,
-38.8159338161007));
#266731=CARTESIAN_POINT('Ctrl Pts',(-42.3565461207186,-58.1570828582558,
-38.7909502725479));
#266732=CARTESIAN_POINT('Ctrl Pts',(-42.3380647902547,-58.0850119200903,
-38.7746901633276));
#266733=CARTESIAN_POINT('Ctrl Pts',(-42.3155659796374,-57.9752818499468,
-38.7509105250088));
#266734=CARTESIAN_POINT('Ctrl Pts',(-42.3089374211558,-57.9384266221928,
-38.7430843922672));
#266735=CARTESIAN_POINT('Ctrl Pts',(-42.297458012674,-57.864178756387,-38.7276438637217));
#266736=CARTESIAN_POINT('Ctrl Pts',(-42.292601515188,-57.8267325312259,
-38.720018782004));
#266737=CARTESIAN_POINT('Ctrl Pts',(-42.2847289916893,-57.7514526301959,
-38.7050196673962));
#266738=CARTESIAN_POINT('Ctrl Pts',(-42.2817363521424,-57.7138759968928,
-38.6976962453237));
#266739=CARTESIAN_POINT('Ctrl Pts',(-42.277596992864,-57.6387184974263,
-38.6833720377019));
#266740=CARTESIAN_POINT('Ctrl Pts',(-42.2764525301716,-57.6011593077097,
-38.6763755686054));
#266741=CARTESIAN_POINT('Ctrl Pts',(-42.2757726188108,-57.4885396176673,
-38.6558809641879));
#266742=CARTESIAN_POINT('Ctrl Pts',(-42.2789845428693,-57.4135368708757,
-38.6428765167438));
#266743=CARTESIAN_POINT('Ctrl Pts',(-42.289333314243,-57.3011476810195,
-38.6243712990017));
#266744=CARTESIAN_POINT('Ctrl Pts',(-42.2937061680812,-57.2637038035873,
-38.618370061439));
#266745=CARTESIAN_POINT('Ctrl Pts',(-42.3043247017591,-57.1888547452426,
-38.6067079534822));
#266746=CARTESIAN_POINT('Ctrl Pts',(-42.3105743117123,-57.1514345461221,
-38.6010450635964));
#266747=CARTESIAN_POINT('Ctrl Pts',(-42.3249704170347,-57.0766935209606,
-38.590076215021));
#266748=CARTESIAN_POINT('Ctrl Pts',(-42.3331592025312,-57.0392159768686,
-38.5847494243559));
#266749=CARTESIAN_POINT('Ctrl Pts',(-42.3512949844302,-56.9651221381903,
-38.5745673038812));
#266750=CARTESIAN_POINT('Ctrl Pts',(-42.3612586135401,-56.9283882021117,
-38.5696936317377));
#266751=CARTESIAN_POINT('Ctrl Pts',(-42.3829467968515,-56.8555905655333,
-38.5603848033813));
#266752=CARTESIAN_POINT('Ctrl Pts',(-42.3946724551093,-56.8195179901625,
-38.555948235663));
#266753=CARTESIAN_POINT('Ctrl Pts',(-42.4198760714445,-56.7480212016901,
-38.5475092141337));
#266754=CARTESIAN_POINT('Ctrl Pts',(-42.4333540386586,-56.712596992043,
-38.5435067618884));
#266755=CARTESIAN_POINT('Ctrl Pts',(-42.4620643651744,-56.6423976051736,
-38.5359375083953));
#266756=CARTESIAN_POINT('Ctrl Pts',(-42.4772967069948,-56.6076224215361,
-38.5323707022785));
#266757=CARTESIAN_POINT('Ctrl Pts',(-42.5095308031841,-56.5387265502116,
-38.5256774075877));
#266758=CARTESIAN_POINT('Ctrl Pts',(-42.5265325119253,-56.5046058456765,
-38.5225509073062));
#266759=CARTESIAN_POINT('Ctrl Pts',(-42.5623338475307,-56.4370293947696,
-38.5167461666044));
#266760=CARTESIAN_POINT('Ctrl Pts',(-42.5811223641794,-56.4035923099625,
-38.5140693065785));
#266761=CARTESIAN_POINT('Ctrl Pts',(-42.620584523009,-56.3373241998654,
-38.5091697400817));
#266762=CARTESIAN_POINT('Ctrl Pts',(-42.6411082254821,-56.3047465904101,
-38.5069659500128));
#266763=CARTESIAN_POINT('Ctrl Pts',(-42.7048067991197,-56.2090283357163,
-38.5011108589349));
#266764=CARTESIAN_POINT('Ctrl Pts',(-42.7502234543428,-56.1476408662828,
-38.4981890389281));
#266765=CARTESIAN_POINT('Ctrl Pts',(-42.846794232383,-56.0297655581676,
-38.4942910511032));
#266766=CARTESIAN_POINT('Ctrl Pts',(-42.8979715413934,-55.9732420482177,
-38.4933125989996));
#266767=CARTESIAN_POINT('Ctrl Pts',(-42.9790570553346,-55.8921695883032,
-38.4933149859728));
#266768=CARTESIAN_POINT('Ctrl Pts',(-43.0068374106561,-55.8657400908869,
-38.4935622007431));
#266769=CARTESIAN_POINT('Ctrl Pts',(-43.0495800649421,-55.8270637749536,
-38.4943063068789));
#266770=CARTESIAN_POINT('Ctrl Pts',(-43.0640222060113,-55.8143203511958,
-38.494617152342));
#266771=CARTESIAN_POINT('Ctrl Pts',(-43.0932714774893,-55.7891564261061,
-38.4953646906773));
#266772=CARTESIAN_POINT('Ctrl Pts',(-43.1080901283633,-55.7767277938553,
-38.4958020036096));
#266773=CARTESIAN_POINT('Ctrl Pts',(-43.1528523310046,-55.7401327167866,
-38.4972962980169));
#266774=CARTESIAN_POINT('Ctrl Pts',(-43.183171240984,-55.7165901373356,
-38.498536032863));
#266775=CARTESIAN_POINT('Ctrl Pts',(-43.2447583556422,-55.6711691509155,
-38.5014931332815));
#266776=CARTESIAN_POINT('Ctrl Pts',(-43.2760240909102,-55.6492920896315,
-38.5032102926999));
#266777=CARTESIAN_POINT('Ctrl Pts',(-43.37121764534,-55.5861255243223,-38.5090666584048));
#266778=CARTESIAN_POINT('Ctrl Pts',(-43.4365388292261,-55.5472953809443,
-38.5139093068404));
#266779=CARTESIAN_POINT('Ctrl Pts',(-43.5372923455653,-55.4939420631336,
-38.5225684468354));
#266780=CARTESIAN_POINT('Ctrl Pts',(-43.5713395927683,-55.4769743237494,
-38.5256877381308));
#266781=CARTESIAN_POINT('Ctrl Pts',(-43.6403672861995,-55.4446857735354,
-38.5323951500278));
#266782=CARTESIAN_POINT('Ctrl Pts',(-43.6753577685123,-55.4293620157832,
-38.5359845633874));
#266783=CARTESIAN_POINT('Ctrl Pts',(-43.7462462065787,-55.4003985583156,
-38.5436333065981));
#266784=CARTESIAN_POINT('Ctrl Pts',(-43.7822717759725,-55.3867204456352,
-38.5477088862383));
#266785=CARTESIAN_POINT('Ctrl Pts',(-43.8543821738219,-55.3613797848081,
-38.5562346427693));
#266786=CARTESIAN_POINT('Ctrl Pts',(-43.890622407919,-55.349649082917,-38.5607007444526));
#266787=CARTESIAN_POINT('Ctrl Pts',(-43.9633781832422,-55.3280633380684,
-38.5700204086244));
#266788=CARTESIAN_POINT('Ctrl Pts',(-43.9999084022592,-55.3182019076378,
-38.5748754846743));
#266789=CARTESIAN_POINT('Ctrl Pts',(-44.0732691651704,-55.300314394282,
-38.5849692074244));
#266790=CARTESIAN_POINT('Ctrl Pts',(-44.1100997159262,-55.2922883538608,
-38.590207863671));
#266791=CARTESIAN_POINT('Ctrl Pts',(-44.1840590812038,-55.2780579645929,
-38.6010647047639));
#266792=CARTESIAN_POINT('Ctrl Pts',(-44.2211878979616,-55.2718536300564,
-38.6066828933265));
#266793=CARTESIAN_POINT('Ctrl Pts',(-44.2957439071301,-55.2612662316006,
-38.6182974837333));
#266794=CARTESIAN_POINT('Ctrl Pts',(-44.3331710973477,-55.256883155031,
-38.624293883757));
#266795=CARTESIAN_POINT('Ctrl Pts',(-44.4083261383181,-55.2499510742625,
-38.6366662922177));
#266796=CARTESIAN_POINT('Ctrl Pts',(-44.446056048267,-55.2474029004138,
-38.6430428201589));
#266797=CARTESIAN_POINT('Ctrl Pts',(-44.5218128020516,-55.2441636366351,
-38.6561775645199));
#266798=CARTESIAN_POINT('Ctrl Pts',(-44.5599089424743,-55.2434808562086,
-38.6629497802385));
#266799=CARTESIAN_POINT('Ctrl Pts',(-44.6354869543582,-55.2439911084578,
-38.6767130108817));
#266800=CARTESIAN_POINT('Ctrl Pts',(-44.6731456892459,-55.2451740103824,
-38.6837342374529));
#266801=CARTESIAN_POINT('Ctrl Pts',(-44.7481014788608,-55.2493620066237,
-38.6980304684339));
#266802=CARTESIAN_POINT('Ctrl Pts',(-44.7854165850557,-55.2523662274994,
-38.7053085862828));
#266803=CARTESIAN_POINT('Ctrl Pts',(-44.8968808056053,-55.2640710758905,
-38.7275256543264));
#266804=CARTESIAN_POINT('Ctrl Pts',(-44.9705498158105,-55.2754583368831,
-38.7428465194087));
#266805=CARTESIAN_POINT('Ctrl Pts',(-45.0801001998238,-55.2978810544009,
-38.7665804202115));
#266806=CARTESIAN_POINT('Ctrl Pts',(-45.1164578754129,-55.3062470656085,
-38.7746173707339));
#266807=CARTESIAN_POINT('Ctrl Pts',(-45.1888527653151,-55.3247763762561,
-38.790943453482));
#266808=CARTESIAN_POINT('Ctrl Pts',(-45.2248832056965,-55.3349380951144,
-38.7992310848652));
#266809=CARTESIAN_POINT('Ctrl Pts',(-45.2966462681613,-55.3570913336823,
-38.8160672125853));
#266810=CARTESIAN_POINT('Ctrl Pts',(-45.3323638946335,-55.3690863290504,
-38.8246135819642));
#266811=CARTESIAN_POINT('Ctrl Pts',(-45.4027951436545,-55.3946744461232,
-38.841798196801));
#266812=CARTESIAN_POINT('Ctrl Pts',(-45.4376370321487,-55.4083060218429,
-38.85046633842));
#266813=CARTESIAN_POINT('Ctrl Pts',(-45.506502018173,-55.4372015589607,
-38.8679331631116));
#266814=CARTESIAN_POINT('Ctrl Pts',(-45.5405385021803,-55.4524695986684,
-38.8767349781349));
#266815=CARTESIAN_POINT('Ctrl Pts',(-45.6078227545407,-55.4846397884908,
-38.8944741574428));
#266816=CARTESIAN_POINT('Ctrl Pts',(-45.6410705220065,-55.501541940162,
-38.9034115223487));
#266817=CARTESIAN_POINT('Ctrl Pts',(-45.6739227574752,-55.5192637582493,
-38.9124165669282));
#266818=CARTESIAN_POINT('Ctrl Pts',(45.6739227548717,-55.5192637629147,
-38.9124165672461));
#266819=CARTESIAN_POINT('Ctrl Pts',(45.9463033563028,-55.6661968728795,
-38.9870781453929));
#266820=CARTESIAN_POINT('Ctrl Pts',(46.1858267356293,-55.8663975819995,
-39.0648125841885));
#266821=CARTESIAN_POINT('Ctrl Pts',(46.5670747159648,-56.3440390221876,
-39.2155227881245));
#266822=CARTESIAN_POINT('Ctrl Pts',(46.7077569552424,-56.6157479841383,
-39.2873405177034));
#266823=CARTESIAN_POINT('Ctrl Pts',(46.8732483280237,-57.193117527531,-39.4159630591699));
#266824=CARTESIAN_POINT('Ctrl Pts',(46.8994629299653,-57.491836002201,-39.4718422136366));
#266825=CARTESIAN_POINT('Ctrl Pts',(46.8361488789456,-58.0797309112136,
-39.5617425029226));
#266826=CARTESIAN_POINT('Ctrl Pts',(46.7497210582493,-58.3628620872618,
-39.5952773538707));
#266827=CARTESIAN_POINT('Ctrl Pts',(46.4731716121117,-58.8837138814873,
-39.6368897595136));
#266828=CARTESIAN_POINT('Ctrl Pts',(46.2860677203498,-59.1155468740635,
-39.6444848425935));
#266829=CARTESIAN_POINT('Ctrl Pts',(45.8355505681189,-59.4949344949909,
-39.6323858167165));
#266830=CARTESIAN_POINT('Ctrl Pts',(45.5779522357561,-59.6388002274368,
-39.6130511192697));
#266831=CARTESIAN_POINT('Ctrl Pts',(45.0213200602056,-59.8236634709355,
-39.5495917659915));
#266832=CARTESIAN_POINT('Ctrl Pts',(44.7274799400336,-59.8615367970039,
-39.505809377011));
#266833=CARTESIAN_POINT('Ctrl Pts',(44.2690495794481,-59.8339566709351,
-39.4221844653343));
#266834=CARTESIAN_POINT('Ctrl Pts',(44.1034036286098,-59.805591449331,-39.3887143293807));
#266835=CARTESIAN_POINT('Ctrl Pts',(43.7818822384013,-59.7136905694733,
-39.3171340045734));
#266836=CARTESIAN_POINT('Ctrl Pts',(43.6270995967251,-59.6505338853945,
-39.2792785244787));
#266837=CARTESIAN_POINT('Ctrl Pts',(43.4805771074156,-59.571276752931,-39.2399080357013));
#266838=CARTESIAN_POINT('Ctrl Pts',(42.4577131944625,32.5104083279571,-38.8606823233882));
#266839=CARTESIAN_POINT('Ctrl Pts',(42.5764874766347,32.7913026701199,-38.9320840733657));
#266840=CARTESIAN_POINT('Ctrl Pts',(42.7498620817929,33.045230719566,-39.0079063692694));
#266841=CARTESIAN_POINT('Ctrl Pts',(43.1829971873387,33.4691717941986,-39.1588503042595));
#266842=CARTESIAN_POINT('Ctrl Pts',(43.4403467231087,33.6371317127336,-39.2331900309774));
#266843=CARTESIAN_POINT('Ctrl Pts',(44.0001699490351,33.8600656882486,-39.3691508264002));
#266844=CARTESIAN_POINT('Ctrl Pts',(44.2964171622572,33.9159480336448,-39.4298820593753));
#266845=CARTESIAN_POINT('Ctrl Pts',(44.8897972396321,33.9103079782275,-39.5308335555166));
#266846=CARTESIAN_POINT('Ctrl Pts',(45.1806764898647,33.8516842141669,-39.5705004520691));
#266847=CARTESIAN_POINT('Ctrl Pts',(45.727470817634,33.6260302804986,-39.6252622695383));
#266848=CARTESIAN_POINT('Ctrl Pts',(45.9772544322443,33.4613850473092,-39.6397263367521));
#266849=CARTESIAN_POINT('Ctrl Pts',(46.3987893110107,33.0478618141268,-39.6410888152754));
#266850=CARTESIAN_POINT('Ctrl Pts',(46.5666649958226,32.8049268459807,-39.6283385881241));
#266851=CARTESIAN_POINT('Ctrl Pts',(46.8034309450006,32.2681230437893,-39.5771908821506));
#266852=CARTESIAN_POINT('Ctrl Pts',(46.8689681641379,31.9798098532618,-39.539160660217));
#266853=CARTESIAN_POINT('Ctrl Pts',(46.8852106261357,31.5204813293332,-39.4631024925703));
#266854=CARTESIAN_POINT('Ctrl Pts',(46.8726727347044,31.3524538143514,-39.4320349173607));
#266855=CARTESIAN_POINT('Ctrl Pts',(46.8115489554923,31.0230026598069,-39.3646022158351));
#266856=CARTESIAN_POINT('Ctrl Pts',(46.7632492070739,30.8626951466146,-39.3284790845633));
#266857=CARTESIAN_POINT('Ctrl Pts',(46.6981266849492,30.7091523375488,-39.2904704603133));
#266858=CARTESIAN_POINT('Ctrl Pts',(-46.6981266849484,30.7091523375492,
-39.2904704603132));
#266859=CARTESIAN_POINT('Ctrl Pts',(-46.6835475486277,30.6747783378881,
-39.2819613777041));
#266860=CARTESIAN_POINT('Ctrl Pts',(-46.6681814960651,30.6408774263401,
-39.2733909118473));
#266861=CARTESIAN_POINT('Ctrl Pts',(-46.6359019229579,30.57400615396,-39.2561284882363));
#266862=CARTESIAN_POINT('Ctrl Pts',(-46.618988316466,30.5410358444554,-39.2474365250187));
#266863=CARTESIAN_POINT('Ctrl Pts',(-46.5659489383047,30.443507428437,-39.2211791249421));
#266864=CARTESIAN_POINT('Ctrl Pts',(-46.5275294393937,30.3803289376591,
-39.2034325264408));
#266865=CARTESIAN_POINT('Ctrl Pts',(-46.4653031952286,30.2883271671429,
-39.1764461222039));
#266866=CARTESIAN_POINT('Ctrl Pts',(-46.4437937583117,30.2581216171786,
-39.1673894861782));
#266867=CARTESIAN_POINT('Ctrl Pts',(-46.3992224148768,30.1986447451181,
-39.1491520227249));
#266868=CARTESIAN_POINT('Ctrl Pts',(-46.3761748773305,30.1693908446446,
-39.1399767764946));
#266869=CARTESIAN_POINT('Ctrl Pts',(-46.3284414024809,30.1117648114072,
-39.1214771434543));
#266870=CARTESIAN_POINT('Ctrl Pts',(-46.3038983378397,30.083571828401,-39.112209259666));
#266871=CARTESIAN_POINT('Ctrl Pts',(-46.2537073876081,30.0286632749651,
-39.0937226519629));
#266872=CARTESIAN_POINT('Ctrl Pts',(-46.2280147026909,30.001893564456,-39.0844865568113));
#266873=CARTESIAN_POINT('Ctrl Pts',(-46.1492148010453,29.9236586721517,
-39.0568159196779));
#266874=CARTESIAN_POINT('Ctrl Pts',(-46.0943603797766,29.8742287883655,
-39.0384077341064));
#266875=CARTESIAN_POINT('Ctrl Pts',(-46.0086385356025,29.8041510538917,
-39.0108577119752));
#266876=CARTESIAN_POINT('Ctrl Pts',(-45.979489670606,29.7814700298992,-39.0016845404958));
#266877=CARTESIAN_POINT('Ctrl Pts',(-45.9200349130685,29.737472830651,-38.9833588596733));
#266878=CARTESIAN_POINT('Ctrl Pts',(-45.8897290709698,29.7161565962466,
-38.9742063485759));
#266879=CARTESIAN_POINT('Ctrl Pts',(-45.8279451173857,29.6749068346782,
-38.9559225627414));
#266880=CARTESIAN_POINT('Ctrl Pts',(-45.7964751089327,29.6549785818455,
-38.9467936623891));
#266881=CARTESIAN_POINT('Ctrl Pts',(-45.748348603817,29.6261284949947,-38.9331097524421));
#266882=CARTESIAN_POINT('Ctrl Pts',(-45.7321473284057,29.616684052073,-38.9285487676402));
#266883=CARTESIAN_POINT('Ctrl Pts',(-45.6996106203311,29.5982459977232,
-38.9194791520014));
#266884=CARTESIAN_POINT('Ctrl Pts',(-45.683249044345,29.5892352448745,-38.9149628379355));
#266885=CARTESIAN_POINT('Ctrl Pts',(-45.6010439155842,29.5452684013657,
-38.8924942188443));
#266886=CARTESIAN_POINT('Ctrl Pts',(-45.5339074995994,29.5134615304068,
-38.8748432972593));
#266887=CARTESIAN_POINT('Ctrl Pts',(-45.3969715882024,29.4565064940367,
-38.840197135303));
#266888=CARTESIAN_POINT('Ctrl Pts',(-45.3271662939831,29.4313508132015,
-38.823199542964));
#266889=CARTESIAN_POINT('Ctrl Pts',(-45.2204298442793,29.398652641048,-38.7982016720699));
#266890=CARTESIAN_POINT('Ctrl Pts',(-45.184512437616,29.3885937253944,-38.7899522655792));
#266891=CARTESIAN_POINT('Ctrl Pts',(-45.1119891467798,29.3701842541612,
-38.7736235920333));
#266892=CARTESIAN_POINT('Ctrl Pts',(-45.0754052578815,29.3618381514785,
-38.7655490803555));
#266893=CARTESIAN_POINT('Ctrl Pts',(-45.0014447932704,29.3468760834355,
-38.7495561846596));
#266894=CARTESIAN_POINT('Ctrl Pts',(-44.964301863367,29.3403115562353,-38.7416890516424));
#266895=CARTESIAN_POINT('Ctrl Pts',(-44.8900079594565,29.3290481892184,
-38.726277749838));
#266896=CARTESIAN_POINT('Ctrl Pts',(-44.8527936282157,29.324336495618,-38.7187198739728));
#266897=CARTESIAN_POINT('Ctrl Pts',(-44.7410083373266,29.3129455735289,
-38.6964994820139));
#266898=CARTESIAN_POINT('Ctrl Pts',(-44.6662563757167,29.3089967422249,
-38.6822807693139));
#266899=CARTESIAN_POINT('Ctrl Pts',(-44.516312468428,29.3084067934202,-38.6550493453909));
#266900=CARTESIAN_POINT('Ctrl Pts',(-44.441103189525,29.3117700143417,-38.6420342479066));
#266901=CARTESIAN_POINT('Ctrl Pts',(-44.3468378615956,29.3206690055189,
-38.6265520162729));
#266902=CARTESIAN_POINT('Ctrl Pts',(-44.3279589148655,29.3226883315868,
-38.6234933649988));
#266903=CARTESIAN_POINT('Ctrl Pts',(-44.2901960653061,29.3271995080041,
-38.6174591262491));
#266904=CARTESIAN_POINT('Ctrl Pts',(-44.2712743932921,29.329697893027,-38.614477863833));
#266905=CARTESIAN_POINT('Ctrl Pts',(-44.2146592782018,29.3378915995821,
-38.60568558559));
#266906=CARTESIAN_POINT('Ctrl Pts',(-44.1772069502033,29.344266758826,-38.6000392683017));
#266907=CARTESIAN_POINT('Ctrl Pts',(-44.1027653084072,29.3588321594788,
-38.5891549147378));
#266908=CARTESIAN_POINT('Ctrl Pts',(-44.0657945489017,29.3670194960673,
-38.5839197203675));
#266909=CARTESIAN_POINT('Ctrl Pts',(-43.9923490656542,29.3851892021794,
-38.5738612453122));
#266910=CARTESIAN_POINT('Ctrl Pts',(-43.9558743463703,29.395171587473,-38.5690379674556));
#266911=CARTESIAN_POINT('Ctrl Pts',(-43.8834205276403,29.4169303996784,
-38.5598042480103));
#266912=CARTESIAN_POINT('Ctrl Pts',(-43.8474414251675,29.4287068153425,
-38.5553938031715));
#266913=CARTESIAN_POINT('Ctrl Pts',(-43.7759820586595,29.4540658195324,
-38.5469896320335));
#266914=CARTESIAN_POINT('Ctrl Pts',(-43.7405017838471,29.467648368817,-38.5429958961485));
#266915=CARTESIAN_POINT('Ctrl Pts',(-43.6700470477634,29.4966453401303,
-38.5354320983078));
#266916=CARTESIAN_POINT('Ctrl Pts',(-43.6350719757086,29.512061063653,-38.5318621614261));
#266917=CARTESIAN_POINT('Ctrl Pts',(-43.5656410085295,29.5447591316771,
-38.525155654825));
#266918=CARTESIAN_POINT('Ctrl Pts',(-43.5311320054746,29.5620794464364,
-38.5220163122062));
#266919=CARTESIAN_POINT('Ctrl Pts',(-43.4634866412135,29.5981758355574,
-38.5162526847879));
#266920=CARTESIAN_POINT('Ctrl Pts',(-43.4301834663391,29.6170276546,-38.5136117755133));
#266921=CARTESIAN_POINT('Ctrl Pts',(-43.3647025891651,29.6562685687332,
-38.5088155315793));
#266922=CARTESIAN_POINT('Ctrl Pts',(-43.3325078231767,29.6766655539003,
-38.5066585209069));
#266923=CARTESIAN_POINT('Ctrl Pts',(-43.2375484321327,29.7401688861791,
-38.5009063965958));
#266924=CARTESIAN_POINT('Ctrl Pts',(-43.1764049274077,29.7855824582168,
-38.4980286134812));
#266925=CARTESIAN_POINT('Ctrl Pts',(-43.0584774180437,29.8826126224142,
-38.4942050936184));
#266926=CARTESIAN_POINT('Ctrl Pts',(-43.001681818637,29.9342392650769,-38.4932590761897));
#266927=CARTESIAN_POINT('Ctrl Pts',(-42.8926599718677,30.0438904492243,
-38.4933742455196));
#266928=CARTESIAN_POINT('Ctrl Pts',(-42.8414047150844,30.1009342501745,
-38.4944336470273));
#266929=CARTESIAN_POINT('Ctrl Pts',(-42.7451036203247,30.2193471227021,
-38.498479276642));
#266930=CARTESIAN_POINT('Ctrl Pts',(-42.7000684110598,30.2807072617414,
-38.5014658126213));
#266931=CARTESIAN_POINT('Ctrl Pts',(-42.6161769337401,30.4076992015223,
-38.5093469123445));
#266932=CARTESIAN_POINT('Ctrl Pts',(-42.5773225406026,30.4733365238586,
-38.5142428327574));
#266933=CARTESIAN_POINT('Ctrl Pts',(-42.5326943378214,30.5580963840027,
-38.5215739479982));
#266934=CARTESIAN_POINT('Ctrl Pts',(-42.5239673850246,30.5751883092729,
-38.5231018165939));
#266935=CARTESIAN_POINT('Ctrl Pts',(-42.5069121510755,30.60964376351,-38.5262794637242));
#266936=CARTESIAN_POINT('Ctrl Pts',(-42.4985805781952,30.627019094627,-38.5279307934181));
#266937=CARTESIAN_POINT('Ctrl Pts',(-42.4743295471271,30.6792614198295,
-38.5330409224498));
#266938=CARTESIAN_POINT('Ctrl Pts',(-42.4591078049536,30.7143247172706,
-38.5366620777082));
#266939=CARTESIAN_POINT('Ctrl Pts',(-42.4305062721789,30.7849297925434,
-38.5443248028235));
#266940=CARTESIAN_POINT('Ctrl Pts',(-42.4171273618354,30.8204683264523,
-38.5483659418649));
#266941=CARTESIAN_POINT('Ctrl Pts',(-42.3921837112499,30.89200995013,-38.556860031436));
#266942=CARTESIAN_POINT('Ctrl Pts',(-42.3806190180342,30.9280130518798,
-38.5613129931637));
#266943=CARTESIAN_POINT('Ctrl Pts',(-42.3592881563091,31.0004799414626,
-38.5706260903895));
#266944=CARTESIAN_POINT('Ctrl Pts',(-42.3495220063211,31.0369437339595,
-38.5754862307243));
#266945=CARTESIAN_POINT('Ctrl Pts',(-42.3317857495347,31.1103315158532,
-38.5856119737634));
#266946=CARTESIAN_POINT('Ctrl Pts',(-42.3238156343608,31.1472555030051,
-38.5908775753381));
#266947=CARTESIAN_POINT('Ctrl Pts',(-42.3096820427396,31.2215665449467,
-38.6018154236264));
#266948=CARTESIAN_POINT('Ctrl Pts',(-42.3035171869091,31.2589715314082,
-38.6074906718877));
#266949=CARTESIAN_POINT('Ctrl Pts',(-42.2930235524414,31.3341791410138,
-38.6192399292287));
#266950=CARTESIAN_POINT('Ctrl Pts',(-42.2886818075092,31.3721585359098,
-38.6253436316658));
#266951=CARTESIAN_POINT('Ctrl Pts',(-42.2819306306109,31.4478003630713,
-38.6378362101326));
#266952=CARTESIAN_POINT('Ctrl Pts',(-42.2795025237186,31.4855414978569,
-38.6442360129219));
#266953=CARTESIAN_POINT('Ctrl Pts',(-42.2765060643256,31.5608485897329,
-38.6573322722499));
#266954=CARTESIAN_POINT('Ctrl Pts',(-42.2759365563455,31.5984178297074,
-38.6640291190605));
#266955=CARTESIAN_POINT('Ctrl Pts',(-42.2769710616629,31.710876916496,-38.6845570305479));
#266956=CARTESIAN_POINT('Ctrl Pts',(-42.2813124759152,31.7855186400122,
-38.698824567557));
#266957=CARTESIAN_POINT('Ctrl Pts',(-42.2932531103751,31.8969906134966,
-38.7210841829084));
#266958=CARTESIAN_POINT('Ctrl Pts',(-42.2981395950573,31.934066030451,-38.7286473545921));
#266959=CARTESIAN_POINT('Ctrl Pts',(-42.3097367777483,32.0080522284017,
-38.7440609732535));
#266960=CARTESIAN_POINT('Ctrl Pts',(-42.3164494406915,32.0449687602613,
-38.7519128032936));
#266961=CARTESIAN_POINT('Ctrl Pts',(-42.3317154579634,32.1186122141692,
-38.7679009120377));
#266962=CARTESIAN_POINT('Ctrl Pts',(-42.3402956643805,32.1554227583218,
-38.7760569897633));
#266963=CARTESIAN_POINT('Ctrl Pts',(-42.3591481714288,32.228169160774,-38.7925026060078));
#266964=CARTESIAN_POINT('Ctrl Pts',(-42.3694448348212,32.2642362896146,
-38.8008201507359));
#266965=CARTESIAN_POINT('Ctrl Pts',(-42.391742799968,32.3356900672865,-38.817625053217));
#266966=CARTESIAN_POINT('Ctrl Pts',(-42.4037465150873,32.3710895326604,
-38.8261151521117));
#266967=CARTESIAN_POINT('Ctrl Pts',(-42.4294540540396,32.4412374294073,
-38.8432687881532));
#266968=CARTESIAN_POINT('Ctrl Pts',(-42.443157884724,32.4759858579956,-38.8519323266277));
#266969=CARTESIAN_POINT('Ctrl Pts',(-42.4577131904514,32.5104083297438,
-38.8606823230314));
#266970=CARTESIAN_POINT('Origin',(0.,-12.9675000200281,-55.24995));
#266971=CARTESIAN_POINT('Ctrl Pts',(43.4805771050572,-59.5712767635336,
-39.239908023115));
#266972=CARTESIAN_POINT('Ctrl Pts',(43.4478249116748,-59.553560405217,-39.231107532009));
#266973=CARTESIAN_POINT('Ctrl Pts',(43.415605601426,-59.5351039101939,-39.2222635680375));
#266974=CARTESIAN_POINT('Ctrl Pts',(43.3522169412117,-59.4967328683047,
-39.2044893782411));
#266975=CARTESIAN_POINT('Ctrl Pts',(43.3210476428442,-59.4768182493402,
-39.1955591492252));
#266976=CARTESIAN_POINT('Ctrl Pts',(43.2291022561607,-59.4149049230149,
-39.1686393161759));
#266977=CARTESIAN_POINT('Ctrl Pts',(43.1698853551558,-59.3707413139551,
-39.1505207919205));
#266978=CARTESIAN_POINT('Ctrl Pts',(43.0556331578966,-59.2766097708902,
-39.1139350506567));
#266979=CARTESIAN_POINT('Ctrl Pts',(43.0005921554074,-59.226637311307,-39.0954660380315));
#266980=CARTESIAN_POINT('Ctrl Pts',(42.8948534521102,-59.1207134161965,
-39.0581733074052));
#266981=CARTESIAN_POINT('Ctrl Pts',(42.8449960503872,-59.0656056594293,
-39.0396462933844));
#266982=CARTESIAN_POINT('Ctrl Pts',(42.7510811155138,-58.9512122356751,
-39.00281395398));
#266983=CARTESIAN_POINT('Ctrl Pts',(42.707028809688,-58.8919306464366,-38.9845102601483));
#266984=CARTESIAN_POINT('Ctrl Pts',(42.6452866292032,-58.799895880903,-38.9572240654017));
#266985=CARTESIAN_POINT('Ctrl Pts',(42.6254297614789,-58.7686980694974,
-38.9481569472075));
#266986=CARTESIAN_POINT('Ctrl Pts',(42.5871756069705,-58.7052546903576,
-38.9300801427061));
#266987=CARTESIAN_POINT('Ctrl Pts',(42.568778246927,-58.6730091755822,-38.9210704523689));
#266988=CARTESIAN_POINT('Ctrl Pts',(42.5334651818316,-58.6074543820717,
-38.9031098855812));
#266989=CARTESIAN_POINT('Ctrl Pts',(42.5165536306125,-58.5741539236527,
-38.8941613232275));
#266990=CARTESIAN_POINT('Ctrl Pts',(42.4842288502722,-58.5064298694789,
-38.8763157031044));
#266991=CARTESIAN_POINT('Ctrl Pts',(42.4689425330898,-58.4722695584619,
-38.8674882383336));
#266992=CARTESIAN_POINT('Ctrl Pts',(42.4401223748888,-58.4034275198172,
-38.8500384888273));
#266993=CARTESIAN_POINT('Ctrl Pts',(42.4265830442083,-58.36873420244,-38.841413157265));
#266994=CARTESIAN_POINT('Ctrl Pts',(42.4012287850559,-58.2988104324777,
-38.8243608560517));
#266995=CARTESIAN_POINT('Ctrl Pts',(42.3894137542831,-58.2635796240295,
-38.8159338035143));
#266996=CARTESIAN_POINT('Ctrl Pts',(42.3565461137483,-58.1570828630459,
-38.7909502599615));
#266997=CARTESIAN_POINT('Ctrl Pts',(42.3380647832096,-58.0850119245834,
-38.7746901507413));
#266998=CARTESIAN_POINT('Ctrl Pts',(42.3155659725018,-57.9752818539874,
-38.7509105124225));
#266999=CARTESIAN_POINT('Ctrl Pts',(42.3089374139936,-57.9384266260814,
-38.7430843796809));
#267000=CARTESIAN_POINT('Ctrl Pts',(42.297458005466,-57.8641787599694,-38.7276438511353));
#267001=CARTESIAN_POINT('Ctrl Pts',(42.2926015079608,-57.8267325346538,
-38.7200187694177));
#267002=CARTESIAN_POINT('Ctrl Pts',(42.2847289844313,-57.7514526333132,
-38.7050196548099));
#267003=CARTESIAN_POINT('Ctrl Pts',(42.2817363448728,-57.7138759998551,
-38.6976962327374));
#267004=CARTESIAN_POINT('Ctrl Pts',(42.277596985579,-57.6387185000784,-38.6833720251155));
#267005=CARTESIAN_POINT('Ctrl Pts',(42.2764525228827,-57.6011593102068,
-38.6763755560191));
#267006=CARTESIAN_POINT('Ctrl Pts',(42.2757726115216,-57.4885396196995,
-38.6558809516015));
#267007=CARTESIAN_POINT('Ctrl Pts',(42.278984535595,-57.4135368725982,-38.6428765041575));
#267008=CARTESIAN_POINT('Ctrl Pts',(42.289333307014,-57.3011476822778,-38.6243712864154));
#267009=CARTESIAN_POINT('Ctrl Pts',(42.2937061608711,-57.2637038046909,
-38.6183700488527));
#267010=CARTESIAN_POINT('Ctrl Pts',(42.3043246945944,-57.188854746037,-38.6067079408958));
#267011=CARTESIAN_POINT('Ctrl Pts',(42.3105743045743,-57.1514345467618,
-38.6010450510101));
#267012=CARTESIAN_POINT('Ctrl Pts',(42.3249704099578,-57.0766935212914,
-38.5900762024347));
#267013=CARTESIAN_POINT('Ctrl Pts',(42.333159195489,-57.0392159770445,-38.5847494117696));
#267014=CARTESIAN_POINT('Ctrl Pts',(42.3512949774645,-56.9651221380599,
-38.5745672912949));
#267015=CARTESIAN_POINT('Ctrl Pts',(42.3612586066164,-56.9283882018294,
-38.5696936191514));
#267016=CARTESIAN_POINT('Ctrl Pts',(42.382946790019,-56.85559056495,-38.560384790795));
#267017=CARTESIAN_POINT('Ctrl Pts',(42.394672448326,-56.81951798943,-38.5559482230767));
#267018=CARTESIAN_POINT('Ctrl Pts',(42.419876064767,-56.7480212006618,-38.5475092015474));
#267019=CARTESIAN_POINT('Ctrl Pts',(42.4333540320375,-56.7125969908682,
-38.543506749302));
#267020=CARTESIAN_POINT('Ctrl Pts',(42.4620643586734,-56.6423976037083,
-38.5359374958091));
#267021=CARTESIAN_POINT('Ctrl Pts',(42.4772967005576,-56.6076224199269,
-38.5323706896922));
#267022=CARTESIAN_POINT('Ctrl Pts',(42.5095307968816,-56.5387265483172,
-38.5256773950013));
#267023=CARTESIAN_POINT('Ctrl Pts',(42.5265325056937,-56.5046058436408,
-38.5225508947199));
#267024=CARTESIAN_POINT('Ctrl Pts',(42.5623338414485,-56.4370293924541,
-38.5167461540181));
#267025=CARTESIAN_POINT('Ctrl Pts',(42.5811223581755,-56.4035923075085,
-38.5140692939922));
#267026=CARTESIAN_POINT('Ctrl Pts',(42.6205845171696,-56.3373241971369,
-38.5091697274954));
#267027=CARTESIAN_POINT('Ctrl Pts',(42.6411082197283,-56.3047465875466,
-38.5069659374265));
#267028=CARTESIAN_POINT('Ctrl Pts',(42.704806793631,-56.2090283324561,-38.5011108463486));
#267029=CARTESIAN_POINT('Ctrl Pts',(42.7502234490431,-56.1476408627681,
-38.4981890263418));
#267030=CARTESIAN_POINT('Ctrl Pts',(42.8467942274848,-56.029765554164,-38.4942910385169));
#267031=CARTESIAN_POINT('Ctrl Pts',(42.8979715367077,-55.9732420439795,
-38.4933125864132));
#267032=CARTESIAN_POINT('Ctrl Pts',(42.9790570509856,-55.8921695837284,
-38.4933149733865));
#267033=CARTESIAN_POINT('Ctrl Pts',(43.0068374064224,-55.8657400862024,
-38.4935621881568));
#267034=CARTESIAN_POINT('Ctrl Pts',(43.0495800608858,-55.8270637701084,
-38.4943062942926));
#267035=CARTESIAN_POINT('Ctrl Pts',(43.064022202015,-55.8143203462976,-38.4946171397557));
#267036=CARTESIAN_POINT('Ctrl Pts',(43.0932714736142,-55.7891564211033,
-38.495364678091));
#267037=CARTESIAN_POINT('Ctrl Pts',(43.1080901245497,-55.7767277888009,
-38.4958019910233));
#267038=CARTESIAN_POINT('Ctrl Pts',(43.1528523273767,-55.74013271158,-38.4972962854306));
#267039=CARTESIAN_POINT('Ctrl Pts',(43.1831712374819,-55.7165901320311,
-38.4985360202767));
#267040=CARTESIAN_POINT('Ctrl Pts',(43.2447583523954,-55.6711691454221,
-38.5014931206952));
#267041=CARTESIAN_POINT('Ctrl Pts',(43.276024087793,-55.649292084047,-38.5032102801136));
#267042=CARTESIAN_POINT('Ctrl Pts',(43.3712176426173,-55.5861255184748,
-38.5090666458185));
#267043=CARTESIAN_POINT('Ctrl Pts',(43.436538826774,-55.547295374935,-38.513909294254));
#267044=CARTESIAN_POINT('Ctrl Pts',(43.5372923435304,-55.4939420569017,
-38.5225684342491));
#267045=CARTESIAN_POINT('Ctrl Pts',(43.5713395908744,-55.4769743174466,
-38.5256877255445));
#267046=CARTESIAN_POINT('Ctrl Pts',(43.6403672845913,-55.4446857670977,
-38.5323951374414));
#267047=CARTESIAN_POINT('Ctrl Pts',(43.6753577670489,-55.4293620092815,
-38.535984550801));
#267048=CARTESIAN_POINT('Ctrl Pts',(43.7462462054086,-55.4003985516927,
-38.5436332940118));
#267049=CARTESIAN_POINT('Ctrl Pts',(43.7822717749515,-55.3867204389549,
-38.547708873652));
#267050=CARTESIAN_POINT('Ctrl Pts',(43.8543821730992,-55.3613797780216,
-38.556234630183));
#267051=CARTESIAN_POINT('Ctrl Pts',(43.8906224073461,-55.3496490760812,
-38.5607007318663));
#267052=CARTESIAN_POINT('Ctrl Pts',(43.9633781829702,-55.3280633311418,
-38.570020396038));
#267053=CARTESIAN_POINT('Ctrl Pts',(43.9999084021383,-55.3182019006697,
-38.574875472088));
#267054=CARTESIAN_POINT('Ctrl Pts',(44.0732691653527,-55.3003143872384,
-38.5849691948381));
#267055=CARTESIAN_POINT('Ctrl Pts',(44.1100997162607,-55.2922883467832,
-38.5902078510847));
#267056=CARTESIAN_POINT('Ctrl Pts',(44.1840590818441,-55.2780579574549,
-38.6010646921776));
#267057=CARTESIAN_POINT('Ctrl Pts',(44.2211878987553,-55.2718536228919,
-38.6066828807402));
#267058=CARTESIAN_POINT('Ctrl Pts',(44.2957439082318,-55.2612662243907,
-38.6182974711469));
#267059=CARTESIAN_POINT('Ctrl Pts',(44.333171098604,-55.2568831478022,-38.6242938711707));
#267060=CARTESIAN_POINT('Ctrl Pts',(44.4083261398848,-55.2499510670034,
-38.6366662796313));
#267061=CARTESIAN_POINT('Ctrl Pts',(44.4460560499895,-55.2474028931433,
-38.6430428075725));
#267062=CARTESIAN_POINT('Ctrl Pts',(44.5218128040869,-55.2441636293496,
-38.6561775519336));
#267063=CARTESIAN_POINT('Ctrl Pts',(44.5599089446669,-55.2434808489194,
-38.6629497676522));
#267064=CARTESIAN_POINT('Ctrl Pts',(44.6354869568629,-55.243991101169,-38.6767129982954));
#267065=CARTESIAN_POINT('Ctrl Pts',(44.673145691906,-55.2451740030977,-38.6837342248666));
#267066=CARTESIAN_POINT('Ctrl Pts',(44.7481014818302,-55.2493619993546,
-38.6980304558476));
#267067=CARTESIAN_POINT('Ctrl Pts',(44.785416588179,-55.2523662202419,-38.7053085736965));
#267068=CARTESIAN_POINT('Ctrl Pts',(44.8968808091885,-55.2640710686789,
-38.7275256417401));
#267069=CARTESIAN_POINT('Ctrl Pts',(44.9705498196976,-55.2754583297169,
-38.7428465068224));
#267070=CARTESIAN_POINT('Ctrl Pts',(45.0801002041626,-55.2978810473249,
-38.7665804076252));
#267071=CARTESIAN_POINT('Ctrl Pts',(45.1164578799016,-55.3062470585662,
-38.7746173581476));
#267072=CARTESIAN_POINT('Ctrl Pts',(45.1888527701022,-55.3247763692888,
-38.7909434408956));
#267073=CARTESIAN_POINT('Ctrl Pts',(45.2248832106321,-55.3349380881883,
-38.7992310722789));
#267074=CARTESIAN_POINT('Ctrl Pts',(45.2966462733926,-55.3570913268461,
-38.816067199999));
#267075=CARTESIAN_POINT('Ctrl Pts',(45.332363900012,-55.369086322263,-38.8246135693778));
#267076=CARTESIAN_POINT('Ctrl Pts',(45.4027951493232,-55.3946744394399,
-38.8417981842147));
#267077=CARTESIAN_POINT('Ctrl Pts',(45.4376370379609,-55.4083060152152,
-38.8504663258337));
#267078=CARTESIAN_POINT('Ctrl Pts',(45.5065020242688,-55.4372015524508,
-38.8679331505253));
#267079=CARTESIAN_POINT('Ctrl Pts',(45.5405385084162,-55.4524695922208,
-38.8767349655486));
#267080=CARTESIAN_POINT('Ctrl Pts',(45.6078227610536,-55.4846397821746,
-38.8944741448564));
#267081=CARTESIAN_POINT('Ctrl Pts',(45.6410705286563,-55.5015419339148,
-38.9034115097624));
#267082=CARTESIAN_POINT('Ctrl Pts',(45.7067749946571,-55.5369855795655,
-38.9214215995571));
#267083=CARTESIAN_POINT('Ctrl Pts',(45.7392219948332,-55.5555212054356,
-38.9304915578471));
#267084=CARTESIAN_POINT('Ctrl Pts',(45.8033556905571,-55.5942722101173,
-38.9487787746614));
#267085=CARTESIAN_POINT('Ctrl Pts',(45.8348443765872,-55.6143675254903,
-38.9579394992153));
#267086=CARTESIAN_POINT('Ctrl Pts',(45.9274099921067,-55.6766588970005,
-38.9854159036859));
#267087=CARTESIAN_POINT('Ctrl Pts',(45.9867610946637,-55.720935310253,-39.0037703512016));
#267088=CARTESIAN_POINT('Ctrl Pts',(46.10073379155,-55.8148102344162,-39.0405190740001));
#267089=CARTESIAN_POINT('Ctrl Pts',(46.1553754339886,-55.8644173716091,
-39.0589184790541));
#267090=CARTESIAN_POINT('Ctrl Pts',(46.2338037360394,-55.9428521263115,
-39.0865551832126));
#267091=CARTESIAN_POINT('Ctrl Pts',(46.2593565839205,-55.9696687309655,
-39.0957737053687));
#267092=CARTESIAN_POINT('Ctrl Pts',(46.3092668173353,-56.0246630492642,
-39.1142236288024));
#267093=CARTESIAN_POINT('Ctrl Pts',(46.3336138271979,-56.0528284069633,
-39.1234510369563));
#267094=CARTESIAN_POINT('Ctrl Pts',(46.3692509380672,-56.0961546927766,
-39.1373141611117));
#267095=CARTESIAN_POINT('Ctrl Pts',(46.3809719652397,-56.110765521319,-39.1419350415337));
#267096=CARTESIAN_POINT('Ctrl Pts',(46.4039851066281,-56.1401806678783,
-39.1511314642401));
#267097=CARTESIAN_POINT('Ctrl Pts',(46.415300200194,-56.155012658913,-39.1557159007951));
#267098=CARTESIAN_POINT('Ctrl Pts',(46.4486370196562,-56.1998310026459,
-39.1694131056795));
#267099=CARTESIAN_POINT('Ctrl Pts',(46.4700835192022,-56.2301795284771,
-39.1784825928561));
#267100=CARTESIAN_POINT('Ctrl Pts',(46.5320719239954,-56.322558395602,-39.2054898607661));
#267101=CARTESIAN_POINT('Ctrl Pts',(46.5703036051881,-56.3859631553179,
-39.2232408436738));
#267102=CARTESIAN_POINT('Ctrl Pts',(46.6230137408496,-56.4837650893312,
-39.2494851247746));
#267103=CARTESIAN_POINT('Ctrl Pts',(46.6398105887851,-56.516816729636,-39.2581697915521));
#267104=CARTESIAN_POINT('Ctrl Pts',(46.6718446993975,-56.5838294913527,
-39.2754119059931));
#267105=CARTESIAN_POINT('Ctrl Pts',(46.6870820411944,-56.6177905669658,
-39.283969358867));
#267106=CARTESIAN_POINT('Ctrl Pts',(46.7159729940879,-56.6866360531864,
-39.3009558743285));
#267107=CARTESIAN_POINT('Ctrl Pts',(46.7296188134962,-56.7214992877386,
-39.3093799092323));
#267108=CARTESIAN_POINT('Ctrl Pts',(46.755321710985,-56.7922546374611,-39.3261176515222));
#267109=CARTESIAN_POINT('Ctrl Pts',(46.7672997055706,-56.8279354873648,
-39.3343809661765));
#267110=CARTESIAN_POINT('Ctrl Pts',(46.8004530616987,-56.9353633956067,
-39.3587371504317));
#267111=CARTESIAN_POINT('Ctrl Pts',(46.8189795616622,-57.0077635587484,
-39.374465799535));
#267112=CARTESIAN_POINT('Ctrl Pts',(46.8489162234024,-57.154008095182,-39.4048998164529));
#267113=CARTESIAN_POINT('Ctrl Pts',(46.8603369561858,-57.2278698681474,
-39.4196100455824));
#267114=CARTESIAN_POINT('Ctrl Pts',(46.8720664861652,-57.3397812908466,
-39.4409093514509));
#267115=CARTESIAN_POINT('Ctrl Pts',(46.8750747613607,-57.3772756907765,
-39.4478819258883));
#267116=CARTESIAN_POINT('Ctrl Pts',(46.8792543070635,-57.452637032744,-39.4615663817213));
#267117=CARTESIAN_POINT('Ctrl Pts',(46.8804258854059,-57.4905390852254,
-39.468284348285));
#267118=CARTESIAN_POINT('Ctrl Pts',(46.8808837860862,-57.5666104395958,
-39.4814341834338));
#267119=CARTESIAN_POINT('Ctrl Pts',(46.8801708754895,-57.6044913973763,
-39.4878166551363));
#267120=CARTESIAN_POINT('Ctrl Pts',(46.87689139966,-57.6800598013179,-39.5002231022271));
#267121=CARTESIAN_POINT('Ctrl Pts',(46.8743246754726,-57.7177285021534,
-39.5062438281333));
#267122=CARTESIAN_POINT('Ctrl Pts',(46.8638675798749,-57.8303908466031,
-39.5237649470641));
#267123=CARTESIAN_POINT('Ctrl Pts',(46.8532263770448,-57.905041491034,-39.5347254769916));
#267124=CARTESIAN_POINT('Ctrl Pts',(46.8317335430131,-58.0163268488721,
-39.5500873284662));
#267125=CARTESIAN_POINT('Ctrl Pts',(46.8236459657866,-58.0533066853948,
-39.5550278296908));
#267126=CARTESIAN_POINT('Ctrl Pts',(46.8055990223885,-58.1270324985156,
-39.5645447277516));
#267127=CARTESIAN_POINT('Ctrl Pts',(46.7956339790501,-58.1637938579406,
-39.5691227795573));
#267128=CARTESIAN_POINT('Ctrl Pts',(46.7738161439719,-58.2370162127271,
-39.5779016343018));
#267129=CARTESIAN_POINT('Ctrl Pts',(46.7619036390658,-58.2736352320482,
-39.5821192077603));
#267130=CARTESIAN_POINT('Ctrl Pts',(46.7364059829356,-58.3458256050085,
-39.5900871728599));
#267131=CARTESIAN_POINT('Ctrl Pts',(46.7227943985224,-58.3815079350702,
-39.5938520139967));
#267132=CARTESIAN_POINT('Ctrl Pts',(46.6938810713598,-58.452011863029,-39.6009443748824));
#267133=CARTESIAN_POINT('Ctrl Pts',(46.6785776360953,-58.4868413824451,
-39.6042729587978));
#267134=CARTESIAN_POINT('Ctrl Pts',(46.6462897444841,-58.555661726432,-39.6104989258044));
#267135=CARTESIAN_POINT('Ctrl Pts',(46.6293052752408,-58.5896525446103,
-39.6133963049726));
#267136=CARTESIAN_POINT('Ctrl Pts',(46.5936553637194,-58.6567954655617,
-39.6187605591878));
#267137=CARTESIAN_POINT('Ctrl Pts',(46.5749899342291,-58.689947574739,-39.6212274370902));
#267138=CARTESIAN_POINT('Ctrl Pts',(46.535965754159,-58.7554068805448,-39.6257281208558));
#267139=CARTESIAN_POINT('Ctrl Pts',(46.5156070431754,-58.7877140969356,
-39.627761936622));
#267140=CARTESIAN_POINT('Ctrl Pts',(46.4731710934002,-58.8514710123629,
-39.6313905509331));
#267141=CARTESIAN_POINT('Ctrl Pts',(46.4511086236678,-58.882900639648,-39.6329844474041));
#267142=CARTESIAN_POINT('Ctrl Pts',(46.4051673298575,-58.9449633096445,
-39.6357273359789));
#267143=CARTESIAN_POINT('Ctrl Pts',(46.3814480039077,-58.9753775970138,
-39.6368662472668));
#267144=CARTESIAN_POINT('Ctrl Pts',(46.3084069002845,-59.0643493221119,
-39.6395761107827));
#267145=CARTESIAN_POINT('Ctrl Pts',(46.2570407937254,-59.1209150540827,
-39.6404603658463));
#267146=CARTESIAN_POINT('Ctrl Pts',(46.1491379842615,-59.2285444723307,
-39.6404138688384));
#267147=CARTESIAN_POINT('Ctrl Pts',(46.0925836639483,-59.2796343138351,
-39.639484568582));
#267148=CARTESIAN_POINT('Ctrl Pts',(46.0038529518281,-59.3521266221997,
-39.6367223261665));
#267149=CARTESIAN_POINT('Ctrl Pts',(45.9736068158058,-59.3756113651479,
-39.6355721037165));
#267150=CARTESIAN_POINT('Ctrl Pts',(45.927265703875,-59.4097723645372,-39.6334997599225));
#267151=CARTESIAN_POINT('Ctrl Pts',(45.9116419292403,-59.4209912919482,
-39.6327502683094));
#267152=CARTESIAN_POINT('Ctrl Pts',(45.88008048702,-59.4430610902896,-39.6311351213432));
#267153=CARTESIAN_POINT('Ctrl Pts',(45.864107784879,-59.4539347719282,-39.6302673854466));
#267154=CARTESIAN_POINT('Ctrl Pts',(45.8159067249643,-59.4858696909571,
-39.6274990121292));
#267155=CARTESIAN_POINT('Ctrl Pts',(45.783409718025,-59.5062439066798,-39.6254354946116));
#267156=CARTESIAN_POINT('Ctrl Pts',(45.7176331131415,-59.5452482017306,
-39.6208773136804));
#267157=CARTESIAN_POINT('Ctrl Pts',(45.6843658562672,-59.5638704429234,
-39.6183834165608));
#267158=CARTESIAN_POINT('Ctrl Pts',(45.5834449351778,-59.6171384233149,
-39.610266415423));
#267159=CARTESIAN_POINT('Ctrl Pts',(45.5146744686846,-59.649190882251,-39.6040093823393));
#267160=CARTESIAN_POINT('Ctrl Pts',(45.4093033711364,-59.6921244775619,
-39.5933617190949));
#267161=CARTESIAN_POINT('Ctrl Pts',(45.3738098063667,-59.7055766893281,
-39.5896017780072));
#267162=CARTESIAN_POINT('Ctrl Pts',(45.3020778865304,-59.7307512232088,
-39.5816566699808));
#267163=CARTESIAN_POINT('Ctrl Pts',(45.2658207361194,-59.7424779971954,
-39.5774690525214));
#267164=CARTESIAN_POINT('Ctrl Pts',(45.1926264722126,-59.7641596130402,
-39.5686714999982));
#267165=CARTESIAN_POINT('Ctrl Pts',(45.1555073953157,-59.7741562626731,
-39.564037603403));
#267166=CARTESIAN_POINT('Ctrl Pts',(45.0812568521898,-59.7921790679244,
-39.5544265573043));
#267167=CARTESIAN_POINT('Ctrl Pts',(45.0440817338732,-59.8002278006182,
-39.5494458265502));
#267168=CARTESIAN_POINT('Ctrl Pts',(44.9696261100397,-59.8144410792825,
-39.5391390379963));
#267169=CARTESIAN_POINT('Ctrl Pts',(44.9323469858339,-59.8206061957129,
-39.5338133160118));
#267170=CARTESIAN_POINT('Ctrl Pts',(44.8576879157223,-59.8310833922412,
-39.5228216447761));
#267171=CARTESIAN_POINT('Ctrl Pts',(44.8203079641943,-59.8353953722009,
-39.5171556783342));
#267172=CARTESIAN_POINT('Ctrl Pts',(44.7080184591272,-59.8455760729762,
-39.4996502652144));
#267173=CARTESIAN_POINT('Ctrl Pts',(44.632937227317,-59.8486931739084,-39.4873001735582));
#267174=CARTESIAN_POINT('Ctrl Pts',(44.5200834460945,-59.8478515250362,
-39.4677634677006));
#267175=CARTESIAN_POINT('Ctrl Pts',(44.4823810889441,-59.8466449835469,
-39.461073637211));
#267176=CARTESIAN_POINT('Ctrl Pts',(44.4258051094776,-59.8434394823804,
-39.4507883306211));
#267177=CARTESIAN_POINT('Ctrl Pts',(44.4069254604469,-59.8421361463935,
-39.447314779011));
#267178=CARTESIAN_POINT('Ctrl Pts',(44.3691376555635,-59.8390581742043,
-39.4402793205582));
#267179=CARTESIAN_POINT('Ctrl Pts',(44.3502459363124,-59.8372838851304,
-39.4367202978598));
#267180=CARTESIAN_POINT('Ctrl Pts',(44.2938476179289,-59.8312837006341,
-39.4259706152766));
#267181=CARTESIAN_POINT('Ctrl Pts',(44.2565162770547,-59.8263768713198,
-39.4186892503679));
#267182=CARTESIAN_POINT('Ctrl Pts',(44.1823865429402,-59.8147890323227,
-39.403902149315));
#267183=CARTESIAN_POINT('Ctrl Pts',(44.1455864852429,-59.8081083873803,
-39.3963961932961));
#267184=CARTESIAN_POINT('Ctrl Pts',(44.0359682133432,-59.7854494436508,
-39.3735449791568));
#267185=CARTESIAN_POINT('Ctrl Pts',(43.9639303525491,-59.7668593234827,
-39.3578670253851));
#267186=CARTESIAN_POINT('Ctrl Pts',(43.8219159030999,-59.7227861766851,
-39.3256251105404));
#267187=CARTESIAN_POINT('Ctrl Pts',(43.7519290521664,-59.6972943177331,
-39.3090578161669));
#267188=CARTESIAN_POINT('Ctrl Pts',(43.6657831761406,-59.6610675917225,
-39.2877890362312));
#267189=CARTESIAN_POINT('Ctrl Pts',(43.6486106649973,-59.6535962089239,
-39.2835041155108));
#267190=CARTESIAN_POINT('Ctrl Pts',(43.6144192997846,-59.6382222468611,
-39.2748825057904));
#267191=CARTESIAN_POINT('Ctrl Pts',(43.5973665810138,-59.6303022461252,
-39.2705368798388));
#267192=CARTESIAN_POINT('Ctrl Pts',(43.5465994162094,-59.6059619140424,
-39.257461632632));
#267193=CARTESIAN_POINT('Ctrl Pts',(43.5133292984396,-59.5889931218502,
-39.248708514221));
#267194=CARTESIAN_POINT('Ctrl Pts',(43.4805771050572,-59.5712767635336,
-39.239908023115));
#267195=CARTESIAN_POINT('Ctrl Pts',(43.5555686724225,-59.2341331371673,
-39.6401254388889));
#267196=CARTESIAN_POINT('Ctrl Pts',(43.5271056611467,-59.2187194887567,
-39.631324947783));
#267197=CARTESIAN_POINT('Ctrl Pts',(43.4991050718461,-59.2026631797235,
-39.6224809838115));
#267198=CARTESIAN_POINT('Ctrl Pts',(43.4440150113987,-59.1692845399769,
-39.6047067940149));
#267199=CARTESIAN_POINT('Ctrl Pts',(43.4169255850374,-59.1519621466579,
-39.5957765649991));
#267200=CARTESIAN_POINT('Ctrl Pts',(43.3370131802655,-59.0981112314642,
-39.5688567319499));
#267201=CARTESIAN_POINT('Ctrl Pts',(43.285543194378,-59.0597029400212,-39.5507382076943));
#267202=CARTESIAN_POINT('Ctrl Pts',(43.1862317502577,-58.9778465535662,
-39.5141524664308));
#267203=CARTESIAN_POINT('Ctrl Pts',(43.1383853322497,-58.934394522841,-39.4956834538053));
#267204=CARTESIAN_POINT('Ctrl Pts',(43.04646128557,-58.8422990997139,-39.4583907231793));
#267205=CARTESIAN_POINT('Ctrl Pts',(43.0031141723556,-58.7943892422201,
-39.4398637091582));
#267206=CARTESIAN_POINT('Ctrl Pts',(42.9214551605844,-58.6949439395988,
-39.403031369754));
#267207=CARTESIAN_POINT('Ctrl Pts',(42.8831478057343,-58.6434120405259,
-39.3847276759222));
#267208=CARTESIAN_POINT('Ctrl Pts',(42.8294513147831,-58.5634133385806,
-39.3574414811757));
#267209=CARTESIAN_POINT('Ctrl Pts',(42.8121809030637,-58.5362962456352,
-39.3483743629814));
#267210=CARTESIAN_POINT('Ctrl Pts',(42.7789072078242,-58.4811528510598,
-39.33029755848));
#267211=CARTESIAN_POINT('Ctrl Pts',(42.7629038607078,-58.4531265953729,
-39.3212878681428));
#267212=CARTESIAN_POINT('Ctrl Pts',(42.7321834511559,-58.3961509948357,
-39.3033273013551));
#267213=CARTESIAN_POINT('Ctrl Pts',(42.7174700031016,-58.3672093155525,
-39.2943787390014));
#267214=CARTESIAN_POINT('Ctrl Pts',(42.689343821659,-58.3083513101081,-39.2765331188783));
#267215=CARTESIAN_POINT('Ctrl Pts',(42.6760415140178,-58.2786638018862,
-39.2677056541075));
#267216=CARTESIAN_POINT('Ctrl Pts',(42.6509587993318,-58.2188370725527,
-39.2502559046012));
#267217=CARTESIAN_POINT('Ctrl Pts',(42.6391736156063,-58.1886877789828,
-39.241630573039));
#267218=CARTESIAN_POINT('Ctrl Pts',(42.6171007474472,-58.127923813745,-39.2245782718256));
#267219=CARTESIAN_POINT('Ctrl Pts',(42.6068129739072,-58.0973088328386,
-39.2161512192883));
#267220=CARTESIAN_POINT('Ctrl Pts',(42.5781879491669,-58.0047670192766,
-39.1911676757355));
#267221=CARTESIAN_POINT('Ctrl Pts',(42.5620836311909,-57.942142746375,-39.1749075665151));
#267222=CARTESIAN_POINT('Ctrl Pts',(42.5424630372967,-57.846799679813,-39.1511279281964));
#267223=CARTESIAN_POINT('Ctrl Pts',(42.5366792610313,-57.8147773284237,
-39.1433017954548));
#267224=CARTESIAN_POINT('Ctrl Pts',(42.5266555052792,-57.7502670865121,
-39.1278612669093));
#267225=CARTESIAN_POINT('Ctrl Pts',(42.5224105823978,-57.7177326388165,
-39.1202361851916));
#267226=CARTESIAN_POINT('Ctrl Pts',(42.5155191585571,-57.6523285347624,
-39.1052370705839));
#267227=CARTESIAN_POINT('Ctrl Pts',(42.5128931531363,-57.6196821975634,
-39.0979136485113));
#267228=CARTESIAN_POINT('Ctrl Pts',(42.5092445696619,-57.5543872405645,
-39.0835894408895));
#267229=CARTESIAN_POINT('Ctrl Pts',(42.5082239674359,-57.5217574535128,
-39.076592971793));
#267230=CARTESIAN_POINT('Ctrl Pts',(42.5075539730829,-57.4239204642568,
-39.0560983673755));
#267231=CARTESIAN_POINT('Ctrl Pts',(42.5102910904574,-57.3587655206248,
-39.0430939199314));
#267232=CARTESIAN_POINT('Ctrl Pts',(42.5192012104666,-57.261137180212,-39.0245887021893));
#267233=CARTESIAN_POINT('Ctrl Pts',(42.5229732500635,-57.2286117736555,
-39.0185874646267));
#267234=CARTESIAN_POINT('Ctrl Pts',(42.5321441805056,-57.1635960137018,
-39.0069253566698));
#267235=CARTESIAN_POINT('Ctrl Pts',(42.5375464746252,-57.1310926165026,
-39.0012624667841));
#267236=CARTESIAN_POINT('Ctrl Pts',(42.5499988642966,-57.0661736081024,
-38.9902936182087));
#267237=CARTESIAN_POINT('Ctrl Pts',(42.5570855845251,-57.0336218831051,
-38.9849668275436));
#267238=CARTESIAN_POINT('Ctrl Pts',(42.5727869142399,-56.9692679819142,
-38.9747847070689));
#267239=CARTESIAN_POINT('Ctrl Pts',(42.5814158886332,-56.9373636193352,
-38.9699110349254));
#267240=CARTESIAN_POINT('Ctrl Pts',(42.6002039592955,-56.8741385048671,
-38.960602206569));
#267241=CARTESIAN_POINT('Ctrl Pts',(42.610364008329,-56.8428100439228,-38.9561656388506));
#267242=CARTESIAN_POINT('Ctrl Pts',(42.6322067310083,-56.78071772285,-38.9477266173214));
#267243=CARTESIAN_POINT('Ctrl Pts',(42.6438894125866,-56.7499538657306,
-38.943724165076));
#267244=CARTESIAN_POINT('Ctrl Pts',(42.6687792295882,-56.6889913336959,
-38.936154911583));
#267245=CARTESIAN_POINT('Ctrl Pts',(42.6819863498137,-56.6587926531977,
-38.9325881054662));
#267246=CARTESIAN_POINT('Ctrl Pts',(42.709938107711,-56.5989652286031,-38.9258948107753));
#267247=CARTESIAN_POINT('Ctrl Pts',(42.7246827057262,-56.5693364698414,
-38.9227683104938));
#267248=CARTESIAN_POINT('Ctrl Pts',(42.7557342012492,-56.5106579944336,
-38.9169635697921));
#267249=CARTESIAN_POINT('Ctrl Pts',(42.7720314608922,-56.481624481206,-38.9142867097661));
#267250=CARTESIAN_POINT('Ctrl Pts',(42.8062640059245,-56.424085389993,-38.9093871432694));
#267251=CARTESIAN_POINT('Ctrl Pts',(42.8240692231992,-56.395799847901,-38.9071833532006));
#267252=CARTESIAN_POINT('Ctrl Pts',(42.8793344551428,-56.3126949484312,
-38.9013282621221));
#267253=CARTESIAN_POINT('Ctrl Pts',(42.918743168177,-56.2594003210213,-38.8984064421158));
#267254=CARTESIAN_POINT('Ctrl Pts',(43.0025483564193,-56.1570717858067,
-38.8945084542909));
#267255=CARTESIAN_POINT('Ctrl Pts',(43.0469649474229,-56.1080069069945,
-38.8935300021871));
#267256=CARTESIAN_POINT('Ctrl Pts',(43.1173450441481,-56.0376381601557,
-38.8935323891605));
#267257=CARTESIAN_POINT('Ctrl Pts',(43.141458661058,-56.0146990549453,-38.8937796039308));
#267258=CARTESIAN_POINT('Ctrl Pts',(43.1785611799511,-55.9811320384022,
-38.8945237100665));
#267259=CARTESIAN_POINT('Ctrl Pts',(43.1910978407718,-55.9700723375204,
-38.8948345555296));
#267260=CARTESIAN_POINT('Ctrl Pts',(43.2164884775807,-55.9482337293115,
-38.8955820938649));
#267261=CARTESIAN_POINT('Ctrl Pts',(43.2293524555614,-55.9374477670517,
-38.8960194067973));
#267262=CARTESIAN_POINT('Ctrl Pts',(43.2682109535356,-55.9056902236256,
-38.8975137012045));
#267263=CARTESIAN_POINT('Ctrl Pts',(43.2945320232725,-55.8852608728333,
-38.8987534360506));
#267264=CARTESIAN_POINT('Ctrl Pts',(43.3480000930852,-55.8458485303625,
-38.9017105364692));
#267265=CARTESIAN_POINT('Ctrl Pts',(43.3751449489233,-55.8268667058867,
-38.9034276958876));
#267266=CARTESIAN_POINT('Ctrl Pts',(43.4577944294251,-55.7720632464052,
-38.9092840615924));
#267267=CARTESIAN_POINT('Ctrl Pts',(43.5145113713215,-55.7383790557516,
-38.9141267100279));
#267268=CARTESIAN_POINT('Ctrl Pts',(43.6019984165122,-55.6921042709396,
-38.922785850023));
#267269=CARTESIAN_POINT('Ctrl Pts',(43.6315633864957,-55.6773891287914,
-38.9259051413184));
#267270=CARTESIAN_POINT('Ctrl Pts',(43.6915052875854,-55.6493901621927,
-38.9326125532154));
#267271=CARTESIAN_POINT('Ctrl Pts',(43.7218909351156,-55.636103784993,-38.9362019665749));
#267272=CARTESIAN_POINT('Ctrl Pts',(43.7834518747983,-55.6109945714021,
-38.9438507097857));
#267273=CARTESIAN_POINT('Ctrl Pts',(43.8147379997369,-55.5991384576554,
-38.9479262894259));
#267274=CARTESIAN_POINT('Ctrl Pts',(43.8773632788004,-55.5771771251162,
-38.9564520459569));
#267275=CARTESIAN_POINT('Ctrl Pts',(43.9088373867163,-55.5670128138588,
-38.9609181476403));
#267276=CARTESIAN_POINT('Ctrl Pts',(43.9720262136544,-55.5483136978037,
-38.9702378118119));
#267277=CARTESIAN_POINT('Ctrl Pts',(44.0037536788592,-55.5397733548593,
-38.9750928878619));
#267278=CARTESIAN_POINT('Ctrl Pts',(44.0674709230106,-55.5242871663795,
-38.985186610612));
#267279=CARTESIAN_POINT('Ctrl Pts',(44.099460707948,-55.5173413577782,-38.9904252668586));
#267280=CARTESIAN_POINT('Ctrl Pts',(44.1637007891551,-55.5050323653042,
-39.0012821079516));
#267281=CARTESIAN_POINT('Ctrl Pts',(44.1959510873779,-55.4996691938696,
-39.0069002965142));
#267282=CARTESIAN_POINT('Ctrl Pts',(44.260712289499,-55.4905251021207,-39.0185148869209));
#267283=CARTESIAN_POINT('Ctrl Pts',(44.2932231914844,-55.4867441708206,
-39.0245112869446));
#267284=CARTESIAN_POINT('Ctrl Pts',(44.3585075922001,-55.480775674059,-39.0368836954053));
#267285=CARTESIAN_POINT('Ctrl Pts',(44.3912828804572,-55.4785888313245,
-39.0432602233464));
#267286=CARTESIAN_POINT('Ctrl Pts',(44.4570928290005,-55.4758284917783,
-39.0563949677075));
#267287=CARTESIAN_POINT('Ctrl Pts',(44.4901876958509,-55.4752622617633,
-39.0631671834262));
#267288=CARTESIAN_POINT('Ctrl Pts',(44.5558452176361,-55.475758769118,-39.0769304140694));
#267289=CARTESIAN_POINT('Ctrl Pts',(44.5885615120018,-55.4768128312226,
-39.0839516406405));
#267290=CARTESIAN_POINT('Ctrl Pts',(44.6536812736587,-55.4805035202407,
-39.0982478716216));
#267291=CARTESIAN_POINT('Ctrl Pts',(44.6861004221968,-55.483139401189,-39.1055259894705));
#267292=CARTESIAN_POINT('Ctrl Pts',(44.7829419444318,-55.4933852274058,
-39.1277430575141));
#267293=CARTESIAN_POINT('Ctrl Pts',(44.8469492543596,-55.503328533356,-39.1430639225963));
#267294=CARTESIAN_POINT('Ctrl Pts',(44.9421361647843,-55.5228829035947,
-39.1667978233991));
#267295=CARTESIAN_POINT('Ctrl Pts',(44.9737275643282,-55.5301755370665,
-39.1748347739215));
#267296=CARTESIAN_POINT('Ctrl Pts',(45.0366332915956,-55.546321762157,-39.1911608566696));
#267297=CARTESIAN_POINT('Ctrl Pts',(45.0679417334004,-55.5551739760488,
-39.1994484880529));
#267298=CARTESIAN_POINT('Ctrl Pts',(45.1303012298678,-55.5744676215724,
-39.216284615773));
#267299=CARTESIAN_POINT('Ctrl Pts',(45.1613392597803,-55.5849120617205,
-39.2248309851518));
#267300=CARTESIAN_POINT('Ctrl Pts',(45.2225442622987,-55.6071884247806,
-39.2420155999886));
#267301=CARTESIAN_POINT('Ctrl Pts',(45.2528226925233,-55.6190538405798,
-39.2506837416077));
#267302=CARTESIAN_POINT('Ctrl Pts',(45.3126694117909,-55.6442020485079,
-39.2681505662992));
#267303=CARTESIAN_POINT('Ctrl Pts',(45.3422493331638,-55.6574883926309,
-39.2769523813226));
#267304=CARTESIAN_POINT('Ctrl Pts',(45.4007251529718,-55.6854799817093,
-39.2946915606304));
#267305=CARTESIAN_POINT('Ctrl Pts',(45.4296210506442,-55.7001852280132,
-39.3036289255364));
#267306=CARTESIAN_POINT('Ctrl Pts',(45.4867267714294,-55.7310191704249,
-39.3216390153311));
#267307=CARTESIAN_POINT('Ctrl Pts',(45.5149281650798,-55.7471427624975,
-39.3307089736211));
#267308=CARTESIAN_POINT('Ctrl Pts',(45.5706716223774,-55.7808485275847,
-39.3489961904353));
#267309=CARTESIAN_POINT('Ctrl Pts',(45.5980415806017,-55.7983262695069,
-39.3581569149896));
#267310=CARTESIAN_POINT('Ctrl Pts',(45.6785018446286,-55.8525001852937,
-39.3856333194591));
#267311=CARTESIAN_POINT('Ctrl Pts',(45.7300942897426,-55.891002260239,-39.4039877669757));
#267312=CARTESIAN_POINT('Ctrl Pts',(45.8291740542806,-55.9726262256725,
-39.4407364897739));
#267313=CARTESIAN_POINT('Ctrl Pts',(45.8766787967759,-56.0157556232289,
-39.459135894828));
#267314=CARTESIAN_POINT('Ctrl Pts',(45.9448683025546,-56.0839428568353,
-39.4867725989864));
#267315=CARTESIAN_POINT('Ctrl Pts',(45.9670860951877,-56.1072550024018,
-39.4959911211427));
#267316=CARTESIAN_POINT('Ctrl Pts',(46.0104840259957,-56.1550608350904,
-39.5144410445764));
#267317=CARTESIAN_POINT('Ctrl Pts',(46.0316551416961,-56.1795437819113,
-39.5236684527303));
#267318=CARTESIAN_POINT('Ctrl Pts',(46.0626450692445,-56.217204251931,-39.5375315768857));
#267319=CARTESIAN_POINT('Ctrl Pts',(46.0728378849325,-56.2299042093275,
-39.5421524573076));
#267320=CARTESIAN_POINT('Ctrl Pts',(46.092851018773,-56.2554719148758,-39.551348880014));
#267321=CARTESIAN_POINT('Ctrl Pts',(46.1026913195214,-56.2683637173689,
-39.555933316569));
#267322=CARTESIAN_POINT('Ctrl Pts',(46.1316838232885,-56.3073187525545,
-39.5696305214535));
#267323=CARTESIAN_POINT('Ctrl Pts',(46.1503365283638,-56.3336962107827,
-39.5787000086301));
#267324=CARTESIAN_POINT('Ctrl Pts',(46.2042529621824,-56.4139852215082,
-39.60570727654));
#267325=CARTESIAN_POINT('Ctrl Pts',(46.2375105436952,-56.4690891650644,
-39.6234582594478));
#267326=CARTESIAN_POINT('Ctrl Pts',(46.2833698408561,-56.5540829658312,
-39.6497025405486));
#267327=CARTESIAN_POINT('Ctrl Pts',(46.2979848351363,-56.5828054986343,
-39.658387207326));
#267328=CARTESIAN_POINT('Ctrl Pts',(46.3258604890836,-56.6410396034225,
-39.6756293217671));
#267329=CARTESIAN_POINT('Ctrl Pts',(46.3391212174584,-56.6705511356645,
-39.684186774641));
#267330=CARTESIAN_POINT('Ctrl Pts',(46.3642673689533,-56.7303752678074,
-39.7011732901024));
#267331=CARTESIAN_POINT('Ctrl Pts',(46.3761460085845,-56.7606694672189,
-39.7095973250063));
#267332=CARTESIAN_POINT('Ctrl Pts',(46.3985236982386,-56.8221506262249,
-39.7263350672961));
#267333=CARTESIAN_POINT('Ctrl Pts',(46.4089539001758,-56.8531540104908,
-39.7345983819507));
#267334=CARTESIAN_POINT('Ctrl Pts',(46.4378289889335,-56.9464971479131,
-39.7589545662051));
#267335=CARTESIAN_POINT('Ctrl Pts',(46.4539730140977,-57.0094025598672,
-39.774683215309));
#267336=CARTESIAN_POINT('Ctrl Pts',(46.480079447285,-57.1364634819838,-39.8051172322268));
#267337=CARTESIAN_POINT('Ctrl Pts',(46.490051050886,-57.2006341137638,-39.8198274613562));
#267338=CARTESIAN_POINT('Ctrl Pts',(46.5003164047383,-57.2978585625442,
-39.8411267672249));
#267339=CARTESIAN_POINT('Ctrl Pts',(46.5029550484688,-57.3304317173846,
-39.8480993416622));
#267340=CARTESIAN_POINT('Ctrl Pts',(46.5066366277352,-57.3959005137752,
-39.8617837974953));
#267341=CARTESIAN_POINT('Ctrl Pts',(46.5076798542157,-57.4288266558715,
-39.8685017640589));
#267342=CARTESIAN_POINT('Ctrl Pts',(46.5081286131878,-57.4949099337061,
-39.8816515992078));
#267343=CARTESIAN_POINT('Ctrl Pts',(46.5075346190154,-57.5278165861342,
-39.8880340709103));
#267344=CARTESIAN_POINT('Ctrl Pts',(46.5047360881509,-57.5934606456236,
-39.900440518001));
#267345=CARTESIAN_POINT('Ctrl Pts',(46.502531400808,-57.626181768562,-39.9064612439072));
#267346=CARTESIAN_POINT('Ctrl Pts',(46.4935219657065,-57.7240448203298,
-39.923982362838));
#267347=CARTESIAN_POINT('Ctrl Pts',(46.4843271372358,-57.7888870954909,
-39.9349428927655));
#267348=CARTESIAN_POINT('Ctrl Pts',(46.4657292594294,-57.8855471837123,
-39.9503047442402));
#267349=CARTESIAN_POINT('Ctrl Pts',(46.458727758375,-57.9176665005431,-39.9552452454648));
#267350=CARTESIAN_POINT('Ctrl Pts',(46.4430984605719,-57.9817008313272,
-39.9647621435255));
#267351=CARTESIAN_POINT('Ctrl Pts',(46.4344657419777,-58.0136292048186,
-39.9693401953313));
#267352=CARTESIAN_POINT('Ctrl Pts',(46.4155601083816,-58.0772238658133,
-39.9781190500757));
#267353=CARTESIAN_POINT('Ctrl Pts',(46.405235422408,-58.1090273916134,-39.9823366235341));
#267354=CARTESIAN_POINT('Ctrl Pts',(46.3831322370528,-58.1717233081051,
-39.9903045886339));
#267355=CARTESIAN_POINT('Ctrl Pts',(46.3713308475608,-58.2027120874814,
-39.9940694297706));
#267356=CARTESIAN_POINT('Ctrl Pts',(46.3462591752663,-58.2639408858517,
-40.0011617906564));
#267357=CARTESIAN_POINT('Ctrl Pts',(46.3329874273489,-58.2941877852093,
-40.0044903745716));
#267358=CARTESIAN_POINT('Ctrl Pts',(46.3049830003936,-58.3539519689038,
-40.0107163415784));
#267359=CARTESIAN_POINT('Ctrl Pts',(46.2902503101408,-58.383469247682,-40.0136137207465));
#267360=CARTESIAN_POINT('Ctrl Pts',(46.2593240500028,-58.4417741675014,
-40.0189779749618));
#267361=CARTESIAN_POINT('Ctrl Pts',(46.2431304912238,-58.470561814118,-40.0214448528642));
#267362=CARTESIAN_POINT('Ctrl Pts',(46.2092717726407,-58.5274020727665,
-40.0259455366297));
#267363=CARTESIAN_POINT('Ctrl Pts',(46.1916066472402,-58.5554547019966,
-40.0279793523959));
#267364=CARTESIAN_POINT('Ctrl Pts',(46.1547828992827,-58.6108139537738,
-40.0316079667071));
#267365=CARTESIAN_POINT('Ctrl Pts',(46.1356370939371,-58.6381031491859,
-40.033201863178));
#267366=CARTESIAN_POINT('Ctrl Pts',(46.0957670512506,-58.6919883971087,
-40.0359447517529));
#267367=CARTESIAN_POINT('Ctrl Pts',(46.075181231902,-58.7183945160565,-40.0370836630407));
#267368=CARTESIAN_POINT('Ctrl Pts',(46.0117863921084,-58.7956387234688,
-40.0397935265569));
#267369=CARTESIAN_POINT('Ctrl Pts',(45.9672001304834,-58.844745304603,-40.0406777816202));
#267370=CARTESIAN_POINT('Ctrl Pts',(45.8735323130258,-58.9381754480581,
-40.0406312846123));
#267371=CARTESIAN_POINT('Ctrl Pts',(45.8244354693604,-58.9825217206044,
-40.0397019843559));
#267372=CARTESIAN_POINT('Ctrl Pts',(45.7474002842578,-59.0454399658155,
-40.0369397419404));
#267373=CARTESIAN_POINT('Ctrl Pts',(45.7211400913291,-59.0658221063687,
-40.0357895194905));
#267374=CARTESIAN_POINT('Ctrl Pts',(45.6809048277922,-59.0954685233027,
-40.0337171756965));
#267375=CARTESIAN_POINT('Ctrl Pts',(45.6673394345786,-59.1052045384925,
-40.0329676840834));
#267376=CARTESIAN_POINT('Ctrl Pts',(45.6399357364193,-59.1243566232342,
-40.0313525371172));
#267377=CARTESIAN_POINT('Ctrl Pts',(45.6260670111341,-59.1337924862528,
-40.0304848012205));
#267378=CARTESIAN_POINT('Ctrl Pts',(45.5842146021532,-59.161503832051,-40.0277164279032));
#267379=CARTESIAN_POINT('Ctrl Pts',(45.5559971110396,-59.1791823026862,
-40.0256529103855));
#267380=CARTESIAN_POINT('Ctrl Pts',(45.4988812016502,-59.2130235382979,
-40.0210947294542));
#267381=CARTESIAN_POINT('Ctrl Pts',(45.4699934991806,-59.2291795021203,
-40.0186008323348));
#267382=CARTESIAN_POINT('Ctrl Pts',(45.3823565697306,-59.2753890254871,
-40.010483831197));
#267383=CARTESIAN_POINT('Ctrl Pts',(45.322635564301,-59.3031889643499,-40.0042267981133));
#267384=CARTESIAN_POINT('Ctrl Pts',(45.2311263675532,-59.3404176099272,
-39.9935791348688));
#267385=CARTESIAN_POINT('Ctrl Pts',(45.2003014699612,-59.352080669579,-39.9898191937811));
#267386=CARTESIAN_POINT('Ctrl Pts',(45.1380036116915,-59.373903446149,-39.9818740857548));
#267387=CARTESIAN_POINT('Ctrl Pts',(45.1065143262852,-59.3840670181506,
-39.9776864682954));
#267388=CARTESIAN_POINT('Ctrl Pts',(45.0429439840219,-59.4028543289242,
-39.9688889157721));
#267389=CARTESIAN_POINT('Ctrl Pts',(45.0107048817299,-59.4115142672699,
-39.9642550191769));
#267390=CARTESIAN_POINT('Ctrl Pts',(44.946214704594,-59.4271222445478,-39.9546439730782));
#267391=CARTESIAN_POINT('Ctrl Pts',(44.9139257231678,-59.4340898684192,
-39.9496632423241));
#267392=CARTESIAN_POINT('Ctrl Pts',(44.8492550541234,-59.4463881271609,
-39.9393564537703));
#267393=CARTESIAN_POINT('Ctrl Pts',(44.8168745667947,-59.4517192585513,
-39.9340307317858));
#267394=CARTESIAN_POINT('Ctrl Pts',(44.7520248705109,-59.4607715904943,
-39.92303906055));
#267395=CARTESIAN_POINT('Ctrl Pts',(44.7195556566076,-59.4644927040579,
-39.9173730941082));
#267396=CARTESIAN_POINT('Ctrl Pts',(44.6220163194673,-59.4732622640888,
-39.8998676809884));
#267397=CARTESIAN_POINT('Ctrl Pts',(44.5567953679904,-59.4759200591614,
-39.8875175893321));
#267398=CARTESIAN_POINT('Ctrl Pts',(44.458759050957,-59.4751132746956,-39.8679808834745));
#267399=CARTESIAN_POINT('Ctrl Pts',(44.4260063620395,-59.4740398065978,
-39.861291052985));
#267400=CARTESIAN_POINT('Ctrl Pts',(44.376856965898,-59.4712170391416,-39.851005746395));
#267401=CARTESIAN_POINT('Ctrl Pts',(44.3604554548704,-59.4700720815201,
-39.8475321947849));
#267402=CARTESIAN_POINT('Ctrl Pts',(44.3276273759585,-59.4673726892737,
-39.8404967363322));
#267403=CARTESIAN_POINT('Ctrl Pts',(44.3112150867197,-59.4658185672318,
-39.8369377136338));
#267404=CARTESIAN_POINT('Ctrl Pts',(44.262218286448,-59.4605679436367,-39.8261880310505));
#267405=CARTESIAN_POINT('Ctrl Pts',(44.2297855973829,-59.4562799745141,
-39.8189066661417));
#267406=CARTESIAN_POINT('Ctrl Pts',(44.1653820777189,-59.4461630097037,
-39.804119565089));
#267407=CARTESIAN_POINT('Ctrl Pts',(44.1334098014393,-59.4403343297903,
-39.79661360907));
#267408=CARTESIAN_POINT('Ctrl Pts',(44.0381705583581,-59.4205751896199,
-39.7737623949309));
#267409=CARTESIAN_POINT('Ctrl Pts',(43.9755798363749,-59.4043761343586,
-39.758084441159));
#267410=CARTESIAN_POINT('Ctrl Pts',(43.8521846091923,-59.3659909301588,
-39.7258425263144));
#267411=CARTESIAN_POINT('Ctrl Pts',(43.7913711836815,-59.3437971009265,
-39.7092752319402));
#267412=CARTESIAN_POINT('Ctrl Pts',(43.7165136160533,-59.3122661488096,
-39.6880064520053));
#267413=CARTESIAN_POINT('Ctrl Pts',(43.7015911797635,-59.3057636179843,
-39.6837215312847));
#267414=CARTESIAN_POINT('Ctrl Pts',(43.6718795073988,-59.2923840419977,
-39.6750999215644));
#267415=CARTESIAN_POINT('Ctrl Pts',(43.6570608420848,-59.2854918386329,
-39.6707542956128));
#267416=CARTESIAN_POINT('Ctrl Pts',(43.6129441176106,-59.2643113087757,
-39.657679048406));
#267417=CARTESIAN_POINT('Ctrl Pts',(43.5840316836982,-59.2495467855778,
-39.6489259299949));
#267418=CARTESIAN_POINT('Ctrl Pts',(43.5555686724225,-59.2341331371673,
-39.6401254388889));
#267419=CARTESIAN_POINT('Ctrl Pts',(46.5057031838161,-57.5702877290152,
-39.8960534363005));
#267420=CARTESIAN_POINT('Ctrl Pts',(46.5058563971114,-57.5670514245044,
-39.8954454022393));
#267421=CARTESIAN_POINT('Ctrl Pts',(46.5060007398109,-57.5638457317421,
-39.8948410900405));
#267422=CARTESIAN_POINT('Ctrl Pts',(46.5061374457113,-57.5606390745173,
-39.894235046025));
#267423=CARTESIAN_POINT('Ctrl Pts',(46.5075367124945,-57.527817016895,-39.8880318224796));
#267424=CARTESIAN_POINT('Ctrl Pts',(46.508130707335,-57.4949103365212,-39.8816493507771));
#267425=CARTESIAN_POINT('Ctrl Pts',(46.5079063278233,-57.4618686695473,
-39.8750744332027));
#267426=CARTESIAN_POINT('Ctrl Pts',(46.5076819483115,-57.4288270025733,
-39.8684995156283));
#267427=CARTESIAN_POINT('Ctrl Pts',(46.5066387211099,-57.3959008325223,
-39.8617815490646));
#267428=CARTESIAN_POINT('Ctrl Pts',(46.5047979300779,-57.3631664065387,
-39.854939321148));
#267429=CARTESIAN_POINT('Ctrl Pts',(46.5029571390459,-57.3304319805551,
-39.8480970932315));
#267430=CARTESIAN_POINT('Ctrl Pts',(46.5003186115917,-57.2978599190912,
-39.8411247640299));
#267431=CARTESIAN_POINT('Ctrl Pts',(46.4968968273198,-57.2654506330812,
-39.8340246192596));
#267432=CARTESIAN_POINT('Ctrl Pts',(46.490053258776,-57.2006320610612,-39.819824329719));
#267433=CARTESIAN_POINT('Ctrl Pts',(46.4800815194185,-57.1364635805499,
-39.8051149837962));
#267434=CARTESIAN_POINT('Ctrl Pts',(46.4670282920657,-57.0729330656046,
-39.7898979753373));
#267435=CARTESIAN_POINT('Ctrl Pts',(46.4539750647129,-57.0094025506593,
-39.7746809668783));
#267436=CARTESIAN_POINT('Ctrl Pts',(46.437831026164,-56.9464970853635,-39.7589523177745));
#267437=CARTESIAN_POINT('Ctrl Pts',(46.4185809509685,-56.8842682743296,
-39.7427148616048));
#267438=CARTESIAN_POINT('Ctrl Pts',(46.4089559133708,-56.8531538688126,
-39.73459613352));
#267439=CARTESIAN_POINT('Ctrl Pts',(46.3985257027381,-56.8221504582685,
-39.7263328188654));
#267440=CARTESIAN_POINT('Ctrl Pts',(46.3873368485705,-56.7914098527142,
-39.7179639477205));
#267441=CARTESIAN_POINT('Ctrl Pts',(46.3761479944029,-56.7606692471599,
-39.7095950765756));
#267442=CARTESIAN_POINT('Ctrl Pts',(46.3642693448436,-56.7303750220794,
-39.7011710416717));
#267443=CARTESIAN_POINT('Ctrl Pts',(46.3516962585769,-56.7004629306669,
-39.692677783941));
#267444=CARTESIAN_POINT('Ctrl Pts',(46.3391231723103,-56.6705508392544,
-39.6841845262104));
#267445=CARTESIAN_POINT('Ctrl Pts',(46.3258624209486,-56.6410391769107,
-39.6756270022281));
#267446=CARTESIAN_POINT('Ctrl Pts',(46.3119246240029,-56.6119222266148,
-39.6670060026179));
#267447=CARTESIAN_POINT('Ctrl Pts',(46.2979868270572,-56.5828052763188,
-39.6583850030077));
#267448=CARTESIAN_POINT('Ctrl Pts',(46.2833719995868,-56.5540830376329,
-39.6497004356907));
#267449=CARTESIAN_POINT('Ctrl Pts',(46.2680854169705,-56.5257513241111,
-39.6409521228394));
#267450=CARTESIAN_POINT('Ctrl Pts',(46.2375122517372,-56.4690878970724,
-39.6234554971376));
#267451=CARTESIAN_POINT('Ctrl Pts',(46.2042548038769,-56.4139847078702,
-39.6057050281093));
#267452=CARTESIAN_POINT('Ctrl Pts',(46.1683104844322,-56.3604586554391,
-39.587700182836));
#267453=CARTESIAN_POINT('Ctrl Pts',(46.1503383247098,-56.3336956292236,
-39.5786977601994));
#267454=CARTESIAN_POINT('Ctrl Pts',(46.1316856039389,-56.3073181486858,
-39.5696282730228));
#267455=CARTESIAN_POINT('Ctrl Pts',(46.1123572518232,-56.2813481032686,
-39.5604968030998));
#267456=CARTESIAN_POINT('Ctrl Pts',(46.1026930757653,-56.2683630805599,
-39.5559310681383));
#267457=CARTESIAN_POINT('Ctrl Pts',(46.0928527667315,-56.2554712671669,
-39.5513466315833));
#267458=CARTESIAN_POINT('Ctrl Pts',(46.0828461913842,-56.2426874035852,
-39.5467484202301));
#267459=CARTESIAN_POINT('Ctrl Pts',(46.0728396160369,-56.2299035400036,
-39.5421502088769));
#267460=CARTESIAN_POINT('Ctrl Pts',(46.0626467917633,-56.2172035718718,
-39.537529328455));
#267461=CARTESIAN_POINT('Ctrl Pts',(46.0523168072112,-56.204650071255,-39.5329082870699));
#267462=CARTESIAN_POINT('Ctrl Pts',(46.031656838107,-56.1795430700214,-39.5236662042996));
#267463=CARTESIAN_POINT('Ctrl Pts',(46.0104857045643,-56.1550601025126,
-39.5144387961457));
#267464=CARTESIAN_POINT('Ctrl Pts',(45.9887867208672,-56.1311571659758,
-39.5052138344289));
#267465=CARTESIAN_POINT('Ctrl Pts',(45.96708773717,-56.107254229439,-39.495988872712));
#267466=CARTESIAN_POINT('Ctrl Pts',(45.944869939679,-56.0839420780633,-39.4867703557641));
#267467=CARTESIAN_POINT('Ctrl Pts',(45.9221401573419,-56.0612129236123,
-39.4775579953252));
#267468=CARTESIAN_POINT('Ctrl Pts',(45.8766805926676,-56.0157546147104,
-39.4591332744475));
#267469=CARTESIAN_POINT('Ctrl Pts',(45.8291755799096,-55.9726253390587,
-39.4407342413432));
#267470=CARTESIAN_POINT('Ctrl Pts',(45.7796356558061,-55.9318133219288,
-39.4223598799441));
#267471=CARTESIAN_POINT('Ctrl Pts',(45.7300957317026,-55.891001304799,-39.403985518545));
#267472=CARTESIAN_POINT('Ctrl Pts',(45.6785032430004,-55.8524991974133,
-39.3856310710283));
#267473=CARTESIAN_POINT('Ctrl Pts',(45.6248630216437,-55.8163832231527,
-39.3673134680487));
#267474=CARTESIAN_POINT('Ctrl Pts',(45.5980429109653,-55.7983252360224,
-39.3581546665589));
#267475=CARTESIAN_POINT('Ctrl Pts',(45.5706729296019,-55.7808474793946,
-39.3489939420046));
#267476=CARTESIAN_POINT('Ctrl Pts',(45.5428011773848,-55.7639945826789,
-39.3398503335975));
#267477=CARTESIAN_POINT('Ctrl Pts',(45.5149294251677,-55.7471416859632,
-39.3307067251904));
#267478=CARTESIAN_POINT('Ctrl Pts',(45.4867280076654,-55.7310180803397,
-39.3216367669004));
#267479=CARTESIAN_POINT('Ctrl Pts',(45.4581751231188,-55.7156010961851,
-39.3126317220031));
#267480=CARTESIAN_POINT('Ctrl Pts',(43.4805771074156,-59.5712767529309,
-39.2399080357013));
#267481=CARTESIAN_POINT('Ctrl Pts',(43.4150727209207,-59.5358440364426,
-39.2223070534893));
#267482=CARTESIAN_POINT('Ctrl Pts',(43.2883193276586,-59.4590682572254,
-39.1867578392588));
#267483=CARTESIAN_POINT('Ctrl Pts',(43.1106712693135,-59.32658002426,-39.1324031814995));
#267484=CARTESIAN_POINT('Ctrl Pts',(43.0005921597408,-59.2266373021163,
-39.0954660506179));
#267485=CARTESIAN_POINT('Ctrl Pts',(42.8948534568781,-59.1207134074407,
-39.0581733199915));
#267486=CARTESIAN_POINT('Ctrl Pts',(42.7951360401793,-59.0104958554849,
-39.0211184761739));
#267487=CARTESIAN_POINT('Ctrl Pts',(42.6850011896347,-58.8622904152127,
-38.9753582681256));
#267488=CARTESIAN_POINT('Ctrl Pts',(42.6055727997797,-58.7375004045667,
-38.939089851323));
#267489=CARTESIAN_POINT('Ctrl Pts',(42.5503788594446,-58.6407591922129,
-38.9120596161462));
#267490=CARTESIAN_POINT('Ctrl Pts',(42.5165536369311,-58.5741539171446,
-38.8941613358138));
#267491=CARTESIAN_POINT('Ctrl Pts',(42.4842288567228,-58.5064298632496,
-38.8763157156907));
#267492=CARTESIAN_POINT('Ctrl Pts',(42.4689425396028,-58.4722695523732,
-38.8674882509199));
#267493=CARTESIAN_POINT('Ctrl Pts',(42.4257123024776,-58.3690064948315,
-38.8413136266604));
#267494=CARTESIAN_POINT('Ctrl Pts',(42.3750272156063,-58.229152189777,-38.8072100415055));
#267495=CARTESIAN_POINT('Ctrl Pts',(42.3380647902547,-58.0850119200902,
-38.7746901633276));
#267496=CARTESIAN_POINT('Ctrl Pts',(42.3155659796374,-57.9752818499468,
-38.7509105250088));
#267497=CARTESIAN_POINT('Ctrl Pts',(42.3089374211558,-57.9384266221928,
-38.7430843922672));
#267498=CARTESIAN_POINT('Ctrl Pts',(42.297458012674,-57.864178756387,-38.7276438637217));
#267499=CARTESIAN_POINT('Ctrl Pts',(42.292601515188,-57.8267325312259,-38.720018782004));
#267500=CARTESIAN_POINT('Ctrl Pts',(42.2847289916893,-57.7514526301959,
-38.7050196673963));
#267501=CARTESIAN_POINT('Ctrl Pts',(42.2817363521424,-57.7138759968928,
-38.6976962453237));
#267502=CARTESIAN_POINT('Ctrl Pts',(42.277596992864,-57.6387184974263,-38.6833720377019));
#267503=CARTESIAN_POINT('Ctrl Pts',(42.2741651307842,-57.5260409596698,
-38.6623829091612));
#267504=CARTESIAN_POINT('Ctrl Pts',(42.2805893100654,-57.3760354719141,
-38.6363740800325));
#267505=CARTESIAN_POINT('Ctrl Pts',(42.2937061680812,-57.2637038035873,
-38.618370061439));
#267506=CARTESIAN_POINT('Ctrl Pts',(42.3043247017591,-57.1888547452426,
-38.6067079534822));
#267507=CARTESIAN_POINT('Ctrl Pts',(42.3105743117123,-57.1514345461221,
-38.6010450635964));
#267508=CARTESIAN_POINT('Ctrl Pts',(42.3249704170347,-57.0766935209607,
-38.590076215021));
#267509=CARTESIAN_POINT('Ctrl Pts',(42.3331592025312,-57.0392159768686,
-38.5847494243559));
#267510=CARTESIAN_POINT('Ctrl Pts',(42.3512949844302,-56.9651221381903,
-38.5745673038812));
#267511=CARTESIAN_POINT('Ctrl Pts',(42.3712216906218,-56.8916587034686,
-38.564820665347));
#267512=CARTESIAN_POINT('Ctrl Pts',(42.4063979707918,-56.7834465224234,
-38.5515118436));
#267513=CARTESIAN_POINT('Ctrl Pts',(42.4468320479729,-56.6771725078319,
-38.5395042677724));
#267514=CARTESIAN_POINT('Ctrl Pts',(42.4925290654744,-56.5728473165674,
-38.5288039137004));
#267515=CARTESIAN_POINT('Ctrl Pts',(42.5265325119253,-56.5046058456765,
-38.5225509073062));
#267516=CARTESIAN_POINT('Ctrl Pts',(42.5623338475306,-56.4370293947697,
-38.5167461666044));
#267517=CARTESIAN_POINT('Ctrl Pts',(42.5811223641794,-56.4035923099625,
-38.5140693065785));
#267518=CARTESIAN_POINT('Ctrl Pts',(42.620584523009,-56.3373241998654,-38.5091697400817));
#267519=CARTESIAN_POINT('Ctrl Pts',(42.6411082254821,-56.3047465904101,
-38.5069659500128));
#267520=CARTESIAN_POINT('Ctrl Pts',(42.7048067991197,-56.2090283357163,
-38.501110858935));
#267521=CARTESIAN_POINT('Ctrl Pts',(42.7502234543428,-56.1476408662828,
-38.4981890389281));
#267522=CARTESIAN_POINT('Ctrl Pts',(42.8467942323831,-56.0297655581676,
-38.4942910511033));
#267523=CARTESIAN_POINT('Ctrl Pts',(42.8979715413934,-55.9732420482176,
-38.4933125989996));
#267524=CARTESIAN_POINT('Ctrl Pts',(42.9790570553347,-55.8921695883033,
-38.4933149859729));
#267525=CARTESIAN_POINT('Ctrl Pts',(43.0068374106561,-55.8657400908868,
-38.4935622007431));
#267526=CARTESIAN_POINT('Ctrl Pts',(43.0495800649421,-55.8270637749536,
-38.4943063068789));
#267527=CARTESIAN_POINT('Ctrl Pts',(43.0640222060113,-55.8143203511958,
-38.494617152342));
#267528=CARTESIAN_POINT('Ctrl Pts',(43.0932714774893,-55.7891564261061,
-38.4953646906773));
#267529=CARTESIAN_POINT('Ctrl Pts',(43.1080901283632,-55.7767277938553,
-38.4958020036096));
#267530=CARTESIAN_POINT('Ctrl Pts',(43.1528523310046,-55.7401327167866,
-38.4972962980169));
#267531=CARTESIAN_POINT('Ctrl Pts',(43.2134913856688,-55.6930468850421,
-38.4997758707861));
#267532=CARTESIAN_POINT('Ctrl Pts',(43.3385569247743,-55.6055389451161,
-38.5066450244003));
#267533=CARTESIAN_POINT('Ctrl Pts',(43.4691986576013,-55.5278792007279,
-38.5163302992824));
#267534=CARTESIAN_POINT('Ctrl Pts',(43.5713395927684,-55.4769743237494,
-38.5256877381308));
#267535=CARTESIAN_POINT('Ctrl Pts',(43.6403672861995,-55.4446857735354,
-38.5323951500278));
#267536=CARTESIAN_POINT('Ctrl Pts',(43.6753577685123,-55.4293620157832,
-38.5359845633874));
#267537=CARTESIAN_POINT('Ctrl Pts',(43.7462462065788,-55.4003985583156,
-38.5436333065981));
#267538=CARTESIAN_POINT('Ctrl Pts',(43.7822717759725,-55.3867204456352,
-38.5477088862383));
#267539=CARTESIAN_POINT('Ctrl Pts',(43.8543821738219,-55.3613797848081,
-38.5562346427694));
#267540=CARTESIAN_POINT('Ctrl Pts',(43.890622407919,-55.349649082917,-38.5607007444526));
#267541=CARTESIAN_POINT('Ctrl Pts',(43.9997560709039,-55.3172704656441,
-38.5746802407103));
#267542=CARTESIAN_POINT('Ctrl Pts',(44.1098017310836,-55.290468361793,-38.5898286859852));
#267543=CARTESIAN_POINT('Ctrl Pts',(44.2583166685835,-55.2656490138239,
-38.612301023075));
#267544=CARTESIAN_POINT('Ctrl Pts',(44.3705972700495,-55.2524997368729,
-38.6302900391873));
#267545=CARTESIAN_POINT('Ctrl Pts',(44.446056048267,-55.2474029004138,-38.6430428201589));
#267546=CARTESIAN_POINT('Ctrl Pts',(44.5218128020516,-55.2441636366351,
-38.65617756452));
#267547=CARTESIAN_POINT('Ctrl Pts',(44.5599089424743,-55.2434808562086,
-38.6629497802385));
#267548=CARTESIAN_POINT('Ctrl Pts',(44.6354869543582,-55.2439911084578,
-38.6767130108817));
#267549=CARTESIAN_POINT('Ctrl Pts',(44.6731456892459,-55.2451740103824,
-38.6837342374529));
#267550=CARTESIAN_POINT('Ctrl Pts',(44.7481014788608,-55.2493620066237,
-38.6980304684339));
#267551=CARTESIAN_POINT('Ctrl Pts',(44.860046548974,-55.2583760573225,-38.7198650218829));
#267552=CARTESIAN_POINT('Ctrl Pts',(45.0073845433675,-55.2811507310277,
-38.7505067688753));
#267553=CARTESIAN_POINT('Ctrl Pts',(45.1528189888476,-55.3146135839333,
-38.7826550300594));
#267554=CARTESIAN_POINT('Ctrl Pts',(45.2248832056965,-55.3349380951144,
-38.7992310848652));
#267555=CARTESIAN_POINT('Ctrl Pts',(45.2966462681613,-55.3570913336823,
-38.8160672125853));
#267556=CARTESIAN_POINT('Ctrl Pts',(45.3323638946335,-55.3690863290504,
-38.8246135819642));
#267557=CARTESIAN_POINT('Ctrl Pts',(45.4027951436545,-55.3946744461232,
-38.841798196801));
#267558=CARTESIAN_POINT('Ctrl Pts',(45.4376370321487,-55.4083060218429,
-38.85046633842));
#267559=CARTESIAN_POINT('Ctrl Pts',(45.5409345111852,-55.4516493275196,
-38.8766665754573));
#267560=CARTESIAN_POINT('Ctrl Pts',(45.6082182891413,-55.4838201174091,
-38.8944064774514));
#267561=CARTESIAN_POINT('Ctrl Pts',(45.7067749877369,-55.5369855856676,
-38.9214216121435));
#267562=CARTESIAN_POINT('Ctrl Pts',(45.7392219877795,-55.5555212114618,
-38.9304915704334));
#267563=CARTESIAN_POINT('Ctrl Pts',(45.8033556832395,-55.5942722159849,
-38.9487787872477));
#267564=CARTESIAN_POINT('Ctrl Pts',(45.8348443691401,-55.6143675312756,
-38.9579395118015));
#267565=CARTESIAN_POINT('Ctrl Pts',(45.9274099842789,-55.6766589025306,
-38.9854159162723));
#267566=CARTESIAN_POINT('Ctrl Pts',(45.9867610865919,-55.7209353156014,
-39.0037703637879));
#267567=CARTESIAN_POINT('Ctrl Pts',(46.1007337830098,-55.8148102393793,
-39.0405190865864));
#267568=CARTESIAN_POINT('Ctrl Pts',(46.1826971388658,-55.889219933262,-39.0681181728269));
#267569=CARTESIAN_POINT('Ctrl Pts',(46.259356574729,-55.9696687352924,-39.0957737179551));
#267570=CARTESIAN_POINT('Ctrl Pts',(46.309266807939,-56.024663053365,-39.1142236413887));
#267571=CARTESIAN_POINT('Ctrl Pts',(46.3336138177017,-56.0528284109483,
-39.1234510495426));
#267572=CARTESIAN_POINT('Ctrl Pts',(46.3692509284248,-56.0961546965833,
-39.1373141736981));
#267573=CARTESIAN_POINT('Ctrl Pts',(46.3809719555493,-56.1107655250657,
-39.14193505412));
#267574=CARTESIAN_POINT('Ctrl Pts',(46.4039850968433,-56.1401806715041,
-39.1511314768264));
#267575=CARTESIAN_POINT('Ctrl Pts',(46.4153001903629,-56.1550126624776,
-39.1557159133813));
#267576=CARTESIAN_POINT('Ctrl Pts',(46.4486370096885,-56.1998310060263,
-39.1694131182659));
#267577=CARTESIAN_POINT('Ctrl Pts',(46.4700835091466,-56.2301795317326,
-39.1784826054425));
#267578=CARTESIAN_POINT('Ctrl Pts',(46.532071913686,-56.3225583984772,-39.2054898733524));
#267579=CARTESIAN_POINT('Ctrl Pts',(46.5894197348374,-56.4176636744323,
-39.23211607576));
#267580=CARTESIAN_POINT('Ctrl Pts',(46.6566074362748,-56.5498680842415,
-39.2668544229849));
#267581=CARTESIAN_POINT('Ctrl Pts',(46.6870820302515,-56.617790568625,-39.2839693714534));
#267582=CARTESIAN_POINT('Ctrl Pts',(46.7159729830272,-56.6866360545619,
-39.3009558869148));
#267583=CARTESIAN_POINT('Ctrl Pts',(46.7296188023799,-56.7214992889704,
-39.3093799218186));
#267584=CARTESIAN_POINT('Ctrl Pts',(46.7553216997643,-56.7922546384013,
-39.3261176641085));
#267585=CARTESIAN_POINT('Ctrl Pts',(46.7672996943011,-56.8279354881579,
-39.3343809787628));
#267586=CARTESIAN_POINT('Ctrl Pts',(46.8004530502947,-56.9353633959568,
-39.358737163018));
#267587=CARTESIAN_POINT('Ctrl Pts',(46.8189795501832,-57.0077635587999,
-39.3744658121213));
#267588=CARTESIAN_POINT('Ctrl Pts',(46.848916211803,-57.1540080946302,-39.4048998290393));
#267589=CARTESIAN_POINT('Ctrl Pts',(46.866048617508,-57.2647966217996,-39.4269646939479));
#267590=CARTESIAN_POINT('Ctrl Pts',(46.875074749658,-57.3772756893033,-39.4478819384746));
#267591=CARTESIAN_POINT('Ctrl Pts',(46.8792542953452,-57.4526370309597,
-39.4615663943076));
#267592=CARTESIAN_POINT('Ctrl Pts',(46.8804258736835,-57.4905390832845,
-39.4682843608713));
#267593=CARTESIAN_POINT('Ctrl Pts',(46.8808837743635,-57.566610437341,-39.4814341960201));
#267594=CARTESIAN_POINT('Ctrl Pts',(46.8801708637706,-57.604491394965,-39.4878166677226));
#267595=CARTESIAN_POINT('Ctrl Pts',(46.8768913879562,-57.6800597985945,
-39.5002231148134));
#267596=CARTESIAN_POINT('Ctrl Pts',(46.8691896925243,-57.7930657109158,
-39.5182849936093));
#267597=CARTESIAN_POINT('Ctrl Pts',(46.8479069711518,-57.9423669591112,
-39.540205996752));
#267598=CARTESIAN_POINT('Ctrl Pts',(46.8236459543104,-58.053306681129,-39.5550278422771));
#267599=CARTESIAN_POINT('Ctrl Pts',(46.8055990109883,-58.1270324939452,
-39.5645447403379));
#267600=CARTESIAN_POINT('Ctrl Pts',(46.7956339676918,-58.1637938532181,
-39.5691227921436));
#267601=CARTESIAN_POINT('Ctrl Pts',(46.7738161327052,-58.2370162077019,
-39.5779016468881));
#267602=CARTESIAN_POINT('Ctrl Pts',(46.7619036278491,-58.2736352268715,
-39.5821192203466));
#267603=CARTESIAN_POINT('Ctrl Pts',(46.7364059718256,-58.3458255995332,
-39.5900871854462));
#267604=CARTESIAN_POINT('Ctrl Pts',(46.7091836493705,-58.4171862986019,
-39.5976163356366));
#267605=CARTESIAN_POINT('Ctrl Pts',(46.663274408039,-58.5216699086648,-39.6076014242402));
#267606=CARTESIAN_POINT('Ctrl Pts',(46.6123207377325,-58.6236436013082,
-39.616293729045));
#267607=CARTESIAN_POINT('Ctrl Pts',(46.5563244858032,-58.7230996041114,
-39.6236943138341));
#267608=CARTESIAN_POINT('Ctrl Pts',(46.515607032986,-58.7877140896312,-39.6277619492082));
#267609=CARTESIAN_POINT('Ctrl Pts',(46.4731710833873,-58.8514710047945,
-39.6313905635194));
#267610=CARTESIAN_POINT('Ctrl Pts',(46.4511086137465,-58.8829006319494,
-39.6329844599904));
#267611=CARTESIAN_POINT('Ctrl Pts',(46.4051673201274,-58.9449633016888,
-39.6357273485653));
#267612=CARTESIAN_POINT('Ctrl Pts',(46.381447994276,-58.975377588932,-39.6368662598532));
#267613=CARTESIAN_POINT('Ctrl Pts',(46.3084068909562,-59.0643493136614,
-39.6395761233691));
#267614=CARTESIAN_POINT('Ctrl Pts',(46.2570407846102,-59.1209150453974,
-39.6404603784325));
#267615=CARTESIAN_POINT('Ctrl Pts',(46.1491379755941,-59.228544463199,-39.6404138814247));
#267616=CARTESIAN_POINT('Ctrl Pts',(46.0925836555155,-59.2796343044913,
-39.6394845811684));
#267617=CARTESIAN_POINT('Ctrl Pts',(46.0038529437629,-59.3521266125547,
-39.6367223387528));
#267618=CARTESIAN_POINT('Ctrl Pts',(45.9736068078661,-59.3756113554055,
-39.6355721163029));
#267619=CARTESIAN_POINT('Ctrl Pts',(45.9272656961273,-59.4097723546528,
-39.6334997725088));
#267620=CARTESIAN_POINT('Ctrl Pts',(45.9116419215573,-59.4209912820171,
-39.6327502808957));
#267621=CARTESIAN_POINT('Ctrl Pts',(45.8800804794677,-59.4430610802669,
-39.6311351339295));
#267622=CARTESIAN_POINT('Ctrl Pts',(45.8321587971618,-59.4756823489919,
-39.628531354857));
#267623=CARTESIAN_POINT('Ctrl Pts',(45.7834097108732,-59.5062438963941,
-39.6254355071979));
#267624=CARTESIAN_POINT('Ctrl Pts',(45.717633106262,-59.5452481912826,-39.6208773262667));
#267625=CARTESIAN_POINT('Ctrl Pts',(45.6178307490054,-59.601113548897,-39.6133952897297));
#267626=CARTESIAN_POINT('Ctrl Pts',(45.4802897643185,-59.6652183443042,
-39.6008811885904));
#267627=CARTESIAN_POINT('Ctrl Pts',(45.3738098009101,-59.7055766782111,
-39.5896017905935));
#267628=CARTESIAN_POINT('Ctrl Pts',(45.3020778813705,-59.7307512119865,
-39.5816566825671));
#267629=CARTESIAN_POINT('Ctrl Pts',(45.2658207311094,-59.7424779859237,
-39.5774690651077));
#267630=CARTESIAN_POINT('Ctrl Pts',(45.1926264675053,-59.7641596016776,
-39.5686715125846));
#267631=CARTESIAN_POINT('Ctrl Pts',(45.1555073907618,-59.7741562512684,
-39.5640376159893));
#267632=CARTESIAN_POINT('Ctrl Pts',(45.0441315765335,-59.8011904590316,
-39.5496210468413));
#267633=CARTESIAN_POINT('Ctrl Pts',(44.9324484012679,-59.8224577850013,
-39.5341534065747));
#267634=CARTESIAN_POINT('Ctrl Pts',(44.8203079610257,-59.8353953605365,
-39.5171556909205));
#267635=CARTESIAN_POINT('Ctrl Pts',(44.7080184564226,-59.8455760612675,
-39.4996502778008));
#267636=CARTESIAN_POINT('Ctrl Pts',(44.6329372249224,-59.8486931621852,
-39.4873001861445));
#267637=CARTESIAN_POINT('Ctrl Pts',(44.5200834441659,-59.8478515133141,
-39.4677634802869));
#267638=CARTESIAN_POINT('Ctrl Pts',(44.4823810871712,-59.8466449718289,
-39.4610736497974));
#267639=CARTESIAN_POINT('Ctrl Pts',(44.4258051079382,-59.8434394706745,
-39.4507883432074));
#267640=CARTESIAN_POINT('Ctrl Pts',(44.4069254589855,-59.8421361346926,
-39.4473147915973));
#267641=CARTESIAN_POINT('Ctrl Pts',(44.3691376542581,-59.8390581625153,
-39.4402793331445));
#267642=CARTESIAN_POINT('Ctrl Pts',(44.3502459350849,-59.8372838734483,
-39.4367203104461));
#267643=CARTESIAN_POINT('Ctrl Pts',(44.2562487381671,-59.8272835659938,
-39.4188041728073));
#267644=CARTESIAN_POINT('Ctrl Pts',(44.1080045765469,-59.8040393501646,
-39.3892226636159));
#267645=CARTESIAN_POINT('Ctrl Pts',(43.9639303529155,-59.7668593120831,
-39.3578670379715));
#267646=CARTESIAN_POINT('Ctrl Pts',(43.8219159040518,-59.7227861654643,
-39.3256251231267));
#267647=CARTESIAN_POINT('Ctrl Pts',(43.7519290534068,-59.6972943066161,
-39.3090578287531));
#267648=CARTESIAN_POINT('Ctrl Pts',(43.665783177736,-59.6610675807531,-39.2877890488175));
#267649=CARTESIAN_POINT('Ctrl Pts',(43.6486106666635,-59.653596197985,-39.2835041280971));
#267650=CARTESIAN_POINT('Ctrl Pts',(43.6144193015916,-59.6382222359849,
-39.2748825183767));
#267651=CARTESIAN_POINT('Ctrl Pts',(43.597366582891,-59.6303022352814,-39.2705368924251));
#267652=CARTESIAN_POINT('Ctrl Pts',(43.5465994182959,-59.605961903298,-39.2574616452183));
#267653=CARTESIAN_POINT('Ctrl Pts',(43.513329300663,-59.588993111175,-39.2487085268073));
#267654=CARTESIAN_POINT('Ctrl Pts',(43.4805771074156,-59.5712767529309,
-39.2399080357013));
#267655=CARTESIAN_POINT('Ctrl Pts',(43.8903154257419,-57.7291941381088,
-41.4266127101804));
#267656=CARTESIAN_POINT('Ctrl Pts',(43.8716814361492,-57.7189244770852,
-41.4090117279687));
#267657=CARTESIAN_POINT('Ctrl Pts',(43.8355945080866,-57.6967277837834,
-41.3734625137379));
#267658=CARTESIAN_POINT('Ctrl Pts',(43.7849271573585,-57.6585752750105,
-41.3191078559793));
#267659=CARTESIAN_POINT('Ctrl Pts',(43.753465403225,-57.62988352171,-41.2821707250961));
#267660=CARTESIAN_POINT('Ctrl Pts',(43.7232071092872,-57.5995155202448,
-41.2448779944712));
#267661=CARTESIAN_POINT('Ctrl Pts',(43.694633283399,-57.5679550683129,-41.2078231506529));
#267662=CARTESIAN_POINT('Ctrl Pts',(43.6629744005209,-57.5256074013359,
-41.162062942605));
#267663=CARTESIAN_POINT('Ctrl Pts',(43.6400741040405,-57.4900012877665,
-41.1257945258022));
#267664=CARTESIAN_POINT('Ctrl Pts',(43.624122646482,-57.4624228770549,-41.0987642906252));
#267665=CARTESIAN_POINT('Ctrl Pts',(43.6143188854815,-57.4434516436916,
-41.0808660102928));
#267666=CARTESIAN_POINT('Ctrl Pts',(43.6049343759216,-57.4241698350281,
-41.0630203901697));
#267667=CARTESIAN_POINT('Ctrl Pts',(43.6004882740613,-57.4144479878336,
-41.054192925399));
#267668=CARTESIAN_POINT('Ctrl Pts',(43.5878889573419,-57.3850715912746,
-41.0280183011396));
#267669=CARTESIAN_POINT('Ctrl Pts',(43.5730447416356,-57.3453166524842,
-40.9939147159844));
#267670=CARTESIAN_POINT('Ctrl Pts',(43.5620571572655,-57.3044044614592,
-40.9613948378065));
#267671=CARTESIAN_POINT('Ctrl Pts',(43.5552843243605,-57.2732819874194,
-40.9376151994878));
#267672=CARTESIAN_POINT('Ctrl Pts',(43.5532714802541,-57.2628325912303,
-40.9297890667463));
#267673=CARTESIAN_POINT('Ctrl Pts',(43.5497454556161,-57.2417890776549,
-40.9143485382007));
#267674=CARTESIAN_POINT('Ctrl Pts',(43.5482304746054,-57.2311797832666,
-40.9067234564832));
#267675=CARTESIAN_POINT('Ctrl Pts',(43.5457184756399,-57.2098591834555,
-40.8917243418755));
#267676=CARTESIAN_POINT('Ctrl Pts',(43.5447290487245,-57.199220662917,-40.8844009198028));
#267677=CARTESIAN_POINT('Ctrl Pts',(43.5432711863927,-57.1779500447907,
-40.8700767121812));
#267678=CARTESIAN_POINT('Ctrl Pts',(43.5418684734652,-57.1460721839032,
-40.8490875836402));
#267679=CARTESIAN_POINT('Ctrl Pts',(43.5431039253892,-57.1036793909824,
-40.8230787545116));
#267680=CARTESIAN_POINT('Ctrl Pts',(43.5463738329101,-57.0719682486671,
-40.8050747359183));
#267681=CARTESIAN_POINT('Ctrl Pts',(43.5490829635055,-57.0508462881094,
-40.7934126279614));
#267682=CARTESIAN_POINT('Ctrl Pts',(43.5507030159248,-57.0402904723448,
-40.7877497380755));
#267683=CARTESIAN_POINT('Ctrl Pts',(43.5544790630841,-57.019214904491,-40.7767808895002));
#267684=CARTESIAN_POINT('Ctrl Pts',(43.5566463931059,-57.0086510117152,
-40.7714540988351));
#267685=CARTESIAN_POINT('Ctrl Pts',(43.5614808344627,-56.9877741662596,
-40.7612719783604));
#267686=CARTESIAN_POINT('Ctrl Pts',(43.5668234022498,-56.9670831174431,
-40.7515253398262));
#267687=CARTESIAN_POINT('Ctrl Pts',(43.5763377125496,-56.9366295208774,
-40.7382165180791));
#267688=CARTESIAN_POINT('Ctrl Pts',(43.5873444561754,-56.9067460923864,
-40.7262089422516));
#267689=CARTESIAN_POINT('Ctrl Pts',(43.5998453117462,-56.8774358278222,
-40.7155085881795));
#267690=CARTESIAN_POINT('Ctrl Pts',(43.6091839698139,-56.8582805167828,
-40.7092555817853));
#267691=CARTESIAN_POINT('Ctrl Pts',(43.6190331668358,-56.8393207538612,
-40.7034508410834));
#267692=CARTESIAN_POINT('Ctrl Pts',(43.6242099732076,-56.8299438685379,
-40.7007739810578));
#267693=CARTESIAN_POINT('Ctrl Pts',(43.6350986096338,-56.8113693026126,
-40.6958744145609));
#267694=CARTESIAN_POINT('Ctrl Pts',(43.6407690742328,-56.8022426567881,
-40.6936706244929));
#267695=CARTESIAN_POINT('Ctrl Pts',(43.6583896223854,-56.7754411523649,
-40.6878155334118));
#267696=CARTESIAN_POINT('Ctrl Pts',(43.6709801307092,-56.7582712890167,
-40.6848937134075));
#267697=CARTESIAN_POINT('Ctrl Pts',(43.6978023804218,-56.725340315416,-40.6809957255822));
#267698=CARTESIAN_POINT('Ctrl Pts',(43.7120405319879,-56.7095692151415,
-40.6800172734785));
#267699=CARTESIAN_POINT('Ctrl Pts',(43.7346338722206,-56.6869796178674,
-40.680019660452));
#267700=CARTESIAN_POINT('Ctrl Pts',(43.7423799312797,-56.6796208977126,
-40.6802668752224));
#267701=CARTESIAN_POINT('Ctrl Pts',(43.7543060585229,-56.6688607312791,
-40.681010981358));
#267702=CARTESIAN_POINT('Ctrl Pts',(43.7583370517177,-56.6653168192219,
-40.6813218268212));
#267703=CARTESIAN_POINT('Ctrl Pts',(43.7665035456834,-56.6583217341419,
-40.6820693651562));
#267704=CARTESIAN_POINT('Ctrl Pts',(43.7706422703,-56.6548683091639,-40.6825066780886));
#267705=CARTESIAN_POINT('Ctrl Pts',(43.7831478581881,-56.6447045100584,
-40.6840009724959));
#267706=CARTESIAN_POINT('Ctrl Pts',(43.8000992888712,-56.6316392340345,
-40.6864805452653));
#267707=CARTESIAN_POINT('Ctrl Pts',(43.8351004518507,-56.6074069729907,
-40.6933496988796));
#267708=CARTESIAN_POINT('Ctrl Pts',(43.8717190640765,-56.5859796680779,
-40.7030349737613));
#267709=CARTESIAN_POINT('Ctrl Pts',(43.9003898794618,-56.5719991465823,
-40.7123924126099));
#267710=CARTESIAN_POINT('Ctrl Pts',(43.919774692733,-56.5631479893168,-40.719099824507));
#267711=CARTESIAN_POINT('Ctrl Pts',(43.9296053152689,-56.5589560552736,
-40.722689237866));
#267712=CARTESIAN_POINT('Ctrl Pts',(43.9495302416178,-56.551051384942,-40.7303379810773));
#267713=CARTESIAN_POINT('Ctrl Pts',(43.959660471973,-56.5473282955902,-40.7344135607172));
#267714=CARTESIAN_POINT('Ctrl Pts',(43.9799461530017,-56.5404515818703,
-40.7429393172485));
#267715=CARTESIAN_POINT('Ctrl Pts',(43.9901452646573,-56.5372793127045,
-40.7474054189318));
#267716=CARTESIAN_POINT('Ctrl Pts',(44.0208712025373,-56.5285586047056,
-40.7613849151889));
#267717=CARTESIAN_POINT('Ctrl Pts',(44.0518784813599,-56.521416173947,-40.7765333604643));
#267718=CARTESIAN_POINT('Ctrl Pts',(44.0937728041468,-56.5149820273198,
-40.799005697554));
#267719=CARTESIAN_POINT('Ctrl Pts',(44.1254693703652,-56.5117027703592,
-40.8169947136667));
#267720=CARTESIAN_POINT('Ctrl Pts',(44.1467868482481,-56.5105547568045,
-40.8297474946377));
#267721=CARTESIAN_POINT('Ctrl Pts',(44.1681963264173,-56.50993223545,-40.842882238999));
#267722=CARTESIAN_POINT('Ctrl Pts',(44.1789665479467,-56.509886262238,-40.8496544547178));
#267723=CARTESIAN_POINT('Ctrl Pts',(44.2003410646824,-56.5103214152413,
-40.8634176853611));
#267724=CARTESIAN_POINT('Ctrl Pts',(44.2109953322312,-56.5108003631786,
-40.8704389119319));
#267725=CARTESIAN_POINT('Ctrl Pts',(44.2322091102727,-56.5122711761573,
-40.8847351429132));
#267726=CARTESIAN_POINT('Ctrl Pts',(44.2639028799147,-56.5152466319394,
-40.9065696963621));
#267727=CARTESIAN_POINT('Ctrl Pts',(44.305661850593,-56.5222422564611,-40.9372114433545));
#267728=CARTESIAN_POINT('Ctrl Pts',(44.346925841944,-56.532247127269,-40.9693597045385));
#267729=CARTESIAN_POINT('Ctrl Pts',(44.3673876336497,-56.53826115526,-40.9859357593442));
#267730=CARTESIAN_POINT('Ctrl Pts',(44.3877715667723,-56.5447901720246,
-41.0027718870644));
#267731=CARTESIAN_POINT('Ctrl Pts',(44.3979208506631,-56.5483132560745,
-41.0113182564434));
#267732=CARTESIAN_POINT('Ctrl Pts',(44.4179418071922,-56.5558066378292,
-41.02850287128));
#267733=CARTESIAN_POINT('Ctrl Pts',(44.4278499085732,-56.5597882829787,
-41.0371710128992));
#267734=CARTESIAN_POINT('Ctrl Pts',(44.4572364860018,-56.5724196473794,
-41.0633712499365));
#267735=CARTESIAN_POINT('Ctrl Pts',(44.4763932211824,-56.581758968269,-41.0811111519311));
#267736=CARTESIAN_POINT('Ctrl Pts',(44.5044772880921,-56.5971447477014,
-41.1081262866225));
#267737=CARTESIAN_POINT('Ctrl Pts',(44.5137271775895,-56.6025015227711,
-41.1171962449124));
#267738=CARTESIAN_POINT('Ctrl Pts',(44.5320183562985,-56.6136863880645,
-41.1354834617267));
#267739=CARTESIAN_POINT('Ctrl Pts',(44.5410031705763,-56.6194798267371,
-41.144644186283));
#267740=CARTESIAN_POINT('Ctrl Pts',(44.5674276642847,-56.6374191091633,
-41.1721205907467));
#267741=CARTESIAN_POINT('Ctrl Pts',(44.5843870769067,-56.6501457393646,
-41.1904750382678));
#267742=CARTESIAN_POINT('Ctrl Pts',(44.616987890196,-56.6770839740703,-41.2272237610649));
#267743=CARTESIAN_POINT('Ctrl Pts',(44.640458797708,-56.6984048650555,-41.2548228473058));
#267744=CARTESIAN_POINT('Ctrl Pts',(44.6624514458289,-56.7214114906953,
-41.2824783924342));
#267745=CARTESIAN_POINT('Ctrl Pts',(44.6767798128067,-56.7371294193188,
-41.3009283158679));
#267746=CARTESIAN_POINT('Ctrl Pts',(44.683774397772,-56.7451748501741,-41.3101557240219));
#267747=CARTESIAN_POINT('Ctrl Pts',(44.6940202659092,-56.7575442973705,
-41.324018848177));
#267748=CARTESIAN_POINT('Ctrl Pts',(44.6973914635031,-56.7617145235639,
-41.328639728599));
#267749=CARTESIAN_POINT('Ctrl Pts',(44.7040131878578,-56.770108052971,-41.3378361513053));
#267750=CARTESIAN_POINT('Ctrl Pts',(44.7072703203268,-56.7743392575068,
-41.3424205878605));
#267751=CARTESIAN_POINT('Ctrl Pts',(44.7168707027477,-56.7871217033085,
-41.3561177927451));
#267752=CARTESIAN_POINT('Ctrl Pts',(44.7230524906066,-56.7957731420119,
-41.3651872799216));
#267753=CARTESIAN_POINT('Ctrl Pts',(44.7409373255192,-56.8220955492914,
-41.3921945478314));
#267754=CARTESIAN_POINT('Ctrl Pts',(44.7575187561203,-56.8491712652862,
-41.4188207502394));
#267755=CARTESIAN_POINT('Ctrl Pts',(44.7770214494108,-56.88676384976,-41.453559097464));
#267756=CARTESIAN_POINT('Ctrl Pts',(44.7858965000619,-56.9060633365117,
-41.4706740459328));
#267757=CARTESIAN_POINT('Ctrl Pts',(44.7943266372896,-56.9256180211132,
-41.4876605613939));
#267758=CARTESIAN_POINT('Ctrl Pts',(44.7983169540911,-56.9355169983302,
-41.4960845962979));
#267759=CARTESIAN_POINT('Ctrl Pts',(44.8058516078422,-56.9556000996462,
-41.5128223385875));
#267760=CARTESIAN_POINT('Ctrl Pts',(44.8093727854448,-56.9657242505397,
-41.5210856532432));
#267761=CARTESIAN_POINT('Ctrl Pts',(44.8191505788346,-56.9961959016236,
-41.5454418374945));
#267762=CARTESIAN_POINT('Ctrl Pts',(44.8246597322132,-57.0167187198372,
-41.5611704866007));
#267763=CARTESIAN_POINT('Ctrl Pts',(44.8336688220904,-57.0581479791523,
-41.5916045035181));
#267764=CARTESIAN_POINT('Ctrl Pts',(44.8389236650083,-57.0895139074259,
-41.613669368427));
#267765=CARTESIAN_POINT('Ctrl Pts',(44.8418900765893,-57.1213299669285,
-41.6345866129535));
#267766=CARTESIAN_POINT('Ctrl Pts',(44.8433488372948,-57.142640498193,-41.6482710687869));
#267767=CARTESIAN_POINT('Ctrl Pts',(44.8438191277705,-57.1533552116615,
-41.6549890353504));
#267768=CARTESIAN_POINT('Ctrl Pts',(44.8442270800594,-57.1748537940466,
-41.6681388704993));
#267769=CARTESIAN_POINT('Ctrl Pts',(44.8441639040618,-57.1855561823783,
-41.6745213422017));
#267770=CARTESIAN_POINT('Ctrl Pts',(44.8435122114514,-57.2069000331791,
-41.6869277892926));
#267771=CARTESIAN_POINT('Ctrl Pts',(44.8417458896958,-57.2388084678274,
-41.7049896680882));
#267772=CARTESIAN_POINT('Ctrl Pts',(44.8362687719071,-57.2809279665006,
-41.7269106712316));
#267773=CARTESIAN_POINT('Ctrl Pts',(44.8298088085522,-57.3121969378441,
-41.7417325167562));
#267774=CARTESIAN_POINT('Ctrl Pts',(44.8249713776488,-57.3329705079708,
-41.751249414817));
#267775=CARTESIAN_POINT('Ctrl Pts',(44.8222858794974,-57.3433254378487,
-41.7558274666229));
#267776=CARTESIAN_POINT('Ctrl Pts',(44.8163797073795,-57.3639440769784,
-41.7646063213672));
#267777=CARTESIAN_POINT('Ctrl Pts',(44.8131427147447,-57.3742522416544,
-41.7688238948253));
#267778=CARTESIAN_POINT('Ctrl Pts',(44.8061917406462,-57.3945668799698,
-41.7767918599254));
#267779=CARTESIAN_POINT('Ctrl Pts',(44.7987498536529,-57.4146412549335,
-41.7843210101159));
#267780=CARTESIAN_POINT('Ctrl Pts',(44.7861419817956,-57.4440129710611,
-41.7943060987191));
#267781=CARTESIAN_POINT('Ctrl Pts',(44.7720982599006,-57.4726583092559,
-41.8029984035242));
#267782=CARTESIAN_POINT('Ctrl Pts',(44.7566193423106,-57.5005749992605,
-41.8103989883131));
#267783=CARTESIAN_POINT('Ctrl Pts',(44.7453362941317,-57.518697088903,-41.8144666236875));
#267784=CARTESIAN_POINT('Ctrl Pts',(44.7335642473644,-57.5365709174371,
-41.8180952379985));
#267785=CARTESIAN_POINT('Ctrl Pts',(44.7274378249752,-57.5453780864623,
-41.8196891344695));
#267786=CARTESIAN_POINT('Ctrl Pts',(44.7146685840676,-57.5627610237142,
-41.8224320230444));
#267787=CARTESIAN_POINT('Ctrl Pts',(44.7080700862024,-57.5712755128024,
-41.8235709343319));
#267788=CARTESIAN_POINT('Ctrl Pts',(44.6877341610586,-57.5961705213949,
-41.8262807978491));
#267789=CARTESIAN_POINT('Ctrl Pts',(44.6734117165454,-57.6119810052107,
-41.8271650529119));
#267790=CARTESIAN_POINT('Ctrl Pts',(44.6432859415473,-57.6420285404153,
-41.827118555904));
#267791=CARTESIAN_POINT('Ctrl Pts',(44.6274777219699,-57.6562729242579,
-41.8261892556471));
#267792=CARTESIAN_POINT('Ctrl Pts',(44.6026489360012,-57.6764545436153,
-41.823427013232));
#267793=CARTESIAN_POINT('Ctrl Pts',(44.5941811636919,-57.6829873126311,
-41.8222767907821));
#267794=CARTESIAN_POINT('Ctrl Pts',(44.5812011369499,-57.6924815728277,
-41.820204446988));
#267795=CARTESIAN_POINT('Ctrl Pts',(44.5768239301145,-57.6955981764101,
-41.8194549553751));
#267796=CARTESIAN_POINT('Ctrl Pts',(44.5679795363474,-57.7017261947271,
-41.8178398084084));
#267797=CARTESIAN_POINT('Ctrl Pts',(44.554547495243,-57.7107794649358,-41.8152360293365));
#267798=CARTESIAN_POINT('Ctrl Pts',(44.5408745509057,-57.7192473537464,
-41.812140181677));
#267799=CARTESIAN_POINT('Ctrl Pts',(44.5224181841827,-57.7300417662926,
-41.8075820007456));
#267800=CARTESIAN_POINT('Ctrl Pts',(44.494403164631,-57.7454824222945,-41.8000999642091));
#267801=CARTESIAN_POINT('Ctrl Pts',(44.4557509611988,-57.7631175354143,
-41.7875858630695));
#267802=CARTESIAN_POINT('Ctrl Pts',(44.4257963579031,-57.7741479888816,
-41.7763064650726));
#267803=CARTESIAN_POINT('Ctrl Pts',(44.4056101875344,-57.781009218212,-41.7683613570464));
#267804=CARTESIAN_POINT('Ctrl Pts',(44.3954036594654,-57.7841949818065,
-41.7641737395871));
#267805=CARTESIAN_POINT('Ctrl Pts',(44.3747925009816,-57.7900627169564,
-41.7553761870634));
#267806=CARTESIAN_POINT('Ctrl Pts',(44.3643365899562,-57.7927558542442,
-41.7507422904685));
#267807=CARTESIAN_POINT('Ctrl Pts',(44.3329536886806,-57.7999988857253,
-41.7363257213199));
#267808=CARTESIAN_POINT('Ctrl Pts',(44.3014645871824,-57.8056090798854,
-41.7208580810542));
#267809=CARTESIAN_POINT('Ctrl Pts',(44.2698183189435,-57.8088603667088,
-41.7038603653999));
#267810=CARTESIAN_POINT('Ctrl Pts',(44.2381206623806,-57.8113308880715,
-41.6863549522799));
#267811=CARTESIAN_POINT('Ctrl Pts',(44.2169139506954,-57.8119384373532,
-41.6740048606234));
#267812=CARTESIAN_POINT('Ctrl Pts',(44.1850197107514,-57.811287280344,-41.6544681547659));
#267813=CARTESIAN_POINT('Ctrl Pts',(44.1743613109546,-57.8108078241776,
-41.6477783242763));
#267814=CARTESIAN_POINT('Ctrl Pts',(44.1583626375358,-57.8096935003687,
-41.6374930176863));
#267815=CARTESIAN_POINT('Ctrl Pts',(44.1530230189312,-57.809255510817,-41.6340194660765));
#267816=CARTESIAN_POINT('Ctrl Pts',(44.1423341247923,-57.8082460206643,
-41.6269840076234));
#267817=CARTESIAN_POINT('Ctrl Pts',(44.1369894952372,-57.8076746784434,
-41.6234249849254));
#267818=CARTESIAN_POINT('Ctrl Pts',(44.1103928894951,-57.8045001122898,
-41.6055088472864));
#267819=CARTESIAN_POINT('Ctrl Pts',(44.0684216046586,-57.7973782151022,
-41.5759273380954));
#267820=CARTESIAN_POINT('Ctrl Pts',(44.0275807082801,-57.78632659952,-41.5445717124501));
#267821=CARTESIAN_POINT('Ctrl Pts',(43.9872978152183,-57.7733311875938,
-41.5123297976061));
#267822=CARTESIAN_POINT('Ctrl Pts',(43.9674326520914,-57.7658590768128,
-41.4957625032292));
#267823=CARTESIAN_POINT('Ctrl Pts',(43.942963744406,-57.7552890823142,-41.4744937232973));
#267824=CARTESIAN_POINT('Ctrl Pts',(43.938085174092,-57.7531113051098,-41.4702088025761));
#267825=CARTESIAN_POINT('Ctrl Pts',(43.9283699185172,-57.7486342535987,
-41.4615871928557));
#267826=CARTESIAN_POINT('Ctrl Pts',(43.9235236029976,-57.7463299238453,
-41.4572415669043));
#267827=CARTESIAN_POINT('Ctrl Pts',(43.9090930604083,-57.739254093668,-41.4441663196977));
#267828=CARTESIAN_POINT('Ctrl Pts',(43.8996324205383,-57.7343289686206,
-41.4354132012863));
#267829=CARTESIAN_POINT('Ctrl Pts',(43.8903154257419,-57.7291941381088,
-41.4266127101804));
#267830=CARTESIAN_POINT('Ctrl Pts',(43.4805771074156,-59.5712767529309,
-39.2399080357013));
#267831=CARTESIAN_POINT('Ctrl Pts',(43.4150727209207,-59.5358440364426,
-39.2223070534893));
#267832=CARTESIAN_POINT('Ctrl Pts',(43.2883193276586,-59.4590682572254,
-39.1867578392588));
#267833=CARTESIAN_POINT('Ctrl Pts',(43.1106712693135,-59.32658002426,-39.1324031814995));
#267834=CARTESIAN_POINT('Ctrl Pts',(43.0005921597408,-59.2266373021163,
-39.0954660506179));
#267835=CARTESIAN_POINT('Ctrl Pts',(42.8948534568781,-59.1207134074407,
-39.0581733199915));
#267836=CARTESIAN_POINT('Ctrl Pts',(42.7951360401793,-59.0104958554849,
-39.0211184761739));
#267837=CARTESIAN_POINT('Ctrl Pts',(42.6850011896347,-58.8622904152127,
-38.9753582681256));
#267838=CARTESIAN_POINT('Ctrl Pts',(42.6055727997797,-58.7375004045667,
-38.939089851323));
#267839=CARTESIAN_POINT('Ctrl Pts',(42.5503788594446,-58.6407591922129,
-38.9120596161462));
#267840=CARTESIAN_POINT('Ctrl Pts',(42.5165536369311,-58.5741539171446,
-38.8941613358138));
#267841=CARTESIAN_POINT('Ctrl Pts',(42.4842288567228,-58.5064298632496,
-38.8763157156907));
#267842=CARTESIAN_POINT('Ctrl Pts',(42.4689425396028,-58.4722695523732,
-38.8674882509199));
#267843=CARTESIAN_POINT('Ctrl Pts',(42.4257123024776,-58.3690064948315,
-38.8413136266604));
#267844=CARTESIAN_POINT('Ctrl Pts',(42.3750272156063,-58.229152189777,-38.8072100415055));
#267845=CARTESIAN_POINT('Ctrl Pts',(42.3380647902547,-58.0850119200902,
-38.7746901633276));
#267846=CARTESIAN_POINT('Ctrl Pts',(42.3155659796374,-57.9752818499468,
-38.7509105250088));
#267847=CARTESIAN_POINT('Ctrl Pts',(42.3089374211558,-57.9384266221928,
-38.7430843922672));
#267848=CARTESIAN_POINT('Ctrl Pts',(42.297458012674,-57.864178756387,-38.7276438637217));
#267849=CARTESIAN_POINT('Ctrl Pts',(42.292601515188,-57.8267325312259,-38.720018782004));
#267850=CARTESIAN_POINT('Ctrl Pts',(42.2847289916893,-57.7514526301959,
-38.7050196673963));
#267851=CARTESIAN_POINT('Ctrl Pts',(42.2817363521424,-57.7138759968928,
-38.6976962453237));
#267852=CARTESIAN_POINT('Ctrl Pts',(42.277596992864,-57.6387184974263,-38.6833720377019));
#267853=CARTESIAN_POINT('Ctrl Pts',(42.2741651307842,-57.5260409596698,
-38.6623829091612));
#267854=CARTESIAN_POINT('Ctrl Pts',(42.2805893100654,-57.3760354719141,
-38.6363740800325));
#267855=CARTESIAN_POINT('Ctrl Pts',(42.2937061680812,-57.2637038035873,
-38.618370061439));
#267856=CARTESIAN_POINT('Ctrl Pts',(42.3043247017591,-57.1888547452426,
-38.6067079534822));
#267857=CARTESIAN_POINT('Ctrl Pts',(42.3105743117123,-57.1514345461221,
-38.6010450635964));
#267858=CARTESIAN_POINT('Ctrl Pts',(42.3249704170347,-57.0766935209607,
-38.590076215021));
#267859=CARTESIAN_POINT('Ctrl Pts',(42.3331592025312,-57.0392159768686,
-38.5847494243559));
#267860=CARTESIAN_POINT('Ctrl Pts',(42.3512949844302,-56.9651221381903,
-38.5745673038812));
#267861=CARTESIAN_POINT('Ctrl Pts',(42.3712216906218,-56.8916587034686,
-38.564820665347));
#267862=CARTESIAN_POINT('Ctrl Pts',(42.4063979707918,-56.7834465224234,
-38.5515118436));
#267863=CARTESIAN_POINT('Ctrl Pts',(42.4468320479729,-56.6771725078319,
-38.5395042677724));
#267864=CARTESIAN_POINT('Ctrl Pts',(42.4925290654744,-56.5728473165674,
-38.5288039137004));
#267865=CARTESIAN_POINT('Ctrl Pts',(42.5265325119253,-56.5046058456765,
-38.5225509073062));
#267866=CARTESIAN_POINT('Ctrl Pts',(42.5623338475306,-56.4370293947697,
-38.5167461666044));
#267867=CARTESIAN_POINT('Ctrl Pts',(42.5811223641794,-56.4035923099625,
-38.5140693065785));
#267868=CARTESIAN_POINT('Ctrl Pts',(42.620584523009,-56.3373241998654,-38.5091697400817));
#267869=CARTESIAN_POINT('Ctrl Pts',(42.6411082254821,-56.3047465904101,
-38.5069659500128));
#267870=CARTESIAN_POINT('Ctrl Pts',(42.7048067991197,-56.2090283357163,
-38.501110858935));
#267871=CARTESIAN_POINT('Ctrl Pts',(42.7502234543428,-56.1476408662828,
-38.4981890389281));
#267872=CARTESIAN_POINT('Ctrl Pts',(42.8467942323831,-56.0297655581676,
-38.4942910511033));
#267873=CARTESIAN_POINT('Ctrl Pts',(42.8979715413934,-55.9732420482176,
-38.4933125989996));
#267874=CARTESIAN_POINT('Ctrl Pts',(42.9790570553347,-55.8921695883033,
-38.4933149859729));
#267875=CARTESIAN_POINT('Ctrl Pts',(43.0068374106561,-55.8657400908868,
-38.4935622007431));
#267876=CARTESIAN_POINT('Ctrl Pts',(43.0495800649421,-55.8270637749536,
-38.4943063068789));
#267877=CARTESIAN_POINT('Ctrl Pts',(43.0640222060113,-55.8143203511958,
-38.494617152342));
#267878=CARTESIAN_POINT('Ctrl Pts',(43.0932714774893,-55.7891564261061,
-38.4953646906773));
#267879=CARTESIAN_POINT('Ctrl Pts',(43.1080901283632,-55.7767277938553,
-38.4958020036096));
#267880=CARTESIAN_POINT('Ctrl Pts',(43.1528523310046,-55.7401327167866,
-38.4972962980169));
#267881=CARTESIAN_POINT('Ctrl Pts',(43.2134913856688,-55.6930468850421,
-38.4997758707861));
#267882=CARTESIAN_POINT('Ctrl Pts',(43.3385569247743,-55.6055389451161,
-38.5066450244003));
#267883=CARTESIAN_POINT('Ctrl Pts',(43.4691986576013,-55.5278792007279,
-38.5163302992824));
#267884=CARTESIAN_POINT('Ctrl Pts',(43.5713395927684,-55.4769743237494,
-38.5256877381308));
#267885=CARTESIAN_POINT('Ctrl Pts',(43.6403672861995,-55.4446857735354,
-38.5323951500278));
#267886=CARTESIAN_POINT('Ctrl Pts',(43.6753577685123,-55.4293620157832,
-38.5359845633874));
#267887=CARTESIAN_POINT('Ctrl Pts',(43.7462462065788,-55.4003985583156,
-38.5436333065981));
#267888=CARTESIAN_POINT('Ctrl Pts',(43.7822717759725,-55.3867204456352,
-38.5477088862383));
#267889=CARTESIAN_POINT('Ctrl Pts',(43.8543821738219,-55.3613797848081,
-38.5562346427694));
#267890=CARTESIAN_POINT('Ctrl Pts',(43.890622407919,-55.349649082917,-38.5607007444526));
#267891=CARTESIAN_POINT('Ctrl Pts',(43.9997560709039,-55.3172704656441,
-38.5746802407103));
#267892=CARTESIAN_POINT('Ctrl Pts',(44.1098017310836,-55.290468361793,-38.5898286859852));
#267893=CARTESIAN_POINT('Ctrl Pts',(44.2583166685835,-55.2656490138239,
-38.612301023075));
#267894=CARTESIAN_POINT('Ctrl Pts',(44.3705972700495,-55.2524997368729,
-38.6302900391873));
#267895=CARTESIAN_POINT('Ctrl Pts',(44.446056048267,-55.2474029004138,-38.6430428201589));
#267896=CARTESIAN_POINT('Ctrl Pts',(44.5218128020516,-55.2441636366351,
-38.65617756452));
#267897=CARTESIAN_POINT('Ctrl Pts',(44.5599089424743,-55.2434808562086,
-38.6629497802385));
#267898=CARTESIAN_POINT('Ctrl Pts',(44.6354869543582,-55.2439911084578,
-38.6767130108817));
#267899=CARTESIAN_POINT('Ctrl Pts',(44.6731456892459,-55.2451740103824,
-38.6837342374529));
#267900=CARTESIAN_POINT('Ctrl Pts',(44.7481014788608,-55.2493620066237,
-38.6980304684339));
#267901=CARTESIAN_POINT('Ctrl Pts',(44.860046548974,-55.2583760573225,-38.7198650218829));
#267902=CARTESIAN_POINT('Ctrl Pts',(45.0073845433675,-55.2811507310277,
-38.7505067688753));
#267903=CARTESIAN_POINT('Ctrl Pts',(45.1528189888476,-55.3146135839333,
-38.7826550300594));
#267904=CARTESIAN_POINT('Ctrl Pts',(45.2248832056965,-55.3349380951144,
-38.7992310848652));
#267905=CARTESIAN_POINT('Ctrl Pts',(45.2966462681613,-55.3570913336823,
-38.8160672125853));
#267906=CARTESIAN_POINT('Ctrl Pts',(45.3323638946335,-55.3690863290504,
-38.8246135819642));
#267907=CARTESIAN_POINT('Ctrl Pts',(45.4027951436545,-55.3946744461232,
-38.841798196801));
#267908=CARTESIAN_POINT('Ctrl Pts',(45.4376370321487,-55.4083060218429,
-38.85046633842));
#267909=CARTESIAN_POINT('Ctrl Pts',(45.5409345111852,-55.4516493275196,
-38.8766665754573));
#267910=CARTESIAN_POINT('Ctrl Pts',(45.6082182891413,-55.4838201174091,
-38.8944064774514));
#267911=CARTESIAN_POINT('Ctrl Pts',(45.7067749877369,-55.5369855856676,
-38.9214216121435));
#267912=CARTESIAN_POINT('Ctrl Pts',(45.7392219877795,-55.5555212114618,
-38.9304915704334));
#267913=CARTESIAN_POINT('Ctrl Pts',(45.8033556832395,-55.5942722159849,
-38.9487787872477));
#267914=CARTESIAN_POINT('Ctrl Pts',(45.8348443691401,-55.6143675312756,
-38.9579395118015));
#267915=CARTESIAN_POINT('Ctrl Pts',(45.9274099842789,-55.6766589025306,
-38.9854159162723));
#267916=CARTESIAN_POINT('Ctrl Pts',(45.9867610865919,-55.7209353156014,
-39.0037703637879));
#267917=CARTESIAN_POINT('Ctrl Pts',(46.1007337830098,-55.8148102393793,
-39.0405190865864));
#267918=CARTESIAN_POINT('Ctrl Pts',(46.1826971388658,-55.889219933262,-39.0681181728269));
#267919=CARTESIAN_POINT('Ctrl Pts',(46.259356574729,-55.9696687352924,-39.0957737179551));
#267920=CARTESIAN_POINT('Ctrl Pts',(46.309266807939,-56.024663053365,-39.1142236413887));
#267921=CARTESIAN_POINT('Ctrl Pts',(46.3336138177017,-56.0528284109483,
-39.1234510495426));
#267922=CARTESIAN_POINT('Ctrl Pts',(46.3692509284248,-56.0961546965833,
-39.1373141736981));
#267923=CARTESIAN_POINT('Ctrl Pts',(46.3809719555493,-56.1107655250657,
-39.14193505412));
#267924=CARTESIAN_POINT('Ctrl Pts',(46.4039850968433,-56.1401806715041,
-39.1511314768264));
#267925=CARTESIAN_POINT('Ctrl Pts',(46.4153001903629,-56.1550126624776,
-39.1557159133813));
#267926=CARTESIAN_POINT('Ctrl Pts',(46.4486370096885,-56.1998310060263,
-39.1694131182659));
#267927=CARTESIAN_POINT('Ctrl Pts',(46.4700835091466,-56.2301795317326,
-39.1784826054425));
#267928=CARTESIAN_POINT('Ctrl Pts',(46.532071913686,-56.3225583984772,-39.2054898733524));
#267929=CARTESIAN_POINT('Ctrl Pts',(46.5894197348374,-56.4176636744323,
-39.23211607576));
#267930=CARTESIAN_POINT('Ctrl Pts',(46.6566074362748,-56.5498680842415,
-39.2668544229849));
#267931=CARTESIAN_POINT('Ctrl Pts',(46.6870820302515,-56.617790568625,-39.2839693714534));
#267932=CARTESIAN_POINT('Ctrl Pts',(46.7159729830272,-56.6866360545619,
-39.3009558869148));
#267933=CARTESIAN_POINT('Ctrl Pts',(46.7296188023799,-56.7214992889704,
-39.3093799218186));
#267934=CARTESIAN_POINT('Ctrl Pts',(46.7553216997643,-56.7922546384013,
-39.3261176641085));
#267935=CARTESIAN_POINT('Ctrl Pts',(46.7672996943011,-56.8279354881579,
-39.3343809787628));
#267936=CARTESIAN_POINT('Ctrl Pts',(46.8004530502947,-56.9353633959568,
-39.358737163018));
#267937=CARTESIAN_POINT('Ctrl Pts',(46.8189795501832,-57.0077635587999,
-39.3744658121213));
#267938=CARTESIAN_POINT('Ctrl Pts',(46.848916211803,-57.1540080946302,-39.4048998290393));
#267939=CARTESIAN_POINT('Ctrl Pts',(46.866048617508,-57.2647966217996,-39.4269646939479));
#267940=CARTESIAN_POINT('Ctrl Pts',(46.875074749658,-57.3772756893033,-39.4478819384746));
#267941=CARTESIAN_POINT('Ctrl Pts',(46.8792542953452,-57.4526370309597,
-39.4615663943076));
#267942=CARTESIAN_POINT('Ctrl Pts',(46.8804258736835,-57.4905390832845,
-39.4682843608713));
#267943=CARTESIAN_POINT('Ctrl Pts',(46.8808837743635,-57.566610437341,-39.4814341960201));
#267944=CARTESIAN_POINT('Ctrl Pts',(46.8801708637706,-57.604491394965,-39.4878166677226));
#267945=CARTESIAN_POINT('Ctrl Pts',(46.8768913879562,-57.6800597985945,
-39.5002231148134));
#267946=CARTESIAN_POINT('Ctrl Pts',(46.8691896925243,-57.7930657109158,
-39.5182849936093));
#267947=CARTESIAN_POINT('Ctrl Pts',(46.8479069711518,-57.9423669591112,
-39.540205996752));
#267948=CARTESIAN_POINT('Ctrl Pts',(46.8236459543104,-58.053306681129,-39.5550278422771));
#267949=CARTESIAN_POINT('Ctrl Pts',(46.8055990109883,-58.1270324939452,
-39.5645447403379));
#267950=CARTESIAN_POINT('Ctrl Pts',(46.7956339676918,-58.1637938532181,
-39.5691227921436));
#267951=CARTESIAN_POINT('Ctrl Pts',(46.7738161327052,-58.2370162077019,
-39.5779016468881));
#267952=CARTESIAN_POINT('Ctrl Pts',(46.7619036278491,-58.2736352268715,
-39.5821192203466));
#267953=CARTESIAN_POINT('Ctrl Pts',(46.7364059718256,-58.3458255995332,
-39.5900871854462));
#267954=CARTESIAN_POINT('Ctrl Pts',(46.7091836493705,-58.4171862986019,
-39.5976163356366));
#267955=CARTESIAN_POINT('Ctrl Pts',(46.663274408039,-58.5216699086648,-39.6076014242402));
#267956=CARTESIAN_POINT('Ctrl Pts',(46.6123207377325,-58.6236436013082,
-39.616293729045));
#267957=CARTESIAN_POINT('Ctrl Pts',(46.5563244858032,-58.7230996041114,
-39.6236943138341));
#267958=CARTESIAN_POINT('Ctrl Pts',(46.515607032986,-58.7877140896312,-39.6277619492082));
#267959=CARTESIAN_POINT('Ctrl Pts',(46.4731710833873,-58.8514710047945,
-39.6313905635194));
#267960=CARTESIAN_POINT('Ctrl Pts',(46.4511086137465,-58.8829006319494,
-39.6329844599904));
#267961=CARTESIAN_POINT('Ctrl Pts',(46.4051673201274,-58.9449633016888,
-39.6357273485653));
#267962=CARTESIAN_POINT('Ctrl Pts',(46.381447994276,-58.975377588932,-39.6368662598532));
#267963=CARTESIAN_POINT('Ctrl Pts',(46.3084068909562,-59.0643493136614,
-39.6395761233691));
#267964=CARTESIAN_POINT('Ctrl Pts',(46.2570407846102,-59.1209150453974,
-39.6404603784325));
#267965=CARTESIAN_POINT('Ctrl Pts',(46.1491379755941,-59.228544463199,-39.6404138814247));
#267966=CARTESIAN_POINT('Ctrl Pts',(46.0925836555155,-59.2796343044913,
-39.6394845811684));
#267967=CARTESIAN_POINT('Ctrl Pts',(46.0038529437629,-59.3521266125547,
-39.6367223387528));
#267968=CARTESIAN_POINT('Ctrl Pts',(45.9736068078661,-59.3756113554055,
-39.6355721163029));
#267969=CARTESIAN_POINT('Ctrl Pts',(45.9272656961273,-59.4097723546528,
-39.6334997725088));
#267970=CARTESIAN_POINT('Ctrl Pts',(45.9116419215573,-59.4209912820171,
-39.6327502808957));
#267971=CARTESIAN_POINT('Ctrl Pts',(45.8800804794677,-59.4430610802669,
-39.6311351339295));
#267972=CARTESIAN_POINT('Ctrl Pts',(45.8321587971618,-59.4756823489919,
-39.628531354857));
#267973=CARTESIAN_POINT('Ctrl Pts',(45.7834097108732,-59.5062438963941,
-39.6254355071979));
#267974=CARTESIAN_POINT('Ctrl Pts',(45.717633106262,-59.5452481912826,-39.6208773262667));
#267975=CARTESIAN_POINT('Ctrl Pts',(45.6178307490054,-59.601113548897,-39.6133952897297));
#267976=CARTESIAN_POINT('Ctrl Pts',(45.4802897643185,-59.6652183443042,
-39.6008811885904));
#267977=CARTESIAN_POINT('Ctrl Pts',(45.3738098009101,-59.7055766782111,
-39.5896017905935));
#267978=CARTESIAN_POINT('Ctrl Pts',(45.3020778813705,-59.7307512119865,
-39.5816566825671));
#267979=CARTESIAN_POINT('Ctrl Pts',(45.2658207311094,-59.7424779859237,
-39.5774690651077));
#267980=CARTESIAN_POINT('Ctrl Pts',(45.1926264675053,-59.7641596016776,
-39.5686715125846));
#267981=CARTESIAN_POINT('Ctrl Pts',(45.1555073907618,-59.7741562512684,
-39.5640376159893));
#267982=CARTESIAN_POINT('Ctrl Pts',(45.0441315765335,-59.8011904590316,
-39.5496210468413));
#267983=CARTESIAN_POINT('Ctrl Pts',(44.9324484012679,-59.8224577850013,
-39.5341534065747));
#267984=CARTESIAN_POINT('Ctrl Pts',(44.8203079610257,-59.8353953605365,
-39.5171556909205));
#267985=CARTESIAN_POINT('Ctrl Pts',(44.7080184564226,-59.8455760612675,
-39.4996502778008));
#267986=CARTESIAN_POINT('Ctrl Pts',(44.6329372249224,-59.8486931621852,
-39.4873001861445));
#267987=CARTESIAN_POINT('Ctrl Pts',(44.5200834441659,-59.8478515133141,
-39.4677634802869));
#267988=CARTESIAN_POINT('Ctrl Pts',(44.4823810871712,-59.8466449718289,
-39.4610736497974));
#267989=CARTESIAN_POINT('Ctrl Pts',(44.4258051079382,-59.8434394706745,
-39.4507883432074));
#267990=CARTESIAN_POINT('Ctrl Pts',(44.4069254589855,-59.8421361346926,
-39.4473147915973));
#267991=CARTESIAN_POINT('Ctrl Pts',(44.3691376542581,-59.8390581625153,
-39.4402793331445));
#267992=CARTESIAN_POINT('Ctrl Pts',(44.3502459350849,-59.8372838734483,
-39.4367203104461));
#267993=CARTESIAN_POINT('Ctrl Pts',(44.2562487381671,-59.8272835659938,
-39.4188041728073));
#267994=CARTESIAN_POINT('Ctrl Pts',(44.1080045765469,-59.8040393501646,
-39.3892226636159));
#267995=CARTESIAN_POINT('Ctrl Pts',(43.9639303529155,-59.7668593120831,
-39.3578670379715));
#267996=CARTESIAN_POINT('Ctrl Pts',(43.8219159040518,-59.7227861654643,
-39.3256251231267));
#267997=CARTESIAN_POINT('Ctrl Pts',(43.7519290534068,-59.6972943066161,
-39.3090578287531));
#267998=CARTESIAN_POINT('Ctrl Pts',(43.665783177736,-59.6610675807531,-39.2877890488175));
#267999=CARTESIAN_POINT('Ctrl Pts',(43.6486106666635,-59.653596197985,-39.2835041280971));
#268000=CARTESIAN_POINT('Ctrl Pts',(43.6144193015916,-59.6382222359849,
-39.2748825183767));
#268001=CARTESIAN_POINT('Ctrl Pts',(43.597366582891,-59.6303022352814,-39.2705368924251));
#268002=CARTESIAN_POINT('Ctrl Pts',(43.5465994182959,-59.605961903298,-39.2574616452183));
#268003=CARTESIAN_POINT('Ctrl Pts',(43.513329300663,-59.588993111175,-39.2487085268073));
#268004=CARTESIAN_POINT('Ctrl Pts',(43.4805771074156,-59.5712767529309,
-39.2399080357013));
#268005=CARTESIAN_POINT('Ctrl Pts',(43.8903154257419,-57.7291941381088,
-41.4266127101804));
#268006=CARTESIAN_POINT('Ctrl Pts',(43.8716814361492,-57.7189244770852,
-41.4090117279687));
#268007=CARTESIAN_POINT('Ctrl Pts',(43.8355945080866,-57.6967277837834,
-41.3734625137379));
#268008=CARTESIAN_POINT('Ctrl Pts',(43.7849271573585,-57.6585752750105,
-41.3191078559793));
#268009=CARTESIAN_POINT('Ctrl Pts',(43.753465403225,-57.62988352171,-41.2821707250961));
#268010=CARTESIAN_POINT('Ctrl Pts',(43.7232071092872,-57.5995155202448,
-41.2448779944712));
#268011=CARTESIAN_POINT('Ctrl Pts',(43.694633283399,-57.5679550683129,-41.2078231506529));
#268012=CARTESIAN_POINT('Ctrl Pts',(43.6629744005209,-57.5256074013359,
-41.162062942605));
#268013=CARTESIAN_POINT('Ctrl Pts',(43.6400741040405,-57.4900012877665,
-41.1257945258022));
#268014=CARTESIAN_POINT('Ctrl Pts',(43.624122646482,-57.4624228770549,-41.0987642906252));
#268015=CARTESIAN_POINT('Ctrl Pts',(43.6143188854815,-57.4434516436916,
-41.0808660102928));
#268016=CARTESIAN_POINT('Ctrl Pts',(43.6049343759216,-57.4241698350281,
-41.0630203901697));
#268017=CARTESIAN_POINT('Ctrl Pts',(43.6004882740613,-57.4144479878336,
-41.054192925399));
#268018=CARTESIAN_POINT('Ctrl Pts',(43.5878889573419,-57.3850715912746,
-41.0280183011396));
#268019=CARTESIAN_POINT('Ctrl Pts',(43.5730447416356,-57.3453166524842,
-40.9939147159844));
#268020=CARTESIAN_POINT('Ctrl Pts',(43.5620571572655,-57.3044044614592,
-40.9613948378065));
#268021=CARTESIAN_POINT('Ctrl Pts',(43.5552843243605,-57.2732819874194,
-40.9376151994878));
#268022=CARTESIAN_POINT('Ctrl Pts',(43.5532714802541,-57.2628325912303,
-40.9297890667463));
#268023=CARTESIAN_POINT('Ctrl Pts',(43.5497454556161,-57.2417890776549,
-40.9143485382007));
#268024=CARTESIAN_POINT('Ctrl Pts',(43.5482304746054,-57.2311797832666,
-40.9067234564832));
#268025=CARTESIAN_POINT('Ctrl Pts',(43.5457184756399,-57.2098591834555,
-40.8917243418755));
#268026=CARTESIAN_POINT('Ctrl Pts',(43.5447290487245,-57.199220662917,-40.8844009198028));
#268027=CARTESIAN_POINT('Ctrl Pts',(43.5432711863927,-57.1779500447907,
-40.8700767121812));
#268028=CARTESIAN_POINT('Ctrl Pts',(43.5418684734652,-57.1460721839032,
-40.8490875836402));
#268029=CARTESIAN_POINT('Ctrl Pts',(43.5431039253892,-57.1036793909824,
-40.8230787545116));
#268030=CARTESIAN_POINT('Ctrl Pts',(43.5463738329101,-57.0719682486671,
-40.8050747359183));
#268031=CARTESIAN_POINT('Ctrl Pts',(43.5490829635055,-57.0508462881094,
-40.7934126279614));
#268032=CARTESIAN_POINT('Ctrl Pts',(43.5507030159248,-57.0402904723448,
-40.7877497380755));
#268033=CARTESIAN_POINT('Ctrl Pts',(43.5544790630841,-57.019214904491,-40.7767808895002));
#268034=CARTESIAN_POINT('Ctrl Pts',(43.5566463931059,-57.0086510117152,
-40.7714540988351));
#268035=CARTESIAN_POINT('Ctrl Pts',(43.5614808344627,-56.9877741662596,
-40.7612719783604));
#268036=CARTESIAN_POINT('Ctrl Pts',(43.5668234022498,-56.9670831174431,
-40.7515253398262));
#268037=CARTESIAN_POINT('Ctrl Pts',(43.5763377125496,-56.9366295208774,
-40.7382165180791));
#268038=CARTESIAN_POINT('Ctrl Pts',(43.5873444561754,-56.9067460923864,
-40.7262089422516));
#268039=CARTESIAN_POINT('Ctrl Pts',(43.5998453117462,-56.8774358278222,
-40.7155085881795));
#268040=CARTESIAN_POINT('Ctrl Pts',(43.6091839698139,-56.8582805167828,
-40.7092555817853));
#268041=CARTESIAN_POINT('Ctrl Pts',(43.6190331668358,-56.8393207538612,
-40.7034508410834));
#268042=CARTESIAN_POINT('Ctrl Pts',(43.6242099732076,-56.8299438685379,
-40.7007739810578));
#268043=CARTESIAN_POINT('Ctrl Pts',(43.6350986096338,-56.8113693026126,
-40.6958744145609));
#268044=CARTESIAN_POINT('Ctrl Pts',(43.6407690742328,-56.8022426567881,
-40.6936706244929));
#268045=CARTESIAN_POINT('Ctrl Pts',(43.6583896223854,-56.7754411523649,
-40.6878155334118));
#268046=CARTESIAN_POINT('Ctrl Pts',(43.6709801307092,-56.7582712890167,
-40.6848937134075));
#268047=CARTESIAN_POINT('Ctrl Pts',(43.6978023804218,-56.725340315416,-40.6809957255822));
#268048=CARTESIAN_POINT('Ctrl Pts',(43.7120405319879,-56.7095692151415,
-40.6800172734785));
#268049=CARTESIAN_POINT('Ctrl Pts',(43.7346338722206,-56.6869796178674,
-40.680019660452));
#268050=CARTESIAN_POINT('Ctrl Pts',(43.7423799312797,-56.6796208977126,
-40.6802668752224));
#268051=CARTESIAN_POINT('Ctrl Pts',(43.7543060585229,-56.6688607312791,
-40.681010981358));
#268052=CARTESIAN_POINT('Ctrl Pts',(43.7583370517177,-56.6653168192219,
-40.6813218268212));
#268053=CARTESIAN_POINT('Ctrl Pts',(43.7665035456834,-56.6583217341419,
-40.6820693651562));
#268054=CARTESIAN_POINT('Ctrl Pts',(43.7706422703,-56.6548683091639,-40.6825066780886));
#268055=CARTESIAN_POINT('Ctrl Pts',(43.7831478581881,-56.6447045100584,
-40.6840009724959));
#268056=CARTESIAN_POINT('Ctrl Pts',(43.8000992888712,-56.6316392340345,
-40.6864805452653));
#268057=CARTESIAN_POINT('Ctrl Pts',(43.8351004518507,-56.6074069729907,
-40.6933496988796));
#268058=CARTESIAN_POINT('Ctrl Pts',(43.8717190640765,-56.5859796680779,
-40.7030349737613));
#268059=CARTESIAN_POINT('Ctrl Pts',(43.9003898794618,-56.5719991465823,
-40.7123924126099));
#268060=CARTESIAN_POINT('Ctrl Pts',(43.919774692733,-56.5631479893168,-40.719099824507));
#268061=CARTESIAN_POINT('Ctrl Pts',(43.9296053152689,-56.5589560552736,
-40.722689237866));
#268062=CARTESIAN_POINT('Ctrl Pts',(43.9495302416178,-56.551051384942,-40.7303379810773));
#268063=CARTESIAN_POINT('Ctrl Pts',(43.959660471973,-56.5473282955902,-40.7344135607172));
#268064=CARTESIAN_POINT('Ctrl Pts',(43.9799461530017,-56.5404515818703,
-40.7429393172485));
#268065=CARTESIAN_POINT('Ctrl Pts',(43.9901452646573,-56.5372793127045,
-40.7474054189318));
#268066=CARTESIAN_POINT('Ctrl Pts',(44.0208712025373,-56.5285586047056,
-40.7613849151889));
#268067=CARTESIAN_POINT('Ctrl Pts',(44.0518784813599,-56.521416173947,-40.7765333604643));
#268068=CARTESIAN_POINT('Ctrl Pts',(44.0937728041468,-56.5149820273198,
-40.799005697554));
#268069=CARTESIAN_POINT('Ctrl Pts',(44.1254693703652,-56.5117027703592,
-40.8169947136667));
#268070=CARTESIAN_POINT('Ctrl Pts',(44.1467868482481,-56.5105547568045,
-40.8297474946377));
#268071=CARTESIAN_POINT('Ctrl Pts',(44.1681963264173,-56.50993223545,-40.842882238999));
#268072=CARTESIAN_POINT('Ctrl Pts',(44.1789665479467,-56.509886262238,-40.8496544547178));
#268073=CARTESIAN_POINT('Ctrl Pts',(44.2003410646824,-56.5103214152413,
-40.8634176853611));
#268074=CARTESIAN_POINT('Ctrl Pts',(44.2109953322312,-56.5108003631786,
-40.8704389119319));
#268075=CARTESIAN_POINT('Ctrl Pts',(44.2322091102727,-56.5122711761573,
-40.8847351429132));
#268076=CARTESIAN_POINT('Ctrl Pts',(44.2639028799147,-56.5152466319394,
-40.9065696963621));
#268077=CARTESIAN_POINT('Ctrl Pts',(44.305661850593,-56.5222422564611,-40.9372114433545));
#268078=CARTESIAN_POINT('Ctrl Pts',(44.346925841944,-56.532247127269,-40.9693597045385));
#268079=CARTESIAN_POINT('Ctrl Pts',(44.3673876336497,-56.53826115526,-40.9859357593442));
#268080=CARTESIAN_POINT('Ctrl Pts',(44.3877715667723,-56.5447901720246,
-41.0027718870644));
#268081=CARTESIAN_POINT('Ctrl Pts',(44.3979208506631,-56.5483132560745,
-41.0113182564434));
#268082=CARTESIAN_POINT('Ctrl Pts',(44.4179418071922,-56.5558066378292,
-41.02850287128));
#268083=CARTESIAN_POINT('Ctrl Pts',(44.4278499085732,-56.5597882829787,
-41.0371710128992));
#268084=CARTESIAN_POINT('Ctrl Pts',(44.4572364860018,-56.5724196473794,
-41.0633712499365));
#268085=CARTESIAN_POINT('Ctrl Pts',(44.4763932211824,-56.581758968269,-41.0811111519311));
#268086=CARTESIAN_POINT('Ctrl Pts',(44.5044772880921,-56.5971447477014,
-41.1081262866225));
#268087=CARTESIAN_POINT('Ctrl Pts',(44.5137271775895,-56.6025015227711,
-41.1171962449124));
#268088=CARTESIAN_POINT('Ctrl Pts',(44.5320183562985,-56.6136863880645,
-41.1354834617267));
#268089=CARTESIAN_POINT('Ctrl Pts',(44.5410031705763,-56.6194798267371,
-41.144644186283));
#268090=CARTESIAN_POINT('Ctrl Pts',(44.5674276642847,-56.6374191091633,
-41.1721205907467));
#268091=CARTESIAN_POINT('Ctrl Pts',(44.5843870769067,-56.6501457393646,
-41.1904750382678));
#268092=CARTESIAN_POINT('Ctrl Pts',(44.616987890196,-56.6770839740703,-41.2272237610649));
#268093=CARTESIAN_POINT('Ctrl Pts',(44.640458797708,-56.6984048650555,-41.2548228473058));
#268094=CARTESIAN_POINT('Ctrl Pts',(44.6624514458289,-56.7214114906953,
-41.2824783924342));
#268095=CARTESIAN_POINT('Ctrl Pts',(44.6767798128067,-56.7371294193188,
-41.3009283158679));
#268096=CARTESIAN_POINT('Ctrl Pts',(44.683774397772,-56.7451748501741,-41.3101557240219));
#268097=CARTESIAN_POINT('Ctrl Pts',(44.6940202659092,-56.7575442973705,
-41.324018848177));
#268098=CARTESIAN_POINT('Ctrl Pts',(44.6973914635031,-56.7617145235639,
-41.328639728599));
#268099=CARTESIAN_POINT('Ctrl Pts',(44.7040131878578,-56.770108052971,-41.3378361513053));
#268100=CARTESIAN_POINT('Ctrl Pts',(44.7072703203268,-56.7743392575068,
-41.3424205878605));
#268101=CARTESIAN_POINT('Ctrl Pts',(44.7168707027477,-56.7871217033085,
-41.3561177927451));
#268102=CARTESIAN_POINT('Ctrl Pts',(44.7230524906066,-56.7957731420119,
-41.3651872799216));
#268103=CARTESIAN_POINT('Ctrl Pts',(44.7409373255192,-56.8220955492914,
-41.3921945478314));
#268104=CARTESIAN_POINT('Ctrl Pts',(44.7575187561203,-56.8491712652862,
-41.4188207502394));
#268105=CARTESIAN_POINT('Ctrl Pts',(44.7770214494108,-56.88676384976,-41.453559097464));
#268106=CARTESIAN_POINT('Ctrl Pts',(44.7858965000619,-56.9060633365117,
-41.4706740459328));
#268107=CARTESIAN_POINT('Ctrl Pts',(44.7943266372896,-56.9256180211132,
-41.4876605613939));
#268108=CARTESIAN_POINT('Ctrl Pts',(44.7983169540911,-56.9355169983302,
-41.4960845962979));
#268109=CARTESIAN_POINT('Ctrl Pts',(44.8058516078422,-56.9556000996462,
-41.5128223385875));
#268110=CARTESIAN_POINT('Ctrl Pts',(44.8093727854448,-56.9657242505397,
-41.5210856532432));
#268111=CARTESIAN_POINT('Ctrl Pts',(44.8191505788346,-56.9961959016236,
-41.5454418374945));
#268112=CARTESIAN_POINT('Ctrl Pts',(44.8246597322132,-57.0167187198372,
-41.5611704866007));
#268113=CARTESIAN_POINT('Ctrl Pts',(44.8336688220904,-57.0581479791523,
-41.5916045035181));
#268114=CARTESIAN_POINT('Ctrl Pts',(44.8389236650083,-57.0895139074259,
-41.613669368427));
#268115=CARTESIAN_POINT('Ctrl Pts',(44.8418900765893,-57.1213299669285,
-41.6345866129535));
#268116=CARTESIAN_POINT('Ctrl Pts',(44.8433488372948,-57.142640498193,-41.6482710687869));
#268117=CARTESIAN_POINT('Ctrl Pts',(44.8438191277705,-57.1533552116615,
-41.6549890353504));
#268118=CARTESIAN_POINT('Ctrl Pts',(44.8442270800594,-57.1748537940466,
-41.6681388704993));
#268119=CARTESIAN_POINT('Ctrl Pts',(44.8441639040618,-57.1855561823783,
-41.6745213422017));
#268120=CARTESIAN_POINT('Ctrl Pts',(44.8435122114514,-57.2069000331791,
-41.6869277892926));
#268121=CARTESIAN_POINT('Ctrl Pts',(44.8417458896958,-57.2388084678274,
-41.7049896680882));
#268122=CARTESIAN_POINT('Ctrl Pts',(44.8362687719071,-57.2809279665006,
-41.7269106712316));
#268123=CARTESIAN_POINT('Ctrl Pts',(44.8298088085522,-57.3121969378441,
-41.7417325167562));
#268124=CARTESIAN_POINT('Ctrl Pts',(44.8249713776488,-57.3329705079708,
-41.751249414817));
#268125=CARTESIAN_POINT('Ctrl Pts',(44.8222858794974,-57.3433254378487,
-41.7558274666229));
#268126=CARTESIAN_POINT('Ctrl Pts',(44.8163797073795,-57.3639440769784,
-41.7646063213672));
#268127=CARTESIAN_POINT('Ctrl Pts',(44.8131427147447,-57.3742522416544,
-41.7688238948253));
#268128=CARTESIAN_POINT('Ctrl Pts',(44.8061917406462,-57.3945668799698,
-41.7767918599254));
#268129=CARTESIAN_POINT('Ctrl Pts',(44.7987498536529,-57.4146412549335,
-41.7843210101159));
#268130=CARTESIAN_POINT('Ctrl Pts',(44.7861419817956,-57.4440129710611,
-41.7943060987191));
#268131=CARTESIAN_POINT('Ctrl Pts',(44.7720982599006,-57.4726583092559,
-41.8029984035242));
#268132=CARTESIAN_POINT('Ctrl Pts',(44.7566193423106,-57.5005749992605,
-41.8103989883131));
#268133=CARTESIAN_POINT('Ctrl Pts',(44.7453362941317,-57.518697088903,-41.8144666236875));
#268134=CARTESIAN_POINT('Ctrl Pts',(44.7335642473644,-57.5365709174371,
-41.8180952379985));
#268135=CARTESIAN_POINT('Ctrl Pts',(44.7274378249752,-57.5453780864623,
-41.8196891344695));
#268136=CARTESIAN_POINT('Ctrl Pts',(44.7146685840676,-57.5627610237142,
-41.8224320230444));
#268137=CARTESIAN_POINT('Ctrl Pts',(44.7080700862024,-57.5712755128024,
-41.8235709343319));
#268138=CARTESIAN_POINT('Ctrl Pts',(44.6877341610586,-57.5961705213949,
-41.8262807978491));
#268139=CARTESIAN_POINT('Ctrl Pts',(44.6734117165454,-57.6119810052107,
-41.8271650529119));
#268140=CARTESIAN_POINT('Ctrl Pts',(44.6432859415473,-57.6420285404153,
-41.827118555904));
#268141=CARTESIAN_POINT('Ctrl Pts',(44.6274777219699,-57.6562729242579,
-41.8261892556471));
#268142=CARTESIAN_POINT('Ctrl Pts',(44.6026489360012,-57.6764545436153,
-41.823427013232));
#268143=CARTESIAN_POINT('Ctrl Pts',(44.5941811636919,-57.6829873126311,
-41.8222767907821));
#268144=CARTESIAN_POINT('Ctrl Pts',(44.5812011369499,-57.6924815728277,
-41.820204446988));
#268145=CARTESIAN_POINT('Ctrl Pts',(44.5768239301145,-57.6955981764101,
-41.8194549553751));
#268146=CARTESIAN_POINT('Ctrl Pts',(44.5679795363474,-57.7017261947271,
-41.8178398084084));
#268147=CARTESIAN_POINT('Ctrl Pts',(44.554547495243,-57.7107794649358,-41.8152360293365));
#268148=CARTESIAN_POINT('Ctrl Pts',(44.5408745509057,-57.7192473537464,
-41.812140181677));
#268149=CARTESIAN_POINT('Ctrl Pts',(44.5224181841827,-57.7300417662926,
-41.8075820007456));
#268150=CARTESIAN_POINT('Ctrl Pts',(44.494403164631,-57.7454824222945,-41.8000999642091));
#268151=CARTESIAN_POINT('Ctrl Pts',(44.4557509611988,-57.7631175354143,
-41.7875858630695));
#268152=CARTESIAN_POINT('Ctrl Pts',(44.4257963579031,-57.7741479888816,
-41.7763064650726));
#268153=CARTESIAN_POINT('Ctrl Pts',(44.4056101875344,-57.781009218212,-41.7683613570464));
#268154=CARTESIAN_POINT('Ctrl Pts',(44.3954036594654,-57.7841949818065,
-41.7641737395871));
#268155=CARTESIAN_POINT('Ctrl Pts',(44.3747925009816,-57.7900627169564,
-41.7553761870634));
#268156=CARTESIAN_POINT('Ctrl Pts',(44.3643365899562,-57.7927558542442,
-41.7507422904685));
#268157=CARTESIAN_POINT('Ctrl Pts',(44.3329536886806,-57.7999988857253,
-41.7363257213199));
#268158=CARTESIAN_POINT('Ctrl Pts',(44.3014645871824,-57.8056090798854,
-41.7208580810542));
#268159=CARTESIAN_POINT('Ctrl Pts',(44.2698183189435,-57.8088603667088,
-41.7038603653999));
#268160=CARTESIAN_POINT('Ctrl Pts',(44.2381206623806,-57.8113308880715,
-41.6863549522799));
#268161=CARTESIAN_POINT('Ctrl Pts',(44.2169139506954,-57.8119384373532,
-41.6740048606234));
#268162=CARTESIAN_POINT('Ctrl Pts',(44.1850197107514,-57.811287280344,-41.6544681547659));
#268163=CARTESIAN_POINT('Ctrl Pts',(44.1743613109546,-57.8108078241776,
-41.6477783242763));
#268164=CARTESIAN_POINT('Ctrl Pts',(44.1583626375358,-57.8096935003687,
-41.6374930176863));
#268165=CARTESIAN_POINT('Ctrl Pts',(44.1530230189312,-57.809255510817,-41.6340194660765));
#268166=CARTESIAN_POINT('Ctrl Pts',(44.1423341247923,-57.8082460206643,
-41.6269840076234));
#268167=CARTESIAN_POINT('Ctrl Pts',(44.1369894952372,-57.8076746784434,
-41.6234249849254));
#268168=CARTESIAN_POINT('Ctrl Pts',(44.1103928894951,-57.8045001122898,
-41.6055088472864));
#268169=CARTESIAN_POINT('Ctrl Pts',(44.0684216046586,-57.7973782151022,
-41.5759273380954));
#268170=CARTESIAN_POINT('Ctrl Pts',(44.0275807082801,-57.78632659952,-41.5445717124501));
#268171=CARTESIAN_POINT('Ctrl Pts',(43.9872978152183,-57.7733311875938,
-41.5123297976061));
#268172=CARTESIAN_POINT('Ctrl Pts',(43.9674326520914,-57.7658590768128,
-41.4957625032292));
#268173=CARTESIAN_POINT('Ctrl Pts',(43.942963744406,-57.7552890823142,-41.4744937232973));
#268174=CARTESIAN_POINT('Ctrl Pts',(43.938085174092,-57.7531113051098,-41.4702088025761));
#268175=CARTESIAN_POINT('Ctrl Pts',(43.9283699185172,-57.7486342535987,
-41.4615871928557));
#268176=CARTESIAN_POINT('Ctrl Pts',(43.9235236029976,-57.7463299238453,
-41.4572415669043));
#268177=CARTESIAN_POINT('Ctrl Pts',(43.9090930604083,-57.739254093668,-41.4441663196977));
#268178=CARTESIAN_POINT('Ctrl Pts',(43.8996324205383,-57.7343289686206,
-41.4354132012863));
#268179=CARTESIAN_POINT('Ctrl Pts',(43.8903154257419,-57.7291941381088,
-41.4266127101804));
#268180=CARTESIAN_POINT('Ctrl Pts',(-43.4805771074156,-59.5712767529309,
-39.2399080357013));
#268181=CARTESIAN_POINT('Ctrl Pts',(-43.4478249141681,-59.5535603946867,
-39.2311075445953));
#268182=CARTESIAN_POINT('Ctrl Pts',(-43.4156056040519,-59.5351038997391,
-39.2222635806238));
#268183=CARTESIAN_POINT('Ctrl Pts',(-43.3522169440986,-59.4967328580069,
-39.2044893908274));
#268184=CARTESIAN_POINT('Ctrl Pts',(-43.3210476458595,-59.4768182391239,
-39.1955591618115));
#268185=CARTESIAN_POINT('Ctrl Pts',(-43.2291022595543,-59.4149049130521,
-39.1686393287622));
#268186=CARTESIAN_POINT('Ctrl Pts',(-43.1698853587931,-59.3707413041733,
-39.1505208045068));
#268187=CARTESIAN_POINT('Ctrl Pts',(-43.0556331620037,-59.2766097614945,
-39.113935063243));
#268188=CARTESIAN_POINT('Ctrl Pts',(-43.0005921597408,-59.2266373021163,
-39.0954660506179));
#268189=CARTESIAN_POINT('Ctrl Pts',(-42.8948534568781,-59.1207134074407,
-39.0581733199915));
#268190=CARTESIAN_POINT('Ctrl Pts',(-42.8449960553599,-59.0656056508999,
-39.0396463059707));
#268191=CARTESIAN_POINT('Ctrl Pts',(-42.7510811208719,-58.9512122276158,
-39.0028139665663));
#268192=CARTESIAN_POINT('Ctrl Pts',(-42.7070288152267,-58.891930638621,
-38.9845102727346));
#268193=CARTESIAN_POINT('Ctrl Pts',(-42.6452866349949,-58.7998958734659,
-38.957224077988));
#268194=CARTESIAN_POINT('Ctrl Pts',(-42.625429767352,-58.7686980621887,
-38.9481569597938));
#268195=CARTESIAN_POINT('Ctrl Pts',(-42.5871756130002,-58.7052546833099,
-38.9300801552924));
#268196=CARTESIAN_POINT('Ctrl Pts',(-42.568778253032,-58.6730091686672,
-38.9210704649552));
#268197=CARTESIAN_POINT('Ctrl Pts',(-42.5334651880811,-58.6074543754265,
-38.9031098981675));
#268198=CARTESIAN_POINT('Ctrl Pts',(-42.5165536369311,-58.5741539171446,
-38.8941613358138));
#268199=CARTESIAN_POINT('Ctrl Pts',(-42.4842288567228,-58.5064298632496,
-38.8763157156907));
#268200=CARTESIAN_POINT('Ctrl Pts',(-42.4689425396028,-58.4722695523732,
-38.8674882509199));
#268201=CARTESIAN_POINT('Ctrl Pts',(-42.4401223815193,-58.4034275140121,
-38.8500385014136));
#268202=CARTESIAN_POINT('Ctrl Pts',(-42.426583050894,-58.3687341967778,
-38.8414131698514));
#268203=CARTESIAN_POINT('Ctrl Pts',(-42.4012287918448,-58.2988104271035,
-38.824360868638));
#268204=CARTESIAN_POINT('Ctrl Pts',(-42.3894137611201,-58.2635796188005,
-38.8159338161007));
#268205=CARTESIAN_POINT('Ctrl Pts',(-42.3565461207186,-58.1570828582558,
-38.7909502725479));
#268206=CARTESIAN_POINT('Ctrl Pts',(-42.3380647902547,-58.0850119200903,
-38.7746901633276));
#268207=CARTESIAN_POINT('Ctrl Pts',(-42.3155659796374,-57.9752818499468,
-38.7509105250088));
#268208=CARTESIAN_POINT('Ctrl Pts',(-42.3089374211558,-57.9384266221928,
-38.7430843922672));
#268209=CARTESIAN_POINT('Ctrl Pts',(-42.297458012674,-57.864178756387,-38.7276438637217));
#268210=CARTESIAN_POINT('Ctrl Pts',(-42.292601515188,-57.8267325312259,
-38.720018782004));
#268211=CARTESIAN_POINT('Ctrl Pts',(-42.2847289916893,-57.7514526301959,
-38.7050196673962));
#268212=CARTESIAN_POINT('Ctrl Pts',(-42.2817363521424,-57.7138759968928,
-38.6976962453237));
#268213=CARTESIAN_POINT('Ctrl Pts',(-42.277596992864,-57.6387184974263,
-38.6833720377019));
#268214=CARTESIAN_POINT('Ctrl Pts',(-42.2764525301716,-57.6011593077097,
-38.6763755686054));
#268215=CARTESIAN_POINT('Ctrl Pts',(-42.2757726188108,-57.4885396176673,
-38.6558809641879));
#268216=CARTESIAN_POINT('Ctrl Pts',(-42.2789845428693,-57.4135368708757,
-38.6428765167438));
#268217=CARTESIAN_POINT('Ctrl Pts',(-42.289333314243,-57.3011476810195,
-38.6243712990017));
#268218=CARTESIAN_POINT('Ctrl Pts',(-42.2937061680812,-57.2637038035873,
-38.618370061439));
#268219=CARTESIAN_POINT('Ctrl Pts',(-42.3043247017591,-57.1888547452426,
-38.6067079534822));
#268220=CARTESIAN_POINT('Ctrl Pts',(-42.3105743117123,-57.1514345461221,
-38.6010450635964));
#268221=CARTESIAN_POINT('Ctrl Pts',(-42.3249704170347,-57.0766935209606,
-38.590076215021));
#268222=CARTESIAN_POINT('Ctrl Pts',(-42.3331592025312,-57.0392159768686,
-38.5847494243559));
#268223=CARTESIAN_POINT('Ctrl Pts',(-42.3512949844302,-56.9651221381903,
-38.5745673038812));
#268224=CARTESIAN_POINT('Ctrl Pts',(-42.3612586135401,-56.9283882021117,
-38.5696936317377));
#268225=CARTESIAN_POINT('Ctrl Pts',(-42.3829467968515,-56.8555905655333,
-38.5603848033813));
#268226=CARTESIAN_POINT('Ctrl Pts',(-42.3946724551093,-56.8195179901625,
-38.555948235663));
#268227=CARTESIAN_POINT('Ctrl Pts',(-42.4198760714445,-56.7480212016901,
-38.5475092141337));
#268228=CARTESIAN_POINT('Ctrl Pts',(-42.4333540386586,-56.712596992043,
-38.5435067618884));
#268229=CARTESIAN_POINT('Ctrl Pts',(-42.4620643651744,-56.6423976051736,
-38.5359375083953));
#268230=CARTESIAN_POINT('Ctrl Pts',(-42.4772967069948,-56.6076224215361,
-38.5323707022785));
#268231=CARTESIAN_POINT('Ctrl Pts',(-42.5095308031841,-56.5387265502116,
-38.5256774075877));
#268232=CARTESIAN_POINT('Ctrl Pts',(-42.5265325119253,-56.5046058456765,
-38.5225509073062));
#268233=CARTESIAN_POINT('Ctrl Pts',(-42.5623338475307,-56.4370293947696,
-38.5167461666044));
#268234=CARTESIAN_POINT('Ctrl Pts',(-42.5811223641794,-56.4035923099625,
-38.5140693065785));
#268235=CARTESIAN_POINT('Ctrl Pts',(-42.620584523009,-56.3373241998654,
-38.5091697400817));
#268236=CARTESIAN_POINT('Ctrl Pts',(-42.6411082254821,-56.3047465904101,
-38.5069659500128));
#268237=CARTESIAN_POINT('Ctrl Pts',(-42.7048067991197,-56.2090283357163,
-38.5011108589349));
#268238=CARTESIAN_POINT('Ctrl Pts',(-42.7502234543428,-56.1476408662828,
-38.4981890389281));
#268239=CARTESIAN_POINT('Ctrl Pts',(-42.846794232383,-56.0297655581676,
-38.4942910511032));
#268240=CARTESIAN_POINT('Ctrl Pts',(-42.8979715413934,-55.9732420482177,
-38.4933125989996));
#268241=CARTESIAN_POINT('Ctrl Pts',(-42.9790570553346,-55.8921695883032,
-38.4933149859728));
#268242=CARTESIAN_POINT('Ctrl Pts',(-43.0068374106561,-55.8657400908869,
-38.4935622007431));
#268243=CARTESIAN_POINT('Ctrl Pts',(-43.0495800649421,-55.8270637749536,
-38.4943063068789));
#268244=CARTESIAN_POINT('Ctrl Pts',(-43.0640222060113,-55.8143203511958,
-38.494617152342));
#268245=CARTESIAN_POINT('Ctrl Pts',(-43.0932714774893,-55.7891564261061,
-38.4953646906773));
#268246=CARTESIAN_POINT('Ctrl Pts',(-43.1080901283633,-55.7767277938553,
-38.4958020036096));
#268247=CARTESIAN_POINT('Ctrl Pts',(-43.1528523310046,-55.7401327167866,
-38.4972962980169));
#268248=CARTESIAN_POINT('Ctrl Pts',(-43.183171240984,-55.7165901373356,
-38.498536032863));
#268249=CARTESIAN_POINT('Ctrl Pts',(-43.2447583556422,-55.6711691509155,
-38.5014931332815));
#268250=CARTESIAN_POINT('Ctrl Pts',(-43.2760240909102,-55.6492920896315,
-38.5032102926999));
#268251=CARTESIAN_POINT('Ctrl Pts',(-43.37121764534,-55.5861255243223,-38.5090666584048));
#268252=CARTESIAN_POINT('Ctrl Pts',(-43.4365388292261,-55.5472953809443,
-38.5139093068404));
#268253=CARTESIAN_POINT('Ctrl Pts',(-43.5372923455653,-55.4939420631336,
-38.5225684468354));
#268254=CARTESIAN_POINT('Ctrl Pts',(-43.5713395927683,-55.4769743237494,
-38.5256877381308));
#268255=CARTESIAN_POINT('Ctrl Pts',(-43.6403672861995,-55.4446857735354,
-38.5323951500278));
#268256=CARTESIAN_POINT('Ctrl Pts',(-43.6753577685123,-55.4293620157832,
-38.5359845633874));
#268257=CARTESIAN_POINT('Ctrl Pts',(-43.7462462065787,-55.4003985583156,
-38.5436333065981));
#268258=CARTESIAN_POINT('Ctrl Pts',(-43.7822717759725,-55.3867204456352,
-38.5477088862383));
#268259=CARTESIAN_POINT('Ctrl Pts',(-43.8543821738219,-55.3613797848081,
-38.5562346427693));
#268260=CARTESIAN_POINT('Ctrl Pts',(-43.890622407919,-55.349649082917,-38.5607007444526));
#268261=CARTESIAN_POINT('Ctrl Pts',(-43.9633781832422,-55.3280633380684,
-38.5700204086244));
#268262=CARTESIAN_POINT('Ctrl Pts',(-43.9999084022592,-55.3182019076378,
-38.5748754846743));
#268263=CARTESIAN_POINT('Ctrl Pts',(-44.0732691651704,-55.300314394282,
-38.5849692074244));
#268264=CARTESIAN_POINT('Ctrl Pts',(-44.1100997159262,-55.2922883538608,
-38.590207863671));
#268265=CARTESIAN_POINT('Ctrl Pts',(-44.1840590812038,-55.2780579645929,
-38.6010647047639));
#268266=CARTESIAN_POINT('Ctrl Pts',(-44.2211878979616,-55.2718536300564,
-38.6066828933265));
#268267=CARTESIAN_POINT('Ctrl Pts',(-44.2957439071301,-55.2612662316006,
-38.6182974837333));
#268268=CARTESIAN_POINT('Ctrl Pts',(-44.3331710973477,-55.256883155031,
-38.624293883757));
#268269=CARTESIAN_POINT('Ctrl Pts',(-44.4083261383181,-55.2499510742625,
-38.6366662922177));
#268270=CARTESIAN_POINT('Ctrl Pts',(-44.446056048267,-55.2474029004138,
-38.6430428201589));
#268271=CARTESIAN_POINT('Ctrl Pts',(-44.5218128020516,-55.2441636366351,
-38.6561775645199));
#268272=CARTESIAN_POINT('Ctrl Pts',(-44.5599089424743,-55.2434808562086,
-38.6629497802385));
#268273=CARTESIAN_POINT('Ctrl Pts',(-44.6354869543582,-55.2439911084578,
-38.6767130108817));
#268274=CARTESIAN_POINT('Ctrl Pts',(-44.6731456892459,-55.2451740103824,
-38.6837342374529));
#268275=CARTESIAN_POINT('Ctrl Pts',(-44.7481014788608,-55.2493620066237,
-38.6980304684339));
#268276=CARTESIAN_POINT('Ctrl Pts',(-44.7854165850557,-55.2523662274994,
-38.7053085862828));
#268277=CARTESIAN_POINT('Ctrl Pts',(-44.8968808056053,-55.2640710758905,
-38.7275256543264));
#268278=CARTESIAN_POINT('Ctrl Pts',(-44.9705498158105,-55.2754583368831,
-38.7428465194087));
#268279=CARTESIAN_POINT('Ctrl Pts',(-45.0801001998238,-55.2978810544009,
-38.7665804202115));
#268280=CARTESIAN_POINT('Ctrl Pts',(-45.1164578754129,-55.3062470656085,
-38.7746173707339));
#268281=CARTESIAN_POINT('Ctrl Pts',(-45.1888527653151,-55.3247763762561,
-38.790943453482));
#268282=CARTESIAN_POINT('Ctrl Pts',(-45.2248832056965,-55.3349380951144,
-38.7992310848652));
#268283=CARTESIAN_POINT('Ctrl Pts',(-45.2966462681613,-55.3570913336823,
-38.8160672125853));
#268284=CARTESIAN_POINT('Ctrl Pts',(-45.3323638946335,-55.3690863290504,
-38.8246135819642));
#268285=CARTESIAN_POINT('Ctrl Pts',(-45.4027951436545,-55.3946744461232,
-38.841798196801));
#268286=CARTESIAN_POINT('Ctrl Pts',(-45.4376370321487,-55.4083060218429,
-38.85046633842));
#268287=CARTESIAN_POINT('Ctrl Pts',(-45.506502018173,-55.4372015589607,
-38.8679331631116));
#268288=CARTESIAN_POINT('Ctrl Pts',(-45.5405385021803,-55.4524695986684,
-38.8767349781349));
#268289=CARTESIAN_POINT('Ctrl Pts',(-45.6078227545416,-55.4846397884912,
-38.894474157443));
#268290=CARTESIAN_POINT('Ctrl Pts',(-45.6410705220074,-55.5015419401624,
-38.903411522349));
#268291=CARTESIAN_POINT('Ctrl Pts',(-45.6739227548726,-55.5192637629152,
-38.9124165672463));
#268292=CARTESIAN_POINT('Ctrl Pts',(-43.5555682511181,-59.2341350312479,
-39.6401231904583));
#268293=CARTESIAN_POINT('Ctrl Pts',(-43.5271052157456,-59.2187213699007,
-39.6313226993523));
#268294=CARTESIAN_POINT('Ctrl Pts',(-43.4991046027441,-59.2026650473832,
-39.6224787353808));
#268295=CARTESIAN_POINT('Ctrl Pts',(-43.4440144956751,-59.1692863795892,
-39.6047045455842));
#268296=CARTESIAN_POINT('Ctrl Pts',(-43.416925046393,-59.151963971707,-39.5957743165685));
#268297=CARTESIAN_POINT('Ctrl Pts',(-43.3370125740194,-59.0981130112185,
-39.5688544835192));
#268298=CARTESIAN_POINT('Ctrl Pts',(-43.2855425446096,-59.0597046874419,
-39.5507359592637));
#268299=CARTESIAN_POINT('Ctrl Pts',(-43.1862310165518,-58.9778482320248,
-39.5141502180001));
#268300=CARTESIAN_POINT('Ctrl Pts',(-43.1383845581245,-58.9343961646677,
-39.4956812053746));
#268301=CARTESIAN_POINT('Ctrl Pts',(-43.0464604338337,-58.8423006638519,
-39.4583884747487));
#268302=CARTESIAN_POINT('Ctrl Pts',(-43.0031132840443,-58.7943907659202,
-39.4398614607275));
#268303=CARTESIAN_POINT('Ctrl Pts',(-42.9214542034191,-58.69494537932,-39.4030291213234));
#268304=CARTESIAN_POINT('Ctrl Pts',(-42.8831468162938,-58.6434134367091,
-39.3847254274915));
#268305=CARTESIAN_POINT('Ctrl Pts',(-42.8294502801417,-58.563414667145,
-39.357439232745));
#268306=CARTESIAN_POINT('Ctrl Pts',(-42.8121798538915,-58.536297551274,
-39.3483721145507));
#268307=CARTESIAN_POINT('Ctrl Pts',(-42.7789061306717,-58.4811541100691,
-39.3302953100494));
#268308=CARTESIAN_POINT('Ctrl Pts',(-42.7629027701056,-58.4531278306783,
-39.3212856197121));
#268309=CARTESIAN_POINT('Ctrl Pts',(-42.732182334752,-58.396152181943,-39.3033250529244));
#268310=CARTESIAN_POINT('Ctrl Pts',(-42.7174688743488,-58.3672104781721,
-39.2943764905707));
#268311=CARTESIAN_POINT('Ctrl Pts',(-42.6893426693184,-58.308352422918,
-39.2765308704477));
#268312=CARTESIAN_POINT('Ctrl Pts',(-42.676040350531,-58.2786648895678,
-39.2677034056768));
#268313=CARTESIAN_POINT('Ctrl Pts',(-42.6509576148479,-58.2188381095861,
-39.2502536561705));
#268314=CARTESIAN_POINT('Ctrl Pts',(-42.6391724212676,-58.1886887904878,
-39.2416283246084));
#268315=CARTESIAN_POINT('Ctrl Pts',(-42.6170995346736,-58.12792477379,-39.224576023395));
#268316=CARTESIAN_POINT('Ctrl Pts',(-42.6068117525533,-58.0973097669517,
-39.2161489708576));
#268317=CARTESIAN_POINT('Ctrl Pts',(-42.578186703978,-58.0047678749905,
-39.1911654273048));
#268318=CARTESIAN_POINT('Ctrl Pts',(-42.5620823726479,-57.9421435490173,
-39.1749053180845));
#268319=CARTESIAN_POINT('Ctrl Pts',(-42.5424617625838,-57.8468004016288,
-39.1511256797658));
#268320=CARTESIAN_POINT('Ctrl Pts',(-42.5366779815724,-57.8147780230883,
-39.1432995470242));
#268321=CARTESIAN_POINT('Ctrl Pts',(-42.5266542176424,-57.7502677264705,
-39.1278590184786));
#268322=CARTESIAN_POINT('Ctrl Pts',(-42.5224092913251,-57.7177332511804,
-39.120233936761));
#268323=CARTESIAN_POINT('Ctrl Pts',(-42.5155178619726,-57.6523290916439,
-39.1052348221532));
#268324=CARTESIAN_POINT('Ctrl Pts',(-42.5128918544921,-57.6196827267464,
-39.0979114000806));
#268325=CARTESIAN_POINT('Ctrl Pts',(-42.5092432682604,-57.5543877143394,
-39.0835871924589));
#268326=CARTESIAN_POINT('Ctrl Pts',(-42.5082226653386,-57.5217578995943,
-39.0765907233623));
#268327=CARTESIAN_POINT('Ctrl Pts',(-42.5075526709299,-57.4239208272887,
-39.0560961189448));
#268328=CARTESIAN_POINT('Ctrl Pts',(-42.5102897909719,-57.3587658283315,
-39.0430916715008));
#268329=CARTESIAN_POINT('Ctrl Pts',(-42.5191999190634,-57.2611374049919,
-39.0245864537587));
#268330=CARTESIAN_POINT('Ctrl Pts',(-42.5229719620357,-57.2286119708033,
-39.018585216196));
#268331=CARTESIAN_POINT('Ctrl Pts',(-42.5321429006105,-57.1635961556059,
-39.0069231082391));
#268332=CARTESIAN_POINT('Ctrl Pts',(-42.5375451994904,-57.131092730784,
-39.0012602183534));
#268333=CARTESIAN_POINT('Ctrl Pts',(-42.5499976000816,-57.0661736672035,
-38.990291369778));
#268334=CARTESIAN_POINT('Ctrl Pts',(-42.5570843265014,-57.0336219145328,
-38.9849645791129));
#268335=CARTESIAN_POINT('Ctrl Pts',(-42.5727856698931,-56.9692679586228,
-38.9747824586382));
#268336=CARTESIAN_POINT('Ctrl Pts',(-42.5814146517845,-56.9373635689111,
-38.9699087864947));
#268337=CARTESIAN_POINT('Ctrl Pts',(-42.6002027387397,-56.8741384006643,
-38.9605999581383));
#268338=CARTESIAN_POINT('Ctrl Pts',(-42.6103627965689,-56.8428099130675,
-38.9561633904199));
#268339=CARTESIAN_POINT('Ctrl Pts',(-42.6322055381297,-56.7807175391602,
-38.9477243688907));
#268340=CARTESIAN_POINT('Ctrl Pts',(-42.643888229794,-56.7499536558588,
-38.9437219166454));
#268341=CARTESIAN_POINT('Ctrl Pts',(-42.6687780682593,-56.6889910719312,
-38.9361526631524));
#268342=CARTESIAN_POINT('Ctrl Pts',(-42.6819851998625,-56.6587923657221,
-38.9325858570355));
#268343=CARTESIAN_POINT('Ctrl Pts',(-42.7099369818181,-56.5989648901808,
-38.9258925623447));
#268344=CARTESIAN_POINT('Ctrl Pts',(-42.7246815925139,-56.5693361061833,
-38.9227660620632));
#268345=CARTESIAN_POINT('Ctrl Pts',(-42.7557331147216,-56.5106575807864,
-38.9169613213614));
#268346=CARTESIAN_POINT('Ctrl Pts',(-42.7720303883604,-56.4816240428195,
-38.9142844613354));
#268347=CARTESIAN_POINT('Ctrl Pts',(-42.8062629627728,-56.4240849025666,
-38.9093848948388));
#268348=CARTESIAN_POINT('Ctrl Pts',(-42.8240681953201,-56.3957993363617,
-38.9071811047699));
#268349=CARTESIAN_POINT('Ctrl Pts',(-42.8793334746424,-56.3126943660298,
-38.9013260136915));
#268350=CARTESIAN_POINT('Ctrl Pts',(-42.9187422214293,-56.2593996931541,
-38.8984041936851));
#268351=CARTESIAN_POINT('Ctrl Pts',(-43.0025474813891,-56.1570710705974,
-38.8945062058602));
#268352=CARTESIAN_POINT('Ctrl Pts',(-43.0469641103745,-56.1080061498824,
-38.8935277537565));
#268353=CARTESIAN_POINT('Ctrl Pts',(-43.117344267243,-56.0376373429099,
-38.8935301407298));
#268354=CARTESIAN_POINT('Ctrl Pts',(-43.1414579047527,-56.0146982180904,
-38.8937773555002));
#268355=CARTESIAN_POINT('Ctrl Pts',(-43.1785604553322,-55.9811311728431,
-38.8945214616358));
#268356=CARTESIAN_POINT('Ctrl Pts',(-43.191097126858,-55.9700714625021,
-38.894832307099));
#268357=CARTESIAN_POINT('Ctrl Pts',(-43.2164877853448,-55.9482328356115,
-38.8955798454342));
#268358=CARTESIAN_POINT('Ctrl Pts',(-43.2293517743068,-55.9374468641231,
-38.8960171583666));
#268359=CARTESIAN_POINT('Ctrl Pts',(-43.2682103054482,-55.9056892935197,
-38.8975114527738));
#268360=CARTESIAN_POINT('Ctrl Pts',(-43.2945313976451,-55.8852599252372,
-38.89875118762));
#268361=CARTESIAN_POINT('Ctrl Pts',(-43.3479995130708,-55.8458475490097,
-38.9017082880385));
#268362=CARTESIAN_POINT('Ctrl Pts',(-43.3751443920601,-55.8268657082684,
-38.9034254474569));
#268363=CARTESIAN_POINT('Ctrl Pts',(-43.4577939430348,-55.7720622018028,
-38.9092818131617));
#268364=CARTESIAN_POINT('Ctrl Pts',(-43.51451093327,-55.7383779822391,-38.9141244615973));
#268365=CARTESIAN_POINT('Ctrl Pts',(-43.601998052992,-55.6921031576597,
-38.9227836015924));
#268366=CARTESIAN_POINT('Ctrl Pts',(-43.631563048157,-55.6773880028564,
-38.9259028928878));
#268367=CARTESIAN_POINT('Ctrl Pts',(-43.6915050002909,-55.6493890121587,
-38.9326103047848));
#268368=CARTESIAN_POINT('Ctrl Pts',(-43.7218906736911,-55.6361026235129,
-38.9361997181443));
#268369=CARTESIAN_POINT('Ctrl Pts',(-43.783451665776,-55.6109933882688,
-38.9438484613551));
#268370=CARTESIAN_POINT('Ctrl Pts',(-43.8147378173409,-55.5991372642861,
-38.9479240409953));
#268371=CARTESIAN_POINT('Ctrl Pts',(-43.877363149692,-55.5771759127617,
-38.9564497975263));
#268372=CARTESIAN_POINT('Ctrl Pts',(-43.9088372843841,-55.5670115927043,
-38.9609158992096));
#268373=CARTESIAN_POINT('Ctrl Pts',(-43.9720261650696,-55.5483124604321,
-38.9702355633813));
#268374=CARTESIAN_POINT('Ctrl Pts',(-44.0037536572564,-55.5397721100658,
-38.9750906394313));
#268375=CARTESIAN_POINT('Ctrl Pts',(-44.0674709555852,-55.5242859080953,
-38.9851843621813));
#268376=CARTESIAN_POINT('Ctrl Pts',(-44.0994607677182,-55.5173400934252,
-38.9904230184279));
#268377=CARTESIAN_POINT('Ctrl Pts',(-44.1637009035284,-55.5050310901567,
-39.0012798595209));
#268378=CARTESIAN_POINT('Ctrl Pts',(-44.1959512291589,-55.4996679139965,
-39.0068980480835));
#268379=CARTESIAN_POINT('Ctrl Pts',(-44.2607124863074,-55.4905238141391,
-39.0185126384903));
#268380=CARTESIAN_POINT('Ctrl Pts',(-44.2932234159127,-55.4867428794561,
-39.0245090385139));
#268381=CARTESIAN_POINT('Ctrl Pts',(-44.3585078720818,-55.480774377281,
-39.0368814469747));
#268382=CARTESIAN_POINT('Ctrl Pts',(-44.3912831881742,-55.4785875325166,
-39.0432579749157));
#268383=CARTESIAN_POINT('Ctrl Pts',(-44.4570931925988,-55.4758271902798,
-39.0563927192769));
#268384=CARTESIAN_POINT('Ctrl Pts',(-44.4901880875464,-55.47526095961,-39.0631649349955));
#268385=CARTESIAN_POINT('Ctrl Pts',(-44.5558456650652,-55.4757574670419,
-39.0769281656387));
#268386=CARTESIAN_POINT('Ctrl Pts',(-44.5885619871977,-55.4768115298703,
-39.0839493922098));
#268387=CARTESIAN_POINT('Ctrl Pts',(-44.6536818041136,-55.4805022216823,
-39.0982456231909));
#268388=CARTESIAN_POINT('Ctrl Pts',(-44.6861009801573,-55.4831381046999,
-39.1055237410398));
#268389=CARTESIAN_POINT('Ctrl Pts',(-44.782942584543,-55.4933839391136,
-39.1277408090834));
#268390=CARTESIAN_POINT('Ctrl Pts',(-44.8469499487504,-55.5033272531759,
-39.1430616741657));
#268391=CARTESIAN_POINT('Ctrl Pts',(-44.9421369398694,-55.5228816395291,
-39.1667955749684));
#268392=CARTESIAN_POINT('Ctrl Pts',(-44.9737283661904,-55.5301742790311,
-39.1748325254908));
#268393=CARTESIAN_POINT('Ctrl Pts',(-45.0366341467681,-55.5463205175099,
-39.1911586082389));
#268394=CARTESIAN_POINT('Ctrl Pts',(-45.0679426151012,-55.5551727387585,
-39.1994462396222));
#268395=CARTESIAN_POINT('Ctrl Pts',(-45.1303021643981,-55.5744664003474,
-39.2162823673423));
#268396=CARTESIAN_POINT('Ctrl Pts',(-45.1613402206007,-55.5849108492065,
-39.2248287367212));
#268397=CARTESIAN_POINT('Ctrl Pts',(-45.2225452749523,-55.6071872308721,
-39.242013351558));
#268398=CARTESIAN_POINT('Ctrl Pts',(-45.2528237308145,-55.6190526565937,
-39.250681493177));
#268399=CARTESIAN_POINT('Ctrl Pts',(-45.312670500747,-55.6442008855743,
-39.2681483178686));
#268400=CARTESIAN_POINT('Ctrl Pts',(-45.342250447157,-55.6574872408305,
-39.276950132892));
#268401=CARTESIAN_POINT('Ctrl Pts',(-45.4007263164517,-55.6854788533848,
-39.2946893121999));
#268402=CARTESIAN_POINT('Ctrl Pts',(-45.429622238573,-55.700184112031,-39.303626677106));
#268403=CARTESIAN_POINT('Ctrl Pts',(-45.4581751231196,-55.7156010961856,
-39.3126317220034));
#268404=CARTESIAN_POINT('Ctrl Pts',(-44.2366247954661,-55.49394262042,-39.0141963249616));
#268405=CARTESIAN_POINT('Ctrl Pts',(-44.2662621726756,-55.4898840014969,
-39.0195373795186));
#268406=CARTESIAN_POINT('Ctrl Pts',(-44.3285305334225,-55.4827749995086,
-39.031049367808));
#268407=CARTESIAN_POINT('Ctrl Pts',(-44.3912831881742,-55.4785875325166,
-39.0432579749157));
#268408=CARTESIAN_POINT('Ctrl Pts',(-44.4570931925989,-55.4758271902798,
-39.0563927192769));
#268409=CARTESIAN_POINT('Ctrl Pts',(-44.4901880875464,-55.47526095961,-39.0631649349955));
#268410=CARTESIAN_POINT('Ctrl Pts',(-44.5558456650653,-55.4757574670419,
-39.0769281656387));
#268411=CARTESIAN_POINT('Ctrl Pts',(-44.5885619871977,-55.4768115298702,
-39.0839493922098));
#268412=CARTESIAN_POINT('Ctrl Pts',(-44.6536818041136,-55.4805022216824,
-39.0982456231909));
#268413=CARTESIAN_POINT('Ctrl Pts',(-44.750939117342,-55.4884110764087,
-39.1200801766399));
#268414=CARTESIAN_POINT('Ctrl Pts',(-44.8789538232237,-55.5082978363117,
-39.1507219236323));
#268415=CARTESIAN_POINT('Ctrl Pts',(-45.0053227794738,-55.5374673614327,
-39.1828701848163));
#268416=CARTESIAN_POINT('Ctrl Pts',(-45.0679426151012,-55.5551727387585,
-39.1994462396222));
#268417=CARTESIAN_POINT('Ctrl Pts',(-45.1303021643981,-55.5744664003474,
-39.2162823673423));
#268418=CARTESIAN_POINT('Ctrl Pts',(-45.1613402206007,-55.5849108492065,
-39.2248287367212));
#268419=CARTESIAN_POINT('Ctrl Pts',(-45.2225452749523,-55.6071872308721,
-39.2420133515579));
#268420=CARTESIAN_POINT('Ctrl Pts',(-45.2528237308145,-55.6190526565937,
-39.250681493177));
#268421=CARTESIAN_POINT('Ctrl Pts',(-45.3425938857133,-55.6567750000645,
-39.2768817302143));
#268422=CARTESIAN_POINT('Ctrl Pts',(-45.4010693540256,-55.684767127876,
-39.2946216322085));
#268423=CARTESIAN_POINT('Ctrl Pts',(-45.4581751231188,-55.7156010961851,
-39.3126317220031));
#268424=CARTESIAN_POINT('Ctrl Pts',(-43.5555682511181,-59.2341350312479,
-39.6401231904583));
#268425=CARTESIAN_POINT('Ctrl Pts',(-43.4986421803732,-59.2033077085535,
-39.6225222082463));
#268426=CARTESIAN_POINT('Ctrl Pts',(-43.3884827487122,-59.1365211050906,
-39.5869729940158));
#268427=CARTESIAN_POINT('Ctrl Pts',(-43.2340749587687,-59.0212983889997,
-39.5326183362566));
#268428=CARTESIAN_POINT('Ctrl Pts',(-43.1383845581245,-58.9343961646677,
-39.4956812053746));
#268429=CARTESIAN_POINT('Ctrl Pts',(-43.0464604338337,-58.8423006638519,
-39.4583884747486));
#268430=CARTESIAN_POINT('Ctrl Pts',(-42.9597638623997,-58.7464790949597,
-39.4213336309308));
#268431=CARTESIAN_POINT('Ctrl Pts',(-42.8639918437047,-58.6176479605167,
-39.3755734228827));
#268432=CARTESIAN_POINT('Ctrl Pts',(-42.7949093409291,-58.5091805688265,
-39.33930500608));
#268433=CARTESIAN_POINT('Ctrl Pts',(-42.7468976399245,-58.4250976736591,
-39.3122747709031));
#268434=CARTESIAN_POINT('Ctrl Pts',(-42.7174688743488,-58.3672104781721,
-39.2943764905707));
#268435=CARTESIAN_POINT('Ctrl Pts',(-42.6893426693184,-58.308352422918,
-39.2765308704476));
#268436=CARTESIAN_POINT('Ctrl Pts',(-42.676040350531,-58.2786648895678,
-39.2677034056768));
#268437=CARTESIAN_POINT('Ctrl Pts',(-42.6394421976857,-58.1913717942018,
-39.242242522637));
#268438=CARTESIAN_POINT('Ctrl Pts',(-42.6181634379433,-58.1331272500595,
-39.225872582076));
#268439=CARTESIAN_POINT('Ctrl Pts',(-42.5996267543263,-58.074028296276,
-39.2098669458287));
#268440=CARTESIAN_POINT('Ctrl Pts',(-43.4805771074156,-59.5712767529309,
-39.2399080357013));
#268441=CARTESIAN_POINT('Ctrl Pts',(-43.4150727209207,-59.5358440364426,
-39.2223070534893));
#268442=CARTESIAN_POINT('Ctrl Pts',(-43.2883193276586,-59.4590682572254,
-39.1867578392588));
#268443=CARTESIAN_POINT('Ctrl Pts',(-43.1106712693135,-59.32658002426,-39.1324031814995));
#268444=CARTESIAN_POINT('Ctrl Pts',(-43.0005921597408,-59.2266373021163,
-39.0954660506179));
#268445=CARTESIAN_POINT('Ctrl Pts',(-42.8948534568781,-59.1207134074407,
-39.0581733199915));
#268446=CARTESIAN_POINT('Ctrl Pts',(-42.7951360401793,-59.0104958554849,
-39.0211184761739));
#268447=CARTESIAN_POINT('Ctrl Pts',(-42.6850011896347,-58.8622904152127,
-38.9753582681256));
#268448=CARTESIAN_POINT('Ctrl Pts',(-42.6055727997797,-58.7375004045667,
-38.939089851323));
#268449=CARTESIAN_POINT('Ctrl Pts',(-42.5503788594446,-58.6407591922129,
-38.9120596161462));
#268450=CARTESIAN_POINT('Ctrl Pts',(-42.5165536369311,-58.5741539171446,
-38.8941613358138));
#268451=CARTESIAN_POINT('Ctrl Pts',(-42.4842288567228,-58.5064298632496,
-38.8763157156907));
#268452=CARTESIAN_POINT('Ctrl Pts',(-42.4689425396028,-58.4722695523732,
-38.8674882509199));
#268453=CARTESIAN_POINT('Ctrl Pts',(-42.4257123024776,-58.3690064948315,
-38.8413136266604));
#268454=CARTESIAN_POINT('Ctrl Pts',(-42.3750272156063,-58.229152189777,
-38.8072100415055));
#268455=CARTESIAN_POINT('Ctrl Pts',(-42.3380647902547,-58.0850119200902,
-38.7746901633276));
#268456=CARTESIAN_POINT('Ctrl Pts',(-42.3155659796374,-57.9752818499468,
-38.7509105250088));
#268457=CARTESIAN_POINT('Ctrl Pts',(-42.3089374211558,-57.9384266221928,
-38.7430843922672));
#268458=CARTESIAN_POINT('Ctrl Pts',(-42.297458012674,-57.864178756387,-38.7276438637217));
#268459=CARTESIAN_POINT('Ctrl Pts',(-42.292601515188,-57.8267325312259,
-38.720018782004));
#268460=CARTESIAN_POINT('Ctrl Pts',(-42.2847289916893,-57.7514526301959,
-38.7050196673963));
#268461=CARTESIAN_POINT('Ctrl Pts',(-42.2817363521424,-57.7138759968928,
-38.6976962453237));
#268462=CARTESIAN_POINT('Ctrl Pts',(-42.277596992864,-57.6387184974263,
-38.6833720377019));
#268463=CARTESIAN_POINT('Ctrl Pts',(-42.2741651307842,-57.5260409596698,
-38.6623829091612));
#268464=CARTESIAN_POINT('Ctrl Pts',(-42.2805893100654,-57.3760354719141,
-38.6363740800325));
#268465=CARTESIAN_POINT('Ctrl Pts',(-42.2937061680812,-57.2637038035873,
-38.618370061439));
#268466=CARTESIAN_POINT('Ctrl Pts',(-42.3043247017591,-57.1888547452426,
-38.6067079534822));
#268467=CARTESIAN_POINT('Ctrl Pts',(-42.3105743117123,-57.1514345461221,
-38.6010450635964));
#268468=CARTESIAN_POINT('Ctrl Pts',(-42.3249704170347,-57.0766935209607,
-38.590076215021));
#268469=CARTESIAN_POINT('Ctrl Pts',(-42.3331592025312,-57.0392159768686,
-38.5847494243559));
#268470=CARTESIAN_POINT('Ctrl Pts',(-42.3512949844302,-56.9651221381903,
-38.5745673038812));
#268471=CARTESIAN_POINT('Ctrl Pts',(-42.3712216906218,-56.8916587034686,
-38.564820665347));
#268472=CARTESIAN_POINT('Ctrl Pts',(-42.4063979707918,-56.7834465224234,
-38.5515118436));
#268473=CARTESIAN_POINT('Ctrl Pts',(-42.4468320479729,-56.6771725078319,
-38.5395042677724));
#268474=CARTESIAN_POINT('Ctrl Pts',(-42.4925290654744,-56.5728473165674,
-38.5288039137004));
#268475=CARTESIAN_POINT('Ctrl Pts',(-42.5265325119253,-56.5046058456765,
-38.5225509073062));
#268476=CARTESIAN_POINT('Ctrl Pts',(-42.5623338475306,-56.4370293947697,
-38.5167461666044));
#268477=CARTESIAN_POINT('Ctrl Pts',(-42.5811223641794,-56.4035923099625,
-38.5140693065785));
#268478=CARTESIAN_POINT('Ctrl Pts',(-42.620584523009,-56.3373241998654,
-38.5091697400817));
#268479=CARTESIAN_POINT('Ctrl Pts',(-42.6411082254821,-56.3047465904101,
-38.5069659500128));
#268480=CARTESIAN_POINT('Ctrl Pts',(-42.7048067991197,-56.2090283357163,
-38.501110858935));
#268481=CARTESIAN_POINT('Ctrl Pts',(-42.7502234543428,-56.1476408662828,
-38.4981890389281));
#268482=CARTESIAN_POINT('Ctrl Pts',(-42.8467942323831,-56.0297655581676,
-38.4942910511033));
#268483=CARTESIAN_POINT('Ctrl Pts',(-42.8979715413934,-55.9732420482176,
-38.4933125989996));
#268484=CARTESIAN_POINT('Ctrl Pts',(-42.9790570553347,-55.8921695883033,
-38.4933149859729));
#268485=CARTESIAN_POINT('Ctrl Pts',(-43.0068374106561,-55.8657400908868,
-38.4935622007431));
#268486=CARTESIAN_POINT('Ctrl Pts',(-43.0495800649421,-55.8270637749536,
-38.4943063068789));
#268487=CARTESIAN_POINT('Ctrl Pts',(-43.0640222060113,-55.8143203511958,
-38.494617152342));
#268488=CARTESIAN_POINT('Ctrl Pts',(-43.0932714774893,-55.7891564261061,
-38.4953646906773));
#268489=CARTESIAN_POINT('Ctrl Pts',(-43.1080901283632,-55.7767277938553,
-38.4958020036096));
#268490=CARTESIAN_POINT('Ctrl Pts',(-43.1528523310046,-55.7401327167866,
-38.4972962980169));
#268491=CARTESIAN_POINT('Ctrl Pts',(-43.2134913856688,-55.6930468850421,
-38.4997758707861));
#268492=CARTESIAN_POINT('Ctrl Pts',(-43.3385569247743,-55.6055389451161,
-38.5066450244003));
#268493=CARTESIAN_POINT('Ctrl Pts',(-43.4691986576013,-55.5278792007279,
-38.5163302992824));
#268494=CARTESIAN_POINT('Ctrl Pts',(-43.5713395927684,-55.4769743237494,
-38.5256877381308));
#268495=CARTESIAN_POINT('Ctrl Pts',(-43.6403672861995,-55.4446857735354,
-38.5323951500278));
#268496=CARTESIAN_POINT('Ctrl Pts',(-43.6753577685123,-55.4293620157832,
-38.5359845633874));
#268497=CARTESIAN_POINT('Ctrl Pts',(-43.7462462065788,-55.4003985583156,
-38.5436333065981));
#268498=CARTESIAN_POINT('Ctrl Pts',(-43.7822717759725,-55.3867204456352,
-38.5477088862383));
#268499=CARTESIAN_POINT('Ctrl Pts',(-43.8543821738219,-55.3613797848081,
-38.5562346427694));
#268500=CARTESIAN_POINT('Ctrl Pts',(-43.890622407919,-55.349649082917,-38.5607007444526));
#268501=CARTESIAN_POINT('Ctrl Pts',(-43.9997560709039,-55.3172704656441,
-38.5746802407103));
#268502=CARTESIAN_POINT('Ctrl Pts',(-44.1098017310836,-55.290468361793,
-38.5898286859852));
#268503=CARTESIAN_POINT('Ctrl Pts',(-44.2583166685835,-55.2656490138239,
-38.612301023075));
#268504=CARTESIAN_POINT('Ctrl Pts',(-44.3705972700495,-55.2524997368729,
-38.6302900391873));
#268505=CARTESIAN_POINT('Ctrl Pts',(-44.446056048267,-55.2474029004138,
-38.6430428201589));
#268506=CARTESIAN_POINT('Ctrl Pts',(-44.5218128020516,-55.2441636366351,
-38.65617756452));
#268507=CARTESIAN_POINT('Ctrl Pts',(-44.5599089424743,-55.2434808562086,
-38.6629497802385));
#268508=CARTESIAN_POINT('Ctrl Pts',(-44.6354869543582,-55.2439911084578,
-38.6767130108817));
#268509=CARTESIAN_POINT('Ctrl Pts',(-44.6731456892459,-55.2451740103824,
-38.6837342374529));
#268510=CARTESIAN_POINT('Ctrl Pts',(-44.7481014788608,-55.2493620066237,
-38.6980304684339));
#268511=CARTESIAN_POINT('Ctrl Pts',(-44.860046548974,-55.2583760573225,
-38.7198650218829));
#268512=CARTESIAN_POINT('Ctrl Pts',(-45.0073845433675,-55.2811507310277,
-38.7505067688753));
#268513=CARTESIAN_POINT('Ctrl Pts',(-45.1528189888476,-55.3146135839333,
-38.7826550300594));
#268514=CARTESIAN_POINT('Ctrl Pts',(-45.2248832056965,-55.3349380951144,
-38.7992310848652));
#268515=CARTESIAN_POINT('Ctrl Pts',(-45.2966462681613,-55.3570913336823,
-38.8160672125853));
#268516=CARTESIAN_POINT('Ctrl Pts',(-45.3323638946335,-55.3690863290504,
-38.8246135819642));
#268517=CARTESIAN_POINT('Ctrl Pts',(-45.4027951436545,-55.3946744461232,
-38.841798196801));
#268518=CARTESIAN_POINT('Ctrl Pts',(-45.4376370321487,-55.4083060218429,
-38.85046633842));
#268519=CARTESIAN_POINT('Ctrl Pts',(-45.5409345111852,-55.4516493275196,
-38.8766665754573));
#268520=CARTESIAN_POINT('Ctrl Pts',(-45.6082182891413,-55.4838201174091,
-38.8944064774514));
#268521=CARTESIAN_POINT('Ctrl Pts',(-45.7067749877369,-55.5369855856676,
-38.9214216121435));
#268522=CARTESIAN_POINT('Ctrl Pts',(-45.7392219877795,-55.5555212114618,
-38.9304915704334));
#268523=CARTESIAN_POINT('Ctrl Pts',(-45.8033556832395,-55.5942722159849,
-38.9487787872477));
#268524=CARTESIAN_POINT('Ctrl Pts',(-45.8348443691401,-55.6143675312756,
-38.9579395118015));
#268525=CARTESIAN_POINT('Ctrl Pts',(-45.9274099842789,-55.6766589025306,
-38.9854159162723));
#268526=CARTESIAN_POINT('Ctrl Pts',(-45.9867610865919,-55.7209353156014,
-39.0037703637879));
#268527=CARTESIAN_POINT('Ctrl Pts',(-46.1007337830098,-55.8148102393793,
-39.0405190865864));
#268528=CARTESIAN_POINT('Ctrl Pts',(-46.1826971388658,-55.889219933262,
-39.0681181728269));
#268529=CARTESIAN_POINT('Ctrl Pts',(-46.259356574729,-55.9696687352924,
-39.0957737179551));
#268530=CARTESIAN_POINT('Ctrl Pts',(-46.309266807939,-56.024663053365,-39.1142236413887));
#268531=CARTESIAN_POINT('Ctrl Pts',(-46.3336138177017,-56.0528284109483,
-39.1234510495426));
#268532=CARTESIAN_POINT('Ctrl Pts',(-46.3692509284248,-56.0961546965833,
-39.1373141736981));
#268533=CARTESIAN_POINT('Ctrl Pts',(-46.3809719555493,-56.1107655250657,
-39.14193505412));
#268534=CARTESIAN_POINT('Ctrl Pts',(-46.4039850968433,-56.1401806715041,
-39.1511314768264));
#268535=CARTESIAN_POINT('Ctrl Pts',(-46.4153001903629,-56.1550126624776,
-39.1557159133813));
#268536=CARTESIAN_POINT('Ctrl Pts',(-46.4486370096885,-56.1998310060263,
-39.1694131182659));
#268537=CARTESIAN_POINT('Ctrl Pts',(-46.4700835091466,-56.2301795317326,
-39.1784826054425));
#268538=CARTESIAN_POINT('Ctrl Pts',(-46.532071913686,-56.3225583984772,
-39.2054898733524));
#268539=CARTESIAN_POINT('Ctrl Pts',(-46.5894197348374,-56.4176636744323,
-39.23211607576));
#268540=CARTESIAN_POINT('Ctrl Pts',(-46.6566074362748,-56.5498680842415,
-39.2668544229849));
#268541=CARTESIAN_POINT('Ctrl Pts',(-46.6870820302515,-56.617790568625,
-39.2839693714534));
#268542=CARTESIAN_POINT('Ctrl Pts',(-46.7159729830272,-56.6866360545619,
-39.3009558869148));
#268543=CARTESIAN_POINT('Ctrl Pts',(-46.7296188023799,-56.7214992889704,
-39.3093799218186));
#268544=CARTESIAN_POINT('Ctrl Pts',(-46.7553216997643,-56.7922546384013,
-39.3261176641085));
#268545=CARTESIAN_POINT('Ctrl Pts',(-46.7672996943011,-56.8279354881579,
-39.3343809787628));
#268546=CARTESIAN_POINT('Ctrl Pts',(-46.8004530502947,-56.9353633959568,
-39.358737163018));
#268547=CARTESIAN_POINT('Ctrl Pts',(-46.8189795501832,-57.0077635587999,
-39.3744658121213));
#268548=CARTESIAN_POINT('Ctrl Pts',(-46.848916211803,-57.1540080946302,
-39.4048998290393));
#268549=CARTESIAN_POINT('Ctrl Pts',(-46.866048617508,-57.2647966217996,
-39.4269646939479));
#268550=CARTESIAN_POINT('Ctrl Pts',(-46.875074749658,-57.3772756893033,
-39.4478819384746));
#268551=CARTESIAN_POINT('Ctrl Pts',(-46.8792542953452,-57.4526370309597,
-39.4615663943076));
#268552=CARTESIAN_POINT('Ctrl Pts',(-46.8804258736835,-57.4905390832845,
-39.4682843608713));
#268553=CARTESIAN_POINT('Ctrl Pts',(-46.8808837743635,-57.566610437341,
-39.4814341960201));
#268554=CARTESIAN_POINT('Ctrl Pts',(-46.8801708637706,-57.604491394965,
-39.4878166677226));
#268555=CARTESIAN_POINT('Ctrl Pts',(-46.8768913879562,-57.6800597985945,
-39.5002231148134));
#268556=CARTESIAN_POINT('Ctrl Pts',(-46.8691896925243,-57.7930657109158,
-39.5182849936093));
#268557=CARTESIAN_POINT('Ctrl Pts',(-46.8479069711518,-57.9423669591112,
-39.540205996752));
#268558=CARTESIAN_POINT('Ctrl Pts',(-46.8236459543104,-58.053306681129,
-39.5550278422771));
#268559=CARTESIAN_POINT('Ctrl Pts',(-46.8055990109883,-58.1270324939452,
-39.5645447403379));
#268560=CARTESIAN_POINT('Ctrl Pts',(-46.7956339676918,-58.1637938532181,
-39.5691227921436));
#268561=CARTESIAN_POINT('Ctrl Pts',(-46.7738161327052,-58.2370162077019,
-39.5779016468881));
#268562=CARTESIAN_POINT('Ctrl Pts',(-46.7619036278491,-58.2736352268715,
-39.5821192203466));
#268563=CARTESIAN_POINT('Ctrl Pts',(-46.7364059718256,-58.3458255995332,
-39.5900871854462));
#268564=CARTESIAN_POINT('Ctrl Pts',(-46.7091836493705,-58.4171862986019,
-39.5976163356366));
#268565=CARTESIAN_POINT('Ctrl Pts',(-46.663274408039,-58.5216699086648,
-39.6076014242402));
#268566=CARTESIAN_POINT('Ctrl Pts',(-46.6123207377325,-58.6236436013082,
-39.616293729045));
#268567=CARTESIAN_POINT('Ctrl Pts',(-46.5563244858032,-58.7230996041114,
-39.6236943138341));
#268568=CARTESIAN_POINT('Ctrl Pts',(-46.515607032986,-58.7877140896312,
-39.6277619492082));
#268569=CARTESIAN_POINT('Ctrl Pts',(-46.4731710833873,-58.8514710047945,
-39.6313905635194));
#268570=CARTESIAN_POINT('Ctrl Pts',(-46.4511086137465,-58.8829006319494,
-39.6329844599904));
#268571=CARTESIAN_POINT('Ctrl Pts',(-46.4051673201274,-58.9449633016888,
-39.6357273485653));
#268572=CARTESIAN_POINT('Ctrl Pts',(-46.381447994276,-58.975377588932,-39.6368662598532));
#268573=CARTESIAN_POINT('Ctrl Pts',(-46.3084068909562,-59.0643493136614,
-39.6395761233691));
#268574=CARTESIAN_POINT('Ctrl Pts',(-46.2570407846102,-59.1209150453974,
-39.6404603784325));
#268575=CARTESIAN_POINT('Ctrl Pts',(-46.1491379755941,-59.228544463199,
-39.6404138814247));
#268576=CARTESIAN_POINT('Ctrl Pts',(-46.0925836555155,-59.2796343044913,
-39.6394845811684));
#268577=CARTESIAN_POINT('Ctrl Pts',(-46.0038529437629,-59.3521266125547,
-39.6367223387528));
#268578=CARTESIAN_POINT('Ctrl Pts',(-45.9736068078661,-59.3756113554055,
-39.6355721163029));
#268579=CARTESIAN_POINT('Ctrl Pts',(-45.9272656961273,-59.4097723546528,
-39.6334997725088));
#268580=CARTESIAN_POINT('Ctrl Pts',(-45.9116419215573,-59.4209912820171,
-39.6327502808957));
#268581=CARTESIAN_POINT('Ctrl Pts',(-45.8800804794677,-59.4430610802669,
-39.6311351339295));
#268582=CARTESIAN_POINT('Ctrl Pts',(-45.8321587971618,-59.4756823489919,
-39.628531354857));
#268583=CARTESIAN_POINT('Ctrl Pts',(-45.7834097108732,-59.5062438963941,
-39.6254355071979));
#268584=CARTESIAN_POINT('Ctrl Pts',(-45.717633106262,-59.5452481912826,
-39.6208773262667));
#268585=CARTESIAN_POINT('Ctrl Pts',(-45.6178307490054,-59.601113548897,
-39.6133952897297));
#268586=CARTESIAN_POINT('Ctrl Pts',(-45.4802897643185,-59.6652183443042,
-39.6008811885904));
#268587=CARTESIAN_POINT('Ctrl Pts',(-45.3738098009101,-59.7055766782111,
-39.5896017905935));
#268588=CARTESIAN_POINT('Ctrl Pts',(-45.3020778813705,-59.7307512119865,
-39.5816566825671));
#268589=CARTESIAN_POINT('Ctrl Pts',(-45.2658207311094,-59.7424779859237,
-39.5774690651077));
#268590=CARTESIAN_POINT('Ctrl Pts',(-45.1926264675053,-59.7641596016776,
-39.5686715125846));
#268591=CARTESIAN_POINT('Ctrl Pts',(-45.1555073907618,-59.7741562512684,
-39.5640376159893));
#268592=CARTESIAN_POINT('Ctrl Pts',(-45.0441315765335,-59.8011904590316,
-39.5496210468413));
#268593=CARTESIAN_POINT('Ctrl Pts',(-44.9324484012679,-59.8224577850013,
-39.5341534065747));
#268594=CARTESIAN_POINT('Ctrl Pts',(-44.8203079610257,-59.8353953605365,
-39.5171556909205));
#268595=CARTESIAN_POINT('Ctrl Pts',(-44.7080184564226,-59.8455760612675,
-39.4996502778008));
#268596=CARTESIAN_POINT('Ctrl Pts',(-44.6329372249224,-59.8486931621852,
-39.4873001861445));
#268597=CARTESIAN_POINT('Ctrl Pts',(-44.5200834441659,-59.8478515133141,
-39.4677634802869));
#268598=CARTESIAN_POINT('Ctrl Pts',(-44.4823810871712,-59.8466449718289,
-39.4610736497974));
#268599=CARTESIAN_POINT('Ctrl Pts',(-44.4258051079382,-59.8434394706745,
-39.4507883432074));
#268600=CARTESIAN_POINT('Ctrl Pts',(-44.4069254589855,-59.8421361346926,
-39.4473147915973));
#268601=CARTESIAN_POINT('Ctrl Pts',(-44.3691376542581,-59.8390581625153,
-39.4402793331445));
#268602=CARTESIAN_POINT('Ctrl Pts',(-44.3502459350849,-59.8372838734483,
-39.4367203104461));
#268603=CARTESIAN_POINT('Ctrl Pts',(-44.2562487381671,-59.8272835659938,
-39.4188041728073));
#268604=CARTESIAN_POINT('Ctrl Pts',(-44.1080045765469,-59.8040393501646,
-39.3892226636159));
#268605=CARTESIAN_POINT('Ctrl Pts',(-43.9639303529155,-59.7668593120831,
-39.3578670379715));
#268606=CARTESIAN_POINT('Ctrl Pts',(-43.8219159040518,-59.7227861654643,
-39.3256251231267));
#268607=CARTESIAN_POINT('Ctrl Pts',(-43.7519290534068,-59.6972943066161,
-39.3090578287531));
#268608=CARTESIAN_POINT('Ctrl Pts',(-43.665783177736,-59.6610675807531,
-39.2877890488175));
#268609=CARTESIAN_POINT('Ctrl Pts',(-43.6486106666635,-59.653596197985,
-39.2835041280971));
#268610=CARTESIAN_POINT('Ctrl Pts',(-43.6144193015916,-59.6382222359849,
-39.2748825183767));
#268611=CARTESIAN_POINT('Ctrl Pts',(-43.597366582891,-59.6303022352814,
-39.2705368924251));
#268612=CARTESIAN_POINT('Ctrl Pts',(-43.5465994182959,-59.605961903298,
-39.2574616452183));
#268613=CARTESIAN_POINT('Ctrl Pts',(-43.513329300663,-59.588993111175,-39.2487085268073));
#268614=CARTESIAN_POINT('Ctrl Pts',(-43.4805771074156,-59.5712767529309,
-39.2399080357013));
#268615=CARTESIAN_POINT('Ctrl Pts',(-43.8341420587998,-57.9817357678076,
-41.1268248734572));
#268616=CARTESIAN_POINT('Ctrl Pts',(-43.8090823387197,-57.9680163597508,
-41.1092238912453));
#268617=CARTESIAN_POINT('Ctrl Pts',(-43.7605654269547,-57.9383371077444,
-41.0736746770147));
#268618=CARTESIAN_POINT('Ctrl Pts',(-43.6924895655639,-57.8872515755908,
-41.019320019256));
#268619=CARTESIAN_POINT('Ctrl Pts',(-43.6502497090231,-57.8487916199066,
-40.9823828883729));
#268620=CARTESIAN_POINT('Ctrl Pts',(-43.6096433745973,-57.8080652293815,
-40.945090157748));
#268621=CARTESIAN_POINT('Ctrl Pts',(-43.5713160673933,-57.7657212262301,
-40.9080353139296));
#268622=CARTESIAN_POINT('Ctrl Pts',(-43.5288984657655,-57.7088609123343,
-40.8622751058818));
#268623=CARTESIAN_POINT('Ctrl Pts',(-43.4982484100127,-57.6610280687967,
-40.826006689079));
#268624=CARTESIAN_POINT('Ctrl Pts',(-43.4769169762936,-57.6239677344727,
-40.798976453902));
#268625=CARTESIAN_POINT('Ctrl Pts',(-43.4638199758968,-57.5984660781933,
-40.7810781735695));
#268626=CARTESIAN_POINT('Ctrl Pts',(-43.4512904535732,-57.5725430453748,
-40.7632325534464));
#268627=CARTESIAN_POINT('Ctrl Pts',(-43.4453582046716,-57.5594707895743,
-40.7544050886758));
#268628=CARTESIAN_POINT('Ctrl Pts',(-43.4285595200757,-57.5199648485381,
-40.7282304644163));
#268629=CARTESIAN_POINT('Ctrl Pts',(-43.4088016745783,-57.4664867157472,
-40.6941268792613));
#268630=CARTESIAN_POINT('Ctrl Pts',(-43.3942530508608,-57.4114223976644,
-40.6616070010832));
#268631=CARTESIAN_POINT('Ctrl Pts',(-43.3853242538269,-57.3695231591805,
-40.6378273627645));
#268632=CARTESIAN_POINT('Ctrl Pts',(-43.3826786150667,-57.3554536366825,
-40.630001230023));
#268633=CARTESIAN_POINT('Ctrl Pts',(-43.378062215599,-57.3271160344971,
-40.6145607014775));
#268634=CARTESIAN_POINT('Ctrl Pts',(-43.3760891270041,-57.3128275119467,
-40.60693561976));
#268635=CARTESIAN_POINT('Ctrl Pts',(-43.3728422231051,-57.2841093232557,
-40.5919365051523));
#268636=CARTESIAN_POINT('Ctrl Pts',(-43.3715781643254,-57.2697777029377,
-40.5846130830795));
#268637=CARTESIAN_POINT('Ctrl Pts',(-43.3697526802575,-57.2411194243864,
-40.5702888754578));
#268638=CARTESIAN_POINT('Ctrl Pts',(-43.3680717796799,-57.1981642741791,
-40.5492997469169));
#268639=CARTESIAN_POINT('Ctrl Pts',(-43.3700185838812,-57.1410182421193,
-40.5232909177883));
#268640=CARTESIAN_POINT('Ctrl Pts',(-43.3746384661022,-57.0982543712987,
-40.505286899195));
#268641=CARTESIAN_POINT('Ctrl Pts',(-43.3784319419536,-57.0697666559562,
-40.4936247912381));
#268642=CARTESIAN_POINT('Ctrl Pts',(-43.3806866868643,-57.0555278483981,
-40.4879619013523));
#268643=CARTESIAN_POINT('Ctrl Pts',(-43.3859186984709,-57.0270949764048,
-40.476993052777));
#268644=CARTESIAN_POINT('Ctrl Pts',(-43.3889115442249,-57.0128413374093,
-40.4716662621118));
#268645=CARTESIAN_POINT('Ctrl Pts',(-43.3955695423488,-56.984668670318,
-40.4614841416371));
#268646=CARTESIAN_POINT('Ctrl Pts',(-43.4029115329907,-56.9567427536229,
-40.4517375031029));
#268647=CARTESIAN_POINT('Ctrl Pts',(-43.4159439893498,-56.915628788467,
-40.4384286813559));
#268648=CARTESIAN_POINT('Ctrl Pts',(-43.4309850942545,-56.8752725380991,
-40.4264211055283));
#268649=CARTESIAN_POINT('Ctrl Pts',(-43.4480370013178,-56.8356780486645,
-40.4157207514563));
#268650=CARTESIAN_POINT('Ctrl Pts',(-43.4607570961379,-56.8097932355363,
-40.409467745062));
#268651=CARTESIAN_POINT('Ctrl Pts',(-43.4741642201056,-56.7841683331057,
-40.4036630043601));
#268652=CARTESIAN_POINT('Ctrl Pts',(-43.4812071336048,-56.7714928975767,
-40.4009861443346));
#268653=CARTESIAN_POINT('Ctrl Pts',(-43.4960130774609,-56.7463797512019,
-40.3960865778375));
#268654=CARTESIAN_POINT('Ctrl Pts',(-43.5037198572985,-56.7340380787953,
-40.3938827877695));
#268655=CARTESIAN_POINT('Ctrl Pts',(-43.527657505214,-56.6977883833479,
-40.3880276966888));
#268656=CARTESIAN_POINT('Ctrl Pts',(-43.5447483375558,-56.6745564757614,
-40.3851058766842));
#268657=CARTESIAN_POINT('Ctrl Pts',(-43.5811328114983,-56.629979998045,
-40.3812078888591));
#268658=CARTESIAN_POINT('Ctrl Pts',(-43.6004351631962,-56.6086219171049,
-40.3802294367552));
#268659=CARTESIAN_POINT('Ctrl Pts',(-43.6310475296952,-56.578014570072,
-40.3802318237287));
#268660=CARTESIAN_POINT('Ctrl Pts',(-43.6415402048873,-56.5680413281089,
-40.3804790384992));
#268661=CARTESIAN_POINT('Ctrl Pts',(-43.6576911458811,-56.5534539772523,
-40.3812231446347));
#268662=CARTESIAN_POINT('Ctrl Pts',(-43.6631494628181,-56.5486488515781,
-40.3815339900979));
#268663=CARTESIAN_POINT('Ctrl Pts',(-43.6742063152013,-56.5391628964206,
-40.3822815284329));
#268664=CARTESIAN_POINT('Ctrl Pts',(-43.6798092119243,-56.534479009001,
-40.3827188413654));
#268665=CARTESIAN_POINT('Ctrl Pts',(-43.6967370434146,-56.5206915949946,
-40.3842131357726));
#268666=CARTESIAN_POINT('Ctrl Pts',(-43.7196778600618,-56.5029622466235,
-40.386692708542));
#268667=CARTESIAN_POINT('Ctrl Pts',(-43.7670264629127,-56.4700551612604,
-40.3935618621563));
#268668=CARTESIAN_POINT('Ctrl Pts',(-43.8165352419067,-56.4409186299576,
-40.4032471370382));
#268669=CARTESIAN_POINT('Ctrl Pts',(-43.8552784957563,-56.4218759376155,
-40.4126045758866));
#268670=CARTESIAN_POINT('Ctrl Pts',(-43.8814691350842,-56.4098116142502,
-40.4193119877837));
#268671=CARTESIAN_POINT('Ctrl Pts',(-43.8947490665381,-56.4040935548973,
-40.4229014011429));
#268672=CARTESIAN_POINT('Ctrl Pts',(-43.9216608718689,-56.3933018151258,
-40.430550144354));
#268673=CARTESIAN_POINT('Ctrl Pts',(-43.9353412421961,-56.3882139347518,
-40.434625723994));
#268674=CARTESIAN_POINT('Ctrl Pts',(-43.9627318697344,-56.3788058930362,
-40.4431514805252));
#268675=CARTESIAN_POINT('Ctrl Pts',(-43.9765011076412,-56.3744602994329,
-40.4476175822086));
#268676=CARTESIAN_POINT('Ctrl Pts',(-44.0179764085085,-56.3624961934912,
-40.4615970784657));
#268677=CARTESIAN_POINT('Ctrl Pts',(-44.0598195105868,-56.3526585058303,
-40.4767455237411));
#268678=CARTESIAN_POINT('Ctrl Pts',(-44.1163310625808,-56.3437038269143,
-40.4992178608308));
#268679=CARTESIAN_POINT('Ctrl Pts',(-44.1590753545772,-56.3390714325247,
-40.5172068769433));
#268680=CARTESIAN_POINT('Ctrl Pts',(-44.1878153726385,-56.337382052278,
-40.5299596579145));
#268681=CARTESIAN_POINT('Ctrl Pts',(-44.2166756293141,-56.3364007867548,
-40.5430944022758));
#268682=CARTESIAN_POINT('Ctrl Pts',(-44.2311921171808,-56.3362675100036,
-40.5498666179945));
#268683=CARTESIAN_POINT('Ctrl Pts',(-44.2599977007373,-56.3367129587916,
-40.5636298486377));
#268684=CARTESIAN_POINT('Ctrl Pts',(-44.2743541649932,-56.3372884158027,
-40.5706510752088));
#268685=CARTESIAN_POINT('Ctrl Pts',(-44.3029357424357,-56.3391317429585,
-40.5849473061899));
#268686=CARTESIAN_POINT('Ctrl Pts',(-44.3456316213443,-56.3429350642169,
-40.6067818596389));
#268687=CARTESIAN_POINT('Ctrl Pts',(-44.4018650235691,-56.3520939287388,
-40.6374236066311));
#268688=CARTESIAN_POINT('Ctrl Pts',(-44.4574103376146,-56.3653147883305,
-40.6695718678152));
#268689=CARTESIAN_POINT('Ctrl Pts',(-44.4849466005937,-56.3732907222196,
-40.686147922621));
#268690=CARTESIAN_POINT('Ctrl Pts',(-44.512374392093,-56.3819617528141,
-40.7029840503412));
#268691=CARTESIAN_POINT('Ctrl Pts',(-44.5260289861432,-56.3866462995878,
-40.7115304197201));
#268692=CARTESIAN_POINT('Ctrl Pts',(-44.5529609776699,-56.3966203919845,
-40.7287150345567));
#268693=CARTESIAN_POINT('Ctrl Pts',(-44.5662873943758,-56.4019250012471,
-40.737383176176));
#268694=CARTESIAN_POINT('Ctrl Pts',(-44.6058068395674,-56.4187668411382,
-40.7635834132132));
#268695=CARTESIAN_POINT('Ctrl Pts',(-44.6315615859976,-56.4312362585519,
-40.7813233152079));
#268696=CARTESIAN_POINT('Ctrl Pts',(-44.6693071486035,-56.4518014713652,
-40.8083384498991));
#268697=CARTESIAN_POINT('Ctrl Pts',(-44.6817372625133,-56.458965010373,
-40.8174084081892));
#268698=CARTESIAN_POINT('Ctrl Pts',(-44.7063132537473,-56.473929075182,
-40.8356956250034));
#268699=CARTESIAN_POINT('Ctrl Pts',(-44.7183832523531,-56.4816832398284,
-40.8448563495594));
#268700=CARTESIAN_POINT('Ctrl Pts',(-44.7538754102704,-56.505703003501,
-40.8723327540241));
#268701=CARTESIAN_POINT('Ctrl Pts',(-44.7766465418209,-56.5227549736834,
-40.8906872015444));
#268702=CARTESIAN_POINT('Ctrl Pts',(-44.8204030914552,-56.5588699415109,
-40.9274359243417));
#268703=CARTESIAN_POINT('Ctrl Pts',(-44.851893062885,-56.5874690797881,
-40.9550350105826));
#268704=CARTESIAN_POINT('Ctrl Pts',(-44.8813802932551,-56.6183507815631,
-40.982690555711));
#268705=CARTESIAN_POINT('Ctrl Pts',(-44.9005867815582,-56.6394533348067,
-41.0011404791447));
#268706=CARTESIAN_POINT('Ctrl Pts',(-44.9099603095753,-56.6502571213647,
-41.0103678872986));
#268707=CARTESIAN_POINT('Ctrl Pts',(-44.9236872082217,-56.6668706184025,
-41.0242310114538));
#268708=CARTESIAN_POINT('Ctrl Pts',(-44.9282031316495,-56.6724722064122,
-41.0288518918758));
#268709=CARTESIAN_POINT('Ctrl Pts',(-44.9370720489983,-56.6837477093971,
-41.038048314582));
#268710=CARTESIAN_POINT('Ctrl Pts',(-44.9414338933841,-56.6894322363092,
-41.0426327511372));
#268711=CARTESIAN_POINT('Ctrl Pts',(-44.9542884395491,-56.7066066663578,
-41.0563299560217));
#268712=CARTESIAN_POINT('Ctrl Pts',(-44.9625629539304,-56.7182326826763,
-41.0653994431984));
#268713=CARTESIAN_POINT('Ctrl Pts',(-44.9864941991718,-56.7536111473724,
-41.0924067111081));
#268714=CARTESIAN_POINT('Ctrl Pts',(-45.0086645271567,-56.7900134244028,
-41.1190329135161));
#268715=CARTESIAN_POINT('Ctrl Pts',(-45.034704630644,-56.8405768845403,
-41.1537712607408));
#268716=CARTESIAN_POINT('Ctrl Pts',(-45.0465408860903,-56.8665423758261,
-41.1708862092094));
#268717=CARTESIAN_POINT('Ctrl Pts',(-45.0577761134165,-56.8928546179869,
-41.1878727246706));
#268718=CARTESIAN_POINT('Ctrl Pts',(-45.0630901582258,-56.906176087846,
-41.1962967595746));
#268719=CARTESIAN_POINT('Ctrl Pts',(-45.0731156002939,-56.9332061371524,
-41.2130345018643));
#268720=CARTESIAN_POINT('Ctrl Pts',(-45.0777961712447,-56.9468340019015,
-41.2212978165198));
#268721=CARTESIAN_POINT('Ctrl Pts',(-45.0907786540592,-56.9878560258786,
-41.2456540007716));
#268722=CARTESIAN_POINT('Ctrl Pts',(-45.0980724298404,-57.0154910056487,
-41.2613826498774));
#268723=CARTESIAN_POINT('Ctrl Pts',(-45.1099506000897,-57.0712899900431,
-41.2918166667949));
#268724=CARTESIAN_POINT('Ctrl Pts',(-45.1168338059478,-57.11354441615,-41.3138815317038));
#268725=CARTESIAN_POINT('Ctrl Pts',(-45.1206309792415,-57.1564190282566,
-41.3347987762303));
#268726=CARTESIAN_POINT('Ctrl Pts',(-45.1224627479043,-57.1851396939165,
-41.3484832320635));
#268727=CARTESIAN_POINT('Ctrl Pts',(-45.1230291819396,-57.199581674993,
-41.3552011986272));
#268728=CARTESIAN_POINT('Ctrl Pts',(-45.1234439819388,-57.2285619504273,
-41.3683510337761));
#268729=CARTESIAN_POINT('Ctrl Pts',(-45.1232917301137,-57.2429904040975,
-41.3747335054784));
#268730=CARTESIAN_POINT('Ctrl Pts',(-45.122279779691,-57.2717682086368,
-41.3871399525693));
#268731=CARTESIAN_POINT('Ctrl Pts',(-45.1196997436484,-57.3147947598186,
-41.4052018313649));
#268732=CARTESIAN_POINT('Ctrl Pts',(-45.1120557453653,-57.3716084168758,
-41.4271228345082));
#268733=CARTESIAN_POINT('Ctrl Pts',(-45.1031553338884,-57.4137999065974,
-41.4419446800329));
#268734=CARTESIAN_POINT('Ctrl Pts',(-45.09650693546,-57.4418330021969,-41.4514615780937));
#268735=CARTESIAN_POINT('Ctrl Pts',(-45.092823442876,-57.4558081403435,
-41.4560396298995));
#268736=CARTESIAN_POINT('Ctrl Pts',(-45.08473584999,-57.4836385233421,-41.464818484644));
#268737=CARTESIAN_POINT('Ctrl Pts',(-45.0803094818206,-57.4975537933777,
-41.4690360581021));
#268738=CARTESIAN_POINT('Ctrl Pts',(-45.0708158371377,-57.5249803724867,
-41.4770040232021));
#268739=CARTESIAN_POINT('Ctrl Pts',(-45.060662137239,-57.5520858826269,
-41.4845331733926));
#268740=CARTESIAN_POINT('Ctrl Pts',(-45.0434887903859,-57.591755117417,
-41.4945182619959));
#268741=CARTESIAN_POINT('Ctrl Pts',(-45.0243848727922,-57.6304534586566,
-41.5032105668009));
#268742=CARTESIAN_POINT('Ctrl Pts',(-45.0033512023575,-57.6681778817651,
-41.51061115159));
#268743=CARTESIAN_POINT('Ctrl Pts',(-44.9880328234845,-57.692673879575,
-41.5146787869643));
#268744=CARTESIAN_POINT('Ctrl Pts',(-44.9720568870916,-57.7168380825906,
-41.5183074012753));
#268745=CARTESIAN_POINT('Ctrl Pts',(-44.9637457009402,-57.7287466936453,
-41.5199012977462));
#268746=CARTESIAN_POINT('Ctrl Pts',(-44.9464287138105,-57.7522550306847,
-41.5226441863212));
#268747=CARTESIAN_POINT('Ctrl Pts',(-44.9374830238235,-57.7637718882179,
-41.5237830976086));
#268748=CARTESIAN_POINT('Ctrl Pts',(-44.9099214446927,-57.7974515399035,
-41.5264929611258));
#268749=CARTESIAN_POINT('Ctrl Pts',(-44.8905204729439,-57.8188493934961,
-41.5273772161885));
#268750=CARTESIAN_POINT('Ctrl Pts',(-44.8497318000032,-57.8595330722204,
-41.5273307191807));
#268751=CARTESIAN_POINT('Ctrl Pts',(-44.8283374647208,-57.878828810327,
-41.5264014189239));
#268752=CARTESIAN_POINT('Ctrl Pts',(-44.7947479986672,-57.9061820008563,
-41.5236391765087));
#268753=CARTESIAN_POINT('Ctrl Pts',(-44.7832945060713,-57.9150388128137,
-41.5224889540588));
#268754=CARTESIAN_POINT('Ctrl Pts',(-44.7657408175914,-57.9279147771907,
-41.5204166102647));
#268755=CARTESIAN_POINT('Ctrl Pts',(-44.7598217545323,-57.9321421746299,
-41.5196671186517));
#268756=CARTESIAN_POINT('Ctrl Pts',(-44.7478629508254,-57.9404557426351,
-41.5180519716851));
#268757=CARTESIAN_POINT('Ctrl Pts',(-44.7297025277655,-57.9527400844071,
-41.5154481926132));
#268758=CARTESIAN_POINT('Ctrl Pts',(-44.711220794734,-57.9642369190977,
-41.5123523449538));
#268759=CARTESIAN_POINT('Ctrl Pts',(-44.6862770262529,-57.9788987855805,
-41.5077941640223));
#268760=CARTESIAN_POINT('Ctrl Pts',(-44.6484202704456,-57.9998814948776,
-41.5003121274858));
#268761=CARTESIAN_POINT('Ctrl Pts',(-44.5962108390282,-58.0238874022289,
-41.4877980263462));
#268762=CARTESIAN_POINT('Ctrl Pts',(-44.5557649369164,-58.0389385823793,
-41.4765186283493));
#268763=CARTESIAN_POINT('Ctrl Pts',(-44.5285120653069,-58.048310487242,
-41.4685735203231));
#268764=CARTESIAN_POINT('Ctrl Pts',(-44.5147341086114,-58.0526671867402,
-41.4643859028639));
#268765=CARTESIAN_POINT('Ctrl Pts',(-44.4869140318333,-58.0607029371288,
-41.4555883503401));
#268766=CARTESIAN_POINT('Ctrl Pts',(-44.4728027150897,-58.0643973546439,
-41.4509544537452));
#268767=CARTESIAN_POINT('Ctrl Pts',(-44.4304531283686,-58.0743536715507,
-41.4365378845966));
#268768=CARTESIAN_POINT('Ctrl Pts',(-44.3879697631396,-58.0821103913619,
-41.4210702443308));
#268769=CARTESIAN_POINT('Ctrl Pts',(-44.3452880889881,-58.0866896268435,
-41.4040725286766));
#268770=CARTESIAN_POINT('Ctrl Pts',(-44.3025416355467,-58.090217180745,
-41.3865671155567));
#268771=CARTESIAN_POINT('Ctrl Pts',(-44.2739489581488,-58.0911687787978,
-41.3742170239002));
#268772=CARTESIAN_POINT('Ctrl Pts',(-44.2309555122234,-58.090491506171,
-41.3546803180427));
#268773=CARTESIAN_POINT('Ctrl Pts',(-44.2165895018292,-58.0899123697243,
-41.347990487553));
#268774=CARTESIAN_POINT('Ctrl Pts',(-44.1950278537333,-58.0885113544661,
-41.337705180963));
#268775=CARTESIAN_POINT('Ctrl Pts',(-44.1878319550126,-58.0879547296283,
-41.3342316293533));
#268776=CARTESIAN_POINT('Ctrl Pts',(-44.1734279164018,-58.0866616594573,
-41.3271961709002));
#268777=CARTESIAN_POINT('Ctrl Pts',(-44.1662260389348,-58.0859253983809,
-41.3236371482021));
#268778=CARTESIAN_POINT('Ctrl Pts',(-44.130389101081,-58.0818150523559,
-41.3057210105631));
#268779=CARTESIAN_POINT('Ctrl Pts',(-44.073848260417,-58.0724828543971,
-41.2761395013722));
#268780=CARTESIAN_POINT('Ctrl Pts',(-44.0188545174212,-58.0578491440998,
-41.2447838757269));
#268781=CARTESIAN_POINT('Ctrl Pts',(-43.9646246641704,-58.0405931079736,
-41.2125419608827));
#268782=CARTESIAN_POINT('Ctrl Pts',(-43.9378880325505,-58.0306505669816,
-41.1959746665064));
#268783=CARTESIAN_POINT('Ctrl Pts',(-43.9049634769563,-58.0165631445999,
-41.174705886574));
#268784=CARTESIAN_POINT('Ctrl Pts',(-43.898399460067,-58.0136596367661,
-41.1704209658528));
#268785=CARTESIAN_POINT('Ctrl Pts',(-43.8853286348063,-58.0076886655405,
-41.1617993561325));
#268786=CARTESIAN_POINT('Ctrl Pts',(-43.8788088737381,-58.0046144513738,
-41.157453730181));
#268787=CARTESIAN_POINT('Ctrl Pts',(-43.8593967360427,-57.9951717320096,
-41.1443784829743));
#268788=CARTESIAN_POINT('Ctrl Pts',(-43.8466719188398,-57.9885954718361,
-41.1356253645631));
#268789=CARTESIAN_POINT('Ctrl Pts',(-43.8341420587998,-57.9817357678076,
-41.1268248734572));
#268790=CARTESIAN_POINT('',(-43.5555682511181,-59.2341350312479,-39.6401231904583));
#268791=CARTESIAN_POINT('Ctrl Pts',(-43.4805771074156,-59.5712767529309,
-39.2399080357013));
#268792=CARTESIAN_POINT('Ctrl Pts',(-43.4150727209207,-59.5358440364426,
-39.2223070534893));
#268793=CARTESIAN_POINT('Ctrl Pts',(-43.2883193276586,-59.4590682572254,
-39.1867578392588));
#268794=CARTESIAN_POINT('Ctrl Pts',(-43.1106712693135,-59.32658002426,-39.1324031814995));
#268795=CARTESIAN_POINT('Ctrl Pts',(-43.0005921597408,-59.2266373021163,
-39.0954660506179));
#268796=CARTESIAN_POINT('Ctrl Pts',(-42.8948534568781,-59.1207134074407,
-39.0581733199915));
#268797=CARTESIAN_POINT('Ctrl Pts',(-42.7951360401793,-59.0104958554849,
-39.0211184761739));
#268798=CARTESIAN_POINT('Ctrl Pts',(-42.6850011896347,-58.8622904152127,
-38.9753582681256));
#268799=CARTESIAN_POINT('Ctrl Pts',(-42.6055727997797,-58.7375004045667,
-38.939089851323));
#268800=CARTESIAN_POINT('Ctrl Pts',(-42.5503788594446,-58.6407591922129,
-38.9120596161462));
#268801=CARTESIAN_POINT('Ctrl Pts',(-42.5165536369311,-58.5741539171446,
-38.8941613358138));
#268802=CARTESIAN_POINT('Ctrl Pts',(-42.4842288567228,-58.5064298632496,
-38.8763157156907));
#268803=CARTESIAN_POINT('Ctrl Pts',(-42.4689425396028,-58.4722695523732,
-38.8674882509199));
#268804=CARTESIAN_POINT('Ctrl Pts',(-42.4257123024776,-58.3690064948315,
-38.8413136266604));
#268805=CARTESIAN_POINT('Ctrl Pts',(-42.3750272156063,-58.229152189777,
-38.8072100415055));
#268806=CARTESIAN_POINT('Ctrl Pts',(-42.3380647902547,-58.0850119200902,
-38.7746901633276));
#268807=CARTESIAN_POINT('Ctrl Pts',(-42.3155659796374,-57.9752818499468,
-38.7509105250088));
#268808=CARTESIAN_POINT('Ctrl Pts',(-42.3089374211558,-57.9384266221928,
-38.7430843922672));
#268809=CARTESIAN_POINT('Ctrl Pts',(-42.297458012674,-57.864178756387,-38.7276438637217));
#268810=CARTESIAN_POINT('Ctrl Pts',(-42.292601515188,-57.8267325312259,
-38.720018782004));
#268811=CARTESIAN_POINT('Ctrl Pts',(-42.2847289916893,-57.7514526301959,
-38.7050196673963));
#268812=CARTESIAN_POINT('Ctrl Pts',(-42.2817363521424,-57.7138759968928,
-38.6976962453237));
#268813=CARTESIAN_POINT('Ctrl Pts',(-42.277596992864,-57.6387184974263,
-38.6833720377019));
#268814=CARTESIAN_POINT('Ctrl Pts',(-42.2741651307842,-57.5260409596698,
-38.6623829091612));
#268815=CARTESIAN_POINT('Ctrl Pts',(-42.2805893100654,-57.3760354719141,
-38.6363740800325));
#268816=CARTESIAN_POINT('Ctrl Pts',(-42.2937061680812,-57.2637038035873,
-38.618370061439));
#268817=CARTESIAN_POINT('Ctrl Pts',(-42.3043247017591,-57.1888547452426,
-38.6067079534822));
#268818=CARTESIAN_POINT('Ctrl Pts',(-42.3105743117123,-57.1514345461221,
-38.6010450635964));
#268819=CARTESIAN_POINT('Ctrl Pts',(-42.3249704170347,-57.0766935209607,
-38.590076215021));
#268820=CARTESIAN_POINT('Ctrl Pts',(-42.3331592025312,-57.0392159768686,
-38.5847494243559));
#268821=CARTESIAN_POINT('Ctrl Pts',(-42.3512949844302,-56.9651221381903,
-38.5745673038812));
#268822=CARTESIAN_POINT('Ctrl Pts',(-42.3712216906218,-56.8916587034686,
-38.564820665347));
#268823=CARTESIAN_POINT('Ctrl Pts',(-42.4063979707918,-56.7834465224234,
-38.5515118436));
#268824=CARTESIAN_POINT('Ctrl Pts',(-42.4468320479729,-56.6771725078319,
-38.5395042677724));
#268825=CARTESIAN_POINT('Ctrl Pts',(-42.4925290654744,-56.5728473165674,
-38.5288039137004));
#268826=CARTESIAN_POINT('Ctrl Pts',(-42.5265325119253,-56.5046058456765,
-38.5225509073062));
#268827=CARTESIAN_POINT('Ctrl Pts',(-42.5623338475306,-56.4370293947697,
-38.5167461666044));
#268828=CARTESIAN_POINT('Ctrl Pts',(-42.5811223641794,-56.4035923099625,
-38.5140693065785));
#268829=CARTESIAN_POINT('Ctrl Pts',(-42.620584523009,-56.3373241998654,
-38.5091697400817));
#268830=CARTESIAN_POINT('Ctrl Pts',(-42.6411082254821,-56.3047465904101,
-38.5069659500128));
#268831=CARTESIAN_POINT('Ctrl Pts',(-42.7048067991197,-56.2090283357163,
-38.501110858935));
#268832=CARTESIAN_POINT('Ctrl Pts',(-42.7502234543428,-56.1476408662828,
-38.4981890389281));
#268833=CARTESIAN_POINT('Ctrl Pts',(-42.8467942323831,-56.0297655581676,
-38.4942910511033));
#268834=CARTESIAN_POINT('Ctrl Pts',(-42.8979715413934,-55.9732420482176,
-38.4933125989996));
#268835=CARTESIAN_POINT('Ctrl Pts',(-42.9790570553347,-55.8921695883033,
-38.4933149859729));
#268836=CARTESIAN_POINT('Ctrl Pts',(-43.0068374106561,-55.8657400908868,
-38.4935622007431));
#268837=CARTESIAN_POINT('Ctrl Pts',(-43.0495800649421,-55.8270637749536,
-38.4943063068789));
#268838=CARTESIAN_POINT('Ctrl Pts',(-43.0640222060113,-55.8143203511958,
-38.494617152342));
#268839=CARTESIAN_POINT('Ctrl Pts',(-43.0932714774893,-55.7891564261061,
-38.4953646906773));
#268840=CARTESIAN_POINT('Ctrl Pts',(-43.1080901283632,-55.7767277938553,
-38.4958020036096));
#268841=CARTESIAN_POINT('Ctrl Pts',(-43.1528523310046,-55.7401327167866,
-38.4972962980169));
#268842=CARTESIAN_POINT('Ctrl Pts',(-43.2134913856688,-55.6930468850421,
-38.4997758707861));
#268843=CARTESIAN_POINT('Ctrl Pts',(-43.3385569247743,-55.6055389451161,
-38.5066450244003));
#268844=CARTESIAN_POINT('Ctrl Pts',(-43.4691986576013,-55.5278792007279,
-38.5163302992824));
#268845=CARTESIAN_POINT('Ctrl Pts',(-43.5713395927684,-55.4769743237494,
-38.5256877381308));
#268846=CARTESIAN_POINT('Ctrl Pts',(-43.6403672861995,-55.4446857735354,
-38.5323951500278));
#268847=CARTESIAN_POINT('Ctrl Pts',(-43.6753577685123,-55.4293620157832,
-38.5359845633874));
#268848=CARTESIAN_POINT('Ctrl Pts',(-43.7462462065788,-55.4003985583156,
-38.5436333065981));
#268849=CARTESIAN_POINT('Ctrl Pts',(-43.7822717759725,-55.3867204456352,
-38.5477088862383));
#268850=CARTESIAN_POINT('Ctrl Pts',(-43.8543821738219,-55.3613797848081,
-38.5562346427694));
#268851=CARTESIAN_POINT('Ctrl Pts',(-43.890622407919,-55.349649082917,-38.5607007444526));
#268852=CARTESIAN_POINT('Ctrl Pts',(-43.9997560709039,-55.3172704656441,
-38.5746802407103));
#268853=CARTESIAN_POINT('Ctrl Pts',(-44.1098017310836,-55.290468361793,
-38.5898286859852));
#268854=CARTESIAN_POINT('Ctrl Pts',(-44.2583166685835,-55.2656490138239,
-38.612301023075));
#268855=CARTESIAN_POINT('Ctrl Pts',(-44.3705972700495,-55.2524997368729,
-38.6302900391873));
#268856=CARTESIAN_POINT('Ctrl Pts',(-44.446056048267,-55.2474029004138,
-38.6430428201589));
#268857=CARTESIAN_POINT('Ctrl Pts',(-44.5218128020516,-55.2441636366351,
-38.65617756452));
#268858=CARTESIAN_POINT('Ctrl Pts',(-44.5599089424743,-55.2434808562086,
-38.6629497802385));
#268859=CARTESIAN_POINT('Ctrl Pts',(-44.6354869543582,-55.2439911084578,
-38.6767130108817));
#268860=CARTESIAN_POINT('Ctrl Pts',(-44.6731456892459,-55.2451740103824,
-38.6837342374529));
#268861=CARTESIAN_POINT('Ctrl Pts',(-44.7481014788608,-55.2493620066237,
-38.6980304684339));
#268862=CARTESIAN_POINT('Ctrl Pts',(-44.860046548974,-55.2583760573225,
-38.7198650218829));
#268863=CARTESIAN_POINT('Ctrl Pts',(-45.0073845433675,-55.2811507310277,
-38.7505067688753));
#268864=CARTESIAN_POINT('Ctrl Pts',(-45.1528189888476,-55.3146135839333,
-38.7826550300594));
#268865=CARTESIAN_POINT('Ctrl Pts',(-45.2248832056965,-55.3349380951144,
-38.7992310848652));
#268866=CARTESIAN_POINT('Ctrl Pts',(-45.2966462681613,-55.3570913336823,
-38.8160672125853));
#268867=CARTESIAN_POINT('Ctrl Pts',(-45.3323638946335,-55.3690863290504,
-38.8246135819642));
#268868=CARTESIAN_POINT('Ctrl Pts',(-45.4027951436545,-55.3946744461232,
-38.841798196801));
#268869=CARTESIAN_POINT('Ctrl Pts',(-45.4376370321487,-55.4083060218429,
-38.85046633842));
#268870=CARTESIAN_POINT('Ctrl Pts',(-45.5409345111852,-55.4516493275196,
-38.8766665754573));
#268871=CARTESIAN_POINT('Ctrl Pts',(-45.6082182891413,-55.4838201174091,
-38.8944064774514));
#268872=CARTESIAN_POINT('Ctrl Pts',(-45.7067749877369,-55.5369855856676,
-38.9214216121435));
#268873=CARTESIAN_POINT('Ctrl Pts',(-45.7392219877795,-55.5555212114618,
-38.9304915704334));
#268874=CARTESIAN_POINT('Ctrl Pts',(-45.8033556832395,-55.5942722159849,
-38.9487787872477));
#268875=CARTESIAN_POINT('Ctrl Pts',(-45.8348443691401,-55.6143675312756,
-38.9579395118015));
#268876=CARTESIAN_POINT('Ctrl Pts',(-45.9274099842789,-55.6766589025306,
-38.9854159162723));
#268877=CARTESIAN_POINT('Ctrl Pts',(-45.9867610865919,-55.7209353156014,
-39.0037703637879));
#268878=CARTESIAN_POINT('Ctrl Pts',(-46.1007337830098,-55.8148102393793,
-39.0405190865864));
#268879=CARTESIAN_POINT('Ctrl Pts',(-46.1826971388658,-55.889219933262,
-39.0681181728269));
#268880=CARTESIAN_POINT('Ctrl Pts',(-46.259356574729,-55.9696687352924,
-39.0957737179551));
#268881=CARTESIAN_POINT('Ctrl Pts',(-46.309266807939,-56.024663053365,-39.1142236413887));
#268882=CARTESIAN_POINT('Ctrl Pts',(-46.3336138177017,-56.0528284109483,
-39.1234510495426));
#268883=CARTESIAN_POINT('Ctrl Pts',(-46.3692509284248,-56.0961546965833,
-39.1373141736981));
#268884=CARTESIAN_POINT('Ctrl Pts',(-46.3809719555493,-56.1107655250657,
-39.14193505412));
#268885=CARTESIAN_POINT('Ctrl Pts',(-46.4039850968433,-56.1401806715041,
-39.1511314768264));
#268886=CARTESIAN_POINT('Ctrl Pts',(-46.4153001903629,-56.1550126624776,
-39.1557159133813));
#268887=CARTESIAN_POINT('Ctrl Pts',(-46.4486370096885,-56.1998310060263,
-39.1694131182659));
#268888=CARTESIAN_POINT('Ctrl Pts',(-46.4700835091466,-56.2301795317326,
-39.1784826054425));
#268889=CARTESIAN_POINT('Ctrl Pts',(-46.532071913686,-56.3225583984772,
-39.2054898733524));
#268890=CARTESIAN_POINT('Ctrl Pts',(-46.5894197348374,-56.4176636744323,
-39.23211607576));
#268891=CARTESIAN_POINT('Ctrl Pts',(-46.6566074362748,-56.5498680842415,
-39.2668544229849));
#268892=CARTESIAN_POINT('Ctrl Pts',(-46.6870820302515,-56.617790568625,
-39.2839693714534));
#268893=CARTESIAN_POINT('Ctrl Pts',(-46.7159729830272,-56.6866360545619,
-39.3009558869148));
#268894=CARTESIAN_POINT('Ctrl Pts',(-46.7296188023799,-56.7214992889704,
-39.3093799218186));
#268895=CARTESIAN_POINT('Ctrl Pts',(-46.7553216997643,-56.7922546384013,
-39.3261176641085));
#268896=CARTESIAN_POINT('Ctrl Pts',(-46.7672996943011,-56.8279354881579,
-39.3343809787628));
#268897=CARTESIAN_POINT('Ctrl Pts',(-46.8004530502947,-56.9353633959568,
-39.358737163018));
#268898=CARTESIAN_POINT('Ctrl Pts',(-46.8189795501832,-57.0077635587999,
-39.3744658121213));
#268899=CARTESIAN_POINT('Ctrl Pts',(-46.848916211803,-57.1540080946302,
-39.4048998290393));
#268900=CARTESIAN_POINT('Ctrl Pts',(-46.866048617508,-57.2647966217996,
-39.4269646939479));
#268901=CARTESIAN_POINT('Ctrl Pts',(-46.875074749658,-57.3772756893033,
-39.4478819384746));
#268902=CARTESIAN_POINT('Ctrl Pts',(-46.8792542953452,-57.4526370309597,
-39.4615663943076));
#268903=CARTESIAN_POINT('Ctrl Pts',(-46.8804258736835,-57.4905390832845,
-39.4682843608713));
#268904=CARTESIAN_POINT('Ctrl Pts',(-46.8808837743635,-57.566610437341,
-39.4814341960201));
#268905=CARTESIAN_POINT('Ctrl Pts',(-46.8801708637706,-57.604491394965,
-39.4878166677226));
#268906=CARTESIAN_POINT('Ctrl Pts',(-46.8768913879562,-57.6800597985945,
-39.5002231148134));
#268907=CARTESIAN_POINT('Ctrl Pts',(-46.8691896925243,-57.7930657109158,
-39.5182849936093));
#268908=CARTESIAN_POINT('Ctrl Pts',(-46.8479069711518,-57.9423669591112,
-39.540205996752));
#268909=CARTESIAN_POINT('Ctrl Pts',(-46.8236459543104,-58.053306681129,
-39.5550278422771));
#268910=CARTESIAN_POINT('Ctrl Pts',(-46.8055990109883,-58.1270324939452,
-39.5645447403379));
#268911=CARTESIAN_POINT('Ctrl Pts',(-46.7956339676918,-58.1637938532181,
-39.5691227921436));
#268912=CARTESIAN_POINT('Ctrl Pts',(-46.7738161327052,-58.2370162077019,
-39.5779016468881));
#268913=CARTESIAN_POINT('Ctrl Pts',(-46.7619036278491,-58.2736352268715,
-39.5821192203466));
#268914=CARTESIAN_POINT('Ctrl Pts',(-46.7364059718256,-58.3458255995332,
-39.5900871854462));
#268915=CARTESIAN_POINT('Ctrl Pts',(-46.7091836493705,-58.4171862986019,
-39.5976163356366));
#268916=CARTESIAN_POINT('Ctrl Pts',(-46.663274408039,-58.5216699086648,
-39.6076014242402));
#268917=CARTESIAN_POINT('Ctrl Pts',(-46.6123207377325,-58.6236436013082,
-39.616293729045));
#268918=CARTESIAN_POINT('Ctrl Pts',(-46.5563244858032,-58.7230996041114,
-39.6236943138341));
#268919=CARTESIAN_POINT('Ctrl Pts',(-46.515607032986,-58.7877140896312,
-39.6277619492082));
#268920=CARTESIAN_POINT('Ctrl Pts',(-46.4731710833873,-58.8514710047945,
-39.6313905635194));
#268921=CARTESIAN_POINT('Ctrl Pts',(-46.4511086137465,-58.8829006319494,
-39.6329844599904));
#268922=CARTESIAN_POINT('Ctrl Pts',(-46.4051673201274,-58.9449633016888,
-39.6357273485653));
#268923=CARTESIAN_POINT('Ctrl Pts',(-46.381447994276,-58.975377588932,-39.6368662598532));
#268924=CARTESIAN_POINT('Ctrl Pts',(-46.3084068909562,-59.0643493136614,
-39.6395761233691));
#268925=CARTESIAN_POINT('Ctrl Pts',(-46.2570407846102,-59.1209150453974,
-39.6404603784325));
#268926=CARTESIAN_POINT('Ctrl Pts',(-46.1491379755941,-59.228544463199,
-39.6404138814247));
#268927=CARTESIAN_POINT('Ctrl Pts',(-46.0925836555155,-59.2796343044913,
-39.6394845811684));
#268928=CARTESIAN_POINT('Ctrl Pts',(-46.0038529437629,-59.3521266125547,
-39.6367223387528));
#268929=CARTESIAN_POINT('Ctrl Pts',(-45.9736068078661,-59.3756113554055,
-39.6355721163029));
#268930=CARTESIAN_POINT('Ctrl Pts',(-45.9272656961273,-59.4097723546528,
-39.6334997725088));
#268931=CARTESIAN_POINT('Ctrl Pts',(-45.9116419215573,-59.4209912820171,
-39.6327502808957));
#268932=CARTESIAN_POINT('Ctrl Pts',(-45.8800804794677,-59.4430610802669,
-39.6311351339295));
#268933=CARTESIAN_POINT('Ctrl Pts',(-45.8321587971618,-59.4756823489919,
-39.628531354857));
#268934=CARTESIAN_POINT('Ctrl Pts',(-45.7834097108732,-59.5062438963941,
-39.6254355071979));
#268935=CARTESIAN_POINT('Ctrl Pts',(-45.717633106262,-59.5452481912826,
-39.6208773262667));
#268936=CARTESIAN_POINT('Ctrl Pts',(-45.6178307490054,-59.601113548897,
-39.6133952897297));
#268937=CARTESIAN_POINT('Ctrl Pts',(-45.4802897643185,-59.6652183443042,
-39.6008811885904));
#268938=CARTESIAN_POINT('Ctrl Pts',(-45.3738098009101,-59.7055766782111,
-39.5896017905935));
#268939=CARTESIAN_POINT('Ctrl Pts',(-45.3020778813705,-59.7307512119865,
-39.5816566825671));
#268940=CARTESIAN_POINT('Ctrl Pts',(-45.2658207311094,-59.7424779859237,
-39.5774690651077));
#268941=CARTESIAN_POINT('Ctrl Pts',(-45.1926264675053,-59.7641596016776,
-39.5686715125846));
#268942=CARTESIAN_POINT('Ctrl Pts',(-45.1555073907618,-59.7741562512684,
-39.5640376159893));
#268943=CARTESIAN_POINT('Ctrl Pts',(-45.0441315765335,-59.8011904590316,
-39.5496210468413));
#268944=CARTESIAN_POINT('Ctrl Pts',(-44.9324484012679,-59.8224577850013,
-39.5341534065747));
#268945=CARTESIAN_POINT('Ctrl Pts',(-44.8203079610257,-59.8353953605365,
-39.5171556909205));
#268946=CARTESIAN_POINT('Ctrl Pts',(-44.7080184564226,-59.8455760612675,
-39.4996502778008));
#268947=CARTESIAN_POINT('Ctrl Pts',(-44.6329372249224,-59.8486931621852,
-39.4873001861445));
#268948=CARTESIAN_POINT('Ctrl Pts',(-44.5200834441659,-59.8478515133141,
-39.4677634802869));
#268949=CARTESIAN_POINT('Ctrl Pts',(-44.4823810871712,-59.8466449718289,
-39.4610736497974));
#268950=CARTESIAN_POINT('Ctrl Pts',(-44.4258051079382,-59.8434394706745,
-39.4507883432074));
#268951=CARTESIAN_POINT('Ctrl Pts',(-44.4069254589855,-59.8421361346926,
-39.4473147915973));
#268952=CARTESIAN_POINT('Ctrl Pts',(-44.3691376542581,-59.8390581625153,
-39.4402793331445));
#268953=CARTESIAN_POINT('Ctrl Pts',(-44.3502459350849,-59.8372838734483,
-39.4367203104461));
#268954=CARTESIAN_POINT('Ctrl Pts',(-44.2562487381671,-59.8272835659938,
-39.4188041728073));
#268955=CARTESIAN_POINT('Ctrl Pts',(-44.1080045765469,-59.8040393501646,
-39.3892226636159));
#268956=CARTESIAN_POINT('Ctrl Pts',(-43.9639303529155,-59.7668593120831,
-39.3578670379715));
#268957=CARTESIAN_POINT('Ctrl Pts',(-43.8219159040518,-59.7227861654643,
-39.3256251231267));
#268958=CARTESIAN_POINT('Ctrl Pts',(-43.7519290534068,-59.6972943066161,
-39.3090578287531));
#268959=CARTESIAN_POINT('Ctrl Pts',(-43.665783177736,-59.6610675807531,
-39.2877890488175));
#268960=CARTESIAN_POINT('Ctrl Pts',(-43.6486106666635,-59.653596197985,
-39.2835041280971));
#268961=CARTESIAN_POINT('Ctrl Pts',(-43.6144193015916,-59.6382222359849,
-39.2748825183767));
#268962=CARTESIAN_POINT('Ctrl Pts',(-43.597366582891,-59.6303022352814,
-39.2705368924251));
#268963=CARTESIAN_POINT('Ctrl Pts',(-43.5465994182959,-59.605961903298,
-39.2574616452183));
#268964=CARTESIAN_POINT('Ctrl Pts',(-43.513329300663,-59.588993111175,-39.2487085268073));
#268965=CARTESIAN_POINT('Ctrl Pts',(-43.4805771074156,-59.5712767529309,
-39.2399080357013));
#268966=CARTESIAN_POINT('Ctrl Pts',(-43.8341420587998,-57.9817357678076,
-41.1268248734572));
#268967=CARTESIAN_POINT('Ctrl Pts',(-43.8090823387197,-57.9680163597508,
-41.1092238912453));
#268968=CARTESIAN_POINT('Ctrl Pts',(-43.7605654269547,-57.9383371077444,
-41.0736746770147));
#268969=CARTESIAN_POINT('Ctrl Pts',(-43.6924895655639,-57.8872515755908,
-41.019320019256));
#268970=CARTESIAN_POINT('Ctrl Pts',(-43.6502497090231,-57.8487916199066,
-40.9823828883729));
#268971=CARTESIAN_POINT('Ctrl Pts',(-43.6096433745973,-57.8080652293815,
-40.945090157748));
#268972=CARTESIAN_POINT('Ctrl Pts',(-43.5713160673933,-57.7657212262301,
-40.9080353139296));
#268973=CARTESIAN_POINT('Ctrl Pts',(-43.5288984657655,-57.7088609123343,
-40.8622751058818));
#268974=CARTESIAN_POINT('Ctrl Pts',(-43.4982484100127,-57.6610280687967,
-40.826006689079));
#268975=CARTESIAN_POINT('Ctrl Pts',(-43.4769169762936,-57.6239677344727,
-40.798976453902));
#268976=CARTESIAN_POINT('Ctrl Pts',(-43.4638199758968,-57.5984660781933,
-40.7810781735695));
#268977=CARTESIAN_POINT('Ctrl Pts',(-43.4512904535732,-57.5725430453748,
-40.7632325534464));
#268978=CARTESIAN_POINT('Ctrl Pts',(-43.4453582046716,-57.5594707895743,
-40.7544050886758));
#268979=CARTESIAN_POINT('Ctrl Pts',(-43.4285595200757,-57.5199648485381,
-40.7282304644163));
#268980=CARTESIAN_POINT('Ctrl Pts',(-43.4088016745783,-57.4664867157472,
-40.6941268792613));
#268981=CARTESIAN_POINT('Ctrl Pts',(-43.3942530508608,-57.4114223976644,
-40.6616070010832));
#268982=CARTESIAN_POINT('Ctrl Pts',(-43.3853242538269,-57.3695231591805,
-40.6378273627645));
#268983=CARTESIAN_POINT('Ctrl Pts',(-43.3826786150667,-57.3554536366825,
-40.630001230023));
#268984=CARTESIAN_POINT('Ctrl Pts',(-43.378062215599,-57.3271160344971,
-40.6145607014775));
#268985=CARTESIAN_POINT('Ctrl Pts',(-43.3760891270041,-57.3128275119467,
-40.60693561976));
#268986=CARTESIAN_POINT('Ctrl Pts',(-43.3728422231051,-57.2841093232557,
-40.5919365051523));
#268987=CARTESIAN_POINT('Ctrl Pts',(-43.3715781643254,-57.2697777029377,
-40.5846130830795));
#268988=CARTESIAN_POINT('Ctrl Pts',(-43.3697526802575,-57.2411194243864,
-40.5702888754578));
#268989=CARTESIAN_POINT('Ctrl Pts',(-43.3680717796799,-57.1981642741791,
-40.5492997469169));
#268990=CARTESIAN_POINT('Ctrl Pts',(-43.3700185838812,-57.1410182421193,
-40.5232909177883));
#268991=CARTESIAN_POINT('Ctrl Pts',(-43.3746384661022,-57.0982543712987,
-40.505286899195));
#268992=CARTESIAN_POINT('Ctrl Pts',(-43.3784319419536,-57.0697666559562,
-40.4936247912381));
#268993=CARTESIAN_POINT('Ctrl Pts',(-43.3806866868643,-57.0555278483981,
-40.4879619013523));
#268994=CARTESIAN_POINT('Ctrl Pts',(-43.3859186984709,-57.0270949764048,
-40.476993052777));
#268995=CARTESIAN_POINT('Ctrl Pts',(-43.3889115442249,-57.0128413374093,
-40.4716662621118));
#268996=CARTESIAN_POINT('Ctrl Pts',(-43.3955695423488,-56.984668670318,
-40.4614841416371));
#268997=CARTESIAN_POINT('Ctrl Pts',(-43.4029115329907,-56.9567427536229,
-40.4517375031029));
#268998=CARTESIAN_POINT('Ctrl Pts',(-43.4159439893498,-56.915628788467,
-40.4384286813559));
#268999=CARTESIAN_POINT('Ctrl Pts',(-43.4309850942545,-56.8752725380991,
-40.4264211055283));
#269000=CARTESIAN_POINT('Ctrl Pts',(-43.4480370013178,-56.8356780486645,
-40.4157207514563));
#269001=CARTESIAN_POINT('Ctrl Pts',(-43.4607570961379,-56.8097932355363,
-40.409467745062));
#269002=CARTESIAN_POINT('Ctrl Pts',(-43.4741642201056,-56.7841683331057,
-40.4036630043601));
#269003=CARTESIAN_POINT('Ctrl Pts',(-43.4812071336048,-56.7714928975767,
-40.4009861443346));
#269004=CARTESIAN_POINT('Ctrl Pts',(-43.4960130774609,-56.7463797512019,
-40.3960865778375));
#269005=CARTESIAN_POINT('Ctrl Pts',(-43.5037198572985,-56.7340380787953,
-40.3938827877695));
#269006=CARTESIAN_POINT('Ctrl Pts',(-43.527657505214,-56.6977883833479,
-40.3880276966888));
#269007=CARTESIAN_POINT('Ctrl Pts',(-43.5447483375558,-56.6745564757614,
-40.3851058766842));
#269008=CARTESIAN_POINT('Ctrl Pts',(-43.5811328114983,-56.629979998045,
-40.3812078888591));
#269009=CARTESIAN_POINT('Ctrl Pts',(-43.6004351631962,-56.6086219171049,
-40.3802294367552));
#269010=CARTESIAN_POINT('Ctrl Pts',(-43.6310475296952,-56.578014570072,
-40.3802318237287));
#269011=CARTESIAN_POINT('Ctrl Pts',(-43.6415402048873,-56.5680413281089,
-40.3804790384992));
#269012=CARTESIAN_POINT('Ctrl Pts',(-43.6576911458811,-56.5534539772523,
-40.3812231446347));
#269013=CARTESIAN_POINT('Ctrl Pts',(-43.6631494628181,-56.5486488515781,
-40.3815339900979));
#269014=CARTESIAN_POINT('Ctrl Pts',(-43.6742063152013,-56.5391628964206,
-40.3822815284329));
#269015=CARTESIAN_POINT('Ctrl Pts',(-43.6798092119243,-56.534479009001,
-40.3827188413654));
#269016=CARTESIAN_POINT('Ctrl Pts',(-43.6967370434146,-56.5206915949946,
-40.3842131357726));
#269017=CARTESIAN_POINT('Ctrl Pts',(-43.7196778600618,-56.5029622466235,
-40.386692708542));
#269018=CARTESIAN_POINT('Ctrl Pts',(-43.7670264629127,-56.4700551612604,
-40.3935618621563));
#269019=CARTESIAN_POINT('Ctrl Pts',(-43.8165352419067,-56.4409186299576,
-40.4032471370382));
#269020=CARTESIAN_POINT('Ctrl Pts',(-43.8552784957563,-56.4218759376155,
-40.4126045758866));
#269021=CARTESIAN_POINT('Ctrl Pts',(-43.8814691350842,-56.4098116142502,
-40.4193119877837));
#269022=CARTESIAN_POINT('Ctrl Pts',(-43.8947490665381,-56.4040935548973,
-40.4229014011429));
#269023=CARTESIAN_POINT('Ctrl Pts',(-43.9216608718689,-56.3933018151258,
-40.430550144354));
#269024=CARTESIAN_POINT('Ctrl Pts',(-43.9353412421961,-56.3882139347518,
-40.434625723994));
#269025=CARTESIAN_POINT('Ctrl Pts',(-43.9627318697344,-56.3788058930362,
-40.4431514805252));
#269026=CARTESIAN_POINT('Ctrl Pts',(-43.9765011076412,-56.3744602994329,
-40.4476175822086));
#269027=CARTESIAN_POINT('Ctrl Pts',(-44.0179764085085,-56.3624961934912,
-40.4615970784657));
#269028=CARTESIAN_POINT('Ctrl Pts',(-44.0598195105868,-56.3526585058303,
-40.4767455237411));
#269029=CARTESIAN_POINT('Ctrl Pts',(-44.1163310625808,-56.3437038269143,
-40.4992178608308));
#269030=CARTESIAN_POINT('Ctrl Pts',(-44.1590753545772,-56.3390714325247,
-40.5172068769433));
#269031=CARTESIAN_POINT('Ctrl Pts',(-44.1878153726385,-56.337382052278,
-40.5299596579145));
#269032=CARTESIAN_POINT('Ctrl Pts',(-44.2166756293141,-56.3364007867548,
-40.5430944022758));
#269033=CARTESIAN_POINT('Ctrl Pts',(-44.2311921171808,-56.3362675100036,
-40.5498666179945));
#269034=CARTESIAN_POINT('Ctrl Pts',(-44.2599977007373,-56.3367129587916,
-40.5636298486377));
#269035=CARTESIAN_POINT('Ctrl Pts',(-44.2743541649932,-56.3372884158027,
-40.5706510752088));
#269036=CARTESIAN_POINT('Ctrl Pts',(-44.3029357424357,-56.3391317429585,
-40.5849473061899));
#269037=CARTESIAN_POINT('Ctrl Pts',(-44.3456316213443,-56.3429350642169,
-40.6067818596389));
#269038=CARTESIAN_POINT('Ctrl Pts',(-44.4018650235691,-56.3520939287388,
-40.6374236066311));
#269039=CARTESIAN_POINT('Ctrl Pts',(-44.4574103376146,-56.3653147883305,
-40.6695718678152));
#269040=CARTESIAN_POINT('Ctrl Pts',(-44.4849466005937,-56.3732907222196,
-40.686147922621));
#269041=CARTESIAN_POINT('Ctrl Pts',(-44.512374392093,-56.3819617528141,
-40.7029840503412));
#269042=CARTESIAN_POINT('Ctrl Pts',(-44.5260289861432,-56.3866462995878,
-40.7115304197201));
#269043=CARTESIAN_POINT('Ctrl Pts',(-44.5529609776699,-56.3966203919845,
-40.7287150345567));
#269044=CARTESIAN_POINT('Ctrl Pts',(-44.5662873943758,-56.4019250012471,
-40.737383176176));
#269045=CARTESIAN_POINT('Ctrl Pts',(-44.6058068395674,-56.4187668411382,
-40.7635834132132));
#269046=CARTESIAN_POINT('Ctrl Pts',(-44.6315615859976,-56.4312362585519,
-40.7813233152079));
#269047=CARTESIAN_POINT('Ctrl Pts',(-44.6693071486035,-56.4518014713652,
-40.8083384498991));
#269048=CARTESIAN_POINT('Ctrl Pts',(-44.6817372625133,-56.458965010373,
-40.8174084081892));
#269049=CARTESIAN_POINT('Ctrl Pts',(-44.7063132537473,-56.473929075182,
-40.8356956250034));
#269050=CARTESIAN_POINT('Ctrl Pts',(-44.7183832523531,-56.4816832398284,
-40.8448563495594));
#269051=CARTESIAN_POINT('Ctrl Pts',(-44.7538754102704,-56.505703003501,
-40.8723327540241));
#269052=CARTESIAN_POINT('Ctrl Pts',(-44.7766465418209,-56.5227549736834,
-40.8906872015444));
#269053=CARTESIAN_POINT('Ctrl Pts',(-44.8204030914552,-56.5588699415109,
-40.9274359243417));
#269054=CARTESIAN_POINT('Ctrl Pts',(-44.851893062885,-56.5874690797881,
-40.9550350105826));
#269055=CARTESIAN_POINT('Ctrl Pts',(-44.8813802932551,-56.6183507815631,
-40.982690555711));
#269056=CARTESIAN_POINT('Ctrl Pts',(-44.9005867815582,-56.6394533348067,
-41.0011404791447));
#269057=CARTESIAN_POINT('Ctrl Pts',(-44.9099603095753,-56.6502571213647,
-41.0103678872986));
#269058=CARTESIAN_POINT('Ctrl Pts',(-44.9236872082217,-56.6668706184025,
-41.0242310114538));
#269059=CARTESIAN_POINT('Ctrl Pts',(-44.9282031316495,-56.6724722064122,
-41.0288518918758));
#269060=CARTESIAN_POINT('Ctrl Pts',(-44.9370720489983,-56.6837477093971,
-41.038048314582));
#269061=CARTESIAN_POINT('Ctrl Pts',(-44.9414338933841,-56.6894322363092,
-41.0426327511372));
#269062=CARTESIAN_POINT('Ctrl Pts',(-44.9542884395491,-56.7066066663578,
-41.0563299560217));
#269063=CARTESIAN_POINT('Ctrl Pts',(-44.9625629539304,-56.7182326826763,
-41.0653994431984));
#269064=CARTESIAN_POINT('Ctrl Pts',(-44.9864941991718,-56.7536111473724,
-41.0924067111081));
#269065=CARTESIAN_POINT('Ctrl Pts',(-45.0086645271567,-56.7900134244028,
-41.1190329135161));
#269066=CARTESIAN_POINT('Ctrl Pts',(-45.034704630644,-56.8405768845403,
-41.1537712607408));
#269067=CARTESIAN_POINT('Ctrl Pts',(-45.0465408860903,-56.8665423758261,
-41.1708862092094));
#269068=CARTESIAN_POINT('Ctrl Pts',(-45.0577761134165,-56.8928546179869,
-41.1878727246706));
#269069=CARTESIAN_POINT('Ctrl Pts',(-45.0630901582258,-56.906176087846,
-41.1962967595746));
#269070=CARTESIAN_POINT('Ctrl Pts',(-45.0731156002939,-56.9332061371524,
-41.2130345018643));
#269071=CARTESIAN_POINT('Ctrl Pts',(-45.0777961712447,-56.9468340019015,
-41.2212978165198));
#269072=CARTESIAN_POINT('Ctrl Pts',(-45.0907786540592,-56.9878560258786,
-41.2456540007716));
#269073=CARTESIAN_POINT('Ctrl Pts',(-45.0980724298404,-57.0154910056487,
-41.2613826498774));
#269074=CARTESIAN_POINT('Ctrl Pts',(-45.1099506000897,-57.0712899900431,
-41.2918166667949));
#269075=CARTESIAN_POINT('Ctrl Pts',(-45.1168338059478,-57.11354441615,-41.3138815317038));
#269076=CARTESIAN_POINT('Ctrl Pts',(-45.1206309792415,-57.1564190282566,
-41.3347987762303));
#269077=CARTESIAN_POINT('Ctrl Pts',(-45.1224627479043,-57.1851396939165,
-41.3484832320635));
#269078=CARTESIAN_POINT('Ctrl Pts',(-45.1230291819396,-57.199581674993,
-41.3552011986272));
#269079=CARTESIAN_POINT('Ctrl Pts',(-45.1234439819388,-57.2285619504273,
-41.3683510337761));
#269080=CARTESIAN_POINT('Ctrl Pts',(-45.1232917301137,-57.2429904040975,
-41.3747335054784));
#269081=CARTESIAN_POINT('Ctrl Pts',(-45.122279779691,-57.2717682086368,
-41.3871399525693));
#269082=CARTESIAN_POINT('Ctrl Pts',(-45.1196997436484,-57.3147947598186,
-41.4052018313649));
#269083=CARTESIAN_POINT('Ctrl Pts',(-45.1120557453653,-57.3716084168758,
-41.4271228345082));
#269084=CARTESIAN_POINT('Ctrl Pts',(-45.1031553338884,-57.4137999065974,
-41.4419446800329));
#269085=CARTESIAN_POINT('Ctrl Pts',(-45.09650693546,-57.4418330021969,-41.4514615780937));
#269086=CARTESIAN_POINT('Ctrl Pts',(-45.092823442876,-57.4558081403435,
-41.4560396298995));
#269087=CARTESIAN_POINT('Ctrl Pts',(-45.08473584999,-57.4836385233421,-41.464818484644));
#269088=CARTESIAN_POINT('Ctrl Pts',(-45.0803094818206,-57.4975537933777,
-41.4690360581021));
#269089=CARTESIAN_POINT('Ctrl Pts',(-45.0708158371377,-57.5249803724867,
-41.4770040232021));
#269090=CARTESIAN_POINT('Ctrl Pts',(-45.060662137239,-57.5520858826269,
-41.4845331733926));
#269091=CARTESIAN_POINT('Ctrl Pts',(-45.0434887903859,-57.591755117417,
-41.4945182619959));
#269092=CARTESIAN_POINT('Ctrl Pts',(-45.0243848727922,-57.6304534586566,
-41.5032105668009));
#269093=CARTESIAN_POINT('Ctrl Pts',(-45.0033512023575,-57.6681778817651,
-41.51061115159));
#269094=CARTESIAN_POINT('Ctrl Pts',(-44.9880328234845,-57.692673879575,
-41.5146787869643));
#269095=CARTESIAN_POINT('Ctrl Pts',(-44.9720568870916,-57.7168380825906,
-41.5183074012753));
#269096=CARTESIAN_POINT('Ctrl Pts',(-44.9637457009402,-57.7287466936453,
-41.5199012977462));
#269097=CARTESIAN_POINT('Ctrl Pts',(-44.9464287138105,-57.7522550306847,
-41.5226441863212));
#269098=CARTESIAN_POINT('Ctrl Pts',(-44.9374830238235,-57.7637718882179,
-41.5237830976086));
#269099=CARTESIAN_POINT('Ctrl Pts',(-44.9099214446927,-57.7974515399035,
-41.5264929611258));
#269100=CARTESIAN_POINT('Ctrl Pts',(-44.8905204729439,-57.8188493934961,
-41.5273772161885));
#269101=CARTESIAN_POINT('Ctrl Pts',(-44.8497318000032,-57.8595330722204,
-41.5273307191807));
#269102=CARTESIAN_POINT('Ctrl Pts',(-44.8283374647208,-57.878828810327,
-41.5264014189239));
#269103=CARTESIAN_POINT('Ctrl Pts',(-44.7947479986672,-57.9061820008563,
-41.5236391765087));
#269104=CARTESIAN_POINT('Ctrl Pts',(-44.7832945060713,-57.9150388128137,
-41.5224889540588));
#269105=CARTESIAN_POINT('Ctrl Pts',(-44.7657408175914,-57.9279147771907,
-41.5204166102647));
#269106=CARTESIAN_POINT('Ctrl Pts',(-44.7598217545323,-57.9321421746299,
-41.5196671186517));
#269107=CARTESIAN_POINT('Ctrl Pts',(-44.7478629508254,-57.9404557426351,
-41.5180519716851));
#269108=CARTESIAN_POINT('Ctrl Pts',(-44.7297025277655,-57.9527400844071,
-41.5154481926132));
#269109=CARTESIAN_POINT('Ctrl Pts',(-44.711220794734,-57.9642369190977,
-41.5123523449538));
#269110=CARTESIAN_POINT('Ctrl Pts',(-44.6862770262529,-57.9788987855805,
-41.5077941640223));
#269111=CARTESIAN_POINT('Ctrl Pts',(-44.6484202704456,-57.9998814948776,
-41.5003121274858));
#269112=CARTESIAN_POINT('Ctrl Pts',(-44.5962108390282,-58.0238874022289,
-41.4877980263462));
#269113=CARTESIAN_POINT('Ctrl Pts',(-44.5557649369164,-58.0389385823793,
-41.4765186283493));
#269114=CARTESIAN_POINT('Ctrl Pts',(-44.5285120653069,-58.048310487242,
-41.4685735203231));
#269115=CARTESIAN_POINT('Ctrl Pts',(-44.5147341086114,-58.0526671867402,
-41.4643859028639));
#269116=CARTESIAN_POINT('Ctrl Pts',(-44.4869140318333,-58.0607029371288,
-41.4555883503401));
#269117=CARTESIAN_POINT('Ctrl Pts',(-44.4728027150897,-58.0643973546439,
-41.4509544537452));
#269118=CARTESIAN_POINT('Ctrl Pts',(-44.4304531283686,-58.0743536715507,
-41.4365378845966));
#269119=CARTESIAN_POINT('Ctrl Pts',(-44.3879697631396,-58.0821103913619,
-41.4210702443308));
#269120=CARTESIAN_POINT('Ctrl Pts',(-44.3452880889881,-58.0866896268435,
-41.4040725286766));
#269121=CARTESIAN_POINT('Ctrl Pts',(-44.3025416355467,-58.090217180745,
-41.3865671155567));
#269122=CARTESIAN_POINT('Ctrl Pts',(-44.2739489581488,-58.0911687787978,
-41.3742170239002));
#269123=CARTESIAN_POINT('Ctrl Pts',(-44.2309555122234,-58.090491506171,
-41.3546803180427));
#269124=CARTESIAN_POINT('Ctrl Pts',(-44.2165895018292,-58.0899123697243,
-41.347990487553));
#269125=CARTESIAN_POINT('Ctrl Pts',(-44.1950278537333,-58.0885113544661,
-41.337705180963));
#269126=CARTESIAN_POINT('Ctrl Pts',(-44.1878319550126,-58.0879547296283,
-41.3342316293533));
#269127=CARTESIAN_POINT('Ctrl Pts',(-44.1734279164018,-58.0866616594573,
-41.3271961709002));
#269128=CARTESIAN_POINT('Ctrl Pts',(-44.1662260389348,-58.0859253983809,
-41.3236371482021));
#269129=CARTESIAN_POINT('Ctrl Pts',(-44.130389101081,-58.0818150523559,
-41.3057210105631));
#269130=CARTESIAN_POINT('Ctrl Pts',(-44.073848260417,-58.0724828543971,
-41.2761395013722));
#269131=CARTESIAN_POINT('Ctrl Pts',(-44.0188545174212,-58.0578491440998,
-41.2447838757269));
#269132=CARTESIAN_POINT('Ctrl Pts',(-43.9646246641704,-58.0405931079736,
-41.2125419608827));
#269133=CARTESIAN_POINT('Ctrl Pts',(-43.9378880325505,-58.0306505669816,
-41.1959746665064));
#269134=CARTESIAN_POINT('Ctrl Pts',(-43.9049634769563,-58.0165631445999,
-41.174705886574));
#269135=CARTESIAN_POINT('Ctrl Pts',(-43.898399460067,-58.0136596367661,
-41.1704209658528));
#269136=CARTESIAN_POINT('Ctrl Pts',(-43.8853286348063,-58.0076886655405,
-41.1617993561325));
#269137=CARTESIAN_POINT('Ctrl Pts',(-43.8788088737381,-58.0046144513738,
-41.157453730181));
#269138=CARTESIAN_POINT('Ctrl Pts',(-43.8593967360427,-57.9951717320096,
-41.1443784829743));
#269139=CARTESIAN_POINT('Ctrl Pts',(-43.8466719188398,-57.9885954718361,
-41.1356253645631));
#269140=CARTESIAN_POINT('Ctrl Pts',(-43.8341420587998,-57.9817357678076,
-41.1268248734572));
#269141=CARTESIAN_POINT('Ctrl Pts',(-46.6981266849492,30.7091523375488,
-39.2904704603133));
#269142=CARTESIAN_POINT('Ctrl Pts',(-46.6835475486277,30.6747783378881,
-39.2819613777041));
#269143=CARTESIAN_POINT('Ctrl Pts',(-46.6681814960651,30.6408774263401,
-39.2733909118473));
#269144=CARTESIAN_POINT('Ctrl Pts',(-46.6359019229579,30.57400615396,-39.2561284882363));
#269145=CARTESIAN_POINT('Ctrl Pts',(-46.618988316466,30.5410358444554,-39.2474365250187));
#269146=CARTESIAN_POINT('Ctrl Pts',(-46.5659489383047,30.443507428437,-39.2211791249421));
#269147=CARTESIAN_POINT('Ctrl Pts',(-46.5275294393937,30.3803289376591,
-39.2034325264408));
#269148=CARTESIAN_POINT('Ctrl Pts',(-46.4653031952286,30.2883271671429,
-39.1764461222039));
#269149=CARTESIAN_POINT('Ctrl Pts',(-46.4437937583117,30.2581216171786,
-39.1673894861782));
#269150=CARTESIAN_POINT('Ctrl Pts',(-46.3992224148768,30.1986447451181,
-39.1491520227249));
#269151=CARTESIAN_POINT('Ctrl Pts',(-46.3761748773305,30.1693908446446,
-39.1399767764946));
#269152=CARTESIAN_POINT('Ctrl Pts',(-46.3284414024809,30.1117648114072,
-39.1214771434543));
#269153=CARTESIAN_POINT('Ctrl Pts',(-46.3038983378397,30.083571828401,-39.112209259666));
#269154=CARTESIAN_POINT('Ctrl Pts',(-46.2537073876081,30.0286632749651,
-39.0937226519629));
#269155=CARTESIAN_POINT('Ctrl Pts',(-46.2280147026909,30.001893564456,-39.0844865568113));
#269156=CARTESIAN_POINT('Ctrl Pts',(-46.1492148010453,29.9236586721517,
-39.0568159196779));
#269157=CARTESIAN_POINT('Ctrl Pts',(-46.0943603797766,29.8742287883655,
-39.0384077341064));
#269158=CARTESIAN_POINT('Ctrl Pts',(-46.0086385356025,29.8041510538917,
-39.0108577119752));
#269159=CARTESIAN_POINT('Ctrl Pts',(-45.979489670606,29.7814700298992,-39.0016845404958));
#269160=CARTESIAN_POINT('Ctrl Pts',(-45.9200349130685,29.737472830651,-38.9833588596733));
#269161=CARTESIAN_POINT('Ctrl Pts',(-45.8897290709698,29.7161565962466,
-38.9742063485759));
#269162=CARTESIAN_POINT('Ctrl Pts',(-45.8279451173857,29.6749068346782,
-38.9559225627414));
#269163=CARTESIAN_POINT('Ctrl Pts',(-45.7964751089327,29.6549785818455,
-38.9467936623891));
#269164=CARTESIAN_POINT('Ctrl Pts',(-45.748348603817,29.6261284949947,-38.9331097524421));
#269165=CARTESIAN_POINT('Ctrl Pts',(-45.7321473284057,29.616684052073,-38.9285487676402));
#269166=CARTESIAN_POINT('Ctrl Pts',(-45.6996106203311,29.5982459977232,
-38.9194791520014));
#269167=CARTESIAN_POINT('Ctrl Pts',(-45.683249044345,29.5892352448745,-38.9149628379355));
#269168=CARTESIAN_POINT('Ctrl Pts',(-45.6010439155842,29.5452684013657,
-38.8924942188443));
#269169=CARTESIAN_POINT('Ctrl Pts',(-45.5339074995994,29.5134615304068,
-38.8748432972593));
#269170=CARTESIAN_POINT('Ctrl Pts',(-45.3969715882024,29.4565064940367,
-38.840197135303));
#269171=CARTESIAN_POINT('Ctrl Pts',(-45.3271662939831,29.4313508132015,
-38.823199542964));
#269172=CARTESIAN_POINT('Ctrl Pts',(-45.2204298442793,29.398652641048,-38.7982016720699));
#269173=CARTESIAN_POINT('Ctrl Pts',(-45.184512437616,29.3885937253944,-38.7899522655792));
#269174=CARTESIAN_POINT('Ctrl Pts',(-45.1119891467798,29.3701842541612,
-38.7736235920333));
#269175=CARTESIAN_POINT('Ctrl Pts',(-45.0754052578815,29.3618381514785,
-38.7655490803555));
#269176=CARTESIAN_POINT('Ctrl Pts',(-45.0014447932704,29.3468760834355,
-38.7495561846596));
#269177=CARTESIAN_POINT('Ctrl Pts',(-44.964301863367,29.3403115562353,-38.7416890516424));
#269178=CARTESIAN_POINT('Ctrl Pts',(-44.8900079594565,29.3290481892184,
-38.726277749838));
#269179=CARTESIAN_POINT('Ctrl Pts',(-44.8527936282157,29.324336495618,-38.7187198739728));
#269180=CARTESIAN_POINT('Ctrl Pts',(-44.7410083373266,29.3129455735289,
-38.6964994820139));
#269181=CARTESIAN_POINT('Ctrl Pts',(-44.6662563757167,29.3089967422249,
-38.6822807693139));
#269182=CARTESIAN_POINT('Ctrl Pts',(-44.516312468428,29.3084067934202,-38.6550493453909));
#269183=CARTESIAN_POINT('Ctrl Pts',(-44.441103189525,29.3117700143417,-38.6420342479066));
#269184=CARTESIAN_POINT('Ctrl Pts',(-44.3468378615956,29.3206690055189,
-38.6265520162729));
#269185=CARTESIAN_POINT('Ctrl Pts',(-44.3279589148655,29.3226883315868,
-38.6234933649988));
#269186=CARTESIAN_POINT('Ctrl Pts',(-44.2901960653061,29.3271995080041,
-38.6174591262491));
#269187=CARTESIAN_POINT('Ctrl Pts',(-44.2712743932921,29.329697893027,-38.614477863833));
#269188=CARTESIAN_POINT('Ctrl Pts',(-44.2146592782018,29.3378915995821,
-38.60568558559));
#269189=CARTESIAN_POINT('Ctrl Pts',(-44.1772069502033,29.344266758826,-38.6000392683017));
#269190=CARTESIAN_POINT('Ctrl Pts',(-44.1027653084072,29.3588321594788,
-38.5891549147378));
#269191=CARTESIAN_POINT('Ctrl Pts',(-44.0657945489017,29.3670194960673,
-38.5839197203675));
#269192=CARTESIAN_POINT('Ctrl Pts',(-43.9923490656542,29.3851892021794,
-38.5738612453122));
#269193=CARTESIAN_POINT('Ctrl Pts',(-43.9558743463703,29.395171587473,-38.5690379674556));
#269194=CARTESIAN_POINT('Ctrl Pts',(-43.8834205276403,29.4169303996784,
-38.5598042480103));
#269195=CARTESIAN_POINT('Ctrl Pts',(-43.8474414251675,29.4287068153425,
-38.5553938031715));
#269196=CARTESIAN_POINT('Ctrl Pts',(-43.7759820586595,29.4540658195324,
-38.5469896320335));
#269197=CARTESIAN_POINT('Ctrl Pts',(-43.7405017838471,29.467648368817,-38.5429958961485));
#269198=CARTESIAN_POINT('Ctrl Pts',(-43.6700470477634,29.4966453401303,
-38.5354320983078));
#269199=CARTESIAN_POINT('Ctrl Pts',(-43.6350719757086,29.512061063653,-38.5318621614261));
#269200=CARTESIAN_POINT('Ctrl Pts',(-43.5656410085295,29.5447591316771,
-38.525155654825));
#269201=CARTESIAN_POINT('Ctrl Pts',(-43.5311320054746,29.5620794464364,
-38.5220163122062));
#269202=CARTESIAN_POINT('Ctrl Pts',(-43.4634866412135,29.5981758355574,
-38.5162526847879));
#269203=CARTESIAN_POINT('Ctrl Pts',(-43.4301834663391,29.6170276546,-38.5136117755133));
#269204=CARTESIAN_POINT('Ctrl Pts',(-43.3647025891651,29.6562685687332,
-38.5088155315793));
#269205=CARTESIAN_POINT('Ctrl Pts',(-43.3325078231767,29.6766655539003,
-38.5066585209069));
#269206=CARTESIAN_POINT('Ctrl Pts',(-43.2375484321327,29.7401688861791,
-38.5009063965958));
#269207=CARTESIAN_POINT('Ctrl Pts',(-43.1764049274077,29.7855824582168,
-38.4980286134812));
#269208=CARTESIAN_POINT('Ctrl Pts',(-43.0584774180437,29.8826126224142,
-38.4942050936184));
#269209=CARTESIAN_POINT('Ctrl Pts',(-43.001681818637,29.9342392650769,-38.4932590761897));
#269210=CARTESIAN_POINT('Ctrl Pts',(-42.8926599718677,30.0438904492243,
-38.4933742455196));
#269211=CARTESIAN_POINT('Ctrl Pts',(-42.8414047150844,30.1009342501745,
-38.4944336470273));
#269212=CARTESIAN_POINT('Ctrl Pts',(-42.7451036203247,30.2193471227021,
-38.498479276642));
#269213=CARTESIAN_POINT('Ctrl Pts',(-42.7000684110598,30.2807072617414,
-38.5014658126213));
#269214=CARTESIAN_POINT('Ctrl Pts',(-42.6161769337401,30.4076992015223,
-38.5093469123445));
#269215=CARTESIAN_POINT('Ctrl Pts',(-42.5773225406026,30.4733365238586,
-38.5142428327574));
#269216=CARTESIAN_POINT('Ctrl Pts',(-42.5326943378214,30.5580963840027,
-38.5215739479982));
#269217=CARTESIAN_POINT('Ctrl Pts',(-42.5239673850246,30.5751883092729,
-38.5231018165939));
#269218=CARTESIAN_POINT('Ctrl Pts',(-42.5069121510755,30.60964376351,-38.5262794637242));
#269219=CARTESIAN_POINT('Ctrl Pts',(-42.4985805781952,30.627019094627,-38.5279307934181));
#269220=CARTESIAN_POINT('Ctrl Pts',(-42.4743295471271,30.6792614198295,
-38.5330409224498));
#269221=CARTESIAN_POINT('Ctrl Pts',(-42.4591078049536,30.7143247172706,
-38.5366620777082));
#269222=CARTESIAN_POINT('Ctrl Pts',(-42.4305062721789,30.7849297925434,
-38.5443248028235));
#269223=CARTESIAN_POINT('Ctrl Pts',(-42.4171273618354,30.8204683264523,
-38.5483659418649));
#269224=CARTESIAN_POINT('Ctrl Pts',(-42.3921837112499,30.89200995013,-38.556860031436));
#269225=CARTESIAN_POINT('Ctrl Pts',(-42.3806190180342,30.9280130518798,
-38.5613129931637));
#269226=CARTESIAN_POINT('Ctrl Pts',(-42.3592881563091,31.0004799414626,
-38.5706260903895));
#269227=CARTESIAN_POINT('Ctrl Pts',(-42.3495220063211,31.0369437339595,
-38.5754862307243));
#269228=CARTESIAN_POINT('Ctrl Pts',(-42.3317857495347,31.1103315158532,
-38.5856119737634));
#269229=CARTESIAN_POINT('Ctrl Pts',(-42.3238156343608,31.1472555030051,
-38.5908775753381));
#269230=CARTESIAN_POINT('Ctrl Pts',(-42.3096820427396,31.2215665449467,
-38.6018154236264));
#269231=CARTESIAN_POINT('Ctrl Pts',(-42.3035171869091,31.2589715314082,
-38.6074906718877));
#269232=CARTESIAN_POINT('Ctrl Pts',(-42.2930235524414,31.3341791410138,
-38.6192399292287));
#269233=CARTESIAN_POINT('Ctrl Pts',(-42.2886818075092,31.3721585359098,
-38.6253436316658));
#269234=CARTESIAN_POINT('Ctrl Pts',(-42.2819306306109,31.4478003630713,
-38.6378362101326));
#269235=CARTESIAN_POINT('Ctrl Pts',(-42.2795025237186,31.4855414978569,
-38.6442360129219));
#269236=CARTESIAN_POINT('Ctrl Pts',(-42.2765060643256,31.5608485897329,
-38.6573322722499));
#269237=CARTESIAN_POINT('Ctrl Pts',(-42.2759365563455,31.5984178297074,
-38.6640291190605));
#269238=CARTESIAN_POINT('Ctrl Pts',(-42.2769710616629,31.710876916496,-38.6845570305479));
#269239=CARTESIAN_POINT('Ctrl Pts',(-42.2813124759152,31.7855186400122,
-38.698824567557));
#269240=CARTESIAN_POINT('Ctrl Pts',(-42.2932531103751,31.8969906134966,
-38.7210841829084));
#269241=CARTESIAN_POINT('Ctrl Pts',(-42.2981395950573,31.934066030451,-38.7286473545921));
#269242=CARTESIAN_POINT('Ctrl Pts',(-42.3097367777483,32.0080522284017,
-38.7440609732535));
#269243=CARTESIAN_POINT('Ctrl Pts',(-42.3164494406915,32.0449687602613,
-38.7519128032936));
#269244=CARTESIAN_POINT('Ctrl Pts',(-42.3317154579634,32.1186122141692,
-38.7679009120377));
#269245=CARTESIAN_POINT('Ctrl Pts',(-42.3402956643805,32.1554227583218,
-38.7760569897633));
#269246=CARTESIAN_POINT('Ctrl Pts',(-42.3591481714288,32.228169160774,-38.7925026060078));
#269247=CARTESIAN_POINT('Ctrl Pts',(-42.3694448348212,32.2642362896146,
-38.8008201507359));
#269248=CARTESIAN_POINT('Ctrl Pts',(-42.391742799968,32.3356900672865,-38.817625053217));
#269249=CARTESIAN_POINT('Ctrl Pts',(-42.4037465150873,32.3710895326604,
-38.8261151521117));
#269250=CARTESIAN_POINT('Ctrl Pts',(-42.4294540540394,32.4412374294065,
-38.843268788153));
#269251=CARTESIAN_POINT('Ctrl Pts',(-42.4431578847231,32.4759858579934,
-38.8519323266271));
#269252=CARTESIAN_POINT('Ctrl Pts',(-42.4577131944628,32.5104083279579,
-38.8606823233885));
#269253=CARTESIAN_POINT('Ctrl Pts',(-46.348736272544,30.7584582252104,-39.6906856150703));
#269254=CARTESIAN_POINT('Ctrl Pts',(-46.3360470969151,30.7285883901681,
-39.6821765324611));
#269255=CARTESIAN_POINT('Ctrl Pts',(-46.3226745755283,30.699129013129,-39.6736060666043));
#269256=CARTESIAN_POINT('Ctrl Pts',(-46.2945857386662,30.6410176089828,
-39.6563436429933));
#269257=CARTESIAN_POINT('Ctrl Pts',(-46.2798693485556,30.6123656264171,
-39.6476516797756));
#269258=CARTESIAN_POINT('Ctrl Pts',(-46.2337241557402,30.5276091385302,
-39.6213942796991));
#269259=CARTESIAN_POINT('Ctrl Pts',(-46.2003035256421,30.4727015800282,
-39.6036476811977));
#269260=CARTESIAN_POINT('Ctrl Pts',(-46.1461806704985,30.3927399191851,
-39.5766612769609));
#269261=CARTESIAN_POINT('Ctrl Pts',(-46.1274733675407,30.3664865966257,
-39.5676046409352));
#269262=CARTESIAN_POINT('Ctrl Pts',(-46.0887106443918,30.3147904520985,
-39.549367177482));
#269263=CARTESIAN_POINT('Ctrl Pts',(-46.0686677193846,30.2893627735597,
-39.5401919312515));
#269264=CARTESIAN_POINT('Ctrl Pts',(-46.0271590696364,30.2392722779402,
-39.5216922982112));
#269265=CARTESIAN_POINT('Ctrl Pts',(-46.0058175903831,30.2147651800999,
-39.512424414423));
#269266=CARTESIAN_POINT('Ctrl Pts',(-45.9621758028444,30.1670336173528,
-39.4939378067199));
#269267=CARTESIAN_POINT('Ctrl Pts',(-45.93983653738,30.1437620920995,-39.4847017115683));
#269268=CARTESIAN_POINT('Ctrl Pts',(-45.8713242771536,30.0757481602649,
-39.4570310744349));
#269269=CARTESIAN_POINT('Ctrl Pts',(-45.8236347617589,30.0327725532112,
-39.4386228888633));
#269270=CARTESIAN_POINT('Ctrl Pts',(-45.7491145832093,29.9718396783148,
-39.4110728667323));
#269271=CARTESIAN_POINT('Ctrl Pts',(-45.7237755280245,29.952117465038,-39.4018996952527));
#269272=CARTESIAN_POINT('Ctrl Pts',(-45.6720931922673,29.9138578177121,
-39.3835740144303));
#269273=CARTESIAN_POINT('Ctrl Pts',(-45.6457499554623,29.8953203323242,
-39.3744215033328));
#269274=CARTESIAN_POINT('Ctrl Pts',(-45.5920460375509,29.8594456348434,
-39.3561377174984));
#269275=CARTESIAN_POINT('Ctrl Pts',(-45.5646923996724,29.8421130099496,
-39.347008817146));
#269276=CARTESIAN_POINT('Ctrl Pts',(-45.5228621313133,29.817018813152,-39.333324907199));
#269277=CARTESIAN_POINT('Ctrl Pts',(-45.5087806057656,29.8088035965387,
-39.3287639223973));
#269278=CARTESIAN_POINT('Ctrl Pts',(-45.4805013249128,29.7927646822922,
-39.3196943067583));
#269279=CARTESIAN_POINT('Ctrl Pts',(-45.4662808454981,29.7849260765311,
-39.3151779926924));
#269280=CARTESIAN_POINT('Ctrl Pts',(-45.394834111845,29.7466769167217,-39.2927093736018));
#269281=CARTESIAN_POINT('Ctrl Pts',(-45.3364869241018,29.7190010072829,
-39.2750584520161));
#269282=CARTESIAN_POINT('Ctrl Pts',(-45.2174838212522,29.6694313228168,
-39.24041229006));
#269283=CARTESIAN_POINT('Ctrl Pts',(-45.1568228629401,29.6475310155415,
-39.223414697721));
#269284=CARTESIAN_POINT('Ctrl Pts',(-45.0640728677801,29.6190530040921,
-39.1984168268269));
#269285=CARTESIAN_POINT('Ctrl Pts',(-45.0328626716162,29.6102901609231,
-39.1901674203362));
#269286=CARTESIAN_POINT('Ctrl Pts',(-44.9698454327154,29.5942479284802,
-39.1738387467903));
#269287=CARTESIAN_POINT('Ctrl Pts',(-44.9380575013641,29.5869724226462,
-39.1657642351124));
#269288=CARTESIAN_POINT('Ctrl Pts',(-44.873794287365,29.5739237069059,-39.1497713394166));
#269289=CARTESIAN_POINT('Ctrl Pts',(-44.8415220194395,29.5681953426883,
-39.1419042063994));
#269290=CARTESIAN_POINT('Ctrl Pts',(-44.7769718892781,29.5583592071516,
-39.126492904595));
#269291=CARTESIAN_POINT('Ctrl Pts',(-44.7446389767916,29.5542402259256,
-39.1189350287298));
#269292=CARTESIAN_POINT('Ctrl Pts',(-44.64751868345,29.5442668522271,-39.0967146367708));
#269293=CARTESIAN_POINT('Ctrl Pts',(-44.5825761125008,29.5407840481455,
-39.0824959240709));
#269294=CARTESIAN_POINT('Ctrl Pts',(-44.4523142911657,29.540165884783,-39.055264500148));
#269295=CARTESIAN_POINT('Ctrl Pts',(-44.386979986101,29.5430342817064,-39.0422494026637));
#269296=CARTESIAN_POINT('Ctrl Pts',(-44.3050952734897,29.5506978499007,
-39.0267671710297));
#269297=CARTESIAN_POINT('Ctrl Pts',(-44.288696030367,29.5524386096434,-39.0237085197559));
#269298=CARTESIAN_POINT('Ctrl Pts',(-44.2558936005359,29.556330581768,-39.017674281006));
#269299=CARTESIAN_POINT('Ctrl Pts',(-44.2394576074491,29.5584874438222,
-39.01469301859));
#269300=CARTESIAN_POINT('Ctrl Pts',(-44.1902803880436,29.5655649308415,
-39.0059007403469));
#269301=CARTESIAN_POINT('Ctrl Pts',(-44.1577491481311,29.5710762653616,
-39.0002544230587));
#269302=CARTESIAN_POINT('Ctrl Pts',(-44.0930902993264,29.5836759361658,
-38.9893700694948));
#269303=CARTESIAN_POINT('Ctrl Pts',(-44.0609788069576,29.5907617622781,
-38.9841348751245));
#269304=CARTESIAN_POINT('Ctrl Pts',(-43.9971881260961,29.6064930329024,
-38.9740764000692));
#269305=CARTESIAN_POINT('Ctrl Pts',(-43.9655089414875,29.6151384911107,
-38.9692531222126));
#269306=CARTESIAN_POINT('Ctrl Pts',(-43.9025825141023,29.6339881744307,
-38.9600194027673));
#269307=CARTESIAN_POINT('Ctrl Pts',(-43.8713352686894,29.644192389763,-38.9556089579285));
#269308=CARTESIAN_POINT('Ctrl Pts',(-43.8092755239302,29.666170138253,-38.9472047867905));
#269309=CARTESIAN_POINT('Ctrl Pts',(-43.7784630151957,29.6779436373071,
-38.9432110509055));
#269310=CARTESIAN_POINT('Ctrl Pts',(-43.7172788205642,29.7030822942954,
-38.9356472530647));
#269311=CARTESIAN_POINT('Ctrl Pts',(-43.68690660506,29.7164485823689,-38.9320773161832));
#269312=CARTESIAN_POINT('Ctrl Pts',(-43.6266146289649,29.7448030239206,
-38.9253708095819));
#269313=CARTESIAN_POINT('Ctrl Pts',(-43.5966487607817,29.7598241234161,
-38.9222314669632));
#269314=CARTESIAN_POINT('Ctrl Pts',(-43.5379105932515,29.7911319045234,
-38.9164678395448));
#269315=CARTESIAN_POINT('Ctrl Pts',(-43.5089934352673,29.8074842645775,
-38.9138269302702));
#269316=CARTESIAN_POINT('Ctrl Pts',(-43.4521380201768,29.8415252139572,
-38.9090306863362));
#269317=CARTESIAN_POINT('Ctrl Pts',(-43.4241849453146,29.8592206450036,
-38.9068736756639));
#269318=CARTESIAN_POINT('Ctrl Pts',(-43.3417390736822,29.9143168693475,
-38.9011215513527));
#269319=CARTESIAN_POINT('Ctrl Pts',(-43.2886563370204,29.9537231156165,
-38.8982437682382));
#269320=CARTESIAN_POINT('Ctrl Pts',(-43.1862827102732,30.0379274090563,
-38.8944202483754));
#269321=CARTESIAN_POINT('Ctrl Pts',(-43.1369817552336,30.0827341785328,
-38.8934742309467));
#269322=CARTESIAN_POINT('Ctrl Pts',(-43.0423540539346,30.1779090615142,
-38.8935894002766));
#269323=CARTESIAN_POINT('Ctrl Pts',(-42.9978700944569,30.2274259110637,
-38.8946488017843));
#269324=CARTESIAN_POINT('Ctrl Pts',(-42.9142995039568,30.330221730441,-38.898694431399));
#269325=CARTESIAN_POINT('Ctrl Pts',(-42.8752220997707,30.3834929481532,
-38.9016809673782));
#269326=CARTESIAN_POINT('Ctrl Pts',(-42.802438005755,30.4937509787714,-38.9095620671015));
#269327=CARTESIAN_POINT('Ctrl Pts',(-42.7687329487861,30.5507425897786,
-38.9144579875143));
#269328=CARTESIAN_POINT('Ctrl Pts',(-42.7300260074317,30.6243421619354,
-38.9217891027552));
#269329=CARTESIAN_POINT('Ctrl Pts',(-42.7224573165159,30.6391838099202,
-38.9233169713508));
#269330=CARTESIAN_POINT('Ctrl Pts',(-42.7076664478388,30.6691033617142,
-38.9264946184813));
#269331=CARTESIAN_POINT('Ctrl Pts',(-42.7004414190611,30.6841915159301,
-38.9281459481751));
#269332=CARTESIAN_POINT('Ctrl Pts',(-42.6794124410656,30.7295576092503,
-38.9332560772068));
#269333=CARTESIAN_POINT('Ctrl Pts',(-42.6662147228328,30.7600066178112,
-38.9368772324651));
#269334=CARTESIAN_POINT('Ctrl Pts',(-42.6414196796479,30.8213217206122,
-38.9445399575806));
#269335=CARTESIAN_POINT('Ctrl Pts',(-42.6298231170419,30.8521849974158,
-38.9485810966219));
#269336=CARTESIAN_POINT('Ctrl Pts',(-42.6082062309801,30.9143165209769,
-38.9570751861931));
#269337=CARTESIAN_POINT('Ctrl Pts',(-42.5981859483915,30.9455847781742,
-38.9615281479207));
#269338=CARTESIAN_POINT('Ctrl Pts',(-42.5797080184842,31.0085228897363,
-38.9708412451465));
#269339=CARTESIAN_POINT('Ctrl Pts',(-42.5712503872647,31.040192748165,-38.9757013854813));
#269340=CARTESIAN_POINT('Ctrl Pts',(-42.555895594383,31.1039336351222,-38.9858271285205));
#269341=CARTESIAN_POINT('Ctrl Pts',(-42.5489984254493,31.1360046616943,
-38.9910927300951));
#269342=CARTESIAN_POINT('Ctrl Pts',(-42.5367737540442,31.2005503855788,
-39.0020305783833));
#269343=CARTESIAN_POINT('Ctrl Pts',(-42.5314450660311,31.2330406596962,
-39.0077058266447));
#269344=CARTESIAN_POINT('Ctrl Pts',(-42.5223828738566,31.2983680565044,
-39.0194550839858));
#269345=CARTESIAN_POINT('Ctrl Pts',(-42.5186382312793,31.3313587369558,
-39.0255587864228));
#269346=CARTESIAN_POINT('Ctrl Pts',(-42.5128272133948,31.3970662193109,
-39.0380513648896));
#269347=CARTESIAN_POINT('Ctrl Pts',(-42.5107446717144,31.4298513784848,
-39.0444511676788));
#269348=CARTESIAN_POINT('Ctrl Pts',(-42.5081949220986,31.4952709313388,
-39.0575474270069));
#269349=CARTESIAN_POINT('Ctrl Pts',(-42.5077267127911,31.5279081760849,
-39.0642442738175));
#269350=CARTESIAN_POINT('Ctrl Pts',(-42.5087046075987,31.6256059960414,
-39.0847721853048));
#269351=CARTESIAN_POINT('Ctrl Pts',(-42.5125283453785,31.6904530960276,
-39.099039722314));
#269352=CARTESIAN_POINT('Ctrl Pts',(-42.5229789971415,31.7873016127624,
-39.1212993376654));
#269353=CARTESIAN_POINT('Ctrl Pts',(-42.5272497098319,31.8195139765299,
-39.128862509349));
#269354=CARTESIAN_POINT('Ctrl Pts',(-42.5373755918422,31.8837970410461,
-39.1442761280104));
#269355=CARTESIAN_POINT('Ctrl Pts',(-42.5432324720224,31.9158727392425,
-39.1521279580505));
#269356=CARTESIAN_POINT('Ctrl Pts',(-42.5565449846397,31.9798607801841,
-39.1681160667947));
#269357=CARTESIAN_POINT('Ctrl Pts',(-42.5640240006773,32.0118457883453,
-39.1762721445204));
#269358=CARTESIAN_POINT('Ctrl Pts',(-42.5804512263956,32.0750571790556,
-39.1927177607647));
#269359=CARTESIAN_POINT('Ctrl Pts',(-42.5894206909713,32.1063976191197,
-39.2010353054929));
#269360=CARTESIAN_POINT('Ctrl Pts',(-42.6088398491466,32.1684885866316,
-39.2178402079739));
#269361=CARTESIAN_POINT('Ctrl Pts',(-42.6192916481159,32.1992502500668,
-39.2263303068687));
#269362=CARTESIAN_POINT('Ctrl Pts',(-42.6416715644566,32.2602092315461,
-39.2434839429101));
#269363=CARTESIAN_POINT('Ctrl Pts',(-42.6535996877758,32.290406547182,-39.252147481384));
#269364=CARTESIAN_POINT('Ctrl Pts',(-42.6662672096695,32.3203213022051,
-39.2608974781455));
#269365=CARTESIAN_POINT('Ctrl Pts',(-42.5264432849996,31.269119253141,-39.0141952505087));
#269366=CARTESIAN_POINT('Ctrl Pts',(-42.5221224658057,31.3006702972118,
-39.0198812138034));
#269367=CARTESIAN_POINT('Ctrl Pts',(-42.5185368438515,31.3325051647859,
-39.0257767500263));
#269368=CARTESIAN_POINT('Ctrl Pts',(-42.515732722337,31.3642124781334,-39.0318050756562));
#269369=CARTESIAN_POINT('Ctrl Pts',(-42.5128272155788,31.3970661946154,
-39.0380513601944));
#269370=CARTESIAN_POINT('Ctrl Pts',(-42.5107447016068,31.4298506115284,
-39.0444510141427));
#269371=CARTESIAN_POINT('Ctrl Pts',(-42.5094697969065,31.4625611549118,
-39.0509992973428));
#269372=CARTESIAN_POINT('Ctrl Pts',(-42.508194891176,31.495271724727,-39.0575475858343));
#269373=CARTESIAN_POINT('Ctrl Pts',(-42.5077267152746,31.5279084227224,
-39.0642443261397));
#269374=CARTESIAN_POINT('Ctrl Pts',(-42.5080525657557,31.5604741525115,
-39.0710867176316));
#269375=CARTESIAN_POINT('Ctrl Pts',(-42.5087042669078,31.6256056310615,
-39.0847715046015));
#269376=CARTESIAN_POINT('Ctrl Pts',(-42.5125279911245,31.6904531051536,
-39.0990390579777));
#269377=CARTESIAN_POINT('Ctrl Pts',(-42.5194952327192,31.7550179760245,
-39.1138790580997));
#269378=CARTESIAN_POINT('Ctrl Pts',(-42.5229788523054,31.7873004002368,
-39.1212990555811));
#269379=CARTESIAN_POINT('Ctrl Pts',(-42.5272493642385,31.8195120978489,
-39.1288619647275));
#269380=CARTESIAN_POINT('Ctrl Pts',(-42.5323125754593,31.8516552046985,
-39.1365691980944));
#269381=CARTESIAN_POINT('Ctrl Pts',(-42.5373757866802,31.8837983115481,
-39.1442764314613));
#269382=CARTESIAN_POINT('Ctrl Pts',(-42.5432324720224,31.9158727392424,
-39.1521279580505));
#269383=CARTESIAN_POINT('Ctrl Pts',(-42.5498887283311,31.9478667597133,
-39.1601220124226));
#269384=CARTESIAN_POINT('Ctrl Pts',(-42.5565449846397,31.9798607801841,
-39.1681160667947));
#269385=CARTESIAN_POINT('Ctrl Pts',(-42.5640240006772,32.0118457883453,
-39.1762721445203));
#269386=CARTESIAN_POINT('Ctrl Pts',(-42.5722376135364,32.0434514837005,
-39.1844949526425));
#269387=CARTESIAN_POINT('Ctrl Pts',(-42.5804512263956,32.0750571790557,
-39.1927177607647));
#269388=CARTESIAN_POINT('Ctrl Pts',(-42.5894206909713,32.1063976191197,
-39.2010353054928));
#269389=CARTESIAN_POINT('Ctrl Pts',(-42.599130270059,32.1374431028757,-39.2094377567334));
#269390=CARTESIAN_POINT('Ctrl Pts',(-42.6088398491467,32.1684885866317,
-39.217840207974));
#269391=CARTESIAN_POINT('Ctrl Pts',(-42.619291648116,32.1992502500668,-39.2263303068687));
#269392=CARTESIAN_POINT('Ctrl Pts',(-42.6304816062863,32.2297297408064,
-39.2349071248894));
#269393=CARTESIAN_POINT('Ctrl Pts',(-42.6416715644565,32.2602092315458,
-39.24348394291));
#269394=CARTESIAN_POINT('Ctrl Pts',(-42.6535996877756,32.2904065471814,
-39.2521474813839));
#269395=CARTESIAN_POINT('Ctrl Pts',(-42.6662672096693,32.3203213022045,
-39.2608974781453));
#269396=CARTESIAN_POINT('Ctrl Pts',(-46.348736272544,30.7584582252104,-39.6906856150703));
#269397=CARTESIAN_POINT('Ctrl Pts',(-46.3360470973409,30.7285883911703,
-39.6821765327467));
#269398=CARTESIAN_POINT('Ctrl Pts',(-46.3226745905749,30.6991290109582,
-39.6736060493954));
#269399=CARTESIAN_POINT('Ctrl Pts',(-46.3086301900114,30.670073305053,-39.6649748164403));
#269400=CARTESIAN_POINT('Ctrl Pts',(-46.2945857887134,30.6410175976279,
-39.6563435830337));
#269401=CARTESIAN_POINT('Ctrl Pts',(-46.2798694188995,30.6123656091012,
-39.6476515945533));
#269402=CARTESIAN_POINT('Ctrl Pts',(-46.2644877017587,30.5841134449057,
-39.6388991131053));
#269403=CARTESIAN_POINT('Ctrl Pts',(-46.2337242678266,30.5276091171564,
-39.6213941504079));
#269404=CARTESIAN_POINT('Ctrl Pts',(-46.2003039001332,30.4727015444266,
-39.6036472934442));
#269405=CARTESIAN_POINT('Ctrl Pts',(-46.1642217344127,30.4193937755162,
-39.5856566097807));
#269406=CARTESIAN_POINT('Ctrl Pts',(-46.146180651686,30.3927398912582,-39.5766612680155));
#269407=CARTESIAN_POINT('Ctrl Pts',(-46.1274733675408,30.3664865966258,
-39.5676046409352));
#269408=CARTESIAN_POINT('Ctrl Pts',(-46.1080920059663,30.3406385243622,
-39.5584859092086));
#269409=CARTESIAN_POINT('Ctrl Pts',(-46.0887106443919,30.3147904520986,
-39.5493671774819));
#269410=CARTESIAN_POINT('Ctrl Pts',(-46.0686677193846,30.2893627735597,
-39.5401919312515));
#269411=CARTESIAN_POINT('Ctrl Pts',(-46.0479133945105,30.2643175257499,
-39.5309421147314));
#269412=CARTESIAN_POINT('Ctrl Pts',(-46.0271590696364,30.2392722779402,
-39.5216922982112));
#269413=CARTESIAN_POINT('Ctrl Pts',(-46.0058175903831,30.2147651800999,
-39.512424414423));
#269414=CARTESIAN_POINT('Ctrl Pts',(-45.9839966966138,30.1908993987264,
-39.5031811105714));
#269415=CARTESIAN_POINT('Ctrl Pts',(-45.9621758028444,30.1670336173528,
-39.4939378067199));
#269416=CARTESIAN_POINT('Ctrl Pts',(-45.93983653738,30.1437620920996,-39.4847017115683));
#269417=CARTESIAN_POINT('Ctrl Pts',(-45.9169991173045,30.121090781488,-39.4754781658572));
#269418=CARTESIAN_POINT('Ctrl Pts',(-45.8713242883866,30.0757481714161,
-39.4570310789716));
#269419=CARTESIAN_POINT('Ctrl Pts',(-45.8236354571138,30.0327727895174,
-39.4386227099774));
#269420=CARTESIAN_POINT('Ctrl Pts',(-45.773954719475,29.992150588615,-39.4202560907654));
#269421=CARTESIAN_POINT('Ctrl Pts',(-45.7491145157246,29.971839623135,-39.4110728421843));
#269422=CARTESIAN_POINT('Ctrl Pts',(-45.7237758311101,29.9521176894074,
-39.4018998026794));
#269423=CARTESIAN_POINT('Ctrl Pts',(-45.6979343678929,29.9329876360372,
-39.3927368425297));
#269424=CARTESIAN_POINT('Ctrl Pts',(-45.6720926283413,29.9138573781007,
-39.3835737843965));
#269425=CARTESIAN_POINT('Ctrl Pts',(-45.6457480380852,29.8953190514989,
-39.3744208505476));
#269426=CARTESIAN_POINT('Ctrl Pts',(-45.6188979971575,29.8773829830905,
-39.36527960933));
#269427=CARTESIAN_POINT('Ctrl Pts',(-45.5920479621773,29.859446918655,-39.3561383701372));
#269428=CARTESIAN_POINT('Ctrl Pts',(-45.5646924995279,29.8421130698535,
-39.3470088498117));
#269429=CARTESIAN_POINT('Ctrl Pts',(-45.5368055540997,29.8253835454179,
-39.3378862105147));
#269430=CARTESIAN_POINT('Ctrl Pts',(-45.5228621313133,29.817018813152,-39.3333249071991));
#269431=CARTESIAN_POINT('Ctrl Pts',(-45.5087806057656,29.8088035965387,
-39.3287639223973));
#269432=CARTESIAN_POINT('Ctrl Pts',(-45.4946409653392,29.8007841394154,
-39.3242291145778));
#269433=CARTESIAN_POINT('Ctrl Pts',(-45.4805013249128,29.7927646822922,
-39.3196943067583));
#269434=CARTESIAN_POINT('Ctrl Pts',(-45.4662808454981,29.7849260765311,
-39.3151779926924));
#269435=CARTESIAN_POINT('Ctrl Pts',(-45.4519914987675,29.7772762445693,
-39.3106842688742));
#269436=CARTESIAN_POINT('Ctrl Pts',(-45.3948341399523,29.746676931769,-39.292709382441));
#269437=CARTESIAN_POINT('Ctrl Pts',(-45.3364886465416,29.7190017247075,
-39.2750589508555));
#269438=CARTESIAN_POINT('Ctrl Pts',(-45.276985562247,29.6942159545788,-39.2577349684532));
#269439=CARTESIAN_POINT('Ctrl Pts',(-45.2211882780065,29.6709738205385,
-39.241489908525));
#269440=CARTESIAN_POINT('Ctrl Pts',(-45.1643742277393,29.6502692579128,
-39.2255326383472));
#269441=CARTESIAN_POINT('Ctrl Pts',(-45.1065114146008,29.6321213447558,
-39.209862333485));
#269442=CARTESIAN_POINT('Ctrl Pts',(-46.8777108695604,31.7246583249715,
-39.4968621491069));
#269443=CARTESIAN_POINT('Ctrl Pts',(-46.8781729355344,31.7155928097276,
-39.4953858594052));
#269444=CARTESIAN_POINT('Ctrl Pts',(-46.8785816536823,31.7065201757618,
-39.4938989911198));
#269445=CARTESIAN_POINT('Ctrl Pts',(-46.8796767940079,31.6785286095959,
-39.4892824810203));
#269446=CARTESIAN_POINT('Ctrl Pts',(-46.8801843407089,31.6595724593507,
-39.4861150486293));
#269447=CARTESIAN_POINT('Ctrl Pts',(-46.8807312344332,31.6216180949417,
-39.479690628598));
#269448=CARTESIAN_POINT('Ctrl Pts',(-46.8807699646674,31.6025797052015,
-39.4764266299692));
#269449=CARTESIAN_POINT('Ctrl Pts',(-46.8801790388754,31.5455906639181,
-39.4665317368708));
#269450=CARTESIAN_POINT('Ctrl Pts',(-46.8788490796135,31.5078273383739,
-39.4598096545541));
#269451=CARTESIAN_POINT('Ctrl Pts',(-46.874360617844,31.4326451774338,-39.4461013696832));
#269452=CARTESIAN_POINT('Ctrl Pts',(-46.864884835636,31.320441459725,-39.4251517854185));
#269453=CARTESIAN_POINT('Ctrl Pts',(-46.8414902947658,31.1730719473388,
-39.3956936109857));
#269454=CARTESIAN_POINT('Ctrl Pts',(-46.8074810934279,31.0279105813681,
-39.364717848004));
#269455=CARTESIAN_POINT('Ctrl Pts',(-46.7869180083019,30.9560697433081,
-39.3487190247537));
#269456=CARTESIAN_POINT('Ctrl Pts',(-46.7645577771926,30.884604709384,-39.332461491893));
#269457=CARTESIAN_POINT('Ctrl Pts',(-46.7524740339114,30.8490466969583,
-39.3242001683612));
#269458=CARTESIAN_POINT('Ctrl Pts',(-46.7264943673172,30.7783632715819,
-39.3074248425479));
#269459=CARTESIAN_POINT('Ctrl Pts',(-46.7127058212706,30.7435263372096,
-39.2989795429224));
#269460=CARTESIAN_POINT('Ctrl Pts',(-46.6981266849492,30.7091523375488,
-39.2904704603133));
#269461=CARTESIAN_POINT('Ctrl Pts',(-45.1104359790682,31.3262729516313,
-41.3967784080596));
#269462=CARTESIAN_POINT('Ctrl Pts',(-45.1105813863711,31.3228595121998,
-41.3953021183579));
#269463=CARTESIAN_POINT('Ctrl Pts',(-45.1107066559544,31.3194432352723,
-41.3938152500725));
#269464=CARTESIAN_POINT('Ctrl Pts',(-45.1110306052012,31.30890259785,-41.3891987399731));
#269465=CARTESIAN_POINT('Ctrl Pts',(-45.1111617199316,31.3017636946428,
-41.3860313075819));
#269466=CARTESIAN_POINT('Ctrl Pts',(-45.1112472734604,31.2874686716035,
-41.3796068875509));
#269467=CARTESIAN_POINT('Ctrl Pts',(-45.111201351958,31.2802974166487,-41.3763428889219));
#269468=CARTESIAN_POINT('Ctrl Pts',(-45.1107973541963,31.25882908612,-41.3664479958234));
#269469=CARTESIAN_POINT('Ctrl Pts',(-45.11017580813,31.2446005169708,-41.3597259135069));
#269470=CARTESIAN_POINT('Ctrl Pts',(-45.1082442962718,31.2162677536902,
-41.3460176286356));
#269471=CARTESIAN_POINT('Ctrl Pts',(-45.104314463686,31.1739750543259,-41.3250680443717));
#269472=CARTESIAN_POINT('Ctrl Pts',(-45.0950241996196,31.1183949914011,
-41.295609869938));
#269473=CARTESIAN_POINT('Ctrl Pts',(-45.0817381040079,31.0636149263882,
-41.264634106957));
#269474=CARTESIAN_POINT('Ctrl Pts',(-45.0737554763462,31.0364928582332,
-41.2486352837062));
#269475=CARTESIAN_POINT('Ctrl Pts',(-45.0650963255467,31.0095068957897,
-41.2323777508457));
#269476=CARTESIAN_POINT('Ctrl Pts',(-45.0604265398991,30.996076905732,-41.224116427314));
#269477=CARTESIAN_POINT('Ctrl Pts',(-45.0504049610752,30.9693743366894,
-41.2073411015006));
#269478=CARTESIAN_POINT('Ctrl Pts',(-45.0450945767524,30.9562107421528,
-41.1988958018751));
#269479=CARTESIAN_POINT('Ctrl Pts',(-45.0394875320819,30.9432190801919,
-41.190386719266));
#269480=CARTESIAN_POINT('',(-46.348736272544,30.7584582252104,-39.6906856150703));
#269481=CARTESIAN_POINT('Ctrl Pts',(-46.6981266849492,30.7091523375488,
-39.2904704603133));
#269482=CARTESIAN_POINT('Ctrl Pts',(-46.6689684123063,30.6404043382273,
-39.273452295095));
#269483=CARTESIAN_POINT('Ctrl Pts',(-46.6043681216411,30.5066861069553,
-39.238925705885));
#269484=CARTESIAN_POINT('Ctrl Pts',(-46.5083209189471,30.3487389562033,
-39.1945593129175));
#269485=CARTESIAN_POINT('Ctrl Pts',(-46.4437937583117,30.2581216171786,
-39.1673894861782));
#269486=CARTESIAN_POINT('Ctrl Pts',(-46.3992224148768,30.1986447451181,
-39.1491520227249));
#269487=CARTESIAN_POINT('Ctrl Pts',(-46.3761748773305,30.1693908446446,
-39.1399767764946));
#269488=CARTESIAN_POINT('Ctrl Pts',(-46.3284414024809,30.1117648114071,
-39.1214771434543));
#269489=CARTESIAN_POINT('Ctrl Pts',(-46.3038983378397,30.083571828401,-39.112209259666));
#269490=CARTESIAN_POINT('Ctrl Pts',(-46.253707387608,30.0286632749651,-39.0937226519629));
#269491=CARTESIAN_POINT('Ctrl Pts',(-46.2280147026909,30.001893564456,-39.0844865568113));
#269492=CARTESIAN_POINT('Ctrl Pts',(-46.1492148010453,29.9236586721517,
-39.0568159196779));
#269493=CARTESIAN_POINT('Ctrl Pts',(-46.0669347173688,29.8495134741745,
-39.0292038481275));
#269494=CARTESIAN_POINT('Ctrl Pts',(-45.9503410384262,29.7587889734315,
-38.9925114043613));
#269495=CARTESIAN_POINT('Ctrl Pts',(-45.8594191065401,29.6948377475824,
-38.9650526418885));
#269496=CARTESIAN_POINT('Ctrl Pts',(-45.7964751089327,29.6549785818455,
-38.9467936623891));
#269497=CARTESIAN_POINT('Ctrl Pts',(-45.748348603817,29.6261284949947,-38.9331097524421));
#269498=CARTESIAN_POINT('Ctrl Pts',(-45.7321473284057,29.616684052073,-38.9285487676403));
#269499=CARTESIAN_POINT('Ctrl Pts',(-45.6996106203311,29.5982459977232,
-38.9194791520014));
#269500=CARTESIAN_POINT('Ctrl Pts',(-45.683249044345,29.5892352448745,-38.9149628379356));
#269501=CARTESIAN_POINT('Ctrl Pts',(-45.6010439155842,29.5452684013657,
-38.8924942188443));
#269502=CARTESIAN_POINT('Ctrl Pts',(-45.4667739830181,29.4816584171599,
-38.8571935516581));
#269503=CARTESIAN_POINT('Ctrl Pts',(-45.2922645146651,29.4187721922835,
-38.8147007629208));
#269504=CARTESIAN_POINT('Ctrl Pts',(-45.184512437616,29.3885937253944,-38.7899522655792));
#269505=CARTESIAN_POINT('Ctrl Pts',(-45.1119891467798,29.3701842541612,
-38.7736235920333));
#269506=CARTESIAN_POINT('Ctrl Pts',(-45.0754052578815,29.3618381514785,
-38.7655490803555));
#269507=CARTESIAN_POINT('Ctrl Pts',(-45.0014447932705,29.3468760834356,
-38.7495561846596));
#269508=CARTESIAN_POINT('Ctrl Pts',(-44.964301863367,29.3403115562353,-38.7416890516424));
#269509=CARTESIAN_POINT('Ctrl Pts',(-44.8900079594565,29.3290481892184,
-38.726277749838));
#269510=CARTESIAN_POINT('Ctrl Pts',(-44.8527936282157,29.324336495618,-38.7187198739728));
#269511=CARTESIAN_POINT('Ctrl Pts',(-44.7410083373266,29.3129455735289,
-38.6964994820139));
#269512=CARTESIAN_POINT('Ctrl Pts',(-44.6662563757167,29.3089967422249,
-38.6822807693139));
#269513=CARTESIAN_POINT('Ctrl Pts',(-44.516312468428,29.3084067934202,-38.6550493453909));
#269514=CARTESIAN_POINT('Ctrl Pts',(-44.441103189525,29.3117700143417,-38.6420342479066));
#269515=CARTESIAN_POINT('Ctrl Pts',(-44.3468378615956,29.3206690055189,
-38.6265520162729));
#269516=CARTESIAN_POINT('Ctrl Pts',(-44.3279589148655,29.3226883315868,
-38.6234933649988));
#269517=CARTESIAN_POINT('Ctrl Pts',(-44.2901960653062,29.3271995080042,
-38.6174591262491));
#269518=CARTESIAN_POINT('Ctrl Pts',(-44.271274393292,29.329697893027,-38.614477863833));
#269519=CARTESIAN_POINT('Ctrl Pts',(-44.2146592782019,29.3378915995821,
-38.60568558559));
#269520=CARTESIAN_POINT('Ctrl Pts',(-44.1772069502033,29.344266758826,-38.6000392683017));
#269521=CARTESIAN_POINT('Ctrl Pts',(-44.0655444875092,29.3661148598052,
-38.5837127379559));
#269522=CARTESIAN_POINT('Ctrl Pts',(-43.9553791862171,29.3933792052515,
-38.5686255047386));
#269523=CARTESIAN_POINT('Ctrl Pts',(-43.8114622524781,29.4404829778103,
-38.5509833019505));
#269524=CARTESIAN_POINT('Ctrl Pts',(-43.705021834675,29.481230340464,-38.5390021142185));
#269525=CARTESIAN_POINT('Ctrl Pts',(-43.6350719757086,29.512061063653,-38.5318621614261));
#269526=CARTESIAN_POINT('Ctrl Pts',(-43.5656410085295,29.5447591316771,
-38.525155654825));
#269527=CARTESIAN_POINT('Ctrl Pts',(-43.5311320054746,29.5620794464364,
-38.5220163122062));
#269528=CARTESIAN_POINT('Ctrl Pts',(-43.4634866412134,29.5981758355574,
-38.5162526847879));
#269529=CARTESIAN_POINT('Ctrl Pts',(-43.4301834663392,29.6170276546,-38.5136117755133));
#269530=CARTESIAN_POINT('Ctrl Pts',(-43.3647025891651,29.6562685687332,
-38.5088155315793));
#269531=CARTESIAN_POINT('Ctrl Pts',(-43.2681192378476,29.7174608121974,
-38.5023448938576));
#269532=CARTESIAN_POINT('Ctrl Pts',(-43.1764049274077,29.7855824582168,
-38.4980286134812));
#269533=CARTESIAN_POINT('Ctrl Pts',(-43.0584774180437,29.8826126224142,
-38.4942050936184));
#269534=CARTESIAN_POINT('Ctrl Pts',(-43.001681818637,29.9342392650769,-38.4932590761897));
#269535=CARTESIAN_POINT('Ctrl Pts',(-42.8926599718677,30.0438904492243,
-38.4933742455196));
#269536=CARTESIAN_POINT('Ctrl Pts',(-42.8414047150844,30.1009342501745,
-38.4944336470273));
#269537=CARTESIAN_POINT('Ctrl Pts',(-42.7451036203247,30.2193471227021,
-38.498479276642));
#269538=CARTESIAN_POINT('Ctrl Pts',(-42.6550322643363,30.3420646399833,
-38.5044516702661));
#269539=CARTESIAN_POINT('Ctrl Pts',(-42.5773225406025,30.4733365238586,
-38.5142428327574));
#269540=CARTESIAN_POINT('Ctrl Pts',(-42.5326943378214,30.5580963840027,
-38.5215739479982));
#269541=CARTESIAN_POINT('Ctrl Pts',(-42.5239673850246,30.5751883092729,
-38.5231018165939));
#269542=CARTESIAN_POINT('Ctrl Pts',(-42.5069121510755,30.60964376351,-38.5262794637242));
#269543=CARTESIAN_POINT('Ctrl Pts',(-42.4985805781952,30.627019094627,-38.5279307934181));
#269544=CARTESIAN_POINT('Ctrl Pts',(-42.4743295471271,30.6792614198295,
-38.5330409224498));
#269545=CARTESIAN_POINT('Ctrl Pts',(-42.4438856226513,30.7493896366731,
-38.5402834483744));
#269546=CARTESIAN_POINT('Ctrl Pts',(-42.4037483179465,30.8560072598611,
-38.5524071291592));
#269547=CARTESIAN_POINT('Ctrl Pts',(-42.3690543371876,30.9640160484273,
-38.5657659376104));
#269548=CARTESIAN_POINT('Ctrl Pts',(-42.3397558527982,31.0734075527136,
-38.5803463747351));
#269549=CARTESIAN_POINT('Ctrl Pts',(-42.3238156343608,31.1472555030051,
-38.5908775753381));
#269550=CARTESIAN_POINT('Ctrl Pts',(-42.3096820427396,31.2215665449467,
-38.6018154236264));
#269551=CARTESIAN_POINT('Ctrl Pts',(-42.3035171869091,31.2589715314082,
-38.6074906718877));
#269552=CARTESIAN_POINT('Ctrl Pts',(-42.2930235524414,31.3341791410138,
-38.6192399292287));
#269553=CARTESIAN_POINT('Ctrl Pts',(-42.2886818075092,31.3721585359098,
-38.6253436316658));
#269554=CARTESIAN_POINT('Ctrl Pts',(-42.281930630611,31.4478003630713,-38.6378362101326));
#269555=CARTESIAN_POINT('Ctrl Pts',(-42.277074994566,31.5232809912004,-38.6506356205751));
#269556=CARTESIAN_POINT('Ctrl Pts',(-42.2747992363309,31.6735553614761,
-38.6774229397946));
#269557=CARTESIAN_POINT('Ctrl Pts',(-42.2834818483937,31.8228397562226,
-38.7059581415094));
#269558=CARTESIAN_POINT('Ctrl Pts',(-42.3030248127084,31.9711385758679,
-38.7362097844166));
#269559=CARTESIAN_POINT('Ctrl Pts',(-42.3164494406915,32.0449687602614,
-38.7519128032936));
#269560=CARTESIAN_POINT('Ctrl Pts',(-42.3317154579634,32.1186122141692,
-38.7679009120377));
#269561=CARTESIAN_POINT('Ctrl Pts',(-42.3402956643805,32.1554227583218,
-38.7760569897633));
#269562=CARTESIAN_POINT('Ctrl Pts',(-42.3591481714288,32.228169160774,-38.7925026060078));
#269563=CARTESIAN_POINT('Ctrl Pts',(-42.3694448348212,32.2642362896146,
-38.8008201507359));
#269564=CARTESIAN_POINT('Ctrl Pts',(-42.4028917825415,32.3714169561226,
-38.8260275044574));
#269565=CARTESIAN_POINT('Ctrl Pts',(-42.428602574983,32.4415633880281,-38.8431823298655));
#269566=CARTESIAN_POINT('Ctrl Pts',(-42.4722685042023,32.5448307979217,
-38.8694323201497));
#269567=CARTESIAN_POINT('Ctrl Pts',(-42.4876674804306,32.5789105800712,
-38.8782643966373));
#269568=CARTESIAN_POINT('Ctrl Pts',(-42.5202146590728,32.6464795812123,
-38.8961197808447));
#269569=CARTESIAN_POINT('Ctrl Pts',(-42.5373018269229,32.6798350022668,
-38.9051083126545));
#269570=CARTESIAN_POINT('Ctrl Pts',(-42.5906929412925,32.7780783962456,
-38.9321048428364));
#269571=CARTESIAN_POINT('Ctrl Pts',(-42.629225789877,32.8414173722334,-38.9502105255135));
#269572=CARTESIAN_POINT('Ctrl Pts',(-42.7120000069194,32.9638220552461,
-38.9866125955294));
#269573=CARTESIAN_POINT('Ctrl Pts',(-42.7783647966162,33.0524402968179,
-39.0140612314234));
#269574=CARTESIAN_POINT('Ctrl Pts',(-42.8754380724448,33.1642175243331,
-39.0509520337677));
#269575=CARTESIAN_POINT('Ctrl Pts',(-42.9268673384212,33.2179450225078,
-39.0694937486382));
#269576=CARTESIAN_POINT('Ctrl Pts',(-42.9797817061918,33.2705900457306,
-39.088089881442));
#269577=CARTESIAN_POINT('Ctrl Pts',(-43.0069972096607,33.2963736994336,
-39.097418269769));
#269578=CARTESIAN_POINT('Ctrl Pts',(-43.0622936398443,33.3462615369726,
-39.1159154063528));
#269579=CARTESIAN_POINT('Ctrl Pts',(-43.0904949946047,33.3704876748183,
-39.1251268688783));
#269580=CARTESIAN_POINT('Ctrl Pts',(-43.176562606447,33.4408730143712,-39.1525915568785));
#269581=CARTESIAN_POINT('Ctrl Pts',(-43.2360245534179,33.4848790444095,
-39.1707230137558));
#269582=CARTESIAN_POINT('Ctrl Pts',(-43.358992255749,33.5670176609587,-39.2066046432507));
#269583=CARTESIAN_POINT('Ctrl Pts',(-43.4542745623933,33.6242424638975,
-39.233238623837));
#269584=CARTESIAN_POINT('Ctrl Pts',(-43.5542222374601,33.6747516510336,
-39.2594493821381));
#269585=CARTESIAN_POINT('Ctrl Pts',(-43.6219256430316,33.7069073870393,
-39.2768314299875));
#269586=CARTESIAN_POINT('Ctrl Pts',(-43.6563381479934,33.7222286468184,
-39.2854811722856));
#269587=CARTESIAN_POINT('Ctrl Pts',(-43.7254519170511,33.7509934760635,
-39.3024907499371));
#269588=CARTESIAN_POINT('Ctrl Pts',(-43.7602995448845,33.7645084608315,
-39.3108885064059));
#269589=CARTESIAN_POINT('Ctrl Pts',(-43.8304781084082,33.789780836939,-39.3274499785309));
#269590=CARTESIAN_POINT('Ctrl Pts',(-43.9365171946568,33.8250735562425,
-39.3519527568515));
#269591=CARTESIAN_POINT('Ctrl Pts',(-44.0809642638621,33.8617420360433,
-39.3832806139221));
#269592=CARTESIAN_POINT('Ctrl Pts',(-44.1916183723467,33.8813683146414,
-39.4057679385072));
#269593=CARTESIAN_POINT('Ctrl Pts',(-44.2659122959159,33.8926702964892,
-39.4205323411483));
#269594=CARTESIAN_POINT('Ctrl Pts',(-44.3033049221432,33.8974288658374,
-39.4277978831022));
#269595=CARTESIAN_POINT('Ctrl Pts',(-44.3598453576919,33.9032050944765,
-39.4385322478049));
#269596=CARTESIAN_POINT('Ctrl Pts',(-44.3787527158677,33.9049006163346,
-39.4420799976889));
#269597=CARTESIAN_POINT('Ctrl Pts',(-44.4164967874688,33.9078161173588,
-39.4490791780208));
#269598=CARTESIAN_POINT('Ctrl Pts',(-44.4353708468856,33.9090400957878,
-39.4525377314439));
#269599=CARTESIAN_POINT('Ctrl Pts',(-44.4919347179527,33.9120095261765,
-39.462779235967));
#269600=CARTESIAN_POINT('Ctrl Pts',(-44.52962054914,33.9130584408517,-39.4694384189012));
#269601=CARTESIAN_POINT('Ctrl Pts',(-44.6425299001817,33.9134342925821,
-39.4889026473125));
#269602=CARTESIAN_POINT('Ctrl Pts',(-44.7176656228988,33.9100023852834,
-39.5012068570978));
#269603=CARTESIAN_POINT('Ctrl Pts',(-44.867623327666,33.8957625538083,-39.524471978366));
#269604=CARTESIAN_POINT('Ctrl Pts',(-44.9424659600731,33.8849485744664,
-39.5354353652432));
#269605=CARTESIAN_POINT('Ctrl Pts',(-45.0357885152669,33.8666999843662,
-39.5482785606344));
#269606=CARTESIAN_POINT('Ctrl Pts',(-45.0544546343785,33.8628074782943,
-39.5508053225112));
#269607=CARTESIAN_POINT('Ctrl Pts',(-45.091743102575,33.8545484160302,-39.5557691634051));
#269608=CARTESIAN_POINT('Ctrl Pts',(-45.1104022544846,33.850171655015,-39.5582107864407));
#269609=CARTESIAN_POINT('Ctrl Pts',(-45.1661672125598,33.8363538303533,
-39.5653802281989));
#269610=CARTESIAN_POINT('Ctrl Pts',(-45.2029511118778,33.8262578362557,
-39.5699395109212));
#269611=CARTESIAN_POINT('Ctrl Pts',(-45.312316831343,33.7933159380614,-39.582990524906));
#269612=CARTESIAN_POINT('Ctrl Pts',(-45.4195983160475,33.7551076509549,
-39.5947758536238));
#269613=CARTESIAN_POINT('Ctrl Pts',(-45.5585113890164,33.6937328563153,
-39.6079933748399));
#269614=CARTESIAN_POINT('Ctrl Pts',(-45.6606150024606,33.6424505696195,
-39.6166516297843));
#269615=CARTESIAN_POINT('Ctrl Pts',(-45.7272860947277,33.6047101271221,
-39.6215780075552));
#269616=CARTESIAN_POINT('Ctrl Pts',(-45.7932287365117,33.5651705839516,
-39.6260731428005));
#269617=CARTESIAN_POINT('Ctrl Pts',(-45.8259059249178,33.5444453395394,
-39.6281074988013));
#269618=CARTESIAN_POINT('Ctrl Pts',(-45.8897275017006,33.5016881508368,
-39.6316923737189));
#269619=CARTESIAN_POINT('Ctrl Pts',(-45.9210297733036,33.4795651380848,
-39.6332542688506));
#269620=CARTESIAN_POINT('Ctrl Pts',(-45.9823424846244,33.4339088874735,
-39.6359180193303));
#269621=CARTESIAN_POINT('Ctrl Pts',(-46.0724202597563,33.3632801300718,
-39.6392265347984));
#269622=CARTESIAN_POINT('Ctrl Pts',(-46.1850394564173,33.2606222983665,
-39.6409205727319));
#269623=CARTESIAN_POINT('Ctrl Pts',(-46.2638636333332,33.1772336958075,
-39.6401443034625));
#269624=CARTESIAN_POINT('Ctrl Pts',(-46.3151397511292,33.1201974856456,
-39.6391646017005));
#269625=CARTESIAN_POINT('Ctrl Pts',(-46.3401349353408,33.0909661742941,
-39.6384440851485));
#269626=CARTESIAN_POINT('Ctrl Pts',(-46.3888523044997,33.0309971480077,
-39.6365301000439));
#269627=CARTESIAN_POINT('Ctrl Pts',(-46.4123735341802,33.0005036828642,
-39.6353439924849));
#269628=CARTESIAN_POINT('Ctrl Pts',(-46.4576879006691,32.9386388625828,
-39.6325280276393));
#269629=CARTESIAN_POINT('Ctrl Pts',(-46.52311576659,32.8444620833496,-39.6276360146217));
#269630=CARTESIAN_POINT('Ctrl Pts',(-46.5810426872604,32.7462345994881,
-39.6207752343847));
#269631=CARTESIAN_POINT('Ctrl Pts',(-46.6516918187307,32.6117039458857,
-39.6098936921283));
#269632=CARTESIAN_POINT('Ctrl Pts',(-46.683723185051,32.5426422373878,-39.6035832967262));
#269633=CARTESIAN_POINT('Ctrl Pts',(-46.7195635412788,32.4540883209461,
-39.5945936116187));
#269634=CARTESIAN_POINT('Ctrl Pts',(-46.7265235775841,32.4362514419463,
-39.5927383889278));
#269635=CARTESIAN_POINT('Ctrl Pts',(-46.7400123459627,32.4003742100513,
-39.5889189813535));
#269636=CARTESIAN_POINT('Ctrl Pts',(-46.7465535157541,32.3822946053341,
-39.5869502184844));
#269637=CARTESIAN_POINT('Ctrl Pts',(-46.7654644360989,32.3279072933142,
-39.5808958427402));
#269638=CARTESIAN_POINT('Ctrl Pts',(-46.7770937339888,32.2915493874551,
-39.5766741707955));
#269639=CARTESIAN_POINT('Ctrl Pts',(-46.8091770518909,32.182013131159,-39.5634457571489));
#269640=CARTESIAN_POINT('Ctrl Pts',(-46.8444383818759,32.034891308334,-39.5443264312115));
#269641=CARTESIAN_POINT('Ctrl Pts',(-46.8650708643864,31.8856621776612,
-39.5223044891954));
#269642=CARTESIAN_POINT('Ctrl Pts',(-46.8750487417844,31.7729724844591,
-39.50469487268));
#269643=CARTESIAN_POINT('Ctrl Pts',(-46.8774570362353,31.7352651712118,
-39.4986397605723));
#269644=CARTESIAN_POINT('Ctrl Pts',(-46.8796767940079,31.6785286095959,
-39.4892824810203));
#269645=CARTESIAN_POINT('Ctrl Pts',(-46.8801843407089,31.6595724593507,
-39.4861150486293));
#269646=CARTESIAN_POINT('Ctrl Pts',(-46.8807312344332,31.6216180949417,
-39.479690628598));
#269647=CARTESIAN_POINT('Ctrl Pts',(-46.8807699646674,31.6025797052015,
-39.4764266299692));
#269648=CARTESIAN_POINT('Ctrl Pts',(-46.8801790388754,31.5455906639181,
-39.4665317368708));
#269649=CARTESIAN_POINT('Ctrl Pts',(-46.8788490796135,31.5078273383739,
-39.4598096545541));
#269650=CARTESIAN_POINT('Ctrl Pts',(-46.874360617844,31.4326451774338,-39.4461013696832));
#269651=CARTESIAN_POINT('Ctrl Pts',(-46.864884835636,31.320441459725,-39.4251517854185));
#269652=CARTESIAN_POINT('Ctrl Pts',(-46.8414902947658,31.1730719473388,
-39.3956936109857));
#269653=CARTESIAN_POINT('Ctrl Pts',(-46.8074810934279,31.0279105813681,
-39.364717848004));
#269654=CARTESIAN_POINT('Ctrl Pts',(-46.7869180083019,30.9560697433081,
-39.3487190247537));
#269655=CARTESIAN_POINT('Ctrl Pts',(-46.7645577771926,30.884604709384,-39.332461491893));
#269656=CARTESIAN_POINT('Ctrl Pts',(-46.7524740339114,30.8490466969583,
-39.3242001683612));
#269657=CARTESIAN_POINT('Ctrl Pts',(-46.7264943673172,30.7783632715819,
-39.3074248425479));
#269658=CARTESIAN_POINT('Ctrl Pts',(-46.7127058212706,30.7435263372096,
-39.2989795429224));
#269659=CARTESIAN_POINT('Ctrl Pts',(-46.6981266849492,30.7091523375488,
-39.2904704603133));
#269660=CARTESIAN_POINT('Ctrl Pts',(-45.0394875320819,30.9432190801919,
-41.190386719266));
#269661=CARTESIAN_POINT('Ctrl Pts',(-45.0282734427409,30.91723575627,-41.1733685540478));
#269662=CARTESIAN_POINT('Ctrl Pts',(-45.0034876660128,30.8666726764904,
-41.1388419648381));
#269663=CARTESIAN_POINT('Ctrl Pts',(-44.9667665375866,30.8068862988478,
-41.09447557187));
#269664=CARTESIAN_POINT('Ctrl Pts',(-44.9421458413835,30.7725558756156,
-41.0673057451311));
#269665=CARTESIAN_POINT('Ctrl Pts',(-44.9251493960809,30.7500159625169,
-41.0490682816776));
#269666=CARTESIAN_POINT('Ctrl Pts',(-44.9163654668634,30.7389260450349,
-41.0398930354472));
#269667=CARTESIAN_POINT('Ctrl Pts',(-44.8981827131164,30.7170729960788,
-41.0213934024069));
#269668=CARTESIAN_POINT('Ctrl Pts',(-44.888838333634,30.7063777841388,-41.0121255186188));
#269669=CARTESIAN_POINT('Ctrl Pts',(-44.8697378119757,30.6855401076749,
-40.9936389109155));
#269670=CARTESIAN_POINT('Ctrl Pts',(-44.8599646045333,30.6753771122426,
-40.984402815764));
#269671=CARTESIAN_POINT('Ctrl Pts',(-44.8300025766326,30.6456635434001,
-40.9567321786306));
#269672=CARTESIAN_POINT('Ctrl Pts',(-44.7987417882795,30.6174785558847,
-40.9291201070801));
#269673=CARTESIAN_POINT('Ctrl Pts',(-44.7544912812914,30.5829390177582,
-40.8924276633141));
#269674=CARTESIAN_POINT('Ctrl Pts',(-44.7200063674423,30.5585634922437,
-40.8649689008411));
#269675=CARTESIAN_POINT('Ctrl Pts',(-44.6961476159991,30.5433500948652,
-40.8467099213417));
#269676=CARTESIAN_POINT('Ctrl Pts',(-44.6779108400504,30.5323301088838,
-40.8330260113948));
#269677=CARTESIAN_POINT('Ctrl Pts',(-44.6717725199842,30.5287210947847,
-40.8284650265932));
#269678=CARTESIAN_POINT('Ctrl Pts',(-44.6594468286685,30.521672327511,-40.8193954109541));
#269679=CARTESIAN_POINT('Ctrl Pts',(-44.6532495459125,30.5182260348866,
-40.8148790968875));
#269680=CARTESIAN_POINT('Ctrl Pts',(-44.6221170703041,30.5014023919654,
-40.7924104777995));
#269681=CARTESIAN_POINT('Ctrl Pts',(-44.5712944462502,30.4770113822335,
-40.7571098106096));
#269682=CARTESIAN_POINT('Ctrl Pts',(-44.5053084694641,30.4527583886953,
-40.7146170218743));
#269683=CARTESIAN_POINT('Ctrl Pts',(-44.4645950315289,30.4410392847555,
-40.6898685245315));
#269684=CARTESIAN_POINT('Ctrl Pts',(-44.4371992237873,30.4338676574989,
-40.6735398509862));
#269685=CARTESIAN_POINT('Ctrl Pts',(-44.4233828828253,30.4306039319716,
-40.6654653393082));
#269686=CARTESIAN_POINT('Ctrl Pts',(-44.395457566773,30.4247250011004,-40.6494724436125));
#269687=CARTESIAN_POINT('Ctrl Pts',(-44.3814368244576,30.4221299378924,
-40.6416053105951));
#269688=CARTESIAN_POINT('Ctrl Pts',(-44.353398925472,30.4176419772095,-40.6261940087904));
#269689=CARTESIAN_POINT('Ctrl Pts',(-44.3393578467875,30.4157440298243,
-40.6186361329255));
#269690=CARTESIAN_POINT('Ctrl Pts',(-44.2971907773647,30.4110825461462,
-40.5964157409664));
#269691=CARTESIAN_POINT('Ctrl Pts',(-44.2690063197214,30.4093460565949,
-40.5821970282665));
#269692=CARTESIAN_POINT('Ctrl Pts',(-44.212497942469,30.4086221665927,-40.5549656043439));
#269693=CARTESIAN_POINT('Ctrl Pts',(-44.1841675064314,30.4096363406377,
-40.5419505068598));
#269694=CARTESIAN_POINT('Ctrl Pts',(-44.1486758957365,30.4126704859088,
-40.5264682752254));
#269695=CARTESIAN_POINT('Ctrl Pts',(-44.141568690144,30.4133673915631,-40.5234096239519));
#269696=CARTESIAN_POINT('Ctrl Pts',(-44.1273541295014,30.414939058346,-40.5173753852017));
#269697=CARTESIAN_POINT('Ctrl Pts',(-44.1202325648852,30.4158161528369,
-40.5143941227858));
#269698=CARTESIAN_POINT('Ctrl Pts',(-44.0989269046614,30.418710900521,-40.5056018445424));
#269699=CARTESIAN_POINT('Ctrl Pts',(-44.0848361489451,30.4209852789275,
-40.4999555272545));
#269700=CARTESIAN_POINT('Ctrl Pts',(-44.0428355440345,30.4288357011986,
-40.4836289969086));
#269701=CARTESIAN_POINT('Ctrl Pts',(-44.001418907738,30.4387301387603,-40.4685417636913));
#269702=CARTESIAN_POINT('Ctrl Pts',(-43.9473552852602,30.4559806561897,
-40.4508995609031));
#269703=CARTESIAN_POINT('Ctrl Pts',(-43.9073915907435,30.4709642266074,
-40.4389183731711));
#269704=CARTESIAN_POINT('Ctrl Pts',(-43.8811432548962,30.4823370897352,
-40.4317784203789));
#269705=CARTESIAN_POINT('Ctrl Pts',(-43.8550972458946,30.4944149327137,
-40.4250719137776));
#269706=CARTESIAN_POINT('Ctrl Pts',(-43.8421555815742,30.5008203273088,
-40.4219325711588));
#269707=CARTESIAN_POINT('Ctrl Pts',(-43.8167947927211,30.5141840584711,
-40.4161689437405));
#269708=CARTESIAN_POINT('Ctrl Pts',(-43.8043130802594,30.5211703528968,
-40.413528034466));
#269709=CARTESIAN_POINT('Ctrl Pts',(-43.7797793173031,30.5357258010655,
-40.4087317905317));
#269710=CARTESIAN_POINT('Ctrl Pts',(-43.7436043213473,30.5584424906522,
-40.4022611528103));
#269711=CARTESIAN_POINT('Ctrl Pts',(-43.7092889915882,30.583786036936,-40.397944872434));
#269712=CARTESIAN_POINT('Ctrl Pts',(-43.6651994519323,30.6199287507259,
-40.394121352571));
#269713=CARTESIAN_POINT('Ctrl Pts',(-43.6439827068456,30.6391798378995,
-40.3931753351425));
#269714=CARTESIAN_POINT('Ctrl Pts',(-43.6032932824946,30.680108587057,-40.3932905044721));
#269715=CARTESIAN_POINT('Ctrl Pts',(-43.5841829799745,30.7014201645355,
-40.3943499059801));
#269716=CARTESIAN_POINT('Ctrl Pts',(-43.5483166082379,30.7456951818503,
-40.3983955355947));
#269717=CARTESIAN_POINT('Ctrl Pts',(-43.5148120542517,30.7916143604394,
-40.4043679292189));
#269718=CARTESIAN_POINT('Ctrl Pts',(-43.4859931451963,30.8408014772341,
-40.4141590917094));
#269719=CARTESIAN_POINT('Ctrl Pts',(-43.469474574758,30.8725808034089,-40.4214902069511));
#269720=CARTESIAN_POINT('Ctrl Pts',(-43.4662461658165,30.8789901287051,
-40.4230180755467));
#269721=CARTESIAN_POINT('Ctrl Pts',(-43.4599404108544,30.8919125782622,
-40.4261957226772));
#269722=CARTESIAN_POINT('Ctrl Pts',(-43.4568618652692,30.8984301381776,
-40.4278470523708));
#269723=CARTESIAN_POINT('Ctrl Pts',(-43.4479066843131,30.9180293597941,
-40.4329571814025));
#269724=CARTESIAN_POINT('Ctrl Pts',(-43.4366800830858,30.9443463169446,
-40.440199707327));
#269725=CARTESIAN_POINT('Ctrl Pts',(-43.4219268251392,30.9843790154574,
-40.4523233881121));
#269726=CARTESIAN_POINT('Ctrl Pts',(-43.4092278315493,31.0249558361973,
-40.4656821965631));
#269727=CARTESIAN_POINT('Ctrl Pts',(-43.3985649158327,31.0660734353404,
-40.4802626336878));
#269728=CARTESIAN_POINT('Ctrl Pts',(-43.3928117504253,31.0938450909326,
-40.4907938342908));
#269729=CARTESIAN_POINT('Ctrl Pts',(-43.3877402558097,31.1217978520093,
-40.5017316825792));
#269730=CARTESIAN_POINT('Ctrl Pts',(-43.3855448869231,31.1358715333473,
-40.5074069308404));
#269731=CARTESIAN_POINT('Ctrl Pts',(-43.3818466485176,31.1641754295066,
-40.5191561881817));
#269732=CARTESIAN_POINT('Ctrl Pts',(-43.3803394900793,31.1784722137567,
-40.5252598906186));
#269733=CARTESIAN_POINT('Ctrl Pts',(-43.3780514709974,31.2069533499868,
-40.5377524690855));
#269734=CARTESIAN_POINT('Ctrl Pts',(-43.3764764291988,31.2353806198054,
-40.5505518795279));
#269735=CARTESIAN_POINT('Ctrl Pts',(-43.3761228002374,31.292003207243,-40.577339198747));
#269736=CARTESIAN_POINT('Ctrl Pts',(-43.3798904844517,31.3482922086547,
-40.6058744004623));
#269737=CARTESIAN_POINT('Ctrl Pts',(-43.3877424304871,31.4042485256067,
-40.6361260433691));
#269738=CARTESIAN_POINT('Ctrl Pts',(-43.393042276717,31.4321193306868,-40.6518290622461));
#269739=CARTESIAN_POINT('Ctrl Pts',(-43.3990345440792,31.4599262492628,
-40.6678171709904));
#269740=CARTESIAN_POINT('Ctrl Pts',(-43.4023871385948,31.4738288295879,
-40.6759732487162));
#269741=CARTESIAN_POINT('Ctrl Pts',(-43.4097262599636,31.5013102698765,
-40.6924188649606));
#269742=CARTESIAN_POINT('Ctrl Pts',(-43.4137223958007,31.5149386860624,
-40.7007364096885));
#269743=CARTESIAN_POINT('Ctrl Pts',(-43.4266697743275,31.5554481319482,
-40.7259437634106));
#269744=CARTESIAN_POINT('Ctrl Pts',(-43.4365815013438,31.5819735775504,
-40.743098588818));
#269745=CARTESIAN_POINT('Ctrl Pts',(-43.453362100664,31.6210434116697,-40.7693485791028));
#269746=CARTESIAN_POINT('Ctrl Pts',(-43.4592720436944,31.6339404199602,
-40.77818065559));
#269747=CARTESIAN_POINT('Ctrl Pts',(-43.471748387858,31.6595177912398,-40.7960360397975));
#269748=CARTESIAN_POINT('Ctrl Pts',(-43.4782913690647,31.6721475181291,
-40.8050245716083));
#269749=CARTESIAN_POINT('Ctrl Pts',(-43.4987158872668,31.7093568101663,
-40.832021101787));
#269750=CARTESIAN_POINT('Ctrl Pts',(-43.5134312848982,31.7333600460206,
-40.8501267844669));
#269751=CARTESIAN_POINT('Ctrl Pts',(-43.5449969636312,31.7797747067972,
-40.8865288544817));
#269752=CARTESIAN_POINT('Ctrl Pts',(-43.570273480101,31.8133992725601,-40.9139774903764));
#269753=CARTESIAN_POINT('Ctrl Pts',(-43.6071874842548,31.8558549470217,
-40.9508682927202));
#269754=CARTESIAN_POINT('Ctrl Pts',(-43.6267265436653,31.8762775041081,
-40.9694100075909));
#269755=CARTESIAN_POINT('Ctrl Pts',(-43.6468212761471,31.8962967826001,
-40.9880061403947));
#269756=CARTESIAN_POINT('Ctrl Pts',(-43.6571524242715,31.9061057307006,
-40.997334528722));
#269757=CARTESIAN_POINT('Ctrl Pts',(-43.6781351765956,31.9250932263188,
-41.0158316653051));
#269758=CARTESIAN_POINT('Ctrl Pts',(-43.6888325213991,31.9343181422645,
-41.0250431278314));
#269759=CARTESIAN_POINT('Ctrl Pts',(-43.7214683281725,31.961133026229,-41.0525078158304));
#269760=CARTESIAN_POINT('Ctrl Pts',(-43.744000771517,31.977916302359,-41.070639272709));
#269761=CARTESIAN_POINT('Ctrl Pts',(-43.7905699795511,32.0092811177654,
-41.106520902203));
#269762=CARTESIAN_POINT('Ctrl Pts',(-43.8266341229871,32.0311632771839,
-41.1331548827895));
#269763=CARTESIAN_POINT('Ctrl Pts',(-43.8644344365312,32.050527928199,-41.1593656410909));
#269764=CARTESIAN_POINT('Ctrl Pts',(-43.8900335656271,32.0628690313763,
-41.1767476889401));
#269765=CARTESIAN_POINT('Ctrl Pts',(-43.903042008964,32.0687560539784,-41.1853974312384));
#269766=CARTESIAN_POINT('Ctrl Pts',(-43.9291618902095,32.0798229381751,
-41.2024070088898));
#269767=CARTESIAN_POINT('Ctrl Pts',(-43.9423286751247,32.0850301956599,
-41.2108047653586));
#269768=CARTESIAN_POINT('Ctrl Pts',(-43.9688389276373,32.0947834481969,
-41.2273662374836));
#269769=CARTESIAN_POINT('Ctrl Pts',(-44.0088868242005,32.1084293286422,
-41.2518690158044));
#269770=CARTESIAN_POINT('Ctrl Pts',(-44.0634057706764,32.1227159830699,
-41.2831968728749));
#269771=CARTESIAN_POINT('Ctrl Pts',(-44.1051448739617,32.1304686073096,
-41.30568419746));
#269772=CARTESIAN_POINT('Ctrl Pts',(-44.1331632182567,32.1349666221674,
-41.3204486001008));
#269773=CARTESIAN_POINT('Ctrl Pts',(-44.1472622735965,32.1368798783668,
-41.3277141420552));
#269774=CARTESIAN_POINT('Ctrl Pts',(-44.1685768983456,32.1392377391899,
-41.3384485067576));
#269775=CARTESIAN_POINT('Ctrl Pts',(-44.1757038998442,32.1399371964,-41.3419962566417));
#269776=CARTESIAN_POINT('Ctrl Pts',(-44.1899298892594,32.1411565650423,
-41.3489954369734));
#269777=CARTESIAN_POINT('Ctrl Pts',(-44.1970429564213,32.1416781032566,
-41.3524539903966));
#269778=CARTESIAN_POINT('Ctrl Pts',(-44.2183581262916,32.1429776302475,
-41.3626954949199));
#269779=CARTESIAN_POINT('Ctrl Pts',(-44.232556678806,32.1434929542666,-41.3693546778539));
#269780=CARTESIAN_POINT('Ctrl Pts',(-44.2750884056492,32.1439936324359,
-41.3888189062651));
#269781=CARTESIAN_POINT('Ctrl Pts',(-44.3033804172497,32.1429384256622,
-41.4011231160504));
#269782=CARTESIAN_POINT('Ctrl Pts',(-44.3598247343314,32.13804594572,-41.4243882373187));
#269783=CARTESIAN_POINT('Ctrl Pts',(-44.3879848006206,32.1342064546963,
-41.4353516241949));
#269784=CARTESIAN_POINT('Ctrl Pts',(-44.4230841862873,32.1276226980045,
-41.4481948195873));
#269785=CARTESIAN_POINT('Ctrl Pts',(-44.4301039616143,32.126214419323,-41.4507215814638));
#269786=CARTESIAN_POINT('Ctrl Pts',(-44.4441256434231,32.1232190082407,
-41.455685422358));
#269787=CARTESIAN_POINT('Ctrl Pts',(-44.4511413829898,32.1216281453652,
-41.4581270453932));
#269788=CARTESIAN_POINT('Ctrl Pts',(-44.472106554004,32.1165956901708,-41.4652964871519));
#269789=CARTESIAN_POINT('Ctrl Pts',(-44.4859328208737,32.1129061786889,
-41.4698557698741));
#269790=CARTESIAN_POINT('Ctrl Pts',(-44.5270324780087,32.1008340938932,
-41.4829067838587));
#269791=CARTESIAN_POINT('Ctrl Pts',(-44.5673316800757,32.08677017453,-41.4946921125766));
#269792=CARTESIAN_POINT('Ctrl Pts',(-44.6194780799712,32.0640738471498,
-41.5079096337926));
#269793=CARTESIAN_POINT('Ctrl Pts',(-44.6577884739158,32.045065905176,-41.5165678887371));
#269794=CARTESIAN_POINT('Ctrl Pts',(-44.6827916371924,32.031050813041,-41.5214942665077));
#269795=CARTESIAN_POINT('Ctrl Pts',(-44.7075150580676,32.0163554529027,
-41.5259894017533));
#269796=CARTESIAN_POINT('Ctrl Pts',(-44.7197631353705,32.0086467826241,
-41.5280237577537));
#269797=CARTESIAN_POINT('Ctrl Pts',(-44.7436779765282,31.9927322821733,
-41.5316086326721));
#269798=CARTESIAN_POINT('Ctrl Pts',(-44.7554039451266,31.9844926239501,
-41.5331705278033));
#269799=CARTESIAN_POINT('Ctrl Pts',(-44.7783650010144,31.9674779303508,
-41.5358342782831));
#269800=CARTESIAN_POINT('Ctrl Pts',(-44.8120876763637,31.941142023486,-41.5391427937509));
#269801=CARTESIAN_POINT('Ctrl Pts',(-44.8542060542843,31.9028069711657,
-41.5408368316843));
#269802=CARTESIAN_POINT('Ctrl Pts',(-44.883650374082,31.8716290815775,-41.5400605624154));
#269803=CARTESIAN_POINT('Ctrl Pts',(-44.9027957424029,31.8502960261458,
-41.5390808606534));
#269804=CARTESIAN_POINT('Ctrl Pts',(-44.912124025092,31.8393588588263,-41.5383603441012));
#269805=CARTESIAN_POINT('Ctrl Pts',(-44.9302963003321,31.816913187918,-41.5364463589967));
#269806=CARTESIAN_POINT('Ctrl Pts',(-44.9390653236876,31.8054960967264,
-41.5352602514373));
#269807=CARTESIAN_POINT('Ctrl Pts',(-44.9559494861592,31.7823260274566,
-41.532444286592));
#269808=CARTESIAN_POINT('Ctrl Pts',(-44.9803129684955,31.7470436123751,
-41.5275522735743));
#269809=CARTESIAN_POINT('Ctrl Pts',(-45.00183725318,31.7102129370948,-41.5206914933375));
#269810=CARTESIAN_POINT('Ctrl Pts',(-45.0280427451288,31.6597446570548,
-41.5098099510806));
#269811=CARTESIAN_POINT('Ctrl Pts',(-45.0398987329805,31.6338241168053,
-41.5034995556801));
#269812=CARTESIAN_POINT('Ctrl Pts',(-45.0531290598229,31.6005723463994,
-41.4945098705711));
#269813=CARTESIAN_POINT('Ctrl Pts',(-45.0556963147994,31.5938738844661,
-41.4926546478805));
#269814=CARTESIAN_POINT('Ctrl Pts',(-45.0606676096559,31.5803990532317,
-41.4888352403062));
#269815=CARTESIAN_POINT('Ctrl Pts',(-45.0630762139805,31.5736079348959,
-41.4868664774371));
#269816=CARTESIAN_POINT('Ctrl Pts',(-45.0700329505347,31.5531765604049,
-41.4808121016924));
#269817=CARTESIAN_POINT('Ctrl Pts',(-45.0743018132827,31.5395152309552,
-41.4765904297482));
#269818=CARTESIAN_POINT('Ctrl Pts',(-45.0860497029301,31.4983488303989,
-41.4633620161014));
#269819=CARTESIAN_POINT('Ctrl Pts',(-45.0988767040151,31.4430340104486,
-41.4442426901641));
#269820=CARTESIAN_POINT('Ctrl Pts',(-45.1061818129997,31.386882792419,-41.4222207481485));
#269821=CARTESIAN_POINT('Ctrl Pts',(-45.1095857869151,31.3444641027996,
-41.4046111316328));
#269822=CARTESIAN_POINT('Ctrl Pts',(-45.1103739871937,31.3302675876129,
-41.3985560195248));
#269823=CARTESIAN_POINT('Ctrl Pts',(-45.1110306052012,31.30890259785,-41.3891987399731));
#269824=CARTESIAN_POINT('Ctrl Pts',(-45.1111617199316,31.3017636946428,
-41.3860313075819));
#269825=CARTESIAN_POINT('Ctrl Pts',(-45.1112472734604,31.2874686716035,
-41.3796068875509));
#269826=CARTESIAN_POINT('Ctrl Pts',(-45.111201351958,31.2802974166487,-41.3763428889219));
#269827=CARTESIAN_POINT('Ctrl Pts',(-45.1107973541963,31.25882908612,-41.3664479958234));
#269828=CARTESIAN_POINT('Ctrl Pts',(-45.11017580813,31.2446005169708,-41.3597259135069));
#269829=CARTESIAN_POINT('Ctrl Pts',(-45.1082442962718,31.2162677536902,
-41.3460176286356));
#269830=CARTESIAN_POINT('Ctrl Pts',(-45.104314463686,31.1739750543259,-41.3250680443717));
#269831=CARTESIAN_POINT('Ctrl Pts',(-45.0950241996196,31.1183949914011,
-41.295609869938));
#269832=CARTESIAN_POINT('Ctrl Pts',(-45.0817381040079,31.0636149263882,
-41.264634106957));
#269833=CARTESIAN_POINT('Ctrl Pts',(-45.0737554763462,31.0364928582332,
-41.2486352837062));
#269834=CARTESIAN_POINT('Ctrl Pts',(-45.0650963255467,31.0095068957897,
-41.2323777508457));
#269835=CARTESIAN_POINT('Ctrl Pts',(-45.0604265398991,30.996076905732,-41.224116427314));
#269836=CARTESIAN_POINT('Ctrl Pts',(-45.0504049610752,30.9693743366894,
-41.2073411015006));
#269837=CARTESIAN_POINT('Ctrl Pts',(-45.0450945767524,30.9562107421528,
-41.1988958018751));
#269838=CARTESIAN_POINT('Ctrl Pts',(-45.0394875320819,30.9432190801919,
-41.190386719266));
#269839=CARTESIAN_POINT('Ctrl Pts',(46.6981266907859,30.7091523367251,-39.2904704536276));
#269840=CARTESIAN_POINT('Ctrl Pts',(46.6835475544328,30.6747783369892,-39.2819613710184));
#269841=CARTESIAN_POINT('Ctrl Pts',(46.6681815018369,30.6408774253669,-39.2733909051616));
#269842=CARTESIAN_POINT('Ctrl Pts',(46.6359019286597,30.5740061528406,-39.2561284815506));
#269843=CARTESIAN_POINT('Ctrl Pts',(46.6189883221311,30.5410358432638,-39.2474365183329));
#269844=CARTESIAN_POINT('Ctrl Pts',(46.5659489438546,30.4435074270321,-39.2211791182564));
#269845=CARTESIAN_POINT('Ctrl Pts',(46.5275294448601,30.380328936116,-39.2034325197551));
#269846=CARTESIAN_POINT('Ctrl Pts',(46.4653032005596,30.2883271653987,-39.1764461155182));
#269847=CARTESIAN_POINT('Ctrl Pts',(46.4437937635959,30.2581216153683,-39.1673894794925));
#269848=CARTESIAN_POINT('Ctrl Pts',(46.399222420064,30.1986447431778,-39.1491520160392));
#269849=CARTESIAN_POINT('Ctrl Pts',(46.3761748824675,30.1693908426405,-39.1399767698089));
#269850=CARTESIAN_POINT('Ctrl Pts',(46.3284414075139,30.1117648092771,-39.1214771367686));
#269851=CARTESIAN_POINT('Ctrl Pts',(46.3038983428192,30.0835718262094,-39.1122092529802));
#269852=CARTESIAN_POINT('Ctrl Pts',(46.2537073924782,30.0286632726536,-39.0937226452772));
#269853=CARTESIAN_POINT('Ctrl Pts',(46.228014707505,30.001893562086,-39.0844865501256));
#269854=CARTESIAN_POINT('Ctrl Pts',(46.1492148056875,29.923658669611,-39.0568159129922));
#269855=CARTESIAN_POINT('Ctrl Pts',(46.0943603842992,29.874228785717,-39.0384077274207));
#269856=CARTESIAN_POINT('Ctrl Pts',(46.0086385399379,29.8041510510904,-39.0108577052895));
#269857=CARTESIAN_POINT('Ctrl Pts',(45.9794896748778,29.7814700270485,-39.00168453381));
#269858=CARTESIAN_POINT('Ctrl Pts',(45.9200349172104,29.7374728277044,-38.9833588529876));
#269859=CARTESIAN_POINT('Ctrl Pts',(45.8897290750455,29.7161565932536,-38.9742063418902));
#269860=CARTESIAN_POINT('Ctrl Pts',(45.8279451213265,29.6749068315954,-38.9559225560557));
#269861=CARTESIAN_POINT('Ctrl Pts',(45.7964751128047,29.6549785787194,-38.9467936557034));
#269862=CARTESIAN_POINT('Ctrl Pts',(45.7483486075838,29.6261284918058,-38.9331097457563));
#269863=CARTESIAN_POINT('Ctrl Pts',(45.7321473321371,29.6166840488636,-38.9285487609545));
#269864=CARTESIAN_POINT('Ctrl Pts',(45.6996106239914,29.5982459944737,-38.9194791453156));
#269865=CARTESIAN_POINT('Ctrl Pts',(45.6832490479695,29.5892352416054,-38.9149628312498));
#269866=CARTESIAN_POINT('Ctrl Pts',(45.601043919029,29.5452683980011,-38.8924942121586));
#269867=CARTESIAN_POINT('Ctrl Pts',(45.5339075028974,29.5134615269732,-38.8748432905736));
#269868=CARTESIAN_POINT('Ctrl Pts',(45.3969715912008,29.4565064904797,-38.8401971286172));
#269869=CARTESIAN_POINT('Ctrl Pts',(45.3271662968287,29.4313508095901,-38.8231995362783));
#269870=CARTESIAN_POINT('Ctrl Pts',(45.2204298468913,29.3986526373661,-38.7982016653842));
#269871=CARTESIAN_POINT('Ctrl Pts',(45.1845124401493,29.3885937216909,-38.7899522588935));
#269872=CARTESIAN_POINT('Ctrl Pts',(45.1119891491544,29.3701842504182,-38.7736235853476));
#269873=CARTESIAN_POINT('Ctrl Pts',(45.0754052601759,29.3618381477176,-38.7655490736698));
#269874=CARTESIAN_POINT('Ctrl Pts',(45.0014447954028,29.3468760796426,-38.7495561779739));
#269875=CARTESIAN_POINT('Ctrl Pts',(44.964301865418,29.3403115524284,-38.7416890449567));
#269876=CARTESIAN_POINT('Ctrl Pts',(44.8900079613448,29.3290481853876,-38.7262777431523));
#269877=CARTESIAN_POINT('Ctrl Pts',(44.8527936300225,29.3243364917773,-38.7187198672871));
#269878=CARTESIAN_POINT('Ctrl Pts',(44.7410083388884,29.3129455696646,-38.6964994753282));
#269879=CARTESIAN_POINT('Ctrl Pts',(44.6662563771146,29.3089967383529,-38.6822807626282));
#269880=CARTESIAN_POINT('Ctrl Pts',(44.5163124694972,29.3084067895486,-38.6550493387052));
#269881=CARTESIAN_POINT('Ctrl Pts',(44.4411031904291,29.3117700104783,-38.6420342412209));
#269882=CARTESIAN_POINT('Ctrl Pts',(44.3468378622929,29.3206690016762,-38.6265520095871));
#269883=CARTESIAN_POINT('Ctrl Pts',(44.3279589155214,29.3226883277488,-38.6234933583131));
#269884=CARTESIAN_POINT('Ctrl Pts',(44.2901960658791,29.3271995041764,-38.6174591195633));
#269885=CARTESIAN_POINT('Ctrl Pts',(44.2712743938236,29.3296978892051,-38.6144778571473));
#269886=CARTESIAN_POINT('Ctrl Pts',(44.2146592786091,29.3378915957788,-38.6056855789043));
#269887=CARTESIAN_POINT('Ctrl Pts',(44.1772069505284,29.344266755037,-38.600039261616));
#269888=CARTESIAN_POINT('Ctrl Pts',(44.1027653085689,29.3588321557227,-38.5891549080521));
#269889=CARTESIAN_POINT('Ctrl Pts',(44.0657945489821,29.3670194923296,-38.5839197136818));
#269890=CARTESIAN_POINT('Ctrl Pts',(43.9923490655734,29.3851891984824,-38.5738612386265));
#269891=CARTESIAN_POINT('Ctrl Pts',(43.9558743462093,29.3951715837984,-38.5690379607699));
#269892=CARTESIAN_POINT('Ctrl Pts',(43.8834205273202,29.4169303960524,-38.5598042413246));
#269893=CARTESIAN_POINT('Ctrl Pts',(43.8474414247684,29.4287068117428,-38.5553937964858));
#269894=CARTESIAN_POINT('Ctrl Pts',(43.7759820581033,29.4540658159891,-38.5469896253478));
#269895=CARTESIAN_POINT('Ctrl Pts',(43.7405017832129,29.467648365304,-38.5429958894628));
#269896=CARTESIAN_POINT('Ctrl Pts',(43.6700470469744,29.4966453366817,-38.5354320916221));
#269897=CARTESIAN_POINT('Ctrl Pts',(43.6350719748427,29.5120610602386,-38.5318621547404));
#269898=CARTESIAN_POINT('Ctrl Pts',(43.5656410075109,29.5447591283353,-38.5251556481393));
#269899=CARTESIAN_POINT('Ctrl Pts',(43.5311320043801,29.562079443133,-38.5220163055204));
#269900=CARTESIAN_POINT('Ctrl Pts',(43.4634866399702,29.598175832334,-38.5162526781022));
#269901=CARTESIAN_POINT('Ctrl Pts',(43.4301834650226,29.6170276514184,-38.5136117688276));
#269902=CARTESIAN_POINT('Ctrl Pts',(43.3647025877044,29.6562685656384,-38.5088155248935));
#269903=CARTESIAN_POINT('Ctrl Pts',(43.3325078216452,29.6766655508507,-38.5066585142211));
#269904=CARTESIAN_POINT('Ctrl Pts',(43.2375484303922,29.7401688832699,-38.5009063899101));
#269905=CARTESIAN_POINT('Ctrl Pts',(43.1764049255325,29.7855824554079,-38.4980286067954));
#269906=CARTESIAN_POINT('Ctrl Pts',(43.0584774159086,29.8826126198196,-38.4942050869327));
#269907=CARTESIAN_POINT('Ctrl Pts',(43.0016818163768,29.9342392625963,-38.4932590695039));
#269908=CARTESIAN_POINT('Ctrl Pts',(42.892659969367,30.0438904469854,-38.4933742388339));
#269909=CARTESIAN_POINT('Ctrl Pts',(42.8414047124706,30.1009342480614,-38.4944336403416));
#269910=CARTESIAN_POINT('Ctrl Pts',(42.7451036174982,30.21934712085,-38.4984792699563));
#269911=CARTESIAN_POINT('Ctrl Pts',(42.7000684081338,30.2807072600243,-38.5014658059356));
#269912=CARTESIAN_POINT('Ctrl Pts',(42.6161769306285,30.4076992000848,-38.5093469056588));
#269913=CARTESIAN_POINT('Ctrl Pts',(42.577322537405,30.4733365225655,-38.5142428260717));
#269914=CARTESIAN_POINT('Ctrl Pts',(42.5326943345249,30.558096382896,-38.5215739413125));
#269915=CARTESIAN_POINT('Ctrl Pts',(42.5239673817088,30.5751883082038,-38.5231018099081));
#269916=CARTESIAN_POINT('Ctrl Pts',(42.5069121477218,30.6096437625167,-38.5262794570385));
#269917=CARTESIAN_POINT('Ctrl Pts',(42.498580574823,30.627019093672,-38.5279307867324));
#269918=CARTESIAN_POINT('Ctrl Pts',(42.4743295437012,30.6792614189893,-38.5330409157641));
#269919=CARTESIAN_POINT('Ctrl Pts',(42.4591078014939,30.7143247165074,-38.5366620710225));
#269920=CARTESIAN_POINT('Ctrl Pts',(42.4305062686555,30.7849297919355,-38.5443247961378));
#269921=CARTESIAN_POINT('Ctrl Pts',(42.4171273582822,30.8204683259224,-38.5483659351791));
#269922=CARTESIAN_POINT('Ctrl Pts',(42.3921837076412,30.8920099497574,-38.5568600247503));
#269923=CARTESIAN_POINT('Ctrl Pts',(42.3806190143997,30.9280130515862,-38.561312986478));
#269924=CARTESIAN_POINT('Ctrl Pts',(42.3592881526269,31.0004799413282,-38.5706260837038));
#269925=CARTESIAN_POINT('Ctrl Pts',(42.3495220026171,31.0369437339053,-38.5754862240386));
#269926=CARTESIAN_POINT('Ctrl Pts',(42.3317857457909,31.1103315159601,-38.5856119670777));
#269927=CARTESIAN_POINT('Ctrl Pts',(42.3238156305991,31.147255503193,-38.5908775686523));
#269928=CARTESIAN_POINT('Ctrl Pts',(42.309682038946,31.2215665452978,-38.6018154169406));
#269929=CARTESIAN_POINT('Ctrl Pts',(42.3035171831015,31.2589715318414,-38.607490665202));
#269930=CARTESIAN_POINT('Ctrl Pts',(42.2930235486099,31.334179141612,-38.619239922543));
#269931=CARTESIAN_POINT('Ctrl Pts',(42.2886818036678,31.3721585365914,-38.6253436249801));
#269932=CARTESIAN_POINT('Ctrl Pts',(42.2819306267537,31.4478003639188,-38.6378362034469));
#269933=CARTESIAN_POINT('Ctrl Pts',(42.2795025198556,31.4855414987872,-38.6442360062361));
#269934=CARTESIAN_POINT('Ctrl Pts',(42.2765060604552,31.5608485908284,-38.6573322655641));
#269935=CARTESIAN_POINT('Ctrl Pts',(42.2759365524734,31.5984178308852,-38.6640291123748));
#269936=CARTESIAN_POINT('Ctrl Pts',(42.2769710577917,31.7108769179205,-38.6845570238621));
#269937=CARTESIAN_POINT('Ctrl Pts',(42.2813124720526,31.7855186416003,-38.6988245608712));
#269938=CARTESIAN_POINT('Ctrl Pts',(42.2932531065375,31.896990615329,-38.7210841762227));
#269939=CARTESIAN_POINT('Ctrl Pts',(42.2981395912299,31.9340660323646,-38.7286473479064));
#269940=CARTESIAN_POINT('Ctrl Pts',(42.3097367739455,32.0080522304774,-38.7440609665678));
#269941=CARTESIAN_POINT('Ctrl Pts',(42.3164494369031,32.0449687624179,-38.7519127966078));
#269942=CARTESIAN_POINT('Ctrl Pts',(42.3317154542076,32.1186122164871,-38.767900905352));
#269943=CARTESIAN_POINT('Ctrl Pts',(42.340295660643,32.1554227607203,-38.7760569830776));
#269944=CARTESIAN_POINT('Ctrl Pts',(42.3591481677318,32.2281691633317,-38.792502599322));
#269945=CARTESIAN_POINT('Ctrl Pts',(42.3694448311464,32.2642362922514,-38.8008201440502));
#269946=CARTESIAN_POINT('Ctrl Pts',(42.3917427963414,32.3356900700797,-38.8176250465312));
#269947=CARTESIAN_POINT('Ctrl Pts',(42.4037465114866,32.3710895355311,-38.826115145426));
#269948=CARTESIAN_POINT('Ctrl Pts',(42.4294540504939,32.4412374324299,-38.8432687814672));
#269949=CARTESIAN_POINT('Ctrl Pts',(42.4431578812073,32.4759858610929,-38.8519323199412));
#269950=CARTESIAN_POINT('Ctrl Pts',(42.4722685007499,32.5448308011725,-38.869432313464));
#269951=CARTESIAN_POINT('Ctrl Pts',(42.4876674770116,32.5789105833965,-38.8782643899516));
#269952=CARTESIAN_POINT('Ctrl Pts',(42.5202146557244,32.6464795846854,-38.896119774159));
#269953=CARTESIAN_POINT('Ctrl Pts',(42.5373018236116,32.6798350058129,-38.9051083059688));
#269954=CARTESIAN_POINT('Ctrl Pts',(42.5906929380972,32.7780784000063,-38.9321048361507));
#269955=CARTESIAN_POINT('Ctrl Pts',(42.6292257867655,32.8414173761326,-38.9502105188277));
#269956=CARTESIAN_POINT('Ctrl Pts',(42.7120000039881,32.9638220594128,-38.9866125888437));
#269957=CARTESIAN_POINT('Ctrl Pts',(42.75624392991,33.0229003398858,-39.0049117127868));
#269958=CARTESIAN_POINT('Ctrl Pts',(42.8269002174294,33.1083282810888,-39.0325062982755));
#269959=CARTESIAN_POINT('Ctrl Pts',(42.85116847875,33.1362718605164,-39.0417288600547));
#269960=CARTESIAN_POINT('Ctrl Pts',(42.9011535509872,33.1910821857371,-39.060223195478));
#269961=CARTESIAN_POINT('Ctrl Pts',(42.9268673359585,33.2179450272291,-39.0694937419525));
#269962=CARTESIAN_POINT('Ctrl Pts',(42.9797817038445,33.2705900505667,-39.0880898747562));
#269963=CARTESIAN_POINT('Ctrl Pts',(43.0069972073728,33.296373704326,-39.0974182630833));
#269964=CARTESIAN_POINT('Ctrl Pts',(43.0622936376772,33.3462615419736,-39.1159153996671));
#269965=CARTESIAN_POINT('Ctrl Pts',(43.0904949924992,33.3704876798722,-39.1251268621925));
#269966=CARTESIAN_POINT('Ctrl Pts',(43.1765626045295,33.4408730195783,-39.1525915501928));
#269967=CARTESIAN_POINT('Ctrl Pts',(43.2360245516304,33.4848790497124,-39.1707230070701));
#269968=CARTESIAN_POINT('Ctrl Pts',(43.3282503285803,33.5464830122584,-39.1976342291912));
#269969=CARTESIAN_POINT('Ctrl Pts',(43.3595022250126,33.5662859422569,-39.2065581988407));
#269970=CARTESIAN_POINT('Ctrl Pts',(43.4230323983204,33.6044188752118,-39.224313204774));
#269971=CARTESIAN_POINT('Ctrl Pts',(43.4553106306814,33.6227489424813,-39.2331442440926));
#269972=CARTESIAN_POINT('Ctrl Pts',(43.5209070235488,33.6579164289522,-39.2507127796806));
#269973=CARTESIAN_POINT('Ctrl Pts',(43.5542222363685,33.6747516567492,-39.2594493754524));
#269974=CARTESIAN_POINT('Ctrl Pts',(43.6219256420881,33.7069073928245,-39.2768314233018));
#269975=CARTESIAN_POINT('Ctrl Pts',(43.6563381471253,33.7222286526369,-39.2854811655998));
#269976=CARTESIAN_POINT('Ctrl Pts',(43.7254519163343,33.7509934819442,-39.3024907432514));
#269977=CARTESIAN_POINT('Ctrl Pts',(43.760299544244,33.7645084667414,-39.3108884997202));
#269978=CARTESIAN_POINT('Ctrl Pts',(43.8304781079213,33.7897808429036,-39.3274499718452));
#269979=CARTESIAN_POINT('Ctrl Pts',(43.8658243281891,33.8015455663885,-39.3356176240585));
#269980=CARTESIAN_POINT('Ctrl Pts',(43.9726293605948,33.8342393235301,-39.3597845464139));
#269981=CARTESIAN_POINT('Ctrl Pts',(44.0448528416252,33.8525737481731,-39.3754484955492));
#269982=CARTESIAN_POINT('Ctrl Pts',(44.1547335163723,33.8748267497094,-39.3982722224796));
#269983=CARTESIAN_POINT('Ctrl Pts',(44.191618372651,33.8813683208027,-39.4057679318215));
#269984=CARTESIAN_POINT('Ctrl Pts',(44.2659122963829,33.8926703026745,-39.4205323344626));
#269985=CARTESIAN_POINT('Ctrl Pts',(44.3033049226923,33.8974288720327,-39.4277978764165));
#269986=CARTESIAN_POINT('Ctrl Pts',(44.359845358365,33.9032051006838,-39.4385322411192));
#269987=CARTESIAN_POINT('Ctrl Pts',(44.3787527165822,33.9049006225454,-39.4420799910032));
#269988=CARTESIAN_POINT('Ctrl Pts',(44.4164967882661,33.9078161235755,-39.449079171335));
#269989=CARTESIAN_POINT('Ctrl Pts',(44.4353708477243,33.9090401020071,-39.4525377247581));
#269990=CARTESIAN_POINT('Ctrl Pts',(44.4919347189154,33.9120095324017,-39.4627792292813));
#269991=CARTESIAN_POINT('Ctrl Pts',(44.5296205501853,33.9130584470787,-39.4694384122155));
#269992=CARTESIAN_POINT('Ctrl Pts',(44.6425299014747,33.9134342988086,-39.4889026406268));
#269993=CARTESIAN_POINT('Ctrl Pts',(44.7176656243566,33.9100023915017,-39.501206850412));
#269994=CARTESIAN_POINT('Ctrl Pts',(44.8676233294529,33.8957625599936,-39.5244719716803));
#269995=CARTESIAN_POINT('Ctrl Pts',(44.9424659620243,33.8849485806272,-39.5354353585575));
#269996=CARTESIAN_POINT('Ctrl Pts',(45.035788517423,33.8666999904859,-39.5482785539486));
#269997=CARTESIAN_POINT('Ctrl Pts',(45.0544546365756,33.8628074844052,-39.5508053158255));
#269998=CARTESIAN_POINT('Ctrl Pts',(45.091743104854,33.8545484221227,-39.5557691567194));
#269999=CARTESIAN_POINT('Ctrl Pts',(45.1104022568045,33.8501716610976,-39.5582107797549));
#270000=CARTESIAN_POINT('Ctrl Pts',(45.1661672150022,33.836353836405,-39.5653802215133));
#270001=CARTESIAN_POINT('Ctrl Pts',(45.202951114401,33.8262578422849,-39.5699395042355));
#270002=CARTESIAN_POINT('Ctrl Pts',(45.2758615942045,33.804296576773,-39.5786401802253));
#270003=CARTESIAN_POINT('Ctrl Pts',(45.3119687162999,33.7924363258948,-39.5827791057116));
#270004=CARTESIAN_POINT('Ctrl Pts',(45.3834929107785,33.76697243113,-39.5906388608178));
#270005=CARTESIAN_POINT('Ctrl Pts',(45.4189099756201,33.7533687680179,-39.5943596850842));
#270006=CARTESIAN_POINT('Ctrl Pts',(45.4890551228987,33.7244209358064,-39.6013847741846));
#270007=CARTESIAN_POINT('Ctrl Pts',(45.5237832082604,33.7090767739723,-39.6046890401843));
#270008=CARTESIAN_POINT('Ctrl Pts',(45.5925464222574,33.6766380727023,-39.6108794174069));
#270009=CARTESIAN_POINT('Ctrl Pts',(45.6265815645382,33.6595435676593,-39.6137655364386));
#270010=CARTESIAN_POINT('Ctrl Pts',(45.6939497298677,33.6235811813386,-39.6191148132429));
#270011=CARTESIAN_POINT('Ctrl Pts',(45.7272860984032,33.6047101326598,-39.6215780008695));
#270012=CARTESIAN_POINT('Ctrl Pts',(45.7932287403323,33.5651705894019,-39.6260731361148));
#270013=CARTESIAN_POINT('Ctrl Pts',(45.8259059288103,33.5444453449438,-39.6281074921155));
#270014=CARTESIAN_POINT('Ctrl Pts',(45.8897275057335,33.5016881561468,-39.6316923670332));
#270015=CARTESIAN_POINT('Ctrl Pts',(45.9210297774054,33.4795651433458,-39.6332542621649));
#270016=CARTESIAN_POINT('Ctrl Pts',(45.9823424888611,33.4339088926338,-39.6359180126446));
#270017=CARTESIAN_POINT('Ctrl Pts',(46.0123687663031,33.4103663730771,-39.6370209832341));
#270018=CARTESIAN_POINT('Ctrl Pts',(46.1005740614019,33.3376145406148,-39.6396496617403));
#270019=CARTESIAN_POINT('Ctrl Pts',(46.1568837698145,33.2862857494669,-39.6404967215965));
#270020=CARTESIAN_POINT('Ctrl Pts',(46.2375893089641,33.2050303509431,-39.6404032020738));
#270021=CARTESIAN_POINT('Ctrl Pts',(46.2638636381901,33.1772337004019,-39.6401442967768));
#270022=CARTESIAN_POINT('Ctrl Pts',(46.3151397560992,33.1201974901143,-39.6391645950147));
#270023=CARTESIAN_POINT('Ctrl Pts',(46.3401349403659,33.0909661786984,-39.6384440784628));
#270024=CARTESIAN_POINT('Ctrl Pts',(46.3888523096323,33.03099715228,-39.6365300933582));
#270025=CARTESIAN_POINT('Ctrl Pts',(46.4123735393647,33.0005036870694,-39.6353439857992));
#270026=CARTESIAN_POINT('Ctrl Pts',(46.4576879059536,32.9386388666518,-39.6325280209535));
#270027=CARTESIAN_POINT('Ctrl Pts',(46.4794979921318,32.9072463868165,-39.6308974524097));
#270028=CARTESIAN_POINT('Ctrl Pts',(46.5424231506391,32.8117200325625,-39.6253488762663));
#270029=CARTESIAN_POINT('Ctrl Pts',(46.5810426928175,32.7462346031338,-39.620775227699));
#270030=CARTESIAN_POINT('Ctrl Pts',(46.6516918244441,32.6117039492356,-39.6098936854426));
#270031=CARTESIAN_POINT('Ctrl Pts',(46.6837231908355,32.5426422405858,-39.6035832900405));
#270032=CARTESIAN_POINT('Ctrl Pts',(46.7195635471429,32.4540883239497,-39.594593604933));
#270033=CARTESIAN_POINT('Ctrl Pts',(46.7265235834636,32.4362514449106,-39.592738382242));
#270034=CARTESIAN_POINT('Ctrl Pts',(46.7400123518722,32.4003742129367,-39.5889189746678));
#270035=CARTESIAN_POINT('Ctrl Pts',(46.7465535216782,32.3822946081798,-39.5869502117987));
#270036=CARTESIAN_POINT('Ctrl Pts',(46.765464442065,32.3279072960404,-39.5808958360545));
#270037=CARTESIAN_POINT('Ctrl Pts',(46.7770937399808,32.2915493901016,-39.5766741641098));
#270038=CARTESIAN_POINT('Ctrl Pts',(46.7984826186299,32.218525219077,-39.5678552216787));
#270039=CARTESIAN_POINT('Ctrl Pts',(46.8082357029931,32.1818782650522,-39.5632601386704));
#270040=CARTESIAN_POINT('Ctrl Pts',(46.8258916183201,32.1083194058768,-39.5537041697811));
#270041=CARTESIAN_POINT('Ctrl Pts',(46.8337943402473,32.0714074849882,-39.5487432633557));
#270042=CARTESIAN_POINT('Ctrl Pts',(46.8547548479309,31.9602784803845,-39.5333157848068));
#270043=CARTESIAN_POINT('Ctrl Pts',(46.8650708705757,31.8856621794164,-39.5223044825097));
#270044=CARTESIAN_POINT('Ctrl Pts',(46.875048747997,31.772972485967,-39.5046948659943));
#270045=CARTESIAN_POINT('Ctrl Pts',(46.8774570424536,31.7352651726369,-39.4986397538865));
#270046=CARTESIAN_POINT('Ctrl Pts',(46.8796768002317,31.6785286108966,-39.4892824743346));
#270047=CARTESIAN_POINT('Ctrl Pts',(46.880184346934,31.6595724606098,-39.4861150419436));
#270048=CARTESIAN_POINT('Ctrl Pts',(46.88073124066,31.6216180961176,-39.4796906219123));
#270049=CARTESIAN_POINT('Ctrl Pts',(46.8807699708944,31.6025797063356,-39.4764266232835));
#270050=CARTESIAN_POINT('Ctrl Pts',(46.8801790451018,31.5455906649272,-39.4665317301851));
#270051=CARTESIAN_POINT('Ctrl Pts',(46.8788490858374,31.5078273393001,-39.4598096478684));
#270052=CARTESIAN_POINT('Ctrl Pts',(46.8743606240589,31.4326451781951,-39.4461013629975));
#270053=CARTESIAN_POINT('Ctrl Pts',(46.8712024781441,31.395243845809,-39.4391182314914));
#270054=CARTESIAN_POINT('Ctrl Pts',(46.859034876608,31.2835993580034,-39.4177870486965));
#270055=CARTESIAN_POINT('Ctrl Pts',(46.8473376351276,31.2099145951219,-39.4030579681171));
#270056=CARTESIAN_POINT('Ctrl Pts',(46.8244864012849,31.100491008194,-39.3802058007947));
#270057=CARTESIAN_POINT('Ctrl Pts',(46.8159835841289,31.0642007181343,-39.3724617791813));
#270058=CARTESIAN_POINT('Ctrl Pts',(46.7971994340653,30.9919902985873,-39.3567184316147));
#270059=CARTESIAN_POINT('Ctrl Pts',(46.7869180143304,30.9560697430251,-39.348719018068));
#270060=CARTESIAN_POINT('Ctrl Pts',(46.7645577831729,30.8846047089445,-39.3324614852073));
#270061=CARTESIAN_POINT('Ctrl Pts',(46.7524740398656,30.8490466964409,-39.3242001616755));
#270062=CARTESIAN_POINT('Ctrl Pts',(46.7264943732153,30.7783632709098,-39.3074248358622));
#270063=CARTESIAN_POINT('Ctrl Pts',(46.7127058271388,30.7435263364611,-39.2989795362367));
#270064=CARTESIAN_POINT('Ctrl Pts',(46.6981266907859,30.7091523367251,-39.2904704536276));
#270065=CARTESIAN_POINT('Ctrl Pts',(46.3487330454107,30.7584586806226,-39.6906893116447));
#270066=CARTESIAN_POINT('Ctrl Pts',(46.3360438872384,30.7285888871829,-39.6821802290355));
#270067=CARTESIAN_POINT('Ctrl Pts',(46.3226713842648,30.6991295511679,-39.6736097631786));
#270068=CARTESIAN_POINT('Ctrl Pts',(46.2945825861103,30.6410182279319,-39.6563473395677));
#270069=CARTESIAN_POINT('Ctrl Pts',(46.2798662162942,30.6123662852523,-39.64765537635));
#270070=CARTESIAN_POINT('Ctrl Pts',(46.2337210871567,30.527609915333,-39.6213979762735));
#270071=CARTESIAN_POINT('Ctrl Pts',(46.2003005032305,30.4727024332251,-39.6036513777721));
#270072=CARTESIAN_POINT('Ctrl Pts',(46.1461777229336,30.3927408835902,-39.5766649735353));
#270073=CARTESIAN_POINT('Ctrl Pts',(46.1274704458576,30.3664875975353,-39.5676083375096));
#270074=CARTESIAN_POINT('Ctrl Pts',(46.0887077763598,30.3147915248746,-39.5493708740563));
#270075=CARTESIAN_POINT('Ctrl Pts',(46.0686648791047,30.2893638816766,-39.5401956278259));
#270076=CARTESIAN_POINT('Ctrl Pts',(46.0271562868518,30.2392734556588,-39.5216959947856));
#270077=CARTESIAN_POINT('Ctrl Pts',(46.0058148371699,30.2147663918631,-39.5124281109973));
#270078=CARTESIAN_POINT('Ctrl Pts',(45.9621731101223,30.167034895406,-39.4939415032943));
#270079=CARTESIAN_POINT('Ctrl Pts',(45.9398338756316,30.1437634024636,-39.4847054081427));
#270080=CARTESIAN_POINT('Ctrl Pts',(45.8713217104267,30.0757495650345,-39.4570347710093));
#270081=CARTESIAN_POINT('Ctrl Pts',(45.8236322612105,30.0327740175956,-39.4386265854377));
#270082=CARTESIAN_POINT('Ctrl Pts',(45.7491121861247,29.9718412271654,-39.4110765633066));
#270083=CARTESIAN_POINT('Ctrl Pts',(45.7237731661291,29.9521190412175,-39.4019033918271));
#270084=CARTESIAN_POINT('Ctrl Pts',(45.6720909021616,29.9138594468863,-39.3835777110047));
#270085=CARTESIAN_POINT('Ctrl Pts',(45.6457477019571,29.8953219871642,-39.3744251999072));
#270086=CARTESIAN_POINT('Ctrl Pts',(45.5920438586766,29.85944733933,-39.3561414140728));
#270087=CARTESIAN_POINT('Ctrl Pts',(45.5646902588189,29.8421147384108,-39.3470125137204));
#270088=CARTESIAN_POINT('Ctrl Pts',(45.5228600486148,29.8170205763042,-39.3333286037734));
#270089=CARTESIAN_POINT('Ctrl Pts',(45.5087785426461,29.8088053710447,-39.3287676189716));
#270090=CARTESIAN_POINT('Ctrl Pts',(45.4804993011169,29.7927664789577,-39.3196980033327));
#270091=CARTESIAN_POINT('Ctrl Pts',(45.4662788414783,29.7849278840232,-39.3151816892667));
#270092=CARTESIAN_POINT('Ctrl Pts',(45.3948322071948,29.7466787770249,-39.2927130701762));
#270093=CARTESIAN_POINT('Ctrl Pts',(45.336485100633,29.7190029057417,-39.2750621485905));
#270094=CARTESIAN_POINT('Ctrl Pts',(45.2174821634192,29.6694332894901,-39.2404159866344));
#270095=CARTESIAN_POINT('Ctrl Pts',(45.1568212895685,29.647533012283,-39.2234183942954));
#270096=CARTESIAN_POINT('Ctrl Pts',(45.0640714235939,29.619055039813,-39.1984205234013));
#270097=CARTESIAN_POINT('Ctrl Pts',(45.032861270908,29.6102922086151,-39.1901711169105));
#270098=CARTESIAN_POINT('Ctrl Pts',(44.9698441198096,29.5942499980371,-39.1738424433647));
#270099=CARTESIAN_POINT('Ctrl Pts',(44.9380562327559,29.5869745020916,-39.1657679316868));
#270100=CARTESIAN_POINT('Ctrl Pts',(44.8737931083252,29.573925804024,-39.149775035991));
#270101=CARTESIAN_POINT('Ctrl Pts',(44.8415208853874,29.5681974475295,-39.1419079029737));
#270102=CARTESIAN_POINT('Ctrl Pts',(44.776970845224,29.5583613251754,-39.1264966011694));
#270103=CARTESIAN_POINT('Ctrl Pts',(44.7446379778246,29.554242349424,-39.1189387253041));
#270104=CARTESIAN_POINT('Ctrl Pts',(44.6475178199358,29.5442689888186,-39.0967183333452));
#270105=CARTESIAN_POINT('Ctrl Pts',(44.5825753395907,29.5407861890414,-39.0824996206453));
#270106=CARTESIAN_POINT('Ctrl Pts',(44.4523137000486,29.5401680254183,-39.0552681967223));
#270107=CARTESIAN_POINT('Ctrl Pts',(44.3869794861938,29.5430364177713,-39.042253099238));
#270108=CARTESIAN_POINT('Ctrl Pts',(44.3050948879356,29.5506999745547,-39.0267708676041));
#270109=CARTESIAN_POINT('Ctrl Pts',(44.2886956677166,29.5524407317244,-39.0237122163303));
#270110=CARTESIAN_POINT('Ctrl Pts',(44.2558932837023,29.5563326981298,-39.0176779775804));
#270111=CARTESIAN_POINT('Ctrl Pts',(44.2394573135744,29.5584895570295,-39.0146967151644));
#270112=CARTESIAN_POINT('Ctrl Pts',(44.1902801628687,29.5655670337388,-39.0059044369212));
#270113=CARTESIAN_POINT('Ctrl Pts',(44.1577489684097,29.5710783602803,-39.0002581196331));
#270114=CARTESIAN_POINT('Ctrl Pts',(44.0930902099635,29.5836780129281,-38.9893737660692));
#270115=CARTESIAN_POINT('Ctrl Pts',(44.0609787624772,29.5907638288663,-38.9841385716989));
#270116=CARTESIAN_POINT('Ctrl Pts',(43.9971881707919,29.6064950769681,-38.9740800966435));
#270117=CARTESIAN_POINT('Ctrl Pts',(43.9655090304771,29.6151405228279,-38.969256818787));
#270118=CARTESIAN_POINT('Ctrl Pts',(43.9025826910914,29.6339901792778,-38.9600230993416));
#270119=CARTESIAN_POINT('Ctrl Pts',(43.8713354893841,29.6441943800886,-38.9556126545029));
#270120=CARTESIAN_POINT('Ctrl Pts',(43.8092758314442,29.6661720973477,-38.9472084833648));
#270121=CARTESIAN_POINT('Ctrl Pts',(43.7784633658234,29.6779455796926,-38.9432147474799));
#270122=CARTESIAN_POINT('Ctrl Pts',(43.7172792568189,29.7030842010437,-38.9356509496391));
#270123=CARTESIAN_POINT('Ctrl Pts',(43.6869070838288,29.7164504701877,-38.9320810127575));
#270124=CARTESIAN_POINT('Ctrl Pts',(43.6266151921457,29.7448048716196,-38.9253745061563));
#270125=CARTESIAN_POINT('Ctrl Pts',(43.5966493659251,29.7598259498784,-38.9222351635375));
#270126=CARTESIAN_POINT('Ctrl Pts',(43.5379112806659,29.7911336867559,-38.9164715361192));
#270127=CARTESIAN_POINT('Ctrl Pts',(43.5089941631931,29.8074860237238,-38.9138306268446));
#270128=CARTESIAN_POINT('Ctrl Pts',(43.4521388277713,29.8415269250742,-38.9090343829106));
#270129=CARTESIAN_POINT('Ctrl Pts',(43.4241857920873,29.8592223311679,-38.9068773722382));
#270130=CARTESIAN_POINT('Ctrl Pts',(43.3417400360357,29.9143184778597,-38.9011252479271));
#270131=CARTESIAN_POINT('Ctrl Pts',(43.2886573738269,29.9537246686422,-38.8982474648125));
#270132=CARTESIAN_POINT('Ctrl Pts',(43.1862838907427,30.0379288436163,-38.8944239449498));
#270133=CARTESIAN_POINT('Ctrl Pts',(43.136983004927,30.0827355501013,-38.893477927521));
#270134=CARTESIAN_POINT('Ctrl Pts',(43.0423554365792,30.1779102993728,-38.893593096851));
#270135=CARTESIAN_POINT('Ctrl Pts',(42.9978715396443,30.2274270793998,-38.8946524983587));
#270136=CARTESIAN_POINT('Ctrl Pts',(42.9143010667291,30.3302227545307,-38.8986981279734));
#270137=CARTESIAN_POINT('Ctrl Pts',(42.8752237175721,30.3834938975299,-38.9016846639526));
#270138=CARTESIAN_POINT('Ctrl Pts',(42.8024397261494,30.4937517735858,-38.9095657636758));
#270139=CARTESIAN_POINT('Ctrl Pts',(42.7687347167421,30.5507433047372,-38.9144616840886));
#270140=CARTESIAN_POINT('Ctrl Pts',(42.7300278300793,30.6243427738123,-38.9217927993296));
#270141=CARTESIAN_POINT('Ctrl Pts',(42.7224591498617,30.6391844010125,-38.9233206679252));
#270142=CARTESIAN_POINT('Ctrl Pts',(42.7076683020993,30.6691039109109,-38.9264983150556));
#270143=CARTESIAN_POINT('Ctrl Pts',(42.7004432835422,30.6841920440013,-38.9281496447495));
#270144=CARTESIAN_POINT('Ctrl Pts',(42.6794143353072,30.7295580738094,-38.9332597737812));
#270145=CARTESIAN_POINT('Ctrl Pts',(42.6662166357692,30.7600070397506,-38.9368809290395));
#270146=CARTESIAN_POINT('Ctrl Pts',(42.6414216277427,30.8213220567451,-38.9445436541549));
#270147=CARTESIAN_POINT('Ctrl Pts',(42.6298250815994,30.8521852903658,-38.9485847931962));
#270148=CARTESIAN_POINT('Ctrl Pts',(42.6082082262651,30.9143167270108,-38.9570788827674));
#270149=CARTESIAN_POINT('Ctrl Pts',(42.5981879579414,30.9455849404748,-38.9615318444951));
#270150=CARTESIAN_POINT('Ctrl Pts',(42.5797100543851,31.0085229640247,-38.9708449417209));
#270151=CARTESIAN_POINT('Ctrl Pts',(42.5712524352517,31.0401927781745,-38.9757050820557));
#270152=CARTESIAN_POINT('Ctrl Pts',(42.5558976643663,31.1039335760284,-38.9858308250948));
#270153=CARTESIAN_POINT('Ctrl Pts',(42.5490005053429,31.1360045577763,-38.9910964266694));
#270154=CARTESIAN_POINT('Ctrl Pts',(42.5367758515694,31.2005501914637,-39.0020342749577));
#270155=CARTESIAN_POINT('Ctrl Pts',(42.5314471712796,31.2330404201865,-39.007709523219));
#270156=CARTESIAN_POINT('Ctrl Pts',(42.5223849923266,31.2983677257365,-39.0194587805602));
#270157=CARTESIAN_POINT('Ctrl Pts',(42.5186403552644,31.3313583601098,-39.0255624829972));
#270158=CARTESIAN_POINT('Ctrl Pts',(42.5128293460636,31.3970657507066,-39.038055061464));
#270159=CARTESIAN_POINT('Ctrl Pts',(42.5107468075751,31.4298508641049,-39.0444548642532));
#270160=CARTESIAN_POINT('Ctrl Pts',(42.5081970620853,31.4952703256329,-39.0575511235813));
#270161=CARTESIAN_POINT('Ctrl Pts',(42.5077288537135,31.5279075248247,-39.0642479703919));
#270162=CARTESIAN_POINT('Ctrl Pts',(42.5087067479981,31.6256052084393,-39.0847758818791));
#270163=CARTESIAN_POINT('Ctrl Pts',(42.5125304809965,31.6904522179578,-39.0990434188884));
#270164=CARTESIAN_POINT('Ctrl Pts',(42.5229811189973,31.7873005996235,-39.1213030342398));
#270165=CARTESIAN_POINT('Ctrl Pts',(42.5272518260001,31.8195129184735,-39.1288662059234));
#270166=CARTESIAN_POINT('Ctrl Pts',(42.5373776944208,31.883795893367,-39.1442798245848));
#270167=CARTESIAN_POINT('Ctrl Pts',(42.5432345666966,31.9158715468512,-39.1521316546249));
#270168=CARTESIAN_POINT('Ctrl Pts',(42.5565470612704,31.979859498611,-39.168119763369));
#270169=CARTESIAN_POINT('Ctrl Pts',(42.5640260671368,32.0118444622012,-39.1762758410947));
#270170=CARTESIAN_POINT('Ctrl Pts',(42.5804532704541,32.0750557648418,-39.1927214573391));
#270171=CARTESIAN_POINT('Ctrl Pts',(42.5894227227712,32.106396161248,-39.2010390020672));
#270172=CARTESIAN_POINT('Ctrl Pts',(42.6088418543565,32.1684870422805,-39.2178439045483));
#270173=CARTESIAN_POINT('Ctrl Pts',(42.6192936389916,32.1992486628788,-39.226334003443));
#270174=CARTESIAN_POINT('Ctrl Pts',(42.6416735245966,32.2602075594843,-39.2434876394842));
#270175=CARTESIAN_POINT('Ctrl Pts',(42.6536016315145,32.290404833084,-39.2521511779583));
#270176=CARTESIAN_POINT('Ctrl Pts',(42.6789366404289,32.3502342598595,-39.2696511714811));
#270177=CARTESIAN_POINT('Ctrl Pts',(42.6923367443656,32.3798518740678,-39.2784832479687));
#270178=CARTESIAN_POINT('Ctrl Pts',(42.7206559859697,32.4385753054162,-39.2963386321761));
#270179=CARTESIAN_POINT('Ctrl Pts',(42.7355220126264,32.4675648427258,-39.3053271639861));
#270180=CARTESIAN_POINT('Ctrl Pts',(42.7819686876355,32.5529513552204,-39.3323236941673));
#270181=CARTESIAN_POINT('Ctrl Pts',(42.8154843714806,32.6080042266715,-39.350429376845));
#270182=CARTESIAN_POINT('Ctrl Pts',(42.8874714697309,32.7144015518502,-39.3868314468607));
#270183=CARTESIAN_POINT('Ctrl Pts',(42.9259451142984,32.7657569305986,-39.405130570804));
#270184=CARTESIAN_POINT('Ctrl Pts',(42.9873802660617,32.8400220747848,-39.4327251562925));
#270185=CARTESIAN_POINT('Ctrl Pts',(43.0084803849644,32.8643150897193,-39.4419477180718));
#270186=CARTESIAN_POINT('Ctrl Pts',(43.0519381822279,32.911966602613,-39.460442053495));
#270187=CARTESIAN_POINT('Ctrl Pts',(43.0742932293765,32.9353217065842,-39.4697125999696));
#270188=CARTESIAN_POINT('Ctrl Pts',(43.1202941152109,32.9810940910691,-39.4883087327733));
#270189=CARTESIAN_POINT('Ctrl Pts',(43.1439529159728,33.0035126604972,-39.4976371211004));
#270190=CARTESIAN_POINT('Ctrl Pts',(43.1920211429799,33.0468913167546,-39.5161342576841));
#270191=CARTESIAN_POINT('Ctrl Pts',(43.2165352643027,33.0679574354316,-39.5253457202097));
#270192=CARTESIAN_POINT('Ctrl Pts',(43.2913474244647,33.1291646243131,-39.5528104082097));
#270193=CARTESIAN_POINT('Ctrl Pts',(43.3430301425081,33.1674361598715,-39.5709418650873));
#270194=CARTESIAN_POINT('Ctrl Pts',(43.4231858671606,33.2210184664833,-39.5978530872083));
#270195=CARTESIAN_POINT('Ctrl Pts',(43.4503469560668,33.2382438729789,-39.6067770568578));
#270196=CARTESIAN_POINT('Ctrl Pts',(43.5055597590889,33.2714157254684,-39.6245320627911));
#270197=CARTESIAN_POINT('Ctrl Pts',(43.5336114345675,33.2873622273092,-39.6333631021097));
#270198=CARTESIAN_POINT('Ctrl Pts',(43.5906171763999,33.3179591419151,-39.6509316376977));
#270199=CARTESIAN_POINT('Ctrl Pts',(43.6195686807026,33.3326076488467,-39.6596682334695));
#270200=CARTESIAN_POINT('Ctrl Pts',(43.6784027873839,33.3605894168931,-39.6770502813188));
#270201=CARTESIAN_POINT('Ctrl Pts',(43.7083065099628,33.3739233472053,-39.6857000236169));
#270202=CARTESIAN_POINT('Ctrl Pts',(43.7683635828038,33.3989600904335,-39.7027096012684));
#270203=CARTESIAN_POINT('Ctrl Pts',(43.7986441240576,33.410725045928,-39.7111073577373));
#270204=CARTESIAN_POINT('Ctrl Pts',(43.8596239235883,33.4327283064733,-39.7276688298622));
#270205=CARTESIAN_POINT('Ctrl Pts',(43.8903364640963,33.4429729918037,-39.7358364820756));
#270206=CARTESIAN_POINT('Ctrl Pts',(43.9831381693492,33.4714483547834,-39.760003404431));
#270207=CARTESIAN_POINT('Ctrl Pts',(44.0458899425586,33.4874253805623,-39.7756673535664));
#270208=CARTESIAN_POINT('Ctrl Pts',(44.1413568263141,33.5068320087337,-39.7984910804967));
#270209=CARTESIAN_POINT('Ctrl Pts',(44.1734026620325,33.512539916883,-39.8059867898386));
#270210=CARTESIAN_POINT('Ctrl Pts',(44.2379485985024,33.5224086377434,-39.8207511924796));
#270211=CARTESIAN_POINT('Ctrl Pts',(44.2704344157376,33.5265678396433,-39.8280167344336));
#270212=CARTESIAN_POINT('Ctrl Pts',(44.31955450659,33.5316239864186,-39.8387510991363));
#270213=CARTESIAN_POINT('Ctrl Pts',(44.3359803233845,33.5331096864767,-39.8422988490203));
#270214=CARTESIAN_POINT('Ctrl Pts',(44.3687702925121,33.5356678958833,-39.8492980293521));
#270215=CARTESIAN_POINT('Ctrl Pts',(44.3851668896783,33.5367439047296,-39.8527565827752));
#270216=CARTESIAN_POINT('Ctrl Pts',(44.4343055941691,33.5393615686568,-39.8629980872985));
#270217=CARTESIAN_POINT('Ctrl Pts',(44.467043811667,33.5402980820414,-39.8696572702326));
#270218=CARTESIAN_POINT('Ctrl Pts',(44.5651280609268,33.5407002285591,-39.8891214986439));
#270219=CARTESIAN_POINT('Ctrl Pts',(44.6303961191261,33.5377689750917,-39.9014257084291));
#270220=CARTESIAN_POINT('Ctrl Pts',(44.7606551553719,33.5254981705544,-39.9246908296974));
#270221=CARTESIAN_POINT('Ctrl Pts',(44.8256640685817,33.5161533726516,-39.9356542165744));
#270222=CARTESIAN_POINT('Ctrl Pts',(44.906721867411,33.5003619888654,-39.9484974119658));
#270223=CARTESIAN_POINT('Ctrl Pts',(44.9229346750623,33.4969927872433,-39.9510241738426));
#270224=CARTESIAN_POINT('Ctrl Pts',(44.9553219764425,33.4898425172325,-39.9559880147365));
#270225=CARTESIAN_POINT('Ctrl Pts',(44.9715284344022,33.4860526078472,-39.958429637772));
#270226=CARTESIAN_POINT('Ctrl Pts',(45.0199627900161,33.4740854281601,-39.9655990795304));
#270227=CARTESIAN_POINT('Ctrl Pts',(45.0519106460378,33.4653389646544,-39.9701583622527));
#270228=CARTESIAN_POINT('Ctrl Pts',(45.1152342592699,33.4463085275747,-39.9788590382424));
#270229=CARTESIAN_POINT('Ctrl Pts',(45.1465931161906,33.4360289026411,-39.9829979637287));
#270230=CARTESIAN_POINT('Ctrl Pts',(45.2087103117349,33.4139546170134,-39.9908577188348));
#270231=CARTESIAN_POINT('Ctrl Pts',(45.2394686437959,33.4021599396053,-39.9945785431013));
#270232=CARTESIAN_POINT('Ctrl Pts',(45.3003857153532,33.3770580671335,-40.0016036322017));
#270233=CARTESIAN_POINT('Ctrl Pts',(45.3305444573974,33.3637508783763,-40.0049078982014));
#270234=CARTESIAN_POINT('Ctrl Pts',(45.390258886243,33.3356154142248,-40.011098275424));
#270235=CARTESIAN_POINT('Ctrl Pts',(45.4198145849242,33.3207871687102,-40.0139843944556));
#270236=CARTESIAN_POINT('Ctrl Pts',(45.4783149483493,33.2895896149825,-40.01933367126));
#270237=CARTESIAN_POINT('Ctrl Pts',(45.507262517348,33.2732175573309,-40.0217968588865));
#270238=CARTESIAN_POINT('Ctrl Pts',(45.5645222978915,33.2389114608181,-40.0262919941319));
#270239=CARTESIAN_POINT('Ctrl Pts',(45.5928960780074,33.2209281679648,-40.0283263501325));
#270240=CARTESIAN_POINT('Ctrl Pts',(45.6483112696052,33.1838254126132,-40.0319112250503));
#270241=CARTESIAN_POINT('Ctrl Pts',(45.6754897776133,33.1646269393907,-40.033473120182));
#270242=CARTESIAN_POINT('Ctrl Pts',(45.7287236826122,33.1250040552468,-40.0361368706617));
#270243=CARTESIAN_POINT('Ctrl Pts',(45.7547928320097,33.1045715914186,-40.0372398412512));
#270244=CARTESIAN_POINT('Ctrl Pts',(45.8313713764485,33.0414275867026,-40.0398685197573));
#270245=CARTESIAN_POINT('Ctrl Pts',(45.8802555440049,32.9968736013142,-40.0407155796136));
#270246=CARTESIAN_POINT('Ctrl Pts',(45.9503135478119,32.9263375747907,-40.0406220600909));
#270247=CARTESIAN_POINT('Ctrl Pts',(45.9731206268418,32.9022070589556,-40.0403631547939));
#270248=CARTESIAN_POINT('Ctrl Pts',(46.0176283770391,32.8526917463635,-40.0393834530318));
#270249=CARTESIAN_POINT('Ctrl Pts',(46.0393233161468,32.8273141108128,-40.0386629364799));
#270250=CARTESIAN_POINT('Ctrl Pts',(46.0816063372946,32.7752494087917,-40.0367489513753));
#270251=CARTESIAN_POINT('Ctrl Pts',(46.1020200031328,32.7487743967956,-40.0355628438162));
#270252=CARTESIAN_POINT('Ctrl Pts',(46.1413455248285,32.6950606561891,-40.0327468789706));
#270253=CARTESIAN_POINT('Ctrl Pts',(46.1602720912561,32.6678035871797,-40.0311163104268));
#270254=CARTESIAN_POINT('Ctrl Pts',(46.2148746530555,32.5848590029048,-40.0255677342833));
#270255=CARTESIAN_POINT('Ctrl Pts',(46.2483818229377,32.5279958230559,-40.0209940857161));
#270256=CARTESIAN_POINT('Ctrl Pts',(46.3096688668557,32.4111729744312,-40.0101125434596));
#270257=CARTESIAN_POINT('Ctrl Pts',(46.3374502738645,32.3511989868894,-40.0038021480578));
#270258=CARTESIAN_POINT('Ctrl Pts',(46.368527809654,32.2742945109209,-39.99481246295));
#270259=CARTESIAN_POINT('Ctrl Pts',(46.3745625031242,32.2588039482195,-39.9929572402591));
#270260=CARTESIAN_POINT('Ctrl Pts',(46.3862570590194,32.2276457996089,-39.9891378326849));
#270261=CARTESIAN_POINT('Ctrl Pts',(46.3919277006514,32.2119441234091,-39.9871690698157));
#270262=CARTESIAN_POINT('Ctrl Pts',(46.4083204627969,32.1647096562841,-39.9811146940715));
#270263=CARTESIAN_POINT('Ctrl Pts',(46.4183992792463,32.1331328020619,-39.9768930221268));
#270264=CARTESIAN_POINT('Ctrl Pts',(46.4369323752314,32.0697100737179,-39.9680740796957));
#270265=CARTESIAN_POINT('Ctrl Pts',(46.4453810238695,32.0378809710586,-39.9634789966875));
#270266=CARTESIAN_POINT('Ctrl Pts',(46.4606707140735,31.9739914674526,-39.9539230277982));
#270267=CARTESIAN_POINT('Ctrl Pts',(46.4675116609156,31.9419310527617,-39.9489621213728));
#270268=CARTESIAN_POINT('Ctrl Pts',(46.4856471656838,31.8454065140233,-39.9335346428238));
#270269=CARTESIAN_POINT('Ctrl Pts',(46.4945595050313,31.7805939086316,-39.9225233405268));
#270270=CARTESIAN_POINT('Ctrl Pts',(46.5031525845005,31.682706857495,-39.9049137240114));
#270271=CARTESIAN_POINT('Ctrl Pts',(46.5052196048422,31.6499521123145,-39.8988586119036));
#270272=CARTESIAN_POINT('Ctrl Pts',(46.5071100859963,31.6006666000752,-39.8895013323517));
#270273=CARTESIAN_POINT('Ctrl Pts',(46.5075383370072,31.5841997621947,-39.8863338999606));
#270274=CARTESIAN_POINT('Ctrl Pts',(46.5079880490572,31.5512292566173,-39.8799094799294));
#270275=CARTESIAN_POINT('Ctrl Pts',(46.5080089473365,31.5346906881349,-39.8766454813005));
#270276=CARTESIAN_POINT('Ctrl Pts',(46.5074573980809,31.4851841124548,-39.8667505882022));
#270277=CARTESIAN_POINT('Ctrl Pts',(46.5062766666147,31.4523784018193,-39.8600285058855));
#270278=CARTESIAN_POINT('Ctrl Pts',(46.5023268283512,31.3870651032717,-39.8463202210145));
#270279=CARTESIAN_POINT('Ctrl Pts',(46.4995580430915,31.3545727204625,-39.8393370895085));
#270280=CARTESIAN_POINT('Ctrl Pts',(46.4889122836107,31.2575799370501,-39.8180059067137));
#270281=CARTESIAN_POINT('Ctrl Pts',(46.4787005768383,31.1935629350167,-39.8032768261342));
#270282=CARTESIAN_POINT('Ctrl Pts',(46.4587745183326,31.098492744583,-39.7804246588118));
#270283=CARTESIAN_POINT('Ctrl Pts',(46.4513631036993,31.0669621704925,-39.7726806371984));
#270284=CARTESIAN_POINT('Ctrl Pts',(46.4349953704741,31.0042214510855,-39.7569372896318));
#270285=CARTESIAN_POINT('Ctrl Pts',(46.426038976159,30.973010935597,-39.7489378760851));
#270286=CARTESIAN_POINT('Ctrl Pts',(46.4065648883721,30.9109154529952,-39.7326803432244));
#270287=CARTESIAN_POINT('Ctrl Pts',(46.3960429010861,30.8800187258512,-39.7244190196926));
#270288=CARTESIAN_POINT('Ctrl Pts',(46.3734248182074,30.8185999023854,-39.7076436938793));
#270289=CARTESIAN_POINT('Ctrl Pts',(46.3614222035831,30.7883284740624,-39.6991983942538));
#270290=CARTESIAN_POINT('Ctrl Pts',(46.3487330454107,30.7584586806226,-39.6906893116447));
#270291=CARTESIAN_POINT('Ctrl Pts',(44.6028102757013,33.538203052834,-39.8960581756957));
#270292=CARTESIAN_POINT('Ctrl Pts',(44.5684884519592,33.5398325791396,-39.8896053029486));
#270293=CARTESIAN_POINT('Ctrl Pts',(44.5341306228379,33.5405765787541,-39.8829664139251));
#270294=CARTESIAN_POINT('Ctrl Pts',(44.4997391850464,33.5404355737569,-39.8761416497953));
#270295=CARTESIAN_POINT('Ctrl Pts',(44.4670443896497,33.5403015249987,-39.8696535736582));
#270296=CARTESIAN_POINT('Ctrl Pts',(44.4343061264537,33.5393650105759,-39.8629943907241));
#270297=CARTESIAN_POINT('Ctrl Pts',(44.4015469444054,33.5376198991251,-39.8561667210419));
#270298=CARTESIAN_POINT('Ctrl Pts',(44.3851673533813,33.5367473433996,-39.8527528862008));
#270299=CARTESIAN_POINT('Ctrl Pts',(44.3687707333322,33.5356713331865,-39.8492943327777));
#270300=CARTESIAN_POINT('Ctrl Pts',(44.3523757258895,33.5343922268333,-39.8457947426118));
#270301=CARTESIAN_POINT('Ctrl Pts',(44.3359807184467,33.53311312048,-39.8422951524459));
#270302=CARTESIAN_POINT('Ctrl Pts',(44.3195548787318,33.5316274184839,-39.8387474025619));
#270303=CARTESIAN_POINT('Ctrl Pts',(44.3031814922686,33.5299420340084,-39.8351692809943));
#270304=CARTESIAN_POINT('Ctrl Pts',(44.2704347193421,33.5265712650576,-39.8280130378592));
#270305=CARTESIAN_POINT('Ctrl Pts',(44.2379488567859,33.5224120576217,-39.8207474959053));
#270306=CARTESIAN_POINT('Ctrl Pts',(44.2056758435329,33.5174776905724,-39.8133652945847));
#270307=CARTESIAN_POINT('Ctrl Pts',(44.1734028307723,33.5125433235984,-39.8059830933769));
#270308=CARTESIAN_POINT('Ctrl Pts',(44.1413569694056,33.506835411636,-39.7984873881882));
#270309=CARTESIAN_POINT('Ctrl Pts',(44.1095346139294,33.5003666523966,-39.7908793336944));
#270310=CARTESIAN_POINT('Ctrl Pts',(44.0458899015202,33.4874291336216,-39.7756632243584));
#270311=CARTESIAN_POINT('Ctrl Pts',(43.9831381149063,33.471452179088,-39.759999220822));
#270312=CARTESIAN_POINT('Ctrl Pts',(43.9212701806475,33.4524682573117,-39.7438882601));
#270313=CARTESIAN_POINT('Ctrl Pts',(43.8903362137541,33.4429762964961,-39.7358327798005));
#270314=CARTESIAN_POINT('Ctrl Pts',(43.8596236543864,33.432731604347,-39.7276651332879));
#270315=CARTESIAN_POINT('Ctrl Pts',(43.8291337121394,33.421729958977,-39.7193843972254));
#270316=CARTESIAN_POINT('Ctrl Pts',(43.7986437698924,33.4107283136069,-39.7111036611629));
#270317=CARTESIAN_POINT('Ctrl Pts',(43.7683631864552,33.3989633419485,-39.7027059046941));
#270318=CARTESIAN_POINT('Ctrl Pts',(43.7383346082092,33.3864449531174,-39.6942011158683));
#270319=CARTESIAN_POINT('Ctrl Pts',(43.7083060299631,33.3739265642863,-39.6856963270425));
#270320=CARTESIAN_POINT('Ctrl Pts',(43.6784022657394,33.3605926156183,-39.6770465847445));
#270321=CARTESIAN_POINT('Ctrl Pts',(43.6489851714386,33.3466017123189,-39.6683555608198));
#270322=CARTESIAN_POINT('Ctrl Pts',(43.6195680771379,33.3326108090195,-39.6596645368951));
#270323=CARTESIAN_POINT('Ctrl Pts',(43.5906156336918,33.3179617994446,-39.6509276635309));
#270324=CARTESIAN_POINT('Ctrl Pts',(43.5621135894733,33.3026639516225,-39.6421434977462));
#270325=CARTESIAN_POINT('Ctrl Pts',(43.5336113200827,33.2873659829441,-39.6333592625648));
#270326=CARTESIAN_POINT('Ctrl Pts',(43.5055593687618,33.2714193184022,-39.6245281992176));
#270327=CARTESIAN_POINT('Ctrl Pts',(43.4779525093745,33.2548330333127,-39.6156506437734));
#270328=CARTESIAN_POINT('Ctrl Pts',(43.4503460861836,33.2382470102913,-39.6067732285971));
#270329=CARTESIAN_POINT('Ctrl Pts',(43.4231847792171,33.2210213314943,-39.5978493197658));
#270330=CARTESIAN_POINT('Ctrl Pts',(43.3964663782543,33.2031606790307,-39.5888789832603));
#270331=CARTESIAN_POINT('Ctrl Pts',(43.3430291541635,33.1674390918953,-39.5709381685129));
#270332=CARTESIAN_POINT('Ctrl Pts',(43.2913463642683,33.129167503371,-39.5528067116353));
#270333=CARTESIAN_POINT('Ctrl Pts',(43.2414715215205,33.088362654268,-39.5344969196353));
#270334=CARTESIAN_POINT('Ctrl Pts',(43.2165341001466,33.0679602297166,-39.5253420236353));
#270335=CARTESIAN_POINT('Ctrl Pts',(43.1920199447671,33.0468940818524,-39.5161305611097));
#270336=CARTESIAN_POINT('Ctrl Pts',(43.1679857978823,33.0252047236631,-39.5068819928179));
#270337=CARTESIAN_POINT('Ctrl Pts',(43.1439516509975,33.0035153654738,-39.497633424526));
#270338=CARTESIAN_POINT('Ctrl Pts',(43.1202928173846,32.9810967649645,-39.4883050361989));
#270339=CARTESIAN_POINT('Ctrl Pts',(43.0972923425396,32.9582105409828,-39.4790069697971));
#270340=CARTESIAN_POINT('Ctrl Pts',(43.0742918676945,32.9353243170012,-39.4697089033952));
#270341=CARTESIAN_POINT('Ctrl Pts',(43.0519360617005,32.9119683859121,-39.460438038431));
#270342=CARTESIAN_POINT('Ctrl Pts',(43.0302080409885,32.8881435936574,-39.451191262225));
#270343=CARTESIAN_POINT('Ctrl Pts',(43.0084800202764,32.8643188014027,-39.4419444860189));
#270344=CARTESIAN_POINT('Ctrl Pts',(42.9873794912476,32.8400253900556,-39.4327217732547));
#270345=CARTESIAN_POINT('Ctrl Pts',(42.9669007794172,32.8152701048891,-39.4235233479461));
#270346=CARTESIAN_POINT('Ctrl Pts',(42.9259433557564,32.7657595345561,-39.4051264973289));
#270347=CARTESIAN_POINT('Ctrl Pts',(42.8874698490093,32.7144038555933,-39.3868277502863));
#270348=CARTESIAN_POINT('Ctrl Pts',(42.8514762500672,32.661205119079,-39.3686267152785));
#270349=CARTESIAN_POINT('Ctrl Pts',(42.8154826511251,32.6080063825646,-39.3504256802706));
#270350=CARTESIAN_POINT('Ctrl Pts',(42.7819669209395,32.5529534345799,-39.332319997593));
#270351=CARTESIAN_POINT('Ctrl Pts',(42.7510024281725,32.4960290137494,-39.3143223108055));
#270352=CARTESIAN_POINT('Ctrl Pts',(42.735520181789,32.4675668033342,-39.3053234674117));
#270353=CARTESIAN_POINT('Ctrl Pts',(42.7206541346169,32.4385772256996,-39.2963349356017));
#270354=CARTESIAN_POINT('Ctrl Pts',(42.7064944942894,32.4092154691749,-39.287407243498));
#270355=CARTESIAN_POINT('Ctrl Pts',(42.6923348539619,32.3798537126501,-39.2784795513943));
#270356=CARTESIAN_POINT('Ctrl Pts',(42.678934731563,32.3502360572277,-39.2696474749068));
#270357=CARTESIAN_POINT('Ctrl Pts',(42.6662672096693,32.3203213022045,-39.2608974781453));
#270358=CARTESIAN_POINT('Ctrl Pts',(46.6981266849492,30.7091523375488,-39.2904704603133));
#270359=CARTESIAN_POINT('Ctrl Pts',(46.6689684123063,30.6404043382273,-39.273452295095));
#270360=CARTESIAN_POINT('Ctrl Pts',(46.6043681216411,30.5066861069553,-39.238925705885));
#270361=CARTESIAN_POINT('Ctrl Pts',(46.5083209189471,30.3487389562033,-39.1945593129175));
#270362=CARTESIAN_POINT('Ctrl Pts',(46.4437937583117,30.2581216171786,-39.1673894861782));
#270363=CARTESIAN_POINT('Ctrl Pts',(46.3992224148768,30.1986447451181,-39.1491520227249));
#270364=CARTESIAN_POINT('Ctrl Pts',(46.3761748773305,30.1693908446446,-39.1399767764946));
#270365=CARTESIAN_POINT('Ctrl Pts',(46.3284414024809,30.1117648114071,-39.1214771434543));
#270366=CARTESIAN_POINT('Ctrl Pts',(46.3038983378397,30.083571828401,-39.112209259666));
#270367=CARTESIAN_POINT('Ctrl Pts',(46.253707387608,30.0286632749651,-39.0937226519629));
#270368=CARTESIAN_POINT('Ctrl Pts',(46.2280147026909,30.001893564456,-39.0844865568113));
#270369=CARTESIAN_POINT('Ctrl Pts',(46.1492148010453,29.9236586721517,-39.0568159196779));
#270370=CARTESIAN_POINT('Ctrl Pts',(46.0669347173688,29.8495134741745,-39.0292038481275));
#270371=CARTESIAN_POINT('Ctrl Pts',(45.9503410384262,29.7587889734315,-38.9925114043613));
#270372=CARTESIAN_POINT('Ctrl Pts',(45.8594191065401,29.6948377475824,-38.9650526418885));
#270373=CARTESIAN_POINT('Ctrl Pts',(45.7964751089327,29.6549785818455,-38.9467936623891));
#270374=CARTESIAN_POINT('Ctrl Pts',(45.748348603817,29.6261284949947,-38.9331097524421));
#270375=CARTESIAN_POINT('Ctrl Pts',(45.7321473284057,29.616684052073,-38.9285487676403));
#270376=CARTESIAN_POINT('Ctrl Pts',(45.6996106203311,29.5982459977232,-38.9194791520014));
#270377=CARTESIAN_POINT('Ctrl Pts',(45.683249044345,29.5892352448745,-38.9149628379356));
#270378=CARTESIAN_POINT('Ctrl Pts',(45.6010439155842,29.5452684013657,-38.8924942188443));
#270379=CARTESIAN_POINT('Ctrl Pts',(45.4667739830181,29.4816584171599,-38.8571935516581));
#270380=CARTESIAN_POINT('Ctrl Pts',(45.2922645146651,29.4187721922835,-38.8147007629208));
#270381=CARTESIAN_POINT('Ctrl Pts',(45.184512437616,29.3885937253944,-38.7899522655792));
#270382=CARTESIAN_POINT('Ctrl Pts',(45.1119891467798,29.3701842541612,-38.7736235920333));
#270383=CARTESIAN_POINT('Ctrl Pts',(45.0754052578815,29.3618381514785,-38.7655490803555));
#270384=CARTESIAN_POINT('Ctrl Pts',(45.0014447932705,29.3468760834356,-38.7495561846596));
#270385=CARTESIAN_POINT('Ctrl Pts',(44.964301863367,29.3403115562353,-38.7416890516424));
#270386=CARTESIAN_POINT('Ctrl Pts',(44.8900079594565,29.3290481892184,-38.726277749838));
#270387=CARTESIAN_POINT('Ctrl Pts',(44.8527936282157,29.324336495618,-38.7187198739728));
#270388=CARTESIAN_POINT('Ctrl Pts',(44.7410083373266,29.3129455735289,-38.6964994820139));
#270389=CARTESIAN_POINT('Ctrl Pts',(44.6662563757167,29.3089967422249,-38.6822807693139));
#270390=CARTESIAN_POINT('Ctrl Pts',(44.516312468428,29.3084067934202,-38.6550493453909));
#270391=CARTESIAN_POINT('Ctrl Pts',(44.441103189525,29.3117700143417,-38.6420342479066));
#270392=CARTESIAN_POINT('Ctrl Pts',(44.3468378615956,29.3206690055189,-38.6265520162729));
#270393=CARTESIAN_POINT('Ctrl Pts',(44.3279589148655,29.3226883315868,-38.6234933649988));
#270394=CARTESIAN_POINT('Ctrl Pts',(44.2901960653062,29.3271995080042,-38.6174591262491));
#270395=CARTESIAN_POINT('Ctrl Pts',(44.271274393292,29.329697893027,-38.614477863833));
#270396=CARTESIAN_POINT('Ctrl Pts',(44.2146592782019,29.3378915995821,-38.60568558559));
#270397=CARTESIAN_POINT('Ctrl Pts',(44.1772069502033,29.344266758826,-38.6000392683017));
#270398=CARTESIAN_POINT('Ctrl Pts',(44.0655444875092,29.3661148598052,-38.5837127379559));
#270399=CARTESIAN_POINT('Ctrl Pts',(43.9553791862171,29.3933792052515,-38.5686255047386));
#270400=CARTESIAN_POINT('Ctrl Pts',(43.8114622524781,29.4404829778103,-38.5509833019505));
#270401=CARTESIAN_POINT('Ctrl Pts',(43.705021834675,29.481230340464,-38.5390021142185));
#270402=CARTESIAN_POINT('Ctrl Pts',(43.6350719757086,29.512061063653,-38.5318621614261));
#270403=CARTESIAN_POINT('Ctrl Pts',(43.5656410085295,29.5447591316771,-38.525155654825));
#270404=CARTESIAN_POINT('Ctrl Pts',(43.5311320054746,29.5620794464364,-38.5220163122062));
#270405=CARTESIAN_POINT('Ctrl Pts',(43.4634866412134,29.5981758355574,-38.5162526847879));
#270406=CARTESIAN_POINT('Ctrl Pts',(43.4301834663392,29.6170276546,-38.5136117755133));
#270407=CARTESIAN_POINT('Ctrl Pts',(43.3647025891651,29.6562685687332,-38.5088155315793));
#270408=CARTESIAN_POINT('Ctrl Pts',(43.2681192378476,29.7174608121974,-38.5023448938576));
#270409=CARTESIAN_POINT('Ctrl Pts',(43.1764049274077,29.7855824582168,-38.4980286134812));
#270410=CARTESIAN_POINT('Ctrl Pts',(43.0584774180437,29.8826126224142,-38.4942050936184));
#270411=CARTESIAN_POINT('Ctrl Pts',(43.001681818637,29.9342392650769,-38.4932590761897));
#270412=CARTESIAN_POINT('Ctrl Pts',(42.8926599718677,30.0438904492243,-38.4933742455196));
#270413=CARTESIAN_POINT('Ctrl Pts',(42.8414047150844,30.1009342501745,-38.4944336470273));
#270414=CARTESIAN_POINT('Ctrl Pts',(42.7451036203247,30.2193471227021,-38.498479276642));
#270415=CARTESIAN_POINT('Ctrl Pts',(42.6550322643363,30.3420646399833,-38.5044516702661));
#270416=CARTESIAN_POINT('Ctrl Pts',(42.5773225406025,30.4733365238586,-38.5142428327574));
#270417=CARTESIAN_POINT('Ctrl Pts',(42.5326943378214,30.5580963840027,-38.5215739479982));
#270418=CARTESIAN_POINT('Ctrl Pts',(42.5239673850246,30.5751883092729,-38.5231018165939));
#270419=CARTESIAN_POINT('Ctrl Pts',(42.5069121510755,30.60964376351,-38.5262794637242));
#270420=CARTESIAN_POINT('Ctrl Pts',(42.4985805781952,30.627019094627,-38.5279307934181));
#270421=CARTESIAN_POINT('Ctrl Pts',(42.4743295471271,30.6792614198295,-38.5330409224498));
#270422=CARTESIAN_POINT('Ctrl Pts',(42.4438856226513,30.7493896366731,-38.5402834483744));
#270423=CARTESIAN_POINT('Ctrl Pts',(42.4037483179465,30.8560072598611,-38.5524071291592));
#270424=CARTESIAN_POINT('Ctrl Pts',(42.3690543371876,30.9640160484273,-38.5657659376104));
#270425=CARTESIAN_POINT('Ctrl Pts',(42.3397558527982,31.0734075527136,-38.5803463747351));
#270426=CARTESIAN_POINT('Ctrl Pts',(42.3238156343608,31.1472555030051,-38.5908775753381));
#270427=CARTESIAN_POINT('Ctrl Pts',(42.3096820427396,31.2215665449467,-38.6018154236264));
#270428=CARTESIAN_POINT('Ctrl Pts',(42.3035171869091,31.2589715314082,-38.6074906718877));
#270429=CARTESIAN_POINT('Ctrl Pts',(42.2930235524414,31.3341791410138,-38.6192399292287));
#270430=CARTESIAN_POINT('Ctrl Pts',(42.2886818075092,31.3721585359098,-38.6253436316658));
#270431=CARTESIAN_POINT('Ctrl Pts',(42.281930630611,31.4478003630713,-38.6378362101326));
#270432=CARTESIAN_POINT('Ctrl Pts',(42.277074994566,31.5232809912004,-38.6506356205751));
#270433=CARTESIAN_POINT('Ctrl Pts',(42.2747992363309,31.6735553614761,-38.6774229397946));
#270434=CARTESIAN_POINT('Ctrl Pts',(42.2834818483937,31.8228397562226,-38.7059581415094));
#270435=CARTESIAN_POINT('Ctrl Pts',(42.3030248127084,31.9711385758679,-38.7362097844166));
#270436=CARTESIAN_POINT('Ctrl Pts',(42.3164494406915,32.0449687602614,-38.7519128032936));
#270437=CARTESIAN_POINT('Ctrl Pts',(42.3317154579634,32.1186122141692,-38.7679009120377));
#270438=CARTESIAN_POINT('Ctrl Pts',(42.3402956643805,32.1554227583218,-38.7760569897633));
#270439=CARTESIAN_POINT('Ctrl Pts',(42.3591481714288,32.228169160774,-38.7925026060078));
#270440=CARTESIAN_POINT('Ctrl Pts',(42.3694448348212,32.2642362896146,-38.8008201507359));
#270441=CARTESIAN_POINT('Ctrl Pts',(42.4028917825415,32.3714169561226,-38.8260275044574));
#270442=CARTESIAN_POINT('Ctrl Pts',(42.428602574983,32.4415633880281,-38.8431823298655));
#270443=CARTESIAN_POINT('Ctrl Pts',(42.4722685042023,32.5448307979217,-38.8694323201497));
#270444=CARTESIAN_POINT('Ctrl Pts',(42.4876674804306,32.5789105800712,-38.8782643966373));
#270445=CARTESIAN_POINT('Ctrl Pts',(42.5202146590728,32.6464795812123,-38.8961197808447));
#270446=CARTESIAN_POINT('Ctrl Pts',(42.5373018269229,32.6798350022668,-38.9051083126545));
#270447=CARTESIAN_POINT('Ctrl Pts',(42.5906929412925,32.7780783962456,-38.9321048428364));
#270448=CARTESIAN_POINT('Ctrl Pts',(42.629225789877,32.8414173722334,-38.9502105255135));
#270449=CARTESIAN_POINT('Ctrl Pts',(42.7120000069194,32.9638220552461,-38.9866125955294));
#270450=CARTESIAN_POINT('Ctrl Pts',(42.7783647966162,33.0524402968179,-39.0140612314234));
#270451=CARTESIAN_POINT('Ctrl Pts',(42.8754380724448,33.1642175243331,-39.0509520337677));
#270452=CARTESIAN_POINT('Ctrl Pts',(42.9268673384212,33.2179450225078,-39.0694937486382));
#270453=CARTESIAN_POINT('Ctrl Pts',(42.9797817061918,33.2705900457306,-39.088089881442));
#270454=CARTESIAN_POINT('Ctrl Pts',(43.0069972096607,33.2963736994336,-39.097418269769));
#270455=CARTESIAN_POINT('Ctrl Pts',(43.0622936398443,33.3462615369726,-39.1159154063528));
#270456=CARTESIAN_POINT('Ctrl Pts',(43.0904949946047,33.3704876748183,-39.1251268688783));
#270457=CARTESIAN_POINT('Ctrl Pts',(43.176562606447,33.4408730143712,-39.1525915568785));
#270458=CARTESIAN_POINT('Ctrl Pts',(43.2360245534179,33.4848790444095,-39.1707230137558));
#270459=CARTESIAN_POINT('Ctrl Pts',(43.358992255749,33.5670176609587,-39.2066046432507));
#270460=CARTESIAN_POINT('Ctrl Pts',(43.4542745623933,33.6242424638975,-39.233238623837));
#270461=CARTESIAN_POINT('Ctrl Pts',(43.5542222374601,33.6747516510336,-39.2594493821381));
#270462=CARTESIAN_POINT('Ctrl Pts',(43.6219256430316,33.7069073870393,-39.2768314299875));
#270463=CARTESIAN_POINT('Ctrl Pts',(43.6563381479934,33.7222286468184,-39.2854811722856));
#270464=CARTESIAN_POINT('Ctrl Pts',(43.7254519170511,33.7509934760635,-39.3024907499371));
#270465=CARTESIAN_POINT('Ctrl Pts',(43.7602995448845,33.7645084608315,-39.3108885064059));
#270466=CARTESIAN_POINT('Ctrl Pts',(43.8304781084082,33.789780836939,-39.3274499785309));
#270467=CARTESIAN_POINT('Ctrl Pts',(43.9365171946568,33.8250735562425,-39.3519527568515));
#270468=CARTESIAN_POINT('Ctrl Pts',(44.0809642638621,33.8617420360433,-39.3832806139221));
#270469=CARTESIAN_POINT('Ctrl Pts',(44.1916183723467,33.8813683146414,-39.4057679385072));
#270470=CARTESIAN_POINT('Ctrl Pts',(44.2659122959159,33.8926702964892,-39.4205323411483));
#270471=CARTESIAN_POINT('Ctrl Pts',(44.3033049221432,33.8974288658374,-39.4277978831022));
#270472=CARTESIAN_POINT('Ctrl Pts',(44.3598453576919,33.9032050944765,-39.4385322478049));
#270473=CARTESIAN_POINT('Ctrl Pts',(44.3787527158677,33.9049006163346,-39.4420799976889));
#270474=CARTESIAN_POINT('Ctrl Pts',(44.4164967874688,33.9078161173588,-39.4490791780208));
#270475=CARTESIAN_POINT('Ctrl Pts',(44.4353708468856,33.9090400957878,-39.4525377314439));
#270476=CARTESIAN_POINT('Ctrl Pts',(44.4919347179527,33.9120095261765,-39.462779235967));
#270477=CARTESIAN_POINT('Ctrl Pts',(44.52962054914,33.9130584408517,-39.4694384189012));
#270478=CARTESIAN_POINT('Ctrl Pts',(44.6425299001817,33.9134342925821,-39.4889026473125));
#270479=CARTESIAN_POINT('Ctrl Pts',(44.7176656228988,33.9100023852834,-39.5012068570978));
#270480=CARTESIAN_POINT('Ctrl Pts',(44.867623327666,33.8957625538083,-39.524471978366));
#270481=CARTESIAN_POINT('Ctrl Pts',(44.9424659600731,33.8849485744664,-39.5354353652432));
#270482=CARTESIAN_POINT('Ctrl Pts',(45.0357885152669,33.8666999843662,-39.5482785606344));
#270483=CARTESIAN_POINT('Ctrl Pts',(45.0544546343785,33.8628074782943,-39.5508053225112));
#270484=CARTESIAN_POINT('Ctrl Pts',(45.091743102575,33.8545484160302,-39.5557691634051));
#270485=CARTESIAN_POINT('Ctrl Pts',(45.1104022544846,33.850171655015,-39.5582107864407));
#270486=CARTESIAN_POINT('Ctrl Pts',(45.1661672125598,33.8363538303533,-39.5653802281989));
#270487=CARTESIAN_POINT('Ctrl Pts',(45.2029511118778,33.8262578362557,-39.5699395109212));
#270488=CARTESIAN_POINT('Ctrl Pts',(45.312316831343,33.7933159380614,-39.582990524906));
#270489=CARTESIAN_POINT('Ctrl Pts',(45.4195983160475,33.7551076509549,-39.5947758536238));
#270490=CARTESIAN_POINT('Ctrl Pts',(45.5585113890164,33.6937328563153,-39.6079933748399));
#270491=CARTESIAN_POINT('Ctrl Pts',(45.6606150024606,33.6424505696195,-39.6166516297843));
#270492=CARTESIAN_POINT('Ctrl Pts',(45.7272860947277,33.6047101271221,-39.6215780075552));
#270493=CARTESIAN_POINT('Ctrl Pts',(45.7932287365117,33.5651705839516,-39.6260731428005));
#270494=CARTESIAN_POINT('Ctrl Pts',(45.8259059249178,33.5444453395394,-39.6281074988013));
#270495=CARTESIAN_POINT('Ctrl Pts',(45.8897275017006,33.5016881508368,-39.6316923737189));
#270496=CARTESIAN_POINT('Ctrl Pts',(45.9210297733036,33.4795651380848,-39.6332542688506));
#270497=CARTESIAN_POINT('Ctrl Pts',(45.9823424846244,33.4339088874735,-39.6359180193303));
#270498=CARTESIAN_POINT('Ctrl Pts',(46.0724202597563,33.3632801300718,-39.6392265347984));
#270499=CARTESIAN_POINT('Ctrl Pts',(46.1850394564173,33.2606222983665,-39.6409205727319));
#270500=CARTESIAN_POINT('Ctrl Pts',(46.2638636333332,33.1772336958075,-39.6401443034625));
#270501=CARTESIAN_POINT('Ctrl Pts',(46.3151397511292,33.1201974856456,-39.6391646017005));
#270502=CARTESIAN_POINT('Ctrl Pts',(46.3401349353408,33.0909661742941,-39.6384440851485));
#270503=CARTESIAN_POINT('Ctrl Pts',(46.3888523044997,33.0309971480077,-39.6365301000439));
#270504=CARTESIAN_POINT('Ctrl Pts',(46.4123735341802,33.0005036828642,-39.6353439924849));
#270505=CARTESIAN_POINT('Ctrl Pts',(46.4576879006691,32.9386388625828,-39.6325280276393));
#270506=CARTESIAN_POINT('Ctrl Pts',(46.52311576659,32.8444620833496,-39.6276360146217));
#270507=CARTESIAN_POINT('Ctrl Pts',(46.5810426872604,32.7462345994881,-39.6207752343847));
#270508=CARTESIAN_POINT('Ctrl Pts',(46.6516918187307,32.6117039458857,-39.6098936921283));
#270509=CARTESIAN_POINT('Ctrl Pts',(46.683723185051,32.5426422373878,-39.6035832967262));
#270510=CARTESIAN_POINT('Ctrl Pts',(46.7195635412788,32.4540883209461,-39.5945936116187));
#270511=CARTESIAN_POINT('Ctrl Pts',(46.7265235775841,32.4362514419463,-39.5927383889278));
#270512=CARTESIAN_POINT('Ctrl Pts',(46.7400123459627,32.4003742100513,-39.5889189813535));
#270513=CARTESIAN_POINT('Ctrl Pts',(46.7465535157541,32.3822946053341,-39.5869502184844));
#270514=CARTESIAN_POINT('Ctrl Pts',(46.7654644360989,32.3279072933142,-39.5808958427402));
#270515=CARTESIAN_POINT('Ctrl Pts',(46.7770937339888,32.2915493874551,-39.5766741707955));
#270516=CARTESIAN_POINT('Ctrl Pts',(46.8091770518909,32.182013131159,-39.5634457571489));
#270517=CARTESIAN_POINT('Ctrl Pts',(46.8444383818759,32.034891308334,-39.5443264312115));
#270518=CARTESIAN_POINT('Ctrl Pts',(46.8650708643864,31.8856621776612,-39.5223044891954));
#270519=CARTESIAN_POINT('Ctrl Pts',(46.8750487417844,31.7729724844591,-39.50469487268));
#270520=CARTESIAN_POINT('Ctrl Pts',(46.8774570362353,31.7352651712118,-39.4986397605723));
#270521=CARTESIAN_POINT('Ctrl Pts',(46.8796767940079,31.6785286095959,-39.4892824810203));
#270522=CARTESIAN_POINT('Ctrl Pts',(46.8801843407089,31.6595724593507,-39.4861150486293));
#270523=CARTESIAN_POINT('Ctrl Pts',(46.8807312344332,31.6216180949417,-39.479690628598));
#270524=CARTESIAN_POINT('Ctrl Pts',(46.8807699646674,31.6025797052015,-39.4764266299692));
#270525=CARTESIAN_POINT('Ctrl Pts',(46.8801790388754,31.5455906639181,-39.4665317368708));
#270526=CARTESIAN_POINT('Ctrl Pts',(46.8788490796135,31.5078273383739,-39.4598096545541));
#270527=CARTESIAN_POINT('Ctrl Pts',(46.874360617844,31.4326451774338,-39.4461013696832));
#270528=CARTESIAN_POINT('Ctrl Pts',(46.864884835636,31.320441459725,-39.4251517854185));
#270529=CARTESIAN_POINT('Ctrl Pts',(46.8414902947658,31.1730719473388,-39.3956936109857));
#270530=CARTESIAN_POINT('Ctrl Pts',(46.8074810934279,31.0279105813681,-39.364717848004));
#270531=CARTESIAN_POINT('Ctrl Pts',(46.7869180083019,30.9560697433081,-39.3487190247537));
#270532=CARTESIAN_POINT('Ctrl Pts',(46.7645577771926,30.884604709384,-39.332461491893));
#270533=CARTESIAN_POINT('Ctrl Pts',(46.7524740339114,30.8490466969583,-39.3242001683612));
#270534=CARTESIAN_POINT('Ctrl Pts',(46.7264943673172,30.7783632715819,-39.3074248425479));
#270535=CARTESIAN_POINT('Ctrl Pts',(46.7127058212706,30.7435263372096,-39.2989795429224));
#270536=CARTESIAN_POINT('Ctrl Pts',(46.6981266849492,30.7091523375488,-39.2904704603133));
#270537=CARTESIAN_POINT('Ctrl Pts',(44.7926621173534,30.9780510210195,-41.4731170634489));
#270538=CARTESIAN_POINT('Ctrl Pts',(44.7841183378731,30.958431594105,-41.4560988982307));
#270539=CARTESIAN_POINT('Ctrl Pts',(44.7652574387158,30.9202429989855,-41.4215723090211));
#270540=CARTESIAN_POINT('Ctrl Pts',(44.7373647422364,30.8750641226134,-41.3772059160528));
#270541=CARTESIAN_POINT('Ctrl Pts',(44.7186826069414,30.8491098680677,-41.3500360893141));
#270542=CARTESIAN_POINT('Ctrl Pts',(44.7057896374646,30.8320666178198,-41.3317986258606));
#270543=CARTESIAN_POINT('Ctrl Pts',(44.6991283043737,30.8236797190306,-41.3226233796301));
#270544=CARTESIAN_POINT('Ctrl Pts',(44.6853430526266,30.8071501195218,-41.3041237465898));
#270545=CARTESIAN_POINT('Ctrl Pts',(44.6782604199269,30.7990587859436,-41.2948558628018));
#270546=CARTESIAN_POINT('Ctrl Pts',(44.6637865272211,30.7832912649286,-41.2763692550984));
#270547=CARTESIAN_POINT('Ctrl Pts',(44.65638232911,30.7755995480316,-41.2671331599469));
#270548=CARTESIAN_POINT('Ctrl Pts',(44.6336879630273,30.7531065345255,-41.2394625228135));
#270549=CARTESIAN_POINT('Ctrl Pts',(44.6100194582072,30.7317609779911,-41.211850451263));
#270550=CARTESIAN_POINT('Ctrl Pts',(44.5765344835469,30.7055824366946,-41.1751580074971));
#270551=CARTESIAN_POINT('Ctrl Pts',(44.5504480754,30.6870962504203,-41.147699245024));
#270552=CARTESIAN_POINT('Ctrl Pts',(44.5324056777293,30.6755504391987,-41.1294402655247));
#270553=CARTESIAN_POINT('Ctrl Pts',(44.5186168522497,30.6671837862428,-41.1157563555777));
#270554=CARTESIAN_POINT('Ctrl Pts',(44.5139760207251,30.6644431539959,-41.1111953707762));
#270555=CARTESIAN_POINT('Ctrl Pts',(44.5046579712977,30.6590892493455,-41.102125755137));
#270556=CARTESIAN_POINT('Ctrl Pts',(44.4999732573772,30.6564710151932,-41.0976094410703));
#270557=CARTESIAN_POINT('Ctrl Pts',(44.4764410055871,30.6436866063214,-41.0751408219827));
#270558=CARTESIAN_POINT('Ctrl Pts',(44.4380363426647,30.6251318507397,-41.0398401547925));
#270559=CARTESIAN_POINT('Ctrl Pts',(44.3881999640401,30.6066279457426,-40.9973473660572));
#270560=CARTESIAN_POINT('Ctrl Pts',(44.3574626802754,30.5976558165788,-40.9725988687145));
#270561=CARTESIAN_POINT('Ctrl Pts',(44.3367823836873,30.5921565153947,-40.9562701951691));
#270562=CARTESIAN_POINT('Ctrl Pts',(44.3263541271388,30.5896491085923,-40.9481956834911));
#270563=CARTESIAN_POINT('Ctrl Pts',(44.3052793937559,30.5851218575581,-40.9322027877955));
#270564=CARTESIAN_POINT('Ctrl Pts',(44.2946995104909,30.5831174982377,-40.924335654778));
#270565=CARTESIAN_POINT('Ctrl Pts',(44.2735450602529,30.5796377993431,-40.9089243529734));
#270566=CARTESIAN_POINT('Ctrl Pts',(44.2629524396991,30.5781585711684,-40.9013664771085));
#270567=CARTESIAN_POINT('Ctrl Pts',(44.2311453972639,30.5744985086998,-40.8791460851492));
#270568=CARTESIAN_POINT('Ctrl Pts',(44.2098907431643,30.5730912421562,-40.8649273724495));
#270569=CARTESIAN_POINT('Ctrl Pts',(44.1672866942957,30.5723474200962,-40.8376959485268));
#270570=CARTESIAN_POINT('Ctrl Pts',(44.1459323927671,30.5730120277702,-40.8246808510428));
#270571=CARTESIAN_POINT('Ctrl Pts',(44.1191870166623,30.5751734135742,-40.8091986194082));
#270572=CARTESIAN_POINT('Ctrl Pts',(44.1138315874482,30.5756735271978,-40.806139968135));
#270573=CARTESIAN_POINT('Ctrl Pts',(44.1031212948485,30.5768077596639,-40.8001057293845));
#270574=CARTESIAN_POINT('Ctrl Pts',(44.0977557278508,30.5774435866632,-40.7971244669688));
#270575=CARTESIAN_POINT('Ctrl Pts',(44.0817045383335,30.5795497856634,-40.7883321887253));
#270576=CARTESIAN_POINT('Ctrl Pts',(44.0710902649836,30.5812139186595,-40.7826858714375));
#270577=CARTESIAN_POINT('Ctrl Pts',(44.0394561806682,30.5869813183234,-40.7663593410916));
#270578=CARTESIAN_POINT('Ctrl Pts',(44.0082701709188,30.5942909050994,-40.7512721078743));
#270579=CARTESIAN_POINT('Ctrl Pts',(43.9675777996734,30.6070988998346,-40.7336299050859));
#270580=CARTESIAN_POINT('Ctrl Pts',(43.9375066395073,30.6182485087226,-40.721648717354));
#270581=CARTESIAN_POINT('Ctrl Pts',(43.917761614853,30.626725808719,-40.7145087645619));
#270582=CARTESIAN_POINT('Ctrl Pts',(43.8981718083816,30.6357351147044,-40.7078022579606));
#270583=CARTESIAN_POINT('Ctrl Pts',(43.8884396229394,30.6405162381665,-40.7046629153417));
#270584=CARTESIAN_POINT('Ctrl Pts',(43.8693712864522,30.6504970769624,-40.6988992879235));
#270585=CARTESIAN_POINT('Ctrl Pts',(43.8599880575193,30.6557176389023,-40.6962583786489));
#270586=CARTESIAN_POINT('Ctrl Pts',(43.8415477166501,30.6665995934339,-40.6914621347147));
#270587=CARTESIAN_POINT('Ctrl Pts',(43.8143622090585,30.6835906587784,-40.6849914969931));
#270588=CARTESIAN_POINT('Ctrl Pts',(43.7885885365895,30.7025683103525,-40.6806752166169));
#270589=CARTESIAN_POINT('Ctrl Pts',(43.7554869731093,30.7296502406846,-40.676851696754));
#270590=CARTESIAN_POINT('Ctrl Pts',(43.7395647886014,30.744083456595,-40.6759056793254));
#270591=CARTESIAN_POINT('Ctrl Pts',(43.7090440489059,30.7747854825451,-40.6760208486551));
#270592=CARTESIAN_POINT('Ctrl Pts',(43.6947173014185,30.7907796762741,-40.6770802501629));
#270593=CARTESIAN_POINT('Ctrl Pts',(43.6678443418708,30.8240220908504,-40.6811258797777));
#270594=CARTESIAN_POINT('Ctrl Pts',(43.6427576069985,30.8585127548254,-40.687098273402));
#270595=CARTESIAN_POINT('Ctrl Pts',(43.6212142380078,30.8954846730083,-40.6968894358922));
#270596=CARTESIAN_POINT('Ctrl Pts',(43.6088787182641,30.9193798597989,-40.7042205511341));
#270597=CARTESIAN_POINT('Ctrl Pts',(43.6064685586478,30.9241994859948,-40.7057484197296));
#270598=CARTESIAN_POINT('Ctrl Pts',(43.6017624551859,30.9339175659931,-40.70892606686));
#270599=CARTESIAN_POINT('Ctrl Pts',(43.5994656231147,30.9388193592268,-40.7105773965538));
#270600=CARTESIAN_POINT('Ctrl Pts',(43.5927866482525,30.953560895212,-40.7156875255853));
#270601=CARTESIAN_POINT('Ctrl Pts',(43.5844198153918,30.9733582110501,-40.72293005151));
#270602=CARTESIAN_POINT('Ctrl Pts',(43.5734440082896,31.0034822735469,-40.7350537322951));
#270603=CARTESIAN_POINT('Ctrl Pts',(43.5640181327981,31.0340244080827,-40.7484125407461));
#270604=CARTESIAN_POINT('Ctrl Pts',(43.5561284133843,31.0649820306433,-40.7629929778707));
#270605=CARTESIAN_POINT('Ctrl Pts',(43.5518912037438,31.0858969805267,-40.7735241784737));
#270606=CARTESIAN_POINT('Ctrl Pts',(43.5481682579358,31.1069510729684,-40.7844620267622));
#270607=CARTESIAN_POINT('Ctrl Pts',(43.5465635963524,31.1175527760565,-40.7901372750232));
#270608=CARTESIAN_POINT('Ctrl Pts',(43.5438765944467,31.1388768366658,-40.8018865323646));
#270609=CARTESIAN_POINT('Ctrl Pts',(43.5427912565025,31.1496493641875,-40.8079902348016));
#270610=CARTESIAN_POINT('Ctrl Pts',(43.5411674088753,31.1711124235333,-40.8204828132684));
#270611=CARTESIAN_POINT('Ctrl Pts',(43.5400805588778,31.19253758885,-40.8332822237109));
#270612=CARTESIAN_POINT('Ctrl Pts',(43.5400129658238,31.2352236668913,-40.8600695429299));
#270613=CARTESIAN_POINT('Ctrl Pts',(43.5430492497798,31.2776738375434,-40.8886047446452));
#270614=CARTESIAN_POINT('Ctrl Pts',(43.5491614319672,31.3198884817001,-40.918856387552));
#270615=CARTESIAN_POINT('Ctrl Pts',(43.5532522131496,31.3409199794841,-40.9345594064291));
#270616=CARTESIAN_POINT('Ctrl Pts',(43.5578644352119,31.361905871423,-40.9505475151733));
#270617=CARTESIAN_POINT('Ctrl Pts',(43.560439098329,31.3723994717644,-40.9587035928991));
#270618=CARTESIAN_POINT('Ctrl Pts',(43.5660648897127,31.3931449423641,-40.9751492091434));
#270619=CARTESIAN_POINT('Ctrl Pts',(43.5691234314236,31.4034342087731,-40.9834667538713));
#270620=CARTESIAN_POINT('Ctrl Pts',(43.5790202279964,31.4340221767704,-41.0086741075936));
#270621=CARTESIAN_POINT('Ctrl Pts',(43.5865808644402,31.4540562960243,-41.0258289330007));
#270622=CARTESIAN_POINT('Ctrl Pts',(43.5993606039644,31.4835727602996,-41.0520789232858));
#270623=CARTESIAN_POINT('Ctrl Pts',(43.6038584649574,31.4933175175814,-41.0609109997729));
#270624=CARTESIAN_POINT('Ctrl Pts',(43.6133480280387,31.5126460303085,-41.0787663839806));
#270625=CARTESIAN_POINT('Ctrl Pts',(43.6183219077102,31.5221915251339,-41.0877549157913));
#270626=CARTESIAN_POINT('Ctrl Pts',(43.6338406007018,31.5503182102049,-41.1147514459697));
#270627=CARTESIAN_POINT('Ctrl Pts',(43.6450116757484,31.5684678157769,-41.13285712865));
#270628=CARTESIAN_POINT('Ctrl Pts',(43.6689569093208,31.6035742491305,-41.1692591986645));
#270629=CARTESIAN_POINT('Ctrl Pts',(43.6881189975485,31.6290150958394,-41.1967078345595));
#270630=CARTESIAN_POINT('Ctrl Pts',(43.7160805799803,31.6611548911343,-41.2335986369031));
#270631=CARTESIAN_POINT('Ctrl Pts',(43.7308739938731,31.6766212732249,-41.2521403517739));
#270632=CARTESIAN_POINT('Ctrl Pts',(43.7460847706871,31.6917854492915,-41.2707364845776));
#270633=CARTESIAN_POINT('Ctrl Pts',(43.7539033240721,31.6992171694526,-41.2800648729051));
#270634=CARTESIAN_POINT('Ctrl Pts',(43.7697797892606,31.7136063232936,-41.298562009488));
#270635=CARTESIAN_POINT('Ctrl Pts',(43.7778723272806,31.7205988773597,-41.3077734720143));
#270636=CARTESIAN_POINT('Ctrl Pts',(43.8025568401133,31.7409299545529,-41.3352381600133));
#270637=CARTESIAN_POINT('Ctrl Pts',(43.8195937300504,31.7536621581445,-41.353369616892));
#270638=CARTESIAN_POINT('Ctrl Pts',(43.8547939251157,31.7774712224987,-41.3892512463859));
#270639=CARTESIAN_POINT('Ctrl Pts',(43.8820456950658,31.7940939723408,-41.4158852269725));
#270640=CARTESIAN_POINT('Ctrl Pts',(43.9105977352555,31.8088239425505,-41.4420959852738));
#270641=CARTESIAN_POINT('Ctrl Pts',(43.9299312426308,31.8182163905263,-41.4594780331231));
#270642=CARTESIAN_POINT('Ctrl Pts',(43.9397545046832,31.8226994853967,-41.4681277754213));
#270643=CARTESIAN_POINT('Ctrl Pts',(43.959476379363,31.8311327029401,-41.4851373530728));
#270644=CARTESIAN_POINT('Ctrl Pts',(43.969416794615,31.835103670887,-41.4935351095415));
#270645=CARTESIAN_POINT('Ctrl Pts',(43.9894286782948,31.8425474915593,-41.5100965816665));
#270646=CARTESIAN_POINT('Ctrl Pts',(44.0196562937352,31.8529720625538,-41.5345993599874));
#270647=CARTESIAN_POINT('Ctrl Pts',(44.0607928561344,31.8639280327151,-41.5659272170578));
#270648=CARTESIAN_POINT('Ctrl Pts',(44.0922765794535,31.8699137146658,-41.5884145416429));
#270649=CARTESIAN_POINT('Ctrl Pts',(44.1134085621028,31.8733992175668,-41.6031789442838));
#270650=CARTESIAN_POINT('Ctrl Pts',(44.1240412545,31.8748890570172,-41.6104444862381));
#270651=CARTESIAN_POINT('Ctrl Pts',(44.1401138557838,31.8767382236783,-41.6211788509405));
#270652=CARTESIAN_POINT('Ctrl Pts',(44.1454877988083,31.8772894545129,-41.6247266008247));
#270653=CARTESIAN_POINT('Ctrl Pts',(44.1562140153048,31.878256418298,-41.6317257811562));
#270654=CARTESIAN_POINT('Ctrl Pts',(44.161576905651,31.8786734249769,-41.6351843345794));
#270655=CARTESIAN_POINT('Ctrl Pts',(44.1776466456902,31.8797244502982,-41.6454258391029));
#270656=CARTESIAN_POINT('Ctrl Pts',(44.1883500092183,31.8801603696231,-41.6520850220369));
#270657=CARTESIAN_POINT('Ctrl Pts',(44.2204087008324,31.8806796234647,-41.671549250448));
#270658=CARTESIAN_POINT('Ctrl Pts',(44.2417298059497,31.8799780982567,-41.6838534602333));
#270659=CARTESIAN_POINT('Ctrl Pts',(44.2842582084951,31.8764766164199,-41.7071185815018));
#270660=CARTESIAN_POINT('Ctrl Pts',(44.3054713486111,31.8736750129732,-41.7180819683776));
#270661=CARTESIAN_POINT('Ctrl Pts',(44.3319064277948,31.8688271235064,-41.7309251637703));
#270662=CARTESIAN_POINT('Ctrl Pts',(44.3371930873745,31.8677885276791,-41.7334519256467));
#270663=CARTESIAN_POINT('Ctrl Pts',(44.3477523920959,31.8655764110726,-41.7384157665409));
#270664=CARTESIAN_POINT('Ctrl Pts',(44.353035452149,31.8644001232798,-41.7408573895762));
#270665=CARTESIAN_POINT('Ctrl Pts',(44.368821997144,31.8606750365135,-41.7480268313348));
#270666=CARTESIAN_POINT('Ctrl Pts',(44.3792318927429,31.8579388865424,-41.752586114057));
#270667=CARTESIAN_POINT('Ctrl Pts',(44.4101727404,31.8489724804825,-41.7656371280416));
#270668=CARTESIAN_POINT('Ctrl Pts',(44.4405041748167,31.8385015328462,-41.7774224567595));
#270669=CARTESIAN_POINT('Ctrl Pts',(44.4797386522914,31.8215610256552,-41.7906399779756));
#270670=CARTESIAN_POINT('Ctrl Pts',(44.5085558494592,31.8073558935676,-41.7992982329201));
#270671=CARTESIAN_POINT('Ctrl Pts',(44.5273583247585,31.7968714183439,-41.8042246106906));
#270672=CARTESIAN_POINT('Ctrl Pts',(44.5459478308046,31.7858731708475,-41.8087197459362));
#270673=CARTESIAN_POINT('Ctrl Pts',(44.5551558111633,31.7801015230391,-41.8107541019367));
#270674=CARTESIAN_POINT('Ctrl Pts',(44.5731320510561,31.7681815367951,-41.814338976855));
#270675=CARTESIAN_POINT('Ctrl Pts',(44.5819448307914,31.7620078883687,-41.8159008719862));
#270676=CARTESIAN_POINT('Ctrl Pts',(44.5991987000126,31.7492554022398,-41.8185646224661));
#270677=CARTESIAN_POINT('Ctrl Pts',(44.6245350600795,31.7295108031857,-41.8218731379338));
#270678=CARTESIAN_POINT('Ctrl Pts',(44.6561620699444,31.7007477525095,-41.8235671758672));
#270679=CARTESIAN_POINT('Ctrl Pts',(44.6782580742923,31.6773394437008,-41.8227909065983));
#270680=CARTESIAN_POINT('Ctrl Pts',(44.6926220014235,31.6613194462407,-41.8218112048364));
#270681=CARTESIAN_POINT('Ctrl Pts',(44.6996188611148,31.6531046671394,-41.8210906882841));
#270682=CARTESIAN_POINT('Ctrl Pts',(44.7132456597446,31.6362429219073,-41.8191767031797));
#270683=CARTESIAN_POINT('Ctrl Pts',(44.7198193777268,31.627664624135,-41.8179905956202));
#270684=CARTESIAN_POINT('Ctrl Pts',(44.7324727845908,31.610252798272,-41.8151746307749));
#270685=CARTESIAN_POINT('Ctrl Pts',(44.7507253937504,31.5837345714901,-41.8102826177571));
#270686=CARTESIAN_POINT('Ctrl Pts',(44.7668325292565,31.5560404782777,-41.8034218375205));
#270687=CARTESIAN_POINT('Ctrl Pts',(44.7864242741839,31.5180816884312,-41.7925402952635));
#270688=CARTESIAN_POINT('Ctrl Pts',(44.7952779235527,31.4985810718442,-41.7862298998632));
#270689=CARTESIAN_POINT('Ctrl Pts',(44.8051436066325,31.4735589245645,-41.777240214754));
#270690=CARTESIAN_POINT('Ctrl Pts',(44.8070571630202,31.4685179927861,-41.7753849920635));
#270691=CARTESIAN_POINT('Ctrl Pts',(44.8107609555809,31.4583769076679,-41.7715655844892));
#270692=CARTESIAN_POINT('Ctrl Pts',(44.8125545845603,31.4532656516023,-41.76959682162));
#270693=CARTESIAN_POINT('Ctrl Pts',(44.8177323950795,31.4378873281915,-41.7635424458753));
#270694=CARTESIAN_POINT('Ctrl Pts',(44.8209059367305,31.4276035217402,-41.7593207739311));
#270695=CARTESIAN_POINT('Ctrl Pts',(44.8296276705658,31.3966113763671,-41.7460923602843));
#270696=CARTESIAN_POINT('Ctrl Pts',(44.8391161742293,31.3549585404116,-41.7269730343471));
#270697=CARTESIAN_POINT('Ctrl Pts',(44.8444380100638,31.312658433005,-41.7049510923314));
#270698=CARTESIAN_POINT('Ctrl Pts',(44.8468637082338,31.2806969121874,-41.6873414758157));
#270699=CARTESIAN_POINT('Ctrl Pts',(44.8474108190536,31.2699990859542,-41.6812863637077));
#270700=CARTESIAN_POINT('Ctrl Pts',(44.8478348231013,31.2538978106508,-41.671929084156));
#270701=CARTESIAN_POINT('Ctrl Pts',(44.8479099202363,31.2485174556463,-41.6687616517648));
#270702=CARTESIAN_POINT('Ctrl Pts',(44.8479268208064,31.2377432265879,-41.6623372317338));
#270703=CARTESIAN_POINT('Ctrl Pts',(44.8478683021095,31.2323379437313,-41.6590732331048));
#270704=CARTESIAN_POINT('Ctrl Pts',(44.8474921214824,31.2161555213209,-41.6491783400064));
#270705=CARTESIAN_POINT('Ctrl Pts',(44.8469759958029,31.2054292064128,-41.6424562576898));
#270706=CARTESIAN_POINT('Ctrl Pts',(44.8454249887827,31.1840681958411,-41.6287479728186));
#270707=CARTESIAN_POINT('Ctrl Pts',(44.8423204600693,31.1521790951542,-41.6077983885548));
#270708=CARTESIAN_POINT('Ctrl Pts',(44.8351290816859,31.1102584040656,-41.5783402141209));
#270709=CARTESIAN_POINT('Ctrl Pts',(44.8249268329474,31.0689281614894,-41.54736445114));
#270710=CARTESIAN_POINT('Ctrl Pts',(44.8188163283608,31.0484607830594,-41.5313656278891));
#270711=CARTESIAN_POINT('Ctrl Pts',(44.8121960627665,31.028093840338,-41.5151080950287));
#270712=CARTESIAN_POINT('Ctrl Pts',(44.808629563005,31.0179567656131,-41.5068467714969));
#270713=CARTESIAN_POINT('Ctrl Pts',(44.8009827391877,30.9977990758989,-41.4900714456835));
#270714=CARTESIAN_POINT('Ctrl Pts',(44.7969340070935,30.9878607344767,-41.4816261460579));
#270715=CARTESIAN_POINT('Ctrl Pts',(44.7926621173534,30.9780510210195,-41.4731170634489));
#270716=CARTESIAN_POINT('Ctrl Pts',(46.6981266849492,30.7091523375488,-39.2904704603133));
#270717=CARTESIAN_POINT('Ctrl Pts',(46.6689684123063,30.6404043382273,-39.273452295095));
#270718=CARTESIAN_POINT('Ctrl Pts',(46.6043681216411,30.5066861069553,-39.238925705885));
#270719=CARTESIAN_POINT('Ctrl Pts',(46.5083209189471,30.3487389562033,-39.1945593129175));
#270720=CARTESIAN_POINT('Ctrl Pts',(46.4437937583117,30.2581216171786,-39.1673894861782));
#270721=CARTESIAN_POINT('Ctrl Pts',(46.3992224148768,30.1986447451181,-39.1491520227249));
#270722=CARTESIAN_POINT('Ctrl Pts',(46.3761748773305,30.1693908446446,-39.1399767764946));
#270723=CARTESIAN_POINT('Ctrl Pts',(46.3284414024809,30.1117648114071,-39.1214771434543));
#270724=CARTESIAN_POINT('Ctrl Pts',(46.3038983378397,30.083571828401,-39.112209259666));
#270725=CARTESIAN_POINT('Ctrl Pts',(46.253707387608,30.0286632749651,-39.0937226519629));
#270726=CARTESIAN_POINT('Ctrl Pts',(46.2280147026909,30.001893564456,-39.0844865568113));
#270727=CARTESIAN_POINT('Ctrl Pts',(46.1492148010453,29.9236586721517,-39.0568159196779));
#270728=CARTESIAN_POINT('Ctrl Pts',(46.0669347173688,29.8495134741745,-39.0292038481275));
#270729=CARTESIAN_POINT('Ctrl Pts',(45.9503410384262,29.7587889734315,-38.9925114043613));
#270730=CARTESIAN_POINT('Ctrl Pts',(45.8594191065401,29.6948377475824,-38.9650526418885));
#270731=CARTESIAN_POINT('Ctrl Pts',(45.7964751089327,29.6549785818455,-38.9467936623891));
#270732=CARTESIAN_POINT('Ctrl Pts',(45.748348603817,29.6261284949947,-38.9331097524421));
#270733=CARTESIAN_POINT('Ctrl Pts',(45.7321473284057,29.616684052073,-38.9285487676403));
#270734=CARTESIAN_POINT('Ctrl Pts',(45.6996106203311,29.5982459977232,-38.9194791520014));
#270735=CARTESIAN_POINT('Ctrl Pts',(45.683249044345,29.5892352448745,-38.9149628379356));
#270736=CARTESIAN_POINT('Ctrl Pts',(45.6010439155842,29.5452684013657,-38.8924942188443));
#270737=CARTESIAN_POINT('Ctrl Pts',(45.4667739830181,29.4816584171599,-38.8571935516581));
#270738=CARTESIAN_POINT('Ctrl Pts',(45.2922645146651,29.4187721922835,-38.8147007629208));
#270739=CARTESIAN_POINT('Ctrl Pts',(45.184512437616,29.3885937253944,-38.7899522655792));
#270740=CARTESIAN_POINT('Ctrl Pts',(45.1119891467798,29.3701842541612,-38.7736235920333));
#270741=CARTESIAN_POINT('Ctrl Pts',(45.0754052578815,29.3618381514785,-38.7655490803555));
#270742=CARTESIAN_POINT('Ctrl Pts',(45.0014447932705,29.3468760834356,-38.7495561846596));
#270743=CARTESIAN_POINT('Ctrl Pts',(44.964301863367,29.3403115562353,-38.7416890516424));
#270744=CARTESIAN_POINT('Ctrl Pts',(44.8900079594565,29.3290481892184,-38.726277749838));
#270745=CARTESIAN_POINT('Ctrl Pts',(44.8527936282157,29.324336495618,-38.7187198739728));
#270746=CARTESIAN_POINT('Ctrl Pts',(44.7410083373266,29.3129455735289,-38.6964994820139));
#270747=CARTESIAN_POINT('Ctrl Pts',(44.6662563757167,29.3089967422249,-38.6822807693139));
#270748=CARTESIAN_POINT('Ctrl Pts',(44.516312468428,29.3084067934202,-38.6550493453909));
#270749=CARTESIAN_POINT('Ctrl Pts',(44.441103189525,29.3117700143417,-38.6420342479066));
#270750=CARTESIAN_POINT('Ctrl Pts',(44.3468378615956,29.3206690055189,-38.6265520162729));
#270751=CARTESIAN_POINT('Ctrl Pts',(44.3279589148655,29.3226883315868,-38.6234933649988));
#270752=CARTESIAN_POINT('Ctrl Pts',(44.2901960653062,29.3271995080042,-38.6174591262491));
#270753=CARTESIAN_POINT('Ctrl Pts',(44.271274393292,29.329697893027,-38.614477863833));
#270754=CARTESIAN_POINT('Ctrl Pts',(44.2146592782019,29.3378915995821,-38.60568558559));
#270755=CARTESIAN_POINT('Ctrl Pts',(44.1772069502033,29.344266758826,-38.6000392683017));
#270756=CARTESIAN_POINT('Ctrl Pts',(44.0655444875092,29.3661148598052,-38.5837127379559));
#270757=CARTESIAN_POINT('Ctrl Pts',(43.9553791862171,29.3933792052515,-38.5686255047386));
#270758=CARTESIAN_POINT('Ctrl Pts',(43.8114622524781,29.4404829778103,-38.5509833019505));
#270759=CARTESIAN_POINT('Ctrl Pts',(43.705021834675,29.481230340464,-38.5390021142185));
#270760=CARTESIAN_POINT('Ctrl Pts',(43.6350719757086,29.512061063653,-38.5318621614261));
#270761=CARTESIAN_POINT('Ctrl Pts',(43.5656410085295,29.5447591316771,-38.525155654825));
#270762=CARTESIAN_POINT('Ctrl Pts',(43.5311320054746,29.5620794464364,-38.5220163122062));
#270763=CARTESIAN_POINT('Ctrl Pts',(43.4634866412134,29.5981758355574,-38.5162526847879));
#270764=CARTESIAN_POINT('Ctrl Pts',(43.4301834663392,29.6170276546,-38.5136117755133));
#270765=CARTESIAN_POINT('Ctrl Pts',(43.3647025891651,29.6562685687332,-38.5088155315793));
#270766=CARTESIAN_POINT('Ctrl Pts',(43.2681192378476,29.7174608121974,-38.5023448938576));
#270767=CARTESIAN_POINT('Ctrl Pts',(43.1764049274077,29.7855824582168,-38.4980286134812));
#270768=CARTESIAN_POINT('Ctrl Pts',(43.0584774180437,29.8826126224142,-38.4942050936184));
#270769=CARTESIAN_POINT('Ctrl Pts',(43.001681818637,29.9342392650769,-38.4932590761897));
#270770=CARTESIAN_POINT('Ctrl Pts',(42.8926599718677,30.0438904492243,-38.4933742455196));
#270771=CARTESIAN_POINT('Ctrl Pts',(42.8414047150844,30.1009342501745,-38.4944336470273));
#270772=CARTESIAN_POINT('Ctrl Pts',(42.7451036203247,30.2193471227021,-38.498479276642));
#270773=CARTESIAN_POINT('Ctrl Pts',(42.6550322643363,30.3420646399833,-38.5044516702661));
#270774=CARTESIAN_POINT('Ctrl Pts',(42.5773225406025,30.4733365238586,-38.5142428327574));
#270775=CARTESIAN_POINT('Ctrl Pts',(42.5326943378214,30.5580963840027,-38.5215739479982));
#270776=CARTESIAN_POINT('Ctrl Pts',(42.5239673850246,30.5751883092729,-38.5231018165939));
#270777=CARTESIAN_POINT('Ctrl Pts',(42.5069121510755,30.60964376351,-38.5262794637242));
#270778=CARTESIAN_POINT('Ctrl Pts',(42.4985805781952,30.627019094627,-38.5279307934181));
#270779=CARTESIAN_POINT('Ctrl Pts',(42.4743295471271,30.6792614198295,-38.5330409224498));
#270780=CARTESIAN_POINT('Ctrl Pts',(42.4438856226513,30.7493896366731,-38.5402834483744));
#270781=CARTESIAN_POINT('Ctrl Pts',(42.4037483179465,30.8560072598611,-38.5524071291592));
#270782=CARTESIAN_POINT('Ctrl Pts',(42.3690543371876,30.9640160484273,-38.5657659376104));
#270783=CARTESIAN_POINT('Ctrl Pts',(42.3397558527982,31.0734075527136,-38.5803463747351));
#270784=CARTESIAN_POINT('Ctrl Pts',(42.3238156343608,31.1472555030051,-38.5908775753381));
#270785=CARTESIAN_POINT('Ctrl Pts',(42.3096820427396,31.2215665449467,-38.6018154236264));
#270786=CARTESIAN_POINT('Ctrl Pts',(42.3035171869091,31.2589715314082,-38.6074906718877));
#270787=CARTESIAN_POINT('Ctrl Pts',(42.2930235524414,31.3341791410138,-38.6192399292287));
#270788=CARTESIAN_POINT('Ctrl Pts',(42.2886818075092,31.3721585359098,-38.6253436316658));
#270789=CARTESIAN_POINT('Ctrl Pts',(42.281930630611,31.4478003630713,-38.6378362101326));
#270790=CARTESIAN_POINT('Ctrl Pts',(42.277074994566,31.5232809912004,-38.6506356205751));
#270791=CARTESIAN_POINT('Ctrl Pts',(42.2747992363309,31.6735553614761,-38.6774229397946));
#270792=CARTESIAN_POINT('Ctrl Pts',(42.2834818483937,31.8228397562226,-38.7059581415094));
#270793=CARTESIAN_POINT('Ctrl Pts',(42.3030248127084,31.9711385758679,-38.7362097844166));
#270794=CARTESIAN_POINT('Ctrl Pts',(42.3164494406915,32.0449687602614,-38.7519128032936));
#270795=CARTESIAN_POINT('Ctrl Pts',(42.3317154579634,32.1186122141692,-38.7679009120377));
#270796=CARTESIAN_POINT('Ctrl Pts',(42.3402956643805,32.1554227583218,-38.7760569897633));
#270797=CARTESIAN_POINT('Ctrl Pts',(42.3591481714288,32.228169160774,-38.7925026060078));
#270798=CARTESIAN_POINT('Ctrl Pts',(42.3694448348212,32.2642362896146,-38.8008201507359));
#270799=CARTESIAN_POINT('Ctrl Pts',(42.4028917825415,32.3714169561226,-38.8260275044574));
#270800=CARTESIAN_POINT('Ctrl Pts',(42.428602574983,32.4415633880281,-38.8431823298655));
#270801=CARTESIAN_POINT('Ctrl Pts',(42.4722685042023,32.5448307979217,-38.8694323201497));
#270802=CARTESIAN_POINT('Ctrl Pts',(42.4876674804306,32.5789105800712,-38.8782643966373));
#270803=CARTESIAN_POINT('Ctrl Pts',(42.5202146590728,32.6464795812123,-38.8961197808447));
#270804=CARTESIAN_POINT('Ctrl Pts',(42.5373018269229,32.6798350022668,-38.9051083126545));
#270805=CARTESIAN_POINT('Ctrl Pts',(42.5906929412925,32.7780783962456,-38.9321048428364));
#270806=CARTESIAN_POINT('Ctrl Pts',(42.629225789877,32.8414173722334,-38.9502105255135));
#270807=CARTESIAN_POINT('Ctrl Pts',(42.7120000069194,32.9638220552461,-38.9866125955294));
#270808=CARTESIAN_POINT('Ctrl Pts',(42.7783647966162,33.0524402968179,-39.0140612314234));
#270809=CARTESIAN_POINT('Ctrl Pts',(42.8754380724448,33.1642175243331,-39.0509520337677));
#270810=CARTESIAN_POINT('Ctrl Pts',(42.9268673384212,33.2179450225078,-39.0694937486382));
#270811=CARTESIAN_POINT('Ctrl Pts',(42.9797817061918,33.2705900457306,-39.088089881442));
#270812=CARTESIAN_POINT('Ctrl Pts',(43.0069972096607,33.2963736994336,-39.097418269769));
#270813=CARTESIAN_POINT('Ctrl Pts',(43.0622936398443,33.3462615369726,-39.1159154063528));
#270814=CARTESIAN_POINT('Ctrl Pts',(43.0904949946047,33.3704876748183,-39.1251268688783));
#270815=CARTESIAN_POINT('Ctrl Pts',(43.176562606447,33.4408730143712,-39.1525915568785));
#270816=CARTESIAN_POINT('Ctrl Pts',(43.2360245534179,33.4848790444095,-39.1707230137558));
#270817=CARTESIAN_POINT('Ctrl Pts',(43.358992255749,33.5670176609587,-39.2066046432507));
#270818=CARTESIAN_POINT('Ctrl Pts',(43.4542745623933,33.6242424638975,-39.233238623837));
#270819=CARTESIAN_POINT('Ctrl Pts',(43.5542222374601,33.6747516510336,-39.2594493821381));
#270820=CARTESIAN_POINT('Ctrl Pts',(43.6219256430316,33.7069073870393,-39.2768314299875));
#270821=CARTESIAN_POINT('Ctrl Pts',(43.6563381479934,33.7222286468184,-39.2854811722856));
#270822=CARTESIAN_POINT('Ctrl Pts',(43.7254519170511,33.7509934760635,-39.3024907499371));
#270823=CARTESIAN_POINT('Ctrl Pts',(43.7602995448845,33.7645084608315,-39.3108885064059));
#270824=CARTESIAN_POINT('Ctrl Pts',(43.8304781084082,33.789780836939,-39.3274499785309));
#270825=CARTESIAN_POINT('Ctrl Pts',(43.9365171946568,33.8250735562425,-39.3519527568515));
#270826=CARTESIAN_POINT('Ctrl Pts',(44.0809642638621,33.8617420360433,-39.3832806139221));
#270827=CARTESIAN_POINT('Ctrl Pts',(44.1916183723467,33.8813683146414,-39.4057679385072));
#270828=CARTESIAN_POINT('Ctrl Pts',(44.2659122959159,33.8926702964892,-39.4205323411483));
#270829=CARTESIAN_POINT('Ctrl Pts',(44.3033049221432,33.8974288658374,-39.4277978831022));
#270830=CARTESIAN_POINT('Ctrl Pts',(44.3598453576919,33.9032050944765,-39.4385322478049));
#270831=CARTESIAN_POINT('Ctrl Pts',(44.3787527158677,33.9049006163346,-39.4420799976889));
#270832=CARTESIAN_POINT('Ctrl Pts',(44.4164967874688,33.9078161173588,-39.4490791780208));
#270833=CARTESIAN_POINT('Ctrl Pts',(44.4353708468856,33.9090400957878,-39.4525377314439));
#270834=CARTESIAN_POINT('Ctrl Pts',(44.4919347179527,33.9120095261765,-39.462779235967));
#270835=CARTESIAN_POINT('Ctrl Pts',(44.52962054914,33.9130584408517,-39.4694384189012));
#270836=CARTESIAN_POINT('Ctrl Pts',(44.6425299001817,33.9134342925821,-39.4889026473125));
#270837=CARTESIAN_POINT('Ctrl Pts',(44.7176656228988,33.9100023852834,-39.5012068570978));
#270838=CARTESIAN_POINT('Ctrl Pts',(44.867623327666,33.8957625538083,-39.524471978366));
#270839=CARTESIAN_POINT('Ctrl Pts',(44.9424659600731,33.8849485744664,-39.5354353652432));
#270840=CARTESIAN_POINT('Ctrl Pts',(45.0357885152669,33.8666999843662,-39.5482785606344));
#270841=CARTESIAN_POINT('Ctrl Pts',(45.0544546343785,33.8628074782943,-39.5508053225112));
#270842=CARTESIAN_POINT('Ctrl Pts',(45.091743102575,33.8545484160302,-39.5557691634051));
#270843=CARTESIAN_POINT('Ctrl Pts',(45.1104022544846,33.850171655015,-39.5582107864407));
#270844=CARTESIAN_POINT('Ctrl Pts',(45.1661672125598,33.8363538303533,-39.5653802281989));
#270845=CARTESIAN_POINT('Ctrl Pts',(45.2029511118778,33.8262578362557,-39.5699395109212));
#270846=CARTESIAN_POINT('Ctrl Pts',(45.312316831343,33.7933159380614,-39.582990524906));
#270847=CARTESIAN_POINT('Ctrl Pts',(45.4195983160475,33.7551076509549,-39.5947758536238));
#270848=CARTESIAN_POINT('Ctrl Pts',(45.5585113890164,33.6937328563153,-39.6079933748399));
#270849=CARTESIAN_POINT('Ctrl Pts',(45.6606150024606,33.6424505696195,-39.6166516297843));
#270850=CARTESIAN_POINT('Ctrl Pts',(45.7272860947277,33.6047101271221,-39.6215780075552));
#270851=CARTESIAN_POINT('Ctrl Pts',(45.7932287365117,33.5651705839516,-39.6260731428005));
#270852=CARTESIAN_POINT('Ctrl Pts',(45.8259059249178,33.5444453395394,-39.6281074988013));
#270853=CARTESIAN_POINT('Ctrl Pts',(45.8897275017006,33.5016881508368,-39.6316923737189));
#270854=CARTESIAN_POINT('Ctrl Pts',(45.9210297733036,33.4795651380848,-39.6332542688506));
#270855=CARTESIAN_POINT('Ctrl Pts',(45.9823424846244,33.4339088874735,-39.6359180193303));
#270856=CARTESIAN_POINT('Ctrl Pts',(46.0724202597563,33.3632801300718,-39.6392265347984));
#270857=CARTESIAN_POINT('Ctrl Pts',(46.1850394564173,33.2606222983665,-39.6409205727319));
#270858=CARTESIAN_POINT('Ctrl Pts',(46.2638636333332,33.1772336958075,-39.6401443034625));
#270859=CARTESIAN_POINT('Ctrl Pts',(46.3151397511292,33.1201974856456,-39.6391646017005));
#270860=CARTESIAN_POINT('Ctrl Pts',(46.3401349353408,33.0909661742941,-39.6384440851485));
#270861=CARTESIAN_POINT('Ctrl Pts',(46.3888523044997,33.0309971480077,-39.6365301000439));
#270862=CARTESIAN_POINT('Ctrl Pts',(46.4123735341802,33.0005036828642,-39.6353439924849));
#270863=CARTESIAN_POINT('Ctrl Pts',(46.4576879006691,32.9386388625828,-39.6325280276393));
#270864=CARTESIAN_POINT('Ctrl Pts',(46.52311576659,32.8444620833496,-39.6276360146217));
#270865=CARTESIAN_POINT('Ctrl Pts',(46.5810426872604,32.7462345994881,-39.6207752343847));
#270866=CARTESIAN_POINT('Ctrl Pts',(46.6516918187307,32.6117039458857,-39.6098936921283));
#270867=CARTESIAN_POINT('Ctrl Pts',(46.683723185051,32.5426422373878,-39.6035832967262));
#270868=CARTESIAN_POINT('Ctrl Pts',(46.7195635412788,32.4540883209461,-39.5945936116187));
#270869=CARTESIAN_POINT('Ctrl Pts',(46.7265235775841,32.4362514419463,-39.5927383889278));
#270870=CARTESIAN_POINT('Ctrl Pts',(46.7400123459627,32.4003742100513,-39.5889189813535));
#270871=CARTESIAN_POINT('Ctrl Pts',(46.7465535157541,32.3822946053341,-39.5869502184844));
#270872=CARTESIAN_POINT('Ctrl Pts',(46.7654644360989,32.3279072933142,-39.5808958427402));
#270873=CARTESIAN_POINT('Ctrl Pts',(46.7770937339888,32.2915493874551,-39.5766741707955));
#270874=CARTESIAN_POINT('Ctrl Pts',(46.8091770518909,32.182013131159,-39.5634457571489));
#270875=CARTESIAN_POINT('Ctrl Pts',(46.8444383818759,32.034891308334,-39.5443264312115));
#270876=CARTESIAN_POINT('Ctrl Pts',(46.8650708643864,31.8856621776612,-39.5223044891954));
#270877=CARTESIAN_POINT('Ctrl Pts',(46.8750487417844,31.7729724844591,-39.50469487268));
#270878=CARTESIAN_POINT('Ctrl Pts',(46.8774570362353,31.7352651712118,-39.4986397605723));
#270879=CARTESIAN_POINT('Ctrl Pts',(46.8796767940079,31.6785286095959,-39.4892824810203));
#270880=CARTESIAN_POINT('Ctrl Pts',(46.8801843407089,31.6595724593507,-39.4861150486293));
#270881=CARTESIAN_POINT('Ctrl Pts',(46.8807312344332,31.6216180949417,-39.479690628598));
#270882=CARTESIAN_POINT('Ctrl Pts',(46.8807699646674,31.6025797052015,-39.4764266299692));
#270883=CARTESIAN_POINT('Ctrl Pts',(46.8801790388754,31.5455906639181,-39.4665317368708));
#270884=CARTESIAN_POINT('Ctrl Pts',(46.8788490796135,31.5078273383739,-39.4598096545541));
#270885=CARTESIAN_POINT('Ctrl Pts',(46.874360617844,31.4326451774338,-39.4461013696832));
#270886=CARTESIAN_POINT('Ctrl Pts',(46.864884835636,31.320441459725,-39.4251517854185));
#270887=CARTESIAN_POINT('Ctrl Pts',(46.8414902947658,31.1730719473388,-39.3956936109857));
#270888=CARTESIAN_POINT('Ctrl Pts',(46.8074810934279,31.0279105813681,-39.364717848004));
#270889=CARTESIAN_POINT('Ctrl Pts',(46.7869180083019,30.9560697433081,-39.3487190247537));
#270890=CARTESIAN_POINT('Ctrl Pts',(46.7645577771926,30.884604709384,-39.332461491893));
#270891=CARTESIAN_POINT('Ctrl Pts',(46.7524740339114,30.8490466969583,-39.3242001683612));
#270892=CARTESIAN_POINT('Ctrl Pts',(46.7264943673172,30.7783632715819,-39.3074248425479));
#270893=CARTESIAN_POINT('Ctrl Pts',(46.7127058212706,30.7435263372096,-39.2989795429224));
#270894=CARTESIAN_POINT('Ctrl Pts',(46.6981266849492,30.7091523375488,-39.2904704603133));
#270895=CARTESIAN_POINT('Ctrl Pts',(44.7926621173534,30.9780510210195,-41.4731170634489));
#270896=CARTESIAN_POINT('Ctrl Pts',(44.7841183378731,30.958431594105,-41.4560988982307));
#270897=CARTESIAN_POINT('Ctrl Pts',(44.7652574387158,30.9202429989855,-41.4215723090211));
#270898=CARTESIAN_POINT('Ctrl Pts',(44.7373647422364,30.8750641226134,-41.3772059160528));
#270899=CARTESIAN_POINT('Ctrl Pts',(44.7186826069414,30.8491098680677,-41.3500360893141));
#270900=CARTESIAN_POINT('Ctrl Pts',(44.7057896374646,30.8320666178198,-41.3317986258606));
#270901=CARTESIAN_POINT('Ctrl Pts',(44.6991283043737,30.8236797190306,-41.3226233796301));
#270902=CARTESIAN_POINT('Ctrl Pts',(44.6853430526266,30.8071501195218,-41.3041237465898));
#270903=CARTESIAN_POINT('Ctrl Pts',(44.6782604199269,30.7990587859436,-41.2948558628018));
#270904=CARTESIAN_POINT('Ctrl Pts',(44.6637865272211,30.7832912649286,-41.2763692550984));
#270905=CARTESIAN_POINT('Ctrl Pts',(44.65638232911,30.7755995480316,-41.2671331599469));
#270906=CARTESIAN_POINT('Ctrl Pts',(44.6336879630273,30.7531065345255,-41.2394625228135));
#270907=CARTESIAN_POINT('Ctrl Pts',(44.6100194582072,30.7317609779911,-41.211850451263));
#270908=CARTESIAN_POINT('Ctrl Pts',(44.5765344835469,30.7055824366946,-41.1751580074971));
#270909=CARTESIAN_POINT('Ctrl Pts',(44.5504480754,30.6870962504203,-41.147699245024));
#270910=CARTESIAN_POINT('Ctrl Pts',(44.5324056777293,30.6755504391987,-41.1294402655247));
#270911=CARTESIAN_POINT('Ctrl Pts',(44.5186168522497,30.6671837862428,-41.1157563555777));
#270912=CARTESIAN_POINT('Ctrl Pts',(44.5139760207251,30.6644431539959,-41.1111953707762));
#270913=CARTESIAN_POINT('Ctrl Pts',(44.5046579712977,30.6590892493455,-41.102125755137));
#270914=CARTESIAN_POINT('Ctrl Pts',(44.4999732573772,30.6564710151932,-41.0976094410703));
#270915=CARTESIAN_POINT('Ctrl Pts',(44.4764410055871,30.6436866063214,-41.0751408219827));
#270916=CARTESIAN_POINT('Ctrl Pts',(44.4380363426647,30.6251318507397,-41.0398401547925));
#270917=CARTESIAN_POINT('Ctrl Pts',(44.3881999640401,30.6066279457426,-40.9973473660572));
#270918=CARTESIAN_POINT('Ctrl Pts',(44.3574626802754,30.5976558165788,-40.9725988687145));
#270919=CARTESIAN_POINT('Ctrl Pts',(44.3367823836873,30.5921565153947,-40.9562701951691));
#270920=CARTESIAN_POINT('Ctrl Pts',(44.3263541271388,30.5896491085923,-40.9481956834911));
#270921=CARTESIAN_POINT('Ctrl Pts',(44.3052793937559,30.5851218575581,-40.9322027877955));
#270922=CARTESIAN_POINT('Ctrl Pts',(44.2946995104909,30.5831174982377,-40.924335654778));
#270923=CARTESIAN_POINT('Ctrl Pts',(44.2735450602529,30.5796377993431,-40.9089243529734));
#270924=CARTESIAN_POINT('Ctrl Pts',(44.2629524396991,30.5781585711684,-40.9013664771085));
#270925=CARTESIAN_POINT('Ctrl Pts',(44.2311453972639,30.5744985086998,-40.8791460851492));
#270926=CARTESIAN_POINT('Ctrl Pts',(44.2098907431643,30.5730912421562,-40.8649273724495));
#270927=CARTESIAN_POINT('Ctrl Pts',(44.1672866942957,30.5723474200962,-40.8376959485268));
#270928=CARTESIAN_POINT('Ctrl Pts',(44.1459323927671,30.5730120277702,-40.8246808510428));
#270929=CARTESIAN_POINT('Ctrl Pts',(44.1191870166623,30.5751734135742,-40.8091986194082));
#270930=CARTESIAN_POINT('Ctrl Pts',(44.1138315874482,30.5756735271978,-40.806139968135));
#270931=CARTESIAN_POINT('Ctrl Pts',(44.1031212948485,30.5768077596639,-40.8001057293845));
#270932=CARTESIAN_POINT('Ctrl Pts',(44.0977557278508,30.5774435866632,-40.7971244669688));
#270933=CARTESIAN_POINT('Ctrl Pts',(44.0817045383335,30.5795497856634,-40.7883321887253));
#270934=CARTESIAN_POINT('Ctrl Pts',(44.0710902649836,30.5812139186595,-40.7826858714375));
#270935=CARTESIAN_POINT('Ctrl Pts',(44.0394561806682,30.5869813183234,-40.7663593410916));
#270936=CARTESIAN_POINT('Ctrl Pts',(44.0082701709188,30.5942909050994,-40.7512721078743));
#270937=CARTESIAN_POINT('Ctrl Pts',(43.9675777996734,30.6070988998346,-40.7336299050859));
#270938=CARTESIAN_POINT('Ctrl Pts',(43.9375066395073,30.6182485087226,-40.721648717354));
#270939=CARTESIAN_POINT('Ctrl Pts',(43.917761614853,30.626725808719,-40.7145087645619));
#270940=CARTESIAN_POINT('Ctrl Pts',(43.8981718083816,30.6357351147044,-40.7078022579606));
#270941=CARTESIAN_POINT('Ctrl Pts',(43.8884396229394,30.6405162381665,-40.7046629153417));
#270942=CARTESIAN_POINT('Ctrl Pts',(43.8693712864522,30.6504970769624,-40.6988992879235));
#270943=CARTESIAN_POINT('Ctrl Pts',(43.8599880575193,30.6557176389023,-40.6962583786489));
#270944=CARTESIAN_POINT('Ctrl Pts',(43.8415477166501,30.6665995934339,-40.6914621347147));
#270945=CARTESIAN_POINT('Ctrl Pts',(43.8143622090585,30.6835906587784,-40.6849914969931));
#270946=CARTESIAN_POINT('Ctrl Pts',(43.7885885365895,30.7025683103525,-40.6806752166169));
#270947=CARTESIAN_POINT('Ctrl Pts',(43.7554869731093,30.7296502406846,-40.676851696754));
#270948=CARTESIAN_POINT('Ctrl Pts',(43.7395647886014,30.744083456595,-40.6759056793254));
#270949=CARTESIAN_POINT('Ctrl Pts',(43.7090440489059,30.7747854825451,-40.6760208486551));
#270950=CARTESIAN_POINT('Ctrl Pts',(43.6947173014185,30.7907796762741,-40.6770802501629));
#270951=CARTESIAN_POINT('Ctrl Pts',(43.6678443418708,30.8240220908504,-40.6811258797777));
#270952=CARTESIAN_POINT('Ctrl Pts',(43.6427576069985,30.8585127548254,-40.687098273402));
#270953=CARTESIAN_POINT('Ctrl Pts',(43.6212142380078,30.8954846730083,-40.6968894358922));
#270954=CARTESIAN_POINT('Ctrl Pts',(43.6088787182641,30.9193798597989,-40.7042205511341));
#270955=CARTESIAN_POINT('Ctrl Pts',(43.6064685586478,30.9241994859948,-40.7057484197296));
#270956=CARTESIAN_POINT('Ctrl Pts',(43.6017624551859,30.9339175659931,-40.70892606686));
#270957=CARTESIAN_POINT('Ctrl Pts',(43.5994656231147,30.9388193592268,-40.7105773965538));
#270958=CARTESIAN_POINT('Ctrl Pts',(43.5927866482525,30.953560895212,-40.7156875255853));
#270959=CARTESIAN_POINT('Ctrl Pts',(43.5844198153918,30.9733582110501,-40.72293005151));
#270960=CARTESIAN_POINT('Ctrl Pts',(43.5734440082896,31.0034822735469,-40.7350537322951));
#270961=CARTESIAN_POINT('Ctrl Pts',(43.5640181327981,31.0340244080827,-40.7484125407461));
#270962=CARTESIAN_POINT('Ctrl Pts',(43.5561284133843,31.0649820306433,-40.7629929778707));
#270963=CARTESIAN_POINT('Ctrl Pts',(43.5518912037438,31.0858969805267,-40.7735241784737));
#270964=CARTESIAN_POINT('Ctrl Pts',(43.5481682579358,31.1069510729684,-40.7844620267622));
#270965=CARTESIAN_POINT('Ctrl Pts',(43.5465635963524,31.1175527760565,-40.7901372750232));
#270966=CARTESIAN_POINT('Ctrl Pts',(43.5438765944467,31.1388768366658,-40.8018865323646));
#270967=CARTESIAN_POINT('Ctrl Pts',(43.5427912565025,31.1496493641875,-40.8079902348016));
#270968=CARTESIAN_POINT('Ctrl Pts',(43.5411674088753,31.1711124235333,-40.8204828132684));
#270969=CARTESIAN_POINT('Ctrl Pts',(43.5400805588778,31.19253758885,-40.8332822237109));
#270970=CARTESIAN_POINT('Ctrl Pts',(43.5400129658238,31.2352236668913,-40.8600695429299));
#270971=CARTESIAN_POINT('Ctrl Pts',(43.5430492497798,31.2776738375434,-40.8886047446452));
#270972=CARTESIAN_POINT('Ctrl Pts',(43.5491614319672,31.3198884817001,-40.918856387552));
#270973=CARTESIAN_POINT('Ctrl Pts',(43.5532522131496,31.3409199794841,-40.9345594064291));
#270974=CARTESIAN_POINT('Ctrl Pts',(43.5578644352119,31.361905871423,-40.9505475151733));
#270975=CARTESIAN_POINT('Ctrl Pts',(43.560439098329,31.3723994717644,-40.9587035928991));
#270976=CARTESIAN_POINT('Ctrl Pts',(43.5660648897127,31.3931449423641,-40.9751492091434));
#270977=CARTESIAN_POINT('Ctrl Pts',(43.5691234314236,31.4034342087731,-40.9834667538713));
#270978=CARTESIAN_POINT('Ctrl Pts',(43.5790202279964,31.4340221767704,-41.0086741075936));
#270979=CARTESIAN_POINT('Ctrl Pts',(43.5865808644402,31.4540562960243,-41.0258289330007));
#270980=CARTESIAN_POINT('Ctrl Pts',(43.5993606039644,31.4835727602996,-41.0520789232858));
#270981=CARTESIAN_POINT('Ctrl Pts',(43.6038584649574,31.4933175175814,-41.0609109997729));
#270982=CARTESIAN_POINT('Ctrl Pts',(43.6133480280387,31.5126460303085,-41.0787663839806));
#270983=CARTESIAN_POINT('Ctrl Pts',(43.6183219077102,31.5221915251339,-41.0877549157913));
#270984=CARTESIAN_POINT('Ctrl Pts',(43.6338406007018,31.5503182102049,-41.1147514459697));
#270985=CARTESIAN_POINT('Ctrl Pts',(43.6450116757484,31.5684678157769,-41.13285712865));
#270986=CARTESIAN_POINT('Ctrl Pts',(43.6689569093208,31.6035742491305,-41.1692591986645));
#270987=CARTESIAN_POINT('Ctrl Pts',(43.6881189975485,31.6290150958394,-41.1967078345595));
#270988=CARTESIAN_POINT('Ctrl Pts',(43.7160805799803,31.6611548911343,-41.2335986369031));
#270989=CARTESIAN_POINT('Ctrl Pts',(43.7308739938731,31.6766212732249,-41.2521403517739));
#270990=CARTESIAN_POINT('Ctrl Pts',(43.7460847706871,31.6917854492915,-41.2707364845776));
#270991=CARTESIAN_POINT('Ctrl Pts',(43.7539033240721,31.6992171694526,-41.2800648729051));
#270992=CARTESIAN_POINT('Ctrl Pts',(43.7697797892606,31.7136063232936,-41.298562009488));
#270993=CARTESIAN_POINT('Ctrl Pts',(43.7778723272806,31.7205988773597,-41.3077734720143));
#270994=CARTESIAN_POINT('Ctrl Pts',(43.8025568401133,31.7409299545529,-41.3352381600133));
#270995=CARTESIAN_POINT('Ctrl Pts',(43.8195937300504,31.7536621581445,-41.353369616892));
#270996=CARTESIAN_POINT('Ctrl Pts',(43.8547939251157,31.7774712224987,-41.3892512463859));
#270997=CARTESIAN_POINT('Ctrl Pts',(43.8820456950658,31.7940939723408,-41.4158852269725));
#270998=CARTESIAN_POINT('Ctrl Pts',(43.9105977352555,31.8088239425505,-41.4420959852738));
#270999=CARTESIAN_POINT('Ctrl Pts',(43.9299312426308,31.8182163905263,-41.4594780331231));
#271000=CARTESIAN_POINT('Ctrl Pts',(43.9397545046832,31.8226994853967,-41.4681277754213));
#271001=CARTESIAN_POINT('Ctrl Pts',(43.959476379363,31.8311327029401,-41.4851373530728));
#271002=CARTESIAN_POINT('Ctrl Pts',(43.969416794615,31.835103670887,-41.4935351095415));
#271003=CARTESIAN_POINT('Ctrl Pts',(43.9894286782948,31.8425474915593,-41.5100965816665));
#271004=CARTESIAN_POINT('Ctrl Pts',(44.0196562937352,31.8529720625538,-41.5345993599874));
#271005=CARTESIAN_POINT('Ctrl Pts',(44.0607928561344,31.8639280327151,-41.5659272170578));
#271006=CARTESIAN_POINT('Ctrl Pts',(44.0922765794535,31.8699137146658,-41.5884145416429));
#271007=CARTESIAN_POINT('Ctrl Pts',(44.1134085621028,31.8733992175668,-41.6031789442838));
#271008=CARTESIAN_POINT('Ctrl Pts',(44.1240412545,31.8748890570172,-41.6104444862381));
#271009=CARTESIAN_POINT('Ctrl Pts',(44.1401138557838,31.8767382236783,-41.6211788509405));
#271010=CARTESIAN_POINT('Ctrl Pts',(44.1454877988083,31.8772894545129,-41.6247266008247));
#271011=CARTESIAN_POINT('Ctrl Pts',(44.1562140153048,31.878256418298,-41.6317257811562));
#271012=CARTESIAN_POINT('Ctrl Pts',(44.161576905651,31.8786734249769,-41.6351843345794));
#271013=CARTESIAN_POINT('Ctrl Pts',(44.1776466456902,31.8797244502982,-41.6454258391029));
#271014=CARTESIAN_POINT('Ctrl Pts',(44.1883500092183,31.8801603696231,-41.6520850220369));
#271015=CARTESIAN_POINT('Ctrl Pts',(44.2204087008324,31.8806796234647,-41.671549250448));
#271016=CARTESIAN_POINT('Ctrl Pts',(44.2417298059497,31.8799780982567,-41.6838534602333));
#271017=CARTESIAN_POINT('Ctrl Pts',(44.2842582084951,31.8764766164199,-41.7071185815018));
#271018=CARTESIAN_POINT('Ctrl Pts',(44.3054713486111,31.8736750129732,-41.7180819683776));
#271019=CARTESIAN_POINT('Ctrl Pts',(44.3319064277948,31.8688271235064,-41.7309251637703));
#271020=CARTESIAN_POINT('Ctrl Pts',(44.3371930873745,31.8677885276791,-41.7334519256467));
#271021=CARTESIAN_POINT('Ctrl Pts',(44.3477523920959,31.8655764110726,-41.7384157665409));
#271022=CARTESIAN_POINT('Ctrl Pts',(44.353035452149,31.8644001232798,-41.7408573895762));
#271023=CARTESIAN_POINT('Ctrl Pts',(44.368821997144,31.8606750365135,-41.7480268313348));
#271024=CARTESIAN_POINT('Ctrl Pts',(44.3792318927429,31.8579388865424,-41.752586114057));
#271025=CARTESIAN_POINT('Ctrl Pts',(44.4101727404,31.8489724804825,-41.7656371280416));
#271026=CARTESIAN_POINT('Ctrl Pts',(44.4405041748167,31.8385015328462,-41.7774224567595));
#271027=CARTESIAN_POINT('Ctrl Pts',(44.4797386522914,31.8215610256552,-41.7906399779756));
#271028=CARTESIAN_POINT('Ctrl Pts',(44.5085558494592,31.8073558935676,-41.7992982329201));
#271029=CARTESIAN_POINT('Ctrl Pts',(44.5273583247585,31.7968714183439,-41.8042246106906));
#271030=CARTESIAN_POINT('Ctrl Pts',(44.5459478308046,31.7858731708475,-41.8087197459362));
#271031=CARTESIAN_POINT('Ctrl Pts',(44.5551558111633,31.7801015230391,-41.8107541019367));
#271032=CARTESIAN_POINT('Ctrl Pts',(44.5731320510561,31.7681815367951,-41.814338976855));
#271033=CARTESIAN_POINT('Ctrl Pts',(44.5819448307914,31.7620078883687,-41.8159008719862));
#271034=CARTESIAN_POINT('Ctrl Pts',(44.5991987000126,31.7492554022398,-41.8185646224661));
#271035=CARTESIAN_POINT('Ctrl Pts',(44.6245350600795,31.7295108031857,-41.8218731379338));
#271036=CARTESIAN_POINT('Ctrl Pts',(44.6561620699444,31.7007477525095,-41.8235671758672));
#271037=CARTESIAN_POINT('Ctrl Pts',(44.6782580742923,31.6773394437008,-41.8227909065983));
#271038=CARTESIAN_POINT('Ctrl Pts',(44.6926220014235,31.6613194462407,-41.8218112048364));
#271039=CARTESIAN_POINT('Ctrl Pts',(44.6996188611148,31.6531046671394,-41.8210906882841));
#271040=CARTESIAN_POINT('Ctrl Pts',(44.7132456597446,31.6362429219073,-41.8191767031797));
#271041=CARTESIAN_POINT('Ctrl Pts',(44.7198193777268,31.627664624135,-41.8179905956202));
#271042=CARTESIAN_POINT('Ctrl Pts',(44.7324727845908,31.610252798272,-41.8151746307749));
#271043=CARTESIAN_POINT('Ctrl Pts',(44.7507253937504,31.5837345714901,-41.8102826177571));
#271044=CARTESIAN_POINT('Ctrl Pts',(44.7668325292565,31.5560404782777,-41.8034218375205));
#271045=CARTESIAN_POINT('Ctrl Pts',(44.7864242741839,31.5180816884312,-41.7925402952635));
#271046=CARTESIAN_POINT('Ctrl Pts',(44.7952779235527,31.4985810718442,-41.7862298998632));
#271047=CARTESIAN_POINT('Ctrl Pts',(44.8051436066325,31.4735589245645,-41.777240214754));
#271048=CARTESIAN_POINT('Ctrl Pts',(44.8070571630202,31.4685179927861,-41.7753849920635));
#271049=CARTESIAN_POINT('Ctrl Pts',(44.8107609555809,31.4583769076679,-41.7715655844892));
#271050=CARTESIAN_POINT('Ctrl Pts',(44.8125545845603,31.4532656516023,-41.76959682162));
#271051=CARTESIAN_POINT('Ctrl Pts',(44.8177323950795,31.4378873281915,-41.7635424458753));
#271052=CARTESIAN_POINT('Ctrl Pts',(44.8209059367305,31.4276035217402,-41.7593207739311));
#271053=CARTESIAN_POINT('Ctrl Pts',(44.8296276705658,31.3966113763671,-41.7460923602843));
#271054=CARTESIAN_POINT('Ctrl Pts',(44.8391161742293,31.3549585404116,-41.7269730343471));
#271055=CARTESIAN_POINT('Ctrl Pts',(44.8444380100638,31.312658433005,-41.7049510923314));
#271056=CARTESIAN_POINT('Ctrl Pts',(44.8468637082338,31.2806969121874,-41.6873414758157));
#271057=CARTESIAN_POINT('Ctrl Pts',(44.8474108190536,31.2699990859542,-41.6812863637077));
#271058=CARTESIAN_POINT('Ctrl Pts',(44.8478348231013,31.2538978106508,-41.671929084156));
#271059=CARTESIAN_POINT('Ctrl Pts',(44.8479099202363,31.2485174556463,-41.6687616517648));
#271060=CARTESIAN_POINT('Ctrl Pts',(44.8479268208064,31.2377432265879,-41.6623372317338));
#271061=CARTESIAN_POINT('Ctrl Pts',(44.8478683021095,31.2323379437313,-41.6590732331048));
#271062=CARTESIAN_POINT('Ctrl Pts',(44.8474921214824,31.2161555213209,-41.6491783400064));
#271063=CARTESIAN_POINT('Ctrl Pts',(44.8469759958029,31.2054292064128,-41.6424562576898));
#271064=CARTESIAN_POINT('Ctrl Pts',(44.8454249887827,31.1840681958411,-41.6287479728186));
#271065=CARTESIAN_POINT('Ctrl Pts',(44.8423204600693,31.1521790951542,-41.6077983885548));
#271066=CARTESIAN_POINT('Ctrl Pts',(44.8351290816859,31.1102584040656,-41.5783402141209));
#271067=CARTESIAN_POINT('Ctrl Pts',(44.8249268329474,31.0689281614894,-41.54736445114));
#271068=CARTESIAN_POINT('Ctrl Pts',(44.8188163283608,31.0484607830594,-41.5313656278891));
#271069=CARTESIAN_POINT('Ctrl Pts',(44.8121960627665,31.028093840338,-41.5151080950287));
#271070=CARTESIAN_POINT('Ctrl Pts',(44.808629563005,31.0179567656131,-41.5068467714969));
#271071=CARTESIAN_POINT('Ctrl Pts',(44.8009827391877,30.9977990758989,-41.4900714456835));
#271072=CARTESIAN_POINT('Ctrl Pts',(44.7969340070935,30.9878607344767,-41.4816261460579));
#271073=CARTESIAN_POINT('Ctrl Pts',(44.7926621173534,30.9780510210195,-41.4731170634489));
#271074=CARTESIAN_POINT('Origin',(-52.7694692252869,296.281453912738,10.95005));
#271075=CARTESIAN_POINT('Origin',(0.,0.,153.53805));
#271076=CARTESIAN_POINT('',(-63.0894692252869,-82.5030998968147,153.53805));
#271077=CARTESIAN_POINT('',(-63.0894692252869,-92.5030998968147,153.53805));
#271078=CARTESIAN_POINT('',(73.0894692252869,-82.5030998968147,153.53805));
#271079=CARTESIAN_POINT('Origin',(-73.0894692252869,-82.5030998968147,-17.14995));
#271080=CARTESIAN_POINT('Origin',(5.38401031719611,-82.5030998968147,-17.14995));
#271081=CARTESIAN_POINT('Ctrl Pts',(-0.169874834567261,-85.851674811826,
-27.1502359615018));
#271082=CARTESIAN_POINT('Ctrl Pts',(-0.145946434383659,-92.5030998968192,
-24.7866082076174));
#271083=CARTESIAN_POINT('Ctrl Pts',(-0.0748618073283795,-92.5030998968147,
-17.7280551702244));
#271084=CARTESIAN_POINT('Ctrl Pts',(0.394610061152761,-85.8685073521107,
-27.1502371407667));
#271085=CARTESIAN_POINT('Ctrl Pts',(0.338716347147105,-92.5030998968009,
-24.7784666680916));
#271086=CARTESIAN_POINT('Ctrl Pts',(0.173920958628183,-92.5030998968147,
-17.7306509939903));
#271087=CARTESIAN_POINT('Ctrl Pts',(0.962014587078309,-85.8002834495678,
-27.1502324270453));
#271088=CARTESIAN_POINT('Ctrl Pts',(0.828565975978851,-92.5030998968164,
-24.8114183373701));
#271089=CARTESIAN_POINT('Ctrl Pts',(0.422955977429241,-92.5030998968147,
-17.7201896452643));
#271090=CARTESIAN_POINT('Ctrl Pts',(1.93889369920201,-85.552294476256,-27.1502147670435));
#271091=CARTESIAN_POINT('Ctrl Pts',(1.69546368882409,-92.5030998968131,
-24.9368559750962));
#271092=CARTESIAN_POINT('Ctrl Pts',(0.896430364579228,-92.5030998968147,
-17.6799095294768));
#271093=CARTESIAN_POINT('Ctrl Pts',(2.35718494292016,-85.3865396246594,
-27.1502028196572));
#271094=CARTESIAN_POINT('Ctrl Pts',(2.08121842339136,-92.5030998968131,
-25.0233036000206));
#271095=CARTESIAN_POINT('Ctrl Pts',(1.12083047611226,-92.5030998968147,
-17.6522940965419));
#271096=CARTESIAN_POINT('Ctrl Pts',(3.0780812402123,-85.0202717903424,-27.1501754494839));
#271097=CARTESIAN_POINT('Ctrl Pts',(2.77549818896186,-92.5030998968163,
-25.2259546915078));
#271098=CARTESIAN_POINT('Ctrl Pts',(1.56980869024178,-92.5030998968147,
-17.5876430272881));
#271099=CARTESIAN_POINT('Ctrl Pts',(3.38194948801199,-84.8206163093558,
-27.1501601110217));
#271100=CARTESIAN_POINT('Ctrl Pts',(3.08467361627495,-92.5030998968131,
-25.3424934416491));
#271101=CARTESIAN_POINT('Ctrl Pts',(1.79438464918826,-92.5030998968147,
-17.5507208438431));
#271102=CARTESIAN_POINT('Ctrl Pts',(3.89377079482511,-84.4303577244072,
-27.1501289936074));
#271103=CARTESIAN_POINT('Ctrl Pts',(3.62855575415517,-92.5030998968163,
-25.5852049434394));
#271104=CARTESIAN_POINT('Ctrl Pts',(2.24356700539472,-92.5030998968147,
-17.4752655247545));
#271105=CARTESIAN_POINT('Ctrl Pts',(4.10257681992759,-84.2394549664702,
-27.1501132274934));
#271106=CARTESIAN_POINT('Ctrl Pts',(3.86265300096946,-92.5030998968147,
-25.711554223593));
#271107=CARTESIAN_POINT('Ctrl Pts',(2.46817300837612,-92.5030998968147,
-17.436753256288));
#271108=CARTESIAN_POINT('Ctrl Pts',(4.45337763448428,-83.8827081815476,
-27.1500827415735));
#271109=CARTESIAN_POINT('Ctrl Pts',(4.26906742896229,-92.5030998968147,
-25.9620711921812));
#271110=CARTESIAN_POINT('Ctrl Pts',(2.91730945232171,-92.5030998968147,
-17.3637278504744));
#271111=CARTESIAN_POINT('Ctrl Pts',(4.59558320478324,-83.716482094176,-27.1500680141482));
#271112=CARTESIAN_POINT('Ctrl Pts',(4.4403397493691,-92.5030998968132,-26.0861356446505));
#271113=CARTESIAN_POINT('Ctrl Pts',(3.14184022161926,-92.5030998968147,
-17.3291973359009));
#271114=CARTESIAN_POINT('Ctrl Pts',(4.83597577945107,-83.410864072468,-27.1500401253627));
#271115=CARTESIAN_POINT('Ctrl Pts',(4.73445387257387,-92.5030998968163,
-26.3263362157338));
#271116=CARTESIAN_POINT('Ctrl Pts',(3.59075876905671,-92.5030998968147,
-17.2677041352167));
#271117=CARTESIAN_POINT('Ctrl Pts',(4.93413245371605,-83.2712700024158,
-27.1500269570775));
#271118=CARTESIAN_POINT('Ctrl Pts',(4.85635963295471,-92.5030998968147,
-26.4422106175989));
#271119=CARTESIAN_POINT('Ctrl Pts',(3.81514693917863,-92.5030998968147,
-17.2407207033043));
#271120=CARTESIAN_POINT('Ctrl Pts',(5.19470999992647,-82.8737477208187,
-27.1499885377058));
#271121=CARTESIAN_POINT('Ctrl Pts',(5.17979449445077,-92.5030998968147,
-26.7890797663465));
#271122=CARTESIAN_POINT('Ctrl Pts',(4.5130376946388,-92.5030998968147,-17.171964762087));
#271123=CARTESIAN_POINT('Ctrl Pts',(5.30881834285142,-82.6567298213553,
-27.1499661445796));
#271124=CARTESIAN_POINT('Ctrl Pts',(5.31191864255755,-92.5030998968147,
-26.997459926319));
#271125=CARTESIAN_POINT('Ctrl Pts',(4.98621969734588,-92.5030998968147,
-17.1472825822804));
#271126=CARTESIAN_POINT('Ctrl Pts',(5.39841089769199,-82.472613872288,-27.1499468655863));
#271127=CARTESIAN_POINT('Ctrl Pts',(5.39819317091255,-92.5030998968147,
-27.1804541962469));
#271128=CARTESIAN_POINT('Ctrl Pts',(5.45887555911843,-92.5030998968147,
-17.150178956551));
#271129=CARTESIAN_POINT('Origin',(1.41042477321282E-15,-82.5030998968147,
-17.7284445206843));
#271130=CARTESIAN_POINT('Ctrl Pts',(-5.39809669430894,-82.4732737992708,
-27.1499469787481));
#271131=CARTESIAN_POINT('Ctrl Pts',(-5.39788655217846,-92.5030998968165,
-27.1797930106087));
#271132=CARTESIAN_POINT('Ctrl Pts',(-5.45726577017968,-92.5030998968147,
-17.1501706266968));
#271133=CARTESIAN_POINT('Ctrl Pts',(-5.30886063243231,-82.6566303581222,
-27.1499658967189));
#271134=CARTESIAN_POINT('Ctrl Pts',(-5.31191862612171,-92.5030998968037,
-26.9975597293636));
#271135=CARTESIAN_POINT('Ctrl Pts',(-4.98640454681432,-92.5030998968147,
-17.1473282668043));
#271136=CARTESIAN_POINT('Ctrl Pts',(-5.19437641593366,-82.8743413684576,
-27.1499880308083));
#271137=CARTESIAN_POINT('Ctrl Pts',(-5.17939033909145,-92.5030998968214,
-26.7885311413234));
#271138=CARTESIAN_POINT('Ctrl Pts',(-4.5118874940125,-92.5030998968147,
-17.1720464128354));
#271139=CARTESIAN_POINT('Ctrl Pts',(-4.93363058595232,-83.2720169605468,
-27.1500258986046));
#271140=CARTESIAN_POINT('Ctrl Pts',(-4.85573761804792,-92.5030998968116,
-26.4415790974878));
#271141=CARTESIAN_POINT('Ctrl Pts',(-3.81392533048433,-92.5030998968147,
-17.2408561198441));
#271142=CARTESIAN_POINT('Ctrl Pts',(-4.83539590630493,-83.4116638334138,
-27.1500388770639));
#271143=CARTESIAN_POINT('Ctrl Pts',(-4.73373456567037,-92.5030998968163,
-26.3256849257087));
#271144=CARTESIAN_POINT('Ctrl Pts',(-3.58954505611625,-92.5030998968147,
-17.2678587127851));
#271145=CARTESIAN_POINT('Ctrl Pts',(-4.5950226526386,-83.7171602823886,
-27.150066343477));
#271146=CARTESIAN_POINT('Ctrl Pts',(-4.43965961273775,-92.5030998968131,
-26.0856204646364));
#271147=CARTESIAN_POINT('Ctrl Pts',(-3.14092565857454,-92.5030998968147,
-17.3293343467266));
#271148=CARTESIAN_POINT('Ctrl Pts',(-4.4529164758076,-83.8832078848245,
-27.1500808379342));
#271149=CARTESIAN_POINT('Ctrl Pts',(-4.26852102169272,-92.5030998968131,
-25.9617090677426));
#271150=CARTESIAN_POINT('Ctrl Pts',(-2.91668691778663,-92.5030998968147,
-17.3638276255333));
#271151=CARTESIAN_POINT('Ctrl Pts',(-4.10263735547408,-84.2393897958904,
-27.1501108287274));
#271152=CARTESIAN_POINT('Ctrl Pts',(-3.86272243617917,-92.5030998968163,
-25.711600464872));
#271153=CARTESIAN_POINT('Ctrl Pts',(-2.46828355116468,-92.5030998968147,
-17.4367367279748));
#271154=CARTESIAN_POINT('Ctrl Pts',(-3.89426477057059,-84.4299010626526,
-27.1501263322654));
#271155=CARTESIAN_POINT('Ctrl Pts',(-3.62910775040391,-92.5030998968131,
-25.5855037071153));
#271156=CARTESIAN_POINT('Ctrl Pts',(-2.24411925992876,-92.5030998968147,
-17.4751702604172));
#271157=CARTESIAN_POINT('Ctrl Pts',(-3.38365208284729,-84.8194236006233,
-27.1501569388914));
#271158=CARTESIAN_POINT('Ctrl Pts',(-3.08643540678968,-92.5030998968163,
-25.3432079853536));
#271159=CARTESIAN_POINT('Ctrl Pts',(-1.79576147994535,-92.5030998968147,
-17.5504920425344));
#271160=CARTESIAN_POINT('Ctrl Pts',(-3.08057929275139,-85.0187465574387,
-27.1501720300308));
#271161=CARTESIAN_POINT('Ctrl Pts',(-2.77799526160932,-92.5030998968131,
-25.2268269826121));
#271162=CARTESIAN_POINT('Ctrl Pts',(-1.57156765625021,-92.5030998968147,
-17.5873625651759));
#271163=CARTESIAN_POINT('Ctrl Pts',(-2.36100384729412,-85.3848777755655,
-27.150198993857));
#271164=CARTESIAN_POINT('Ctrl Pts',(-2.08479461247351,-92.5030998968162,
-25.0241879469932));
#271165=CARTESIAN_POINT('Ctrl Pts',(-1.12300814069231,-92.5030998968147,
-17.6520074619466));
#271166=CARTESIAN_POINT('Ctrl Pts',(-1.94321144755505,-85.5508732644712,
-27.1502107853729));
#271167=CARTESIAN_POINT('Ctrl Pts',(-1.69937754472461,-92.5030998968131,
-24.9375848748653));
#271168=CARTESIAN_POINT('Ctrl Pts',(-0.898640395518054,-92.5030998968147,
-17.6796731644661));
#271169=CARTESIAN_POINT('Ctrl Pts',(-0.966563031715962,-85.7995116268941,
-27.1502282342258));
#271170=CARTESIAN_POINT('Ctrl Pts',(-0.832525978497703,-92.5030998968165,
-24.8117943080671));
#271171=CARTESIAN_POINT('Ctrl Pts',(-0.425031788870384,-92.5030998968147,
-17.7200662512515));
#271172=CARTESIAN_POINT('Ctrl Pts',(-0.398829554477319,-85.8683863875495,
-27.150232923976));
#271173=CARTESIAN_POINT('Ctrl Pts',(-0.342329126887928,-92.5030998968067,
-24.7785206905936));
#271174=CARTESIAN_POINT('Ctrl Pts',(-0.175752411133516,-92.5030998968147,
-17.7306309540816));
#271175=CARTESIAN_POINT('Ctrl Pts',(0.167436639224824,-85.8517605842216,
-27.1502317757357));
#271176=CARTESIAN_POINT('Ctrl Pts',(0.143847524607735,-92.5030998968173,
-24.7865630937963));
#271177=CARTESIAN_POINT('Ctrl Pts',(0.0737804994758404,-92.5030998968147,
-17.7280665405117));
#271178=CARTESIAN_POINT('Origin',(-5.38401031719611,-82.5030998968147,-17.14995));
#271179=CARTESIAN_POINT('Origin',(0.,-82.5030998968147,143.53805));
#271180=CARTESIAN_POINT('Origin',(-63.0894692252869,-82.5030998968147,143.53805));
#271181=CARTESIAN_POINT('Origin',(-63.0894692252869,-82.5030998968147,178.93805));
#271182=CARTESIAN_POINT('Origin',(-63.0894692252869,-82.5030998968147,-17.14995));
#271183=CARTESIAN_POINT('Origin',(-63.0894692252869,-82.5030998968147,143.53805));
#271184=CARTESIAN_POINT('Origin',(-73.0894692252869,-82.5030998968147,-17.14995));
#271185=CARTESIAN_POINT('Origin',(-63.0894692252869,-82.5030998968147,-17.14995));
#271186=CARTESIAN_POINT('Origin',(-63.0894692252869,-82.5030998968147,143.53805));
#271187=CARTESIAN_POINT('Origin',(-63.0894692252869,-82.5030998968147,143.53805));
#271188=CARTESIAN_POINT('Origin',(-63.0894692252869,-82.5030998968147,-17.14995));
#271189=CARTESIAN_POINT('Origin',(-63.0894692252869,-82.5030998968147,-17.14995));
#271190=CARTESIAN_POINT('Origin',(-63.0894692252869,0.,143.53805));
#271191=CARTESIAN_POINT('Origin',(-63.0894692252885,54.390525141761,143.538050000002));
#271192=CARTESIAN_POINT('Origin',(-63.0894692252869,-64.3905251417593,-17.14995));
#271193=CARTESIAN_POINT('Origin',(-63.0894692252876,54.39052514176,-17.1499500000007));
#271194=CARTESIAN_POINT('Origin',(-63.0894692252869,54.3905251417593,178.93805));
#271195=CARTESIAN_POINT('',(0.,0.,0.));
#271196=CARTESIAN_POINT('Origin',(10.,130.,910.));
#271197=CARTESIAN_POINT('',(0.,130.,910.));
#271198=CARTESIAN_POINT('',(0.,0.,910.));
#271199=CARTESIAN_POINT('',(0.,130.,910.));
#271200=CARTESIAN_POINT('',(10.,0.,910.));
#271201=CARTESIAN_POINT('',(10.,0.,910.));
#271202=CARTESIAN_POINT('',(10.,130.,910.));
#271203=CARTESIAN_POINT('',(10.,130.,910.));
#271204=CARTESIAN_POINT('',(10.,130.,910.));
#271205=CARTESIAN_POINT('Origin',(10.,0.,910.));
#271206=CARTESIAN_POINT('',(0.,2.77555756156289E-14,-910.));
#271207=CARTESIAN_POINT('',(0.,0.,910.));
#271208=CARTESIAN_POINT('',(10.,2.77555756156289E-14,-910.));
#271209=CARTESIAN_POINT('',(10.,2.77555756156289E-14,-910.));
#271210=CARTESIAN_POINT('',(10.,0.,910.));
#271211=CARTESIAN_POINT('Origin',(10.,130.,-910.));
#271212=CARTESIAN_POINT('',(0.,130.,-910.));
#271213=CARTESIAN_POINT('',(0.,130.,-910.));
#271214=CARTESIAN_POINT('',(10.,130.,-910.));
#271215=CARTESIAN_POINT('',(10.,130.,-910.));
#271216=CARTESIAN_POINT('',(10.,130.,-910.));
#271217=CARTESIAN_POINT('Origin',(10.,130.,910.));
#271218=CARTESIAN_POINT('',(0.,130.,910.));
#271219=CARTESIAN_POINT('',(10.,130.,910.));
#271220=CARTESIAN_POINT('Origin',(10.,0.,0.));
#271221=CARTESIAN_POINT('Origin',(0.,0.,0.));
#271222=CARTESIAN_POINT('',(0.,0.,0.));
#271223=CARTESIAN_POINT('',(0.,0.,0.));
#271224=CARTESIAN_POINT('Origin',(-9.8073702912372,3.06591104035337,1.49207703394933));
#271225=CARTESIAN_POINT('',(-9.2313702912372,3.06591104035336,34.4680770339493));
#271226=CARTESIAN_POINT('Origin',(-9.2313702912372,3.06591104035337,1.49207703394933));
#271227=CARTESIAN_POINT('',(-9.8073702912372,3.06591104035336,33.8920770339493));
#271228=CARTESIAN_POINT('Origin',(-9.8073702912372,3.06591104035336,34.4680770339493));
#271229=CARTESIAN_POINT('Origin',(-9.8073702912372,3.06591104035337,1.49207703394933));
#271230=CARTESIAN_POINT('Origin',(-22.7900502912372,3.06591104035337,1.49207703394933));
#271231=CARTESIAN_POINT('',(-22.7900502912372,3.06591104035336,33.8920770339493));
#271232=CARTESIAN_POINT('',(-22.7900502912372,3.06591104035336,33.8920770339493));
#271233=CARTESIAN_POINT('Origin',(-22.7900502912372,3.06591104035337,1.49207703394933));
#271234=CARTESIAN_POINT('Origin',(2.4103097087628,-39.1068178299802,-0.976120122868075));
#271235=CARTESIAN_POINT('',(0.0328697087628034,-42.1293633290516,22.1517542177188));
#271236=CARTESIAN_POINT('',(2.35340786587074,-33.8599370650904,21.750617325498));
#271237=CARTESIAN_POINT('Ctrl Pts',(0.032869708762803,-42.1293633290516,
22.1517542177189));
#271238=CARTESIAN_POINT('Ctrl Pts',(0.0352790378720918,-42.1243919042646,
22.1524039254003));
#271239=CARTESIAN_POINT('Ctrl Pts',(0.0376867650499835,-42.1194196830561,
22.1530521068472));
#271240=CARTESIAN_POINT('Ctrl Pts',(0.986850403300165,-40.1576732102835,
22.4081429612987));
#271241=CARTESIAN_POINT('Ctrl Pts',(1.68188687638377,-38.0910153822988,
22.4207048816548));
#271242=CARTESIAN_POINT('Ctrl Pts',(2.20268963592813,-35.2864204920949,
22.0449936368422));
#271243=CARTESIAN_POINT('Ctrl Pts',(2.2980625106802,-34.5685597403789,21.9142157607324));
#271244=CARTESIAN_POINT('Ctrl Pts',(2.35340786587134,-33.8599370650903,
21.750617325498));
#271245=CARTESIAN_POINT('',(-9.17446844834575,-33.8599370650904,21.750617325498));
#271246=CARTESIAN_POINT('',(2.4103097087628,-33.8599370650904,21.750617325498));
#271247=CARTESIAN_POINT('',(-6.85393029123721,-42.1293633290516,22.1517542177189));
#271248=CARTESIAN_POINT('Ctrl Pts',(-9.17446844834572,-33.8599370650904,
21.750617325498));
#271249=CARTESIAN_POINT('Ctrl Pts',(-9.0531834377728,-35.4128281499478,
22.1091304812741));
#271250=CARTESIAN_POINT('Ctrl Pts',(-8.74406947844718,-36.9665376966092,
22.2993317754169));
#271251=CARTESIAN_POINT('Ctrl Pts',(-7.90182428445088,-39.743167770045,
22.3739423544079));
#271252=CARTESIAN_POINT('Ctrl Pts',(-7.41851411808578,-40.9643975216401,
22.3040017656738));
#271253=CARTESIAN_POINT('Ctrl Pts',(-6.85393029123719,-42.1293633290516,
22.1517542177189));
#271254=CARTESIAN_POINT('',(-3.4105302912372,-42.1293633290516,22.1517542177189));
#271255=CARTESIAN_POINT('Origin',(2.4103097087628,-32.5610768757423,-24.3924448318277));
#271256=CARTESIAN_POINT('',(2.4103097087628,-32.2877498558738,-18.6249498118703));
#271257=CARTESIAN_POINT('',(2.35340786587186,-33.8599370650901,-18.7664632575998));
#271258=CARTESIAN_POINT('Ctrl Pts',(2.41030970876281,-32.2877498558686,
-18.6249498118705));
#271259=CARTESIAN_POINT('Ctrl Pts',(2.41030970876289,-32.7156984306091,
-18.604668925942));
#271260=CARTESIAN_POINT('Ctrl Pts',(2.3994466364292,-33.1452146487367,-18.6320357943675));
#271261=CARTESIAN_POINT('Ctrl Pts',(2.36767303424712,-33.6663772566688,
-18.7243858860329));
#271262=CARTESIAN_POINT('Ctrl Pts',(2.36093683952928,-33.7635387054221,
-18.7442079426758));
#271263=CARTESIAN_POINT('Ctrl Pts',(2.35340786587134,-33.8599370650901,
-18.7664632575998));
#271264=CARTESIAN_POINT('',(-9.17446844834572,-33.8599370650901,-18.7664632575998));
#271265=CARTESIAN_POINT('',(2.4103097087628,-33.8599370650901,-18.7664632575998));
#271266=CARTESIAN_POINT('',(-9.2313702912372,-32.2877498558738,-18.6249498118703));
#271267=CARTESIAN_POINT('Ctrl Pts',(-9.17446844834573,-33.8599370650901,
-18.7664632575998));
#271268=CARTESIAN_POINT('Ctrl Pts',(-9.21458398225969,-33.3463117235494,
-18.6478835040821));
#271269=CARTESIAN_POINT('Ctrl Pts',(-9.23137029123717,-32.8175683814159,
-18.5998412130495));
#271270=CARTESIAN_POINT('Ctrl Pts',(-9.2313702912372,-32.2877498558753,
-18.6249498118702));
#271271=CARTESIAN_POINT('',(-9.2313702912372,-26.9914004601507,-25.9147493646419));
#271272=CARTESIAN_POINT('Origin',(-9.2313702912372,-32.5610768757423,-24.3924448318277));
#271273=CARTESIAN_POINT('',(-9.17446844834575,-27.6118203108419,-27.3662581951399));
#271274=CARTESIAN_POINT('Ctrl Pts',(-9.2313702912372,-26.9914004601507,
-25.9147493646419));
#271275=CARTESIAN_POINT('Ctrl Pts',(-9.2313702912372,-27.0255164279608,
-26.0395699226914));
#271276=CARTESIAN_POINT('Ctrl Pts',(-9.2303894871794,-27.0638636212061,
-26.1633730084678));
#271277=CARTESIAN_POINT('Ctrl Pts',(-9.22181693596821,-27.2377195901812,
-26.6642059035602));
#271278=CARTESIAN_POINT('Ctrl Pts',(-9.20467998252579,-27.4073538643018,
-27.0259688833341));
#271279=CARTESIAN_POINT('Ctrl Pts',(-9.17446844834573,-27.6118203108419,
-27.3662581951399));
#271280=CARTESIAN_POINT('',(2.3534078658721,-27.6118203108419,-27.3662581951399));
#271281=CARTESIAN_POINT('',(2.4103097087628,-27.6118203108419,-27.3662581951399));
#271282=CARTESIAN_POINT('',(2.4103097087628,-26.9914004601507,-25.9147493646419));
#271283=CARTESIAN_POINT('Ctrl Pts',(2.35340786587134,-27.6118203108419,
-27.3662581951399));
#271284=CARTESIAN_POINT('Ctrl Pts',(2.36852800519452,-27.5094898187796,
-27.1959516567818));
#271285=CARTESIAN_POINT('Ctrl Pts',(2.38043097016003,-27.4156364467956,
-27.0198481109634));
#271286=CARTESIAN_POINT('Ctrl Pts',(2.40398237976074,-27.1912363180884,
-26.5400168162761));
#271287=CARTESIAN_POINT('Ctrl Pts',(2.41030970876281,-27.0778295126518,
-26.2309685211646));
#271288=CARTESIAN_POINT('Ctrl Pts',(2.41030970876281,-26.9914004601507,
-25.9147493646419));
#271289=CARTESIAN_POINT('Origin',(2.4103097087628,-32.5610768757423,-24.3924448318277));
#271290=CARTESIAN_POINT('Origin',(2.4103097087628,-18.9527784085753,-36.6454118076767));
#271291=CARTESIAN_POINT('',(2.4103097087628,-13.2454487831566,-35.7707147104817));
#271292=CARTESIAN_POINT('',(2.4103097087628,-21.0489333144974,-31.2653708156951));
#271293=CARTESIAN_POINT('Origin',(2.4103097087628,-18.9527784085753,-36.6454118076767));
#271294=CARTESIAN_POINT('',(2.35340786587055,-22.4276390941746,-32.034115929));
#271295=CARTESIAN_POINT('Ctrl Pts',(2.41030970876281,-21.0489333144974,
-31.2653708156951));
#271296=CARTESIAN_POINT('Ctrl Pts',(2.41030970876281,-21.4481327705155,
-31.4209056711769));
#271297=CARTESIAN_POINT('Ctrl Pts',(2.3994466364291,-21.8293842523733,-31.620606534224));
#271298=CARTESIAN_POINT('Ctrl Pts',(2.36767303424712,-22.2679278192698,
-31.9169484706239));
#271299=CARTESIAN_POINT('Ctrl Pts',(2.36093683952928,-22.3486268626585,
-31.9745759419334));
#271300=CARTESIAN_POINT('Ctrl Pts',(2.35340786587133,-22.4276390941746,
-32.0341159290001));
#271301=CARTESIAN_POINT('',(-9.17446844834572,-22.4276390941746,-32.034115929));
#271302=CARTESIAN_POINT('',(2.4103097087628,-22.4276390941746,-32.034115929));
#271303=CARTESIAN_POINT('',(-9.2313702912372,-21.0489333144974,-31.2653708156951));
#271304=CARTESIAN_POINT('Ctrl Pts',(-9.17446844834573,-22.4276390941746,
-32.034115929));
#271305=CARTESIAN_POINT('Ctrl Pts',(-9.21458398225983,-22.006649727361,
-31.7168776865875));
#271306=CARTESIAN_POINT('Ctrl Pts',(-9.2313702912372,-21.5431592090758,
-31.457929577812));
#271307=CARTESIAN_POINT('Ctrl Pts',(-9.2313702912372,-21.0489333144974,
-31.2653708156951));
#271308=CARTESIAN_POINT('',(-9.2313702912372,-13.2454487831566,-35.7707147104817));
#271309=CARTESIAN_POINT('Origin',(-9.2313702912372,-18.9527784085753,-36.6454118076767));
#271310=CARTESIAN_POINT('',(-9.17446844834574,-13.2218486904752,-37.349081496679));
#271311=CARTESIAN_POINT('Ctrl Pts',(-9.2313702912372,-13.2454487831566,
-35.7707147104817));
#271312=CARTESIAN_POINT('Ctrl Pts',(-9.2313702912372,-13.2258461758147,
-35.8986201785306));
#271313=CARTESIAN_POINT('Ctrl Pts',(-9.2303894871794,-13.2105228285062,
-36.0273171338357));
#271314=CARTESIAN_POINT('Ctrl Pts',(-9.2218169359682,-13.1656410687555,
-36.5555643433858));
#271315=CARTESIAN_POINT('Ctrl Pts',(-9.20467998252573,-13.1734674293567,
-36.9550477455079));
#271316=CARTESIAN_POINT('Ctrl Pts',(-9.17446844834573,-13.2218486904752,
-37.349081496679));
#271317=CARTESIAN_POINT('',(2.3534078658719,-13.2218486904752,-37.349081496679));
#271318=CARTESIAN_POINT('',(2.4103097087628,-13.2218486904752,-37.349081496679));
#271319=CARTESIAN_POINT('Ctrl Pts',(2.35340786587134,-13.2218486904752,
-37.349081496679));
#271320=CARTESIAN_POINT('Ctrl Pts',(2.36852800519451,-13.197635043979,-37.1518771713295));
#271321=CARTESIAN_POINT('Ctrl Pts',(2.38043097016002,-13.1835234873784,
-36.9528249715102));
#271322=CARTESIAN_POINT('Ctrl Pts',(2.40398237976074,-13.1736887391474,
-36.4232055167577));
#271323=CARTESIAN_POINT('Ctrl Pts',(2.41030970876281,-13.195787733277,-36.0947491472211));
#271324=CARTESIAN_POINT('Ctrl Pts',(2.41030970876281,-13.2454487831566,
-35.7707147104817));
#271325=CARTESIAN_POINT('Origin',(2.4103097087628,32.5326690847323,-31.234073221581));
#271326=CARTESIAN_POINT('',(2.4103097087628,33.4644445574145,-25.5357839227184));
#271327=CARTESIAN_POINT('',(2.4103097087628,26.7681985526008,-31.565110907066));
#271328=CARTESIAN_POINT('Origin',(2.4103097087628,32.5326690847323,-31.234073221581));
#271329=CARTESIAN_POINT('',(2.35340786587078,27.0732750858163,-33.1138933272357));
#271330=CARTESIAN_POINT('Ctrl Pts',(2.41030970876281,26.7681985526008,-31.565110907066));
#271331=CARTESIAN_POINT('Ctrl Pts',(2.41030970876281,26.7927615743629,-31.992835064575));
#271332=CARTESIAN_POINT('Ctrl Pts',(2.3994466364291,26.864875194449,-32.417137731216));
#271333=CARTESIAN_POINT('Ctrl Pts',(2.36767303424712,27.0111957091688,-32.9257921426857));
#271334=CARTESIAN_POINT('Ctrl Pts',(2.36093683952928,27.0410653154384,-33.0203493617368));
#271335=CARTESIAN_POINT('Ctrl Pts',(2.35340786587133,27.0732750858163,-33.1138933272358));
#271336=CARTESIAN_POINT('',(-9.17446844834572,27.0732750858163,-33.1138933272357));
#271337=CARTESIAN_POINT('',(2.4103097087628,27.0732750858163,-33.1138933272357));
#271338=CARTESIAN_POINT('',(-9.2313702912372,26.7681985526008,-31.565110907066));
#271339=CARTESIAN_POINT('Ctrl Pts',(-9.17446844834573,27.0732750858163,
-33.1138933272357));
#271340=CARTESIAN_POINT('Ctrl Pts',(-9.21458398225973,26.9016564569488,
-32.6154766384669));
#271341=CARTESIAN_POINT('Ctrl Pts',(-9.2313702912372,26.798608617597,-32.094651594538));
#271342=CARTESIAN_POINT('Ctrl Pts',(-9.2313702912372,26.7681985526008,-31.565110907066));
#271343=CARTESIAN_POINT('',(-9.2313702912372,33.4644445574145,-25.5357839227184));
#271344=CARTESIAN_POINT('Origin',(-9.2313702912372,32.5326690847323,-31.234073221581));
#271345=CARTESIAN_POINT('',(-9.17446844834452,34.9728534042387,-26.0010810610805));
#271346=CARTESIAN_POINT('Ctrl Pts',(-9.2313702912372,33.4644445574145,-25.5357839227184));
#271347=CARTESIAN_POINT('Ctrl Pts',(-9.2313702912372,33.5921474250748,-25.5566656985701));
#271348=CARTESIAN_POINT('Ctrl Pts',(-9.2303894871794,33.7192806777741,-25.5818618755744));
#271349=CARTESIAN_POINT('Ctrl Pts',(-9.22181693596821,34.2355428551313,
-25.7024141504828));
#271350=CARTESIAN_POINT('Ctrl Pts',(-9.20467998252578,34.6130556694415,
-25.8333046219577));
#271351=CARTESIAN_POINT('Ctrl Pts',(-9.17446844834572,34.9728534042388,
-26.0010810610805));
#271352=CARTESIAN_POINT('',(2.35340786587065,34.9728534042387,-26.0010810610805));
#271353=CARTESIAN_POINT('',(2.4103097087628,34.9728534042387,-26.0010810610805));
#271354=CARTESIAN_POINT('Ctrl Pts',(2.35340786587133,34.9728534042387,-26.0010810610805));
#271355=CARTESIAN_POINT('Ctrl Pts',(2.36852800519451,34.7927833738366,-25.9171130268998));
#271356=CARTESIAN_POINT('Ctrl Pts',(2.38043097016002,34.6078341929221,-25.8421816265278));
#271357=CARTESIAN_POINT('Ctrl Pts',(2.40398237976075,34.1071752636619,-25.6691668130665));
#271358=CARTESIAN_POINT('Ctrl Pts',(2.41030970876281,33.7879657283509,-25.5886856053395));
#271359=CARTESIAN_POINT('Ctrl Pts',(2.41030970876281,33.4644445574145,-25.5357839227184));
#271360=CARTESIAN_POINT('Origin',(2.4103097087628,43.296058498978,-16.4195386288221));
#271361=CARTESIAN_POINT('',(2.35340786587189,43.3968281352698,-10.6464500321153));
#271362=CARTESIAN_POINT('',(2.4103097087628,41.8295746888954,-10.8349050956536));
#271363=CARTESIAN_POINT('Ctrl Pts',(2.35340786587134,43.3968281352698,-10.6464500321153));
#271364=CARTESIAN_POINT('Ctrl Pts',(2.36852800519451,43.19817310059,-10.6429824955866));
#271365=CARTESIAN_POINT('Ctrl Pts',(2.38043097016002,42.9987362702226,-10.6497548641268));
#271366=CARTESIAN_POINT('Ctrl Pts',(2.40398237976065,42.4709901151412,-10.6953342993973));
#271367=CARTESIAN_POINT('Ctrl Pts',(2.41030970876272,42.1466430378622,-10.7516452724824));
#271368=CARTESIAN_POINT('Ctrl Pts',(2.41030970876281,41.8295746889017,-10.8349050956519));
#271369=CARTESIAN_POINT('',(2.4103097087628,38.1645977855604,-19.066577996054));
#271370=CARTESIAN_POINT('Origin',(2.4103097087628,43.296058498978,-16.4195386288221));
#271371=CARTESIAN_POINT('',(2.35340786587133,39.0732456291474,-20.3573753358755));
#271372=CARTESIAN_POINT('Ctrl Pts',(2.41030970876281,38.1645977855604,-19.066577996054));
#271373=CARTESIAN_POINT('Ctrl Pts',(2.41030970876281,38.3610083105048,-19.4473327762551));
#271374=CARTESIAN_POINT('Ctrl Pts',(2.3994466364291,38.5994668228463,-19.8056212982767));
#271375=CARTESIAN_POINT('Ctrl Pts',(2.36767303424712,38.9400256522353,-20.2107863104145));
#271376=CARTESIAN_POINT('Ctrl Pts',(2.36093683952928,39.00577278122,-20.2850195649818));
#271377=CARTESIAN_POINT('Ctrl Pts',(2.35340786587133,39.0732456291474,-20.3573753358755));
#271378=CARTESIAN_POINT('',(-9.17446844834689,39.0732456291474,-20.3573753358755));
#271379=CARTESIAN_POINT('',(2.4103097087628,39.0732456291474,-20.3573753358755));
#271380=CARTESIAN_POINT('',(-9.2313702912372,38.1645977855604,-19.066577996054));
#271381=CARTESIAN_POINT('Ctrl Pts',(-9.17446844834573,39.0732456291473,
-20.3573753358754));
#271382=CARTESIAN_POINT('Ctrl Pts',(-9.21458398225972,38.7137398794559,
-19.9718526188323));
#271383=CARTESIAN_POINT('Ctrl Pts',(-9.2313702912372,38.4077623638987,-19.5379685979788));
#271384=CARTESIAN_POINT('Ctrl Pts',(-9.2313702912372,38.1645977855604,-19.066577996054));
#271385=CARTESIAN_POINT('',(-9.2313702912372,41.8295746888954,-10.8349050956536));
#271386=CARTESIAN_POINT('Origin',(-9.2313702912372,43.296058498978,-16.4195386288221));
#271387=CARTESIAN_POINT('',(-9.17446844834574,43.3968281352698,-10.6464500321153));
#271388=CARTESIAN_POINT('Ctrl Pts',(-9.2313702912372,41.829574688899,-10.8349050956526));
#271389=CARTESIAN_POINT('Ctrl Pts',(-9.23137029123718,41.9547304469883,
-10.8020401114265));
#271390=CARTESIAN_POINT('Ctrl Pts',(-9.23038948717938,42.081120660959,-10.7733482120529));
#271391=CARTESIAN_POINT('Ctrl Pts',(-9.22181693596821,42.6017826556463,
-10.6734954502389));
#271392=CARTESIAN_POINT('Ctrl Pts',(-9.20467998252579,42.9998957233396,
-10.6395215510929));
#271393=CARTESIAN_POINT('Ctrl Pts',(-9.17446844834573,43.3968281352698,
-10.6464500321153));
#271394=CARTESIAN_POINT('',(2.4103097087628,43.3968281352698,-10.6464500321153));
#271395=CARTESIAN_POINT('Origin',(2.4103097087628,16.6742095075206,-40.3899591274171));
#271396=CARTESIAN_POINT('',(2.4103097087628,19.8431318188264,-35.5633000499669));
#271397=CARTESIAN_POINT('',(2.4103097087628,11.2734584802515,-38.347755707952));
#271398=CARTESIAN_POINT('Origin',(2.4103097087628,16.6742095075206,-40.3899591274171));
#271399=CARTESIAN_POINT('',(2.35340786587083,10.9222131989692,-39.886724657776));
#271400=CARTESIAN_POINT('Ctrl Pts',(2.41030970876281,11.2734584802515,-38.347755707952));
#271401=CARTESIAN_POINT('Ctrl Pts',(2.41030970876281,11.1219268292206,-38.7484918501837));
#271402=CARTESIAN_POINT('Ctrl Pts',(2.3994466364291,11.0152264570068,-39.165442875713));
#271403=CARTESIAN_POINT('Ctrl Pts',(2.36767303424712,10.9420085107821,-39.6896357177914));
#271404=CARTESIAN_POINT('Ctrl Pts',(2.36093683952928,10.9308358680558,-39.7881670991269));
#271405=CARTESIAN_POINT('Ctrl Pts',(2.35340786587133,10.9222131989692,-39.886724657776));
#271406=CARTESIAN_POINT('',(-9.17446844834572,10.9222131989692,-39.886724657776));
#271407=CARTESIAN_POINT('',(2.4103097087628,10.9222131989692,-39.886724657776));
#271408=CARTESIAN_POINT('',(-9.2313702912372,11.2734584802515,-38.347755707952));
#271409=CARTESIAN_POINT('Ctrl Pts',(-9.17446844834573,10.9222131989692,
-39.886724657776));
#271410=CARTESIAN_POINT('Ctrl Pts',(-9.21458398225962,10.9681561109631,
-39.3615947707445));
#271411=CARTESIAN_POINT('Ctrl Pts',(-9.2313702912372,11.0858558554005,-38.8438840853825));
#271412=CARTESIAN_POINT('Ctrl Pts',(-9.2313702912372,11.2734584802515,-38.347755707952));
#271413=CARTESIAN_POINT('',(-9.2313702912372,19.8431318188264,-35.5633000499669));
#271414=CARTESIAN_POINT('Origin',(-9.2313702912372,16.6742095075206,-40.3899591274171));
#271415=CARTESIAN_POINT('',(-9.17446844834461,21.0318784730203,-36.6018952879149));
#271416=CARTESIAN_POINT('Ctrl Pts',(-9.2313702912372,19.8431318188264,-35.5633000499669));
#271417=CARTESIAN_POINT('Ctrl Pts',(-9.2313702912372,19.951300810094,-35.6343179371471));
#271418=CARTESIAN_POINT('Ctrl Pts',(-9.2303894871794,20.0571946071597,-35.7090455426256));
#271419=CARTESIAN_POINT('Ctrl Pts',(-9.22181693596822,20.479790546625,-36.0291582707414));
#271420=CARTESIAN_POINT('Ctrl Pts',(-9.20467998252584,20.7714277123617,
-36.3022809612165));
#271421=CARTESIAN_POINT('Ctrl Pts',(-9.17446844834572,21.0318784730204,
-36.6018952879149));
#271422=CARTESIAN_POINT('',(2.35340786587133,21.0318784730203,-36.6018952879149));
#271423=CARTESIAN_POINT('',(2.4103097087628,21.0318784730203,-36.6018952879149));
#271424=CARTESIAN_POINT('Ctrl Pts',(2.35340786587133,21.0318784730203,-36.6018952879149));
#271425=CARTESIAN_POINT('Ctrl Pts',(2.36852800519452,20.9015291910372,-36.4519455920175));
#271426=CARTESIAN_POINT('Ctrl Pts',(2.38043097016003,20.7630470531663,-36.3082667425882));
#271427=CARTESIAN_POINT('Ctrl Pts',(2.40398237976075,20.3760438269421,-35.9465735134324));
#271428=CARTESIAN_POINT('Ctrl Pts',(2.41030970876281,20.1171660621841,-35.7432160568577));
#271429=CARTESIAN_POINT('Ctrl Pts',(2.41030970876281,19.8431318188264,-35.5633000499669));
#271430=CARTESIAN_POINT('Origin',(2.4103097087628,-1.5372485021747,-42.3040604945994));
#271431=CARTESIAN_POINT('',(2.4103097087628,3.32088519137438,-39.1836048418737));
#271432=CARTESIAN_POINT('',(2.4103097087628,-5.64044110768385,-38.2417314942451));
#271433=CARTESIAN_POINT('Origin',(2.4103097087628,-1.5372485021747,-42.3040604945994));
#271434=CARTESIAN_POINT('',(2.35340786587068,-6.58727470336698,-39.5047852612049));
#271435=CARTESIAN_POINT('Ctrl Pts',(2.41030970876281,-5.64044110768385,
-38.2417314942451));
#271436=CARTESIAN_POINT('Ctrl Pts',(2.41030970876281,-5.9418662324227,-38.5461887016341));
#271437=CARTESIAN_POINT('Ctrl Pts',(2.3994466364291,-6.20893113323825,-38.8836934658567));
#271438=CARTESIAN_POINT('Ctrl Pts',(2.36767303424712,-6.48902749234103,
-39.3327870340057));
#271439=CARTESIAN_POINT('Ctrl Pts',(2.36093683952928,-6.5393105326355,-39.4182556066633));
#271440=CARTESIAN_POINT('Ctrl Pts',(2.35340786587133,-6.587274703367,-39.504785261205));
#271441=CARTESIAN_POINT('',(-9.17446844834572,-6.58727470336698,-39.5047852612049));
#271442=CARTESIAN_POINT('',(2.4103097087628,-6.58727470336698,-39.5047852612049));
#271443=CARTESIAN_POINT('',(-9.2313702912372,-5.64044110768384,-38.2417314942451));
#271444=CARTESIAN_POINT('Ctrl Pts',(-9.17446844834573,-6.58727470336698,
-39.5047852612049));
#271445=CARTESIAN_POINT('Ctrl Pts',(-9.21458398225973,-6.33171419737343,
-39.0437419040312));
#271446=CARTESIAN_POINT('Ctrl Pts',(-9.2313702912372,-6.01361822422805,
-38.6186624579893));
#271447=CARTESIAN_POINT('Ctrl Pts',(-9.2313702912372,-5.64044110768386,
-38.2417314942451));
#271448=CARTESIAN_POINT('',(-9.2313702912372,3.32088519137438,-39.1836048418737));
#271449=CARTESIAN_POINT('Origin',(-9.2313702912372,-1.5372485021747,-42.3040604945994));
#271450=CARTESIAN_POINT('',(-9.17446844834575,3.98442455700367,-40.6159156274248));
#271451=CARTESIAN_POINT('Ctrl Pts',(-9.2313702912372,3.32088519137438,-39.1836048418737));
#271452=CARTESIAN_POINT('Ctrl Pts',(-9.2313702912372,3.39081690497477,-39.2924792025117));
#271453=CARTESIAN_POINT('Ctrl Pts',(-9.2303894871794,3.45716124687923,-39.4038171545982));
#271454=CARTESIAN_POINT('Ctrl Pts',(-9.22181693596821,3.71302027135661,
-39.8681399370981));
#271455=CARTESIAN_POINT('Ctrl Pts',(-9.20467998252579,3.86835507312333,
-40.2362694521487));
#271456=CARTESIAN_POINT('Ctrl Pts',(-9.17446844834573,3.98442455700367,
-40.6159156274248));
#271457=CARTESIAN_POINT('',(2.35340786587072,3.98442455700367,-40.6159156274248));
#271458=CARTESIAN_POINT('',(2.4103097087628,3.98442455700367,-40.6159156274248));
#271459=CARTESIAN_POINT('Ctrl Pts',(2.35340786587133,3.98442455700368,-40.6159156274248));
#271460=CARTESIAN_POINT('Ctrl Pts',(2.36852800519451,3.92633459848055,-40.4259119344818));
#271461=CARTESIAN_POINT('Ctrl Pts',(2.38043097016002,3.85826432336187,-40.2383290143428));
#271462=CARTESIAN_POINT('Ctrl Pts',(2.40398237976074,3.65183317380175,-39.7504974146935));
#271463=CARTESIAN_POINT('Ctrl Pts',(2.41030970876281,3.49804949695401,-39.4594260609572));
#271464=CARTESIAN_POINT('Ctrl Pts',(2.41030970876281,3.32088519137438,-39.1836048418737));
#271465=CARTESIAN_POINT('Origin',(2.4103097087628,43.803897557122,-9.69038745895935));
#271466=CARTESIAN_POINT('',(2.35340786587183,43.3968281352696,13.6306041000145));
#271467=CARTESIAN_POINT('',(0.0328697087628034,51.5689486443194,12.3036647920732));
#271468=CARTESIAN_POINT('Ctrl Pts',(2.35340786587133,43.3968281352696,13.6306041000145));
#271469=CARTESIAN_POINT('Ctrl Pts',(2.2321228552984,44.9903239005217,13.6584186720598));
#271470=CARTESIAN_POINT('Ctrl Pts',(1.92300889597276,46.5496262384867,13.521429232696));
#271471=CARTESIAN_POINT('Ctrl Pts',(1.08076370197647,49.2810926945741,13.0171155381819));
#271472=CARTESIAN_POINT('Ctrl Pts',(0.597453535611357,50.4610941799812,
12.6947953765867));
#271473=CARTESIAN_POINT('Ctrl Pts',(0.0328697087627933,51.5689486443194,
12.3036647920732));
#271474=CARTESIAN_POINT('',(-6.85393029123721,51.5689486443194,12.3036647920732));
#271475=CARTESIAN_POINT('',(-3.4105302912372,51.5689486443194,12.3036647920732));
#271476=CARTESIAN_POINT('',(-9.17446844834572,43.3968281352696,13.6306041000145));
#271477=CARTESIAN_POINT('Ctrl Pts',(-6.85393029123722,51.5689486443194,
12.3036647920732));
#271478=CARTESIAN_POINT('Ctrl Pts',(-6.8563396203465,51.5642209389144,12.3053339194162));
#271479=CARTESIAN_POINT('Ctrl Pts',(-6.85874734752439,51.5594921371695,
12.3070017194619));
#271480=CARTESIAN_POINT('Ctrl Pts',(-7.80791098577456,49.6936509024402,
12.9643882528227));
#271481=CARTESIAN_POINT('Ctrl Pts',(-8.50294745885817,47.6747662765604,
13.4063579884377));
#271482=CARTESIAN_POINT('Ctrl Pts',(-9.02375021840253,44.8533437535089,
13.6219650014366));
#271483=CARTESIAN_POINT('Ctrl Pts',(-9.1191230931546,44.1239797322133,13.6432965783518));
#271484=CARTESIAN_POINT('Ctrl Pts',(-9.17446844834574,43.3968281352695,
13.6306041000145));
#271485=CARTESIAN_POINT('',(2.4103097087628,43.3968281352696,13.6306041000145));
#271486=CARTESIAN_POINT('Origin',(15.9689897087628,3.06591104035337,1.49207703394933));
#271487=CARTESIAN_POINT('',(2.4103097087628,17.555631534552,5.81207703394933));
#271488=CARTESIAN_POINT('',(2.4103097087628,17.555631534552,-2.82792296605067));
#271489=CARTESIAN_POINT('Origin',(2.4103097087628,3.06591104035337,1.49207703394933));
#271490=CARTESIAN_POINT('',(-22.7900502912372,17.555631534552,-2.82792296605067));
#271491=CARTESIAN_POINT('',(15.9689897087628,17.555631534552,-2.82792296605067));
#271492=CARTESIAN_POINT('',(-22.7900502912372,17.555631534552,5.81207703394933));
#271493=CARTESIAN_POINT('Origin',(-22.7900502912372,3.06591104035337,1.49207703394933));
#271494=CARTESIAN_POINT('',(15.9689897087628,17.555631534552,5.81207703394933));
#271495=CARTESIAN_POINT('Origin',(2.4103097087628,3.06591104035337,1.49207703394933));
#271496=CARTESIAN_POINT('',(2.4103097087628,-5.64044110768439,41.2258855621436));
#271497=CARTESIAN_POINT('',(2.4103097087628,3.32088519137383,42.1677589097724));
#271498=CARTESIAN_POINT('Origin',(2.4103097087628,-1.53724850217529,45.2882145624979));
#271499=CARTESIAN_POINT('',(2.4103097087628,-13.2454487831571,38.7548687783801));
#271500=CARTESIAN_POINT('Origin',(2.4103097087628,3.06591104035337,1.49207703394933));
#271501=CARTESIAN_POINT('',(2.4103097087628,-21.0489333144978,34.2495248835934));
#271502=CARTESIAN_POINT('Origin',(2.4103097087628,-18.9527784085759,39.6295658755751));
#271503=CARTESIAN_POINT('',(2.4103097087628,-26.9914004601511,28.8989034325401));
#271504=CARTESIAN_POINT('Origin',(2.4103097087628,3.06591104035337,1.49207703394933));
#271505=CARTESIAN_POINT('',(2.4103097087628,-32.2877498558741,21.6091038797685));
#271506=CARTESIAN_POINT('Origin',(2.4103097087628,-32.5610768757426,27.3765988997259));
#271507=CARTESIAN_POINT('',(2.4103097087628,-35.5401699166052,14.3040488191824));
#271508=CARTESIAN_POINT('Origin',(2.4103097087628,3.06591104035337,1.49207703394933));
#271509=CARTESIAN_POINT('',(2.4103097087628,-37.4135972503663,5.49026617684987));
#271510=CARTESIAN_POINT('Origin',(2.4103097087628,-40.0091454711921,10.647962939785));
#271511=CARTESIAN_POINT('',(2.4103097087628,-37.4135972503662,-2.50611210895176));
#271512=CARTESIAN_POINT('Origin',(2.4103097087628,3.06591104035337,1.49207703394933));
#271513=CARTESIAN_POINT('',(2.4103097087628,-35.540169916605,-11.3198947512843));
#271514=CARTESIAN_POINT('Origin',(2.4103097087628,-40.009145471192,-7.66380887188698));
#271515=CARTESIAN_POINT('Origin',(2.4103097087628,3.06591104035337,1.49207703394933));
#271516=CARTESIAN_POINT('Origin',(2.4103097087628,3.06591104035337,1.49207703394933));
#271517=CARTESIAN_POINT('Origin',(2.4103097087628,3.06591104035337,1.49207703394933));
#271518=CARTESIAN_POINT('Origin',(2.4103097087628,3.06591104035337,1.49207703394933));
#271519=CARTESIAN_POINT('Origin',(2.4103097087628,3.06591104035337,1.49207703394933));
#271520=CARTESIAN_POINT('Origin',(2.4103097087628,3.06591104035337,1.49207703394933));
#271521=CARTESIAN_POINT('',(2.4103097087628,43.4921152187147,-3.01326686083735));
#271522=CARTESIAN_POINT('Origin',(2.4103097087628,3.06591104035337,1.49207703394933));
#271523=CARTESIAN_POINT('',(2.4103097087628,43.4921152187147,5.997420928736));
#271524=CARTESIAN_POINT('Origin',(2.4103097087628,47.1032899382114,1.49207703394933));
#271525=CARTESIAN_POINT('',(2.4103097087628,41.8295746888953,13.8190591635527));
#271526=CARTESIAN_POINT('Origin',(2.4103097087628,3.06591104035337,1.49207703394933));
#271527=CARTESIAN_POINT('',(2.4103097087628,38.1645977855601,22.0507320639531));
#271528=CARTESIAN_POINT('Origin',(2.4103097087628,43.2960584989777,19.4036926967212));
#271529=CARTESIAN_POINT('',(2.4103097087628,33.4644445574141,28.5199379906174));
#271530=CARTESIAN_POINT('Origin',(2.4103097087628,3.06591104035337,1.49207703394933));
#271531=CARTESIAN_POINT('',(2.4103097087628,26.7681985526003,34.549264974965));
#271532=CARTESIAN_POINT('Origin',(2.4103097087628,32.5326690847319,34.21822728948));
#271533=CARTESIAN_POINT('',(2.4103097087628,19.8431318188259,38.5474541178658));
#271534=CARTESIAN_POINT('Origin',(2.4103097087628,3.06591104035337,1.49207703394933));
#271535=CARTESIAN_POINT('',(2.4103097087628,11.273458480251,41.3319097758507));
#271536=CARTESIAN_POINT('Origin',(2.4103097087628,16.6742095075201,43.374113195316));
#271537=CARTESIAN_POINT('Origin',(2.4103097087628,3.06591104035337,1.49207703394933));
#271538=CARTESIAN_POINT('',(2.4103097087628,20.5619110403534,-2.82792296605067));
#271539=CARTESIAN_POINT('',(2.4103097087628,3.06591104035337,-2.82792296605067));
#271540=CARTESIAN_POINT('',(2.4103097087628,20.5619110403534,5.81207703394933));
#271541=CARTESIAN_POINT('',(2.4103097087628,3.06591104035337,5.81207703394933));
#271542=CARTESIAN_POINT('',(2.4103097087628,20.5619110403534,1.49207703394933));
#271543=CARTESIAN_POINT('Origin',(-22.7900502912372,3.06591104035337,1.49207703394933));
#271544=CARTESIAN_POINT('',(-22.7900502912372,20.5619110403534,-2.82792296605067));
#271545=CARTESIAN_POINT('',(-22.7900502912372,3.06591104035337,-2.82792296605067));
#271546=CARTESIAN_POINT('',(-22.7900502912372,20.5619110403534,5.81207703394933));
#271547=CARTESIAN_POINT('',(-22.7900502912372,20.5619110403534,1.49207703394933));
#271548=CARTESIAN_POINT('',(-22.7900502912372,3.06591104035337,5.81207703394933));
#271549=CARTESIAN_POINT('Origin',(-15.8776902912372,3.06591104035337,1.49207703394933));
#271550=CARTESIAN_POINT('',(0.0328697087628034,-11.8224981078497,48.9027336387577));
#271551=CARTESIAN_POINT('',(2.35340786587133,-6.58727470336753,42.4889393291034));
#271552=CARTESIAN_POINT('Ctrl Pts',(0.0328697087628055,-11.8224981078497,
48.9027336387577));
#271553=CARTESIAN_POINT('Ctrl Pts',(0.035279037872096,-11.8186887484661,
48.8994738894469));
#271554=CARTESIAN_POINT('Ctrl Pts',(0.0376867650499826,-11.8148799903856,
48.8962125270292));
#271555=CARTESIAN_POINT('Ctrl Pts',(0.986850403300172,-10.3126459350247,
47.6090398850055));
#271556=CARTESIAN_POINT('Ctrl Pts',(1.68188687638377,-8.92044660333834,
46.0816193794912));
#271557=CARTESIAN_POINT('Ctrl Pts',(2.20268963592813,-7.32301419132144,
43.7459993062186));
#271558=CARTESIAN_POINT('Ctrl Pts',(2.29806251068019,-6.93985849316234,
43.1250173236278));
#271559=CARTESIAN_POINT('Ctrl Pts',(2.35340786587134,-6.58727470336753,
42.4889393291034));
#271560=CARTESIAN_POINT('',(0.0328697087628034,-12.7563976933524,48.5992912691242));
#271561=CARTESIAN_POINT('Origin',(0.0328697087628034,3.06591104035337,1.49207703394933));
#271562=CARTESIAN_POINT('',(2.35340786587083,-13.2218486904757,40.3332355645775));
#271563=CARTESIAN_POINT('Ctrl Pts',(2.35340786587133,-13.2218486904757,
40.3332355645775));
#271564=CARTESIAN_POINT('Ctrl Pts',(2.2321228552984,-13.4160765549504,41.9150945788249));
#271565=CARTESIAN_POINT('Ctrl Pts',(1.92300889597277,-13.4428290352261,
43.4801741910106));
#271566=CARTESIAN_POINT('Ctrl Pts',(1.08076370197648,-13.2267940150197,
46.2493925235459));
#271567=CARTESIAN_POINT('Ctrl Pts',(0.597453535611382,-13.0295832989177,
47.456621468522));
#271568=CARTESIAN_POINT('Ctrl Pts',(0.0328697087628101,-12.7563976933524,
48.5992912691242));
#271569=CARTESIAN_POINT('Ctrl Pts',(2.41030970876281,-13.2454487831571,
38.7548687783801));
#271570=CARTESIAN_POINT('Ctrl Pts',(2.41030970876281,-13.1805461911692,
39.1783530762096));
#271571=CARTESIAN_POINT('Ctrl Pts',(2.3994466364291,-13.1628664707968,39.6083769762526));
#271572=CARTESIAN_POINT('Ctrl Pts',(2.36767303424712,-13.2002343324775,
40.1363378140511));
#271573=CARTESIAN_POINT('Ctrl Pts',(2.36093683952928,-13.2097916648931,
40.2350389713415));
#271574=CARTESIAN_POINT('Ctrl Pts',(2.35340786587133,-13.2218486904757,
40.3332355645775));
#271575=CARTESIAN_POINT('Ctrl Pts',(2.35340786587133,-6.58727470336753,
42.4889393291034));
#271576=CARTESIAN_POINT('Ctrl Pts',(2.36852800519451,-6.49095016075001,
42.3151652542167));
#271577=CARTESIAN_POINT('Ctrl Pts',(2.38043097016002,-6.38536670236675,
42.1458340769385));
#271578=CARTESIAN_POINT('Ctrl Pts',(2.40398237976074,-6.0820206759904,41.7115822175219));
#271579=CARTESIAN_POINT('Ctrl Pts',(2.41030970876281,-5.87108040414584,
41.458844895496));
#271580=CARTESIAN_POINT('Ctrl Pts',(2.41030970876281,-5.6404411076844,41.2258855621436));
#271581=CARTESIAN_POINT('Origin',(-15.8776902912372,3.06591104035337,1.49207703394933));
#271582=CARTESIAN_POINT('',(2.35340786587079,3.9844245570031,43.6000696953234));
#271583=CARTESIAN_POINT('Ctrl Pts',(2.41030970876281,3.32088519137384,42.1677589097724));
#271584=CARTESIAN_POINT('Ctrl Pts',(2.41030970876281,3.5524232411681,42.5282328040454));
#271585=CARTESIAN_POINT('Ctrl Pts',(2.3994466364291,3.7434809469525,42.9138881944926));
#271586=CARTESIAN_POINT('Ctrl Pts',(2.36767303424712,3.92408472549392,43.4114032982955));
#271587=CARTESIAN_POINT('Ctrl Pts',(2.36093683952928,3.95549904526253,43.5054586095058));
#271588=CARTESIAN_POINT('Ctrl Pts',(2.35340786587133,3.98442455700311,43.6000696953235));
#271589=CARTESIAN_POINT('',(2.35340786587077,10.9222131989687,42.8708787256748));
#271590=CARTESIAN_POINT('Ctrl Pts',(2.35340786587133,10.9222131989687,42.8708787256748));
#271591=CARTESIAN_POINT('Ctrl Pts',(2.36852800519451,10.9395297634634,42.6729494877959));
#271592=CARTESIAN_POINT('Ctrl Pts',(2.38043097016002,10.9671118576574,42.4753130985289));
#271593=CARTESIAN_POINT('Ctrl Pts',(2.40398237976075,11.0676060985989,41.9552223404273));
#271594=CARTESIAN_POINT('Ctrl Pts',(2.41030970876281,11.1575120958356,41.6385381698543));
#271595=CARTESIAN_POINT('Ctrl Pts',(2.41030970876281,11.273458480251,41.3319097758507));
#271596=CARTESIAN_POINT('',(0.0328697087628034,8.74832380494721,50.8595285768044));
#271597=CARTESIAN_POINT('Ctrl Pts',(0.0328697087628022,8.74832380494719,
50.8595285768044));
#271598=CARTESIAN_POINT('Ctrl Pts',(0.0352790378721036,8.75047796841673,
50.8550012415804));
#271599=CARTESIAN_POINT('Ctrl Pts',(0.0376867650500019,8.75263092645877,
50.850472677282));
#271600=CARTESIAN_POINT('Ctrl Pts',(0.986850403300229,9.60144974457407,
49.0635683201677));
#271601=CARTESIAN_POINT('Ctrl Pts',(1.68188687638381,10.2520292311912,47.1019417727825));
#271602=CARTESIAN_POINT('Ctrl Pts',(2.20268963592814,10.7613740869769,44.3185123672612));
#271603=CARTESIAN_POINT('Ctrl Pts',(2.2980625106802,10.8588281075905,43.595373635343));
#271604=CARTESIAN_POINT('Ctrl Pts',(2.35340786587133,10.9222131989687,42.8708787256748));
#271605=CARTESIAN_POINT('',(0.0328697087628034,7.77174294992524,50.9621713607466));
#271606=CARTESIAN_POINT('Origin',(0.0328697087628034,3.06591104035337,1.49207703394933));
#271607=CARTESIAN_POINT('Ctrl Pts',(2.35340786587133,3.98442455700312,43.6000696953235));
#271608=CARTESIAN_POINT('Ctrl Pts',(2.2321228552984,4.45038859893883,45.1241694020084));
#271609=CARTESIAN_POINT('Ctrl Pts',(1.92300889597277,5.06252421970915,46.564821986591));
#271610=CARTESIAN_POINT('Ctrl Pts',(1.08076370197648,6.38622459962975,49.0067594565937));
#271611=CARTESIAN_POINT('Ctrl Pts',(0.597453535611385,7.05740980202667,
50.0294051509654));
#271612=CARTESIAN_POINT('Ctrl Pts',(0.0328697087627989,7.77174294992525,
50.9621713607466));
#271613=CARTESIAN_POINT('Origin',(-15.8776902912372,3.06591104035337,1.49207703394933));
#271614=CARTESIAN_POINT('',(2.35340786587221,21.0318784730198,39.5860493558137));
#271615=CARTESIAN_POINT('Ctrl Pts',(2.41030970876281,19.8431318188259,38.5474541178658));
#271616=CARTESIAN_POINT('Ctrl Pts',(2.41030970876281,20.20127029416,38.78258839746));
#271617=CARTESIAN_POINT('Ctrl Pts',(2.3994466364291,20.5326703723215,39.0571919577339));
#271618=CARTESIAN_POINT('Ctrl Pts',(2.36767303424712,20.9000177570413,39.4382364463109));
#271619=CARTESIAN_POINT('Ctrl Pts',(2.36093683952928,20.966971907716,39.511382893667));
#271620=CARTESIAN_POINT('Ctrl Pts',(2.35340786587134,21.0318784730198,39.5860493558137));
#271621=CARTESIAN_POINT('',(2.35340786587071,27.0732750858158,36.0980473951347));
#271622=CARTESIAN_POINT('Ctrl Pts',(2.35340786587133,27.0732750858159,36.0980473951347));
#271623=CARTESIAN_POINT('Ctrl Pts',(2.36852800519451,27.0085894808706,35.9101867576236));
#271624=CARTESIAN_POINT('Ctrl Pts',(2.38043097016003,26.9534010162137,35.7184182835424));
#271625=CARTESIAN_POINT('Ctrl Pts',(2.40398237976075,26.8336671045001,35.2024170437078));
#271626=CARTESIAN_POINT('Ctrl Pts',(2.41030970876281,26.7869932634364,34.876543594665));
#271627=CARTESIAN_POINT('Ctrl Pts',(2.41030970876281,26.7681985526003,34.549264974965));
#271628=CARTESIAN_POINT('',(0.0328697087628034,28.3366049276465,44.2802426538737));
#271629=CARTESIAN_POINT('Ctrl Pts',(0.0328697087628083,28.3366049276465,
44.2802426538738));
#271630=CARTESIAN_POINT('Ctrl Pts',(0.0352790378720938,28.3367314207681,
44.2752305501264));
#271631=CARTESIAN_POINT('Ctrl Pts',(0.0376867650499842,28.3368563127672,
44.2702178138554));
#271632=CARTESIAN_POINT('Ctrl Pts',(0.986850403300163,28.3854914087078,
42.2925537385122));
#271633=CARTESIAN_POINT('Ctrl Pts',(1.68188687638376,28.1819599466905,40.2359042001166));
#271634=CARTESIAN_POINT('Ctrl Pts',(2.20268963592813,27.515146893427,37.4859456932235));
#271635=CARTESIAN_POINT('Ctrl Pts',(2.29806251068019,27.310048550989,36.7856874682356));
#271636=CARTESIAN_POINT('Ctrl Pts',(2.35340786587133,27.0732750858159,36.0980473951347));
#271637=CARTESIAN_POINT('',(0.0328697087628034,27.4862025048971,44.7712227215677));
#271638=CARTESIAN_POINT('Origin',(0.0328697087628034,3.06591104035337,1.49207703394933));
#271639=CARTESIAN_POINT('Ctrl Pts',(2.35340786587134,21.0318784730198,39.5860493558137));
#271640=CARTESIAN_POINT('Ctrl Pts',(2.23212285529842,22.0774650053648,40.7888590696392));
#271641=CARTESIAN_POINT('Ctrl Pts',(1.9230088959728,23.2226449172723,41.8559827068265));
#271642=CARTESIAN_POINT('Ctrl Pts',(1.08076370197648,25.4251308357786,43.5484061414277));
#271643=CARTESIAN_POINT('Ctrl Pts',(0.597453535611381,26.4542365054499,
44.2096438541936));
#271644=CARTESIAN_POINT('Ctrl Pts',(0.0328697087628023,27.4862025048971,
44.7712227215677));
#271645=CARTESIAN_POINT('Origin',(-15.8776902912372,3.06591104035337,1.49207703394933));
#271646=CARTESIAN_POINT('',(2.35340786587194,34.9728534042383,28.9852351289796));
#271647=CARTESIAN_POINT('Ctrl Pts',(2.41030970876281,33.4644445574141,28.5199379906174));
#271648=CARTESIAN_POINT('Ctrl Pts',(2.41030970876281,33.8872580623168,28.5890758024631));
#271649=CARTESIAN_POINT('Ctrl Pts',(2.3994466364291,34.3016984286661,28.7051460822974));
#271650=CARTESIAN_POINT('Ctrl Pts',(2.36767303424712,34.7922717195002,28.903833901893));
#271651=CARTESIAN_POINT('Ctrl Pts',(2.36093683952928,34.8831887201699,28.9434238001324));
#271652=CARTESIAN_POINT('Ctrl Pts',(2.35340786587134,34.9728534042383,28.9852351289796));
#271653=CARTESIAN_POINT('',(2.35340786587133,39.0732456291471,23.3415294037746));
#271654=CARTESIAN_POINT('Ctrl Pts',(2.35340786587134,39.0732456291471,23.3415294037746));
#271655=CARTESIAN_POINT('Ctrl Pts',(2.36852800519451,38.9377425835071,23.1962201775173));
#271656=CARTESIAN_POINT('Ctrl Pts',(2.38043097016002,38.80932614691,23.0434781299524));
#271657=CARTESIAN_POINT('Ctrl Pts',(2.40398237976074,38.490067163625,22.6207877104763));
#271658=CARTESIAN_POINT('Ctrl Pts',(2.41030970876281,38.3148838153993,22.3420714627706));
#271659=CARTESIAN_POINT('Ctrl Pts',(2.41030970876281,38.1645977855601,22.0507320639531));
#271660=CARTESIAN_POINT('',(0.0328697087628034,43.5553535001861,30.3024941769768));
#271661=CARTESIAN_POINT('Ctrl Pts',(0.0328697087628094,43.5553535001861,
30.3024941769768));
#271662=CARTESIAN_POINT('Ctrl Pts',(0.0352790378720948,43.5534304511498,
30.2978639429776));
#271663=CARTESIAN_POINT('Ctrl Pts',(0.0376867650499853,43.5515056821448,
30.2932337823743));
#271664=CARTESIAN_POINT('Ctrl Pts',(0.986850403300188,42.7915476059866,
28.466766073943));
#271665=CARTESIAN_POINT('Ctrl Pts',(1.68188687638378,41.7690976341429,26.6707069338002));
#271666=CARTESIAN_POINT('Ctrl Pts',(2.20268963592813,40.0414247065458,24.429712133966));
#271667=CARTESIAN_POINT('Ctrl Pts',(2.29806251068019,39.5692373677238,23.873415424655));
#271668=CARTESIAN_POINT('Ctrl Pts',(2.35340786587133,39.0732456291471,23.3415294037746));
#271669=CARTESIAN_POINT('',(0.0328697087628034,42.9781718142661,31.0969166143042));
#271670=CARTESIAN_POINT('Origin',(0.0328697087628034,3.06591104035337,1.49207703394933));
#271671=CARTESIAN_POINT('Ctrl Pts',(2.35340786587134,34.9728534042383,28.9852351289796));
#271672=CARTESIAN_POINT('Ctrl Pts',(2.23212285529841,36.4172710166947,29.658778123242));
#271673=CARTESIAN_POINT('Ctrl Pts',(1.92300889597277,37.8974832093378,30.1678574416503));
#271674=CARTESIAN_POINT('Ctrl Pts',(1.08076370197648,40.5979248421634,30.8181314538232));
#271675=CARTESIAN_POINT('Ctrl Pts',(0.597453535611371,41.8070092596915,
31.0036271772901));
#271676=CARTESIAN_POINT('Ctrl Pts',(0.0328697087628057,42.9781718142661,
31.0969166143042));
#271677=CARTESIAN_POINT('Origin',(-15.8776902912372,3.06591104035337,1.49207703394933));
#271678=CARTESIAN_POINT('',(0.0328697087628034,-42.5287624981535,21.2546889964492));
#271679=CARTESIAN_POINT('Origin',(0.0328697087628034,3.06591104035337,1.49207703394933));
#271680=CARTESIAN_POINT('',(2.35340786587208,-36.6973334821472,15.3777206306443));
#271681=CARTESIAN_POINT('Ctrl Pts',(2.35340786587134,-36.6973334821471,
15.3777206306443));
#271682=CARTESIAN_POINT('Ctrl Pts',(2.23212285529842,-38.0028476319476,
16.291851479574));
#271683=CARTESIAN_POINT('Ctrl Pts',(1.9230088959728,-39.183829350552,17.3192131821901));
#271684=CARTESIAN_POINT('Ctrl Pts',(1.08076370197649,-41.0972039809274,
19.3327272315678));
#271685=CARTESIAN_POINT('Ctrl Pts',(0.597453535611395,-41.8623901985072,
20.2870771907335));
#271686=CARTESIAN_POINT('Ctrl Pts',(0.0328697087628098,-42.5287624981535,
21.2546889964492));
#271687=CARTESIAN_POINT('Ctrl Pts',(2.41030970876281,-35.5401699166052,
14.3040488191824));
#271688=CARTESIAN_POINT('Ctrl Pts',(2.41030970876281,-35.811451770477,14.6356471495685));
#271689=CARTESIAN_POINT('Ctrl Pts',(2.3994466364291,-36.1191917646125,14.9365278952636));
#271690=CARTESIAN_POINT('Ctrl Pts',(2.36767303424712,-36.5365471092219,
15.2620329177462));
#271691=CARTESIAN_POINT('Ctrl Pts',(2.36093683952928,-36.6162914671653,
15.3209744008423));
#271692=CARTESIAN_POINT('Ctrl Pts',(2.35340786587134,-36.6973334821471,
15.3777206306443));
#271693=CARTESIAN_POINT('Ctrl Pts',(2.35340786587133,-33.8599370650904,
21.750617325498));
#271694=CARTESIAN_POINT('Ctrl Pts',(2.36852800519451,-33.6663440609273,
21.7059228588123));
#271695=CARTESIAN_POINT('Ctrl Pts',(2.38043097016003,-33.4698573492114,
21.6710819862382));
#271696=CARTESIAN_POINT('Ctrl Pts',(2.40398237976075,-32.9441672163663,
21.605940806065));
#271697=CARTESIAN_POINT('Ctrl Pts',(2.41030970876281,-32.6152001912929,
21.5935857000344));
#271698=CARTESIAN_POINT('Ctrl Pts',(2.41030970876281,-32.2877498558741,
21.6091038797685));
#271699=CARTESIAN_POINT('Origin',(-15.8776902912372,3.06591104035337,1.49207703394933));
#271700=CARTESIAN_POINT('',(2.35340786587201,-27.6118203108423,30.3504122630382));
#271701=CARTESIAN_POINT('Ctrl Pts',(2.41030970876281,-26.9914004601511,
28.8989034325401));
#271702=CARTESIAN_POINT('Ctrl Pts',(2.41030970876281,-27.1043555737458,
29.3121738515974));
#271703=CARTESIAN_POINT('Ctrl Pts',(2.3994466364291,-27.263110823053,29.7122112222741));
#271704=CARTESIAN_POINT('Ctrl Pts',(2.36767303424712,-27.5119890821949,
30.1793285688391));
#271705=CARTESIAN_POINT('Ctrl Pts',(2.36093683952928,-27.5608655171943,
30.2656092454424));
#271706=CARTESIAN_POINT('Ctrl Pts',(2.35340786587134,-27.6118203108423,
30.3504122630381));
#271707=CARTESIAN_POINT('',(2.35340786587221,-22.427639094175,35.0182699968983));
#271708=CARTESIAN_POINT('Ctrl Pts',(2.35340786587134,-22.427639094175,35.0182699968983));
#271709=CARTESIAN_POINT('Ctrl Pts',(2.36852800519451,-22.2689619619342,
34.8986982012396));
#271710=CARTESIAN_POINT('Ctrl Pts',(2.38043097016002,-22.1036334785118,
34.7869511348269));
#271711=CARTESIAN_POINT('Ctrl Pts',(2.40398237976074,-21.6498869504732,
34.5136242656428));
#271712=CARTESIAN_POINT('Ctrl Pts',(2.41030970876281,-21.354385893355,34.3685343711888));
#271713=CARTESIAN_POINT('Ctrl Pts',(2.41030970876281,-21.0489333144978,
34.2495248835934));
#271714=CARTESIAN_POINT('',(0.0328697087628034,-29.8189788219714,38.748205461446));
#271715=CARTESIAN_POINT('Ctrl Pts',(0.0328697087628022,-29.8189788219714,
38.748205461446));
#271716=CARTESIAN_POINT('Ctrl Pts',(0.0352790378720899,-29.814172939518,
38.746776938318));
#271717=CARTESIAN_POINT('Ctrl Pts',(0.0376867650499825,-29.8093669502727,
38.7453466969716));
#271718=CARTESIAN_POINT('Ctrl Pts',(0.986850403300177,-27.913467573206,
38.1804696134406));
#271719=CARTESIAN_POINT('Ctrl Pts',(1.68188687638377,-26.0203723086328,
37.3513600313804));
#271720=CARTESIAN_POINT('Ctrl Pts',(2.20268963592813,-23.6110629166404,
35.8673992194675));
#271721=CARTESIAN_POINT('Ctrl Pts',(2.2980625106802,-23.0084566420077,35.4559474124384));
#271722=CARTESIAN_POINT('Ctrl Pts',(2.35340786587134,-22.427639094175,35.0182699968983));
#271723=CARTESIAN_POINT('',(0.0328697087628034,-30.54871741541,38.0911458806337));
#271724=CARTESIAN_POINT('Origin',(0.0328697087628034,3.06591104035337,1.49207703394933));
#271725=CARTESIAN_POINT('Ctrl Pts',(2.35340786587134,-27.6118203108423,
30.3504122630381));
#271726=CARTESIAN_POINT('Ctrl Pts',(2.23212285529841,-28.4326563194549,
31.7165127905467));
#271727=CARTESIAN_POINT('Ctrl Pts',(1.92300889597278,-29.0936711538983,
33.1354029470867));
#271728=CARTESIAN_POINT('Ctrl Pts',(1.08076370197647,-30.0226559110164,
35.7530791349006));
#271729=CARTESIAN_POINT('Ctrl Pts',(0.59745353561138,-30.3335192056265,
36.936150478564));
#271730=CARTESIAN_POINT('Ctrl Pts',(0.0328697087628135,-30.5487174154099,
38.0911458806337));
#271731=CARTESIAN_POINT('Origin',(-15.8776902912372,3.06591104035337,1.49207703394933));
#271732=CARTESIAN_POINT('',(0.0328697087628034,-46.6250743114837,1.9830571016429));
#271733=CARTESIAN_POINT('',(2.35340786587075,-38.9074204377757,4.98007899462811));
#271734=CARTESIAN_POINT('Ctrl Pts',(0.0328697087628096,-46.6250743114837,
1.98305710164289));
#271735=CARTESIAN_POINT('Ctrl Pts',(0.0352790378720954,-46.6207969488729,
1.9856726997732));
#271736=CARTESIAN_POINT('Ctrl Pts',(0.0376867650499864,-46.6165182379192,
1.98828722755271));
#271737=CARTESIAN_POINT('Ctrl Pts',(0.98685040330017,-44.9281284564905,
3.01923849382438));
#271738=CARTESIAN_POINT('Ctrl Pts',(1.68188687638377,-43.0452519785497,
3.8712998464458));
#271739=CARTESIAN_POINT('Ctrl Pts',(2.20268963592813,-40.3303115255954,
4.66880205619103));
#271740=CARTESIAN_POINT('Ctrl Pts',(2.29806251068019,-39.6213209423279,
4.84131079385968));
#271741=CARTESIAN_POINT('Ctrl Pts',(2.35340786587133,-38.9074204377758,
4.9800789946281));
#271742=CARTESIAN_POINT('',(0.0328697087628034,-46.6250743114837,1.00109696625507));
#271743=CARTESIAN_POINT('Origin',(0.0328697087628034,3.06591104035337,1.49207703394933));
#271744=CARTESIAN_POINT('',(2.35340786587081,-38.9074204377757,-1.99592492673002));
#271745=CARTESIAN_POINT('Ctrl Pts',(2.35340786587133,-38.9074204377758,
-1.99592492673002));
#271746=CARTESIAN_POINT('Ctrl Pts',(2.23212285529841,-40.4718774720397,
-1.69182528477713));
#271747=CARTESIAN_POINT('Ctrl Pts',(1.92300889597281,-41.9686236067765,
-1.23363220775526));
#271748=CARTESIAN_POINT('Ctrl Pts',(1.08076370197649,-44.5355482543544,
-0.172435168151975));
#271749=CARTESIAN_POINT('Ctrl Pts',(0.597453535611403,-45.6227497463857,
0.388177628579008));
#271750=CARTESIAN_POINT('Ctrl Pts',(0.0328697087628152,-46.6250743114837,
1.00109696625508));
#271751=CARTESIAN_POINT('Ctrl Pts',(2.41030970876281,-37.4135972503662,
-2.50611210895176));
#271752=CARTESIAN_POINT('Ctrl Pts',(2.41030970876281,-37.7962987474624,
-2.31352223103693));
#271753=CARTESIAN_POINT('Ctrl Pts',(2.3994466364291,-38.19981244571,-2.16382312466987));
#271754=CARTESIAN_POINT('Ctrl Pts',(2.36767303424712,-38.7134803451498,
-2.03621320177717));
#271755=CARTESIAN_POINT('Ctrl Pts',(2.36093683952928,-38.810304102094,-2.01480243008215));
#271756=CARTESIAN_POINT('Ctrl Pts',(2.35340786587133,-38.9074204377758,
-1.99592492673001));
#271757=CARTESIAN_POINT('Ctrl Pts',(2.35340786587133,-38.9074204377758,
4.9800789946281));
#271758=CARTESIAN_POINT('Ctrl Pts',(2.36852800519451,-38.7123855508474,
5.01798993624188));
#271759=CARTESIAN_POINT('Ctrl Pts',(2.38043097016002,-38.5187149483196,
5.06607956089376));
#271760=CARTESIAN_POINT('Ctrl Pts',(2.40398237976074,-38.0119778103818,
5.2203875715726));
#271761=CARTESIAN_POINT('Ctrl Pts',(2.41030970876281,-37.70642620456,5.34290356404062));
#271762=CARTESIAN_POINT('Ctrl Pts',(2.41030970876281,-37.4135972503663,
5.49026617684987));
#271763=CARTESIAN_POINT('Origin',(-15.8776902912372,3.06591104035337,1.49207703394933));
#271764=CARTESIAN_POINT('',(0.0328697087628034,-30.5487174154094,-35.1069918127356));
#271765=CARTESIAN_POINT('Ctrl Pts',(0.0328697087628055,-30.5487174154095,
-35.1069918127356));
#271766=CARTESIAN_POINT('Ctrl Pts',(0.0352790378720928,-30.5477990693881,
-35.1020629360817));
#271767=CARTESIAN_POINT('Ctrl Pts',(0.0376867650499851,-30.5468790257237,
-35.0971337736183));
#271768=CARTESIAN_POINT('Ctrl Pts',(0.986850403300176,-30.1832718463553,
-33.1525745982338));
#271769=CARTESIAN_POINT('Ctrl Pts',(1.68188687638377,-29.5565865521619,
-31.1831843571046));
#271770=CARTESIAN_POINT('Ctrl Pts',(2.20268963592813,-28.3325964411273,
-28.631957270833));
#271771=CARTESIAN_POINT('Ctrl Pts',(2.2980625106802,-27.9863881179909,-27.989643711327));
#271772=CARTESIAN_POINT('Ctrl Pts',(2.35340786587134,-27.6118203108419,
-27.3662581951399));
#271773=CARTESIAN_POINT('',(0.0328697087628034,-29.8189788219709,-35.7640513935478));
#271774=CARTESIAN_POINT('Origin',(0.0328697087628034,3.06591104035337,1.49207703394933));
#271775=CARTESIAN_POINT('Ctrl Pts',(2.35340786587133,-22.4276390941746,
-32.0341159290001));
#271776=CARTESIAN_POINT('Ctrl Pts',(2.2321228552984,-23.7004552534809,-32.9932517008816));
#271777=CARTESIAN_POINT('Ctrl Pts',(1.92300889597279,-25.042477716441,-33.7989598345075));
#271778=CARTESIAN_POINT('Ctrl Pts',(1.08076370197648,-27.5487086511453,
-34.9964771851694));
#271779=CARTESIAN_POINT('Ctrl Pts',(0.597453535611387,-28.6928049437295,
-35.4293021676146));
#271780=CARTESIAN_POINT('Ctrl Pts',(0.0328697087628135,-29.8189788219709,
-35.7640513935478));
#271781=CARTESIAN_POINT('Origin',(-15.8776902912372,3.06591104035337,1.49207703394933));
#271782=CARTESIAN_POINT('',(2.35340786587133,-36.697333482147,-12.3935665627462));
#271783=CARTESIAN_POINT('Ctrl Pts',(2.35340786587133,-36.697333482147,-12.3935665627462));
#271784=CARTESIAN_POINT('Ctrl Pts',(2.36852800519451,-36.5345800162395,
-12.2796053590481));
#271785=CARTESIAN_POINT('Ctrl Pts',(2.38043097016002,-36.3772129295191,
-12.156900370153));
#271786=CARTESIAN_POINT('Ctrl Pts',(2.40398237976074,-35.9770482412004,
-11.8098244255128));
#271787=CARTESIAN_POINT('Ctrl Pts',(2.41030970876281,-35.7477447031261,
-11.5736214626667));
#271788=CARTESIAN_POINT('Ctrl Pts',(2.41030970876281,-35.540169916605,-11.3198947512843));
#271789=CARTESIAN_POINT('',(0.0328697087628034,-42.5287624981532,-18.2705349285512));
#271790=CARTESIAN_POINT('Ctrl Pts',(0.0328697087628071,-42.5287624981532,
-18.2705349285512));
#271791=CARTESIAN_POINT('Ctrl Pts',(0.0352790378720939,-42.5259187925725,
-18.2664057006507));
#271792=CARTESIAN_POINT('Ctrl Pts',(0.0376867650499849,-42.5230734198686,
-18.2622769021438));
#271793=CARTESIAN_POINT('Ctrl Pts',(0.986850403300142,-41.3999782615322,
-16.6337260638887));
#271794=CARTESIAN_POINT('Ctrl Pts',(1.68188687638376,-40.0264495820672,
-15.0894944276046));
#271795=CARTESIAN_POINT('Ctrl Pts',(2.20268963592813,-37.870601435138,-13.2566741404465));
#271796=CARTESIAN_POINT('Ctrl Pts',(2.29806251068019,-37.2930719331431,
-12.8107071169351));
#271797=CARTESIAN_POINT('Ctrl Pts',(2.35340786587133,-36.697333482147,-12.3935665627462));
#271798=CARTESIAN_POINT('',(0.0328697087628034,-42.1293633290513,-19.1676001498208));
#271799=CARTESIAN_POINT('Origin',(0.0328697087628034,3.06591104035337,1.49207703394933));
#271800=CARTESIAN_POINT('Ctrl Pts',(2.35340786587134,-33.8599370650901,
-18.7664632575998));
#271801=CARTESIAN_POINT('Ctrl Pts',(2.23212285529841,-35.4128281499475,
-19.1249764133759));
#271802=CARTESIAN_POINT('Ctrl Pts',(1.9230088959728,-36.9665376966088,-19.3151777075188));
#271803=CARTESIAN_POINT('Ctrl Pts',(1.08076370197649,-39.7431677700446,
-19.3897882865098));
#271804=CARTESIAN_POINT('Ctrl Pts',(0.597453535611398,-40.9643975216398,
-19.3198476977757));
#271805=CARTESIAN_POINT('Ctrl Pts',(0.0328697087628097,-42.1293633290513,
-19.1676001498208));
#271806=CARTESIAN_POINT('Origin',(-15.8776902912372,3.06591104035337,1.49207703394933));
#271807=CARTESIAN_POINT('',(0.0328697087628034,-12.7563976933517,-45.6151372012257));
#271808=CARTESIAN_POINT('Ctrl Pts',(0.0328697087628133,-12.7563976933517,
-45.6151372012257));
#271809=CARTESIAN_POINT('Ctrl Pts',(0.0352790378720981,-12.7575634972597,
-45.6102609233694));
#271810=CARTESIAN_POINT('Ctrl Pts',(0.0376867650499855,-12.7587278665428,
-45.6053836939195));
#271811=CARTESIAN_POINT('Ctrl Pts',(0.9868504033002,-13.2174796507227,-43.6810481285951));
#271812=CARTESIAN_POINT('Ctrl Pts',(1.68188687638379,-13.445997322424,-41.6270247466606));
#271813=CARTESIAN_POINT('Ctrl Pts',(2.20268963592814,-13.3655042570831,
-38.7985212016622));
#271814=CARTESIAN_POINT('Ctrl Pts',(2.2980625106802,-13.3104796770793,-38.070922955836));
#271815=CARTESIAN_POINT('Ctrl Pts',(2.35340786587134,-13.2218486904752,
-37.349081496679));
#271816=CARTESIAN_POINT('',(0.0328697087628034,-11.8224981078491,-45.9185795708593));
#271817=CARTESIAN_POINT('Origin',(0.0328697087628034,3.06591104035337,1.49207703394933));
#271818=CARTESIAN_POINT('Ctrl Pts',(2.35340786587133,-6.587274703367,-39.5047852612049));
#271819=CARTESIAN_POINT('Ctrl Pts',(2.2321228552984,-7.35993446000634,-40.8987003607588));
#271820=CARTESIAN_POINT('Ctrl Pts',(1.92300889597277,-8.25822196352803,
-42.180601077935));
#271821=CARTESIAN_POINT('Ctrl Pts',(1.08076370197648,-10.0607036624973,
-44.2939635712348));
#271822=CARTESIAN_POINT('Ctrl Pts',(0.597453535611391,-10.9298418532942,
-45.154714753303));
#271823=CARTESIAN_POINT('Ctrl Pts',(0.032869708762817,-11.8224981078491,
-45.9185795708593));
#271824=CARTESIAN_POINT('Origin',(-15.8776902912372,3.06591104035337,1.49207703394933));
#271825=CARTESIAN_POINT('',(0.0328697087628034,42.9781718142665,-28.112762546405));
#271826=CARTESIAN_POINT('Ctrl Pts',(0.0328697087628044,42.9781718142665,
-28.112762546405));
#271827=CARTESIAN_POINT('Ctrl Pts',(0.0352790378720942,42.9731739452163,
-28.1123644390816));
#271828=CARTESIAN_POINT('Ctrl Pts',(0.0376867650499829,42.9681756144703,
-28.1119646732901));
#271829=CARTESIAN_POINT('Ctrl Pts',(0.986850403300196,40.9962616380186,
-27.9536111544311));
#271830=CARTESIAN_POINT('Ctrl Pts',(1.68188687638377,38.9721534719365,-27.53621624333));
#271831=CARTESIAN_POINT('Ctrl Pts',(2.20268963592813,36.3069604692216,-26.5856071249667));
#271832=CARTESIAN_POINT('Ctrl Pts',(2.29806251068019,35.6319769466131,-26.3084354165599));
#271833=CARTESIAN_POINT('Ctrl Pts',(2.35340786587133,34.9728534042387,-26.0010810610805));
#271834=CARTESIAN_POINT('',(0.0328697087628034,43.5553535001865,-27.3183401090776));
#271835=CARTESIAN_POINT('Origin',(0.0328697087628034,3.06591104035337,1.49207703394933));
#271836=CARTESIAN_POINT('Ctrl Pts',(2.35340786587133,39.0732456291474,-20.3573753358755));
#271837=CARTESIAN_POINT('Ctrl Pts',(2.23212285529841,40.1601726720691,-21.5229618867843));
#271838=CARTESIAN_POINT('Ctrl Pts',(1.92300889597281,41.1017465979602,-22.773413177224));
#271839=CARTESIAN_POINT('Ctrl Pts',(1.0807637019765,42.5546762914754,-25.1407400682357));
#271840=CARTESIAN_POINT('Ctrl Pts',(0.597453535611398,43.1047208406736,
-26.2333263513415));
#271841=CARTESIAN_POINT('Ctrl Pts',(0.0328697087628114,43.5553535001865,
-27.3183401090776));
#271842=CARTESIAN_POINT('Origin',(-15.8776902912372,3.06591104035337,1.49207703394933));
#271843=CARTESIAN_POINT('',(0.0328697087628034,27.4862025048977,-41.7870686536687));
#271844=CARTESIAN_POINT('Ctrl Pts',(0.0328697087628071,27.4862025048977,
-41.7870686536687));
#271845=CARTESIAN_POINT('Ctrl Pts',(0.0352790378720934,27.4817986491653,
-41.7846721480517));
#271846=CARTESIAN_POINT('Ctrl Pts',(0.0376867650499835,27.4773950462125,
-41.7822739395601));
#271847=CARTESIAN_POINT('Ctrl Pts',(0.986850403300234,25.740370168843,-40.8355611304885));
#271848=CARTESIAN_POINT('Ctrl Pts',(1.68188687638379,24.0610251529196,-39.6309729447144));
#271849=CARTESIAN_POINT('Ctrl Pts',(2.20268963592813,22.0128977532289,-37.6785166475666));
#271850=CARTESIAN_POINT('Ctrl Pts',(2.2980625106802,21.5090055123993,-37.1507671602473));
#271851=CARTESIAN_POINT('Ctrl Pts',(2.35340786587133,21.0318784730203,-36.6018952879149));
#271852=CARTESIAN_POINT('',(0.0328697087628034,28.3366049276471,-41.2960885859748));
#271853=CARTESIAN_POINT('Origin',(0.0328697087628034,3.06591104035337,1.49207703394933));
#271854=CARTESIAN_POINT('Ctrl Pts',(2.35340786587133,27.0732750858163,-33.1138933272358));
#271855=CARTESIAN_POINT('Ctrl Pts',(2.2321228552984,27.5921455877354,-34.6208026830141));
#271856=CARTESIAN_POINT('Ctrl Pts',(1.92300889597279,27.9437118105647,-36.1461193972233));
#271857=CARTESIAN_POINT('Ctrl Pts',(1.08076370197649,28.3081505396363,-38.8997398714277));
#271858=CARTESIAN_POINT('Ctrl Pts',(0.597453535611393,28.3662463619963,
-40.1215903809247));
#271859=CARTESIAN_POINT('Ctrl Pts',(0.0328697087628079,28.3366049276471,
-41.2960885859748));
#271860=CARTESIAN_POINT('Origin',(-15.8776902912372,3.06591104035337,1.49207703394933));
#271861=CARTESIAN_POINT('',(0.0328697087628034,51.5689486443196,-9.31951072417391));
#271862=CARTESIAN_POINT('Ctrl Pts',(0.0328697087628049,51.5689486443196,
-9.31951072417391));
#271863=CARTESIAN_POINT('Ctrl Pts',(0.035279037872092,51.5642209389145,
-9.3211798515169));
#271864=CARTESIAN_POINT('Ctrl Pts',(0.0376867650499852,51.5594921371697,
-9.3228476515626));
#271865=CARTESIAN_POINT('Ctrl Pts',(0.98685040330015,49.6936509024404,-9.98023418492342));
#271866=CARTESIAN_POINT('Ctrl Pts',(1.68188687638376,47.6747662765606,-10.4222039205384));
#271867=CARTESIAN_POINT('Ctrl Pts',(2.20268963592813,44.8533437535091,-10.6378109335374));
#271868=CARTESIAN_POINT('Ctrl Pts',(2.2980625106802,44.1239797322136,-10.6591425104526));
#271869=CARTESIAN_POINT('Ctrl Pts',(2.35340786587134,43.3968281352698,-10.6464500321153));
#271870=CARTESIAN_POINT('',(0.0328697087628034,51.7731096363835,-8.35900877372875));
#271871=CARTESIAN_POINT('Origin',(0.0328697087628034,3.06591104035337,1.49207703394933));
#271872=CARTESIAN_POINT('',(2.35340786587192,44.8472209057105,-3.82288853372976));
#271873=CARTESIAN_POINT('Ctrl Pts',(2.35340786587134,44.8472209057105,-3.82288853372974));
#271874=CARTESIAN_POINT('Ctrl Pts',(2.23212285529842,46.3142649294914,-4.44561177609555));
#271875=CARTESIAN_POINT('Ctrl Pts',(1.92300889597281,47.6830398727272,-5.20498325465543));
#271876=CARTESIAN_POINT('Ctrl Pts',(1.08076370197649,49.9732357872253,-6.77668423652894));
#271877=CARTESIAN_POINT('Ctrl Pts',(0.597453535611392,50.9201213637075,
-7.55108819905984));
#271878=CARTESIAN_POINT('Ctrl Pts',(0.0328697087628119,51.7731096363835,
-8.35900877372874));
#271879=CARTESIAN_POINT('Ctrl Pts',(2.41030970876281,43.4921152187147,-3.01326686083735));
#271880=CARTESIAN_POINT('Ctrl Pts',(2.41030970876281,43.8264120827449,-3.28121630318514));
#271881=CARTESIAN_POINT('Ctrl Pts',(2.39944663642909,44.1899838442304,-3.51153934018084));
#271882=CARTESIAN_POINT('Ctrl Pts',(2.36767303424712,44.6658952728075,-3.74315824157946));
#271883=CARTESIAN_POINT('Ctrl Pts',(2.36093683952928,44.7561516486117,-3.78423192756042));
#271884=CARTESIAN_POINT('Ctrl Pts',(2.35340786587134,44.8472209057105,-3.82288853372975));
#271885=CARTESIAN_POINT('Origin',(-15.8776902912372,3.06591104035337,1.49207703394933));
#271886=CARTESIAN_POINT('',(0.0328697087628034,7.77174294992589,-47.9780172928478));
#271887=CARTESIAN_POINT('Ctrl Pts',(0.0328697087628155,7.77174294992591,
-47.9780172928478));
#271888=CARTESIAN_POINT('Ctrl Pts',(0.0352790378721102,7.76869457417527,
-47.97403676653));
#271889=CARTESIAN_POINT('Ctrl Pts',(0.0376867650500066,7.76564712197171,
-47.9700547873736));
#271890=CARTESIAN_POINT('Ctrl Pts',(0.986850403300151,6.56385872535737,
-46.3986779333939));
#271891=CARTESIAN_POINT('Ctrl Pts',(1.68188687638379,5.51965086921625,-44.6151807136072));
#271892=CARTESIAN_POINT('Ctrl Pts',(2.20268963592814,4.44272890660951,-41.9984746689602));
#271893=CARTESIAN_POINT('Ctrl Pts',(2.29806251068019,4.19705549371556,-41.3114000835396));
#271894=CARTESIAN_POINT('Ctrl Pts',(2.35340786587133,3.98442455700369,-40.6159156274248));
#271895=CARTESIAN_POINT('',(0.0328697087628034,8.74832380494785,-47.8753745089056));
#271896=CARTESIAN_POINT('Origin',(0.0328697087628034,3.06591104035337,1.49207703394933));
#271897=CARTESIAN_POINT('Ctrl Pts',(2.35340786587133,10.9222131989692,-39.8867246577761));
#271898=CARTESIAN_POINT('Ctrl Pts',(2.2321228552984,10.7833097363133,-41.4743985009681));
#271899=CARTESIAN_POINT('Ctrl Pts',(1.92300889597278,10.4840792622747,-43.0108395219927));
#271900=CARTESIAN_POINT('Ctrl Pts',(1.08076370197648,9.69701225982446,-45.6746275835432));
#271901=CARTESIAN_POINT('Ctrl Pts',(0.597453535611381,9.25311405987619,
-46.8144732661759));
#271902=CARTESIAN_POINT('Ctrl Pts',(0.0328697087628118,8.74832380494786,
-47.8753745089056));
#271903=CARTESIAN_POINT('Origin',(-16.4313702912372,3.06591104035337,1.49207703394933));
#271904=CARTESIAN_POINT('',(-6.85393029123721,-11.8224981078497,48.9027336387577));
#271905=CARTESIAN_POINT('',(-3.4105302912372,-11.8224981078497,48.9027336387577));
#271906=CARTESIAN_POINT('',(-6.85393029123721,-12.7563976933524,48.5992912691242));
#271907=CARTESIAN_POINT('Origin',(-6.8539302912372,3.06591104035337,1.49207703394933));
#271908=CARTESIAN_POINT('',(-3.4105302912372,-12.7563976933524,48.5992912691242));
#271909=CARTESIAN_POINT('Origin',(-16.4313702912372,3.06591104035337,1.49207703394933));
#271910=CARTESIAN_POINT('',(-6.85393029123721,7.77174294992524,50.9621713607466));
#271911=CARTESIAN_POINT('',(-3.4105302912372,7.77174294992524,50.9621713607466));
#271912=CARTESIAN_POINT('',(-6.85393029123721,8.74832380494721,50.8595285768044));
#271913=CARTESIAN_POINT('',(-3.4105302912372,8.7483238049472,50.8595285768044));
#271914=CARTESIAN_POINT('Origin',(-6.8539302912372,3.06591104035337,1.49207703394933));
#271915=CARTESIAN_POINT('Origin',(-16.4313702912372,3.06591104035337,1.49207703394933));
#271916=CARTESIAN_POINT('',(-6.85393029123721,27.4862025048971,44.7712227215677));
#271917=CARTESIAN_POINT('',(-3.4105302912372,27.4862025048971,44.7712227215677));
#271918=CARTESIAN_POINT('',(-6.8539302912372,28.3366049276465,44.2802426538738));
#271919=CARTESIAN_POINT('',(-3.4105302912372,28.3366049276465,44.2802426538737));
#271920=CARTESIAN_POINT('Origin',(-6.8539302912372,3.06591104035337,1.49207703394933));
#271921=CARTESIAN_POINT('Origin',(-16.4313702912372,3.06591104035337,1.49207703394933));
#271922=CARTESIAN_POINT('',(-6.85393029123721,42.9781718142661,31.0969166143042));
#271923=CARTESIAN_POINT('',(-3.4105302912372,42.9781718142661,31.0969166143043));
#271924=CARTESIAN_POINT('',(-6.8539302912372,43.5553535001861,30.3024941769768));
#271925=CARTESIAN_POINT('',(-3.4105302912372,43.5553535001861,30.3024941769768));
#271926=CARTESIAN_POINT('Origin',(-6.8539302912372,3.06591104035337,1.49207703394933));
#271927=CARTESIAN_POINT('Origin',(-16.4313702912372,3.06591104035337,1.49207703394933));
#271928=CARTESIAN_POINT('',(-6.8539302912372,-42.5287624981535,21.2546889964492));
#271929=CARTESIAN_POINT('Origin',(-6.8539302912372,3.06591104035337,1.49207703394933));
#271930=CARTESIAN_POINT('',(-3.4105302912372,-42.5287624981535,21.2546889964492));
#271931=CARTESIAN_POINT('Origin',(-16.4313702912372,3.06591104035337,1.49207703394933));
#271932=CARTESIAN_POINT('',(-6.8539302912372,-30.5487174154099,38.0911458806337));
#271933=CARTESIAN_POINT('',(-3.4105302912372,-30.54871741541,38.0911458806337));
#271934=CARTESIAN_POINT('',(-6.8539302912372,-29.8189788219714,38.748205461446));
#271935=CARTESIAN_POINT('',(-3.4105302912372,-29.8189788219714,38.748205461446));
#271936=CARTESIAN_POINT('Origin',(-6.8539302912372,3.06591104035337,1.49207703394933));
#271937=CARTESIAN_POINT('Origin',(-16.4313702912372,3.06591104035337,1.49207703394933));
#271938=CARTESIAN_POINT('',(-6.85393029123721,-46.6250743114837,1.98305710164289));
#271939=CARTESIAN_POINT('',(-3.4105302912372,-46.6250743114837,1.98305710164289));
#271940=CARTESIAN_POINT('',(-6.85393029123721,-46.6250743114837,1.00109696625508));
#271941=CARTESIAN_POINT('Origin',(-6.8539302912372,3.06591104035337,1.49207703394933));
#271942=CARTESIAN_POINT('',(-3.4105302912372,-46.6250743114837,1.00109696625508));
#271943=CARTESIAN_POINT('Origin',(-16.4313702912372,3.06591104035337,1.49207703394933));
#271944=CARTESIAN_POINT('',(-6.85393029123721,-30.5487174154095,-35.1069918127355));
#271945=CARTESIAN_POINT('',(-3.4105302912372,-30.5487174154095,-35.1069918127355));
#271946=CARTESIAN_POINT('',(-6.85393029123721,-29.8189788219709,-35.7640513935478));
#271947=CARTESIAN_POINT('Origin',(-6.8539302912372,3.06591104035337,1.49207703394933));
#271948=CARTESIAN_POINT('',(-3.4105302912372,-29.8189788219709,-35.7640513935478));
#271949=CARTESIAN_POINT('Origin',(-16.4313702912372,3.06591104035337,1.49207703394933));
#271950=CARTESIAN_POINT('',(-6.85393029123721,-42.1293633290513,-19.1676001498208));
#271951=CARTESIAN_POINT('',(-3.4105302912372,-42.1293633290513,-19.1676001498208));
#271952=CARTESIAN_POINT('',(-6.85393029123721,-42.5287624981532,-18.2705349285512));
#271953=CARTESIAN_POINT('',(-3.4105302912372,-42.5287624981532,-18.2705349285512));
#271954=CARTESIAN_POINT('Origin',(-6.8539302912372,3.06591104035337,1.49207703394933));
#271955=CARTESIAN_POINT('Origin',(-16.4313702912372,3.06591104035337,1.49207703394933));
#271956=CARTESIAN_POINT('',(-6.85393029123721,-12.7563976933517,-45.6151372012257));
#271957=CARTESIAN_POINT('',(-3.4105302912372,-12.7563976933517,-45.6151372012257));
#271958=CARTESIAN_POINT('',(-6.85393029123721,-11.8224981078491,-45.9185795708593));
#271959=CARTESIAN_POINT('Origin',(-6.8539302912372,3.06591104035337,1.49207703394933));
#271960=CARTESIAN_POINT('',(-3.4105302912372,-11.8224981078491,-45.9185795708593));
#271961=CARTESIAN_POINT('Origin',(-16.4313702912372,3.06591104035337,1.49207703394933));
#271962=CARTESIAN_POINT('',(-6.85393029123721,42.9781718142665,-28.112762546405));
#271963=CARTESIAN_POINT('',(-3.4105302912372,42.9781718142665,-28.112762546405));
#271964=CARTESIAN_POINT('',(-6.85393029123721,43.5553535001865,-27.3183401090776));
#271965=CARTESIAN_POINT('Origin',(-6.8539302912372,3.06591104035337,1.49207703394933));
#271966=CARTESIAN_POINT('',(-3.4105302912372,43.5553535001865,-27.3183401090776));
#271967=CARTESIAN_POINT('Origin',(-16.4313702912372,3.06591104035337,1.49207703394933));
#271968=CARTESIAN_POINT('',(-6.85393029123721,28.3366049276471,-41.2960885859748));
#271969=CARTESIAN_POINT('',(-3.4105302912372,28.3366049276471,-41.2960885859748));
#271970=CARTESIAN_POINT('',(-6.85393029123721,27.4862025048976,-41.7870686536687));
#271971=CARTESIAN_POINT('',(-3.4105302912372,27.4862025048977,-41.7870686536687));
#271972=CARTESIAN_POINT('Origin',(-6.8539302912372,3.06591104035337,1.49207703394933));
#271973=CARTESIAN_POINT('Origin',(-16.4313702912372,3.06591104035337,1.49207703394933));
#271974=CARTESIAN_POINT('',(-6.85393029123721,51.5689486443196,-9.31951072417391));
#271975=CARTESIAN_POINT('',(-3.4105302912372,51.5689486443196,-9.31951072417391));
#271976=CARTESIAN_POINT('',(-6.8539302912372,51.7731096363835,-8.35900877372874));
#271977=CARTESIAN_POINT('Origin',(-6.8539302912372,3.06591104035337,1.49207703394933));
#271978=CARTESIAN_POINT('',(-3.4105302912372,51.7731096363835,-8.35900877372874));
#271979=CARTESIAN_POINT('Origin',(-16.4313702912372,3.06591104035337,1.49207703394933));
#271980=CARTESIAN_POINT('',(-6.85393029123721,8.74832380494785,-47.8753745089056));
#271981=CARTESIAN_POINT('',(-3.4105302912372,8.74832380494785,-47.8753745089056));
#271982=CARTESIAN_POINT('',(-6.85393029123721,7.77174294992591,-47.9780172928478));
#271983=CARTESIAN_POINT('',(-3.4105302912372,7.7717429499259,-47.9780172928478));
#271984=CARTESIAN_POINT('Origin',(-6.8539302912372,3.06591104035337,1.49207703394933));
#271985=CARTESIAN_POINT('Origin',(9.0566297087628,3.06591104035337,1.49207703394933));
#271986=CARTESIAN_POINT('',(-9.17446844834478,-6.58727470336753,42.4889393291034));
#271987=CARTESIAN_POINT('Ctrl Pts',(-9.17446844834572,-6.58727470336757,
42.4889393291035));
#271988=CARTESIAN_POINT('Ctrl Pts',(-9.0531834377728,-7.3599344600069,43.8828544286572));
#271989=CARTESIAN_POINT('Ctrl Pts',(-8.74406947844719,-8.25822196352857,
45.1647551458335));
#271990=CARTESIAN_POINT('Ctrl Pts',(-7.90182428445088,-10.0607036624979,
47.2781176391333));
#271991=CARTESIAN_POINT('Ctrl Pts',(-7.41851411808579,-10.9298418532948,
48.1388688212015));
#271992=CARTESIAN_POINT('Ctrl Pts',(-6.85393029123721,-11.8224981078497,
48.9027336387577));
#271993=CARTESIAN_POINT('',(-9.2313702912372,-5.64044110768439,41.2258855621436));
#271994=CARTESIAN_POINT('Ctrl Pts',(-9.2313702912372,-5.64044110768439,
41.2258855621436));
#271995=CARTESIAN_POINT('Ctrl Pts',(-9.2313702912372,-5.73148089796471,
41.3178411359666));
#271996=CARTESIAN_POINT('Ctrl Pts',(-9.2303894871794,-5.81952391869129,
41.412952322369));
#271997=CARTESIAN_POINT('Ctrl Pts',(-9.22181693596821,-6.16632994440474,
41.8139324556473));
#271998=CARTESIAN_POINT('Ctrl Pts',(-9.20467998252579,-6.39480873797743,
42.1417215362753));
#271999=CARTESIAN_POINT('Ctrl Pts',(-9.17446844834572,-6.58727470336757,
42.4889393291035));
#272000=CARTESIAN_POINT('',(-9.2313702912372,-13.2454487831571,38.7548687783801));
#272001=CARTESIAN_POINT('Origin',(-9.2313702912372,3.06591104035337,1.49207703394933));
#272002=CARTESIAN_POINT('',(-9.17446844834572,-13.2218486904757,40.3332355645775));
#272003=CARTESIAN_POINT('Ctrl Pts',(-9.17446844834573,-13.2218486904757,
40.3332355645775));
#272004=CARTESIAN_POINT('Ctrl Pts',(-9.21458398225973,-13.1576069969014,
39.8100289569889));
#272005=CARTESIAN_POINT('Ctrl Pts',(-9.2313702912372,-13.1650966155822,
39.279160339353));
#272006=CARTESIAN_POINT('Ctrl Pts',(-9.2313702912372,-13.2454487831571,
38.7548687783801));
#272007=CARTESIAN_POINT('Ctrl Pts',(-6.85393029123721,-12.7563976933524,
48.5992912691241));
#272008=CARTESIAN_POINT('Ctrl Pts',(-6.8563396203465,-12.7575634972604,
48.5944149912678));
#272009=CARTESIAN_POINT('Ctrl Pts',(-6.85874734752439,-12.7587278665434,
48.5895377618179));
#272010=CARTESIAN_POINT('Ctrl Pts',(-7.80791098577455,-13.2174796507233,
46.6652021964936));
#272011=CARTESIAN_POINT('Ctrl Pts',(-8.50294745885817,-13.4459973224246,
44.6111788145591));
#272012=CARTESIAN_POINT('Ctrl Pts',(-9.02375021840253,-13.3655042570837,
41.7826752695607));
#272013=CARTESIAN_POINT('Ctrl Pts',(-9.11912309315459,-13.3104796770798,
41.0550770237344));
#272014=CARTESIAN_POINT('Ctrl Pts',(-9.17446844834573,-13.2218486904757,
40.3332355645775));
#272015=CARTESIAN_POINT('Origin',(9.0566297087628,3.06591104035337,1.49207703394933));
#272016=CARTESIAN_POINT('',(-9.17446844834725,3.9844245570031,43.6000696953234));
#272017=CARTESIAN_POINT('',(-9.2313702912372,3.32088519137382,42.1677589097724));
#272018=CARTESIAN_POINT('Ctrl Pts',(-9.17446844834574,3.98442455700307,
43.6000696953233));
#272019=CARTESIAN_POINT('Ctrl Pts',(-9.21458398225973,3.83030496515345,
43.0959672247623));
#272020=CARTESIAN_POINT('Ctrl Pts',(-9.2313702912372,3.6075391385767,42.6140409128762));
#272021=CARTESIAN_POINT('Ctrl Pts',(-9.2313702912372,3.32088519137384,42.1677589097724));
#272022=CARTESIAN_POINT('Ctrl Pts',(-6.85393029123721,7.77174294992524,
50.9621713607466));
#272023=CARTESIAN_POINT('Ctrl Pts',(-6.8563396203465,7.7686945741746,50.9581908344287));
#272024=CARTESIAN_POINT('Ctrl Pts',(-6.8587473475244,7.76564712197105,50.9542088552723));
#272025=CARTESIAN_POINT('Ctrl Pts',(-7.80791098577456,6.5638587253567,49.3828320012926));
#272026=CARTESIAN_POINT('Ctrl Pts',(-8.50294745885817,5.51965086921566,
47.5993347815059));
#272027=CARTESIAN_POINT('Ctrl Pts',(-9.02375021840254,4.44272890660893,
44.9826287368589));
#272028=CARTESIAN_POINT('Ctrl Pts',(-9.1191230931546,4.19705549371495,44.2955541514382));
#272029=CARTESIAN_POINT('Ctrl Pts',(-9.17446844834574,3.98442455700307,
43.6000696953233));
#272030=CARTESIAN_POINT('',(-9.17446844834575,10.9222131989687,42.8708787256748));
#272031=CARTESIAN_POINT('Ctrl Pts',(-9.17446844834573,10.9222131989687,
42.8708787256748));
#272032=CARTESIAN_POINT('Ctrl Pts',(-9.0531834377728,10.7833097363127,44.4585525688669));
#272033=CARTESIAN_POINT('Ctrl Pts',(-8.74406947844717,10.4840792622741,
45.9949935898914));
#272034=CARTESIAN_POINT('Ctrl Pts',(-7.90182428445088,9.69701225982382,
48.658781651442));
#272035=CARTESIAN_POINT('Ctrl Pts',(-7.41851411808578,9.25311405987554,
49.7986273340746));
#272036=CARTESIAN_POINT('Ctrl Pts',(-6.85393029123721,8.74832380494719,
50.8595285768044));
#272037=CARTESIAN_POINT('',(-9.2313702912372,11.273458480251,41.3319097758507));
#272038=CARTESIAN_POINT('Ctrl Pts',(-9.2313702912372,11.273458480251,41.3319097758507));
#272039=CARTESIAN_POINT('Ctrl Pts',(-9.2313702912372,11.2276911947845,41.4529445913066));
#272040=CARTESIAN_POINT('Ctrl Pts',(-9.2303894871794,11.1859450977989,41.5756433063122));
#272041=CARTESIAN_POINT('Ctrl Pts',(-9.22181693596821,11.032215341675,42.0830156043706));
#272042=CARTESIAN_POINT('Ctrl Pts',(-9.20467998252579,10.9568134079305,
42.4753965275548));
#272043=CARTESIAN_POINT('Ctrl Pts',(-9.17446844834573,10.9222131989687,
42.8708787256748));
#272044=CARTESIAN_POINT('Origin',(-9.2313702912372,3.06591104035337,1.49207703394933));
#272045=CARTESIAN_POINT('Origin',(9.0566297087628,3.06591104035337,1.49207703394933));
#272046=CARTESIAN_POINT('',(-9.17446844834697,21.0318784730198,39.5860493558137));
#272047=CARTESIAN_POINT('',(-9.2313702912372,19.8431318188259,38.5474541178658));
#272048=CARTESIAN_POINT('Ctrl Pts',(-9.17446844834573,21.0318784730198,
39.5860493558137));
#272049=CARTESIAN_POINT('Ctrl Pts',(-9.21458398225973,20.6860462733096,
39.1882149190674));
#272050=CARTESIAN_POINT('Ctrl Pts',(-9.2313702912372,20.286522474016,38.8385603504192));
#272051=CARTESIAN_POINT('Ctrl Pts',(-9.2313702912372,19.8431318188259,38.5474541178658));
#272052=CARTESIAN_POINT('Ctrl Pts',(-6.85393029123721,27.4862025048971,
44.7712227215677));
#272053=CARTESIAN_POINT('Ctrl Pts',(-6.8563396203465,27.4817986491647,44.7688262159506));
#272054=CARTESIAN_POINT('Ctrl Pts',(-6.85874734752438,27.477395046212,44.7664280074591));
#272055=CARTESIAN_POINT('Ctrl Pts',(-7.80791098577456,25.7403701688426,
43.8197151983875));
#272056=CARTESIAN_POINT('Ctrl Pts',(-8.50294745885817,24.0610251529191,
42.6151270126134));
#272057=CARTESIAN_POINT('Ctrl Pts',(-9.02375021840253,22.0128977532284,
40.6626707154655));
#272058=CARTESIAN_POINT('Ctrl Pts',(-9.1191230931546,21.5090055123988,40.1349212281462));
#272059=CARTESIAN_POINT('Ctrl Pts',(-9.17446844834573,21.0318784730198,
39.5860493558137));
#272060=CARTESIAN_POINT('',(-9.17446844834461,27.0732750858158,36.0980473951347));
#272061=CARTESIAN_POINT('Ctrl Pts',(-9.17446844834572,27.0732750858159,
36.0980473951348));
#272062=CARTESIAN_POINT('Ctrl Pts',(-9.05318343777279,27.5921455877349,
37.6049567509131));
#272063=CARTESIAN_POINT('Ctrl Pts',(-8.74406947844717,27.9437118105642,
39.1302734651222));
#272064=CARTESIAN_POINT('Ctrl Pts',(-7.90182428445088,28.3081505396358,
41.8838939393267));
#272065=CARTESIAN_POINT('Ctrl Pts',(-7.41851411808578,28.3662463619957,
43.1057444488237));
#272066=CARTESIAN_POINT('Ctrl Pts',(-6.85393029123721,28.3366049276465,
44.2802426538738));
#272067=CARTESIAN_POINT('',(-9.2313702912372,26.7681985526003,34.549264974965));
#272068=CARTESIAN_POINT('Ctrl Pts',(-9.2313702912372,26.7681985526003,34.549264974965));
#272069=CARTESIAN_POINT('Ctrl Pts',(-9.2313702912372,26.7756173513876,34.6784510128945));
#272070=CARTESIAN_POINT('Ctrl Pts',(-9.2303894871794,26.7873864575631,34.8075215339958));
#272071=CARTESIAN_POINT('Ctrl Pts',(-9.22181693596822,26.8533142424535,
35.3335567171668));
#272072=CARTESIAN_POINT('Ctrl Pts',(-9.20467998252585,26.9440268478866,
35.7226832566201));
#272073=CARTESIAN_POINT('Ctrl Pts',(-9.17446844834572,27.0732750858159,
36.0980473951348));
#272074=CARTESIAN_POINT('Origin',(-9.2313702912372,3.06591104035337,1.49207703394933));
#272075=CARTESIAN_POINT('Origin',(9.0566297087628,3.06591104035337,1.49207703394933));
#272076=CARTESIAN_POINT('',(-9.17446844834746,34.9728534042383,28.9852351289796));
#272077=CARTESIAN_POINT('',(-9.2313702912372,33.4644445574141,28.5199379906174));
#272078=CARTESIAN_POINT('Ctrl Pts',(-9.17446844834574,34.9728534042382,
28.9852351289795));
#272079=CARTESIAN_POINT('Ctrl Pts',(-9.21458398225963,34.4951061257856,
28.7624579143744));
#272080=CARTESIAN_POINT('Ctrl Pts',(-9.2313702912372,33.9879056482328,28.6055335403951));
#272081=CARTESIAN_POINT('Ctrl Pts',(-9.2313702912372,33.4644445574141,28.5199379906174));
#272082=CARTESIAN_POINT('Ctrl Pts',(-6.85393029123721,42.9781718142661,
31.0969166143042));
#272083=CARTESIAN_POINT('Ctrl Pts',(-6.8563396203465,42.9731739452159,31.0965185069808));
#272084=CARTESIAN_POINT('Ctrl Pts',(-6.85874734752439,42.9681756144698,
31.0961187411893));
#272085=CARTESIAN_POINT('Ctrl Pts',(-7.80791098577464,40.996261638018,30.9377652223303));
#272086=CARTESIAN_POINT('Ctrl Pts',(-8.5029474588582,38.9721534719359,30.5203703112291));
#272087=CARTESIAN_POINT('Ctrl Pts',(-9.02375021840254,36.3069604692211,
29.5697611928658));
#272088=CARTESIAN_POINT('Ctrl Pts',(-9.1191230931546,35.6319769466126,29.292589484459));
#272089=CARTESIAN_POINT('Ctrl Pts',(-9.17446844834574,34.9728534042382,
28.9852351289795));
#272090=CARTESIAN_POINT('',(-9.17446844834483,39.0732456291471,23.3415294037746));
#272091=CARTESIAN_POINT('Ctrl Pts',(-9.17446844834572,39.0732456291472,
23.3415294037746));
#272092=CARTESIAN_POINT('Ctrl Pts',(-9.0531834377728,40.1601726720688,24.5071159546834));
#272093=CARTESIAN_POINT('Ctrl Pts',(-8.74406947844721,41.1017465979598,
25.7575672451231));
#272094=CARTESIAN_POINT('Ctrl Pts',(-7.90182428445089,42.554676291475,28.1248941361349));
#272095=CARTESIAN_POINT('Ctrl Pts',(-7.4185141180858,43.1047208406732,29.2174804192407));
#272096=CARTESIAN_POINT('Ctrl Pts',(-6.85393029123721,43.5553535001861,
30.3024941769768));
#272097=CARTESIAN_POINT('',(-9.2313702912372,38.1645977855601,22.0507320639531));
#272098=CARTESIAN_POINT('Ctrl Pts',(-9.2313702912372,38.1645977855601,22.0507320639531));
#272099=CARTESIAN_POINT('Ctrl Pts',(-9.2313702912372,38.2239198908931,22.1657318847802));
#272100=CARTESIAN_POINT('Ctrl Pts',(-9.2303894871794,38.2871692148531,22.27885674631));
#272101=CARTESIAN_POINT('Ctrl Pts',(-9.22181693596821,38.5613550278152,
22.7325985525449));
#272102=CARTESIAN_POINT('Ctrl Pts',(-9.20467998252579,38.8024971388486,
23.051187194492));
#272103=CARTESIAN_POINT('Ctrl Pts',(-9.17446844834572,39.0732456291471,
23.3415294037746));
#272104=CARTESIAN_POINT('Origin',(-9.2313702912372,3.06591104035337,1.49207703394933));
#272105=CARTESIAN_POINT('Origin',(9.0566297087628,3.06591104035337,1.49207703394933));
#272106=CARTESIAN_POINT('',(-9.2313702912372,-32.2877498558741,21.6091038797685));
#272107=CARTESIAN_POINT('Ctrl Pts',(-9.2313702912372,-32.2877498558741,
21.6091038797685));
#272108=CARTESIAN_POINT('Ctrl Pts',(-9.2313702912372,-32.4170036748076,
21.6029784195793));
#272109=CARTESIAN_POINT('Ctrl Pts',(-9.2303894871794,-32.5465973406721,
21.6011915101359));
#272110=CARTESIAN_POINT('Ctrl Pts',(-9.22181693596819,-33.0766421781123,
21.611772486401));
#272111=CARTESIAN_POINT('Ctrl Pts',(-9.20467998252573,-33.4731190909123,
21.6613133595047));
#272112=CARTESIAN_POINT('Ctrl Pts',(-9.17446844834573,-33.8599370650904,
21.750617325498));
#272113=CARTESIAN_POINT('',(-9.2313702912372,-35.5401699166052,14.3040488191824));
#272114=CARTESIAN_POINT('Origin',(-9.2313702912372,3.06591104035337,1.49207703394933));
#272115=CARTESIAN_POINT('',(-9.17446844834664,-36.6973334821472,15.3777206306443));
#272116=CARTESIAN_POINT('Ctrl Pts',(-9.17446844834573,-36.6973334821471,
15.3777206306443));
#272117=CARTESIAN_POINT('Ctrl Pts',(-9.21458398225973,-36.2655291156872,
15.0753679582172));
#272118=CARTESIAN_POINT('Ctrl Pts',(-9.2313702912372,-35.876028382572,14.7145816468342));
#272119=CARTESIAN_POINT('Ctrl Pts',(-9.2313702912372,-35.5401699166052,
14.3040488191824));
#272120=CARTESIAN_POINT('Ctrl Pts',(-6.85393029123721,-42.5287624981535,
21.2546889964492));
#272121=CARTESIAN_POINT('Ctrl Pts',(-6.8563396203465,-42.5259187925728,
21.2505597685487));
#272122=CARTESIAN_POINT('Ctrl Pts',(-6.85874734752439,-42.5230734198688,
21.2464309700419));
#272123=CARTESIAN_POINT('Ctrl Pts',(-7.80791098577461,-41.3999782615324,
19.6178801317866));
#272124=CARTESIAN_POINT('Ctrl Pts',(-8.50294745885819,-40.0264495820673,
18.0736484955025));
#272125=CARTESIAN_POINT('Ctrl Pts',(-9.02375021840253,-37.8706014351381,
16.2408282083446));
#272126=CARTESIAN_POINT('Ctrl Pts',(-9.1191230931546,-37.2930719331433,
15.7948611848331));
#272127=CARTESIAN_POINT('Ctrl Pts',(-9.17446844834573,-36.6973334821471,
15.3777206306443));
#272128=CARTESIAN_POINT('Origin',(9.0566297087628,3.06591104035337,1.49207703394933));
#272129=CARTESIAN_POINT('',(-9.17446844834572,-27.6118203108423,30.3504122630382));
#272130=CARTESIAN_POINT('',(-9.2313702912372,-26.9914004601511,28.8989034325401));
#272131=CARTESIAN_POINT('Ctrl Pts',(-9.17446844834573,-27.6118203108423,
30.3504122630382));
#272132=CARTESIAN_POINT('Ctrl Pts',(-9.21458398225983,-27.3403253042799,
29.8985686940558));
#272133=CARTESIAN_POINT('Ctrl Pts',(-9.2313702912372,-27.131243691954,29.4105497774492));
#272134=CARTESIAN_POINT('Ctrl Pts',(-9.2313702912372,-26.9914004601511,
28.8989034325401));
#272135=CARTESIAN_POINT('Ctrl Pts',(-6.85393029123721,-30.5487174154099,
38.0911458806337));
#272136=CARTESIAN_POINT('Ctrl Pts',(-6.85633962034649,-30.5477990693886,
38.0862170039799));
#272137=CARTESIAN_POINT('Ctrl Pts',(-6.85874734752438,-30.5468790257242,
38.0812878415165));
#272138=CARTESIAN_POINT('Ctrl Pts',(-7.80791098577459,-30.1832718463558,
36.136728666132));
#272139=CARTESIAN_POINT('Ctrl Pts',(-8.50294745885818,-29.5565865521623,
34.1673384250027));
#272140=CARTESIAN_POINT('Ctrl Pts',(-9.02375021840253,-28.3325964411277,
31.6161113387312));
#272141=CARTESIAN_POINT('Ctrl Pts',(-9.11912309315459,-27.9863881179913,
30.9737977792253));
#272142=CARTESIAN_POINT('Ctrl Pts',(-9.17446844834573,-27.6118203108423,
30.3504122630382));
#272143=CARTESIAN_POINT('',(-9.17446844834421,-22.427639094175,35.0182699968983));
#272144=CARTESIAN_POINT('Ctrl Pts',(-9.17446844834572,-22.4276390941751,
35.0182699968984));
#272145=CARTESIAN_POINT('Ctrl Pts',(-9.05318343777278,-23.7004552534814,
35.97740576878));
#272146=CARTESIAN_POINT('Ctrl Pts',(-8.74406947844716,-25.0424777164415,
36.7831139024057));
#272147=CARTESIAN_POINT('Ctrl Pts',(-7.90182428445088,-27.5487086511458,
37.9806312530676));
#272148=CARTESIAN_POINT('Ctrl Pts',(-7.41851411808578,-28.69280494373,38.4134562355128));
#272149=CARTESIAN_POINT('Ctrl Pts',(-6.85393029123721,-29.8189788219714,
38.748205461446));
#272150=CARTESIAN_POINT('',(-9.2313702912372,-21.0489333144978,34.2495248835934));
#272151=CARTESIAN_POINT('Ctrl Pts',(-9.2313702912372,-21.0489333144978,
34.2495248835934));
#272152=CARTESIAN_POINT('Ctrl Pts',(-9.2313702912372,-21.1695040027821,
34.2965012616794));
#272153=CARTESIAN_POINT('Ctrl Pts',(-9.2303894871794,-21.2886205091203,
34.3475793312918));
#272154=CARTESIAN_POINT('Ctrl Pts',(-9.2218169359682,-21.7685368919436,
34.5728341919559));
#272155=CARTESIAN_POINT('Ctrl Pts',(-9.20467998252578,-22.1105864862711,
34.7793537201167));
#272156=CARTESIAN_POINT('Ctrl Pts',(-9.17446844834572,-22.4276390941751,
35.0182699968984));
#272157=CARTESIAN_POINT('Origin',(-9.2313702912372,3.06591104035337,1.49207703394933));
#272158=CARTESIAN_POINT('Origin',(9.0566297087628,3.06591104035337,1.49207703394933));
#272159=CARTESIAN_POINT('',(-9.17446844834575,-38.9074204377757,4.98007899462811));
#272160=CARTESIAN_POINT('Ctrl Pts',(-9.17446844834573,-38.9074204377757,
4.98007899462811));
#272161=CARTESIAN_POINT('Ctrl Pts',(-9.0531834377728,-40.4718774720398,
4.67597935267518));
#272162=CARTESIAN_POINT('Ctrl Pts',(-8.74406947844718,-41.9686236067766,
4.21778627565327));
#272163=CARTESIAN_POINT('Ctrl Pts',(-7.90182428445088,-44.5355482543544,
3.15658923604996));
#272164=CARTESIAN_POINT('Ctrl Pts',(-7.41851411808577,-45.6227497463857,
2.59597643931895));
#272165=CARTESIAN_POINT('Ctrl Pts',(-6.85393029123721,-46.6250743114837,
1.98305710164289));
#272166=CARTESIAN_POINT('',(-9.2313702912372,-37.4135972503663,5.49026617684986));
#272167=CARTESIAN_POINT('Ctrl Pts',(-9.2313702912372,-37.4135972503663,
5.49026617684986));
#272168=CARTESIAN_POINT('Ctrl Pts',(-9.2313702912372,-37.5291850404213,
5.43209802610041));
#272169=CARTESIAN_POINT('Ctrl Pts',(-9.2303894871794,-37.6468479436625,
5.37775511047759));
#272170=CARTESIAN_POINT('Ctrl Pts',(-9.22181693596821,-38.1353716680188,
5.17183265542212));
#272171=CARTESIAN_POINT('Ctrl Pts',(-9.20467998252579,-38.5177214391886,
5.05582880644415));
#272172=CARTESIAN_POINT('Ctrl Pts',(-9.17446844834573,-38.9074204377757,
4.98007899462811));
#272173=CARTESIAN_POINT('',(-9.2313702912372,-37.4135972503662,-2.50611210895178));
#272174=CARTESIAN_POINT('Origin',(-9.2313702912372,3.06591104035337,1.49207703394933));
#272175=CARTESIAN_POINT('',(-9.17446844834572,-38.9074204377757,-1.99592492673002));
#272176=CARTESIAN_POINT('Ctrl Pts',(-9.17446844834573,-38.9074204377757,
-1.99592492673002));
#272177=CARTESIAN_POINT('Ctrl Pts',(-9.21458398225963,-38.3899696091993,
-2.09650717875226));
#272178=CARTESIAN_POINT('Ctrl Pts',(-9.2313702912372,-37.8873979705538,
-2.26767765403261));
#272179=CARTESIAN_POINT('Ctrl Pts',(-9.2313702912372,-37.4135972503662,
-2.50611210895176));
#272180=CARTESIAN_POINT('Ctrl Pts',(-6.85393029123721,-46.6250743114837,
1.00109696625508));
#272181=CARTESIAN_POINT('Ctrl Pts',(-6.8563396203465,-46.6207969488729,
0.998481368124769));
#272182=CARTESIAN_POINT('Ctrl Pts',(-6.85874734752438,-46.6165182379192,
0.995866840345263));
#272183=CARTESIAN_POINT('Ctrl Pts',(-7.8079109857745,-44.9281284564905,
-0.0350844259263218));
#272184=CARTESIAN_POINT('Ctrl Pts',(-8.50294745885815,-43.0452519785498,
-0.887145778547745));
#272185=CARTESIAN_POINT('Ctrl Pts',(-9.02375021840252,-40.3303115255954,
-1.68464798829298));
#272186=CARTESIAN_POINT('Ctrl Pts',(-9.11912309315459,-39.6213209423278,
-1.85715672596162));
#272187=CARTESIAN_POINT('Ctrl Pts',(-9.17446844834573,-38.9074204377757,
-1.99592492673003));
#272188=CARTESIAN_POINT('Origin',(9.0566297087628,3.06591104035337,1.49207703394933));
#272189=CARTESIAN_POINT('Ctrl Pts',(-9.17446844834573,-27.6118203108419,
-27.3662581951399));
#272190=CARTESIAN_POINT('Ctrl Pts',(-9.0531834377728,-28.4326563194546,
-28.7323587226485));
#272191=CARTESIAN_POINT('Ctrl Pts',(-8.74406947844717,-29.0936711538979,
-30.1512488791885));
#272192=CARTESIAN_POINT('Ctrl Pts',(-7.90182428445088,-30.022655911016,
-32.7689250670023));
#272193=CARTESIAN_POINT('Ctrl Pts',(-7.41851411808577,-30.3335192056261,
-33.9519964106658));
#272194=CARTESIAN_POINT('Ctrl Pts',(-6.85393029123721,-30.5487174154095,
-35.1069918127356));
#272195=CARTESIAN_POINT('Origin',(-9.2313702912372,3.06591104035337,1.49207703394933));
#272196=CARTESIAN_POINT('Ctrl Pts',(-6.85393029123721,-29.8189788219709,
-35.7640513935478));
#272197=CARTESIAN_POINT('Ctrl Pts',(-6.8563396203465,-29.8141729395174,
-35.7626228704198));
#272198=CARTESIAN_POINT('Ctrl Pts',(-6.85874734752439,-29.8093669502722,
-35.7611926290733));
#272199=CARTESIAN_POINT('Ctrl Pts',(-7.80791098577461,-27.9134675732054,
-35.1963155455424));
#272200=CARTESIAN_POINT('Ctrl Pts',(-8.50294745885819,-26.0203723086323,
-34.3672059634821));
#272201=CARTESIAN_POINT('Ctrl Pts',(-9.02375021840253,-23.6110629166399,
-32.8832451515692));
#272202=CARTESIAN_POINT('Ctrl Pts',(-9.11912309315459,-23.0084566420073,
-32.4717933445401));
#272203=CARTESIAN_POINT('Ctrl Pts',(-9.17446844834573,-22.4276390941746,
-32.034115929));
#272204=CARTESIAN_POINT('Origin',(9.0566297087628,3.06591104035337,1.49207703394933));
#272205=CARTESIAN_POINT('Ctrl Pts',(-6.85393029123721,-42.1293633290513,
-19.1676001498208));
#272206=CARTESIAN_POINT('Ctrl Pts',(-6.8563396203465,-42.1243919042643,
-19.1682498575022));
#272207=CARTESIAN_POINT('Ctrl Pts',(-6.85874734752439,-42.1194196830558,
-19.1688980389491));
#272208=CARTESIAN_POINT('Ctrl Pts',(-7.80791098577457,-40.1576732102832,
-19.4239888934006));
#272209=CARTESIAN_POINT('Ctrl Pts',(-8.50294745885817,-38.0910153822985,
-19.4365508137567));
#272210=CARTESIAN_POINT('Ctrl Pts',(-9.02375021840253,-35.2864204920946,
-19.060839568944));
#272211=CARTESIAN_POINT('Ctrl Pts',(-9.11912309315459,-34.5685597403786,
-18.9300616928343));
#272212=CARTESIAN_POINT('Ctrl Pts',(-9.17446844834573,-33.8599370650901,
-18.7664632575999));
#272213=CARTESIAN_POINT('',(-9.17446844834426,-36.697333482147,-12.3935665627462));
#272214=CARTESIAN_POINT('Ctrl Pts',(-9.17446844834572,-36.6973334821471,
-12.3935665627462));
#272215=CARTESIAN_POINT('Ctrl Pts',(-9.05318343777279,-38.0028476319475,
-13.3076974116759));
#272216=CARTESIAN_POINT('Ctrl Pts',(-8.74406947844718,-39.1838293505519,
-14.3350591142921));
#272217=CARTESIAN_POINT('Ctrl Pts',(-7.90182428445088,-41.0972039809272,
-16.3485731636698));
#272218=CARTESIAN_POINT('Ctrl Pts',(-7.41851411808579,-41.8623901985069,
-17.3029231228355));
#272219=CARTESIAN_POINT('Ctrl Pts',(-6.85393029123721,-42.5287624981532,
-18.2705349285512));
#272220=CARTESIAN_POINT('',(-9.2313702912372,-35.540169916605,-11.3198947512843));
#272221=CARTESIAN_POINT('Ctrl Pts',(-9.2313702912372,-35.540169916605,-11.3198947512843));
#272222=CARTESIAN_POINT('Ctrl Pts',(-9.2313702912372,-35.6221054987989,
-11.4200477908884));
#272223=CARTESIAN_POINT('Ctrl Pts',(-9.2303894871794,-35.7074926545126,
-11.5175503288896));
#272224=CARTESIAN_POINT('Ctrl Pts',(-9.22181693596822,-36.0700250757452,
-11.9043703520391));
#272225=CARTESIAN_POINT('Ctrl Pts',(-9.20467998252585,-36.3721359563108,
-12.1658608037486));
#272226=CARTESIAN_POINT('Ctrl Pts',(-9.17446844834572,-36.6973334821471,
-12.3935665627463));
#272227=CARTESIAN_POINT('Origin',(-9.2313702912372,3.06591104035337,1.49207703394933));
#272228=CARTESIAN_POINT('Origin',(9.0566297087628,3.06591104035337,1.49207703394933));
#272229=CARTESIAN_POINT('Ctrl Pts',(-9.17446844834573,-13.2218486904752,
-37.349081496679));
#272230=CARTESIAN_POINT('Ctrl Pts',(-9.0531834377728,-13.4160765549498,
-38.9309405109264));
#272231=CARTESIAN_POINT('Ctrl Pts',(-8.74406947844719,-13.4428290352255,
-40.4960201231121));
#272232=CARTESIAN_POINT('Ctrl Pts',(-7.90182428445088,-13.2267940150191,
-43.2652384556475));
#272233=CARTESIAN_POINT('Ctrl Pts',(-7.41851411808578,-13.0295832989171,
-44.4724674006236));
#272234=CARTESIAN_POINT('Ctrl Pts',(-6.85393029123721,-12.7563976933517,
-45.6151372012257));
#272235=CARTESIAN_POINT('Origin',(-9.2313702912372,3.06591104035337,1.49207703394933));
#272236=CARTESIAN_POINT('Ctrl Pts',(-6.85393029123721,-11.8224981078491,
-45.9185795708593));
#272237=CARTESIAN_POINT('Ctrl Pts',(-6.8563396203465,-11.8186887484654,
-45.9153198215484));
#272238=CARTESIAN_POINT('Ctrl Pts',(-6.85874734752438,-11.814879990385,
-45.9120584591307));
#272239=CARTESIAN_POINT('Ctrl Pts',(-7.80791098577457,-10.3126459350241,
-44.624885817107));
#272240=CARTESIAN_POINT('Ctrl Pts',(-8.50294745885817,-8.92044660333771,
-43.0974653115927));
#272241=CARTESIAN_POINT('Ctrl Pts',(-9.02375021840253,-7.32301419132085,
-40.76184523832));
#272242=CARTESIAN_POINT('Ctrl Pts',(-9.11912309315459,-6.93985849316177,
-40.1408632557293));
#272243=CARTESIAN_POINT('Ctrl Pts',(-9.17446844834573,-6.58727470336698,
-39.5047852612049));
#272244=CARTESIAN_POINT('Origin',(9.0566297087628,3.06591104035337,1.49207703394933));
#272245=CARTESIAN_POINT('Ctrl Pts',(-9.17446844834572,34.9728534042388,
-26.0010810610805));
#272246=CARTESIAN_POINT('Ctrl Pts',(-9.05318343777278,36.4172710166952,
-26.6746240553429));
#272247=CARTESIAN_POINT('Ctrl Pts',(-8.74406947844716,37.8974832093382,
-27.1837033737512));
#272248=CARTESIAN_POINT('Ctrl Pts',(-7.90182428445088,40.5979248421638,
-27.833977385924));
#272249=CARTESIAN_POINT('Ctrl Pts',(-7.41851411808578,41.8070092596918,
-28.019473109391));
#272250=CARTESIAN_POINT('Ctrl Pts',(-6.85393029123721,42.9781718142665,
-28.112762546405));
#272251=CARTESIAN_POINT('Origin',(-9.2313702912372,3.06591104035337,1.49207703394933));
#272252=CARTESIAN_POINT('Ctrl Pts',(-6.85393029123721,43.5553535001865,
-27.3183401090776));
#272253=CARTESIAN_POINT('Ctrl Pts',(-6.8563396203465,43.5534304511502,-27.3137098750784));
#272254=CARTESIAN_POINT('Ctrl Pts',(-6.85874734752438,43.5515056821452,
-27.3090797144751));
#272255=CARTESIAN_POINT('Ctrl Pts',(-7.80791098577445,42.7915476059871,
-25.482612006044));
#272256=CARTESIAN_POINT('Ctrl Pts',(-8.50294745885813,41.7690976341434,
-23.6865528659012));
#272257=CARTESIAN_POINT('Ctrl Pts',(-9.02375021840253,40.0414247065461,
-21.4455580660668));
#272258=CARTESIAN_POINT('Ctrl Pts',(-9.1191230931546,39.5692373677241,-20.8892613567558));
#272259=CARTESIAN_POINT('Ctrl Pts',(-9.17446844834573,39.0732456291473,
-20.3573753358754));
#272260=CARTESIAN_POINT('Origin',(9.0566297087628,3.06591104035337,1.49207703394933));
#272261=CARTESIAN_POINT('Ctrl Pts',(-6.85393029123721,28.3366049276471,
-41.2960885859748));
#272262=CARTESIAN_POINT('Ctrl Pts',(-6.85633962034649,28.3367314207686,
-41.2910764822274));
#272263=CARTESIAN_POINT('Ctrl Pts',(-6.85874734752437,28.3368563127678,
-41.2860637459564));
#272264=CARTESIAN_POINT('Ctrl Pts',(-7.80791098577455,28.3854914087084,
-39.3083996706132));
#272265=CARTESIAN_POINT('Ctrl Pts',(-8.50294745885815,28.181959946691,-37.2517501322177));
#272266=CARTESIAN_POINT('Ctrl Pts',(-9.02375021840252,27.5151468934274,
-34.5017916253246));
#272267=CARTESIAN_POINT('Ctrl Pts',(-9.11912309315459,27.3100485509895,
-33.8015334003366));
#272268=CARTESIAN_POINT('Ctrl Pts',(-9.17446844834573,27.0732750858163,
-33.1138933272357));
#272269=CARTESIAN_POINT('Ctrl Pts',(-9.17446844834572,21.0318784730204,
-36.6018952879149));
#272270=CARTESIAN_POINT('Ctrl Pts',(-9.05318343777278,22.0774650053655,
-37.8047050017404));
#272271=CARTESIAN_POINT('Ctrl Pts',(-8.74406947844713,23.222644917273,-38.8718286389277));
#272272=CARTESIAN_POINT('Ctrl Pts',(-7.90182428445086,25.4251308357792,
-40.5642520735287));
#272273=CARTESIAN_POINT('Ctrl Pts',(-7.41851411808576,26.4542365054505,
-41.2254897862947));
#272274=CARTESIAN_POINT('Ctrl Pts',(-6.85393029123721,27.4862025048976,
-41.7870686536687));
#272275=CARTESIAN_POINT('Origin',(-9.2313702912372,3.06591104035337,1.49207703394933));
#272276=CARTESIAN_POINT('Origin',(9.0566297087628,3.06591104035337,1.49207703394933));
#272277=CARTESIAN_POINT('Ctrl Pts',(-9.17446844834573,43.3968281352698,
-10.6464500321153));
#272278=CARTESIAN_POINT('Ctrl Pts',(-9.0531834377728,44.9903239005218,-10.6742646041606));
#272279=CARTESIAN_POINT('Ctrl Pts',(-8.7440694784472,46.5496262384867,-10.5372751647968));
#272280=CARTESIAN_POINT('Ctrl Pts',(-7.90182428445089,49.2810926945742,
-10.0329614702827));
#272281=CARTESIAN_POINT('Ctrl Pts',(-7.41851411808579,50.4610941799812,
-9.71064130868742));
#272282=CARTESIAN_POINT('Ctrl Pts',(-6.8539302912372,51.5689486443196,-9.31951072417391));
#272283=CARTESIAN_POINT('',(-9.2313702912372,43.4921152187147,-3.01326686083733));
#272284=CARTESIAN_POINT('Origin',(-9.2313702912372,3.06591104035337,1.49207703394933));
#272285=CARTESIAN_POINT('',(-9.17446844834572,44.8472209057105,-3.82288853372976));
#272286=CARTESIAN_POINT('Ctrl Pts',(-9.17446844834573,44.8472209057105,
-3.82288853372977));
#272287=CARTESIAN_POINT('Ctrl Pts',(-9.21458398225962,44.3619898453251,
-3.61692016855346));
#272288=CARTESIAN_POINT('Ctrl Pts',(-9.2313702912372,43.9059889457207,-3.34499965969369));
#272289=CARTESIAN_POINT('Ctrl Pts',(-9.2313702912372,43.4921152187147,-3.01326686083734));
#272290=CARTESIAN_POINT('Ctrl Pts',(-6.85393029123721,51.7731096363835,
-8.35900877372875));
#272291=CARTESIAN_POINT('Ctrl Pts',(-6.8563396203465,51.769469557838,-8.35556101900044));
#272292=CARTESIAN_POINT('Ctrl Pts',(-6.85874734752439,51.7658279378758,
-8.35211403089695));
#272293=CARTESIAN_POINT('Ctrl Pts',(-7.80791098577456,50.328680344989,-6.99265554910357));
#272294=CARTESIAN_POINT('Ctrl Pts',(-8.50294745885818,48.6641027521171,
-5.76774174922925));
#272295=CARTESIAN_POINT('Ctrl Pts',(-9.02375021840253,46.1743002947837,
-4.4231990161438));
#272296=CARTESIAN_POINT('Ctrl Pts',(-9.11912309315459,45.5166694401473,
-4.1070525773466));
#272297=CARTESIAN_POINT('Ctrl Pts',(-9.17446844834573,44.8472209057105,
-3.82288853372976));
#272298=CARTESIAN_POINT('Origin',(9.0566297087628,3.06591104035337,1.49207703394933));
#272299=CARTESIAN_POINT('Ctrl Pts',(-6.85393029123721,8.74832380494786,
-47.8753745089056));
#272300=CARTESIAN_POINT('Ctrl Pts',(-6.8563396203465,8.75047796841738,-47.8708471736816));
#272301=CARTESIAN_POINT('Ctrl Pts',(-6.85874734752438,8.75263092645941,
-47.8663186093833));
#272302=CARTESIAN_POINT('Ctrl Pts',(-7.80791098577455,9.60144974457463,
-46.0794142522692));
#272303=CARTESIAN_POINT('Ctrl Pts',(-8.50294745885816,10.2520292311917,
-44.1177877048839));
#272304=CARTESIAN_POINT('Ctrl Pts',(-9.02375021840252,10.7613740869774,
-41.3343582993625));
#272305=CARTESIAN_POINT('Ctrl Pts',(-9.11912309315459,10.858828107591,-40.6112195674443));
#272306=CARTESIAN_POINT('Ctrl Pts',(-9.17446844834573,10.9222131989692,
-39.886724657776));
#272307=CARTESIAN_POINT('Ctrl Pts',(-9.17446844834573,3.98442455700367,
-40.6159156274248));
#272308=CARTESIAN_POINT('Ctrl Pts',(-9.0531834377728,4.4503885989394,-42.1400153341097));
#272309=CARTESIAN_POINT('Ctrl Pts',(-8.7440694784472,5.06252421970969,-43.5806679186922));
#272310=CARTESIAN_POINT('Ctrl Pts',(-7.90182428445087,6.3862245996304,-46.022605388695));
#272311=CARTESIAN_POINT('Ctrl Pts',(-7.41851411808577,7.05740980202734,
-47.0452510830667));
#272312=CARTESIAN_POINT('Ctrl Pts',(-6.85393029123721,7.77174294992592,
-47.9780172928478));
#272313=CARTESIAN_POINT('Origin',(-9.2313702912372,3.06591104035337,1.49207703394933));
#272314=CARTESIAN_POINT('Origin',(-15.8776902912372,3.06591104035337,1.49207703394933));
#272315=CARTESIAN_POINT('Ctrl Pts',(2.41030970876281,41.8295746888953,13.8190591635527));
#272316=CARTESIAN_POINT('Ctrl Pts',(2.41030970876281,42.2439549272288,13.7102459518845));
#272317=CARTESIAN_POINT('Ctrl Pts',(2.39944663642909,42.6697750773516,13.6477133454304));
#272318=CARTESIAN_POINT('Ctrl Pts',(2.36767303424711,43.1987496955963,13.6296895670144));
#272319=CARTESIAN_POINT('Ctrl Pts',(2.36093683952928,43.2979091708901,13.6288774630686));
#272320=CARTESIAN_POINT('Ctrl Pts',(2.35340786587134,43.3968281352696,13.6306041000145));
#272321=CARTESIAN_POINT('',(2.35340786587067,44.8472209057105,6.80704260162841));
#272322=CARTESIAN_POINT('Ctrl Pts',(2.35340786587133,44.8472209057106,6.80704260162844));
#272323=CARTESIAN_POINT('Ctrl Pts',(2.36852800519451,44.6643301269736,6.72941007193762));
#272324=CARTESIAN_POINT('Ctrl Pts',(2.38043097016002,44.4848900869505,6.64210493853095));
#272325=CARTESIAN_POINT('Ctrl Pts',(2.40398237976074,44.0213088106809,6.38581235296264));
#272326=CARTESIAN_POINT('Ctrl Pts',(2.41030970876281,43.7479067476922,6.20244587788006));
#272327=CARTESIAN_POINT('Ctrl Pts',(2.41030970876281,43.4921152187147,5.997420928736));
#272328=CARTESIAN_POINT('',(0.0328697087628034,51.7731096363835,11.3431628416274));
#272329=CARTESIAN_POINT('Ctrl Pts',(0.0328697087628105,51.7731096363835,
11.3431628416274));
#272330=CARTESIAN_POINT('Ctrl Pts',(0.035279037872097,51.769469557838,11.3397150868991));
#272331=CARTESIAN_POINT('Ctrl Pts',(0.037686765049985,51.7658279378758,
11.3362680987956));
#272332=CARTESIAN_POINT('Ctrl Pts',(0.986850403300099,50.3286803449892,
9.97680961700231));
#272333=CARTESIAN_POINT('Ctrl Pts',(1.68188687638375,48.6641027521173,8.75189581712803));
#272334=CARTESIAN_POINT('Ctrl Pts',(2.20268963592813,46.1743002947838,7.40735308404252));
#272335=CARTESIAN_POINT('Ctrl Pts',(2.29806251068019,45.5166694401474,7.0912066452453));
#272336=CARTESIAN_POINT('Ctrl Pts',(2.35340786587133,44.8472209057106,6.80704260162844));
#272337=CARTESIAN_POINT('Origin',(0.0328697087628034,3.06591104035337,1.49207703394933));
#272338=CARTESIAN_POINT('Origin',(-16.4313702912372,3.06591104035337,1.49207703394933));
#272339=CARTESIAN_POINT('',(-6.8539302912372,51.7731096363835,11.3431628416274));
#272340=CARTESIAN_POINT('',(-3.4105302912372,51.7731096363835,11.3431628416274));
#272341=CARTESIAN_POINT('Origin',(-6.8539302912372,3.06591104035337,1.49207703394933));
#272342=CARTESIAN_POINT('Origin',(9.0566297087628,3.06591104035337,1.49207703394933));
#272343=CARTESIAN_POINT('',(-9.2313702912372,41.8295746888953,13.8190591635528));
#272344=CARTESIAN_POINT('Ctrl Pts',(-9.17446844834573,43.3968281352696,
13.6306041000145));
#272345=CARTESIAN_POINT('Ctrl Pts',(-9.21458398225972,42.8697726227144,
13.6214043118221));
#272346=CARTESIAN_POINT('Ctrl Pts',(-9.2313702912372,42.3425950372429,13.6843437823865));
#272347=CARTESIAN_POINT('Ctrl Pts',(-9.2313702912372,41.8295746888953,13.8190591635527));
#272348=CARTESIAN_POINT('',(-9.17446844834455,44.8472209057105,6.80704260162841));
#272349=CARTESIAN_POINT('Ctrl Pts',(-9.17446844834572,44.8472209057106,
6.80704260162845));
#272350=CARTESIAN_POINT('Ctrl Pts',(-9.05318343777279,46.3142649294915,
7.42976584399426));
#272351=CARTESIAN_POINT('Ctrl Pts',(-8.74406947844719,47.6830398727272,
8.18913732255413));
#272352=CARTESIAN_POINT('Ctrl Pts',(-7.90182428445088,49.9732357872253,
9.76083830442761));
#272353=CARTESIAN_POINT('Ctrl Pts',(-7.41851411808578,50.9201213637075,
10.5352422669585));
#272354=CARTESIAN_POINT('Ctrl Pts',(-6.85393029123721,51.7731096363835,
11.3431628416274));
#272355=CARTESIAN_POINT('',(-9.2313702912372,43.4921152187147,5.99742092873599));
#272356=CARTESIAN_POINT('Ctrl Pts',(-9.2313702912372,43.4921152187147,5.99742092873599));
#272357=CARTESIAN_POINT('Ctrl Pts',(-9.2313702912372,43.5930832996569,6.07835001869884));
#272358=CARTESIAN_POINT('Ctrl Pts',(-9.2303894871794,43.6968764586866,6.15596890439157));
#272359=CARTESIAN_POINT('Ctrl Pts',(-9.22181693596822,44.1319110817587,
6.45896125327636));
#272360=CARTESIAN_POINT('Ctrl Pts',(-9.20467998252585,44.4817870366871,
6.65192512723797));
#272361=CARTESIAN_POINT('Ctrl Pts',(-9.17446844834572,44.8472209057106,
6.80704260162845));
#272362=CARTESIAN_POINT('Origin',(-9.2313702912372,3.06591104035337,1.49207703394933));
#272363=CARTESIAN_POINT('Origin',(-9.2313702912372,3.06591104035337,1.49207703394933));
#272364=CARTESIAN_POINT('Origin',(-9.2313702912372,-1.53724850217529,45.2882145624979));
#272365=CARTESIAN_POINT('Origin',(-9.2313702912372,16.6742095075201,43.374113195316));
#272366=CARTESIAN_POINT('Origin',(-9.2313702912372,32.5326690847319,34.21822728948));
#272367=CARTESIAN_POINT('Origin',(-9.2313702912372,43.2960584989777,19.4036926967212));
#272368=CARTESIAN_POINT('Origin',(-9.2313702912372,47.1032899382114,1.49207703394933));
#272369=CARTESIAN_POINT('Origin',(-9.2313702912372,-40.009145471192,-7.66380887188698));
#272370=CARTESIAN_POINT('Origin',(-9.2313702912372,-40.0091454711921,10.647962939785));
#272371=CARTESIAN_POINT('Origin',(-9.2313702912372,-32.5610768757426,27.3765988997259));
#272372=CARTESIAN_POINT('Origin',(-9.2313702912372,-18.9527784085759,39.6295658755751));
#272373=CARTESIAN_POINT('Origin',(2.4103097087628,35.7335955070929,28.2773985581935));
#272374=CARTESIAN_POINT('',(2.4103097087628,44.8472209057105,6.80704260162841));
#272375=CARTESIAN_POINT('Origin',(2.4103097087628,35.7335955070929,-25.2932444902948));
#272376=CARTESIAN_POINT('',(2.4103097087628,44.8472209057105,-3.82288853372976));
#272377=CARTESIAN_POINT('Origin',(2.4103097087628,47.1032899382114,1.49207703394933));
#272378=CARTESIAN_POINT('Origin',(2.4103097087628,22.0147540361679,39.2488301609802));
#272379=CARTESIAN_POINT('',(2.4103097087628,39.0732456291471,23.3415294037746));
#272380=CARTESIAN_POINT('Origin',(2.4103097087628,43.2960584989777,19.4036926967212));
#272381=CARTESIAN_POINT('Origin',(2.4103097087628,26.2897969148727,-33.7964789362641));
#272382=CARTESIAN_POINT('Origin',(2.4103097087628,-26.9873805458071,-28.1968219421462));
#272383=CARTESIAN_POINT('Origin',(2.4103097087628,38.6351352841478,-21.2996175996284));
#272384=CARTESIAN_POINT('Origin',(2.4103097087628,-12.3135738692384,-37.8538567012059));
#272385=CARTESIAN_POINT('Origin',(2.4103097087628,43.8038975571219,12.6745415268586));
#272386=CARTESIAN_POINT('Origin',(2.4103097087628,22.0147540361684,-36.2646760930813));
#272387=CARTESIAN_POINT('Origin',(2.4103097087628,44.830231645413,-4.86186520480143));
#272388=CARTESIAN_POINT('Origin',(2.4103097087628,5.01948546643284,-40.7076220708708));
#272389=CARTESIAN_POINT('Origin',(2.4103097087628,-23.3189246551137,-31.4999144624547));
#272390=CARTESIAN_POINT('',(2.4103097087628,-36.697333482147,-12.3935665627462));
#272391=CARTESIAN_POINT('Origin',(2.4103097087628,-34.4568876295199,20.9000815051911));
#272392=CARTESIAN_POINT('',(2.4103097087628,-38.9074204377757,-1.99592492673002));
#272393=CARTESIAN_POINT('Origin',(2.4103097087628,-40.009145471192,-7.66380887188698));
#272394=CARTESIAN_POINT('Origin',(2.4103097087628,9.92883769551353,-40.1916283591834));
#272395=CARTESIAN_POINT('Origin',(2.4103097087628,-36.4647000815458,-13.4063068349397));
#272396=CARTESIAN_POINT('Origin',(2.4103097087628,-7.6187838902542,-39.3792864350547));
#272397=CARTESIAN_POINT('Origin',(2.4103097087628,-39.1068178299802,3.96027419076616));
#272398=CARTESIAN_POINT('Origin',(2.4103097087628,-36.464700081546,16.3904609028378));
#272399=CARTESIAN_POINT('',(2.4103097087628,-22.427639094175,35.0182699968983));
#272400=CARTESIAN_POINT('Origin',(2.4103097087628,9.92883769551295,43.1757824270821));
#272401=CARTESIAN_POINT('',(2.4103097087628,-13.2218486904757,40.3332355645775));
#272402=CARTESIAN_POINT('Origin',(2.4103097087628,-18.9527784085759,39.6295658755751));
#272403=CARTESIAN_POINT('Origin',(2.4103097087628,-34.4568876295197,-17.915927437293));
#272404=CARTESIAN_POINT('',(2.4103097087628,-38.9074204377757,4.98007899462811));
#272405=CARTESIAN_POINT('Origin',(2.4103097087628,-23.3189246551142,34.484068530353));
#272406=CARTESIAN_POINT('',(2.4103097087628,-36.6973334821472,15.3777206306443));
#272407=CARTESIAN_POINT('Origin',(2.4103097087628,-40.0091454711921,10.647962939785));
#272408=CARTESIAN_POINT('Origin',(2.4103097087628,-7.61878389025475,42.3634405029532));
#272409=CARTESIAN_POINT('',(2.4103097087628,-27.6118203108423,30.3504122630382));
#272410=CARTESIAN_POINT('Origin',(2.4103097087628,-32.5610768757426,27.3765988997259));
#272411=CARTESIAN_POINT('Origin',(2.4103097087628,5.01948546643226,43.6917761387695));
#272412=CARTESIAN_POINT('',(2.4103097087628,27.0732750858158,36.0980473951347));
#272413=CARTESIAN_POINT('Origin',(2.4103097087628,44.8302316454129,7.84601927270067));
#272414=CARTESIAN_POINT('',(2.4103097087628,34.9728534042383,28.9852351289796));
#272415=CARTESIAN_POINT('Origin',(2.4103097087628,32.5326690847319,34.21822728948));
#272416=CARTESIAN_POINT('Origin',(2.4103097087628,-12.3135738692389,40.8380107691044));
#272417=CARTESIAN_POINT('',(2.4103097087628,10.9222131989687,42.8708787256748));
#272418=CARTESIAN_POINT('Origin',(2.4103097087628,38.6351352841475,24.2837716675275));
#272419=CARTESIAN_POINT('',(2.4103097087628,21.0318784730198,39.5860493558137));
#272420=CARTESIAN_POINT('Origin',(2.4103097087628,16.6742095075201,43.374113195316));
#272421=CARTESIAN_POINT('Origin',(2.4103097087628,-26.9873805458075,31.1809760100444));
#272422=CARTESIAN_POINT('',(2.4103097087628,-6.58727470336753,42.4889393291034));
#272423=CARTESIAN_POINT('Origin',(2.4103097087628,26.2897969148722,36.7806330041631));
#272424=CARTESIAN_POINT('',(2.4103097087628,3.9844245570031,43.6000696953234));
#272425=CARTESIAN_POINT('Origin',(2.4103097087628,-1.53724850217529,45.2882145624979));
#272426=CARTESIAN_POINT('Origin',(15.9689897087628,20.5619110403534,5.81207703394933));
#272427=CARTESIAN_POINT('',(15.9689897087628,20.5619110403534,5.81207703394933));
#272428=CARTESIAN_POINT('',(15.9689897087628,20.5619110403534,-2.82792296605067));
#272429=CARTESIAN_POINT('Origin',(15.9689897087628,20.5619110403534,-2.82792296605067));
#272430=CARTESIAN_POINT('Origin',(15.9689897087628,3.06591104035337,5.81207703394933));
#272431=CARTESIAN_POINT('Origin',(-53.7090169915742,3.06591104035337,1.49207703394933));
#272432=CARTESIAN_POINT('',(-9.2313702912372,3.06591104035337,11.6120770339493));
#272433=CARTESIAN_POINT('Origin',(-9.2313702912372,3.06591104035337,1.49207703394933));
#272434=CARTESIAN_POINT('',(2.4103097087628,3.06591104035337,11.6120770339493));
#272435=CARTESIAN_POINT('',(-53.7090169915742,3.06591104035337,11.6120770339493));
#272436=CARTESIAN_POINT('Origin',(2.4103097087628,3.06591104035337,1.49207703394933));
#272437=CARTESIAN_POINT('Origin',(-53.7090169915742,3.06591104035337,1.49207703394933));
#272438=CARTESIAN_POINT('',(-9.2313702912372,17.555631534552,-2.82792296605067));
#272439=CARTESIAN_POINT('',(-9.2313702912372,17.555631534552,5.81207703394933));
#272440=CARTESIAN_POINT('Origin',(-9.2313702912372,3.06591104035337,1.49207703394933));
#272441=CARTESIAN_POINT('',(2.4103097087628,17.555631534552,-2.82792296605067));
#272442=CARTESIAN_POINT('',(-53.7090169915742,17.555631534552,-2.82792296605067));
#272443=CARTESIAN_POINT('',(2.4103097087628,17.555631534552,5.81207703394933));
#272444=CARTESIAN_POINT('Origin',(2.4103097087628,3.06591104035337,1.49207703394933));
#272445=CARTESIAN_POINT('',(-53.7090169915742,17.555631534552,5.81207703394933));
#272446=CARTESIAN_POINT('Origin',(-53.7090169915742,17.555631534552,-2.82792296605067));
#272447=CARTESIAN_POINT('',(-9.2313702912372,20.5619110403534,-2.82792296605067));
#272448=CARTESIAN_POINT('',(-9.2313702912372,17.555631534552,-2.82792296605067));
#272449=CARTESIAN_POINT('',(2.4103097087628,20.5619110403534,-2.82792296605067));
#272450=CARTESIAN_POINT('',(-53.7090169915742,20.5619110403534,-2.82792296605067));
#272451=CARTESIAN_POINT('',(2.4103097087628,17.555631534552,-2.82792296605067));
#272452=CARTESIAN_POINT('Origin',(-53.7090169915742,20.5619110403534,-2.82792296605067));
#272453=CARTESIAN_POINT('',(-9.2313702912372,20.5619110403534,5.81207703394933));
#272454=CARTESIAN_POINT('',(-9.2313702912372,20.5619110403534,-2.82792296605067));
#272455=CARTESIAN_POINT('',(2.4103097087628,20.5619110403534,5.81207703394933));
#272456=CARTESIAN_POINT('',(-53.7090169915742,20.5619110403534,5.81207703394933));
#272457=CARTESIAN_POINT('',(2.4103097087628,20.5619110403534,-2.82792296605067));
#272458=CARTESIAN_POINT('Origin',(-53.7090169915742,20.5619110403534,5.81207703394933));
#272459=CARTESIAN_POINT('',(-9.2313702912372,20.5619110403534,5.81207703394933));
#272460=CARTESIAN_POINT('',(2.4103097087628,20.5619110403534,5.81207703394933));
#272461=CARTESIAN_POINT('Origin',(2.4103097087628,3.06591104035337,1.49207703394933));
#272462=CARTESIAN_POINT('Origin',(-9.2313702912372,3.06591104035337,1.49207703394933));
#272463=CARTESIAN_POINT('',(0.,0.,0.));
#272464=CARTESIAN_POINT('Origin',(4.42504848420342,-17.542318193471,0.972561099047131));
#272465=CARTESIAN_POINT('',(4.76104848420342,-17.542318193471,26.5085610990471));
#272466=CARTESIAN_POINT('Origin',(4.76104848420342,-17.542318193471,0.972561099047131));
#272467=CARTESIAN_POINT('',(4.42504848420342,-17.542318193471,26.1725610990471));
#272468=CARTESIAN_POINT('Origin',(4.42504848420342,-17.542318193471,26.5085610990471));
#272469=CARTESIAN_POINT('Origin',(4.42504848420342,-17.542318193471,0.972561099047131));
#272470=CARTESIAN_POINT('Origin',(-3.14818151579658,-17.542318193471,0.972561099047131));
#272471=CARTESIAN_POINT('',(-3.14818151579658,-17.542318193471,26.1725610990471));
#272472=CARTESIAN_POINT('',(-3.14818151579658,-17.542318193471,26.1725610990471));
#272473=CARTESIAN_POINT('Origin',(-3.14818151579658,-17.542318193471,0.972561099047131));
#272474=CARTESIAN_POINT('Origin',(11.5520284842034,30.3696711225593,-7.21027454921227));
#272475=CARTESIAN_POINT('',(11.5201159294504,29.2525234772273,18.3766132024512));
#272476=CARTESIAN_POINT('',(10.1651884842034,34.038690149408,18.1368188355985));
#272477=CARTESIAN_POINT('Ctrl Pts',(11.5201159294506,29.2525234772274,18.3766132024512));
#272478=CARTESIAN_POINT('Ctrl Pts',(11.5064953958128,29.4369831852153,18.3846668872306));
#272479=CARTESIAN_POINT('Ctrl Pts',(11.4885385348232,29.6214916739098,18.3907232698498));
#272480=CARTESIAN_POINT('Ctrl Pts',(11.2877548088084,31.2852685491064,18.427357082409));
#272481=CARTESIAN_POINT('Ctrl Pts',(10.8383054247332,32.7235821608133,18.3271821312736));
#272482=CARTESIAN_POINT('Ctrl Pts',(10.1651884842031,34.0386901494087,18.1368188355984));
#272483=CARTESIAN_POINT('',(6.14788848420341,34.038690149408,18.1368188355985));
#272484=CARTESIAN_POINT('',(8.15653848420341,34.038690149408,18.1368188355985));
#272485=CARTESIAN_POINT('',(4.79296103895619,29.2525234772273,18.3766132024512));
#272486=CARTESIAN_POINT('Ctrl Pts',(6.14788848420342,34.038690149408,18.1368188355985));
#272487=CARTESIAN_POINT('Ctrl Pts',(6.12358695752486,33.9912108334888,18.1436915176392));
#272488=CARTESIAN_POINT('Ctrl Pts',(6.099576183545,33.9435659759386,18.1504519561046));
#272489=CARTESIAN_POINT('Ctrl Pts',(5.43709796638902,32.6082554610184,18.3360613630301));
#272490=CARTESIAN_POINT('Ctrl Pts',(5.01156238585602,31.2076315268735,18.427677818826));
#272491=CARTESIAN_POINT('Ctrl Pts',(4.82218298524757,29.5970927300154,18.3899136899737));
#272492=CARTESIAN_POINT('Ctrl Pts',(4.80568122363092,29.4247899693517,18.3841345199289));
#272493=CARTESIAN_POINT('Ctrl Pts',(4.79296103895619,29.2525234772273,18.3766132024512));
#272494=CARTESIAN_POINT('',(11.5520284842034,29.2525234772273,18.3766132024512));
#272495=CARTESIAN_POINT('Origin',(11.5520284842034,-65.4543075095013,-7.2102745492126));
#272496=CARTESIAN_POINT('',(10.1651884842034,-69.1233265363501,18.1368188355982));
#272497=CARTESIAN_POINT('',(11.520115929451,-64.3371598641695,18.3766132024509));
#272498=CARTESIAN_POINT('Ctrl Pts',(10.1651884842034,-69.1233265363502,
18.1368188355982));
#272499=CARTESIAN_POINT('Ctrl Pts',(10.189490010882,-69.0758472204308,18.1436915176389));
#272500=CARTESIAN_POINT('Ctrl Pts',(10.2135007848619,-69.0282023628806,
18.1504519561043));
#272501=CARTESIAN_POINT('Ctrl Pts',(10.8759790020178,-67.6928918479604,
18.3360613630298));
#272502=CARTESIAN_POINT('Ctrl Pts',(11.3015145825508,-66.2922679138155,
18.4276778188257));
#272503=CARTESIAN_POINT('Ctrl Pts',(11.4908939831593,-64.6817291169574,
18.3899136899734));
#272504=CARTESIAN_POINT('Ctrl Pts',(11.5073957447759,-64.5094263562938,
18.3841345199286));
#272505=CARTESIAN_POINT('Ctrl Pts',(11.5201159294506,-64.3371598641694,
18.3766132024509));
#272506=CARTESIAN_POINT('',(4.79296103895619,-64.3371598641695,18.3766132024509));
#272507=CARTESIAN_POINT('',(11.5520284842034,-64.3371598641695,18.3766132024509));
#272508=CARTESIAN_POINT('',(6.14788848420341,-69.1233265363501,18.1368188355982));
#272509=CARTESIAN_POINT('Ctrl Pts',(4.79296103895619,-64.3371598641695,
18.3766132024509));
#272510=CARTESIAN_POINT('Ctrl Pts',(4.80658157259404,-64.5216195721574,
18.3846668872303));
#272511=CARTESIAN_POINT('Ctrl Pts',(4.8245384335836,-64.7061280608519,18.3907232698495));
#272512=CARTESIAN_POINT('Ctrl Pts',(5.02532215959842,-66.3699049360485,
18.4273570824086));
#272513=CARTESIAN_POINT('Ctrl Pts',(5.47477154367356,-67.8082185477554,
18.3271821312732));
#272514=CARTESIAN_POINT('Ctrl Pts',(6.14788848420374,-69.1233265363508,
18.1368188355981));
#272515=CARTESIAN_POINT('',(8.15653848420341,-69.1233265363501,18.1368188355982));
#272516=CARTESIAN_POINT('Origin',(11.5520284842034,-22.8798040147362,-49.8102242737207));
#272517=CARTESIAN_POINT('',(11.5520284842034,-19.9972458266101,-48.0680189924834));
#272518=CARTESIAN_POINT('',(11.5520284842034,-25.3371465446537,-47.5067728111188));
#272519=CARTESIAN_POINT('Origin',(11.5520284842034,-22.8798040147362,-49.8102242737207));
#272520=CARTESIAN_POINT('',(11.5201159294503,-25.8673877784838,-48.2549866055504));
#272521=CARTESIAN_POINT('Ctrl Pts',(11.5520284842034,-25.3371465446537,
-47.5067728111188));
#272522=CARTESIAN_POINT('Ctrl Pts',(11.5520284842034,-25.4218077136364,
-47.5970901000009));
#272523=CARTESIAN_POINT('Ctrl Pts',(11.5505455276579,-25.5014883801418,
-47.6920685179292));
#272524=CARTESIAN_POINT('Ctrl Pts',(11.5472515368861,-25.5758260890567,
-47.7913393065626));
#272525=CARTESIAN_POINT('Ctrl Pts',(11.5440442061753,-25.6482080819925,
-47.8879984264961));
#272526=CARTESIAN_POINT('Ctrl Pts',(11.539119436029,-25.7155242765753,-47.9887269871974));
#272527=CARTESIAN_POINT('Ctrl Pts',(11.532206799367,-25.7774102007914,-48.0931625380847));
#272528=CARTESIAN_POINT('Ctrl Pts',(11.5286984812716,-25.8088186948865,
-48.1461659217282));
#272529=CARTESIAN_POINT('Ctrl Pts',(11.5246786952113,-25.8388280077787,
-48.2001237964755));
#272530=CARTESIAN_POINT('Ctrl Pts',(11.5201159294506,-25.8673877784838,
-48.2549866055504));
#272531=CARTESIAN_POINT('',(4.79296103895619,-25.8673877784838,-48.2549866055504));
#272532=CARTESIAN_POINT('',(11.5520284842034,-25.8673877784838,-48.2549866055504));
#272533=CARTESIAN_POINT('',(4.76104848420342,-25.3371465446537,-47.5067728111188));
#272534=CARTESIAN_POINT('Ctrl Pts',(4.79296103895619,-25.8673877784838,
-48.2549866055504));
#272535=CARTESIAN_POINT('Ctrl Pts',(4.77035892158038,-25.725914092661,-47.9832181836481));
#272536=CARTESIAN_POINT('Ctrl Pts',(4.76104848420342,-25.5477399600458,
-47.7314357417538));
#272537=CARTESIAN_POINT('Ctrl Pts',(4.76104848420342,-25.3371465446537,
-47.5067728111189));
#272538=CARTESIAN_POINT('',(4.76104848420342,-19.9972458266101,-48.0680189924834));
#272539=CARTESIAN_POINT('Origin',(4.76104848420342,-22.8798040147362,-49.8102242737207));
#272540=CARTESIAN_POINT('',(4.79296103895619,-19.6341540310225,-48.9101258718094));
#272541=CARTESIAN_POINT('Ctrl Pts',(4.76104848420342,-19.9972458266101,
-48.0680189924834));
#272542=CARTESIAN_POINT('Ctrl Pts',(4.76104848420342,-19.933217960153,-48.1739560210942));
#272543=CARTESIAN_POINT('Ctrl Pts',(4.76253119975839,-19.8750297749198,
-48.2834165710042));
#272544=CARTESIAN_POINT('Ctrl Pts',(4.76582464685228,-19.8229591767546,
-48.3959644781904));
#272545=CARTESIAN_POINT('Ctrl Pts',(4.76903141935803,-19.7722589353985,
-48.505550429947));
#272546=CARTESIAN_POINT('Ctrl Pts',(4.773955313379,-19.7273587788838,-48.618063270801));
#272547=CARTESIAN_POINT('Ctrl Pts',(4.78086668106801,-19.6885398848474,
-48.7330726175708));
#272548=CARTESIAN_POINT('Ctrl Pts',(4.78437582490195,-19.6688301705364,
-48.7914668975778));
#272549=CARTESIAN_POINT('Ctrl Pts',(4.78839676418624,-19.6506885493468,
-48.8505043248586));
#272550=CARTESIAN_POINT('Ctrl Pts',(4.79296103895619,-19.6341540310225,
-48.9101258718095));
#272551=CARTESIAN_POINT('',(11.520115929451,-19.6341540310225,-48.9101258718094));
#272552=CARTESIAN_POINT('',(11.5520284842034,-19.6341540310225,-48.9101258718094));
#272553=CARTESIAN_POINT('Ctrl Pts',(11.5201159294506,-19.6341540310225,
-48.9101258718094));
#272554=CARTESIAN_POINT('Ctrl Pts',(11.5379482942249,-19.6987534640074,
-48.677187841734));
#272555=CARTESIAN_POINT('Ctrl Pts',(11.5475950755165,-19.7884941430255,
-48.4509138861737));
#272556=CARTESIAN_POINT('Ctrl Pts',(11.5516325551658,-19.9325572097809,
-48.1785764633217));
#272557=CARTESIAN_POINT('Ctrl Pts',(11.5520284842034,-19.9641379606009,
-48.1227974685242));
#272558=CARTESIAN_POINT('Ctrl Pts',(11.5520284842034,-19.9972458266101,
-48.0680189924834));
#272559=CARTESIAN_POINT('Origin',(11.5520284842034,-33.3215019147798,-47.5907728700904));
#272560=CARTESIAN_POINT('',(11.5520284842034,-30.139709693315,-46.4859565010363));
#272561=CARTESIAN_POINT('',(11.5520284842034,-35.2462311262936,-44.8267471082261));
#272562=CARTESIAN_POINT('Origin',(11.5520284842034,-33.3215019147798,-47.5907728700904));
#272563=CARTESIAN_POINT('',(11.5201159294502,-35.920447712068,-45.4483672846184));
#272564=CARTESIAN_POINT('Ctrl Pts',(11.5520284842034,-35.2462311262936,
-44.8267471082261));
#272565=CARTESIAN_POINT('Ctrl Pts',(11.5520284842034,-35.3478213939342,
-44.8974894864019));
#272566=CARTESIAN_POINT('Ctrl Pts',(11.5505454949267,-35.4455089937706,
-44.9738267449025));
#272567=CARTESIAN_POINT('Ctrl Pts',(11.5472514286393,-35.5388627267499,
-45.0554735553234));
#272568=CARTESIAN_POINT('Ctrl Pts',(11.5440440212189,-35.6297605502186,
-45.1349724368738));
#272569=CARTESIAN_POINT('Ctrl Pts',(11.539119130381,-35.7165492567715,-45.2195051912617));
#272570=CARTESIAN_POINT('Ctrl Pts',(11.5322063173366,-35.7987969833134,
-45.3087930763808));
#272571=CARTESIAN_POINT('Ctrl Pts',(11.5286981135764,-35.8405371232053,
-45.3541060469908));
#272572=CARTESIAN_POINT('Ctrl Pts',(11.5246784869469,-35.8811072172304,
-45.4006434481913));
#272573=CARTESIAN_POINT('Ctrl Pts',(11.5201159294506,-35.9204477120681,
-45.4483672846184));
#272574=CARTESIAN_POINT('',(4.79296103895619,-35.920447712068,-45.4483672846184));
#272575=CARTESIAN_POINT('',(11.5520284842034,-35.920447712068,-45.4483672846184));
#272576=CARTESIAN_POINT('',(4.76104848420342,-35.2462311262936,-44.8267471082261));
#272577=CARTESIAN_POINT('Ctrl Pts',(4.79296103895618,-35.920447712068,-45.4483672846184));
#272578=CARTESIAN_POINT('Ctrl Pts',(4.77035892158034,-35.7255617336046,
-45.2119516880047));
#272579=CARTESIAN_POINT('Ctrl Pts',(4.76104848420342,-35.4989326200616,
-45.002715781731));
#272580=CARTESIAN_POINT('Ctrl Pts',(4.76104848420342,-35.2462311262936,
-44.8267471082261));
#272581=CARTESIAN_POINT('',(4.76104848420342,-30.139709693315,-46.4859565010363));
#272582=CARTESIAN_POINT('Origin',(4.76104848420342,-33.3215019147798,-47.5907728700904));
#272583=CARTESIAN_POINT('',(4.79296103895619,-29.9596361897448,-47.3851523537532));
#272584=CARTESIAN_POINT('Ctrl Pts',(4.76104848420342,-30.139709693315,-46.4859565010363));
#272585=CARTESIAN_POINT('Ctrl Pts',(4.76104848420342,-30.0991044446722,
-46.6028967165337));
#272586=CARTESIAN_POINT('Ctrl Pts',(4.76253135162959,-30.0649445444981,
-46.7220693473933));
#272587=CARTESIAN_POINT('Ctrl Pts',(4.76582514301997,-30.0374111372492,
-46.8429900493133));
#272588=CARTESIAN_POINT('Ctrl Pts',(4.76903226819381,-30.0106021888235,
-46.9607290865517));
#272589=CARTESIAN_POINT('Ctrl Pts',(4.7739567160318,-29.990075838413,-47.080125258691));
#272590=CARTESIAN_POINT('Ctrl Pts',(4.78086888743444,-29.9760176360285,
-47.2006991758224));
#272591=CARTESIAN_POINT('Ctrl Pts',(4.78437750874215,-29.9688816861856,
-47.2619025502989));
#272592=CARTESIAN_POINT('Ctrl Pts',(4.78839771848159,-29.9634125828066,
-47.3234088729724));
#272593=CARTESIAN_POINT('Ctrl Pts',(4.79296103895619,-29.9596361897448,
-47.3851523537532));
#272594=CARTESIAN_POINT('',(11.520115929451,-29.9596361897448,-47.3851523537532));
#272595=CARTESIAN_POINT('',(11.5520284842034,-29.9596361897448,-47.3851523537532));
#272596=CARTESIAN_POINT('Ctrl Pts',(11.5201159294506,-29.9596361897448,
-47.3851523537531));
#272597=CARTESIAN_POINT('Ctrl Pts',(11.5379482942249,-29.974393430439,-47.1438736011772));
#272598=CARTESIAN_POINT('Ctrl Pts',(11.5475950755165,-30.0151280596203,
-46.9038861381276));
#272599=CARTESIAN_POINT('Ctrl Pts',(11.5516325551658,-30.0994208686632,
-46.6075475455815));
#272600=CARTESIAN_POINT('Ctrl Pts',(11.5520284842034,-30.1187143991867,
-46.5464214483487));
#272601=CARTESIAN_POINT('Ctrl Pts',(11.5520284842034,-30.139709693315,-46.4859565010363));
#272602=CARTESIAN_POINT('Origin',(11.5520284842034,-51.7098072425568,-36.9742798391576));
#272603=CARTESIAN_POINT('',(11.5520284842034,-48.3537261103108,-37.2591313508023));
#272604=CARTESIAN_POINT('',(11.5520284842034,-52.3439043111715,-33.6663587612783));
#272605=CARTESIAN_POINT('Origin',(11.5520284842034,-51.7098072425568,-36.9742798391576));
#272606=CARTESIAN_POINT('',(11.520115929451,-53.212667514387,-33.9600084589965));
#272607=CARTESIAN_POINT('Ctrl Pts',(11.5520284842034,-52.3439043111714,
-33.6663587612783));
#272608=CARTESIAN_POINT('Ctrl Pts',(11.5520284842034,-52.4654852159812,
-33.6896646665657));
#272609=CARTESIAN_POINT('Ctrl Pts',(11.5505454934861,-52.585776508724,-33.7196691161155));
#272610=CARTESIAN_POINT('Ctrl Pts',(11.5472514229146,-52.7042682136749,
-33.7562868369326));
#272611=CARTESIAN_POINT('Ctrl Pts',(11.5440440116043,-52.8196426801257,
-33.7919412315054));
#272612=CARTESIAN_POINT('Ctrl Pts',(11.5391191144802,-52.9333107492123,
-33.8338656362247));
#272613=CARTESIAN_POINT('Ctrl Pts',(11.5322062913588,-53.0447645176165,
-33.8819810649254));
#272614=CARTESIAN_POINT('Ctrl Pts',(11.5286980938785,-53.1013263336234,
-33.9063992256053));
#272615=CARTESIAN_POINT('Ctrl Pts',(11.5246784758733,-53.1573172853413,
-33.9324118527927));
#272616=CARTESIAN_POINT('Ctrl Pts',(11.5201159294506,-53.212667514387,-33.9600084589965));
#272617=CARTESIAN_POINT('',(4.79296103895619,-53.212667514387,-33.9600084589965));
#272618=CARTESIAN_POINT('',(11.5520284842034,-53.212667514387,-33.9600084589965));
#272619=CARTESIAN_POINT('',(4.76104848420342,-52.3439043111715,-33.6663587612783));
#272620=CARTESIAN_POINT('Ctrl Pts',(4.79296103895618,-53.212667514387,-33.9600084589965));
#272621=CARTESIAN_POINT('Ctrl Pts',(4.77035892157491,-52.9384714278002,
-33.8232993332241));
#272622=CARTESIAN_POINT('Ctrl Pts',(4.76104848420342,-52.6463315204171,
-33.7243311863565));
#272623=CARTESIAN_POINT('Ctrl Pts',(4.76104848420342,-52.3439043111715,
-33.6663587612783));
#272624=CARTESIAN_POINT('',(4.76104848420342,-48.3537261103108,-37.2591313508023));
#272625=CARTESIAN_POINT('Origin',(4.76104848420342,-51.7098072425568,-36.9742798391576));
#272626=CARTESIAN_POINT('',(4.79296103895619,-48.5549566816842,-38.1538301299319));
#272627=CARTESIAN_POINT('Ctrl Pts',(4.76104848420342,-48.3537261103108,
-37.2591313508023));
#272628=CARTESIAN_POINT('Ctrl Pts',(4.76104848420342,-48.3641956404984,
-37.382481908162));
#272629=CARTESIAN_POINT('Ctrl Pts',(4.76253146428112,-48.3814617755203,
-37.5052501260783));
#272630=CARTESIAN_POINT('Ctrl Pts',(4.76582551084937,-48.405493015206,-37.6269199042606));
#272631=CARTESIAN_POINT('Ctrl Pts',(4.76903289751466,-48.4288920401198,
-37.74538878927));
#272632=CARTESIAN_POINT('Ctrl Pts',(4.77395775595718,-48.4587050452691,
-37.8628160339725));
#272633=CARTESIAN_POINT('Ctrl Pts',(4.78087052305202,-48.4949065665866,
-37.9786882576892));
#272634=CARTESIAN_POINT('Ctrl Pts',(4.78437875699289,-48.5132788629558,
-38.0374934890054));
#272635=CARTESIAN_POINT('Ctrl Pts',(4.78839842591371,-48.5332966106966,
-38.0958976385085));
#272636=CARTESIAN_POINT('Ctrl Pts',(4.79296103895619,-48.5549566816842,
-38.1538301299319));
#272637=CARTESIAN_POINT('',(11.5201159294503,-48.5549566816842,-38.1538301299319));
#272638=CARTESIAN_POINT('',(11.5520284842034,-48.5549566816842,-38.1538301299319));
#272639=CARTESIAN_POINT('Ctrl Pts',(11.5201159294506,-48.5549566816842,
-38.1538301299319));
#272640=CARTESIAN_POINT('Ctrl Pts',(11.5379482942249,-48.4703011820194,
-37.9274087109495));
#272641=CARTESIAN_POINT('Ctrl Pts',(11.5475950755165,-48.4099024223757,
-37.6916009878592));
#272642=CARTESIAN_POINT('Ctrl Pts',(11.5516325551658,-48.3663759708428,
-37.386597238529));
#272643=CARTESIAN_POINT('Ctrl Pts',(11.5520284842034,-48.3591392644216,
-37.3229083842203));
#272644=CARTESIAN_POINT('Ctrl Pts',(11.5520284842034,-48.3537261103108,
-37.2591313508023));
#272645=CARTESIAN_POINT('Origin',(11.5520284842034,-43.0735737692781,-43.2488707392779));
#272646=CARTESIAN_POINT('',(11.5520284842034,-39.7316071024856,-42.8297290592317));
#272647=CARTESIAN_POINT('',(11.5520284842034,-44.3815697599695,-40.1450718672117));
#272648=CARTESIAN_POINT('Origin',(11.5520284842034,-43.0735737692781,-43.2488707392779));
#272649=CARTESIAN_POINT('',(11.5201159294502,-45.1702951976398,-40.6129306409918));
#272650=CARTESIAN_POINT('Ctrl Pts',(11.5520284842034,-44.3815697599695,
-40.1450718672117));
#272651=CARTESIAN_POINT('Ctrl Pts',(11.5520284842034,-44.4956485670534,
-40.1931467033848));
#272652=CARTESIAN_POINT('Ctrl Pts',(11.5505454855483,-44.6070732101029,
-40.2475056052893));
#272653=CARTESIAN_POINT('Ctrl Pts',(11.5472513973451,-44.7153625908673,
-40.3079591348944));
#272654=CARTESIAN_POINT('Ctrl Pts',(11.5440439677953,-44.8208031675502,
-40.3668222937663));
#272655=CARTESIAN_POINT('Ctrl Pts',(11.5391190420915,-44.9232710031711,
-40.4314636981042));
#272656=CARTESIAN_POINT('Ctrl Pts',(11.5322061778344,-45.0222857184828,
-40.5017004896391));
#272657=CARTESIAN_POINT('Ctrl Pts',(11.5286980071981,-45.0725341399615,
-40.5373445642926));
#272658=CARTESIAN_POINT('Ctrl Pts',(11.5246784267181,-45.1218926824322,
-40.5744295419386));
#272659=CARTESIAN_POINT('Ctrl Pts',(11.5201159294506,-45.1702951976399,
-40.6129306409918));
#272660=CARTESIAN_POINT('',(4.79296103895619,-45.1702951976398,-40.6129306409918));
#272661=CARTESIAN_POINT('',(11.5520284842034,-45.1702951976398,-40.6129306409918));
#272662=CARTESIAN_POINT('',(4.76104848420342,-44.3815697599695,-40.1450718672117));
#272663=CARTESIAN_POINT('Ctrl Pts',(4.79296103895618,-45.1702951976398,
-40.6129306409918));
#272664=CARTESIAN_POINT('Ctrl Pts',(4.77035892157484,-44.9305143789032,
-40.4222003656407));
#272665=CARTESIAN_POINT('Ctrl Pts',(4.76104848420342,-44.66533506417,-40.2646556081339));
#272666=CARTESIAN_POINT('Ctrl Pts',(4.76104848420342,-44.3815697599695,
-40.1450718672118));
#272667=CARTESIAN_POINT('',(4.76104848420342,-39.7316071024856,-42.8297290592317));
#272668=CARTESIAN_POINT('Origin',(4.76104848420342,-43.0735737692781,-43.2488707392779));
#272669=CARTESIAN_POINT('',(4.79296103895619,-39.7424219671274,-43.7467147117553));
#272670=CARTESIAN_POINT('Ctrl Pts',(4.76104848420342,-39.7316071024856,
-42.8297290592317));
#272671=CARTESIAN_POINT('Ctrl Pts',(4.76104848420342,-39.7162020260021,
-42.952559249018));
#272672=CARTESIAN_POINT('Ctrl Pts',(4.7625314258757,-39.7075659332827,-43.0762329497052));
#272673=CARTESIAN_POINT('Ctrl Pts',(4.76582538552449,-39.7057753139107,
-43.2002387723342));
#272674=CARTESIAN_POINT('Ctrl Pts',(4.76903268308154,-39.7040318046544,
-43.3209820765593));
#272675=CARTESIAN_POINT('Ctrl Pts',(4.77395740161558,-39.708778498989,-43.4420400564706));
#272676=CARTESIAN_POINT('Ctrl Pts',(4.78086996580659,-39.7200972254492,
-43.5629052434041));
#272677=CARTESIAN_POINT('Ctrl Pts',(4.78437833171491,-39.7258418714215,
-43.6242485148189));
#272678=CARTESIAN_POINT('Ctrl Pts',(4.78839818488704,-39.7332795799699,
-43.6855415708931));
#272679=CARTESIAN_POINT('Ctrl Pts',(4.79296103895619,-39.7424219671274,
-43.7467147117553));
#272680=CARTESIAN_POINT('',(11.520115929451,-39.7424219671274,-43.7467147117553));
#272681=CARTESIAN_POINT('',(11.5520284842034,-39.7424219671274,-43.7467147117553));
#272682=CARTESIAN_POINT('Ctrl Pts',(11.5201159294506,-39.7424219671274,
-43.7467147117553));
#272683=CARTESIAN_POINT('Ctrl Pts',(11.5379482942249,-39.7066920532994,
-43.5076402759505));
#272684=CARTESIAN_POINT('Ctrl Pts',(11.5475950755165,-39.6966403338822,
-43.2644279091345));
#272685=CARTESIAN_POINT('Ctrl Pts',(11.5516325551658,-39.7174788849758,
-42.9570395653788));
#272686=CARTESIAN_POINT('Ctrl Pts',(11.5520284842034,-39.7236419753383,
-42.8932378694753));
#272687=CARTESIAN_POINT('Ctrl Pts',(11.5520284842034,-39.7316071024856,
-42.8297290592317));
#272688=CARTESIAN_POINT('Origin',(11.5520284842034,-64.1902433118534,-19.7964332737817));
#272689=CARTESIAN_POINT('',(11.5520284842034,-63.4240670938145,-16.5165864857723));
#272690=CARTESIAN_POINT('',(11.5201159294509,-64.3371598641692,-16.4314910043572));
#272691=CARTESIAN_POINT('Ctrl Pts',(11.5520284842034,-63.4240670938102,
-16.5165864857733));
#272692=CARTESIAN_POINT('Ctrl Pts',(11.5520284842035,-63.6673411199273,
-16.4597573759625));
#272693=CARTESIAN_POINT('Ctrl Pts',(11.5459435973759,-63.9165045298839,
-16.430089037035));
#272694=CARTESIAN_POINT('Ctrl Pts',(11.5280276651045,-64.2239049548286,
-16.4279739330299));
#272695=CARTESIAN_POINT('Ctrl Pts',(11.5242910209322,-64.2806175747128,
-16.4290223146854));
#272696=CARTESIAN_POINT('Ctrl Pts',(11.5201159294506,-64.3371598641692,
-16.4314910043572));
#272697=CARTESIAN_POINT('',(4.79296103895619,-64.3371598641692,-16.4314910043572));
#272698=CARTESIAN_POINT('',(11.5520284842034,-64.3371598641692,-16.4314910043572));
#272699=CARTESIAN_POINT('',(4.76104848420342,-63.4240670938145,-16.5165864857723));
#272700=CARTESIAN_POINT('Ctrl Pts',(4.79296103895618,-64.3371598641692,
-16.4314910043572));
#272701=CARTESIAN_POINT('Ctrl Pts',(4.77035892158601,-64.0310646640203,
-16.418126599299));
#272702=CARTESIAN_POINT('Ctrl Pts',(4.76104848420348,-63.7239276068057,
-16.446538703473));
#272703=CARTESIAN_POINT('Ctrl Pts',(4.76104848420342,-63.4240670938177,
-16.5165864857716));
#272704=CARTESIAN_POINT('',(4.76104848420342,-61.2401701856314,-21.4216992519672));
#272705=CARTESIAN_POINT('Origin',(4.76104848420342,-64.1902433118534,-19.7964332737817));
#272706=CARTESIAN_POINT('',(4.79296103895619,-61.7879102380356,-22.1571994105147));
#272707=CARTESIAN_POINT('Ctrl Pts',(4.76104848420342,-61.2401701856314,
-21.4216992519672));
#272708=CARTESIAN_POINT('Ctrl Pts',(4.76104848420342,-61.2999060970774,
-21.5301278472817));
#272709=CARTESIAN_POINT('Ctrl Pts',(4.76253148048503,-61.3656142043588,
-21.6352599593845));
#272710=CARTESIAN_POINT('Ctrl Pts',(4.76582556303018,-61.4370558175347,
-21.7366369273954));
#272711=CARTESIAN_POINT('Ctrl Pts',(4.76903298692,-61.5066179896073,-21.8353469337836));
#272712=CARTESIAN_POINT('Ctrl Pts',(4.77395790368722,-61.5816160066493,
-21.9304964980193));
#272713=CARTESIAN_POINT('Ctrl Pts',(4.78087075471546,-61.6618177977816,
-22.0216269866694));
#272714=CARTESIAN_POINT('Ctrl Pts',(4.78437893387933,-61.7025191309083,
-22.0678744871825));
#272715=CARTESIAN_POINT('Ctrl Pts',(4.78839852622511,-61.7445604645742,
-22.1130863605567));
#272716=CARTESIAN_POINT('Ctrl Pts',(4.79296103895619,-61.7879102380356,
-22.1571994105147));
#272717=CARTESIAN_POINT('',(11.5201159294506,-61.7879102380356,-22.1571994105147));
#272718=CARTESIAN_POINT('',(11.5520284842034,-61.7879102380356,-22.1571994105147));
#272719=CARTESIAN_POINT('',(11.5520284842034,-61.2401701856314,-21.4216992519671));
#272720=CARTESIAN_POINT('Ctrl Pts',(11.5201159294506,-61.7879102380356,
-22.1571994105147));
#272721=CARTESIAN_POINT('Ctrl Pts',(11.5379482942249,-61.6184797029751,
-21.9847856454419));
#272722=CARTESIAN_POINT('Ctrl Pts',(11.5475950755165,-61.4673910487542,
-21.7939309598791));
#272723=CARTESIAN_POINT('Ctrl Pts',(11.5516325551658,-61.3035714555409,
-21.5329999728961));
#272724=CARTESIAN_POINT('Ctrl Pts',(11.5520284842034,-61.2710558044587,
-21.4777607430166));
#272725=CARTESIAN_POINT('Ctrl Pts',(11.5520284842034,-61.2401701856314,
-21.4216992519671));
#272726=CARTESIAN_POINT('Origin',(11.5520284842034,-64.1902433118534,-19.7964332737817));
#272727=CARTESIAN_POINT('Origin',(11.5520284842034,-58.8527574905876,-29.0412299008925));
#272728=CARTESIAN_POINT('',(11.5520284842034,-58.7852425524918,-25.6737586414698));
#272729=CARTESIAN_POINT('',(11.5201159294504,-59.6960744004836,-25.7803653622482));
#272730=CARTESIAN_POINT('Ctrl Pts',(11.5520284842034,-58.7852425524873,
-25.6737586414699));
#272731=CARTESIAN_POINT('Ctrl Pts',(11.5520284842035,-59.0350158937629,
-25.6687508981586));
#272732=CARTESIAN_POINT('Ctrl Pts',(11.5459435973759,-59.2849028799128,
-25.6915348694728));
#272733=CARTESIAN_POINT('Ctrl Pts',(11.5280276651045,-59.5860256228871,
-25.7533781276734));
#272734=CARTESIAN_POINT('Ctrl Pts',(11.5242910209322,-59.6412809651556,
-25.7661948163652));
#272735=CARTESIAN_POINT('Ctrl Pts',(11.5201159294506,-59.6960744004836,
-25.7803653622482));
#272736=CARTESIAN_POINT('',(4.79296103895619,-59.6960744004836,-25.7803653622482));
#272737=CARTESIAN_POINT('',(11.5520284842034,-59.6960744004836,-25.7803653622482));
#272738=CARTESIAN_POINT('',(4.76104848420342,-58.7852425524918,-25.6737586414698));
#272739=CARTESIAN_POINT('Ctrl Pts',(4.79296103895618,-59.6960744004836,
-25.7803653622482));
#272740=CARTESIAN_POINT('Ctrl Pts',(4.77035892158043,-59.399446730841,-25.7036522308722));
#272741=CARTESIAN_POINT('Ctrl Pts',(4.76104848420348,-59.0931141466079,
-25.6675860775439));
#272742=CARTESIAN_POINT('Ctrl Pts',(4.76104848420342,-58.785242552495,-25.6737586414697));
#272743=CARTESIAN_POINT('',(4.76104848420342,-55.6292387426312,-30.0176252263));
#272744=CARTESIAN_POINT('Origin',(4.76104848420342,-58.8527574905876,-29.0412299008925));
#272745=CARTESIAN_POINT('',(4.79296103895619,-56.0120902791558,-30.8509345021466));
#272746=CARTESIAN_POINT('Ctrl Pts',(4.76104848420342,-55.6292387426312,
-30.0176252263));
#272747=CARTESIAN_POINT('Ctrl Pts',(4.76104848420342,-55.6651257148422,
-30.1361042119314));
#272748=CARTESIAN_POINT('Ctrl Pts',(4.76253148100061,-55.7075397574459,
-30.2526004442625));
#272749=CARTESIAN_POINT('Ctrl Pts',(4.76582556519912,-55.7563427586828,
-30.3666156575337));
#272750=CARTESIAN_POINT('Ctrl Pts',(4.76903299054489,-55.803861878925,-30.477631424834));
#272751=CARTESIAN_POINT('Ctrl Pts',(4.77395790968286,-55.8574383198187,
-30.5862947331828));
#272752=CARTESIAN_POINT('Ctrl Pts',(4.7808707646055,-55.9169404382669,-30.6921087199474));
#272753=CARTESIAN_POINT('Ctrl Pts',(4.78437894136648,-55.9471369274894,
-30.7458078317481));
#272754=CARTESIAN_POINT('Ctrl Pts',(4.78839853042556,-55.9788594516498,
-30.7987725514947));
#272755=CARTESIAN_POINT('Ctrl Pts',(4.79296103895619,-56.0120902791558,
-30.8509345021466));
#272756=CARTESIAN_POINT('',(11.5201159294502,-56.0120902791558,-30.8509345021466));
#272757=CARTESIAN_POINT('',(11.5520284842034,-56.0120902791558,-30.8509345021466));
#272758=CARTESIAN_POINT('',(11.5520284842034,-55.6292387426312,-30.0176252263));
#272759=CARTESIAN_POINT('Ctrl Pts',(11.5201159294506,-56.0120902791558,
-30.8509345021466));
#272760=CARTESIAN_POINT('Ctrl Pts',(11.5379482942249,-55.8822090452119,
-30.6470618024867));
#272761=CARTESIAN_POINT('Ctrl Pts',(11.5475950755165,-55.7741029609635,
-30.4289646521523));
#272762=CARTESIAN_POINT('Ctrl Pts',(11.5516325551658,-55.6681138215991,
-30.1396756246635));
#272763=CARTESIAN_POINT('Ctrl Pts',(11.5520284842034,-55.6477935971904,
-30.0788831204959));
#272764=CARTESIAN_POINT('Ctrl Pts',(11.5520284842034,-55.6292387426312,
-30.0176252262999));
#272765=CARTESIAN_POINT('Origin',(11.5520284842034,-58.8527574905876,-29.0412299008925));
#272766=CARTESIAN_POINT('Origin',(11.5520284842034,23.7681211036462,-29.0412299008916));
#272767=CARTESIAN_POINT('',(11.520115929451,24.6114380135421,-25.7803653622474));
#272768=CARTESIAN_POINT('',(11.5520284842034,23.7006061655503,-25.6737586414689));
#272769=CARTESIAN_POINT('Ctrl Pts',(11.5201159294506,24.6114380135421,-25.7803653622474));
#272770=CARTESIAN_POINT('Ctrl Pts',(11.5379482942249,24.3774080454967,-25.7198410972446));
#272771=CARTESIAN_POINT('Ctrl Pts',(11.5475950755165,24.1365787122577,-25.6844218272471));
#272772=CARTESIAN_POINT('Ctrl Pts',(11.5516325551658,23.8286960522908,-25.6730153913783));
#272773=CARTESIAN_POINT('Ctrl Pts',(11.5520284842034,23.7645996503902,-25.6724756264602));
#272774=CARTESIAN_POINT('Ctrl Pts',(11.5520284842034,23.7006061655553,-25.6737586414688));
#272775=CARTESIAN_POINT('',(11.5520284842034,20.5446023556898,-30.0176252262992));
#272776=CARTESIAN_POINT('Origin',(11.5520284842034,23.7681211036462,-29.0412299008916));
#272777=CARTESIAN_POINT('',(11.5201159294503,20.9274538922144,-30.8509345021458));
#272778=CARTESIAN_POINT('Ctrl Pts',(11.5520284842034,20.5446023556898,-30.0176252262992));
#272779=CARTESIAN_POINT('Ctrl Pts',(11.5520284842034,20.5804893279013,-30.1361042119321));
#272780=CARTESIAN_POINT('Ctrl Pts',(11.5505454874062,20.6229033705057,-30.2526004442646));
#272781=CARTESIAN_POINT('Ctrl Pts',(11.5472514032076,20.6717063717434,-30.3666156575372));
#272782=CARTESIAN_POINT('Ctrl Pts',(11.5440439778617,20.7192254919869,-30.4776314248403));
#272783=CARTESIAN_POINT('Ctrl Pts',(11.5391190587235,20.7728019328823,-30.5862947331918));
#272784=CARTESIAN_POINT('Ctrl Pts',(11.5322062038005,20.8323040513325,-30.6921087199588));
#272785=CARTESIAN_POINT('Ctrl Pts',(11.5286980270397,20.8625005405529,-30.7458078317553));
#272786=CARTESIAN_POINT('Ctrl Pts',(11.5246784379809,20.894223064711,-30.7987725514979));
#272787=CARTESIAN_POINT('Ctrl Pts',(11.5201159294506,20.9274538922145,-30.8509345021458));
#272788=CARTESIAN_POINT('',(4.79296103895619,20.9274538922144,-30.8509345021458));
#272789=CARTESIAN_POINT('',(11.5520284842034,20.9274538922144,-30.8509345021458));
#272790=CARTESIAN_POINT('',(4.76104848420342,20.5446023556898,-30.0176252262992));
#272791=CARTESIAN_POINT('Ctrl Pts',(4.79296103895619,20.9274538922145,-30.8509345021458));
#272792=CARTESIAN_POINT('Ctrl Pts',(4.77035892158035,20.7628323778119,-30.5925304853049));
#272793=CARTESIAN_POINT('Ctrl Pts',(4.76104848420342,20.6338694532122,-30.3123359392156));
#272794=CARTESIAN_POINT('Ctrl Pts',(4.76104848420342,20.5446023556898,-30.0176252262992));
#272795=CARTESIAN_POINT('',(4.76104848420342,23.7006061655503,-25.6737586414689));
#272796=CARTESIAN_POINT('Origin',(4.76104848420342,23.7681211036462,-29.0412299008916));
#272797=CARTESIAN_POINT('',(4.79296103895619,24.6114380135421,-25.7803653622474));
#272798=CARTESIAN_POINT('Ctrl Pts',(4.76104848420342,23.7006061655501,-25.6737586414689));
#272799=CARTESIAN_POINT('Ctrl Pts',(4.76104848420341,23.8861826621397,-25.6700379903589));
#272800=CARTESIAN_POINT('Ctrl Pts',(4.76439185786763,24.0720879013436,-25.6816555797029));
#272801=CARTESIAN_POINT('Ctrl Pts',(4.77719931294499,24.376417237712,-25.7262486108204));
#272802=CARTESIAN_POINT('Ctrl Pts',(4.78408071207329,24.4948935931612,-25.7502249257783));
#272803=CARTESIAN_POINT('Ctrl Pts',(4.79296103895618,24.6114380135421,-25.7803653622474));
#272804=CARTESIAN_POINT('',(11.5520284842034,24.6114380135421,-25.7803653622474));
#272805=CARTESIAN_POINT('Origin',(11.5520284842034,16.6251708556156,-36.9742798391569));
#272806=CARTESIAN_POINT('',(11.5520284842034,17.2592679242302,-33.6663587612776));
#272807=CARTESIAN_POINT('',(11.5520284842034,13.2690897233696,-37.2591313508016));
#272808=CARTESIAN_POINT('Origin',(11.5520284842034,16.6251708556156,-36.9742798391569));
#272809=CARTESIAN_POINT('',(11.5201159294504,13.470320294743,-38.1538301299313));
#272810=CARTESIAN_POINT('Ctrl Pts',(11.5520284842034,13.2690897233696,-37.2591313508016));
#272811=CARTESIAN_POINT('Ctrl Pts',(11.5520284842034,13.2795592535577,-37.3824819081667));
#272812=CARTESIAN_POINT('Ctrl Pts',(11.5505455041256,13.2968253885807,-37.5052501260884));
#272813=CARTESIAN_POINT('Ctrl Pts',(11.547251457557,13.320856628268,-37.6269199042761));
#272814=CARTESIAN_POINT('Ctrl Pts',(11.544044070892,13.3442556531797,-37.7453887892715));
#272815=CARTESIAN_POINT('Ctrl Pts',(11.53911921245,13.3740686583253,-37.8628160339603));
#272816=CARTESIAN_POINT('Ctrl Pts',(11.5322064453563,13.4102701796377,-37.9786882576637));
#272817=CARTESIAN_POINT('Ctrl Pts',(11.5286982114151,13.428642476009,-38.0374934889883));
#272818=CARTESIAN_POINT('Ctrl Pts',(11.5246785424938,13.4486602237524,-38.0958976384997));
#272819=CARTESIAN_POINT('Ctrl Pts',(11.5201159294506,13.470320294743,-38.1538301299313));
#272820=CARTESIAN_POINT('',(4.79296103895619,13.470320294743,-38.1538301299313));
#272821=CARTESIAN_POINT('',(11.5520284842034,13.470320294743,-38.1538301299313));
#272822=CARTESIAN_POINT('',(4.76104848420342,13.2690897233696,-37.2591313508017));
#272823=CARTESIAN_POINT('Ctrl Pts',(4.79296103895619,13.470320294743,-38.1538301299313));
#272824=CARTESIAN_POINT('Ctrl Pts',(4.77035892158041,13.3630213714567,-37.8668461234347));
#272825=CARTESIAN_POINT('Ctrl Pts',(4.76104848420342,13.2951323180111,-37.5659616007325));
#272826=CARTESIAN_POINT('Ctrl Pts',(4.76104848420342,13.2690897233696,-37.2591313508017));
#272827=CARTESIAN_POINT('',(4.76104848420342,17.2592679242302,-33.6663587612776));
#272828=CARTESIAN_POINT('Origin',(4.76104848420342,16.6251708556156,-36.9742798391569));
#272829=CARTESIAN_POINT('',(4.79296103895619,18.1280311274457,-33.9600084589958));
#272830=CARTESIAN_POINT('Ctrl Pts',(4.76104848420342,17.2592679242302,-33.6663587612776));
#272831=CARTESIAN_POINT('Ctrl Pts',(4.76104848420342,17.3808488290439,-33.6896646665658));
#272832=CARTESIAN_POINT('Ctrl Pts',(4.76253147492084,17.5011401217906,-33.7196691161167));
#272833=CARTESIAN_POINT('Ctrl Pts',(4.76582554549253,17.6196318267452,-33.7562868369354));
#272834=CARTESIAN_POINT('Ctrl Pts',(4.7690329568029,17.7350062931944,-33.7919412315082));
#272835=CARTESIAN_POINT('Ctrl Pts',(4.77395785392703,17.8486743622794,-33.8338656362274));
#272836=CARTESIAN_POINT('Ctrl Pts',(4.7808706770485,17.9601281306821,-33.8819810649277));
#272837=CARTESIAN_POINT('Ctrl Pts',(4.78437887452869,18.0166899466867,-33.9063992256067));
#272838=CARTESIAN_POINT('Ctrl Pts',(4.78839849253368,18.0726808984023,-33.9324118527932));
#272839=CARTESIAN_POINT('Ctrl Pts',(4.79296103895619,18.1280311274457,-33.9600084589958));
#272840=CARTESIAN_POINT('',(11.5201159294502,18.1280311274457,-33.9600084589958));
#272841=CARTESIAN_POINT('',(11.5520284842034,18.1280311274457,-33.9600084589958));
#272842=CARTESIAN_POINT('Ctrl Pts',(11.5201159294506,18.1280311274458,-33.9600084589958));
#272843=CARTESIAN_POINT('Ctrl Pts',(11.5379482942249,17.9116989779746,-33.8521492280388));
#272844=CARTESIAN_POINT('Ctrl Pts',(11.5475950755165,17.6834964237933,-33.7674327201988));
#272845=CARTESIAN_POINT('Ctrl Pts',(11.5516325551658,17.3847132700051,-33.6922631379132));
#272846=CARTESIAN_POINT('Ctrl Pts',(11.5520284842034,17.3221297517055,-33.6784087768588));
#272847=CARTESIAN_POINT('Ctrl Pts',(11.5520284842034,17.2592679242302,-33.6663587612776));
#272848=CARTESIAN_POINT('Origin',(11.5520284842034,29.1056069249118,-19.7964332737808));
#272849=CARTESIAN_POINT('',(11.5201159294503,29.2525234772276,-16.4314910043563));
#272850=CARTESIAN_POINT('',(11.5520284842034,28.3394307068729,-16.5165864857714));
#272851=CARTESIAN_POINT('Ctrl Pts',(11.5201159294506,29.2525234772276,-16.4314910043563));
#272852=CARTESIAN_POINT('Ctrl Pts',(11.5379482942249,29.011023923212,-16.420946906116));
#272853=CARTESIAN_POINT('Ctrl Pts',(11.5475950755165,28.7680932084051,-16.4363728660204));
#272854=CARTESIAN_POINT('Ctrl Pts',(11.5516325551658,28.4645669918831,-16.4892280925497));
#272855=CARTESIAN_POINT('Ctrl Pts',(11.5520284842034,28.4017590267117,-16.5020265140846));
#272856=CARTESIAN_POINT('Ctrl Pts',(11.5520284842034,28.3394307068777,-16.5165864857703));
#272857=CARTESIAN_POINT('',(11.5520284842034,26.1555337986899,-21.4216992519662));
#272858=CARTESIAN_POINT('Origin',(11.5520284842034,29.1056069249118,-19.7964332737808));
#272859=CARTESIAN_POINT('',(11.5201159294506,26.7032738510941,-22.1571994105138));
#272860=CARTESIAN_POINT('Ctrl Pts',(11.5520284842034,26.1555337986899,-21.4216992519662));
#272861=CARTESIAN_POINT('Ctrl Pts',(11.5520284842034,26.2152697101401,-21.5301278472884));
#272862=CARTESIAN_POINT('Ctrl Pts',(11.5505454879216,26.2809778174266,-21.6352599593984));
#272863=CARTESIAN_POINT('Ctrl Pts',(11.547251405376,26.3524194306083,-21.7366369274159));
#272864=CARTESIAN_POINT('Ctrl Pts',(11.5440439814859,26.4219816026811,-21.8353469338028));
#272865=CARTESIAN_POINT('Ctrl Pts',(11.5391190647185,26.4969796197233,-21.9304964980372));
#272866=CARTESIAN_POINT('Ctrl Pts',(11.53220621369,26.5771814108555,-22.021626986686));
#272867=CARTESIAN_POINT('Ctrl Pts',(11.5286980345265,26.6178827439774,-22.0678744871931));
#272868=CARTESIAN_POINT('Ctrl Pts',(11.5246784421811,26.6599240776381,-22.1130863605614));
#272869=CARTESIAN_POINT('Ctrl Pts',(11.5201159294506,26.7032738510941,-22.1571994105138));
#272870=CARTESIAN_POINT('',(4.79296103895619,26.7032738510941,-22.1571994105138));
#272871=CARTESIAN_POINT('',(11.5520284842034,26.7032738510941,-22.1571994105138));
#272872=CARTESIAN_POINT('',(4.76104848420342,26.1555337986899,-21.4216992519663));
#272873=CARTESIAN_POINT('Ctrl Pts',(4.79296103895619,26.7032738510941,-22.1571994105138));
#272874=CARTESIAN_POINT('Ctrl Pts',(4.77035892158039,26.4885244956969,-21.9386688788256));
#272875=CARTESIAN_POINT('Ctrl Pts',(4.76104848420342,26.3041239985807,-21.6914101555361));
#272876=CARTESIAN_POINT('Ctrl Pts',(4.76104848420342,26.1555337986899,-21.4216992519663));
#272877=CARTESIAN_POINT('',(4.76104848420342,28.3394307068729,-16.5165864857714));
#272878=CARTESIAN_POINT('Origin',(4.76104848420342,29.1056069249118,-19.7964332737808));
#272879=CARTESIAN_POINT('',(4.79296103895619,29.2525234772276,-16.4314910043563));
#272880=CARTESIAN_POINT('Ctrl Pts',(4.76104848420342,28.3394307068727,-16.5165864857715));
#272881=CARTESIAN_POINT('Ctrl Pts',(4.76104848420341,28.5201783449009,-16.4743636166331));
#272882=CARTESIAN_POINT('Ctrl Pts',(4.76439185786762,28.7044365412357,-16.4470754611615));
#272883=CARTESIAN_POINT('Ctrl Pts',(4.77719931294497,29.0113869639358,-16.4274204006687));
#272884=CARTESIAN_POINT('Ctrl Pts',(4.78408071207328,29.1322592829447,-16.4262401562358));
#272885=CARTESIAN_POINT('Ctrl Pts',(4.79296103895619,29.2525234772276,-16.4314910043563));
#272886=CARTESIAN_POINT('',(11.5520284842034,29.2525234772276,-16.4314910043563));
#272887=CARTESIAN_POINT('Origin',(11.5520284842034,7.98893738233704,-43.2488707392774));
#272888=CARTESIAN_POINT('',(11.5520284842034,9.29693337302835,-40.1450718672112));
#272889=CARTESIAN_POINT('',(11.5520284842034,4.64697071554456,-42.8297290592312));
#272890=CARTESIAN_POINT('Origin',(11.5520284842034,7.98893738233704,-43.2488707392774));
#272891=CARTESIAN_POINT('',(11.5201159294509,4.65778558018634,-43.7467147117548));
#272892=CARTESIAN_POINT('Ctrl Pts',(11.5520284842034,4.64697071554456,-42.8297290592312));
#272893=CARTESIAN_POINT('Ctrl Pts',(11.5520284842034,4.63156563906103,-42.9525592490173));
#272894=CARTESIAN_POINT('Ctrl Pts',(11.5505455425311,4.62292954634169,-43.0762329497044));
#272895=CARTESIAN_POINT('Ctrl Pts',(11.5472515828824,4.62113892696966,-43.2002387723334));
#272896=CARTESIAN_POINT('Ctrl Pts',(11.5440442853252,4.61939541771331,-43.3209820765611));
#272897=CARTESIAN_POINT('Ctrl Pts',(11.5391195667911,4.62414211204812,-43.442040056475));
#272898=CARTESIAN_POINT('Ctrl Pts',(11.5322070025998,4.63546083850879,-43.5629052434111));
#272899=CARTESIAN_POINT('Ctrl Pts',(11.5286986366916,4.64120548448104,-43.6242485148234));
#272900=CARTESIAN_POINT('Ctrl Pts',(11.5246787835196,4.64864319302917,-43.6855415708951));
#272901=CARTESIAN_POINT('Ctrl Pts',(11.5201159294506,4.65778558018632,-43.7467147117548));
#272902=CARTESIAN_POINT('',(4.79296103895619,4.65778558018634,-43.7467147117548));
#272903=CARTESIAN_POINT('',(11.5520284842034,4.65778558018634,-43.7467147117548));
#272904=CARTESIAN_POINT('',(4.76104848420342,4.64697071554454,-42.8297290592312));
#272905=CARTESIAN_POINT('Ctrl Pts',(4.79296103895618,4.65778558018634,-43.7467147117548));
#272906=CARTESIAN_POINT('Ctrl Pts',(4.77035892157484,4.61249872582977,-43.4436932937131));
#272907=CARTESIAN_POINT('Ctrl Pts',(4.76104848420341,4.60865062096244,-43.1352688918427));
#272908=CARTESIAN_POINT('Ctrl Pts',(4.76104848420342,4.64697071554455,-42.8297290592312));
#272909=CARTESIAN_POINT('',(4.76104848420342,9.29693337302838,-40.1450718672112));
#272910=CARTESIAN_POINT('Origin',(4.76104848420342,7.98893738233704,-43.2488707392774));
#272911=CARTESIAN_POINT('',(4.79296103895619,10.0856588106987,-40.6129306409912));
#272912=CARTESIAN_POINT('Ctrl Pts',(4.76104848420342,9.29693337302838,-40.1450718672112));
#272913=CARTESIAN_POINT('Ctrl Pts',(4.76104848420342,9.41101218012303,-40.1931467033887));
#272914=CARTESIAN_POINT('Ctrl Pts',(4.76253148285884,9.52243682318274,-40.247505605299));
#272915=CARTESIAN_POINT('Ctrl Pts',(4.76582557106269,9.63072620395674,-40.3079591349109));
#272916=CARTESIAN_POINT('Ctrl Pts',(4.76903300061286,9.73616678064156,-40.3668222937853));
#272917=CARTESIAN_POINT('Ctrl Pts',(4.77395792631717,9.83863461626415,-40.4314636981259));
#272918=CARTESIAN_POINT('Ctrl Pts',(4.78087079057491,9.93764933157731,-40.5017004896638));
#272919=CARTESIAN_POINT('Ctrl Pts',(4.7843789612106,9.98789775304374,-40.5373445643096));
#272920=CARTESIAN_POINT('Ctrl Pts',(4.7883985416898,10.0372562955025,-40.5744295419471));
#272921=CARTESIAN_POINT('Ctrl Pts',(4.79296103895619,10.0856588106987,-40.6129306409912));
#272922=CARTESIAN_POINT('',(11.5201159294506,10.0856588106987,-40.6129306409912));
#272923=CARTESIAN_POINT('',(11.5520284842034,10.0856588106987,-40.6129306409912));
#272924=CARTESIAN_POINT('Ctrl Pts',(11.5201159294506,10.0856588106987,-40.6129306409912));
#272925=CARTESIAN_POINT('Ctrl Pts',(11.5379482942249,9.8964792328107,-40.462450410039));
#272926=CARTESIAN_POINT('Ctrl Pts',(11.5475950755165,9.69087700434215,-40.3321391822639));
#272927=CARTESIAN_POINT('Ctrl Pts',(11.5516325551658,9.41425161427548,-40.1964917250111));
#272928=CARTESIAN_POINT('Ctrl Pts',(11.5520284842034,9.35591617963722,-40.169928269879));
#272929=CARTESIAN_POINT('Ctrl Pts',(11.5520284842034,9.29693337302835,-40.1450718672112));
#272930=CARTESIAN_POINT('Origin',(11.5520284842034,-1.76313447216117,-47.5907728700901));
#272931=CARTESIAN_POINT('',(11.5520284842034,0.161594739352518,-44.8267471082258));
#272932=CARTESIAN_POINT('',(11.5520284842034,-4.944926693626,-46.485956501036));
#272933=CARTESIAN_POINT('Origin',(11.5520284842034,-1.76313447216117,-47.5907728700901));
#272934=CARTESIAN_POINT('',(11.5201159294504,-5.12500019719618,-47.3851523537529));
#272935=CARTESIAN_POINT('Ctrl Pts',(11.5520284842034,-4.94492669362599,
-46.485956501036));
#272936=CARTESIAN_POINT('Ctrl Pts',(11.5520284842034,-4.98553194227204,
-46.6028967165428));
#272937=CARTESIAN_POINT('Ctrl Pts',(11.550545616777,-5.01969184244845,-46.7220693474121));
#272938=CARTESIAN_POINT('Ctrl Pts',(11.5472518253861,-5.04722524969846,
-46.8429900493421));
#272939=CARTESIAN_POINT('Ctrl Pts',(11.5440447002121,-5.07403419812174,
-46.9607290865747));
#272940=CARTESIAN_POINT('Ctrl Pts',(11.5391202523742,-5.09456054853041,
-47.0801252587079));
#272941=CARTESIAN_POINT('Ctrl Pts',(11.5322080809718,-5.10861875091385,
-47.2006991758331));
#272942=CARTESIAN_POINT('Ctrl Pts',(11.5286994596642,-5.11575470075611,
-47.261902550306));
#272943=CARTESIAN_POINT('Ctrl Pts',(11.524679249925,-5.12122380413464,-47.3234088729758));
#272944=CARTESIAN_POINT('Ctrl Pts',(11.5201159294506,-5.12500019719618,
-47.3851523537529));
#272945=CARTESIAN_POINT('',(4.79296103895619,-5.12500019719618,-47.3851523537529));
#272946=CARTESIAN_POINT('',(11.5520284842034,-5.12500019719618,-47.3851523537529));
#272947=CARTESIAN_POINT('',(4.76104848420342,-4.94492669362602,-46.485956501036));
#272948=CARTESIAN_POINT('Ctrl Pts',(4.79296103895618,-5.12500019719618,
-47.3851523537529));
#272949=CARTESIAN_POINT('Ctrl Pts',(4.77035892158036,-5.10629572975537,
-47.0793370143381));
#272950=CARTESIAN_POINT('Ctrl Pts',(4.76104848420342,-5.04593470543677,
-46.7768523596485));
#272951=CARTESIAN_POINT('Ctrl Pts',(4.76104848420342,-4.94492669362601,
-46.485956501036));
#272952=CARTESIAN_POINT('',(4.76104848420342,0.161594739352547,-44.8267471082258));
#272953=CARTESIAN_POINT('Origin',(4.76104848420342,-1.76313447216117,-47.5907728700901));
#272954=CARTESIAN_POINT('',(4.79296103895619,0.835811325126992,-45.448367284618));
#272955=CARTESIAN_POINT('Ctrl Pts',(4.76104848420342,0.161594739352541,
-44.8267471082258));
#272956=CARTESIAN_POINT('Ctrl Pts',(4.76104848420342,0.263185006973524,
-44.8974894863879));
#272957=CARTESIAN_POINT('Ctrl Pts',(4.76253147347957,0.360872606791814,
-44.9738267448727));
#272958=CARTESIAN_POINT('Ctrl Pts',(4.76582553976561,0.454226339754833,
-45.0554735552757));
#272959=CARTESIAN_POINT('Ctrl Pts',(4.76903294718512,0.54512416321815,-45.134972436818));
#272960=CARTESIAN_POINT('Ctrl Pts',(4.77395783802177,0.631912869766447,
-45.2195051911972));
#272961=CARTESIAN_POINT('Ctrl Pts',(4.78087065106457,0.714160596304464,
-45.3087930763068));
#272962=CARTESIAN_POINT('Ctrl Pts',(4.78437885482611,0.755900736220323,
-45.35410604694));
#272963=CARTESIAN_POINT('Ctrl Pts',(4.7883984814575,0.796470830268012,-45.400643448165));
#272964=CARTESIAN_POINT('Ctrl Pts',(4.79296103895619,0.835811325126995,
-45.448367284618));
#272965=CARTESIAN_POINT('',(11.5201159294506,0.835811325126992,-45.448367284618));
#272966=CARTESIAN_POINT('',(11.5520284842034,0.835811325126992,-45.448367284618));
#272967=CARTESIAN_POINT('Ctrl Pts',(11.5201159294506,0.835811325126992,
-45.448367284618));
#272968=CARTESIAN_POINT('Ctrl Pts',(11.5379482942249,0.682052374159662,
-45.261842761847));
#272969=CARTESIAN_POINT('Ctrl Pts',(11.5475950755165,0.508036275376835,
-45.0916320400934));
#272970=CARTESIAN_POINT('Ctrl Pts',(11.5516325551658,0.26565850597392,-44.9014351526643));
#272971=CARTESIAN_POINT('Ctrl Pts',(11.5520284842034,0.214120693415193,
-44.8633235539094));
#272972=CARTESIAN_POINT('Ctrl Pts',(11.5520284842034,0.161594739352511,
-44.8267471082258));
#272973=CARTESIAN_POINT('Origin',(11.5520284842034,-12.2048323722047,-49.8102242737206));
#272974=CARTESIAN_POINT('',(11.5520284842034,-9.7474898422873,-47.5067728111187));
#272975=CARTESIAN_POINT('',(11.5520284842034,-15.0873905603309,-48.0680189924833));
#272976=CARTESIAN_POINT('Origin',(11.5520284842034,-12.2048323722047,-49.8102242737206));
#272977=CARTESIAN_POINT('',(11.5201159294509,-15.4504823559185,-48.9101258718094));
#272978=CARTESIAN_POINT('Ctrl Pts',(11.5520284842034,-15.0873905603309,
-48.0680189924833));
#272979=CARTESIAN_POINT('Ctrl Pts',(11.5520284842034,-15.1514184267909,
-48.173956021099));
#272980=CARTESIAN_POINT('Ctrl Pts',(11.5505457686483,-15.2096066120264,
-48.2834165710142));
#272981=CARTESIAN_POINT('Ctrl Pts',(11.5472523215541,-15.2616772101935,
-48.3959644782058));
#272982=CARTESIAN_POINT('Ctrl Pts',(11.5440455490482,-15.3123774515486,
-48.5055504299616));
#272983=CARTESIAN_POINT('Ctrl Pts',(11.5391216550271,-15.3572776080623,
-48.6180632708147));
#272984=CARTESIAN_POINT('Ctrl Pts',(11.5322102873381,-15.3960965020979,
-48.7330726175836));
#272985=CARTESIAN_POINT('Ctrl Pts',(11.5287011435043,-15.4158062164073,
-48.7914668975864));
#272986=CARTESIAN_POINT('Ctrl Pts',(11.5246802042203,-15.4339478375954,
-48.8505043248629));
#272987=CARTESIAN_POINT('Ctrl Pts',(11.5201159294506,-15.4504823559185,
-48.9101258718094));
#272988=CARTESIAN_POINT('',(4.79296103895619,-15.4504823559185,-48.9101258718094));
#272989=CARTESIAN_POINT('',(11.5520284842034,-15.4504823559185,-48.9101258718094));
#272990=CARTESIAN_POINT('',(4.76104848420342,-15.0873905603309,-48.0680189924834));
#272991=CARTESIAN_POINT('Ctrl Pts',(4.79296103895619,-15.4504823559185,
-48.9101258718094));
#272992=CARTESIAN_POINT('Ctrl Pts',(4.77035892158032,-15.3686040416723,
-48.6148822087441));
#272993=CARTESIAN_POINT('Ctrl Pts',(4.76104848420342,-15.2466719545542,
-48.3315573321263));
#272994=CARTESIAN_POINT('Ctrl Pts',(4.76104848420342,-15.0873905603309,
-48.0680189924834));
#272995=CARTESIAN_POINT('',(4.76104848420342,-9.74748984228727,-47.5067728111187));
#272996=CARTESIAN_POINT('Origin',(4.76104848420342,-12.2048323722047,-49.8102242737206));
#272997=CARTESIAN_POINT('',(4.79296103895619,-9.21724860845719,-48.2549866055502));
#272998=CARTESIAN_POINT('Ctrl Pts',(4.76104848420342,-9.74748984228727,
-47.5067728111187));
#272999=CARTESIAN_POINT('Ctrl Pts',(4.76104848420342,-9.66282867327375,
-47.5970901000337));
#273000=CARTESIAN_POINT('Ctrl Pts',(4.76253144075005,-9.58314800674111,
-47.6920685179983));
#273001=CARTESIAN_POINT('Ctrl Pts',(4.76582543152432,-9.50881029780304,
-47.7913393066709));
#273002=CARTESIAN_POINT('Ctrl Pts',(4.76903276223637,-9.43642830487133,
-47.8879984266072));
#273003=CARTESIAN_POINT('Ctrl Pts',(4.77395753238408,-9.36911211029268,
-47.988726987311));
#273004=CARTESIAN_POINT('Ctrl Pts',(4.78087016904751,-9.30722618608076,
-48.0931625382006));
#273005=CARTESIAN_POINT('Ctrl Pts',(4.78437848714111,-9.27581769201065,
-48.1461659218068));
#273006=CARTESIAN_POINT('Ctrl Pts',(4.78839827319888,-9.24580837914143,
-48.2001237965154));
#273007=CARTESIAN_POINT('Ctrl Pts',(4.79296103895619,-9.21724860845719,
-48.2549866055502));
#273008=CARTESIAN_POINT('',(11.5201159294506,-9.21724860845719,-48.2549866055502));
#273009=CARTESIAN_POINT('',(11.5520284842034,-9.21724860845719,-48.2549866055502));
#273010=CARTESIAN_POINT('Ctrl Pts',(11.5201159294506,-9.21724860845719,
-48.2549866055502));
#273011=CARTESIAN_POINT('Ctrl Pts',(11.5379482942249,-9.32886692852894,
-48.0405698076498));
#273012=CARTESIAN_POINT('Ctrl Pts',(11.5475950755165,-9.46369155908738,
-47.8378986172198));
#273013=CARTESIAN_POINT('Ctrl Pts',(11.5516325551658,-9.66122863624646,
-47.6014648162607));
#273014=CARTESIAN_POINT('Ctrl Pts',(11.5520284842034,-9.70371637701088,
-47.5534707336284));
#273015=CARTESIAN_POINT('Ctrl Pts',(11.5520284842034,-9.7474898422873,-47.5067728111187));
#273016=CARTESIAN_POINT('Origin',(15.4290484842034,-17.542318193471,0.972561099047131));
#273017=CARTESIAN_POINT('',(6.14788848420341,-17.9270891962423,55.333062537043));
#273018=CARTESIAN_POINT('',(6.14788848420342,-17.1575471907001,55.333062537043));
#273019=CARTESIAN_POINT('Origin',(6.14788848420341,-17.542318193471,0.972561099047131));
#273020=CARTESIAN_POINT('',(4.79296103895619,-15.4504823559191,50.8552480699037));
#273021=CARTESIAN_POINT('Ctrl Pts',(4.79296103895619,-15.4504823559191,
50.8552480699037));
#273022=CARTESIAN_POINT('Ctrl Pts',(4.80658157259404,-15.4998240310752,
51.0331684026437));
#273023=CARTESIAN_POINT('Ctrl Pts',(4.8245384335836,-15.5510803275331,51.2105179282822));
#273024=CARTESIAN_POINT('Ctrl Pts',(5.02532215959839,-16.0303748306657,
52.8041842377484));
#273025=CARTESIAN_POINT('Ctrl Pts',(5.47477154367344,-16.5701102199707,
54.1411460083266));
#273026=CARTESIAN_POINT('Ctrl Pts',(6.14788848420342,-17.1575471907001,
55.333062537043));
#273027=CARTESIAN_POINT('',(4.76104848420342,-15.0873905603315,50.0131411905777));
#273028=CARTESIAN_POINT('Ctrl Pts',(4.76104848420342,-15.0873905603315,
50.0131411905777));
#273029=CARTESIAN_POINT('Ctrl Pts',(4.76104848420342,-15.1514184267896,
50.1190782191899));
#273030=CARTESIAN_POINT('Ctrl Pts',(4.76253119975843,-15.2096066120234,
50.2285387691015));
#273031=CARTESIAN_POINT('Ctrl Pts',(4.76582464685242,-15.2616772101892,
50.3410866762893));
#273032=CARTESIAN_POINT('Ctrl Pts',(4.76903141935819,-15.3123774515448,
50.4506726280453));
#273033=CARTESIAN_POINT('Ctrl Pts',(4.77395531337918,-15.3572776080591,
50.5631854688987));
#273034=CARTESIAN_POINT('Ctrl Pts',(4.78086668106818,-15.3960965020952,
50.6781948156679));
#273035=CARTESIAN_POINT('Ctrl Pts',(4.78437582490208,-15.4158062164058,
50.736589095674));
#273036=CARTESIAN_POINT('Ctrl Pts',(4.78839676418632,-15.4339478375951,
50.7956265229538));
#273037=CARTESIAN_POINT('Ctrl Pts',(4.79296103895619,-15.4504823559191,
50.8552480699037));
#273038=CARTESIAN_POINT('',(4.76104848420342,-19.9972458266108,50.0131411905776));
#273039=CARTESIAN_POINT('Origin',(4.76104848420342,-17.542318193471,0.972561099047131));
#273040=CARTESIAN_POINT('',(4.79296103895619,-19.6341540310232,50.8552480699037));
#273041=CARTESIAN_POINT('Ctrl Pts',(4.79296103895619,-19.6341540310232,
50.8552480699037));
#273042=CARTESIAN_POINT('Ctrl Pts',(4.77035892158037,-19.7160323452691,
50.5600044068391));
#273043=CARTESIAN_POINT('Ctrl Pts',(4.76104848420342,-19.8379644323871,
50.2766795302212));
#273044=CARTESIAN_POINT('Ctrl Pts',(4.76104848420342,-19.9972458266108,
50.0131411905776));
#273045=CARTESIAN_POINT('Ctrl Pts',(6.14788848420341,-17.9270891962423,
55.333062537043));
#273046=CARTESIAN_POINT('Ctrl Pts',(6.12358695752485,-17.9482974207819,
55.2900307997962));
#273047=CARTESIAN_POINT('Ctrl Pts',(6.099576183545,-17.969450050515,55.2468069379304));
#273048=CARTESIAN_POINT('Ctrl Pts',(5.43709796638902,-18.558608728335,54.0342076324939));
#273049=CARTESIAN_POINT('Ctrl Pts',(5.01156238585603,-19.0785577539987,
52.7304461548518));
#273050=CARTESIAN_POINT('Ctrl Pts',(4.82218298524757,-19.5403257915009,
51.1870629797606));
#273051=CARTESIAN_POINT('Ctrl Pts',(4.80568122363092,-19.5880739553937,
51.0214074546985));
#273052=CARTESIAN_POINT('Ctrl Pts',(4.79296103895619,-19.6341540310232,
50.8552480699037));
#273053=CARTESIAN_POINT('Origin',(0.561048484203417,-17.542318193471,0.972561099047131));
#273054=CARTESIAN_POINT('',(10.1651884842034,-17.9270891962423,55.333062537043));
#273055=CARTESIAN_POINT('',(10.1651884842034,-17.1575471907001,55.333062537043));
#273056=CARTESIAN_POINT('Origin',(10.1651884842034,-17.542318193471,0.972561099047131));
#273057=CARTESIAN_POINT('',(8.15653848420341,-17.1575471907001,55.333062537043));
#273058=CARTESIAN_POINT('',(8.15653848420342,-17.9270891962423,55.333062537043));
#273059=CARTESIAN_POINT('Origin',(0.884028484203416,-17.542318193471,0.972561099047131));
#273060=CARTESIAN_POINT('',(11.5520284842034,-19.9972458266108,50.0131411905776));
#273061=CARTESIAN_POINT('',(11.5520284842034,-15.0873905603315,50.0131411905776));
#273062=CARTESIAN_POINT('Origin',(11.5520284842034,-17.542318193471,0.972561099047131));
#273063=CARTESIAN_POINT('',(11.520115929451,-15.4504823559191,50.8552480699037));
#273064=CARTESIAN_POINT('Ctrl Pts',(11.5201159294506,-15.4504823559191,
50.8552480699037));
#273065=CARTESIAN_POINT('Ctrl Pts',(11.5379482942249,-15.3858829229342,
50.6223100398281));
#273066=CARTESIAN_POINT('Ctrl Pts',(11.5475950755165,-15.296142243916,50.3960360842679));
#273067=CARTESIAN_POINT('Ctrl Pts',(11.5516325551658,-15.1520791771608,
50.123698661416));
#273068=CARTESIAN_POINT('Ctrl Pts',(11.5520284842034,-15.1204984263408,
50.0679196666184));
#273069=CARTESIAN_POINT('Ctrl Pts',(11.5520284842034,-15.0873905603315,
50.0131411905776));
#273070=CARTESIAN_POINT('Ctrl Pts',(10.1651884842034,-17.1575471907001,
55.333062537043));
#273071=CARTESIAN_POINT('Ctrl Pts',(10.189490010882,-17.1363389661605,55.2900307997962));
#273072=CARTESIAN_POINT('Ctrl Pts',(10.2135007848618,-17.1151863364273,
55.2468069379303));
#273073=CARTESIAN_POINT('Ctrl Pts',(10.8759790020178,-16.5260276586073,
54.0342076324939));
#273074=CARTESIAN_POINT('Ctrl Pts',(11.3015145825508,-16.0060786329436,
52.7304461548518));
#273075=CARTESIAN_POINT('Ctrl Pts',(11.4908939831593,-15.5443105954415,
51.1870629797606));
#273076=CARTESIAN_POINT('Ctrl Pts',(11.5073957447759,-15.4965624315486,
51.0214074546985));
#273077=CARTESIAN_POINT('Ctrl Pts',(11.5201159294506,-15.4504823559191,
50.8552480699037));
#273078=CARTESIAN_POINT('',(11.5201159294504,-19.6341540310232,50.8552480699037));
#273079=CARTESIAN_POINT('Ctrl Pts',(11.5201159294506,-19.6341540310232,
50.8552480699037));
#273080=CARTESIAN_POINT('Ctrl Pts',(11.5064953958128,-19.5848123558671,
51.0331684026437));
#273081=CARTESIAN_POINT('Ctrl Pts',(11.4885385348232,-19.5335560594093,
51.2105179282821));
#273082=CARTESIAN_POINT('Ctrl Pts',(11.2877548088084,-19.0542615562767,
52.8041842377484));
#273083=CARTESIAN_POINT('Ctrl Pts',(10.8383054247334,-18.5145261669716,
54.1411460083265));
#273084=CARTESIAN_POINT('Ctrl Pts',(10.1651884842034,-17.9270891962423,
55.333062537043));
#273085=CARTESIAN_POINT('Ctrl Pts',(11.5520284842034,-19.9972458266108,
50.0131411905776));
#273086=CARTESIAN_POINT('Ctrl Pts',(11.5520284842034,-19.9332179601523,
50.1190782191907));
#273087=CARTESIAN_POINT('Ctrl Pts',(11.5505457686484,-19.875029774918,50.2285387691031));
#273088=CARTESIAN_POINT('Ctrl Pts',(11.5472523215543,-19.822959176752,50.3410866762919));
#273089=CARTESIAN_POINT('Ctrl Pts',(11.5440455490485,-19.7722589353958,
50.4506726280492));
#273090=CARTESIAN_POINT('Ctrl Pts',(11.5391216550274,-19.7273587788812,
50.563185468904));
#273091=CARTESIAN_POINT('Ctrl Pts',(11.5322102873382,-19.6885398848448,
50.6781948156747));
#273092=CARTESIAN_POINT('Ctrl Pts',(11.5287011435044,-19.6688301705351,
50.7365890956786));
#273093=CARTESIAN_POINT('Ctrl Pts',(11.5246802042203,-19.6506885493466,
50.7956265229561));
#273094=CARTESIAN_POINT('Ctrl Pts',(11.5201159294506,-19.6341540310232,
50.8552480699037));
#273095=CARTESIAN_POINT('Origin',(19.4612584842034,-17.542318193471,0.972561099047131));
#273096=CARTESIAN_POINT('',(11.5520284842034,-9.08998123852178,3.49256109904713));
#273097=CARTESIAN_POINT('',(11.5520284842034,-9.08998123852178,-1.54743890095287));
#273098=CARTESIAN_POINT('Origin',(11.5520284842034,-17.542318193471,0.972561099047131));
#273099=CARTESIAN_POINT('',(-3.14818151579658,-9.08998123852178,-1.54743890095287));
#273100=CARTESIAN_POINT('',(19.4612584842034,-9.08998123852178,-1.54743890095287));
#273101=CARTESIAN_POINT('',(-3.14818151579658,-9.08998123852178,3.49256109904713));
#273102=CARTESIAN_POINT('Origin',(-3.14818151579658,-17.542318193471,0.972561099047131));
#273103=CARTESIAN_POINT('',(19.4612584842034,-9.08998123852178,3.49256109904713));
#273104=CARTESIAN_POINT('Origin',(11.5520284842034,-17.542318193471,0.972561099047131));
#273105=CARTESIAN_POINT('',(11.5520284842034,-25.3371465446544,49.451895009213));
#273106=CARTESIAN_POINT('Origin',(11.5520284842034,-22.8798040147369,51.7553464718149));
#273107=CARTESIAN_POINT('',(11.5520284842034,-30.1397096933157,48.4310786991304));
#273108=CARTESIAN_POINT('Origin',(11.5520284842034,-17.542318193471,0.972561099047131));
#273109=CARTESIAN_POINT('',(11.5520284842034,-35.2462311262942,46.7718693063201));
#273110=CARTESIAN_POINT('Origin',(11.5520284842034,-33.3215019147805,49.5358950681845));
#273111=CARTESIAN_POINT('',(11.5520284842034,-39.7316071024862,44.7748512573256));
#273112=CARTESIAN_POINT('Origin',(11.5520284842034,-17.542318193471,0.972561099047131));
#273113=CARTESIAN_POINT('',(11.5520284842034,-44.38156975997,42.0901940653056));
#273114=CARTESIAN_POINT('Origin',(11.5520284842034,-43.0735737692787,45.1939929373718));
#273115=CARTESIAN_POINT('',(11.5520284842034,-48.3537261103113,39.2042535488961));
#273116=CARTESIAN_POINT('Origin',(11.5520284842034,-17.542318193471,0.972561099047131));
#273117=CARTESIAN_POINT('',(11.5520284842034,-52.3439043111719,35.6114809593721));
#273118=CARTESIAN_POINT('Origin',(11.5520284842034,-51.7098072425573,38.9194020372514));
#273119=CARTESIAN_POINT('',(11.5520284842034,-55.6292387426316,31.9627474243937));
#273120=CARTESIAN_POINT('Origin',(11.5520284842034,-17.542318193471,0.972561099047131));
#273121=CARTESIAN_POINT('',(11.5520284842034,-58.7852425524921,27.6188808395635));
#273122=CARTESIAN_POINT('Origin',(11.5520284842034,-58.852757490588,30.9863520989862));
#273123=CARTESIAN_POINT('',(11.5520284842034,-61.2401701856317,23.3668214500608));
#273124=CARTESIAN_POINT('Origin',(11.5520284842034,-17.542318193471,0.972561099047131));
#273125=CARTESIAN_POINT('',(11.5520284842034,-63.4240670938147,18.461708683866));
#273126=CARTESIAN_POINT('Origin',(11.5520284842034,-64.1902433118537,21.7415554718754));
#273127=CARTESIAN_POINT('',(11.5520284842034,-64.9412958110163,13.792158838805));
#273128=CARTESIAN_POINT('Origin',(11.5520284842034,-17.542318193471,0.972561099047131));
#273129=CARTESIAN_POINT('',(11.5520284842034,-66.0576390431342,8.54017685647076));
#273130=CARTESIAN_POINT('Origin',(11.5520284842034,-67.4889909638665,11.5890541299798));
#273131=CARTESIAN_POINT('',(11.5520284842034,-66.5708586689849,3.65721829106678));
#273132=CARTESIAN_POINT('Origin',(11.5520284842034,-17.542318193471,0.972561099047131));
#273133=CARTESIAN_POINT('',(11.5520284842034,-66.5708586689849,-1.7120960929732));
#273134=CARTESIAN_POINT('Origin',(11.5520284842034,-68.604829345086,0.972561099046774));
#273135=CARTESIAN_POINT('',(11.5520284842034,-66.0576390431341,-6.59505465837716));
#273136=CARTESIAN_POINT('Origin',(11.5520284842034,-17.542318193471,0.972561099047131));
#273137=CARTESIAN_POINT('',(11.5520284842034,-64.9412958110161,-11.8470366407114));
#273138=CARTESIAN_POINT('Origin',(11.5520284842034,-67.4889909638663,-9.6439319318862));
#273139=CARTESIAN_POINT('Origin',(11.5520284842034,-17.542318193471,0.972561099047131));
#273140=CARTESIAN_POINT('Origin',(11.5520284842034,-17.542318193471,0.972561099047131));
#273141=CARTESIAN_POINT('Origin',(11.5520284842034,-17.542318193471,0.972561099047131));
#273142=CARTESIAN_POINT('Origin',(11.5520284842034,-17.542318193471,0.972561099047131));
#273143=CARTESIAN_POINT('Origin',(11.5520284842034,-17.542318193471,0.972561099047131));
#273144=CARTESIAN_POINT('Origin',(11.5520284842034,-17.542318193471,0.972561099047131));
#273145=CARTESIAN_POINT('Origin',(11.5520284842034,-17.542318193471,0.972561099047131));
#273146=CARTESIAN_POINT('Origin',(11.5520284842034,-17.542318193471,0.972561099047131));
#273147=CARTESIAN_POINT('Origin',(11.5520284842034,-17.542318193471,0.972561099047131));
#273148=CARTESIAN_POINT('Origin',(11.5520284842034,-17.542318193471,0.972561099047131));
#273149=CARTESIAN_POINT('Origin',(11.5520284842034,-17.542318193471,0.972561099047131));
#273150=CARTESIAN_POINT('Origin',(11.5520284842034,-17.542318193471,0.972561099047131));
#273151=CARTESIAN_POINT('',(11.5520284842034,29.8566594240744,-11.8470366407104));
#273152=CARTESIAN_POINT('Origin',(11.5520284842034,-17.542318193471,0.972561099047131));
#273153=CARTESIAN_POINT('',(11.5520284842034,30.9730026561922,-6.59505465837618));
#273154=CARTESIAN_POINT('Origin',(11.5520284842034,32.4043545769246,-9.6439319318852));
#273155=CARTESIAN_POINT('',(11.5520284842034,31.4862222820429,-1.71209609297287));
#273156=CARTESIAN_POINT('Origin',(11.5520284842034,-17.542318193471,0.972561099047131));
#273157=CARTESIAN_POINT('',(11.5520284842034,31.4862222820429,3.65721829106713));
#273158=CARTESIAN_POINT('Origin',(11.5520284842034,33.520192958144,0.972561099047131));
#273159=CARTESIAN_POINT('',(11.5520284842034,30.9730026561921,8.54017685647108));
#273160=CARTESIAN_POINT('Origin',(11.5520284842034,-17.542318193471,0.972561099047131));
#273161=CARTESIAN_POINT('',(11.5520284842034,29.8566594240743,13.7921588388053));
#273162=CARTESIAN_POINT('Origin',(11.5520284842034,32.4043545769244,11.5890541299801));
#273163=CARTESIAN_POINT('',(11.5520284842034,28.3394307068726,18.4617086838663));
#273164=CARTESIAN_POINT('Origin',(11.5520284842034,-17.542318193471,0.972561099047131));
#273165=CARTESIAN_POINT('',(11.5520284842034,26.1555337986896,23.3668214500611));
#273166=CARTESIAN_POINT('Origin',(11.5520284842034,29.1056069249115,21.7415554718757));
#273167=CARTESIAN_POINT('',(11.5520284842034,23.70060616555,27.6188808395637));
#273168=CARTESIAN_POINT('Origin',(11.5520284842034,-17.542318193471,0.972561099047131));
#273169=CARTESIAN_POINT('',(11.5520284842034,20.5446023556894,31.9627474243939));
#273170=CARTESIAN_POINT('Origin',(11.5520284842034,23.7681211036458,30.9863520989864));
#273171=CARTESIAN_POINT('',(11.5520284842034,17.2592679242297,35.6114809593723));
#273172=CARTESIAN_POINT('Origin',(11.5520284842034,-17.542318193471,0.972561099047131));
#273173=CARTESIAN_POINT('',(11.5520284842034,13.269089723369,39.2042535488963));
#273174=CARTESIAN_POINT('Origin',(11.5520284842034,16.6251708556151,38.9194020372516));
#273175=CARTESIAN_POINT('',(11.5520284842034,9.29693337302777,42.0901940653058));
#273176=CARTESIAN_POINT('Origin',(11.5520284842034,-17.542318193471,0.972561099047131));
#273177=CARTESIAN_POINT('',(11.5520284842034,4.64697071554394,44.7748512573258));
#273178=CARTESIAN_POINT('Origin',(11.5520284842034,7.98893738233642,45.193992937372));
#273179=CARTESIAN_POINT('',(11.5520284842034,0.161594739351914,46.7718693063202));
#273180=CARTESIAN_POINT('Origin',(11.5520284842034,-17.542318193471,0.972561099047131));
#273181=CARTESIAN_POINT('',(11.5520284842034,-4.94492669362662,48.4310786991304));
#273182=CARTESIAN_POINT('Origin',(11.5520284842034,-1.76313447216181,49.5358950681846));
#273183=CARTESIAN_POINT('',(11.5520284842034,-9.74748984228794,49.451895009213));
#273184=CARTESIAN_POINT('Origin',(11.5520284842034,-17.542318193471,0.972561099047131));
#273185=CARTESIAN_POINT('Origin',(11.5520284842034,-12.2048323722054,51.7553464718149));
#273186=CARTESIAN_POINT('',(11.5520284842034,-7.33631819347099,-1.54743890095287));
#273187=CARTESIAN_POINT('',(11.5520284842034,-17.542318193471,-1.54743890095287));
#273188=CARTESIAN_POINT('',(11.5520284842034,-7.33631819347099,3.49256109904713));
#273189=CARTESIAN_POINT('',(11.5520284842034,-17.542318193471,3.49256109904713));
#273190=CARTESIAN_POINT('',(11.5520284842034,-7.33631819347099,0.972561099047131));
#273191=CARTESIAN_POINT('Origin',(-3.14818151579658,-17.542318193471,0.972561099047131));
#273192=CARTESIAN_POINT('',(-3.14818151579658,-7.33631819347099,-1.54743890095287));
#273193=CARTESIAN_POINT('',(-3.14818151579658,-17.542318193471,-1.54743890095287));
#273194=CARTESIAN_POINT('',(-3.14818151579658,-7.33631819347099,3.49256109904713));
#273195=CARTESIAN_POINT('',(-3.14818151579658,-7.33631819347099,0.972561099047131));
#273196=CARTESIAN_POINT('',(-3.14818151579658,-17.542318193471,3.49256109904713));
#273197=CARTESIAN_POINT('Origin',(0.884028484203416,-17.542318193471,0.972561099047131));
#273198=CARTESIAN_POINT('',(10.1651884842034,-28.4681391279536,54.2251535450731));
#273199=CARTESIAN_POINT('',(11.5201159294506,-25.8673877784845,50.2001088036445));
#273200=CARTESIAN_POINT('Ctrl Pts',(10.1651884842034,-28.4681391279536,
54.2251535450731));
#273201=CARTESIAN_POINT('Ctrl Pts',(10.189490010882,-28.4384475527546,54.187471592353));
#273202=CARTESIAN_POINT('Ctrl Pts',(10.2135007848618,-28.4087704125277,
54.1495901545875));
#273203=CARTESIAN_POINT('Ctrl Pts',(10.8759790020178,-27.5803726934888,
53.0859820301889));
#273204=CARTESIAN_POINT('Ctrl Pts',(11.3015145825508,-26.8007185482924,
51.918814349969));
#273205=CARTESIAN_POINT('Ctrl Pts',(11.4908939831593,-26.0281538448012,
50.5051647736832));
#273206=CARTESIAN_POINT('Ctrl Pts',(11.5073957447759,-25.947007372541,50.3530566207839));
#273207=CARTESIAN_POINT('Ctrl Pts',(11.5201159294506,-25.8673877784845,
50.2001088036445));
#273208=CARTESIAN_POINT('',(10.1651884842034,-29.2208647943387,54.0651567655455));
#273209=CARTESIAN_POINT('Origin',(10.1651884842034,-17.542318193471,0.972561099047131));
#273210=CARTESIAN_POINT('',(11.5201159294509,-29.9596361897455,49.3302745518473));
#273211=CARTESIAN_POINT('Ctrl Pts',(11.5201159294506,-29.9596361897455,
49.3302745518472));
#273212=CARTESIAN_POINT('Ctrl Pts',(11.5064953958128,-29.9483644657862,
49.5145656095481));
#273213=CARTESIAN_POINT('Ctrl Pts',(11.4885385348232,-29.9351012821247,
49.6986964058043));
#273214=CARTESIAN_POINT('Ctrl Pts',(11.2877548088084,-29.7976223708411,
51.3571882133249));
#273215=CARTESIAN_POINT('Ctrl Pts',(10.8383054247334,-29.5476514770408,
52.7771514588734));
#273216=CARTESIAN_POINT('Ctrl Pts',(10.1651884842034,-29.2208647943387,
54.0651567655455));
#273217=CARTESIAN_POINT('Ctrl Pts',(11.5520284842034,-30.1397096933157,
48.4310786991304));
#273218=CARTESIAN_POINT('Ctrl Pts',(11.5520284842034,-30.0991044446738,
48.5480189146251));
#273219=CARTESIAN_POINT('Ctrl Pts',(11.5505456167773,-30.0649445445003,
48.6671915454817));
#273220=CARTESIAN_POINT('Ctrl Pts',(11.5472518253871,-30.0374111372518,
48.7881122473988));
#273221=CARTESIAN_POINT('Ctrl Pts',(11.5440447002134,-30.0106021888263,
48.905851284635));
#273222=CARTESIAN_POINT('Ctrl Pts',(11.5391202523756,-29.9900758384157,
49.025247456772));
#273223=CARTESIAN_POINT('Ctrl Pts',(11.5322080809733,-29.9760176360309,
49.1458213739011));
#273224=CARTESIAN_POINT('Ctrl Pts',(11.5286994596654,-29.9688816861871,
49.2070247483827));
#273225=CARTESIAN_POINT('Ctrl Pts',(11.5246792499256,-29.9634125828076,
49.2685310710613));
#273226=CARTESIAN_POINT('Ctrl Pts',(11.5201159294506,-29.9596361897455,
49.3302745518473));
#273227=CARTESIAN_POINT('Ctrl Pts',(11.5201159294506,-25.8673877784845,
50.2001088036445));
#273228=CARTESIAN_POINT('Ctrl Pts',(11.5379482942249,-25.7557694584127,
49.9856920057442));
#273229=CARTESIAN_POINT('Ctrl Pts',(11.5475950755165,-25.6209448278543,
49.7830208153142));
#273230=CARTESIAN_POINT('Ctrl Pts',(11.5516325551658,-25.4234077506953,
49.5465870143551));
#273231=CARTESIAN_POINT('Ctrl Pts',(11.5520284842034,-25.3809200099309,
49.4985929317228));
#273232=CARTESIAN_POINT('Ctrl Pts',(11.5520284842034,-25.3371465446544,
49.451895009213));
#273233=CARTESIAN_POINT('Origin',(0.884028484203416,-17.542318193471,0.972561099047131));
#273234=CARTESIAN_POINT('',(11.5201159294503,-9.21724860845784,50.2001088036446));
#273235=CARTESIAN_POINT('Ctrl Pts',(11.5520284842034,-9.74748984228794,
49.451895009213));
#273236=CARTESIAN_POINT('Ctrl Pts',(11.5520284842034,-9.66282867329459,
49.5422122981065));
#273237=CARTESIAN_POINT('Ctrl Pts',(11.5505455276575,-9.58314800677971,
49.6371907160474));
#273238=CARTESIAN_POINT('Ctrl Pts',(11.5472515368849,-9.50881029785681,
49.7364615046943));
#273239=CARTESIAN_POINT('Ctrl Pts',(11.5440442061737,-9.43642830492456,
49.833120624626));
#273240=CARTESIAN_POINT('Ctrl Pts',(11.5391194360271,-9.36911211034505,
49.9338491853251));
#273241=CARTESIAN_POINT('Ctrl Pts',(11.532206799365,-9.30722618613184,50.0382847362099));
#273242=CARTESIAN_POINT('Ctrl Pts',(11.52869848127,-9.27581769204343,50.0912881198434));
#273243=CARTESIAN_POINT('Ctrl Pts',(11.5246786952104,-9.24580837915736,
50.1452459945804));
#273244=CARTESIAN_POINT('Ctrl Pts',(11.5201159294506,-9.21724860845783,
50.2001088036446));
#273245=CARTESIAN_POINT('',(11.520115929451,-5.12500019719682,49.3302745518473));
#273246=CARTESIAN_POINT('Ctrl Pts',(11.5201159294506,-5.12500019719681,
49.3302745518473));
#273247=CARTESIAN_POINT('Ctrl Pts',(11.5379482942249,-5.11024295650262,
49.0889957992713));
#273248=CARTESIAN_POINT('Ctrl Pts',(11.5475950755165,-5.06950832732133,
48.8490083362216));
#273249=CARTESIAN_POINT('Ctrl Pts',(11.5516325551658,-4.98521551827838,
48.5526697436755));
#273250=CARTESIAN_POINT('Ctrl Pts',(11.5520284842034,-4.96592198775489,
48.4915436464428));
#273251=CARTESIAN_POINT('Ctrl Pts',(11.5520284842034,-4.94492669362662,
48.4310786991304));
#273252=CARTESIAN_POINT('',(10.1651884842034,-5.86377159260369,54.0651567655456));
#273253=CARTESIAN_POINT('Ctrl Pts',(10.1651884842034,-5.86377159260369,
54.0651567655456));
#273254=CARTESIAN_POINT('Ctrl Pts',(10.189490010882,-5.85197361990428,54.018655937179));
#273255=CARTESIAN_POINT('Ctrl Pts',(10.2135007848618,-5.84026997208577,
53.9719787413874));
#273256=CARTESIAN_POINT('Ctrl Pts',(10.8759790020178,-5.51609939680231,
52.6633846632577));
#273257=CARTESIAN_POINT('Ctrl Pts',(11.3015145825508,-5.27857975808516,
51.2800100209082));
#273258=CARTESIAN_POINT('Ctrl Pts',(11.4908939831593,-5.14778986561978,
49.6743464977371));
#273259=CARTESIAN_POINT('Ctrl Pts',(11.5073957447759,-5.1355268339775,49.5023835418609));
#273260=CARTESIAN_POINT('Ctrl Pts',(11.5201159294506,-5.12500019719682,
49.3302745518473));
#273261=CARTESIAN_POINT('',(10.1651884842034,-6.6164972589887,54.2251535450731));
#273262=CARTESIAN_POINT('Origin',(10.1651884842034,-17.542318193471,0.972561099047131));
#273263=CARTESIAN_POINT('Ctrl Pts',(11.5201159294506,-9.21724860845782,
50.2001088036446));
#273264=CARTESIAN_POINT('Ctrl Pts',(11.5064953958128,-9.13199345007686,
50.3638824391265));
#273265=CARTESIAN_POINT('Ctrl Pts',(11.4885385348232,-9.04498418693293,
50.5266996688594));
#273266=CARTESIAN_POINT('Ctrl Pts',(11.2877548088084,-8.24482156164845,
51.9858896152882));
#273267=CARTESIAN_POINT('Ctrl Pts',(10.8383054247334,-7.438910703289,53.1814182660674));
#273268=CARTESIAN_POINT('Ctrl Pts',(10.1651884842034,-6.61649725898869,
54.2251535450731));
#273269=CARTESIAN_POINT('Origin',(0.884028484203416,-17.542318193471,0.972561099047131));
#273270=CARTESIAN_POINT('',(11.5201159294502,0.835811325126388,47.3934894827125));
#273271=CARTESIAN_POINT('Ctrl Pts',(11.5520284842034,0.161594739351916,
46.7718693063203));
#273272=CARTESIAN_POINT('Ctrl Pts',(11.5520284842034,0.2631850069628,46.8426116844753));
#273273=CARTESIAN_POINT('Ctrl Pts',(11.5505454949276,0.360872606771722,
46.918948942952));
#273274=CARTESIAN_POINT('Ctrl Pts',(11.5472514286422,0.454226339726327,
47.0005957533459));
#273275=CARTESIAN_POINT('Ctrl Pts',(11.5440440212228,0.545124163197585,
47.0800946348934));
#273276=CARTESIAN_POINT('Ctrl Pts',(11.539119130386,0.631912869753242,47.1646273892785));
#273277=CARTESIAN_POINT('Ctrl Pts',(11.5322063173428,0.714160596297907,
47.2539152743948));
#273278=CARTESIAN_POINT('Ctrl Pts',(11.5286981135811,0.755900736215872,
47.2992282450301));
#273279=CARTESIAN_POINT('Ctrl Pts',(11.5246784869495,0.796470830265539,
47.3457656462573));
#273280=CARTESIAN_POINT('Ctrl Pts',(11.5201159294506,0.8358113251264,47.3934894827125));
#273281=CARTESIAN_POINT('',(11.520115929451,4.65778558018571,45.6918369098494));
#273282=CARTESIAN_POINT('Ctrl Pts',(11.5201159294506,4.65778558018571,45.6918369098493));
#273283=CARTESIAN_POINT('Ctrl Pts',(11.5379482942249,4.62205566635771,45.4527624740445));
#273284=CARTESIAN_POINT('Ctrl Pts',(11.5475950755165,4.6120039469405,45.2095501072284));
#273285=CARTESIAN_POINT('Ctrl Pts',(11.5516325551658,4.63284249803413,44.9021617634728));
#273286=CARTESIAN_POINT('Ctrl Pts',(11.5520284842034,4.63900558839659,44.8383600675693));
#273287=CARTESIAN_POINT('Ctrl Pts',(11.5520284842034,4.64697071554394,44.7748512573258));
#273288=CARTESIAN_POINT('',(10.1651884842034,4.91959547915064,50.4768497968823));
#273289=CARTESIAN_POINT('Ctrl Pts',(10.1651884842034,4.91959547915065,50.4768497968823));
#273290=CARTESIAN_POINT('Ctrl Pts',(10.189490010882,4.92146757198998,50.4289121867312));
#273291=CARTESIAN_POINT('Ctrl Pts',(10.2135007848618,4.9232107323238,50.380821674452));
#273292=CARTESIAN_POINT('Ctrl Pts',(10.8759790020178,4.96822539538776,49.0334246641745));
#273293=CARTESIAN_POINT('Ctrl Pts',(11.3015145825508,4.91293489920084,47.6308969671562));
#273294=CARTESIAN_POINT('Ctrl Pts',(11.4908939831593,4.70703050072919,46.0331282966963));
#273295=CARTESIAN_POINT('Ctrl Pts',(11.5073957447759,4.68327244679356,45.8623735163476));
#273296=CARTESIAN_POINT('Ctrl Pts',(11.5201159294506,4.65778558018571,45.6918369098494));
#273297=CARTESIAN_POINT('',(10.1651884842034,4.21658387552238,50.7898507289224));
#273298=CARTESIAN_POINT('Origin',(10.1651884842034,-17.542318193471,0.972561099047131));
#273299=CARTESIAN_POINT('Ctrl Pts',(11.5201159294506,0.83581132512641,47.3934894827125));
#273300=CARTESIAN_POINT('Ctrl Pts',(11.5064953958128,0.953253907211338,
47.5359587271927));
#273301=CARTESIAN_POINT('Ctrl Pts',(11.4885385348232,1.07221341472524,47.677127766797));
#273302=CARTESIAN_POINT('Ctrl Pts',(11.2877548088084,2.15827321583037,48.9380677475591));
#273303=CARTESIAN_POINT('Ctrl Pts',(10.8383054247334,3.19513737154455,49.9399129397174));
#273304=CARTESIAN_POINT('Ctrl Pts',(10.1651884842034,4.21658387552238,50.7898507289224));
#273305=CARTESIAN_POINT('Origin',(0.884028484203416,-17.542318193471,0.972561099047131));
#273306=CARTESIAN_POINT('',(11.5201159294502,10.0856588106982,42.5580528390859));
#273307=CARTESIAN_POINT('Ctrl Pts',(11.5520284842034,9.29693337302777,42.0901940653058));
#273308=CARTESIAN_POINT('Ctrl Pts',(11.5520284842034,9.41101218010821,42.1382689014774));
#273309=CARTESIAN_POINT('Ctrl Pts',(11.5505454855484,9.52243682315436,42.19262780338));
#273310=CARTESIAN_POINT('Ctrl Pts',(11.5472513973454,9.63072620391565,42.2530813329829));
#273311=CARTESIAN_POINT('Ctrl Pts',(11.5440439677956,9.73616678060244,42.3119444918565));
#273312=CARTESIAN_POINT('Ctrl Pts',(11.5391190420917,9.83863461622702,42.3765858961965));
#273313=CARTESIAN_POINT('Ctrl Pts',(11.5322061778343,9.93764933154213,42.4468226877339));
#273314=CARTESIAN_POINT('Ctrl Pts',(11.5286980071981,9.98789775302051,42.4824667623872));
#273315=CARTESIAN_POINT('Ctrl Pts',(11.5246784267181,10.0372562954908,42.5195517400329));
#273316=CARTESIAN_POINT('Ctrl Pts',(11.5201159294506,10.0856588106982,42.5580528390859));
#273317=CARTESIAN_POINT('',(11.520115929451,13.4703202947425,40.098952328026));
#273318=CARTESIAN_POINT('Ctrl Pts',(11.5201159294506,13.4703202947425,40.0989523280259));
#273319=CARTESIAN_POINT('Ctrl Pts',(11.5379482942249,13.3856647950777,39.8725309090435));
#273320=CARTESIAN_POINT('Ctrl Pts',(11.5475950755165,13.325266035434,39.6367231859533));
#273321=CARTESIAN_POINT('Ctrl Pts',(11.5516325551658,13.2817395839011,39.3317194366231));
#273322=CARTESIAN_POINT('Ctrl Pts',(11.5520284842034,13.2745028774799,39.2680305823144));
#273323=CARTESIAN_POINT('Ctrl Pts',(11.5520284842034,13.2690897233691,39.2042535488963));
#273324=CARTESIAN_POINT('',(10.1651884842034,14.7212691391912,44.7249678641909));
#273325=CARTESIAN_POINT('Ctrl Pts',(10.1651884842034,14.7212691391912,44.7249678641909));
#273326=CARTESIAN_POINT('Ctrl Pts',(10.189490010882,14.71313353273,44.6776885758492));
#273327=CARTESIAN_POINT('Ctrl Pts',(10.2135007848618,14.704840021108,44.6302865332328));
#273328=CARTESIAN_POINT('Ctrl Pts',(10.8759790020178,14.4687314151723,43.3029743056847));
#273329=CARTESIAN_POINT('Ctrl Pts',(11.3015145825508,14.1230472440778,41.9425907444319));
#273330=CARTESIAN_POINT('Ctrl Pts',(11.4908939831593,13.5894475649212,40.422547084527));
#273331=CARTESIAN_POINT('Ctrl Pts',(11.5073957447759,13.5307067663685,40.2604632829794));
#273332=CARTESIAN_POINT('Ctrl Pts',(11.5201159294506,13.4703202947424,40.0989523280259));
#273333=CARTESIAN_POINT('',(10.1651884842034,14.0986965788221,45.1772933060682));
#273334=CARTESIAN_POINT('Origin',(10.1651884842034,-17.542318193471,0.972561099047131));
#273335=CARTESIAN_POINT('Ctrl Pts',(11.5201159294506,10.0856588106982,42.5580528390859));
#273336=CARTESIAN_POINT('Ctrl Pts',(11.5064953958128,10.2301560120979,42.6729911029372));
#273337=CARTESIAN_POINT('Ctrl Pts',(11.4885385348232,10.3758666626724,42.786342187978));
#273338=CARTESIAN_POINT('Ctrl Pts',(11.2877548088084,11.7003576147968,43.7939230752528));
#273339=CARTESIAN_POINT('Ctrl Pts',(10.8383054247334,12.9228591288348,44.5582993665063));
#273340=CARTESIAN_POINT('Ctrl Pts',(10.1651884842034,14.0986965788221,45.1772933060682));
#273341=CARTESIAN_POINT('Origin',(0.884028484203416,-17.542318193471,0.972561099047131));
#273342=CARTESIAN_POINT('',(10.1651884842034,29.7276425156794,27.8195903550057));
#273343=CARTESIAN_POINT('',(11.5201159294506,26.7032738510938,24.1023216086087));
#273344=CARTESIAN_POINT('Ctrl Pts',(10.1651884842034,29.7276425156794,27.8195903550057));
#273345=CARTESIAN_POINT('Ctrl Pts',(10.189490010882,29.7009800503245,27.7797076251619));
#273346=CARTESIAN_POINT('Ctrl Pts',(10.2135007848618,29.6741234027656,27.7397769795232));
#273347=CARTESIAN_POINT('Ctrl Pts',(10.8759790020178,28.9185609385563,26.6232509449527));
#273348=CARTESIAN_POINT('Ctrl Pts',(11.3015145825508,28.0494448912745,25.521081141234));
#273349=CARTESIAN_POINT('Ctrl Pts',(11.4908939831593,26.9437198726232,24.3494867025559));
#273350=CARTESIAN_POINT('Ctrl Pts',(11.5073957447759,26.8241320615886,24.2253078171096));
#273351=CARTESIAN_POINT('Ctrl Pts',(11.5201159294506,26.7032738510938,24.1023216086087));
#273352=CARTESIAN_POINT('',(10.1651884842034,29.3428715129083,28.4860332810845));
#273353=CARTESIAN_POINT('Origin',(10.1651884842034,-17.542318193471,0.972561099047131));
#273354=CARTESIAN_POINT('',(11.5201159294504,24.6114380135418,27.7254875603422));
#273355=CARTESIAN_POINT('Ctrl Pts',(11.5201159294506,24.6114380135418,27.7254875603422));
#273356=CARTESIAN_POINT('Ctrl Pts',(11.5064953958128,24.7901923791225,27.7717165825618));
#273357=CARTESIAN_POINT('Ctrl Pts',(11.4885385348232,24.9694097219034,27.8160020905446));
#273358=CARTESIAN_POINT('Ctrl Pts',(11.2877548088084,26.5892124826229,28.1977540296707));
#273359=CARTESIAN_POINT('Ctrl Pts',(10.8383054247334,28.0169230344847,28.3988103565001));
#273360=CARTESIAN_POINT('Ctrl Pts',(10.1651884842034,29.3428715129083,28.4860332810845));
#273361=CARTESIAN_POINT('Ctrl Pts',(11.5520284842034,23.7006061655499,27.6188808395637));
#273362=CARTESIAN_POINT('Ctrl Pts',(11.5520284842034,23.8243746910238,27.6163993857689));
#273363=CARTESIAN_POINT('Ctrl Pts',(11.5505455200547,23.9482745265803,27.6207381048773));
#273364=CARTESIAN_POINT('Ctrl Pts',(11.547251509512,24.0717890993467,27.631919614997));
#273365=CARTESIAN_POINT('Ctrl Pts',(11.544044159792,24.1920541759846,27.6428069551817));
#273366=CARTESIAN_POINT('Ctrl Pts',(11.5391193593529,24.311953775325,27.6601819444671));
#273367=CARTESIAN_POINT('Ctrl Pts',(11.5322066763546,24.4309746622713,27.6840729200195));
#273368=CARTESIAN_POINT('Ctrl Pts',(11.5286983877109,24.4913795189887,27.6961979427118));
#273369=CARTESIAN_POINT('Ctrl Pts',(11.5246786424116,24.5515574771146,27.7100014006615));
#273370=CARTESIAN_POINT('Ctrl Pts',(11.5201159294506,24.6114380135418,27.7254875603422));
#273371=CARTESIAN_POINT('Ctrl Pts',(11.5201159294506,26.7032738510938,24.1023216086087));
#273372=CARTESIAN_POINT('Ctrl Pts',(11.5379482942249,26.5338433160333,23.9299078435359));
#273373=CARTESIAN_POINT('Ctrl Pts',(11.5475950755165,26.3827546618124,23.7390531579732));
#273374=CARTESIAN_POINT('Ctrl Pts',(11.5516325551658,26.218935068599,23.47812217099));
#273375=CARTESIAN_POINT('Ctrl Pts',(11.5520284842034,26.1864194175169,23.4228829411106));
#273376=CARTESIAN_POINT('Ctrl Pts',(11.5520284842034,26.1555337986896,23.3668214500611));
#273377=CARTESIAN_POINT('Origin',(0.884028484203416,-17.542318193471,0.972561099047131));
#273378=CARTESIAN_POINT('Ctrl Pts',(11.5520284842034,28.3394307068726,18.4617086838663));
#273379=CARTESIAN_POINT('Ctrl Pts',(11.5520284842034,28.4599764800091,18.4335490439404));
#273380=CARTESIAN_POINT('Ctrl Pts',(11.5505455736236,28.5820687040887,18.4120329930338));
#273381=CARTESIAN_POINT('Ctrl Pts',(11.5472516844235,28.7052067728467,18.3972900560855));
#273382=CARTESIAN_POINT('Ctrl Pts',(11.544044459049,28.8251050191691,18.3829350129735));
#273383=CARTESIAN_POINT('Ctrl Pts',(11.539119853862,28.9459946217007,18.3750015769573));
#273384=CARTESIAN_POINT('Ctrl Pts',(11.5322074541281,29.067379435199,18.3736241726326));
#273385=CARTESIAN_POINT('Ctrl Pts',(11.528698981281,29.1289897787257,18.3729250542571));
#273386=CARTESIAN_POINT('Ctrl Pts',(11.5246789788102,29.1907271647795,18.3739151171815));
#273387=CARTESIAN_POINT('Ctrl Pts',(11.5201159294506,29.2525234772274,18.3766132024512));
#273388=CARTESIAN_POINT('',(11.5201159294506,30.5453491237196,14.397704993804));
#273389=CARTESIAN_POINT('Ctrl Pts',(11.5201159294506,30.5453491237196,14.397704993804));
#273390=CARTESIAN_POINT('Ctrl Pts',(11.5379482942249,30.3437742149424,14.264285472185));
#273391=CARTESIAN_POINT('Ctrl Pts',(11.5475950755165,30.1563062899423,14.1090145169754));
#273392=CARTESIAN_POINT('Ctrl Pts',(11.5516325551658,29.9418159451973,13.887845506715));
#273393=CARTESIAN_POINT('Ctrl Pts',(11.5520284842034,29.8985259574212,13.8405737705366));
#273394=CARTESIAN_POINT('Ctrl Pts',(11.5520284842034,29.8566594240743,13.7921588388053));
#273395=CARTESIAN_POINT('',(10.1651884842034,34.2764917070059,17.4049408966648));
#273396=CARTESIAN_POINT('Ctrl Pts',(10.1651884842034,34.2764917070059,17.4049408966648));
#273397=CARTESIAN_POINT('Ctrl Pts',(10.189490010882,34.2421197946932,17.3714731384106));
#273398=CARTESIAN_POINT('Ctrl Pts',(10.2135007848618,34.2075479812695,17.337998884187));
#273399=CARTESIAN_POINT('Ctrl Pts',(10.8759790020178,33.236357554009,16.4029618917673));
#273400=CARTESIAN_POINT('Ctrl Pts',(11.3015145825508,32.1570797901417,15.5055765295658));
#273401=CARTESIAN_POINT('Ctrl Pts',(11.4908939831593,30.8319293353782,14.589477398547));
#273402=CARTESIAN_POINT('Ctrl Pts',(11.5073957447759,30.6891365629007,14.4928758236793));
#273403=CARTESIAN_POINT('Ctrl Pts',(11.5201159294506,30.5453491237196,14.397704993804));
#273404=CARTESIAN_POINT('Origin',(10.1651884842034,-17.542318193471,0.972561099047131));
#273405=CARTESIAN_POINT('Origin',(0.884028484203416,-17.542318193471,0.972561099047131));
#273406=CARTESIAN_POINT('',(11.5201159294503,18.1280311274453,35.9051306570905));
#273407=CARTESIAN_POINT('Ctrl Pts',(11.5520284842034,17.2592679242297,35.6114809593723));
#273408=CARTESIAN_POINT('Ctrl Pts',(11.5520284842034,17.3808488290273,35.6347868646574));
#273409=CARTESIAN_POINT('Ctrl Pts',(11.5505454934864,17.5011401217583,35.6647913142035));
#273410=CARTESIAN_POINT('Ctrl Pts',(11.5472514229156,17.6196318266977,35.7014090350157));
#273411=CARTESIAN_POINT('Ctrl Pts',(11.5440440116058,17.7350062931456,35.7370634295862));
#273412=CARTESIAN_POINT('Ctrl Pts',(11.5391191144822,17.8486743622293,35.7789878343029));
#273413=CARTESIAN_POINT('Ctrl Pts',(11.5322062913615,17.9601281306309,35.8271032630006));
#273414=CARTESIAN_POINT('Ctrl Pts',(11.5286980938805,18.0166899466528,35.8515214236859));
#273415=CARTESIAN_POINT('Ctrl Pts',(11.5246784758745,18.0726808983853,35.8775340508797));
#273416=CARTESIAN_POINT('Ctrl Pts',(11.5201159294506,18.1280311274453,35.9051306570905));
#273417=CARTESIAN_POINT('',(11.5201159294502,20.927453892214,32.7960567002406));
#273418=CARTESIAN_POINT('Ctrl Pts',(11.5201159294506,20.927453892214,32.7960567002406));
#273419=CARTESIAN_POINT('Ctrl Pts',(11.5379482942249,20.7975726582702,32.5921840005807));
#273420=CARTESIAN_POINT('Ctrl Pts',(11.5475950755165,20.6894665740218,32.3740868502464));
#273421=CARTESIAN_POINT('Ctrl Pts',(11.5516325551658,20.5834774346573,32.0847978227575));
#273422=CARTESIAN_POINT('Ctrl Pts',(11.5520284842034,20.5631572102486,32.0240053185899));
#273423=CARTESIAN_POINT('Ctrl Pts',(11.5520284842034,20.5446023556894,31.9627474243939));
#273424=CARTESIAN_POINT('',(10.1651884842034,23.1128692149255,37.0608958085218));
#273425=CARTESIAN_POINT('Ctrl Pts',(10.1651884842034,23.1128692149255,37.0608958085218));
#273426=CARTESIAN_POINT('Ctrl Pts',(10.189490010882,23.0950814742053,37.0163411737611));
#273427=CARTESIAN_POINT('Ctrl Pts',(10.2135007848618,23.0771137568819,36.9716992975302));
#273428=CARTESIAN_POINT('Ctrl Pts',(10.8759790020178,22.5702009610007,35.722481766206));
#273429=CARTESIAN_POINT('Ctrl Pts',(11.3015145825508,21.9492311720522,34.4636976301901));
#273430=CARTESIAN_POINT('Ctrl Pts',(11.4908939831593,21.1112570786853,33.0878121827568));
#273431=CARTESIAN_POINT('Ctrl Pts',(11.5073957447759,21.0201007902818,32.9414831999023));
#273432=CARTESIAN_POINT('Ctrl Pts',(11.5201159294506,20.927453892214,32.7960567002406));
#273433=CARTESIAN_POINT('',(10.1651884842034,22.5979451061385,37.632776967928));
#273434=CARTESIAN_POINT('Origin',(10.1651884842034,-17.542318193471,0.972561099047131));
#273435=CARTESIAN_POINT('Ctrl Pts',(11.5201159294506,18.1280311274453,35.9051306570905));
#273436=CARTESIAN_POINT('Ctrl Pts',(11.5064953958128,18.2932677270842,35.9875145866478));
#273437=CARTESIAN_POINT('Ctrl Pts',(11.4885385348232,18.4593612660918,36.0680937307899));
#273438=CARTESIAN_POINT('Ctrl Pts',(11.2877548088084,19.9643967590149,36.778279404894));
#273439=CARTESIAN_POINT('Ctrl Pts',(10.8383054247334,21.3191064490001,37.2717798834305));
#273440=CARTESIAN_POINT('Ctrl Pts',(10.1651884842034,22.5979451061385,37.632776967928));
#273441=CARTESIAN_POINT('Origin',(0.884028484203416,-17.542318193471,0.972561099047131));
#273442=CARTESIAN_POINT('',(10.1651884842034,-71.6452466383859,-4.32699539176734));
#273443=CARTESIAN_POINT('',(11.5201159294503,-67.370398971297,-2.16122297171674));
#273444=CARTESIAN_POINT('Ctrl Pts',(10.1651884842034,-71.6452466383859,
-4.32699539176736));
#273445=CARTESIAN_POINT('Ctrl Pts',(10.189490010882,-71.604667496618,-4.30140530673472));
#273446=CARTESIAN_POINT('Ctrl Pts',(10.2135007848618,-71.5638914714702,
-4.27585042946313));
#273447=CARTESIAN_POINT('Ctrl Pts',(10.8759790020178,-70.4195187631186,
-3.56316808256816));
#273448=CARTESIAN_POINT('Ctrl Pts',(11.3015145825508,-69.177248899896,-2.90978720834477));
#273449=CARTESIAN_POINT('Ctrl Pts',(11.4908939831593,-67.690588442671,-2.28922131294222));
#273450=CARTESIAN_POINT('Ctrl Pts',(11.5073957447759,-67.5308314381036,
-2.22441900102061));
#273451=CARTESIAN_POINT('Ctrl Pts',(11.5201159294506,-67.370398971297,-2.16122297171675));
#273452=CARTESIAN_POINT('',(10.1651884842034,-71.5648075951267,-5.09232176568469));
#273453=CARTESIAN_POINT('Origin',(10.1651884842034,-17.542318193471,0.972561099047131));
#273454=CARTESIAN_POINT('',(11.5201159294504,-66.9330862002819,-6.32197605563978));
#273455=CARTESIAN_POINT('Ctrl Pts',(11.5201159294506,-66.933086200282,-6.32197605563978));
#273456=CARTESIAN_POINT('Ctrl Pts',(11.5064953958128,-67.1151894763022,
-6.29150241830828));
#273457=CARTESIAN_POINT('Ctrl Pts',(11.4885385348232,-67.2969252045844,
-6.25906498258172));
#273458=CARTESIAN_POINT('Ctrl Pts',(11.2877548088084,-68.9319611611244,
-5.94897959517663));
#273459=CARTESIAN_POINT('Ctrl Pts',(10.8383054247334,-70.3180166260499,
-5.55195149213379));
#273460=CARTESIAN_POINT('Ctrl Pts',(10.1651884842034,-71.5648075951267,
-5.0923217656847));
#273461=CARTESIAN_POINT('Ctrl Pts',(11.5520284842034,-66.0576390431341,
-6.59505465837715));
#273462=CARTESIAN_POINT('Ctrl Pts',(11.5520284842034,-66.1696919168509,
-6.54244936087575));
#273463=CARTESIAN_POINT('Ctrl Pts',(11.5505456780052,-66.2846386577793,
-6.49602047434678));
#273464=CARTESIAN_POINT('Ctrl Pts',(11.5472520254149,-66.4020164824461,
-6.45599878354303));
#273465=CARTESIAN_POINT('Ctrl Pts',(11.5440450424203,-66.5163056120188,
-6.41703022863092));
#273466=CARTESIAN_POINT('Ctrl Pts',(11.5391208178552,-66.6328994339461,
-6.3841363514087));
#273467=CARTESIAN_POINT('Ctrl Pts',(11.532208970468,-66.7513405603435,-6.35755179799039));
#273468=CARTESIAN_POINT('Ctrl Pts',(11.5287001384983,-66.8114677575395,
-6.34405602389257));
#273469=CARTESIAN_POINT('Ctrl Pts',(11.5246796346431,-66.8720705537274,
-6.332186573129));
#273470=CARTESIAN_POINT('Ctrl Pts',(11.5201159294506,-66.9330862002819,
-6.32197605563978));
#273471=CARTESIAN_POINT('Ctrl Pts',(11.5201159294506,-67.370398971297,-2.16122297171675));
#273472=CARTESIAN_POINT('Ctrl Pts',(11.5379482942249,-67.1454894795807,
-2.07262876686444));
#273473=CARTESIAN_POINT('Ctrl Pts',(11.5475950755165,-66.9298355316947,
-1.95972762782341));
#273474=CARTESIAN_POINT('Ctrl Pts',(11.5516325551658,-66.674048692722,-1.78798674132045));
#273475=CARTESIAN_POINT('Ctrl Pts',(11.5520284842034,-66.6218763484463,
-1.750748500549));
#273476=CARTESIAN_POINT('Ctrl Pts',(11.5520284842034,-66.5708586689849,
-1.71209609297321));
#273477=CARTESIAN_POINT('Origin',(0.884028484203416,-17.542318193471,0.972561099047131));
#273478=CARTESIAN_POINT('',(11.5201159294509,-67.370398971297,4.1063451698103));
#273479=CARTESIAN_POINT('Ctrl Pts',(11.5520284842034,-66.5708586689849,
3.65721829106678));
#273480=CARTESIAN_POINT('Ctrl Pts',(11.5520284842034,-66.6695318325109,
3.73197581382481));
#273481=CARTESIAN_POINT('Ctrl Pts',(11.5505454936051,-66.7723200664417,
3.80129276827458));
#273482=CARTESIAN_POINT('Ctrl Pts',(11.5472514232079,-66.8788187601877,
3.86484722697449));
#273483=CARTESIAN_POINT('Ctrl Pts',(11.5440440121231,-66.98251572159,3.92672971603551));
#273484=CARTESIAN_POINT('Ctrl Pts',(11.5391191153365,-67.0897304064872,
3.98314865000039));
#273485=CARTESIAN_POINT('Ctrl Pts',(11.5322062926153,-67.200064263055,4.03377943485101));
#273486=CARTESIAN_POINT('Ctrl Pts',(11.5286980948493,-67.2560577413694,
4.05947412043318));
#273487=CARTESIAN_POINT('Ctrl Pts',(11.524678476432,-67.312854156827,4.08367766457325));
#273488=CARTESIAN_POINT('Ctrl Pts',(11.5201159294506,-67.370398971297,4.1063451698103));
#273489=CARTESIAN_POINT('',(11.5201159294503,-66.933086200282,8.26709825373337));
#273490=CARTESIAN_POINT('Ctrl Pts',(11.5201159294506,-66.9330862002821,
8.26709825373337));
#273491=CARTESIAN_POINT('Ctrl Pts',(11.5379482942249,-66.6946717496501,
8.30699514994484));
#273492=CARTESIAN_POINT('Ctrl Pts',(11.5475950755165,-66.4602568912234,
8.37259215128143));
#273493=CARTESIAN_POINT('Ctrl Pts',(11.5516325551658,-66.1743526702874,
8.4873990131825));
#273494=CARTESIAN_POINT('Ctrl Pts',(11.5520284842034,-66.1155781513076,
8.51297626873635));
#273495=CARTESIAN_POINT('Ctrl Pts',(11.5520284842034,-66.0576390431342,
8.54017685647076));
#273496=CARTESIAN_POINT('',(10.1651884842034,-71.5648075951268,7.03744396377821));
#273497=CARTESIAN_POINT('Ctrl Pts',(10.1651884842034,-71.5648075951268,
7.03744396377821));
#273498=CARTESIAN_POINT('Ctrl Pts',(10.189490010882,-71.5197947271194,7.05403796607858));
#273499=CARTESIAN_POINT('Ctrl Pts',(10.2135007848618,-71.4745965982113,
7.07055659563549));
#273500=CARTESIAN_POINT('Ctrl Pts',(10.8759790020178,-70.2070561874331,
7.52973665861706));
#273501=CARTESIAN_POINT('Ctrl Pts',(11.3015145825508,-68.8560873789502,
7.91055716538948));
#273502=CARTESIAN_POINT('Ctrl Pts',(11.4908939831593,-67.2728911150328,
8.20846811774117));
#273503=CARTESIAN_POINT('Ctrl Pts',(11.5073957447759,-67.1031520260743,
8.23863899472971));
#273504=CARTESIAN_POINT('Ctrl Pts',(11.5201159294506,-66.9330862002821,
8.26709825373337));
#273505=CARTESIAN_POINT('',(10.1651884842034,-71.645246638386,6.27211758986086));
#273506=CARTESIAN_POINT('Origin',(10.1651884842034,-17.542318193471,0.972561099047131));
#273507=CARTESIAN_POINT('Ctrl Pts',(11.5201159294507,-67.370398971297,4.10634516981029));
#273508=CARTESIAN_POINT('Ctrl Pts',(11.5064953958128,-67.5421870283591,
4.17401428507257));
#273509=CARTESIAN_POINT('Ctrl Pts',(11.4885385348232,-67.7132072728382,
4.24352786755159));
#273510=CARTESIAN_POINT('Ctrl Pts',(11.2877548088084,-69.2480433936481,
4.88678023553657));
#273511=CARTESIAN_POINT('Ctrl Pts',(10.8383054247334,-70.5212634369431,
5.5633094572317));
#273512=CARTESIAN_POINT('Ctrl Pts',(10.1651884842034,-71.645246638386,6.27211758986087));
#273513=CARTESIAN_POINT('Origin',(0.884028484203416,-17.542318193471,0.972561099047131));
#273514=CARTESIAN_POINT('',(11.5201159294503,-65.6299855106617,14.3977049938037));
#273515=CARTESIAN_POINT('Ctrl Pts',(11.5520284842034,-64.9412958110163,
13.792158838805));
#273516=CARTESIAN_POINT('Ctrl Pts',(11.5520284842034,-65.0222693835792,
13.8857975921066));
#273517=CARTESIAN_POINT('Ctrl Pts',(11.5505455075224,-65.1083992116548,
13.9749702764953));
#273518=CARTESIAN_POINT('Ctrl Pts',(11.5472514703206,-65.1993564521249,
14.0592778788253));
#273519=CARTESIAN_POINT('Ctrl Pts',(11.544044092433,-65.287920795488,14.1413675222917));
#273520=CARTESIAN_POINT('Ctrl Pts',(11.539119248065,-65.3810618737815,14.2188444200145));
#273521=CARTESIAN_POINT('Ctrl Pts',(11.5322065029564,-65.4784573259309,
14.2913082108836));
#273522=CARTESIAN_POINT('Ctrl Pts',(11.5286982551647,-65.5278859356303,
14.3280838955502));
#273523=CARTESIAN_POINT('Ctrl Pts',(11.5246785671409,-65.5784100024307,
14.3635679095943));
#273524=CARTESIAN_POINT('Ctrl Pts',(11.5201159294506,-65.6299855106617,
14.3977049938037));
#273525=CARTESIAN_POINT('Ctrl Pts',(11.5201159294506,-64.3371598641694,
18.3766132024509));
#273526=CARTESIAN_POINT('Ctrl Pts',(11.5379482942249,-64.095660310154,18.3660691042106));
#273527=CARTESIAN_POINT('Ctrl Pts',(11.5475950755165,-63.8527295953472,
18.381495064115));
#273528=CARTESIAN_POINT('Ctrl Pts',(11.5516325551658,-63.5492033788236,
18.4343502906445));
#273529=CARTESIAN_POINT('Ctrl Pts',(11.5520284842034,-63.4863954136504,
18.4471487121798));
#273530=CARTESIAN_POINT('Ctrl Pts',(11.5520284842034,-63.4240670938147,
18.461708683866));
#273531=CARTESIAN_POINT('',(10.1651884842034,-69.361128093948,17.4049408966644));
#273532=CARTESIAN_POINT('Origin',(10.1651884842034,-17.542318193471,0.972561099047131));
#273533=CARTESIAN_POINT('Ctrl Pts',(11.5201159294506,-65.6299855106617,
14.3977049938037));
#273534=CARTESIAN_POINT('Ctrl Pts',(11.5064953958128,-65.7839503863413,
14.4996121219473));
#273535=CARTESIAN_POINT('Ctrl Pts',(11.4885385348232,-65.9367807416874,
14.6031637740613));
#273536=CARTESIAN_POINT('Ctrl Pts',(11.2877548088084,-67.3043373233269,
15.5514699074779));
#273537=CARTESIAN_POINT('Ctrl Pts',(10.8383054247334,-68.4090761195119,
16.4779326744898));
#273538=CARTESIAN_POINT('Ctrl Pts',(10.1651884842034,-69.361128093948,17.4049408966644));
#273539=CARTESIAN_POINT('Origin',(0.884028484203416,-17.542318193471,0.972561099047131));
#273540=CARTESIAN_POINT('',(10.1651884842034,-64.4275078998505,28.4860332810842));
#273541=CARTESIAN_POINT('',(11.5201159294503,-59.6960744004839,27.7254875603419));
#273542=CARTESIAN_POINT('Ctrl Pts',(10.1651884842034,-64.4275078998505,
28.4860332810842));
#273543=CARTESIAN_POINT('Ctrl Pts',(10.189490010882,-64.379637209956,28.4828842736812));
#273544=CARTESIAN_POINT('Ctrl Pts',(10.2135007848618,-64.3316279326639,
28.4795910574541));
#273545=CARTESIAN_POINT('Ctrl Pts',(10.8759790020178,-62.9869067906345,
28.3835177865881));
#273546=CARTESIAN_POINT('Ctrl Pts',(11.3015145825508,-61.5978417176892,
28.1819261126647));
#273547=CARTESIAN_POINT('Ctrl Pts',(11.4908939831593,-60.0303486615357,
27.8101373762517));
#273548=CARTESIAN_POINT('Ctrl Pts',(11.5073957447759,-59.8630126866082,
27.7686607366359));
#273549=CARTESIAN_POINT('Ctrl Pts',(11.5201159294506,-59.6960744004839,
27.7254875603419));
#273550=CARTESIAN_POINT('',(10.1651884842034,-64.8122789026216,27.8195903550054));
#273551=CARTESIAN_POINT('Origin',(10.1651884842034,-17.542318193471,0.972561099047131));
#273552=CARTESIAN_POINT('',(11.5201159294506,-61.7879102380359,24.1023216086084));
#273553=CARTESIAN_POINT('Ctrl Pts',(11.5201159294506,-61.7879102380359,
24.1023216086084));
#273554=CARTESIAN_POINT('Ctrl Pts',(11.5064953958128,-61.9173229284605,
24.2340129191289));
#273555=CARTESIAN_POINT('Ctrl Pts',(11.4885385348232,-62.0452839747836,
24.3670769367845));
#273556=CARTESIAN_POINT('Ctrl Pts',(11.2877548088084,-63.1857922323705,
25.5789913071247));
#273557=CARTESIAN_POINT('Ctrl Pts',(10.8383054247334,-64.0737673949273,
26.7148967508734));
#273558=CARTESIAN_POINT('Ctrl Pts',(10.1651884842034,-64.8122789026216,
27.8195903550054));
#273559=CARTESIAN_POINT('Ctrl Pts',(11.5520284842034,-61.2401701856317,
23.3668214500608));
#273560=CARTESIAN_POINT('Ctrl Pts',(11.5520284842034,-61.2999060970714,
23.475250045364));
#273561=CARTESIAN_POINT('Ctrl Pts',(11.5505454879221,-61.3656142043454,
23.5803821574562));
#273562=CARTESIAN_POINT('Ctrl Pts',(11.5472514053777,-61.4370558175126,
23.6817591254573));
#273563=CARTESIAN_POINT('Ctrl Pts',(11.5440439814882,-61.5066179895845,
23.7804691318469));
#273564=CARTESIAN_POINT('Ctrl Pts',(11.5391190647213,-61.5816160066261,
23.8756186960842));
#273565=CARTESIAN_POINT('Ctrl Pts',(11.5322062136934,-61.6618177977578,
23.9667491847357));
#273566=CARTESIAN_POINT('Ctrl Pts',(11.5286980345291,-61.702519130892,24.0129966852584));
#273567=CARTESIAN_POINT('Ctrl Pts',(11.5246784421826,-61.7445604645659,
24.0582085586416));
#273568=CARTESIAN_POINT('Ctrl Pts',(11.5201159294506,-61.7879102380359,
24.1023216086084));
#273569=CARTESIAN_POINT('Ctrl Pts',(11.5201159294506,-59.6960744004839,
27.7254875603419));
#273570=CARTESIAN_POINT('Ctrl Pts',(11.5379482942249,-59.4620444324384,
27.6649632953391));
#273571=CARTESIAN_POINT('Ctrl Pts',(11.5475950755165,-59.2212150991993,
27.6295440253416));
#273572=CARTESIAN_POINT('Ctrl Pts',(11.5516325551658,-58.9133324392308,
27.6181375894728));
#273573=CARTESIAN_POINT('Ctrl Pts',(11.5520284842034,-58.8492360373286,
27.6175978245548));
#273574=CARTESIAN_POINT('Ctrl Pts',(11.5520284842034,-58.7852425524921,
27.6188808395635));
#273575=CARTESIAN_POINT('Origin',(0.884028484203416,-17.542318193471,0.972561099047131));
#273576=CARTESIAN_POINT('',(11.5201159294503,-56.0120902791562,32.7960567002403));
#273577=CARTESIAN_POINT('Ctrl Pts',(11.5520284842034,-55.6292387426316,
31.9627474243937));
#273578=CARTESIAN_POINT('Ctrl Pts',(11.5520284842034,-55.6651257148405,
32.0812264100182));
#273579=CARTESIAN_POINT('Ctrl Pts',(11.5505454874064,-55.7075397574413,
32.1977226423425));
#273580=CARTESIAN_POINT('Ctrl Pts',(11.5472514032083,-55.7563427586746,
32.3117378556073));
#273581=CARTESIAN_POINT('Ctrl Pts',(11.5440439778628,-55.8038618789157,
32.422753622907));
#273582=CARTESIAN_POINT('Ctrl Pts',(11.5391190587251,-55.8574383198082,
32.5314169312553));
#273583=CARTESIAN_POINT('Ctrl Pts',(11.5322062038027,-55.916940438255,32.6372309180193));
#273584=CARTESIAN_POINT('Ctrl Pts',(11.5286980270414,-55.9471369274812,
32.6909300298275));
#273585=CARTESIAN_POINT('Ctrl Pts',(11.5246784379819,-55.9788594516457,
32.7438947495814));
#273586=CARTESIAN_POINT('Ctrl Pts',(11.5201159294506,-56.0120902791562,
32.7960567002404));
#273587=CARTESIAN_POINT('',(11.5201159294502,-53.2126675143875,35.9051306570903));
#273588=CARTESIAN_POINT('Ctrl Pts',(11.5201159294506,-53.2126675143875,
35.9051306570903));
#273589=CARTESIAN_POINT('Ctrl Pts',(11.5379482942249,-52.9963353649162,
35.7972714261332));
#273590=CARTESIAN_POINT('Ctrl Pts',(11.5475950755165,-52.7681328107348,
35.7125549182932));
#273591=CARTESIAN_POINT('Ctrl Pts',(11.5516325551658,-52.4693496569467,
35.6373853360076));
#273592=CARTESIAN_POINT('Ctrl Pts',(11.5520284842034,-52.4067661386471,
35.6235309749533));
#273593=CARTESIAN_POINT('Ctrl Pts',(11.5520284842034,-52.3439043111719,
35.6114809593721));
#273594=CARTESIAN_POINT('',(10.1651884842034,-57.6825814930807,37.6327769679278));
#273595=CARTESIAN_POINT('Ctrl Pts',(10.1651884842034,-57.6825814930807,
37.6327769679277));
#273596=CARTESIAN_POINT('Ctrl Pts',(10.189490010882,-57.6364116080685,37.6197438978153));
#273597=CARTESIAN_POINT('Ctrl Pts',(10.2135007848618,-57.5901361468263,
37.6065409562473));
#273598=CARTESIAN_POINT('Ctrl Pts',(10.8759790020178,-56.2947751442824,
37.2329838705373));
#273599=CARTESIAN_POINT('Ctrl Pts',(11.3015145825508,-54.9779777416979,
36.7469945903893));
#273600=CARTESIAN_POINT('Ctrl Pts',(11.4908939831593,-53.5220373944691,
36.057430198237));
#273601=CARTESIAN_POINT('Ctrl Pts',(11.5073957447759,-53.3669815903493,
35.9820688172286));
#273602=CARTESIAN_POINT('Ctrl Pts',(11.5201159294506,-53.2126675143875,
35.9051306570903));
#273603=CARTESIAN_POINT('',(10.1651884842034,-58.1975056018677,37.0608958085216));
#273604=CARTESIAN_POINT('Origin',(10.1651884842034,-17.542318193471,0.972561099047131));
#273605=CARTESIAN_POINT('Ctrl Pts',(11.5201159294506,-56.0120902791562,
32.7960567002404));
#273606=CARTESIAN_POINT('Ctrl Pts',(11.5064953958128,-56.1112948287632,
32.9517766509429));
#273607=CARTESIAN_POINT('Ctrl Pts',(11.4885385348232,-56.2087940543137,
33.1085374980566));
#273608=CARTESIAN_POINT('Ctrl Pts',(11.2877548088084,-57.0724083042256,
34.5310936319262));
#273609=CARTESIAN_POINT('Ctrl Pts',(10.8383054247334,-57.7048110575729,
35.8267972338408));
#273610=CARTESIAN_POINT('Ctrl Pts',(10.1651884842034,-58.1975056018678,
37.0608958085216));
#273611=CARTESIAN_POINT('Origin',(0.884028484203416,-17.542318193471,0.972561099047131));
#273612=CARTESIAN_POINT('',(10.1651884842034,-49.1833329657644,45.177293306068));
#273613=CARTESIAN_POINT('',(11.5201159294506,-45.1702951976404,42.5580528390857));
#273614=CARTESIAN_POINT('Ctrl Pts',(10.1651884842034,-49.1833329657644,
45.177293306068));
#273615=CARTESIAN_POINT('Ctrl Pts',(10.189490010882,-49.1408817311572,45.1549457809496));
#273616=CARTESIAN_POINT('Ctrl Pts',(10.2135007848618,-49.0983625456755,
45.1324101459419));
#273617=CARTESIAN_POINT('Ctrl Pts',(10.8759790020178,-47.9089751742599,
44.4976954825594));
#273618=CARTESIAN_POINT('Ctrl Pts',(11.3015145825508,-46.7219958072243,
43.7485486597644));
#273619=CARTESIAN_POINT('Ctrl Pts',(11.4908939831593,-45.441239748471,42.7713458847071));
#273620=CARTESIAN_POINT('Ctrl Pts',(11.5073957447759,-45.3052407978392,
42.6653934162801));
#273621=CARTESIAN_POINT('Ctrl Pts',(11.5201159294506,-45.1702951976404,
42.5580528390857));
#273622=CARTESIAN_POINT('',(10.1651884842034,-49.8059055261334,44.7249678641907));
#273623=CARTESIAN_POINT('Origin',(10.1651884842034,-17.542318193471,0.972561099047131));
#273624=CARTESIAN_POINT('',(11.5201159294504,-48.5549566816847,40.0989523280257));
#273625=CARTESIAN_POINT('Ctrl Pts',(11.5201159294506,-48.5549566816847,
40.0989523280258));
#273626=CARTESIAN_POINT('Ctrl Pts',(11.5064953958128,-48.61961737562,40.2718952098375));
#273627=CARTESIAN_POINT('Ctrl Pts',(11.4885385348232,-48.6823935963883,
40.4455016851683));
#273628=CARTESIAN_POINT('Ctrl Pts',(11.2877548088084,-49.2313697518231,
42.0165270533355));
#273629=CARTESIAN_POINT('Ctrl Pts',(10.8383054247334,-49.5805610610345,
43.4154003485366));
#273630=CARTESIAN_POINT('Ctrl Pts',(10.1651884842034,-49.8059055261334,
44.7249678641907));
#273631=CARTESIAN_POINT('Ctrl Pts',(11.5520284842034,-48.3537261103113,
39.2042535488961));
#273632=CARTESIAN_POINT('Ctrl Pts',(11.5520284842034,-48.3641956404978,
39.3276041062429));
#273633=CARTESIAN_POINT('Ctrl Pts',(11.550545504126,-48.3814617755172,39.4503723241464));
#273634=CARTESIAN_POINT('Ctrl Pts',(11.5472514575585,-48.405493015199,39.5720421023164));
#273635=CARTESIAN_POINT('Ctrl Pts',(11.5440440708938,-48.4288920401097,
39.690510987317));
#273636=CARTESIAN_POINT('Ctrl Pts',(11.5391192124522,-48.4587050452548,
39.8079382320109));
#273637=CARTESIAN_POINT('Ctrl Pts',(11.5322064453586,-48.4949065665672,
39.9238104557194));
#273638=CARTESIAN_POINT('Ctrl Pts',(11.5286982114168,-48.5132788629418,
39.9826156870571));
#273639=CARTESIAN_POINT('Ctrl Pts',(11.5246785424948,-48.5332966106893,
40.0410198365814));
#273640=CARTESIAN_POINT('Ctrl Pts',(11.5201159294506,-48.5549566816847,
40.0989523280258));
#273641=CARTESIAN_POINT('Ctrl Pts',(11.5201159294506,-45.1702951976404,
42.5580528390857));
#273642=CARTESIAN_POINT('Ctrl Pts',(11.5379482942249,-44.9811156197522,
42.4075726081333));
#273643=CARTESIAN_POINT('Ctrl Pts',(11.5475950755165,-44.7755133912835,
42.2772613803582));
#273644=CARTESIAN_POINT('Ctrl Pts',(11.5516325551658,-44.4988880012169,
42.1416139231055));
#273645=CARTESIAN_POINT('Ctrl Pts',(11.5520284842034,-44.4405525665788,
42.1150504679734));
#273646=CARTESIAN_POINT('Ctrl Pts',(11.5520284842034,-44.38156975997,42.0901940653056));
#273647=CARTESIAN_POINT('Origin',(0.884028484203416,-17.542318193471,0.972561099047131));
#273648=CARTESIAN_POINT('',(11.5201159294504,-39.742421967128,45.6918369098492));
#273649=CARTESIAN_POINT('Ctrl Pts',(11.5520284842034,-39.7316071024862,
44.7748512573256));
#273650=CARTESIAN_POINT('Ctrl Pts',(11.5520284842034,-39.7162020260023,
44.897681447115));
#273651=CARTESIAN_POINT('Ctrl Pts',(11.5505455425311,-39.7075659332829,
45.0213551478053));
#273652=CARTESIAN_POINT('Ctrl Pts',(11.5472515828821,-39.7057753139112,
45.1453609704374));
#273653=CARTESIAN_POINT('Ctrl Pts',(11.5440442853249,-39.7040318046552,
45.2661042746653));
#273654=CARTESIAN_POINT('Ctrl Pts',(11.5391195667906,-39.7087784989904,
45.3871622545795));
#273655=CARTESIAN_POINT('Ctrl Pts',(11.5322070025992,-39.7200972254515,
45.5080274415157));
#273656=CARTESIAN_POINT('Ctrl Pts',(11.5286986366911,-39.7258418714236,
45.5693707129246));
#273657=CARTESIAN_POINT('Ctrl Pts',(11.5246787835194,-39.7332795799714,
45.630663768993));
#273658=CARTESIAN_POINT('Ctrl Pts',(11.5201159294506,-39.742421967128,45.6918369098492));
#273659=CARTESIAN_POINT('',(11.5201159294506,-35.9204477120687,47.3934894827124));
#273660=CARTESIAN_POINT('Ctrl Pts',(11.5201159294506,-35.9204477120687,
47.3934894827124));
#273661=CARTESIAN_POINT('Ctrl Pts',(11.5379482942249,-35.7666887611015,
47.2069649599417));
#273662=CARTESIAN_POINT('Ctrl Pts',(11.5475950755165,-35.5926726623188,
47.0367542381881));
#273663=CARTESIAN_POINT('Ctrl Pts',(11.5516325551658,-35.3502948929158,
46.8465573507588));
#273664=CARTESIAN_POINT('Ctrl Pts',(11.5520284842034,-35.298757080357,46.8084457520039));
#273665=CARTESIAN_POINT('Ctrl Pts',(11.5520284842034,-35.2462311262942,
46.7718693063201));
#273666=CARTESIAN_POINT('',(10.1651884842034,-39.3012202624647,50.7898507289222));
#273667=CARTESIAN_POINT('Ctrl Pts',(10.1651884842034,-39.3012202624647,
50.7898507289222));
#273668=CARTESIAN_POINT('Ctrl Pts',(10.189490010882,-39.2643430009184,50.7591654428808));
#273669=CARTESIAN_POINT('Ctrl Pts',(10.2135007848618,-39.2274383836324,
50.7282820298214));
#273670=CARTESIAN_POINT('Ctrl Pts',(10.8759790020178,-38.1960065787899,
49.8601498652548));
#273671=CARTESIAN_POINT('Ctrl Pts',(11.3015145825508,-37.1907219414015,
48.8805868107745));
#273672=CARTESIAN_POINT('Ctrl Pts',(11.4908939831593,-36.1411253566406,
47.6584541032212));
#273673=CARTESIAN_POINT('Ctrl Pts',(11.5073957447759,-36.0301270662348,
47.5265411786622));
#273674=CARTESIAN_POINT('Ctrl Pts',(11.5201159294506,-35.9204477120687,
47.3934894827124));
#273675=CARTESIAN_POINT('',(10.1651884842034,-40.004231866093,50.4768497968822));
#273676=CARTESIAN_POINT('Origin',(10.1651884842034,-17.542318193471,0.972561099047131));
#273677=CARTESIAN_POINT('Ctrl Pts',(11.5201159294506,-39.742421967128,45.6918369098492));
#273678=CARTESIAN_POINT('Ctrl Pts',(11.5064953958128,-39.7697128227903,
45.8744442889629));
#273679=CARTESIAN_POINT('Ctrl Pts',(11.4885385348232,-39.7950224166949,
46.0573089564827));
#273680=CARTESIAN_POINT('Ctrl Pts',(11.2877548088084,-40.0053675853803,
47.7081422117425));
#273681=CARTESIAN_POINT('Ctrl Pts',(10.8383054247334,-40.0560861146374,
49.1490477246911));
#273682=CARTESIAN_POINT('Ctrl Pts',(10.1651884842034,-40.004231866093,50.4768497968821));
#273683=CARTESIAN_POINT('Origin',(0.884028484203416,-17.542318193471,0.972561099047131));
#273684=CARTESIAN_POINT('',(10.1651884842034,-17.9270891962415,-53.3879403389487));
#273685=CARTESIAN_POINT('Ctrl Pts',(10.1651884842034,-17.9270891962415,
-53.3879403389487));
#273686=CARTESIAN_POINT('Ctrl Pts',(10.189490010882,-17.9482974207811,-53.3449086017019));
#273687=CARTESIAN_POINT('Ctrl Pts',(10.2135007848618,-17.9694500505142,
-53.3016847398361));
#273688=CARTESIAN_POINT('Ctrl Pts',(10.8759790020178,-18.5586087283343,
-52.0890854343996));
#273689=CARTESIAN_POINT('Ctrl Pts',(11.3015145825508,-19.0785577539979,
-50.7853239567576));
#273690=CARTESIAN_POINT('Ctrl Pts',(11.4908939831593,-19.5403257915001,
-49.2419407816664));
#273691=CARTESIAN_POINT('Ctrl Pts',(11.5073957447759,-19.588073955393,-49.0762852566043));
#273692=CARTESIAN_POINT('Ctrl Pts',(11.5201159294506,-19.6341540310225,
-48.9101258718094));
#273693=CARTESIAN_POINT('',(10.1651884842034,-17.1575471906993,-53.3879403389487));
#273694=CARTESIAN_POINT('Origin',(10.1651884842034,-17.542318193471,0.972561099047131));
#273695=CARTESIAN_POINT('Ctrl Pts',(11.5201159294506,-15.4504823559185,
-48.9101258718094));
#273696=CARTESIAN_POINT('Ctrl Pts',(11.5064953958128,-15.4998240310746,
-49.0880462045494));
#273697=CARTESIAN_POINT('Ctrl Pts',(11.4885385348232,-15.5510803275324,
-49.2653957301879));
#273698=CARTESIAN_POINT('Ctrl Pts',(11.2877548088084,-16.030374830665,-50.8590620396541));
#273699=CARTESIAN_POINT('Ctrl Pts',(10.8383054247334,-16.57011021997,-52.1960238102323));
#273700=CARTESIAN_POINT('Ctrl Pts',(10.1651884842034,-17.1575471906993,
-53.3879403389487));
#273701=CARTESIAN_POINT('Origin',(0.884028484203416,-17.542318193471,0.972561099047131));
#273702=CARTESIAN_POINT('',(10.1651884842034,-29.2208647943379,-52.1200345674514));
#273703=CARTESIAN_POINT('Ctrl Pts',(10.1651884842034,-29.2208647943379,
-52.1200345674514));
#273704=CARTESIAN_POINT('Ctrl Pts',(10.189490010882,-29.2326627670373,-52.0735337390848));
#273705=CARTESIAN_POINT('Ctrl Pts',(10.2135007848618,-29.2443664148558,
-52.0268565432932));
#273706=CARTESIAN_POINT('Ctrl Pts',(10.8759790020178,-29.5685369901393,
-50.7182624651635));
#273707=CARTESIAN_POINT('Ctrl Pts',(11.3015145825508,-29.8060566288565,
-49.334887822814));
#273708=CARTESIAN_POINT('Ctrl Pts',(11.4908939831593,-29.9368465213218,
-47.729224299643));
#273709=CARTESIAN_POINT('Ctrl Pts',(11.5073957447759,-29.9491095529641,
-47.5572613437668));
#273710=CARTESIAN_POINT('Ctrl Pts',(11.5201159294507,-29.9596361897448,
-47.3851523537531));
#273711=CARTESIAN_POINT('',(10.1651884842034,-28.4681391279529,-52.280031346979));
#273712=CARTESIAN_POINT('Origin',(10.1651884842034,-17.542318193471,0.972561099047131));
#273713=CARTESIAN_POINT('Ctrl Pts',(11.5201159294506,-25.8673877784838,
-48.2549866055504));
#273714=CARTESIAN_POINT('Ctrl Pts',(11.5064953958128,-25.9526429368648,
-48.4187602410323));
#273715=CARTESIAN_POINT('Ctrl Pts',(11.4885385348232,-26.0396522000087,
-48.5815774707652));
#273716=CARTESIAN_POINT('Ctrl Pts',(11.2877548088084,-26.8398148252932,
-50.040767417194));
#273717=CARTESIAN_POINT('Ctrl Pts',(10.8383054247334,-27.6457256836526,
-51.2362960679732));
#273718=CARTESIAN_POINT('Ctrl Pts',(10.1651884842034,-28.4681391279529,
-52.2800313469789));
#273719=CARTESIAN_POINT('Origin',(0.884028484203416,-17.542318193471,0.972561099047131));
#273720=CARTESIAN_POINT('',(10.1651884842034,-40.0042318660923,-48.5317275987882));
#273721=CARTESIAN_POINT('Ctrl Pts',(10.1651884842034,-40.0042318660923,
-48.5317275987882));
#273722=CARTESIAN_POINT('Ctrl Pts',(10.189490010882,-40.0061039589316,-48.4837899886371));
#273723=CARTESIAN_POINT('Ctrl Pts',(10.2135007848618,-40.0078471192654,
-48.4356994763579));
#273724=CARTESIAN_POINT('Ctrl Pts',(10.8759790020178,-40.0528617823294,
-47.0883024660804));
#273725=CARTESIAN_POINT('Ctrl Pts',(11.3015145825508,-39.9975712861425,
-45.6857747690621));
#273726=CARTESIAN_POINT('Ctrl Pts',(11.4908939831593,-39.7916668876708,
-44.0880060986022));
#273727=CARTESIAN_POINT('Ctrl Pts',(11.5073957447759,-39.7679088337352,
-43.9172513182535));
#273728=CARTESIAN_POINT('Ctrl Pts',(11.5201159294506,-39.7424219671274,
-43.7467147117552));
#273729=CARTESIAN_POINT('',(10.1651884842034,-39.301220262464,-48.8447285308283));
#273730=CARTESIAN_POINT('Origin',(10.1651884842034,-17.542318193471,0.972561099047131));
#273731=CARTESIAN_POINT('Ctrl Pts',(11.5201159294506,-35.9204477120681,
-45.4483672846184));
#273732=CARTESIAN_POINT('Ctrl Pts',(11.5064953958128,-36.037890294153,-45.5908365290986));
#273733=CARTESIAN_POINT('Ctrl Pts',(11.4885385348232,-36.1568498016669,
-45.7320055687029));
#273734=CARTESIAN_POINT('Ctrl Pts',(11.2877548088084,-37.242909602772,-46.9929455494649));
#273735=CARTESIAN_POINT('Ctrl Pts',(10.8383054247334,-38.2797737584862,
-47.9947907416233));
#273736=CARTESIAN_POINT('Ctrl Pts',(10.1651884842034,-39.301220262464,-48.8447285308282));
#273737=CARTESIAN_POINT('Origin',(0.884028484203416,-17.542318193471,0.972561099047131));
#273738=CARTESIAN_POINT('',(10.1651884842034,-49.8059055261328,-42.7798456660969));
#273739=CARTESIAN_POINT('Ctrl Pts',(10.1651884842034,-49.8059055261328,
-42.7798456660969));
#273740=CARTESIAN_POINT('Ctrl Pts',(10.189490010882,-49.7977699196717,-42.7325663777551));
#273741=CARTESIAN_POINT('Ctrl Pts',(10.2135007848618,-49.7894764080497,
-42.6851643351388));
#273742=CARTESIAN_POINT('Ctrl Pts',(10.8759790020178,-49.5533678021139,
-41.3578521075907));
#273743=CARTESIAN_POINT('Ctrl Pts',(11.3015145825508,-49.2076836310195,
-39.9974685463379));
#273744=CARTESIAN_POINT('Ctrl Pts',(11.4908939831593,-48.674083951863,-38.477424886433));
#273745=CARTESIAN_POINT('Ctrl Pts',(11.5073957447759,-48.6153431533102,
-38.3153410848854));
#273746=CARTESIAN_POINT('Ctrl Pts',(11.5201159294506,-48.5549566816842,
-38.1538301299319));
#273747=CARTESIAN_POINT('',(10.1651884842034,-49.1833329657638,-43.2321711079742));
#273748=CARTESIAN_POINT('Origin',(10.1651884842034,-17.542318193471,0.972561099047131));
#273749=CARTESIAN_POINT('Ctrl Pts',(11.5201159294506,-45.1702951976399,
-40.6129306409918));
#273750=CARTESIAN_POINT('Ctrl Pts',(11.5064953958128,-45.3147923990396,
-40.7278689048432));
#273751=CARTESIAN_POINT('Ctrl Pts',(11.4885385348232,-45.4605030496141,
-40.841219989884));
#273752=CARTESIAN_POINT('Ctrl Pts',(11.2877548088084,-46.7849940017385,
-41.8488008771588));
#273753=CARTESIAN_POINT('Ctrl Pts',(10.8383054247334,-48.0074955157765,
-42.6131771684123));
#273754=CARTESIAN_POINT('Ctrl Pts',(10.1651884842034,-49.1833329657638,
-43.2321711079742));
#273755=CARTESIAN_POINT('Origin',(0.884028484203416,-17.542318193471,0.972561099047131));
#273756=CARTESIAN_POINT('',(10.1651884842034,-58.1975056018673,-35.1157736104279));
#273757=CARTESIAN_POINT('Ctrl Pts',(10.1651884842034,-58.1975056018673,
-35.1157736104278));
#273758=CARTESIAN_POINT('Ctrl Pts',(10.189490010882,-58.179717861147,-35.0712189756671));
#273759=CARTESIAN_POINT('Ctrl Pts',(10.2135007848618,-58.1617501438237,
-35.0265770994362));
#273760=CARTESIAN_POINT('Ctrl Pts',(10.8759790020178,-57.6548373479424,
-33.7773595681121));
#273761=CARTESIAN_POINT('Ctrl Pts',(11.3015145825508,-57.033867558994,-32.5185754320962));
#273762=CARTESIAN_POINT('Ctrl Pts',(11.4908939831593,-56.1958934656271,
-31.1426899846628));
#273763=CARTESIAN_POINT('Ctrl Pts',(11.5073957447759,-56.1047371772236,
-30.9963610018083));
#273764=CARTESIAN_POINT('Ctrl Pts',(11.5201159294506,-56.0120902791558,
-30.8509345021466));
#273765=CARTESIAN_POINT('',(10.1651884842034,-57.6825814930802,-35.687654769834));
#273766=CARTESIAN_POINT('Origin',(10.1651884842034,-17.542318193471,0.972561099047131));
#273767=CARTESIAN_POINT('Ctrl Pts',(11.5201159294506,-53.212667514387,-33.9600084589965));
#273768=CARTESIAN_POINT('Ctrl Pts',(11.5064953958128,-53.3779041140259,
-34.0423923885538));
#273769=CARTESIAN_POINT('Ctrl Pts',(11.4885385348232,-53.5439976530335,
-34.1229715326959));
#273770=CARTESIAN_POINT('Ctrl Pts',(11.2877548088084,-55.0490331459566,
-34.8331572068));
#273771=CARTESIAN_POINT('Ctrl Pts',(10.8383054247334,-56.4037428359418,
-35.3266576853365));
#273772=CARTESIAN_POINT('Ctrl Pts',(10.1651884842034,-57.6825814930802,
-35.687654769834));
#273773=CARTESIAN_POINT('Origin',(0.884028484203416,-17.542318193471,0.972561099047131));
#273774=CARTESIAN_POINT('',(10.1651884842034,-64.8122789026212,-25.8744681569117));
#273775=CARTESIAN_POINT('Ctrl Pts',(10.1651884842034,-64.8122789026212,
-25.8744681569117));
#273776=CARTESIAN_POINT('Ctrl Pts',(10.189490010882,-64.7856164372663,-25.8345854270679));
#273777=CARTESIAN_POINT('Ctrl Pts',(10.2135007848618,-64.7587597897074,
-25.7946547814292));
#273778=CARTESIAN_POINT('Ctrl Pts',(10.8759790020178,-64.0031973254981,
-24.6781287468588));
#273779=CARTESIAN_POINT('Ctrl Pts',(11.3015145825508,-63.1340812782164,
-23.5759589431401));
#273780=CARTESIAN_POINT('Ctrl Pts',(11.4908939831593,-62.028356259565,-22.4043645044619));
#273781=CARTESIAN_POINT('Ctrl Pts',(11.5073957447759,-61.9087684485304,
-22.2801856190156));
#273782=CARTESIAN_POINT('Ctrl Pts',(11.5201159294506,-61.7879102380356,
-22.1571994105147));
#273783=CARTESIAN_POINT('',(10.1651884842034,-64.4275078998501,-26.5409110829905));
#273784=CARTESIAN_POINT('Origin',(10.1651884842034,-17.542318193471,0.972561099047131));
#273785=CARTESIAN_POINT('Ctrl Pts',(11.5201159294506,-59.6960744004836,
-25.7803653622482));
#273786=CARTESIAN_POINT('Ctrl Pts',(11.5064953958128,-59.8748287660643,
-25.8265943844678));
#273787=CARTESIAN_POINT('Ctrl Pts',(11.4885385348232,-60.0540461088452,
-25.8708798924506));
#273788=CARTESIAN_POINT('Ctrl Pts',(11.2877548088084,-61.6738488695646,
-26.2526318315767));
#273789=CARTESIAN_POINT('Ctrl Pts',(10.8383054247334,-63.1015594214264,
-26.4536881584061));
#273790=CARTESIAN_POINT('Ctrl Pts',(10.1651884842034,-64.4275078998501,
-26.5409110829905));
#273791=CARTESIAN_POINT('Origin',(0.884028484203416,-17.542318193471,0.972561099047131));
#273792=CARTESIAN_POINT('',(11.5201159294506,-65.6299855106615,-12.4525827957101));
#273793=CARTESIAN_POINT('Ctrl Pts',(11.5201159294506,-65.6299855106615,
-12.4525827957101));
#273794=CARTESIAN_POINT('Ctrl Pts',(11.5379482942249,-65.4284106018844,
-12.3191632740911));
#273795=CARTESIAN_POINT('Ctrl Pts',(11.5475950755165,-65.2409426768843,
-12.1638923188816));
#273796=CARTESIAN_POINT('Ctrl Pts',(11.5516325551658,-65.0264523321392,
-11.9427233086211));
#273797=CARTESIAN_POINT('Ctrl Pts',(11.5520284842034,-64.9831623443631,
-11.8954515724427));
#273798=CARTESIAN_POINT('Ctrl Pts',(11.5520284842034,-64.9412958110162,
-11.8470366407114));
#273799=CARTESIAN_POINT('',(10.1651884842034,-69.3611280939478,-15.4598186985709));
#273800=CARTESIAN_POINT('Ctrl Pts',(10.1651884842034,-69.3611280939478,
-15.4598186985709));
#273801=CARTESIAN_POINT('Ctrl Pts',(10.189490010882,-69.3267561816351,-15.4263509403167));
#273802=CARTESIAN_POINT('Ctrl Pts',(10.2135007848618,-69.2921843682114,
-15.3928766860931));
#273803=CARTESIAN_POINT('Ctrl Pts',(10.8759790020178,-68.3209939409509,
-14.4578396936734));
#273804=CARTESIAN_POINT('Ctrl Pts',(11.3015145825508,-67.2417161770836,
-13.5604543314719));
#273805=CARTESIAN_POINT('Ctrl Pts',(11.4908939831593,-65.9165657223201,
-12.6443552004531));
#273806=CARTESIAN_POINT('Ctrl Pts',(11.5073957447759,-65.7737729498426,
-12.5477536255854));
#273807=CARTESIAN_POINT('Ctrl Pts',(11.5201159294506,-65.6299855106615,
-12.4525827957101));
#273808=CARTESIAN_POINT('',(10.1651884842034,-69.1233265363499,-16.1916966375046));
#273809=CARTESIAN_POINT('Origin',(10.1651884842034,-17.542318193471,0.972561099047131));
#273810=CARTESIAN_POINT('Ctrl Pts',(11.5201159294507,-64.3371598641692,
-16.4314910043572));
#273811=CARTESIAN_POINT('Ctrl Pts',(11.5064953958128,-64.5216195721572,
-16.4395446891366));
#273812=CARTESIAN_POINT('Ctrl Pts',(11.4885385348232,-64.7061280608517,
-16.4456010717559));
#273813=CARTESIAN_POINT('Ctrl Pts',(11.2877548088084,-66.369904936048,-16.4822348843151));
#273814=CARTESIAN_POINT('Ctrl Pts',(10.8383054247334,-67.8082185477548,
-16.3820599331797));
#273815=CARTESIAN_POINT('Ctrl Pts',(10.1651884842034,-69.1233265363499,
-16.1916966375046));
#273816=CARTESIAN_POINT('Origin',(0.884028484203416,-17.542318193471,0.972561099047131));
#273817=CARTESIAN_POINT('',(10.1651884842034,29.3428715129087,-26.5409110829896));
#273818=CARTESIAN_POINT('Ctrl Pts',(10.1651884842034,29.3428715129087,-26.5409110829896));
#273819=CARTESIAN_POINT('Ctrl Pts',(10.189490010882,29.2950008230142,-26.5377620755867));
#273820=CARTESIAN_POINT('Ctrl Pts',(10.2135007848618,29.2469915457221,-26.5344688593595));
#273821=CARTESIAN_POINT('Ctrl Pts',(10.8759790020178,27.9022704036928,-26.4383955884935));
#273822=CARTESIAN_POINT('Ctrl Pts',(11.3015145825508,26.5132053307474,-26.2368039145702));
#273823=CARTESIAN_POINT('Ctrl Pts',(11.4908939831593,24.9457122745938,-25.8650151781571));
#273824=CARTESIAN_POINT('Ctrl Pts',(11.5073957447759,24.7783762996664,-25.8235385385413));
#273825=CARTESIAN_POINT('Ctrl Pts',(11.5201159294506,24.6114380135421,-25.7803653622474));
#273826=CARTESIAN_POINT('',(10.1651884842034,29.7276425156798,-25.8744681569108));
#273827=CARTESIAN_POINT('Origin',(10.1651884842034,-17.542318193471,0.972561099047131));
#273828=CARTESIAN_POINT('Ctrl Pts',(11.5201159294506,26.7032738510941,-22.1571994105139));
#273829=CARTESIAN_POINT('Ctrl Pts',(11.5064953958128,26.8326865415187,-22.2888907210343));
#273830=CARTESIAN_POINT('Ctrl Pts',(11.4885385348232,26.9606475878418,-22.4219547386899));
#273831=CARTESIAN_POINT('Ctrl Pts',(11.2877548088084,28.1011558454287,-23.6338691090301));
#273832=CARTESIAN_POINT('Ctrl Pts',(10.8383054247334,28.9891310079854,-24.7697745527788));
#273833=CARTESIAN_POINT('Ctrl Pts',(10.1651884842034,29.7276425156798,-25.8744681569108));
#273834=CARTESIAN_POINT('Origin',(0.884028484203416,-17.542318193471,0.972561099047131));
#273835=CARTESIAN_POINT('',(10.1651884842034,22.597945106139,-35.6876547698332));
#273836=CARTESIAN_POINT('Ctrl Pts',(10.1651884842034,22.5979451061389,-35.6876547698332));
#273837=CARTESIAN_POINT('Ctrl Pts',(10.189490010882,22.5517752211267,-35.6746216997208));
#273838=CARTESIAN_POINT('Ctrl Pts',(10.2135007848618,22.5054997598846,-35.6614187581527));
#273839=CARTESIAN_POINT('Ctrl Pts',(10.8759790020178,21.2101387573406,-35.2878616724428));
#273840=CARTESIAN_POINT('Ctrl Pts',(11.3015145825508,19.8933413547562,-34.8018723922948));
#273841=CARTESIAN_POINT('Ctrl Pts',(11.4908939831593,18.4374010075274,-34.1123080001425));
#273842=CARTESIAN_POINT('Ctrl Pts',(11.5073957447759,18.2823452034076,-34.0369466191341));
#273843=CARTESIAN_POINT('Ctrl Pts',(11.5201159294506,18.1280311274458,-33.9600084589958));
#273844=CARTESIAN_POINT('',(10.1651884842034,23.112869214926,-35.115773610427));
#273845=CARTESIAN_POINT('Origin',(10.1651884842034,-17.542318193471,0.972561099047131));
#273846=CARTESIAN_POINT('Ctrl Pts',(11.5201159294506,20.9274538922145,-30.8509345021458));
#273847=CARTESIAN_POINT('Ctrl Pts',(11.5064953958128,21.0266584418215,-31.0066544528484));
#273848=CARTESIAN_POINT('Ctrl Pts',(11.4885385348232,21.124157667372,-31.163415299962));
#273849=CARTESIAN_POINT('Ctrl Pts',(11.2877548088084,21.9877719172839,-32.5859714338316));
#273850=CARTESIAN_POINT('Ctrl Pts',(10.8383054247334,22.6201746706312,-33.8816750357462));
#273851=CARTESIAN_POINT('Ctrl Pts',(10.1651884842034,23.112869214926,-35.115773610427));
#273852=CARTESIAN_POINT('Origin',(0.884028484203416,-17.542318193471,0.972561099047131));
#273853=CARTESIAN_POINT('',(10.1651884842034,14.0986965788227,-43.2321711079735));
#273854=CARTESIAN_POINT('Ctrl Pts',(10.1651884842034,14.0986965788227,-43.2321711079735));
#273855=CARTESIAN_POINT('Ctrl Pts',(10.189490010882,14.0562453442155,-43.2098235828551));
#273856=CARTESIAN_POINT('Ctrl Pts',(10.2135007848618,14.0137261587338,-43.1872879478475));
#273857=CARTESIAN_POINT('Ctrl Pts',(10.8759790020178,12.8243387873183,-42.5525732844649));
#273858=CARTESIAN_POINT('Ctrl Pts',(11.3015145825508,11.6373594202826,-41.80342646167));
#273859=CARTESIAN_POINT('Ctrl Pts',(11.4908939831593,10.3566033615292,-40.8262236866127));
#273860=CARTESIAN_POINT('Ctrl Pts',(11.5073957447759,10.2206044108975,-40.7202712181856));
#273861=CARTESIAN_POINT('Ctrl Pts',(11.5201159294506,10.0856588106987,-40.6129306409912));
#273862=CARTESIAN_POINT('',(10.1651884842034,14.7212691391918,-42.7798456660962));
#273863=CARTESIAN_POINT('Origin',(10.1651884842034,-17.542318193471,0.972561099047131));
#273864=CARTESIAN_POINT('Ctrl Pts',(11.5201159294506,13.470320294743,-38.1538301299313));
#273865=CARTESIAN_POINT('Ctrl Pts',(11.5064953958128,13.5349809886783,-38.326773011743));
#273866=CARTESIAN_POINT('Ctrl Pts',(11.4885385348232,13.5977572094466,-38.5003794870738));
#273867=CARTESIAN_POINT('Ctrl Pts',(11.2877548088084,14.1467333648814,-40.071404855241));
#273868=CARTESIAN_POINT('Ctrl Pts',(10.8383054247334,14.4959246740928,-41.4702781504422));
#273869=CARTESIAN_POINT('Ctrl Pts',(10.1651884842034,14.7212691391918,-42.7798456660963));
#273870=CARTESIAN_POINT('Origin',(0.884028484203416,-17.542318193471,0.972561099047131));
#273871=CARTESIAN_POINT('',(10.1651884842034,34.0386901494083,-16.1916966375036));
#273872=CARTESIAN_POINT('Ctrl Pts',(10.1651884842034,34.0386901494082,-16.1916966375036));
#273873=CARTESIAN_POINT('Ctrl Pts',(10.189490010882,33.991210833489,-16.1985693195443));
#273874=CARTESIAN_POINT('Ctrl Pts',(10.2135007848618,33.9435659759387,-16.2053297580097));
#273875=CARTESIAN_POINT('Ctrl Pts',(10.8759790020178,32.6082554610186,-16.3909391649352));
#273876=CARTESIAN_POINT('Ctrl Pts',(11.3015145825508,31.2076315268737,-16.4825556207311));
#273877=CARTESIAN_POINT('Ctrl Pts',(11.4908939831593,29.5970927300156,-16.4447914918788));
#273878=CARTESIAN_POINT('Ctrl Pts',(11.5073957447759,29.4247899693519,-16.439012321834));
#273879=CARTESIAN_POINT('Ctrl Pts',(11.5201159294506,29.2525234772276,-16.4314910043563));
#273880=CARTESIAN_POINT('',(10.1651884842034,34.2764917070062,-15.4598186985698));
#273881=CARTESIAN_POINT('Origin',(10.1651884842034,-17.542318193471,0.972561099047131));
#273882=CARTESIAN_POINT('',(11.5201159294503,30.5453491237198,-12.4525827957091));
#273883=CARTESIAN_POINT('Ctrl Pts',(11.5201159294506,30.5453491237198,-12.4525827957091));
#273884=CARTESIAN_POINT('Ctrl Pts',(11.5064953958128,30.6993139993994,-12.5544899238528));
#273885=CARTESIAN_POINT('Ctrl Pts',(11.4885385348232,30.8521443547455,-12.6580415759667));
#273886=CARTESIAN_POINT('Ctrl Pts',(11.2877548088084,32.219700936385,-13.6063477093833));
#273887=CARTESIAN_POINT('Ctrl Pts',(10.8383054247334,33.32443973257,-14.5328104763952));
#273888=CARTESIAN_POINT('Ctrl Pts',(10.1651884842034,34.2764917070062,-15.4598186985698));
#273889=CARTESIAN_POINT('Ctrl Pts',(11.5520284842034,29.8566594240744,-11.8470366407104));
#273890=CARTESIAN_POINT('Ctrl Pts',(11.5520284842034,29.9376329966379,-11.9406753940128));
#273891=CARTESIAN_POINT('Ctrl Pts',(11.5505455075224,30.0237628247143,-12.0298480784021));
#273892=CARTESIAN_POINT('Ctrl Pts',(11.5472514703205,30.1147200651852,-12.1141556807327));
#273893=CARTESIAN_POINT('Ctrl Pts',(11.544044092433,30.2032844085471,-12.196245324198));
#273894=CARTESIAN_POINT('Ctrl Pts',(11.539119248065,30.2964254868395,-12.2737222219197));
#273895=CARTESIAN_POINT('Ctrl Pts',(11.5322065029565,30.3938209389875,-12.3461860127879));
#273896=CARTESIAN_POINT('Ctrl Pts',(11.5286982551648,30.4432495486874,-12.3829616974549));
#273897=CARTESIAN_POINT('Ctrl Pts',(11.5246785671409,30.4937736154884,-12.4184457114994));
#273898=CARTESIAN_POINT('Ctrl Pts',(11.5201159294506,30.5453491237198,-12.4525827957091));
#273899=CARTESIAN_POINT('Origin',(0.884028484203416,-17.542318193471,0.972561099047131));
#273900=CARTESIAN_POINT('',(10.1651884842034,36.4801712081848,-5.09232176568361));
#273901=CARTESIAN_POINT('',(11.520115929451,31.8484498133401,-6.32197605563879));
#273902=CARTESIAN_POINT('Ctrl Pts',(10.1651884842034,36.4801712081848,-5.09232176568361));
#273903=CARTESIAN_POINT('Ctrl Pts',(10.189490010882,36.4351583401774,-5.10891576798397));
#273904=CARTESIAN_POINT('Ctrl Pts',(10.2135007848618,36.3899602112694,-5.12543439754089));
#273905=CARTESIAN_POINT('Ctrl Pts',(10.8759790020178,35.1224198004912,-5.58461446052246));
#273906=CARTESIAN_POINT('Ctrl Pts',(11.3015145825508,33.7714509920083,-5.96543496729491));
#273907=CARTESIAN_POINT('Ctrl Pts',(11.4908939831593,32.1882547280909,-6.26334591964661));
#273908=CARTESIAN_POINT('Ctrl Pts',(11.5073957447759,32.0185156391323,-6.29351679663514));
#273909=CARTESIAN_POINT('Ctrl Pts',(11.5201159294506,31.8484498133401,-6.3219760556388));
#273910=CARTESIAN_POINT('',(10.1651884842034,36.560610251444,-4.32699539176697));
#273911=CARTESIAN_POINT('Origin',(10.1651884842034,-17.542318193471,0.972561099047131));
#273912=CARTESIAN_POINT('',(11.5201159294509,32.2857625843551,-2.16122297171639));
#273913=CARTESIAN_POINT('Ctrl Pts',(11.5201159294506,32.285762584355,-2.16122297171638));
#273914=CARTESIAN_POINT('Ctrl Pts',(11.5064953958128,32.4575506414171,-2.22889208697866));
#273915=CARTESIAN_POINT('Ctrl Pts',(11.4885385348232,32.6285708858962,-2.29840566945766));
#273916=CARTESIAN_POINT('Ctrl Pts',(11.2877548088084,34.1634070067061,-2.94165803744265));
#273917=CARTESIAN_POINT('Ctrl Pts',(10.8383054247334,35.4366270500011,-3.6181872591378));
#273918=CARTESIAN_POINT('Ctrl Pts',(10.1651884842034,36.560610251444,-4.32699539176698));
#273919=CARTESIAN_POINT('Ctrl Pts',(11.5520284842034,31.4862222820429,-1.71209609297288));
#273920=CARTESIAN_POINT('Ctrl Pts',(11.5520284842034,31.5848954455677,-1.78685361573));
#273921=CARTESIAN_POINT('Ctrl Pts',(11.5505454936052,31.6876836794972,-1.85617057017899));
#273922=CARTESIAN_POINT('Ctrl Pts',(11.547251423208,31.7941823732418,-1.91972502887827));
#273923=CARTESIAN_POINT('Ctrl Pts',(11.5440440121231,31.8978793346475,-1.98160751794148));
#273924=CARTESIAN_POINT('Ctrl Pts',(11.5391191153364,32.0050940195483,-2.03802645190818));
#273925=CARTESIAN_POINT('Ctrl Pts',(11.5322062926149,32.1154278761199,-2.08865723676024));
#273926=CARTESIAN_POINT('Ctrl Pts',(11.528698094849,32.1714213544321,-2.11435192234124));
#273927=CARTESIAN_POINT('Ctrl Pts',(11.5246784764318,32.2282177698874,-2.13855546648027));
#273928=CARTESIAN_POINT('Ctrl Pts',(11.5201159294506,32.285762584355,-2.16122297171638));
#273929=CARTESIAN_POINT('Ctrl Pts',(11.5201159294506,31.8484498133401,-6.32197605563879));
#273930=CARTESIAN_POINT('Ctrl Pts',(11.5379482942249,31.610035362708,-6.36187295185028));
#273931=CARTESIAN_POINT('Ctrl Pts',(11.5475950755165,31.3756205042814,-6.42746995318688));
#273932=CARTESIAN_POINT('Ctrl Pts',(11.5516325551658,31.0897162833456,-6.54227681508785));
#273933=CARTESIAN_POINT('Ctrl Pts',(11.5520284842034,31.0309417643657,-6.56785407064173));
#273934=CARTESIAN_POINT('Ctrl Pts',(11.5520284842034,30.9730026561922,-6.59505465837618));
#273935=CARTESIAN_POINT('Origin',(0.884028484203416,-17.542318193471,0.972561099047131));
#273936=CARTESIAN_POINT('',(10.1651884842034,4.21658387552303,-48.8447285308278));
#273937=CARTESIAN_POINT('Ctrl Pts',(10.1651884842034,4.21658387552304,-48.8447285308278));
#273938=CARTESIAN_POINT('Ctrl Pts',(10.189490010882,4.17970661397677,-48.8140432447864));
#273939=CARTESIAN_POINT('Ctrl Pts',(10.2135007848618,4.14280199669075,-48.783159831727));
#273940=CARTESIAN_POINT('Ctrl Pts',(10.8759790020178,3.11137019184823,-47.9150276671604));
#273941=CARTESIAN_POINT('Ctrl Pts',(11.3015145825508,2.10608555445984,-46.9354646126801));
#273942=CARTESIAN_POINT('Ctrl Pts',(11.4908939831593,1.05648896969897,-45.7133319051268));
#273943=CARTESIAN_POINT('Ctrl Pts',(11.5073957447759,0.945490679293149,
-45.5814189805678));
#273944=CARTESIAN_POINT('Ctrl Pts',(11.5201159294506,0.835811325126995,
-45.448367284618));
#273945=CARTESIAN_POINT('',(10.1651884842034,4.91959547915134,-48.5317275987877));
#273946=CARTESIAN_POINT('Origin',(10.1651884842034,-17.542318193471,0.972561099047131));
#273947=CARTESIAN_POINT('Ctrl Pts',(11.5201159294506,4.65778558018633,-43.7467147117548));
#273948=CARTESIAN_POINT('Ctrl Pts',(11.5064953958128,4.68507643584861,-43.9293220908684));
#273949=CARTESIAN_POINT('Ctrl Pts',(11.4885385348232,4.71038602975324,-44.1121867583883));
#273950=CARTESIAN_POINT('Ctrl Pts',(11.2877548088084,4.9207311984387,-45.763020013648));
#273951=CARTESIAN_POINT('Ctrl Pts',(10.8383054247334,4.97144972769578,-47.2039255265966));
#273952=CARTESIAN_POINT('Ctrl Pts',(10.1651884842034,4.91959547915134,-48.5317275987877));
#273953=CARTESIAN_POINT('Origin',(0.884028484203416,-17.542318193471,0.972561099047131));
#273954=CARTESIAN_POINT('',(10.1651884842034,-6.616497258988,-52.2800313469788));
#273955=CARTESIAN_POINT('Ctrl Pts',(10.1651884842034,-6.61649725898799,
-52.2800313469787));
#273956=CARTESIAN_POINT('Ctrl Pts',(10.189490010882,-6.646188834187,-52.2423493942587));
#273957=CARTESIAN_POINT('Ctrl Pts',(10.2135007848618,-6.67586597441391,
-52.2044679564932));
#273958=CARTESIAN_POINT('Ctrl Pts',(10.8759790020178,-7.50426369345284,
-51.1408598320946));
#273959=CARTESIAN_POINT('Ctrl Pts',(11.3015145825508,-8.28391783864927,
-49.9736921518746));
#273960=CARTESIAN_POINT('Ctrl Pts',(11.4908939831593,-9.05648254214045,
-48.5600425755889));
#273961=CARTESIAN_POINT('Ctrl Pts',(11.5073957447759,-9.13762901440063,
-48.4079344226896));
#273962=CARTESIAN_POINT('Ctrl Pts',(11.5201159294506,-9.21724860845719,
-48.2549866055502));
#273963=CARTESIAN_POINT('',(10.1651884842034,-5.863771592603,-52.1200345674512));
#273964=CARTESIAN_POINT('Origin',(10.1651884842034,-17.542318193471,0.972561099047131));
#273965=CARTESIAN_POINT('Ctrl Pts',(11.5201159294506,-5.12500019719618,
-47.3851523537529));
#273966=CARTESIAN_POINT('Ctrl Pts',(11.5064953958128,-5.13627192115547,
-47.5694434114538));
#273967=CARTESIAN_POINT('Ctrl Pts',(11.4885385348232,-5.14953510481703,
-47.75357420771));
#273968=CARTESIAN_POINT('Ctrl Pts',(11.2877548088084,-5.28701401610064,
-49.4120660152306));
#273969=CARTESIAN_POINT('Ctrl Pts',(10.8383054247334,-5.53698490990081,
-50.832029260779));
#273970=CARTESIAN_POINT('Ctrl Pts',(10.1651884842034,-5.863771592603,-52.1200345674512));
#273971=CARTESIAN_POINT('Origin',(0.561048484203417,-17.542318193471,0.972561099047131));
#273972=CARTESIAN_POINT('',(6.14788848420341,-28.4681391279537,54.2251535450731));
#273973=CARTESIAN_POINT('',(8.15653848420341,-28.4681391279536,54.2251535450731));
#273974=CARTESIAN_POINT('',(6.14788848420341,-29.2208647943386,54.0651567655455));
#273975=CARTESIAN_POINT('Origin',(6.14788848420341,-17.542318193471,0.972561099047131));
#273976=CARTESIAN_POINT('',(8.15653848420342,-29.2208647943386,54.0651567655455));
#273977=CARTESIAN_POINT('Origin',(0.561048484203417,-17.542318193471,0.972561099047131));
#273978=CARTESIAN_POINT('',(6.14788848420341,-6.6164972589887,54.2251535450731));
#273979=CARTESIAN_POINT('',(8.15653848420342,-6.6164972589887,54.2251535450731));
#273980=CARTESIAN_POINT('',(6.14788848420341,-5.86377159260369,54.0651567655456));
#273981=CARTESIAN_POINT('',(8.15653848420342,-5.86377159260369,54.0651567655456));
#273982=CARTESIAN_POINT('Origin',(6.14788848420341,-17.542318193471,0.972561099047131));
#273983=CARTESIAN_POINT('Origin',(0.561048484203417,-17.542318193471,0.972561099047131));
#273984=CARTESIAN_POINT('',(6.14788848420341,4.21658387552239,50.7898507289224));
#273985=CARTESIAN_POINT('',(8.15653848420342,4.21658387552238,50.7898507289224));
#273986=CARTESIAN_POINT('',(6.14788848420341,4.91959547915065,50.4768497968823));
#273987=CARTESIAN_POINT('',(8.15653848420342,4.91959547915064,50.4768497968823));
#273988=CARTESIAN_POINT('Origin',(6.14788848420341,-17.542318193471,0.972561099047131));
#273989=CARTESIAN_POINT('Origin',(0.561048484203417,-17.542318193471,0.972561099047131));
#273990=CARTESIAN_POINT('',(6.14788848420341,14.0986965788221,45.1772933060682));
#273991=CARTESIAN_POINT('',(8.15653848420342,14.0986965788221,45.1772933060682));
#273992=CARTESIAN_POINT('',(6.14788848420341,14.7212691391912,44.7249678641909));
#273993=CARTESIAN_POINT('',(8.15653848420341,14.7212691391912,44.7249678641909));
#273994=CARTESIAN_POINT('Origin',(6.14788848420341,-17.542318193471,0.972561099047131));
#273995=CARTESIAN_POINT('Origin',(0.561048484203417,-17.542318193471,0.972561099047131));
#273996=CARTESIAN_POINT('',(6.14788848420341,29.7276425156794,27.8195903550057));
#273997=CARTESIAN_POINT('',(8.15653848420341,29.7276425156794,27.8195903550057));
#273998=CARTESIAN_POINT('',(6.14788848420342,29.3428715129083,28.4860332810845));
#273999=CARTESIAN_POINT('Origin',(6.14788848420341,-17.542318193471,0.972561099047131));
#274000=CARTESIAN_POINT('',(8.15653848420341,29.3428715129083,28.4860332810845));
#274001=CARTESIAN_POINT('Origin',(0.561048484203417,-17.542318193471,0.972561099047131));
#274002=CARTESIAN_POINT('',(6.14788848420342,34.2764917070059,17.4049408966648));
#274003=CARTESIAN_POINT('',(8.15653848420342,34.2764917070059,17.4049408966648));
#274004=CARTESIAN_POINT('Origin',(6.14788848420341,-17.542318193471,0.972561099047131));
#274005=CARTESIAN_POINT('Origin',(0.561048484203417,-17.542318193471,0.972561099047131));
#274006=CARTESIAN_POINT('',(6.14788848420341,22.5979451061385,37.632776967928));
#274007=CARTESIAN_POINT('',(8.15653848420341,22.5979451061385,37.632776967928));
#274008=CARTESIAN_POINT('',(6.14788848420341,23.1128692149255,37.0608958085218));
#274009=CARTESIAN_POINT('',(8.15653848420341,23.1128692149255,37.0608958085218));
#274010=CARTESIAN_POINT('Origin',(6.14788848420341,-17.542318193471,0.972561099047131));
#274011=CARTESIAN_POINT('Origin',(0.561048484203417,-17.542318193471,0.972561099047131));
#274012=CARTESIAN_POINT('',(6.14788848420342,-71.6452466383859,-4.32699539176735));
#274013=CARTESIAN_POINT('',(8.15653848420341,-71.6452466383859,-4.32699539176735));
#274014=CARTESIAN_POINT('',(6.14788848420341,-71.5648075951267,-5.0923217656847));
#274015=CARTESIAN_POINT('Origin',(6.14788848420341,-17.542318193471,0.972561099047131));
#274016=CARTESIAN_POINT('',(8.15653848420342,-71.5648075951267,-5.0923217656847));
#274017=CARTESIAN_POINT('Origin',(0.561048484203417,-17.542318193471,0.972561099047131));
#274018=CARTESIAN_POINT('',(6.14788848420341,-71.645246638386,6.27211758986086));
#274019=CARTESIAN_POINT('',(8.15653848420342,-71.645246638386,6.27211758986086));
#274020=CARTESIAN_POINT('',(6.14788848420341,-71.5648075951268,7.03744396377822));
#274021=CARTESIAN_POINT('',(8.15653848420341,-71.5648075951268,7.03744396377822));
#274022=CARTESIAN_POINT('Origin',(6.14788848420341,-17.542318193471,0.972561099047131));
#274023=CARTESIAN_POINT('Origin',(0.561048484203417,-17.542318193471,0.972561099047131));
#274024=CARTESIAN_POINT('',(6.14788848420341,-69.361128093948,17.4049408966644));
#274025=CARTESIAN_POINT('',(8.15653848420342,-69.361128093948,17.4049408966644));
#274026=CARTESIAN_POINT('Origin',(6.14788848420341,-17.542318193471,0.972561099047131));
#274027=CARTESIAN_POINT('Origin',(0.561048484203417,-17.542318193471,0.972561099047131));
#274028=CARTESIAN_POINT('',(6.14788848420341,-64.4275078998505,28.4860332810842));
#274029=CARTESIAN_POINT('',(8.15653848420341,-64.4275078998505,28.4860332810842));
#274030=CARTESIAN_POINT('',(6.14788848420341,-64.8122789026216,27.8195903550054));
#274031=CARTESIAN_POINT('Origin',(6.14788848420341,-17.542318193471,0.972561099047131));
#274032=CARTESIAN_POINT('',(8.15653848420342,-64.8122789026216,27.8195903550054));
#274033=CARTESIAN_POINT('Origin',(0.561048484203417,-17.542318193471,0.972561099047131));
#274034=CARTESIAN_POINT('',(6.14788848420341,-58.1975056018677,37.0608958085216));
#274035=CARTESIAN_POINT('',(8.15653848420341,-58.1975056018677,37.0608958085215));
#274036=CARTESIAN_POINT('',(6.14788848420342,-57.6825814930807,37.6327769679278));
#274037=CARTESIAN_POINT('',(8.15653848420341,-57.6825814930807,37.6327769679278));
#274038=CARTESIAN_POINT('Origin',(6.14788848420341,-17.542318193471,0.972561099047131));
#274039=CARTESIAN_POINT('Origin',(0.561048484203417,-17.542318193471,0.972561099047131));
#274040=CARTESIAN_POINT('',(6.14788848420341,-49.1833329657644,45.177293306068));
#274041=CARTESIAN_POINT('',(8.15653848420341,-49.1833329657644,45.177293306068));
#274042=CARTESIAN_POINT('',(6.14788848420341,-49.8059055261334,44.7249678641907));
#274043=CARTESIAN_POINT('Origin',(6.14788848420341,-17.542318193471,0.972561099047131));
#274044=CARTESIAN_POINT('',(8.15653848420341,-49.8059055261334,44.7249678641907));
#274045=CARTESIAN_POINT('Origin',(0.561048484203417,-17.542318193471,0.972561099047131));
#274046=CARTESIAN_POINT('',(6.14788848420341,-40.004231866093,50.4768497968821));
#274047=CARTESIAN_POINT('',(8.15653848420341,-40.004231866093,50.4768497968821));
#274048=CARTESIAN_POINT('',(6.14788848420341,-39.3012202624647,50.7898507289222));
#274049=CARTESIAN_POINT('',(8.15653848420341,-39.3012202624647,50.7898507289222));
#274050=CARTESIAN_POINT('Origin',(6.14788848420341,-17.542318193471,0.972561099047131));
#274051=CARTESIAN_POINT('Origin',(0.561048484203417,-17.542318193471,0.972561099047131));
#274052=CARTESIAN_POINT('',(6.14788848420341,-17.9270891962415,-53.3879403389487));
#274053=CARTESIAN_POINT('',(8.15653848420342,-17.9270891962415,-53.3879403389487));
#274054=CARTESIAN_POINT('',(6.14788848420341,-17.1575471906993,-53.3879403389487));
#274055=CARTESIAN_POINT('Origin',(6.14788848420341,-17.542318193471,0.972561099047131));
#274056=CARTESIAN_POINT('',(8.15653848420341,-17.1575471906993,-53.3879403389487));
#274057=CARTESIAN_POINT('Origin',(0.561048484203417,-17.542318193471,0.972561099047131));
#274058=CARTESIAN_POINT('',(6.14788848420341,-28.4681391279529,-52.280031346979));
#274059=CARTESIAN_POINT('',(8.15653848420342,-28.4681391279529,-52.280031346979));
#274060=CARTESIAN_POINT('',(6.14788848420341,-29.2208647943379,-52.1200345674514));
#274061=CARTESIAN_POINT('',(8.15653848420342,-29.2208647943379,-52.1200345674514));
#274062=CARTESIAN_POINT('Origin',(6.14788848420341,-17.542318193471,0.972561099047131));
#274063=CARTESIAN_POINT('Origin',(0.561048484203417,-17.542318193471,0.972561099047131));
#274064=CARTESIAN_POINT('',(6.14788848420341,-39.301220262464,-48.8447285308283));
#274065=CARTESIAN_POINT('',(8.15653848420342,-39.301220262464,-48.8447285308283));
#274066=CARTESIAN_POINT('',(6.14788848420342,-40.0042318660923,-48.5317275987882));
#274067=CARTESIAN_POINT('',(8.15653848420342,-40.0042318660923,-48.5317275987882));
#274068=CARTESIAN_POINT('Origin',(6.14788848420341,-17.542318193471,0.972561099047131));
#274069=CARTESIAN_POINT('Origin',(0.561048484203417,-17.542318193471,0.972561099047131));
#274070=CARTESIAN_POINT('',(6.14788848420342,-49.8059055261329,-42.7798456660969));
#274071=CARTESIAN_POINT('',(8.15653848420341,-49.8059055261328,-42.7798456660969));
#274072=CARTESIAN_POINT('',(6.14788848420341,-49.1833329657638,-43.2321711079742));
#274073=CARTESIAN_POINT('Origin',(6.14788848420341,-17.542318193471,0.972561099047131));
#274074=CARTESIAN_POINT('',(8.15653848420342,-49.1833329657638,-43.2321711079742));
#274075=CARTESIAN_POINT('Origin',(0.561048484203417,-17.542318193471,0.972561099047131));
#274076=CARTESIAN_POINT('',(6.14788848420341,-57.6825814930802,-35.687654769834));
#274077=CARTESIAN_POINT('',(8.15653848420341,-57.6825814930802,-35.687654769834));
#274078=CARTESIAN_POINT('',(6.14788848420341,-58.1975056018673,-35.1157736104278));
#274079=CARTESIAN_POINT('',(8.15653848420341,-58.1975056018673,-35.1157736104278));
#274080=CARTESIAN_POINT('Origin',(6.14788848420341,-17.542318193471,0.972561099047131));
#274081=CARTESIAN_POINT('Origin',(0.561048484203417,-17.542318193471,0.972561099047131));
#274082=CARTESIAN_POINT('',(6.14788848420341,-64.8122789026212,-25.8744681569117));
#274083=CARTESIAN_POINT('',(8.15653848420341,-64.8122789026212,-25.8744681569117));
#274084=CARTESIAN_POINT('',(6.14788848420341,-64.4275078998501,-26.5409110829905));
#274085=CARTESIAN_POINT('Origin',(6.14788848420341,-17.542318193471,0.972561099047131));
#274086=CARTESIAN_POINT('',(8.15653848420341,-64.4275078998501,-26.5409110829905));
#274087=CARTESIAN_POINT('Origin',(0.561048484203417,-17.542318193471,0.972561099047131));
#274088=CARTESIAN_POINT('',(6.14788848420341,-69.1233265363499,-16.1916966375046));
#274089=CARTESIAN_POINT('',(8.15653848420341,-69.1233265363499,-16.1916966375046));
#274090=CARTESIAN_POINT('',(6.14788848420341,-69.3611280939478,-15.4598186985709));
#274091=CARTESIAN_POINT('',(8.15653848420342,-69.3611280939478,-15.4598186985708));
#274092=CARTESIAN_POINT('Origin',(6.14788848420341,-17.542318193471,0.972561099047131));
#274093=CARTESIAN_POINT('Origin',(0.561048484203417,-17.542318193471,0.972561099047131));
#274094=CARTESIAN_POINT('',(6.14788848420342,29.3428715129087,-26.5409110829896));
#274095=CARTESIAN_POINT('',(8.15653848420341,29.3428715129087,-26.5409110829896));
#274096=CARTESIAN_POINT('',(6.14788848420341,29.7276425156798,-25.8744681569108));
#274097=CARTESIAN_POINT('Origin',(6.14788848420341,-17.542318193471,0.972561099047131));
#274098=CARTESIAN_POINT('',(8.15653848420341,29.7276425156798,-25.8744681569108));
#274099=CARTESIAN_POINT('Origin',(0.561048484203417,-17.542318193471,0.972561099047131));
#274100=CARTESIAN_POINT('',(6.14788848420341,23.112869214926,-35.115773610427));
#274101=CARTESIAN_POINT('',(8.15653848420341,23.112869214926,-35.115773610427));
#274102=CARTESIAN_POINT('',(6.14788848420341,22.597945106139,-35.6876547698332));
#274103=CARTESIAN_POINT('',(8.15653848420341,22.5979451061389,-35.6876547698332));
#274104=CARTESIAN_POINT('Origin',(6.14788848420341,-17.542318193471,0.972561099047131));
#274105=CARTESIAN_POINT('Origin',(0.561048484203417,-17.542318193471,0.972561099047131));
#274106=CARTESIAN_POINT('',(6.14788848420341,14.7212691391918,-42.7798456660962));
#274107=CARTESIAN_POINT('',(8.15653848420341,14.7212691391918,-42.7798456660962));
#274108=CARTESIAN_POINT('',(6.14788848420341,14.0986965788227,-43.2321711079735));
#274109=CARTESIAN_POINT('',(8.15653848420341,14.0986965788227,-43.2321711079735));
#274110=CARTESIAN_POINT('Origin',(6.14788848420341,-17.542318193471,0.972561099047131));
#274111=CARTESIAN_POINT('Origin',(0.561048484203417,-17.542318193471,0.972561099047131));
#274112=CARTESIAN_POINT('',(6.14788848420341,34.0386901494082,-16.1916966375036));
#274113=CARTESIAN_POINT('',(8.15653848420342,34.0386901494082,-16.1916966375036));
#274114=CARTESIAN_POINT('',(6.14788848420341,34.2764917070062,-15.4598186985698));
#274115=CARTESIAN_POINT('Origin',(6.14788848420341,-17.542318193471,0.972561099047131));
#274116=CARTESIAN_POINT('',(8.15653848420341,34.2764917070062,-15.4598186985698));
#274117=CARTESIAN_POINT('Origin',(0.561048484203417,-17.542318193471,0.972561099047131));
#274118=CARTESIAN_POINT('',(6.14788848420341,36.4801712081848,-5.09232176568361));
#274119=CARTESIAN_POINT('',(8.15653848420342,36.4801712081848,-5.09232176568361));
#274120=CARTESIAN_POINT('',(6.14788848420341,36.560610251444,-4.32699539176698));
#274121=CARTESIAN_POINT('Origin',(6.14788848420341,-17.542318193471,0.972561099047131));
#274122=CARTESIAN_POINT('',(8.15653848420341,36.560610251444,-4.32699539176697));
#274123=CARTESIAN_POINT('Origin',(0.561048484203417,-17.542318193471,0.972561099047131));
#274124=CARTESIAN_POINT('',(6.14788848420341,4.91959547915134,-48.5317275987877));
#274125=CARTESIAN_POINT('',(8.15653848420341,4.91959547915134,-48.5317275987877));
#274126=CARTESIAN_POINT('',(6.14788848420342,4.21658387552304,-48.8447285308278));
#274127=CARTESIAN_POINT('',(8.15653848420342,4.21658387552303,-48.8447285308278));
#274128=CARTESIAN_POINT('Origin',(6.14788848420341,-17.542318193471,0.972561099047131));
#274129=CARTESIAN_POINT('Origin',(0.561048484203417,-17.542318193471,0.972561099047131));
#274130=CARTESIAN_POINT('',(6.14788848420341,-5.863771592603,-52.1200345674512));
#274131=CARTESIAN_POINT('',(8.15653848420341,-5.863771592603,-52.1200345674512));
#274132=CARTESIAN_POINT('',(6.14788848420341,-6.61649725898799,-52.2800313469788));
#274133=CARTESIAN_POINT('',(8.15653848420342,-6.61649725898799,-52.2800313469788));
#274134=CARTESIAN_POINT('Origin',(6.14788848420341,-17.542318193471,0.972561099047131));
#274135=CARTESIAN_POINT('Origin',(15.4290484842034,-17.542318193471,0.972561099047131));
#274136=CARTESIAN_POINT('',(4.79296103895619,-25.8673877784845,50.2001088036445));
#274137=CARTESIAN_POINT('Ctrl Pts',(4.79296103895619,-25.8673877784845,
50.2001088036445));
#274138=CARTESIAN_POINT('Ctrl Pts',(4.80658157259404,-25.9526429368654,
50.3638824391265));
#274139=CARTESIAN_POINT('Ctrl Pts',(4.8245384335836,-26.0396522000094,50.5266996688594));
#274140=CARTESIAN_POINT('Ctrl Pts',(5.0253221595984,-26.8398148252939,51.9858896152881));
#274141=CARTESIAN_POINT('Ctrl Pts',(5.47477154367345,-27.6457256836533,
53.1814182660674));
#274142=CARTESIAN_POINT('Ctrl Pts',(6.14788848420342,-28.4681391279537,
54.2251535450731));
#274143=CARTESIAN_POINT('',(4.76104848420342,-25.3371465446544,49.451895009213));
#274144=CARTESIAN_POINT('Ctrl Pts',(4.76104848420342,-25.3371465446544,
49.451895009213));
#274145=CARTESIAN_POINT('Ctrl Pts',(4.76104848420342,-25.4218077136479,
49.5422122981067));
#274146=CARTESIAN_POINT('Ctrl Pts',(4.76253144074934,-25.5014883801629,
49.6371907160477));
#274147=CARTESIAN_POINT('Ctrl Pts',(4.76582543152198,-25.575826089086,49.7364615046949));
#274148=CARTESIAN_POINT('Ctrl Pts',(4.76903276223312,-25.6482080820183,
49.8331206246266));
#274149=CARTESIAN_POINT('Ctrl Pts',(4.77395753237976,-25.7155242765978,
49.9338491853259));
#274150=CARTESIAN_POINT('Ctrl Pts',(4.78087016904194,-25.777410200811,50.0382847362108));
#274151=CARTESIAN_POINT('Ctrl Pts',(4.78437848713686,-25.8088186948993,
50.091288119844));
#274152=CARTESIAN_POINT('Ctrl Pts',(4.78839827319647,-25.8388280077851,
50.1452459945807));
#274153=CARTESIAN_POINT('Ctrl Pts',(4.79296103895619,-25.8673877784845,
50.2001088036445));
#274154=CARTESIAN_POINT('',(4.76104848420342,-30.1397096933157,48.4310786991304));
#274155=CARTESIAN_POINT('Origin',(4.76104848420342,-17.542318193471,0.972561099047131));
#274156=CARTESIAN_POINT('',(4.79296103895619,-29.9596361897455,49.3302745518473));
#274157=CARTESIAN_POINT('Ctrl Pts',(4.79296103895619,-29.9596361897455,
49.3302745518473));
#274158=CARTESIAN_POINT('Ctrl Pts',(4.77035892158036,-29.9783406571863,
49.0244592124324));
#274159=CARTESIAN_POINT('Ctrl Pts',(4.76104848420342,-30.0387016815049,
48.7219745577429));
#274160=CARTESIAN_POINT('Ctrl Pts',(4.76104848420342,-30.1397096933157,
48.4310786991304));
#274161=CARTESIAN_POINT('Ctrl Pts',(6.14788848420341,-29.2208647943386,
54.0651567655455));
#274162=CARTESIAN_POINT('Ctrl Pts',(6.12358695752486,-29.2326627670381,
54.0186559371789));
#274163=CARTESIAN_POINT('Ctrl Pts',(6.099576183545,-29.2443664148566,53.9719787413873));
#274164=CARTESIAN_POINT('Ctrl Pts',(5.437097966389,-29.56853699014,52.6633846632577));
#274165=CARTESIAN_POINT('Ctrl Pts',(5.01156238585602,-29.8060566288571,
51.2800100209081));
#274166=CARTESIAN_POINT('Ctrl Pts',(4.82218298524757,-29.9368465213225,
49.6743464977371));
#274167=CARTESIAN_POINT('Ctrl Pts',(4.80568122363092,-29.9491095529648,
49.5023835418609));
#274168=CARTESIAN_POINT('Ctrl Pts',(4.79296103895619,-29.9596361897455,
49.3302745518473));
#274169=CARTESIAN_POINT('Origin',(15.4290484842034,-17.542318193471,0.972561099047131));
#274170=CARTESIAN_POINT('',(4.79296103895619,-9.21724860845784,50.2001088036446));
#274171=CARTESIAN_POINT('',(4.76104848420342,-9.74748984228791,49.4518950092131));
#274172=CARTESIAN_POINT('Ctrl Pts',(4.79296103895619,-9.21724860845785,
50.2001088036446));
#274173=CARTESIAN_POINT('Ctrl Pts',(4.77035892158039,-9.35872229428056,
49.9283403817424));
#274174=CARTESIAN_POINT('Ctrl Pts',(4.76104848420342,-9.53689642689581,
49.6765579398481));
#274175=CARTESIAN_POINT('Ctrl Pts',(4.76104848420342,-9.74748984228792,
49.4518950092131));
#274176=CARTESIAN_POINT('Ctrl Pts',(6.14788848420341,-6.61649725898869,
54.2251535450731));
#274177=CARTESIAN_POINT('Ctrl Pts',(6.12358695752485,-6.64618883418769,
54.1874715923531));
#274178=CARTESIAN_POINT('Ctrl Pts',(6.099576183545,-6.6758659744146,54.1495901545876));
#274179=CARTESIAN_POINT('Ctrl Pts',(5.43709796638901,-7.50426369345351,
53.085982030189));
#274180=CARTESIAN_POINT('Ctrl Pts',(5.01156238585602,-8.28391783864993,
51.918814349969));
#274181=CARTESIAN_POINT('Ctrl Pts',(4.82218298524757,-9.05648254214109,
50.5051647736833));
#274182=CARTESIAN_POINT('Ctrl Pts',(4.80568122363092,-9.13762901440128,
50.3530566207839));
#274183=CARTESIAN_POINT('Ctrl Pts',(4.79296103895619,-9.21724860845783,
50.2001088036446));
#274184=CARTESIAN_POINT('',(4.79296103895619,-5.12500019719682,49.3302745518473));
#274185=CARTESIAN_POINT('Ctrl Pts',(4.79296103895619,-5.12500019719682,
49.3302745518473));
#274186=CARTESIAN_POINT('Ctrl Pts',(4.80658157259404,-5.13627192115611,
49.5145656095482));
#274187=CARTESIAN_POINT('Ctrl Pts',(4.8245384335836,-5.14953510481761,49.6986964058044));
#274188=CARTESIAN_POINT('Ctrl Pts',(5.02532215959839,-5.28701401610125,
51.357188213325));
#274189=CARTESIAN_POINT('Ctrl Pts',(5.47477154367344,-5.53698490990151,
52.7771514588735));
#274190=CARTESIAN_POINT('Ctrl Pts',(6.14788848420341,-5.86377159260369,
54.0651567655456));
#274191=CARTESIAN_POINT('',(4.76104848420342,-4.94492669362663,48.4310786991305));
#274192=CARTESIAN_POINT('Ctrl Pts',(4.76104848420342,-4.94492669362663,
48.4310786991305));
#274193=CARTESIAN_POINT('Ctrl Pts',(4.76104848420342,-4.98553194226763,
48.5480189146228));
#274194=CARTESIAN_POINT('Ctrl Pts',(4.76253135162946,-5.01969184244055,
48.6671915454769));
#274195=CARTESIAN_POINT('Ctrl Pts',(4.76582514301953,-5.0472252496888,48.7881122473915));
#274196=CARTESIAN_POINT('Ctrl Pts',(4.76903226819321,-5.07403419811496,
48.9058512846292));
#274197=CARTESIAN_POINT('Ctrl Pts',(4.773956716031,-5.09456054852597,49.0252474567679));
#274198=CARTESIAN_POINT('Ctrl Pts',(4.7808688874334,-5.1086187509111,49.1458213738986));
#274199=CARTESIAN_POINT('Ctrl Pts',(4.78437750874136,-5.11575470075501,
49.2070247483811));
#274200=CARTESIAN_POINT('Ctrl Pts',(4.78839771848114,-5.12122380413468,
49.2685310710606));
#274201=CARTESIAN_POINT('Ctrl Pts',(4.79296103895619,-5.12500019719681,
49.3302745518474));
#274202=CARTESIAN_POINT('Origin',(4.76104848420342,-17.542318193471,0.972561099047131));
#274203=CARTESIAN_POINT('Origin',(15.4290484842034,-17.542318193471,0.972561099047131));
#274204=CARTESIAN_POINT('',(4.79296103895619,0.835811325126388,47.3934894827125));
#274205=CARTESIAN_POINT('',(4.76104848420342,0.161594739351947,46.7718693063203));
#274206=CARTESIAN_POINT('Ctrl Pts',(4.79296103895619,0.835811325126386,
47.3934894827125));
#274207=CARTESIAN_POINT('Ctrl Pts',(4.77035892158032,0.640925346662839,
47.1570738860987));
#274208=CARTESIAN_POINT('Ctrl Pts',(4.76104848420342,0.414296233119738,
46.947837979825));
#274209=CARTESIAN_POINT('Ctrl Pts',(4.76104848420342,0.161594739351935,
46.7718693063203));
#274210=CARTESIAN_POINT('Ctrl Pts',(6.14788848420341,4.21658387552238,50.7898507289224));
#274211=CARTESIAN_POINT('Ctrl Pts',(6.12358695752485,4.17970661397612,50.7591654428809));
#274212=CARTESIAN_POINT('Ctrl Pts',(6.09957618354499,4.14280199669011,50.7282820298215));
#274213=CARTESIAN_POINT('Ctrl Pts',(5.43709796638899,3.11137019184759,49.860149865255));
#274214=CARTESIAN_POINT('Ctrl Pts',(5.01156238585601,2.10608555445921,48.8805868107746));
#274215=CARTESIAN_POINT('Ctrl Pts',(4.82218298524757,1.05648896969834,47.6584541032213));
#274216=CARTESIAN_POINT('Ctrl Pts',(4.80568122363092,0.945490679292535,
47.5265411786623));
#274217=CARTESIAN_POINT('Ctrl Pts',(4.79296103895619,0.835811325126389,
47.3934894827125));
#274218=CARTESIAN_POINT('',(4.79296103895619,4.65778558018571,45.6918369098494));
#274219=CARTESIAN_POINT('Ctrl Pts',(4.79296103895619,4.65778558018571,45.6918369098494));
#274220=CARTESIAN_POINT('Ctrl Pts',(4.80658157259404,4.68507643584799,45.874444288963));
#274221=CARTESIAN_POINT('Ctrl Pts',(4.8245384335836,4.71038602975262,46.0573089564828));
#274222=CARTESIAN_POINT('Ctrl Pts',(5.02532215959839,4.92073119843806,47.7081422117426));
#274223=CARTESIAN_POINT('Ctrl Pts',(5.47477154367343,4.97144972769511,49.1490477246912));
#274224=CARTESIAN_POINT('Ctrl Pts',(6.14788848420341,4.91959547915065,50.4768497968823));
#274225=CARTESIAN_POINT('',(4.76104848420342,4.64697071554394,44.7748512573258));
#274226=CARTESIAN_POINT('Ctrl Pts',(4.76104848420342,4.64697071554394,44.7748512573258));
#274227=CARTESIAN_POINT('Ctrl Pts',(4.76104848420342,4.63156563905975,44.8976814471172));
#274228=CARTESIAN_POINT('Ctrl Pts',(4.76253142587583,4.62292954634033,45.0213551478097));
#274229=CARTESIAN_POINT('Ctrl Pts',(4.7658253855249,4.6211389269688,45.1453609704439));
#274230=CARTESIAN_POINT('Ctrl Pts',(4.76903268308216,4.61939541771304,45.2661042746713));
#274231=CARTESIAN_POINT('Ctrl Pts',(4.77395740161648,4.62414211204842,45.3871622545849));
#274232=CARTESIAN_POINT('Ctrl Pts',(4.78086996580786,4.6354608385096,45.5080274415206));
#274233=CARTESIAN_POINT('Ctrl Pts',(4.78437833171589,4.64120548448167,45.5693707129278));
#274234=CARTESIAN_POINT('Ctrl Pts',(4.78839818488759,4.64864319302931,45.6306637689947));
#274235=CARTESIAN_POINT('Ctrl Pts',(4.79296103895619,4.65778558018572,45.6918369098494));
#274236=CARTESIAN_POINT('Origin',(4.76104848420342,-17.542318193471,0.972561099047131));
#274237=CARTESIAN_POINT('Origin',(15.4290484842034,-17.542318193471,0.972561099047131));
#274238=CARTESIAN_POINT('',(4.79296103895619,10.0856588106982,42.5580528390859));
#274239=CARTESIAN_POINT('',(4.76104848420342,9.29693337302781,42.0901940653058));
#274240=CARTESIAN_POINT('Ctrl Pts',(4.79296103895619,10.0856588106982,42.5580528390859));
#274241=CARTESIAN_POINT('Ctrl Pts',(4.77035892158037,9.84587799202021,42.3673225637814));
#274242=CARTESIAN_POINT('Ctrl Pts',(4.76104848420342,9.58069867729854,42.2097778062576));
#274243=CARTESIAN_POINT('Ctrl Pts',(4.76104848420342,9.29693337302781,42.0901940653058));
#274244=CARTESIAN_POINT('Ctrl Pts',(6.14788848420341,14.0986965788221,45.1772933060682));
#274245=CARTESIAN_POINT('Ctrl Pts',(6.12358695752485,14.0562453442149,45.1549457809498));
#274246=CARTESIAN_POINT('Ctrl Pts',(6.099576183545,14.0137261587332,45.1324101459422));
#274247=CARTESIAN_POINT('Ctrl Pts',(5.43709796638899,12.8243387873176,44.4976954825596));
#274248=CARTESIAN_POINT('Ctrl Pts',(5.01156238585602,11.637359420282,43.7485486597646));
#274249=CARTESIAN_POINT('Ctrl Pts',(4.82218298524757,10.3566033615287,42.7713458847073));
#274250=CARTESIAN_POINT('Ctrl Pts',(4.80568122363092,10.2206044108969,42.6653934162803));
#274251=CARTESIAN_POINT('Ctrl Pts',(4.79296103895619,10.0856588106982,42.5580528390859));
#274252=CARTESIAN_POINT('',(4.79296103895619,13.4703202947425,40.098952328026));
#274253=CARTESIAN_POINT('Ctrl Pts',(4.79296103895619,13.4703202947425,40.098952328026));
#274254=CARTESIAN_POINT('Ctrl Pts',(4.80658157259404,13.5349809886778,40.2718952098376));
#274255=CARTESIAN_POINT('Ctrl Pts',(4.8245384335836,13.597757209446,40.4455016851685));
#274256=CARTESIAN_POINT('Ctrl Pts',(5.02532215959839,14.1467333648809,42.0165270533357));
#274257=CARTESIAN_POINT('Ctrl Pts',(5.47477154367343,14.4959246740922,43.4154003485369));
#274258=CARTESIAN_POINT('Ctrl Pts',(6.14788848420341,14.7212691391912,44.7249678641909));
#274259=CARTESIAN_POINT('',(4.76104848420342,13.2690897233691,39.2042535488964));
#274260=CARTESIAN_POINT('Ctrl Pts',(4.76104848420342,13.2690897233691,39.2042535488964));
#274261=CARTESIAN_POINT('Ctrl Pts',(4.76104848420342,13.2795592535557,39.3276041062441));
#274262=CARTESIAN_POINT('Ctrl Pts',(4.76253146428083,13.2968253885752,39.4503723241485));
#274263=CARTESIAN_POINT('Ctrl Pts',(4.76582551084842,13.3208566282573,39.5720421023193));
#274264=CARTESIAN_POINT('Ctrl Pts',(4.76903289751316,13.3442556531684,39.6905109873215));
#274265=CARTESIAN_POINT('Ctrl Pts',(4.77395775595489,13.3740686583141,39.807938232017));
#274266=CARTESIAN_POINT('Ctrl Pts',(4.78087052304866,13.4102701796273,39.923810455727));
#274267=CARTESIAN_POINT('Ctrl Pts',(4.78437875699033,13.4286424760013,39.9826156870622));
#274268=CARTESIAN_POINT('Ctrl Pts',(4.78839842591226,13.4486602237479,40.041019836584));
#274269=CARTESIAN_POINT('Ctrl Pts',(4.79296103895619,13.4703202947425,40.098952328026));
#274270=CARTESIAN_POINT('Origin',(4.76104848420342,-17.542318193471,0.972561099047131));
#274271=CARTESIAN_POINT('Origin',(15.4290484842034,-17.542318193471,0.972561099047131));
#274272=CARTESIAN_POINT('',(4.79296103895619,26.7032738510938,24.1023216086087));
#274273=CARTESIAN_POINT('Ctrl Pts',(4.79296103895619,26.7032738510938,24.1023216086087));
#274274=CARTESIAN_POINT('Ctrl Pts',(4.80658157259404,26.8326865415184,24.2340129191292));
#274275=CARTESIAN_POINT('Ctrl Pts',(4.8245384335836,26.9606475878415,24.3670769367848));
#274276=CARTESIAN_POINT('Ctrl Pts',(5.02532215959839,28.1011558454284,25.578991307125));
#274277=CARTESIAN_POINT('Ctrl Pts',(5.47477154367343,28.9891310079851,26.7148967508737));
#274278=CARTESIAN_POINT('Ctrl Pts',(6.14788848420341,29.7276425156794,27.8195903550057));
#274279=CARTESIAN_POINT('',(4.76104848420342,26.1555337986896,23.3668214500611));
#274280=CARTESIAN_POINT('Ctrl Pts',(4.76104848420342,26.1555337986896,23.3668214500611));
#274281=CARTESIAN_POINT('Ctrl Pts',(4.76104848420342,26.2152697101275,23.475250045361));
#274282=CARTESIAN_POINT('Ctrl Pts',(4.76253148048463,26.2809778173993,23.5803821574501));
#274283=CARTESIAN_POINT('Ctrl Pts',(4.76582556302885,26.3524194305639,23.6817591254482));
#274284=CARTESIAN_POINT('Ctrl Pts',(4.76903298691825,26.4219816026365,23.7804691318395));
#274285=CARTESIAN_POINT('Ctrl Pts',(4.77395790368511,26.4969796196788,23.8756186960783));
#274286=CARTESIAN_POINT('Ctrl Pts',(4.78087075471303,26.5771814108115,23.9667491847313));
#274287=CARTESIAN_POINT('Ctrl Pts',(4.78437893387748,26.617882743947,24.0129966852556));
#274288=CARTESIAN_POINT('Ctrl Pts',(4.78839852622406,26.6599240776223,24.0582085586405));
#274289=CARTESIAN_POINT('Ctrl Pts',(4.79296103895619,26.7032738510938,24.1023216086087));
#274290=CARTESIAN_POINT('',(4.76104848420342,23.70060616555,27.6188808395637));
#274291=CARTESIAN_POINT('Origin',(4.76104848420342,-17.542318193471,0.972561099047131));
#274292=CARTESIAN_POINT('',(4.79296103895619,24.6114380135418,27.7254875603422));
#274293=CARTESIAN_POINT('Ctrl Pts',(4.79296103895619,24.6114380135418,27.7254875603422));
#274294=CARTESIAN_POINT('Ctrl Pts',(4.77035892158035,24.3148103438982,27.6487744289659));
#274295=CARTESIAN_POINT('Ctrl Pts',(4.76104848420342,24.008477759664,27.6127082756377));
#274296=CARTESIAN_POINT('Ctrl Pts',(4.76104848420342,23.70060616555,27.6188808395637));
#274297=CARTESIAN_POINT('Ctrl Pts',(6.14788848420342,29.3428715129083,28.4860332810845));
#274298=CARTESIAN_POINT('Ctrl Pts',(6.12358695752486,29.2950008230139,28.4828842736815));
#274299=CARTESIAN_POINT('Ctrl Pts',(6.099576183545,29.2469915457218,28.4795910574544));
#274300=CARTESIAN_POINT('Ctrl Pts',(5.43709796638904,27.9022704036925,28.3835177865884));
#274301=CARTESIAN_POINT('Ctrl Pts',(5.01156238585603,26.5132053307471,28.181926112665));
#274302=CARTESIAN_POINT('Ctrl Pts',(4.82218298524757,24.9457122745935,27.8101373762519));
#274303=CARTESIAN_POINT('Ctrl Pts',(4.80568122363092,24.7783762996661,27.7686607366362));
#274304=CARTESIAN_POINT('Ctrl Pts',(4.79296103895619,24.6114380135418,27.7254875603422));
#274305=CARTESIAN_POINT('Origin',(15.4290484842034,-17.542318193471,0.972561099047131));
#274306=CARTESIAN_POINT('',(4.76104848420342,28.3394307068727,18.4617086838663));
#274307=CARTESIAN_POINT('Ctrl Pts',(4.79296103895619,29.2525234772273,18.3766132024512));
#274308=CARTESIAN_POINT('Ctrl Pts',(4.77035892158037,28.9464282770021,18.3632487973896));
#274309=CARTESIAN_POINT('Ctrl Pts',(4.76104848420342,28.639291219787,18.3916609015845));
#274310=CARTESIAN_POINT('Ctrl Pts',(4.76104848420342,28.3394307068727,18.4617086838663));
#274311=CARTESIAN_POINT('',(4.79296103895618,30.5453491237196,14.397704993804));
#274312=CARTESIAN_POINT('Ctrl Pts',(4.79296103895619,30.5453491237196,14.397704993804));
#274313=CARTESIAN_POINT('Ctrl Pts',(4.80658157259404,30.6993139993992,14.4996121219477));
#274314=CARTESIAN_POINT('Ctrl Pts',(4.8245384335836,30.8521443547454,14.6031637740616));
#274315=CARTESIAN_POINT('Ctrl Pts',(5.02532215959839,32.2197009363848,15.5514699074782));
#274316=CARTESIAN_POINT('Ctrl Pts',(5.47477154367344,33.3244397325698,16.4779326744902));
#274317=CARTESIAN_POINT('Ctrl Pts',(6.14788848420341,34.276491707006,17.4049408966648));
#274318=CARTESIAN_POINT('',(4.76104848420342,29.8566594240743,13.7921588388053));
#274319=CARTESIAN_POINT('Ctrl Pts',(4.76104848420342,29.8566594240743,13.7921588388053));
#274320=CARTESIAN_POINT('Ctrl Pts',(4.76104848420342,29.9376329966339,13.8857975921032));
#274321=CARTESIAN_POINT('Ctrl Pts',(4.76253146088426,30.0237628247058,13.9749702764883));
#274322=CARTESIAN_POINT('Ctrl Pts',(4.76582549808585,30.1147200651718,14.0592778788154));
#274323=CARTESIAN_POINT('Ctrl Pts',(4.76903287597333,30.2032844085363,14.1413675222838));
#274324=CARTESIAN_POINT('Ctrl Pts',(4.77395772034131,30.2964254868314,14.2188444200085));
#274325=CARTESIAN_POINT('Ctrl Pts',(4.78087046544997,30.3938209389826,14.2913082108793));
#274326=CARTESIAN_POINT('Ctrl Pts',(4.78437871324177,30.443249548684,14.3280838955475));
#274327=CARTESIAN_POINT('Ctrl Pts',(4.78839840126576,30.4937736154865,14.3635679095932));
#274328=CARTESIAN_POINT('Ctrl Pts',(4.79296103895619,30.5453491237196,14.397704993804));
#274329=CARTESIAN_POINT('Origin',(4.76104848420342,-17.542318193471,0.972561099047131));
#274330=CARTESIAN_POINT('Origin',(15.4290484842034,-17.542318193471,0.972561099047131));
#274331=CARTESIAN_POINT('',(4.79296103895619,18.1280311274453,35.9051306570905));
#274332=CARTESIAN_POINT('',(4.76104848420342,17.2592679242297,35.6114809593723));
#274333=CARTESIAN_POINT('Ctrl Pts',(4.79296103895619,18.1280311274453,35.9051306570905));
#274334=CARTESIAN_POINT('Ctrl Pts',(4.77035892158039,17.853835040925,35.7684215313513));
#274335=CARTESIAN_POINT('Ctrl Pts',(4.76104848420342,17.5616951335496,35.6694533844648));
#274336=CARTESIAN_POINT('Ctrl Pts',(4.76104848420342,17.2592679242297,35.6114809593723));
#274337=CARTESIAN_POINT('Ctrl Pts',(6.14788848420341,22.5979451061385,37.632776967928));
#274338=CARTESIAN_POINT('Ctrl Pts',(6.12358695752485,22.5517752211263,37.6197438978156));
#274339=CARTESIAN_POINT('Ctrl Pts',(6.099576183545,22.5054997598841,37.6065409562476));
#274340=CARTESIAN_POINT('Ctrl Pts',(5.43709796638902,21.2101387573402,37.2329838705376));
#274341=CARTESIAN_POINT('Ctrl Pts',(5.01156238585603,19.8933413547557,36.7469945903896));
#274342=CARTESIAN_POINT('Ctrl Pts',(4.82218298524757,18.4374010075269,36.0574301982373));
#274343=CARTESIAN_POINT('Ctrl Pts',(4.80568122363092,18.2823452034071,35.9820688172288));
#274344=CARTESIAN_POINT('Ctrl Pts',(4.79296103895619,18.1280311274453,35.9051306570905));
#274345=CARTESIAN_POINT('',(4.79296103895619,20.927453892214,32.7960567002406));
#274346=CARTESIAN_POINT('Ctrl Pts',(4.79296103895619,20.927453892214,32.7960567002406));
#274347=CARTESIAN_POINT('Ctrl Pts',(4.80658157259404,21.026658441821,32.9517766509431));
#274348=CARTESIAN_POINT('Ctrl Pts',(4.8245384335836,21.1241576673716,33.1085374980568));
#274349=CARTESIAN_POINT('Ctrl Pts',(5.02532215959839,21.9877719172835,34.5310936319264));
#274350=CARTESIAN_POINT('Ctrl Pts',(5.47477154367344,22.6201746706307,35.826797233841));
#274351=CARTESIAN_POINT('Ctrl Pts',(6.1478884842034,23.1128692149255,37.0608958085218));
#274352=CARTESIAN_POINT('',(4.76104848420342,20.5446023556894,31.962747424394));
#274353=CARTESIAN_POINT('Ctrl Pts',(4.76104848420342,20.5446023556894,31.962747424394));
#274354=CARTESIAN_POINT('Ctrl Pts',(4.76104848420342,20.5804893278971,32.0812264100145));
#274355=CARTESIAN_POINT('Ctrl Pts',(4.76253148100033,20.6229033704963,32.197722642335));
#274356=CARTESIAN_POINT('Ctrl Pts',(4.76582556519821,20.6717063717276,32.3117378555962));
#274357=CARTESIAN_POINT('Ctrl Pts',(4.76903299054366,20.7192254919687,32.422753622897));
#274358=CARTESIAN_POINT('Ctrl Pts',(4.77395790968128,20.7728019328613,32.5314169312464));
#274359=CARTESIAN_POINT('Ctrl Pts',(4.78087076460355,20.8323040513083,32.6372309180115));
#274360=CARTESIAN_POINT('Ctrl Pts',(4.78437894136499,20.8625005405358,32.6909300298225));
#274361=CARTESIAN_POINT('Ctrl Pts',(4.78839853042471,20.8942230647019,32.743894749579));
#274362=CARTESIAN_POINT('Ctrl Pts',(4.79296103895619,20.927453892214,32.7960567002406));
#274363=CARTESIAN_POINT('Origin',(4.76104848420342,-17.542318193471,0.972561099047131));
#274364=CARTESIAN_POINT('Origin',(15.4290484842034,-17.542318193471,0.972561099047131));
#274365=CARTESIAN_POINT('',(4.79296103895619,-67.370398971297,-2.16122297171674));
#274366=CARTESIAN_POINT('Ctrl Pts',(4.79296103895618,-67.370398971297,-2.16122297171673));
#274367=CARTESIAN_POINT('Ctrl Pts',(4.80658157259404,-67.5421870283591,
-2.22889208697901));
#274368=CARTESIAN_POINT('Ctrl Pts',(4.8245384335836,-67.7132072728381,-2.29840566945804));
#274369=CARTESIAN_POINT('Ctrl Pts',(5.02532215959839,-69.248043393648,-2.94165803744303));
#274370=CARTESIAN_POINT('Ctrl Pts',(5.47477154367342,-70.521263436943,-3.61818725913814));
#274371=CARTESIAN_POINT('Ctrl Pts',(6.14788848420341,-71.6452466383859,
-4.32699539176736));
#274372=CARTESIAN_POINT('',(4.76104848420342,-66.5708586689849,-1.71209609297323));
#274373=CARTESIAN_POINT('Ctrl Pts',(4.76104848420342,-66.5708586689849,
-1.71209609297323));
#274374=CARTESIAN_POINT('Ctrl Pts',(4.76104848420342,-66.669531832499,-1.78685361572226));
#274375=CARTESIAN_POINT('Ctrl Pts',(4.76253147480136,-66.7723200664169,
-1.85617057016433));
#274376=CARTESIAN_POINT('Ctrl Pts',(4.76582554519776,-66.8788187601492,
-1.91972502885798));
#274377=CARTESIAN_POINT('Ctrl Pts',(4.76903295628211,-66.9825157215496,
-1.98160751791974));
#274378=CARTESIAN_POINT('Ctrl Pts',(4.77395785306817,-67.0897304064449,
-2.03802645188551));
#274379=CARTESIAN_POINT('Ctrl Pts',(4.78087067578871,-67.2000642630108,
-2.08865723673717));
#274380=CARTESIAN_POINT('Ctrl Pts',(4.78437887355539,-67.2560577413395,
-2.11435192232688));
#274381=CARTESIAN_POINT('Ctrl Pts',(4.78839849197368,-67.3128541568119,
-2.13855546647373));
#274382=CARTESIAN_POINT('Ctrl Pts',(4.79296103895619,-67.370398971297,-2.16122297171674));
#274383=CARTESIAN_POINT('',(4.76104848420342,-66.0576390431341,-6.59505465837713));
#274384=CARTESIAN_POINT('Origin',(4.76104848420342,-17.542318193471,0.972561099047131));
#274385=CARTESIAN_POINT('',(4.79296103895619,-66.9330862002819,-6.32197605563978));
#274386=CARTESIAN_POINT('Ctrl Pts',(4.79296103895618,-66.9330862002819,
-6.32197605563978));
#274387=CARTESIAN_POINT('Ctrl Pts',(4.77035892158033,-66.6309012985319,
-6.37254446552365));
#274388=CARTESIAN_POINT('Ctrl Pts',(4.76104848420342,-66.3363831315434,
-6.46419308195223));
#274389=CARTESIAN_POINT('Ctrl Pts',(4.76104848420342,-66.0576390431341,
-6.59505465837713));
#274390=CARTESIAN_POINT('Ctrl Pts',(6.14788848420341,-71.5648075951267,
-5.0923217656847));
#274391=CARTESIAN_POINT('Ctrl Pts',(6.12358695752485,-71.5197947271193,
-5.10891576798505));
#274392=CARTESIAN_POINT('Ctrl Pts',(6.099576183545,-71.4745965982113,-5.12543439754196));
#274393=CARTESIAN_POINT('Ctrl Pts',(5.43709796638902,-70.2070561874331,
-5.58461446052352));
#274394=CARTESIAN_POINT('Ctrl Pts',(5.01156238585603,-68.8560873789502,
-5.96543496729592));
#274395=CARTESIAN_POINT('Ctrl Pts',(4.82218298524757,-67.2728911150327,
-6.26334591964759));
#274396=CARTESIAN_POINT('Ctrl Pts',(4.80568122363092,-67.1031520260742,
-6.29351679663613));
#274397=CARTESIAN_POINT('Ctrl Pts',(4.79296103895619,-66.933086200282,-6.32197605563978));
#274398=CARTESIAN_POINT('Origin',(15.4290484842034,-17.542318193471,0.972561099047131));
#274399=CARTESIAN_POINT('',(4.79296103895619,-67.370398971297,4.1063451698103));
#274400=CARTESIAN_POINT('',(4.76104848420342,-66.570858668985,3.65721829106681));
#274401=CARTESIAN_POINT('Ctrl Pts',(4.79296103895618,-67.370398971297,4.1063451698103));
#274402=CARTESIAN_POINT('Ctrl Pts',(4.7703589215748,-67.0853312982033,3.99405402711951));
#274403=CARTESIAN_POINT('Ctrl Pts',(4.76104848420342,-66.8163038786029,
3.84317438275566));
#274404=CARTESIAN_POINT('Ctrl Pts',(4.76104848420342,-66.570858668985,3.65721829106682));
#274405=CARTESIAN_POINT('Ctrl Pts',(6.14788848420341,-71.645246638386,6.27211758986087));
#274406=CARTESIAN_POINT('Ctrl Pts',(6.12358695752485,-71.6046674966181,
6.24652750482824));
#274407=CARTESIAN_POINT('Ctrl Pts',(6.099576183545,-71.5638914714703,6.22097262755666));
#274408=CARTESIAN_POINT('Ctrl Pts',(5.43709796638903,-70.4195187631187,
5.50829028066173));
#274409=CARTESIAN_POINT('Ctrl Pts',(5.01156238585603,-69.1772488998961,
4.85490940643834));
#274410=CARTESIAN_POINT('Ctrl Pts',(4.82218298524757,-67.6905884426711,
4.23434351103579));
#274411=CARTESIAN_POINT('Ctrl Pts',(4.80568122363092,-67.5308314381037,
4.16954119911417));
#274412=CARTESIAN_POINT('Ctrl Pts',(4.79296103895618,-67.370398971297,4.1063451698103));
#274413=CARTESIAN_POINT('',(4.79296103895619,-66.933086200282,8.26709825373337));
#274414=CARTESIAN_POINT('Ctrl Pts',(4.79296103895619,-66.933086200282,8.26709825373337));
#274415=CARTESIAN_POINT('Ctrl Pts',(4.80658157259404,-67.1151894763023,
8.23662461640187));
#274416=CARTESIAN_POINT('Ctrl Pts',(4.8245384335836,-67.2969252045845,8.20418718067529));
#274417=CARTESIAN_POINT('Ctrl Pts',(5.02532215959839,-68.9319611611245,
7.89410179327018));
#274418=CARTESIAN_POINT('Ctrl Pts',(5.47477154367344,-70.31801662605,7.49707369022733));
#274419=CARTESIAN_POINT('Ctrl Pts',(6.14788848420342,-71.5648075951268,
7.03744396377821));
#274420=CARTESIAN_POINT('',(4.76104848420342,-66.0576390431342,8.54017685647074));
#274421=CARTESIAN_POINT('Ctrl Pts',(4.76104848420342,-66.0576390431342,
8.54017685647073));
#274422=CARTESIAN_POINT('Ctrl Pts',(4.76104848420342,-66.1696919168572,
8.48757155896645));
#274423=CARTESIAN_POINT('Ctrl Pts',(4.76253129040183,-66.2846386577921,
8.44114267243526));
#274424=CARTESIAN_POINT('Ctrl Pts',(4.76582494299244,-66.4020164824655,
8.40112098163002));
#274425=CARTESIAN_POINT('Ctrl Pts',(4.76903192598719,-66.5163056120359,
8.3621524267195));
#274426=CARTESIAN_POINT('Ctrl Pts',(4.77395615055237,-66.6328994339606,
8.32925854949861));
#274427=CARTESIAN_POINT('Ctrl Pts',(4.7808679979395,-66.7513405603554,8.30267399608132));
#274428=CARTESIAN_POINT('Ctrl Pts',(4.78437682990909,-66.8114677575475,
8.2891782219846));
#274429=CARTESIAN_POINT('Ctrl Pts',(4.78839733376406,-66.8720705537315,
8.27730877122192));
#274430=CARTESIAN_POINT('Ctrl Pts',(4.79296103895619,-66.933086200282,8.26709825373337));
#274431=CARTESIAN_POINT('Origin',(4.76104848420342,-17.542318193471,0.972561099047131));
#274432=CARTESIAN_POINT('Origin',(15.4290484842034,-17.542318193471,0.972561099047131));
#274433=CARTESIAN_POINT('',(4.79296103895619,-65.6299855106617,14.3977049938037));
#274434=CARTESIAN_POINT('',(4.76104848420342,-64.9412958110163,13.792158838805));
#274435=CARTESIAN_POINT('Ctrl Pts',(4.79296103895619,-65.6299855106617,
14.3977049938037));
#274436=CARTESIAN_POINT('Ctrl Pts',(4.77035892158033,-65.3744938915815,
14.228598780128));
#274437=CARTESIAN_POINT('Ctrl Pts',(4.76104848420342,-65.1427150085247,
14.0250822723247));
#274438=CARTESIAN_POINT('Ctrl Pts',(4.76104848420342,-64.9412958110163,
13.792158838805));
#274439=CARTESIAN_POINT('Ctrl Pts',(6.14788848420341,-69.361128093948,17.4049408966644));
#274440=CARTESIAN_POINT('Ctrl Pts',(6.12358695752485,-69.3267561816353,
17.3714731384103));
#274441=CARTESIAN_POINT('Ctrl Pts',(6.099576183545,-69.2921843682116,17.3379988841867));
#274442=CARTESIAN_POINT('Ctrl Pts',(5.437097966389,-68.3209939409511,16.402961891767));
#274443=CARTESIAN_POINT('Ctrl Pts',(5.01156238585602,-67.2417161770838,
15.5055765295655));
#274444=CARTESIAN_POINT('Ctrl Pts',(4.82218298524757,-65.9165657223203,
14.5894773985467));
#274445=CARTESIAN_POINT('Ctrl Pts',(4.80568122363092,-65.7737729498428,
14.492875823679));
#274446=CARTESIAN_POINT('Ctrl Pts',(4.79296103895619,-65.6299855106617,
14.3977049938037));
#274447=CARTESIAN_POINT('',(4.76104848420342,-63.4240670938148,18.461708683866));
#274448=CARTESIAN_POINT('Ctrl Pts',(4.76104848420342,-63.4240670938148,
18.461708683866));
#274449=CARTESIAN_POINT('Ctrl Pts',(4.76104848420342,-63.5446128669712,
18.4335490439355));
#274450=CARTESIAN_POINT('Ctrl Pts',(4.76253139478368,-63.6667050910714,
18.4120329930263));
#274451=CARTESIAN_POINT('Ctrl Pts',(4.76582528398501,-63.7898431598502,
18.3972900560778));
#274452=CARTESIAN_POINT('Ctrl Pts',(4.76903250936003,-63.9097414061722,
18.3829350129682));
#274453=CARTESIAN_POINT('Ctrl Pts',(4.7739571145476,-64.0306310087032,18.3750015769542));
#274454=CARTESIAN_POINT('Ctrl Pts',(4.78086951428214,-64.1520158222007,
18.3736241726316));
#274455=CARTESIAN_POINT('Ctrl Pts',(4.78437798712838,-64.2136261657077,
18.3729250542574));
#274456=CARTESIAN_POINT('Ctrl Pts',(4.78839798959814,-64.2753635517415,
18.373915117182));
#274457=CARTESIAN_POINT('Ctrl Pts',(4.79296103895619,-64.3371598641695,
18.3766132024509));
#274458=CARTESIAN_POINT('Origin',(4.76104848420342,-17.542318193471,0.972561099047131));
#274459=CARTESIAN_POINT('Origin',(15.4290484842034,-17.542318193471,0.972561099047131));
#274460=CARTESIAN_POINT('',(4.79296103895619,-59.6960744004839,27.7254875603419));
#274461=CARTESIAN_POINT('Ctrl Pts',(4.79296103895618,-59.6960744004839,
27.7254875603419));
#274462=CARTESIAN_POINT('Ctrl Pts',(4.80658157259404,-59.8748287660646,
27.7717165825615));
#274463=CARTESIAN_POINT('Ctrl Pts',(4.8245384335836,-60.0540461088455,27.8160020905443));
#274464=CARTESIAN_POINT('Ctrl Pts',(5.0253221595984,-61.673848869565,28.1977540296704));
#274465=CARTESIAN_POINT('Ctrl Pts',(5.47477154367345,-63.1015594214269,
28.3988103564998));
#274466=CARTESIAN_POINT('Ctrl Pts',(6.14788848420342,-64.4275078998505,
28.4860332810842));
#274467=CARTESIAN_POINT('',(4.76104848420342,-58.7852425524921,27.6188808395635));
#274468=CARTESIAN_POINT('Ctrl Pts',(4.76104848420342,-58.7852425524921,
27.6188808395635));
#274469=CARTESIAN_POINT('Ctrl Pts',(4.76104848420342,-58.9090110779737,
27.6163993857685));
#274470=CARTESIAN_POINT('Ctrl Pts',(4.76253144835227,-59.0329109135381,
27.6207381048775));
#274471=CARTESIAN_POINT('Ctrl Pts',(4.7658254588955,-59.1564254863122,27.6319196149988));
#274472=CARTESIAN_POINT('Ctrl Pts',(4.76903280861577,-59.2766905629532,
27.6428069551847));
#274473=CARTESIAN_POINT('Ctrl Pts',(4.77395760905528,-59.3965901622967,
27.6601819444716));
#274474=CARTESIAN_POINT('Ctrl Pts',(4.7808702920541,-59.5156110492459,27.6840729200258));
#274475=CARTESIAN_POINT('Ctrl Pts',(4.78437858069741,-59.5760159059524,
27.6961979427165));
#274476=CARTESIAN_POINT('Ctrl Pts',(4.78839832599606,-59.6361938640674,
27.710001400664));
#274477=CARTESIAN_POINT('Ctrl Pts',(4.79296103895619,-59.6960744004839,
27.7254875603419));
#274478=CARTESIAN_POINT('',(4.76104848420342,-61.2401701856317,23.3668214500608));
#274479=CARTESIAN_POINT('Origin',(4.76104848420342,-17.542318193471,0.972561099047131));
#274480=CARTESIAN_POINT('',(4.79296103895619,-61.7879102380359,24.1023216086084));
#274481=CARTESIAN_POINT('Ctrl Pts',(4.79296103895618,-61.7879102380359,
24.1023216086084));
#274482=CARTESIAN_POINT('Ctrl Pts',(4.77035892157486,-61.5731608825862,
23.8837910768667));
#274483=CARTESIAN_POINT('Ctrl Pts',(4.76104848420342,-61.3887603854858,
23.636532353564));
#274484=CARTESIAN_POINT('Ctrl Pts',(4.76104848420342,-61.2401701856317,
23.3668214500608));
#274485=CARTESIAN_POINT('Ctrl Pts',(6.14788848420341,-64.8122789026216,
27.8195903550054));
#274486=CARTESIAN_POINT('Ctrl Pts',(6.12358695752485,-64.7856164372667,
27.7797076251616));
#274487=CARTESIAN_POINT('Ctrl Pts',(6.099576183545,-64.7587597897078,27.7397769795229));
#274488=CARTESIAN_POINT('Ctrl Pts',(5.43709796638903,-64.0031973254985,
26.6232509449525));
#274489=CARTESIAN_POINT('Ctrl Pts',(5.01156238585602,-63.1340812782167,
25.5210811412337));
#274490=CARTESIAN_POINT('Ctrl Pts',(4.82218298524757,-62.0283562595653,
24.3494867025556));
#274491=CARTESIAN_POINT('Ctrl Pts',(4.80568122363092,-61.9087684485308,
24.2253078171093));
#274492=CARTESIAN_POINT('Ctrl Pts',(4.79296103895619,-61.7879102380359,
24.1023216086084));
#274493=CARTESIAN_POINT('Origin',(15.4290484842034,-17.542318193471,0.972561099047131));
#274494=CARTESIAN_POINT('',(4.79296103895619,-56.0120902791562,32.7960567002403));
#274495=CARTESIAN_POINT('',(4.76104848420342,-55.6292387426316,31.9627474243937));
#274496=CARTESIAN_POINT('Ctrl Pts',(4.79296103895618,-56.0120902791562,
32.7960567002403));
#274497=CARTESIAN_POINT('Ctrl Pts',(4.77035892158035,-55.8474687647536,
32.5376526833993));
#274498=CARTESIAN_POINT('Ctrl Pts',(4.76104848420342,-55.718505840154,32.25745813731));
#274499=CARTESIAN_POINT('Ctrl Pts',(4.76104848420342,-55.6292387426316,
31.9627474243937));
#274500=CARTESIAN_POINT('Ctrl Pts',(6.14788848420341,-58.1975056018678,
37.0608958085216));
#274501=CARTESIAN_POINT('Ctrl Pts',(6.12358695752485,-58.1797178611475,
37.0163411737608));
#274502=CARTESIAN_POINT('Ctrl Pts',(6.09957618354499,-58.1617501438242,
36.9716992975299));
#274503=CARTESIAN_POINT('Ctrl Pts',(5.43709796638901,-57.6548373479429,
35.7224817662058));
#274504=CARTESIAN_POINT('Ctrl Pts',(5.01156238585602,-57.0338675589944,
34.4636976301899));
#274505=CARTESIAN_POINT('Ctrl Pts',(4.82218298524757,-56.1958934656274,
33.0878121827565));
#274506=CARTESIAN_POINT('Ctrl Pts',(4.80568122363092,-56.104737177224,32.941483199902));
#274507=CARTESIAN_POINT('Ctrl Pts',(4.79296103895619,-56.0120902791562,
32.7960567002403));
#274508=CARTESIAN_POINT('',(4.79296103895619,-53.2126675143875,35.9051306570903));
#274509=CARTESIAN_POINT('Ctrl Pts',(4.79296103895618,-53.2126675143875,
35.9051306570903));
#274510=CARTESIAN_POINT('Ctrl Pts',(4.80658157259404,-53.3779041140264,
35.9875145866475));
#274511=CARTESIAN_POINT('Ctrl Pts',(4.8245384335836,-53.543997653034,36.0680937307897));
#274512=CARTESIAN_POINT('Ctrl Pts',(5.02532215959839,-55.0490331459571,
36.7782794048937));
#274513=CARTESIAN_POINT('Ctrl Pts',(5.47477154367343,-56.4037428359424,
37.2717798834302));
#274514=CARTESIAN_POINT('Ctrl Pts',(6.14788848420341,-57.6825814930807,
37.6327769679277));
#274515=CARTESIAN_POINT('',(4.76104848420342,-52.343904311172,35.6114809593721));
#274516=CARTESIAN_POINT('Ctrl Pts',(4.76104848420342,-52.343904311172,35.6114809593721));
#274517=CARTESIAN_POINT('Ctrl Pts',(4.76104848420342,-52.465485215972,35.6347868646577));
#274518=CARTESIAN_POINT('Ctrl Pts',(4.7625314749205,-52.5857765087052,35.6647913142045));
#274519=CARTESIAN_POINT('Ctrl Pts',(4.76582554549142,-52.7042682136469,
35.7014090350176));
#274520=CARTESIAN_POINT('Ctrl Pts',(4.76903295680144,-52.8196426800984,
35.7370634295895));
#274521=CARTESIAN_POINT('Ctrl Pts',(4.77395785392526,-52.9333107491858,
35.778987834308));
#274522=CARTESIAN_POINT('Ctrl Pts',(4.78087067704644,-53.0447645175907,
35.8271032630079));
#274523=CARTESIAN_POINT('Ctrl Pts',(4.78437887452713,-53.1013263336066,
35.851521423691));
#274524=CARTESIAN_POINT('Ctrl Pts',(4.78839849253279,-53.1573172853332,
35.8775340508823));
#274525=CARTESIAN_POINT('Ctrl Pts',(4.79296103895619,-53.2126675143875,
35.9051306570903));
#274526=CARTESIAN_POINT('Origin',(4.76104848420342,-17.542318193471,0.972561099047131));
#274527=CARTESIAN_POINT('Origin',(15.4290484842034,-17.542318193471,0.972561099047131));
#274528=CARTESIAN_POINT('',(4.79296103895619,-45.1702951976404,42.5580528390857));
#274529=CARTESIAN_POINT('Ctrl Pts',(4.79296103895619,-45.1702951976404,
42.5580528390857));
#274530=CARTESIAN_POINT('Ctrl Pts',(4.80658157259404,-45.3147923990402,
42.672991102937));
#274531=CARTESIAN_POINT('Ctrl Pts',(4.8245384335836,-45.4605030496147,42.7863421879778));
#274532=CARTESIAN_POINT('Ctrl Pts',(5.02532215959839,-46.7849940017391,
43.7939230752526));
#274533=CARTESIAN_POINT('Ctrl Pts',(5.47477154367344,-48.0074955157771,
44.5582993665061));
#274534=CARTESIAN_POINT('Ctrl Pts',(6.14788848420341,-49.1833329657644,
45.177293306068));
#274535=CARTESIAN_POINT('',(4.76104848420342,-44.3815697599701,42.0901940653056));
#274536=CARTESIAN_POINT('Ctrl Pts',(4.76104848420342,-44.3815697599701,
42.0901940653057));
#274537=CARTESIAN_POINT('Ctrl Pts',(4.76104848420342,-44.4956485670493,
42.1382689014767));
#274538=CARTESIAN_POINT('Ctrl Pts',(4.76253148285844,-44.6070732100943,
42.1926278033787));
#274539=CARTESIAN_POINT('Ctrl Pts',(4.76582557106135,-44.7153625908546,
42.2530813329808));
#274540=CARTESIAN_POINT('Ctrl Pts',(4.76903300061106,-44.8208031675407,
42.3119444918539));
#274541=CARTESIAN_POINT('Ctrl Pts',(4.7739579263149,-44.9232710031647,42.3765858961933));
#274542=CARTESIAN_POINT('Ctrl Pts',(4.78087079057214,-45.0222857184793,
42.4468226877301));
#274543=CARTESIAN_POINT('Ctrl Pts',(4.78437896120848,-45.0725341399594,
42.4824667623845));
#274544=CARTESIAN_POINT('Ctrl Pts',(4.7883985416886,-45.1218926824315,42.5195517400314));
#274545=CARTESIAN_POINT('Ctrl Pts',(4.79296103895619,-45.1702951976404,
42.5580528390857));
#274546=CARTESIAN_POINT('',(4.76104848420342,-48.3537261103113,39.2042535488962));
#274547=CARTESIAN_POINT('Origin',(4.76104848420342,-17.542318193471,0.972561099047131));
#274548=CARTESIAN_POINT('',(4.79296103895619,-48.5549566816847,40.0989523280257));
#274549=CARTESIAN_POINT('Ctrl Pts',(4.79296103895619,-48.5549566816847,
40.0989523280257));
#274550=CARTESIAN_POINT('Ctrl Pts',(4.77035892158593,-48.4476577584246,
39.8119683215992));
#274551=CARTESIAN_POINT('Ctrl Pts',(4.76104848420342,-48.3797687049592,
39.5110837989026));
#274552=CARTESIAN_POINT('Ctrl Pts',(4.76104848420342,-48.3537261103113,
39.2042535488962));
#274553=CARTESIAN_POINT('Ctrl Pts',(6.14788848420341,-49.8059055261334,
44.7249678641907));
#274554=CARTESIAN_POINT('Ctrl Pts',(6.12358695752485,-49.7977699196723,
44.677688575849));
#274555=CARTESIAN_POINT('Ctrl Pts',(6.099576183545,-49.7894764080503,44.6302865332326));
#274556=CARTESIAN_POINT('Ctrl Pts',(5.43709796638902,-49.5533678021145,
43.3029743056845));
#274557=CARTESIAN_POINT('Ctrl Pts',(5.01156238585602,-49.2076836310201,
41.9425907444318));
#274558=CARTESIAN_POINT('Ctrl Pts',(4.82218298524757,-48.6740839518635,
40.4225470845268));
#274559=CARTESIAN_POINT('Ctrl Pts',(4.80568122363092,-48.6153431533108,
40.2604632829792));
#274560=CARTESIAN_POINT('Ctrl Pts',(4.79296103895619,-48.5549566816847,
40.0989523280258));
#274561=CARTESIAN_POINT('Origin',(15.4290484842034,-17.542318193471,0.972561099047131));
#274562=CARTESIAN_POINT('',(4.79296103895619,-39.742421967128,45.6918369098492));
#274563=CARTESIAN_POINT('',(4.76104848420342,-39.7316071024862,44.7748512573257));
#274564=CARTESIAN_POINT('Ctrl Pts',(4.79296103895619,-39.742421967128,45.6918369098492));
#274565=CARTESIAN_POINT('Ctrl Pts',(4.77035892158033,-39.6971351127824,
45.3888154918811));
#274566=CARTESIAN_POINT('Ctrl Pts',(4.76104848420342,-39.6932870078947,
45.0803910900121));
#274567=CARTESIAN_POINT('Ctrl Pts',(4.76104848420342,-39.7316071024862,
44.7748512573257));
#274568=CARTESIAN_POINT('Ctrl Pts',(6.14788848420341,-40.004231866093,50.4768497968822));
#274569=CARTESIAN_POINT('Ctrl Pts',(6.12358695752485,-40.0061039589323,
50.4289121867311));
#274570=CARTESIAN_POINT('Ctrl Pts',(6.099576183545,-40.0078471192661,50.3808216744519));
#274571=CARTESIAN_POINT('Ctrl Pts',(5.43709796638902,-40.0528617823301,
49.0334246641744));
#274572=CARTESIAN_POINT('Ctrl Pts',(5.01156238585603,-39.9975712861431,
47.6308969671561));
#274573=CARTESIAN_POINT('Ctrl Pts',(4.82218298524757,-39.7916668876715,
46.0331282966962));
#274574=CARTESIAN_POINT('Ctrl Pts',(4.80568122363092,-39.7679088337358,
45.8623735163475));
#274575=CARTESIAN_POINT('Ctrl Pts',(4.79296103895618,-39.742421967128,45.6918369098492));
#274576=CARTESIAN_POINT('',(4.79296103895619,-35.9204477120687,47.3934894827124));
#274577=CARTESIAN_POINT('Ctrl Pts',(4.79296103895619,-35.9204477120687,
47.3934894827124));
#274578=CARTESIAN_POINT('Ctrl Pts',(4.80658157259404,-36.0378902941536,
47.5359587271926));
#274579=CARTESIAN_POINT('Ctrl Pts',(4.82453843358361,-36.1568498016675,
47.6771277667969));
#274580=CARTESIAN_POINT('Ctrl Pts',(5.02532215959839,-37.2429096027727,
48.938067747559));
#274581=CARTESIAN_POINT('Ctrl Pts',(5.47477154367343,-38.2797737584869,
49.9399129397173));
#274582=CARTESIAN_POINT('Ctrl Pts',(6.14788848420341,-39.3012202624647,
50.7898507289222));
#274583=CARTESIAN_POINT('',(4.76104848420342,-35.2462311262942,46.7718693063201));
#274584=CARTESIAN_POINT('Ctrl Pts',(4.76104848420342,-35.2462311262942,
46.7718693063201));
#274585=CARTESIAN_POINT('Ctrl Pts',(4.76104848420342,-35.3478213939069,
46.8426116844765));
#274586=CARTESIAN_POINT('Ctrl Pts',(4.76253147347933,-35.4455089937174,
46.9189489429545));
#274587=CARTESIAN_POINT('Ctrl Pts',(4.7658255397648,-35.5388627266735,47.00059575335));
#274588=CARTESIAN_POINT('Ctrl Pts',(4.76903294718426,-35.6297605501445,
47.0800946348976));
#274589=CARTESIAN_POINT('Ctrl Pts',(4.77395783802111,-35.7165492566998,
47.1646273892827));
#274590=CARTESIAN_POINT('Ctrl Pts',(4.7808706510644,-35.7987969832442,47.253915274399));
#274591=CARTESIAN_POINT('Ctrl Pts',(4.78437885482598,-35.8405371231608,
47.2992282450329));
#274592=CARTESIAN_POINT('Ctrl Pts',(4.78839848145743,-35.8811072172091,
47.3457656462587));
#274593=CARTESIAN_POINT('Ctrl Pts',(4.79296103895619,-35.9204477120687,
47.3934894827124));
#274594=CARTESIAN_POINT('Origin',(4.76104848420342,-17.542318193471,0.972561099047131));
#274595=CARTESIAN_POINT('Origin',(15.4290484842034,-17.542318193471,0.972561099047131));
#274596=CARTESIAN_POINT('Ctrl Pts',(4.79296103895619,-19.6341540310225,
-48.9101258718094));
#274597=CARTESIAN_POINT('Ctrl Pts',(4.80658157259404,-19.5848123558664,
-49.0880462045495));
#274598=CARTESIAN_POINT('Ctrl Pts',(4.8245384335836,-19.5335560594086,-49.2653957301879));
#274599=CARTESIAN_POINT('Ctrl Pts',(5.02532215959839,-19.0542615562759,
-50.8590620396541));
#274600=CARTESIAN_POINT('Ctrl Pts',(5.47477154367343,-18.5145261669709,
-52.1960238102323));
#274601=CARTESIAN_POINT('Ctrl Pts',(6.14788848420341,-17.9270891962415,
-53.3879403389487));
#274602=CARTESIAN_POINT('Origin',(4.76104848420342,-17.542318193471,0.972561099047131));
#274603=CARTESIAN_POINT('Ctrl Pts',(6.1478884842034,-17.1575471906993,-53.3879403389487));
#274604=CARTESIAN_POINT('Ctrl Pts',(6.12358695752485,-17.1363389661598,
-53.344908601702));
#274605=CARTESIAN_POINT('Ctrl Pts',(6.099576183545,-17.1151863364266,-53.3016847398361));
#274606=CARTESIAN_POINT('Ctrl Pts',(5.43709796638902,-16.5260276586066,
-52.0890854343997));
#274607=CARTESIAN_POINT('Ctrl Pts',(5.01156238585603,-16.0060786329429,
-50.7853239567576));
#274608=CARTESIAN_POINT('Ctrl Pts',(4.82218298524757,-15.5443105954408,
-49.2419407816664));
#274609=CARTESIAN_POINT('Ctrl Pts',(4.80568122363092,-15.496562431548,-49.0762852566043));
#274610=CARTESIAN_POINT('Ctrl Pts',(4.79296103895619,-15.4504823559185,
-48.9101258718094));
#274611=CARTESIAN_POINT('Origin',(15.4290484842034,-17.542318193471,0.972561099047131));
#274612=CARTESIAN_POINT('Ctrl Pts',(6.14788848420341,-28.4681391279529,
-52.280031346979));
#274613=CARTESIAN_POINT('Ctrl Pts',(6.12358695752485,-28.4384475527539,
-52.2423493942589));
#274614=CARTESIAN_POINT('Ctrl Pts',(6.099576183545,-28.408770412527,-52.2044679564935));
#274615=CARTESIAN_POINT('Ctrl Pts',(5.43709796638901,-27.5803726934881,
-51.1408598320948));
#274616=CARTESIAN_POINT('Ctrl Pts',(5.01156238585602,-26.8007185482917,
-49.9736921518748));
#274617=CARTESIAN_POINT('Ctrl Pts',(4.82218298524757,-26.0281538448006,
-48.5600425755891));
#274618=CARTESIAN_POINT('Ctrl Pts',(4.80568122363092,-25.9470073725404,
-48.4079344226897));
#274619=CARTESIAN_POINT('Ctrl Pts',(4.79296103895619,-25.8673877784838,
-48.2549866055504));
#274620=CARTESIAN_POINT('Ctrl Pts',(4.79296103895619,-29.9596361897448,
-47.3851523537532));
#274621=CARTESIAN_POINT('Ctrl Pts',(4.80658157259404,-29.9483644657855,
-47.5694434114541));
#274622=CARTESIAN_POINT('Ctrl Pts',(4.8245384335836,-29.935101282124,-47.7535742077102));
#274623=CARTESIAN_POINT('Ctrl Pts',(5.02532215959839,-29.7976223708404,
-49.4120660152309));
#274624=CARTESIAN_POINT('Ctrl Pts',(5.47477154367343,-29.5476514770401,
-50.8320292607793));
#274625=CARTESIAN_POINT('Ctrl Pts',(6.1478884842034,-29.2208647943379,-52.1200345674514));
#274626=CARTESIAN_POINT('Origin',(4.76104848420342,-17.542318193471,0.972561099047131));
#274627=CARTESIAN_POINT('Origin',(15.4290484842034,-17.542318193471,0.972561099047131));
#274628=CARTESIAN_POINT('Ctrl Pts',(6.14788848420341,-39.301220262464,-48.8447285308283));
#274629=CARTESIAN_POINT('Ctrl Pts',(6.12358695752485,-39.2643430009178,
-48.8140432447869));
#274630=CARTESIAN_POINT('Ctrl Pts',(6.09957618354499,-39.2274383836317,
-48.7831598317274));
#274631=CARTESIAN_POINT('Ctrl Pts',(5.437097966389,-38.1960065787892,-47.9150276671609));
#274632=CARTESIAN_POINT('Ctrl Pts',(5.01156238585601,-37.1907219414009,
-46.9354646126805));
#274633=CARTESIAN_POINT('Ctrl Pts',(4.82218298524757,-36.14112535664,-45.7133319051272));
#274634=CARTESIAN_POINT('Ctrl Pts',(4.80568122363092,-36.0301270662342,
-45.5814189805682));
#274635=CARTESIAN_POINT('Ctrl Pts',(4.79296103895618,-35.920447712068,-45.4483672846184));
#274636=CARTESIAN_POINT('Ctrl Pts',(4.79296103895619,-39.7424219671274,
-43.7467147117553));
#274637=CARTESIAN_POINT('Ctrl Pts',(4.80658157259404,-39.7697128227896,
-43.9293220908689));
#274638=CARTESIAN_POINT('Ctrl Pts',(4.8245384335836,-39.7950224166943,-44.1121867583887));
#274639=CARTESIAN_POINT('Ctrl Pts',(5.02532215959839,-40.0053675853797,
-45.7630200136485));
#274640=CARTESIAN_POINT('Ctrl Pts',(5.47477154367342,-40.0560861146367,
-47.2039255265971));
#274641=CARTESIAN_POINT('Ctrl Pts',(6.14788848420341,-40.0042318660923,
-48.5317275987882));
#274642=CARTESIAN_POINT('Origin',(4.76104848420342,-17.542318193471,0.972561099047131));
#274643=CARTESIAN_POINT('Origin',(15.4290484842034,-17.542318193471,0.972561099047131));
#274644=CARTESIAN_POINT('Ctrl Pts',(4.79296103895618,-48.5549566816842,
-38.1538301299319));
#274645=CARTESIAN_POINT('Ctrl Pts',(4.80658157259404,-48.6196173756195,
-38.3267730117436));
#274646=CARTESIAN_POINT('Ctrl Pts',(4.8245384335836,-48.6823935963878,-38.5003794870745));
#274647=CARTESIAN_POINT('Ctrl Pts',(5.02532215959839,-49.2313697518226,
-40.0714048552417));
#274648=CARTESIAN_POINT('Ctrl Pts',(5.47477154367344,-49.5805610610339,
-41.4702781504429));
#274649=CARTESIAN_POINT('Ctrl Pts',(6.14788848420341,-49.8059055261328,
-42.7798456660969));
#274650=CARTESIAN_POINT('Origin',(4.76104848420342,-17.542318193471,0.972561099047131));
#274651=CARTESIAN_POINT('Ctrl Pts',(6.14788848420341,-49.1833329657638,
-43.2321711079742));
#274652=CARTESIAN_POINT('Ctrl Pts',(6.12358695752485,-49.1408817311566,
-43.2098235828558));
#274653=CARTESIAN_POINT('Ctrl Pts',(6.099576183545,-49.0983625456749,-43.1872879478481));
#274654=CARTESIAN_POINT('Ctrl Pts',(5.43709796638902,-47.9089751742594,
-42.5525732844655));
#274655=CARTESIAN_POINT('Ctrl Pts',(5.01156238585602,-46.7219958072237,
-41.8034264616706));
#274656=CARTESIAN_POINT('Ctrl Pts',(4.82218298524757,-45.4412397484704,
-40.8262236866132));
#274657=CARTESIAN_POINT('Ctrl Pts',(4.80568122363092,-45.3052407978386,
-40.7202712181862));
#274658=CARTESIAN_POINT('Ctrl Pts',(4.79296103895619,-45.1702951976398,
-40.6129306409918));
#274659=CARTESIAN_POINT('Origin',(15.4290484842034,-17.542318193471,0.972561099047131));
#274660=CARTESIAN_POINT('Ctrl Pts',(6.14788848420341,-57.6825814930802,
-35.687654769834));
#274661=CARTESIAN_POINT('Ctrl Pts',(6.12358695752484,-57.636411608068,-35.6746216997216));
#274662=CARTESIAN_POINT('Ctrl Pts',(6.09957618354498,-57.5901361468258,
-35.6614187581536));
#274663=CARTESIAN_POINT('Ctrl Pts',(5.43709796638901,-56.2947751442819,
-35.2878616724436));
#274664=CARTESIAN_POINT('Ctrl Pts',(5.01156238585601,-54.9779777416974,
-34.8018723922956));
#274665=CARTESIAN_POINT('Ctrl Pts',(4.82218298524757,-53.5220373944686,
-34.1123080001433));
#274666=CARTESIAN_POINT('Ctrl Pts',(4.80568122363092,-53.3669815903488,
-34.0369466191348));
#274667=CARTESIAN_POINT('Ctrl Pts',(4.79296103895619,-53.212667514387,-33.9600084589965));
#274668=CARTESIAN_POINT('Ctrl Pts',(4.79296103895619,-56.0120902791558,
-30.8509345021466));
#274669=CARTESIAN_POINT('Ctrl Pts',(4.80658157259404,-56.1112948287628,
-31.0066544528491));
#274670=CARTESIAN_POINT('Ctrl Pts',(4.8245384335836,-56.2087940543133,-31.1634152999628));
#274671=CARTESIAN_POINT('Ctrl Pts',(5.02532215959839,-57.0724083042252,
-32.5859714338324));
#274672=CARTESIAN_POINT('Ctrl Pts',(5.47477154367343,-57.7048110575724,
-33.881675035747));
#274673=CARTESIAN_POINT('Ctrl Pts',(6.14788848420341,-58.1975056018673,
-35.1157736104278));
#274674=CARTESIAN_POINT('Origin',(4.76104848420342,-17.542318193471,0.972561099047131));
#274675=CARTESIAN_POINT('Origin',(15.4290484842034,-17.542318193471,0.972561099047131));
#274676=CARTESIAN_POINT('Ctrl Pts',(4.79296103895619,-61.7879102380356,
-22.1571994105147));
#274677=CARTESIAN_POINT('Ctrl Pts',(4.80658157259404,-61.9173229284602,
-22.2888907210352));
#274678=CARTESIAN_POINT('Ctrl Pts',(4.8245384335836,-62.0452839747833,-22.4219547386908));
#274679=CARTESIAN_POINT('Ctrl Pts',(5.02532215959839,-63.1857922323702,
-23.633869109031));
#274680=CARTESIAN_POINT('Ctrl Pts',(5.47477154367342,-64.0737673949269,
-24.7697745527797));
#274681=CARTESIAN_POINT('Ctrl Pts',(6.14788848420341,-64.8122789026212,
-25.8744681569118));
#274682=CARTESIAN_POINT('Origin',(4.76104848420342,-17.542318193471,0.972561099047131));
#274683=CARTESIAN_POINT('Ctrl Pts',(6.14788848420341,-64.4275078998501,
-26.5409110829905));
#274684=CARTESIAN_POINT('Ctrl Pts',(6.12358695752485,-64.3796372099557,
-26.5377620755876));
#274685=CARTESIAN_POINT('Ctrl Pts',(6.099576183545,-64.3316279326636,-26.5344688593604));
#274686=CARTESIAN_POINT('Ctrl Pts',(5.43709796638901,-62.9869067906343,
-26.4383955884944));
#274687=CARTESIAN_POINT('Ctrl Pts',(5.01156238585603,-61.5978417176889,
-26.2368039145711));
#274688=CARTESIAN_POINT('Ctrl Pts',(4.82218298524757,-60.0303486615353,
-25.865015178158));
#274689=CARTESIAN_POINT('Ctrl Pts',(4.80568122363092,-59.8630126866079,
-25.8235385385422));
#274690=CARTESIAN_POINT('Ctrl Pts',(4.79296103895619,-59.6960744004836,
-25.7803653622482));
#274691=CARTESIAN_POINT('Origin',(15.4290484842034,-17.542318193471,0.972561099047131));
#274692=CARTESIAN_POINT('Ctrl Pts',(6.14788848420341,-69.1233265363499,
-16.1916966375046));
#274693=CARTESIAN_POINT('Ctrl Pts',(6.12358695752485,-69.0758472204306,
-16.1985693195453));
#274694=CARTESIAN_POINT('Ctrl Pts',(6.099576183545,-69.0282023628804,-16.2053297580107));
#274695=CARTESIAN_POINT('Ctrl Pts',(5.43709796638902,-67.6928918479603,
-16.3909391649362));
#274696=CARTESIAN_POINT('Ctrl Pts',(5.01156238585603,-66.2922679138154,
-16.4825556207321));
#274697=CARTESIAN_POINT('Ctrl Pts',(4.82218298524757,-64.6817291169572,
-16.4447914918798));
#274698=CARTESIAN_POINT('Ctrl Pts',(4.80568122363092,-64.5094263562936,
-16.4390123218349));
#274699=CARTESIAN_POINT('Ctrl Pts',(4.79296103895618,-64.3371598641692,
-16.4314910043572));
#274700=CARTESIAN_POINT('',(4.79296103895618,-65.6299855106615,-12.4525827957101));
#274701=CARTESIAN_POINT('Ctrl Pts',(4.79296103895619,-65.6299855106615,
-12.4525827957101));
#274702=CARTESIAN_POINT('Ctrl Pts',(4.80658157259404,-65.7839503863411,
-12.5544899238537));
#274703=CARTESIAN_POINT('Ctrl Pts',(4.8245384335836,-65.9367807416872,-12.6580415759677));
#274704=CARTESIAN_POINT('Ctrl Pts',(5.02532215959839,-67.3043373233267,
-13.6063477093843));
#274705=CARTESIAN_POINT('Ctrl Pts',(5.47477154367343,-68.4090761195117,
-14.5328104763962));
#274706=CARTESIAN_POINT('Ctrl Pts',(6.14788848420341,-69.3611280939478,
-15.4598186985709));
#274707=CARTESIAN_POINT('',(4.76104848420342,-64.9412958110162,-11.8470366407114));
#274708=CARTESIAN_POINT('Ctrl Pts',(4.76104848420342,-64.9412958110162,
-11.8470366407114));
#274709=CARTESIAN_POINT('Ctrl Pts',(4.76104848420342,-65.022269383582,-11.9406753940164));
#274710=CARTESIAN_POINT('Ctrl Pts',(4.76253146088449,-65.108399211661,-12.0298480784081));
#274711=CARTESIAN_POINT('Ctrl Pts',(4.76582549808661,-65.1993564521347,
-12.1141556807409));
#274712=CARTESIAN_POINT('Ctrl Pts',(4.76903287597436,-65.2879207954999,
-12.1962453242087));
#274713=CARTESIAN_POINT('Ctrl Pts',(4.77395772034264,-65.3810618737959,
-12.2737222219327));
#274714=CARTESIAN_POINT('Ctrl Pts',(4.78087046545162,-65.4784573259478,
-12.3461860128027));
#274715=CARTESIAN_POINT('Ctrl Pts',(4.78437871324304,-65.5278859356418,
-12.3829616974648));
#274716=CARTESIAN_POINT('Ctrl Pts',(4.78839840126648,-65.5784100024365,
-12.4184457115046));
#274717=CARTESIAN_POINT('Ctrl Pts',(4.79296103895619,-65.6299855106615,
-12.4525827957101));
#274718=CARTESIAN_POINT('Origin',(4.76104848420342,-17.542318193471,0.972561099047131));
#274719=CARTESIAN_POINT('Origin',(15.4290484842034,-17.542318193471,0.972561099047131));
#274720=CARTESIAN_POINT('Ctrl Pts',(4.79296103895619,24.6114380135421,-25.7803653622474));
#274721=CARTESIAN_POINT('Ctrl Pts',(4.80658157259404,24.7901923791228,-25.8265943844669));
#274722=CARTESIAN_POINT('Ctrl Pts',(4.8245384335836,24.9694097219037,-25.8708798924498));
#274723=CARTESIAN_POINT('Ctrl Pts',(5.02532215959839,26.5892124826232,-26.2526318315758));
#274724=CARTESIAN_POINT('Ctrl Pts',(5.47477154367343,28.016923034485,-26.4536881584052));
#274725=CARTESIAN_POINT('Ctrl Pts',(6.14788848420341,29.3428715129087,-26.5409110829896));
#274726=CARTESIAN_POINT('Origin',(4.76104848420342,-17.542318193471,0.972561099047131));
#274727=CARTESIAN_POINT('Ctrl Pts',(6.14788848420341,29.7276425156798,-25.8744681569108));
#274728=CARTESIAN_POINT('Ctrl Pts',(6.12358695752485,29.7009800503249,-25.834585427067));
#274729=CARTESIAN_POINT('Ctrl Pts',(6.099576183545,29.674123402766,-25.7946547814283));
#274730=CARTESIAN_POINT('Ctrl Pts',(5.43709796638902,28.9185609385567,-24.6781287468579));
#274731=CARTESIAN_POINT('Ctrl Pts',(5.01156238585602,28.0494448912749,-23.5759589431392));
#274732=CARTESIAN_POINT('Ctrl Pts',(4.82218298524757,26.9437198726235,-22.4043645044611));
#274733=CARTESIAN_POINT('Ctrl Pts',(4.80568122363092,26.8241320615889,-22.2801856190147));
#274734=CARTESIAN_POINT('Ctrl Pts',(4.79296103895619,26.7032738510941,-22.1571994105139));
#274735=CARTESIAN_POINT('Origin',(15.4290484842034,-17.542318193471,0.972561099047131));
#274736=CARTESIAN_POINT('Ctrl Pts',(6.14788848420341,23.112869214926,-35.115773610427));
#274737=CARTESIAN_POINT('Ctrl Pts',(6.12358695752485,23.0950814742058,-35.0712189756663));
#274738=CARTESIAN_POINT('Ctrl Pts',(6.099576183545,23.0771137568824,-35.0265770994354));
#274739=CARTESIAN_POINT('Ctrl Pts',(5.43709796638905,22.5702009610012,-33.7773595681114));
#274740=CARTESIAN_POINT('Ctrl Pts',(5.01156238585603,21.9492311720527,-32.5185754320954));
#274741=CARTESIAN_POINT('Ctrl Pts',(4.82218298524757,21.1112570786857,-31.1426899846619));
#274742=CARTESIAN_POINT('Ctrl Pts',(4.80568122363092,21.0201007902822,-30.9963610018075));
#274743=CARTESIAN_POINT('Ctrl Pts',(4.79296103895619,20.9274538922144,-30.8509345021458));
#274744=CARTESIAN_POINT('Ctrl Pts',(4.79296103895619,18.1280311274457,-33.9600084589958));
#274745=CARTESIAN_POINT('Ctrl Pts',(4.80658157259404,18.2932677270847,-34.042392388553));
#274746=CARTESIAN_POINT('Ctrl Pts',(4.8245384335836,18.4593612660923,-34.1229715326951));
#274747=CARTESIAN_POINT('Ctrl Pts',(5.02532215959839,19.9643967590154,-34.8331572067992));
#274748=CARTESIAN_POINT('Ctrl Pts',(5.47477154367342,21.3191064490006,-35.3266576853357));
#274749=CARTESIAN_POINT('Ctrl Pts',(6.1478884842034,22.597945106139,-35.6876547698332));
#274750=CARTESIAN_POINT('Origin',(4.76104848420342,-17.542318193471,0.972561099047131));
#274751=CARTESIAN_POINT('Origin',(15.4290484842034,-17.542318193471,0.972561099047131));
#274752=CARTESIAN_POINT('Ctrl Pts',(6.14788848420341,14.7212691391918,-42.7798456660962));
#274753=CARTESIAN_POINT('Ctrl Pts',(6.12358695752485,14.7131335327306,-42.7325663777545));
#274754=CARTESIAN_POINT('Ctrl Pts',(6.099576183545,14.7048400211086,-42.6851643351381));
#274755=CARTESIAN_POINT('Ctrl Pts',(5.43709796638902,14.4687314151729,-41.35785210759));
#274756=CARTESIAN_POINT('Ctrl Pts',(5.01156238585603,14.1230472440783,-39.9974685463373));
#274757=CARTESIAN_POINT('Ctrl Pts',(4.82218298524757,13.5894475649218,-38.4774248864324));
#274758=CARTESIAN_POINT('Ctrl Pts',(4.80568122363092,13.5307067663691,-38.3153410848847));
#274759=CARTESIAN_POINT('Ctrl Pts',(4.79296103895619,13.470320294743,-38.1538301299313));
#274760=CARTESIAN_POINT('Ctrl Pts',(4.79296103895619,10.0856588106987,-40.6129306409912));
#274761=CARTESIAN_POINT('Ctrl Pts',(4.80658157259404,10.2301560120985,-40.7278689048426));
#274762=CARTESIAN_POINT('Ctrl Pts',(4.8245384335836,10.375866662673,-40.8412199898834));
#274763=CARTESIAN_POINT('Ctrl Pts',(5.02532215959839,11.7003576147974,-41.8488008771582));
#274764=CARTESIAN_POINT('Ctrl Pts',(5.47477154367342,12.9228591288354,-42.6131771684116));
#274765=CARTESIAN_POINT('Ctrl Pts',(6.14788848420341,14.0986965788227,-43.2321711079735));
#274766=CARTESIAN_POINT('Origin',(4.76104848420342,-17.542318193471,0.972561099047131));
#274767=CARTESIAN_POINT('Origin',(15.4290484842034,-17.542318193471,0.972561099047131));
#274768=CARTESIAN_POINT('Ctrl Pts',(4.79296103895619,29.2525234772276,-16.4314910043563));
#274769=CARTESIAN_POINT('Ctrl Pts',(4.80658157259404,29.4369831852156,-16.4395446891357));
#274770=CARTESIAN_POINT('Ctrl Pts',(4.82453843358361,29.62149167391,-16.4456010717549));
#274771=CARTESIAN_POINT('Ctrl Pts',(5.02532215959839,31.2852685491064,-16.482234884314));
#274772=CARTESIAN_POINT('Ctrl Pts',(5.47477154367342,32.7235821608131,-16.3820599331787));
#274773=CARTESIAN_POINT('Ctrl Pts',(6.1478884842034,34.0386901494082,-16.1916966375036));
#274774=CARTESIAN_POINT('',(4.76104848420342,29.8566594240745,-11.8470366407105));
#274775=CARTESIAN_POINT('Origin',(4.76104848420342,-17.542318193471,0.972561099047131));
#274776=CARTESIAN_POINT('',(4.79296103895619,30.5453491237198,-12.4525827957091));
#274777=CARTESIAN_POINT('Ctrl Pts',(4.79296103895619,30.5453491237198,-12.4525827957091));
#274778=CARTESIAN_POINT('Ctrl Pts',(4.77035892158032,30.2898575046396,-12.2834765820334));
#274779=CARTESIAN_POINT('Ctrl Pts',(4.76104848420342,30.0580786215828,-12.0799600742301));
#274780=CARTESIAN_POINT('Ctrl Pts',(4.76104848420342,29.8566594240745,-11.8470366407104));
#274781=CARTESIAN_POINT('Ctrl Pts',(6.14788848420342,34.2764917070062,-15.4598186985698));
#274782=CARTESIAN_POINT('Ctrl Pts',(6.12358695752485,34.2421197946934,-15.4263509403157));
#274783=CARTESIAN_POINT('Ctrl Pts',(6.099576183545,34.2075479812697,-15.3928766860921));
#274784=CARTESIAN_POINT('Ctrl Pts',(5.43709796638905,33.2363575540093,-14.4578396936725));
#274785=CARTESIAN_POINT('Ctrl Pts',(5.01156238585603,32.157079790142,-13.5604543314709));
#274786=CARTESIAN_POINT('Ctrl Pts',(4.82218298524757,30.8319293353784,-12.6443552004521));
#274787=CARTESIAN_POINT('Ctrl Pts',(4.80568122363092,30.6891365629009,-12.5477536255844));
#274788=CARTESIAN_POINT('Ctrl Pts',(4.79296103895619,30.5453491237198,-12.4525827957091));
#274789=CARTESIAN_POINT('Origin',(15.4290484842034,-17.542318193471,0.972561099047131));
#274790=CARTESIAN_POINT('',(4.79296103895619,31.8484498133401,-6.32197605563879));
#274791=CARTESIAN_POINT('Ctrl Pts',(4.79296103895619,31.8484498133401,-6.32197605563879));
#274792=CARTESIAN_POINT('Ctrl Pts',(4.80658157259404,32.0305530893604,-6.29150241830728));
#274793=CARTESIAN_POINT('Ctrl Pts',(4.8245384335836,32.2122888176425,-6.25906498258073));
#274794=CARTESIAN_POINT('Ctrl Pts',(5.02532215959839,33.8473247741825,-5.94897959517561));
#274795=CARTESIAN_POINT('Ctrl Pts',(5.47477154367343,35.2333802391081,-5.55195149213274));
#274796=CARTESIAN_POINT('Ctrl Pts',(6.14788848420341,36.4801712081848,-5.09232176568362));
#274797=CARTESIAN_POINT('',(4.76104848420342,30.9730026561923,-6.59505465837617));
#274798=CARTESIAN_POINT('Ctrl Pts',(4.76104848420342,30.9730026561923,-6.59505465837617));
#274799=CARTESIAN_POINT('Ctrl Pts',(4.76104848420342,31.085055529905,-6.54244936087672));
#274800=CARTESIAN_POINT('Ctrl Pts',(4.76253129040156,31.200002270829,-6.49602047434924));
#274801=CARTESIAN_POINT('Ctrl Pts',(4.76582494299153,31.3173800954912,-6.45599878354649));
#274802=CARTESIAN_POINT('Ctrl Pts',(4.76903192598598,31.4316692250621,-6.41703022863448));
#274803=CARTESIAN_POINT('Ctrl Pts',(4.77395615055087,31.5482630469874,-6.38413635141219));
#274804=CARTESIAN_POINT('Ctrl Pts',(4.78086799793772,31.666704173383,-6.35755179799359));
#274805=CARTESIAN_POINT('Ctrl Pts',(4.78437682990773,31.7268313705851,-6.34405602389403));
#274806=CARTESIAN_POINT('Ctrl Pts',(4.78839733376329,31.7874341667793,-6.33218657312908));
#274807=CARTESIAN_POINT('Ctrl Pts',(4.79296103895619,31.8484498133401,-6.3219760556388));
#274808=CARTESIAN_POINT('',(4.76104848420342,31.4862222820429,-1.71209609297289));
#274809=CARTESIAN_POINT('Origin',(4.76104848420342,-17.542318193471,0.972561099047131));
#274810=CARTESIAN_POINT('',(4.79296103895619,32.2857625843551,-2.16122297171639));
#274811=CARTESIAN_POINT('Ctrl Pts',(4.79296103895619,32.2857625843551,-2.16122297171639));
#274812=CARTESIAN_POINT('Ctrl Pts',(4.77035892158039,32.0006949113319,-2.0489318290534));
#274813=CARTESIAN_POINT('Ctrl Pts',(4.76104848420342,31.7316674917223,-1.89805218470827));
#274814=CARTESIAN_POINT('Ctrl Pts',(4.76104848420342,31.4862222820429,-1.71209609297289));
#274815=CARTESIAN_POINT('Ctrl Pts',(6.14788848420341,36.560610251444,-4.32699539176698));
#274816=CARTESIAN_POINT('Ctrl Pts',(6.12358695752485,36.5200311096761,-4.30140530673435));
#274817=CARTESIAN_POINT('Ctrl Pts',(6.099576183545,36.4792550845282,-4.27585042946278));
#274818=CARTESIAN_POINT('Ctrl Pts',(5.43709796638903,35.3348823761767,-3.56316808256783));
#274819=CARTESIAN_POINT('Ctrl Pts',(5.01156238585603,34.0926125129541,-2.90978720834442));
#274820=CARTESIAN_POINT('Ctrl Pts',(4.82218298524757,32.6059520557291,-2.28922131294187));
#274821=CARTESIAN_POINT('Ctrl Pts',(4.80568122363092,32.4461950511617,-2.22441900102026));
#274822=CARTESIAN_POINT('Ctrl Pts',(4.79296103895619,32.2857625843551,-2.16122297171639));
#274823=CARTESIAN_POINT('Origin',(15.4290484842034,-17.542318193471,0.972561099047131));
#274824=CARTESIAN_POINT('Ctrl Pts',(6.14788848420341,4.91959547915134,-48.5317275987877));
#274825=CARTESIAN_POINT('Ctrl Pts',(6.12358695752485,4.92146757199067,-48.4837899886367));
#274826=CARTESIAN_POINT('Ctrl Pts',(6.099576183545,4.9232107323245,-48.4356994763575));
#274827=CARTESIAN_POINT('Ctrl Pts',(5.43709796638903,4.96822539538845,-47.08830246608));
#274828=CARTESIAN_POINT('Ctrl Pts',(5.01156238585602,4.91293489920149,-45.6857747690617));
#274829=CARTESIAN_POINT('Ctrl Pts',(4.82218298524757,4.70703050072981,-44.0880060986017));
#274830=CARTESIAN_POINT('Ctrl Pts',(4.80568122363092,4.68327244679418,-43.917251318253));
#274831=CARTESIAN_POINT('Ctrl Pts',(4.79296103895619,4.65778558018633,-43.7467147117548));
#274832=CARTESIAN_POINT('Ctrl Pts',(4.79296103895618,0.835811325126994,
-45.448367284618));
#274833=CARTESIAN_POINT('Ctrl Pts',(4.80658157259404,0.953253907211932,
-45.5908365290982));
#274834=CARTESIAN_POINT('Ctrl Pts',(4.8245384335836,1.07221341472582,-45.7320055687025));
#274835=CARTESIAN_POINT('Ctrl Pts',(5.02532215959839,2.158273215831,-46.9929455494646));
#274836=CARTESIAN_POINT('Ctrl Pts',(5.47477154367344,3.19513737154524,-47.9947907416229));
#274837=CARTESIAN_POINT('Ctrl Pts',(6.14788848420341,4.21658387552305,-48.8447285308278));
#274838=CARTESIAN_POINT('Origin',(4.76104848420342,-17.542318193471,0.972561099047131));
#274839=CARTESIAN_POINT('Origin',(15.4290484842034,-17.542318193471,0.972561099047131));
#274840=CARTESIAN_POINT('Ctrl Pts',(6.1478884842034,-5.863771592603,-52.1200345674512));
#274841=CARTESIAN_POINT('Ctrl Pts',(6.12358695752484,-5.85197361990358,
-52.0735337390846));
#274842=CARTESIAN_POINT('Ctrl Pts',(6.099576183545,-5.84026997208509,-52.026856543293));
#274843=CARTESIAN_POINT('Ctrl Pts',(5.43709796638902,-5.51609939680166,
-50.7182624651634));
#274844=CARTESIAN_POINT('Ctrl Pts',(5.01156238585602,-5.2785797580845,-49.3348878228138));
#274845=CARTESIAN_POINT('Ctrl Pts',(4.82218298524757,-5.14778986561914,
-47.7292242996427));
#274846=CARTESIAN_POINT('Ctrl Pts',(4.80568122363092,-5.13552683397687,
-47.5572613437665));
#274847=CARTESIAN_POINT('Ctrl Pts',(4.79296103895619,-5.12500019719618,
-47.3851523537529));
#274848=CARTESIAN_POINT('Ctrl Pts',(4.79296103895618,-9.21724860845719,
-48.2549866055502));
#274849=CARTESIAN_POINT('Ctrl Pts',(4.80658157259404,-9.13199345007622,
-48.4187602410321));
#274850=CARTESIAN_POINT('Ctrl Pts',(4.8245384335836,-9.04498418693225,-48.5815774707651));
#274851=CARTESIAN_POINT('Ctrl Pts',(5.02532215959839,-8.24482156164778,
-50.0407674171938));
#274852=CARTESIAN_POINT('Ctrl Pts',(5.47477154367339,-7.43891070328836,
-51.236296067973));
#274853=CARTESIAN_POINT('Ctrl Pts',(6.14788848420341,-6.61649725898798,
-52.2800313469787));
#274854=CARTESIAN_POINT('Origin',(4.76104848420342,-17.542318193471,0.972561099047131));
#274855=CARTESIAN_POINT('Origin',(0.884028484203416,-17.542318193471,0.972561099047131));
#274856=CARTESIAN_POINT('',(11.5201159294509,31.84844981334,8.2670982537337));
#274857=CARTESIAN_POINT('Ctrl Pts',(11.5520284842034,30.9730026561921,8.54017685647109));
#274858=CARTESIAN_POINT('Ctrl Pts',(11.5520284842034,31.085055529906,8.4875715589711));
#274859=CARTESIAN_POINT('Ctrl Pts',(11.5505456780052,31.2000022708313,8.44114267244317));
#274860=CARTESIAN_POINT('Ctrl Pts',(11.5472520254152,31.3173800954948,8.40112098164014));
#274861=CARTESIAN_POINT('Ctrl Pts',(11.5440450424208,31.4316692250642,8.36215242672879));
#274862=CARTESIAN_POINT('Ctrl Pts',(11.5391208178559,31.5482630469879,8.329258549507));
#274863=CARTESIAN_POINT('Ctrl Pts',(11.5322089704692,31.6667041733819,8.30267399608871));
#274864=CARTESIAN_POINT('Ctrl Pts',(11.5287001384991,31.7268313705843,8.28917822198906));
#274865=CARTESIAN_POINT('Ctrl Pts',(11.5246796346436,31.7874341667788,8.27730877122404));
#274866=CARTESIAN_POINT('Ctrl Pts',(11.5201159294506,31.84844981334,8.2670982537337));
#274867=CARTESIAN_POINT('',(11.520115929451,32.2857625843551,4.10634516981065));
#274868=CARTESIAN_POINT('Ctrl Pts',(11.5201159294506,32.285762584355,4.10634516981064));
#274869=CARTESIAN_POINT('Ctrl Pts',(11.5379482942249,32.0608530926385,4.01775096495828));
#274870=CARTESIAN_POINT('Ctrl Pts',(11.5475950755165,31.8451991447526,3.90484982591719));
#274871=CARTESIAN_POINT('Ctrl Pts',(11.5516325551658,31.5894123057798,3.73310893941423));
#274872=CARTESIAN_POINT('Ctrl Pts',(11.5520284842034,31.5372399615042,3.69587069864284));
#274873=CARTESIAN_POINT('Ctrl Pts',(11.5520284842034,31.4862222820429,3.65721829106713));
#274874=CARTESIAN_POINT('',(10.1651884842034,36.560610251444,6.27211758986124));
#274875=CARTESIAN_POINT('Ctrl Pts',(10.1651884842034,36.560610251444,6.27211758986124));
#274876=CARTESIAN_POINT('Ctrl Pts',(10.189490010882,36.5200311096761,6.2465275048286));
#274877=CARTESIAN_POINT('Ctrl Pts',(10.2135007848618,36.4792550845282,6.22097262755701));
#274878=CARTESIAN_POINT('Ctrl Pts',(10.8759790020178,35.3348823761766,5.50829028066204));
#274879=CARTESIAN_POINT('Ctrl Pts',(11.3015145825508,34.092612512954,4.85490940643868));
#274880=CARTESIAN_POINT('Ctrl Pts',(11.4908939831593,32.605952055729,4.23434351103614));
#274881=CARTESIAN_POINT('Ctrl Pts',(11.5073957447759,32.4461950511616,4.16954119911451));
#274882=CARTESIAN_POINT('Ctrl Pts',(11.5201159294506,32.285762584355,4.10634516981064));
#274883=CARTESIAN_POINT('',(10.1651884842034,36.4801712081847,7.03744396377858));
#274884=CARTESIAN_POINT('Origin',(10.1651884842034,-17.542318193471,0.972561099047131));
#274885=CARTESIAN_POINT('Ctrl Pts',(11.5201159294506,31.84844981334,8.2670982537337));
#274886=CARTESIAN_POINT('Ctrl Pts',(11.5064953958128,32.0305530893603,8.2366246164022));
#274887=CARTESIAN_POINT('Ctrl Pts',(11.4885385348232,32.2122888176424,8.20418718067565));
#274888=CARTESIAN_POINT('Ctrl Pts',(11.2877548088084,33.8473247741825,7.89410179327056));
#274889=CARTESIAN_POINT('Ctrl Pts',(10.8383054247334,35.233380239108,7.49707369022769));
#274890=CARTESIAN_POINT('Ctrl Pts',(10.1651884842034,36.4801712081847,7.03744396377858));
#274891=CARTESIAN_POINT('Origin',(0.561048484203417,-17.542318193471,0.972561099047131));
#274892=CARTESIAN_POINT('',(6.14788848420341,36.4801712081847,7.03744396377859));
#274893=CARTESIAN_POINT('',(8.15653848420342,36.4801712081847,7.03744396377858));
#274894=CARTESIAN_POINT('',(6.14788848420341,36.560610251444,6.27211758986124));
#274895=CARTESIAN_POINT('',(8.15653848420341,36.560610251444,6.27211758986124));
#274896=CARTESIAN_POINT('Origin',(6.14788848420341,-17.542318193471,0.972561099047131));
#274897=CARTESIAN_POINT('Origin',(15.4290484842034,-17.542318193471,0.972561099047131));
#274898=CARTESIAN_POINT('',(4.79296103895619,31.84844981334,8.2670982537337));
#274899=CARTESIAN_POINT('',(4.76104848420342,30.9730026561922,8.54017685647106));
#274900=CARTESIAN_POINT('Ctrl Pts',(4.79296103895619,31.84844981334,8.2670982537337));
#274901=CARTESIAN_POINT('Ctrl Pts',(4.77035892158034,31.5462649115901,8.31766666361755));
#274902=CARTESIAN_POINT('Ctrl Pts',(4.76104848420342,31.2517467446016,8.40931528004612));
#274903=CARTESIAN_POINT('Ctrl Pts',(4.76104848420342,30.9730026561922,8.54017685647107));
#274904=CARTESIAN_POINT('Ctrl Pts',(6.14788848420341,36.4801712081847,7.03744396377859));
#274905=CARTESIAN_POINT('Ctrl Pts',(6.12358695752485,36.4351583401774,7.05403796607894));
#274906=CARTESIAN_POINT('Ctrl Pts',(6.099576183545,36.3899602112693,7.07055659563583));
#274907=CARTESIAN_POINT('Ctrl Pts',(5.43709796638902,35.1224198004911,7.52973665861739));
#274908=CARTESIAN_POINT('Ctrl Pts',(5.01156238585602,33.7714509920082,7.91055716538982));
#274909=CARTESIAN_POINT('Ctrl Pts',(4.82218298524757,32.1882547280908,8.20846811774149));
#274910=CARTESIAN_POINT('Ctrl Pts',(4.80568122363092,32.0185156391322,8.23863899473005));
#274911=CARTESIAN_POINT('Ctrl Pts',(4.79296103895619,31.84844981334,8.2670982537337));
#274912=CARTESIAN_POINT('',(4.79296103895619,32.2857625843551,4.10634516981065));
#274913=CARTESIAN_POINT('Ctrl Pts',(4.79296103895619,32.2857625843551,4.10634516981065));
#274914=CARTESIAN_POINT('Ctrl Pts',(4.80658157259404,32.4575506414171,4.17401428507293));
#274915=CARTESIAN_POINT('Ctrl Pts',(4.8245384335836,32.6285708858962,4.24352786755193));
#274916=CARTESIAN_POINT('Ctrl Pts',(5.02532215959839,34.163407006706,4.88678023553691));
#274917=CARTESIAN_POINT('Ctrl Pts',(5.47477154367344,35.4366270500011,5.56330945723206));
#274918=CARTESIAN_POINT('Ctrl Pts',(6.14788848420341,36.560610251444,6.27211758986124));
#274919=CARTESIAN_POINT('',(4.76104848420342,31.4862222820429,3.65721829106715));
#274920=CARTESIAN_POINT('Ctrl Pts',(4.76104848420342,31.4862222820429,3.65721829106714));
#274921=CARTESIAN_POINT('Ctrl Pts',(4.76104848420342,31.5848954455554,3.73197581381493));
#274922=CARTESIAN_POINT('Ctrl Pts',(4.76253147480131,31.6876836794715,3.80129276825595));
#274923=CARTESIAN_POINT('Ctrl Pts',(4.7658255451976,31.7941823732019,3.86484722694874));
#274924=CARTESIAN_POINT('Ctrl Pts',(4.76903295628176,31.8978793345982,3.9267297160083));
#274925=CARTESIAN_POINT('Ctrl Pts',(4.7739578530675,32.0050940194892,3.98314864997226));
#274926=CARTESIAN_POINT('Ctrl Pts',(4.78087067578756,32.1154278760504,4.03377943482262));
#274927=CARTESIAN_POINT('Ctrl Pts',(4.78437887355451,32.1714213543851,4.05947412041549));
#274928=CARTESIAN_POINT('Ctrl Pts',(4.78839849197318,32.2282177698636,4.08367766456516));
#274929=CARTESIAN_POINT('Ctrl Pts',(4.79296103895619,32.2857625843551,4.10634516981065));
#274930=CARTESIAN_POINT('Origin',(4.76104848420342,-17.542318193471,0.972561099047131));
#274931=CARTESIAN_POINT('Origin',(4.76104848420342,-17.542318193471,0.972561099047131));
#274932=CARTESIAN_POINT('Origin',(4.76104848420342,-22.8798040147369,51.7553464718149));
#274933=CARTESIAN_POINT('Origin',(4.76104848420342,-12.2048323722054,51.7553464718149));
#274934=CARTESIAN_POINT('Origin',(4.76104848420342,-1.76313447216181,49.5358950681846));
#274935=CARTESIAN_POINT('Origin',(4.76104848420342,7.98893738233642,45.193992937372));
#274936=CARTESIAN_POINT('Origin',(4.76104848420342,16.6251708556151,38.9194020372516));
#274937=CARTESIAN_POINT('Origin',(4.76104848420342,23.7681211036458,30.9863520989864));
#274938=CARTESIAN_POINT('Origin',(4.76104848420342,29.1056069249115,21.7415554718757));
#274939=CARTESIAN_POINT('Origin',(4.76104848420342,32.4043545769244,11.5890541299801));
#274940=CARTESIAN_POINT('Origin',(4.76104848420342,33.520192958144,0.972561099047131));
#274941=CARTESIAN_POINT('Origin',(4.76104848420342,32.4043545769246,-9.6439319318852));
#274942=CARTESIAN_POINT('Origin',(4.76104848420342,-67.4889909638663,-9.6439319318862));
#274943=CARTESIAN_POINT('Origin',(4.76104848420342,-68.604829345086,0.972561099046774));
#274944=CARTESIAN_POINT('Origin',(4.76104848420342,-67.4889909638665,11.5890541299798));
#274945=CARTESIAN_POINT('Origin',(4.76104848420342,-64.1902433118537,21.7415554718754));
#274946=CARTESIAN_POINT('Origin',(4.76104848420342,-58.852757490588,30.9863520989862));
#274947=CARTESIAN_POINT('Origin',(4.76104848420342,-51.7098072425573,38.9194020372514));
#274948=CARTESIAN_POINT('Origin',(4.76104848420342,-43.0735737692787,45.1939929373718));
#274949=CARTESIAN_POINT('Origin',(4.76104848420342,-33.3215019147805,49.5358950681845));
#274950=CARTESIAN_POINT('Origin',(11.5520284842034,22.8992029103953,27.9355151336363));
#274951=CARTESIAN_POINT('',(11.5520284842034,32.2857625843551,4.10634516981065));
#274952=CARTESIAN_POINT('Origin',(11.5520284842034,22.8992029103953,-25.990392935542));
#274953=CARTESIAN_POINT('',(11.5520284842034,32.2857625843551,-2.16122297171639));
#274954=CARTESIAN_POINT('Origin',(11.5520284842034,33.520192958144,0.972561099047131));
#274955=CARTESIAN_POINT('Origin',(11.5520284842034,16.4095452815284,35.7545749286233));
#274956=CARTESIAN_POINT('',(11.5520284842034,30.5453491237196,14.397704993804));
#274957=CARTESIAN_POINT('Origin',(11.5520284842034,27.6213720070744,-16.9929226666352));
#274958=CARTESIAN_POINT('',(11.5520284842034,31.84844981334,8.2670982537337));
#274959=CARTESIAN_POINT('Origin',(11.5520284842034,32.4043545769244,11.5890541299801));
#274960=CARTESIAN_POINT('Origin',(11.5520284842034,13.5002200109301,-36.4290209703537));
#274961=CARTESIAN_POINT('Origin',(11.5520284842034,-40.1302762914843,-42.0658132711382));
#274962=CARTESIAN_POINT('Origin',(11.5520284842034,20.5980922391598,-29.1576000604339));
#274963=CARTESIAN_POINT('Origin',(11.5520284842034,-30.6884940271654,-45.8216220909116));
#274964=CARTESIAN_POINT('Origin',(11.5520284842034,26.0290455134887,-20.5693465272905));
#274965=CARTESIAN_POINT('Origin',(11.5520284842034,-20.6721607965636,-47.5323005618802));
#274966=CARTESIAN_POINT('Origin',(11.5520284842034,27.6213720070741,18.93804486473));
#274967=CARTESIAN_POINT('',(11.5520284842034,31.8484498133401,-6.32197605563879));
#274968=CARTESIAN_POINT('Origin',(11.5520284842034,16.4095452815289,-33.8094527305286));
#274969=CARTESIAN_POINT('',(11.5520284842034,30.5453491237198,-12.4525827957091));
#274970=CARTESIAN_POINT('Origin',(11.5520284842034,32.4043545769246,-9.6439319318852));
#274971=CARTESIAN_POINT('Origin',(11.5520284842034,30.3696711225592,9.15539674730717));
#274972=CARTESIAN_POINT('Origin',(11.5520284842034,8.43602829968808,-40.1083716185434));
#274973=CARTESIAN_POINT('Origin',(11.5520284842034,29.5557211152235,-11.0396082613347));
#274974=CARTESIAN_POINT('Origin',(11.5520284842034,-10.5190384255555,-47.1230838261165));
#274975=CARTESIAN_POINT('Origin',(11.5520284842034,31.0239863977013,-0.984880553546538));
#274976=CARTESIAN_POINT('Origin',(11.5520284842034,-0.672867081840852,-44.6118566186133));
#274977=CARTESIAN_POINT('Origin',(11.5520284842034,-51.4941816684702,-33.8094527305293));
#274978=CARTESIAN_POINT('',(11.5520284842034,-65.6299855106615,-12.4525827957101));
#274979=CARTESIAN_POINT('Origin',(11.5520284842034,-62.7060083940165,18.9380448647291));
#274980=CARTESIAN_POINT('',(11.5520284842034,-66.9330862002819,-6.32197605563978));
#274981=CARTESIAN_POINT('Origin',(11.5520284842034,-67.4889909638663,-9.6439319318862));
#274982=CARTESIAN_POINT('Origin',(11.5520284842034,-34.4117693051002,-44.6118566186136));
#274983=CARTESIAN_POINT('Origin',(11.5520284842034,-66.1086227846432,-0.984880553547528));
#274984=CARTESIAN_POINT('Origin',(11.5520284842034,-43.5206646866292,-40.1083716185439));
#274985=CARTESIAN_POINT('Origin',(11.5520284842034,-65.4543075095014,9.15539674730621));
#274986=CARTESIAN_POINT('Origin',(11.5520284842034,-14.4124755903774,-47.5323005618801));
#274987=CARTESIAN_POINT('Origin',(11.5520284842034,-61.1136819004303,-20.5693465272914));
#274988=CARTESIAN_POINT('Origin',(11.5520284842034,-24.5655979613854,-47.1230838261167));
#274989=CARTESIAN_POINT('Origin',(11.5520284842034,-64.6403575021652,-11.0396082613357));
#274990=CARTESIAN_POINT('Origin',(11.5520284842034,-4.39614235977561,-45.8216220909114));
#274991=CARTESIAN_POINT('Origin',(11.5520284842034,-55.6827286261012,-29.1576000604346));
#274992=CARTESIAN_POINT('Origin',(11.5520284842034,5.04563990454314,-42.0658132711378));
#274993=CARTESIAN_POINT('Origin',(11.5520284842034,-48.5848563978714,-36.4290209703543));
#274994=CARTESIAN_POINT('Origin',(11.5520284842034,-55.6827286261016,31.1027222585284));
#274995=CARTESIAN_POINT('',(11.5520284842034,-35.9204477120687,47.3934894827124));
#274996=CARTESIAN_POINT('Origin',(11.5520284842034,-4.39614235977625,47.7667442890058));
#274997=CARTESIAN_POINT('',(11.5520284842034,-29.9596361897455,49.3302745518473));
#274998=CARTESIAN_POINT('Origin',(11.5520284842034,-33.3215019147805,49.5358950681845));
#274999=CARTESIAN_POINT('Origin',(11.5520284842034,-64.6403575021654,12.9847304594293));
#275000=CARTESIAN_POINT('',(11.5520284842034,-53.2126675143875,35.9051306570903));
#275001=CARTESIAN_POINT('Origin',(11.5520284842034,-24.5655979613861,49.0682060242108));
#275002=CARTESIAN_POINT('',(11.5520284842034,-48.5549566816847,40.0989523280257));
#275003=CARTESIAN_POINT('Origin',(11.5520284842034,-51.7098072425573,38.9194020372514));
#275004=CARTESIAN_POINT('Origin',(11.5520284842034,-61.1136819004306,22.5144687253851));
#275005=CARTESIAN_POINT('',(11.5520284842034,-45.1702951976404,42.5580528390857));
#275006=CARTESIAN_POINT('Origin',(11.5520284842034,-14.412475590378,49.4774227599744));
#275007=CARTESIAN_POINT('',(11.5520284842034,-39.742421967128,45.6918369098492));
#275008=CARTESIAN_POINT('Origin',(11.5520284842034,-43.0735737692787,45.1939929373718));
#275009=CARTESIAN_POINT('Origin',(11.5520284842034,-43.5206646866298,42.0534938166378));
#275010=CARTESIAN_POINT('',(11.5520284842034,-61.7879102380359,24.1023216086084));
#275011=CARTESIAN_POINT('Origin',(11.5520284842034,-64.1902433118537,21.7415554718754));
#275012=CARTESIAN_POINT('Origin',(11.5520284842034,-66.1086227846432,2.93000275164114));
#275013=CARTESIAN_POINT('',(11.5520284842034,-59.6960744004839,27.7254875603419));
#275014=CARTESIAN_POINT('Origin',(11.5520284842034,-34.4117693051008,46.5569788167076));
#275015=CARTESIAN_POINT('',(11.5520284842034,-56.0120902791562,32.7960567002403));
#275016=CARTESIAN_POINT('Origin',(11.5520284842034,-58.852757490588,30.9863520989862));
#275017=CARTESIAN_POINT('Origin',(11.5520284842034,-62.7060083940162,-16.9929226666355));
#275018=CARTESIAN_POINT('',(11.5520284842034,-66.933086200282,8.26709825373337));
#275019=CARTESIAN_POINT('Origin',(11.5520284842034,-51.4941816684706,35.7545749286231));
#275020=CARTESIAN_POINT('',(11.5520284842034,-65.6299855106617,14.3977049938037));
#275021=CARTESIAN_POINT('Origin',(11.5520284842034,-67.4889909638665,11.5890541299798));
#275022=CARTESIAN_POINT('Origin',(11.5520284842034,-57.9838392973371,-25.9903929355423));
#275023=CARTESIAN_POINT('',(11.5520284842034,-67.370398971297,-2.16122297171674));
#275024=CARTESIAN_POINT('Origin',(11.5520284842034,-57.9838392973375,27.935515133636));
#275025=CARTESIAN_POINT('',(11.5520284842034,-67.370398971297,4.1063451698103));
#275026=CARTESIAN_POINT('Origin',(11.5520284842034,-68.604829345086,0.972561099046774));
#275027=CARTESIAN_POINT('Origin',(11.5520284842034,-0.672867081841461,46.5569788167077));
#275028=CARTESIAN_POINT('',(11.5520284842034,20.927453892214,32.7960567002406));
#275029=CARTESIAN_POINT('Origin',(11.5520284842034,31.0239863977013,2.93000275164145));
#275030=CARTESIAN_POINT('',(11.5520284842034,24.6114380135418,27.7254875603422));
#275031=CARTESIAN_POINT('Origin',(11.5520284842034,23.7681211036458,30.9863520989864));
#275032=CARTESIAN_POINT('Origin',(11.5520284842034,-10.5190384255562,49.0682060242109));
#275033=CARTESIAN_POINT('',(11.5520284842034,13.4703202947425,40.098952328026));
#275034=CARTESIAN_POINT('Origin',(11.5520284842034,29.5557211152234,12.9847304594296));
#275035=CARTESIAN_POINT('',(11.5520284842034,18.1280311274453,35.9051306570905));
#275036=CARTESIAN_POINT('Origin',(11.5520284842034,16.6251708556151,38.9194020372516));
#275037=CARTESIAN_POINT('Origin',(11.5520284842034,8.43602829968752,42.053493816638));
#275038=CARTESIAN_POINT('',(11.5520284842034,26.7032738510938,24.1023216086087));
#275039=CARTESIAN_POINT('Origin',(11.5520284842034,29.1056069249115,21.7415554718757));
#275040=CARTESIAN_POINT('Origin',(11.5520284842034,-20.6721607965643,49.4774227599744));
#275041=CARTESIAN_POINT('',(11.5520284842034,4.65778558018571,45.6918369098494));
#275042=CARTESIAN_POINT('Origin',(11.5520284842034,26.0290455134884,22.5144687253854));
#275043=CARTESIAN_POINT('',(11.5520284842034,10.0856588106982,42.5580528390859));
#275044=CARTESIAN_POINT('Origin',(11.5520284842034,7.98893738233642,45.193992937372));
#275045=CARTESIAN_POINT('Origin',(11.5520284842034,-30.688494027166,47.7667442890057));
#275046=CARTESIAN_POINT('',(11.5520284842034,-5.12500019719682,49.3302745518473));
#275047=CARTESIAN_POINT('Origin',(11.5520284842034,20.5980922391594,31.1027222585287));
#275048=CARTESIAN_POINT('',(11.5520284842034,0.835811325126388,47.3934894827125));
#275049=CARTESIAN_POINT('Origin',(11.5520284842034,-1.76313447216181,49.5358950681846));
#275050=CARTESIAN_POINT('Origin',(11.5520284842034,-40.1302762914848,44.0109354692322));
#275051=CARTESIAN_POINT('',(11.5520284842034,-15.4504823559191,50.8552480699037));
#275052=CARTESIAN_POINT('Origin',(11.5520284842034,13.5002200109296,38.3741431684484));
#275053=CARTESIAN_POINT('',(11.5520284842034,-9.21724860845784,50.2001088036446));
#275054=CARTESIAN_POINT('Origin',(11.5520284842034,-12.2048323722054,51.7553464718149));
#275055=CARTESIAN_POINT('Origin',(11.5520284842034,-48.5848563978719,38.3741431684482));
#275056=CARTESIAN_POINT('',(11.5520284842034,-25.8673877784845,50.2001088036445));
#275057=CARTESIAN_POINT('Origin',(11.5520284842034,5.04563990454256,44.0109354692323));
#275058=CARTESIAN_POINT('',(11.5520284842034,-19.6341540310232,50.8552480699037));
#275059=CARTESIAN_POINT('Origin',(11.5520284842034,-22.8798040147369,51.7553464718149));
#275060=CARTESIAN_POINT('Origin',(19.4612584842034,-7.33631819347099,3.49256109904713));
#275061=CARTESIAN_POINT('',(19.4612584842034,-7.33631819347099,3.49256109904713));
#275062=CARTESIAN_POINT('',(19.4612584842034,-7.33631819347099,-1.54743890095287));
#275063=CARTESIAN_POINT('Origin',(19.4612584842034,-7.33631819347099,-1.54743890095287));
#275064=CARTESIAN_POINT('Origin',(19.4612584842034,-17.542318193471,3.49256109904713));
#275065=CARTESIAN_POINT('',(0.,0.,0.));
#275066=CARTESIAN_POINT('Origin',(12.6996622584713,0.0926203042559918,2.));
#275067=CARTESIAN_POINT('',(16.6496622584713,0.0926203042559914,2.));
#275068=CARTESIAN_POINT('Origin',(12.6996622584713,0.0926203042559918,2.));
#275069=CARTESIAN_POINT('',(16.6496622584713,0.0926203042559914,-2.));
#275070=CARTESIAN_POINT('',(16.6496622584713,0.0926203042559914,2.));
#275071=CARTESIAN_POINT('Origin',(12.6996622584713,0.0926203042559918,-2.));
#275072=CARTESIAN_POINT('Origin',(-12.7003377415287,0.0926203042559918,
2.));
#275073=CARTESIAN_POINT('',(-4.95988141030959,7.18736031249375,2.));
#275074=CARTESIAN_POINT('',(-4.9598814103096,-7.00211970398177,2.));
#275075=CARTESIAN_POINT('Origin',(-12.7003377415287,0.0926203042559918,
2.));
#275076=CARTESIAN_POINT('',(-4.95988141030959,7.18736031249375,-2.));
#275077=CARTESIAN_POINT('',(-4.95988141030959,7.18736031249375,2.));
#275078=CARTESIAN_POINT('',(-4.9598814103096,-7.00211970398177,-2.));
#275079=CARTESIAN_POINT('Origin',(-12.7003377415287,0.0926203042559918,
-2.));
#275080=CARTESIAN_POINT('',(-4.9598814103096,-7.00211970398177,2.));
#275081=CARTESIAN_POINT('Origin',(-12.7003377415287,0.0926203042559918,
2.));
#275082=CARTESIAN_POINT('',(-8.75033774152873,0.0926203042559914,2.));
#275083=CARTESIAN_POINT('Origin',(-12.7003377415287,0.0926203042559918,
2.));
#275084=CARTESIAN_POINT('',(-8.75033774152873,0.0926203042559914,-2.));
#275085=CARTESIAN_POINT('',(-8.75033774152873,0.0926203042559914,2.));
#275086=CARTESIAN_POINT('Origin',(-12.7003377415287,0.0926203042559918,
-2.));
#275087=CARTESIAN_POINT('Origin',(-0.10965027657137,-16.314759391488,2.));
#275088=CARTESIAN_POINT('',(5.20000000000002,-7.25619361425234,-2.));
#275089=CARTESIAN_POINT('Origin',(-0.10965027657137,-16.314759391488,-2.));
#275090=CARTESIAN_POINT('',(5.20000000000002,-7.25619361425234,2.));
#275091=CARTESIAN_POINT('',(5.20000000000002,-7.25619361425234,2.));
#275092=CARTESIAN_POINT('Origin',(-0.10965027657137,-16.314759391488,2.));
#275093=CARTESIAN_POINT('Origin',(12.6996622584713,0.0926203042559918,2.));
#275094=CARTESIAN_POINT('',(5.20000000000002,7.44143422276433,-2.));
#275095=CARTESIAN_POINT('Origin',(12.6996622584713,0.0926203042559918,-2.));
#275096=CARTESIAN_POINT('',(5.20000000000002,7.44143422276433,2.));
#275097=CARTESIAN_POINT('',(5.20000000000002,7.44143422276433,2.));
#275098=CARTESIAN_POINT('Origin',(12.6996622584713,0.0926203042559918,2.));
#275099=CARTESIAN_POINT('Origin',(-0.10965027657137,16.5,2.));
#275100=CARTESIAN_POINT('Origin',(-0.10965027657137,16.5,-2.));
#275101=CARTESIAN_POINT('Origin',(-0.10965027657137,16.5,2.));
#275102=CARTESIAN_POINT('Origin',(0.,0.,2.));
#275103=CARTESIAN_POINT('Origin',(0.,0.,-2.));
#275104=CARTESIAN_POINT('Origin',(-12.7003377415287,0.0926203042559918,
29.8));
#275105=CARTESIAN_POINT('',(-8.75033774152873,0.0926203042559914,29.8));
#275106=CARTESIAN_POINT('Origin',(-12.7003377415287,0.0926203042559918,
29.8));
#275107=CARTESIAN_POINT('',(-8.75033774152873,0.0926203042559914,25.8));
#275108=CARTESIAN_POINT('',(-8.75033774152873,0.0926203042559914,29.8));
#275109=CARTESIAN_POINT('Origin',(-12.7003377415287,0.0926203042559918,
25.8));
#275110=CARTESIAN_POINT('Origin',(12.6996622584713,0.0926203042559918,29.8));
#275111=CARTESIAN_POINT('',(16.6496622584713,0.0926203042559914,29.8));
#275112=CARTESIAN_POINT('Origin',(12.6996622584713,0.0926203042559918,29.8));
#275113=CARTESIAN_POINT('',(16.6496622584713,0.0926203042559914,25.8));
#275114=CARTESIAN_POINT('',(16.6496622584713,0.0926203042559914,29.8));
#275115=CARTESIAN_POINT('Origin',(12.6996622584713,0.0926203042559918,25.8));
#275116=CARTESIAN_POINT('Origin',(-12.7003377415287,0.0926203042559918,
29.8));
#275117=CARTESIAN_POINT('',(-4.9598814103096,7.18736031249375,29.8));
#275118=CARTESIAN_POINT('',(-4.9598814103096,-7.00211970398178,29.8));
#275119=CARTESIAN_POINT('Origin',(-12.7003377415287,0.0926203042559918,
29.8));
#275120=CARTESIAN_POINT('',(-4.9598814103096,7.18736031249375,25.8));
#275121=CARTESIAN_POINT('',(-4.9598814103096,7.18736031249375,29.8));
#275122=CARTESIAN_POINT('',(-4.9598814103096,-7.00211970398178,25.8));
#275123=CARTESIAN_POINT('Origin',(-12.7003377415287,0.0926203042559918,
25.8));
#275124=CARTESIAN_POINT('',(-4.9598814103096,-7.00211970398178,29.8));
#275125=CARTESIAN_POINT('Origin',(-6.40499400905005,-8.11106954361601,29.8));
#275126=CARTESIAN_POINT('',(5.20000000000001,-7.25619361425234,29.8));
#275127=CARTESIAN_POINT('Origin',(-0.10965027657137,-16.314759391488,29.8));
#275128=CARTESIAN_POINT('',(5.20000000000002,7.44143422276433,29.8));
#275129=CARTESIAN_POINT('Origin',(12.6996622584713,0.0926203042559918,29.8));
#275130=CARTESIAN_POINT('Origin',(-0.10965027657137,16.5,29.8));
#275131=CARTESIAN_POINT('Origin',(-6.40499400905005,-8.11106954361601,25.8));
#275132=CARTESIAN_POINT('',(5.20000000000001,-7.25619361425234,25.8));
#275133=CARTESIAN_POINT('Origin',(-0.10965027657137,-16.314759391488,25.8));
#275134=CARTESIAN_POINT('',(5.20000000000002,7.44143422276433,25.8));
#275135=CARTESIAN_POINT('Origin',(-0.10965027657137,16.5,25.8));
#275136=CARTESIAN_POINT('Origin',(12.6996622584713,0.0926203042559918,25.8));
#275137=CARTESIAN_POINT('Origin',(-0.10965027657137,-16.314759391488,29.8));
#275138=CARTESIAN_POINT('',(5.20000000000001,-7.25619361425234,29.8));
#275139=CARTESIAN_POINT('Origin',(12.6996622584713,0.0926203042559918,29.8));
#275140=CARTESIAN_POINT('',(5.20000000000002,7.44143422276433,29.8));
#275141=CARTESIAN_POINT('Origin',(-0.10965027657137,16.5,29.8));
#275142=CARTESIAN_POINT('Origin',(-12.7003377415287,0.0926203042559918,
32.4));
#275143=CARTESIAN_POINT('',(-8.75033774152873,0.0926203042559914,-4.59999999999999));
#275144=CARTESIAN_POINT('Origin',(-12.7003377415287,0.0926203042559918,
-4.6));
#275145=CARTESIAN_POINT('',(-8.75033774152873,0.0926203042559914,32.4));
#275146=CARTESIAN_POINT('',(-8.75033774152873,0.0926203042559914,32.4));
#275147=CARTESIAN_POINT('Origin',(-12.7003377415287,0.0926203042559918,
32.4));
#275148=CARTESIAN_POINT('Origin',(-12.7003377415287,0.0926203042559918,
32.4));
#275149=CARTESIAN_POINT('Origin',(-12.7003377415287,0.0926203042559918,
-4.6));
#275150=CARTESIAN_POINT('Origin',(12.6996622584713,0.0926203042559918,32.4));
#275151=CARTESIAN_POINT('',(16.6496622584713,0.0926203042559914,-4.59999999999999));
#275152=CARTESIAN_POINT('Origin',(12.6996622584713,0.0926203042559918,-4.6));
#275153=CARTESIAN_POINT('',(16.6496622584713,0.0926203042559914,32.4));
#275154=CARTESIAN_POINT('',(16.6496622584713,0.0926203042559914,32.4));
#275155=CARTESIAN_POINT('Origin',(12.6996622584713,0.0926203042559918,32.4));
#275156=CARTESIAN_POINT('Origin',(12.6996622584713,0.0926203042559918,32.4));
#275157=CARTESIAN_POINT('Origin',(12.6996622584713,0.0926203042559918,-4.6));
#275158=CARTESIAN_POINT('',(-23.6277142247157,61.9505921401413,785.173663670255));
#275159=CARTESIAN_POINT('',(-44.638378428336,59.198579754616,-736.731776872445));
#275160=CARTESIAN_POINT('',(-41.4045999999974,111.913829306091,768.015546649378));
#275161=CARTESIAN_POINT('',(-41.4045999999974,111.913829306091,743.015546649378));
#275162=CARTESIAN_POINT('',(-41.4045999999974,111.913829306091,718.015546649378));
#275163=CARTESIAN_POINT('',(-41.4045999999974,111.913829306091,693.015546649378));
#275164=CARTESIAN_POINT('',(-41.4045999999974,111.913829306091,668.015546649378));
#275165=CARTESIAN_POINT('',(-41.4045999999974,111.913829306091,643.015546649378));
#275166=CARTESIAN_POINT('',(-41.4045999999974,111.913829306091,618.015546649378));
#275167=CARTESIAN_POINT('',(-41.4045999999974,111.913829306091,593.015546649378));
#275168=CARTESIAN_POINT('',(-41.4045999999974,111.913829306091,568.015546649378));
#275169=CARTESIAN_POINT('',(-41.4045999999974,111.913829306091,543.015546649378));
#275170=CARTESIAN_POINT('',(-41.4045999999974,111.913829306091,518.015546649378));
#275171=CARTESIAN_POINT('',(-41.4045999999974,111.913829306091,493.015546649378));
#275172=CARTESIAN_POINT('',(-41.4045999999974,111.913829306091,468.015546649378));
#275173=CARTESIAN_POINT('',(-41.4045999999974,111.913829306091,443.015546649378));
#275174=CARTESIAN_POINT('',(-41.4045999999974,111.913829306091,418.015546649378));
#275175=CARTESIAN_POINT('',(-41.4045999999974,111.913829306091,393.015546649378));
#275176=CARTESIAN_POINT('',(-41.4045999999974,111.913829306091,368.015546649378));
#275177=CARTESIAN_POINT('',(-41.4045999999974,111.913829306091,343.015546649378));
#275178=CARTESIAN_POINT('',(-41.4045999999974,111.913829306091,318.015546649378));
#275179=CARTESIAN_POINT('',(-41.4045999999974,111.913829306091,293.015546649378));
#275180=CARTESIAN_POINT('',(-41.4045999999974,111.913829306091,268.015546649378));
#275181=CARTESIAN_POINT('',(-41.4045999999974,111.913829306091,243.015546649378));
#275182=CARTESIAN_POINT('',(-41.4045999999974,111.913829306091,218.015546649378));
#275183=CARTESIAN_POINT('',(-41.4045999999974,111.913829306091,193.015546649378));
#275184=CARTESIAN_POINT('',(-41.4045999999974,111.913829306091,168.015546649378));
#275185=CARTESIAN_POINT('',(-41.4045999999974,111.913829306091,143.015546649378));
#275186=CARTESIAN_POINT('',(-41.4045999999974,111.913829306091,118.015546649378));
#275187=CARTESIAN_POINT('',(-41.4045999999974,111.913829306091,93.0155466493778));
#275188=CARTESIAN_POINT('',(-41.4045999999974,111.913829306091,68.0155466493778));
#275189=CARTESIAN_POINT('',(-41.4045999999974,111.913829306091,43.0155466493778));
#275190=CARTESIAN_POINT('',(-41.4045999999974,111.913829306091,18.0155466493779));
#275191=CARTESIAN_POINT('',(-41.4045999999974,111.913829306091,-6.98445335062214));
#275192=CARTESIAN_POINT('',(-41.4045999999974,111.913829306091,-31.9844533506222));
#275193=CARTESIAN_POINT('',(-41.4045999999974,111.913829306091,-56.9844533506222));
#275194=CARTESIAN_POINT('',(-41.4045999999974,111.913829306091,-81.9844533506222));
#275195=CARTESIAN_POINT('',(-41.4045999999974,111.913829306091,-106.984453350622));
#275196=CARTESIAN_POINT('',(-41.4045999999974,111.913829306091,-131.984453350622));
#275197=CARTESIAN_POINT('',(-41.4045999999974,111.913829306091,-156.984453350622));
#275198=CARTESIAN_POINT('',(-41.4045999999974,111.913829306091,-181.984453350622));
#275199=CARTESIAN_POINT('',(-41.4045999999974,111.913829306091,-206.984453350622));
#275200=CARTESIAN_POINT('',(-41.4045999999974,111.913829306091,-231.984453350622));
#275201=CARTESIAN_POINT('',(-41.4045999999974,111.913829306091,-256.984453350622));
#275202=CARTESIAN_POINT('',(-41.4045999999974,111.913829306091,-281.984453350622));
#275203=CARTESIAN_POINT('',(-41.4045999999974,111.913829306091,-306.984453350622));
#275204=CARTESIAN_POINT('',(-41.4045999999974,111.913829306091,-331.984453350622));
#275205=CARTESIAN_POINT('',(-41.4045999999974,111.913829306091,-356.984453350622));
#275206=CARTESIAN_POINT('',(-41.4045999999974,111.913829306091,-381.984453350622));
#275207=CARTESIAN_POINT('',(-41.4045999999974,111.913829306091,-406.984453350622));
#275208=CARTESIAN_POINT('',(-41.4045999999974,111.913829306091,-431.984453350622));
#275209=CARTESIAN_POINT('',(-41.4045999999974,111.913829306091,-456.984453350622));
#275210=CARTESIAN_POINT('',(-41.4045999999974,111.913829306091,-481.984453350622));
#275211=CARTESIAN_POINT('',(-41.4045999999974,111.913829306091,-506.984453350622));
#275212=CARTESIAN_POINT('',(-41.4045999999974,111.913829306091,-531.984453350622));
#275213=CARTESIAN_POINT('',(-41.4045999999974,111.913829306091,-556.984453350622));
#275214=CARTESIAN_POINT('',(-41.4045999999974,111.913829306091,-581.984453350622));
#275215=CARTESIAN_POINT('',(-41.4045999999974,111.913829306091,-606.984453350622));
#275216=CARTESIAN_POINT('',(-41.4045999999974,111.913829306091,-631.984453350622));
#275217=CARTESIAN_POINT('',(-41.4045999999974,111.913829306091,-656.984453350622));
#275218=CARTESIAN_POINT('',(-41.4045999999974,111.913829306091,-681.984453350622));
#275219=CARTESIAN_POINT('',(-41.4045999999974,111.913829306091,-706.984453350622));
#275220=CARTESIAN_POINT('',(-41.4045999999974,111.913829306091,-731.984453350622));
#275221=CARTESIAN_POINT('',(-38.2959750514476,15.4302832282296,768.555683732354));
#275222=CARTESIAN_POINT('',(-38.2959750514478,15.4302832281189,743.555683732442));
#275223=CARTESIAN_POINT('',(-38.2959750514478,15.4302832281189,718.555683732442));
#275224=CARTESIAN_POINT('',(-38.2959750514478,15.4302832281189,693.555683732442));
#275225=CARTESIAN_POINT('',(-38.2959750514478,15.430283228119,668.555683732442));
#275226=CARTESIAN_POINT('',(-38.2959750514478,15.430283228119,643.555683732442));
#275227=CARTESIAN_POINT('',(-38.2959750514478,15.430283228119,618.555683732442));
#275228=CARTESIAN_POINT('',(-38.2959750514478,15.430283228119,593.555683732442));
#275229=CARTESIAN_POINT('',(-38.2959750514478,15.430283228119,568.555683732442));
#275230=CARTESIAN_POINT('',(-38.2959750514478,15.430283228119,543.555683732442));
#275231=CARTESIAN_POINT('',(-38.2959750514478,15.430283228119,518.555683732442));
#275232=CARTESIAN_POINT('',(-38.2959750514478,15.430283228119,493.555683732442));
#275233=CARTESIAN_POINT('',(-38.2959750514478,15.430283228119,468.555683732442));
#275234=CARTESIAN_POINT('',(-38.2959750514478,15.430283228119,443.555683732442));
#275235=CARTESIAN_POINT('',(-38.2959750514478,15.430283228119,418.555683732442));
#275236=CARTESIAN_POINT('',(-38.2959750514478,15.430283228119,393.555683732442));
#275237=CARTESIAN_POINT('',(-38.2959750514478,15.430283228119,368.555683732442));
#275238=CARTESIAN_POINT('',(-38.2959750514478,15.430283228119,343.555683732442));
#275239=CARTESIAN_POINT('',(-38.2959750514478,15.430283228119,318.555683732442));
#275240=CARTESIAN_POINT('',(-38.2959750514478,15.430283228119,293.555683732442));
#275241=CARTESIAN_POINT('',(-38.2959750514478,15.430283228119,268.555683732442));
#275242=CARTESIAN_POINT('',(-38.2959750514478,15.430283228119,243.555683732442));
#275243=CARTESIAN_POINT('',(-38.2959750514478,15.430283228119,218.555683732442));
#275244=CARTESIAN_POINT('',(-38.2959750514478,15.430283228119,193.555683732442));
#275245=CARTESIAN_POINT('',(-38.2959750514478,15.430283228119,168.555683732442));
#275246=CARTESIAN_POINT('',(-38.2959750514478,15.430283228119,143.555683732442));
#275247=CARTESIAN_POINT('',(-38.2959750514478,15.430283228119,118.555683732442));
#275248=CARTESIAN_POINT('',(-38.2959750514478,15.430283228119,93.5556837324418));
#275249=CARTESIAN_POINT('',(-38.2959750514478,15.430283228119,68.5556837324418));
#275250=CARTESIAN_POINT('',(-38.2959750514478,15.430283228119,43.5556837324418));
#275251=CARTESIAN_POINT('',(-38.2959750514478,15.430283228119,18.5556837324419));
#275252=CARTESIAN_POINT('',(-38.2959750514478,15.430283228119,-6.44431626755815));
#275253=CARTESIAN_POINT('',(-38.2959750514478,15.430283228119,-31.4443162675582));
#275254=CARTESIAN_POINT('',(-38.2959750514478,15.430283228119,-56.4443162675582));
#275255=CARTESIAN_POINT('',(-38.2959750514478,15.430283228119,-81.4443162675582));
#275256=CARTESIAN_POINT('',(-38.2959750514478,15.430283228119,-106.444316267558));
#275257=CARTESIAN_POINT('',(-38.2959750514478,15.430283228119,-131.444316267558));
#275258=CARTESIAN_POINT('',(-38.2959750514478,15.4302832281191,-156.444316267558));
#275259=CARTESIAN_POINT('',(-38.2959750514478,15.4302832281191,-181.444316267558));
#275260=CARTESIAN_POINT('',(-38.2959750514478,15.4302832281191,-206.444316267558));
#275261=CARTESIAN_POINT('',(-38.2959750514478,15.4302832281191,-231.444316267558));
#275262=CARTESIAN_POINT('',(-38.2959750514478,15.4302832281191,-256.444316267558));
#275263=CARTESIAN_POINT('',(-38.2959750514478,15.4302832281191,-281.444316267558));
#275264=CARTESIAN_POINT('',(-38.2959750514478,15.4302832281191,-306.444316267558));
#275265=CARTESIAN_POINT('',(-38.2959750514478,15.4302832281191,-331.444316267558));
#275266=CARTESIAN_POINT('',(-38.2959750514478,15.4302832281191,-356.444316267558));
#275267=CARTESIAN_POINT('',(-38.2959750514478,15.4302832281191,-381.444316267558));
#275268=CARTESIAN_POINT('',(-38.2959750514478,15.4302832281191,-406.444316267558));
#275269=CARTESIAN_POINT('',(-38.2959750514478,15.4302832281191,-431.444316267558));
#275270=CARTESIAN_POINT('',(-38.2959750514478,15.4302832281191,-456.444316267558));
#275271=CARTESIAN_POINT('',(-38.2959750514478,15.4302832281191,-481.444316267558));
#275272=CARTESIAN_POINT('',(-38.2959750514478,15.4302832281191,-506.444316267558));
#275273=CARTESIAN_POINT('',(-38.2959750514478,15.4302832281191,-531.444316267558));
#275274=CARTESIAN_POINT('',(-38.2959750514478,15.4302832281191,-556.444316267558));
#275275=CARTESIAN_POINT('',(-38.2959750514478,15.4302832281191,-581.444316267558));
#275276=CARTESIAN_POINT('',(-38.2959750514478,15.4302832281191,-606.444316267558));
#275277=CARTESIAN_POINT('',(-38.2959750514478,15.4302832281191,-631.444316267558));
#275278=CARTESIAN_POINT('',(-38.2959750514478,15.4302832281191,-656.444316267558));
#275279=CARTESIAN_POINT('',(-38.2959750514478,15.4302832281191,-681.444316267558));
#275280=CARTESIAN_POINT('',(-38.2959750514478,15.4302832281191,-706.444316267558));
#275281=CARTESIAN_POINT('',(-38.2959750514297,15.4302832282113,-731.444316267658));
#275282=CARTESIAN_POINT('',(-42.1104271920802,112.021020569781,793.41587603213));
#275283=CARTESIAN_POINT('',(-39.5104271921298,105.440204329242,816.853373334007));
#275284=CARTESIAN_POINT('',(-39.5104271921298,87.7643394186573,833.946155661552));
#275285=CARTESIAN_POINT('',(-39.5104271921297,64.1151333275587,839.830231614584));
#275286=CARTESIAN_POINT('',(-36.1124956440428,40.3145477181419,833.319992864115));
#275287=CARTESIAN_POINT('',(-36.112495644043,15.0468440963824,793.9477717347));
#275288=CARTESIAN_POINT('',(-36.1124956440429,21.8288092633938,816.921723846702));
#275289=CARTESIAN_POINT('',(-40.7779344593138,105.597550309198,-780.919361011843));
#275290=CARTESIAN_POINT('',(-40.7779344593138,87.8567627431459,-798.074923517112));
#275291=CARTESIAN_POINT('',(-41.544540380328,112.206254579911,-757.382543778522));
#275292=CARTESIAN_POINT('',(-38.295975051427,64.1087111198557,-803.983592080533));
#275293=CARTESIAN_POINT('',(-38.295975051427,40.2258460707983,-797.450846654312));
#275294=CARTESIAN_POINT('',(-38.2959750514271,21.6779238628137,-780.997415192991));
#275295=CARTESIAN_POINT('',(-38.2959750514272,14.8617892193548,-757.907709836733));
#275296=CARTESIAN_POINT('',(0.,0.,0.));
#275297=CARTESIAN_POINT('Origin',(0.,0.,-260.5));
#275298=CARTESIAN_POINT('',(36.25,-4.43934464690916E-15,-260.5));
#275299=CARTESIAN_POINT('Origin',(0.,0.,-260.5));
#275300=CARTESIAN_POINT('',(36.25,-4.43934464690916E-15,-287.5));
#275301=CARTESIAN_POINT('',(36.25,-4.43934464690916E-15,-260.5));
#275302=CARTESIAN_POINT('Origin',(0.,0.,-287.5));
#275303=CARTESIAN_POINT('Origin',(0.,0.,260.5));
#275304=CARTESIAN_POINT('',(-36.25,-4.43934464690916E-15,260.5));
#275305=CARTESIAN_POINT('Origin',(0.,0.,260.5));
#275306=CARTESIAN_POINT('',(-36.25,-4.43934464690916E-15,287.5));
#275307=CARTESIAN_POINT('',(-36.25,-4.43934464690916E-15,260.5));
#275308=CARTESIAN_POINT('Origin',(0.,0.,287.5));
#275309=CARTESIAN_POINT('Origin',(0.,0.,287.5));
#275310=CARTESIAN_POINT('',(45.,-5.51091059616309E-15,-287.5));
#275311=CARTESIAN_POINT('Origin',(0.,0.,-287.5));
#275312=CARTESIAN_POINT('',(45.,-5.51091059616309E-15,287.5));
#275313=CARTESIAN_POINT('',(45.,-5.51091059616309E-15,287.5));
#275314=CARTESIAN_POINT('Origin',(0.,0.,287.5));
#275315=CARTESIAN_POINT('Origin',(0.,0.,287.5));
#275316=CARTESIAN_POINT('',(30.,-3.67394039744206E-15,260.5));
#275317=CARTESIAN_POINT('Origin',(0.,0.,260.5));
#275318=CARTESIAN_POINT('',(30.,-3.67394039744206E-15,-260.5));
#275319=CARTESIAN_POINT('',(30.,-3.67394039744206E-15,287.5));
#275320=CARTESIAN_POINT('Origin',(0.,0.,-260.5));
#275321=CARTESIAN_POINT('Origin',(0.,0.,287.5));
#275322=CARTESIAN_POINT('Origin',(0.,0.,-287.5));
#275323=CARTESIAN_POINT('Origin',(0.,0.,260.5));
#275324=CARTESIAN_POINT('Origin',(0.,0.,-260.5));
#275325=CARTESIAN_POINT('',(0.,0.,0.));
#275326=CARTESIAN_POINT('Origin',(0.,0.,-12.5));
#275327=CARTESIAN_POINT('',(-16.0425342723895,-1.96464382468935E-15,-13.5));
#275328=CARTESIAN_POINT('Origin',(0.,0.,-13.5));
#275329=CARTESIAN_POINT('',(-15.0434011963687,1.90606889192839E-15,-12.4583695255704));
#275330=CARTESIAN_POINT('Origin',(-16.0425342723895,-1.96464382468935E-15,
-12.5));
#275331=CARTESIAN_POINT('Origin',(0.,0.,-12.4583695255704));
#275332=CARTESIAN_POINT('Origin',(0.,0.,6.75));
#275333=CARTESIAN_POINT('',(-23.4,2.86567351000481E-15,10.9275551957205));
#275334=CARTESIAN_POINT('Origin',(0.,0.,10.9275551957205));
#275335=CARTESIAN_POINT('',(-23.4,-2.86567351000481E-15,2.57244480427945));
#275336=CARTESIAN_POINT('Origin',(-26.5598538869239,-3.25264400484428E-15,
6.75));
#275337=CARTESIAN_POINT('Origin',(0.,0.,2.57244480427945));
#275338=CARTESIAN_POINT('Origin',(0.,0.,-6.75));
#275339=CARTESIAN_POINT('',(-23.4,2.86567351000481E-15,-2.57244480427945));
#275340=CARTESIAN_POINT('Origin',(0.,0.,-2.57244480427945));
#275341=CARTESIAN_POINT('',(-23.4,-2.86567351000481E-15,-10.9275551957205));
#275342=CARTESIAN_POINT('Origin',(-26.5598538869239,-3.25264400484428E-15,
-6.75));
#275343=CARTESIAN_POINT('Origin',(0.,0.,-10.9275551957205));
#275344=CARTESIAN_POINT('Origin',(0.,0.,12.5416304744296));
#275345=CARTESIAN_POINT('',(-16.0850661013937,-1.96985247151454E-15,12.5416304744296));
#275346=CARTESIAN_POINT('',(-16.0850661013937,-1.96985247151454E-15,12.5416304744296));
#275347=CARTESIAN_POINT('Origin',(0.,0.,12.5416304744296));
#275348=CARTESIAN_POINT('Origin',(0.,0.,12.5));
#275349=CARTESIAN_POINT('',(-17.0841991774145,-2.09221098386165E-15,13.5));
#275350=CARTESIAN_POINT('Origin',(-17.0841991774145,-2.09221098386165E-15,
12.5));
#275351=CARTESIAN_POINT('Origin',(0.,0.,13.5));
#275352=CARTESIAN_POINT('Origin',(0.,0.,12.5));
#275353=CARTESIAN_POINT('',(-22.4,-2.74320883009007E-15,13.5));
#275354=CARTESIAN_POINT('Origin',(0.,0.,13.5));
#275355=CARTESIAN_POINT('',(-23.4,-2.86567351000481E-15,12.5));
#275356=CARTESIAN_POINT('Origin',(-22.4,-2.74320883009007E-15,12.5));
#275357=CARTESIAN_POINT('Origin',(0.,0.,12.5));
#275358=CARTESIAN_POINT('Origin',(0.,0.,0.));
#275359=CARTESIAN_POINT('',(-23.4,-2.86567351000481E-15,0.));
#275360=CARTESIAN_POINT('Origin',(0.,0.,0.));
#275361=CARTESIAN_POINT('',(-23.4,-2.86567351000481E-15,0.));
#275362=CARTESIAN_POINT('Origin',(0.,0.,0.));
#275363=CARTESIAN_POINT('',(-23.4,-2.86567351000481E-15,-12.5));
#275364=CARTESIAN_POINT('',(-23.4,-2.86567351000481E-15,0.));
#275365=CARTESIAN_POINT('Origin',(0.,0.,-12.5));
#275366=CARTESIAN_POINT('Origin',(0.,0.,-12.5));
#275367=CARTESIAN_POINT('',(-22.4,-2.74320883009007E-15,-13.5));
#275368=CARTESIAN_POINT('Origin',(-22.4,-2.74320883009007E-15,-12.5));
#275369=CARTESIAN_POINT('Origin',(0.,0.,-13.5));
#275370=CARTESIAN_POINT('Origin',(0.,22.4,13.5));
#275371=CARTESIAN_POINT('Origin',(0.,22.4,-13.5));
#275372=CARTESIAN_POINT('Origin',(0.,0.,0.));
#275373=CARTESIAN_POINT('',(32.6421664440783,-1.99875623264878E-15,2.44777042258915E-31));
#275374=CARTESIAN_POINT('',(-32.6421664440783,-1.99875623264878E-15,2.44777042258915E-31));
#275375=CARTESIAN_POINT('Origin',(0.,0.,0.));
#275376=CARTESIAN_POINT('',(0.,29.7197077738478,-13.5));
#275377=CARTESIAN_POINT('Origin',(0.,0.,-13.5));
#275378=CARTESIAN_POINT('',(0.,29.7197077738479,13.5));
#275379=CARTESIAN_POINT('Origin',(0.,0.,13.5));
#275380=CARTESIAN_POINT('Origin',(0.,0.,12.5));
#275381=CARTESIAN_POINT('',(-35.,-4.28626379701574E-15,13.5));
#275382=CARTESIAN_POINT('Origin',(0.,0.,13.5));
#275383=CARTESIAN_POINT('',(-36.,-4.40872847693047E-15,12.5));
#275384=CARTESIAN_POINT('Origin',(-35.,-4.28626379701574E-15,12.5));
#275385=CARTESIAN_POINT('Origin',(0.,0.,12.5));
#275386=CARTESIAN_POINT('Origin',(0.,0.,0.));
#275387=CARTESIAN_POINT('',(-36.,-4.40872847693047E-15,-12.5));
#275388=CARTESIAN_POINT('',(-36.,-4.40872847693047E-15,0.));
#275389=CARTESIAN_POINT('Origin',(0.,0.,-12.5));
#275390=CARTESIAN_POINT('Origin',(0.,0.,-12.5));
#275391=CARTESIAN_POINT('',(-35.,-4.28626379701574E-15,-13.5));
#275392=CARTESIAN_POINT('Origin',(-35.,-4.28626379701574E-15,-12.5));
#275393=CARTESIAN_POINT('Origin',(0.,0.,-13.5));
#275394=CARTESIAN_POINT('Origin',(0.,29.7197077738479,13.5));
#275395=CARTESIAN_POINT('Origin',(0.,35.,-13.5));
#275396=CARTESIAN_POINT('Origin',(0.,26.5598538869239,6.75));
#275397=CARTESIAN_POINT('',(-5.238,26.5598538869239,6.75));
#275398=CARTESIAN_POINT('',(5.238,26.5598538869239,6.75));
#275399=CARTESIAN_POINT('Origin',(0.,26.5598538869239,6.75));
#275400=CARTESIAN_POINT('Origin',(0.,26.5598538869239,-6.75));
#275401=CARTESIAN_POINT('',(-5.238,26.5598538869239,-6.75));
#275402=CARTESIAN_POINT('',(5.238,26.5598538869239,-6.75));
#275403=CARTESIAN_POINT('Origin',(0.,26.5598538869239,-6.75));
#275404=CARTESIAN_POINT('Origin',(-13.279926943462,23.001508186879,6.75));
#275405=CARTESIAN_POINT('',(-17.8161680084849,20.382508186879,6.75));
#275406=CARTESIAN_POINT('',(-8.7436858784391,25.620508186879,6.75));
#275407=CARTESIAN_POINT('Origin',(-13.279926943462,23.001508186879,6.75));
#275408=CARTESIAN_POINT('Origin',(-23.001508186879,13.2799269434619,6.75));
#275409=CARTESIAN_POINT('',(-25.620508186879,8.74368587843902,6.75));
#275410=CARTESIAN_POINT('',(-20.382508186879,17.8161680084848,6.75));
#275411=CARTESIAN_POINT('Origin',(-23.001508186879,13.2799269434619,6.75));
#275412=CARTESIAN_POINT('Origin',(-26.5598538869239,-9.27332342085952E-14,
6.75));
#275413=CARTESIAN_POINT('',(-26.5598538869239,-5.2380000000001,6.75));
#275414=CARTESIAN_POINT('',(-26.5598538869239,5.23799999999991,6.75));
#275415=CARTESIAN_POINT('Origin',(-26.5598538869239,-9.27332342085952E-14,
6.75));
#275416=CARTESIAN_POINT('Origin',(-23.0015081868789,-13.2799269434621,6.75));
#275417=CARTESIAN_POINT('',(-20.3825081868789,-17.816168008485,6.75));
#275418=CARTESIAN_POINT('',(-25.620508186879,-8.74368587843919,6.75));
#275419=CARTESIAN_POINT('Origin',(-23.0015081868789,-13.2799269434621,6.75));
#275420=CARTESIAN_POINT('Origin',(-13.2799269434618,-23.0015081868791,6.75));
#275421=CARTESIAN_POINT('',(-8.74368587843892,-25.620508186879,6.75));
#275422=CARTESIAN_POINT('',(-17.8161680084847,-20.3825081868791,6.75));
#275423=CARTESIAN_POINT('Origin',(-13.2799269434618,-23.0015081868791,6.75));
#275424=CARTESIAN_POINT('Origin',(0.,-26.5598538869239,6.75));
#275425=CARTESIAN_POINT('',(5.238,-26.5598538869239,6.75));
#275426=CARTESIAN_POINT('',(-5.238,-26.5598538869239,6.75));
#275427=CARTESIAN_POINT('Origin',(0.,-26.5598538869239,6.75));
#275428=CARTESIAN_POINT('Origin',(13.2799269434622,-23.0015081868789,6.75));
#275429=CARTESIAN_POINT('',(17.816168008485,-20.3825081868788,6.75));
#275430=CARTESIAN_POINT('',(8.74368587843928,-25.6205081868789,6.75));
#275431=CARTESIAN_POINT('Origin',(13.2799269434622,-23.0015081868789,6.75));
#275432=CARTESIAN_POINT('Origin',(23.0015081868791,-13.2799269434618,6.75));
#275433=CARTESIAN_POINT('',(25.6205081868791,-8.74368587843884,6.75));
#275434=CARTESIAN_POINT('',(20.3825081868792,-17.8161680084847,6.75));
#275435=CARTESIAN_POINT('Origin',(23.0015081868791,-13.2799269434618,6.75));
#275436=CARTESIAN_POINT('Origin',(26.5598538869239,2.78199702625785E-13,
6.75));
#275437=CARTESIAN_POINT('',(26.5598538869239,5.23800000000028,6.75));
#275438=CARTESIAN_POINT('',(26.559853886924,-5.23799999999972,6.75));
#275439=CARTESIAN_POINT('Origin',(26.5598538869239,2.78199702625785E-13,
6.75));
#275440=CARTESIAN_POINT('Origin',(23.0015081868788,13.2799269434622,6.75));
#275441=CARTESIAN_POINT('',(20.3825081868788,17.8161680084851,6.75));
#275442=CARTESIAN_POINT('',(25.6205081868789,8.74368587843937,6.75));
#275443=CARTESIAN_POINT('Origin',(23.0015081868788,13.2799269434622,6.75));
#275444=CARTESIAN_POINT('Origin',(13.2799269434617,23.0015081868792,6.75));
#275445=CARTESIAN_POINT('',(8.74368587843875,25.6205081868791,6.75));
#275446=CARTESIAN_POINT('',(17.8161680084846,20.3825081868792,6.75));
#275447=CARTESIAN_POINT('Origin',(13.2799269434617,23.0015081868792,6.75));
#275448=CARTESIAN_POINT('Origin',(-13.279926943462,23.001508186879,-6.75));
#275449=CARTESIAN_POINT('',(-17.8161680084849,20.382508186879,-6.75));
#275450=CARTESIAN_POINT('',(-8.7436858784391,25.620508186879,-6.75));
#275451=CARTESIAN_POINT('Origin',(-13.279926943462,23.001508186879,-6.75));
#275452=CARTESIAN_POINT('Origin',(-23.001508186879,13.2799269434619,-6.75));
#275453=CARTESIAN_POINT('',(-25.620508186879,8.74368587843901,-6.75));
#275454=CARTESIAN_POINT('',(-20.382508186879,17.8161680084848,-6.75));
#275455=CARTESIAN_POINT('Origin',(-23.001508186879,13.2799269434619,-6.75));
#275456=CARTESIAN_POINT('Origin',(-26.5598538869239,-9.27332342085952E-14,
-6.75));
#275457=CARTESIAN_POINT('',(-26.5598538869239,-5.2380000000001,-6.75));
#275458=CARTESIAN_POINT('',(-26.5598538869239,5.23799999999991,-6.75));
#275459=CARTESIAN_POINT('Origin',(-26.5598538869239,-9.27332342085952E-14,
-6.75));
#275460=CARTESIAN_POINT('Origin',(-23.0015081868789,-13.2799269434621,-6.75));
#275461=CARTESIAN_POINT('',(-20.3825081868789,-17.816168008485,-6.75));
#275462=CARTESIAN_POINT('',(-25.620508186879,-8.74368587843919,-6.75));
#275463=CARTESIAN_POINT('Origin',(-23.0015081868789,-13.2799269434621,-6.75));
#275464=CARTESIAN_POINT('Origin',(-13.2799269434618,-23.0015081868791,-6.75));
#275465=CARTESIAN_POINT('',(-8.74368587843892,-25.620508186879,-6.75));
#275466=CARTESIAN_POINT('',(-17.8161680084847,-20.3825081868791,-6.75));
#275467=CARTESIAN_POINT('Origin',(-13.2799269434618,-23.0015081868791,-6.75));
#275468=CARTESIAN_POINT('Origin',(0.,-26.5598538869239,-6.75));
#275469=CARTESIAN_POINT('',(5.238,-26.5598538869239,-6.75));
#275470=CARTESIAN_POINT('',(-5.238,-26.5598538869239,-6.75));
#275471=CARTESIAN_POINT('Origin',(0.,-26.5598538869239,-6.75));
#275472=CARTESIAN_POINT('Origin',(13.2799269434622,-23.0015081868789,-6.75));
#275473=CARTESIAN_POINT('',(17.816168008485,-20.3825081868788,-6.75));
#275474=CARTESIAN_POINT('',(8.74368587843928,-25.6205081868789,-6.75));
#275475=CARTESIAN_POINT('Origin',(13.2799269434622,-23.0015081868789,-6.75));
#275476=CARTESIAN_POINT('Origin',(23.0015081868791,-13.2799269434618,-6.75));
#275477=CARTESIAN_POINT('',(25.6205081868791,-8.74368587843884,-6.75));
#275478=CARTESIAN_POINT('',(20.3825081868792,-17.8161680084847,-6.75));
#275479=CARTESIAN_POINT('Origin',(23.0015081868791,-13.2799269434618,-6.75));
#275480=CARTESIAN_POINT('Origin',(26.5598538869239,2.78199702625785E-13,
-6.75));
#275481=CARTESIAN_POINT('',(26.5598538869239,5.23800000000028,-6.75));
#275482=CARTESIAN_POINT('',(26.559853886924,-5.23799999999973,-6.75));
#275483=CARTESIAN_POINT('Origin',(26.5598538869239,2.78199702625785E-13,
-6.75));
#275484=CARTESIAN_POINT('Origin',(23.0015081868788,13.2799269434622,-6.75));
#275485=CARTESIAN_POINT('',(20.3825081868788,17.8161680084851,-6.75));
#275486=CARTESIAN_POINT('',(25.6205081868789,8.74368587843937,-6.75));
#275487=CARTESIAN_POINT('Origin',(23.0015081868788,13.2799269434622,-6.75));
#275488=CARTESIAN_POINT('Origin',(13.2799269434617,23.0015081868792,-6.75));
#275489=CARTESIAN_POINT('',(8.74368587843874,25.6205081868791,-6.75));
#275490=CARTESIAN_POINT('',(17.8161680084846,20.3825081868792,-6.75));
#275491=CARTESIAN_POINT('Origin',(13.2799269434617,23.0015081868792,-6.75));
#275492=CARTESIAN_POINT('',(0.,0.,0.));
#275493=CARTESIAN_POINT('Origin',(0.,0.,-325.25));
#275494=CARTESIAN_POINT('',(-7.25,-8.87868929381831E-16,-295.25));
#275495=CARTESIAN_POINT('Origin',(0.,0.,-295.25));
#275496=CARTESIAN_POINT('',(-7.25,-8.87868929381831E-16,-325.25));
#275497=CARTESIAN_POINT('',(-7.25,-8.87868929381831E-16,-325.25));
#275498=CARTESIAN_POINT('Origin',(0.,0.,-325.25));
#275499=CARTESIAN_POINT('Origin',(0.,0.,-295.25));
#275500=CARTESIAN_POINT('',(-16.,-1.95943487863577E-15,-260.25));
#275501=CARTESIAN_POINT('Origin',(0.,0.,-260.25));
#275502=CARTESIAN_POINT('',(-16.,-1.95943487863577E-15,-295.25));
#275503=CARTESIAN_POINT('',(-16.,-1.95943487863577E-15,-295.25));
#275504=CARTESIAN_POINT('Origin',(0.,0.,-295.25));
#275505=CARTESIAN_POINT('Origin',(0.,0.,325.25));
#275506=CARTESIAN_POINT('',(7.25,-8.87868929381831E-16,295.25));
#275507=CARTESIAN_POINT('Origin',(0.,0.,295.25));
#275508=CARTESIAN_POINT('',(7.25,-8.87868929381831E-16,325.25));
#275509=CARTESIAN_POINT('',(7.25,-8.87868929381831E-16,325.25));
#275510=CARTESIAN_POINT('Origin',(0.,0.,325.25));
#275511=CARTESIAN_POINT('Origin',(0.,0.,295.25));
#275512=CARTESIAN_POINT('',(16.,-1.95943487863577E-15,260.25));
#275513=CARTESIAN_POINT('Origin',(0.,0.,260.25));
#275514=CARTESIAN_POINT('',(16.,-1.95943487863577E-15,295.25));
#275515=CARTESIAN_POINT('',(16.,-1.95943487863577E-15,295.25));
#275516=CARTESIAN_POINT('Origin',(0.,0.,295.25));
#275517=CARTESIAN_POINT('Origin',(21.650635094611,12.5,260.25));
#275518=CARTESIAN_POINT('',(21.650635094611,12.5,-260.25));
#275519=CARTESIAN_POINT('',(3.0046291974743E-15,25.,-260.25));
#275520=CARTESIAN_POINT('',(21.650635094611,12.5,-260.25));
#275521=CARTESIAN_POINT('',(3.0046291974743E-15,25.,260.25));
#275522=CARTESIAN_POINT('',(3.0046291974743E-15,25.,260.25));
#275523=CARTESIAN_POINT('',(21.650635094611,12.5,260.25));
#275524=CARTESIAN_POINT('',(21.650635094611,12.5,260.25));
#275525=CARTESIAN_POINT('',(21.650635094611,12.5,260.25));
#275526=CARTESIAN_POINT('Origin',(3.0046291974743E-15,25.,260.25));
#275527=CARTESIAN_POINT('',(-21.650635094611,12.5,-260.25));
#275528=CARTESIAN_POINT('',(3.0046291974743E-15,25.,-260.25));
#275529=CARTESIAN_POINT('',(-21.650635094611,12.5,260.25));
#275530=CARTESIAN_POINT('',(-21.650635094611,12.5,260.25));
#275531=CARTESIAN_POINT('',(3.0046291974743E-15,25.,260.25));
#275532=CARTESIAN_POINT('Origin',(-21.650635094611,12.5,260.25));
#275533=CARTESIAN_POINT('',(-21.650635094611,-12.5,-260.25));
#275534=CARTESIAN_POINT('',(-21.650635094611,12.5,-260.25));
#275535=CARTESIAN_POINT('',(-21.650635094611,-12.5,260.25));
#275536=CARTESIAN_POINT('',(-21.650635094611,-12.5,260.25));
#275537=CARTESIAN_POINT('',(-21.650635094611,12.5,260.25));
#275538=CARTESIAN_POINT('Origin',(-21.650635094611,-12.5,260.25));
#275539=CARTESIAN_POINT('',(3.87537447643023E-16,-25.,-260.25));
#275540=CARTESIAN_POINT('',(-21.650635094611,-12.5,-260.25));
#275541=CARTESIAN_POINT('',(3.87537447643023E-16,-25.,260.25));
#275542=CARTESIAN_POINT('',(3.87537447643023E-16,-25.,260.25));
#275543=CARTESIAN_POINT('',(-21.650635094611,-12.5,260.25));
#275544=CARTESIAN_POINT('Origin',(3.87537447643023E-16,-25.,260.25));
#275545=CARTESIAN_POINT('',(21.650635094611,-12.5,-260.25));
#275546=CARTESIAN_POINT('',(3.87537447643023E-16,-25.,-260.25));
#275547=CARTESIAN_POINT('',(21.650635094611,-12.5,260.25));
#275548=CARTESIAN_POINT('',(21.650635094611,-12.5,260.25));
#275549=CARTESIAN_POINT('',(3.87537447643023E-16,-25.,260.25));
#275550=CARTESIAN_POINT('Origin',(21.650635094611,-12.5,260.25));
#275551=CARTESIAN_POINT('',(21.650635094611,-12.5,-260.25));
#275552=CARTESIAN_POINT('',(21.650635094611,-12.5,260.25));
#275553=CARTESIAN_POINT('Origin',(0.,0.,260.25));
#275554=CARTESIAN_POINT('Origin',(0.,0.,-260.25));
#275555=CARTESIAN_POINT('Origin',(0.,0.,295.25));
#275556=CARTESIAN_POINT('Origin',(0.,0.,325.25));
#275557=CARTESIAN_POINT('Origin',(0.,0.,-295.25));
#275558=CARTESIAN_POINT('Origin',(0.,0.,-325.25));
#275559=CARTESIAN_POINT('',(0.,0.,0.));
#275560=CARTESIAN_POINT('Origin',(-3.77475828372553E-14,-1.881249999982,
2.68644078414671E-15));
#275561=CARTESIAN_POINT('',(10.0514428414941,107.431249999581,1.00171110072065E-15));
#275562=CARTESIAN_POINT('',(10.0514428414941,107.431911591494,-1.23094673026484E-15));
#275563=CARTESIAN_POINT('',(10.0514428414941,-1.881249999982,4.14193483802857E-15));
#275564=CARTESIAN_POINT('',(10.0514325246607,107.431911591494,-0.0144013199032517));
#275565=CARTESIAN_POINT('Origin',(-3.77475828372553E-14,107.431911591494,
1.77886938496422E-15));
#275566=CARTESIAN_POINT('Ctrl Pts',(10.0514428414941,107.431249999581,-1.23094673026484E-15));
#275567=CARTESIAN_POINT('Ctrl Pts',(10.0514428414941,107.431580718727,-0.00720066364701881));
#275568=CARTESIAN_POINT('Ctrl Pts',(10.0514325246607,107.431911591494,-0.0144013199032517));
#275569=CARTESIAN_POINT('Origin',(-3.77475828372553E-14,-1.881249999982,
2.68644078414671E-15));
#275570=CARTESIAN_POINT('',(10.0514428414941,104.431249999593,1.01416483528425E-15));
#275571=CARTESIAN_POINT('',(10.0514428414941,104.806249999591,1.0126081184638E-15));
#275572=CARTESIAN_POINT('',(10.0514428414941,-1.881249999982,4.14193483802857E-15));
#275573=CARTESIAN_POINT('',(7.10339095491525,107.431911591494,7.11149352368764));
#275574=CARTESIAN_POINT('Ctrl Pts',(10.0514428414941,104.806249999591,-1.23094673026484E-15));
#275575=CARTESIAN_POINT('Ctrl Pts',(10.0514428414941,104.956249999591,-3.26591175476071));
#275576=CARTESIAN_POINT('Ctrl Pts',(8.13178807675712,105.10624999959,-5.90808986649102));
#275577=CARTESIAN_POINT('Ctrl Pts',(6.21213331202014,105.256249999589,-8.55026797822134));
#275578=CARTESIAN_POINT('Ctrl Pts',(3.10606665601003,105.406249999589,-9.5594902125713));
#275579=CARTESIAN_POINT('Ctrl Pts',(-7.39149410146522E-14,105.556249999588,
-10.5687124469213));
#275580=CARTESIAN_POINT('Ctrl Pts',(-3.10606665601018,105.706249999588,
-9.5594902125713));
#275581=CARTESIAN_POINT('Ctrl Pts',(-6.21213331202029,105.856249999587,
-8.55026797822134));
#275582=CARTESIAN_POINT('Ctrl Pts',(-8.13178807675726,106.006249999586,
-5.90808986649102));
#275583=CARTESIAN_POINT('Ctrl Pts',(-10.0514428414942,106.156249999586,
-3.2659117547607));
#275584=CARTESIAN_POINT('Ctrl Pts',(-10.0514428414942,106.306249999585,
2.46189346052968E-15));
#275585=CARTESIAN_POINT('Ctrl Pts',(-10.0514428414942,106.456249999585,
3.26591175476071));
#275586=CARTESIAN_POINT('Ctrl Pts',(-8.13178807675726,106.606249999584,
5.90808986649102));
#275587=CARTESIAN_POINT('Ctrl Pts',(-6.21213331202029,106.756249999583,
8.55026797822134));
#275588=CARTESIAN_POINT('Ctrl Pts',(-3.10606665601018,106.906249999583,
9.5594902125713));
#275589=CARTESIAN_POINT('Ctrl Pts',(-7.21902076766369E-14,107.056249999582,
10.5687124469213));
#275590=CARTESIAN_POINT('Ctrl Pts',(3.10606665601003,107.206249999582,9.5594902125713));
#275591=CARTESIAN_POINT('Ctrl Pts',(5.3982158846568,107.316943819893,8.8147257814789));
#275592=CARTESIAN_POINT('Ctrl Pts',(7.10339095491525,107.431911591494,7.11149352368764));
#275593=CARTESIAN_POINT('Origin',(-3.77475828372553E-14,107.431911591494,
1.77886938496422E-15));
#275594=CARTESIAN_POINT('Ctrl Pts',(10.0514428414941,104.431249999593,-1.23094673026484E-15));
#275595=CARTESIAN_POINT('Ctrl Pts',(10.0514428414941,104.581249999592,-3.26591175476071));
#275596=CARTESIAN_POINT('Ctrl Pts',(8.13178807675712,104.731249999592,-5.90808986649102));
#275597=CARTESIAN_POINT('Ctrl Pts',(6.21213331202014,104.881249999591,-8.55026797822134));
#275598=CARTESIAN_POINT('Ctrl Pts',(3.10606665601003,105.03124999959,-9.5594902125713));
#275599=CARTESIAN_POINT('Ctrl Pts',(-7.36989773556944E-14,105.18124999959,
-10.5687124469213));
#275600=CARTESIAN_POINT('Ctrl Pts',(-3.10606665601018,105.331249999589,
-9.5594902125713));
#275601=CARTESIAN_POINT('Ctrl Pts',(-6.21213331202029,105.481249999589,
-8.55026797822134));
#275602=CARTESIAN_POINT('Ctrl Pts',(-8.13178807675726,105.631249999588,
-5.90808986649102));
#275603=CARTESIAN_POINT('Ctrl Pts',(-10.0514428414942,105.781249999587,
-3.2659117547607));
#275604=CARTESIAN_POINT('Ctrl Pts',(-10.0514428414942,105.931249999587,
2.46189346052968E-15));
#275605=CARTESIAN_POINT('Ctrl Pts',(-10.0514428414942,106.081249999586,
3.26591175476071));
#275606=CARTESIAN_POINT('Ctrl Pts',(-8.13178807675726,106.231249999586,
5.90808986649102));
#275607=CARTESIAN_POINT('Ctrl Pts',(-6.21213331202029,106.381249999585,
8.55026797822134));
#275608=CARTESIAN_POINT('Ctrl Pts',(-3.10606665601018,106.531249999584,
9.5594902125713));
#275609=CARTESIAN_POINT('Ctrl Pts',(-7.19742440176792E-14,106.681249999584,
10.5687124469213));
#275610=CARTESIAN_POINT('Ctrl Pts',(3.10606665601004,106.831249999583,9.5594902125713));
#275611=CARTESIAN_POINT('Ctrl Pts',(6.21213331202014,106.981249999583,8.55026797822134));
#275612=CARTESIAN_POINT('Ctrl Pts',(8.13178807675711,107.131249999582,5.90808986649102));
#275613=CARTESIAN_POINT('Ctrl Pts',(10.0514428414941,107.281249999581,3.2659117547607));
#275614=CARTESIAN_POINT('Ctrl Pts',(10.0514428414941,107.431249999581,-1.23094673026484E-15));
#275615=CARTESIAN_POINT('Origin',(-3.77475828372553E-14,-1.881249999982,
2.68644078414671E-15));
#275616=CARTESIAN_POINT('',(10.0514428414941,101.431249999605,1.02661856984785E-15));
#275617=CARTESIAN_POINT('',(10.0514428414941,101.806249999603,1.0250618530274E-15));
#275618=CARTESIAN_POINT('',(10.0514428414941,-1.881249999982,4.14193483802857E-15));
#275619=CARTESIAN_POINT('Ctrl Pts',(10.0514428414941,101.806249999603,-1.23094673026484E-15));
#275620=CARTESIAN_POINT('Ctrl Pts',(10.0514428414941,101.956249999603,-3.26591175476071));
#275621=CARTESIAN_POINT('Ctrl Pts',(8.13178807675712,102.106249999602,-5.90808986649102));
#275622=CARTESIAN_POINT('Ctrl Pts',(6.21213331202014,102.256249999601,-8.55026797822134));
#275623=CARTESIAN_POINT('Ctrl Pts',(3.10606665601004,102.406249999601,-9.5594902125713));
#275624=CARTESIAN_POINT('Ctrl Pts',(-7.21872317429903E-14,102.5562499996,
-10.5687124469213));
#275625=CARTESIAN_POINT('Ctrl Pts',(-3.10606665601018,102.7062499996,-9.5594902125713));
#275626=CARTESIAN_POINT('Ctrl Pts',(-6.21213331202029,102.856249999599,
-8.55026797822134));
#275627=CARTESIAN_POINT('Ctrl Pts',(-8.13178807675726,103.006249999598,
-5.90808986649102));
#275628=CARTESIAN_POINT('Ctrl Pts',(-10.0514428414942,103.156249999598,
-3.2659117547607));
#275629=CARTESIAN_POINT('Ctrl Pts',(-10.0514428414942,103.306249999597,
2.46189346052968E-15));
#275630=CARTESIAN_POINT('Ctrl Pts',(-10.0514428414942,103.456249999597,
3.26591175476071));
#275631=CARTESIAN_POINT('Ctrl Pts',(-8.13178807675726,103.606249999596,
5.90808986649102));
#275632=CARTESIAN_POINT('Ctrl Pts',(-6.21213331202029,103.756249999595,
8.55026797822134));
#275633=CARTESIAN_POINT('Ctrl Pts',(-3.10606665601018,103.906249999595,
9.5594902125713));
#275634=CARTESIAN_POINT('Ctrl Pts',(-7.0462498404975E-14,104.056249999594,
10.5687124469213));
#275635=CARTESIAN_POINT('Ctrl Pts',(3.10606665601004,104.206249999594,9.5594902125713));
#275636=CARTESIAN_POINT('Ctrl Pts',(6.21213331202014,104.356249999593,8.55026797822134));
#275637=CARTESIAN_POINT('Ctrl Pts',(8.13178807675712,104.506249999592,5.90808986649102));
#275638=CARTESIAN_POINT('Ctrl Pts',(10.0514428414941,104.656249999592,3.2659117547607));
#275639=CARTESIAN_POINT('Ctrl Pts',(10.0514428414941,104.806249999591,-1.23094673026484E-15));
#275640=CARTESIAN_POINT('Ctrl Pts',(10.0514428414941,101.431249999605,-1.23094673026484E-15));
#275641=CARTESIAN_POINT('Ctrl Pts',(10.0514428414941,101.581249999604,-3.26591175476071));
#275642=CARTESIAN_POINT('Ctrl Pts',(8.13178807675712,101.731249999604,-5.90808986649102));
#275643=CARTESIAN_POINT('Ctrl Pts',(6.21213331202014,101.881249999603,-8.55026797822134));
#275644=CARTESIAN_POINT('Ctrl Pts',(3.10606665601004,102.031249999602,-9.5594902125713));
#275645=CARTESIAN_POINT('Ctrl Pts',(-7.19712680840326E-14,102.181249999602,
-10.5687124469213));
#275646=CARTESIAN_POINT('Ctrl Pts',(-3.10606665601018,102.331249999601,
-9.5594902125713));
#275647=CARTESIAN_POINT('Ctrl Pts',(-6.21213331202029,102.481249999601,
-8.55026797822134));
#275648=CARTESIAN_POINT('Ctrl Pts',(-8.13178807675726,102.6312499996,-5.90808986649102));
#275649=CARTESIAN_POINT('Ctrl Pts',(-10.0514428414942,102.781249999599,
-3.2659117547607));
#275650=CARTESIAN_POINT('Ctrl Pts',(-10.0514428414942,102.931249999599,
2.46189346052968E-15));
#275651=CARTESIAN_POINT('Ctrl Pts',(-10.0514428414942,103.081249999598,
3.26591175476071));
#275652=CARTESIAN_POINT('Ctrl Pts',(-8.13178807675726,103.231249999598,
5.90808986649102));
#275653=CARTESIAN_POINT('Ctrl Pts',(-6.21213331202029,103.381249999597,
8.55026797822134));
#275654=CARTESIAN_POINT('Ctrl Pts',(-3.10606665601018,103.531249999596,
9.5594902125713));
#275655=CARTESIAN_POINT('Ctrl Pts',(-7.02465347460173E-14,103.681249999596,
10.5687124469213));
#275656=CARTESIAN_POINT('Ctrl Pts',(3.10606665601004,103.831249999595,9.5594902125713));
#275657=CARTESIAN_POINT('Ctrl Pts',(6.21213331202014,103.981249999595,8.55026797822134));
#275658=CARTESIAN_POINT('Ctrl Pts',(8.13178807675712,104.131249999594,5.90808986649102));
#275659=CARTESIAN_POINT('Ctrl Pts',(10.0514428414941,104.281249999593,3.2659117547607));
#275660=CARTESIAN_POINT('Ctrl Pts',(10.0514428414941,104.431249999593,-1.23094673026484E-15));
#275661=CARTESIAN_POINT('Origin',(-3.77475828372553E-14,-1.881249999982,
2.68644078414671E-15));
#275662=CARTESIAN_POINT('',(10.0514428414941,98.4312499996168,1.03907230441145E-15));
#275663=CARTESIAN_POINT('',(10.0514428414941,98.8062499996153,1.037515587591E-15));
#275664=CARTESIAN_POINT('',(10.0514428414941,-1.881249999982,4.14193483802857E-15));
#275665=CARTESIAN_POINT('Ctrl Pts',(10.0514428414941,98.8062499996153,-1.23094673026484E-15));
#275666=CARTESIAN_POINT('Ctrl Pts',(10.0514428414941,98.9562499996147,-3.26591175476071));
#275667=CARTESIAN_POINT('Ctrl Pts',(8.13178807675712,99.1062499996141,-5.90808986649102));
#275668=CARTESIAN_POINT('Ctrl Pts',(6.21213331202014,99.2562499996134,-8.55026797822134));
#275669=CARTESIAN_POINT('Ctrl Pts',(3.10606665601004,99.4062499996129,-9.5594902125713));
#275670=CARTESIAN_POINT('Ctrl Pts',(-7.04595224713285E-14,99.5562499996122,
-10.5687124469213));
#275671=CARTESIAN_POINT('Ctrl Pts',(-3.10606665601018,99.7062499996117,
-9.5594902125713));
#275672=CARTESIAN_POINT('Ctrl Pts',(-6.21213331202029,99.856249999611,-8.55026797822134));
#275673=CARTESIAN_POINT('Ctrl Pts',(-8.13178807675726,100.00624999961,-5.90808986649102));
#275674=CARTESIAN_POINT('Ctrl Pts',(-10.0514428414942,100.15624999961,-3.2659117547607));
#275675=CARTESIAN_POINT('Ctrl Pts',(-10.0514428414942,100.306249999609,
2.46189346052968E-15));
#275676=CARTESIAN_POINT('Ctrl Pts',(-10.0514428414942,100.456249999609,
3.26591175476071));
#275677=CARTESIAN_POINT('Ctrl Pts',(-8.13178807675726,100.606249999608,
5.90808986649102));
#275678=CARTESIAN_POINT('Ctrl Pts',(-6.21213331202028,100.756249999607,
8.55026797822134));
#275679=CARTESIAN_POINT('Ctrl Pts',(-3.10606665601018,100.906249999607,
9.5594902125713));
#275680=CARTESIAN_POINT('Ctrl Pts',(-6.87347891333132E-14,101.056249999606,
10.5687124469213));
#275681=CARTESIAN_POINT('Ctrl Pts',(3.10606665601004,101.206249999606,9.5594902125713));
#275682=CARTESIAN_POINT('Ctrl Pts',(6.21213331202015,101.356249999605,8.55026797822134));
#275683=CARTESIAN_POINT('Ctrl Pts',(8.13178807675712,101.506249999604,5.90808986649102));
#275684=CARTESIAN_POINT('Ctrl Pts',(10.0514428414941,101.656249999604,3.2659117547607));
#275685=CARTESIAN_POINT('Ctrl Pts',(10.0514428414941,101.806249999603,-1.23094673026484E-15));
#275686=CARTESIAN_POINT('Ctrl Pts',(10.0514428414941,98.4312499996168,-1.23094673026484E-15));
#275687=CARTESIAN_POINT('Ctrl Pts',(10.0514428414941,98.5812499996162,-3.26591175476071));
#275688=CARTESIAN_POINT('Ctrl Pts',(8.13178807675712,98.7312499996156,-5.90808986649102));
#275689=CARTESIAN_POINT('Ctrl Pts',(6.21213331202014,98.8812499996149,-8.55026797822134));
#275690=CARTESIAN_POINT('Ctrl Pts',(3.10606665601004,99.0312499996143,-9.5594902125713));
#275691=CARTESIAN_POINT('Ctrl Pts',(-7.02435588123707E-14,99.1812499996138,
-10.5687124469213));
#275692=CARTESIAN_POINT('Ctrl Pts',(-3.10606665601018,99.3312499996131,
-9.5594902125713));
#275693=CARTESIAN_POINT('Ctrl Pts',(-6.21213331202029,99.4812499996125,
-8.55026797822134));
#275694=CARTESIAN_POINT('Ctrl Pts',(-8.13178807675726,99.631249999612,-5.90808986649102));
#275695=CARTESIAN_POINT('Ctrl Pts',(-10.0514428414942,99.7812499996114,
-3.2659117547607));
#275696=CARTESIAN_POINT('Ctrl Pts',(-10.0514428414942,99.9312499996108,
2.46189346052968E-15));
#275697=CARTESIAN_POINT('Ctrl Pts',(-10.0514428414942,100.08124999961,3.26591175476071));
#275698=CARTESIAN_POINT('Ctrl Pts',(-8.13178807675726,100.23124999961,5.90808986649102));
#275699=CARTESIAN_POINT('Ctrl Pts',(-6.21213331202028,100.381249999609,
8.55026797822134));
#275700=CARTESIAN_POINT('Ctrl Pts',(-3.10606665601018,100.531249999608,
9.5594902125713));
#275701=CARTESIAN_POINT('Ctrl Pts',(-6.85188254743555E-14,100.681249999608,
10.5687124469213));
#275702=CARTESIAN_POINT('Ctrl Pts',(3.10606665601004,100.831249999607,9.5594902125713));
#275703=CARTESIAN_POINT('Ctrl Pts',(6.21213331202015,100.981249999607,8.55026797822134));
#275704=CARTESIAN_POINT('Ctrl Pts',(8.13178807675712,101.131249999606,5.90808986649102));
#275705=CARTESIAN_POINT('Ctrl Pts',(10.0514428414941,101.281249999605,3.2659117547607));
#275706=CARTESIAN_POINT('Ctrl Pts',(10.0514428414941,101.431249999605,-1.23094673026484E-15));
#275707=CARTESIAN_POINT('Origin',(-3.77475828372553E-14,-1.881249999982,
2.68644078414671E-15));
#275708=CARTESIAN_POINT('',(10.0514428414941,95.4312499996288,1.05152603897505E-15));
#275709=CARTESIAN_POINT('',(10.0514428414941,95.8062499996273,1.0499693221546E-15));
#275710=CARTESIAN_POINT('',(10.0514428414941,-1.881249999982,4.14193483802857E-15));
#275711=CARTESIAN_POINT('',(-5.07904231626403,94.4290259085059,8.67380149331447));
#275712=CARTESIAN_POINT('Ctrl Pts',(-5.07904231626403,94.4290259085059,
8.67380149331447));
#275713=CARTESIAN_POINT('Ctrl Pts',(-4.14047348819779,94.4812958157686,
9.22339105887566));
#275714=CARTESIAN_POINT('Ctrl Pts',(-3.10606665601017,94.5312499996324,
9.5594902125713));
#275715=CARTESIAN_POINT('Ctrl Pts',(-6.50634069310318E-14,94.6812499996317,
10.5687124469213));
#275716=CARTESIAN_POINT('Ctrl Pts',(3.10606665601004,94.8312499996312,9.5594902125713));
#275717=CARTESIAN_POINT('Ctrl Pts',(6.21213331202015,94.9812499996305,8.55026797822134));
#275718=CARTESIAN_POINT('Ctrl Pts',(8.13178807675712,95.13124999963,5.90808986649102));
#275719=CARTESIAN_POINT('Ctrl Pts',(10.0514428414941,95.2812499996293,3.2659117547607));
#275720=CARTESIAN_POINT('Ctrl Pts',(10.0514428414941,95.4312499996288,-1.23094673026484E-15));
#275721=CARTESIAN_POINT('',(-9.71864656122976,94.4290259085058,2.56503649364343));
#275722=CARTESIAN_POINT('Origin',(1.17683640610267E-13,94.4290259085057,
-1.79301018476963E-13));
#275723=CARTESIAN_POINT('Ctrl Pts',(-9.71864656122976,94.4290259085058,
2.56503649364343));
#275724=CARTESIAN_POINT('Ctrl Pts',(-9.23826308175394,94.5197910936883,
4.38515767416034));
#275725=CARTESIAN_POINT('Ctrl Pts',(-8.13178807675726,94.606249999632,5.90808986649102));
#275726=CARTESIAN_POINT('Ctrl Pts',(-6.21213331202028,94.7562499996315,
8.55026797822134));
#275727=CARTESIAN_POINT('Ctrl Pts',(-3.10606665601017,94.9062499996309,
9.5594902125713));
#275728=CARTESIAN_POINT('Ctrl Pts',(-6.52793705899895E-14,95.0562499996302,
10.5687124469213));
#275729=CARTESIAN_POINT('Ctrl Pts',(3.10606665601004,95.2062499996296,9.5594902125713));
#275730=CARTESIAN_POINT('Ctrl Pts',(6.21213331202015,95.3562499996291,8.55026797822134));
#275731=CARTESIAN_POINT('Ctrl Pts',(8.13178807675712,95.5062499996285,5.90808986649102));
#275732=CARTESIAN_POINT('Ctrl Pts',(10.0514428414941,95.6562499996278,3.2659117547607));
#275733=CARTESIAN_POINT('Ctrl Pts',(10.0514428414941,95.8062499996273,-1.23094673026484E-15));
#275734=CARTESIAN_POINT('Origin',(-7.54701734185159E-14,109.38046875,0.));
#275735=CARTESIAN_POINT('',(10.9371370246358,108.317605774636,-5.59181276817946E-13));
#275736=CARTESIAN_POINT('',(11.9999999999999,109.38046875,-1.46957615897682E-15));
#275737=CARTESIAN_POINT('Ctrl Pts',(7.10339095492142,107.431911591495,7.11149352368269));
#275738=CARTESIAN_POINT('Ctrl Pts',(8.21640283011763,107.591475283561,6.22527839381925));
#275739=CARTESIAN_POINT('Ctrl Pts',(8.97013365125207,107.719075998133,5.23075558842423));
#275740=CARTESIAN_POINT('Ctrl Pts',(10.1564570384933,107.968118058239,3.26634758870711));
#275741=CARTESIAN_POINT('Ctrl Pts',(10.6203336593551,108.110353403587,2.01694121932577));
#275742=CARTESIAN_POINT('Ctrl Pts',(10.8812264225221,108.269539083346,0.477180535167351));
#275743=CARTESIAN_POINT('Ctrl Pts',(10.9132812486255,108.293749998626,0.238870532520754));
#275744=CARTESIAN_POINT('Ctrl Pts',(10.9371370246358,108.317605774636,-1.22700460902792E-12));
#275745=CARTESIAN_POINT('Origin',(-6.51327129430312E-14,91.43046875,0.));
#275746=CARTESIAN_POINT('',(-10.1292796487468,94.3511891012534,-1.41514480213812E-13));
#275747=CARTESIAN_POINT('',(-11.2291932872669,93.2512754627332,4.26135578759189E-11));
#275748=CARTESIAN_POINT('',(-13.0500000000001,91.43046875,-1.5981640728873E-15));
#275749=CARTESIAN_POINT('Ctrl Pts',(-10.1292796487468,94.3511891012534,
-3.42503803096861E-13));
#275750=CARTESIAN_POINT('Ctrl Pts',(-10.1042382905,94.3762304595001,0.866661225011173));
#275751=CARTESIAN_POINT('Ctrl Pts',(-9.96696795140311,94.4023681640516,
1.72863551637103));
#275752=CARTESIAN_POINT('Ctrl Pts',(-9.71864656122976,94.4290259085059,
2.56503649364344));
#275753=CARTESIAN_POINT('Ctrl Pts',(-5.07904231626394,94.4290259085059,
8.67380149331451));
#275754=CARTESIAN_POINT('Ctrl Pts',(-5.69337143249224,94.3531311547402,
8.40202310412634));
#275755=CARTESIAN_POINT('Ctrl Pts',(-6.27907719474524,94.2775482324335,
8.06962005777155));
#275756=CARTESIAN_POINT('Ctrl Pts',(-7.39904906850036,94.1258950262357,
7.27704780513819));
#275757=CARTESIAN_POINT('Ctrl Pts',(-7.92712996465539,94.0503398117793,
6.81422983223111));
#275758=CARTESIAN_POINT('Ctrl Pts',(-9.07535528122801,93.8747927058122,
5.57538689591588));
#275759=CARTESIAN_POINT('Ctrl Pts',(-9.97387089070914,93.7211313789459,
4.40428884548453));
#275760=CARTESIAN_POINT('Ctrl Pts',(-10.9571199054006,93.4285476733796,
1.7735086098561));
#275761=CARTESIAN_POINT('Ctrl Pts',(-11.1468677668107,93.3336009831894,
0.846346921087316));
#275762=CARTESIAN_POINT('Ctrl Pts',(-11.2291932872669,93.2512754627332,
8.5342589378412E-11));
#275763=CARTESIAN_POINT('Origin',(-8.79029313101884E-14,130.96875,0.));
#275764=CARTESIAN_POINT('',(-12.0000000000001,92.80624999964,-1.44737980092247E-14));
#275765=CARTESIAN_POINT('',(-12.0000000000001,92.4804687499999,-1.46957615897682E-15));
#275766=CARTESIAN_POINT('',(-12.0000000000001,130.96875,-1.46957615897682E-15));
#275767=CARTESIAN_POINT('',(-9.3029332573012,92.4804687499999,-7.57993620093208));
#275768=CARTESIAN_POINT('Origin',(-6.57374111881153E-14,92.48046875,0.));
#275769=CARTESIAN_POINT('Ctrl Pts',(-9.3029332573012,92.4804687499999,-7.57993620093207));
#275770=CARTESIAN_POINT('Ctrl Pts',(-9.96781199016407,92.5216290384817,
-6.76392372905115));
#275771=CARTESIAN_POINT('Ctrl Pts',(-10.5224449433889,92.5621874194225,
-5.86397241395083));
#275772=CARTESIAN_POINT('Ctrl Pts',(-11.3879370382823,92.6473816274152,
-3.93068574796497));
#275773=CARTESIAN_POINT('Ctrl Pts',(-11.6918564422266,92.6906603937711,
-2.90446525895254));
#275774=CARTESIAN_POINT('Ctrl Pts',(-11.9521621005444,92.7580357386561,
-1.23771756688517));
#275775=CARTESIAN_POINT('Ctrl Pts',(-12.0000000000001,92.7824500276289,
-0.618646374098709));
#275776=CARTESIAN_POINT('Ctrl Pts',(-12.0000000000001,92.80624999964,-1.40165656858926E-14));
#275777=CARTESIAN_POINT('Origin',(-8.79029313101884E-14,130.96875,0.));
#275778=CARTESIAN_POINT('',(-12.0000000000001,95.806249999628,1.5016501082381E-14));
#275779=CARTESIAN_POINT('',(-12.0000000000001,95.431249999628,6.34288370249696E-15));
#275780=CARTESIAN_POINT('',(-12.0000000000001,130.96875,-1.46957615897682E-15));
#275781=CARTESIAN_POINT('',(-11.9338891906744,92.48046875,1.25789060919729));
#275782=CARTESIAN_POINT('Ctrl Pts',(-12.0000000000001,95.431249999628,-1.94289029309402E-15));
#275783=CARTESIAN_POINT('Ctrl Pts',(-12.0000000000001,95.3976641187748,
-0.873017136364969));
#275784=CARTESIAN_POINT('Ctrl Pts',(-11.9047347890664,95.3629119207413,
-1.74539748324885));
#275785=CARTESIAN_POINT('Ctrl Pts',(-11.3767138011809,95.2648407604998,
-4.12305319186097));
#275786=CARTESIAN_POINT('Ctrl Pts',(-10.7455985797956,95.2015050546979,
-5.56431288903644));
#275787=CARTESIAN_POINT('Ctrl Pts',(-8.95241664100026,95.0797473280993,
-8.14659144143737));
#275788=CARTESIAN_POINT('Ctrl Pts',(-7.79912443701758,95.0163880159116,
-9.25672200041033));
#275789=CARTESIAN_POINT('Ctrl Pts',(-5.16054929757683,94.8899343416185,
-10.9434853481133));
#275790=CARTESIAN_POINT('Ctrl Pts',(-3.70891226333863,94.8312786522147,
-11.5167337635027));
#275791=CARTESIAN_POINT('Ctrl Pts',(-0.642921654553635,94.7072567268602,
-12.0854313202532));
#275792=CARTESIAN_POINT('Ctrl Pts',(0.944038589215958,94.6430628365301,
-12.065646538642));
#275793=CARTESIAN_POINT('Ctrl Pts',(4.01115415839253,94.5189954055718,-11.4172439533036));
#275794=CARTESIAN_POINT('Ctrl Pts',(5.46251131982209,94.4592323691957,-10.7983224510908));
#275795=CARTESIAN_POINT('Ctrl Pts',(8.03555543718115,94.3333675962428,-9.04613168988572));
#275796=CARTESIAN_POINT('Ctrl Pts',(9.13561348468754,94.2722709092646,-7.93365723288517));
#275797=CARTESIAN_POINT('Ctrl Pts',(10.8714801211651,94.1501067125908,-5.32219019919355));
#275798=CARTESIAN_POINT('Ctrl Pts',(11.478882329683,94.0855139334344,-3.84054984568375));
#275799=CARTESIAN_POINT('Ctrl Pts',(12.075644253326,93.9596281460411,-0.762227804634905));
#275800=CARTESIAN_POINT('Ctrl Pts',(12.073058682881,93.9013041019789,0.802139162615167));
#275801=CARTESIAN_POINT('Ctrl Pts',(11.470686639618,93.7763142357512,3.85535017066264));
#275802=CARTESIAN_POINT('Ctrl Pts',(10.8719169399683,93.7127014512904,5.31432183002772));
#275803=CARTESIAN_POINT('Ctrl Pts',(9.14006629815543,93.590267568913,7.93410383523557));
#275804=CARTESIAN_POINT('Ctrl Pts',(8.01845603372403,93.5280963364804,9.06617177346286));
#275805=CARTESIAN_POINT('Ctrl Pts',(5.42793703261786,93.4017787800147,10.8133538109976));
#275806=CARTESIAN_POINT('Ctrl Pts',(3.99082685614984,93.342682337048,11.4221031877892));
#275807=CARTESIAN_POINT('Ctrl Pts',(0.936043788692094,93.2191137662634,
12.0667624748179));
#275808=CARTESIAN_POINT('Ctrl Pts',(-0.654821989464978,93.1547618937488,
12.0852847774843));
#275809=CARTESIAN_POINT('Ctrl Pts',(-3.73563892343538,93.0301402309423,
11.5097179367768));
#275810=CARTESIAN_POINT('Ctrl Pts',(-5.19718729288481,92.9709947981446,
10.9278452452945));
#275811=CARTESIAN_POINT('Ctrl Pts',(-7.81137968310086,92.8453341046328,
9.24087349583016));
#275812=CARTESIAN_POINT('Ctrl Pts',(-8.94033127393691,92.7831736812992,
8.15360822633876));
#275813=CARTESIAN_POINT('Ctrl Pts',(-10.4099330659214,92.6840372314516,
6.05419998055747));
#275814=CARTESIAN_POINT('Ctrl Pts',(-10.8823321061612,92.6436164194797,
5.15701029741631));
#275815=CARTESIAN_POINT('Ctrl Pts',(-11.5931709912404,92.5617640622437,
3.26034040809238));
#275816=CARTESIAN_POINT('Ctrl Pts',(-11.8274267264064,92.5206565619121,
2.26792378875226));
#275817=CARTESIAN_POINT('Ctrl Pts',(-11.9338891906744,92.48046875,1.25789060919715));
#275818=CARTESIAN_POINT('Origin',(-6.57374111881153E-14,92.48046875,0.));
#275819=CARTESIAN_POINT('Ctrl Pts',(-12.0000000000001,92.80624999964,9.15933995315754E-15));
#275820=CARTESIAN_POINT('Ctrl Pts',(-12.0000000000001,92.8417057528578,
0.921621805222653));
#275821=CARTESIAN_POINT('Ctrl Pts',(-11.8938313654259,92.8784483916136,
1.84219808659633));
#275822=CARTESIAN_POINT('Ctrl Pts',(-11.318208857505,92.9799433628676,4.29338421451095));
#275823=CARTESIAN_POINT('Ctrl Pts',(-10.6493327544983,93.0445577132886,
5.7556112031982));
#275824=CARTESIAN_POINT('Ctrl Pts',(-8.80169039827924,93.165673838157,8.30351697017158));
#275825=CARTESIAN_POINT('Ctrl Pts',(-7.65266103423919,93.2286729874806,
9.37313682937302));
#275826=CARTESIAN_POINT('Ctrl Pts',(-5.01001216616424,93.3541810897256,
11.0145238390819));
#275827=CARTESIAN_POINT('Ctrl Pts',(-3.54148403116243,93.4129939613117,
11.5705616108616));
#275828=CARTESIAN_POINT('Ctrl Pts',(-0.451643875509239,93.5379806211025,
12.0949290217605));
#275829=CARTESIAN_POINT('Ctrl Pts',(1.14142505877038,93.6024216131544,12.0494200828072));
#275830=CARTESIAN_POINT('Ctrl Pts',(4.18767675127626,93.7256450825729,11.3514703820219));
#275831=CARTESIAN_POINT('Ctrl Pts',(5.61447034546205,93.7851561667958,10.7177546608328));
#275832=CARTESIAN_POINT('Ctrl Pts',(8.17091909548136,93.9113660883478,8.92820590750656));
#275833=CARTESIAN_POINT('Ctrl Pts',(9.27013306719489,93.9727901849844,7.78082540002013));
#275834=CARTESIAN_POINT('Ctrl Pts',(10.9581556951928,94.0956813091259,5.1349174614681));
#275835=CARTESIAN_POINT('Ctrl Pts',(11.5336481270458,94.1594708447873,3.66378816360723));
#275836=CARTESIAN_POINT('Ctrl Pts',(12.0846225089599,94.2842356801235,0.599726400558802));
#275837=CARTESIAN_POINT('Ctrl Pts',(12.0611102430209,94.3425338274646,-0.963002346951906));
#275838=CARTESIAN_POINT('Ctrl Pts',(11.4133145370304,94.4687101029181,-4.03229333032655));
#275839=CARTESIAN_POINT('Ctrl Pts',(10.7799275253742,94.5333243696182,-5.50604924758921));
#275840=CARTESIAN_POINT('Ctrl Pts',(8.99681676547324,94.6550618151086,-8.09107294585621));
#275841=CARTESIAN_POINT('Ctrl Pts',(7.87614575620454,94.7169000396803,-9.18558476524078));
#275842=CARTESIAN_POINT('Ctrl Pts',(5.27372199527324,94.8426210955086,-10.8912933911025));
#275843=CARTESIAN_POINT('Ctrl Pts',(3.8150761730276,94.9019269266909,-11.4837995702507));
#275844=CARTESIAN_POINT('Ctrl Pts',(0.738100769421628,95.02639319633,-12.0803427809247));
#275845=CARTESIAN_POINT('Ctrl Pts',(-0.851733171522372,95.0907033301526,
-12.0728637452725));
#275846=CARTESIAN_POINT('Ctrl Pts',(-3.90985616165455,95.2144070036474,
-11.4500627845247));
#275847=CARTESIAN_POINT('Ctrl Pts',(-5.35116761717258,95.2733585740668,
-10.8515384694098));
#275848=CARTESIAN_POINT('Ctrl Pts',(-7.95557556476879,95.3997173981778,
-9.12173727191776));
#275849=CARTESIAN_POINT('Ctrl Pts',(-9.08633141264699,95.4622159086525,
-7.99596787439197));
#275850=CARTESIAN_POINT('Ctrl Pts',(-10.8359666341656,95.5844581215649,
-5.38694660416549));
#275851=CARTESIAN_POINT('Ctrl Pts',(-11.4441438879658,95.647994145039,-3.93302693695522));
#275852=CARTESIAN_POINT('Ctrl Pts',(-11.9189061176973,95.7432696367485,
-1.61073583043876));
#275853=CARTESIAN_POINT('Ctrl Pts',(-12.0000000000001,95.7752626448447,
-0.805472152264365));
#275854=CARTESIAN_POINT('Ctrl Pts',(-12.0000000000001,95.806249999628,-2.38697950294409E-14));
#275855=CARTESIAN_POINT('Origin',(-8.79029313101884E-14,130.96875,0.));
#275856=CARTESIAN_POINT('',(-12.0000000000001,98.806249999616,-2.88584518969965E-15));
#275857=CARTESIAN_POINT('',(-12.0000000000001,98.431249999616,6.19234238727939E-14));
#275858=CARTESIAN_POINT('',(-12.0000000000001,130.96875,-1.46957615897682E-15));
#275859=CARTESIAN_POINT('Ctrl Pts',(-12.0000000000001,98.431249999616,-3.44169137633799E-14));
#275860=CARTESIAN_POINT('Ctrl Pts',(-12.0000000000001,98.3903362637419,
-1.06349429056132));
#275861=CARTESIAN_POINT('Ctrl Pts',(-11.858626067169,98.3477542696158,-2.12441740297027));
#275862=CARTESIAN_POINT('Ctrl Pts',(-11.1699243170239,98.2419053899608,
-4.65203550545811));
#275863=CARTESIAN_POINT('Ctrl Pts',(-10.475302824406,98.1800666739711,-6.05608851369005));
#275864=CARTESIAN_POINT('Ctrl Pts',(-8.56783571805061,98.0583295023047,
-8.55076676634347));
#275865=CARTESIAN_POINT('Ctrl Pts',(-7.36194773443014,97.9937152278146,
-9.6085830985033));
#275866=CARTESIAN_POINT('Ctrl Pts',(-4.64307379929293,97.867538776801,-11.1731650433297));
#275867=CARTESIAN_POINT('Ctrl Pts',(-3.16410215805437,97.8092406205087,
-11.6784514411006));
#275868=CARTESIAN_POINT('Ctrl Pts',(-0.0797494407164467,97.6844759322606,
-12.1013233929251));
#275869=CARTESIAN_POINT('Ctrl Pts',(1.49721720145038,97.620686291607,-12.0086177058656));
#275870=CARTESIAN_POINT('Ctrl Pts',(4.53525976859494,97.4977948882848,-11.2208743559025));
#275871=CARTESIAN_POINT('Ctrl Pts',(5.96616398510963,97.4363712324694,-10.5300360074582));
#275872=CARTESIAN_POINT('Ctrl Pts',(8.45813053307474,97.3101613807666,-8.6517380547846));
#275873=CARTESIAN_POINT('Ctrl Pts',(9.50174622702573,97.2506500121776,-7.49061654751233));
#275874=CARTESIAN_POINT('Ctrl Pts',(11.1069091342363,97.1274267637706,-4.80915275641748));
#275875=CARTESIAN_POINT('Ctrl Pts',(11.6424924087258,97.0629857220061,-3.30812121405916));
#275876=CARTESIAN_POINT('Ctrl Pts',(12.0986344003864,96.9379988418735,-0.2074748013541));
#275877=CARTESIAN_POINT('Ctrl Pts',(12.0236277365977,96.8791861509043,1.36100270980834));
#275878=CARTESIAN_POINT('Ctrl Pts',(11.2792316172137,96.7536781456885,4.38153558319533));
#275879=CARTESIAN_POINT('Ctrl Pts',(10.617046518114,96.69067845295,5.80486658217108));
#275880=CARTESIAN_POINT('Ctrl Pts',(8.76482133190042,96.5695626085286,8.34944672988));
#275881=CARTESIAN_POINT('Ctrl Pts',(7.58086464519092,96.5049482655075,9.43745178491119));
#275882=CARTESIAN_POINT('Ctrl Pts',(4.89611881243507,96.3784052508018,11.0644241478338));
#275883=CARTESIAN_POINT('Ctrl Pts',(3.43039307442459,96.3200123143542,11.6028404232851));
#275884=CARTESIAN_POINT('Ctrl Pts',(0.354478117635857,96.19558894069,12.0968472765385));
#275885=CARTESIAN_POINT('Ctrl Pts',(-1.22777108824699,96.1315856158455,
12.0396035186058));
#275886=CARTESIAN_POINT('Ctrl Pts',(-4.2804515265945,96.0081020981951,11.3197518587139));
#275887=CARTESIAN_POINT('Ctrl Pts',(-5.72148749750293,95.9475666604573,
10.6641304978391));
#275888=CARTESIAN_POINT('Ctrl Pts',(-8.25336177812795,95.821517205652,8.84750687802869));
#275889=CARTESIAN_POINT('Ctrl Pts',(-9.32467774413927,95.7613095515572,
7.71016305346253));
#275890=CARTESIAN_POINT('Ctrl Pts',(-10.994220774471,95.6385858189331,5.06260183372988));
#275891=CARTESIAN_POINT('Ctrl Pts',(-11.5651597717373,95.5740532770615,
3.57067964711787));
#275892=CARTESIAN_POINT('Ctrl Pts',(-11.9434861476433,95.4837054996373,
1.34514354656573));
#275893=CARTESIAN_POINT('Ctrl Pts',(-12.0000000000001,95.4571183235931,
0.672410237188394));
#275894=CARTESIAN_POINT('Ctrl Pts',(-12.0000000000001,95.431249999628,8.88178419700125E-15));
#275895=CARTESIAN_POINT('Ctrl Pts',(-12.0000000000001,95.806249999628,-6.78623823802127E-14));
#275896=CARTESIAN_POINT('Ctrl Pts',(-12.0000000000001,95.8346404553987,
0.737969461197185));
#275897=CARTESIAN_POINT('Ctrl Pts',(-11.9319288660828,95.8638859980307,
1.47604803529853));
#275898=CARTESIAN_POINT('Ctrl Pts',(-11.5045591024659,95.9571893719954,
3.76247549562259));
#275899=CARTESIAN_POINT('Ctrl Pts',(-10.9077188258606,96.021768297912,5.24718753360586));
#275900=CARTESIAN_POINT('Ctrl Pts',(-9.19105849417976,96.1440992565816,
7.8692298145771));
#275901=CARTESIAN_POINT('Ctrl Pts',(-8.09934644811893,96.2049203555293,
8.98894674875177));
#275902=CARTESIAN_POINT('Ctrl Pts',(-5.53823235938179,96.3308406503862,
10.7598929530529));
#275903=CARTESIAN_POINT('Ctrl Pts',(-4.08985281277005,96.3908119781246,
11.3894873386763));
#275904=CARTESIAN_POINT('Ctrl Pts',(-1.02684768862722,96.5147131380885,
12.0587411242401));
#275905=CARTESIAN_POINT('Ctrl Pts',(0.558827698358478,96.5788550548699,
12.0894709642923));
#275906=CARTESIAN_POINT('Ctrl Pts',(3.62782455931501,96.7029985856793,11.5425525780104));
#275907=CARTESIAN_POINT('Ctrl Pts',(5.0835892948793,96.7615602696415,10.979467360577));
#275908=CARTESIAN_POINT('Ctrl Pts',(7.73583477131505,96.88804916169,9.31003841198302));
#275909=CARTESIAN_POINT('Ctrl Pts',(8.89815879494356,96.9517749723513,8.20622415256473));
#275910=CARTESIAN_POINT('Ctrl Pts',(10.7086824081936,97.0733336918042,5.63475315906449));
#275911=CARTESIAN_POINT('Ctrl Pts',(11.3488925173778,97.1365847129197,4.19864982787631));
#275912=CARTESIAN_POINT('Ctrl Pts',(12.0437715610302,97.2619262188028,1.16635579429267));
#275913=CARTESIAN_POINT('Ctrl Pts',(12.0934795422874,97.3204991868119,-0.40076067034903));
#275914=CARTESIAN_POINT('Ctrl Pts',(11.588393733587,97.4458152708407,-3.49406145928547));
#275915=CARTESIAN_POINT('Ctrl Pts',(11.0277840731536,97.5103244286932,-4.98873201661399));
#275916=CARTESIAN_POINT('Ctrl Pts',(9.37704085620864,97.6331984422303,-7.64630800428874));
#275917=CARTESIAN_POINT('Ctrl Pts',(8.31383312200354,97.693185951036,-8.79063100717509));
#275918=CARTESIAN_POINT('Ctrl Pts',(5.79361671391148,97.8192841593186,-10.6253508095566));
#275919=CARTESIAN_POINT('Ctrl Pts',(4.35552718395247,97.8800652240558,-11.2912965327819));
#275920=CARTESIAN_POINT('Ctrl Pts',(1.30705920366105,98.0033783441985,-12.0311201834856));
#275921=CARTESIAN_POINT('Ctrl Pts',(-0.273717490831138,98.067322104706,
-12.0988102824553));
#275922=CARTESIAN_POINT('Ctrl Pts',(-3.35221551586651,98.1918499656757,
-11.6257129109516));
#275923=CARTESIAN_POINT('Ctrl Pts',(-4.82185190647142,98.2501993887458,
-11.0970382348483));
#275924=CARTESIAN_POINT('Ctrl Pts',(-7.51674502260938,98.3766381746483,
-9.48841611527849));
#275925=CARTESIAN_POINT('Ctrl Pts',(-8.70724253525681,98.4412560350765,
-8.40926579798738));
#275926=CARTESIAN_POINT('Ctrl Pts',(-10.575840211191,98.5625593777037,-5.87933455790365));
#275927=CARTESIAN_POINT('Ctrl Pts',(-11.2476213291911,98.6251994919137,
-4.46168742808438));
#275928=CARTESIAN_POINT('Ctrl Pts',(-11.8763701518246,98.7282508017786,
-1.98730828071283));
#275929=CARTESIAN_POINT('Ctrl Pts',(-12.0000000000001,98.7679896997974,
-0.994521999591797));
#275930=CARTESIAN_POINT('Ctrl Pts',(-12.0000000000001,98.806249999616,1.22124532708767E-14));
#275931=CARTESIAN_POINT('Origin',(-8.79029313101884E-14,130.96875,0.));
#275932=CARTESIAN_POINT('',(-12.0000000000001,101.806249999604,1.21771383793994E-13));
#275933=CARTESIAN_POINT('',(-12.0000000000001,101.431249999604,9.59933929409784E-14));
#275934=CARTESIAN_POINT('',(-12.0000000000001,130.96875,-1.46957615897682E-15));
#275935=CARTESIAN_POINT('Ctrl Pts',(-12.0000000000001,101.431249999604,
4.35484981409218E-13));
#275936=CARTESIAN_POINT('Ctrl Pts',(-12.0000000000001,101.382732225158,
-1.26115044279506));
#275937=CARTESIAN_POINT('Ctrl Pts',(-11.8011858555912,101.3319584443,-2.51634392763927));
#275938=CARTESIAN_POINT('Ctrl Pts',(-10.9295576026251,101.218191084799,
-5.19035521167642));
#275939=CARTESIAN_POINT('Ctrl Pts',(-10.1698051033365,101.158203246843,
-6.55514968186482));
#275940=CARTESIAN_POINT('Ctrl Pts',(-8.15243145592084,101.03532946252,-8.94635876935562));
#275941=CARTESIAN_POINT('Ctrl Pts',(-6.90416210454257,100.970820266432,
-9.94142271432126));
#275942=CARTESIAN_POINT('Ctrl Pts',(-4.11835256299701,100.845503978089,
-11.3776985584927));
#275943=CARTESIAN_POINT('Ctrl Pts',(-2.61258144852507,100.786931139159,
-11.8147041098655));
#275944=CARTESIAN_POINT('Ctrl Pts',(0.48602831587838,100.661589741242,-12.090897530964));
#275945=CARTESIAN_POINT('Ctrl Pts',(2.04968283481498,100.598338587285,-11.9258176747727));
#275946=CARTESIAN_POINT('Ctrl Pts',(5.05478730302487,100.476779558053,-10.9985662576491));
#275947=CARTESIAN_POINT('Ctrl Pts',(6.46375991644632,100.413054323408,-10.2342440890019));
#275948=CARTESIAN_POINT('Ctrl Pts',(8.87108911775026,100.286565484546,-8.22771904423435));
#275949=CARTESIAN_POINT('Ctrl Pts',(9.85648401275463,100.228003666168,-7.01721833210744));
#275950=CARTESIAN_POINT('Ctrl Pts',(11.3250371392221,100.103860320699,-4.26745071991765));
#275951=CARTESIAN_POINT('Ctrl Pts',(11.785828698054,100.039718321178,-2.74989105323262));
#275952=CARTESIAN_POINT('Ctrl Pts',(12.0958838319189,99.9158169013089,0.370006863414581));
#275953=CARTESIAN_POINT('Ctrl Pts',(11.9446950421818,99.8558459067457,1.94205232576911));
#275954=CARTESIAN_POINT('Ctrl Pts',(11.0518862428444,99.7299256967796,4.92507767164746));
#275955=CARTESIAN_POINT('Ctrl Pts',(10.324344397283,99.6691041815619,6.30937792967838));
#275956=CARTESIAN_POINT('Ctrl Pts',(8.3611359667578,99.5467734787521,8.75229785457037));
#275957=CARTESIAN_POINT('Ctrl Pts',(7.13353424042131,99.4821945290531,9.77874207649069));
#275958=CARTESIAN_POINT('Ctrl Pts',(4.38054731532025,99.3564319089459,11.2789664160656));
#275959=CARTESIAN_POINT('Ctrl Pts',(2.88805958243837,99.2980744637605,11.7500374076434));
#275960=CARTESIAN_POINT('Ctrl Pts',(-0.203968503235057,99.1729993003413,
12.0994021381704));
#275961=CARTESIAN_POINT('Ctrl Pts',(-1.7746683838583,99.1094631555172,11.9702933860124));
#275962=CARTESIAN_POINT('Ctrl Pts',(-4.79666950094096,98.9872206424807,
11.1125547405502));
#275963=CARTESIAN_POINT('Ctrl Pts',(-6.21676753370284,98.9247226506023,
10.3850404492276));
#275964=CARTESIAN_POINT('Ctrl Pts',(-8.66673161054512,98.7983638894037,
8.4426681463036));
#275965=CARTESIAN_POINT('Ctrl Pts',(-9.68136490617877,98.7394121048799,
7.25686480030045));
#275966=CARTESIAN_POINT('Ctrl Pts',(-11.21872656147,98.6157086387229,4.54088847059025));
#275967=CARTESIAN_POINT('Ctrl Pts',(-11.717142100468,98.5513984376063,3.03118141519292));
#275968=CARTESIAN_POINT('Ctrl Pts',(-11.9700060674013,98.4693355863612,
0.980234962623068));
#275969=CARTESIAN_POINT('Ctrl Pts',(-12.0000000000001,98.4500953949073,
0.489859209079169));
#275970=CARTESIAN_POINT('Ctrl Pts',(-12.0000000000001,98.431249999616,-6.66133814775094E-15));
#275971=CARTESIAN_POINT('Ctrl Pts',(-12.0000000000001,98.806249999616,1.38777878078145E-16));
#275972=CARTESIAN_POINT('Ctrl Pts',(-12.0000000000001,98.8276233756076,
0.555570466773574));
#275973=CARTESIAN_POINT('Ctrl Pts',(-11.9614195863975,98.849498410001,1.11164529292389));
#275974=CARTESIAN_POINT('Ctrl Pts',(-11.6652978475081,98.9345505045725,
3.22623756605706));
#275975=CARTESIAN_POINT('Ctrl Pts',(-11.1407172499593,98.9989564945593,
4.72993297382568));
#275976=CARTESIAN_POINT('Ctrl Pts',(-9.55561030902574,99.1223266653623,
7.42173238181464));
#275977=CARTESIAN_POINT('Ctrl Pts',(-8.52058700319381,99.181654125327,8.5901921471054));
#275978=CARTESIAN_POINT('Ctrl Pts',(-6.04104625614187,99.3079101631137,
10.4875352643976));
#275979=CARTESIAN_POINT('Ctrl Pts',(-4.61332333281783,99.369637150774,11.1892657235087));
#275980=CARTESIAN_POINT('Ctrl Pts',(-1.57996080837295,99.4923392423923,
11.9978723487919));
#275981=CARTESIAN_POINT('Ctrl Pts',(-0.00477503949806751,99.5560568452079,
12.1014463532335));
#275982=CARTESIAN_POINT('Ctrl Pts',(3.08197465134809,99.6809184930712,11.700466524053));
#275983=CARTESIAN_POINT('Ctrl Pts',(4.56498990025355,99.739217703611,11.2053710962917));
#275984=CARTESIAN_POINT('Ctrl Pts',(7.29414460370894,99.8652745822897,9.65996844683288));
#275985=CARTESIAN_POINT('Ctrl Pts',(8.50659980384892,99.9298820381286,8.61147789493034));
#275986=CARTESIAN_POINT('Ctrl Pts',(10.4308090856514,100.051801075647,6.13219426693295));
#275987=CARTESIAN_POINT('Ctrl Pts',(11.1352964859028,100.113317690063,4.73404138995748));
#275988=CARTESIAN_POINT('Ctrl Pts',(11.9717301606602,100.23850541014,1.75173868711237));
#275989=CARTESIAN_POINT('Ctrl Pts',(12.0976219836414,100.297482843836,0.196170422008661));
#275990=CARTESIAN_POINT('Ctrl Pts',(11.7489890472703,100.421161649931,-2.90540627876741));
#275991=CARTESIAN_POINT('Ctrl Pts',(11.2667093682072,100.485479782146,-4.42056235048717));
#275992=CARTESIAN_POINT('Ctrl Pts',(9.75201543617218,100.60997523142,-7.16449034304141));
#275993=CARTESIAN_POINT('Ctrl Pts',(8.73947898856186,100.669250142572,-8.3697783466813));
#275994=CARTESIAN_POINT('Ctrl Pts',(6.31570132789617,100.794960060076,-10.320903774));
#275995=CARTESIAN_POINT('Ctrl Pts',(4.92925879702124,100.856857292785,-11.0503875663945));
#275996=CARTESIAN_POINT('Ctrl Pts',(1.92055461475842,100.978561933509,-11.9513820703781));
#275997=CARTESIAN_POINT('Ctrl Pts',(0.323180305856766,101.043177081623,
-12.1003857993283));
#275998=CARTESIAN_POINT('Ctrl Pts',(-2.79658640397,101.169374295959,-11.7718550594554));
#275999=CARTESIAN_POINT('Ctrl Pts',(-4.29057784217851,101.227673735964,
-11.3131971364897));
#276000=CARTESIAN_POINT('Ctrl Pts',(-7.03634923360482,101.352420926947,
-9.84574888144511));
#276001=CARTESIAN_POINT('Ctrl Pts',(-8.25902714011372,101.416222968348,
-8.84520319199907));
#276002=CARTESIAN_POINT('Ctrl Pts',(-10.2566560747344,101.539147416662,
-6.42468698789539));
#276003=CARTESIAN_POINT('Ctrl Pts',(-11.0097963852458,101.600519033734,
-5.02594677720654));
#276004=CARTESIAN_POINT('Ctrl Pts',(-11.8224652873435,101.712515064644,
-2.37882160259375));
#276005=CARTESIAN_POINT('Ctrl Pts',(-12.0000000000001,101.760401871696,
-1.19175678342724));
#276006=CARTESIAN_POINT('Ctrl Pts',(-12.0000000000001,101.806249999604,
4.51583215266282E-13));
#276007=CARTESIAN_POINT('Origin',(-8.79029313101884E-14,130.96875,0.));
#276008=CARTESIAN_POINT('',(-12.0000000000001,104.806249999592,9.27456637689777E-15));
#276009=CARTESIAN_POINT('',(-12.0000000000001,104.431249999592,6.316403021549E-16));
#276010=CARTESIAN_POINT('',(-12.0000000000001,130.96875,-1.46957615897682E-15));
#276011=CARTESIAN_POINT('Ctrl Pts',(-12.0000000000001,104.431249999592,
-1.60982338570648E-14));
#276012=CARTESIAN_POINT('Ctrl Pts',(-12.0000000000001,104.3754124827,-1.45141672215856));
#276013=CARTESIAN_POINT('Ctrl Pts',(-11.7366682504109,104.316709487413,
-2.8917558018116));
#276014=CARTESIAN_POINT('Ctrl Pts',(-10.6694625868215,104.194978937878,
-5.70921191596897));
#276015=CARTESIAN_POINT('Ctrl Pts',(-9.83791481246829,104.135668144137,
-7.04613425402326));
#276016=CARTESIAN_POINT('Ctrl Pts',(-7.6996867104163,104.011206526125,-9.3377833408248));
#276017=CARTESIAN_POINT('Ctrl Pts',(-6.40930566327384,103.946897674067,
-10.2664593419611));
#276018=CARTESIAN_POINT('Ctrl Pts',(-3.56946054311442,103.823190057369,
-11.560703293972));
#276019=CARTESIAN_POINT('Ctrl Pts',(-2.0516887747929,103.764242553893,-11.923986377946));
#276020=CARTESIAN_POINT('Ctrl Pts',(1.07210272081072,103.637882533553,-12.056038083896));
#276021=CARTESIAN_POINT('Ctrl Pts',(2.64872314137544,103.57537415047,-11.810223102415));
#276022=CARTESIAN_POINT('Ctrl Pts',(5.59798914903062,103.453137648988,-10.7284569647133));
#276023=CARTESIAN_POINT('Ctrl Pts',(6.94474352371526,103.389603935508,-9.9099733497718));
#276024=CARTESIAN_POINT('Ctrl Pts',(9.24133620388024,103.264526173037,-7.81038030019616));
#276025=CARTESIAN_POINT('Ctrl Pts',(10.1721743389527,103.206167475913,-6.55219167295185));
#276026=CARTESIAN_POINT('Ctrl Pts',(11.5181621169873,103.080408738882,-3.72061036212782));
#276027=CARTESIAN_POINT('Ctrl Pts',(11.9083049834493,103.015830266773,-2.16875006051643));
#276028=CARTESIAN_POINT('Ctrl Pts',(12.0613369283081,102.893494442124,0.961472365135507));
#276029=CARTESIAN_POINT('Ctrl Pts',(11.8366010142436,102.832681255944,2.50906255089275));
#276030=CARTESIAN_POINT('Ctrl Pts',(10.8061620462178,102.706759346794,5.44741331201057));
#276031=CARTESIAN_POINT('Ctrl Pts',(10.0047208534933,102.64678167457,6.80830477624646));
#276032=CARTESIAN_POINT('Ctrl Pts',(7.92053483803228,102.522885460395,9.15055638290675));
#276033=CARTESIAN_POINT('Ctrl Pts',(6.65597983170444,102.458745118947,10.1076915780615));
#276034=CARTESIAN_POINT('Ctrl Pts',(3.85194512226161,102.334598064039,11.4697064390822));
#276035=CARTESIAN_POINT('Ctrl Pts',(2.34331124432273,102.276038930589,11.8701513059845));
#276036=CARTESIAN_POINT('Ctrl Pts',(-0.783691128516117,102.149549027536,
12.0791548994081));
#276037=CARTESIAN_POINT('Ctrl Pts',(-2.37294220292942,102.085812253944,
11.8696540642989));
#276038=CARTESIAN_POINT('Ctrl Pts',(-5.34938384061895,101.964259428575,
10.8540463567392));
#276039=CARTESIAN_POINT('Ctrl Pts',(-6.71157120332194,101.901010935596,
10.0688003707522));
#276040=CARTESIAN_POINT('Ctrl Pts',(-9.05647978478012,101.775667377541,
8.02452949354289));
#276041=CARTESIAN_POINT('Ctrl Pts',(-10.0180799873236,101.717091948471,
6.78608948726545));
#276042=CARTESIAN_POINT('Ctrl Pts',(-11.4220280949518,101.592327134818,
3.99917625171409));
#276043=CARTESIAN_POINT('Ctrl Pts',(-11.846153848979,101.528383280513,2.4748536455238));
#276044=CARTESIAN_POINT('Ctrl Pts',(-11.9884536108764,101.454792207264,
0.608194507680637));
#276045=CARTESIAN_POINT('Ctrl Pts',(-12.0000000000001,101.442942496614,
0.303929806132952));
#276046=CARTESIAN_POINT('Ctrl Pts',(-12.0000000000001,101.431249999604,
4.79130624064794E-13));
#276047=CARTESIAN_POINT('Ctrl Pts',(-12.0000000000001,101.806249999604,
4.41591208044656E-13));
#276048=CARTESIAN_POINT('Ctrl Pts',(-12.0000000000001,101.819718521391,
0.350095040632927));
#276049=CARTESIAN_POINT('Ctrl Pts',(-11.9846796226145,101.833393558327,
0.700580256045129));
#276050=CARTESIAN_POINT('Ctrl Pts',(-11.8157459659036,101.909462883929,
2.62300415699322));
#276051=CARTESIAN_POINT('Ctrl Pts',(-11.3686032455459,101.973909767947,
4.15292363840108));
#276052=CARTESIAN_POINT('Ctrl Pts',(-9.91849965274548,102.098922706532,
6.9312897019481));
#276053=CARTESIAN_POINT('Ctrl Pts',(-8.93753485777631,102.157714218484,
8.15719532852502));
#276054=CARTESIAN_POINT('Ctrl Pts',(-6.56255730271517,102.283203504547,
10.1662089139473));
#276055=CARTESIAN_POINT('Ctrl Pts',(-5.19104211732635,102.346255274138,
10.930342364952));
#276056=CARTESIAN_POINT('Ctrl Pts',(-2.19787636457957,102.467356960704,
11.9039570865563));
#276057=CARTESIAN_POINT('Ctrl Pts',(-0.600720123462492,102.531950360164,
12.0902774525815));
#276058=CARTESIAN_POINT('Ctrl Pts',(2.5280641425565,102.658512342311,11.83225172001));
#276059=CARTESIAN_POINT('Ctrl Pts',(4.03079793476824,102.716914572037,11.4081549457105));
#276060=CARTESIAN_POINT('Ctrl Pts',(6.81147777948937,102.841318626694,10.0031858500243));
#276061=CARTESIAN_POINT('Ctrl Pts',(8.05922212204603,102.905332462921,9.02823337963791));
#276062=CARTESIAN_POINT('Ctrl Pts',(10.1085155120594,103.028846556572,6.65402760599244));
#276063=CARTESIAN_POINT('Ctrl Pts',(10.8905026907458,103.089338828686,5.27779941230339));
#276064=CARTESIAN_POINT('Ctrl Pts',(11.8746799498332,103.215379301704,2.32133541188133));
#276065=CARTESIAN_POINT('Ctrl Pts',(12.0748094649417,103.275628241651,0.771661914612208));
#276066=CARTESIAN_POINT('Ctrl Pts',(11.8731200331309,103.398324418499,-2.35211757732449));
#276067=CARTESIAN_POINT('Ctrl Pts',(11.4598969894638,103.462860891733,-3.89538697384107));
#276068=CARTESIAN_POINT('Ctrl Pts',(10.0718393722471,103.588331234776,-6.70580257434195));
#276069=CARTESIAN_POINT('Ctrl Pts',(9.12085643168401,103.646814276566,-7.95108074182539));
#276070=CARTESIAN_POINT('Ctrl Pts',(6.79254880140641,103.772070823266,-10.0145413019603));
#276071=CARTESIAN_POINT('Ctrl Pts',(5.43560345393382,103.835421547407,-10.8113019911486));
#276072=CARTESIAN_POINT('Ctrl Pts',(2.46845787887802,103.957214899215,-11.8498208098566));
#276073=CARTESIAN_POINT('Ctrl Pts',(0.883557038940081,104.020509366595,
-12.0719252313962));
#276074=CARTESIAN_POINT('Ctrl Pts',(-2.24238830252252,104.146956511831,
-11.889607902365));
#276075=CARTESIAN_POINT('Ctrl Pts',(-3.75420805423453,104.20563067194,-11.5020454222977));
#276076=CARTESIAN_POINT('Ctrl Pts',(-6.57077945978205,104.329630283488,
-10.1634870880653));
#276077=CARTESIAN_POINT('Ctrl Pts',(-7.84436963905717,104.39383322516,-9.21615487078874));
#276078=CARTESIAN_POINT('Ctrl Pts',(-9.94739883655799,104.517930272847,
-6.89139192513552));
#276079=CARTESIAN_POINT('Ctrl Pts',(-10.7593396456813,104.577657251294,
-5.53882792160448));
#276080=CARTESIAN_POINT('Ctrl Pts',(-11.759913674213,104.696968996814,-2.76259524211232));
#276081=CARTESIAN_POINT('Ctrl Pts',(-12.0000000000001,104.752933891441,
-1.38587629317705));
#276082=CARTESIAN_POINT('Ctrl Pts',(-12.0000000000001,104.806249999592,
3.52495810318487E-14));
#276083=CARTESIAN_POINT('Origin',(-8.79029313101884E-14,130.96875,0.));
#276084=CARTESIAN_POINT('',(-12.0000000000001,107.80624999958,-1.42867746987913E-15));
#276085=CARTESIAN_POINT('',(-12.0000000000001,107.43124999958,6.31640302154899E-16));
#276086=CARTESIAN_POINT('',(-12.0000000000001,130.96875,-1.46957615897682E-15));
#276087=CARTESIAN_POINT('',(11.8516579398691,109.38046875,-1.8810114503466));
#276088=CARTESIAN_POINT('Ctrl Pts',(-12.0000000000001,107.80624999958,-2.22044604925031E-15));
#276089=CARTESIAN_POINT('Ctrl Pts',(-12.0000000000001,107.866343814516,
1.56205312755359));
#276090=CARTESIAN_POINT('Ctrl Pts',(-11.6949938433683,107.92969090644,3.10956804902835));
#276091=CARTESIAN_POINT('Ctrl Pts',(-10.5145746762546,108.055118102493,
5.98632792710984));
#276092=CARTESIAN_POINT('Ctrl Pts',(-9.65626038750239,108.113582953069,
7.29034181478346));
#276093=CARTESIAN_POINT('Ctrl Pts',(-7.47603641389864,108.237872369909,
9.51694602212484));
#276094=CARTESIAN_POINT('Ctrl Pts',(-6.16853086833224,108.301945582296,
10.4121415247227));
#276095=CARTESIAN_POINT('Ctrl Pts',(-3.28613682807818,108.42563556719,11.6470803453935));
#276096=CARTESIAN_POINT('Ctrl Pts',(-1.73951548877978,108.485885119957,
11.9761130077834));
#276097=CARTESIAN_POINT('Ctrl Pts',(1.37506378162063,108.611872497961,12.021126122061));
#276098=CARTESIAN_POINT('Ctrl Pts',(2.91330421762905,108.672369841524,11.7435408531582));
#276099=CARTESIAN_POINT('Ctrl Pts',(5.83156931012537,108.794903894772,10.6065910386354));
#276100=CARTESIAN_POINT('Ctrl Pts',(7.17862656088049,108.859461370049,9.74546642258997));
#276101=CARTESIAN_POINT('Ctrl Pts',(9.4377057368,108.985065275805,7.57211167244003));
#276102=CARTESIAN_POINT('Ctrl Pts',(10.3366228846815,109.043483264628,6.28978302888967));
#276103=CARTESIAN_POINT('Ctrl Pts',(11.4376342634708,109.152590405637,3.81143858254238));
#276104=CARTESIAN_POINT('Ctrl Pts',(11.7524514429401,109.199737369538,2.68821070974933));
#276105=CARTESIAN_POINT('Ctrl Pts',(12.0478585774647,109.291407362996,0.401363391909027));
#276106=CARTESIAN_POINT('Ctrl Pts',(12.0312037663556,109.334703618332,-0.749750011370815));
#276107=CARTESIAN_POINT('Ctrl Pts',(11.8516579398691,109.38046875,-1.88101145034674));
#276108=CARTESIAN_POINT('',(7.06903888345947,109.38046875,-9.696839137788));
#276109=CARTESIAN_POINT('Origin',(-7.54701734185159E-14,109.38046875,0.));
#276110=CARTESIAN_POINT('Ctrl Pts',(7.06903888345945,109.38046875,-9.69683913778803));
#276111=CARTESIAN_POINT('Ctrl Pts',(8.02804380632041,109.332462367855,-8.99772028134388));
#276112=CARTESIAN_POINT('Ctrl Pts',(8.8780784676924,109.28473067987,-8.16016994838996));
#276113=CARTESIAN_POINT('Ctrl Pts',(10.3026613015982,109.193061552059,-6.26547500429061));
#276114=CARTESIAN_POINT('Ctrl Pts',(10.8701502580611,109.14616524121,-5.21930516734868));
#276115=CARTESIAN_POINT('Ctrl Pts',(11.8155022909111,109.034502891345,-2.62396491876396));
#276116=CARTESIAN_POINT('Ctrl Pts',(12.0578170407519,108.972322229049,-1.04882821065039));
#276117=CARTESIAN_POINT('Ctrl Pts',(11.9196530803474,108.849893935341,2.08862871745094));
#276118=CARTESIAN_POINT('Ctrl Pts',(11.5468169083728,108.786283367778,3.620953004917));
#276119=CARTESIAN_POINT('Ctrl Pts',(10.240088817047,108.661290939061,6.44537146805403));
#276120=CARTESIAN_POINT('Ctrl Pts',(9.32291011631986,108.602966100172,7.71268965593937));
#276121=CARTESIAN_POINT('Ctrl Pts',(7.03115871052508,108.477083897142,9.85277970239431));
#276122=CARTESIAN_POINT('Ctrl Pts',(5.66907121068656,108.412491483342,10.6946864168547));
#276123=CARTESIAN_POINT('Ctrl Pts',(2.73001709375482,108.290322327293,11.7876755691295));
#276124=CARTESIAN_POINT('Ctrl Pts',(1.18622866805082,108.22923395716,12.0414055389981));
#276125=CARTESIAN_POINT('Ctrl Pts',(-1.92536059284584,108.103367527582,
11.9472136780264));
#276126=CARTESIAN_POINT('Ctrl Pts',(-3.46344019184888,108.043598548278,
11.5951511074519));
#276127=CARTESIAN_POINT('Ctrl Pts',(-6.32617469954648,107.919535973427,
10.3174826910173));
#276128=CARTESIAN_POINT('Ctrl Pts',(-7.62184176508883,107.855343573278,
9.40098006137079));
#276129=CARTESIAN_POINT('Ctrl Pts',(-9.76845852360064,107.731318008446,
7.13921670750586));
#276130=CARTESIAN_POINT('Ctrl Pts',(-10.6061854625943,107.672665296767,
5.82236900617445));
#276131=CARTESIAN_POINT('Ctrl Pts',(-11.7190826474381,107.549629717902,
2.98583658854305));
#276132=CARTESIAN_POINT('Ctrl Pts',(-12.0000000000001,107.48892173526,1.49909462707177));
#276133=CARTESIAN_POINT('Ctrl Pts',(-12.0000000000001,107.43124999958,-4.10782519111308E-14));
#276134=CARTESIAN_POINT('Origin',(-8.79029313101884E-14,130.96875,0.));
#276135=CARTESIAN_POINT('Ctrl Pts',(-12.0000000000001,107.43124999958,2.73285676328662E-15));
#276136=CARTESIAN_POINT('Ctrl Pts',(-12.0000000000001,107.427995874985,
-0.0845863340034995));
#276137=CARTESIAN_POINT('Ctrl Pts',(-11.9991056463269,107.424729090763,
-0.169211143825749));
#276138=CARTESIAN_POINT('Ctrl Pts',(-11.964341287163,107.361088711466,-1.81215653557658));
#276139=CARTESIAN_POINT('Ctrl Pts',(-11.6280800167193,107.297755470126,
-3.34915602874002));
#276140=CARTESIAN_POINT('Ctrl Pts',(-10.3891578369817,107.172483440034,
-6.20287380756784));
#276141=CARTESIAN_POINT('Ctrl Pts',(-9.50039687721795,107.113985669083,
-7.49351280749634));
#276142=CARTESIAN_POINT('Ctrl Pts',(-7.25951074047479,106.988542511097,
-9.68514731953922));
#276143=CARTESIAN_POINT('Ctrl Pts',(-5.92088023027487,106.924010620768,
-10.5567942847113));
#276144=CARTESIAN_POINT('Ctrl Pts',(-3.01426889782003,106.801282393196,
-11.7179508024918));
#276145=CARTESIAN_POINT('Ctrl Pts',(-1.47911473022806,106.741081447252,
-12.0086858454301));
#276146=CARTESIAN_POINT('Ctrl Pts',(1.63703535302971,106.615030528534,-11.9908030836491));
#276147=CARTESIAN_POINT('Ctrl Pts',(3.18833183487053,106.554487995537,-11.674490635908));
#276148=CARTESIAN_POINT('Ctrl Pts',(6.08136829751295,106.431009484748,-10.4630941343253));
#276149=CARTESIAN_POINT('Ctrl Pts',(7.39522944879173,106.36700788638,-9.57965834995361));
#276150=CARTESIAN_POINT('Ctrl Pts',(9.59375419220535,106.242581366008,-7.37247662390832));
#276151=CARTESIAN_POINT('Ctrl Pts',(10.4633417627637,106.184189907485,-6.07552211554223));
#276152=CARTESIAN_POINT('Ctrl Pts',(11.6796006270252,106.057649939537,-3.18148234050514));
#276153=CARTESIAN_POINT('Ctrl Pts',(11.9982402648555,105.993035449527,-1.60545299752112));
#276154=CARTESIAN_POINT('Ctrl Pts',(12.0017042150108,105.871913988982,1.54180135026534));
#276155=CARTESIAN_POINT('Ctrl Pts',(11.7011401038563,105.808925175336,3.08255411229185));
#276156=CARTESIAN_POINT('Ctrl Pts',(10.5285614620387,105.683415227199,5.96401255403122));
#276157=CARTESIAN_POINT('Ctrl Pts',(9.66757293360446,105.624598912445,7.27723393041331));
#276158=CARTESIAN_POINT('Ctrl Pts',(7.47649463281433,105.499616447155,9.51804700867654));
#276159=CARTESIAN_POINT('Ctrl Pts',(6.16113181584196,105.435176402445,10.4178563181802));
#276160=CARTESIAN_POINT('Ctrl Pts',(3.28670360005198,105.311948728854,11.6443150407754));
#276161=CARTESIAN_POINT('Ctrl Pts',(1.75998898775683,105.252443049639,11.9705871715524));
#276162=CARTESIAN_POINT('Ctrl Pts',(-1.36012470385981,105.126231799595,
12.0260967757031));
#276163=CARTESIAN_POINT('Ctrl Pts',(-2.92392934879068,105.064799308801,
11.7442500892509));
#276164=CARTESIAN_POINT('Ctrl Pts',(-5.84503502917611,104.941913498483,
10.5964156377292));
#276165=CARTESIAN_POINT('Ctrl Pts',(-7.17546734499953,104.878125961916,
9.74479122052804));
#276166=CARTESIAN_POINT('Ctrl Pts',(-9.42264554811813,104.753358329308,
7.59022857154424));
#276167=CARTESIAN_POINT('Ctrl Pts',(-10.3224350204873,104.695060346315,
6.31230031409505));
#276168=CARTESIAN_POINT('Ctrl Pts',(-11.6029971251243,104.568887412855,
3.44869446711149));
#276169=CARTESIAN_POINT('Ctrl Pts',(-11.9571346890154,104.504273295728,
1.88420879207154));
#276170=CARTESIAN_POINT('Ctrl Pts',(-11.9987825322073,104.43886058118,0.197430649364387));
#276171=CARTESIAN_POINT('Ctrl Pts',(-12.0000000000001,104.435046718343,
0.0986902962678449));
#276172=CARTESIAN_POINT('Ctrl Pts',(-12.0000000000001,104.431249999592,
2.73285676328662E-15));
#276173=CARTESIAN_POINT('Ctrl Pts',(-12.0000000000001,104.806249999592,
-3.30291349825984E-14));
#276174=CARTESIAN_POINT('Ctrl Pts',(-12.0000000000001,104.812464713841,
0.161542645279967));
#276175=CARTESIAN_POINT('Ctrl Pts',(-11.9967380233314,104.818724869803,
0.323206602683525));
#276176=CARTESIAN_POINT('Ctrl Pts',(-11.9261120943596,104.886793472473,
2.06960522352684));
#276177=CARTESIAN_POINT('Ctrl Pts',(-11.54848852509,104.95138842782,3.62596174965847));
#276178=CARTESIAN_POINT('Ctrl Pts',(-10.2252760523671,105.077296051354,
6.46881329835151));
#276179=CARTESIAN_POINT('Ctrl Pts',(-9.30528386847831,105.135615489699,
7.7339192777929));
#276180=CARTESIAN_POINT('Ctrl Pts',(-7.0258812088237,105.260589638183,9.85281451307973));
#276181=CARTESIAN_POINT('Ctrl Pts',(-5.68474473736919,105.32421591025,10.6829233828083));
#276182=CARTESIAN_POINT('Ctrl Pts',(-2.74523390111701,105.446683865421,
11.7878509544643));
#276183=CARTESIAN_POINT('Ctrl Pts',(-1.17308397829313,105.508797755876,
12.0463228935084));
#276184=CARTESIAN_POINT('Ctrl Pts',(1.94947066697386,105.63510774457,11.9411368396299));
#276185=CARTESIAN_POINT('Ctrl Pts',(3.47039778126117,105.694231675528,11.5908386583477));
#276186=CARTESIAN_POINT('Ctrl Pts',(6.32249939755816,105.817775656283,10.3203466064808));
#276187=CARTESIAN_POINT('Ctrl Pts',(7.62173048099895,105.882134685304,9.40174126806386));
#276188=CARTESIAN_POINT('Ctrl Pts',(9.77861242901587,106.006783826509,7.12788005545473));
#276189=CARTESIAN_POINT('Ctrl Pts',(10.6205501364151,106.065902010767,5.79929321074988));
#276190=CARTESIAN_POINT('Ctrl Pts',(11.7475699929408,106.191551757011,2.89939796966487));
#276191=CARTESIAN_POINT('Ctrl Pts',(12.0237923310024,106.253771231836,1.35638022512553));
#276192=CARTESIAN_POINT('Ctrl Pts',(11.9723929312291,106.375299269845,-1.78586735302398));
#276193=CARTESIAN_POINT('Ctrl Pts',(11.6307531771349,106.43991740774,-3.35451832678343));
#276194=CARTESIAN_POINT('Ctrl Pts',(10.3728507076161,106.566224175867,-6.22896557707807));
#276195=CARTESIAN_POINT('Ctrl Pts',(9.48373849128698,106.624538019851,-7.51363935107693));
#276196=CARTESIAN_POINT('Ctrl Pts',(7.25369658646848,106.749189457153,-9.68690109223212));
#276197=CARTESIAN_POINT('Ctrl Pts',(5.92904573149467,106.813056369374,-10.5498214277077));
#276198=CARTESIAN_POINT('Ctrl Pts',(3.01778852767233,106.936156081398,-11.7202075268318));
#276199=CARTESIAN_POINT('Ctrl Pts',(1.45840227756446,106.997256388224,-12.0143038356566));
#276200=CARTESIAN_POINT('Ctrl Pts',(-1.66035201914284,107.123412649589,
-11.9848591271093));
#276201=CARTESIAN_POINT('Ctrl Pts',(-3.1900790292478,107.183147372144,-11.6712020474588));
#276202=CARTESIAN_POINT('Ctrl Pts',(-6.0760466845703,107.306202024025,-10.4679030324817));
#276203=CARTESIAN_POINT('Ctrl Pts',(-7.39975098695485,107.370678482113,
-9.57804330102746));
#276204=CARTESIAN_POINT('Ctrl Pts',(-9.6086165723654,107.495828889602,-7.35464892462781));
#276205=CARTESIAN_POINT('Ctrl Pts',(-10.4795187353534,107.554514780734,
-6.04946415648028));
#276206=CARTESIAN_POINT('Ctrl Pts',(-11.6757493718232,107.679940049496,
-3.17789183339809));
#276207=CARTESIAN_POINT('Ctrl Pts',(-11.989082469283,107.743082695574,-1.63839677759871));
#276208=CARTESIAN_POINT('Ctrl Pts',(-11.9999066094214,107.804145561296,
-0.054671531396247));
#276209=CARTESIAN_POINT('Ctrl Pts',(-12.0000000000001,107.805198448039,
-0.0273335845947108));
#276210=CARTESIAN_POINT('Ctrl Pts',(-12.0000000000001,107.80624999958,2.17774546598592E-15));
#276211=CARTESIAN_POINT('Origin',(-6.51327129430312E-14,91.43046875,0.));
#276212=CARTESIAN_POINT('Ctrl Pts',(-11.2291932872669,93.2512754627332,
8.5342589378412E-11));
#276213=CARTESIAN_POINT('Ctrl Pts',(-11.2847945964217,93.1956741535784,
-0.57160885882348));
#276214=CARTESIAN_POINT('Ctrl Pts',(-11.2935934610398,93.143158872129,-1.10587788332065));
#276215=CARTESIAN_POINT('Ctrl Pts',(-11.2307768438364,92.9923394153088,
-2.6300800192019));
#276216=CARTESIAN_POINT('Ctrl Pts',(-11.0476053526866,92.8890071879839,
-3.65836031572687));
#276217=CARTESIAN_POINT('Ctrl Pts',(-10.3932827518185,92.6811478925007,
-5.6915126996453));
#276218=CARTESIAN_POINT('Ctrl Pts',(-9.9151798225123,92.5816333031356,-6.66836341355856));
#276219=CARTESIAN_POINT('Ctrl Pts',(-9.30293325730102,92.4804687499998,
-7.57993620093262));
#276220=CARTESIAN_POINT('',(-13.0500000000001,91.43046875,-1.5981640728873E-15));
#276221=CARTESIAN_POINT('',(-13.0500000000001,91.43046875,-1.5981640728873E-15));
#276222=CARTESIAN_POINT('Origin',(-6.51327129430312E-14,91.43046875,0.));
#276223=CARTESIAN_POINT('Ctrl Pts',(-11.9338891906744,92.48046875,1.25789060919728));
#276224=CARTESIAN_POINT('Ctrl Pts',(-11.770923660508,92.511971325493,2.50345334854318));
#276225=CARTESIAN_POINT('Ctrl Pts',(-11.4122992544335,92.5444554192473,
3.71547200511176));
#276226=CARTESIAN_POINT('Ctrl Pts',(-10.3244245330618,92.6093697694792,
5.99501809473401));
#276227=CARTESIAN_POINT('Ctrl Pts',(-9.59484510342232,92.6404645939112,
7.05327596796796));
#276228=CARTESIAN_POINT('Ctrl Pts',(-7.6557591345177,92.7118196954419,9.06644546422308));
#276229=CARTESIAN_POINT('Ctrl Pts',(-6.39836926084137,92.7519983328108,
9.94624499765885));
#276230=CARTESIAN_POINT('Ctrl Pts',(-4.3200113853284,92.8107939361435,10.8666927631942));
#276231=CARTESIAN_POINT('Ctrl Pts',(-3.59982559121635,92.8296305703617,
11.1064875492582));
#276232=CARTESIAN_POINT('Ctrl Pts',(-1.39093647983724,92.8876938258724,
11.6075000465635));
#276233=CARTESIAN_POINT('Ctrl Pts',(0.132137348818577,92.9281282121338,
11.6496887621334));
#276234=CARTESIAN_POINT('Ctrl Pts',(3.02010897419524,93.0056179478086,11.1608980046078));
#276235=CARTESIAN_POINT('Ctrl Pts',(4.46788175864068,93.0435700320912,10.6515406785813));
#276236=CARTESIAN_POINT('Ctrl Pts',(7.05209221412667,93.1258189120352,9.01507985911188));
#276237=CARTESIAN_POINT('Ctrl Pts',(8.11193039348105,93.165100379407,8.01934582510662));
#276238=CARTESIAN_POINT('Ctrl Pts',(9.9463038250971,93.2468518201986,5.48682671511057));
#276239=CARTESIAN_POINT('Ctrl Pts',(10.4991557746749,93.2874302123591,4.08411044948916));
#276240=CARTESIAN_POINT('Ctrl Pts',(11.1192237564845,93.3623130546168,1.43522933079907));
#276241=CARTESIAN_POINT('Ctrl Pts',(11.1747094657362,93.4000738876541,-0.0302329141322163));
#276242=CARTESIAN_POINT('Ctrl Pts',(10.7175467303705,93.4786371807489,-2.86025213866675));
#276243=CARTESIAN_POINT('Ctrl Pts',(10.2229105328389,93.518696977927,-4.20226784190578));
#276244=CARTESIAN_POINT('Ctrl Pts',(8.74706554744609,93.5970629058072,-6.63063803679562));
#276245=CARTESIAN_POINT('Ctrl Pts',(7.77752378047288,93.6351162741571,-7.69213698519598));
#276246=CARTESIAN_POINT('Ctrl Pts',(6.05893990234535,93.6957097996795,-8.94941269430666));
#276247=CARTESIAN_POINT('Ctrl Pts',(5.45372378818858,93.7157422931018,-9.30741418619836));
#276248=CARTESIAN_POINT('Ctrl Pts',(3.61704124833991,93.7729986214116,-10.1647555333684));
#276249=CARTESIAN_POINT('Ctrl Pts',(2.23967766451721,93.8109335955831,-10.5392880962719));
#276250=CARTESIAN_POINT('Ctrl Pts',(-0.814433850702704,93.8992040341989,
-10.6637298323807));
#276251=CARTESIAN_POINT('Ctrl Pts',(-2.205161618853,93.9397832479048,-10.3781035460965));
#276252=CARTESIAN_POINT('Ctrl Pts',(-4.56420121931845,94.0099587092093,
-9.51297076079011));
#276253=CARTESIAN_POINT('Ctrl Pts',(-5.69260107256812,94.0483614325352,
-8.83854113951805));
#276254=CARTESIAN_POINT('Ctrl Pts',(-7.63861966215954,94.1251920550018,
-7.11118943227298));
#276255=CARTESIAN_POINT('Ctrl Pts',(-8.50510758937149,94.163586056503,-6.0180431767386));
#276256=CARTESIAN_POINT('Ctrl Pts',(-9.66899795618243,94.2432885837152,
-3.58491338927264));
#276257=CARTESIAN_POINT('Ctrl Pts',(-9.99624123320409,94.2809774299658,
-2.37613833619406));
#276258=CARTESIAN_POINT('Ctrl Pts',(-10.1300916521385,94.3290886022729,
-0.759197386330359));
#276259=CARTESIAN_POINT('Ctrl Pts',(-10.1402351895106,94.3402335604895,
-0.379162435421409));
#276260=CARTESIAN_POINT('Ctrl Pts',(-10.1292796487468,94.3511891012534,
-3.61308205576449E-13));
#276261=CARTESIAN_POINT('Origin',(-7.54701734185159E-14,109.38046875,0.));
#276262=CARTESIAN_POINT('Ctrl Pts',(10.9371370246358,108.317605774636,-1.20722876140178E-12));
#276263=CARTESIAN_POINT('Ctrl Pts',(10.9828089962346,108.363277746235,-0.457318519945779));
#276264=CARTESIAN_POINT('Ctrl Pts',(11.0000648203508,108.409479285711,-0.916344195964511));
#276265=CARTESIAN_POINT('Ctrl Pts',(10.9568199431785,108.605400899729,-2.84979780113602));
#276266=CARTESIAN_POINT('Ctrl Pts',(10.6307901096444,108.756544688372,-4.31034356862055));
#276267=CARTESIAN_POINT('Ctrl Pts',(9.63928557161438,108.994702486232,-6.54978660282652));
#276268=CARTESIAN_POINT('Ctrl Pts',(9.18158964065412,109.07307336719,-7.27431422591661));
#276269=CARTESIAN_POINT('Ctrl Pts',(8.26278618214127,109.220237796992,-8.52069965894701));
#276270=CARTESIAN_POINT('Ctrl Pts',(7.69604270790284,109.300636569957,-9.14095690657997));
#276271=CARTESIAN_POINT('Ctrl Pts',(7.06903888345942,109.38046875,-9.69683913778806));
#276272=CARTESIAN_POINT('',(11.952947197667,109.333415947667,-1.48178615512317E-14));
#276273=CARTESIAN_POINT('Ctrl Pts',(11.8516579398691,109.38046875,-1.88101145034666));
#276274=CARTESIAN_POINT('Ctrl Pts',(11.9344344341192,109.364552105091,-1.25792197685612));
#276275=CARTESIAN_POINT('Ctrl Pts',(11.9683416601056,109.348810410106,-0.628713018278117));
#276276=CARTESIAN_POINT('Ctrl Pts',(11.952947197667,109.333415947667,-3.24740234702858E-14));
#276277=CARTESIAN_POINT('',(13.0499999999999,110.43046875,-1.5981640728873E-15));
#276278=CARTESIAN_POINT('',(11.9999999999999,109.38046875,-1.46957615897682E-15));
#276279=CARTESIAN_POINT('Origin',(-7.60748716635999E-14,110.43046875,0.));
#276280=CARTESIAN_POINT('Ctrl Pts',(11.952947197667,109.333415947667,3.13638004456607E-14));
#276281=CARTESIAN_POINT('Ctrl Pts',(11.9361764328271,109.316645182827,0.684921491956612));
#276282=CARTESIAN_POINT('Ctrl Pts',(11.8599674216354,109.29935041853,1.36919665137744));
#276283=CARTESIAN_POINT('Ctrl Pts',(11.4730011189775,109.249063059047,3.29578789917538));
#276284=CARTESIAN_POINT('Ctrl Pts',(11.0211144208823,109.215720290848,4.4985163450752));
#276285=CARTESIAN_POINT('Ctrl Pts',(10.0086823313146,109.163528707969,6.26438058673198));
#276286=CARTESIAN_POINT('Ctrl Pts',(9.56664237078174,109.144696058498,6.88882718671992));
#276287=CARTESIAN_POINT('Ctrl Pts',(8.06901266781109,109.086716018239,8.6169708190365));
#276288=CARTESIAN_POINT('Ctrl Pts',(6.85368625009054,109.046260158232,9.56255164669703));
#276289=CARTESIAN_POINT('Ctrl Pts',(4.21079500114126,108.968719165965,10.890719112925));
#276290=CARTESIAN_POINT('Ctrl Pts',(2.72850500147909,108.930794662696,11.3415417579546));
#276291=CARTESIAN_POINT('Ctrl Pts',(-0.353974635331329,108.848567400121,
11.5547589716743));
#276292=CARTESIAN_POINT('Ctrl Pts',(-1.81312200817527,108.809238555222,
11.377609085633));
#276293=CARTESIAN_POINT('Ctrl Pts',(-4.7766980905649,108.72856277097,10.426047251413));
#276294=CARTESIAN_POINT('Ctrl Pts',(-6.06885139591756,108.688381621656,
9.63585458101247));
#276295=CARTESIAN_POINT('Ctrl Pts',(-8.19920523793862,108.611961202264,
7.81291676199372));
#276296=CARTESIAN_POINT('Ctrl Pts',(-9.11924339429115,108.57419762057,6.65404377338028));
#276297=CARTESIAN_POINT('Ctrl Pts',(-10.439195517319,108.49573029401,4.07719125689671));
#276298=CARTESIAN_POINT('Ctrl Pts',(-10.8391889019031,108.455639008447,
2.6874865390273));
#276299=CARTESIAN_POINT('Ctrl Pts',(-11.0891692155128,108.377141915412,
-0.174830130587083));
#276300=CARTESIAN_POINT('Ctrl Pts',(-10.9338206948192,108.339099105353,
-1.62092318083063));
#276301=CARTESIAN_POINT('Ctrl Pts',(-10.0428368869227,108.255905747577,
-4.43801234683806));
#276302=CARTESIAN_POINT('Ctrl Pts',(-9.31543510841679,108.216187512317,
-5.6993707846993));
#276303=CARTESIAN_POINT('Ctrl Pts',(-7.566753328723,108.141749268725,-7.76993416685136));
#276304=CARTESIAN_POINT('Ctrl Pts',(-6.50812173253096,108.102871888907,
-8.62766004041432));
#276305=CARTESIAN_POINT('Ctrl Pts',(-4.16308966090255,108.026690485365,
-9.88571225891757));
#276306=CARTESIAN_POINT('Ctrl Pts',(-2.80350980033859,107.988483056552,
-10.3421060224423));
#276307=CARTESIAN_POINT('Ctrl Pts',(0.0619227332583308,107.905310295235,
-10.6126892031837));
#276308=CARTESIAN_POINT('Ctrl Pts',(1.43257949959365,107.865068333532,-10.4754648420145));
#276309=CARTESIAN_POINT('Ctrl Pts',(3.38998859143884,107.806953429599,-9.88342127397056));
#276310=CARTESIAN_POINT('Ctrl Pts',(4.01942385278669,107.787935859554,-9.62411150470083));
#276311=CARTESIAN_POINT('Ctrl Pts',(5.79234492729014,107.729258630109,-8.67805514103696));
#276312=CARTESIAN_POINT('Ctrl Pts',(6.83259006553437,107.689352061935,-7.8327023884626));
#276313=CARTESIAN_POINT('Ctrl Pts',(8.48087656920956,107.614172913412,-5.86047188401398));
#276314=CARTESIAN_POINT('Ctrl Pts',(9.0983171567984,107.578847249204,-4.77235854786256));
#276315=CARTESIAN_POINT('Ctrl Pts',(9.89948065809396,107.504398305741,-2.44433261748365));
#276316=CARTESIAN_POINT('Ctrl Pts',(10.0851375233499,107.467360083825,-1.23130189093642));
#276317=CARTESIAN_POINT('Ctrl Pts',(10.0514325246607,107.431911591494,-0.0144013199032733));
#276318=CARTESIAN_POINT('Origin',(2.27702183671572E-14,91.43046875,0.));
#276319=CARTESIAN_POINT('',(-1.38777878078145E-14,91.43046875,18.));
#276320=CARTESIAN_POINT('',(15.5884572681199,91.43046875,9.));
#276321=CARTESIAN_POINT('Origin',(-1.38777878078145E-14,91.43046875,0.));
#276322=CARTESIAN_POINT('',(-15.5884572681199,91.43046875,9.));
#276323=CARTESIAN_POINT('Origin',(-1.38777878078145E-14,91.43046875,0.));
#276324=CARTESIAN_POINT('',(-15.5884572681199,91.43046875,-9.));
#276325=CARTESIAN_POINT('Origin',(-1.38777878078145E-14,91.43046875,0.));
#276326=CARTESIAN_POINT('',(-1.38777878078145E-14,91.43046875,-18.));
#276327=CARTESIAN_POINT('Origin',(-1.38777878078145E-14,91.43046875,0.));
#276328=CARTESIAN_POINT('',(15.5884572681199,91.43046875,-9.));
#276329=CARTESIAN_POINT('Origin',(-1.38777878078145E-14,91.43046875,0.));
#276330=CARTESIAN_POINT('Origin',(-1.38777878078145E-14,91.43046875,0.));
#276331=CARTESIAN_POINT('Origin',(-20.7846096908266,91.43046875,-6.94962355144037E-15));
#276332=CARTESIAN_POINT('',(-10.3923048454133,93.0381639045868,18.));
#276333=CARTESIAN_POINT('Ctrl Pts',(-10.39230484538,93.038163904606,18.0000000000577));
#276334=CARTESIAN_POINT('Ctrl Pts',(-13.1769145362265,91.43046875,13.176914536263));
#276335=CARTESIAN_POINT('Ctrl Pts',(-15.5884572681199,91.43046875,9.00000000000001));
#276336=CARTESIAN_POINT('',(-10.3923048454133,108.822773595413,18.));
#276337=CARTESIAN_POINT('',(-10.3923048454133,91.43046875,18.));
#276338=CARTESIAN_POINT('',(-15.5884572681199,110.43046875,9.));
#276339=CARTESIAN_POINT('Ctrl Pts',(-10.3923048453801,108.822773595394,
18.0000000000576));
#276340=CARTESIAN_POINT('Ctrl Pts',(-13.1769145362265,110.43046875,13.176914536263));
#276341=CARTESIAN_POINT('Ctrl Pts',(-15.5884572681199,110.43046875,9.00000000000004));
#276342=CARTESIAN_POINT('',(-20.7846096908266,108.822773595413,-4.36661259642003E-15));
#276343=CARTESIAN_POINT('Ctrl Pts',(-15.5884572681199,110.43046875,9.00000000000004));
#276344=CARTESIAN_POINT('Ctrl Pts',(-18.0000000000134,110.43046875,4.82308546373706));
#276345=CARTESIAN_POINT('Ctrl Pts',(-20.7846096908599,108.822773595394,
-5.76492496878966E-11));
#276346=CARTESIAN_POINT('',(-20.7846096908266,93.0381639045868,-6.10030560343973E-15));
#276347=CARTESIAN_POINT('',(-20.7846096908266,91.43046875,-6.94962355144037E-15));
#276348=CARTESIAN_POINT('Ctrl Pts',(-15.5884572681199,91.43046875,9.00000000000001));
#276349=CARTESIAN_POINT('Ctrl Pts',(-18.0000000000134,91.43046875,4.82308546373705));
#276350=CARTESIAN_POINT('Ctrl Pts',(-20.7846096908599,93.038163904606,-5.76355956615792E-11));
#276351=CARTESIAN_POINT('Origin',(-10.3923048454133,91.43046875,-18.));
#276352=CARTESIAN_POINT('Ctrl Pts',(-20.7846096908598,93.038163904606,5.75936582950325E-11));
#276353=CARTESIAN_POINT('Ctrl Pts',(-18.0000000000134,91.4304687500001,
-4.82308546373707));
#276354=CARTESIAN_POINT('Ctrl Pts',(-15.58845726812,91.4304687500001,-9.00000000000002));
#276355=CARTESIAN_POINT('',(-15.5884572681199,110.43046875,-9.));
#276356=CARTESIAN_POINT('Ctrl Pts',(-20.7846096908599,108.822773595394,
5.7616089909697E-11));
#276357=CARTESIAN_POINT('Ctrl Pts',(-18.0000000000135,110.43046875,-4.82308546373705));
#276358=CARTESIAN_POINT('Ctrl Pts',(-15.58845726812,110.43046875,-9.00000000000001));
#276359=CARTESIAN_POINT('',(-10.3923048454133,108.822773595413,-18.));
#276360=CARTESIAN_POINT('Ctrl Pts',(-15.58845726812,110.43046875,-9.00000000000001));
#276361=CARTESIAN_POINT('Ctrl Pts',(-13.1769145362265,110.43046875,-13.176914536263));
#276362=CARTESIAN_POINT('Ctrl Pts',(-10.3923048453801,108.822773595394,
-18.0000000000577));
#276363=CARTESIAN_POINT('',(-10.3923048454133,93.0381639045868,-18.));
#276364=CARTESIAN_POINT('',(-10.3923048454133,91.43046875,-18.));
#276365=CARTESIAN_POINT('Ctrl Pts',(-15.58845726812,91.4304687500001,-9.00000000000002));
#276366=CARTESIAN_POINT('Ctrl Pts',(-13.1769145362265,91.43046875,-13.176914536263));
#276367=CARTESIAN_POINT('Ctrl Pts',(-10.3923048453801,93.038163904606,-18.0000000000576));
#276368=CARTESIAN_POINT('Origin',(10.3923048454132,91.43046875,-18.));
#276369=CARTESIAN_POINT('Ctrl Pts',(-10.3923048454799,93.038163904606,-18.));
#276370=CARTESIAN_POINT('Ctrl Pts',(-4.82308546378702,91.43046875,-18.));
#276371=CARTESIAN_POINT('Ctrl Pts',(-3.2589543430822E-14,91.43046875,-18.));
#276372=CARTESIAN_POINT('',(-1.38777878078145E-14,110.43046875,-18.));
#276373=CARTESIAN_POINT('Ctrl Pts',(-10.3923048454799,108.822773595394,
-18.));
#276374=CARTESIAN_POINT('Ctrl Pts',(-4.82308546378693,110.43046875,-18.));
#276375=CARTESIAN_POINT('Ctrl Pts',(9.0526509530061E-14,110.43046875,-18.));
#276376=CARTESIAN_POINT('',(10.3923048454132,108.822773595413,-18.));
#276377=CARTESIAN_POINT('Ctrl Pts',(9.0526509530061E-14,110.43046875,-18.));
#276378=CARTESIAN_POINT('Ctrl Pts',(4.82308546378697,110.43046875,-18.));
#276379=CARTESIAN_POINT('Ctrl Pts',(10.3923048454797,108.822773595394,-18.));
#276380=CARTESIAN_POINT('',(10.3923048454132,93.0381639045867,-18.));
#276381=CARTESIAN_POINT('',(10.3923048454132,91.43046875,-18.));
#276382=CARTESIAN_POINT('Ctrl Pts',(-3.2589543430822E-14,91.43046875,-18.));
#276383=CARTESIAN_POINT('Ctrl Pts',(4.8230854637869,91.43046875,-18.));
#276384=CARTESIAN_POINT('Ctrl Pts',(10.3923048454797,93.0381639046059,-18.));
#276385=CARTESIAN_POINT('Origin',(20.7846096908265,91.43046875,-3.86306572340787E-15));
#276386=CARTESIAN_POINT('Ctrl Pts',(10.3923048453799,93.0381639046059,-18.0000000000576));
#276387=CARTESIAN_POINT('Ctrl Pts',(13.1769145362264,91.43046875,-13.176914536263));
#276388=CARTESIAN_POINT('Ctrl Pts',(15.5884572681198,91.43046875,-8.99999999999999));
#276389=CARTESIAN_POINT('',(15.5884572681199,110.43046875,-9.));
#276390=CARTESIAN_POINT('Ctrl Pts',(10.3923048453799,108.822773595394,-18.0000000000576));
#276391=CARTESIAN_POINT('Ctrl Pts',(13.1769145362264,110.43046875,-13.1769145362629));
#276392=CARTESIAN_POINT('Ctrl Pts',(15.5884572681199,110.43046875,-8.99999999999993));
#276393=CARTESIAN_POINT('',(20.7846096908264,108.822773595413,-3.76180926347169E-15));
#276394=CARTESIAN_POINT('Ctrl Pts',(15.5884572681199,110.43046875,-8.99999999999993));
#276395=CARTESIAN_POINT('Ctrl Pts',(18.0000000000133,110.43046875,-4.82308546373703));
#276396=CARTESIAN_POINT('Ctrl Pts',(20.7846096908597,108.822773595394,5.75790289811204E-11));
#276397=CARTESIAN_POINT('',(20.7846096908265,93.0381639045867,-2.6733106584905E-15));
#276398=CARTESIAN_POINT('',(20.7846096908265,91.43046875,-3.86306572340787E-15));
#276399=CARTESIAN_POINT('Ctrl Pts',(15.5884572681198,91.43046875,-8.99999999999999));
#276400=CARTESIAN_POINT('Ctrl Pts',(18.0000000000133,91.43046875,-4.82308546373704));
#276401=CARTESIAN_POINT('Ctrl Pts',(20.7846096908597,93.0381639046059,5.76336450863906E-11));
#276402=CARTESIAN_POINT('Origin',(10.3923048454132,91.43046875,18.));
#276403=CARTESIAN_POINT('Ctrl Pts',(20.7846096908597,93.0381639046059,-5.76141393345085E-11));
#276404=CARTESIAN_POINT('Ctrl Pts',(18.0000000000133,91.43046875,4.82308546373704));
#276405=CARTESIAN_POINT('Ctrl Pts',(15.5884572681198,91.43046875,8.99999999999998));
#276406=CARTESIAN_POINT('',(15.5884572681199,110.43046875,9.));
#276407=CARTESIAN_POINT('Ctrl Pts',(20.7846096908597,108.822773595394,-5.76531508382729E-11));
#276408=CARTESIAN_POINT('Ctrl Pts',(18.0000000000133,110.43046875,4.82308546373702));
#276409=CARTESIAN_POINT('Ctrl Pts',(15.5884572681198,110.43046875,8.99999999999998));
#276410=CARTESIAN_POINT('',(10.3923048454132,108.822773595413,18.));
#276411=CARTESIAN_POINT('Ctrl Pts',(15.5884572681198,110.43046875,8.99999999999998));
#276412=CARTESIAN_POINT('Ctrl Pts',(13.1769145362263,110.43046875,13.176914536263));
#276413=CARTESIAN_POINT('Ctrl Pts',(10.3923048453799,108.822773595394,18.0000000000577));
#276414=CARTESIAN_POINT('',(10.3923048454132,93.0381639045867,18.));
#276415=CARTESIAN_POINT('',(10.3923048454132,91.43046875,18.));
#276416=CARTESIAN_POINT('Ctrl Pts',(15.5884572681198,91.43046875,8.99999999999998));
#276417=CARTESIAN_POINT('Ctrl Pts',(13.1769145362264,91.43046875,13.1769145362629));
#276418=CARTESIAN_POINT('Ctrl Pts',(10.3923048453799,93.0381639046059,18.0000000000576));
#276419=CARTESIAN_POINT('Origin',(-10.3923048454133,91.43046875,18.));
#276420=CARTESIAN_POINT('Ctrl Pts',(10.3923048454797,93.0381639046059,18.));
#276421=CARTESIAN_POINT('Ctrl Pts',(4.8230854637869,91.43046875,18.));
#276422=CARTESIAN_POINT('Ctrl Pts',(-2.17263622872146E-14,91.43046875,18.));
#276423=CARTESIAN_POINT('',(-1.38777878078145E-14,110.43046875,18.));
#276424=CARTESIAN_POINT('Ctrl Pts',(10.3923048454797,108.822773595394,18.));
#276425=CARTESIAN_POINT('Ctrl Pts',(4.82308546378686,110.43046875,18.));
#276426=CARTESIAN_POINT('Ctrl Pts',(-1.14063402007877E-13,110.43046875,
18.));
#276427=CARTESIAN_POINT('Ctrl Pts',(-1.14063402007877E-13,110.43046875,
18.));
#276428=CARTESIAN_POINT('Ctrl Pts',(-4.82308546378701,110.43046875,18.));
#276429=CARTESIAN_POINT('Ctrl Pts',(-10.3923048454798,108.822773595394,
18.));
#276430=CARTESIAN_POINT('Ctrl Pts',(-1.44842415248098E-14,91.43046875,18.));
#276431=CARTESIAN_POINT('Ctrl Pts',(-4.82308546378699,91.43046875,18.));
#276432=CARTESIAN_POINT('Ctrl Pts',(-10.3923048454799,93.038163904606,18.));
#276433=CARTESIAN_POINT('Origin',(1.18280596465885E-14,110.43046875,0.));
#276434=CARTESIAN_POINT('Origin',(-1.38777878078145E-14,110.43046875,0.));
#276435=CARTESIAN_POINT('Origin',(-1.38777878078145E-14,110.43046875,0.));
#276436=CARTESIAN_POINT('Origin',(-1.38777878078145E-14,110.43046875,0.));
#276437=CARTESIAN_POINT('Origin',(-1.38777878078145E-14,110.43046875,0.));
#276438=CARTESIAN_POINT('Origin',(-1.38777878078145E-14,110.43046875,0.));
#276439=CARTESIAN_POINT('Origin',(-1.38777878078145E-14,110.43046875,0.));
#276440=CARTESIAN_POINT('Origin',(-1.38777878078145E-14,110.43046875,0.));
#276441=CARTESIAN_POINT('Origin',(-1.38777878078145E-14,110.43046875,0.));
#276442=CARTESIAN_POINT('Origin',(-1.38777878078145E-14,110.43046875,0.));
#276443=CARTESIAN_POINT('Origin',(-1.38777878078145E-14,110.43046875,0.));
#276444=CARTESIAN_POINT('Origin',(-1.38777878078145E-14,110.43046875,0.));
#276445=CARTESIAN_POINT('Origin',(-1.38777878078145E-14,110.43046875,0.));
#276446=CARTESIAN_POINT('Origin',(-1.38777878078145E-14,91.43046875,0.));
#276447=CARTESIAN_POINT('Origin',(-1.38777878078145E-14,91.43046875,0.));
#276448=CARTESIAN_POINT('Origin',(-1.38777878078145E-14,91.43046875,0.));
#276449=CARTESIAN_POINT('Origin',(-1.38777878078145E-14,91.43046875,0.));
#276450=CARTESIAN_POINT('Origin',(-1.38777878078145E-14,91.43046875,0.));
#276451=CARTESIAN_POINT('Origin',(-1.38777878078145E-14,91.43046875,0.));
#276452=CARTESIAN_POINT('Ctrl Pts',(-10.0514385264422,-1.69375249127916,
2.46189240364677E-15));
#276453=CARTESIAN_POINT('Ctrl Pts',(-10.0514385264422,-1.54375249127976,
3.26591035271534));
#276454=CARTESIAN_POINT('Ctrl Pts',(-8.13178458580685,-1.39375249128036,
5.90808733016713));
#276455=CARTESIAN_POINT('Ctrl Pts',(-6.21213064517146,-1.24375249128095,
8.55026430761891));
#276456=CARTESIAN_POINT('Ctrl Pts',(-3.10606532258574,-1.09375249128155,
9.55948610871303));
#276457=CARTESIAN_POINT('Ctrl Pts',(-9.99267329551972E-15,-0.943752491282151,
10.5687079098071));
#276458=CARTESIAN_POINT('Ctrl Pts',(3.10606532258571,-0.79375249128275,
9.55948610871303));
#276459=CARTESIAN_POINT('Ctrl Pts',(6.21213064517144,-0.643752491283348,
8.55026430761891));
#276460=CARTESIAN_POINT('Ctrl Pts',(8.13178458580682,-0.493752491283947,
5.90808733016712));
#276461=CARTESIAN_POINT('Ctrl Pts',(10.0514385264422,-0.343752491284545,
3.26591035271534));
#276462=CARTESIAN_POINT('Ctrl Pts',(10.0514385264422,-0.193752491285145,
-1.23094620182339E-15));
#276463=CARTESIAN_POINT('Ctrl Pts',(10.0514385264422,-0.0437524912857454,
-3.26591035271534));
#276464=CARTESIAN_POINT('Ctrl Pts',(8.13178458580682,0.106247508713654,
-5.90808733016713));
#276465=CARTESIAN_POINT('Ctrl Pts',(6.21213064517144,0.256247508713052,
-8.55026430761891));
#276466=CARTESIAN_POINT('Ctrl Pts',(3.10606532258571,0.40624750871245,-9.55948610871303));
#276467=CARTESIAN_POINT('Ctrl Pts',(-1.34451147939244E-14,0.556247508711849,
-10.5687079098071));
#276468=CARTESIAN_POINT('Ctrl Pts',(-3.10606532258574,0.706247508711247,
-9.55948610871303));
#276469=CARTESIAN_POINT('Ctrl Pts',(-6.21213064517146,0.856247508710645,
-8.55026430761891));
#276470=CARTESIAN_POINT('Ctrl Pts',(-8.13178458580685,1.00624750871004,
-5.90808733016712));
#276471=CARTESIAN_POINT('Ctrl Pts',(-10.0514385264422,1.15624750870944,
-3.26591035271534));
#276472=CARTESIAN_POINT('Ctrl Pts',(-10.0514385264422,1.30624750870884,
2.46189240364677E-15));
#276473=CARTESIAN_POINT('Ctrl Pts',(-10.0514385264422,1.45624750870824,
3.26591035271534));
#276474=CARTESIAN_POINT('Ctrl Pts',(-8.13178458580685,1.60624750870764,
5.90808733016713));
#276475=CARTESIAN_POINT('Ctrl Pts',(-6.21213064517146,1.75624750870705,
8.55026430761891));
#276476=CARTESIAN_POINT('Ctrl Pts',(-3.10606532258574,1.90624750870645,
9.55948610871303));
#276477=CARTESIAN_POINT('Ctrl Pts',(-1.17203825671816E-14,2.05624750870585,
10.5687079098071));
#276478=CARTESIAN_POINT('Ctrl Pts',(3.10606532258571,2.20624750870525,9.55948610871303));
#276479=CARTESIAN_POINT('Ctrl Pts',(6.21213064517144,2.35624750870465,8.55026430761891));
#276480=CARTESIAN_POINT('Ctrl Pts',(8.13178458580682,2.50624750870405,5.90808733016712));
#276481=CARTESIAN_POINT('Ctrl Pts',(10.0514385264422,2.65624750870345,3.26591035271534));
#276482=CARTESIAN_POINT('Ctrl Pts',(10.0514385264422,2.80624750870286,-1.23094620182339E-15));
#276483=CARTESIAN_POINT('Ctrl Pts',(10.0514385264422,2.95624750870225,-3.26591035271534));
#276484=CARTESIAN_POINT('Ctrl Pts',(8.13178458580682,3.10624750870165,-5.90808733016713));
#276485=CARTESIAN_POINT('Ctrl Pts',(6.21213064517143,3.25624750870105,-8.55026430761891));
#276486=CARTESIAN_POINT('Ctrl Pts',(3.10606532258571,3.40624750870045,-9.55948610871303));
#276487=CARTESIAN_POINT('Ctrl Pts',(-1.51728240655862E-14,3.55624750869985,
-10.5687079098071));
#276488=CARTESIAN_POINT('Ctrl Pts',(-3.10606532258574,3.70624750869925,
-9.55948610871303));
#276489=CARTESIAN_POINT('Ctrl Pts',(-6.21213064517146,3.85624750869865,
-8.55026430761891));
#276490=CARTESIAN_POINT('Ctrl Pts',(-8.13178458580685,4.00624750869804,
-5.90808733016712));
#276491=CARTESIAN_POINT('Ctrl Pts',(-10.0514385264422,4.15624750869744,
-3.26591035271534));
#276492=CARTESIAN_POINT('Ctrl Pts',(-10.0514385264422,4.30624750869684,
2.46189240364677E-15));
#276493=CARTESIAN_POINT('Ctrl Pts',(-10.0514385264422,4.45624750869624,
3.26591035271534));
#276494=CARTESIAN_POINT('Ctrl Pts',(-8.13178458580685,4.60624750869564,
5.90808733016713));
#276495=CARTESIAN_POINT('Ctrl Pts',(-6.21213064517146,4.75624750869505,
8.55026430761891));
#276496=CARTESIAN_POINT('Ctrl Pts',(-3.10606532258574,4.90624750869445,
9.55948610871303));
#276497=CARTESIAN_POINT('Ctrl Pts',(-1.34480918388434E-14,5.05624750869385,
10.5687079098071));
#276498=CARTESIAN_POINT('Ctrl Pts',(3.10606532258571,5.20624750869325,9.55948610871303));
#276499=CARTESIAN_POINT('Ctrl Pts',(6.21213064517144,5.35624750869265,8.55026430761891));
#276500=CARTESIAN_POINT('Ctrl Pts',(8.13178458580682,5.50624750869205,5.90808733016712));
#276501=CARTESIAN_POINT('Ctrl Pts',(10.0514385264422,5.65624750869145,3.26591035271534));
#276502=CARTESIAN_POINT('Ctrl Pts',(10.0514385264422,5.80624750869085,-1.23094620182339E-15));
#276503=CARTESIAN_POINT('Ctrl Pts',(10.0514385264422,5.95624750869025,-3.26591035271534));
#276504=CARTESIAN_POINT('Ctrl Pts',(8.13178458580682,6.10624750868966,-5.90808733016713));
#276505=CARTESIAN_POINT('Ctrl Pts',(6.21213064517143,6.25624750868905,-8.55026430761891));
#276506=CARTESIAN_POINT('Ctrl Pts',(3.10606532258571,6.40624750868845,-9.55948610871303));
#276507=CARTESIAN_POINT('Ctrl Pts',(-1.6900533337248E-14,6.55624750868785,
-10.5687079098071));
#276508=CARTESIAN_POINT('Ctrl Pts',(-3.10606532258574,6.70624750868725,
-9.55948610871303));
#276509=CARTESIAN_POINT('Ctrl Pts',(-6.21213064517146,6.85624750868664,
-8.55026430761891));
#276510=CARTESIAN_POINT('Ctrl Pts',(-8.13178458580685,7.00624750868604,
-5.90808733016712));
#276511=CARTESIAN_POINT('Ctrl Pts',(-10.0514385264422,7.15624750868544,
-3.26591035271534));
#276512=CARTESIAN_POINT('Ctrl Pts',(-10.0514385264422,7.30624750868484,
2.46189240364677E-15));
#276513=CARTESIAN_POINT('Ctrl Pts',(-10.0514385264422,7.45624750868424,
3.26591035271534));
#276514=CARTESIAN_POINT('Ctrl Pts',(-8.13178458580685,7.60624750868365,
5.90808733016713));
#276515=CARTESIAN_POINT('Ctrl Pts',(-6.21213064517146,7.75624750868305,
8.55026430761891));
#276516=CARTESIAN_POINT('Ctrl Pts',(-3.10606532258574,7.90624750868245,
9.55948610871303));
#276517=CARTESIAN_POINT('Ctrl Pts',(-1.51758011105052E-14,8.05624750868185,
10.5687079098071));
#276518=CARTESIAN_POINT('Ctrl Pts',(3.10606532258571,8.20624750868125,9.55948610871303));
#276519=CARTESIAN_POINT('Ctrl Pts',(6.21213064517143,8.35624750868065,8.55026430761891));
#276520=CARTESIAN_POINT('Ctrl Pts',(8.13178458580682,8.50624750868005,5.90808733016712));
#276521=CARTESIAN_POINT('Ctrl Pts',(10.0514385264422,8.65624750867945,3.26591035271534));
#276522=CARTESIAN_POINT('Ctrl Pts',(10.0514385264422,8.80624750867885,-1.23094620182339E-15));
#276523=CARTESIAN_POINT('Ctrl Pts',(10.0514385264422,8.95624750867826,-3.26591035271534));
#276524=CARTESIAN_POINT('Ctrl Pts',(8.13178458580681,9.10624750867765,-5.90808733016713));
#276525=CARTESIAN_POINT('Ctrl Pts',(6.21213064517143,9.25624750867705,-8.55026430761891));
#276526=CARTESIAN_POINT('Ctrl Pts',(3.10606532258571,9.40624750867645,-9.55948610871303));
#276527=CARTESIAN_POINT('Ctrl Pts',(-1.86282426089099E-14,9.55624750867585,
-10.5687079098071));
#276528=CARTESIAN_POINT('Ctrl Pts',(-3.10606532258574,9.70624750867525,
-9.55948610871303));
#276529=CARTESIAN_POINT('Ctrl Pts',(-6.21213064517147,9.85624750867465,
-8.55026430761891));
#276530=CARTESIAN_POINT('Ctrl Pts',(-8.13178458580685,10.006247508674,-5.90808733016712));
#276531=CARTESIAN_POINT('Ctrl Pts',(-10.0514385264422,10.1562475086734,
-3.26591035271534));
#276532=CARTESIAN_POINT('Ctrl Pts',(-10.0514385264422,10.3062475086728,
2.46189240364677E-15));
#276533=CARTESIAN_POINT('Ctrl Pts',(-10.0514385264422,10.4562475086722,
3.26591035271534));
#276534=CARTESIAN_POINT('Ctrl Pts',(-8.13178458580685,10.6062475086716,
5.90808733016713));
#276535=CARTESIAN_POINT('Ctrl Pts',(-6.21213064517146,10.756247508671,8.55026430761891));
#276536=CARTESIAN_POINT('Ctrl Pts',(-3.10606532258574,10.9062475086704,
9.55948610871303));
#276537=CARTESIAN_POINT('Ctrl Pts',(-1.69035103821671E-14,11.0562475086699,
10.5687079098071));
#276538=CARTESIAN_POINT('Ctrl Pts',(3.10606532258571,11.2062475086693,9.55948610871303));
#276539=CARTESIAN_POINT('Ctrl Pts',(6.21213064517143,11.3562475086687,8.55026430761891));
#276540=CARTESIAN_POINT('Ctrl Pts',(8.13178458580681,11.5062475086681,5.90808733016712));
#276541=CARTESIAN_POINT('Ctrl Pts',(10.0514385264422,11.6562475086675,3.26591035271534));
#276542=CARTESIAN_POINT('Ctrl Pts',(10.0514385264422,11.8062475086669,-1.23094620182339E-15));
#276543=CARTESIAN_POINT('Ctrl Pts',(10.0514385264422,11.9562475086663,-3.26591035271534));
#276544=CARTESIAN_POINT('Ctrl Pts',(8.13178458580681,12.1062475086657,-5.90808733016713));
#276545=CARTESIAN_POINT('Ctrl Pts',(6.21213064517143,12.2562475086651,-8.55026430761891));
#276546=CARTESIAN_POINT('Ctrl Pts',(3.1060653225857,12.4062475086645,-9.55948610871303));
#276547=CARTESIAN_POINT('Ctrl Pts',(-2.03559518805717E-14,12.5562475086638,
-10.5687079098071));
#276548=CARTESIAN_POINT('Ctrl Pts',(-3.10606532258575,12.7062475086632,
-9.55948610871303));
#276549=CARTESIAN_POINT('Ctrl Pts',(-6.21213064517147,12.8562475086626,
-8.55026430761891));
#276550=CARTESIAN_POINT('Ctrl Pts',(-8.13178458580686,13.006247508662,-5.90808733016712));
#276551=CARTESIAN_POINT('Ctrl Pts',(-10.0514385264422,13.1562475086614,
-3.26591035271534));
#276552=CARTESIAN_POINT('Ctrl Pts',(-10.0514385264422,13.3062475086608,
2.46189240364677E-15));
#276553=CARTESIAN_POINT('Ctrl Pts',(-10.0514385264422,13.4562475086602,
3.26591035271534));
#276554=CARTESIAN_POINT('Ctrl Pts',(-8.13178458580686,13.6062475086596,
5.90808733016713));
#276555=CARTESIAN_POINT('Ctrl Pts',(-6.21213064517146,13.756247508659,8.55026430761891));
#276556=CARTESIAN_POINT('Ctrl Pts',(-3.10606532258574,13.9062475086584,
9.55948610871303));
#276557=CARTESIAN_POINT('Ctrl Pts',(-1.86312196538289E-14,14.0562475086578,
10.5687079098071));
#276558=CARTESIAN_POINT('Ctrl Pts',(3.10606532258571,14.2062475086573,9.55948610871303));
#276559=CARTESIAN_POINT('Ctrl Pts',(6.21213064517143,14.3562475086567,8.55026430761891));
#276560=CARTESIAN_POINT('Ctrl Pts',(8.13178458580681,14.5062475086561,5.90808733016712));
#276561=CARTESIAN_POINT('Ctrl Pts',(10.0514385264422,14.6562475086555,3.26591035271534));
#276562=CARTESIAN_POINT('Ctrl Pts',(10.0514385264422,14.8062475086549,-1.23094620182339E-15));
#276563=CARTESIAN_POINT('Ctrl Pts',(10.0514385264422,14.9562475086543,-3.26591035271534));
#276564=CARTESIAN_POINT('Ctrl Pts',(8.13178458580681,15.1062475086537,-5.90808733016713));
#276565=CARTESIAN_POINT('Ctrl Pts',(6.21213064517143,15.2562475086531,-8.55026430761891));
#276566=CARTESIAN_POINT('Ctrl Pts',(3.1060653225857,15.4062475086525,-9.55948610871303));
#276567=CARTESIAN_POINT('Ctrl Pts',(-2.20836611522336E-14,15.5562475086518,
-10.5687079098071));
#276568=CARTESIAN_POINT('Ctrl Pts',(-3.10606532258575,15.7062475086513,
-9.55948610871303));
#276569=CARTESIAN_POINT('Ctrl Pts',(-6.21213064517147,15.8562475086506,
-8.55026430761891));
#276570=CARTESIAN_POINT('Ctrl Pts',(-8.13178458580686,16.00624750865,-5.90808733016712));
#276571=CARTESIAN_POINT('Ctrl Pts',(-10.0514385264422,16.1562475086494,
-3.26591035271534));
#276572=CARTESIAN_POINT('Ctrl Pts',(-10.0514385264422,16.3062475086488,
2.46189240364677E-15));
#276573=CARTESIAN_POINT('Ctrl Pts',(-10.0514385264422,16.4562475086482,
3.26591035271534));
#276574=CARTESIAN_POINT('Ctrl Pts',(-8.13178458580686,16.6062475086476,
5.90808733016713));
#276575=CARTESIAN_POINT('Ctrl Pts',(-6.21213064517147,16.756247508647,8.55026430761891));
#276576=CARTESIAN_POINT('Ctrl Pts',(-3.10606532258575,16.9062475086464,
9.55948610871303));
#276577=CARTESIAN_POINT('Ctrl Pts',(-2.03589289254908E-14,17.0562475086458,
10.5687079098071));
#276578=CARTESIAN_POINT('Ctrl Pts',(3.1060653225857,17.2062475086453,9.55948610871303));
#276579=CARTESIAN_POINT('Ctrl Pts',(6.21213064517143,17.3562475086446,8.55026430761891));
#276580=CARTESIAN_POINT('Ctrl Pts',(8.13178458580681,17.5062475086441,5.90808733016712));
#276581=CARTESIAN_POINT('Ctrl Pts',(10.0514385264422,17.6562475086435,3.26591035271534));
#276582=CARTESIAN_POINT('Ctrl Pts',(10.0514385264422,17.8062475086429,-1.23094620182339E-15));
#276583=CARTESIAN_POINT('Ctrl Pts',(10.0514385264422,17.9562475086423,-3.26591035271534));
#276584=CARTESIAN_POINT('Ctrl Pts',(8.13178458580681,18.1062475086417,-5.90808733016713));
#276585=CARTESIAN_POINT('Ctrl Pts',(6.21213064517142,18.2562475086411,-8.55026430761891));
#276586=CARTESIAN_POINT('Ctrl Pts',(3.1060653225857,18.4062475086405,-9.55948610871303));
#276587=CARTESIAN_POINT('Ctrl Pts',(-2.38113704238954E-14,18.5562475086398,
-10.5687079098071));
#276588=CARTESIAN_POINT('Ctrl Pts',(-3.10606532258575,18.7062475086392,
-9.55948610871303));
#276589=CARTESIAN_POINT('Ctrl Pts',(-6.21213064517147,18.8562475086386,
-8.55026430761891));
#276590=CARTESIAN_POINT('Ctrl Pts',(-8.13178458580686,19.006247508638,-5.90808733016712));
#276591=CARTESIAN_POINT('Ctrl Pts',(-10.0514385264422,19.1562475086374,
-3.26591035271534));
#276592=CARTESIAN_POINT('Ctrl Pts',(-10.0514385264422,19.3062475086368,
2.46189240364677E-15));
#276593=CARTESIAN_POINT('Ctrl Pts',(-10.0514385264422,19.4562475086362,
3.26591035271534));
#276594=CARTESIAN_POINT('Ctrl Pts',(-8.13178458580686,19.6062475086356,
5.90808733016713));
#276595=CARTESIAN_POINT('Ctrl Pts',(-6.21213064517147,19.756247508635,8.55026430761891));
#276596=CARTESIAN_POINT('Ctrl Pts',(-3.10606532258575,19.9062475086345,
9.55948610871303));
#276597=CARTESIAN_POINT('Ctrl Pts',(-2.20866381971526E-14,20.0562475086338,
10.5687079098071));
#276598=CARTESIAN_POINT('Ctrl Pts',(3.1060653225857,20.2062475086333,9.55948610871303));
#276599=CARTESIAN_POINT('Ctrl Pts',(6.21213064517142,20.3562475086326,8.55026430761891));
#276600=CARTESIAN_POINT('Ctrl Pts',(8.13178458580681,20.5062475086321,5.90808733016712));
#276601=CARTESIAN_POINT('Ctrl Pts',(10.0514385264422,20.6562475086315,3.26591035271534));
#276602=CARTESIAN_POINT('Ctrl Pts',(10.0514385264422,20.8062475086309,-1.23094620182339E-15));
#276603=CARTESIAN_POINT('Ctrl Pts',(10.0514385264422,20.9562475086302,-3.26591035271534));
#276604=CARTESIAN_POINT('Ctrl Pts',(8.13178458580681,21.1062475086297,-5.90808733016713));
#276605=CARTESIAN_POINT('Ctrl Pts',(6.21213064517142,21.256247508629,-8.55026430761891));
#276606=CARTESIAN_POINT('Ctrl Pts',(3.1060653225857,21.4062475086285,-9.55948610871303));
#276607=CARTESIAN_POINT('Ctrl Pts',(-2.55390796955572E-14,21.5562475086278,
-10.5687079098071));
#276608=CARTESIAN_POINT('Ctrl Pts',(-3.10606532258575,21.7062475086273,
-9.55948610871303));
#276609=CARTESIAN_POINT('Ctrl Pts',(-6.21213064517148,21.8562475086266,
-8.55026430761891));
#276610=CARTESIAN_POINT('Ctrl Pts',(-8.13178458580686,22.006247508626,-5.90808733016712));
#276611=CARTESIAN_POINT('Ctrl Pts',(-10.0514385264422,22.1562475086254,
-3.26591035271534));
#276612=CARTESIAN_POINT('Ctrl Pts',(-10.0514385264422,22.3062475086248,
2.46189240364677E-15));
#276613=CARTESIAN_POINT('Ctrl Pts',(-10.0514385264422,22.4562475086242,
3.26591035271534));
#276614=CARTESIAN_POINT('Ctrl Pts',(-8.13178458580686,22.6062475086236,
5.90808733016713));
#276615=CARTESIAN_POINT('Ctrl Pts',(-6.21213064517147,22.756247508623,8.55026430761891));
#276616=CARTESIAN_POINT('Ctrl Pts',(-3.10606532258575,22.9062475086224,
9.55948610871303));
#276617=CARTESIAN_POINT('Ctrl Pts',(-2.38143474688144E-14,23.0562475086218,
10.5687079098071));
#276618=CARTESIAN_POINT('Ctrl Pts',(3.1060653225857,23.2062475086213,9.55948610871303));
#276619=CARTESIAN_POINT('Ctrl Pts',(6.21213064517142,23.3562475086206,8.55026430761891));
#276620=CARTESIAN_POINT('Ctrl Pts',(8.13178458580681,23.5062475086201,5.90808733016712));
#276621=CARTESIAN_POINT('Ctrl Pts',(10.0514385264422,23.6562475086195,3.26591035271534));
#276622=CARTESIAN_POINT('Ctrl Pts',(10.0514385264422,23.8062475086189,-1.23094620182339E-15));
#276623=CARTESIAN_POINT('Ctrl Pts',(10.0514385264422,23.9562475086183,-3.26591035271534));
#276624=CARTESIAN_POINT('Ctrl Pts',(8.13178458580681,24.1062475086177,-5.90808733016713));
#276625=CARTESIAN_POINT('Ctrl Pts',(6.21213064517142,24.256247508617,-8.55026430761891));
#276626=CARTESIAN_POINT('Ctrl Pts',(3.1060653225857,24.4062475086165,-9.55948610871303));
#276627=CARTESIAN_POINT('Ctrl Pts',(-2.72667889672191E-14,24.5562475086158,
-10.5687079098071));
#276628=CARTESIAN_POINT('Ctrl Pts',(-3.10606532258575,24.7062475086152,
-9.55948610871303));
#276629=CARTESIAN_POINT('Ctrl Pts',(-6.21213064517148,24.8562475086146,
-8.55026430761891));
#276630=CARTESIAN_POINT('Ctrl Pts',(-8.13178458580686,25.006247508614,-5.90808733016712));
#276631=CARTESIAN_POINT('Ctrl Pts',(-10.0514385264422,25.1562475086134,
-3.26591035271534));
#276632=CARTESIAN_POINT('Ctrl Pts',(-10.0514385264422,25.3062475086128,
2.46189240364677E-15));
#276633=CARTESIAN_POINT('Ctrl Pts',(-10.0514385264422,25.4562475086122,
3.26591035271534));
#276634=CARTESIAN_POINT('Ctrl Pts',(-8.13178458580686,25.6062475086116,
5.90808733016713));
#276635=CARTESIAN_POINT('Ctrl Pts',(-6.21213064517148,25.756247508611,8.55026430761891));
#276636=CARTESIAN_POINT('Ctrl Pts',(-3.10606532258575,25.9062475086105,
9.55948610871303));
#276637=CARTESIAN_POINT('Ctrl Pts',(-2.55420567404763E-14,26.0562475086098,
10.5687079098071));
#276638=CARTESIAN_POINT('Ctrl Pts',(3.1060653225857,26.2062475086093,9.55948610871303));
#276639=CARTESIAN_POINT('Ctrl Pts',(6.21213064517142,26.3562475086086,8.55026430761891));
#276640=CARTESIAN_POINT('Ctrl Pts',(8.13178458580681,26.5062475086081,5.90808733016712));
#276641=CARTESIAN_POINT('Ctrl Pts',(10.0514385264422,26.6562475086075,3.26591035271534));
#276642=CARTESIAN_POINT('Ctrl Pts',(10.0514385264422,26.8062475086069,-1.23094620182339E-15));
#276643=CARTESIAN_POINT('Ctrl Pts',(10.0514385264422,26.9562475086063,-3.26591035271534));
#276644=CARTESIAN_POINT('Ctrl Pts',(8.13178458580681,27.1062475086057,-5.90808733016713));
#276645=CARTESIAN_POINT('Ctrl Pts',(6.21213064517142,27.256247508605,-8.55026430761891));
#276646=CARTESIAN_POINT('Ctrl Pts',(3.1060653225857,27.4062475086045,-9.55948610871303));
#276647=CARTESIAN_POINT('Ctrl Pts',(-2.89944982388809E-14,27.5562475086038,
-10.5687079098071));
#276648=CARTESIAN_POINT('Ctrl Pts',(-3.10606532258575,27.7062475086032,
-9.55948610871303));
#276649=CARTESIAN_POINT('Ctrl Pts',(-6.21213064517148,27.8562475086026,
-8.55026430761891));
#276650=CARTESIAN_POINT('Ctrl Pts',(-8.13178458580686,28.006247508602,-5.90808733016712));
#276651=CARTESIAN_POINT('Ctrl Pts',(-10.0514385264422,28.1562475086014,
-3.26591035271534));
#276652=CARTESIAN_POINT('Ctrl Pts',(-10.0514385264423,28.3062475086009,
2.46189240364677E-15));
#276653=CARTESIAN_POINT('Ctrl Pts',(-10.0514385264422,28.4562475086002,
3.26591035271534));
#276654=CARTESIAN_POINT('Ctrl Pts',(-8.13178458580686,28.6062475085996,
5.90808733016713));
#276655=CARTESIAN_POINT('Ctrl Pts',(-6.21213064517148,28.756247508599,8.55026430761891));
#276656=CARTESIAN_POINT('Ctrl Pts',(-3.10606532258575,28.9062475085985,
9.55948610871303));
#276657=CARTESIAN_POINT('Ctrl Pts',(-2.72697660121381E-14,29.0562475085978,
10.5687079098071));
#276658=CARTESIAN_POINT('Ctrl Pts',(3.1060653225857,29.2062475085973,9.55948610871303));
#276659=CARTESIAN_POINT('Ctrl Pts',(6.21213064517142,29.3562475085966,8.55026430761891));
#276660=CARTESIAN_POINT('Ctrl Pts',(8.13178458580681,29.5062475085961,5.90808733016712));
#276661=CARTESIAN_POINT('Ctrl Pts',(10.0514385264422,29.6562475085955,3.26591035271534));
#276662=CARTESIAN_POINT('Ctrl Pts',(10.0514385264422,29.8062475085949,-1.23094620182339E-15));
#276663=CARTESIAN_POINT('Ctrl Pts',(10.0514385264422,29.9562475085943,-3.26591035271534));
#276664=CARTESIAN_POINT('Ctrl Pts',(8.1317845858068,30.1062475085937,-5.90808733016713));
#276665=CARTESIAN_POINT('Ctrl Pts',(6.21213064517142,30.256247508593,-8.55026430761891));
#276666=CARTESIAN_POINT('Ctrl Pts',(3.10606532258569,30.4062475085925,-9.55948610871303));
#276667=CARTESIAN_POINT('Ctrl Pts',(-3.07222075105427E-14,30.5562475085918,
-10.5687079098071));
#276668=CARTESIAN_POINT('Ctrl Pts',(-3.10606532258576,30.7062475085912,
-9.55948610871303));
#276669=CARTESIAN_POINT('Ctrl Pts',(-6.21213064517148,30.8562475085907,
-8.55026430761891));
#276670=CARTESIAN_POINT('Ctrl Pts',(-8.13178458580687,31.00624750859,-5.90808733016712));
#276671=CARTESIAN_POINT('Ctrl Pts',(-10.0514385264422,31.1562475085894,
-3.26591035271534));
#276672=CARTESIAN_POINT('Ctrl Pts',(-10.0514385264423,31.3062475085889,
2.46189240364677E-15));
#276673=CARTESIAN_POINT('Ctrl Pts',(-10.0514385264422,31.4562475085882,
3.26591035271534));
#276674=CARTESIAN_POINT('Ctrl Pts',(-8.13178458580687,31.6062475085876,
5.90808733016713));
#276675=CARTESIAN_POINT('Ctrl Pts',(-6.21213064517148,31.756247508587,8.55026430761891));
#276676=CARTESIAN_POINT('Ctrl Pts',(-3.10606532258575,31.9062475085864,
9.55948610871303));
#276677=CARTESIAN_POINT('Ctrl Pts',(-2.89974752837999E-14,32.0562475085858,
10.5687079098071));
#276678=CARTESIAN_POINT('Ctrl Pts',(3.1060653225857,32.2062475085852,9.55948610871303));
#276679=CARTESIAN_POINT('Ctrl Pts',(6.21213064517142,32.3562475085847,8.55026430761891));
#276680=CARTESIAN_POINT('Ctrl Pts',(8.1317845858068,32.5062475085841,5.90808733016712));
#276681=CARTESIAN_POINT('Ctrl Pts',(10.0514385264422,32.6562475085834,3.26591035271534));
#276682=CARTESIAN_POINT('Ctrl Pts',(10.0514385264422,32.8062475085829,-1.23094620182339E-15));
#276683=CARTESIAN_POINT('Ctrl Pts',(10.0514385264422,32.9562475085823,-3.26591035271534));
#276684=CARTESIAN_POINT('Ctrl Pts',(8.1317845858068,33.1062475085817,-5.90808733016713));
#276685=CARTESIAN_POINT('Ctrl Pts',(6.21213064517142,33.256247508581,-8.55026430761891));
#276686=CARTESIAN_POINT('Ctrl Pts',(3.10606532258569,33.4062475085805,-9.55948610871303));
#276687=CARTESIAN_POINT('Ctrl Pts',(-3.24499167822046E-14,33.5562475085799,
-10.5687079098071));
#276688=CARTESIAN_POINT('Ctrl Pts',(-3.10606532258576,33.7062475085792,
-9.55948610871303));
#276689=CARTESIAN_POINT('Ctrl Pts',(-6.21213064517148,33.8562475085787,
-8.55026430761891));
#276690=CARTESIAN_POINT('Ctrl Pts',(-8.13178458580687,34.006247508578,-5.90808733016712));
#276691=CARTESIAN_POINT('Ctrl Pts',(-10.0514385264423,34.1562475085774,
-3.26591035271534));
#276692=CARTESIAN_POINT('Ctrl Pts',(-10.0514385264423,34.3062475085768,
2.46189240364677E-15));
#276693=CARTESIAN_POINT('Ctrl Pts',(-10.0514385264423,34.4562475085762,
3.26591035271534));
#276694=CARTESIAN_POINT('Ctrl Pts',(-8.13178458580687,34.6062475085756,
5.90808733016713));
#276695=CARTESIAN_POINT('Ctrl Pts',(-6.21213064517148,34.7562475085751,
8.55026430761891));
#276696=CARTESIAN_POINT('Ctrl Pts',(-3.10606532258576,34.9062475085744,
9.55948610871303));
#276697=CARTESIAN_POINT('Ctrl Pts',(-3.07251845554618E-14,35.0562475085739,
10.5687079098071));
#276698=CARTESIAN_POINT('Ctrl Pts',(3.10606532258569,35.2062475085733,9.55948610871303));
#276699=CARTESIAN_POINT('Ctrl Pts',(6.21213064517142,35.3562475085727,8.55026430761891));
#276700=CARTESIAN_POINT('Ctrl Pts',(8.1317845858068,35.5062475085721,5.90808733016712));
#276701=CARTESIAN_POINT('Ctrl Pts',(10.0514385264422,35.6562475085715,3.26591035271534));
#276702=CARTESIAN_POINT('Ctrl Pts',(10.0514385264422,35.8062475085709,-1.23094620182339E-15));
#276703=CARTESIAN_POINT('Ctrl Pts',(10.0514385264422,35.9562475085703,-3.26591035271534));
#276704=CARTESIAN_POINT('Ctrl Pts',(8.1317845858068,36.1062475085696,-5.90808733016713));
#276705=CARTESIAN_POINT('Ctrl Pts',(6.21213064517142,36.256247508569,-8.55026430761891));
#276706=CARTESIAN_POINT('Ctrl Pts',(3.10606532258569,36.4062475085685,-9.55948610871303));
#276707=CARTESIAN_POINT('Ctrl Pts',(-3.41776260538664E-14,36.5562475085678,
-10.5687079098071));
#276708=CARTESIAN_POINT('Ctrl Pts',(-3.10606532258576,36.7062475085672,
-9.55948610871303));
#276709=CARTESIAN_POINT('Ctrl Pts',(-6.21213064517148,36.8562475085666,
-8.55026430761891));
#276710=CARTESIAN_POINT('Ctrl Pts',(-8.13178458580687,37.006247508566,-5.90808733016712));
#276711=CARTESIAN_POINT('Ctrl Pts',(-10.0514385264423,37.1562475085654,
-3.26591035271534));
#276712=CARTESIAN_POINT('Ctrl Pts',(-10.0514385264423,37.3062475085648,
2.46189240364677E-15));
#276713=CARTESIAN_POINT('Ctrl Pts',(-10.0514385264423,37.4562475085642,
3.26591035271534));
#276714=CARTESIAN_POINT('Ctrl Pts',(-8.13178458580687,37.6062475085636,
5.90808733016713));
#276715=CARTESIAN_POINT('Ctrl Pts',(-6.21213064517148,37.756247508563,8.55026430761891));
#276716=CARTESIAN_POINT('Ctrl Pts',(-3.10606532258576,37.9062475085624,
9.55948610871303));
#276717=CARTESIAN_POINT('Ctrl Pts',(-3.24528938271236E-14,38.0562475085619,
10.5687079098071));
#276718=CARTESIAN_POINT('Ctrl Pts',(3.10606532258569,38.2062475085613,9.55948610871303));
#276719=CARTESIAN_POINT('Ctrl Pts',(6.21213064517142,38.3562475085607,8.55026430761891));
#276720=CARTESIAN_POINT('Ctrl Pts',(8.1317845858068,38.5062475085601,5.90808733016712));
#276721=CARTESIAN_POINT('Ctrl Pts',(10.0514385264422,38.6562475085595,3.26591035271534));
#276722=CARTESIAN_POINT('Ctrl Pts',(10.0514385264422,38.8062475085589,-1.23094620182339E-15));
#276723=CARTESIAN_POINT('Ctrl Pts',(10.0514385264422,38.9562475085582,-3.26591035271534));
#276724=CARTESIAN_POINT('Ctrl Pts',(8.1317845858068,39.1062475085576,-5.90808733016713));
#276725=CARTESIAN_POINT('Ctrl Pts',(6.21213064517141,39.2562475085571,-8.55026430761891));
#276726=CARTESIAN_POINT('Ctrl Pts',(3.10606532258569,39.4062475085565,-9.55948610871303));
#276727=CARTESIAN_POINT('Ctrl Pts',(-3.59053353255283E-14,39.5562475085559,
-10.5687079098071));
#276728=CARTESIAN_POINT('Ctrl Pts',(-3.10606532258576,39.7062475085552,
-9.55948610871303));
#276729=CARTESIAN_POINT('Ctrl Pts',(-6.21213064517148,39.8562475085546,
-8.55026430761891));
#276730=CARTESIAN_POINT('Ctrl Pts',(-8.13178458580687,40.0062475085541,
-5.90808733016712));
#276731=CARTESIAN_POINT('Ctrl Pts',(-10.0514385264423,40.1562475085534,
-3.26591035271534));
#276732=CARTESIAN_POINT('Ctrl Pts',(-10.0514385264423,40.3062475085529,
2.46189240364677E-15));
#276733=CARTESIAN_POINT('Ctrl Pts',(-10.0514385264423,40.4562475085523,
3.26591035271534));
#276734=CARTESIAN_POINT('Ctrl Pts',(-8.13178458580687,40.6062475085516,
5.90808733016713));
#276735=CARTESIAN_POINT('Ctrl Pts',(-6.21213064517148,40.756247508551,8.55026430761891));
#276736=CARTESIAN_POINT('Ctrl Pts',(-3.10606532258576,40.9062475085505,
9.55948610871303));
#276737=CARTESIAN_POINT('Ctrl Pts',(-3.41806030987855E-14,41.0562475085499,
10.5687079098071));
#276738=CARTESIAN_POINT('Ctrl Pts',(3.10606532258569,41.2062475085493,9.55948610871303));
#276739=CARTESIAN_POINT('Ctrl Pts',(6.21213064517141,41.3562475085487,8.55026430761891));
#276740=CARTESIAN_POINT('Ctrl Pts',(8.1317845858068,41.5062475085481,5.90808733016712));
#276741=CARTESIAN_POINT('Ctrl Pts',(10.0514385264422,41.6562475085475,3.26591035271534));
#276742=CARTESIAN_POINT('Ctrl Pts',(10.0514385264422,41.8062475085469,-1.23094620182339E-15));
#276743=CARTESIAN_POINT('Ctrl Pts',(10.0514385264422,41.9562475085463,-3.26591035271534));
#276744=CARTESIAN_POINT('Ctrl Pts',(8.1317845858068,42.1062475085457,-5.90808733016713));
#276745=CARTESIAN_POINT('Ctrl Pts',(6.21213064517141,42.256247508545,-8.55026430761891));
#276746=CARTESIAN_POINT('Ctrl Pts',(3.10606532258569,42.4062475085444,-9.55948610871303));
#276747=CARTESIAN_POINT('Ctrl Pts',(-3.76330445971901E-14,42.5562475085438,
-10.5687079098071));
#276748=CARTESIAN_POINT('Ctrl Pts',(-3.10606532258576,42.7062475085432,
-9.55948610871303));
#276749=CARTESIAN_POINT('Ctrl Pts',(-6.21213064517149,42.8562475085426,
-8.55026430761891));
#276750=CARTESIAN_POINT('Ctrl Pts',(-8.13178458580687,43.006247508542,-5.90808733016712));
#276751=CARTESIAN_POINT('Ctrl Pts',(-10.0514385264423,43.1562475085414,
-3.26591035271534));
#276752=CARTESIAN_POINT('Ctrl Pts',(-10.0514385264423,43.3062475085409,
2.46189240364677E-15));
#276753=CARTESIAN_POINT('Ctrl Pts',(-10.0514385264423,43.4562475085402,
3.26591035271534));
#276754=CARTESIAN_POINT('Ctrl Pts',(-8.13178458580687,43.6062475085397,
5.90808733016713));
#276755=CARTESIAN_POINT('Ctrl Pts',(-6.21213064517148,43.756247508539,8.55026430761891));
#276756=CARTESIAN_POINT('Ctrl Pts',(-3.10606532258576,43.9062475085384,
9.55948610871303));
#276757=CARTESIAN_POINT('Ctrl Pts',(-3.59083123704473E-14,44.0562475085379,
10.5687079098071));
#276758=CARTESIAN_POINT('Ctrl Pts',(3.10606532258569,44.2062475085373,9.55948610871303));
#276759=CARTESIAN_POINT('Ctrl Pts',(6.21213064517141,44.3562475085367,8.55026430761891));
#276760=CARTESIAN_POINT('Ctrl Pts',(8.1317845858068,44.5062475085361,5.90808733016712));
#276761=CARTESIAN_POINT('Ctrl Pts',(10.0514385264422,44.6562475085355,3.26591035271534));
#276762=CARTESIAN_POINT('Ctrl Pts',(10.0514385264422,44.8062475085349,-1.23094620182339E-15));
#276763=CARTESIAN_POINT('Ctrl Pts',(10.0514385264422,44.9562475085342,-3.26591035271534));
#276764=CARTESIAN_POINT('Ctrl Pts',(8.13178458580679,45.1062475085337,-5.90808733016713));
#276765=CARTESIAN_POINT('Ctrl Pts',(6.21213064517141,45.2562475085331,-8.55026430761891));
#276766=CARTESIAN_POINT('Ctrl Pts',(3.10606532258569,45.4062475085325,-9.55948610871303));
#276767=CARTESIAN_POINT('Ctrl Pts',(-3.93607538688519E-14,45.5562475085318,
-10.5687079098071));
#276768=CARTESIAN_POINT('Ctrl Pts',(-3.10606532258576,45.7062475085312,
-9.55948610871303));
#276769=CARTESIAN_POINT('Ctrl Pts',(-6.21213064517149,45.8562475085306,
-8.55026430761891));
#276770=CARTESIAN_POINT('Ctrl Pts',(-8.13178458580687,46.0062475085301,
-5.90808733016712));
#276771=CARTESIAN_POINT('Ctrl Pts',(-10.0514385264423,46.1562475085295,
-3.26591035271534));
#276772=CARTESIAN_POINT('Ctrl Pts',(-10.0514385264423,46.3062475085288,
2.46189240364677E-15));
#276773=CARTESIAN_POINT('Ctrl Pts',(-10.0514385264423,46.4562475085283,
3.26591035271534));
#276774=CARTESIAN_POINT('Ctrl Pts',(-8.13178458580687,46.6062475085277,
5.90808733016713));
#276775=CARTESIAN_POINT('Ctrl Pts',(-6.21213064517149,46.756247508527,8.55026430761891));
#276776=CARTESIAN_POINT('Ctrl Pts',(-3.10606532258576,46.9062475085265,
9.55948610871303));
#276777=CARTESIAN_POINT('Ctrl Pts',(-3.76360216421092E-14,47.0562475085259,
10.5687079098071));
#276778=CARTESIAN_POINT('Ctrl Pts',(3.10606532258569,47.2062475085253,9.55948610871303));
#276779=CARTESIAN_POINT('Ctrl Pts',(6.21213064517141,47.3562475085247,8.55026430761891));
#276780=CARTESIAN_POINT('Ctrl Pts',(8.13178458580679,47.5062475085241,5.90808733016712));
#276781=CARTESIAN_POINT('Ctrl Pts',(10.0514385264422,47.6562475085235,3.26591035271534));
#276782=CARTESIAN_POINT('Ctrl Pts',(10.0514385264422,47.8062475085229,-1.23094620182339E-15));
#276783=CARTESIAN_POINT('Ctrl Pts',(10.0514385264422,47.9562475085222,-3.26591035271534));
#276784=CARTESIAN_POINT('Ctrl Pts',(8.13178458580679,48.1062475085216,-5.90808733016713));
#276785=CARTESIAN_POINT('Ctrl Pts',(6.21213064517141,48.256247508521,-8.55026430761891));
#276786=CARTESIAN_POINT('Ctrl Pts',(3.10606532258568,48.4062475085205,-9.55948610871303));
#276787=CARTESIAN_POINT('Ctrl Pts',(-4.10884631405138E-14,48.5562475085198,
-10.5687079098071));
#276788=CARTESIAN_POINT('Ctrl Pts',(-3.10606532258577,48.7062475085193,
-9.55948610871303));
#276789=CARTESIAN_POINT('Ctrl Pts',(-6.21213064517149,48.8562475085186,
-8.55026430761891));
#276790=CARTESIAN_POINT('Ctrl Pts',(-8.13178458580688,49.006247508518,-5.90808733016712));
#276791=CARTESIAN_POINT('Ctrl Pts',(-10.0514385264423,49.1562475085174,
-3.26591035271534));
#276792=CARTESIAN_POINT('Ctrl Pts',(-10.0514385264423,49.3062475085168,
2.46189240364677E-15));
#276793=CARTESIAN_POINT('Ctrl Pts',(-10.0514385264423,49.4562475085162,
3.26591035271534));
#276794=CARTESIAN_POINT('Ctrl Pts',(-8.13178458580688,49.6062475085157,
5.90808733016713));
#276795=CARTESIAN_POINT('Ctrl Pts',(-6.21213064517149,49.7562475085151,
8.55026430761891));
#276796=CARTESIAN_POINT('Ctrl Pts',(-3.10606532258576,49.9062475085144,
9.55948610871303));
#276797=CARTESIAN_POINT('Ctrl Pts',(-3.9363730913771E-14,50.0562475085139,
10.5687079098071));
#276798=CARTESIAN_POINT('Ctrl Pts',(3.10606532258568,50.2062475085133,9.55948610871303));
#276799=CARTESIAN_POINT('Ctrl Pts',(6.21213064517141,50.3562475085127,8.55026430761891));
#276800=CARTESIAN_POINT('Ctrl Pts',(8.13178458580679,50.5062475085121,5.90808733016712));
#276801=CARTESIAN_POINT('Ctrl Pts',(10.0514385264422,50.6562475085115,3.26591035271534));
#276802=CARTESIAN_POINT('Ctrl Pts',(10.0514385264422,50.8062475085109,-1.23094620182339E-15));
#276803=CARTESIAN_POINT('Ctrl Pts',(10.0514385264422,50.9562475085102,-3.26591035271534));
#276804=CARTESIAN_POINT('Ctrl Pts',(8.13178458580679,51.1062475085097,-5.90808733016713));
#276805=CARTESIAN_POINT('Ctrl Pts',(6.21213064517141,51.256247508509,-8.55026430761891));
#276806=CARTESIAN_POINT('Ctrl Pts',(3.10606532258568,51.4062475085084,-9.55948610871303));
#276807=CARTESIAN_POINT('Ctrl Pts',(-4.28161724121756E-14,51.5562475085078,
-10.5687079098071));
#276808=CARTESIAN_POINT('Ctrl Pts',(-3.10606532258577,51.7062475085073,
-9.55948610871303));
#276809=CARTESIAN_POINT('Ctrl Pts',(-6.21213064517149,51.8562475085066,
-8.55026430761891));
#276810=CARTESIAN_POINT('Ctrl Pts',(-8.13178458580688,52.0062475085061,
-5.90808733016712));
#276811=CARTESIAN_POINT('Ctrl Pts',(-10.0514385264423,52.1562475085055,
-3.26591035271534));
#276812=CARTESIAN_POINT('Ctrl Pts',(-10.0514385264423,52.3062475085048,
2.46189240364677E-15));
#276813=CARTESIAN_POINT('Ctrl Pts',(-10.0514385264423,52.4562475085042,
3.26591035271534));
#276814=CARTESIAN_POINT('Ctrl Pts',(-8.13178458580688,52.6062475085036,
5.90808733016713));
#276815=CARTESIAN_POINT('Ctrl Pts',(-6.21213064517149,52.7562475085031,
8.55026430761891));
#276816=CARTESIAN_POINT('Ctrl Pts',(-3.10606532258577,52.9062475085025,
9.55948610871303));
#276817=CARTESIAN_POINT('Ctrl Pts',(-4.10914401854328E-14,53.0562475085018,
10.5687079098071));
#276818=CARTESIAN_POINT('Ctrl Pts',(3.10606532258568,53.2062475085012,9.55948610871303));
#276819=CARTESIAN_POINT('Ctrl Pts',(6.21213064517141,53.3562475085007,8.55026430761891));
#276820=CARTESIAN_POINT('Ctrl Pts',(8.13178458580679,53.5062475085001,5.90808733016712));
#276821=CARTESIAN_POINT('Ctrl Pts',(10.0514385264422,53.6562475084995,3.26591035271534));
#276822=CARTESIAN_POINT('Ctrl Pts',(10.0514385264422,53.8062475084989,-1.23094620182339E-15));
#276823=CARTESIAN_POINT('Ctrl Pts',(10.0514385264422,53.9562475084982,-3.26591035271534));
#276824=CARTESIAN_POINT('Ctrl Pts',(8.13178458580679,54.1062475084976,-5.90808733016713));
#276825=CARTESIAN_POINT('Ctrl Pts',(6.21213064517141,54.2562475084971,-8.55026430761891));
#276826=CARTESIAN_POINT('Ctrl Pts',(3.10606532258568,54.4062475084964,-9.55948610871303));
#276827=CARTESIAN_POINT('Ctrl Pts',(-4.45438816838375E-14,54.5562475084958,
-10.5687079098071));
#276828=CARTESIAN_POINT('Ctrl Pts',(-3.10606532258577,54.7062475084953,
-9.55948610871303));
#276829=CARTESIAN_POINT('Ctrl Pts',(-6.2121306451715,54.8562475084946,-8.55026430761891));
#276830=CARTESIAN_POINT('Ctrl Pts',(-8.13178458580688,55.0062475084941,
-5.90808733016712));
#276831=CARTESIAN_POINT('Ctrl Pts',(-10.0514385264423,55.1562475084934,
-3.26591035271534));
#276832=CARTESIAN_POINT('Ctrl Pts',(-10.0514385264423,55.3062475084929,
2.46189240364677E-15));
#276833=CARTESIAN_POINT('Ctrl Pts',(-10.0514385264423,55.4562475084922,
3.26591035271534));
#276834=CARTESIAN_POINT('Ctrl Pts',(-8.13178458580688,55.6062475084916,
5.90808733016713));
#276835=CARTESIAN_POINT('Ctrl Pts',(-6.21213064517149,55.756247508491,8.55026430761891));
#276836=CARTESIAN_POINT('Ctrl Pts',(-3.10606532258577,55.9062475084905,
9.55948610871303));
#276837=CARTESIAN_POINT('Ctrl Pts',(-4.28191494570947E-14,56.0562475084898,
10.5687079098071));
#276838=CARTESIAN_POINT('Ctrl Pts',(3.10606532258568,56.2062475084893,9.55948610871303));
#276839=CARTESIAN_POINT('Ctrl Pts',(6.21213064517141,56.3562475084887,8.55026430761891));
#276840=CARTESIAN_POINT('Ctrl Pts',(8.13178458580679,56.5062475084881,5.90808733016712));
#276841=CARTESIAN_POINT('Ctrl Pts',(10.0514385264422,56.6562475084875,3.26591035271534));
#276842=CARTESIAN_POINT('Ctrl Pts',(10.0514385264422,56.8062475084869,-1.23094620182339E-15));
#276843=CARTESIAN_POINT('Ctrl Pts',(10.0514385264422,56.9562475084863,-3.26591035271534));
#276844=CARTESIAN_POINT('Ctrl Pts',(8.13178458580679,57.1062475084857,-5.90808733016713));
#276845=CARTESIAN_POINT('Ctrl Pts',(6.2121306451714,57.256247508485,-8.55026430761891));
#276846=CARTESIAN_POINT('Ctrl Pts',(3.10606532258568,57.4062475084844,-9.55948610871303));
#276847=CARTESIAN_POINT('Ctrl Pts',(-4.62715909554993E-14,57.5562475084838,
-10.5687079098071));
#276848=CARTESIAN_POINT('Ctrl Pts',(-3.10606532258577,57.7062475084833,
-9.55948610871303));
#276849=CARTESIAN_POINT('Ctrl Pts',(-6.2121306451715,57.8562475084826,-8.55026430761891));
#276850=CARTESIAN_POINT('Ctrl Pts',(-8.13178458580688,58.006247508482,-5.90808733016712));
#276851=CARTESIAN_POINT('Ctrl Pts',(-10.0514385264423,58.1562475084814,
-3.26591035271534));
#276852=CARTESIAN_POINT('Ctrl Pts',(-10.0514385264423,58.3062475084808,
2.46189240364677E-15));
#276853=CARTESIAN_POINT('Ctrl Pts',(-10.0514385264423,58.4562475084802,
3.26591035271534));
#276854=CARTESIAN_POINT('Ctrl Pts',(-8.13178458580688,58.6062475084797,
5.90808733016713));
#276855=CARTESIAN_POINT('Ctrl Pts',(-6.21213064517149,58.756247508479,8.55026430761891));
#276856=CARTESIAN_POINT('Ctrl Pts',(-3.10606532258577,58.9062475084785,
9.55948610871303));
#276857=CARTESIAN_POINT('Ctrl Pts',(-4.45468587287565E-14,59.0562475084778,
10.5687079098071));
#276858=CARTESIAN_POINT('Ctrl Pts',(3.10606532258568,59.2062475084773,9.55948610871303));
#276859=CARTESIAN_POINT('Ctrl Pts',(6.2121306451714,59.3562475084766,8.55026430761891));
#276860=CARTESIAN_POINT('Ctrl Pts',(8.13178458580679,59.5062475084761,5.90808733016712));
#276861=CARTESIAN_POINT('Ctrl Pts',(10.0514385264422,59.6562475084754,3.26591035271534));
#276862=CARTESIAN_POINT('Ctrl Pts',(10.0514385264422,59.8062475084749,-1.23094620182339E-15));
#276863=CARTESIAN_POINT('Ctrl Pts',(10.0514385264422,59.9562475084742,-3.26591035271534));
#276864=CARTESIAN_POINT('Ctrl Pts',(8.13178458580678,60.1062475084737,-5.90808733016713));
#276865=CARTESIAN_POINT('Ctrl Pts',(6.2121306451714,60.2562475084731,-8.55026430761891));
#276866=CARTESIAN_POINT('Ctrl Pts',(3.10606532258568,60.4062475084725,-9.55948610871303));
#276867=CARTESIAN_POINT('Ctrl Pts',(-4.79993002271612E-14,60.5562475084718,
-10.5687079098071));
#276868=CARTESIAN_POINT('Ctrl Pts',(-3.10606532258577,60.7062475084712,
-9.55948610871303));
#276869=CARTESIAN_POINT('Ctrl Pts',(-6.2121306451715,60.8562475084706,-8.55026430761891));
#276870=CARTESIAN_POINT('Ctrl Pts',(-8.13178458580688,61.00624750847,-5.90808733016712));
#276871=CARTESIAN_POINT('Ctrl Pts',(-10.0514385264423,61.1562475084694,
-3.26591035271534));
#276872=CARTESIAN_POINT('Ctrl Pts',(-10.0514385264423,61.3062475084689,
2.46189240364677E-15));
#276873=CARTESIAN_POINT('Ctrl Pts',(-10.0514385264423,61.4562475084682,
3.26591035271534));
#276874=CARTESIAN_POINT('Ctrl Pts',(-8.13178458580688,61.6062475084676,
5.90808733016713));
#276875=CARTESIAN_POINT('Ctrl Pts',(-6.2121306451715,61.756247508467,8.55026430761891));
#276876=CARTESIAN_POINT('Ctrl Pts',(-3.10606532258577,61.9062475084664,
9.55948610871303));
#276877=CARTESIAN_POINT('Ctrl Pts',(-4.62745680004183E-14,62.0562475084658,
10.5687079098071));
#276878=CARTESIAN_POINT('Ctrl Pts',(3.10606532258568,62.2062475084653,9.55948610871303));
#276879=CARTESIAN_POINT('Ctrl Pts',(6.2121306451714,62.3562475084646,8.55026430761891));
#276880=CARTESIAN_POINT('Ctrl Pts',(8.13178458580678,62.5062475084641,5.90808733016712));
#276881=CARTESIAN_POINT('Ctrl Pts',(10.0514385264422,62.6562475084635,3.26591035271534));
#276882=CARTESIAN_POINT('Ctrl Pts',(10.0514385264422,62.8062475084629,-1.23094620182339E-15));
#276883=CARTESIAN_POINT('Ctrl Pts',(10.0514385264422,62.9562475084623,-3.26591035271534));
#276884=CARTESIAN_POINT('Ctrl Pts',(8.13178458580678,63.1062475084617,-5.90808733016713));
#276885=CARTESIAN_POINT('Ctrl Pts',(6.2121306451714,63.2562475084611,-8.55026430761891));
#276886=CARTESIAN_POINT('Ctrl Pts',(3.10606532258567,63.4062475084604,-9.55948610871303));
#276887=CARTESIAN_POINT('Ctrl Pts',(-4.9727009498823E-14,63.5562475084598,
-10.5687079098071));
#276888=CARTESIAN_POINT('Ctrl Pts',(-3.10606532258578,63.7062475084593,
-9.55948610871303));
#276889=CARTESIAN_POINT('Ctrl Pts',(-6.2121306451715,63.8562475084587,-8.55026430761891));
#276890=CARTESIAN_POINT('Ctrl Pts',(-8.13178458580689,64.006247508458,-5.90808733016712));
#276891=CARTESIAN_POINT('Ctrl Pts',(-10.0514385264423,64.1562475084574,
-3.26591035271534));
#276892=CARTESIAN_POINT('Ctrl Pts',(-10.0514385264423,64.3062475084568,
2.46189240364677E-15));
#276893=CARTESIAN_POINT('Ctrl Pts',(-10.0514385264423,64.4562475084562,
3.26591035271534));
#276894=CARTESIAN_POINT('Ctrl Pts',(-8.13178458580689,64.6062475084557,
5.90808733016713));
#276895=CARTESIAN_POINT('Ctrl Pts',(-6.2121306451715,64.7562475084551,8.55026430761891));
#276896=CARTESIAN_POINT('Ctrl Pts',(-3.10606532258577,64.9062475084545,
9.55948610871303));
#276897=CARTESIAN_POINT('Ctrl Pts',(-4.80022772720802E-14,65.0562475084539,
10.5687079098071));
#276898=CARTESIAN_POINT('Ctrl Pts',(3.10606532258568,65.2062475084533,9.55948610871303));
#276899=CARTESIAN_POINT('Ctrl Pts',(6.2121306451714,65.3562475084527,8.55026430761891));
#276900=CARTESIAN_POINT('Ctrl Pts',(8.13178458580678,65.506247508452,5.90808733016712));
#276901=CARTESIAN_POINT('Ctrl Pts',(10.0514385264422,65.6562475084515,3.26591035271534));
#276902=CARTESIAN_POINT('Ctrl Pts',(10.0514385264422,65.8062475084509,-1.23094620182339E-15));
#276903=CARTESIAN_POINT('Ctrl Pts',(10.0514385264422,65.9562475084503,-3.26591035271534));
#276904=CARTESIAN_POINT('Ctrl Pts',(8.13178458580678,66.1062475084497,-5.90808733016713));
#276905=CARTESIAN_POINT('Ctrl Pts',(6.2121306451714,66.2562475084491,-8.55026430761891));
#276906=CARTESIAN_POINT('Ctrl Pts',(3.10606532258567,66.4062475084485,-9.55948610871303));
#276907=CARTESIAN_POINT('Ctrl Pts',(-5.14547187704848E-14,66.5562475084479,
-10.5687079098071));
#276908=CARTESIAN_POINT('Ctrl Pts',(-3.10606532258578,66.7062475084472,
-9.55948610871303));
#276909=CARTESIAN_POINT('Ctrl Pts',(-6.2121306451715,66.8562475084467,-8.55026430761891));
#276910=CARTESIAN_POINT('Ctrl Pts',(-8.13178458580689,67.0062475084461,
-5.90808733016712));
#276911=CARTESIAN_POINT('Ctrl Pts',(-10.0514385264423,67.1562475084454,
-3.26591035271534));
#276912=CARTESIAN_POINT('Ctrl Pts',(-10.0514385264423,67.3062475084448,
2.46189240364677E-15));
#276913=CARTESIAN_POINT('Ctrl Pts',(-10.0514385264423,67.4562475084442,
3.26591035271534));
#276914=CARTESIAN_POINT('Ctrl Pts',(-8.13178458580689,67.6062475084436,
5.90808733016713));
#276915=CARTESIAN_POINT('Ctrl Pts',(-6.2121306451715,67.7562475084431,8.55026430761891));
#276916=CARTESIAN_POINT('Ctrl Pts',(-3.10606532258578,67.9062475084425,
9.55948610871303));
#276917=CARTESIAN_POINT('Ctrl Pts',(-4.9729986543742E-14,68.0562475084418,
10.5687079098071));
#276918=CARTESIAN_POINT('Ctrl Pts',(3.10606532258567,68.2062475084413,9.55948610871303));
#276919=CARTESIAN_POINT('Ctrl Pts',(6.2121306451714,68.3562475084406,8.55026430761891));
#276920=CARTESIAN_POINT('Ctrl Pts',(8.13178458580678,68.5062475084401,5.90808733016712));
#276921=CARTESIAN_POINT('Ctrl Pts',(10.0514385264422,68.6562475084394,3.26591035271534));
#276922=CARTESIAN_POINT('Ctrl Pts',(10.0514385264422,68.8062475084389,-1.23094620182339E-15));
#276923=CARTESIAN_POINT('Ctrl Pts',(10.0514385264422,68.9562475084383,-3.26591035271534));
#276924=CARTESIAN_POINT('Ctrl Pts',(8.13178458580678,69.1062475084377,-5.90808733016713));
#276925=CARTESIAN_POINT('Ctrl Pts',(6.2121306451714,69.2562475084371,-8.55026430761891));
#276926=CARTESIAN_POINT('Ctrl Pts',(3.10606532258567,69.4062475084365,-9.55948610871303));
#276927=CARTESIAN_POINT('Ctrl Pts',(-5.31824280421467E-14,69.5562475084359,
-10.5687079098071));
#276928=CARTESIAN_POINT('Ctrl Pts',(-3.10606532258578,69.7062475084353,
-9.55948610871303));
#276929=CARTESIAN_POINT('Ctrl Pts',(-6.2121306451715,69.8562475084346,-8.55026430761891));
#276930=CARTESIAN_POINT('Ctrl Pts',(-8.13178458580689,70.006247508434,-5.90808733016712));
#276931=CARTESIAN_POINT('Ctrl Pts',(-10.0514385264423,70.1562475084334,
-3.26591035271534));
#276932=CARTESIAN_POINT('Ctrl Pts',(-10.0514385264423,70.3062475084328,
2.46189240364677E-15));
#276933=CARTESIAN_POINT('Ctrl Pts',(-10.0514385264423,70.4562475084322,
3.26591035271534));
#276934=CARTESIAN_POINT('Ctrl Pts',(-8.13178458580689,70.6062475084316,
5.90808733016713));
#276935=CARTESIAN_POINT('Ctrl Pts',(-6.2121306451715,70.756247508431,8.55026430761891));
#276936=CARTESIAN_POINT('Ctrl Pts',(-3.10606532258578,70.9062475084305,
9.55948610871303));
#276937=CARTESIAN_POINT('Ctrl Pts',(-5.14576958154038E-14,71.0562475084299,
10.5687079098071));
#276938=CARTESIAN_POINT('Ctrl Pts',(3.10606532258567,71.2062475084292,9.55948610871303));
#276939=CARTESIAN_POINT('Ctrl Pts',(6.2121306451714,71.3562475084287,8.55026430761891));
#276940=CARTESIAN_POINT('Ctrl Pts',(8.13178458580678,71.506247508428,5.90808733016712));
#276941=CARTESIAN_POINT('Ctrl Pts',(10.0514385264422,71.6562475084275,3.26591035271534));
#276942=CARTESIAN_POINT('Ctrl Pts',(10.0514385264422,71.8062475084268,-1.23094620182339E-15));
#276943=CARTESIAN_POINT('Ctrl Pts',(10.0514385264422,71.9562475084263,-3.26591035271534));
#276944=CARTESIAN_POINT('Ctrl Pts',(8.13178458580678,72.1062475084257,-5.90808733016713));
#276945=CARTESIAN_POINT('Ctrl Pts',(6.21213064517139,72.2562475084251,-8.55026430761891));
#276946=CARTESIAN_POINT('Ctrl Pts',(3.10606532258567,72.4062475084245,-9.55948610871303));
#276947=CARTESIAN_POINT('Ctrl Pts',(-5.49101373138085E-14,72.5562475084239,
-10.5687079098071));
#276948=CARTESIAN_POINT('Ctrl Pts',(-3.10606532258578,72.7062475084233,
-9.55948610871303));
#276949=CARTESIAN_POINT('Ctrl Pts',(-6.2121306451715,72.8562475084227,-8.55026430761891));
#276950=CARTESIAN_POINT('Ctrl Pts',(-8.13178458580689,73.006247508422,-5.90808733016712));
#276951=CARTESIAN_POINT('Ctrl Pts',(-10.0514385264423,73.1562475084214,
-3.26591035271534));
#276952=CARTESIAN_POINT('Ctrl Pts',(-10.0514385264423,73.3062475084208,
2.46189240364677E-15));
#276953=CARTESIAN_POINT('Ctrl Pts',(-10.0514385264423,73.4562475084202,
3.26591035271534));
#276954=CARTESIAN_POINT('Ctrl Pts',(-8.13178458580689,73.6062475084196,
5.90808733016713));
#276955=CARTESIAN_POINT('Ctrl Pts',(-6.2121306451715,73.7562475084191,8.55026430761891));
#276956=CARTESIAN_POINT('Ctrl Pts',(-3.10606532258578,73.9062475084185,
9.55948610871303));
#276957=CARTESIAN_POINT('Ctrl Pts',(-5.31854050870657E-14,74.0562475084179,
10.5687079098071));
#276958=CARTESIAN_POINT('Ctrl Pts',(3.10606532258567,74.2062475084172,9.55948610871303));
#276959=CARTESIAN_POINT('Ctrl Pts',(6.21213064517139,74.3562475084167,8.55026430761891));
#276960=CARTESIAN_POINT('Ctrl Pts',(8.13178458580678,74.5062475084161,5.90808733016712));
#276961=CARTESIAN_POINT('Ctrl Pts',(10.0514385264422,74.6562475084154,3.26591035271534));
#276962=CARTESIAN_POINT('Ctrl Pts',(10.0514385264422,74.8062475084149,-1.23094620182339E-15));
#276963=CARTESIAN_POINT('Ctrl Pts',(10.0514385264422,74.9562475084143,-3.26591035271534));
#276964=CARTESIAN_POINT('Ctrl Pts',(8.13178458580678,75.1062475084136,-5.90808733016713));
#276965=CARTESIAN_POINT('Ctrl Pts',(6.21213064517139,75.256247508413,-8.55026430761891));
#276966=CARTESIAN_POINT('Ctrl Pts',(3.10606532258567,75.4062475084124,-9.55948610871303));
#276967=CARTESIAN_POINT('Ctrl Pts',(-5.66378465854703E-14,75.5562475084119,
-10.5687079098071));
#276968=CARTESIAN_POINT('Ctrl Pts',(-3.10606532258578,75.7062475084113,
-9.55948610871303));
#276969=CARTESIAN_POINT('Ctrl Pts',(-6.21213064517151,75.8562475084106,
-8.55026430761891));
#276970=CARTESIAN_POINT('Ctrl Pts',(-8.13178458580689,76.00624750841,-5.90808733016712));
#276971=CARTESIAN_POINT('Ctrl Pts',(-10.0514385264423,76.1562475084095,
-3.26591035271534));
#276972=CARTESIAN_POINT('Ctrl Pts',(-10.0514385264423,76.3062475084089,
2.46189240364677E-15));
#276973=CARTESIAN_POINT('Ctrl Pts',(-10.0514385264423,76.4562475084082,
3.26591035271534));
#276974=CARTESIAN_POINT('Ctrl Pts',(-8.13178458580689,76.6062475084076,
5.90808733016713));
#276975=CARTESIAN_POINT('Ctrl Pts',(-6.2121306451715,76.7562475084071,8.55026430761891));
#276976=CARTESIAN_POINT('Ctrl Pts',(-3.10606532258578,76.9062475084065,
9.55948610871303));
#276977=CARTESIAN_POINT('Ctrl Pts',(-5.49131143587276E-14,77.0562475084058,
10.5687079098071));
#276978=CARTESIAN_POINT('Ctrl Pts',(3.10606532258567,77.2062475084053,9.55948610871303));
#276979=CARTESIAN_POINT('Ctrl Pts',(6.21213064517139,77.3562475084047,8.55026430761891));
#276980=CARTESIAN_POINT('Ctrl Pts',(8.13178458580678,77.506247508404,5.90808733016712));
#276981=CARTESIAN_POINT('Ctrl Pts',(10.0514385264422,77.6562475084034,3.26591035271534));
#276982=CARTESIAN_POINT('Ctrl Pts',(10.0514385264422,77.8062475084029,-1.23094620182339E-15));
#276983=CARTESIAN_POINT('Ctrl Pts',(10.0514385264422,77.9562475084023,-3.26591035271534));
#276984=CARTESIAN_POINT('Ctrl Pts',(8.13178458580678,78.1062475084017,-5.90808733016713));
#276985=CARTESIAN_POINT('Ctrl Pts',(6.21213064517139,78.256247508401,-8.55026430761891));
#276986=CARTESIAN_POINT('Ctrl Pts',(3.10606532258567,78.4062475084005,-9.55948610871303));
#276987=CARTESIAN_POINT('Ctrl Pts',(-5.83655558571322E-14,78.5562475083999,
-10.5687079098071));
#276988=CARTESIAN_POINT('Ctrl Pts',(-3.10606532258578,78.7062475083993,
-9.55948610871303));
#276989=CARTESIAN_POINT('Ctrl Pts',(-6.21213064517151,78.8562475083986,
-8.55026430761891));
#276990=CARTESIAN_POINT('Ctrl Pts',(-8.13178458580689,79.006247508398,-5.90808733016712));
#276991=CARTESIAN_POINT('Ctrl Pts',(-10.0514385264423,79.1562475083975,
-3.26591035271534));
#276992=CARTESIAN_POINT('Ctrl Pts',(-10.0514385264423,79.3062475083968,
2.46189240364677E-15));
#276993=CARTESIAN_POINT('Ctrl Pts',(-10.0514385264423,79.4562475083962,
3.26591035271534));
#276994=CARTESIAN_POINT('Ctrl Pts',(-8.13178458580689,79.6062475083957,
5.90808733016713));
#276995=CARTESIAN_POINT('Ctrl Pts',(-6.21213064517151,79.7562475083951,
8.55026430761891));
#276996=CARTESIAN_POINT('Ctrl Pts',(-3.10606532258578,79.9062475083944,
9.55948610871303));
#276997=CARTESIAN_POINT('Ctrl Pts',(-5.66408236303894E-14,80.0562475083938,
10.5687079098071));
#276998=CARTESIAN_POINT('Ctrl Pts',(3.10606532258567,80.2062475083933,9.55948610871303));
#276999=CARTESIAN_POINT('Ctrl Pts',(6.21213064517139,80.3562475083926,8.55026430761891));
#277000=CARTESIAN_POINT('Ctrl Pts',(8.13178458580678,80.5062475083921,5.90808733016712));
#277001=CARTESIAN_POINT('Ctrl Pts',(10.0514385264422,80.6562475083914,3.26591035271534));
#277002=CARTESIAN_POINT('Ctrl Pts',(10.0514385264422,80.8062475083909,-1.23094620182339E-15));
#277003=CARTESIAN_POINT('Ctrl Pts',(10.0514385264422,80.9562475083902,-3.26591035271534));
#277004=CARTESIAN_POINT('Ctrl Pts',(8.13178458580678,81.1062475083897,-5.90808733016713));
#277005=CARTESIAN_POINT('Ctrl Pts',(6.21213064517139,81.256247508389,-8.55026430761891));
#277006=CARTESIAN_POINT('Ctrl Pts',(3.10606532258566,81.4062475083885,-9.55948610871303));
#277007=CARTESIAN_POINT('Ctrl Pts',(-6.0093265128794E-14,81.5562475083879,
-10.5687079098071));
#277008=CARTESIAN_POINT('Ctrl Pts',(-3.10606532258579,81.7062475083873,
-9.55948610871303));
#277009=CARTESIAN_POINT('Ctrl Pts',(-6.21213064517151,81.8562475083866,
-8.55026430761891));
#277010=CARTESIAN_POINT('Ctrl Pts',(-8.13178458580689,82.0062475083861,
-5.90808733016712));
#277011=CARTESIAN_POINT('Ctrl Pts',(-10.0514385264423,82.1562475083854,
-3.26591035271534));
#277012=CARTESIAN_POINT('Ctrl Pts',(-10.0514385264423,82.3062475083849,
2.46189240364677E-15));
#277013=CARTESIAN_POINT('Ctrl Pts',(-10.0514385264423,82.4562475083842,
3.26591035271534));
#277014=CARTESIAN_POINT('Ctrl Pts',(-8.13178458580689,82.6062475083837,
5.90808733016713));
#277015=CARTESIAN_POINT('Ctrl Pts',(-6.21213064517151,82.7562475083831,
8.55026430761891));
#277016=CARTESIAN_POINT('Ctrl Pts',(-3.10606532258578,82.9062475083825,
9.55948610871303));
#277017=CARTESIAN_POINT('Ctrl Pts',(-5.83685329020512E-14,83.0562475083818,
10.5687079098071));
#277018=CARTESIAN_POINT('Ctrl Pts',(3.10606532258567,83.2062475083812,9.55948610871303));
#277019=CARTESIAN_POINT('Ctrl Pts',(6.21213064517139,83.3562475083806,8.55026430761891));
#277020=CARTESIAN_POINT('Ctrl Pts',(8.13178458580677,83.5062475083801,5.90808733016712));
#277021=CARTESIAN_POINT('Ctrl Pts',(10.0514385264422,83.6562475083795,3.26591035271534));
#277022=CARTESIAN_POINT('Ctrl Pts',(10.0514385264422,83.8062475083788,-1.23094620182339E-15));
#277023=CARTESIAN_POINT('Ctrl Pts',(10.0514385264422,83.9562475083783,-3.26591035271534));
#277024=CARTESIAN_POINT('Ctrl Pts',(8.13178458580677,84.1062475083777,-5.90808733016713));
#277025=CARTESIAN_POINT('Ctrl Pts',(6.21213064517139,84.256247508377,-8.55026430761891));
#277026=CARTESIAN_POINT('Ctrl Pts',(3.10606532258566,84.4062475083765,-9.55948610871303));
#277027=CARTESIAN_POINT('Ctrl Pts',(-6.18209744004559E-14,84.5562475083758,
-10.5687079098071));
#277028=CARTESIAN_POINT('Ctrl Pts',(-3.10606532258579,84.7062475083753,
-9.55948610871303));
#277029=CARTESIAN_POINT('Ctrl Pts',(-6.21213064517151,84.8562475083747,
-8.55026430761891));
#277030=CARTESIAN_POINT('Ctrl Pts',(-8.1317845858069,85.006247508374,-5.90808733016712));
#277031=CARTESIAN_POINT('Ctrl Pts',(-10.0514385264423,85.1562475083734,
-3.26591035271534));
#277032=CARTESIAN_POINT('Ctrl Pts',(-10.0514385264423,85.3062475083728,
2.46189240364677E-15));
#277033=CARTESIAN_POINT('Ctrl Pts',(-10.0514385264423,85.4562475083722,
3.26591035271534));
#277034=CARTESIAN_POINT('Ctrl Pts',(-8.1317845858069,85.6062475083716,5.90808733016713));
#277035=CARTESIAN_POINT('Ctrl Pts',(-6.21213064517151,85.7562475083711,
8.55026430761891));
#277036=CARTESIAN_POINT('Ctrl Pts',(-3.10606532258578,85.9062475083705,
9.55948610871303));
#277037=CARTESIAN_POINT('Ctrl Pts',(-6.00962421737131E-14,86.0562475083699,
10.5687079098071));
#277038=CARTESIAN_POINT('Ctrl Pts',(3.10606532258566,86.2062475083693,9.55948610871303));
#277039=CARTESIAN_POINT('Ctrl Pts',(6.21213064517139,86.3562475083687,8.55026430761891));
#277040=CARTESIAN_POINT('Ctrl Pts',(8.13178458580677,86.506247508368,5.90808733016712));
#277041=CARTESIAN_POINT('Ctrl Pts',(10.0514385264422,86.6562475083674,3.26591035271534));
#277042=CARTESIAN_POINT('Ctrl Pts',(10.0514385264422,86.8062475083669,-1.23094620182339E-15));
#277043=CARTESIAN_POINT('Ctrl Pts',(10.0514385264422,86.9562475083663,-3.26591035271534));
#277044=CARTESIAN_POINT('Ctrl Pts',(8.13178458580677,87.1062475083657,-5.90808733016713));
#277045=CARTESIAN_POINT('Ctrl Pts',(6.21213064517139,87.256247508365,-8.55026430761891));
#277046=CARTESIAN_POINT('Ctrl Pts',(3.10606532258566,87.4062475083645,-9.55948610871303));
#277047=CARTESIAN_POINT('Ctrl Pts',(-6.35486836721177E-14,87.5562475083638,
-10.5687079098071));
#277048=CARTESIAN_POINT('Ctrl Pts',(-3.10606532258579,87.7062475083633,
-9.55948610871303));
#277049=CARTESIAN_POINT('Ctrl Pts',(-6.21213064517151,87.8562475083626,
-8.55026430761891));
#277050=CARTESIAN_POINT('Ctrl Pts',(-8.1317845858069,88.0062475083621,-5.90808733016712));
#277051=CARTESIAN_POINT('Ctrl Pts',(-10.0514385264423,88.1562475083614,
-3.26591035271534));
#277052=CARTESIAN_POINT('Ctrl Pts',(-10.0514385264423,88.3062475083609,
2.46189240364677E-15));
#277053=CARTESIAN_POINT('Ctrl Pts',(-10.0514385264423,88.4562475083602,
3.26591035271534));
#277054=CARTESIAN_POINT('Ctrl Pts',(-8.1317845858069,88.6062475083597,5.90808733016713));
#277055=CARTESIAN_POINT('Ctrl Pts',(-6.21213064517151,88.7562475083591,
8.55026430761891));
#277056=CARTESIAN_POINT('Ctrl Pts',(-3.10606532258579,88.9062475083585,
9.55948610871303));
#277057=CARTESIAN_POINT('Ctrl Pts',(-6.18239514453749E-14,89.0562475083578,
10.5687079098071));
#277058=CARTESIAN_POINT('Ctrl Pts',(3.10606532258566,89.2062475083573,9.55948610871303));
#277059=CARTESIAN_POINT('Ctrl Pts',(6.21213064517139,89.3562475083567,8.55026430761891));
#277060=CARTESIAN_POINT('Ctrl Pts',(8.13178458580677,89.5062475083561,5.90808733016712));
#277061=CARTESIAN_POINT('Ctrl Pts',(10.0514385264422,89.6562475083554,3.26591035271534));
#277062=CARTESIAN_POINT('Ctrl Pts',(10.0514385264422,89.8062475083549,-1.23094620182339E-15));
#277063=CARTESIAN_POINT('Ctrl Pts',(10.0514385264422,89.9562475083543,-3.26591035271534));
#277064=CARTESIAN_POINT('Ctrl Pts',(8.13178458580677,90.1062475083536,-5.90808733016713));
#277065=CARTESIAN_POINT('Ctrl Pts',(6.21213064517138,90.256247508353,-8.55026430761891));
#277066=CARTESIAN_POINT('Ctrl Pts',(3.10606532258566,90.4062475083525,-9.55948610871303));
#277067=CARTESIAN_POINT('Ctrl Pts',(-6.52763929437795E-14,90.5562475083518,
-10.5687079098071));
#277068=CARTESIAN_POINT('Ctrl Pts',(-3.10606532258579,90.7062475083512,
-9.55948610871303));
#277069=CARTESIAN_POINT('Ctrl Pts',(-6.21213064517151,90.8562475083506,
-8.55026430761891));
#277070=CARTESIAN_POINT('Ctrl Pts',(-8.1317845858069,91.00624750835,-5.90808733016712));
#277071=CARTESIAN_POINT('Ctrl Pts',(-10.0514385264423,91.1562475083494,
-3.26591035271534));
#277072=CARTESIAN_POINT('Ctrl Pts',(-10.0514385264423,91.3062475083488,
2.46189240364677E-15));
#277073=CARTESIAN_POINT('Ctrl Pts',(-10.0514385264423,91.4562475083482,
3.26591035271534));
#277074=CARTESIAN_POINT('Ctrl Pts',(-8.1317845858069,91.6062475083476,5.90808733016713));
#277075=CARTESIAN_POINT('Ctrl Pts',(-6.21213064517151,91.7562475083471,
8.55026430761891));
#277076=CARTESIAN_POINT('Ctrl Pts',(-3.10606532258579,91.9062475083465,
9.55948610871303));
#277077=CARTESIAN_POINT('Ctrl Pts',(-6.35516607170367E-14,92.0562475083459,
10.5687079098071));
#277078=CARTESIAN_POINT('Ctrl Pts',(3.10606532258566,92.2062475083453,9.55948610871303));
#277079=CARTESIAN_POINT('Ctrl Pts',(6.21213064517139,92.3562475083446,8.55026430761891));
#277080=CARTESIAN_POINT('Ctrl Pts',(8.13178458580677,92.506247508344,5.90808733016712));
#277081=CARTESIAN_POINT('Ctrl Pts',(10.0514385264422,92.6562475083435,3.26591035271534));
#277082=CARTESIAN_POINT('Ctrl Pts',(10.0514385264422,92.8062475083428,-1.23094620182339E-15));
#277083=CARTESIAN_POINT('Ctrl Pts',(10.0514385264422,92.9562475083423,-3.26591035271534));
#277084=CARTESIAN_POINT('Ctrl Pts',(8.13178458580677,93.1062475083417,-5.90808733016713));
#277085=CARTESIAN_POINT('Ctrl Pts',(6.21213064517138,93.256247508341,-8.55026430761891));
#277086=CARTESIAN_POINT('Ctrl Pts',(3.10606532258566,93.4062475083405,-9.55948610871303));
#277087=CARTESIAN_POINT('Ctrl Pts',(-6.70041022154414E-14,93.5562475083398,
-10.5687079098071));
#277088=CARTESIAN_POINT('Ctrl Pts',(-3.10606532258579,93.7062475083393,
-9.55948610871303));
#277089=CARTESIAN_POINT('Ctrl Pts',(-6.21213064517151,93.8562475083386,
-8.55026430761891));
#277090=CARTESIAN_POINT('Ctrl Pts',(-8.1317845858069,94.006247508338,-5.90808733016712));
#277091=CARTESIAN_POINT('Ctrl Pts',(-10.0514385264423,94.1562475083374,
-3.26591035271534));
#277092=CARTESIAN_POINT('Ctrl Pts',(-10.0514385264423,94.3062475083369,
2.46189240364677E-15));
#277093=CARTESIAN_POINT('Ctrl Pts',(-10.0514385264423,94.4562475083362,
3.26591035271534));
#277094=CARTESIAN_POINT('Ctrl Pts',(-8.1317845858069,94.6062475083356,5.90808733016713));
#277095=CARTESIAN_POINT('Ctrl Pts',(-6.21213064517151,94.7562475083351,
8.55026430761891));
#277096=CARTESIAN_POINT('Ctrl Pts',(-3.10606532258579,94.9062475083345,
9.55948610871303));
#277097=CARTESIAN_POINT('Ctrl Pts',(-6.52793699886986E-14,95.0562475083338,
10.5687079098071));
#277098=CARTESIAN_POINT('Ctrl Pts',(3.10606532258566,95.2062475083333,9.55948610871303));
#277099=CARTESIAN_POINT('Ctrl Pts',(6.21213064517138,95.3562475083327,8.55026430761891));
#277100=CARTESIAN_POINT('Ctrl Pts',(8.13178458580677,95.5062475083321,5.90808733016712));
#277101=CARTESIAN_POINT('Ctrl Pts',(10.0514385264422,95.6562475083314,3.26591035271534));
#277102=CARTESIAN_POINT('Ctrl Pts',(10.0514385264422,95.8062475083309,-1.23094620182339E-15));
#277103=CARTESIAN_POINT('Ctrl Pts',(10.0514385264422,95.9562475083303,-3.26591035271534));
#277104=CARTESIAN_POINT('Ctrl Pts',(8.13178458580677,96.1062475083297,-5.90808733016713));
#277105=CARTESIAN_POINT('Ctrl Pts',(6.21213064517138,96.2562475083291,-8.55026430761891));
#277106=CARTESIAN_POINT('Ctrl Pts',(3.10606532258566,96.4062475083284,-9.55948610871303));
#277107=CARTESIAN_POINT('Ctrl Pts',(-6.87318114871032E-14,96.5562475083278,
-10.5687079098071));
#277108=CARTESIAN_POINT('Ctrl Pts',(-3.10606532258579,96.7062475083272,
-9.55948610871303));
#277109=CARTESIAN_POINT('Ctrl Pts',(-6.21213064517152,96.8562475083267,
-8.55026430761891));
#277110=CARTESIAN_POINT('Ctrl Pts',(-8.1317845858069,97.0062475083261,-5.90808733016712));
#277111=CARTESIAN_POINT('Ctrl Pts',(-10.0514385264423,97.1562475083254,
-3.26591035271534));
#277112=CARTESIAN_POINT('Ctrl Pts',(-10.0514385264423,97.3062475083248,
2.46189240364677E-15));
#277113=CARTESIAN_POINT('Ctrl Pts',(-10.0514385264423,97.4562475083242,
3.26591035271534));
#277114=CARTESIAN_POINT('Ctrl Pts',(-8.1317845858069,97.6062475083236,5.90808733016713));
#277115=CARTESIAN_POINT('Ctrl Pts',(-6.21213064517151,97.7562475083231,
8.55026430761891));
#277116=CARTESIAN_POINT('Ctrl Pts',(-3.10606532258579,97.9062475083225,
9.55948610871303));
#277117=CARTESIAN_POINT('Ctrl Pts',(-6.70070792603604E-14,98.0562475083219,
10.5687079098071));
#277118=CARTESIAN_POINT('Ctrl Pts',(3.10606532258566,98.2062475083213,9.55948610871303));
#277119=CARTESIAN_POINT('Ctrl Pts',(6.21213064517138,98.3562475083206,8.55026430761891));
#277120=CARTESIAN_POINT('Ctrl Pts',(8.13178458580676,98.5062475083201,5.90808733016712));
#277121=CARTESIAN_POINT('Ctrl Pts',(10.0514385264422,98.6562475083194,3.26591035271534));
#277122=CARTESIAN_POINT('Ctrl Pts',(10.0514385264422,98.8062475083189,-1.23094620182339E-15));
#277123=CARTESIAN_POINT('Ctrl Pts',(10.0514385264421,98.9562475083183,-3.26591035271534));
#277124=CARTESIAN_POINT('Ctrl Pts',(8.13178458580676,99.1062475083177,-5.90808733016713));
#277125=CARTESIAN_POINT('Ctrl Pts',(6.21213064517138,99.256247508317,-8.55026430761891));
#277126=CARTESIAN_POINT('Ctrl Pts',(3.10606532258565,99.4062475083165,-9.55948610871303));
#277127=CARTESIAN_POINT('Ctrl Pts',(-7.0459520758765E-14,99.5562475083159,
-10.5687079098071));
#277128=CARTESIAN_POINT('Ctrl Pts',(-3.1060653225858,99.7062475083153,-9.55948610871303));
#277129=CARTESIAN_POINT('Ctrl Pts',(-6.21213064517152,99.8562475083146,
-8.55026430761891));
#277130=CARTESIAN_POINT('Ctrl Pts',(-8.1317845858069,100.006247508314,-5.90808733016712));
#277131=CARTESIAN_POINT('Ctrl Pts',(-10.0514385264423,100.156247508313,
-3.26591035271534));
#277132=CARTESIAN_POINT('Ctrl Pts',(-10.0514385264423,100.306247508313,
2.46189240364677E-15));
#277133=CARTESIAN_POINT('Ctrl Pts',(-10.0514385264423,100.456247508312,
3.26591035271534));
#277134=CARTESIAN_POINT('Ctrl Pts',(-8.1317845858069,100.606247508312,5.90808733016713));
#277135=CARTESIAN_POINT('Ctrl Pts',(-6.21213064517152,100.756247508311,
8.55026430761891));
#277136=CARTESIAN_POINT('Ctrl Pts',(-3.10606532258579,100.90624750831,9.55948610871303));
#277137=CARTESIAN_POINT('Ctrl Pts',(-6.87347885320222E-14,101.05624750831,
10.5687079098071));
#277138=CARTESIAN_POINT('Ctrl Pts',(3.10606532258566,101.206247508309,9.55948610871303));
#277139=CARTESIAN_POINT('Ctrl Pts',(6.21213064517138,101.356247508309,8.55026430761891));
#277140=CARTESIAN_POINT('Ctrl Pts',(8.13178458580676,101.506247508308,5.90808733016712));
#277141=CARTESIAN_POINT('Ctrl Pts',(10.0514385264421,101.656247508307,3.26591035271534));
#277142=CARTESIAN_POINT('Ctrl Pts',(10.0514385264421,101.806247508307,-1.23094620182339E-15));
#277143=CARTESIAN_POINT('Ctrl Pts',(10.0514385264421,101.956247508306,-3.26591035271534));
#277144=CARTESIAN_POINT('Ctrl Pts',(8.13178458580676,102.106247508306,-5.90808733016713));
#277145=CARTESIAN_POINT('Ctrl Pts',(6.21213064517138,102.256247508305,-8.55026430761891));
#277146=CARTESIAN_POINT('Ctrl Pts',(3.10606532258565,102.406247508304,-9.55948610871303));
#277147=CARTESIAN_POINT('Ctrl Pts',(-7.21872300304269E-14,102.556247508304,
-10.5687079098071));
#277148=CARTESIAN_POINT('Ctrl Pts',(-3.1060653225858,102.706247508303,-9.55948610871303));
#277149=CARTESIAN_POINT('Ctrl Pts',(-6.21213064517152,102.856247508303,
-8.55026430761891));
#277150=CARTESIAN_POINT('Ctrl Pts',(-8.13178458580691,103.006247508302,
-5.90808733016712));
#277151=CARTESIAN_POINT('Ctrl Pts',(-10.0514385264423,103.156247508301,
-3.26591035271534));
#277152=CARTESIAN_POINT('Ctrl Pts',(-10.0514385264423,103.306247508301,
2.46189240364677E-15));
#277153=CARTESIAN_POINT('Ctrl Pts',(-10.0514385264423,103.4562475083,3.26591035271534));
#277154=CARTESIAN_POINT('Ctrl Pts',(-8.13178458580691,103.6062475083,5.90808733016713));
#277155=CARTESIAN_POINT('Ctrl Pts',(-6.21213064517152,103.756247508299,
8.55026430761891));
#277156=CARTESIAN_POINT('Ctrl Pts',(-3.1060653225858,103.906247508298,9.55948610871303));
#277157=CARTESIAN_POINT('Ctrl Pts',(-7.04624978036841E-14,104.056247508298,
10.5687079098071));
#277158=CARTESIAN_POINT('Ctrl Pts',(3.10606532258565,104.206247508297,9.55948610871303));
#277159=CARTESIAN_POINT('Ctrl Pts',(6.21213064517138,104.356247508297,8.55026430761891));
#277160=CARTESIAN_POINT('Ctrl Pts',(8.13178458580676,104.506247508296,5.90808733016712));
#277161=CARTESIAN_POINT('Ctrl Pts',(10.0514385264421,104.656247508295,3.26591035271534));
#277162=CARTESIAN_POINT('Ctrl Pts',(10.0514385264421,104.806247508295,-1.23094620182339E-15));
#277163=CARTESIAN_POINT('Ctrl Pts',(10.0514385264421,104.956247508294,-3.26591035271534));
#277164=CARTESIAN_POINT('Ctrl Pts',(8.13178458580676,105.106247508294,-5.90808733016713));
#277165=CARTESIAN_POINT('Ctrl Pts',(6.21213064517137,105.256247508293,-8.55026430761891));
#277166=CARTESIAN_POINT('Ctrl Pts',(3.10606532258565,105.406247508292,-9.55948610871303));
#277167=CARTESIAN_POINT('Ctrl Pts',(-7.39149393020888E-14,105.556247508292,
-10.5687079098071));
#277168=CARTESIAN_POINT('Ctrl Pts',(-3.1060653225858,105.706247508291,-9.55948610871303));
#277169=CARTESIAN_POINT('Ctrl Pts',(-6.21213064517152,105.856247508291,
-8.55026430761891));
#277170=CARTESIAN_POINT('Ctrl Pts',(-8.13178458580691,106.00624750829,-5.90808733016712));
#277171=CARTESIAN_POINT('Ctrl Pts',(-10.0514385264423,106.156247508289,
-3.26591035271534));
#277172=CARTESIAN_POINT('Ctrl Pts',(-10.0514385264423,106.306247508289,
2.46189240364677E-15));
#277173=CARTESIAN_POINT('Ctrl Pts',(-10.0514385264423,106.456247508288,
3.26591035271534));
#277174=CARTESIAN_POINT('Ctrl Pts',(-8.13178458580691,106.606247508288,
5.90808733016713));
#277175=CARTESIAN_POINT('Ctrl Pts',(-6.21213064517152,106.756247508287,
8.55026430761891));
#277176=CARTESIAN_POINT('Ctrl Pts',(-3.1060653225858,106.906247508286,9.55948610871303));
#277177=CARTESIAN_POINT('Ctrl Pts',(-7.21902070753459E-14,107.056247508286,
10.5687079098071));
#277178=CARTESIAN_POINT('Ctrl Pts',(3.10606532258565,107.206247508285,9.55948610871303));
#277179=CARTESIAN_POINT('Ctrl Pts',(6.21213064517138,107.356247508285,8.55026430761891));
#277180=CARTESIAN_POINT('Ctrl Pts',(8.13178458580676,107.506247508284,5.90808733016712));
#277181=CARTESIAN_POINT('Ctrl Pts',(10.0514385264421,107.656247508283,3.26591035271534));
#277182=CARTESIAN_POINT('Ctrl Pts',(10.0514385264421,107.806247508283,-1.23094620182339E-15));
#277183=CARTESIAN_POINT('Ctrl Pts',(10.0514385264421,107.956247508282,-3.26591035271534));
#277184=CARTESIAN_POINT('Ctrl Pts',(8.13178458580676,108.106247508282,-5.90808733016713));
#277185=CARTESIAN_POINT('Ctrl Pts',(6.21213064517137,108.256247508281,-8.55026430761891));
#277186=CARTESIAN_POINT('Ctrl Pts',(3.10606532258565,108.40624750828,-9.55948610871303));
#277187=CARTESIAN_POINT('Ctrl Pts',(-7.56426485737506E-14,108.55624750828,
-10.5687079098071));
#277188=CARTESIAN_POINT('Ctrl Pts',(-3.1060653225858,108.706247508279,-9.55948610871303));
#277189=CARTESIAN_POINT('Ctrl Pts',(-6.21213064517153,108.856247508279,
-8.55026430761891));
#277190=CARTESIAN_POINT('Ctrl Pts',(-8.13178458580691,109.006247508278,
-5.90808733016712));
#277191=CARTESIAN_POINT('Ctrl Pts',(-10.0514385264423,109.156247508277,
-3.26591035271534));
#277192=CARTESIAN_POINT('Ctrl Pts',(-10.0514385264423,109.306247508277,
2.46189240364677E-15));
#277193=CARTESIAN_POINT('Ctrl Pts',(-10.0514385264423,109.456247508276,
3.26591035271534));
#277194=CARTESIAN_POINT('Ctrl Pts',(-8.13178458580691,109.606247508276,
5.90808733016713));
#277195=CARTESIAN_POINT('Ctrl Pts',(-6.21213064517152,109.756247508275,
8.55026430761891));
#277196=CARTESIAN_POINT('Ctrl Pts',(-3.1060653225858,109.906247508274,9.55948610871303));
#277197=CARTESIAN_POINT('Ctrl Pts',(-7.39179163470078E-14,110.056247508274,
10.5687079098071));
#277198=CARTESIAN_POINT('Ctrl Pts',(3.10606532258565,110.206247508273,9.55948610871303));
#277199=CARTESIAN_POINT('Ctrl Pts',(6.21213064517137,110.356247508273,8.55026430761891));
#277200=CARTESIAN_POINT('Ctrl Pts',(8.13178458580676,110.506247508272,5.90808733016712));
#277201=CARTESIAN_POINT('Ctrl Pts',(10.0514385264421,110.656247508271,3.26591035271534));
#277202=CARTESIAN_POINT('Ctrl Pts',(10.0514385264421,110.806247508271,-1.23094620182339E-15));
#277203=CARTESIAN_POINT('Ctrl Pts',(10.0514385264421,110.95624750827,-3.26591035271534));
#277204=CARTESIAN_POINT('Ctrl Pts',(8.13178458580676,111.10624750827,-5.90808733016713));
#277205=CARTESIAN_POINT('Ctrl Pts',(6.21213064517137,111.256247508269,-8.55026430761891));
#277206=CARTESIAN_POINT('Ctrl Pts',(3.10606532258565,111.406247508268,-9.55948610871303));
#277207=CARTESIAN_POINT('Ctrl Pts',(-7.73703578454124E-14,111.556247508268,
-10.5687079098071));
#277208=CARTESIAN_POINT('Ctrl Pts',(-3.1060653225858,111.706247508267,-9.55948610871303));
#277209=CARTESIAN_POINT('Ctrl Pts',(-6.21213064517153,111.856247508267,
-8.55026430761891));
#277210=CARTESIAN_POINT('Ctrl Pts',(-8.13178458580691,112.006247508266,
-5.90808733016712));
#277211=CARTESIAN_POINT('Ctrl Pts',(-10.0514385264423,112.156247508265,
-3.26591035271534));
#277212=CARTESIAN_POINT('Ctrl Pts',(-10.0514385264423,112.306247508265,
2.46189240364677E-15));
#277213=CARTESIAN_POINT('Ctrl Pts',(-10.0514385264423,112.456247508264,
3.26591035271534));
#277214=CARTESIAN_POINT('Ctrl Pts',(-8.13178458580691,112.606247508264,
5.90808733016713));
#277215=CARTESIAN_POINT('Ctrl Pts',(-6.21213064517153,112.756247508263,
8.55026430761891));
#277216=CARTESIAN_POINT('Ctrl Pts',(-3.1060653225858,112.906247508262,9.55948610871303));
#277217=CARTESIAN_POINT('Ctrl Pts',(-7.56456256186696E-14,113.056247508262,
10.5687079098071));
#277218=CARTESIAN_POINT('Ctrl Pts',(3.10606532258565,113.206247508261,9.55948610871303));
#277219=CARTESIAN_POINT('Ctrl Pts',(6.21213064517137,113.356247508261,8.55026430761891));
#277220=CARTESIAN_POINT('Ctrl Pts',(8.13178458580676,113.50624750826,5.90808733016712));
#277221=CARTESIAN_POINT('Ctrl Pts',(10.0514385264421,113.656247508259,3.26591035271534));
#277222=CARTESIAN_POINT('Ctrl Pts',(10.0514385264421,113.806247508259,-1.23094620182339E-15));
#277223=CARTESIAN_POINT('Ctrl Pts',(10.0514385264421,113.956247508258,-3.26591035271534));
#277224=CARTESIAN_POINT('Ctrl Pts',(8.13178458580676,114.106247508258,-5.90808733016713));
#277225=CARTESIAN_POINT('Ctrl Pts',(6.21213064517137,114.256247508257,-8.55026430761891));
#277226=CARTESIAN_POINT('Ctrl Pts',(3.10606532258565,114.406247508256,-9.55948610871303));
#277227=CARTESIAN_POINT('Ctrl Pts',(-7.90980671170742E-14,114.556247508256,
-10.5687079098071));
#277228=CARTESIAN_POINT('Ctrl Pts',(-3.1060653225858,114.706247508255,-9.55948610871303));
#277229=CARTESIAN_POINT('Ctrl Pts',(-6.21213064517153,114.856247508255,
-8.55026430761891));
#277230=CARTESIAN_POINT('Ctrl Pts',(-8.13178458580691,115.006247508254,
-5.90808733016712));
#277231=CARTESIAN_POINT('Ctrl Pts',(-10.0514385264423,115.156247508253,
-3.26591035271534));
#277232=CARTESIAN_POINT('Ctrl Pts',(-10.0514385264423,115.306247508253,
2.46189240364677E-15));
#277233=CARTESIAN_POINT('Ctrl Pts',(-10.0514385264423,115.456247508252,
3.26591035271534));
#277234=CARTESIAN_POINT('Ctrl Pts',(-8.13178458580691,115.606247508252,
5.90808733016713));
#277235=CARTESIAN_POINT('Ctrl Pts',(-6.21213064517153,115.756247508251,
8.55026430761891));
#277236=CARTESIAN_POINT('Ctrl Pts',(-3.1060653225858,115.90624750825,9.55948610871303));
#277237=CARTESIAN_POINT('Ctrl Pts',(-7.73733348903315E-14,116.05624750825,
10.5687079098071));
#277238=CARTESIAN_POINT('Ctrl Pts',(3.10606532258565,116.206247508249,9.55948610871303));
#277239=CARTESIAN_POINT('Ctrl Pts',(6.21213064517137,116.356247508249,8.55026430761891));
#277240=CARTESIAN_POINT('Ctrl Pts',(8.13178458580676,116.506247508248,5.90808733016712));
#277241=CARTESIAN_POINT('Ctrl Pts',(10.0514385264421,116.656247508247,3.26591035271534));
#277242=CARTESIAN_POINT('Ctrl Pts',(10.0514385264421,116.806247508247,-1.23094620182339E-15));
#277243=CARTESIAN_POINT('Ctrl Pts',(10.0514385264421,116.956247508246,-3.26591035271534));
#277244=CARTESIAN_POINT('Ctrl Pts',(8.13178458580676,117.106247508246,-5.90808733016713));
#277245=CARTESIAN_POINT('Ctrl Pts',(6.21213064517137,117.256247508245,-8.55026430761891));
#277246=CARTESIAN_POINT('Ctrl Pts',(3.10606532258564,117.406247508244,-9.55948610871303));
#277247=CARTESIAN_POINT('Ctrl Pts',(-8.08257763887361E-14,117.556247508244,
-10.5687079098071));
#277248=CARTESIAN_POINT('Ctrl Pts',(-3.10606532258581,117.706247508243,
-9.55948610871303));
#277249=CARTESIAN_POINT('Ctrl Pts',(-6.21213064517153,117.856247508243,
-8.55026430761891));
#277250=CARTESIAN_POINT('Ctrl Pts',(-8.13178458580692,118.006247508242,
-5.90808733016712));
#277251=CARTESIAN_POINT('Ctrl Pts',(-10.0514385264423,118.156247508241,
-3.26591035271534));
#277252=CARTESIAN_POINT('Ctrl Pts',(-10.0514385264423,118.306247508241,
2.46189240364677E-15));
#277253=CARTESIAN_POINT('Ctrl Pts',(-10.0514385264423,118.45624750824,3.26591035271534));
#277254=CARTESIAN_POINT('Ctrl Pts',(-8.13178458580692,118.60624750824,5.90808733016713));
#277255=CARTESIAN_POINT('Ctrl Pts',(-6.21213064517153,118.756247508239,
8.55026430761891));
#277256=CARTESIAN_POINT('Ctrl Pts',(-3.1060653225858,118.906247508238,9.55948610871303));
#277257=CARTESIAN_POINT('Ctrl Pts',(-7.91010441619933E-14,119.056247508238,
10.5687079098071));
#277258=CARTESIAN_POINT('Ctrl Pts',(3.10606532258564,119.206247508237,9.55948610871303));
#277259=CARTESIAN_POINT('Ctrl Pts',(6.21213064517137,119.356247508237,8.55026430761891));
#277260=CARTESIAN_POINT('Ctrl Pts',(8.13178458580675,119.506247508236,5.90808733016712));
#277261=CARTESIAN_POINT('Ctrl Pts',(10.0514385264421,119.656247508235,3.26591035271534));
#277262=CARTESIAN_POINT('Ctrl Pts',(10.0514385264421,119.806247508235,-1.23094620182339E-15));
#277263=CARTESIAN_POINT('Ctrl Pts',(10.0514385264421,119.956247508234,-3.26591035271534));
#277264=CARTESIAN_POINT('Ctrl Pts',(8.13178458580675,120.106247508234,-5.90808733016713));
#277265=CARTESIAN_POINT('Ctrl Pts',(6.21213064517137,120.256247508233,-8.55026430761891));
#277266=CARTESIAN_POINT('Ctrl Pts',(3.10606532258564,120.406247508232,-9.55948610871303));
#277267=CARTESIAN_POINT('Ctrl Pts',(-8.25534856603979E-14,120.556247508232,
-10.5687079098071));
#277268=CARTESIAN_POINT('Ctrl Pts',(-3.10606532258581,120.706247508231,
-9.55948610871303));
#277269=CARTESIAN_POINT('Ctrl Pts',(-6.21213064517153,120.856247508231,
-8.55026430761891));
#277270=CARTESIAN_POINT('Ctrl Pts',(-8.13178458580692,121.00624750823,-5.90808733016712));
#277271=CARTESIAN_POINT('Ctrl Pts',(-10.0514385264423,121.156247508229,
-3.26591035271534));
#277272=CARTESIAN_POINT('Ctrl Pts',(-10.0514385264423,121.306247508229,
2.46189240364677E-15));
#277273=CARTESIAN_POINT('Ctrl Pts',(-10.0514385264423,121.456247508228,
3.26591035271534));
#277274=CARTESIAN_POINT('Ctrl Pts',(-8.13178458580692,121.606247508228,
5.90808733016713));
#277275=CARTESIAN_POINT('Ctrl Pts',(-6.21213064517153,121.756247508227,
8.55026430761891));
#277276=CARTESIAN_POINT('Ctrl Pts',(-3.10606532258581,121.906247508226,
9.55948610871303));
#277277=CARTESIAN_POINT('Ctrl Pts',(-8.08287534336551E-14,122.056247508226,
10.5687079098071));
#277278=CARTESIAN_POINT('Ctrl Pts',(3.10606532258564,122.206247508225,9.55948610871303));
#277279=CARTESIAN_POINT('Ctrl Pts',(6.21213064517137,122.356247508225,8.55026430761891));
#277280=CARTESIAN_POINT('Ctrl Pts',(8.13178458580675,122.506247508224,5.90808733016712));
#277281=CARTESIAN_POINT('Ctrl Pts',(10.0514385264421,122.656247508223,3.26591035271534));
#277282=CARTESIAN_POINT('Ctrl Pts',(10.0514385264421,122.806247508223,-1.23094620182339E-15));
#277283=CARTESIAN_POINT('Ctrl Pts',(10.0514385264421,122.956247508222,-3.26591035271534));
#277284=CARTESIAN_POINT('Ctrl Pts',(8.13178458580675,123.106247508222,-5.90808733016713));
#277285=CARTESIAN_POINT('Ctrl Pts',(6.21213064517137,123.256247508221,-8.55026430761891));
#277286=CARTESIAN_POINT('Ctrl Pts',(3.10606532258564,123.40624750822,-9.55948610871303));
#277287=CARTESIAN_POINT('Ctrl Pts',(-8.42811949320597E-14,123.55624750822,
-10.5687079098071));
#277288=CARTESIAN_POINT('Ctrl Pts',(-3.10606532258581,123.706247508219,
-9.55948610871303));
#277289=CARTESIAN_POINT('Ctrl Pts',(-6.21213064517153,123.856247508219,
-8.55026430761891));
#277290=CARTESIAN_POINT('Ctrl Pts',(-8.13178458580692,124.006247508218,
-5.90808733016712));
#277291=CARTESIAN_POINT('Ctrl Pts',(-10.0514385264423,124.156247508217,
-3.26591035271534));
#277292=CARTESIAN_POINT('Ctrl Pts',(-10.0514385264423,124.306247508217,
2.46189240364677E-15));
#277293=CARTESIAN_POINT('Ctrl Pts',(-10.0514385264423,124.456247508216,
3.26591035271534));
#277294=CARTESIAN_POINT('Ctrl Pts',(-8.13178458580692,124.606247508216,
5.90808733016713));
#277295=CARTESIAN_POINT('Ctrl Pts',(-6.21213064517153,124.756247508215,
8.55026430761891));
#277296=CARTESIAN_POINT('Ctrl Pts',(-3.10606532258581,124.906247508214,
9.55948610871303));
#277297=CARTESIAN_POINT('Ctrl Pts',(-8.25564627053169E-14,125.056247508214,
10.5687079098071));
#277298=CARTESIAN_POINT('Ctrl Pts',(3.10606532258564,125.206247508213,9.55948610871303));
#277299=CARTESIAN_POINT('Ctrl Pts',(6.21213064517137,125.356247508213,8.55026430761891));
#277300=CARTESIAN_POINT('Ctrl Pts',(8.13178458580675,125.506247508212,5.90808733016712));
#277301=CARTESIAN_POINT('Ctrl Pts',(10.0514385264421,125.656247508211,3.26591035271534));
#277302=CARTESIAN_POINT('Ctrl Pts',(10.0514385264421,125.806247508211,-1.23094620182339E-15));
#277303=CARTESIAN_POINT('Ctrl Pts',(10.0514385264421,125.95624750821,-3.26591035271534));
#277304=CARTESIAN_POINT('Ctrl Pts',(8.13178458580675,126.10624750821,-5.90808733016713));
#277305=CARTESIAN_POINT('Ctrl Pts',(6.21213064517136,126.256247508209,-8.55026430761891));
#277306=CARTESIAN_POINT('Ctrl Pts',(3.10606532258564,126.406247508208,-9.55948610871303));
#277307=CARTESIAN_POINT('Ctrl Pts',(-8.60089042037216E-14,126.556247508208,
-10.5687079098071));
#277308=CARTESIAN_POINT('Ctrl Pts',(-3.10606532258581,126.706247508207,
-9.55948610871303));
#277309=CARTESIAN_POINT('Ctrl Pts',(-6.21213064517153,126.856247508207,
-8.55026430761891));
#277310=CARTESIAN_POINT('Ctrl Pts',(-8.13178458580692,127.006247508206,
-5.90808733016712));
#277311=CARTESIAN_POINT('Ctrl Pts',(-10.0514385264423,127.156247508205,
-3.26591035271534));
#277312=CARTESIAN_POINT('Ctrl Pts',(-10.0514385264423,127.306247508205,
2.46189240364677E-15));
#277313=CARTESIAN_POINT('Ctrl Pts',(-10.0514385264423,127.456247508204,
3.26591035271534));
#277314=CARTESIAN_POINT('Ctrl Pts',(-8.13178458580692,127.606247508204,
5.90808733016713));
#277315=CARTESIAN_POINT('Ctrl Pts',(-6.21213064517153,127.756247508203,
8.55026430761891));
#277316=CARTESIAN_POINT('Ctrl Pts',(-3.10606532258581,127.906247508202,
9.55948610871303));
#277317=CARTESIAN_POINT('Ctrl Pts',(-8.42841719769788E-14,128.056247508202,
10.5687079098071));
#277318=CARTESIAN_POINT('Ctrl Pts',(3.10606532258564,128.206247508201,9.55948610871303));
#277319=CARTESIAN_POINT('Ctrl Pts',(6.21213064517137,128.356247508201,8.55026430761891));
#277320=CARTESIAN_POINT('Ctrl Pts',(8.13178458580675,128.5062475082,5.90808733016712));
#277321=CARTESIAN_POINT('Ctrl Pts',(10.0514385264421,128.656247508199,3.26591035271534));
#277322=CARTESIAN_POINT('Ctrl Pts',(10.0514385264421,128.806247508199,-1.23094620182339E-15));
#277323=CARTESIAN_POINT('Ctrl Pts',(10.0514385264421,128.956247508198,-3.26591035271534));
#277324=CARTESIAN_POINT('Ctrl Pts',(8.13178458580675,129.106247508198,-5.90808733016713));
#277325=CARTESIAN_POINT('Ctrl Pts',(6.21213064517136,129.256247508197,-8.55026430761891));
#277326=CARTESIAN_POINT('Ctrl Pts',(3.10606532258564,129.406247508196,-9.55948610871303));
#277327=CARTESIAN_POINT('Ctrl Pts',(-8.77366134753835E-14,129.556247508196,
-10.5687079098071));
#277328=CARTESIAN_POINT('Ctrl Pts',(-3.10606532258581,129.706247508195,
-9.55948610871303));
#277329=CARTESIAN_POINT('Ctrl Pts',(-6.21213064517154,129.856247508195,
-8.55026430761891));
#277330=CARTESIAN_POINT('Ctrl Pts',(-8.13178458580692,130.006247508194,
-5.90808733016712));
#277331=CARTESIAN_POINT('Ctrl Pts',(-10.0514385264423,130.156247508193,
-3.26591035271534));
#277332=CARTESIAN_POINT('Ctrl Pts',(-10.0514385264423,130.306247508193,
2.46189240364677E-15));
#277333=CARTESIAN_POINT('Ctrl Pts',(-10.0514385264423,130.456247508192,
3.26591035271534));
#277334=CARTESIAN_POINT('Ctrl Pts',(-8.13178458580692,130.606247508192,
5.90808733016713));
#277335=CARTESIAN_POINT('Ctrl Pts',(-6.21213064517153,130.756247508191,
8.55026430761891));
#277336=CARTESIAN_POINT('Ctrl Pts',(-3.10606532258581,130.90624750819,9.55948610871303));
#277337=CARTESIAN_POINT('Ctrl Pts',(-8.60118812486407E-14,131.05624750819,
10.5687079098071));
#277338=CARTESIAN_POINT('Ctrl Pts',(3.10606532258564,131.206247508189,9.55948610871303));
#277339=CARTESIAN_POINT('Ctrl Pts',(6.21213064517136,131.356247508189,8.55026430761891));
#277340=CARTESIAN_POINT('Ctrl Pts',(8.13178458580675,131.506247508188,5.90808733016712));
#277341=CARTESIAN_POINT('Ctrl Pts',(10.0514385264421,131.656247508187,3.26591035271534));
#277342=CARTESIAN_POINT('Ctrl Pts',(10.0514385264421,131.806247508187,-1.23094620182339E-15));
#277343=CARTESIAN_POINT('Ctrl Pts',(10.0514385264421,131.956247508186,-3.26591035271534));
#277344=CARTESIAN_POINT('Ctrl Pts',(8.13178458580675,132.106247508186,-5.90808733016713));
#277345=CARTESIAN_POINT('Ctrl Pts',(6.21213064517136,132.256247508185,-8.55026430761891));
#277346=CARTESIAN_POINT('Ctrl Pts',(3.10606532258563,132.406247508184,-9.55948610871303));
#277347=CARTESIAN_POINT('Ctrl Pts',(-8.94643227470453E-14,132.556247508184,
-10.5687079098071));
#277348=CARTESIAN_POINT('Ctrl Pts',(-3.10606532258582,132.706247508183,
-9.55948610871303));
#277349=CARTESIAN_POINT('Ctrl Pts',(-6.21213064517154,132.856247508183,
-8.55026430761891));
#277350=CARTESIAN_POINT('Ctrl Pts',(-8.13178458580692,133.006247508182,
-5.90808733016712));
#277351=CARTESIAN_POINT('Ctrl Pts',(-10.0514385264423,133.156247508181,
-3.26591035271534));
#277352=CARTESIAN_POINT('Ctrl Pts',(-10.0514385264423,133.306247508181,
2.46189240364677E-15));
#277353=CARTESIAN_POINT('Ctrl Pts',(-10.0514385264423,133.45624750818,3.26591035271534));
#277354=CARTESIAN_POINT('Ctrl Pts',(-8.13178458580692,133.60624750818,5.90808733016713));
#277355=CARTESIAN_POINT('Ctrl Pts',(-6.21213064517154,133.756247508179,
8.55026430761891));
#277356=CARTESIAN_POINT('Ctrl Pts',(-3.10606532258581,133.906247508178,
9.55948610871303));
#277357=CARTESIAN_POINT('Ctrl Pts',(-8.77395905203025E-14,134.056247508178,
10.5687079098071));
#277358=CARTESIAN_POINT('Ctrl Pts',(3.10606532258564,134.206247508177,9.55948610871303));
#277359=CARTESIAN_POINT('Ctrl Pts',(6.21213064517136,134.356247508177,8.55026430761891));
#277360=CARTESIAN_POINT('Ctrl Pts',(8.13178458580674,134.506247508176,5.90808733016712));
#277361=CARTESIAN_POINT('Ctrl Pts',(10.0514385264421,134.656247508175,3.26591035271534));
#277362=CARTESIAN_POINT('Ctrl Pts',(10.0514385264421,134.806247508175,-1.23094620182339E-15));
#277363=CARTESIAN_POINT('Ctrl Pts',(10.0514385264421,134.956247508174,-3.26591035271534));
#277364=CARTESIAN_POINT('Ctrl Pts',(8.13178458580674,135.106247508174,-5.90808733016713));
#277365=CARTESIAN_POINT('Ctrl Pts',(6.21213064517136,135.256247508173,-8.55026430761891));
#277366=CARTESIAN_POINT('Ctrl Pts',(3.10606532258563,135.406247508172,-9.55948610871303));
#277367=CARTESIAN_POINT('Ctrl Pts',(-9.11920320187072E-14,135.556247508172,
-10.5687079098071));
#277368=CARTESIAN_POINT('Ctrl Pts',(-3.10606532258582,135.706247508171,
-9.55948610871303));
#277369=CARTESIAN_POINT('Ctrl Pts',(-6.21213064517154,135.856247508171,
-8.55026430761891));
#277370=CARTESIAN_POINT('Ctrl Pts',(-8.13178458580693,136.00624750817,-5.90808733016712));
#277371=CARTESIAN_POINT('Ctrl Pts',(-10.0514385264423,136.156247508169,
-3.26591035271534));
#277372=CARTESIAN_POINT('Ctrl Pts',(-10.0514385264423,136.306247508169,
2.46189240364677E-15));
#277373=CARTESIAN_POINT('Ctrl Pts',(-10.0514385264423,136.456247508168,
3.26591035271534));
#277374=CARTESIAN_POINT('Ctrl Pts',(-8.13178458580693,136.606247508168,
5.90808733016713));
#277375=CARTESIAN_POINT('Ctrl Pts',(-6.21213064517154,136.756247508167,
8.55026430761891));
#277376=CARTESIAN_POINT('Ctrl Pts',(-3.10606532258582,136.906247508166,
9.55948610871303));
#277377=CARTESIAN_POINT('Ctrl Pts',(-8.94672997919643E-14,137.056247508166,
10.5687079098071));
#277378=CARTESIAN_POINT('Ctrl Pts',(3.10606532258563,137.206247508165,9.55948610871303));
#277379=CARTESIAN_POINT('Ctrl Pts',(6.21213064517136,137.356247508165,8.55026430761891));
#277380=CARTESIAN_POINT('Ctrl Pts',(8.13178458580674,137.506247508164,5.90808733016712));
#277381=CARTESIAN_POINT('Ctrl Pts',(10.0514385264421,137.656247508163,3.26591035271534));
#277382=CARTESIAN_POINT('Ctrl Pts',(10.0514385264421,137.806247508163,-1.23094620182339E-15));
#277383=CARTESIAN_POINT('Ctrl Pts',(10.0514385264421,137.956247508162,-3.26591035271534));
#277384=CARTESIAN_POINT('Ctrl Pts',(8.13178458580674,138.106247508162,-5.90808733016713));
#277385=CARTESIAN_POINT('Ctrl Pts',(6.21213064517135,138.256247508161,-8.55026430761891));
#277386=CARTESIAN_POINT('Ctrl Pts',(3.10606532258563,138.40624750816,-9.55948610871303));
#277387=CARTESIAN_POINT('Ctrl Pts',(-9.2919741290369E-14,138.55624750816,
-10.5687079098071));
#277388=CARTESIAN_POINT('Ctrl Pts',(-3.10606532258582,138.706247508159,
-9.55948610871303));
#277389=CARTESIAN_POINT('Ctrl Pts',(-6.21213064517154,138.856247508159,
-8.55026430761891));
#277390=CARTESIAN_POINT('Ctrl Pts',(-8.13178458580693,139.006247508158,
-5.90808733016712));
#277391=CARTESIAN_POINT('Ctrl Pts',(-10.0514385264423,139.156247508157,
-3.26591035271534));
#277392=CARTESIAN_POINT('Ctrl Pts',(-10.0514385264423,139.306247508157,
2.46189240364677E-15));
#277393=CARTESIAN_POINT('Ctrl Pts',(-10.0514385264423,139.456247508156,
3.26591035271534));
#277394=CARTESIAN_POINT('Ctrl Pts',(-8.13178458580693,139.606247508156,
5.90808733016713));
#277395=CARTESIAN_POINT('Ctrl Pts',(-6.21213064517154,139.756247508155,
8.55026430761891));
#277396=CARTESIAN_POINT('Ctrl Pts',(-3.10606532258582,139.906247508154,
9.55948610871303));
#277397=CARTESIAN_POINT('Ctrl Pts',(-9.11950090636262E-14,140.056247508154,
10.5687079098071));
#277398=CARTESIAN_POINT('Ctrl Pts',(3.10606532258563,140.206247508153,9.55948610871303));
#277399=CARTESIAN_POINT('Ctrl Pts',(6.21213064517136,140.356247508153,8.55026430761891));
#277400=CARTESIAN_POINT('Ctrl Pts',(8.13178458580674,140.506247508152,5.90808733016712));
#277401=CARTESIAN_POINT('Ctrl Pts',(10.0514385264421,140.656247508151,3.26591035271534));
#277402=CARTESIAN_POINT('Ctrl Pts',(10.0514385264421,140.806247508151,-1.23094620182339E-15));
#277403=CARTESIAN_POINT('Ctrl Pts',(10.0514385264421,140.95624750815,-3.26591035271534));
#277404=CARTESIAN_POINT('Ctrl Pts',(8.13178458580674,141.10624750815,-5.90808733016713));
#277405=CARTESIAN_POINT('Ctrl Pts',(6.21213064517135,141.256247508149,-8.55026430761891));
#277406=CARTESIAN_POINT('Ctrl Pts',(3.10606532258563,141.406247508148,-9.55948610871303));
#277407=CARTESIAN_POINT('Ctrl Pts',(-9.46474505620308E-14,141.556247508148,
-10.5687079098071));
#277408=CARTESIAN_POINT('Ctrl Pts',(-3.10606532258582,141.706247508147,
-9.55948610871303));
#277409=CARTESIAN_POINT('Ctrl Pts',(-6.21213064517154,141.856247508147,
-8.55026430761891));
#277410=CARTESIAN_POINT('Ctrl Pts',(-8.13178458580693,142.006247508146,
-5.90808733016712));
#277411=CARTESIAN_POINT('Ctrl Pts',(-10.0514385264423,142.156247508145,
-3.26591035271534));
#277412=CARTESIAN_POINT('Ctrl Pts',(-10.0514385264423,142.306247508145,
2.46189240364677E-15));
#277413=CARTESIAN_POINT('Ctrl Pts',(-10.0514385264423,142.456247508144,
3.26591035271534));
#277414=CARTESIAN_POINT('Ctrl Pts',(-8.13178458580693,142.606247508144,
5.90808733016713));
#277415=CARTESIAN_POINT('Ctrl Pts',(-6.21213064517154,142.756247508143,
8.55026430761891));
#277416=CARTESIAN_POINT('Ctrl Pts',(-3.10606532258582,142.906247508142,
9.55948610871303));
#277417=CARTESIAN_POINT('Ctrl Pts',(-9.2922718335288E-14,143.056247508142,
10.5687079098071));
#277418=CARTESIAN_POINT('Ctrl Pts',(3.10606532258563,143.206247508141,9.55948610871303));
#277419=CARTESIAN_POINT('Ctrl Pts',(6.21213064517135,143.356247508141,8.55026430761891));
#277420=CARTESIAN_POINT('Ctrl Pts',(8.13178458580674,143.50624750814,5.90808733016712));
#277421=CARTESIAN_POINT('Ctrl Pts',(10.0514385264421,143.656247508139,3.26591035271534));
#277422=CARTESIAN_POINT('Ctrl Pts',(10.0514385264421,143.806247508139,-1.23094620182339E-15));
#277423=CARTESIAN_POINT('Ctrl Pts',(10.0514385264421,143.956247508138,-3.26591035271534));
#277424=CARTESIAN_POINT('Ctrl Pts',(8.13178458580674,144.106247508138,-5.90808733016713));
#277425=CARTESIAN_POINT('Ctrl Pts',(6.21213064517135,144.256247508137,-8.55026430761891));
#277426=CARTESIAN_POINT('Ctrl Pts',(3.10606532258563,144.406247508136,-9.55948610871303));
#277427=CARTESIAN_POINT('Ctrl Pts',(-9.63751598336927E-14,144.556247508136,
-10.5687079098071));
#277428=CARTESIAN_POINT('Ctrl Pts',(-3.10606532258582,144.706247508135,
-9.55948610871303));
#277429=CARTESIAN_POINT('Ctrl Pts',(-6.21213064517155,144.856247508135,
-8.55026430761891));
#277430=CARTESIAN_POINT('Ctrl Pts',(-8.13178458580693,145.006247508134,
-5.90808733016712));
#277431=CARTESIAN_POINT('Ctrl Pts',(-10.0514385264423,145.156247508133,
-3.26591035271534));
#277432=CARTESIAN_POINT('Ctrl Pts',(-10.0514385264423,145.306247508133,
2.46189240364677E-15));
#277433=CARTESIAN_POINT('Ctrl Pts',(-10.0514385264423,145.456247508132,
3.26591035271534));
#277434=CARTESIAN_POINT('Ctrl Pts',(-8.13178458580693,145.606247508132,
5.90808733016713));
#277435=CARTESIAN_POINT('Ctrl Pts',(-6.21213064517154,145.756247508131,
8.55026430761891));
#277436=CARTESIAN_POINT('Ctrl Pts',(-3.10606532258582,145.90624750813,9.55948610871303));
#277437=CARTESIAN_POINT('Ctrl Pts',(-9.46504276069498E-14,146.05624750813,
10.5687079098071));
#277438=CARTESIAN_POINT('Ctrl Pts',(3.10606532258563,146.206247508129,9.55948610871303));
#277439=CARTESIAN_POINT('Ctrl Pts',(6.21213064517135,146.356247508129,8.55026430761891));
#277440=CARTESIAN_POINT('Ctrl Pts',(8.13178458580674,146.506247508128,5.90808733016712));
#277441=CARTESIAN_POINT('Ctrl Pts',(10.0514385264421,146.656247508127,3.26591035271534));
#277442=CARTESIAN_POINT('Ctrl Pts',(10.0514385264421,146.806247508127,-1.23094620182339E-15));
#277443=CARTESIAN_POINT('Ctrl Pts',(10.0514385264421,146.956247508126,-3.26591035271534));
#277444=CARTESIAN_POINT('Ctrl Pts',(8.13178458580674,147.106247508126,-5.90808733016713));
#277445=CARTESIAN_POINT('Ctrl Pts',(6.21213064517135,147.256247508125,-8.55026430761891));
#277446=CARTESIAN_POINT('Ctrl Pts',(3.10606532258563,147.406247508124,-9.55948610871303));
#277447=CARTESIAN_POINT('Ctrl Pts',(-9.81028691053545E-14,147.556247508124,
-10.5687079098071));
#277448=CARTESIAN_POINT('Ctrl Pts',(-3.10606532258582,147.706247508123,
-9.55948610871303));
#277449=CARTESIAN_POINT('Ctrl Pts',(-6.21213064517155,147.856247508123,
-8.55026430761891));
#277450=CARTESIAN_POINT('Ctrl Pts',(-8.13178458580693,148.006247508122,
-5.90808733016712));
#277451=CARTESIAN_POINT('Ctrl Pts',(-10.0514385264423,148.156247508121,
-3.26591035271534));
#277452=CARTESIAN_POINT('Ctrl Pts',(-10.0514385264423,148.306247508121,
2.46189240364677E-15));
#277453=CARTESIAN_POINT('Ctrl Pts',(-10.0514385264423,148.45624750812,3.26591035271534));
#277454=CARTESIAN_POINT('Ctrl Pts',(-8.13178458580693,148.60624750812,5.90808733016713));
#277455=CARTESIAN_POINT('Ctrl Pts',(-6.21213064517155,148.756247508119,
8.55026430761891));
#277456=CARTESIAN_POINT('Ctrl Pts',(-3.10606532258582,148.906247508118,
9.55948610871303));
#277457=CARTESIAN_POINT('Ctrl Pts',(-9.63781368786116E-14,149.056247508118,
10.5687079098071));
#277458=CARTESIAN_POINT('Ctrl Pts',(3.10606532258563,149.206247508117,9.55948610871303));
#277459=CARTESIAN_POINT('Ctrl Pts',(6.21213064517135,149.356247508117,8.55026430761891));
#277460=CARTESIAN_POINT('Ctrl Pts',(8.13178458580673,149.506247508116,5.90808733016712));
#277461=CARTESIAN_POINT('Ctrl Pts',(10.0514385264421,149.656247508115,3.26591035271534));
#277462=CARTESIAN_POINT('Ctrl Pts',(10.0514385264421,149.806247508115,-1.23094620182339E-15));
#277463=CARTESIAN_POINT('Ctrl Pts',(10.0514385264421,149.956247508114,-3.26591035271534));
#277464=CARTESIAN_POINT('Ctrl Pts',(8.13178458580673,150.106247508114,-5.90808733016713));
#277465=CARTESIAN_POINT('Ctrl Pts',(6.21213064517135,150.256247508113,-8.55026430761891));
#277466=CARTESIAN_POINT('Ctrl Pts',(3.10606532258562,150.406247508112,-9.55948610871303));
#277467=CARTESIAN_POINT('Ctrl Pts',(-9.98305783770163E-14,150.556247508112,
-10.5687079098071));
#277468=CARTESIAN_POINT('Ctrl Pts',(-3.10606532258582,150.706247508111,
-9.55948610871303));
#277469=CARTESIAN_POINT('Ctrl Pts',(-6.21213064517155,150.856247508111,
-8.55026430761891));
#277470=CARTESIAN_POINT('Ctrl Pts',(-8.13178458580694,151.00624750811,-5.90808733016712));
#277471=CARTESIAN_POINT('Ctrl Pts',(-10.0514385264423,151.156247508109,
-3.26591035271534));
#277472=CARTESIAN_POINT('Ctrl Pts',(-10.0514385264423,151.306247508109,
2.46189240364677E-15));
#277473=CARTESIAN_POINT('Ctrl Pts',(-10.0514385264423,151.456247508108,
3.26591035271534));
#277474=CARTESIAN_POINT('Ctrl Pts',(-8.13178458580694,151.606247508108,
5.90808733016713));
#277475=CARTESIAN_POINT('Ctrl Pts',(-6.21213064517155,151.756247508107,
8.55026430761891));
#277476=CARTESIAN_POINT('Ctrl Pts',(-3.10606532258582,151.906247508106,
9.55948610871303));
#277477=CARTESIAN_POINT('Ctrl Pts',(-9.81058461502735E-14,152.056247508106,
10.5687079098071));
#277478=CARTESIAN_POINT('Ctrl Pts',(3.10606532258563,152.206247508105,9.55948610871303));
#277479=CARTESIAN_POINT('Ctrl Pts',(6.21213064517135,152.356247508105,8.55026430761891));
#277480=CARTESIAN_POINT('Ctrl Pts',(8.13178458580673,152.506247508104,5.90808733016712));
#277481=CARTESIAN_POINT('Ctrl Pts',(10.0514385264421,152.656247508103,3.26591035271534));
#277482=CARTESIAN_POINT('Ctrl Pts',(10.0514385264421,152.806247508103,-1.23094620182339E-15));
#277483=CARTESIAN_POINT('Ctrl Pts',(10.0514385264421,152.956247508102,-3.26591035271534));
#277484=CARTESIAN_POINT('Ctrl Pts',(8.13178458580673,153.106247508102,-5.90808733016713));
#277485=CARTESIAN_POINT('Ctrl Pts',(6.21213064517135,153.256247508101,-8.55026430761891));
#277486=CARTESIAN_POINT('Ctrl Pts',(3.10606532258562,153.4062475081,-9.55948610871303));
#277487=CARTESIAN_POINT('Ctrl Pts',(-1.01558287648678E-13,153.5562475081,
-10.5687079098071));
#277488=CARTESIAN_POINT('Ctrl Pts',(-3.10606532258583,153.706247508099,
-9.55948610871303));
#277489=CARTESIAN_POINT('Ctrl Pts',(-12.1623797632097,-0.474999999988005,
2.97892388940585E-15));
#277490=CARTESIAN_POINT('Ctrl Pts',(-12.1623797632096,-0.324999999988605,
3.95179673813133));
#277491=CARTESIAN_POINT('Ctrl Pts',(-9.83957192047856,-0.174999999989203,
7.14886745759505));
#277492=CARTESIAN_POINT('Ctrl Pts',(-7.51676407774747,-0.0249999999898023,
10.3459381770588));
#277493=CARTESIAN_POINT('Ctrl Pts',(-3.75838203887374,0.1250000000096,11.5671105274568));
#277494=CARTESIAN_POINT('Ctrl Pts',(-1.02868273148643E-14,0.275000000009002,
12.7882828778549));
#277495=CARTESIAN_POINT('Ctrl Pts',(3.75838203887372,0.425000000008404,
11.5671105274568));
#277496=CARTESIAN_POINT('Ctrl Pts',(7.51676407774745,0.575000000007806,
10.3459381770588));
#277497=CARTESIAN_POINT('Ctrl Pts',(9.83957192047854,0.725000000007208,
7.14886745759505));
#277498=CARTESIAN_POINT('Ctrl Pts',(12.1623797632096,0.875000000006609,
3.95179673813132));
#277499=CARTESIAN_POINT('Ctrl Pts',(12.1623797632096,1.02500000000601,-1.48946194470292E-15));
#277500=CARTESIAN_POINT('Ctrl Pts',(12.1623797632096,1.17500000000541,-3.95179673813132));
#277501=CARTESIAN_POINT('Ctrl Pts',(9.83957192047853,1.32500000000481,-7.14886745759505));
#277502=CARTESIAN_POINT('Ctrl Pts',(7.51676407774744,1.47500000000421,-10.3459381770588));
#277503=CARTESIAN_POINT('Ctrl Pts',(3.75838203887371,1.6250000000036,-11.5671105274568));
#277504=CARTESIAN_POINT('Ctrl Pts',(-1.42829078892864E-14,1.775000000003,
-12.7882828778549));
#277505=CARTESIAN_POINT('Ctrl Pts',(-3.75838203887374,1.9250000000024,-11.5671105274568));
#277506=CARTESIAN_POINT('Ctrl Pts',(-7.51676407774747,2.0750000000018,-10.3459381770588));
#277507=CARTESIAN_POINT('Ctrl Pts',(-9.83957192047856,2.2250000000012,-7.14886745759505));
#277508=CARTESIAN_POINT('Ctrl Pts',(-12.1623797632097,2.37500000000059,
-3.95179673813132));
#277509=CARTESIAN_POINT('Ctrl Pts',(-12.1623797632097,2.525,2.97892388940585E-15));
#277510=CARTESIAN_POINT('Ctrl Pts',(-12.1623797632097,2.6749999999994,3.95179673813133));
#277511=CARTESIAN_POINT('Ctrl Pts',(-9.83957192047856,2.8249999999988,7.14886745759505));
#277512=CARTESIAN_POINT('Ctrl Pts',(-7.51676407774747,2.9749999999982,10.3459381770588));
#277513=CARTESIAN_POINT('Ctrl Pts',(-3.75838203887374,3.1249999999976,11.5671105274568));
#277514=CARTESIAN_POINT('Ctrl Pts',(-1.20145365865262E-14,3.274999999997,
12.7882828778549));
#277515=CARTESIAN_POINT('Ctrl Pts',(3.75838203887372,3.4249999999964,11.5671105274568));
#277516=CARTESIAN_POINT('Ctrl Pts',(7.51676407774744,3.57499999999581,10.3459381770588));
#277517=CARTESIAN_POINT('Ctrl Pts',(9.83957192047853,3.72499999999521,7.14886745759505));
#277518=CARTESIAN_POINT('Ctrl Pts',(12.1623797632096,3.87499999999461,3.95179673813132));
#277519=CARTESIAN_POINT('Ctrl Pts',(12.1623797632096,4.02499999999401,-1.48946194470292E-15));
#277520=CARTESIAN_POINT('Ctrl Pts',(12.1623797632096,4.17499999999341,-3.95179673813132));
#277521=CARTESIAN_POINT('Ctrl Pts',(9.83957192047853,4.32499999999281,-7.14886745759505));
#277522=CARTESIAN_POINT('Ctrl Pts',(7.51676407774744,4.47499999999221,-10.3459381770588));
#277523=CARTESIAN_POINT('Ctrl Pts',(3.75838203887371,4.6249999999916,-11.5671105274568));
#277524=CARTESIAN_POINT('Ctrl Pts',(-1.60106171609483E-14,4.774999999991,
-12.7882828778549));
#277525=CARTESIAN_POINT('Ctrl Pts',(-3.75838203887374,4.9249999999904,-11.5671105274568));
#277526=CARTESIAN_POINT('Ctrl Pts',(-7.51676407774747,5.0749999999898,-10.3459381770588));
#277527=CARTESIAN_POINT('Ctrl Pts',(-9.83957192047857,5.2249999999892,-7.14886745759505));
#277528=CARTESIAN_POINT('Ctrl Pts',(-12.1623797632097,5.3749999999886,-3.95179673813132));
#277529=CARTESIAN_POINT('Ctrl Pts',(-12.1623797632097,5.52499999998799,
2.97892388940585E-15));
#277530=CARTESIAN_POINT('Ctrl Pts',(-12.1623797632097,5.67499999998739,
3.95179673813133));
#277531=CARTESIAN_POINT('Ctrl Pts',(-9.83957192047857,5.8249999999868,7.14886745759505));
#277532=CARTESIAN_POINT('Ctrl Pts',(-7.51676407774747,5.9749999999862,10.3459381770588));
#277533=CARTESIAN_POINT('Ctrl Pts',(-3.75838203887374,6.1249999999856,11.5671105274568));
#277534=CARTESIAN_POINT('Ctrl Pts',(-1.3742245858188E-14,6.274999999985,
12.7882828778549));
#277535=CARTESIAN_POINT('Ctrl Pts',(3.75838203887371,6.4249999999844,11.5671105274568));
#277536=CARTESIAN_POINT('Ctrl Pts',(7.51676407774744,6.57499999998381,10.3459381770588));
#277537=CARTESIAN_POINT('Ctrl Pts',(9.83957192047853,6.72499999998321,7.14886745759505));
#277538=CARTESIAN_POINT('Ctrl Pts',(12.1623797632096,6.87499999998261,3.95179673813132));
#277539=CARTESIAN_POINT('Ctrl Pts',(12.1623797632096,7.02499999998201,-1.48946194470292E-15));
#277540=CARTESIAN_POINT('Ctrl Pts',(12.1623797632096,7.17499999998141,-3.95179673813132));
#277541=CARTESIAN_POINT('Ctrl Pts',(9.83957192047853,7.32499999998081,-7.14886745759505));
#277542=CARTESIAN_POINT('Ctrl Pts',(7.51676407774744,7.47499999998021,-10.3459381770588));
#277543=CARTESIAN_POINT('Ctrl Pts',(3.75838203887371,7.6249999999796,-11.5671105274568));
#277544=CARTESIAN_POINT('Ctrl Pts',(-1.77383264326101E-14,7.774999999979,
-12.7882828778549));
#277545=CARTESIAN_POINT('Ctrl Pts',(-3.75838203887375,7.9249999999784,-11.5671105274568));
#277546=CARTESIAN_POINT('Ctrl Pts',(-7.51676407774747,8.0749999999778,-10.3459381770588));
#277547=CARTESIAN_POINT('Ctrl Pts',(-9.83957192047857,8.2249999999772,-7.14886745759505));
#277548=CARTESIAN_POINT('Ctrl Pts',(-12.1623797632097,8.3749999999766,-3.95179673813132));
#277549=CARTESIAN_POINT('Ctrl Pts',(-12.1623797632097,8.52499999997599,
2.97892388940585E-15));
#277550=CARTESIAN_POINT('Ctrl Pts',(-12.1623797632097,8.6749999999754,3.95179673813133));
#277551=CARTESIAN_POINT('Ctrl Pts',(-9.83957192047857,8.8249999999748,7.14886745759505));
#277552=CARTESIAN_POINT('Ctrl Pts',(-7.51676407774747,8.9749999999742,10.3459381770588));
#277553=CARTESIAN_POINT('Ctrl Pts',(-3.75838203887374,9.1249999999736,11.5671105274568));
#277554=CARTESIAN_POINT('Ctrl Pts',(-1.54699551298498E-14,9.274999999973,
12.7882828778549));
#277555=CARTESIAN_POINT('Ctrl Pts',(3.75838203887371,9.4249999999724,11.5671105274568));
#277556=CARTESIAN_POINT('Ctrl Pts',(7.51676407774744,9.57499999997181,10.3459381770588));
#277557=CARTESIAN_POINT('Ctrl Pts',(9.83957192047853,9.72499999997121,7.14886745759505));
#277558=CARTESIAN_POINT('Ctrl Pts',(12.1623797632096,9.87499999997061,3.95179673813132));
#277559=CARTESIAN_POINT('Ctrl Pts',(12.1623797632096,10.02499999997,-1.48946194470292E-15));
#277560=CARTESIAN_POINT('Ctrl Pts',(12.1623797632096,10.1749999999694,-3.95179673813132));
#277561=CARTESIAN_POINT('Ctrl Pts',(9.83957192047853,10.3249999999688,-7.14886745759505));
#277562=CARTESIAN_POINT('Ctrl Pts',(7.51676407774744,10.4749999999682,-10.3459381770588));
#277563=CARTESIAN_POINT('Ctrl Pts',(3.75838203887371,10.6249999999676,-11.5671105274568));
#277564=CARTESIAN_POINT('Ctrl Pts',(-1.9466035704272E-14,10.774999999967,
-12.7882828778549));
#277565=CARTESIAN_POINT('Ctrl Pts',(-3.75838203887375,10.9249999999664,
-11.5671105274568));
#277566=CARTESIAN_POINT('Ctrl Pts',(-7.51676407774748,11.0749999999658,
-10.3459381770588));
#277567=CARTESIAN_POINT('Ctrl Pts',(-9.83957192047857,11.2249999999652,
-7.14886745759505));
#277568=CARTESIAN_POINT('Ctrl Pts',(-12.1623797632097,11.3749999999646,
-3.95179673813132));
#277569=CARTESIAN_POINT('Ctrl Pts',(-12.1623797632097,11.524999999964,2.97892388940585E-15));
#277570=CARTESIAN_POINT('Ctrl Pts',(-12.1623797632097,11.6749999999634,
3.95179673813133));
#277571=CARTESIAN_POINT('Ctrl Pts',(-9.83957192047857,11.8249999999628,
7.14886745759505));
#277572=CARTESIAN_POINT('Ctrl Pts',(-7.51676407774747,11.9749999999622,
10.3459381770588));
#277573=CARTESIAN_POINT('Ctrl Pts',(-3.75838203887375,12.1249999999616,
11.5671105274568));
#277574=CARTESIAN_POINT('Ctrl Pts',(-1.71976644015117E-14,12.274999999961,
12.7882828778549));
#277575=CARTESIAN_POINT('Ctrl Pts',(3.75838203887371,12.4249999999604,11.5671105274568));
#277576=CARTESIAN_POINT('Ctrl Pts',(7.51676407774744,12.5749999999598,10.3459381770588));
#277577=CARTESIAN_POINT('Ctrl Pts',(9.83957192047853,12.7249999999592,7.14886745759505));
#277578=CARTESIAN_POINT('Ctrl Pts',(12.1623797632096,12.8749999999586,3.95179673813132));
#277579=CARTESIAN_POINT('Ctrl Pts',(12.1623797632096,13.024999999958,-1.48946194470292E-15));
#277580=CARTESIAN_POINT('Ctrl Pts',(12.1623797632096,13.1749999999574,-3.95179673813132));
#277581=CARTESIAN_POINT('Ctrl Pts',(9.83957192047853,13.3249999999568,-7.14886745759505));
#277582=CARTESIAN_POINT('Ctrl Pts',(7.51676407774743,13.4749999999562,-10.3459381770588));
#277583=CARTESIAN_POINT('Ctrl Pts',(3.75838203887371,13.6249999999556,-11.5671105274568));
#277584=CARTESIAN_POINT('Ctrl Pts',(-2.11937449759338E-14,13.774999999955,
-12.7882828778549));
#277585=CARTESIAN_POINT('Ctrl Pts',(-3.75838203887375,13.9249999999544,
-11.5671105274568));
#277586=CARTESIAN_POINT('Ctrl Pts',(-7.51676407774748,14.0749999999538,
-10.3459381770588));
#277587=CARTESIAN_POINT('Ctrl Pts',(-9.83957192047857,14.2249999999532,
-7.14886745759505));
#277588=CARTESIAN_POINT('Ctrl Pts',(-12.1623797632097,14.3749999999526,
-3.95179673813132));
#277589=CARTESIAN_POINT('Ctrl Pts',(-12.1623797632097,14.524999999952,2.97892388940585E-15));
#277590=CARTESIAN_POINT('Ctrl Pts',(-12.1623797632097,14.6749999999514,
3.95179673813133));
#277591=CARTESIAN_POINT('Ctrl Pts',(-9.83957192047857,14.8249999999508,
7.14886745759505));
#277592=CARTESIAN_POINT('Ctrl Pts',(-7.51676407774747,14.9749999999502,
10.3459381770588));
#277593=CARTESIAN_POINT('Ctrl Pts',(-3.75838203887375,15.1249999999496,
11.5671105274568));
#277594=CARTESIAN_POINT('Ctrl Pts',(-1.89253736731735E-14,15.274999999949,
12.7882828778549));
#277595=CARTESIAN_POINT('Ctrl Pts',(3.75838203887371,15.4249999999484,11.5671105274568));
#277596=CARTESIAN_POINT('Ctrl Pts',(7.51676407774744,15.5749999999478,10.3459381770588));
#277597=CARTESIAN_POINT('Ctrl Pts',(9.83957192047853,15.7249999999472,7.14886745759505));
#277598=CARTESIAN_POINT('Ctrl Pts',(12.1623797632096,15.8749999999466,3.95179673813132));
#277599=CARTESIAN_POINT('Ctrl Pts',(12.1623797632096,16.024999999946,-1.48946194470292E-15));
#277600=CARTESIAN_POINT('Ctrl Pts',(12.1623797632096,16.1749999999454,-3.95179673813132));
#277601=CARTESIAN_POINT('Ctrl Pts',(9.83957192047852,16.3249999999448,-7.14886745759505));
#277602=CARTESIAN_POINT('Ctrl Pts',(7.51676407774743,16.4749999999442,-10.3459381770588));
#277603=CARTESIAN_POINT('Ctrl Pts',(3.7583820388737,16.6249999999436,-11.5671105274568));
#277604=CARTESIAN_POINT('Ctrl Pts',(-2.29214542475956E-14,16.774999999943,
-12.7882828778549));
#277605=CARTESIAN_POINT('Ctrl Pts',(-3.75838203887375,16.9249999999424,
-11.5671105274568));
#277606=CARTESIAN_POINT('Ctrl Pts',(-7.51676407774748,17.0749999999418,
-10.3459381770588));
#277607=CARTESIAN_POINT('Ctrl Pts',(-9.83957192047857,17.2249999999412,
-7.14886745759505));
#277608=CARTESIAN_POINT('Ctrl Pts',(-12.1623797632097,17.3749999999406,
-3.95179673813132));
#277609=CARTESIAN_POINT('Ctrl Pts',(-12.1623797632097,17.52499999994,2.97892388940585E-15));
#277610=CARTESIAN_POINT('Ctrl Pts',(-12.1623797632097,17.6749999999394,
3.95179673813133));
#277611=CARTESIAN_POINT('Ctrl Pts',(-9.83957192047857,17.8249999999388,
7.14886745759505));
#277612=CARTESIAN_POINT('Ctrl Pts',(-7.51676407774748,17.9749999999382,
10.3459381770588));
#277613=CARTESIAN_POINT('Ctrl Pts',(-3.75838203887375,18.1249999999376,
11.5671105274568));
#277614=CARTESIAN_POINT('Ctrl Pts',(-2.06530829448354E-14,18.274999999937,
12.7882828778549));
#277615=CARTESIAN_POINT('Ctrl Pts',(3.75838203887371,18.4249999999364,11.5671105274568));
#277616=CARTESIAN_POINT('Ctrl Pts',(7.51676407774743,18.5749999999358,10.3459381770588));
#277617=CARTESIAN_POINT('Ctrl Pts',(9.83957192047852,18.7249999999352,7.14886745759505));
#277618=CARTESIAN_POINT('Ctrl Pts',(12.1623797632096,18.8749999999346,3.95179673813132));
#277619=CARTESIAN_POINT('Ctrl Pts',(12.1623797632096,19.024999999934,-1.48946194470292E-15));
#277620=CARTESIAN_POINT('Ctrl Pts',(12.1623797632096,19.1749999999334,-3.95179673813132));
#277621=CARTESIAN_POINT('Ctrl Pts',(9.83957192047852,19.3249999999328,-7.14886745759505));
#277622=CARTESIAN_POINT('Ctrl Pts',(7.51676407774743,19.4749999999322,-10.3459381770588));
#277623=CARTESIAN_POINT('Ctrl Pts',(3.7583820388737,19.6249999999316,-11.5671105274568));
#277624=CARTESIAN_POINT('Ctrl Pts',(-2.46491635192575E-14,19.774999999931,
-12.7882828778549));
#277625=CARTESIAN_POINT('Ctrl Pts',(-3.75838203887375,19.9249999999304,
-11.5671105274568));
#277626=CARTESIAN_POINT('Ctrl Pts',(-7.51676407774748,20.0749999999298,
-10.3459381770588));
#277627=CARTESIAN_POINT('Ctrl Pts',(-9.83957192047857,20.2249999999292,
-7.14886745759505));
#277628=CARTESIAN_POINT('Ctrl Pts',(-12.1623797632097,20.3749999999286,
-3.95179673813132));
#277629=CARTESIAN_POINT('Ctrl Pts',(-12.1623797632097,20.524999999928,2.97892388940585E-15));
#277630=CARTESIAN_POINT('Ctrl Pts',(-12.1623797632097,20.6749999999274,
3.95179673813133));
#277631=CARTESIAN_POINT('Ctrl Pts',(-9.83957192047857,20.8249999999268,
7.14886745759505));
#277632=CARTESIAN_POINT('Ctrl Pts',(-7.51676407774748,20.9749999999262,
10.3459381770588));
#277633=CARTESIAN_POINT('Ctrl Pts',(-3.75838203887375,21.1249999999256,
11.5671105274568));
#277634=CARTESIAN_POINT('Ctrl Pts',(-2.23807922164972E-14,21.274999999925,
12.7882828778549));
#277635=CARTESIAN_POINT('Ctrl Pts',(3.7583820388737,21.4249999999244,11.5671105274568));
#277636=CARTESIAN_POINT('Ctrl Pts',(7.51676407774743,21.5749999999238,10.3459381770588));
#277637=CARTESIAN_POINT('Ctrl Pts',(9.83957192047852,21.7249999999232,7.14886745759505));
#277638=CARTESIAN_POINT('Ctrl Pts',(12.1623797632096,21.8749999999226,3.95179673813132));
#277639=CARTESIAN_POINT('Ctrl Pts',(12.1623797632096,22.024999999922,-1.48946194470292E-15));
#277640=CARTESIAN_POINT('Ctrl Pts',(12.1623797632096,22.1749999999214,-3.95179673813132));
#277641=CARTESIAN_POINT('Ctrl Pts',(9.83957192047852,22.3249999999208,-7.14886745759505));
#277642=CARTESIAN_POINT('Ctrl Pts',(7.51676407774743,22.4749999999202,-10.3459381770588));
#277643=CARTESIAN_POINT('Ctrl Pts',(3.7583820388737,22.6249999999196,-11.5671105274568));
#277644=CARTESIAN_POINT('Ctrl Pts',(-2.63768727909193E-14,22.774999999919,
-12.7882828778549));
#277645=CARTESIAN_POINT('Ctrl Pts',(-3.75838203887375,22.9249999999184,
-11.5671105274568));
#277646=CARTESIAN_POINT('Ctrl Pts',(-7.51676407774748,23.0749999999178,
-10.3459381770588));
#277647=CARTESIAN_POINT('Ctrl Pts',(-9.83957192047857,23.2249999999172,
-7.14886745759505));
#277648=CARTESIAN_POINT('Ctrl Pts',(-12.1623797632097,23.3749999999166,
-3.95179673813132));
#277649=CARTESIAN_POINT('Ctrl Pts',(-12.1623797632097,23.524999999916,2.97892388940585E-15));
#277650=CARTESIAN_POINT('Ctrl Pts',(-12.1623797632097,23.6749999999154,
3.95179673813133));
#277651=CARTESIAN_POINT('Ctrl Pts',(-9.83957192047857,23.8249999999148,
7.14886745759505));
#277652=CARTESIAN_POINT('Ctrl Pts',(-7.51676407774748,23.9749999999142,
10.3459381770588));
#277653=CARTESIAN_POINT('Ctrl Pts',(-3.75838203887375,24.1249999999136,
11.5671105274568));
#277654=CARTESIAN_POINT('Ctrl Pts',(-2.4108501488159E-14,24.274999999913,
12.7882828778549));
#277655=CARTESIAN_POINT('Ctrl Pts',(3.7583820388737,24.4249999999124,11.5671105274568));
#277656=CARTESIAN_POINT('Ctrl Pts',(7.51676407774743,24.5749999999118,10.3459381770588));
#277657=CARTESIAN_POINT('Ctrl Pts',(9.83957192047852,24.7249999999112,7.14886745759505));
#277658=CARTESIAN_POINT('Ctrl Pts',(12.1623797632096,24.8749999999106,3.95179673813132));
#277659=CARTESIAN_POINT('Ctrl Pts',(12.1623797632096,25.02499999991,-1.48946194470292E-15));
#277660=CARTESIAN_POINT('Ctrl Pts',(12.1623797632096,25.1749999999094,-3.95179673813132));
#277661=CARTESIAN_POINT('Ctrl Pts',(9.83957192047852,25.3249999999088,-7.14886745759505));
#277662=CARTESIAN_POINT('Ctrl Pts',(7.51676407774743,25.4749999999082,-10.3459381770588));
#277663=CARTESIAN_POINT('Ctrl Pts',(3.7583820388737,25.6249999999076,-11.5671105274568));
#277664=CARTESIAN_POINT('Ctrl Pts',(-2.81045820625811E-14,25.774999999907,
-12.7882828778549));
#277665=CARTESIAN_POINT('Ctrl Pts',(-3.75838203887376,25.9249999999064,
-11.5671105274568));
#277666=CARTESIAN_POINT('Ctrl Pts',(-7.51676407774749,26.0749999999058,
-10.3459381770588));
#277667=CARTESIAN_POINT('Ctrl Pts',(-9.83957192047857,26.2249999999052,
-7.14886745759505));
#277668=CARTESIAN_POINT('Ctrl Pts',(-12.1623797632097,26.3749999999046,
-3.95179673813132));
#277669=CARTESIAN_POINT('Ctrl Pts',(-12.1623797632097,26.524999999904,2.97892388940585E-15));
#277670=CARTESIAN_POINT('Ctrl Pts',(-12.1623797632097,26.6749999999034,
3.95179673813133));
#277671=CARTESIAN_POINT('Ctrl Pts',(-9.83957192047857,26.8249999999028,
7.14886745759505));
#277672=CARTESIAN_POINT('Ctrl Pts',(-7.51676407774748,26.9749999999022,
10.3459381770588));
#277673=CARTESIAN_POINT('Ctrl Pts',(-3.75838203887375,27.1249999999016,
11.5671105274568));
#277674=CARTESIAN_POINT('Ctrl Pts',(-2.58362107598209E-14,27.274999999901,
12.7882828778549));
#277675=CARTESIAN_POINT('Ctrl Pts',(3.7583820388737,27.4249999999004,11.5671105274568));
#277676=CARTESIAN_POINT('Ctrl Pts',(7.51676407774743,27.5749999998998,10.3459381770588));
#277677=CARTESIAN_POINT('Ctrl Pts',(9.83957192047852,27.7249999998992,7.14886745759505));
#277678=CARTESIAN_POINT('Ctrl Pts',(12.1623797632096,27.8749999998986,3.95179673813132));
#277679=CARTESIAN_POINT('Ctrl Pts',(12.1623797632096,28.024999999898,-1.48946194470292E-15));
#277680=CARTESIAN_POINT('Ctrl Pts',(12.1623797632096,28.1749999998974,-3.95179673813132));
#277681=CARTESIAN_POINT('Ctrl Pts',(9.83957192047852,28.3249999998968,-7.14886745759505));
#277682=CARTESIAN_POINT('Ctrl Pts',(7.51676407774743,28.4749999998962,-10.3459381770588));
#277683=CARTESIAN_POINT('Ctrl Pts',(3.7583820388737,28.6249999998956,-11.5671105274568));
#277684=CARTESIAN_POINT('Ctrl Pts',(-2.9832291334243E-14,28.774999999895,
-12.7882828778549));
#277685=CARTESIAN_POINT('Ctrl Pts',(-3.75838203887376,28.9249999998944,
-11.5671105274568));
#277686=CARTESIAN_POINT('Ctrl Pts',(-7.51676407774749,29.0749999998938,
-10.3459381770588));
#277687=CARTESIAN_POINT('Ctrl Pts',(-9.83957192047858,29.2249999998932,
-7.14886745759505));
#277688=CARTESIAN_POINT('Ctrl Pts',(-12.1623797632097,29.3749999998926,
-3.95179673813132));
#277689=CARTESIAN_POINT('Ctrl Pts',(-12.1623797632097,29.524999999892,2.97892388940585E-15));
#277690=CARTESIAN_POINT('Ctrl Pts',(-12.1623797632097,29.6749999998914,
3.95179673813133));
#277691=CARTESIAN_POINT('Ctrl Pts',(-9.83957192047858,29.8249999998908,
7.14886745759505));
#277692=CARTESIAN_POINT('Ctrl Pts',(-7.51676407774748,29.9749999998902,
10.3459381770588));
#277693=CARTESIAN_POINT('Ctrl Pts',(-3.75838203887376,30.1249999998896,
11.5671105274568));
#277694=CARTESIAN_POINT('Ctrl Pts',(-2.75639200314827E-14,30.274999999889,
12.7882828778549));
#277695=CARTESIAN_POINT('Ctrl Pts',(3.7583820388737,30.4249999998884,11.5671105274568));
#277696=CARTESIAN_POINT('Ctrl Pts',(7.51676407774743,30.5749999998878,10.3459381770588));
#277697=CARTESIAN_POINT('Ctrl Pts',(9.83957192047852,30.7249999998872,7.14886745759505));
#277698=CARTESIAN_POINT('Ctrl Pts',(12.1623797632096,30.8749999998866,3.95179673813132));
#277699=CARTESIAN_POINT('Ctrl Pts',(12.1623797632096,31.024999999886,-1.48946194470292E-15));
#277700=CARTESIAN_POINT('Ctrl Pts',(12.1623797632096,31.1749999998854,-3.95179673813132));
#277701=CARTESIAN_POINT('Ctrl Pts',(9.83957192047852,31.3249999998848,-7.14886745759505));
#277702=CARTESIAN_POINT('Ctrl Pts',(7.51676407774742,31.4749999998842,-10.3459381770588));
#277703=CARTESIAN_POINT('Ctrl Pts',(3.7583820388737,31.6249999998836,-11.5671105274568));
#277704=CARTESIAN_POINT('Ctrl Pts',(-3.15600006059048E-14,31.774999999883,
-12.7882828778549));
#277705=CARTESIAN_POINT('Ctrl Pts',(-3.75838203887376,31.9249999998824,
-11.5671105274568));
#277706=CARTESIAN_POINT('Ctrl Pts',(-7.51676407774749,32.0749999998818,
-10.3459381770588));
#277707=CARTESIAN_POINT('Ctrl Pts',(-9.83957192047858,32.2249999998812,
-7.14886745759505));
#277708=CARTESIAN_POINT('Ctrl Pts',(-12.1623797632097,32.3749999998806,
-3.95179673813132));
#277709=CARTESIAN_POINT('Ctrl Pts',(-12.1623797632097,32.52499999988,2.97892388940585E-15));
#277710=CARTESIAN_POINT('Ctrl Pts',(-12.1623797632097,32.6749999998794,
3.95179673813133));
#277711=CARTESIAN_POINT('Ctrl Pts',(-9.83957192047858,32.8249999998788,
7.14886745759505));
#277712=CARTESIAN_POINT('Ctrl Pts',(-7.51676407774749,32.9749999998782,
10.3459381770588));
#277713=CARTESIAN_POINT('Ctrl Pts',(-3.75838203887376,33.1249999998776,
11.5671105274568));
#277714=CARTESIAN_POINT('Ctrl Pts',(-2.92916293031446E-14,33.274999999877,
12.7882828778549));
#277715=CARTESIAN_POINT('Ctrl Pts',(3.7583820388737,33.4249999998764,11.5671105274568));
#277716=CARTESIAN_POINT('Ctrl Pts',(7.51676407774743,33.5749999998758,10.3459381770588));
#277717=CARTESIAN_POINT('Ctrl Pts',(9.83957192047852,33.7249999998752,7.14886745759505));
#277718=CARTESIAN_POINT('Ctrl Pts',(12.1623797632096,33.8749999998746,3.95179673813132));
#277719=CARTESIAN_POINT('Ctrl Pts',(12.1623797632096,34.024999999874,-1.48946194470292E-15));
#277720=CARTESIAN_POINT('Ctrl Pts',(12.1623797632096,34.1749999998734,-3.95179673813132));
#277721=CARTESIAN_POINT('Ctrl Pts',(9.83957192047851,34.3249999998728,-7.14886745759505));
#277722=CARTESIAN_POINT('Ctrl Pts',(7.51676407774742,34.4749999998722,-10.3459381770588));
#277723=CARTESIAN_POINT('Ctrl Pts',(3.7583820388737,34.6249999998716,-11.5671105274568));
#277724=CARTESIAN_POINT('Ctrl Pts',(-3.32877098775667E-14,34.774999999871,
-12.7882828778549));
#277725=CARTESIAN_POINT('Ctrl Pts',(-3.75838203887376,34.9249999998704,
-11.5671105274568));
#277726=CARTESIAN_POINT('Ctrl Pts',(-7.51676407774749,35.0749999998698,
-10.3459381770588));
#277727=CARTESIAN_POINT('Ctrl Pts',(-9.83957192047858,35.2249999998692,
-7.14886745759505));
#277728=CARTESIAN_POINT('Ctrl Pts',(-12.1623797632097,35.3749999998686,
-3.95179673813132));
#277729=CARTESIAN_POINT('Ctrl Pts',(-12.1623797632097,35.524999999868,2.97892388940585E-15));
#277730=CARTESIAN_POINT('Ctrl Pts',(-12.1623797632097,35.6749999998674,
3.95179673813133));
#277731=CARTESIAN_POINT('Ctrl Pts',(-9.83957192047858,35.8249999998668,
7.14886745759505));
#277732=CARTESIAN_POINT('Ctrl Pts',(-7.51676407774749,35.9749999998662,
10.3459381770588));
#277733=CARTESIAN_POINT('Ctrl Pts',(-3.75838203887376,36.1249999998656,
11.5671105274568));
#277734=CARTESIAN_POINT('Ctrl Pts',(-3.10193385748064E-14,36.274999999865,
12.7882828778549));
#277735=CARTESIAN_POINT('Ctrl Pts',(3.7583820388737,36.4249999998644,11.5671105274568));
#277736=CARTESIAN_POINT('Ctrl Pts',(7.51676407774742,36.5749999998638,10.3459381770588));
#277737=CARTESIAN_POINT('Ctrl Pts',(9.83957192047851,36.7249999998632,7.14886745759505));
#277738=CARTESIAN_POINT('Ctrl Pts',(12.1623797632096,36.8749999998626,3.95179673813132));
#277739=CARTESIAN_POINT('Ctrl Pts',(12.1623797632096,37.024999999862,-1.48946194470292E-15));
#277740=CARTESIAN_POINT('Ctrl Pts',(12.1623797632096,37.1749999998614,-3.95179673813132));
#277741=CARTESIAN_POINT('Ctrl Pts',(9.83957192047851,37.3249999998608,-7.14886745759505));
#277742=CARTESIAN_POINT('Ctrl Pts',(7.51676407774742,37.4749999998602,-10.3459381770588));
#277743=CARTESIAN_POINT('Ctrl Pts',(3.75838203887369,37.6249999998596,-11.5671105274568));
#277744=CARTESIAN_POINT('Ctrl Pts',(-3.50154191492285E-14,37.774999999859,
-12.7882828778549));
#277745=CARTESIAN_POINT('Ctrl Pts',(-3.75838203887376,37.9249999998584,
-11.5671105274568));
#277746=CARTESIAN_POINT('Ctrl Pts',(-7.51676407774749,38.0749999998578,
-10.3459381770588));
#277747=CARTESIAN_POINT('Ctrl Pts',(-9.83957192047858,38.2249999998572,
-7.14886745759505));
#277748=CARTESIAN_POINT('Ctrl Pts',(-12.1623797632097,38.3749999998566,
-3.95179673813132));
#277749=CARTESIAN_POINT('Ctrl Pts',(-12.1623797632097,38.524999999856,2.97892388940585E-15));
#277750=CARTESIAN_POINT('Ctrl Pts',(-12.1623797632097,38.6749999998554,
3.95179673813133));
#277751=CARTESIAN_POINT('Ctrl Pts',(-9.83957192047858,38.8249999998548,
7.14886745759505));
#277752=CARTESIAN_POINT('Ctrl Pts',(-7.51676407774749,38.9749999998542,
10.3459381770588));
#277753=CARTESIAN_POINT('Ctrl Pts',(-3.75838203887376,39.1249999998536,
11.5671105274568));
#277754=CARTESIAN_POINT('Ctrl Pts',(-3.27470478464682E-14,39.274999999853,
12.7882828778549));
#277755=CARTESIAN_POINT('Ctrl Pts',(3.7583820388737,39.4249999998524,11.5671105274568));
#277756=CARTESIAN_POINT('Ctrl Pts',(7.51676407774742,39.5749999998518,10.3459381770588));
#277757=CARTESIAN_POINT('Ctrl Pts',(9.83957192047851,39.7249999998512,7.14886745759505));
#277758=CARTESIAN_POINT('Ctrl Pts',(12.1623797632096,39.8749999998506,3.95179673813132));
#277759=CARTESIAN_POINT('Ctrl Pts',(12.1623797632096,40.02499999985,-1.48946194470292E-15));
#277760=CARTESIAN_POINT('Ctrl Pts',(12.1623797632096,40.1749999998494,-3.95179673813132));
#277761=CARTESIAN_POINT('Ctrl Pts',(9.83957192047851,40.3249999998488,-7.14886745759505));
#277762=CARTESIAN_POINT('Ctrl Pts',(7.51676407774742,40.4749999998482,-10.3459381770588));
#277763=CARTESIAN_POINT('Ctrl Pts',(3.75838203887369,40.6249999998476,-11.5671105274568));
#277764=CARTESIAN_POINT('Ctrl Pts',(-3.67431284208903E-14,40.774999999847,
-12.7882828778549));
#277765=CARTESIAN_POINT('Ctrl Pts',(-3.75838203887376,40.9249999998464,
-11.5671105274568));
#277766=CARTESIAN_POINT('Ctrl Pts',(-7.51676407774749,41.0749999998458,
-10.3459381770588));
#277767=CARTESIAN_POINT('Ctrl Pts',(-9.83957192047858,41.2249999998452,
-7.14886745759505));
#277768=CARTESIAN_POINT('Ctrl Pts',(-12.1623797632097,41.3749999998446,
-3.95179673813132));
#277769=CARTESIAN_POINT('Ctrl Pts',(-12.1623797632097,41.524999999844,2.97892388940585E-15));
#277770=CARTESIAN_POINT('Ctrl Pts',(-12.1623797632097,41.6749999998434,
3.95179673813133));
#277771=CARTESIAN_POINT('Ctrl Pts',(-9.83957192047858,41.8249999998428,
7.14886745759505));
#277772=CARTESIAN_POINT('Ctrl Pts',(-7.51676407774749,41.9749999998422,
10.3459381770588));
#277773=CARTESIAN_POINT('Ctrl Pts',(-3.75838203887376,42.1249999998416,
11.5671105274568));
#277774=CARTESIAN_POINT('Ctrl Pts',(-3.44747571181301E-14,42.274999999841,
12.7882828778549));
#277775=CARTESIAN_POINT('Ctrl Pts',(3.75838203887369,42.4249999998404,11.5671105274568));
#277776=CARTESIAN_POINT('Ctrl Pts',(7.51676407774742,42.5749999998398,10.3459381770588));
#277777=CARTESIAN_POINT('Ctrl Pts',(9.83957192047851,42.7249999998392,7.14886745759505));
#277778=CARTESIAN_POINT('Ctrl Pts',(12.1623797632096,42.8749999998386,3.95179673813132));
#277779=CARTESIAN_POINT('Ctrl Pts',(12.1623797632096,43.024999999838,-1.48946194470292E-15));
#277780=CARTESIAN_POINT('Ctrl Pts',(12.1623797632096,43.1749999998374,-3.95179673813132));
#277781=CARTESIAN_POINT('Ctrl Pts',(9.83957192047851,43.3249999998368,-7.14886745759505));
#277782=CARTESIAN_POINT('Ctrl Pts',(7.51676407774742,43.4749999998362,-10.3459381770588));
#277783=CARTESIAN_POINT('Ctrl Pts',(3.75838203887369,43.6249999998356,-11.5671105274568));
#277784=CARTESIAN_POINT('Ctrl Pts',(-3.84708376925522E-14,43.774999999835,
-12.7882828778549));
#277785=CARTESIAN_POINT('Ctrl Pts',(-3.75838203887377,43.9249999998344,
-11.5671105274568));
#277786=CARTESIAN_POINT('Ctrl Pts',(-7.51676407774749,44.0749999998338,
-10.3459381770588));
#277787=CARTESIAN_POINT('Ctrl Pts',(-9.83957192047859,44.2249999998332,
-7.14886745759505));
#277788=CARTESIAN_POINT('Ctrl Pts',(-12.1623797632097,44.3749999998326,
-3.95179673813132));
#277789=CARTESIAN_POINT('Ctrl Pts',(-12.1623797632097,44.524999999832,2.97892388940585E-15));
#277790=CARTESIAN_POINT('Ctrl Pts',(-12.1623797632097,44.6749999998314,
3.95179673813133));
#277791=CARTESIAN_POINT('Ctrl Pts',(-9.83957192047859,44.8249999998308,
7.14886745759505));
#277792=CARTESIAN_POINT('Ctrl Pts',(-7.51676407774749,44.9749999998302,
10.3459381770588));
#277793=CARTESIAN_POINT('Ctrl Pts',(-3.75838203887376,45.1249999998296,
11.5671105274568));
#277794=CARTESIAN_POINT('Ctrl Pts',(-3.62024663897919E-14,45.274999999829,
12.7882828778549));
#277795=CARTESIAN_POINT('Ctrl Pts',(3.75838203887369,45.4249999998284,11.5671105274568));
#277796=CARTESIAN_POINT('Ctrl Pts',(7.51676407774742,45.5749999998278,10.3459381770588));
#277797=CARTESIAN_POINT('Ctrl Pts',(9.83957192047851,45.7249999998272,7.14886745759505));
#277798=CARTESIAN_POINT('Ctrl Pts',(12.1623797632096,45.8749999998266,3.95179673813132));
#277799=CARTESIAN_POINT('Ctrl Pts',(12.1623797632096,46.024999999826,-1.48946194470292E-15));
#277800=CARTESIAN_POINT('Ctrl Pts',(12.1623797632096,46.1749999998254,-3.95179673813132));
#277801=CARTESIAN_POINT('Ctrl Pts',(9.83957192047851,46.3249999998248,-7.14886745759505));
#277802=CARTESIAN_POINT('Ctrl Pts',(7.51676407774742,46.4749999998242,-10.3459381770588));
#277803=CARTESIAN_POINT('Ctrl Pts',(3.75838203887369,46.6249999998236,-11.5671105274568));
#277804=CARTESIAN_POINT('Ctrl Pts',(-4.0198546964214E-14,46.774999999823,
-12.7882828778549));
#277805=CARTESIAN_POINT('Ctrl Pts',(-3.75838203887377,46.9249999998224,
-11.5671105274568));
#277806=CARTESIAN_POINT('Ctrl Pts',(-7.5167640777475,47.0749999998218,-10.3459381770588));
#277807=CARTESIAN_POINT('Ctrl Pts',(-9.83957192047859,47.2249999998212,
-7.14886745759505));
#277808=CARTESIAN_POINT('Ctrl Pts',(-12.1623797632097,47.3749999998206,
-3.95179673813132));
#277809=CARTESIAN_POINT('Ctrl Pts',(-12.1623797632097,47.52499999982,2.97892388940585E-15));
#277810=CARTESIAN_POINT('Ctrl Pts',(-12.1623797632097,47.6749999998194,
3.95179673813133));
#277811=CARTESIAN_POINT('Ctrl Pts',(-9.83957192047859,47.8249999998188,
7.14886745759505));
#277812=CARTESIAN_POINT('Ctrl Pts',(-7.51676407774749,47.9749999998182,
10.3459381770588));
#277813=CARTESIAN_POINT('Ctrl Pts',(-3.75838203887377,48.1249999998176,
11.5671105274568));
#277814=CARTESIAN_POINT('Ctrl Pts',(-3.79301756614538E-14,48.274999999817,
12.7882828778549));
#277815=CARTESIAN_POINT('Ctrl Pts',(3.75838203887369,48.4249999998164,11.5671105274568));
#277816=CARTESIAN_POINT('Ctrl Pts',(7.51676407774742,48.5749999998158,10.3459381770588));
#277817=CARTESIAN_POINT('Ctrl Pts',(9.83957192047851,48.7249999998152,7.14886745759505));
#277818=CARTESIAN_POINT('Ctrl Pts',(12.1623797632096,48.8749999998146,3.95179673813132));
#277819=CARTESIAN_POINT('Ctrl Pts',(12.1623797632096,49.024999999814,-1.48946194470292E-15));
#277820=CARTESIAN_POINT('Ctrl Pts',(12.1623797632096,49.1749999998134,-3.95179673813132));
#277821=CARTESIAN_POINT('Ctrl Pts',(9.83957192047851,49.3249999998128,-7.14886745759505));
#277822=CARTESIAN_POINT('Ctrl Pts',(7.51676407774741,49.4749999998122,-10.3459381770588));
#277823=CARTESIAN_POINT('Ctrl Pts',(3.75838203887369,49.6249999998116,-11.5671105274568));
#277824=CARTESIAN_POINT('Ctrl Pts',(-4.19262562358759E-14,49.774999999811,
-12.7882828778549));
#277825=CARTESIAN_POINT('Ctrl Pts',(-3.75838203887377,49.9249999998104,
-11.5671105274568));
#277826=CARTESIAN_POINT('Ctrl Pts',(-7.5167640777475,50.0749999998098,-10.3459381770588));
#277827=CARTESIAN_POINT('Ctrl Pts',(-9.83957192047859,50.2249999998092,
-7.14886745759505));
#277828=CARTESIAN_POINT('Ctrl Pts',(-12.1623797632097,50.3749999998086,
-3.95179673813132));
#277829=CARTESIAN_POINT('Ctrl Pts',(-12.1623797632097,50.524999999808,2.97892388940585E-15));
#277830=CARTESIAN_POINT('Ctrl Pts',(-12.1623797632097,50.6749999998074,
3.95179673813133));
#277831=CARTESIAN_POINT('Ctrl Pts',(-9.83957192047859,50.8249999998068,
7.14886745759505));
#277832=CARTESIAN_POINT('Ctrl Pts',(-7.51676407774749,50.9749999998062,
10.3459381770588));
#277833=CARTESIAN_POINT('Ctrl Pts',(-3.75838203887377,51.1249999998056,
11.5671105274568));
#277834=CARTESIAN_POINT('Ctrl Pts',(-3.96578849331156E-14,51.274999999805,
12.7882828778549));
#277835=CARTESIAN_POINT('Ctrl Pts',(3.75838203887369,51.4249999998044,11.5671105274568));
#277836=CARTESIAN_POINT('Ctrl Pts',(7.51676407774742,51.5749999998038,10.3459381770588));
#277837=CARTESIAN_POINT('Ctrl Pts',(9.83957192047851,51.7249999998032,7.14886745759505));
#277838=CARTESIAN_POINT('Ctrl Pts',(12.1623797632096,51.8749999998026,3.95179673813132));
#277839=CARTESIAN_POINT('Ctrl Pts',(12.1623797632096,52.024999999802,-1.48946194470292E-15));
#277840=CARTESIAN_POINT('Ctrl Pts',(12.1623797632096,52.1749999998014,-3.95179673813132));
#277841=CARTESIAN_POINT('Ctrl Pts',(9.8395719204785,52.3249999998008,-7.14886745759505));
#277842=CARTESIAN_POINT('Ctrl Pts',(7.51676407774741,52.4749999998002,-10.3459381770588));
#277843=CARTESIAN_POINT('Ctrl Pts',(3.75838203887368,52.6249999997996,-11.5671105274568));
#277844=CARTESIAN_POINT('Ctrl Pts',(-4.36539655075377E-14,52.774999999799,
-12.7882828778549));
#277845=CARTESIAN_POINT('Ctrl Pts',(-3.75838203887377,52.9249999997984,
-11.5671105274568));
#277846=CARTESIAN_POINT('Ctrl Pts',(-7.5167640777475,53.0749999997978,-10.3459381770588));
#277847=CARTESIAN_POINT('Ctrl Pts',(-9.83957192047859,53.2249999997972,
-7.14886745759505));
#277848=CARTESIAN_POINT('Ctrl Pts',(-12.1623797632097,53.3749999997966,
-3.95179673813132));
#277849=CARTESIAN_POINT('Ctrl Pts',(-12.1623797632097,53.524999999796,2.97892388940585E-15));
#277850=CARTESIAN_POINT('Ctrl Pts',(-12.1623797632097,53.6749999997954,
3.95179673813133));
#277851=CARTESIAN_POINT('Ctrl Pts',(-9.83957192047859,53.8249999997948,
7.14886745759505));
#277852=CARTESIAN_POINT('Ctrl Pts',(-7.5167640777475,53.9749999997942,10.3459381770588));
#277853=CARTESIAN_POINT('Ctrl Pts',(-3.75838203887377,54.1249999997936,
11.5671105274568));
#277854=CARTESIAN_POINT('Ctrl Pts',(-4.13855942047774E-14,54.274999999793,
12.7882828778549));
#277855=CARTESIAN_POINT('Ctrl Pts',(3.75838203887369,54.4249999997924,11.5671105274568));
#277856=CARTESIAN_POINT('Ctrl Pts',(7.51676407774741,54.5749999997918,10.3459381770588));
#277857=CARTESIAN_POINT('Ctrl Pts',(9.8395719204785,54.7249999997912,7.14886745759505));
#277858=CARTESIAN_POINT('Ctrl Pts',(12.1623797632096,54.8749999997906,3.95179673813132));
#277859=CARTESIAN_POINT('Ctrl Pts',(12.1623797632096,55.02499999979,-1.48946194470292E-15));
#277860=CARTESIAN_POINT('Ctrl Pts',(12.1623797632096,55.1749999997894,-3.95179673813132));
#277861=CARTESIAN_POINT('Ctrl Pts',(9.8395719204785,55.3249999997888,-7.14886745759505));
#277862=CARTESIAN_POINT('Ctrl Pts',(7.51676407774741,55.4749999997882,-10.3459381770588));
#277863=CARTESIAN_POINT('Ctrl Pts',(3.75838203887368,55.6249999997876,-11.5671105274568));
#277864=CARTESIAN_POINT('Ctrl Pts',(-4.53816747791995E-14,55.774999999787,
-12.7882828778549));
#277865=CARTESIAN_POINT('Ctrl Pts',(-3.75838203887377,55.9249999997864,
-11.5671105274568));
#277866=CARTESIAN_POINT('Ctrl Pts',(-7.5167640777475,56.0749999997858,-10.3459381770588));
#277867=CARTESIAN_POINT('Ctrl Pts',(-9.83957192047859,56.2249999997852,
-7.14886745759505));
#277868=CARTESIAN_POINT('Ctrl Pts',(-12.1623797632097,56.3749999997846,
-3.95179673813132));
#277869=CARTESIAN_POINT('Ctrl Pts',(-12.1623797632097,56.524999999784,2.97892388940585E-15));
#277870=CARTESIAN_POINT('Ctrl Pts',(-12.1623797632097,56.6749999997834,
3.95179673813133));
#277871=CARTESIAN_POINT('Ctrl Pts',(-9.83957192047859,56.8249999997828,
7.14886745759505));
#277872=CARTESIAN_POINT('Ctrl Pts',(-7.5167640777475,56.9749999997822,10.3459381770588));
#277873=CARTESIAN_POINT('Ctrl Pts',(-3.75838203887377,57.1249999997816,
11.5671105274568));
#277874=CARTESIAN_POINT('Ctrl Pts',(-4.31133034764393E-14,57.274999999781,
12.7882828778549));
#277875=CARTESIAN_POINT('Ctrl Pts',(3.75838203887368,57.4249999997804,11.5671105274568));
#277876=CARTESIAN_POINT('Ctrl Pts',(7.51676407774741,57.5749999997798,10.3459381770588));
#277877=CARTESIAN_POINT('Ctrl Pts',(9.8395719204785,57.7249999997792,7.14886745759505));
#277878=CARTESIAN_POINT('Ctrl Pts',(12.1623797632096,57.8749999997786,3.95179673813132));
#277879=CARTESIAN_POINT('Ctrl Pts',(12.1623797632096,58.024999999778,-1.48946194470292E-15));
#277880=CARTESIAN_POINT('Ctrl Pts',(12.1623797632096,58.1749999997774,-3.95179673813132));
#277881=CARTESIAN_POINT('Ctrl Pts',(9.8395719204785,58.3249999997768,-7.14886745759505));
#277882=CARTESIAN_POINT('Ctrl Pts',(7.51676407774741,58.4749999997762,-10.3459381770588));
#277883=CARTESIAN_POINT('Ctrl Pts',(3.75838203887368,58.6249999997756,-11.5671105274568));
#277884=CARTESIAN_POINT('Ctrl Pts',(-4.71093840508614E-14,58.774999999775,
-12.7882828778549));
#277885=CARTESIAN_POINT('Ctrl Pts',(-3.75838203887377,58.9249999997744,
-11.5671105274568));
#277886=CARTESIAN_POINT('Ctrl Pts',(-7.5167640777475,59.0749999997738,-10.3459381770588));
#277887=CARTESIAN_POINT('Ctrl Pts',(-9.83957192047859,59.2249999997732,
-7.14886745759505));
#277888=CARTESIAN_POINT('Ctrl Pts',(-12.1623797632097,59.3749999997726,
-3.95179673813132));
#277889=CARTESIAN_POINT('Ctrl Pts',(-12.1623797632097,59.524999999772,2.97892388940585E-15));
#277890=CARTESIAN_POINT('Ctrl Pts',(-12.1623797632097,59.6749999997714,
3.95179673813133));
#277891=CARTESIAN_POINT('Ctrl Pts',(-9.83957192047859,59.8249999997708,
7.14886745759505));
#277892=CARTESIAN_POINT('Ctrl Pts',(-7.5167640777475,59.9749999997702,10.3459381770588));
#277893=CARTESIAN_POINT('Ctrl Pts',(-3.75838203887377,60.1249999997696,
11.5671105274568));
#277894=CARTESIAN_POINT('Ctrl Pts',(-4.48410127481011E-14,60.274999999769,
12.7882828778549));
#277895=CARTESIAN_POINT('Ctrl Pts',(3.75838203887368,60.4249999997684,11.5671105274568));
#277896=CARTESIAN_POINT('Ctrl Pts',(7.51676407774741,60.5749999997678,10.3459381770588));
#277897=CARTESIAN_POINT('Ctrl Pts',(9.8395719204785,60.7249999997672,7.14886745759505));
#277898=CARTESIAN_POINT('Ctrl Pts',(12.1623797632096,60.8749999997666,3.95179673813132));
#277899=CARTESIAN_POINT('Ctrl Pts',(12.1623797632096,61.024999999766,-1.48946194470292E-15));
#277900=CARTESIAN_POINT('Ctrl Pts',(12.1623797632096,61.1749999997654,-3.95179673813132));
#277901=CARTESIAN_POINT('Ctrl Pts',(9.8395719204785,61.3249999997648,-7.14886745759505));
#277902=CARTESIAN_POINT('Ctrl Pts',(7.51676407774741,61.4749999997642,-10.3459381770588));
#277903=CARTESIAN_POINT('Ctrl Pts',(3.75838203887368,61.6249999997636,-11.5671105274568));
#277904=CARTESIAN_POINT('Ctrl Pts',(-4.88370933225232E-14,61.774999999763,
-12.7882828778549));
#277905=CARTESIAN_POINT('Ctrl Pts',(-3.75838203887378,61.9249999997624,
-11.5671105274568));
#277906=CARTESIAN_POINT('Ctrl Pts',(-7.5167640777475,62.0749999997618,-10.3459381770588));
#277907=CARTESIAN_POINT('Ctrl Pts',(-9.8395719204786,62.2249999997612,-7.14886745759505));
#277908=CARTESIAN_POINT('Ctrl Pts',(-12.1623797632097,62.3749999997606,
-3.95179673813132));
#277909=CARTESIAN_POINT('Ctrl Pts',(-12.1623797632097,62.52499999976,2.97892388940585E-15));
#277910=CARTESIAN_POINT('Ctrl Pts',(-12.1623797632097,62.6749999997594,
3.95179673813133));
#277911=CARTESIAN_POINT('Ctrl Pts',(-9.8395719204786,62.8249999997588,7.14886745759505));
#277912=CARTESIAN_POINT('Ctrl Pts',(-7.5167640777475,62.9749999997582,10.3459381770588));
#277913=CARTESIAN_POINT('Ctrl Pts',(-3.75838203887377,63.1249999997576,
11.5671105274568));
#277914=CARTESIAN_POINT('Ctrl Pts',(-4.6568722019763E-14,63.274999999757,
12.7882828778549));
#277915=CARTESIAN_POINT('Ctrl Pts',(3.75838203887368,63.4249999997564,11.5671105274568));
#277916=CARTESIAN_POINT('Ctrl Pts',(7.51676407774741,63.5749999997558,10.3459381770588));
#277917=CARTESIAN_POINT('Ctrl Pts',(9.8395719204785,63.7249999997552,7.14886745759505));
#277918=CARTESIAN_POINT('Ctrl Pts',(12.1623797632096,63.8749999997546,3.95179673813132));
#277919=CARTESIAN_POINT('Ctrl Pts',(12.1623797632096,64.024999999754,-1.48946194470292E-15));
#277920=CARTESIAN_POINT('Ctrl Pts',(12.1623797632096,64.1749999997534,-3.95179673813132));
#277921=CARTESIAN_POINT('Ctrl Pts',(9.8395719204785,64.3249999997528,-7.14886745759505));
#277922=CARTESIAN_POINT('Ctrl Pts',(7.5167640777474,64.4749999997522,-10.3459381770588));
#277923=CARTESIAN_POINT('Ctrl Pts',(3.75838203887368,64.6249999997516,-11.5671105274568));
#277924=CARTESIAN_POINT('Ctrl Pts',(-5.05648025941851E-14,64.774999999751,
-12.7882828778549));
#277925=CARTESIAN_POINT('Ctrl Pts',(-3.75838203887378,64.9249999997504,
-11.5671105274568));
#277926=CARTESIAN_POINT('Ctrl Pts',(-7.51676407774751,65.0749999997498,
-10.3459381770588));
#277927=CARTESIAN_POINT('Ctrl Pts',(-9.8395719204786,65.2249999997492,-7.14886745759505));
#277928=CARTESIAN_POINT('Ctrl Pts',(-12.1623797632097,65.3749999997486,
-3.95179673813132));
#277929=CARTESIAN_POINT('Ctrl Pts',(-12.1623797632097,65.524999999748,2.97892388940585E-15));
#277930=CARTESIAN_POINT('Ctrl Pts',(-12.1623797632097,65.6749999997474,
3.95179673813133));
#277931=CARTESIAN_POINT('Ctrl Pts',(-9.8395719204786,65.8249999997468,7.14886745759505));
#277932=CARTESIAN_POINT('Ctrl Pts',(-7.5167640777475,65.9749999997462,10.3459381770588));
#277933=CARTESIAN_POINT('Ctrl Pts',(-3.75838203887378,66.1249999997456,
11.5671105274568));
#277934=CARTESIAN_POINT('Ctrl Pts',(-4.82964312914248E-14,66.274999999745,
12.7882828778549));
#277935=CARTESIAN_POINT('Ctrl Pts',(3.75838203887368,66.4249999997444,11.5671105274568));
#277936=CARTESIAN_POINT('Ctrl Pts',(7.51676407774741,66.5749999997438,10.3459381770588));
#277937=CARTESIAN_POINT('Ctrl Pts',(9.8395719204785,66.7249999997432,7.14886745759505));
#277938=CARTESIAN_POINT('Ctrl Pts',(12.1623797632096,66.8749999997426,3.95179673813132));
#277939=CARTESIAN_POINT('Ctrl Pts',(12.1623797632096,67.024999999742,-1.48946194470292E-15));
#277940=CARTESIAN_POINT('Ctrl Pts',(12.1623797632096,67.1749999997414,-3.95179673813132));
#277941=CARTESIAN_POINT('Ctrl Pts',(9.8395719204785,67.3249999997408,-7.14886745759505));
#277942=CARTESIAN_POINT('Ctrl Pts',(7.5167640777474,67.4749999997402,-10.3459381770588));
#277943=CARTESIAN_POINT('Ctrl Pts',(3.75838203887368,67.6249999997396,-11.5671105274568));
#277944=CARTESIAN_POINT('Ctrl Pts',(-5.22925118658469E-14,67.774999999739,
-12.7882828778549));
#277945=CARTESIAN_POINT('Ctrl Pts',(-3.75838203887378,67.9249999997384,
-11.5671105274568));
#277946=CARTESIAN_POINT('Ctrl Pts',(-7.51676407774751,68.0749999997378,
-10.3459381770588));
#277947=CARTESIAN_POINT('Ctrl Pts',(-9.8395719204786,68.2249999997372,-7.14886745759505));
#277948=CARTESIAN_POINT('Ctrl Pts',(-12.1623797632097,68.3749999997366,
-3.95179673813132));
#277949=CARTESIAN_POINT('Ctrl Pts',(-12.1623797632097,68.524999999736,2.97892388940585E-15));
#277950=CARTESIAN_POINT('Ctrl Pts',(-12.1623797632097,68.6749999997354,
3.95179673813133));
#277951=CARTESIAN_POINT('Ctrl Pts',(-9.8395719204786,68.8249999997348,7.14886745759505));
#277952=CARTESIAN_POINT('Ctrl Pts',(-7.51676407774751,68.9749999997342,
10.3459381770588));
#277953=CARTESIAN_POINT('Ctrl Pts',(-3.75838203887378,69.1249999997336,
11.5671105274568));
#277954=CARTESIAN_POINT('Ctrl Pts',(-5.00241405630866E-14,69.274999999733,
12.7882828778549));
#277955=CARTESIAN_POINT('Ctrl Pts',(3.75838203887368,69.4249999997324,11.5671105274568));
#277956=CARTESIAN_POINT('Ctrl Pts',(7.5167640777474,69.5749999997318,10.3459381770588));
#277957=CARTESIAN_POINT('Ctrl Pts',(9.8395719204785,69.7249999997312,7.14886745759505));
#277958=CARTESIAN_POINT('Ctrl Pts',(12.1623797632096,69.8749999997306,3.95179673813132));
#277959=CARTESIAN_POINT('Ctrl Pts',(12.1623797632096,70.02499999973,-1.48946194470292E-15));
#277960=CARTESIAN_POINT('Ctrl Pts',(12.1623797632096,70.1749999997294,-3.95179673813132));
#277961=CARTESIAN_POINT('Ctrl Pts',(9.83957192047849,70.3249999997288,-7.14886745759505));
#277962=CARTESIAN_POINT('Ctrl Pts',(7.5167640777474,70.4749999997282,-10.3459381770588));
#277963=CARTESIAN_POINT('Ctrl Pts',(3.75838203887367,70.6249999997276,-11.5671105274568));
#277964=CARTESIAN_POINT('Ctrl Pts',(-5.40202211375087E-14,70.774999999727,
-12.7882828778549));
#277965=CARTESIAN_POINT('Ctrl Pts',(-3.75838203887378,70.9249999997264,
-11.5671105274568));
#277966=CARTESIAN_POINT('Ctrl Pts',(-7.51676407774751,71.0749999997258,
-10.3459381770588));
#277967=CARTESIAN_POINT('Ctrl Pts',(-9.8395719204786,71.2249999997252,-7.14886745759505));
#277968=CARTESIAN_POINT('Ctrl Pts',(-12.1623797632097,71.3749999997246,
-3.95179673813132));
#277969=CARTESIAN_POINT('Ctrl Pts',(-12.1623797632097,71.524999999724,2.97892388940585E-15));
#277970=CARTESIAN_POINT('Ctrl Pts',(-12.1623797632097,71.6749999997234,
3.95179673813133));
#277971=CARTESIAN_POINT('Ctrl Pts',(-9.8395719204786,71.8249999997228,7.14886745759505));
#277972=CARTESIAN_POINT('Ctrl Pts',(-7.51676407774751,71.9749999997222,
10.3459381770588));
#277973=CARTESIAN_POINT('Ctrl Pts',(-3.75838203887378,72.1249999997216,
11.5671105274568));
#277974=CARTESIAN_POINT('Ctrl Pts',(-5.17518498347485E-14,72.274999999721,
12.7882828778549));
#277975=CARTESIAN_POINT('Ctrl Pts',(3.75838203887368,72.4249999997204,11.5671105274568));
#277976=CARTESIAN_POINT('Ctrl Pts',(7.5167640777474,72.5749999997198,10.3459381770588));
#277977=CARTESIAN_POINT('Ctrl Pts',(9.83957192047849,72.7249999997192,7.14886745759505));
#277978=CARTESIAN_POINT('Ctrl Pts',(12.1623797632096,72.8749999997186,3.95179673813132));
#277979=CARTESIAN_POINT('Ctrl Pts',(12.1623797632096,73.024999999718,-1.48946194470292E-15));
#277980=CARTESIAN_POINT('Ctrl Pts',(12.1623797632096,73.1749999997174,-3.95179673813132));
#277981=CARTESIAN_POINT('Ctrl Pts',(9.83957192047849,73.3249999997168,-7.14886745759505));
#277982=CARTESIAN_POINT('Ctrl Pts',(7.5167640777474,73.4749999997162,-10.3459381770588));
#277983=CARTESIAN_POINT('Ctrl Pts',(3.75838203887367,73.6249999997156,-11.5671105274568));
#277984=CARTESIAN_POINT('Ctrl Pts',(-5.57479304091706E-14,73.774999999715,
-12.7882828778549));
#277985=CARTESIAN_POINT('Ctrl Pts',(-3.75838203887378,73.9249999997144,
-11.5671105274568));
#277986=CARTESIAN_POINT('Ctrl Pts',(-7.51676407774751,74.0749999997138,
-10.3459381770588));
#277987=CARTESIAN_POINT('Ctrl Pts',(-9.8395719204786,74.2249999997132,-7.14886745759505));
#277988=CARTESIAN_POINT('Ctrl Pts',(-12.1623797632097,74.3749999997126,
-3.95179673813132));
#277989=CARTESIAN_POINT('Ctrl Pts',(-12.1623797632097,74.524999999712,2.97892388940585E-15));
#277990=CARTESIAN_POINT('Ctrl Pts',(-12.1623797632097,74.6749999997114,
3.95179673813133));
#277991=CARTESIAN_POINT('Ctrl Pts',(-9.8395719204786,74.8249999997108,7.14886745759505));
#277992=CARTESIAN_POINT('Ctrl Pts',(-7.51676407774751,74.9749999997102,
10.3459381770588));
#277993=CARTESIAN_POINT('Ctrl Pts',(-3.75838203887378,75.1249999997096,
11.5671105274568));
#277994=CARTESIAN_POINT('Ctrl Pts',(-5.34795591064103E-14,75.274999999709,
12.7882828778549));
#277995=CARTESIAN_POINT('Ctrl Pts',(3.75838203887367,75.4249999997084,11.5671105274568));
#277996=CARTESIAN_POINT('Ctrl Pts',(7.5167640777474,75.5749999997078,10.3459381770588));
#277997=CARTESIAN_POINT('Ctrl Pts',(9.83957192047849,75.7249999997072,7.14886745759505));
#277998=CARTESIAN_POINT('Ctrl Pts',(12.1623797632096,75.8749999997066,3.95179673813132));
#277999=CARTESIAN_POINT('Ctrl Pts',(12.1623797632096,76.024999999706,-1.48946194470292E-15));
#278000=CARTESIAN_POINT('Ctrl Pts',(12.1623797632096,76.1749999997054,-3.95179673813132));
#278001=CARTESIAN_POINT('Ctrl Pts',(9.83957192047849,76.3249999997048,-7.14886745759505));
#278002=CARTESIAN_POINT('Ctrl Pts',(7.5167640777474,76.4749999997042,-10.3459381770588));
#278003=CARTESIAN_POINT('Ctrl Pts',(3.75838203887367,76.6249999997036,-11.5671105274568));
#278004=CARTESIAN_POINT('Ctrl Pts',(-5.74756396808324E-14,76.774999999703,
-12.7882828778549));
#278005=CARTESIAN_POINT('Ctrl Pts',(-3.75838203887379,76.9249999997024,
-11.5671105274568));
#278006=CARTESIAN_POINT('Ctrl Pts',(-7.51676407774751,77.0749999997018,
-10.3459381770588));
#278007=CARTESIAN_POINT('Ctrl Pts',(-9.8395719204786,77.2249999997012,-7.14886745759505));
#278008=CARTESIAN_POINT('Ctrl Pts',(-12.1623797632097,77.3749999997006,
-3.95179673813132));
#278009=CARTESIAN_POINT('Ctrl Pts',(-12.1623797632097,77.5249999997,2.97892388940585E-15));
#278010=CARTESIAN_POINT('Ctrl Pts',(-12.1623797632097,77.6749999996994,
3.95179673813133));
#278011=CARTESIAN_POINT('Ctrl Pts',(-9.8395719204786,77.8249999996988,7.14886745759505));
#278012=CARTESIAN_POINT('Ctrl Pts',(-7.51676407774751,77.9749999996982,
10.3459381770588));
#278013=CARTESIAN_POINT('Ctrl Pts',(-3.75838203887378,78.1249999996976,
11.5671105274568));
#278014=CARTESIAN_POINT('Ctrl Pts',(-5.52072683780721E-14,78.274999999697,
12.7882828778549));
#278015=CARTESIAN_POINT('Ctrl Pts',(3.75838203887367,78.4249999996964,11.5671105274568));
#278016=CARTESIAN_POINT('Ctrl Pts',(7.5167640777474,78.5749999996958,10.3459381770588));
#278017=CARTESIAN_POINT('Ctrl Pts',(9.83957192047849,78.7249999996952,7.14886745759505));
#278018=CARTESIAN_POINT('Ctrl Pts',(12.1623797632096,78.8749999996946,3.95179673813132));
#278019=CARTESIAN_POINT('Ctrl Pts',(12.1623797632096,79.024999999694,-1.48946194470292E-15));
#278020=CARTESIAN_POINT('Ctrl Pts',(12.1623797632096,79.1749999996934,-3.95179673813132));
#278021=CARTESIAN_POINT('Ctrl Pts',(9.83957192047849,79.3249999996928,-7.14886745759505));
#278022=CARTESIAN_POINT('Ctrl Pts',(7.5167640777474,79.4749999996922,-10.3459381770588));
#278023=CARTESIAN_POINT('Ctrl Pts',(3.75838203887367,79.6249999996916,-11.5671105274568));
#278024=CARTESIAN_POINT('Ctrl Pts',(-5.92033489524943E-14,79.774999999691,
-12.7882828778549));
#278025=CARTESIAN_POINT('Ctrl Pts',(-3.75838203887379,79.9249999996904,
-11.5671105274568));
#278026=CARTESIAN_POINT('Ctrl Pts',(-7.51676407774751,80.0749999996898,
-10.3459381770588));
#278027=CARTESIAN_POINT('Ctrl Pts',(-9.83957192047861,80.2249999996892,
-7.14886745759505));
#278028=CARTESIAN_POINT('Ctrl Pts',(-12.1623797632097,80.3749999996886,
-3.95179673813132));
#278029=CARTESIAN_POINT('Ctrl Pts',(-12.1623797632097,80.524999999688,2.97892388940585E-15));
#278030=CARTESIAN_POINT('Ctrl Pts',(-12.1623797632097,80.6749999996874,
3.95179673813133));
#278031=CARTESIAN_POINT('Ctrl Pts',(-9.83957192047861,80.8249999996868,
7.14886745759505));
#278032=CARTESIAN_POINT('Ctrl Pts',(-7.51676407774751,80.9749999996862,
10.3459381770588));
#278033=CARTESIAN_POINT('Ctrl Pts',(-3.75838203887378,81.1249999996856,
11.5671105274568));
#278034=CARTESIAN_POINT('Ctrl Pts',(-5.6934977649734E-14,81.274999999685,
12.7882828778549));
#278035=CARTESIAN_POINT('Ctrl Pts',(3.75838203887367,81.4249999996844,11.5671105274568));
#278036=CARTESIAN_POINT('Ctrl Pts',(7.5167640777474,81.5749999996838,10.3459381770588));
#278037=CARTESIAN_POINT('Ctrl Pts',(9.83957192047849,81.7249999996832,7.14886745759505));
#278038=CARTESIAN_POINT('Ctrl Pts',(12.1623797632096,81.8749999996826,3.95179673813132));
#278039=CARTESIAN_POINT('Ctrl Pts',(12.1623797632096,82.024999999682,-1.48946194470292E-15));
#278040=CARTESIAN_POINT('Ctrl Pts',(12.1623797632096,82.1749999996814,-3.95179673813132));
#278041=CARTESIAN_POINT('Ctrl Pts',(9.83957192047849,82.3249999996808,-7.14886745759505));
#278042=CARTESIAN_POINT('Ctrl Pts',(7.5167640777474,82.4749999996802,-10.3459381770588));
#278043=CARTESIAN_POINT('Ctrl Pts',(3.75838203887367,82.6249999996796,-11.5671105274568));
#278044=CARTESIAN_POINT('Ctrl Pts',(-6.09310582241561E-14,82.774999999679,
-12.7882828778549));
#278045=CARTESIAN_POINT('Ctrl Pts',(-3.75838203887379,82.9249999996784,
-11.5671105274568));
#278046=CARTESIAN_POINT('Ctrl Pts',(-7.51676407774752,83.0749999996778,
-10.3459381770588));
#278047=CARTESIAN_POINT('Ctrl Pts',(-9.83957192047861,83.2249999996772,
-7.14886745759505));
#278048=CARTESIAN_POINT('Ctrl Pts',(-12.1623797632097,83.3749999996766,
-3.95179673813132));
#278049=CARTESIAN_POINT('Ctrl Pts',(-12.1623797632097,83.524999999676,2.97892388940585E-15));
#278050=CARTESIAN_POINT('Ctrl Pts',(-12.1623797632097,83.6749999996754,
3.95179673813133));
#278051=CARTESIAN_POINT('Ctrl Pts',(-9.83957192047861,83.8249999996748,
7.14886745759505));
#278052=CARTESIAN_POINT('Ctrl Pts',(-7.51676407774751,83.9749999996742,
10.3459381770588));
#278053=CARTESIAN_POINT('Ctrl Pts',(-3.75838203887379,84.1249999996736,
11.5671105274568));
#278054=CARTESIAN_POINT('Ctrl Pts',(-5.86626869213958E-14,84.274999999673,
12.7882828778549));
#278055=CARTESIAN_POINT('Ctrl Pts',(3.75838203887367,84.4249999996724,11.5671105274568));
#278056=CARTESIAN_POINT('Ctrl Pts',(7.5167640777474,84.5749999996718,10.3459381770588));
#278057=CARTESIAN_POINT('Ctrl Pts',(9.83957192047849,84.7249999996712,7.14886745759505));
#278058=CARTESIAN_POINT('Ctrl Pts',(12.1623797632096,84.8749999996706,3.95179673813132));
#278059=CARTESIAN_POINT('Ctrl Pts',(12.1623797632096,85.02499999967,-1.48946194470292E-15));
#278060=CARTESIAN_POINT('Ctrl Pts',(12.1623797632096,85.1749999996694,-3.95179673813132));
#278061=CARTESIAN_POINT('Ctrl Pts',(9.83957192047849,85.3249999996688,-7.14886745759505));
#278062=CARTESIAN_POINT('Ctrl Pts',(7.51676407774739,85.4749999996682,-10.3459381770588));
#278063=CARTESIAN_POINT('Ctrl Pts',(3.75838203887367,85.6249999996676,-11.5671105274568));
#278064=CARTESIAN_POINT('Ctrl Pts',(-6.26587674958179E-14,85.774999999667,
-12.7882828778549));
#278065=CARTESIAN_POINT('Ctrl Pts',(-3.75838203887379,85.9249999996664,
-11.5671105274568));
#278066=CARTESIAN_POINT('Ctrl Pts',(-7.51676407774752,86.0749999996658,
-10.3459381770588));
#278067=CARTESIAN_POINT('Ctrl Pts',(-9.83957192047861,86.2249999996652,
-7.14886745759505));
#278068=CARTESIAN_POINT('Ctrl Pts',(-12.1623797632097,86.3749999996646,
-3.95179673813132));
#278069=CARTESIAN_POINT('Ctrl Pts',(-12.1623797632097,86.524999999664,2.97892388940585E-15));
#278070=CARTESIAN_POINT('Ctrl Pts',(-12.1623797632097,86.6749999996634,
3.95179673813133));
#278071=CARTESIAN_POINT('Ctrl Pts',(-9.83957192047861,86.8249999996628,
7.14886745759505));
#278072=CARTESIAN_POINT('Ctrl Pts',(-7.51676407774752,86.9749999996622,
10.3459381770588));
#278073=CARTESIAN_POINT('Ctrl Pts',(-3.75838203887379,87.1249999996616,
11.5671105274568));
#278074=CARTESIAN_POINT('Ctrl Pts',(-6.03903961930577E-14,87.274999999661,
12.7882828778549));
#278075=CARTESIAN_POINT('Ctrl Pts',(3.75838203887367,87.4249999996604,11.5671105274568));
#278076=CARTESIAN_POINT('Ctrl Pts',(7.5167640777474,87.5749999996598,10.3459381770588));
#278077=CARTESIAN_POINT('Ctrl Pts',(9.83957192047849,87.7249999996592,7.14886745759505));
#278078=CARTESIAN_POINT('Ctrl Pts',(12.1623797632096,87.8749999996586,3.95179673813132));
#278079=CARTESIAN_POINT('Ctrl Pts',(12.1623797632096,88.024999999658,-1.48946194470292E-15));
#278080=CARTESIAN_POINT('Ctrl Pts',(12.1623797632096,88.1749999996574,-3.95179673813132));
#278081=CARTESIAN_POINT('Ctrl Pts',(9.83957192047849,88.3249999996568,-7.14886745759505));
#278082=CARTESIAN_POINT('Ctrl Pts',(7.51676407774739,88.4749999996562,-10.3459381770588));
#278083=CARTESIAN_POINT('Ctrl Pts',(3.75838203887366,88.6249999996556,-11.5671105274568));
#278084=CARTESIAN_POINT('Ctrl Pts',(-6.43864767674798E-14,88.774999999655,
-12.7882828778549));
#278085=CARTESIAN_POINT('Ctrl Pts',(-3.75838203887379,88.9249999996544,
-11.5671105274568));
#278086=CARTESIAN_POINT('Ctrl Pts',(-7.51676407774752,89.0749999996538,
-10.3459381770588));
#278087=CARTESIAN_POINT('Ctrl Pts',(-9.83957192047861,89.2249999996532,
-7.14886745759505));
#278088=CARTESIAN_POINT('Ctrl Pts',(-12.1623797632097,89.3749999996526,
-3.95179673813132));
#278089=CARTESIAN_POINT('Ctrl Pts',(-12.1623797632097,89.524999999652,2.97892388940585E-15));
#278090=CARTESIAN_POINT('Ctrl Pts',(-12.1623797632097,89.6749999996514,
3.95179673813133));
#278091=CARTESIAN_POINT('Ctrl Pts',(-9.83957192047861,89.8249999996508,
7.14886745759505));
#278092=CARTESIAN_POINT('Ctrl Pts',(-7.51676407774752,89.9749999996502,
10.3459381770588));
#278093=CARTESIAN_POINT('Ctrl Pts',(-3.75838203887379,90.1249999996496,
11.5671105274568));
#278094=CARTESIAN_POINT('Ctrl Pts',(-6.21181054647195E-14,90.274999999649,
12.7882828778549));
#278095=CARTESIAN_POINT('Ctrl Pts',(3.75838203887366,90.4249999996484,11.5671105274568));
#278096=CARTESIAN_POINT('Ctrl Pts',(7.51676407774739,90.5749999996478,10.3459381770588));
#278097=CARTESIAN_POINT('Ctrl Pts',(9.83957192047848,90.7249999996472,7.14886745759505));
#278098=CARTESIAN_POINT('Ctrl Pts',(12.1623797632096,90.8749999996466,3.95179673813132));
#278099=CARTESIAN_POINT('Ctrl Pts',(12.1623797632096,91.024999999646,-1.48946194470292E-15));
#278100=CARTESIAN_POINT('Ctrl Pts',(12.1623797632096,91.1749999996454,-3.95179673813132));
#278101=CARTESIAN_POINT('Ctrl Pts',(9.83957192047848,91.3249999996448,-7.14886745759505));
#278102=CARTESIAN_POINT('Ctrl Pts',(7.51676407774739,91.4749999996442,-10.3459381770588));
#278103=CARTESIAN_POINT('Ctrl Pts',(3.75838203887366,91.6249999996436,-11.5671105274568));
#278104=CARTESIAN_POINT('Ctrl Pts',(-6.61141860391416E-14,91.774999999643,
-12.7882828778549));
#278105=CARTESIAN_POINT('Ctrl Pts',(-3.75838203887379,91.9249999996424,
-11.5671105274568));
#278106=CARTESIAN_POINT('Ctrl Pts',(-7.51676407774752,92.0749999996418,
-10.3459381770588));
#278107=CARTESIAN_POINT('Ctrl Pts',(-9.83957192047861,92.2249999996412,
-7.14886745759505));
#278108=CARTESIAN_POINT('Ctrl Pts',(-12.1623797632097,92.3749999996406,
-3.95179673813132));
#278109=CARTESIAN_POINT('Ctrl Pts',(-12.1623797632097,92.52499999964,2.97892388940585E-15));
#278110=CARTESIAN_POINT('Ctrl Pts',(-12.1623797632097,92.6749999996394,
3.95179673813133));
#278111=CARTESIAN_POINT('Ctrl Pts',(-9.83957192047861,92.8249999996388,
7.14886745759505));
#278112=CARTESIAN_POINT('Ctrl Pts',(-7.51676407774752,92.9749999996382,
10.3459381770588));
#278113=CARTESIAN_POINT('Ctrl Pts',(-3.75838203887379,93.1249999996376,
11.5671105274568));
#278114=CARTESIAN_POINT('Ctrl Pts',(-6.38458147363813E-14,93.274999999637,
12.7882828778549));
#278115=CARTESIAN_POINT('Ctrl Pts',(3.75838203887366,93.4249999996364,11.5671105274568));
#278116=CARTESIAN_POINT('Ctrl Pts',(7.51676407774739,93.5749999996358,10.3459381770588));
#278117=CARTESIAN_POINT('Ctrl Pts',(9.83957192047848,93.7249999996352,7.14886745759505));
#278118=CARTESIAN_POINT('Ctrl Pts',(12.1623797632096,93.8749999996346,3.95179673813132));
#278119=CARTESIAN_POINT('Ctrl Pts',(12.1623797632096,94.024999999634,-1.48946194470292E-15));
#278120=CARTESIAN_POINT('Ctrl Pts',(12.1623797632096,94.1749999996334,-3.95179673813132));
#278121=CARTESIAN_POINT('Ctrl Pts',(9.83957192047848,94.3249999996328,-7.14886745759505));
#278122=CARTESIAN_POINT('Ctrl Pts',(7.51676407774739,94.4749999996322,-10.3459381770588));
#278123=CARTESIAN_POINT('Ctrl Pts',(3.75838203887366,94.6249999996316,-11.5671105274568));
#278124=CARTESIAN_POINT('Ctrl Pts',(-6.78418953108034E-14,94.774999999631,
-12.7882828778549));
#278125=CARTESIAN_POINT('Ctrl Pts',(-3.7583820388738,94.9249999996304,-11.5671105274568));
#278126=CARTESIAN_POINT('Ctrl Pts',(-7.51676407774752,95.0749999996298,
-10.3459381770588));
#278127=CARTESIAN_POINT('Ctrl Pts',(-9.83957192047862,95.2249999996292,
-7.14886745759505));
#278128=CARTESIAN_POINT('Ctrl Pts',(-12.1623797632097,95.3749999996286,
-3.95179673813132));
#278129=CARTESIAN_POINT('Ctrl Pts',(-12.1623797632097,95.524999999628,2.97892388940585E-15));
#278130=CARTESIAN_POINT('Ctrl Pts',(-12.1623797632097,95.6749999996274,
3.95179673813133));
#278131=CARTESIAN_POINT('Ctrl Pts',(-9.83957192047862,95.8249999996268,
7.14886745759505));
#278132=CARTESIAN_POINT('Ctrl Pts',(-7.51676407774752,95.9749999996262,
10.3459381770588));
#278133=CARTESIAN_POINT('Ctrl Pts',(-3.75838203887379,96.1249999996256,
11.5671105274568));
#278134=CARTESIAN_POINT('Ctrl Pts',(-6.55735240080432E-14,96.274999999625,
12.7882828778549));
#278135=CARTESIAN_POINT('Ctrl Pts',(3.75838203887366,96.4249999996244,11.5671105274568));
#278136=CARTESIAN_POINT('Ctrl Pts',(7.51676407774739,96.5749999996238,10.3459381770588));
#278137=CARTESIAN_POINT('Ctrl Pts',(9.83957192047848,96.7249999996232,7.14886745759505));
#278138=CARTESIAN_POINT('Ctrl Pts',(12.1623797632096,96.8749999996226,3.95179673813132));
#278139=CARTESIAN_POINT('Ctrl Pts',(12.1623797632096,97.024999999622,-1.48946194470292E-15));
#278140=CARTESIAN_POINT('Ctrl Pts',(12.1623797632096,97.1749999996214,-3.95179673813132));
#278141=CARTESIAN_POINT('Ctrl Pts',(9.83957192047848,97.3249999996208,-7.14886745759505));
#278142=CARTESIAN_POINT('Ctrl Pts',(7.51676407774739,97.4749999996202,-10.3459381770588));
#278143=CARTESIAN_POINT('Ctrl Pts',(3.75838203887366,97.6249999996196,-11.5671105274568));
#278144=CARTESIAN_POINT('Ctrl Pts',(-6.95696045824653E-14,97.774999999619,
-12.7882828778549));
#278145=CARTESIAN_POINT('Ctrl Pts',(-3.7583820388738,97.9249999996184,-11.5671105274568));
#278146=CARTESIAN_POINT('Ctrl Pts',(-7.51676407774752,98.0749999996178,
-10.3459381770588));
#278147=CARTESIAN_POINT('Ctrl Pts',(-9.83957192047862,98.2249999996172,
-7.14886745759505));
#278148=CARTESIAN_POINT('Ctrl Pts',(-12.1623797632097,98.3749999996166,
-3.95179673813132));
#278149=CARTESIAN_POINT('Ctrl Pts',(-12.1623797632097,98.524999999616,2.97892388940585E-15));
#278150=CARTESIAN_POINT('Ctrl Pts',(-12.1623797632097,98.6749999996154,
3.95179673813133));
#278151=CARTESIAN_POINT('Ctrl Pts',(-9.83957192047862,98.8249999996148,
7.14886745759505));
#278152=CARTESIAN_POINT('Ctrl Pts',(-7.51676407774752,98.9749999996142,
10.3459381770588));
#278153=CARTESIAN_POINT('Ctrl Pts',(-3.7583820388738,99.1249999996136,11.5671105274568));
#278154=CARTESIAN_POINT('Ctrl Pts',(-6.7301233279705E-14,99.274999999613,
12.7882828778549));
#278155=CARTESIAN_POINT('Ctrl Pts',(3.75838203887366,99.4249999996124,11.5671105274568));
#278156=CARTESIAN_POINT('Ctrl Pts',(7.51676407774739,99.5749999996118,10.3459381770588));
#278157=CARTESIAN_POINT('Ctrl Pts',(9.83957192047848,99.7249999996112,7.14886745759505));
#278158=CARTESIAN_POINT('Ctrl Pts',(12.1623797632096,99.8749999996106,3.95179673813132));
#278159=CARTESIAN_POINT('Ctrl Pts',(12.1623797632096,100.02499999961,-1.48946194470292E-15));
#278160=CARTESIAN_POINT('Ctrl Pts',(12.1623797632096,100.174999999609,-3.95179673813132));
#278161=CARTESIAN_POINT('Ctrl Pts',(9.83957192047848,100.324999999609,-7.14886745759505));
#278162=CARTESIAN_POINT('Ctrl Pts',(7.51676407774738,100.474999999608,-10.3459381770588));
#278163=CARTESIAN_POINT('Ctrl Pts',(3.75838203887366,100.624999999608,-11.5671105274568));
#278164=CARTESIAN_POINT('Ctrl Pts',(-7.12973138541271E-14,100.774999999607,
-12.7882828778549));
#278165=CARTESIAN_POINT('Ctrl Pts',(-3.7583820388738,100.924999999606,-11.5671105274568));
#278166=CARTESIAN_POINT('Ctrl Pts',(-7.51676407774753,101.074999999606,
-10.3459381770588));
#278167=CARTESIAN_POINT('Ctrl Pts',(-9.83957192047862,101.224999999605,
-7.14886745759505));
#278168=CARTESIAN_POINT('Ctrl Pts',(-12.1623797632097,101.374999999605,
-3.95179673813132));
#278169=CARTESIAN_POINT('Ctrl Pts',(-12.1623797632097,101.524999999604,
2.97892388940585E-15));
#278170=CARTESIAN_POINT('Ctrl Pts',(-12.1623797632097,101.674999999603,
3.95179673813133));
#278171=CARTESIAN_POINT('Ctrl Pts',(-9.83957192047862,101.824999999603,
7.14886745759505));
#278172=CARTESIAN_POINT('Ctrl Pts',(-7.51676407774752,101.974999999602,
10.3459381770588));
#278173=CARTESIAN_POINT('Ctrl Pts',(-3.7583820388738,102.124999999602,11.5671105274568));
#278174=CARTESIAN_POINT('Ctrl Pts',(-6.90289425513669E-14,102.274999999601,
12.7882828778549));
#278175=CARTESIAN_POINT('Ctrl Pts',(3.75838203887366,102.4249999996,11.5671105274568));
#278176=CARTESIAN_POINT('Ctrl Pts',(7.51676407774739,102.5749999996,10.3459381770588));
#278177=CARTESIAN_POINT('Ctrl Pts',(9.83957192047848,102.724999999599,7.14886745759505));
#278178=CARTESIAN_POINT('Ctrl Pts',(12.1623797632096,102.874999999599,3.95179673813132));
#278179=CARTESIAN_POINT('Ctrl Pts',(12.1623797632096,103.024999999598,-1.48946194470292E-15));
#278180=CARTESIAN_POINT('Ctrl Pts',(12.1623797632096,103.174999999597,-3.95179673813132));
#278181=CARTESIAN_POINT('Ctrl Pts',(9.83957192047848,103.324999999597,-7.14886745759505));
#278182=CARTESIAN_POINT('Ctrl Pts',(7.51676407774738,103.474999999596,-10.3459381770588));
#278183=CARTESIAN_POINT('Ctrl Pts',(3.75838203887366,103.624999999596,-11.5671105274568));
#278184=CARTESIAN_POINT('Ctrl Pts',(-7.3025023125789E-14,103.774999999595,
-12.7882828778549));
#278185=CARTESIAN_POINT('Ctrl Pts',(-3.7583820388738,103.924999999594,-11.5671105274568));
#278186=CARTESIAN_POINT('Ctrl Pts',(-7.51676407774753,104.074999999594,
-10.3459381770588));
#278187=CARTESIAN_POINT('Ctrl Pts',(-9.83957192047862,104.224999999593,
-7.14886745759505));
#278188=CARTESIAN_POINT('Ctrl Pts',(-12.1623797632097,104.374999999593,
-3.95179673813132));
#278189=CARTESIAN_POINT('Ctrl Pts',(-12.1623797632097,104.524999999592,
2.97892388940585E-15));
#278190=CARTESIAN_POINT('Ctrl Pts',(-12.1623797632097,104.674999999591,
3.95179673813133));
#278191=CARTESIAN_POINT('Ctrl Pts',(-9.83957192047862,104.824999999591,
7.14886745759505));
#278192=CARTESIAN_POINT('Ctrl Pts',(-7.51676407774753,104.97499999959,10.3459381770588));
#278193=CARTESIAN_POINT('Ctrl Pts',(-3.7583820388738,105.12499999959,11.5671105274568));
#278194=CARTESIAN_POINT('Ctrl Pts',(-7.07566518230287E-14,105.274999999589,
12.7882828778549));
#278195=CARTESIAN_POINT('Ctrl Pts',(3.75838203887366,105.424999999588,11.5671105274568));
#278196=CARTESIAN_POINT('Ctrl Pts',(7.51676407774738,105.574999999588,10.3459381770588));
#278197=CARTESIAN_POINT('Ctrl Pts',(9.83957192047848,105.724999999587,7.14886745759505));
#278198=CARTESIAN_POINT('Ctrl Pts',(12.1623797632096,105.874999999587,3.95179673813132));
#278199=CARTESIAN_POINT('Ctrl Pts',(12.1623797632096,106.024999999586,-1.48946194470292E-15));
#278200=CARTESIAN_POINT('Ctrl Pts',(12.1623797632096,106.174999999585,-3.95179673813132));
#278201=CARTESIAN_POINT('Ctrl Pts',(9.83957192047848,106.324999999585,-7.14886745759505));
#278202=CARTESIAN_POINT('Ctrl Pts',(7.51676407774738,106.474999999584,-10.3459381770588));
#278203=CARTESIAN_POINT('Ctrl Pts',(3.75838203887365,106.624999999584,-11.5671105274568));
#278204=CARTESIAN_POINT('Ctrl Pts',(-7.47527323974508E-14,106.774999999583,
-12.7882828778549));
#278205=CARTESIAN_POINT('Ctrl Pts',(-3.7583820388738,106.924999999582,-11.5671105274568));
#278206=CARTESIAN_POINT('Ctrl Pts',(-7.51676407774753,107.074999999582,
-10.3459381770588));
#278207=CARTESIAN_POINT('Ctrl Pts',(-9.83957192047862,107.224999999581,
-7.14886745759505));
#278208=CARTESIAN_POINT('Ctrl Pts',(-12.1623797632097,107.374999999581,
-3.95179673813132));
#278209=CARTESIAN_POINT('Ctrl Pts',(-12.1623797632097,107.52499999958,2.97892388940585E-15));
#278210=CARTESIAN_POINT('Ctrl Pts',(-12.1623797632097,107.674999999579,
3.95179673813133));
#278211=CARTESIAN_POINT('Ctrl Pts',(-9.83957192047862,107.824999999579,
7.14886745759505));
#278212=CARTESIAN_POINT('Ctrl Pts',(-7.51676407774753,107.974999999578,
10.3459381770588));
#278213=CARTESIAN_POINT('Ctrl Pts',(-3.7583820388738,108.124999999578,11.5671105274568));
#278214=CARTESIAN_POINT('Ctrl Pts',(-7.24843610946905E-14,108.274999999577,
12.7882828778549));
#278215=CARTESIAN_POINT('Ctrl Pts',(3.75838203887366,108.424999999576,11.5671105274568));
#278216=CARTESIAN_POINT('Ctrl Pts',(7.51676407774738,108.574999999576,10.3459381770588));
#278217=CARTESIAN_POINT('Ctrl Pts',(9.83957192047847,108.724999999575,7.14886745759505));
#278218=CARTESIAN_POINT('Ctrl Pts',(12.1623797632096,108.874999999575,3.95179673813132));
#278219=CARTESIAN_POINT('Ctrl Pts',(12.1623797632096,109.024999999574,-1.48946194470292E-15));
#278220=CARTESIAN_POINT('Ctrl Pts',(12.1623797632096,109.174999999573,-3.95179673813132));
#278221=CARTESIAN_POINT('Ctrl Pts',(9.83957192047847,109.324999999573,-7.14886745759505));
#278222=CARTESIAN_POINT('Ctrl Pts',(7.51676407774738,109.474999999572,-10.3459381770588));
#278223=CARTESIAN_POINT('Ctrl Pts',(3.75838203887365,109.624999999572,-11.5671105274568));
#278224=CARTESIAN_POINT('Ctrl Pts',(-7.64804416691126E-14,109.774999999571,
-12.7882828778549));
#278225=CARTESIAN_POINT('Ctrl Pts',(-3.7583820388738,109.92499999957,-11.5671105274568));
#278226=CARTESIAN_POINT('Ctrl Pts',(-7.51676407774753,110.07499999957,-10.3459381770588));
#278227=CARTESIAN_POINT('Ctrl Pts',(-9.83957192047862,110.224999999569,
-7.14886745759505));
#278228=CARTESIAN_POINT('Ctrl Pts',(-12.1623797632097,110.374999999569,
-3.95179673813132));
#278229=CARTESIAN_POINT('Ctrl Pts',(-12.1623797632097,110.524999999568,
2.97892388940585E-15));
#278230=CARTESIAN_POINT('Ctrl Pts',(-12.1623797632097,110.674999999567,
3.95179673813133));
#278231=CARTESIAN_POINT('Ctrl Pts',(-9.83957192047862,110.824999999567,
7.14886745759505));
#278232=CARTESIAN_POINT('Ctrl Pts',(-7.51676407774753,110.974999999566,
10.3459381770588));
#278233=CARTESIAN_POINT('Ctrl Pts',(-3.7583820388738,111.124999999566,11.5671105274568));
#278234=CARTESIAN_POINT('Ctrl Pts',(-7.42120703663524E-14,111.274999999565,
12.7882828778549));
#278235=CARTESIAN_POINT('Ctrl Pts',(3.75838203887365,111.424999999564,11.5671105274568));
#278236=CARTESIAN_POINT('Ctrl Pts',(7.51676407774738,111.574999999564,10.3459381770588));
#278237=CARTESIAN_POINT('Ctrl Pts',(9.83957192047847,111.724999999563,7.14886745759505));
#278238=CARTESIAN_POINT('Ctrl Pts',(12.1623797632096,111.874999999563,3.95179673813132));
#278239=CARTESIAN_POINT('Ctrl Pts',(12.1623797632096,112.024999999562,-1.48946194470292E-15));
#278240=CARTESIAN_POINT('Ctrl Pts',(12.1623797632096,112.174999999561,-3.95179673813132));
#278241=CARTESIAN_POINT('Ctrl Pts',(9.83957192047847,112.324999999561,-7.14886745759505));
#278242=CARTESIAN_POINT('Ctrl Pts',(7.51676407774738,112.47499999956,-10.3459381770588));
#278243=CARTESIAN_POINT('Ctrl Pts',(3.75838203887365,112.62499999956,-11.5671105274568));
#278244=CARTESIAN_POINT('Ctrl Pts',(-7.82081509407745E-14,112.774999999559,
-12.7882828778549));
#278245=CARTESIAN_POINT('Ctrl Pts',(-3.75838203887381,112.924999999558,
-11.5671105274568));
#278246=CARTESIAN_POINT('Ctrl Pts',(-7.51676407774753,113.074999999558,
-10.3459381770588));
#278247=CARTESIAN_POINT('Ctrl Pts',(-9.83957192047863,113.224999999557,
-7.14886745759505));
#278248=CARTESIAN_POINT('Ctrl Pts',(-12.1623797632097,113.374999999557,
-3.95179673813132));
#278249=CARTESIAN_POINT('Ctrl Pts',(-12.1623797632097,113.524999999556,
2.97892388940585E-15));
#278250=CARTESIAN_POINT('Ctrl Pts',(-12.1623797632097,113.674999999555,
3.95179673813133));
#278251=CARTESIAN_POINT('Ctrl Pts',(-9.83957192047863,113.824999999555,
7.14886745759505));
#278252=CARTESIAN_POINT('Ctrl Pts',(-7.51676407774753,113.974999999554,
10.3459381770588));
#278253=CARTESIAN_POINT('Ctrl Pts',(-3.7583820388738,114.124999999554,11.5671105274568));
#278254=CARTESIAN_POINT('Ctrl Pts',(-7.59397796380142E-14,114.274999999553,
12.7882828778549));
#278255=CARTESIAN_POINT('Ctrl Pts',(3.75838203887365,114.424999999552,11.5671105274568));
#278256=CARTESIAN_POINT('Ctrl Pts',(7.51676407774738,114.574999999552,10.3459381770588));
#278257=CARTESIAN_POINT('Ctrl Pts',(9.83957192047847,114.724999999551,7.14886745759505));
#278258=CARTESIAN_POINT('Ctrl Pts',(12.1623797632096,114.874999999551,3.95179673813132));
#278259=CARTESIAN_POINT('Ctrl Pts',(12.1623797632096,115.02499999955,-1.48946194470292E-15));
#278260=CARTESIAN_POINT('Ctrl Pts',(12.1623797632096,115.174999999549,-3.95179673813132));
#278261=CARTESIAN_POINT('Ctrl Pts',(9.83957192047847,115.324999999549,-7.14886745759505));
#278262=CARTESIAN_POINT('Ctrl Pts',(7.51676407774738,115.474999999548,-10.3459381770588));
#278263=CARTESIAN_POINT('Ctrl Pts',(3.75838203887365,115.624999999548,-11.5671105274568));
#278264=CARTESIAN_POINT('Ctrl Pts',(-7.99358602124363E-14,115.774999999547,
-12.7882828778549));
#278265=CARTESIAN_POINT('Ctrl Pts',(-3.75838203887381,115.924999999546,
-11.5671105274568));
#278266=CARTESIAN_POINT('Ctrl Pts',(-7.51676407774754,116.074999999546,
-10.3459381770588));
#278267=CARTESIAN_POINT('Ctrl Pts',(-9.83957192047863,116.224999999545,
-7.14886745759505));
#278268=CARTESIAN_POINT('Ctrl Pts',(-12.1623797632097,116.374999999545,
-3.95179673813132));
#278269=CARTESIAN_POINT('Ctrl Pts',(-12.1623797632097,116.524999999544,
2.97892388940585E-15));
#278270=CARTESIAN_POINT('Ctrl Pts',(-12.1623797632097,116.674999999543,
3.95179673813133));
#278271=CARTESIAN_POINT('Ctrl Pts',(-9.83957192047863,116.824999999543,
7.14886745759505));
#278272=CARTESIAN_POINT('Ctrl Pts',(-7.51676407774753,116.974999999542,
10.3459381770588));
#278273=CARTESIAN_POINT('Ctrl Pts',(-3.75838203887381,117.124999999542,
11.5671105274568));
#278274=CARTESIAN_POINT('Ctrl Pts',(-7.76674889096761E-14,117.274999999541,
12.7882828778549));
#278275=CARTESIAN_POINT('Ctrl Pts',(3.75838203887365,117.42499999954,11.5671105274568));
#278276=CARTESIAN_POINT('Ctrl Pts',(7.51676407774738,117.57499999954,10.3459381770588));
#278277=CARTESIAN_POINT('Ctrl Pts',(9.83957192047847,117.724999999539,7.14886745759505));
#278278=CARTESIAN_POINT('Ctrl Pts',(12.1623797632096,117.874999999539,3.95179673813132));
#278279=CARTESIAN_POINT('Ctrl Pts',(12.1623797632096,118.024999999538,-1.48946194470292E-15));
#278280=CARTESIAN_POINT('Ctrl Pts',(12.1623797632096,118.174999999537,-3.95179673813132));
#278281=CARTESIAN_POINT('Ctrl Pts',(9.83957192047847,118.324999999537,-7.14886745759505));
#278282=CARTESIAN_POINT('Ctrl Pts',(7.51676407774737,118.474999999536,-10.3459381770588));
#278283=CARTESIAN_POINT('Ctrl Pts',(3.75838203887365,118.624999999536,-11.5671105274568));
#278284=CARTESIAN_POINT('Ctrl Pts',(-8.16635694840981E-14,118.774999999535,
-12.7882828778549));
#278285=CARTESIAN_POINT('Ctrl Pts',(-3.75838203887381,118.924999999534,
-11.5671105274568));
#278286=CARTESIAN_POINT('Ctrl Pts',(-7.51676407774754,119.074999999534,
-10.3459381770588));
#278287=CARTESIAN_POINT('Ctrl Pts',(-9.83957192047863,119.224999999533,
-7.14886745759505));
#278288=CARTESIAN_POINT('Ctrl Pts',(-12.1623797632097,119.374999999533,
-3.95179673813132));
#278289=CARTESIAN_POINT('Ctrl Pts',(-12.1623797632097,119.524999999532,
2.97892388940585E-15));
#278290=CARTESIAN_POINT('Ctrl Pts',(-12.1623797632097,119.674999999531,
3.95179673813133));
#278291=CARTESIAN_POINT('Ctrl Pts',(-9.83957192047863,119.824999999531,
7.14886745759505));
#278292=CARTESIAN_POINT('Ctrl Pts',(-7.51676407774754,119.97499999953,10.3459381770588));
#278293=CARTESIAN_POINT('Ctrl Pts',(-3.75838203887381,120.12499999953,11.5671105274568));
#278294=CARTESIAN_POINT('Ctrl Pts',(-7.93951981813379E-14,120.274999999529,
12.7882828778549));
#278295=CARTESIAN_POINT('Ctrl Pts',(3.75838203887365,120.424999999528,11.5671105274568));
#278296=CARTESIAN_POINT('Ctrl Pts',(7.51676407774738,120.574999999528,10.3459381770588));
#278297=CARTESIAN_POINT('Ctrl Pts',(9.83957192047847,120.724999999527,7.14886745759505));
#278298=CARTESIAN_POINT('Ctrl Pts',(12.1623797632096,120.874999999527,3.95179673813132));
#278299=CARTESIAN_POINT('Ctrl Pts',(12.1623797632096,121.024999999526,-1.48946194470292E-15));
#278300=CARTESIAN_POINT('Ctrl Pts',(12.1623797632096,121.174999999525,-3.95179673813132));
#278301=CARTESIAN_POINT('Ctrl Pts',(9.83957192047847,121.324999999525,-7.14886745759505));
#278302=CARTESIAN_POINT('Ctrl Pts',(7.51676407774737,121.474999999524,-10.3459381770588));
#278303=CARTESIAN_POINT('Ctrl Pts',(3.75838203887364,121.624999999524,-11.5671105274568));
#278304=CARTESIAN_POINT('Ctrl Pts',(-8.339127875576E-14,121.774999999523,
-12.7882828778549));
#278305=CARTESIAN_POINT('Ctrl Pts',(-3.75838203887381,121.924999999522,
-11.5671105274568));
#278306=CARTESIAN_POINT('Ctrl Pts',(-7.51676407774754,122.074999999522,
-10.3459381770588));
#278307=CARTESIAN_POINT('Ctrl Pts',(-9.83957192047863,122.224999999521,
-7.14886745759505));
#278308=CARTESIAN_POINT('Ctrl Pts',(-12.1623797632097,122.374999999521,
-3.95179673813132));
#278309=CARTESIAN_POINT('Ctrl Pts',(-12.1623797632097,122.52499999952,2.97892388940585E-15));
#278310=CARTESIAN_POINT('Ctrl Pts',(-12.1623797632097,122.674999999519,
3.95179673813133));
#278311=CARTESIAN_POINT('Ctrl Pts',(-9.83957192047863,122.824999999519,
7.14886745759505));
#278312=CARTESIAN_POINT('Ctrl Pts',(-7.51676407774754,122.974999999518,
10.3459381770588));
#278313=CARTESIAN_POINT('Ctrl Pts',(-3.75838203887381,123.124999999518,
11.5671105274568));
#278314=CARTESIAN_POINT('Ctrl Pts',(-8.11229074529997E-14,123.274999999517,
12.7882828778549));
#278315=CARTESIAN_POINT('Ctrl Pts',(3.75838203887365,123.424999999516,11.5671105274568));
#278316=CARTESIAN_POINT('Ctrl Pts',(7.51676407774737,123.574999999516,10.3459381770588));
#278317=CARTESIAN_POINT('Ctrl Pts',(9.83957192047846,123.724999999515,7.14886745759505));
#278318=CARTESIAN_POINT('Ctrl Pts',(12.1623797632096,123.874999999515,3.95179673813132));
#278319=CARTESIAN_POINT('Ctrl Pts',(12.1623797632096,124.024999999514,-1.48946194470292E-15));
#278320=CARTESIAN_POINT('Ctrl Pts',(12.1623797632096,124.174999999513,-3.95179673813132));
#278321=CARTESIAN_POINT('Ctrl Pts',(9.83957192047846,124.324999999513,-7.14886745759505));
#278322=CARTESIAN_POINT('Ctrl Pts',(7.51676407774737,124.474999999512,-10.3459381770588));
#278323=CARTESIAN_POINT('Ctrl Pts',(3.75838203887364,124.624999999512,-11.5671105274568));
#278324=CARTESIAN_POINT('Ctrl Pts',(-8.51189880274219E-14,124.774999999511,
-12.7882828778549));
#278325=CARTESIAN_POINT('Ctrl Pts',(-3.75838203887381,124.92499999951,-11.5671105274568));
#278326=CARTESIAN_POINT('Ctrl Pts',(-7.51676407774754,125.07499999951,-10.3459381770588));
#278327=CARTESIAN_POINT('Ctrl Pts',(-9.83957192047863,125.224999999509,
-7.14886745759505));
#278328=CARTESIAN_POINT('Ctrl Pts',(-12.1623797632097,125.374999999509,
-3.95179673813132));
#278329=CARTESIAN_POINT('Ctrl Pts',(-12.1623797632097,125.524999999508,
2.97892388940585E-15));
#278330=CARTESIAN_POINT('Ctrl Pts',(-12.1623797632097,125.674999999507,
3.95179673813133));
#278331=CARTESIAN_POINT('Ctrl Pts',(-9.83957192047863,125.824999999507,
7.14886745759505));
#278332=CARTESIAN_POINT('Ctrl Pts',(-7.51676407774754,125.974999999506,
10.3459381770588));
#278333=CARTESIAN_POINT('Ctrl Pts',(-3.75838203887381,126.124999999506,
11.5671105274568));
#278334=CARTESIAN_POINT('Ctrl Pts',(-8.28506167246616E-14,126.274999999505,
12.7882828778549));
#278335=CARTESIAN_POINT('Ctrl Pts',(3.75838203887364,126.424999999504,11.5671105274568));
#278336=CARTESIAN_POINT('Ctrl Pts',(7.51676407774737,126.574999999504,10.3459381770588));
#278337=CARTESIAN_POINT('Ctrl Pts',(9.83957192047846,126.724999999503,7.14886745759505));
#278338=CARTESIAN_POINT('Ctrl Pts',(12.1623797632096,126.874999999503,3.95179673813132));
#278339=CARTESIAN_POINT('Ctrl Pts',(12.1623797632096,127.024999999502,-1.48946194470292E-15));
#278340=CARTESIAN_POINT('Ctrl Pts',(12.1623797632096,127.174999999501,-3.95179673813132));
#278341=CARTESIAN_POINT('Ctrl Pts',(9.83957192047846,127.324999999501,-7.14886745759505));
#278342=CARTESIAN_POINT('Ctrl Pts',(7.51676407774737,127.4749999995,-10.3459381770588));
#278343=CARTESIAN_POINT('Ctrl Pts',(3.75838203887364,127.6249999995,-11.5671105274568));
#278344=CARTESIAN_POINT('Ctrl Pts',(-8.68466972990837E-14,127.774999999499,
-12.7882828778549));
#278345=CARTESIAN_POINT('Ctrl Pts',(-3.75838203887381,127.924999999498,
-11.5671105274568));
#278346=CARTESIAN_POINT('Ctrl Pts',(-7.51676407774754,128.074999999498,
-10.3459381770588));
#278347=CARTESIAN_POINT('Ctrl Pts',(-9.83957192047864,128.224999999497,
-7.14886745759505));
#278348=CARTESIAN_POINT('Ctrl Pts',(-12.1623797632097,128.374999999497,
-3.95179673813132));
#278349=CARTESIAN_POINT('Ctrl Pts',(-12.1623797632097,128.524999999496,
2.97892388940585E-15));
#278350=CARTESIAN_POINT('Ctrl Pts',(-12.1623797632097,128.674999999495,
3.95179673813133));
#278351=CARTESIAN_POINT('Ctrl Pts',(-9.83957192047864,128.824999999495,
7.14886745759505));
#278352=CARTESIAN_POINT('Ctrl Pts',(-7.51676407774754,128.974999999494,
10.3459381770588));
#278353=CARTESIAN_POINT('Ctrl Pts',(-3.75838203887381,129.124999999494,
11.5671105274568));
#278354=CARTESIAN_POINT('Ctrl Pts',(-8.45783259963234E-14,129.274999999493,
12.7882828778549));
#278355=CARTESIAN_POINT('Ctrl Pts',(3.75838203887364,129.424999999492,11.5671105274568));
#278356=CARTESIAN_POINT('Ctrl Pts',(7.51676407774737,129.574999999492,10.3459381770588));
#278357=CARTESIAN_POINT('Ctrl Pts',(9.83957192047846,129.724999999491,7.14886745759505));
#278358=CARTESIAN_POINT('Ctrl Pts',(12.1623797632096,129.874999999491,3.95179673813132));
#278359=CARTESIAN_POINT('Ctrl Pts',(12.1623797632096,130.02499999949,-1.48946194470292E-15));
#278360=CARTESIAN_POINT('Ctrl Pts',(12.1623797632096,130.174999999489,-3.95179673813132));
#278361=CARTESIAN_POINT('Ctrl Pts',(9.83957192047846,130.324999999489,-7.14886745759505));
#278362=CARTESIAN_POINT('Ctrl Pts',(7.51676407774737,130.474999999488,-10.3459381770588));
#278363=CARTESIAN_POINT('Ctrl Pts',(3.75838203887364,130.624999999488,-11.5671105274568));
#278364=CARTESIAN_POINT('Ctrl Pts',(-8.85744065707455E-14,130.774999999487,
-12.7882828778549));
#278365=CARTESIAN_POINT('Ctrl Pts',(-3.75838203887382,130.924999999486,
-11.5671105274568));
#278366=CARTESIAN_POINT('Ctrl Pts',(-7.51676407774754,131.074999999486,
-10.3459381770588));
#278367=CARTESIAN_POINT('Ctrl Pts',(-9.83957192047864,131.224999999485,
-7.14886745759505));
#278368=CARTESIAN_POINT('Ctrl Pts',(-12.1623797632097,131.374999999485,
-3.95179673813132));
#278369=CARTESIAN_POINT('Ctrl Pts',(-12.1623797632097,131.524999999484,
2.97892388940585E-15));
#278370=CARTESIAN_POINT('Ctrl Pts',(-12.1623797632097,131.674999999483,
3.95179673813133));
#278371=CARTESIAN_POINT('Ctrl Pts',(-9.83957192047864,131.824999999483,
7.14886745759505));
#278372=CARTESIAN_POINT('Ctrl Pts',(-7.51676407774754,131.974999999482,
10.3459381770588));
#278373=CARTESIAN_POINT('Ctrl Pts',(-3.75838203887381,132.124999999482,
11.5671105274568));
#278374=CARTESIAN_POINT('Ctrl Pts',(-8.63060352679853E-14,132.274999999481,
12.7882828778549));
#278375=CARTESIAN_POINT('Ctrl Pts',(3.75838203887364,132.42499999948,11.5671105274568));
#278376=CARTESIAN_POINT('Ctrl Pts',(7.51676407774737,132.57499999948,10.3459381770588));
#278377=CARTESIAN_POINT('Ctrl Pts',(9.83957192047846,132.724999999479,7.14886745759505));
#278378=CARTESIAN_POINT('Ctrl Pts',(12.1623797632096,132.874999999479,3.95179673813132));
#278379=CARTESIAN_POINT('Ctrl Pts',(12.1623797632096,133.024999999478,-1.48946194470292E-15));
#278380=CARTESIAN_POINT('Ctrl Pts',(12.1623797632096,133.174999999477,-3.95179673813132));
#278381=CARTESIAN_POINT('Ctrl Pts',(9.83957192047846,133.324999999477,-7.14886745759505));
#278382=CARTESIAN_POINT('Ctrl Pts',(7.51676407774736,133.474999999476,-10.3459381770588));
#278383=CARTESIAN_POINT('Ctrl Pts',(3.75838203887364,133.624999999476,-11.5671105274568));
#278384=CARTESIAN_POINT('Ctrl Pts',(-9.03021158424074E-14,133.774999999475,
-12.7882828778549));
#278385=CARTESIAN_POINT('Ctrl Pts',(-3.75838203887382,133.924999999474,
-11.5671105274568));
#278386=CARTESIAN_POINT('Ctrl Pts',(-7.51676407774755,134.074999999474,
-10.3459381770588));
#278387=CARTESIAN_POINT('Ctrl Pts',(-9.83957192047864,134.224999999473,
-7.14886745759505));
#278388=CARTESIAN_POINT('Ctrl Pts',(-12.1623797632097,134.374999999473,
-3.95179673813132));
#278389=CARTESIAN_POINT('Ctrl Pts',(-12.1623797632097,134.524999999472,
2.97892388940585E-15));
#278390=CARTESIAN_POINT('Ctrl Pts',(-12.1623797632097,134.674999999471,
3.95179673813133));
#278391=CARTESIAN_POINT('Ctrl Pts',(-9.83957192047864,134.824999999471,
7.14886745759505));
#278392=CARTESIAN_POINT('Ctrl Pts',(-7.51676407774754,134.97499999947,10.3459381770588));
#278393=CARTESIAN_POINT('Ctrl Pts',(-3.75838203887382,135.12499999947,11.5671105274568));
#278394=CARTESIAN_POINT('Ctrl Pts',(-8.80337445396471E-14,135.274999999469,
12.7882828778549));
#278395=CARTESIAN_POINT('Ctrl Pts',(3.75838203887364,135.424999999468,11.5671105274568));
#278396=CARTESIAN_POINT('Ctrl Pts',(7.51676407774737,135.574999999468,10.3459381770588));
#278397=CARTESIAN_POINT('Ctrl Pts',(9.83957192047846,135.724999999467,7.14886745759505));
#278398=CARTESIAN_POINT('Ctrl Pts',(12.1623797632096,135.874999999467,3.95179673813132));
#278399=CARTESIAN_POINT('Ctrl Pts',(12.1623797632096,136.024999999466,-1.48946194470292E-15));
#278400=CARTESIAN_POINT('Ctrl Pts',(12.1623797632095,136.174999999465,-3.95179673813132));
#278401=CARTESIAN_POINT('Ctrl Pts',(9.83957192047846,136.324999999465,-7.14886745759505));
#278402=CARTESIAN_POINT('Ctrl Pts',(7.51676407774736,136.474999999464,-10.3459381770588));
#278403=CARTESIAN_POINT('Ctrl Pts',(3.75838203887364,136.624999999464,-11.5671105274568));
#278404=CARTESIAN_POINT('Ctrl Pts',(-9.20298251140692E-14,136.774999999463,
-12.7882828778549));
#278405=CARTESIAN_POINT('Ctrl Pts',(-3.75838203887382,136.924999999462,
-11.5671105274568));
#278406=CARTESIAN_POINT('Ctrl Pts',(-7.51676407774755,137.074999999462,
-10.3459381770588));
#278407=CARTESIAN_POINT('Ctrl Pts',(-9.83957192047864,137.224999999461,
-7.14886745759505));
#278408=CARTESIAN_POINT('Ctrl Pts',(-12.1623797632097,137.374999999461,
-3.95179673813132));
#278409=CARTESIAN_POINT('Ctrl Pts',(-12.1623797632097,137.52499999946,2.97892388940585E-15));
#278410=CARTESIAN_POINT('Ctrl Pts',(-12.1623797632097,137.674999999459,
3.95179673813133));
#278411=CARTESIAN_POINT('Ctrl Pts',(-9.83957192047864,137.824999999459,
7.14886745759505));
#278412=CARTESIAN_POINT('Ctrl Pts',(-7.51676407774755,137.974999999458,
10.3459381770588));
#278413=CARTESIAN_POINT('Ctrl Pts',(-3.75838203887382,138.124999999458,
11.5671105274568));
#278414=CARTESIAN_POINT('Ctrl Pts',(-8.97614538113089E-14,138.274999999457,
12.7882828778549));
#278415=CARTESIAN_POINT('Ctrl Pts',(3.75838203887364,138.424999999456,11.5671105274568));
#278416=CARTESIAN_POINT('Ctrl Pts',(7.51676407774736,138.574999999456,10.3459381770588));
#278417=CARTESIAN_POINT('Ctrl Pts',(9.83957192047846,138.724999999455,7.14886745759505));
#278418=CARTESIAN_POINT('Ctrl Pts',(12.1623797632096,138.874999999455,3.95179673813132));
#278419=CARTESIAN_POINT('Ctrl Pts',(12.1623797632096,139.024999999454,-1.48946194470292E-15));
#278420=CARTESIAN_POINT('Ctrl Pts',(12.1623797632095,139.174999999453,-3.95179673813132));
#278421=CARTESIAN_POINT('Ctrl Pts',(9.83957192047846,139.324999999453,-7.14886745759505));
#278422=CARTESIAN_POINT('Ctrl Pts',(7.51676407774736,139.474999999452,-10.3459381770588));
#278423=CARTESIAN_POINT('Ctrl Pts',(3.75838203887363,139.624999999452,-11.5671105274568));
#278424=CARTESIAN_POINT('Ctrl Pts',(-9.3757534385731E-14,139.774999999451,
-12.7882828778549));
#278425=CARTESIAN_POINT('Ctrl Pts',(-3.75838203887382,139.92499999945,-11.5671105274568));
#278426=CARTESIAN_POINT('Ctrl Pts',(-7.51676407774755,140.07499999945,-10.3459381770588));
#278427=CARTESIAN_POINT('Ctrl Pts',(-9.83957192047864,140.224999999449,
-7.14886745759505));
#278428=CARTESIAN_POINT('Ctrl Pts',(-12.1623797632097,140.374999999449,
-3.95179673813132));
#278429=CARTESIAN_POINT('Ctrl Pts',(-12.1623797632097,140.524999999448,
2.97892388940585E-15));
#278430=CARTESIAN_POINT('Ctrl Pts',(-12.1623797632097,140.674999999447,
3.95179673813133));
#278431=CARTESIAN_POINT('Ctrl Pts',(-9.83957192047864,140.824999999447,
7.14886745759505));
#278432=CARTESIAN_POINT('Ctrl Pts',(-7.51676407774755,140.974999999446,
10.3459381770588));
#278433=CARTESIAN_POINT('Ctrl Pts',(-3.75838203887382,141.124999999446,
11.5671105274568));
#278434=CARTESIAN_POINT('Ctrl Pts',(-9.14891630829708E-14,141.274999999445,
12.7882828778549));
#278435=CARTESIAN_POINT('Ctrl Pts',(3.75838203887364,141.424999999444,11.5671105274568));
#278436=CARTESIAN_POINT('Ctrl Pts',(7.51676407774736,141.574999999444,10.3459381770588));
#278437=CARTESIAN_POINT('Ctrl Pts',(9.83957192047845,141.724999999443,7.14886745759505));
#278438=CARTESIAN_POINT('Ctrl Pts',(12.1623797632095,141.874999999443,3.95179673813132));
#278439=CARTESIAN_POINT('Ctrl Pts',(12.1623797632095,142.024999999442,-1.48946194470292E-15));
#278440=CARTESIAN_POINT('Ctrl Pts',(12.1623797632095,142.174999999441,-3.95179673813132));
#278441=CARTESIAN_POINT('Ctrl Pts',(9.83957192047845,142.324999999441,-7.14886745759505));
#278442=CARTESIAN_POINT('Ctrl Pts',(7.51676407774736,142.47499999944,-10.3459381770588));
#278443=CARTESIAN_POINT('Ctrl Pts',(3.75838203887363,142.62499999944,-11.5671105274568));
#278444=CARTESIAN_POINT('Ctrl Pts',(-9.54852436573929E-14,142.774999999439,
-12.7882828778549));
#278445=CARTESIAN_POINT('Ctrl Pts',(-3.75838203887382,142.924999999438,
-11.5671105274568));
#278446=CARTESIAN_POINT('Ctrl Pts',(-7.51676407774755,143.074999999438,
-10.3459381770588));
#278447=CARTESIAN_POINT('Ctrl Pts',(-9.83957192047864,143.224999999437,
-7.14886745759505));
#278448=CARTESIAN_POINT('Ctrl Pts',(-12.1623797632097,143.374999999437,
-3.95179673813132));
#278449=CARTESIAN_POINT('Ctrl Pts',(-12.1623797632097,143.524999999436,
2.97892388940585E-15));
#278450=CARTESIAN_POINT('Ctrl Pts',(-12.1623797632097,143.674999999435,
3.95179673813133));
#278451=CARTESIAN_POINT('Ctrl Pts',(-9.83957192047864,143.824999999435,
7.14886745759505));
#278452=CARTESIAN_POINT('Ctrl Pts',(-7.51676407774755,143.974999999434,
10.3459381770588));
#278453=CARTESIAN_POINT('Ctrl Pts',(-3.75838203887382,144.124999999434,
11.5671105274568));
#278454=CARTESIAN_POINT('Ctrl Pts',(-9.32168723546326E-14,144.274999999433,
12.7882828778549));
#278455=CARTESIAN_POINT('Ctrl Pts',(3.75838203887363,144.424999999432,11.5671105274568));
#278456=CARTESIAN_POINT('Ctrl Pts',(7.51676407774736,144.574999999432,10.3459381770588));
#278457=CARTESIAN_POINT('Ctrl Pts',(9.83957192047845,144.724999999431,7.14886745759505));
#278458=CARTESIAN_POINT('Ctrl Pts',(12.1623797632095,144.874999999431,3.95179673813132));
#278459=CARTESIAN_POINT('Ctrl Pts',(12.1623797632095,145.02499999943,-1.48946194470292E-15));
#278460=CARTESIAN_POINT('Ctrl Pts',(12.1623797632095,145.174999999429,-3.95179673813132));
#278461=CARTESIAN_POINT('Ctrl Pts',(9.83957192047845,145.324999999429,-7.14886745759505));
#278462=CARTESIAN_POINT('Ctrl Pts',(7.51676407774736,145.474999999428,-10.3459381770588));
#278463=CARTESIAN_POINT('Ctrl Pts',(3.75838203887363,145.624999999428,-11.5671105274568));
#278464=CARTESIAN_POINT('Ctrl Pts',(-9.72129529290547E-14,145.774999999427,
-12.7882828778549));
#278465=CARTESIAN_POINT('Ctrl Pts',(-3.75838203887382,145.924999999426,
-11.5671105274568));
#278466=CARTESIAN_POINT('Ctrl Pts',(-7.51676407774755,146.074999999426,
-10.3459381770588));
#278467=CARTESIAN_POINT('Ctrl Pts',(-9.83957192047865,146.224999999425,
-7.14886745759505));
#278468=CARTESIAN_POINT('Ctrl Pts',(-12.1623797632097,146.374999999425,
-3.95179673813132));
#278469=CARTESIAN_POINT('Ctrl Pts',(-12.1623797632097,146.524999999424,
2.97892388940585E-15));
#278470=CARTESIAN_POINT('Ctrl Pts',(-12.1623797632097,146.674999999423,
3.95179673813133));
#278471=CARTESIAN_POINT('Ctrl Pts',(-9.83957192047865,146.824999999423,
7.14886745759505));
#278472=CARTESIAN_POINT('Ctrl Pts',(-7.51676407774755,146.974999999422,
10.3459381770588));
#278473=CARTESIAN_POINT('Ctrl Pts',(-3.75838203887382,147.124999999422,
11.5671105274568));
#278474=CARTESIAN_POINT('Ctrl Pts',(-9.49445816262944E-14,147.274999999421,
12.7882828778549));
#278475=CARTESIAN_POINT('Ctrl Pts',(3.75838203887363,147.42499999942,11.5671105274568));
#278476=CARTESIAN_POINT('Ctrl Pts',(7.51676407774736,147.57499999942,10.3459381770588));
#278477=CARTESIAN_POINT('Ctrl Pts',(9.83957192047845,147.724999999419,7.14886745759505));
#278478=CARTESIAN_POINT('Ctrl Pts',(12.1623797632095,147.874999999419,3.95179673813132));
#278479=CARTESIAN_POINT('Ctrl Pts',(12.1623797632095,148.024999999418,-1.48946194470292E-15));
#278480=CARTESIAN_POINT('Ctrl Pts',(12.1623797632095,148.174999999417,-3.95179673813132));
#278481=CARTESIAN_POINT('Ctrl Pts',(9.83957192047845,148.324999999417,-7.14886745759505));
#278482=CARTESIAN_POINT('Ctrl Pts',(7.51676407774736,148.474999999416,-10.3459381770588));
#278483=CARTESIAN_POINT('Ctrl Pts',(3.75838203887363,148.624999999416,-11.5671105274568));
#278484=CARTESIAN_POINT('Ctrl Pts',(-9.89406622007166E-14,148.774999999415,
-12.7882828778549));
#278485=CARTESIAN_POINT('Ctrl Pts',(-3.75838203887383,148.924999999414,
-11.5671105274568));
#278486=CARTESIAN_POINT('Ctrl Pts',(-7.51676407774756,149.074999999414,
-10.3459381770588));
#278487=CARTESIAN_POINT('Ctrl Pts',(-9.83957192047865,149.224999999413,
-7.14886745759505));
#278488=CARTESIAN_POINT('Ctrl Pts',(-12.1623797632097,149.374999999413,
-3.95179673813132));
#278489=CARTESIAN_POINT('Ctrl Pts',(-12.1623797632097,149.524999999412,
2.97892388940585E-15));
#278490=CARTESIAN_POINT('Ctrl Pts',(-12.1623797632097,149.674999999411,
3.95179673813133));
#278491=CARTESIAN_POINT('Ctrl Pts',(-9.83957192047865,149.824999999411,
7.14886745759505));
#278492=CARTESIAN_POINT('Ctrl Pts',(-7.51676407774755,149.97499999941,10.3459381770588));
#278493=CARTESIAN_POINT('Ctrl Pts',(-3.75838203887382,150.12499999941,11.5671105274568));
#278494=CARTESIAN_POINT('Ctrl Pts',(-9.66722908979563E-14,150.274999999409,
12.7882828778549));
#278495=CARTESIAN_POINT('Ctrl Pts',(3.75838203887363,150.424999999408,11.5671105274568));
#278496=CARTESIAN_POINT('Ctrl Pts',(7.51676407774736,150.574999999408,10.3459381770588));
#278497=CARTESIAN_POINT('Ctrl Pts',(9.83957192047845,150.724999999407,7.14886745759505));
#278498=CARTESIAN_POINT('Ctrl Pts',(12.1623797632095,150.874999999407,3.95179673813132));
#278499=CARTESIAN_POINT('Ctrl Pts',(12.1623797632095,151.024999999406,-1.48946194470292E-15));
#278500=CARTESIAN_POINT('Ctrl Pts',(12.1623797632095,151.174999999405,-3.95179673813132));
#278501=CARTESIAN_POINT('Ctrl Pts',(9.83957192047845,151.324999999405,-7.14886745759505));
#278502=CARTESIAN_POINT('Ctrl Pts',(7.51676407774736,151.474999999404,-10.3459381770588));
#278503=CARTESIAN_POINT('Ctrl Pts',(3.75838203887363,151.624999999404,-11.5671105274568));
#278504=CARTESIAN_POINT('Ctrl Pts',(-1.00668371472378E-13,151.774999999403,
-12.7882828778549));
#278505=CARTESIAN_POINT('Ctrl Pts',(-3.75838203887383,151.924999999402,
-11.5671105274568));
#278506=CARTESIAN_POINT('Ctrl Pts',(-7.51676407774756,152.074999999402,
-10.3459381770588));
#278507=CARTESIAN_POINT('Ctrl Pts',(-9.83957192047865,152.224999999401,
-7.14886745759505));
#278508=CARTESIAN_POINT('Ctrl Pts',(-12.1623797632097,152.374999999401,
-3.95179673813132));
#278509=CARTESIAN_POINT('Ctrl Pts',(-12.1623797632097,152.5249999994,2.97892388940585E-15));
#278510=CARTESIAN_POINT('Ctrl Pts',(-12.1623797632097,152.674999999399,
3.95179673813133));
#278511=CARTESIAN_POINT('Ctrl Pts',(-9.83957192047865,152.824999999399,
7.14886745759505));
#278512=CARTESIAN_POINT('Ctrl Pts',(-7.51676407774756,152.974999999398,
10.3459381770588));
#278513=CARTESIAN_POINT('Ctrl Pts',(-3.75838203887383,153.124999999398,
11.5671105274568));
#278514=CARTESIAN_POINT('Ctrl Pts',(-9.84000001696181E-14,153.274999999397,
12.7882828778549));
#278515=CARTESIAN_POINT('Ctrl Pts',(3.75838203887363,153.424999999396,11.5671105274568));
#278516=CARTESIAN_POINT('Ctrl Pts',(7.51676407774736,153.574999999396,10.3459381770588));
#278517=CARTESIAN_POINT('Ctrl Pts',(9.83957192047845,153.724999999395,7.14886745759505));
#278518=CARTESIAN_POINT('Ctrl Pts',(12.1623797632095,153.874999999395,3.95179673813132));
#278519=CARTESIAN_POINT('Ctrl Pts',(12.1623797632095,154.024999999394,-1.48946194470292E-15));
#278520=CARTESIAN_POINT('Ctrl Pts',(12.1623797632095,154.174999999393,-3.95179673813132));
#278521=CARTESIAN_POINT('Ctrl Pts',(9.83957192047845,154.324999999393,-7.14886745759505));
#278522=CARTESIAN_POINT('Ctrl Pts',(7.51676407774735,154.474999999392,-10.3459381770588));
#278523=CARTESIAN_POINT('Ctrl Pts',(3.75838203887363,154.624999999392,-11.5671105274568));
#278524=CARTESIAN_POINT('Ctrl Pts',(-1.0239608074404E-13,154.774999999391,
-12.7882828778549));
#278525=CARTESIAN_POINT('Ctrl Pts',(-3.75838203887383,154.92499999939,-11.5671105274568));
#278526=CARTESIAN_POINT('Ctrl Pts',(10.0514428414941,95.8062499996273,-1.23094673026484E-15));
#278527=CARTESIAN_POINT('Ctrl Pts',(10.0514428414941,95.9562499996266,-3.26591175476071));
#278528=CARTESIAN_POINT('Ctrl Pts',(8.13178807675712,96.1062499996261,-5.90808986649102));
#278529=CARTESIAN_POINT('Ctrl Pts',(6.21213331202015,96.2562499996255,-8.55026797822134));
#278530=CARTESIAN_POINT('Ctrl Pts',(3.10606665601004,96.4062499996248,-9.5594902125713));
#278531=CARTESIAN_POINT('Ctrl Pts',(-6.87318131996666E-14,96.5562499996243,
-10.5687124469213));
#278532=CARTESIAN_POINT('Ctrl Pts',(-3.10606665601018,96.7062499996236,
-9.5594902125713));
#278533=CARTESIAN_POINT('Ctrl Pts',(-6.21213331202028,96.856249999623,-8.55026797822134));
#278534=CARTESIAN_POINT('Ctrl Pts',(-8.13178807675726,97.0062499996224,
-5.90808986649102));
#278535=CARTESIAN_POINT('Ctrl Pts',(-10.0514428414942,97.1562499996218,
-3.2659117547607));
#278536=CARTESIAN_POINT('Ctrl Pts',(-10.0514428414942,97.3062499996212,
2.46189346052968E-15));
#278537=CARTESIAN_POINT('Ctrl Pts',(-10.0514428414942,97.4562499996206,
3.26591175476071));
#278538=CARTESIAN_POINT('Ctrl Pts',(-8.13178807675726,97.60624999962,5.90808986649102));
#278539=CARTESIAN_POINT('Ctrl Pts',(-6.21213331202028,97.7562499996194,
8.55026797822134));
#278540=CARTESIAN_POINT('Ctrl Pts',(-3.10606665601018,97.9062499996189,
9.5594902125713));
#278541=CARTESIAN_POINT('Ctrl Pts',(-6.70070798616514E-14,98.0562499996182,
10.5687124469213));
#278542=CARTESIAN_POINT('Ctrl Pts',(3.10606665601004,98.2062499996177,9.5594902125713));
#278543=CARTESIAN_POINT('Ctrl Pts',(6.21213331202015,98.3562499996171,8.55026797822134));
#278544=CARTESIAN_POINT('Ctrl Pts',(8.13178807675712,98.5062499996165,5.90808986649102));
#278545=CARTESIAN_POINT('Ctrl Pts',(10.0514428414941,98.6562499996158,3.2659117547607));
#278546=CARTESIAN_POINT('Ctrl Pts',(10.0514428414941,98.8062499996153,-1.23094673026484E-15));
#278547=CARTESIAN_POINT('Ctrl Pts',(-12.1623797632103,-3.28749999997638,
2.97892388940601E-15));
#278548=CARTESIAN_POINT('Ctrl Pts',(-12.1623797632103,-3.13749999997698,
3.95179673813154));
#278549=CARTESIAN_POINT('Ctrl Pts',(-9.83957192047908,-2.98749999997758,
7.14886745759543));
#278550=CARTESIAN_POINT('Ctrl Pts',(-7.51676407774787,-2.83749999997817,
10.3459381770593));
#278551=CARTESIAN_POINT('Ctrl Pts',(-3.75838203887394,-2.68749999997877,
11.5671105274575));
#278552=CARTESIAN_POINT('Ctrl Pts',(-8.66709987268145E-15,-2.53749999997937,
12.7882828778556));
#278553=CARTESIAN_POINT('Ctrl Pts',(3.75838203887392,-2.38749999997997,
11.5671105274575));
#278554=CARTESIAN_POINT('Ctrl Pts',(7.51676407774785,-2.23749999998057,
10.3459381770593));
#278555=CARTESIAN_POINT('Ctrl Pts',(9.83957192047906,-2.08749999998117,
7.14886745759543));
#278556=CARTESIAN_POINT('Ctrl Pts',(12.1623797632103,-1.93749999998176,
3.95179673813153));
#278557=CARTESIAN_POINT('Ctrl Pts',(12.1623797632103,-1.78749999998236,
-1.489461944703E-15));
#278558=CARTESIAN_POINT('Ctrl Pts',(12.1623797632103,-1.63749999998296,
-3.95179673813154));
#278559=CARTESIAN_POINT('Ctrl Pts',(9.83957192047906,-1.48749999998357,
-7.14886745759543));
#278560=CARTESIAN_POINT('Ctrl Pts',(7.51676407774784,-1.33749999998417,
-10.3459381770593));
#278561=CARTESIAN_POINT('Ctrl Pts',(3.75838203887392,-1.18749999998477,
-11.5671105274575));
#278562=CARTESIAN_POINT('Ctrl Pts',(-1.26631804471037E-14,-1.03749999998537,
-12.7882828778556));
#278563=CARTESIAN_POINT('Ctrl Pts',(-3.75838203887394,-0.887499999985973,
-11.5671105274575));
#278564=CARTESIAN_POINT('Ctrl Pts',(-7.51676407774787,-0.737499999986575,
-10.3459381770593));
#278565=CARTESIAN_POINT('Ctrl Pts',(-9.83957192047909,-0.587499999987176,
-7.14886745759543));
#278566=CARTESIAN_POINT('Ctrl Pts',(-12.1623797632103,-0.437499999987778,
-3.95179673813153));
#278567=CARTESIAN_POINT('Ctrl Pts',(-12.1623797632103,-0.287499999988378,
2.97892388940601E-15));
#278568=CARTESIAN_POINT('Ctrl Pts',(-12.1623797632103,-0.137499999988978,
3.95179673813154));
#278569=CARTESIAN_POINT('Ctrl Pts',(-9.83957192047909,0.0125000000104236,
7.14886745759543));
#278570=CARTESIAN_POINT('Ctrl Pts',(-7.51676407774787,0.162500000009825,
10.3459381770593));
#278571=CARTESIAN_POINT('Ctrl Pts',(-3.75838203887394,0.312500000009227,
11.5671105274575));
#278572=CARTESIAN_POINT('Ctrl Pts',(-1.03948091443433E-14,0.462500000008629,
12.7882828778556));
#278573=CARTESIAN_POINT('Ctrl Pts',(3.75838203887392,0.612500000008031,
11.5671105274575));
#278574=CARTESIAN_POINT('Ctrl Pts',(7.51676407774785,0.762500000007433,
10.3459381770593));
#278575=CARTESIAN_POINT('Ctrl Pts',(9.83957192047906,0.912500000006835,
7.14886745759543));
#278576=CARTESIAN_POINT('Ctrl Pts',(12.1623797632103,1.06250000000624,3.95179673813153));
#278577=CARTESIAN_POINT('Ctrl Pts',(12.1623797632103,1.21250000000564,-1.489461944703E-15));
#278578=CARTESIAN_POINT('Ctrl Pts',(12.1623797632103,1.36250000000504,-3.95179673813154));
#278579=CARTESIAN_POINT('Ctrl Pts',(9.83957192047906,1.51250000000444,-7.14886745759543));
#278580=CARTESIAN_POINT('Ctrl Pts',(7.51676407774784,1.66250000000383,-10.3459381770593));
#278581=CARTESIAN_POINT('Ctrl Pts',(3.75838203887391,1.81250000000323,-11.5671105274575));
#278582=CARTESIAN_POINT('Ctrl Pts',(-1.43908897187656E-14,1.96250000000263,
-12.7882828778556));
#278583=CARTESIAN_POINT('Ctrl Pts',(-3.75838203887394,2.11250000000203,
-11.5671105274575));
#278584=CARTESIAN_POINT('Ctrl Pts',(-7.51676407774787,2.26250000000143,
-10.3459381770593));
#278585=CARTESIAN_POINT('Ctrl Pts',(-9.83957192047909,2.41250000000082,
-7.14886745759543));
#278586=CARTESIAN_POINT('Ctrl Pts',(-12.1623797632103,2.56250000000022,
-3.95179673813153));
#278587=CARTESIAN_POINT('Ctrl Pts',(-12.1623797632103,2.71249999999962,
2.97892388940601E-15));
#278588=CARTESIAN_POINT('Ctrl Pts',(-12.1623797632103,2.86249999999902,
3.95179673813154));
#278589=CARTESIAN_POINT('Ctrl Pts',(-9.83957192047909,3.01249999999842,
7.14886745759543));
#278590=CARTESIAN_POINT('Ctrl Pts',(-7.51676407774787,3.16249999999782,
10.3459381770593));
#278591=CARTESIAN_POINT('Ctrl Pts',(-3.75838203887394,3.31249999999723,
11.5671105274575));
#278592=CARTESIAN_POINT('Ctrl Pts',(-1.21225184160051E-14,3.46249999999663,
12.7882828778556));
#278593=CARTESIAN_POINT('Ctrl Pts',(3.75838203887392,3.61249999999603,11.5671105274575));
#278594=CARTESIAN_POINT('Ctrl Pts',(7.51676407774784,3.76249999999543,10.3459381770593));
#278595=CARTESIAN_POINT('Ctrl Pts',(9.83957192047906,3.91249999999483,7.14886745759543));
#278596=CARTESIAN_POINT('Ctrl Pts',(12.1623797632103,4.06249999999424,3.95179673813153));
#278597=CARTESIAN_POINT('Ctrl Pts',(12.1623797632103,4.21249999999364,-1.489461944703E-15));
#278598=CARTESIAN_POINT('Ctrl Pts',(12.1623797632103,4.36249999999303,-3.95179673813154));
#278599=CARTESIAN_POINT('Ctrl Pts',(9.83957192047906,4.51249999999243,-7.14886745759543));
#278600=CARTESIAN_POINT('Ctrl Pts',(7.51676407774784,4.66249999999183,-10.3459381770593));
#278601=CARTESIAN_POINT('Ctrl Pts',(3.75838203887391,4.81249999999123,-11.5671105274575));
#278602=CARTESIAN_POINT('Ctrl Pts',(-1.61185989904274E-14,4.96249999999063,
-12.7882828778556));
#278603=CARTESIAN_POINT('Ctrl Pts',(-3.75838203887394,5.11249999999003,
-11.5671105274575));
#278604=CARTESIAN_POINT('Ctrl Pts',(-7.51676407774788,5.26249999998942,
-10.3459381770593));
#278605=CARTESIAN_POINT('Ctrl Pts',(-9.83957192047909,5.41249999998882,
-7.14886745759543));
#278606=CARTESIAN_POINT('Ctrl Pts',(-12.1623797632103,5.56249999998822,
-3.95179673813153));
#278607=CARTESIAN_POINT('Ctrl Pts',(-12.1623797632103,5.71249999998762,
2.97892388940601E-15));
#278608=CARTESIAN_POINT('Ctrl Pts',(-12.1623797632103,5.86249999998702,
3.95179673813154));
#278609=CARTESIAN_POINT('Ctrl Pts',(-9.83957192047909,6.01249999998642,
7.14886745759543));
#278610=CARTESIAN_POINT('Ctrl Pts',(-7.51676407774787,6.16249999998582,
10.3459381770593));
#278611=CARTESIAN_POINT('Ctrl Pts',(-3.75838203887394,6.31249999998523,
11.5671105274575));
#278612=CARTESIAN_POINT('Ctrl Pts',(-1.3850227687667E-14,6.46249999998463,
12.7882828778556));
#278613=CARTESIAN_POINT('Ctrl Pts',(3.75838203887392,6.61249999998403,11.5671105274575));
#278614=CARTESIAN_POINT('Ctrl Pts',(7.51676407774784,6.76249999998343,10.3459381770593));
#278615=CARTESIAN_POINT('Ctrl Pts',(9.83957192047906,6.91249999998283,7.14886745759543));
#278616=CARTESIAN_POINT('Ctrl Pts',(12.1623797632103,7.06249999998224,3.95179673813153));
#278617=CARTESIAN_POINT('Ctrl Pts',(12.1623797632103,7.21249999998164,-1.489461944703E-15));
#278618=CARTESIAN_POINT('Ctrl Pts',(12.1623797632103,7.36249999998104,-3.95179673813154));
#278619=CARTESIAN_POINT('Ctrl Pts',(9.83957192047906,7.51249999998044,-7.14886745759543));
#278620=CARTESIAN_POINT('Ctrl Pts',(7.51676407774784,7.66249999997983,-10.3459381770593));
#278621=CARTESIAN_POINT('Ctrl Pts',(3.75838203887391,7.81249999997923,-11.5671105274575));
#278622=CARTESIAN_POINT('Ctrl Pts',(-1.78463082620892E-14,7.96249999997863,
-12.7882828778556));
#278623=CARTESIAN_POINT('Ctrl Pts',(-3.75838203887395,8.11249999997803,
-11.5671105274575));
#278624=CARTESIAN_POINT('Ctrl Pts',(-7.51676407774788,8.26249999997743,
-10.3459381770593));
#278625=CARTESIAN_POINT('Ctrl Pts',(-9.83957192047909,8.41249999997682,
-7.14886745759543));
#278626=CARTESIAN_POINT('Ctrl Pts',(-12.1623797632103,8.56249999997622,
-3.95179673813153));
#278627=CARTESIAN_POINT('Ctrl Pts',(-12.1623797632103,8.71249999997562,
2.97892388940601E-15));
#278628=CARTESIAN_POINT('Ctrl Pts',(-12.1623797632103,8.86249999997502,
3.95179673813154));
#278629=CARTESIAN_POINT('Ctrl Pts',(-9.83957192047909,9.01249999997442,
7.14886745759543));
#278630=CARTESIAN_POINT('Ctrl Pts',(-7.51676407774787,9.16249999997382,
10.3459381770593));
#278631=CARTESIAN_POINT('Ctrl Pts',(-3.75838203887394,9.31249999997323,
11.5671105274575));
#278632=CARTESIAN_POINT('Ctrl Pts',(-1.55779369593288E-14,9.46249999997263,
12.7882828778556));
#278633=CARTESIAN_POINT('Ctrl Pts',(3.75838203887391,9.61249999997203,11.5671105274575));
#278634=CARTESIAN_POINT('Ctrl Pts',(7.51676407774784,9.76249999997144,10.3459381770593));
#278635=CARTESIAN_POINT('Ctrl Pts',(9.83957192047906,9.91249999997084,7.14886745759543));
#278636=CARTESIAN_POINT('Ctrl Pts',(12.1623797632103,10.0624999999702,3.95179673813153));
#278637=CARTESIAN_POINT('Ctrl Pts',(12.1623797632103,10.2124999999696,-1.489461944703E-15));
#278638=CARTESIAN_POINT('Ctrl Pts',(12.1623797632103,10.362499999969,-3.95179673813154));
#278639=CARTESIAN_POINT('Ctrl Pts',(9.83957192047905,10.5124999999684,-7.14886745759543));
#278640=CARTESIAN_POINT('Ctrl Pts',(7.51676407774784,10.6624999999678,-10.3459381770593));
#278641=CARTESIAN_POINT('Ctrl Pts',(3.75838203887391,10.8124999999672,-11.5671105274575));
#278642=CARTESIAN_POINT('Ctrl Pts',(-1.95740175337511E-14,10.9624999999666,
-12.7882828778556));
#278643=CARTESIAN_POINT('Ctrl Pts',(-3.75838203887395,11.112499999966,-11.5671105274575));
#278644=CARTESIAN_POINT('Ctrl Pts',(-7.51676407774788,11.2624999999654,
-10.3459381770593));
#278645=CARTESIAN_POINT('Ctrl Pts',(-9.83957192047909,11.4124999999648,
-7.14886745759543));
#278646=CARTESIAN_POINT('Ctrl Pts',(-12.1623797632103,11.5624999999642,
-3.95179673813153));
#278647=CARTESIAN_POINT('Ctrl Pts',(-12.1623797632103,11.7124999999636,
2.97892388940601E-15));
#278648=CARTESIAN_POINT('Ctrl Pts',(-12.1623797632103,11.862499999963,3.95179673813154));
#278649=CARTESIAN_POINT('Ctrl Pts',(-9.83957192047909,12.0124999999624,
7.14886745759543));
#278650=CARTESIAN_POINT('Ctrl Pts',(-7.51676407774788,12.1624999999618,
10.3459381770593));
#278651=CARTESIAN_POINT('Ctrl Pts',(-3.75838203887395,12.3124999999612,
11.5671105274575));
#278652=CARTESIAN_POINT('Ctrl Pts',(-1.73056462309906E-14,12.4624999999606,
12.7882828778556));
#278653=CARTESIAN_POINT('Ctrl Pts',(3.75838203887391,12.61249999996,11.5671105274575));
#278654=CARTESIAN_POINT('Ctrl Pts',(7.51676407774784,12.7624999999594,10.3459381770593));
#278655=CARTESIAN_POINT('Ctrl Pts',(9.83957192047906,12.9124999999588,7.14886745759543));
#278656=CARTESIAN_POINT('Ctrl Pts',(12.1623797632103,13.0624999999582,3.95179673813153));
#278657=CARTESIAN_POINT('Ctrl Pts',(12.1623797632103,13.2124999999576,-1.489461944703E-15));
#278658=CARTESIAN_POINT('Ctrl Pts',(12.1623797632103,13.362499999957,-3.95179673813154));
#278659=CARTESIAN_POINT('Ctrl Pts',(9.83957192047905,13.5124999999564,-7.14886745759543));
#278660=CARTESIAN_POINT('Ctrl Pts',(7.51676407774784,13.6624999999558,-10.3459381770593));
#278661=CARTESIAN_POINT('Ctrl Pts',(3.75838203887391,13.8124999999552,-11.5671105274575));
#278662=CARTESIAN_POINT('Ctrl Pts',(-2.13017268054129E-14,13.9624999999546,
-12.7882828778556));
#278663=CARTESIAN_POINT('Ctrl Pts',(-3.75838203887395,14.112499999954,-11.5671105274575));
#278664=CARTESIAN_POINT('Ctrl Pts',(-7.51676407774788,14.2624999999534,
-10.3459381770593));
#278665=CARTESIAN_POINT('Ctrl Pts',(-9.8395719204791,14.4124999999528,-7.14886745759543));
#278666=CARTESIAN_POINT('Ctrl Pts',(-12.1623797632103,14.5624999999522,
-3.95179673813153));
#278667=CARTESIAN_POINT('Ctrl Pts',(-12.1623797632103,14.7124999999516,
2.97892388940601E-15));
#278668=CARTESIAN_POINT('Ctrl Pts',(-12.1623797632103,14.862499999951,3.95179673813154));
#278669=CARTESIAN_POINT('Ctrl Pts',(-9.83957192047909,15.0124999999504,
7.14886745759543));
#278670=CARTESIAN_POINT('Ctrl Pts',(-7.51676407774788,15.1624999999498,
10.3459381770593));
#278671=CARTESIAN_POINT('Ctrl Pts',(-3.75838203887395,15.3124999999492,
11.5671105274575));
#278672=CARTESIAN_POINT('Ctrl Pts',(-1.90333555026525E-14,15.4624999999486,
12.7882828778556));
#278673=CARTESIAN_POINT('Ctrl Pts',(3.75838203887391,15.612499999948,11.5671105274575));
#278674=CARTESIAN_POINT('Ctrl Pts',(7.51676407774784,15.7624999999474,10.3459381770593));
#278675=CARTESIAN_POINT('Ctrl Pts',(9.83957192047905,15.9124999999468,7.14886745759543));
#278676=CARTESIAN_POINT('Ctrl Pts',(12.1623797632103,16.0624999999462,3.95179673813153));
#278677=CARTESIAN_POINT('Ctrl Pts',(12.1623797632103,16.2124999999456,-1.489461944703E-15));
#278678=CARTESIAN_POINT('Ctrl Pts',(12.1623797632103,16.362499999945,-3.95179673813154));
#278679=CARTESIAN_POINT('Ctrl Pts',(9.83957192047905,16.5124999999444,-7.14886745759543));
#278680=CARTESIAN_POINT('Ctrl Pts',(7.51676407774784,16.6624999999438,-10.3459381770593));
#278681=CARTESIAN_POINT('Ctrl Pts',(3.75838203887391,16.8124999999432,-11.5671105274575));
#278682=CARTESIAN_POINT('Ctrl Pts',(-2.30294360770748E-14,16.9624999999426,
-12.7882828778556));
#278683=CARTESIAN_POINT('Ctrl Pts',(-3.75838203887395,17.112499999942,-11.5671105274575));
#278684=CARTESIAN_POINT('Ctrl Pts',(-7.51676407774788,17.2624999999414,
-10.3459381770593));
#278685=CARTESIAN_POINT('Ctrl Pts',(-9.8395719204791,17.4124999999408,-7.14886745759543));
#278686=CARTESIAN_POINT('Ctrl Pts',(-12.1623797632103,17.5624999999402,
-3.95179673813153));
#278687=CARTESIAN_POINT('Ctrl Pts',(-12.1623797632103,17.7124999999396,
2.97892388940601E-15));
#278688=CARTESIAN_POINT('Ctrl Pts',(-12.1623797632103,17.862499999939,3.95179673813154));
#278689=CARTESIAN_POINT('Ctrl Pts',(-9.8395719204791,18.0124999999384,7.14886745759543));
#278690=CARTESIAN_POINT('Ctrl Pts',(-7.51676407774788,18.1624999999378,
10.3459381770593));
#278691=CARTESIAN_POINT('Ctrl Pts',(-3.75838203887395,18.3124999999372,
11.5671105274575));
#278692=CARTESIAN_POINT('Ctrl Pts',(-2.07610647743143E-14,18.4624999999366,
12.7882828778556));
#278693=CARTESIAN_POINT('Ctrl Pts',(3.75838203887391,18.612499999936,11.5671105274575));
#278694=CARTESIAN_POINT('Ctrl Pts',(7.51676407774784,18.7624999999354,10.3459381770593));
#278695=CARTESIAN_POINT('Ctrl Pts',(9.83957192047905,18.9124999999348,7.14886745759543));
#278696=CARTESIAN_POINT('Ctrl Pts',(12.1623797632103,19.0624999999342,3.95179673813153));
#278697=CARTESIAN_POINT('Ctrl Pts',(12.1623797632103,19.2124999999336,-1.489461944703E-15));
#278698=CARTESIAN_POINT('Ctrl Pts',(12.1623797632103,19.362499999933,-3.95179673813154));
#278699=CARTESIAN_POINT('Ctrl Pts',(9.83957192047905,19.5124999999324,-7.14886745759543));
#278700=CARTESIAN_POINT('Ctrl Pts',(7.51676407774784,19.6624999999318,-10.3459381770593));
#278701=CARTESIAN_POINT('Ctrl Pts',(3.7583820388739,19.8124999999312,-11.5671105274575));
#278702=CARTESIAN_POINT('Ctrl Pts',(-2.47571453487366E-14,19.9624999999306,
-12.7882828778556));
#278703=CARTESIAN_POINT('Ctrl Pts',(-3.75838203887395,20.11249999993,-11.5671105274575));
#278704=CARTESIAN_POINT('Ctrl Pts',(-7.51676407774788,20.2624999999294,
-10.3459381770593));
#278705=CARTESIAN_POINT('Ctrl Pts',(-9.8395719204791,20.4124999999288,-7.14886745759543));
#278706=CARTESIAN_POINT('Ctrl Pts',(-12.1623797632103,20.5624999999282,
-3.95179673813153));
#278707=CARTESIAN_POINT('Ctrl Pts',(-12.1623797632103,20.7124999999276,
2.97892388940601E-15));
#278708=CARTESIAN_POINT('Ctrl Pts',(-12.1623797632103,20.862499999927,3.95179673813154));
#278709=CARTESIAN_POINT('Ctrl Pts',(-9.8395719204791,21.0124999999264,7.14886745759543));
#278710=CARTESIAN_POINT('Ctrl Pts',(-7.51676407774788,21.1624999999258,
10.3459381770593));
#278711=CARTESIAN_POINT('Ctrl Pts',(-3.75838203887395,21.3124999999252,
11.5671105274575));
#278712=CARTESIAN_POINT('Ctrl Pts',(-2.24887740459762E-14,21.4624999999246,
12.7882828778556));
#278713=CARTESIAN_POINT('Ctrl Pts',(3.75838203887391,21.612499999924,11.5671105274575));
#278714=CARTESIAN_POINT('Ctrl Pts',(7.51676407774784,21.7624999999234,10.3459381770593));
#278715=CARTESIAN_POINT('Ctrl Pts',(9.83957192047905,21.9124999999228,7.14886745759543));
#278716=CARTESIAN_POINT('Ctrl Pts',(12.1623797632103,22.0624999999222,3.95179673813153));
#278717=CARTESIAN_POINT('Ctrl Pts',(12.1623797632103,22.2124999999216,-1.489461944703E-15));
#278718=CARTESIAN_POINT('Ctrl Pts',(12.1623797632103,22.362499999921,-3.95179673813154));
#278719=CARTESIAN_POINT('Ctrl Pts',(9.83957192047905,22.5124999999204,-7.14886745759543));
#278720=CARTESIAN_POINT('Ctrl Pts',(7.51676407774783,22.6624999999198,-10.3459381770593));
#278721=CARTESIAN_POINT('Ctrl Pts',(3.7583820388739,22.8124999999192,-11.5671105274575));
#278722=CARTESIAN_POINT('Ctrl Pts',(-2.64848546203984E-14,22.9624999999186,
-12.7882828778556));
#278723=CARTESIAN_POINT('Ctrl Pts',(-3.75838203887396,23.112499999918,-11.5671105274575));
#278724=CARTESIAN_POINT('Ctrl Pts',(-7.51676407774788,23.2624999999174,
-10.3459381770593));
#278725=CARTESIAN_POINT('Ctrl Pts',(-9.8395719204791,23.4124999999168,-7.14886745759543));
#278726=CARTESIAN_POINT('Ctrl Pts',(-12.1623797632103,23.5624999999162,
-3.95179673813153));
#278727=CARTESIAN_POINT('Ctrl Pts',(-12.1623797632103,23.7124999999156,
2.97892388940601E-15));
#278728=CARTESIAN_POINT('Ctrl Pts',(-12.1623797632103,23.862499999915,3.95179673813154));
#278729=CARTESIAN_POINT('Ctrl Pts',(-9.8395719204791,24.0124999999144,7.14886745759543));
#278730=CARTESIAN_POINT('Ctrl Pts',(-7.51676407774788,24.1624999999138,
10.3459381770593));
#278731=CARTESIAN_POINT('Ctrl Pts',(-3.75838203887395,24.3124999999132,
11.5671105274575));
#278732=CARTESIAN_POINT('Ctrl Pts',(-2.4216483317638E-14,24.4624999999126,
12.7882828778556));
#278733=CARTESIAN_POINT('Ctrl Pts',(3.7583820388739,24.612499999912,11.5671105274575));
#278734=CARTESIAN_POINT('Ctrl Pts',(7.51676407774783,24.7624999999114,10.3459381770593));
#278735=CARTESIAN_POINT('Ctrl Pts',(9.83957192047905,24.9124999999108,7.14886745759543));
#278736=CARTESIAN_POINT('Ctrl Pts',(12.1623797632103,25.0624999999102,3.95179673813153));
#278737=CARTESIAN_POINT('Ctrl Pts',(12.1623797632103,25.2124999999096,-1.489461944703E-15));
#278738=CARTESIAN_POINT('Ctrl Pts',(12.1623797632103,25.362499999909,-3.95179673813154));
#278739=CARTESIAN_POINT('Ctrl Pts',(9.83957192047905,25.5124999999084,-7.14886745759543));
#278740=CARTESIAN_POINT('Ctrl Pts',(7.51676407774783,25.6624999999078,-10.3459381770593));
#278741=CARTESIAN_POINT('Ctrl Pts',(3.7583820388739,25.8124999999072,-11.5671105274575));
#278742=CARTESIAN_POINT('Ctrl Pts',(-2.82125638920603E-14,25.9624999999066,
-12.7882828778556));
#278743=CARTESIAN_POINT('Ctrl Pts',(-3.75838203887396,26.112499999906,-11.5671105274575));
#278744=CARTESIAN_POINT('Ctrl Pts',(-7.51676407774788,26.2624999999054,
-10.3459381770593));
#278745=CARTESIAN_POINT('Ctrl Pts',(-9.8395719204791,26.4124999999048,-7.14886745759543));
#278746=CARTESIAN_POINT('Ctrl Pts',(-12.1623797632103,26.5624999999042,
-3.95179673813153));
#278747=CARTESIAN_POINT('Ctrl Pts',(-12.1623797632103,26.7124999999036,
2.97892388940601E-15));
#278748=CARTESIAN_POINT('Ctrl Pts',(-12.1623797632103,26.862499999903,3.95179673813154));
#278749=CARTESIAN_POINT('Ctrl Pts',(-9.8395719204791,27.0124999999024,7.14886745759543));
#278750=CARTESIAN_POINT('Ctrl Pts',(-7.51676407774788,27.1624999999018,
10.3459381770593));
#278751=CARTESIAN_POINT('Ctrl Pts',(-3.75838203887396,27.3124999999012,
11.5671105274575));
#278752=CARTESIAN_POINT('Ctrl Pts',(-2.59441925892998E-14,27.4624999999006,
12.7882828778556));
#278753=CARTESIAN_POINT('Ctrl Pts',(3.7583820388739,27.6124999999,11.5671105274575));
#278754=CARTESIAN_POINT('Ctrl Pts',(7.51676407774783,27.7624999998994,10.3459381770593));
#278755=CARTESIAN_POINT('Ctrl Pts',(9.83957192047905,27.9124999998988,7.14886745759543));
#278756=CARTESIAN_POINT('Ctrl Pts',(12.1623797632103,28.0624999998982,3.95179673813153));
#278757=CARTESIAN_POINT('Ctrl Pts',(12.1623797632103,28.2124999998976,-1.489461944703E-15));
#278758=CARTESIAN_POINT('Ctrl Pts',(12.1623797632103,28.362499999897,-3.95179673813154));
#278759=CARTESIAN_POINT('Ctrl Pts',(9.83957192047905,28.5124999998964,-7.14886745759543));
#278760=CARTESIAN_POINT('Ctrl Pts',(7.51676407774783,28.6624999998958,-10.3459381770593));
#278761=CARTESIAN_POINT('Ctrl Pts',(3.7583820388739,28.8124999998952,-11.5671105274575));
#278762=CARTESIAN_POINT('Ctrl Pts',(-2.99402731637221E-14,28.9624999998946,
-12.7882828778556));
#278763=CARTESIAN_POINT('Ctrl Pts',(-3.75838203887396,29.112499999894,-11.5671105274575));
#278764=CARTESIAN_POINT('Ctrl Pts',(-7.51676407774789,29.2624999998934,
-10.3459381770593));
#278765=CARTESIAN_POINT('Ctrl Pts',(-9.8395719204791,29.4124999998928,-7.14886745759543));
#278766=CARTESIAN_POINT('Ctrl Pts',(-12.1623797632103,29.5624999998922,
-3.95179673813153));
#278767=CARTESIAN_POINT('Ctrl Pts',(-12.1623797632103,29.7124999998916,
2.97892388940601E-15));
#278768=CARTESIAN_POINT('Ctrl Pts',(-12.1623797632103,29.862499999891,3.95179673813154));
#278769=CARTESIAN_POINT('Ctrl Pts',(-9.8395719204791,30.0124999998904,7.14886745759543));
#278770=CARTESIAN_POINT('Ctrl Pts',(-7.51676407774788,30.1624999998898,
10.3459381770593));
#278771=CARTESIAN_POINT('Ctrl Pts',(-3.75838203887396,30.3124999998892,
11.5671105274575));
#278772=CARTESIAN_POINT('Ctrl Pts',(-2.76719018609617E-14,30.4624999998886,
12.7882828778556));
#278773=CARTESIAN_POINT('Ctrl Pts',(3.7583820388739,30.612499999888,11.5671105274575));
#278774=CARTESIAN_POINT('Ctrl Pts',(7.51676407774783,30.7624999998874,10.3459381770593));
#278775=CARTESIAN_POINT('Ctrl Pts',(9.83957192047905,30.9124999998868,7.14886745759543));
#278776=CARTESIAN_POINT('Ctrl Pts',(12.1623797632103,31.0624999998862,3.95179673813153));
#278777=CARTESIAN_POINT('Ctrl Pts',(12.1623797632103,31.2124999998856,-1.489461944703E-15));
#278778=CARTESIAN_POINT('Ctrl Pts',(12.1623797632103,31.362499999885,-3.95179673813154));
#278779=CARTESIAN_POINT('Ctrl Pts',(9.83957192047904,31.5124999998844,-7.14886745759543));
#278780=CARTESIAN_POINT('Ctrl Pts',(7.51676407774783,31.6624999998838,-10.3459381770593));
#278781=CARTESIAN_POINT('Ctrl Pts',(3.7583820388739,31.8124999998832,-11.5671105274575));
#278782=CARTESIAN_POINT('Ctrl Pts',(-3.16679824353839E-14,31.9624999998826,
-12.7882828778556));
#278783=CARTESIAN_POINT('Ctrl Pts',(-3.75838203887396,32.112499999882,-11.5671105274575));
#278784=CARTESIAN_POINT('Ctrl Pts',(-7.51676407774789,32.2624999998814,
-10.3459381770593));
#278785=CARTESIAN_POINT('Ctrl Pts',(-9.83957192047911,32.4124999998808,
-7.14886745759543));
#278786=CARTESIAN_POINT('Ctrl Pts',(-12.1623797632103,32.5624999998802,
-3.95179673813153));
#278787=CARTESIAN_POINT('Ctrl Pts',(-12.1623797632103,32.7124999998796,
2.97892388940601E-15));
#278788=CARTESIAN_POINT('Ctrl Pts',(-12.1623797632103,32.862499999879,3.95179673813154));
#278789=CARTESIAN_POINT('Ctrl Pts',(-9.8395719204791,33.0124999998784,7.14886745759543));
#278790=CARTESIAN_POINT('Ctrl Pts',(-7.51676407774789,33.1624999998778,
10.3459381770593));
#278791=CARTESIAN_POINT('Ctrl Pts',(-3.75838203887396,33.3124999998772,
11.5671105274575));
#278792=CARTESIAN_POINT('Ctrl Pts',(-2.93996111326235E-14,33.4624999998766,
12.7882828778556));
#278793=CARTESIAN_POINT('Ctrl Pts',(3.7583820388739,33.612499999876,11.5671105274575));
#278794=CARTESIAN_POINT('Ctrl Pts',(7.51676407774783,33.7624999998754,10.3459381770593));
#278795=CARTESIAN_POINT('Ctrl Pts',(9.83957192047905,33.9124999998748,7.14886745759543));
#278796=CARTESIAN_POINT('Ctrl Pts',(12.1623797632103,34.0624999998742,3.95179673813153));
#278797=CARTESIAN_POINT('Ctrl Pts',(12.1623797632103,34.2124999998736,-1.489461944703E-15));
#278798=CARTESIAN_POINT('Ctrl Pts',(12.1623797632103,34.362499999873,-3.95179673813154));
#278799=CARTESIAN_POINT('Ctrl Pts',(9.83957192047904,34.5124999998724,-7.14886745759543));
#278800=CARTESIAN_POINT('Ctrl Pts',(7.51676407774783,34.6624999998718,-10.3459381770593));
#278801=CARTESIAN_POINT('Ctrl Pts',(3.7583820388739,34.8124999998712,-11.5671105274575));
#278802=CARTESIAN_POINT('Ctrl Pts',(-3.33956917070458E-14,34.9624999998706,
-12.7882828778556));
#278803=CARTESIAN_POINT('Ctrl Pts',(-3.75838203887396,35.11249999987,-11.5671105274575));
#278804=CARTESIAN_POINT('Ctrl Pts',(-7.51676407774789,35.2624999998694,
-10.3459381770593));
#278805=CARTESIAN_POINT('Ctrl Pts',(-9.83957192047911,35.4124999998688,
-7.14886745759543));
#278806=CARTESIAN_POINT('Ctrl Pts',(-12.1623797632103,35.5624999998682,
-3.95179673813153));
#278807=CARTESIAN_POINT('Ctrl Pts',(-12.1623797632103,35.7124999998676,
2.97892388940601E-15));
#278808=CARTESIAN_POINT('Ctrl Pts',(-12.1623797632103,35.862499999867,3.95179673813154));
#278809=CARTESIAN_POINT('Ctrl Pts',(-9.83957192047911,36.0124999998664,
7.14886745759543));
#278810=CARTESIAN_POINT('Ctrl Pts',(-7.51676407774789,36.1624999998658,
10.3459381770593));
#278811=CARTESIAN_POINT('Ctrl Pts',(-3.75838203887396,36.3124999998652,
11.5671105274575));
#278812=CARTESIAN_POINT('Ctrl Pts',(-3.11273204042854E-14,36.4624999998646,
12.7882828778556));
#278813=CARTESIAN_POINT('Ctrl Pts',(3.7583820388739,36.612499999864,11.5671105274575));
#278814=CARTESIAN_POINT('Ctrl Pts',(7.51676407774783,36.7624999998634,10.3459381770593));
#278815=CARTESIAN_POINT('Ctrl Pts',(9.83957192047904,36.9124999998628,7.14886745759543));
#278816=CARTESIAN_POINT('Ctrl Pts',(12.1623797632103,37.0624999998622,3.95179673813153));
#278817=CARTESIAN_POINT('Ctrl Pts',(12.1623797632103,37.2124999998616,-1.489461944703E-15));
#278818=CARTESIAN_POINT('Ctrl Pts',(12.1623797632103,37.362499999861,-3.95179673813154));
#278819=CARTESIAN_POINT('Ctrl Pts',(9.83957192047904,37.5124999998604,-7.14886745759543));
#278820=CARTESIAN_POINT('Ctrl Pts',(7.51676407774782,37.6624999998598,-10.3459381770593));
#278821=CARTESIAN_POINT('Ctrl Pts',(3.75838203887389,37.8124999998592,-11.5671105274575));
#278822=CARTESIAN_POINT('Ctrl Pts',(-3.51234009787076E-14,37.9624999998586,
-12.7882828778556));
#278823=CARTESIAN_POINT('Ctrl Pts',(-3.75838203887396,38.112499999858,-11.5671105274575));
#278824=CARTESIAN_POINT('Ctrl Pts',(-7.51676407774789,38.2624999998574,
-10.3459381770593));
#278825=CARTESIAN_POINT('Ctrl Pts',(-9.83957192047911,38.4124999998568,
-7.14886745759543));
#278826=CARTESIAN_POINT('Ctrl Pts',(-12.1623797632103,38.5624999998562,
-3.95179673813153));
#278827=CARTESIAN_POINT('Ctrl Pts',(-12.1623797632103,38.7124999998556,
2.97892388940601E-15));
#278828=CARTESIAN_POINT('Ctrl Pts',(-12.1623797632103,38.862499999855,3.95179673813154));
#278829=CARTESIAN_POINT('Ctrl Pts',(-9.83957192047911,39.0124999998544,
7.14886745759543));
#278830=CARTESIAN_POINT('Ctrl Pts',(-7.51676407774789,39.1624999998538,
10.3459381770593));
#278831=CARTESIAN_POINT('Ctrl Pts',(-3.75838203887396,39.3124999998532,
11.5671105274575));
#278832=CARTESIAN_POINT('Ctrl Pts',(-3.28550296759472E-14,39.4624999998526,
12.7882828778556));
#278833=CARTESIAN_POINT('Ctrl Pts',(3.7583820388739,39.612499999852,11.5671105274575));
#278834=CARTESIAN_POINT('Ctrl Pts',(7.51676407774782,39.7624999998514,10.3459381770593));
#278835=CARTESIAN_POINT('Ctrl Pts',(9.83957192047904,39.9124999998508,7.14886745759543));
#278836=CARTESIAN_POINT('Ctrl Pts',(12.1623797632103,40.0624999998502,3.95179673813153));
#278837=CARTESIAN_POINT('Ctrl Pts',(12.1623797632103,40.2124999998496,-1.489461944703E-15));
#278838=CARTESIAN_POINT('Ctrl Pts',(12.1623797632103,40.362499999849,-3.95179673813154));
#278839=CARTESIAN_POINT('Ctrl Pts',(9.83957192047904,40.5124999998484,-7.14886745759543));
#278840=CARTESIAN_POINT('Ctrl Pts',(7.51676407774782,40.6624999998478,-10.3459381770593));
#278841=CARTESIAN_POINT('Ctrl Pts',(3.75838203887389,40.8124999998472,-11.5671105274575));
#278842=CARTESIAN_POINT('Ctrl Pts',(-3.68511102503695E-14,40.9624999998466,
-12.7882828778556));
#278843=CARTESIAN_POINT('Ctrl Pts',(-3.75838203887397,41.112499999846,-11.5671105274575));
#278844=CARTESIAN_POINT('Ctrl Pts',(-7.51676407774789,41.2624999998454,
-10.3459381770593));
#278845=CARTESIAN_POINT('Ctrl Pts',(-9.83957192047911,41.4124999998448,
-7.14886745759543));
#278846=CARTESIAN_POINT('Ctrl Pts',(-12.1623797632103,41.5624999998442,
-3.95179673813153));
#278847=CARTESIAN_POINT('Ctrl Pts',(-12.1623797632103,41.7124999998436,
2.97892388940601E-15));
#278848=CARTESIAN_POINT('Ctrl Pts',(-12.1623797632103,41.862499999843,3.95179673813154));
#278849=CARTESIAN_POINT('Ctrl Pts',(-9.83957192047911,42.0124999998424,
7.14886745759543));
#278850=CARTESIAN_POINT('Ctrl Pts',(-7.51676407774789,42.1624999998418,
10.3459381770593));
#278851=CARTESIAN_POINT('Ctrl Pts',(-3.75838203887396,42.3124999998412,
11.5671105274575));
#278852=CARTESIAN_POINT('Ctrl Pts',(-3.4582738947609E-14,42.4624999998406,
12.7882828778556));
#278853=CARTESIAN_POINT('Ctrl Pts',(3.75838203887389,42.61249999984,11.5671105274575));
#278854=CARTESIAN_POINT('Ctrl Pts',(7.51676407774782,42.7624999998394,10.3459381770593));
#278855=CARTESIAN_POINT('Ctrl Pts',(9.83957192047904,42.9124999998388,7.14886745759543));
#278856=CARTESIAN_POINT('Ctrl Pts',(12.1623797632103,43.0624999998382,3.95179673813153));
#278857=CARTESIAN_POINT('Ctrl Pts',(12.1623797632103,43.2124999998376,-1.489461944703E-15));
#278858=CARTESIAN_POINT('Ctrl Pts',(12.1623797632103,43.362499999837,-3.95179673813154));
#278859=CARTESIAN_POINT('Ctrl Pts',(9.83957192047903,43.5124999998364,-7.14886745759543));
#278860=CARTESIAN_POINT('Ctrl Pts',(7.51676407774782,43.6624999998358,-10.3459381770593));
#278861=CARTESIAN_POINT('Ctrl Pts',(3.75838203887389,43.8124999998352,-11.5671105274575));
#278862=CARTESIAN_POINT('Ctrl Pts',(-3.85788195220313E-14,43.9624999998346,
-12.7882828778556));
#278863=CARTESIAN_POINT('Ctrl Pts',(-3.75838203887397,44.112499999834,-11.5671105274575));
#278864=CARTESIAN_POINT('Ctrl Pts',(-7.5167640777479,44.2624999998334,-10.3459381770593));
#278865=CARTESIAN_POINT('Ctrl Pts',(-9.83957192047911,44.4124999998328,
-7.14886745759543));
#278866=CARTESIAN_POINT('Ctrl Pts',(-12.1623797632103,44.5624999998322,
-3.95179673813153));
#278867=CARTESIAN_POINT('Ctrl Pts',(-12.1623797632103,44.7124999998316,
2.97892388940601E-15));
#278868=CARTESIAN_POINT('Ctrl Pts',(-12.1623797632103,44.862499999831,3.95179673813154));
#278869=CARTESIAN_POINT('Ctrl Pts',(-9.83957192047911,45.0124999998304,
7.14886745759543));
#278870=CARTESIAN_POINT('Ctrl Pts',(-7.51676407774789,45.1624999998298,
10.3459381770593));
#278871=CARTESIAN_POINT('Ctrl Pts',(-3.75838203887397,45.3124999998292,
11.5671105274575));
#278872=CARTESIAN_POINT('Ctrl Pts',(-3.63104482192709E-14,45.4624999998286,
12.7882828778556));
#278873=CARTESIAN_POINT('Ctrl Pts',(3.75838203887389,45.612499999828,11.5671105274575));
#278874=CARTESIAN_POINT('Ctrl Pts',(7.51676407774782,45.7624999998274,10.3459381770593));
#278875=CARTESIAN_POINT('Ctrl Pts',(9.83957192047904,45.9124999998268,7.14886745759543));
#278876=CARTESIAN_POINT('Ctrl Pts',(12.1623797632103,46.0624999998262,3.95179673813153));
#278877=CARTESIAN_POINT('Ctrl Pts',(12.1623797632103,46.2124999998256,-1.489461944703E-15));
#278878=CARTESIAN_POINT('Ctrl Pts',(12.1623797632103,46.362499999825,-3.95179673813154));
#278879=CARTESIAN_POINT('Ctrl Pts',(9.83957192047903,46.5124999998244,-7.14886745759543));
#278880=CARTESIAN_POINT('Ctrl Pts',(7.51676407774782,46.6624999998238,-10.3459381770593));
#278881=CARTESIAN_POINT('Ctrl Pts',(3.75838203887389,46.8124999998232,-11.5671105274575));
#278882=CARTESIAN_POINT('Ctrl Pts',(-4.03065287936931E-14,46.9624999998226,
-12.7882828778556));
#278883=CARTESIAN_POINT('Ctrl Pts',(-3.75838203887397,47.112499999822,-11.5671105274575));
#278884=CARTESIAN_POINT('Ctrl Pts',(-7.5167640777479,47.2624999998214,-10.3459381770593));
#278885=CARTESIAN_POINT('Ctrl Pts',(-9.83957192047912,47.4124999998208,
-7.14886745759543));
#278886=CARTESIAN_POINT('Ctrl Pts',(-12.1623797632103,47.5624999998202,
-3.95179673813153));
#278887=CARTESIAN_POINT('Ctrl Pts',(-12.1623797632103,47.7124999998196,
2.97892388940601E-15));
#278888=CARTESIAN_POINT('Ctrl Pts',(-12.1623797632103,47.862499999819,3.95179673813154));
#278889=CARTESIAN_POINT('Ctrl Pts',(-9.83957192047911,48.0124999998184,
7.14886745759543));
#278890=CARTESIAN_POINT('Ctrl Pts',(-7.51676407774789,48.1624999998178,
10.3459381770593));
#278891=CARTESIAN_POINT('Ctrl Pts',(-3.75838203887397,48.3124999998172,
11.5671105274575));
#278892=CARTESIAN_POINT('Ctrl Pts',(-3.80381574909327E-14,48.4624999998166,
12.7882828778556));
#278893=CARTESIAN_POINT('Ctrl Pts',(3.75838203887389,48.612499999816,11.5671105274575));
#278894=CARTESIAN_POINT('Ctrl Pts',(7.51676407774782,48.7624999998154,10.3459381770593));
#278895=CARTESIAN_POINT('Ctrl Pts',(9.83957192047903,48.9124999998148,7.14886745759543));
#278896=CARTESIAN_POINT('Ctrl Pts',(12.1623797632103,49.0624999998142,3.95179673813153));
#278897=CARTESIAN_POINT('Ctrl Pts',(12.1623797632103,49.2124999998136,-1.489461944703E-15));
#278898=CARTESIAN_POINT('Ctrl Pts',(12.1623797632103,49.362499999813,-3.95179673813154));
#278899=CARTESIAN_POINT('Ctrl Pts',(9.83957192047903,49.5124999998124,-7.14886745759543));
#278900=CARTESIAN_POINT('Ctrl Pts',(7.51676407774782,49.6624999998118,-10.3459381770593));
#278901=CARTESIAN_POINT('Ctrl Pts',(3.75838203887389,49.8124999998112,-11.5671105274575));
#278902=CARTESIAN_POINT('Ctrl Pts',(-4.2034238065355E-14,49.9624999998106,
-12.7882828778556));
#278903=CARTESIAN_POINT('Ctrl Pts',(-3.75838203887397,50.11249999981,-11.5671105274575));
#278904=CARTESIAN_POINT('Ctrl Pts',(-7.5167640777479,50.2624999998094,-10.3459381770593));
#278905=CARTESIAN_POINT('Ctrl Pts',(-9.83957192047912,50.4124999998088,
-7.14886745759543));
#278906=CARTESIAN_POINT('Ctrl Pts',(-12.1623797632103,50.5624999998082,
-3.95179673813153));
#278907=CARTESIAN_POINT('Ctrl Pts',(-12.1623797632103,50.7124999998076,
2.97892388940601E-15));
#278908=CARTESIAN_POINT('Ctrl Pts',(-12.1623797632103,50.862499999807,3.95179673813154));
#278909=CARTESIAN_POINT('Ctrl Pts',(-9.83957192047912,51.0124999998064,
7.14886745759543));
#278910=CARTESIAN_POINT('Ctrl Pts',(-7.5167640777479,51.1624999998058,10.3459381770593));
#278911=CARTESIAN_POINT('Ctrl Pts',(-3.75838203887397,51.3124999998052,
11.5671105274575));
#278912=CARTESIAN_POINT('Ctrl Pts',(-3.97658667625946E-14,51.4624999998046,
12.7882828778556));
#278913=CARTESIAN_POINT('Ctrl Pts',(3.75838203887389,51.612499999804,11.5671105274575));
#278914=CARTESIAN_POINT('Ctrl Pts',(7.51676407774782,51.7624999998034,10.3459381770593));
#278915=CARTESIAN_POINT('Ctrl Pts',(9.83957192047903,51.9124999998028,7.14886745759543));
#278916=CARTESIAN_POINT('Ctrl Pts',(12.1623797632103,52.0624999998022,3.95179673813153));
#278917=CARTESIAN_POINT('Ctrl Pts',(12.1623797632103,52.2124999998016,-1.489461944703E-15));
#278918=CARTESIAN_POINT('Ctrl Pts',(12.1623797632103,52.362499999801,-3.95179673813154));
#278919=CARTESIAN_POINT('Ctrl Pts',(9.83957192047903,52.5124999998004,-7.14886745759543));
#278920=CARTESIAN_POINT('Ctrl Pts',(7.51676407774781,52.6624999997998,-10.3459381770593));
#278921=CARTESIAN_POINT('Ctrl Pts',(3.75838203887388,52.8124999997992,-11.5671105274575));
#278922=CARTESIAN_POINT('Ctrl Pts',(-4.37619473370168E-14,52.9624999997986,
-12.7882828778556));
#278923=CARTESIAN_POINT('Ctrl Pts',(-3.75838203887397,53.112499999798,-11.5671105274575));
#278924=CARTESIAN_POINT('Ctrl Pts',(-7.5167640777479,53.2624999997974,-10.3459381770593));
#278925=CARTESIAN_POINT('Ctrl Pts',(-9.83957192047912,53.4124999997968,
-7.14886745759543));
#278926=CARTESIAN_POINT('Ctrl Pts',(-12.1623797632103,53.5624999997962,
-3.95179673813153));
#278927=CARTESIAN_POINT('Ctrl Pts',(-12.1623797632103,53.7124999997956,
2.97892388940601E-15));
#278928=CARTESIAN_POINT('Ctrl Pts',(-12.1623797632103,53.862499999795,3.95179673813154));
#278929=CARTESIAN_POINT('Ctrl Pts',(-9.83957192047912,54.0124999997944,
7.14886745759543));
#278930=CARTESIAN_POINT('Ctrl Pts',(-7.5167640777479,54.1624999997938,10.3459381770593));
#278931=CARTESIAN_POINT('Ctrl Pts',(-3.75838203887397,54.3124999997932,
11.5671105274575));
#278932=CARTESIAN_POINT('Ctrl Pts',(-4.14935760342564E-14,54.4624999997926,
12.7882828778556));
#278933=CARTESIAN_POINT('Ctrl Pts',(3.75838203887389,54.612499999792,11.5671105274575));
#278934=CARTESIAN_POINT('Ctrl Pts',(7.51676407774782,54.7624999997914,10.3459381770593));
#278935=CARTESIAN_POINT('Ctrl Pts',(9.83957192047903,54.9124999997908,7.14886745759543));
#278936=CARTESIAN_POINT('Ctrl Pts',(12.1623797632103,55.0624999997902,3.95179673813153));
#278937=CARTESIAN_POINT('Ctrl Pts',(12.1623797632103,55.2124999997896,-1.489461944703E-15));
#278938=CARTESIAN_POINT('Ctrl Pts',(12.1623797632103,55.362499999789,-3.95179673813154));
#278939=CARTESIAN_POINT('Ctrl Pts',(9.83957192047903,55.5124999997884,-7.14886745759543));
#278940=CARTESIAN_POINT('Ctrl Pts',(7.51676407774781,55.6624999997878,-10.3459381770593));
#278941=CARTESIAN_POINT('Ctrl Pts',(3.75838203887388,55.8124999997872,-11.5671105274575));
#278942=CARTESIAN_POINT('Ctrl Pts',(-4.54896566086787E-14,55.9624999997866,
-12.7882828778556));
#278943=CARTESIAN_POINT('Ctrl Pts',(-3.75838203887397,56.112499999786,-11.5671105274575));
#278944=CARTESIAN_POINT('Ctrl Pts',(-7.5167640777479,56.2624999997854,-10.3459381770593));
#278945=CARTESIAN_POINT('Ctrl Pts',(-9.83957192047912,56.4124999997848,
-7.14886745759543));
#278946=CARTESIAN_POINT('Ctrl Pts',(-12.1623797632103,56.5624999997842,
-3.95179673813153));
#278947=CARTESIAN_POINT('Ctrl Pts',(-12.1623797632103,56.7124999997836,
2.97892388940601E-15));
#278948=CARTESIAN_POINT('Ctrl Pts',(-12.1623797632103,56.862499999783,3.95179673813154));
#278949=CARTESIAN_POINT('Ctrl Pts',(-9.83957192047912,57.0124999997824,
7.14886745759543));
#278950=CARTESIAN_POINT('Ctrl Pts',(-7.5167640777479,57.1624999997818,10.3459381770593));
#278951=CARTESIAN_POINT('Ctrl Pts',(-3.75838203887397,57.3124999997812,
11.5671105274575));
#278952=CARTESIAN_POINT('Ctrl Pts',(-4.32212853059182E-14,57.4624999997806,
12.7882828778556));
#278953=CARTESIAN_POINT('Ctrl Pts',(3.75838203887389,57.61249999978,11.5671105274575));
#278954=CARTESIAN_POINT('Ctrl Pts',(7.51676407774781,57.7624999997794,10.3459381770593));
#278955=CARTESIAN_POINT('Ctrl Pts',(9.83957192047903,57.9124999997788,7.14886745759543));
#278956=CARTESIAN_POINT('Ctrl Pts',(12.1623797632103,58.0624999997782,3.95179673813153));
#278957=CARTESIAN_POINT('Ctrl Pts',(12.1623797632102,58.2124999997776,-1.489461944703E-15));
#278958=CARTESIAN_POINT('Ctrl Pts',(12.1623797632102,58.362499999777,-3.95179673813154));
#278959=CARTESIAN_POINT('Ctrl Pts',(9.83957192047903,58.5124999997764,-7.14886745759543));
#278960=CARTESIAN_POINT('Ctrl Pts',(7.51676407774781,58.6624999997758,-10.3459381770593));
#278961=CARTESIAN_POINT('Ctrl Pts',(3.75838203887388,58.8124999997752,-11.5671105274575));
#278962=CARTESIAN_POINT('Ctrl Pts',(-4.72173658803405E-14,58.9624999997746,
-12.7882828778556));
#278963=CARTESIAN_POINT('Ctrl Pts',(-3.75838203887398,59.112499999774,-11.5671105274575));
#278964=CARTESIAN_POINT('Ctrl Pts',(-7.51676407774791,59.2624999997734,
-10.3459381770593));
#278965=CARTESIAN_POINT('Ctrl Pts',(-9.83957192047912,59.4124999997728,
-7.14886745759543));
#278966=CARTESIAN_POINT('Ctrl Pts',(-12.1623797632103,59.5624999997722,
-3.95179673813153));
#278967=CARTESIAN_POINT('Ctrl Pts',(-12.1623797632103,59.7124999997716,
2.97892388940601E-15));
#278968=CARTESIAN_POINT('Ctrl Pts',(-12.1623797632103,59.862499999771,3.95179673813154));
#278969=CARTESIAN_POINT('Ctrl Pts',(-9.83957192047912,60.0124999997704,
7.14886745759543));
#278970=CARTESIAN_POINT('Ctrl Pts',(-7.5167640777479,60.1624999997698,10.3459381770593));
#278971=CARTESIAN_POINT('Ctrl Pts',(-3.75838203887397,60.3124999997692,
11.5671105274575));
#278972=CARTESIAN_POINT('Ctrl Pts',(-4.49489945775801E-14,60.4624999997686,
12.7882828778556));
#278973=CARTESIAN_POINT('Ctrl Pts',(3.75838203887388,60.612499999768,11.5671105274575));
#278974=CARTESIAN_POINT('Ctrl Pts',(7.51676407774781,60.7624999997674,10.3459381770593));
#278975=CARTESIAN_POINT('Ctrl Pts',(9.83957192047903,60.9124999997668,7.14886745759543));
#278976=CARTESIAN_POINT('Ctrl Pts',(12.1623797632103,61.0624999997662,3.95179673813153));
#278977=CARTESIAN_POINT('Ctrl Pts',(12.1623797632102,61.2124999997656,-1.489461944703E-15));
#278978=CARTESIAN_POINT('Ctrl Pts',(12.1623797632102,61.362499999765,-3.95179673813154));
#278979=CARTESIAN_POINT('Ctrl Pts',(9.83957192047902,61.5124999997644,-7.14886745759543));
#278980=CARTESIAN_POINT('Ctrl Pts',(7.51676407774781,61.6624999997638,-10.3459381770593));
#278981=CARTESIAN_POINT('Ctrl Pts',(3.75838203887388,61.8124999997632,-11.5671105274575));
#278982=CARTESIAN_POINT('Ctrl Pts',(-4.89450751520023E-14,61.9624999997626,
-12.7882828778556));
#278983=CARTESIAN_POINT('Ctrl Pts',(-3.75838203887398,62.112499999762,-11.5671105274575));
#278984=CARTESIAN_POINT('Ctrl Pts',(-7.51676407774791,62.2624999997614,
-10.3459381770593));
#278985=CARTESIAN_POINT('Ctrl Pts',(-9.83957192047912,62.4124999997608,
-7.14886745759543));
#278986=CARTESIAN_POINT('Ctrl Pts',(-12.1623797632103,62.5624999997602,
-3.95179673813153));
#278987=CARTESIAN_POINT('Ctrl Pts',(-12.1623797632103,62.7124999997596,
2.97892388940601E-15));
#278988=CARTESIAN_POINT('Ctrl Pts',(-12.1623797632103,62.862499999759,3.95179673813154));
#278989=CARTESIAN_POINT('Ctrl Pts',(-9.83957192047912,63.0124999997584,
7.14886745759543));
#278990=CARTESIAN_POINT('Ctrl Pts',(-7.5167640777479,63.1624999997578,10.3459381770593));
#278991=CARTESIAN_POINT('Ctrl Pts',(-3.75838203887398,63.3124999997572,
11.5671105274575));
#278992=CARTESIAN_POINT('Ctrl Pts',(-4.66767038492419E-14,63.4624999997566,
12.7882828778556));
#278993=CARTESIAN_POINT('Ctrl Pts',(3.75838203887388,63.612499999756,11.5671105274575));
#278994=CARTESIAN_POINT('Ctrl Pts',(7.51676407774781,63.7624999997554,10.3459381770593));
#278995=CARTESIAN_POINT('Ctrl Pts',(9.83957192047903,63.9124999997548,7.14886745759543));
#278996=CARTESIAN_POINT('Ctrl Pts',(12.1623797632102,64.0624999997542,3.95179673813153));
#278997=CARTESIAN_POINT('Ctrl Pts',(12.1623797632102,64.2124999997536,-1.489461944703E-15));
#278998=CARTESIAN_POINT('Ctrl Pts',(12.1623797632102,64.362499999753,-3.95179673813154));
#278999=CARTESIAN_POINT('Ctrl Pts',(9.83957192047902,64.5124999997524,-7.14886745759543));
#279000=CARTESIAN_POINT('Ctrl Pts',(7.51676407774781,64.6624999997518,-10.3459381770593));
#279001=CARTESIAN_POINT('Ctrl Pts',(3.75838203887388,64.8124999997512,-11.5671105274575));
#279002=CARTESIAN_POINT('Ctrl Pts',(-5.06727844236642E-14,64.9624999997506,
-12.7882828778556));
#279003=CARTESIAN_POINT('Ctrl Pts',(-3.75838203887398,65.11249999975,-11.5671105274575));
#279004=CARTESIAN_POINT('Ctrl Pts',(-7.51676407774791,65.2624999997494,
-10.3459381770593));
#279005=CARTESIAN_POINT('Ctrl Pts',(-9.83957192047913,65.4124999997488,
-7.14886745759543));
#279006=CARTESIAN_POINT('Ctrl Pts',(-12.1623797632103,65.5624999997482,
-3.95179673813153));
#279007=CARTESIAN_POINT('Ctrl Pts',(-12.1623797632103,65.7124999997476,
2.97892388940601E-15));
#279008=CARTESIAN_POINT('Ctrl Pts',(-12.1623797632103,65.862499999747,3.95179673813154));
#279009=CARTESIAN_POINT('Ctrl Pts',(-9.83957192047912,66.0124999997464,
7.14886745759543));
#279010=CARTESIAN_POINT('Ctrl Pts',(-7.51676407774791,66.1624999997458,
10.3459381770593));
#279011=CARTESIAN_POINT('Ctrl Pts',(-3.75838203887398,66.3124999997452,
11.5671105274575));
#279012=CARTESIAN_POINT('Ctrl Pts',(-4.84044131209037E-14,66.4624999997446,
12.7882828778556));
#279013=CARTESIAN_POINT('Ctrl Pts',(3.75838203887388,66.612499999744,11.5671105274575));
#279014=CARTESIAN_POINT('Ctrl Pts',(7.51676407774781,66.7624999997434,10.3459381770593));
#279015=CARTESIAN_POINT('Ctrl Pts',(9.83957192047902,66.9124999997428,7.14886745759543));
#279016=CARTESIAN_POINT('Ctrl Pts',(12.1623797632102,67.0624999997422,3.95179673813153));
#279017=CARTESIAN_POINT('Ctrl Pts',(12.1623797632102,67.2124999997416,-1.489461944703E-15));
#279018=CARTESIAN_POINT('Ctrl Pts',(12.1623797632102,67.362499999741,-3.95179673813154));
#279019=CARTESIAN_POINT('Ctrl Pts',(9.83957192047902,67.5124999997404,-7.14886745759543));
#279020=CARTESIAN_POINT('Ctrl Pts',(7.51676407774781,67.6624999997398,-10.3459381770593));
#279021=CARTESIAN_POINT('Ctrl Pts',(3.75838203887388,67.8124999997392,-11.5671105274575));
#279022=CARTESIAN_POINT('Ctrl Pts',(-5.2400493695326E-14,67.9624999997386,
-12.7882828778556));
#279023=CARTESIAN_POINT('Ctrl Pts',(-3.75838203887398,68.112499999738,-11.5671105274575));
#279024=CARTESIAN_POINT('Ctrl Pts',(-7.51676407774791,68.2624999997374,
-10.3459381770593));
#279025=CARTESIAN_POINT('Ctrl Pts',(-9.83957192047913,68.4124999997368,
-7.14886745759543));
#279026=CARTESIAN_POINT('Ctrl Pts',(-12.1623797632103,68.5624999997362,
-3.95179673813153));
#279027=CARTESIAN_POINT('Ctrl Pts',(-12.1623797632103,68.7124999997356,
2.97892388940601E-15));
#279028=CARTESIAN_POINT('Ctrl Pts',(-12.1623797632103,68.862499999735,3.95179673813154));
#279029=CARTESIAN_POINT('Ctrl Pts',(-9.83957192047913,69.0124999997344,
7.14886745759543));
#279030=CARTESIAN_POINT('Ctrl Pts',(-7.51676407774791,69.1624999997338,
10.3459381770593));
#279031=CARTESIAN_POINT('Ctrl Pts',(-3.75838203887398,69.3124999997332,
11.5671105274575));
#279032=CARTESIAN_POINT('Ctrl Pts',(-5.01321223925656E-14,69.4624999997326,
12.7882828778556));
#279033=CARTESIAN_POINT('Ctrl Pts',(3.75838203887388,69.612499999732,11.5671105274575));
#279034=CARTESIAN_POINT('Ctrl Pts',(7.51676407774781,69.7624999997314,10.3459381770593));
#279035=CARTESIAN_POINT('Ctrl Pts',(9.83957192047902,69.9124999997308,7.14886745759543));
#279036=CARTESIAN_POINT('Ctrl Pts',(12.1623797632102,70.0624999997302,3.95179673813153));
#279037=CARTESIAN_POINT('Ctrl Pts',(12.1623797632102,70.2124999997296,-1.489461944703E-15));
#279038=CARTESIAN_POINT('Ctrl Pts',(12.1623797632102,70.362499999729,-3.95179673813154));
#279039=CARTESIAN_POINT('Ctrl Pts',(9.83957192047902,70.5124999997284,-7.14886745759543));
#279040=CARTESIAN_POINT('Ctrl Pts',(7.5167640777478,70.6624999997278,-10.3459381770593));
#279041=CARTESIAN_POINT('Ctrl Pts',(3.75838203887388,70.8124999997272,-11.5671105274575));
#279042=CARTESIAN_POINT('Ctrl Pts',(-5.41282029669879E-14,70.9624999997266,
-12.7882828778556));
#279043=CARTESIAN_POINT('Ctrl Pts',(-3.75838203887398,71.112499999726,-11.5671105274575));
#279044=CARTESIAN_POINT('Ctrl Pts',(-7.51676407774791,71.2624999997254,
-10.3459381770593));
#279045=CARTESIAN_POINT('Ctrl Pts',(-9.83957192047913,71.4124999997248,
-7.14886745759543));
#279046=CARTESIAN_POINT('Ctrl Pts',(-12.1623797632103,71.5624999997242,
-3.95179673813153));
#279047=CARTESIAN_POINT('Ctrl Pts',(-12.1623797632103,71.7124999997236,
2.97892388940601E-15));
#279048=CARTESIAN_POINT('Ctrl Pts',(-12.1623797632103,71.862499999723,3.95179673813154));
#279049=CARTESIAN_POINT('Ctrl Pts',(-9.83957192047913,72.0124999997224,
7.14886745759543));
#279050=CARTESIAN_POINT('Ctrl Pts',(-7.51676407774791,72.1624999997218,
10.3459381770593));
#279051=CARTESIAN_POINT('Ctrl Pts',(-3.75838203887398,72.3124999997212,
11.5671105274575));
#279052=CARTESIAN_POINT('Ctrl Pts',(-5.18598316642274E-14,72.4624999997206,
12.7882828778556));
#279053=CARTESIAN_POINT('Ctrl Pts',(3.75838203887388,72.61249999972,11.5671105274575));
#279054=CARTESIAN_POINT('Ctrl Pts',(7.51676407774781,72.7624999997194,10.3459381770593));
#279055=CARTESIAN_POINT('Ctrl Pts',(9.83957192047902,72.9124999997188,7.14886745759543));
#279056=CARTESIAN_POINT('Ctrl Pts',(12.1623797632102,73.0624999997182,3.95179673813153));
#279057=CARTESIAN_POINT('Ctrl Pts',(12.1623797632102,73.2124999997176,-1.489461944703E-15));
#279058=CARTESIAN_POINT('Ctrl Pts',(12.1623797632102,73.362499999717,-3.95179673813154));
#279059=CARTESIAN_POINT('Ctrl Pts',(9.83957192047902,73.5124999997164,-7.14886745759543));
#279060=CARTESIAN_POINT('Ctrl Pts',(7.5167640777478,73.6624999997158,-10.3459381770593));
#279061=CARTESIAN_POINT('Ctrl Pts',(3.75838203887387,73.8124999997152,-11.5671105274575));
#279062=CARTESIAN_POINT('Ctrl Pts',(-5.58559122386497E-14,73.9624999997146,
-12.7882828778556));
#279063=CARTESIAN_POINT('Ctrl Pts',(-3.75838203887398,74.112499999714,-11.5671105274575));
#279064=CARTESIAN_POINT('Ctrl Pts',(-7.51676407774791,74.2624999997134,
-10.3459381770593));
#279065=CARTESIAN_POINT('Ctrl Pts',(-9.83957192047913,74.4124999997128,
-7.14886745759543));
#279066=CARTESIAN_POINT('Ctrl Pts',(-12.1623797632103,74.5624999997122,
-3.95179673813153));
#279067=CARTESIAN_POINT('Ctrl Pts',(-12.1623797632103,74.7124999997116,
2.97892388940601E-15));
#279068=CARTESIAN_POINT('Ctrl Pts',(-12.1623797632103,74.862499999711,3.95179673813154));
#279069=CARTESIAN_POINT('Ctrl Pts',(-9.83957192047913,75.0124999997104,
7.14886745759543));
#279070=CARTESIAN_POINT('Ctrl Pts',(-7.51676407774791,75.1624999997098,
10.3459381770593));
#279071=CARTESIAN_POINT('Ctrl Pts',(-3.75838203887398,75.3124999997092,
11.5671105274575));
#279072=CARTESIAN_POINT('Ctrl Pts',(-5.35875409358893E-14,75.4624999997086,
12.7882828778556));
#279073=CARTESIAN_POINT('Ctrl Pts',(3.75838203887388,75.612499999708,11.5671105274575));
#279074=CARTESIAN_POINT('Ctrl Pts',(7.5167640777478,75.7624999997074,10.3459381770593));
#279075=CARTESIAN_POINT('Ctrl Pts',(9.83957192047902,75.9124999997068,7.14886745759543));
#279076=CARTESIAN_POINT('Ctrl Pts',(12.1623797632102,76.0624999997062,3.95179673813153));
#279077=CARTESIAN_POINT('Ctrl Pts',(12.1623797632102,76.2124999997056,-1.489461944703E-15));
#279078=CARTESIAN_POINT('Ctrl Pts',(12.1623797632102,76.362499999705,-3.95179673813154));
#279079=CARTESIAN_POINT('Ctrl Pts',(9.83957192047902,76.5124999997044,-7.14886745759543));
#279080=CARTESIAN_POINT('Ctrl Pts',(7.5167640777478,76.6624999997038,-10.3459381770593));
#279081=CARTESIAN_POINT('Ctrl Pts',(3.75838203887387,76.8124999997032,-11.5671105274575));
#279082=CARTESIAN_POINT('Ctrl Pts',(-5.75836215103115E-14,76.9624999997026,
-12.7882828778556));
#279083=CARTESIAN_POINT('Ctrl Pts',(-3.75838203887399,77.112499999702,-11.5671105274575));
#279084=CARTESIAN_POINT('Ctrl Pts',(-7.51676407774791,77.2624999997014,
-10.3459381770593));
#279085=CARTESIAN_POINT('Ctrl Pts',(-9.83957192047913,77.4124999997008,
-7.14886745759543));
#279086=CARTESIAN_POINT('Ctrl Pts',(-12.1623797632103,77.5624999997002,
-3.95179673813153));
#279087=CARTESIAN_POINT('Ctrl Pts',(-12.1623797632103,77.7124999996996,
2.97892388940601E-15));
#279088=CARTESIAN_POINT('Ctrl Pts',(-12.1623797632103,77.862499999699,3.95179673813154));
#279089=CARTESIAN_POINT('Ctrl Pts',(-9.83957192047913,78.0124999996984,
7.14886745759543));
#279090=CARTESIAN_POINT('Ctrl Pts',(-7.51676407774791,78.1624999996978,
10.3459381770593));
#279091=CARTESIAN_POINT('Ctrl Pts',(-3.75838203887398,78.3124999996972,
11.5671105274575));
#279092=CARTESIAN_POINT('Ctrl Pts',(-5.53152502075511E-14,78.4624999996966,
12.7882828778556));
#279093=CARTESIAN_POINT('Ctrl Pts',(3.75838203887387,78.612499999696,11.5671105274575));
#279094=CARTESIAN_POINT('Ctrl Pts',(7.5167640777478,78.7624999996954,10.3459381770593));
#279095=CARTESIAN_POINT('Ctrl Pts',(9.83957192047902,78.9124999996948,7.14886745759543));
#279096=CARTESIAN_POINT('Ctrl Pts',(12.1623797632102,79.0624999996942,3.95179673813153));
#279097=CARTESIAN_POINT('Ctrl Pts',(12.1623797632102,79.2124999996936,-1.489461944703E-15));
#279098=CARTESIAN_POINT('Ctrl Pts',(12.1623797632102,79.362499999693,-3.95179673813154));
#279099=CARTESIAN_POINT('Ctrl Pts',(9.83957192047902,79.5124999996924,-7.14886745759543));
#279100=CARTESIAN_POINT('Ctrl Pts',(7.5167640777478,79.6624999996918,-10.3459381770593));
#279101=CARTESIAN_POINT('Ctrl Pts',(3.75838203887387,79.8124999996912,-11.5671105274575));
#279102=CARTESIAN_POINT('Ctrl Pts',(-5.93113307819734E-14,79.9624999996906,
-12.7882828778556));
#279103=CARTESIAN_POINT('Ctrl Pts',(-3.75838203887399,80.11249999969,-11.5671105274575));
#279104=CARTESIAN_POINT('Ctrl Pts',(-7.51676407774791,80.2624999996894,
-10.3459381770593));
#279105=CARTESIAN_POINT('Ctrl Pts',(-9.83957192047913,80.4124999996888,
-7.14886745759543));
#279106=CARTESIAN_POINT('Ctrl Pts',(-12.1623797632104,80.5624999996882,
-3.95179673813153));
#279107=CARTESIAN_POINT('Ctrl Pts',(-12.1623797632104,80.7124999996876,
2.97892388940601E-15));
#279108=CARTESIAN_POINT('Ctrl Pts',(-12.1623797632104,80.862499999687,3.95179673813154));
#279109=CARTESIAN_POINT('Ctrl Pts',(-9.83957192047913,81.0124999996864,
7.14886745759543));
#279110=CARTESIAN_POINT('Ctrl Pts',(-7.51676407774791,81.1624999996858,
10.3459381770593));
#279111=CARTESIAN_POINT('Ctrl Pts',(-3.75838203887399,81.3124999996852,
11.5671105274575));
#279112=CARTESIAN_POINT('Ctrl Pts',(-5.70429594792129E-14,81.4624999996846,
12.7882828778556));
#279113=CARTESIAN_POINT('Ctrl Pts',(3.75838203887387,81.612499999684,11.5671105274575));
#279114=CARTESIAN_POINT('Ctrl Pts',(7.5167640777478,81.7624999996834,10.3459381770593));
#279115=CARTESIAN_POINT('Ctrl Pts',(9.83957192047902,81.9124999996828,7.14886745759543));
#279116=CARTESIAN_POINT('Ctrl Pts',(12.1623797632102,82.0624999996822,3.95179673813153));
#279117=CARTESIAN_POINT('Ctrl Pts',(12.1623797632102,82.2124999996816,-1.489461944703E-15));
#279118=CARTESIAN_POINT('Ctrl Pts',(12.1623797632102,82.362499999681,-3.95179673813154));
#279119=CARTESIAN_POINT('Ctrl Pts',(9.83957192047902,82.5124999996804,-7.14886745759543));
#279120=CARTESIAN_POINT('Ctrl Pts',(7.5167640777478,82.6624999996798,-10.3459381770593));
#279121=CARTESIAN_POINT('Ctrl Pts',(3.75838203887387,82.8124999996792,-11.5671105274575));
#279122=CARTESIAN_POINT('Ctrl Pts',(-6.10390400536352E-14,82.9624999996786,
-12.7882828778556));
#279123=CARTESIAN_POINT('Ctrl Pts',(-3.75838203887399,83.112499999678,-11.5671105274575));
#279124=CARTESIAN_POINT('Ctrl Pts',(-7.51676407774792,83.2624999996774,
-10.3459381770593));
#279125=CARTESIAN_POINT('Ctrl Pts',(-9.83957192047914,83.4124999996768,
-7.14886745759543));
#279126=CARTESIAN_POINT('Ctrl Pts',(-12.1623797632104,83.5624999996762,
-3.95179673813153));
#279127=CARTESIAN_POINT('Ctrl Pts',(-12.1623797632104,83.7124999996756,
2.97892388940601E-15));
#279128=CARTESIAN_POINT('Ctrl Pts',(-12.1623797632104,83.862499999675,3.95179673813154));
#279129=CARTESIAN_POINT('Ctrl Pts',(-9.83957192047913,84.0124999996744,
7.14886745759543));
#279130=CARTESIAN_POINT('Ctrl Pts',(-7.51676407774791,84.1624999996738,
10.3459381770593));
#279131=CARTESIAN_POINT('Ctrl Pts',(-3.75838203887399,84.3124999996732,
11.5671105274575));
#279132=CARTESIAN_POINT('Ctrl Pts',(-5.87706687508748E-14,84.4624999996726,
12.7882828778556));
#279133=CARTESIAN_POINT('Ctrl Pts',(3.75838203887387,84.6124999996721,11.5671105274575));
#279134=CARTESIAN_POINT('Ctrl Pts',(7.5167640777478,84.7624999996714,10.3459381770593));
#279135=CARTESIAN_POINT('Ctrl Pts',(9.83957192047902,84.9124999996708,7.14886745759543));
#279136=CARTESIAN_POINT('Ctrl Pts',(12.1623797632102,85.0624999996702,3.95179673813153));
#279137=CARTESIAN_POINT('Ctrl Pts',(12.1623797632102,85.2124999996696,-1.489461944703E-15));
#279138=CARTESIAN_POINT('Ctrl Pts',(12.1623797632102,85.362499999669,-3.95179673813154));
#279139=CARTESIAN_POINT('Ctrl Pts',(9.83957192047901,85.5124999996684,-7.14886745759543));
#279140=CARTESIAN_POINT('Ctrl Pts',(7.5167640777478,85.6624999996678,-10.3459381770593));
#279141=CARTESIAN_POINT('Ctrl Pts',(3.75838203887387,85.8124999996672,-11.5671105274575));
#279142=CARTESIAN_POINT('Ctrl Pts',(-6.27667493252971E-14,85.9624999996666,
-12.7882828778556));
#279143=CARTESIAN_POINT('Ctrl Pts',(-3.75838203887399,86.112499999666,-11.5671105274575));
#279144=CARTESIAN_POINT('Ctrl Pts',(-7.51676407774792,86.2624999996654,
-10.3459381770593));
#279145=CARTESIAN_POINT('Ctrl Pts',(-9.83957192047914,86.4124999996648,
-7.14886745759543));
#279146=CARTESIAN_POINT('Ctrl Pts',(-12.1623797632104,86.5624999996642,
-3.95179673813153));
#279147=CARTESIAN_POINT('Ctrl Pts',(-12.1623797632104,86.7124999996636,
2.97892388940601E-15));
#279148=CARTESIAN_POINT('Ctrl Pts',(-12.1623797632104,86.862499999663,3.95179673813154));
#279149=CARTESIAN_POINT('Ctrl Pts',(-9.83957192047914,87.0124999996624,
7.14886745759543));
#279150=CARTESIAN_POINT('Ctrl Pts',(-7.51676407774792,87.1624999996618,
10.3459381770593));
#279151=CARTESIAN_POINT('Ctrl Pts',(-3.75838203887399,87.3124999996612,
11.5671105274575));
#279152=CARTESIAN_POINT('Ctrl Pts',(-6.04983780225366E-14,87.4624999996606,
12.7882828778556));
#279153=CARTESIAN_POINT('Ctrl Pts',(3.75838203887387,87.61249999966,11.5671105274575));
#279154=CARTESIAN_POINT('Ctrl Pts',(7.5167640777478,87.7624999996594,10.3459381770593));
#279155=CARTESIAN_POINT('Ctrl Pts',(9.83957192047901,87.9124999996588,7.14886745759543));
#279156=CARTESIAN_POINT('Ctrl Pts',(12.1623797632102,88.0624999996582,3.95179673813153));
#279157=CARTESIAN_POINT('Ctrl Pts',(12.1623797632102,88.2124999996576,-1.489461944703E-15));
#279158=CARTESIAN_POINT('Ctrl Pts',(12.1623797632102,88.362499999657,-3.95179673813154));
#279159=CARTESIAN_POINT('Ctrl Pts',(9.83957192047901,88.5124999996564,-7.14886745759543));
#279160=CARTESIAN_POINT('Ctrl Pts',(7.51676407774779,88.6624999996558,-10.3459381770593));
#279161=CARTESIAN_POINT('Ctrl Pts',(3.75838203887386,88.8124999996552,-11.5671105274575));
#279162=CARTESIAN_POINT('Ctrl Pts',(-6.44944585969589E-14,88.9624999996546,
-12.7882828778556));
#279163=CARTESIAN_POINT('Ctrl Pts',(-3.75838203887399,89.112499999654,-11.5671105274575));
#279164=CARTESIAN_POINT('Ctrl Pts',(-7.51676407774792,89.2624999996534,
-10.3459381770593));
#279165=CARTESIAN_POINT('Ctrl Pts',(-9.83957192047914,89.4124999996528,
-7.14886745759543));
#279166=CARTESIAN_POINT('Ctrl Pts',(-12.1623797632104,89.5624999996522,
-3.95179673813153));
#279167=CARTESIAN_POINT('Ctrl Pts',(-12.1623797632104,89.7124999996516,
2.97892388940601E-15));
#279168=CARTESIAN_POINT('Ctrl Pts',(-12.1623797632104,89.862499999651,3.95179673813154));
#279169=CARTESIAN_POINT('Ctrl Pts',(-9.83957192047914,90.0124999996504,
7.14886745759543));
#279170=CARTESIAN_POINT('Ctrl Pts',(-7.51676407774792,90.1624999996498,
10.3459381770593));
#279171=CARTESIAN_POINT('Ctrl Pts',(-3.75838203887399,90.3124999996492,
11.5671105274575));
#279172=CARTESIAN_POINT('Ctrl Pts',(-6.22260872941985E-14,90.4624999996486,
12.7882828778556));
#279173=CARTESIAN_POINT('Ctrl Pts',(3.75838203887387,90.612499999648,11.5671105274575));
#279174=CARTESIAN_POINT('Ctrl Pts',(7.5167640777478,90.7624999996474,10.3459381770593));
#279175=CARTESIAN_POINT('Ctrl Pts',(9.83957192047901,90.9124999996468,7.14886745759543));
#279176=CARTESIAN_POINT('Ctrl Pts',(12.1623797632102,91.0624999996462,3.95179673813153));
#279177=CARTESIAN_POINT('Ctrl Pts',(12.1623797632102,91.2124999996456,-1.489461944703E-15));
#279178=CARTESIAN_POINT('Ctrl Pts',(12.1623797632102,91.362499999645,-3.95179673813154));
#279179=CARTESIAN_POINT('Ctrl Pts',(9.83957192047901,91.5124999996444,-7.14886745759543));
#279180=CARTESIAN_POINT('Ctrl Pts',(7.51676407774779,91.6624999996438,-10.3459381770593));
#279181=CARTESIAN_POINT('Ctrl Pts',(3.75838203887386,91.8124999996432,-11.5671105274575));
#279182=CARTESIAN_POINT('Ctrl Pts',(-6.62221678686207E-14,91.9624999996426,
-12.7882828778556));
#279183=CARTESIAN_POINT('Ctrl Pts',(-3.75838203887399,92.112499999642,-11.5671105274575));
#279184=CARTESIAN_POINT('Ctrl Pts',(-7.51676407774792,92.2624999996414,
-10.3459381770593));
#279185=CARTESIAN_POINT('Ctrl Pts',(-9.83957192047914,92.4124999996408,
-7.14886745759543));
#279186=CARTESIAN_POINT('Ctrl Pts',(-12.1623797632104,92.5624999996402,
-3.95179673813153));
#279187=CARTESIAN_POINT('Ctrl Pts',(-12.1623797632104,92.7124999996396,
2.97892388940601E-15));
#279188=CARTESIAN_POINT('Ctrl Pts',(-12.1623797632104,92.862499999639,3.95179673813154));
#279189=CARTESIAN_POINT('Ctrl Pts',(-9.83957192047914,93.0124999996384,
7.14886745759543));
#279190=CARTESIAN_POINT('Ctrl Pts',(-7.51676407774792,93.1624999996378,
10.3459381770593));
#279191=CARTESIAN_POINT('Ctrl Pts',(-3.75838203887399,93.3124999996372,
11.5671105274575));
#279192=CARTESIAN_POINT('Ctrl Pts',(-6.39537965658603E-14,93.4624999996366,
12.7882828778556));
#279193=CARTESIAN_POINT('Ctrl Pts',(3.75838203887386,93.612499999636,11.5671105274575));
#279194=CARTESIAN_POINT('Ctrl Pts',(7.51676407774779,93.7624999996354,10.3459381770593));
#279195=CARTESIAN_POINT('Ctrl Pts',(9.83957192047901,93.9124999996348,7.14886745759543));
#279196=CARTESIAN_POINT('Ctrl Pts',(12.1623797632102,94.0624999996342,3.95179673813153));
#279197=CARTESIAN_POINT('Ctrl Pts',(12.1623797632102,94.2124999996336,-1.489461944703E-15));
#279198=CARTESIAN_POINT('Ctrl Pts',(12.1623797632102,94.362499999633,-3.95179673813154));
#279199=CARTESIAN_POINT('Ctrl Pts',(9.83957192047901,94.5124999996324,-7.14886745759543));
#279200=CARTESIAN_POINT('Ctrl Pts',(7.51676407774779,94.6624999996318,-10.3459381770593));
#279201=CARTESIAN_POINT('Ctrl Pts',(3.75838203887386,94.8124999996312,-11.5671105274575));
#279202=CARTESIAN_POINT('Ctrl Pts',(-6.79498771402825E-14,94.9624999996306,
-12.7882828778556));
#279203=CARTESIAN_POINT('Ctrl Pts',(-3.758382038874,95.11249999963,-11.5671105274575));
#279204=CARTESIAN_POINT('Ctrl Pts',(-7.51676407774792,95.2624999996294,
-10.3459381770593));
#279205=CARTESIAN_POINT('Ctrl Pts',(-9.83957192047914,95.4124999996288,
-7.14886745759543));
#279206=CARTESIAN_POINT('Ctrl Pts',(-12.1623797632104,95.5624999996282,
-3.95179673813153));
#279207=CARTESIAN_POINT('Ctrl Pts',(-12.1623797632104,95.7124999996276,
2.97892388940601E-15));
#279208=CARTESIAN_POINT('Ctrl Pts',(-12.1623797632104,95.862499999627,3.95179673813154));
#279209=CARTESIAN_POINT('Ctrl Pts',(-9.83957192047914,96.0124999996264,
7.14886745759543));
#279210=CARTESIAN_POINT('Ctrl Pts',(-7.51676407774792,96.1624999996258,
10.3459381770593));
#279211=CARTESIAN_POINT('Ctrl Pts',(-3.75838203887399,96.3124999996252,
11.5671105274575));
#279212=CARTESIAN_POINT('Ctrl Pts',(-6.56815058375222E-14,96.4624999996246,
12.7882828778556));
#279213=CARTESIAN_POINT('Ctrl Pts',(3.75838203887386,96.612499999624,11.5671105274575));
#279214=CARTESIAN_POINT('Ctrl Pts',(7.51676407774779,96.7624999996234,10.3459381770593));
#279215=CARTESIAN_POINT('Ctrl Pts',(9.83957192047901,96.9124999996228,7.14886745759543));
#279216=CARTESIAN_POINT('Ctrl Pts',(12.1623797632102,97.0624999996222,3.95179673813153));
#279217=CARTESIAN_POINT('Ctrl Pts',(12.1623797632102,97.2124999996216,-1.489461944703E-15));
#279218=CARTESIAN_POINT('Ctrl Pts',(12.1623797632102,97.3624999996211,-3.95179673813154));
#279219=CARTESIAN_POINT('Ctrl Pts',(9.83957192047901,97.5124999996204,-7.14886745759543));
#279220=CARTESIAN_POINT('Ctrl Pts',(7.51676407774779,97.6624999996198,-10.3459381770593));
#279221=CARTESIAN_POINT('Ctrl Pts',(3.75838203887386,97.8124999996192,-11.5671105274575));
#279222=CARTESIAN_POINT('Ctrl Pts',(-6.96775864119444E-14,97.9624999996187,
-12.7882828778556));
#279223=CARTESIAN_POINT('Ctrl Pts',(-3.758382038874,98.112499999618,-11.5671105274575));
#279224=CARTESIAN_POINT('Ctrl Pts',(-7.51676407774793,98.2624999996174,
-10.3459381770593));
#279225=CARTESIAN_POINT('Ctrl Pts',(-9.83957192047914,98.4124999996168,
-7.14886745759543));
#279226=CARTESIAN_POINT('Ctrl Pts',(-12.1623797632104,98.5624999996162,
-3.95179673813153));
#279227=CARTESIAN_POINT('Ctrl Pts',(-12.1623797632104,98.7124999996156,
2.97892388940601E-15));
#279228=CARTESIAN_POINT('Ctrl Pts',(-12.1623797632104,98.862499999615,3.95179673813154));
#279229=CARTESIAN_POINT('Ctrl Pts',(-9.83957192047914,99.0124999996144,
7.14886745759543));
#279230=CARTESIAN_POINT('Ctrl Pts',(-7.51676407774792,99.1624999996138,
10.3459381770593));
#279231=CARTESIAN_POINT('Ctrl Pts',(-3.758382038874,99.3124999996132,11.5671105274575));
#279232=CARTESIAN_POINT('Ctrl Pts',(-6.7409215109184E-14,99.4624999996126,
12.7882828778556));
#279233=CARTESIAN_POINT('Ctrl Pts',(3.75838203887386,99.612499999612,11.5671105274575));
#279234=CARTESIAN_POINT('Ctrl Pts',(7.51676407774779,99.7624999996114,10.3459381770593));
#279235=CARTESIAN_POINT('Ctrl Pts',(9.83957192047901,99.9124999996108,7.14886745759543));
#279236=CARTESIAN_POINT('Ctrl Pts',(12.1623797632102,100.06249999961,3.95179673813153));
#279237=CARTESIAN_POINT('Ctrl Pts',(12.1623797632102,100.21249999961,-1.489461944703E-15));
#279238=CARTESIAN_POINT('Ctrl Pts',(12.1623797632102,100.362499999609,-3.95179673813154));
#279239=CARTESIAN_POINT('Ctrl Pts',(9.839571920479,100.512499999608,-7.14886745759543));
#279240=CARTESIAN_POINT('Ctrl Pts',(7.51676407774779,100.662499999608,-10.3459381770593));
#279241=CARTESIAN_POINT('Ctrl Pts',(3.75838203887386,100.812499999607,-11.5671105274575));
#279242=CARTESIAN_POINT('Ctrl Pts',(-7.14052956836063E-14,100.962499999607,
-12.7882828778556));
#279243=CARTESIAN_POINT('Ctrl Pts',(-3.758382038874,101.112499999606,-11.5671105274575));
#279244=CARTESIAN_POINT('Ctrl Pts',(-7.51676407774793,101.262499999605,
-10.3459381770593));
#279245=CARTESIAN_POINT('Ctrl Pts',(-9.83957192047915,101.412499999605,
-7.14886745759543));
#279246=CARTESIAN_POINT('Ctrl Pts',(-12.1623797632104,101.562499999604,
-3.95179673813153));
#279247=CARTESIAN_POINT('Ctrl Pts',(-12.1623797632104,101.712499999604,
2.97892388940601E-15));
#279248=CARTESIAN_POINT('Ctrl Pts',(-12.1623797632104,101.862499999603,
3.95179673813154));
#279249=CARTESIAN_POINT('Ctrl Pts',(-9.83957192047914,102.012499999602,
7.14886745759543));
#279250=CARTESIAN_POINT('Ctrl Pts',(-7.51676407774793,102.162499999602,
10.3459381770593));
#279251=CARTESIAN_POINT('Ctrl Pts',(-3.758382038874,102.312499999601,11.5671105274575));
#279252=CARTESIAN_POINT('Ctrl Pts',(-6.91369243808458E-14,102.462499999601,
12.7882828778556));
#279253=CARTESIAN_POINT('Ctrl Pts',(3.75838203887386,102.6124999996,11.5671105274575));
#279254=CARTESIAN_POINT('Ctrl Pts',(7.51676407774779,102.762499999599,10.3459381770593));
#279255=CARTESIAN_POINT('Ctrl Pts',(9.839571920479,102.912499999599,7.14886745759543));
#279256=CARTESIAN_POINT('Ctrl Pts',(12.1623797632102,103.062499999598,3.95179673813153));
#279257=CARTESIAN_POINT('Ctrl Pts',(12.1623797632102,103.212499999598,-1.489461944703E-15));
#279258=CARTESIAN_POINT('Ctrl Pts',(12.1623797632102,103.362499999597,-3.95179673813154));
#279259=CARTESIAN_POINT('Ctrl Pts',(9.839571920479,103.512499999596,-7.14886745759543));
#279260=CARTESIAN_POINT('Ctrl Pts',(7.51676407774779,103.662499999596,-10.3459381770593));
#279261=CARTESIAN_POINT('Ctrl Pts',(3.75838203887386,103.812499999595,-11.5671105274575));
#279262=CARTESIAN_POINT('Ctrl Pts',(-7.31330049552681E-14,103.962499999595,
-12.7882828778556));
#279263=CARTESIAN_POINT('Ctrl Pts',(-3.758382038874,104.112499999594,-11.5671105274575));
#279264=CARTESIAN_POINT('Ctrl Pts',(-7.51676407774793,104.262499999593,
-10.3459381770593));
#279265=CARTESIAN_POINT('Ctrl Pts',(-9.83957192047915,104.412499999593,
-7.14886745759543));
#279266=CARTESIAN_POINT('Ctrl Pts',(-12.1623797632104,104.562499999592,
-3.95179673813153));
#279267=CARTESIAN_POINT('Ctrl Pts',(-12.1623797632104,104.712499999592,
2.97892388940601E-15));
#279268=CARTESIAN_POINT('Ctrl Pts',(-12.1623797632104,104.862499999591,
3.95179673813154));
#279269=CARTESIAN_POINT('Ctrl Pts',(-9.83957192047915,105.01249999959,7.14886745759543));
#279270=CARTESIAN_POINT('Ctrl Pts',(-7.51676407774793,105.16249999959,10.3459381770593));
#279271=CARTESIAN_POINT('Ctrl Pts',(-3.758382038874,105.312499999589,11.5671105274575));
#279272=CARTESIAN_POINT('Ctrl Pts',(-7.08646336525076E-14,105.462499999589,
12.7882828778556));
#279273=CARTESIAN_POINT('Ctrl Pts',(3.75838203887386,105.612499999588,11.5671105274575));
#279274=CARTESIAN_POINT('Ctrl Pts',(7.51676407774779,105.762499999587,10.3459381770593));
#279275=CARTESIAN_POINT('Ctrl Pts',(9.839571920479,105.912499999587,7.14886745759543));
#279276=CARTESIAN_POINT('Ctrl Pts',(12.1623797632102,106.062499999586,3.95179673813153));
#279277=CARTESIAN_POINT('Ctrl Pts',(12.1623797632102,106.212499999586,-1.489461944703E-15));
#279278=CARTESIAN_POINT('Ctrl Pts',(12.1623797632102,106.362499999585,-3.95179673813154));
#279279=CARTESIAN_POINT('Ctrl Pts',(9.839571920479,106.512499999584,-7.14886745759543));
#279280=CARTESIAN_POINT('Ctrl Pts',(7.51676407774778,106.662499999584,-10.3459381770593));
#279281=CARTESIAN_POINT('Ctrl Pts',(3.75838203887385,106.812499999583,-11.5671105274575));
#279282=CARTESIAN_POINT('Ctrl Pts',(-7.48607142269299E-14,106.962499999583,
-12.7882828778556));
#279283=CARTESIAN_POINT('Ctrl Pts',(-3.758382038874,107.112499999582,-11.5671105274575));
#279284=CARTESIAN_POINT('Ctrl Pts',(-7.51676407774793,107.262499999581,
-10.3459381770593));
#279285=CARTESIAN_POINT('Ctrl Pts',(-9.83957192047915,107.412499999581,
-7.14886745759543));
#279286=CARTESIAN_POINT('Ctrl Pts',(-12.1623797632104,107.56249999958,-3.95179673813153));
#279287=CARTESIAN_POINT('Ctrl Pts',(-12.1623797632104,107.71249999958,2.97892388940601E-15));
#279288=CARTESIAN_POINT('Ctrl Pts',(-12.1623797632104,107.862499999579,
3.95179673813154));
#279289=CARTESIAN_POINT('Ctrl Pts',(-9.83957192047915,108.012499999578,
7.14886745759543));
#279290=CARTESIAN_POINT('Ctrl Pts',(-7.51676407774793,108.162499999578,
10.3459381770593));
#279291=CARTESIAN_POINT('Ctrl Pts',(-3.758382038874,108.312499999577,11.5671105274575));
#279292=CARTESIAN_POINT('Ctrl Pts',(-7.25923429241695E-14,108.462499999577,
12.7882828778556));
#279293=CARTESIAN_POINT('Ctrl Pts',(3.75838203887386,108.612499999576,11.5671105274575));
#279294=CARTESIAN_POINT('Ctrl Pts',(7.51676407774779,108.762499999575,10.3459381770593));
#279295=CARTESIAN_POINT('Ctrl Pts',(9.839571920479,108.912499999575,7.14886745759543));
#279296=CARTESIAN_POINT('Ctrl Pts',(12.1623797632102,109.062499999574,3.95179673813153));
#279297=CARTESIAN_POINT('Ctrl Pts',(12.1623797632102,109.212499999574,-1.489461944703E-15));
#279298=CARTESIAN_POINT('Ctrl Pts',(12.1623797632102,109.362499999573,-3.95179673813154));
#279299=CARTESIAN_POINT('Ctrl Pts',(9.839571920479,109.512499999572,-7.14886745759543));
#279300=CARTESIAN_POINT('Ctrl Pts',(7.51676407774778,109.662499999572,-10.3459381770593));
#279301=CARTESIAN_POINT('Ctrl Pts',(3.75838203887385,109.812499999571,-11.5671105274575));
#279302=CARTESIAN_POINT('Ctrl Pts',(-7.65884234985918E-14,109.962499999571,
-12.7882828778556));
#279303=CARTESIAN_POINT('Ctrl Pts',(-3.75838203887401,110.11249999957,-11.5671105274575));
#279304=CARTESIAN_POINT('Ctrl Pts',(-7.51676407774793,110.262499999569,
-10.3459381770593));
#279305=CARTESIAN_POINT('Ctrl Pts',(-9.83957192047915,110.412499999569,
-7.14886745759543));
#279306=CARTESIAN_POINT('Ctrl Pts',(-12.1623797632104,110.562499999568,
-3.95179673813153));
#279307=CARTESIAN_POINT('Ctrl Pts',(-12.1623797632104,110.712499999568,
2.97892388940601E-15));
#279308=CARTESIAN_POINT('Ctrl Pts',(-12.1623797632104,110.862499999567,
3.95179673813154));
#279309=CARTESIAN_POINT('Ctrl Pts',(-9.83957192047915,111.012499999566,
7.14886745759543));
#279310=CARTESIAN_POINT('Ctrl Pts',(-7.51676407774793,111.162499999566,
10.3459381770593));
#279311=CARTESIAN_POINT('Ctrl Pts',(-3.758382038874,111.312499999565,11.5671105274575));
#279312=CARTESIAN_POINT('Ctrl Pts',(-7.43200521958313E-14,111.462499999565,
12.7882828778556));
#279313=CARTESIAN_POINT('Ctrl Pts',(3.75838203887385,111.612499999564,11.5671105274575));
#279314=CARTESIAN_POINT('Ctrl Pts',(7.51676407774778,111.762499999563,10.3459381770593));
#279315=CARTESIAN_POINT('Ctrl Pts',(9.839571920479,111.912499999563,7.14886745759543));
#279316=CARTESIAN_POINT('Ctrl Pts',(12.1623797632102,112.062499999562,3.95179673813153));
#279317=CARTESIAN_POINT('Ctrl Pts',(12.1623797632102,112.212499999562,-1.489461944703E-15));
#279318=CARTESIAN_POINT('Ctrl Pts',(12.1623797632102,112.362499999561,-3.95179673813154));
#279319=CARTESIAN_POINT('Ctrl Pts',(9.839571920479,112.51249999956,-7.14886745759543));
#279320=CARTESIAN_POINT('Ctrl Pts',(7.51676407774778,112.66249999956,-10.3459381770593));
#279321=CARTESIAN_POINT('Ctrl Pts',(3.75838203887385,112.812499999559,-11.5671105274575));
#279322=CARTESIAN_POINT('Ctrl Pts',(-7.83161327702536E-14,112.962499999559,
-12.7882828778556));
#279323=CARTESIAN_POINT('Ctrl Pts',(-3.75838203887401,113.112499999558,
-11.5671105274575));
#279324=CARTESIAN_POINT('Ctrl Pts',(-7.51676407774793,113.262499999557,
-10.3459381770593));
#279325=CARTESIAN_POINT('Ctrl Pts',(-9.83957192047915,113.412499999557,
-7.14886745759543));
#279326=CARTESIAN_POINT('Ctrl Pts',(-12.1623797632104,113.562499999556,
-3.95179673813153));
#279327=CARTESIAN_POINT('Ctrl Pts',(-12.1623797632104,113.712499999556,
2.97892388940601E-15));
#279328=CARTESIAN_POINT('Ctrl Pts',(-12.1623797632104,113.862499999555,
3.95179673813154));
#279329=CARTESIAN_POINT('Ctrl Pts',(-9.83957192047915,114.012499999554,
7.14886745759543));
#279330=CARTESIAN_POINT('Ctrl Pts',(-7.51676407774793,114.162499999554,
10.3459381770593));
#279331=CARTESIAN_POINT('Ctrl Pts',(-3.758382038874,114.312499999553,11.5671105274575));
#279332=CARTESIAN_POINT('Ctrl Pts',(-7.60477614674932E-14,114.462499999553,
12.7882828778556));
#279333=CARTESIAN_POINT('Ctrl Pts',(3.75838203887385,114.612499999552,11.5671105274575));
#279334=CARTESIAN_POINT('Ctrl Pts',(7.51676407774778,114.762499999551,10.3459381770593));
#279335=CARTESIAN_POINT('Ctrl Pts',(9.839571920479,114.912499999551,7.14886745759543));
#279336=CARTESIAN_POINT('Ctrl Pts',(12.1623797632102,115.06249999955,3.95179673813153));
#279337=CARTESIAN_POINT('Ctrl Pts',(12.1623797632102,115.21249999955,-1.489461944703E-15));
#279338=CARTESIAN_POINT('Ctrl Pts',(12.1623797632102,115.362499999549,-3.95179673813154));
#279339=CARTESIAN_POINT('Ctrl Pts',(9.839571920479,115.512499999548,-7.14886745759543));
#279340=CARTESIAN_POINT('Ctrl Pts',(7.51676407774778,115.662499999548,-10.3459381770593));
#279341=CARTESIAN_POINT('Ctrl Pts',(3.75838203887385,115.812499999547,-11.5671105274575));
#279342=CARTESIAN_POINT('Ctrl Pts',(-8.00438420419154E-14,115.962499999547,
-12.7882828778556));
#279343=CARTESIAN_POINT('Ctrl Pts',(-3.75838203887401,116.112499999546,
-11.5671105274575));
#279344=CARTESIAN_POINT('Ctrl Pts',(-7.51676407774794,116.262499999545,
-10.3459381770593));
#279345=CARTESIAN_POINT('Ctrl Pts',(-9.83957192047916,116.412499999545,
-7.14886745759543));
#279346=CARTESIAN_POINT('Ctrl Pts',(-12.1623797632104,116.562499999544,
-3.95179673813153));
#279347=CARTESIAN_POINT('Ctrl Pts',(-12.1623797632104,116.712499999544,
2.97892388940601E-15));
#279348=CARTESIAN_POINT('Ctrl Pts',(-12.1623797632104,116.862499999543,
3.95179673813154));
#279349=CARTESIAN_POINT('Ctrl Pts',(-9.83957192047915,117.012499999542,
7.14886745759543));
#279350=CARTESIAN_POINT('Ctrl Pts',(-7.51676407774793,117.162499999542,
10.3459381770593));
#279351=CARTESIAN_POINT('Ctrl Pts',(-3.75838203887401,117.312499999541,
11.5671105274575));
#279352=CARTESIAN_POINT('Ctrl Pts',(-7.7775470739155E-14,117.462499999541,
12.7882828778556));
#279353=CARTESIAN_POINT('Ctrl Pts',(3.75838203887385,117.61249999954,11.5671105274575));
#279354=CARTESIAN_POINT('Ctrl Pts',(7.51676407774778,117.762499999539,10.3459381770593));
#279355=CARTESIAN_POINT('Ctrl Pts',(9.839571920479,117.912499999539,7.14886745759543));
#279356=CARTESIAN_POINT('Ctrl Pts',(12.1623797632102,118.062499999538,3.95179673813153));
#279357=CARTESIAN_POINT('Ctrl Pts',(12.1623797632102,118.212499999538,-1.489461944703E-15));
#279358=CARTESIAN_POINT('Ctrl Pts',(12.1623797632102,118.362499999537,-3.95179673813154));
#279359=CARTESIAN_POINT('Ctrl Pts',(9.83957192047899,118.512499999536,-7.14886745759543));
#279360=CARTESIAN_POINT('Ctrl Pts',(7.51676407774778,118.662499999536,-10.3459381770593));
#279361=CARTESIAN_POINT('Ctrl Pts',(3.75838203887385,118.812499999535,-11.5671105274575));
#279362=CARTESIAN_POINT('Ctrl Pts',(-8.17715513135773E-14,118.962499999535,
-12.7882828778556));
#279363=CARTESIAN_POINT('Ctrl Pts',(-3.75838203887401,119.112499999534,
-11.5671105274575));
#279364=CARTESIAN_POINT('Ctrl Pts',(-7.51676407774794,119.262499999533,
-10.3459381770593));
#279365=CARTESIAN_POINT('Ctrl Pts',(-9.83957192047916,119.412499999533,
-7.14886745759543));
#279366=CARTESIAN_POINT('Ctrl Pts',(-12.1623797632104,119.562499999532,
-3.95179673813153));
#279367=CARTESIAN_POINT('Ctrl Pts',(-12.1623797632104,119.712499999532,
2.97892388940601E-15));
#279368=CARTESIAN_POINT('Ctrl Pts',(-12.1623797632104,119.862499999531,
3.95179673813154));
#279369=CARTESIAN_POINT('Ctrl Pts',(-9.83957192047916,120.01249999953,7.14886745759543));
#279370=CARTESIAN_POINT('Ctrl Pts',(-7.51676407774794,120.16249999953,10.3459381770593));
#279371=CARTESIAN_POINT('Ctrl Pts',(-3.75838203887401,120.312499999529,
11.5671105274575));
#279372=CARTESIAN_POINT('Ctrl Pts',(-7.95031800108169E-14,120.462499999529,
12.7882828778556));
#279373=CARTESIAN_POINT('Ctrl Pts',(3.75838203887385,120.612499999528,11.5671105274575));
#279374=CARTESIAN_POINT('Ctrl Pts',(7.51676407774778,120.762499999527,10.3459381770593));
#279375=CARTESIAN_POINT('Ctrl Pts',(9.83957192047899,120.912499999527,7.14886745759543));
#279376=CARTESIAN_POINT('Ctrl Pts',(12.1623797632102,121.062499999526,3.95179673813153));
#279377=CARTESIAN_POINT('Ctrl Pts',(12.1623797632102,121.212499999526,-1.489461944703E-15));
#279378=CARTESIAN_POINT('Ctrl Pts',(12.1623797632102,121.362499999525,-3.95179673813154));
#279379=CARTESIAN_POINT('Ctrl Pts',(9.83957192047899,121.512499999524,-7.14886745759543));
#279380=CARTESIAN_POINT('Ctrl Pts',(7.51676407774777,121.662499999524,-10.3459381770593));
#279381=CARTESIAN_POINT('Ctrl Pts',(3.75838203887385,121.812499999523,-11.5671105274575));
#279382=CARTESIAN_POINT('Ctrl Pts',(-8.34992605852391E-14,121.962499999523,
-12.7882828778556));
#279383=CARTESIAN_POINT('Ctrl Pts',(-3.75838203887401,122.112499999522,
-11.5671105274575));
#279384=CARTESIAN_POINT('Ctrl Pts',(-7.51676407774794,122.262499999521,
-10.3459381770593));
#279385=CARTESIAN_POINT('Ctrl Pts',(-9.83957192047916,122.412499999521,
-7.14886745759543));
#279386=CARTESIAN_POINT('Ctrl Pts',(-12.1623797632104,122.56249999952,-3.95179673813153));
#279387=CARTESIAN_POINT('Ctrl Pts',(-12.1623797632104,122.71249999952,2.97892388940601E-15));
#279388=CARTESIAN_POINT('Ctrl Pts',(-12.1623797632104,122.862499999519,
3.95179673813154));
#279389=CARTESIAN_POINT('Ctrl Pts',(-9.83957192047916,123.012499999518,
7.14886745759543));
#279390=CARTESIAN_POINT('Ctrl Pts',(-7.51676407774794,123.162499999518,
10.3459381770593));
#279391=CARTESIAN_POINT('Ctrl Pts',(-3.75838203887401,123.312499999517,
11.5671105274575));
#279392=CARTESIAN_POINT('Ctrl Pts',(-8.12308892824787E-14,123.462499999517,
12.7882828778556));
#279393=CARTESIAN_POINT('Ctrl Pts',(3.75838203887385,123.612499999516,11.5671105274575));
#279394=CARTESIAN_POINT('Ctrl Pts',(7.51676407774778,123.762499999515,10.3459381770593));
#279395=CARTESIAN_POINT('Ctrl Pts',(9.83957192047899,123.912499999515,7.14886745759543));
#279396=CARTESIAN_POINT('Ctrl Pts',(12.1623797632102,124.062499999514,3.95179673813153));
#279397=CARTESIAN_POINT('Ctrl Pts',(12.1623797632102,124.212499999514,-1.489461944703E-15));
#279398=CARTESIAN_POINT('Ctrl Pts',(12.1623797632102,124.362499999513,-3.95179673813154));
#279399=CARTESIAN_POINT('Ctrl Pts',(9.83957192047899,124.512499999512,-7.14886745759543));
#279400=CARTESIAN_POINT('Ctrl Pts',(7.51676407774777,124.662499999512,-10.3459381770593));
#279401=CARTESIAN_POINT('Ctrl Pts',(3.75838203887384,124.812499999511,-11.5671105274575));
#279402=CARTESIAN_POINT('Ctrl Pts',(-8.52269698569009E-14,124.962499999511,
-12.7882828778556));
#279403=CARTESIAN_POINT('Ctrl Pts',(-3.75838203887401,125.11249999951,-11.5671105274575));
#279404=CARTESIAN_POINT('Ctrl Pts',(-7.51676407774794,125.262499999509,
-10.3459381770593));
#279405=CARTESIAN_POINT('Ctrl Pts',(-9.83957192047916,125.412499999509,
-7.14886745759543));
#279406=CARTESIAN_POINT('Ctrl Pts',(-12.1623797632104,125.562499999508,
-3.95179673813153));
#279407=CARTESIAN_POINT('Ctrl Pts',(-12.1623797632104,125.712499999508,
2.97892388940601E-15));
#279408=CARTESIAN_POINT('Ctrl Pts',(-12.1623797632104,125.862499999507,
3.95179673813154));
#279409=CARTESIAN_POINT('Ctrl Pts',(-9.83957192047916,126.012499999506,
7.14886745759543));
#279410=CARTESIAN_POINT('Ctrl Pts',(-7.51676407774794,126.162499999506,
10.3459381770593));
#279411=CARTESIAN_POINT('Ctrl Pts',(-3.75838203887401,126.312499999505,
11.5671105274575));
#279412=CARTESIAN_POINT('Ctrl Pts',(-8.29585985541405E-14,126.462499999505,
12.7882828778556));
#279413=CARTESIAN_POINT('Ctrl Pts',(3.75838203887385,126.612499999504,11.5671105274575));
#279414=CARTESIAN_POINT('Ctrl Pts',(7.51676407774777,126.762499999503,10.3459381770593));
#279415=CARTESIAN_POINT('Ctrl Pts',(9.83957192047899,126.912499999503,7.14886745759543));
#279416=CARTESIAN_POINT('Ctrl Pts',(12.1623797632102,127.062499999502,3.95179673813153));
#279417=CARTESIAN_POINT('Ctrl Pts',(12.1623797632102,127.212499999502,-1.489461944703E-15));
#279418=CARTESIAN_POINT('Ctrl Pts',(12.1623797632102,127.362499999501,-3.95179673813154));
#279419=CARTESIAN_POINT('Ctrl Pts',(9.83957192047899,127.5124999995,-7.14886745759543));
#279420=CARTESIAN_POINT('Ctrl Pts',(7.51676407774777,127.6624999995,-10.3459381770593));
#279421=CARTESIAN_POINT('Ctrl Pts',(3.75838203887384,127.812499999499,-11.5671105274575));
#279422=CARTESIAN_POINT('Ctrl Pts',(-8.69546791285628E-14,127.962499999499,
-12.7882828778556));
#279423=CARTESIAN_POINT('Ctrl Pts',(-3.75838203887402,128.112499999498,
-11.5671105274575));
#279424=CARTESIAN_POINT('Ctrl Pts',(-7.51676407774795,128.262499999497,
-10.3459381770593));
#279425=CARTESIAN_POINT('Ctrl Pts',(-9.83957192047916,128.412499999497,
-7.14886745759543));
#279426=CARTESIAN_POINT('Ctrl Pts',(-12.1623797632104,128.562499999496,
-3.95179673813153));
#279427=CARTESIAN_POINT('Ctrl Pts',(-12.1623797632104,128.712499999496,
2.97892388940601E-15));
#279428=CARTESIAN_POINT('Ctrl Pts',(-12.1623797632104,128.862499999495,
3.95179673813154));
#279429=CARTESIAN_POINT('Ctrl Pts',(-9.83957192047916,129.012499999494,
7.14886745759543));
#279430=CARTESIAN_POINT('Ctrl Pts',(-7.51676407774794,129.162499999494,
10.3459381770593));
#279431=CARTESIAN_POINT('Ctrl Pts',(-3.75838203887401,129.312499999493,
11.5671105274575));
#279432=CARTESIAN_POINT('Ctrl Pts',(-8.46863078258024E-14,129.462499999493,
12.7882828778556));
#279433=CARTESIAN_POINT('Ctrl Pts',(3.75838203887384,129.612499999492,11.5671105274575));
#279434=CARTESIAN_POINT('Ctrl Pts',(7.51676407774777,129.762499999491,10.3459381770593));
#279435=CARTESIAN_POINT('Ctrl Pts',(9.83957192047899,129.912499999491,7.14886745759543));
#279436=CARTESIAN_POINT('Ctrl Pts',(12.1623797632102,130.06249999949,3.95179673813153));
#279437=CARTESIAN_POINT('Ctrl Pts',(12.1623797632102,130.21249999949,-1.489461944703E-15));
#279438=CARTESIAN_POINT('Ctrl Pts',(12.1623797632102,130.362499999489,-3.95179673813154));
#279439=CARTESIAN_POINT('Ctrl Pts',(9.83957192047899,130.512499999488,-7.14886745759543));
#279440=CARTESIAN_POINT('Ctrl Pts',(7.51676407774777,130.662499999488,-10.3459381770593));
#279441=CARTESIAN_POINT('Ctrl Pts',(3.75838203887384,130.812499999487,-11.5671105274575));
#279442=CARTESIAN_POINT('Ctrl Pts',(-8.86823884002247E-14,130.962499999487,
-12.7882828778556));
#279443=CARTESIAN_POINT('Ctrl Pts',(-3.75838203887402,131.112499999486,
-11.5671105274575));
#279444=CARTESIAN_POINT('Ctrl Pts',(-7.51676407774795,131.262499999485,
-10.3459381770593));
#279445=CARTESIAN_POINT('Ctrl Pts',(-9.83957192047916,131.412499999485,
-7.14886745759543));
#279446=CARTESIAN_POINT('Ctrl Pts',(-12.1623797632104,131.562499999484,
-3.95179673813153));
#279447=CARTESIAN_POINT('Ctrl Pts',(-12.1623797632104,131.712499999484,
2.97892388940601E-15));
#279448=CARTESIAN_POINT('Ctrl Pts',(-12.1623797632104,131.862499999483,
3.95179673813154));
#279449=CARTESIAN_POINT('Ctrl Pts',(-9.83957192047916,132.012499999482,
7.14886745759543));
#279450=CARTESIAN_POINT('Ctrl Pts',(-7.51676407774795,132.162499999482,
10.3459381770593));
#279451=CARTESIAN_POINT('Ctrl Pts',(-3.75838203887402,132.312499999481,
11.5671105274575));
#279452=CARTESIAN_POINT('Ctrl Pts',(-8.64140170974642E-14,132.462499999481,
12.7882828778556));
#279453=CARTESIAN_POINT('Ctrl Pts',(3.75838203887384,132.61249999948,11.5671105274575));
#279454=CARTESIAN_POINT('Ctrl Pts',(7.51676407774777,132.762499999479,10.3459381770593));
#279455=CARTESIAN_POINT('Ctrl Pts',(9.83957192047899,132.912499999479,7.14886745759543));
#279456=CARTESIAN_POINT('Ctrl Pts',(12.1623797632102,133.062499999478,3.95179673813153));
#279457=CARTESIAN_POINT('Ctrl Pts',(12.1623797632102,133.212499999478,-1.489461944703E-15));
#279458=CARTESIAN_POINT('Ctrl Pts',(12.1623797632102,133.362499999477,-3.95179673813154));
#279459=CARTESIAN_POINT('Ctrl Pts',(9.83957192047898,133.512499999476,-7.14886745759543));
#279460=CARTESIAN_POINT('Ctrl Pts',(7.51676407774777,133.662499999476,-10.3459381770593));
#279461=CARTESIAN_POINT('Ctrl Pts',(3.75838203887384,133.812499999475,-11.5671105274575));
#279462=CARTESIAN_POINT('Ctrl Pts',(-9.04100976718865E-14,133.962499999475,
-12.7882828778556));
#279463=CARTESIAN_POINT('Ctrl Pts',(-3.75838203887402,134.112499999474,
-11.5671105274575));
#279464=CARTESIAN_POINT('Ctrl Pts',(-7.51676407774795,134.262499999473,
-10.3459381770593));
#279465=CARTESIAN_POINT('Ctrl Pts',(-9.83957192047917,134.412499999473,
-7.14886745759543));
#279466=CARTESIAN_POINT('Ctrl Pts',(-12.1623797632104,134.562499999472,
-3.95179673813153));
#279467=CARTESIAN_POINT('Ctrl Pts',(-12.1623797632104,134.712499999472,
2.97892388940601E-15));
#279468=CARTESIAN_POINT('Ctrl Pts',(-12.1623797632104,134.862499999471,
3.95179673813154));
#279469=CARTESIAN_POINT('Ctrl Pts',(-9.83957192047916,135.01249999947,7.14886745759543));
#279470=CARTESIAN_POINT('Ctrl Pts',(-7.51676407774795,135.16249999947,10.3459381770593));
#279471=CARTESIAN_POINT('Ctrl Pts',(-3.75838203887402,135.312499999469,
11.5671105274575));
#279472=CARTESIAN_POINT('Ctrl Pts',(-8.8141726369126E-14,135.462499999469,
12.7882828778556));
#279473=CARTESIAN_POINT('Ctrl Pts',(3.75838203887384,135.612499999468,11.5671105274575));
#279474=CARTESIAN_POINT('Ctrl Pts',(7.51676407774777,135.762499999467,10.3459381770593));
#279475=CARTESIAN_POINT('Ctrl Pts',(9.83957192047898,135.912499999467,7.14886745759543));
#279476=CARTESIAN_POINT('Ctrl Pts',(12.1623797632102,136.062499999466,3.95179673813153));
#279477=CARTESIAN_POINT('Ctrl Pts',(12.1623797632102,136.212499999466,-1.489461944703E-15));
#279478=CARTESIAN_POINT('Ctrl Pts',(12.1623797632102,136.362499999465,-3.95179673813154));
#279479=CARTESIAN_POINT('Ctrl Pts',(9.83957192047898,136.512499999464,-7.14886745759543));
#279480=CARTESIAN_POINT('Ctrl Pts',(7.51676407774776,136.662499999464,-10.3459381770593));
#279481=CARTESIAN_POINT('Ctrl Pts',(3.75838203887384,136.812499999463,-11.5671105274575));
#279482=CARTESIAN_POINT('Ctrl Pts',(-9.21378069435483E-14,136.962499999463,
-12.7882828778556));
#279483=CARTESIAN_POINT('Ctrl Pts',(-3.75838203887402,137.112499999462,
-11.5671105274575));
#279484=CARTESIAN_POINT('Ctrl Pts',(-7.51676407774795,137.262499999461,
-10.3459381770593));
#279485=CARTESIAN_POINT('Ctrl Pts',(-9.83957192047917,137.412499999461,
-7.14886745759543));
#279486=CARTESIAN_POINT('Ctrl Pts',(-12.1623797632104,137.56249999946,-3.95179673813153));
#279487=CARTESIAN_POINT('Ctrl Pts',(-12.1623797632104,137.71249999946,2.97892388940601E-15));
#279488=CARTESIAN_POINT('Ctrl Pts',(-12.1623797632104,137.862499999459,
3.95179673813154));
#279489=CARTESIAN_POINT('Ctrl Pts',(-9.83957192047917,138.012499999458,
7.14886745759543));
#279490=CARTESIAN_POINT('Ctrl Pts',(-7.51676407774795,138.162499999458,
10.3459381770593));
#279491=CARTESIAN_POINT('Ctrl Pts',(-3.75838203887402,138.312499999457,
11.5671105274575));
#279492=CARTESIAN_POINT('Ctrl Pts',(-8.98694356407879E-14,138.462499999457,
12.7882828778556));
#279493=CARTESIAN_POINT('Ctrl Pts',(3.75838203887384,138.612499999456,11.5671105274575));
#279494=CARTESIAN_POINT('Ctrl Pts',(7.51676407774777,138.762499999455,10.3459381770593));
#279495=CARTESIAN_POINT('Ctrl Pts',(9.83957192047898,138.912499999455,7.14886745759543));
#279496=CARTESIAN_POINT('Ctrl Pts',(12.1623797632102,139.062499999454,3.95179673813153));
#279497=CARTESIAN_POINT('Ctrl Pts',(12.1623797632102,139.212499999454,-1.489461944703E-15));
#279498=CARTESIAN_POINT('Ctrl Pts',(12.1623797632102,139.362499999453,-3.95179673813154));
#279499=CARTESIAN_POINT('Ctrl Pts',(9.83957192047898,139.512499999452,-7.14886745759543));
#279500=CARTESIAN_POINT('Ctrl Pts',(7.51676407774776,139.662499999452,-10.3459381770593));
#279501=CARTESIAN_POINT('Ctrl Pts',(3.75838203887384,139.812499999451,-11.5671105274575));
#279502=CARTESIAN_POINT('Ctrl Pts',(-9.38655162152102E-14,139.962499999451,
-12.7882828778556));
#279503=CARTESIAN_POINT('Ctrl Pts',(-3.75838203887402,140.11249999945,-11.5671105274575));
#279504=CARTESIAN_POINT('Ctrl Pts',(-7.51676407774795,140.262499999449,
-10.3459381770593));
#279505=CARTESIAN_POINT('Ctrl Pts',(-9.83957192047917,140.412499999449,
-7.14886745759543));
#279506=CARTESIAN_POINT('Ctrl Pts',(-12.1623797632104,140.562499999448,
-3.95179673813153));
#279507=CARTESIAN_POINT('Ctrl Pts',(-12.1623797632104,140.712499999448,
2.97892388940601E-15));
#279508=CARTESIAN_POINT('Ctrl Pts',(-12.1623797632104,140.862499999447,
3.95179673813154));
#279509=CARTESIAN_POINT('Ctrl Pts',(-9.83957192047917,141.012499999446,
7.14886745759543));
#279510=CARTESIAN_POINT('Ctrl Pts',(-7.51676407774795,141.162499999446,
10.3459381770593));
#279511=CARTESIAN_POINT('Ctrl Pts',(-3.75838203887402,141.312499999445,
11.5671105274575));
#279512=CARTESIAN_POINT('Ctrl Pts',(-9.15971449124498E-14,141.462499999445,
12.7882828778556));
#279513=CARTESIAN_POINT('Ctrl Pts',(3.75838203887384,141.612499999444,11.5671105274575));
#279514=CARTESIAN_POINT('Ctrl Pts',(7.51676407774776,141.762499999443,10.3459381770593));
#279515=CARTESIAN_POINT('Ctrl Pts',(9.83957192047898,141.912499999443,7.14886745759543));
#279516=CARTESIAN_POINT('Ctrl Pts',(12.1623797632102,142.062499999442,3.95179673813153));
#279517=CARTESIAN_POINT('Ctrl Pts',(12.1623797632102,142.212499999442,-1.489461944703E-15));
#279518=CARTESIAN_POINT('Ctrl Pts',(12.1623797632102,142.362499999441,-3.95179673813154));
#279519=CARTESIAN_POINT('Ctrl Pts',(9.83957192047898,142.51249999944,-7.14886745759543));
#279520=CARTESIAN_POINT('Ctrl Pts',(7.51676407774776,142.66249999944,-10.3459381770593));
#279521=CARTESIAN_POINT('Ctrl Pts',(3.75838203887383,142.812499999439,-11.5671105274575));
#279522=CARTESIAN_POINT('Ctrl Pts',(-9.5593225486872E-14,142.962499999439,
-12.7882828778556));
#279523=CARTESIAN_POINT('Ctrl Pts',(-3.75838203887402,143.112499999438,
-11.5671105274575));
#279524=CARTESIAN_POINT('Ctrl Pts',(-7.51676407774795,143.262499999437,
-10.3459381770593));
#279525=CARTESIAN_POINT('Ctrl Pts',(-9.83957192047917,143.412499999437,
-7.14886745759543));
#279526=CARTESIAN_POINT('Ctrl Pts',(-12.1623797632104,143.562499999436,
-3.95179673813153));
#279527=CARTESIAN_POINT('Ctrl Pts',(-12.1623797632104,143.712499999436,
2.97892388940601E-15));
#279528=CARTESIAN_POINT('Ctrl Pts',(-12.1623797632104,143.862499999435,
3.95179673813154));
#279529=CARTESIAN_POINT('Ctrl Pts',(-9.83957192047917,144.012499999434,
7.14886745759543));
#279530=CARTESIAN_POINT('Ctrl Pts',(-7.51676407774795,144.162499999434,
10.3459381770593));
#279531=CARTESIAN_POINT('Ctrl Pts',(-3.75838203887402,144.312499999433,
11.5671105274575));
#279532=CARTESIAN_POINT('Ctrl Pts',(-9.33248541841116E-14,144.462499999433,
12.7882828778556));
#279533=CARTESIAN_POINT('Ctrl Pts',(3.75838203887384,144.612499999432,11.5671105274575));
#279534=CARTESIAN_POINT('Ctrl Pts',(7.51676407774776,144.762499999431,10.3459381770593));
#279535=CARTESIAN_POINT('Ctrl Pts',(9.83957192047898,144.912499999431,7.14886745759543));
#279536=CARTESIAN_POINT('Ctrl Pts',(12.1623797632102,145.06249999943,3.95179673813153));
#279537=CARTESIAN_POINT('Ctrl Pts',(12.1623797632102,145.21249999943,-1.489461944703E-15));
#279538=CARTESIAN_POINT('Ctrl Pts',(12.1623797632102,145.362499999429,-3.95179673813154));
#279539=CARTESIAN_POINT('Ctrl Pts',(9.83957192047898,145.512499999428,-7.14886745759543));
#279540=CARTESIAN_POINT('Ctrl Pts',(7.51676407774776,145.662499999428,-10.3459381770593));
#279541=CARTESIAN_POINT('Ctrl Pts',(3.75838203887383,145.812499999427,-11.5671105274575));
#279542=CARTESIAN_POINT('Ctrl Pts',(-9.73209347585338E-14,145.962499999427,
-12.7882828778556));
#279543=CARTESIAN_POINT('Ctrl Pts',(-3.75838203887403,146.112499999426,
-11.5671105274575));
#279544=CARTESIAN_POINT('Ctrl Pts',(-7.51676407774795,146.262499999425,
-10.3459381770593));
#279545=CARTESIAN_POINT('Ctrl Pts',(-9.83957192047917,146.412499999425,
-7.14886745759543));
#279546=CARTESIAN_POINT('Ctrl Pts',(-12.1623797632104,146.562499999424,
-3.95179673813153));
#279547=CARTESIAN_POINT('Ctrl Pts',(-12.1623797632104,146.712499999424,
2.97892388940601E-15));
#279548=CARTESIAN_POINT('Ctrl Pts',(-12.1623797632104,146.862499999423,
3.95179673813154));
#279549=CARTESIAN_POINT('Ctrl Pts',(-9.83957192047917,147.012499999422,
7.14886745759543));
#279550=CARTESIAN_POINT('Ctrl Pts',(-7.51676407774795,147.162499999422,
10.3459381770593));
#279551=CARTESIAN_POINT('Ctrl Pts',(-3.75838203887402,147.312499999421,
11.5671105274575));
#279552=CARTESIAN_POINT('Ctrl Pts',(-9.50525634557734E-14,147.462499999421,
12.7882828778556));
#279553=CARTESIAN_POINT('Ctrl Pts',(3.75838203887383,147.61249999942,11.5671105274575));
#279554=CARTESIAN_POINT('Ctrl Pts',(7.51676407774776,147.762499999419,10.3459381770593));
#279555=CARTESIAN_POINT('Ctrl Pts',(9.83957192047898,147.912499999419,7.14886745759543));
#279556=CARTESIAN_POINT('Ctrl Pts',(12.1623797632102,148.062499999418,3.95179673813153));
#279557=CARTESIAN_POINT('Ctrl Pts',(12.1623797632102,148.212499999418,-1.489461944703E-15));
#279558=CARTESIAN_POINT('Ctrl Pts',(12.1623797632102,148.362499999417,-3.95179673813154));
#279559=CARTESIAN_POINT('Ctrl Pts',(9.83957192047898,148.512499999416,-7.14886745759543));
#279560=CARTESIAN_POINT('Ctrl Pts',(7.51676407774776,148.662499999416,-10.3459381770593));
#279561=CARTESIAN_POINT('Ctrl Pts',(3.75838203887383,148.812499999415,-11.5671105274575));
#279562=CARTESIAN_POINT('Ctrl Pts',(-9.90486440301957E-14,148.962499999415,
-12.7882828778556));
#279563=CARTESIAN_POINT('Ctrl Pts',(-3.75838203887403,149.112499999414,
-11.5671105274575));
#279564=CARTESIAN_POINT('Ctrl Pts',(-7.51676407774795,149.262499999413,
-10.3459381770593));
#279565=CARTESIAN_POINT('Ctrl Pts',(-9.83957192047917,149.412499999413,
-7.14886745759543));
#279566=CARTESIAN_POINT('Ctrl Pts',(-12.1623797632104,149.562499999412,
-3.95179673813153));
#279567=CARTESIAN_POINT('Ctrl Pts',(-12.1623797632104,149.712499999412,
2.97892388940601E-15));
#279568=CARTESIAN_POINT('Ctrl Pts',(-12.1623797632104,149.862499999411,
3.95179673813154));
#279569=CARTESIAN_POINT('Ctrl Pts',(-9.83957192047917,150.01249999941,7.14886745759543));
#279570=CARTESIAN_POINT('Ctrl Pts',(-7.51676407774795,150.16249999941,10.3459381770593));
#279571=CARTESIAN_POINT('Ctrl Pts',(-3.75838203887403,150.312499999409,
11.5671105274575));
#279572=CARTESIAN_POINT('Ctrl Pts',(-9.67802727274353E-14,150.462499999409,
12.7882828778556));
#279573=CARTESIAN_POINT('Ctrl Pts',(3.75838203887383,150.612499999408,11.5671105274575));
#279574=CARTESIAN_POINT('Ctrl Pts',(7.51676407774776,150.762499999407,10.3459381770593));
#279575=CARTESIAN_POINT('Ctrl Pts',(9.83957192047898,150.912499999407,7.14886745759543));
#279576=CARTESIAN_POINT('Ctrl Pts',(12.1623797632102,151.062499999406,3.95179673813153));
#279577=CARTESIAN_POINT('Ctrl Pts',(12.1623797632102,151.212499999406,-1.489461944703E-15));
#279578=CARTESIAN_POINT('Ctrl Pts',(12.1623797632102,151.362499999405,-3.95179673813154));
#279579=CARTESIAN_POINT('Ctrl Pts',(9.83957192047897,151.512499999404,-7.14886745759543));
#279580=CARTESIAN_POINT('Ctrl Pts',(7.51676407774776,151.662499999404,-10.3459381770593));
#279581=CARTESIAN_POINT('Ctrl Pts',(3.75838203887383,151.812499999403,-11.5671105274575));
#279582=CARTESIAN_POINT('Ctrl Pts',(-1.00776353301858E-13,151.962499999403,
-12.7882828778556));
#279583=CARTESIAN_POINT('Ctrl Pts',(-3.75838203887403,152.112499999402,
-11.5671105274575));
#279584=CARTESIAN_POINT('Ctrl Pts',(-10.0514278971316,-2.0687413718495,
2.46188980021652E-15));
#279585=CARTESIAN_POINT('Ctrl Pts',(-10.0514278971316,-1.9187413718501,
3.26590689904296));
#279586=CARTESIAN_POINT('Ctrl Pts',(-8.13177598651391,-1.7687413718507,
5.9080810824151));
#279587=CARTESIAN_POINT('Ctrl Pts',(-6.21212407589621,-1.61874137185129,
8.55025526578723));
#279588=CARTESIAN_POINT('Ctrl Pts',(-3.10606203794811,-1.46874137185189,
9.55947599963789));
#279589=CARTESIAN_POINT('Ctrl Pts',(-9.77671809333146E-15,-1.31874137185249,
10.5686967334885));
#279590=CARTESIAN_POINT('Ctrl Pts',(3.10606203794809,-1.16874137185309,
9.55947599963789));
#279591=CARTESIAN_POINT('Ctrl Pts',(6.21212407589619,-1.01874137185369,
8.55025526578723));
#279592=CARTESIAN_POINT('Ctrl Pts',(8.13177598651388,-0.868741371854286,
5.90808108241509));
#279593=CARTESIAN_POINT('Ctrl Pts',(10.0514278971316,-0.718741371854885,
3.26590689904295));
#279594=CARTESIAN_POINT('Ctrl Pts',(10.0514278971316,-0.568741371855485,
-1.23094490010826E-15));
#279595=CARTESIAN_POINT('Ctrl Pts',(10.0514278971316,-0.418741371856085,
-3.26590689904296));
#279596=CARTESIAN_POINT('Ctrl Pts',(8.13177598651388,-0.268741371856686,
-5.9080810824151));
#279597=CARTESIAN_POINT('Ctrl Pts',(6.21212407589619,-0.118741371857287,
-8.55025526578723));
#279598=CARTESIAN_POINT('Ctrl Pts',(3.10606203794809,0.0312586281421111,
-9.55947599963789));
#279599=CARTESIAN_POINT('Ctrl Pts',(-1.32291568543275E-14,0.181258628141509,
-10.5686967334885));
#279600=CARTESIAN_POINT('Ctrl Pts',(-3.10606203794812,0.331258628140907,
-9.55947599963789));
#279601=CARTESIAN_POINT('Ctrl Pts',(-6.21212407589621,0.481258628140306,
-8.55025526578723));
#279602=CARTESIAN_POINT('Ctrl Pts',(-8.13177598651391,0.631258628139705,
-5.90808108241509));
#279603=CARTESIAN_POINT('Ctrl Pts',(-10.0514278971316,0.781258628139103,
-3.26590689904296));
#279604=CARTESIAN_POINT('Ctrl Pts',(-10.0514278971316,0.931258628138503,
2.46188980021652E-15));
#279605=CARTESIAN_POINT('Ctrl Pts',(-10.0514278971316,1.0812586281379,3.26590689904296));
#279606=CARTESIAN_POINT('Ctrl Pts',(-8.13177598651391,1.2312586281373,5.9080810824151));
#279607=CARTESIAN_POINT('Ctrl Pts',(-6.21212407589621,1.38125862813671,
8.55025526578723));
#279608=CARTESIAN_POINT('Ctrl Pts',(-3.10606203794811,1.53125862813611,
9.55947599963789));
#279609=CARTESIAN_POINT('Ctrl Pts',(-1.15044273649933E-14,1.68125862813551,
10.5686967334885));
#279610=CARTESIAN_POINT('Ctrl Pts',(3.10606203794809,1.83125862813491,9.55947599963789));
#279611=CARTESIAN_POINT('Ctrl Pts',(6.21212407589619,1.98125862813431,8.55025526578723));
#279612=CARTESIAN_POINT('Ctrl Pts',(8.13177598651388,2.13125862813371,5.90808108241509));
#279613=CARTESIAN_POINT('Ctrl Pts',(10.0514278971316,2.28125862813311,3.26590689904295));
#279614=CARTESIAN_POINT('Ctrl Pts',(10.0514278971316,2.43125862813252,-1.23094490010826E-15));
#279615=CARTESIAN_POINT('Ctrl Pts',(10.0514278971316,2.58125862813192,-3.26590689904296));
#279616=CARTESIAN_POINT('Ctrl Pts',(8.13177598651388,2.73125862813131,-5.9080810824151));
#279617=CARTESIAN_POINT('Ctrl Pts',(6.21212407589619,2.88125862813071,-8.55025526578723));
#279618=CARTESIAN_POINT('Ctrl Pts',(3.10606203794809,3.03125862813011,-9.55947599963789));
#279619=CARTESIAN_POINT('Ctrl Pts',(-1.49568661259894E-14,3.18125862812951,
-10.5686967334885));
#279620=CARTESIAN_POINT('Ctrl Pts',(-3.10606203794812,3.33125862812891,
-9.55947599963789));
#279621=CARTESIAN_POINT('Ctrl Pts',(-6.21212407589622,3.48125862812831,
-8.55025526578723));
#279622=CARTESIAN_POINT('Ctrl Pts',(-8.13177598651391,3.6312586281277,-5.90808108241509));
#279623=CARTESIAN_POINT('Ctrl Pts',(-10.0514278971316,3.7812586281271,-3.26590689904296));
#279624=CARTESIAN_POINT('Ctrl Pts',(-10.0514278971316,3.9312586281265,2.46188980021652E-15));
#279625=CARTESIAN_POINT('Ctrl Pts',(-10.0514278971316,4.0812586281259,3.26590689904296));
#279626=CARTESIAN_POINT('Ctrl Pts',(-8.13177598651391,4.2312586281253,5.9080810824151));
#279627=CARTESIAN_POINT('Ctrl Pts',(-6.21212407589621,4.38125862812471,
8.55025526578723));
#279628=CARTESIAN_POINT('Ctrl Pts',(-3.10606203794812,4.53125862812411,
9.55947599963789));
#279629=CARTESIAN_POINT('Ctrl Pts',(-1.32321366366551E-14,4.68125862812351,
10.5686967334885));
#279630=CARTESIAN_POINT('Ctrl Pts',(3.10606203794809,4.83125862812291,9.55947599963789));
#279631=CARTESIAN_POINT('Ctrl Pts',(6.21212407589619,4.98125862812231,8.55025526578723));
#279632=CARTESIAN_POINT('Ctrl Pts',(8.13177598651388,5.13125862812171,5.90808108241509));
#279633=CARTESIAN_POINT('Ctrl Pts',(10.0514278971316,5.28125862812112,3.26590689904295));
#279634=CARTESIAN_POINT('Ctrl Pts',(10.0514278971316,5.43125862812051,-1.23094490010826E-15));
#279635=CARTESIAN_POINT('Ctrl Pts',(10.0514278971316,5.58125862811991,-3.26590689904296));
#279636=CARTESIAN_POINT('Ctrl Pts',(8.13177598651388,5.73125862811931,-5.9080810824151));
#279637=CARTESIAN_POINT('Ctrl Pts',(6.21212407589619,5.88125862811871,-8.55025526578723));
#279638=CARTESIAN_POINT('Ctrl Pts',(3.10606203794809,6.03125862811811,-9.55947599963789));
#279639=CARTESIAN_POINT('Ctrl Pts',(-1.66845753976512E-14,6.18125862811751,
-10.5686967334885));
#279640=CARTESIAN_POINT('Ctrl Pts',(-3.10606203794812,6.33125862811691,
-9.55947599963789));
#279641=CARTESIAN_POINT('Ctrl Pts',(-6.21212407589622,6.48125862811631,
-8.55025526578723));
#279642=CARTESIAN_POINT('Ctrl Pts',(-8.13177598651391,6.63125862811571,
-5.90808108241509));
#279643=CARTESIAN_POINT('Ctrl Pts',(-10.0514278971316,6.7812586281151,-3.26590689904296));
#279644=CARTESIAN_POINT('Ctrl Pts',(-10.0514278971316,6.9312586281145,2.46188980021652E-15));
#279645=CARTESIAN_POINT('Ctrl Pts',(-10.0514278971316,7.0812586281139,3.26590689904296));
#279646=CARTESIAN_POINT('Ctrl Pts',(-8.13177598651391,7.2312586281133,5.9080810824151));
#279647=CARTESIAN_POINT('Ctrl Pts',(-6.21212407589622,7.38125862811271,
8.55025526578723));
#279648=CARTESIAN_POINT('Ctrl Pts',(-3.10606203794812,7.53125862811211,
9.55947599963789));
#279649=CARTESIAN_POINT('Ctrl Pts',(-1.4959845908317E-14,7.68125862811151,
10.5686967334885));
#279650=CARTESIAN_POINT('Ctrl Pts',(3.10606203794809,7.83125862811091,9.55947599963789));
#279651=CARTESIAN_POINT('Ctrl Pts',(6.21212407589619,7.98125862811031,8.55025526578723));
#279652=CARTESIAN_POINT('Ctrl Pts',(8.13177598651388,8.13125862810971,5.90808108241509));
#279653=CARTESIAN_POINT('Ctrl Pts',(10.0514278971316,8.28125862810912,3.26590689904295));
#279654=CARTESIAN_POINT('Ctrl Pts',(10.0514278971316,8.43125862810852,-1.23094490010826E-15));
#279655=CARTESIAN_POINT('Ctrl Pts',(10.0514278971316,8.58125862810792,-3.26590689904296));
#279656=CARTESIAN_POINT('Ctrl Pts',(8.13177598651388,8.73125862810731,-5.9080810824151));
#279657=CARTESIAN_POINT('Ctrl Pts',(6.21212407589618,8.88125862810671,-8.55025526578723));
#279658=CARTESIAN_POINT('Ctrl Pts',(3.10606203794808,9.03125862810611,-9.55947599963789));
#279659=CARTESIAN_POINT('Ctrl Pts',(-1.84122846693131E-14,9.18125862810551,
-10.5686967334885));
#279660=CARTESIAN_POINT('Ctrl Pts',(-3.10606203794812,9.33125862810491,
-9.55947599963789));
#279661=CARTESIAN_POINT('Ctrl Pts',(-6.21212407589622,9.48125862810431,
-8.55025526578723));
#279662=CARTESIAN_POINT('Ctrl Pts',(-8.13177598651391,9.6312586281037,-5.90808108241509));
#279663=CARTESIAN_POINT('Ctrl Pts',(-10.0514278971316,9.7812586281031,-3.26590689904296));
#279664=CARTESIAN_POINT('Ctrl Pts',(-10.0514278971316,9.9312586281025,2.46188980021652E-15));
#279665=CARTESIAN_POINT('Ctrl Pts',(-10.0514278971316,10.0812586281019,
3.26590689904296));
#279666=CARTESIAN_POINT('Ctrl Pts',(-8.13177598651391,10.2312586281013,
5.9080810824151));
#279667=CARTESIAN_POINT('Ctrl Pts',(-6.21212407589622,10.3812586281007,
8.55025526578723));
#279668=CARTESIAN_POINT('Ctrl Pts',(-3.10606203794812,10.5312586281001,
9.55947599963789));
#279669=CARTESIAN_POINT('Ctrl Pts',(-1.66875551799788E-14,10.6812586280995,
10.5686967334885));
#279670=CARTESIAN_POINT('Ctrl Pts',(3.10606203794808,10.8312586280989,9.55947599963789));
#279671=CARTESIAN_POINT('Ctrl Pts',(6.21212407589618,10.9812586280983,8.55025526578723));
#279672=CARTESIAN_POINT('Ctrl Pts',(8.13177598651388,11.1312586280977,5.90808108241509));
#279673=CARTESIAN_POINT('Ctrl Pts',(10.0514278971316,11.2812586280971,3.26590689904295));
#279674=CARTESIAN_POINT('Ctrl Pts',(10.0514278971316,11.4312586280965,-1.23094490010826E-15));
#279675=CARTESIAN_POINT('Ctrl Pts',(10.0514278971316,11.5812586280959,-3.26590689904296));
#279676=CARTESIAN_POINT('Ctrl Pts',(8.13177598651387,11.7312586280953,-5.9080810824151));
#279677=CARTESIAN_POINT('Ctrl Pts',(6.21212407589618,11.8812586280947,-8.55025526578723));
#279678=CARTESIAN_POINT('Ctrl Pts',(3.10606203794808,12.0312586280941,-9.55947599963789));
#279679=CARTESIAN_POINT('Ctrl Pts',(-2.01399939409749E-14,12.1812586280935,
-10.5686967334885));
#279680=CARTESIAN_POINT('Ctrl Pts',(-3.10606203794812,12.3312586280929,
-9.55947599963789));
#279681=CARTESIAN_POINT('Ctrl Pts',(-6.21212407589622,12.4812586280923,
-8.55025526578723));
#279682=CARTESIAN_POINT('Ctrl Pts',(-8.13177598651392,12.6312586280917,
-5.90808108241509));
#279683=CARTESIAN_POINT('Ctrl Pts',(-10.0514278971316,12.7812586280911,
-3.26590689904296));
#279684=CARTESIAN_POINT('Ctrl Pts',(-10.0514278971316,12.9312586280905,
2.46188980021652E-15));
#279685=CARTESIAN_POINT('Ctrl Pts',(-10.0514278971316,13.0812586280899,
3.26590689904296));
#279686=CARTESIAN_POINT('Ctrl Pts',(-8.13177598651392,13.2312586280893,
5.9080810824151));
#279687=CARTESIAN_POINT('Ctrl Pts',(-6.21212407589622,13.3812586280887,
8.55025526578723));
#279688=CARTESIAN_POINT('Ctrl Pts',(-3.10606203794812,13.5312586280881,
9.55947599963789));
#279689=CARTESIAN_POINT('Ctrl Pts',(-1.84152644516406E-14,13.6812586280875,
10.5686967334885));
#279690=CARTESIAN_POINT('Ctrl Pts',(3.10606203794808,13.8312586280869,9.55947599963789));
#279691=CARTESIAN_POINT('Ctrl Pts',(6.21212407589618,13.9812586280863,8.55025526578723));
#279692=CARTESIAN_POINT('Ctrl Pts',(8.13177598651387,14.1312586280857,5.90808108241509));
#279693=CARTESIAN_POINT('Ctrl Pts',(10.0514278971316,14.2812586280851,3.26590689904295));
#279694=CARTESIAN_POINT('Ctrl Pts',(10.0514278971316,14.4312586280845,-1.23094490010826E-15));
#279695=CARTESIAN_POINT('Ctrl Pts',(10.0514278971316,14.5812586280839,-3.26590689904296));
#279696=CARTESIAN_POINT('Ctrl Pts',(8.13177598651387,14.7312586280833,-5.9080810824151));
#279697=CARTESIAN_POINT('Ctrl Pts',(6.21212407589618,14.8812586280827,-8.55025526578723));
#279698=CARTESIAN_POINT('Ctrl Pts',(3.10606203794808,15.0312586280821,-9.55947599963789));
#279699=CARTESIAN_POINT('Ctrl Pts',(-2.18677032126367E-14,15.1812586280815,
-10.5686967334885));
#279700=CARTESIAN_POINT('Ctrl Pts',(-3.10606203794812,15.3312586280809,
-9.55947599963789));
#279701=CARTESIAN_POINT('Ctrl Pts',(-6.21212407589623,15.4812586280803,
-8.55025526578723));
#279702=CARTESIAN_POINT('Ctrl Pts',(-8.13177598651392,15.6312586280797,
-5.90808108241509));
#279703=CARTESIAN_POINT('Ctrl Pts',(-10.0514278971316,15.7812586280791,
-3.26590689904296));
#279704=CARTESIAN_POINT('Ctrl Pts',(-10.0514278971316,15.9312586280785,
2.46188980021652E-15));
#279705=CARTESIAN_POINT('Ctrl Pts',(-10.0514278971316,16.0812586280779,
3.26590689904296));
#279706=CARTESIAN_POINT('Ctrl Pts',(-8.13177598651392,16.2312586280773,
5.9080810824151));
#279707=CARTESIAN_POINT('Ctrl Pts',(-6.21212407589622,16.3812586280767,
8.55025526578723));
#279708=CARTESIAN_POINT('Ctrl Pts',(-3.10606203794812,16.5312586280761,
9.55947599963789));
#279709=CARTESIAN_POINT('Ctrl Pts',(-2.01429737233025E-14,16.6812586280755,
10.5686967334885));
#279710=CARTESIAN_POINT('Ctrl Pts',(3.10606203794808,16.8312586280749,9.55947599963789));
#279711=CARTESIAN_POINT('Ctrl Pts',(6.21212407589618,16.9812586280743,8.55025526578723));
#279712=CARTESIAN_POINT('Ctrl Pts',(8.13177598651387,17.1312586280737,5.90808108241509));
#279713=CARTESIAN_POINT('Ctrl Pts',(10.0514278971316,17.2812586280731,3.26590689904295));
#279714=CARTESIAN_POINT('Ctrl Pts',(10.0514278971316,17.4312586280725,-1.23094490010826E-15));
#279715=CARTESIAN_POINT('Ctrl Pts',(10.0514278971316,17.5812586280719,-3.26590689904296));
#279716=CARTESIAN_POINT('Ctrl Pts',(8.13177598651387,17.7312586280713,-5.9080810824151));
#279717=CARTESIAN_POINT('Ctrl Pts',(6.21212407589618,17.8812586280707,-8.55025526578723));
#279718=CARTESIAN_POINT('Ctrl Pts',(3.10606203794808,18.0312586280701,-9.55947599963789));
#279719=CARTESIAN_POINT('Ctrl Pts',(-2.35954124842986E-14,18.1812586280695,
-10.5686967334885));
#279720=CARTESIAN_POINT('Ctrl Pts',(-3.10606203794813,18.3312586280689,
-9.55947599963789));
#279721=CARTESIAN_POINT('Ctrl Pts',(-6.21212407589623,18.4812586280683,
-8.55025526578723));
#279722=CARTESIAN_POINT('Ctrl Pts',(-8.13177598651392,18.6312586280677,
-5.90808108241509));
#279723=CARTESIAN_POINT('Ctrl Pts',(-10.0514278971316,18.7812586280671,
-3.26590689904296));
#279724=CARTESIAN_POINT('Ctrl Pts',(-10.0514278971316,18.9312586280665,
2.46188980021652E-15));
#279725=CARTESIAN_POINT('Ctrl Pts',(-10.0514278971316,19.0812586280659,
3.26590689904296));
#279726=CARTESIAN_POINT('Ctrl Pts',(-8.13177598651392,19.2312586280653,
5.9080810824151));
#279727=CARTESIAN_POINT('Ctrl Pts',(-6.21212407589623,19.3812586280647,
8.55025526578723));
#279728=CARTESIAN_POINT('Ctrl Pts',(-3.10606203794812,19.5312586280641,
9.55947599963789));
#279729=CARTESIAN_POINT('Ctrl Pts',(-2.18706829949643E-14,19.6812586280635,
10.5686967334885));
#279730=CARTESIAN_POINT('Ctrl Pts',(3.10606203794808,19.8312586280629,9.55947599963789));
#279731=CARTESIAN_POINT('Ctrl Pts',(6.21212407589618,19.9812586280623,8.55025526578723));
#279732=CARTESIAN_POINT('Ctrl Pts',(8.13177598651387,20.1312586280617,5.90808108241509));
#279733=CARTESIAN_POINT('Ctrl Pts',(10.0514278971316,20.2812586280611,3.26590689904295));
#279734=CARTESIAN_POINT('Ctrl Pts',(10.0514278971316,20.4312586280605,-1.23094490010826E-15));
#279735=CARTESIAN_POINT('Ctrl Pts',(10.0514278971316,20.5812586280599,-3.26590689904296));
#279736=CARTESIAN_POINT('Ctrl Pts',(8.13177598651387,20.7312586280593,-5.9080810824151));
#279737=CARTESIAN_POINT('Ctrl Pts',(6.21212407589618,20.8812586280587,-8.55025526578723));
#279738=CARTESIAN_POINT('Ctrl Pts',(3.10606203794808,21.0312586280581,-9.55947599963789));
#279739=CARTESIAN_POINT('Ctrl Pts',(-2.53231217559604E-14,21.1812586280575,
-10.5686967334885));
#279740=CARTESIAN_POINT('Ctrl Pts',(-3.10606203794813,21.3312586280569,
-9.55947599963789));
#279741=CARTESIAN_POINT('Ctrl Pts',(-6.21212407589623,21.4812586280563,
-8.55025526578723));
#279742=CARTESIAN_POINT('Ctrl Pts',(-8.13177598651392,21.6312586280557,
-5.90808108241509));
#279743=CARTESIAN_POINT('Ctrl Pts',(-10.0514278971316,21.7812586280551,
-3.26590689904296));
#279744=CARTESIAN_POINT('Ctrl Pts',(-10.0514278971316,21.9312586280545,
2.46188980021652E-15));
#279745=CARTESIAN_POINT('Ctrl Pts',(-10.0514278971316,22.0812586280539,
3.26590689904296));
#279746=CARTESIAN_POINT('Ctrl Pts',(-8.13177598651392,22.2312586280533,
5.9080810824151));
#279747=CARTESIAN_POINT('Ctrl Pts',(-6.21212407589623,22.3812586280527,
8.55025526578723));
#279748=CARTESIAN_POINT('Ctrl Pts',(-3.10606203794813,22.5312586280521,
9.55947599963789));
#279749=CARTESIAN_POINT('Ctrl Pts',(-2.35983922666262E-14,22.6812586280515,
10.5686967334885));
#279750=CARTESIAN_POINT('Ctrl Pts',(3.10606203794808,22.8312586280509,9.55947599963789));
#279751=CARTESIAN_POINT('Ctrl Pts',(6.21212407589618,22.9812586280503,8.55025526578723));
#279752=CARTESIAN_POINT('Ctrl Pts',(8.13177598651387,23.1312586280497,5.90808108241509));
#279753=CARTESIAN_POINT('Ctrl Pts',(10.0514278971316,23.2812586280491,3.26590689904295));
#279754=CARTESIAN_POINT('Ctrl Pts',(10.0514278971316,23.4312586280485,-1.23094490010826E-15));
#279755=CARTESIAN_POINT('Ctrl Pts',(10.0514278971316,23.5812586280479,-3.26590689904296));
#279756=CARTESIAN_POINT('Ctrl Pts',(8.13177598651387,23.7312586280473,-5.9080810824151));
#279757=CARTESIAN_POINT('Ctrl Pts',(6.21212407589618,23.8812586280467,-8.55025526578723));
#279758=CARTESIAN_POINT('Ctrl Pts',(3.10606203794807,24.0312586280461,-9.55947599963789));
#279759=CARTESIAN_POINT('Ctrl Pts',(-2.70508310276223E-14,24.1812586280455,
-10.5686967334885));
#279760=CARTESIAN_POINT('Ctrl Pts',(-3.10606203794813,24.3312586280449,
-9.55947599963789));
#279761=CARTESIAN_POINT('Ctrl Pts',(-6.21212407589623,24.4812586280443,
-8.55025526578723));
#279762=CARTESIAN_POINT('Ctrl Pts',(-8.13177598651392,24.6312586280437,
-5.90808108241509));
#279763=CARTESIAN_POINT('Ctrl Pts',(-10.0514278971316,24.7812586280431,
-3.26590689904296));
#279764=CARTESIAN_POINT('Ctrl Pts',(-10.0514278971316,24.9312586280425,
2.46188980021652E-15));
#279765=CARTESIAN_POINT('Ctrl Pts',(-10.0514278971316,25.0812586280419,
3.26590689904296));
#279766=CARTESIAN_POINT('Ctrl Pts',(-8.13177598651392,25.2312586280413,
5.9080810824151));
#279767=CARTESIAN_POINT('Ctrl Pts',(-6.21212407589623,25.3812586280407,
8.55025526578723));
#279768=CARTESIAN_POINT('Ctrl Pts',(-3.10606203794813,25.5312586280401,
9.55947599963789));
#279769=CARTESIAN_POINT('Ctrl Pts',(-2.5326101538288E-14,25.6812586280395,
10.5686967334885));
#279770=CARTESIAN_POINT('Ctrl Pts',(3.10606203794808,25.8312586280389,9.55947599963789));
#279771=CARTESIAN_POINT('Ctrl Pts',(6.21212407589618,25.9812586280383,8.55025526578723));
#279772=CARTESIAN_POINT('Ctrl Pts',(8.13177598651387,26.1312586280377,5.90808108241509));
#279773=CARTESIAN_POINT('Ctrl Pts',(10.0514278971316,26.2812586280371,3.26590689904295));
#279774=CARTESIAN_POINT('Ctrl Pts',(10.0514278971316,26.4312586280365,-1.23094490010826E-15));
#279775=CARTESIAN_POINT('Ctrl Pts',(10.0514278971316,26.5812586280359,-3.26590689904296));
#279776=CARTESIAN_POINT('Ctrl Pts',(8.13177598651387,26.7312586280353,-5.9080810824151));
#279777=CARTESIAN_POINT('Ctrl Pts',(6.21212407589617,26.8812586280347,-8.55025526578723));
#279778=CARTESIAN_POINT('Ctrl Pts',(3.10606203794807,27.0312586280341,-9.55947599963789));
#279779=CARTESIAN_POINT('Ctrl Pts',(-2.87785402992841E-14,27.1812586280335,
-10.5686967334885));
#279780=CARTESIAN_POINT('Ctrl Pts',(-3.10606203794813,27.3312586280329,
-9.55947599963789));
#279781=CARTESIAN_POINT('Ctrl Pts',(-6.21212407589623,27.4812586280323,
-8.55025526578723));
#279782=CARTESIAN_POINT('Ctrl Pts',(-8.13177598651393,27.6312586280317,
-5.90808108241509));
#279783=CARTESIAN_POINT('Ctrl Pts',(-10.0514278971316,27.7812586280311,
-3.26590689904296));
#279784=CARTESIAN_POINT('Ctrl Pts',(-10.0514278971316,27.9312586280305,
2.46188980021652E-15));
#279785=CARTESIAN_POINT('Ctrl Pts',(-10.0514278971316,28.0812586280299,
3.26590689904296));
#279786=CARTESIAN_POINT('Ctrl Pts',(-8.13177598651393,28.2312586280293,
5.9080810824151));
#279787=CARTESIAN_POINT('Ctrl Pts',(-6.21212407589623,28.3812586280287,
8.55025526578723));
#279788=CARTESIAN_POINT('Ctrl Pts',(-3.10606203794813,28.5312586280281,
9.55947599963789));
#279789=CARTESIAN_POINT('Ctrl Pts',(-2.70538108099498E-14,28.6812586280275,
10.5686967334885));
#279790=CARTESIAN_POINT('Ctrl Pts',(3.10606203794807,28.8312586280269,9.55947599963789));
#279791=CARTESIAN_POINT('Ctrl Pts',(6.21212407589618,28.9812586280263,8.55025526578723));
#279792=CARTESIAN_POINT('Ctrl Pts',(8.13177598651387,29.1312586280257,5.90808108241509));
#279793=CARTESIAN_POINT('Ctrl Pts',(10.0514278971316,29.2812586280251,3.26590689904295));
#279794=CARTESIAN_POINT('Ctrl Pts',(10.0514278971316,29.4312586280245,-1.23094490010826E-15));
#279795=CARTESIAN_POINT('Ctrl Pts',(10.0514278971316,29.5812586280239,-3.26590689904296));
#279796=CARTESIAN_POINT('Ctrl Pts',(8.13177598651386,29.7312586280233,-5.9080810824151));
#279797=CARTESIAN_POINT('Ctrl Pts',(6.21212407589617,29.8812586280227,-8.55025526578723));
#279798=CARTESIAN_POINT('Ctrl Pts',(3.10606203794807,30.0312586280221,-9.55947599963789));
#279799=CARTESIAN_POINT('Ctrl Pts',(-3.05062495709459E-14,30.1812586280215,
-10.5686967334885));
#279800=CARTESIAN_POINT('Ctrl Pts',(-3.10606203794813,30.3312586280209,
-9.55947599963789));
#279801=CARTESIAN_POINT('Ctrl Pts',(-6.21212407589623,30.4812586280203,
-8.55025526578723));
#279802=CARTESIAN_POINT('Ctrl Pts',(-8.13177598651393,30.6312586280197,
-5.90808108241509));
#279803=CARTESIAN_POINT('Ctrl Pts',(-10.0514278971316,30.7812586280191,
-3.26590689904296));
#279804=CARTESIAN_POINT('Ctrl Pts',(-10.0514278971316,30.9312586280185,
2.46188980021652E-15));
#279805=CARTESIAN_POINT('Ctrl Pts',(-10.0514278971316,31.0812586280179,
3.26590689904296));
#279806=CARTESIAN_POINT('Ctrl Pts',(-8.13177598651393,31.2312586280173,
5.9080810824151));
#279807=CARTESIAN_POINT('Ctrl Pts',(-6.21212407589623,31.3812586280167,
8.55025526578723));
#279808=CARTESIAN_POINT('Ctrl Pts',(-3.10606203794813,31.5312586280161,
9.55947599963789));
#279809=CARTESIAN_POINT('Ctrl Pts',(-2.87815200816117E-14,31.6812586280155,
10.5686967334885));
#279810=CARTESIAN_POINT('Ctrl Pts',(3.10606203794807,31.8312586280149,9.55947599963789));
#279811=CARTESIAN_POINT('Ctrl Pts',(6.21212407589617,31.9812586280143,8.55025526578723));
#279812=CARTESIAN_POINT('Ctrl Pts',(8.13177598651386,32.1312586280137,5.90808108241509));
#279813=CARTESIAN_POINT('Ctrl Pts',(10.0514278971316,32.2812586280131,3.26590689904295));
#279814=CARTESIAN_POINT('Ctrl Pts',(10.0514278971316,32.4312586280125,-1.23094490010826E-15));
#279815=CARTESIAN_POINT('Ctrl Pts',(10.0514278971316,32.5812586280119,-3.26590689904296));
#279816=CARTESIAN_POINT('Ctrl Pts',(8.13177598651386,32.7312586280113,-5.9080810824151));
#279817=CARTESIAN_POINT('Ctrl Pts',(6.21212407589617,32.8812586280107,-8.55025526578723));
#279818=CARTESIAN_POINT('Ctrl Pts',(3.10606203794807,33.0312586280101,-9.55947599963789));
#279819=CARTESIAN_POINT('Ctrl Pts',(-3.22339588426078E-14,33.1812586280095,
-10.5686967334885));
#279820=CARTESIAN_POINT('Ctrl Pts',(-3.10606203794813,33.3312586280089,
-9.55947599963789));
#279821=CARTESIAN_POINT('Ctrl Pts',(-6.21212407589623,33.4812586280083,
-8.55025526578723));
#279822=CARTESIAN_POINT('Ctrl Pts',(-8.13177598651393,33.6312586280077,
-5.90808108241509));
#279823=CARTESIAN_POINT('Ctrl Pts',(-10.0514278971316,33.7812586280071,
-3.26590689904296));
#279824=CARTESIAN_POINT('Ctrl Pts',(-10.0514278971316,33.9312586280065,
2.46188980021652E-15));
#279825=CARTESIAN_POINT('Ctrl Pts',(-10.0514278971316,34.0812586280059,
3.26590689904296));
#279826=CARTESIAN_POINT('Ctrl Pts',(-8.13177598651393,34.2312586280053,
5.9080810824151));
#279827=CARTESIAN_POINT('Ctrl Pts',(-6.21212407589623,34.3812586280047,
8.55025526578723));
#279828=CARTESIAN_POINT('Ctrl Pts',(-3.10606203794813,34.5312586280041,
9.55947599963789));
#279829=CARTESIAN_POINT('Ctrl Pts',(-3.05092293532735E-14,34.6812586280035,
10.5686967334885));
#279830=CARTESIAN_POINT('Ctrl Pts',(3.10606203794807,34.8312586280029,9.55947599963789));
#279831=CARTESIAN_POINT('Ctrl Pts',(6.21212407589617,34.9812586280023,8.55025526578723));
#279832=CARTESIAN_POINT('Ctrl Pts',(8.13177598651386,35.1312586280017,5.90808108241509));
#279833=CARTESIAN_POINT('Ctrl Pts',(10.0514278971316,35.2812586280011,3.26590689904295));
#279834=CARTESIAN_POINT('Ctrl Pts',(10.0514278971316,35.4312586280005,-1.23094490010826E-15));
#279835=CARTESIAN_POINT('Ctrl Pts',(10.0514278971315,35.5812586279999,-3.26590689904296));
#279836=CARTESIAN_POINT('Ctrl Pts',(8.13177598651386,35.7312586279993,-5.9080810824151));
#279837=CARTESIAN_POINT('Ctrl Pts',(6.21212407589617,35.8812586279987,-8.55025526578723));
#279838=CARTESIAN_POINT('Ctrl Pts',(3.10606203794807,36.0312586279981,-9.55947599963789));
#279839=CARTESIAN_POINT('Ctrl Pts',(-3.39616681142696E-14,36.1812586279975,
-10.5686967334885));
#279840=CARTESIAN_POINT('Ctrl Pts',(-3.10606203794814,36.3312586279969,
-9.55947599963789));
#279841=CARTESIAN_POINT('Ctrl Pts',(-6.21212407589624,36.4812586279963,
-8.55025526578723));
#279842=CARTESIAN_POINT('Ctrl Pts',(-8.13177598651393,36.6312586279957,
-5.90808108241509));
#279843=CARTESIAN_POINT('Ctrl Pts',(-10.0514278971316,36.7812586279951,
-3.26590689904296));
#279844=CARTESIAN_POINT('Ctrl Pts',(-10.0514278971316,36.9312586279945,
2.46188980021652E-15));
#279845=CARTESIAN_POINT('Ctrl Pts',(-10.0514278971316,37.0812586279939,
3.26590689904296));
#279846=CARTESIAN_POINT('Ctrl Pts',(-8.13177598651393,37.2312586279933,
5.9080810824151));
#279847=CARTESIAN_POINT('Ctrl Pts',(-6.21212407589623,37.3812586279927,
8.55025526578723));
#279848=CARTESIAN_POINT('Ctrl Pts',(-3.10606203794813,37.5312586279921,
9.55947599963789));
#279849=CARTESIAN_POINT('Ctrl Pts',(-3.22369386249354E-14,37.6812586279915,
10.5686967334885));
#279850=CARTESIAN_POINT('Ctrl Pts',(3.10606203794807,37.8312586279909,9.55947599963789));
#279851=CARTESIAN_POINT('Ctrl Pts',(6.21212407589617,37.9812586279903,8.55025526578723));
#279852=CARTESIAN_POINT('Ctrl Pts',(8.13177598651386,38.1312586279897,5.90808108241509));
#279853=CARTESIAN_POINT('Ctrl Pts',(10.0514278971316,38.2812586279891,3.26590689904295));
#279854=CARTESIAN_POINT('Ctrl Pts',(10.0514278971316,38.4312586279885,-1.23094490010826E-15));
#279855=CARTESIAN_POINT('Ctrl Pts',(10.0514278971315,38.5812586279879,-3.26590689904296));
#279856=CARTESIAN_POINT('Ctrl Pts',(8.13177598651386,38.7312586279873,-5.9080810824151));
#279857=CARTESIAN_POINT('Ctrl Pts',(6.21212407589617,38.8812586279867,-8.55025526578723));
#279858=CARTESIAN_POINT('Ctrl Pts',(3.10606203794807,39.0312586279861,-9.55947599963789));
#279859=CARTESIAN_POINT('Ctrl Pts',(-3.56893773859315E-14,39.1812586279855,
-10.5686967334885));
#279860=CARTESIAN_POINT('Ctrl Pts',(-3.10606203794814,39.3312586279849,
-9.55947599963789));
#279861=CARTESIAN_POINT('Ctrl Pts',(-6.21212407589624,39.4812586279843,
-8.55025526578723));
#279862=CARTESIAN_POINT('Ctrl Pts',(-8.13177598651393,39.6312586279837,
-5.90808108241509));
#279863=CARTESIAN_POINT('Ctrl Pts',(-10.0514278971316,39.7812586279831,
-3.26590689904296));
#279864=CARTESIAN_POINT('Ctrl Pts',(-10.0514278971316,39.9312586279825,
2.46188980021652E-15));
#279865=CARTESIAN_POINT('Ctrl Pts',(-10.0514278971316,40.0812586279819,
3.26590689904296));
#279866=CARTESIAN_POINT('Ctrl Pts',(-8.13177598651393,40.2312586279813,
5.9080810824151));
#279867=CARTESIAN_POINT('Ctrl Pts',(-6.21212407589624,40.3812586279807,
8.55025526578723));
#279868=CARTESIAN_POINT('Ctrl Pts',(-3.10606203794814,40.5312586279801,
9.55947599963789));
#279869=CARTESIAN_POINT('Ctrl Pts',(-3.39646478965972E-14,40.6812586279795,
10.5686967334885));
#279870=CARTESIAN_POINT('Ctrl Pts',(3.10606203794807,40.8312586279789,9.55947599963789));
#279871=CARTESIAN_POINT('Ctrl Pts',(6.21212407589617,40.9812586279783,8.55025526578723));
#279872=CARTESIAN_POINT('Ctrl Pts',(8.13177598651386,41.1312586279777,5.90808108241509));
#279873=CARTESIAN_POINT('Ctrl Pts',(10.0514278971315,41.2812586279771,3.26590689904295));
#279874=CARTESIAN_POINT('Ctrl Pts',(10.0514278971315,41.4312586279765,-1.23094490010826E-15));
#279875=CARTESIAN_POINT('Ctrl Pts',(10.0514278971315,41.5812586279759,-3.26590689904296));
#279876=CARTESIAN_POINT('Ctrl Pts',(8.13177598651386,41.7312586279753,-5.9080810824151));
#279877=CARTESIAN_POINT('Ctrl Pts',(6.21212407589617,41.8812586279747,-8.55025526578723));
#279878=CARTESIAN_POINT('Ctrl Pts',(3.10606203794806,42.0312586279741,-9.55947599963789));
#279879=CARTESIAN_POINT('Ctrl Pts',(-3.74170866575933E-14,42.1812586279735,
-10.5686967334885));
#279880=CARTESIAN_POINT('Ctrl Pts',(-3.10606203794814,42.3312586279729,
-9.55947599963789));
#279881=CARTESIAN_POINT('Ctrl Pts',(-6.21212407589624,42.4812586279723,
-8.55025526578723));
#279882=CARTESIAN_POINT('Ctrl Pts',(-8.13177598651393,42.6312586279717,
-5.90808108241509));
#279883=CARTESIAN_POINT('Ctrl Pts',(-10.0514278971316,42.7812586279711,
-3.26590689904296));
#279884=CARTESIAN_POINT('Ctrl Pts',(-10.0514278971316,42.9312586279705,
2.46188980021652E-15));
#279885=CARTESIAN_POINT('Ctrl Pts',(-10.0514278971316,43.0812586279699,
3.26590689904296));
#279886=CARTESIAN_POINT('Ctrl Pts',(-8.13177598651393,43.2312586279693,
5.9080810824151));
#279887=CARTESIAN_POINT('Ctrl Pts',(-6.21212407589624,43.3812586279687,
8.55025526578723));
#279888=CARTESIAN_POINT('Ctrl Pts',(-3.10606203794814,43.5312586279681,
9.55947599963789));
#279889=CARTESIAN_POINT('Ctrl Pts',(-3.5692357168259E-14,43.6812586279675,
10.5686967334885));
#279890=CARTESIAN_POINT('Ctrl Pts',(3.10606203794807,43.8312586279669,9.55947599963789));
#279891=CARTESIAN_POINT('Ctrl Pts',(6.21212407589617,43.9812586279663,8.55025526578723));
#279892=CARTESIAN_POINT('Ctrl Pts',(8.13177598651386,44.1312586279657,5.90808108241509));
#279893=CARTESIAN_POINT('Ctrl Pts',(10.0514278971315,44.2812586279651,3.26590689904295));
#279894=CARTESIAN_POINT('Ctrl Pts',(10.0514278971315,44.4312586279645,-1.23094490010826E-15));
#279895=CARTESIAN_POINT('Ctrl Pts',(10.0514278971315,44.5812586279639,-3.26590689904296));
#279896=CARTESIAN_POINT('Ctrl Pts',(8.13177598651385,44.7312586279633,-5.9080810824151));
#279897=CARTESIAN_POINT('Ctrl Pts',(6.21212407589616,44.8812586279627,-8.55025526578723));
#279898=CARTESIAN_POINT('Ctrl Pts',(3.10606203794806,45.0312586279621,-9.55947599963789));
#279899=CARTESIAN_POINT('Ctrl Pts',(-3.91447959292551E-14,45.1812586279615,
-10.5686967334885));
#279900=CARTESIAN_POINT('Ctrl Pts',(-3.10606203794814,45.3312586279609,
-9.55947599963789));
#279901=CARTESIAN_POINT('Ctrl Pts',(-6.21212407589624,45.4812586279603,
-8.55025526578723));
#279902=CARTESIAN_POINT('Ctrl Pts',(-8.13177598651393,45.6312586279597,
-5.90808108241509));
#279903=CARTESIAN_POINT('Ctrl Pts',(-10.0514278971316,45.7812586279591,
-3.26590689904296));
#279904=CARTESIAN_POINT('Ctrl Pts',(-10.0514278971316,45.9312586279585,
2.46188980021652E-15));
#279905=CARTESIAN_POINT('Ctrl Pts',(-10.0514278971316,46.0812586279579,
3.26590689904296));
#279906=CARTESIAN_POINT('Ctrl Pts',(-8.13177598651393,46.2312586279573,
5.9080810824151));
#279907=CARTESIAN_POINT('Ctrl Pts',(-6.21212407589624,46.3812586279567,
8.55025526578723));
#279908=CARTESIAN_POINT('Ctrl Pts',(-3.10606203794814,46.5312586279561,
9.55947599963789));
#279909=CARTESIAN_POINT('Ctrl Pts',(-3.74200664399209E-14,46.6812586279555,
10.5686967334885));
#279910=CARTESIAN_POINT('Ctrl Pts',(3.10606203794806,46.8312586279549,9.55947599963789));
#279911=CARTESIAN_POINT('Ctrl Pts',(6.21212407589617,46.9812586279543,8.55025526578723));
#279912=CARTESIAN_POINT('Ctrl Pts',(8.13177598651385,47.1312586279537,5.90808108241509));
#279913=CARTESIAN_POINT('Ctrl Pts',(10.0514278971315,47.2812586279531,3.26590689904295));
#279914=CARTESIAN_POINT('Ctrl Pts',(10.0514278971315,47.4312586279525,-1.23094490010826E-15));
#279915=CARTESIAN_POINT('Ctrl Pts',(10.0514278971315,47.5812586279519,-3.26590689904296));
#279916=CARTESIAN_POINT('Ctrl Pts',(8.13177598651385,47.7312586279513,-5.9080810824151));
#279917=CARTESIAN_POINT('Ctrl Pts',(6.21212407589616,47.8812586279507,-8.55025526578723));
#279918=CARTESIAN_POINT('Ctrl Pts',(3.10606203794806,48.0312586279501,-9.55947599963789));
#279919=CARTESIAN_POINT('Ctrl Pts',(-4.0872505200917E-14,48.1812586279495,
-10.5686967334885));
#279920=CARTESIAN_POINT('Ctrl Pts',(-3.10606203794814,48.3312586279489,
-9.55947599963789));
#279921=CARTESIAN_POINT('Ctrl Pts',(-6.21212407589625,48.4812586279483,
-8.55025526578723));
#279922=CARTESIAN_POINT('Ctrl Pts',(-8.13177598651394,48.6312586279477,
-5.90808108241509));
#279923=CARTESIAN_POINT('Ctrl Pts',(-10.0514278971316,48.7812586279471,
-3.26590689904296));
#279924=CARTESIAN_POINT('Ctrl Pts',(-10.0514278971316,48.9312586279465,
2.46188980021652E-15));
#279925=CARTESIAN_POINT('Ctrl Pts',(-10.0514278971316,49.0812586279459,
3.26590689904296));
#279926=CARTESIAN_POINT('Ctrl Pts',(-8.13177598651394,49.2312586279453,
5.9080810824151));
#279927=CARTESIAN_POINT('Ctrl Pts',(-6.21212407589624,49.3812586279447,
8.55025526578723));
#279928=CARTESIAN_POINT('Ctrl Pts',(-3.10606203794814,49.5312586279441,
9.55947599963789));
#279929=CARTESIAN_POINT('Ctrl Pts',(-3.91477757115827E-14,49.6812586279435,
10.5686967334885));
#279930=CARTESIAN_POINT('Ctrl Pts',(3.10606203794806,49.8312586279429,9.55947599963789));
#279931=CARTESIAN_POINT('Ctrl Pts',(6.21212407589616,49.9812586279423,8.55025526578723));
#279932=CARTESIAN_POINT('Ctrl Pts',(8.13177598651385,50.1312586279417,5.90808108241509));
#279933=CARTESIAN_POINT('Ctrl Pts',(10.0514278971315,50.2812586279411,3.26590689904295));
#279934=CARTESIAN_POINT('Ctrl Pts',(10.0514278971315,50.4312586279405,-1.23094490010826E-15));
#279935=CARTESIAN_POINT('Ctrl Pts',(10.0514278971315,50.5812586279399,-3.26590689904296));
#279936=CARTESIAN_POINT('Ctrl Pts',(8.13177598651385,50.7312586279393,-5.9080810824151));
#279937=CARTESIAN_POINT('Ctrl Pts',(6.21212407589616,50.8812586279387,-8.55025526578723));
#279938=CARTESIAN_POINT('Ctrl Pts',(3.10606203794806,51.0312586279381,-9.55947599963789));
#279939=CARTESIAN_POINT('Ctrl Pts',(-4.26002144725788E-14,51.1812586279375,
-10.5686967334885));
#279940=CARTESIAN_POINT('Ctrl Pts',(-3.10606203794814,51.3312586279369,
-9.55947599963789));
#279941=CARTESIAN_POINT('Ctrl Pts',(-6.21212407589625,51.4812586279363,
-8.55025526578723));
#279942=CARTESIAN_POINT('Ctrl Pts',(-8.13177598651394,51.6312586279357,
-5.90808108241509));
#279943=CARTESIAN_POINT('Ctrl Pts',(-10.0514278971316,51.7812586279351,
-3.26590689904296));
#279944=CARTESIAN_POINT('Ctrl Pts',(-10.0514278971316,51.9312586279345,
2.46188980021652E-15));
#279945=CARTESIAN_POINT('Ctrl Pts',(-10.0514278971316,52.0812586279339,
3.26590689904296));
#279946=CARTESIAN_POINT('Ctrl Pts',(-8.13177598651394,52.2312586279333,
5.9080810824151));
#279947=CARTESIAN_POINT('Ctrl Pts',(-6.21212407589625,52.3812586279327,
8.55025526578723));
#279948=CARTESIAN_POINT('Ctrl Pts',(-3.10606203794814,52.5312586279321,
9.55947599963789));
#279949=CARTESIAN_POINT('Ctrl Pts',(-4.08754849832446E-14,52.6812586279315,
10.5686967334885));
#279950=CARTESIAN_POINT('Ctrl Pts',(3.10606203794806,52.8312586279309,9.55947599963789));
#279951=CARTESIAN_POINT('Ctrl Pts',(6.21212407589616,52.9812586279303,8.55025526578723));
#279952=CARTESIAN_POINT('Ctrl Pts',(8.13177598651385,53.1312586279297,5.90808108241509));
#279953=CARTESIAN_POINT('Ctrl Pts',(10.0514278971315,53.2812586279291,3.26590689904295));
#279954=CARTESIAN_POINT('Ctrl Pts',(10.0514278971315,53.4312586279285,-1.23094490010826E-15));
#279955=CARTESIAN_POINT('Ctrl Pts',(10.0514278971315,53.5812586279279,-3.26590689904296));
#279956=CARTESIAN_POINT('Ctrl Pts',(8.13177598651385,53.7312586279273,-5.9080810824151));
#279957=CARTESIAN_POINT('Ctrl Pts',(6.21212407589616,53.8812586279267,-8.55025526578723));
#279958=CARTESIAN_POINT('Ctrl Pts',(3.10606203794806,54.0312586279261,-9.55947599963789));
#279959=CARTESIAN_POINT('Ctrl Pts',(-4.43279237442407E-14,54.1812586279255,
-10.5686967334885));
#279960=CARTESIAN_POINT('Ctrl Pts',(-3.10606203794815,54.3312586279249,
-9.55947599963789));
#279961=CARTESIAN_POINT('Ctrl Pts',(-6.21212407589625,54.4812586279243,
-8.55025526578723));
#279962=CARTESIAN_POINT('Ctrl Pts',(-8.13177598651394,54.6312586279237,
-5.90808108241509));
#279963=CARTESIAN_POINT('Ctrl Pts',(-10.0514278971316,54.7812586279231,
-3.26590689904296));
#279964=CARTESIAN_POINT('Ctrl Pts',(-10.0514278971316,54.9312586279225,
2.46188980021652E-15));
#279965=CARTESIAN_POINT('Ctrl Pts',(-10.0514278971316,55.0812586279219,
3.26590689904296));
#279966=CARTESIAN_POINT('Ctrl Pts',(-8.13177598651394,55.2312586279213,
5.9080810824151));
#279967=CARTESIAN_POINT('Ctrl Pts',(-6.21212407589625,55.3812586279207,
8.55025526578723));
#279968=CARTESIAN_POINT('Ctrl Pts',(-3.10606203794814,55.5312586279201,
9.55947599963789));
#279969=CARTESIAN_POINT('Ctrl Pts',(-4.26031942549064E-14,55.6812586279195,
10.5686967334885));
#279970=CARTESIAN_POINT('Ctrl Pts',(3.10606203794806,55.8312586279189,9.55947599963789));
#279971=CARTESIAN_POINT('Ctrl Pts',(6.21212407589616,55.9812586279183,8.55025526578723));
#279972=CARTESIAN_POINT('Ctrl Pts',(8.13177598651385,56.1312586279177,5.90808108241509));
#279973=CARTESIAN_POINT('Ctrl Pts',(10.0514278971315,56.2812586279171,3.26590689904295));
#279974=CARTESIAN_POINT('Ctrl Pts',(10.0514278971315,56.4312586279165,-1.23094490010826E-15));
#279975=CARTESIAN_POINT('Ctrl Pts',(10.0514278971315,56.5812586279159,-3.26590689904296));
#279976=CARTESIAN_POINT('Ctrl Pts',(8.13177598651385,56.7312586279153,-5.9080810824151));
#279977=CARTESIAN_POINT('Ctrl Pts',(6.21212407589616,56.8812586279147,-8.55025526578723));
#279978=CARTESIAN_POINT('Ctrl Pts',(3.10606203794806,57.0312586279141,-9.55947599963789));
#279979=CARTESIAN_POINT('Ctrl Pts',(-4.60556330159025E-14,57.1812586279135,
-10.5686967334885));
#279980=CARTESIAN_POINT('Ctrl Pts',(-3.10606203794815,57.3312586279129,
-9.55947599963789));
#279981=CARTESIAN_POINT('Ctrl Pts',(-6.21212407589625,57.4812586279123,
-8.55025526578723));
#279982=CARTESIAN_POINT('Ctrl Pts',(-8.13177598651394,57.6312586279117,
-5.90808108241509));
#279983=CARTESIAN_POINT('Ctrl Pts',(-10.0514278971316,57.7812586279111,
-3.26590689904296));
#279984=CARTESIAN_POINT('Ctrl Pts',(-10.0514278971316,57.9312586279105,
2.46188980021652E-15));
#279985=CARTESIAN_POINT('Ctrl Pts',(-10.0514278971316,58.0812586279099,
3.26590689904296));
#279986=CARTESIAN_POINT('Ctrl Pts',(-8.13177598651394,58.2312586279093,
5.9080810824151));
#279987=CARTESIAN_POINT('Ctrl Pts',(-6.21212407589625,58.3812586279087,
8.55025526578723));
#279988=CARTESIAN_POINT('Ctrl Pts',(-3.10606203794815,58.5312586279081,
9.55947599963789));
#279989=CARTESIAN_POINT('Ctrl Pts',(-4.43309035265682E-14,58.6812586279075,
10.5686967334885));
#279990=CARTESIAN_POINT('Ctrl Pts',(3.10606203794806,58.8312586279069,9.55947599963789));
#279991=CARTESIAN_POINT('Ctrl Pts',(6.21212407589616,58.9812586279063,8.55025526578723));
#279992=CARTESIAN_POINT('Ctrl Pts',(8.13177598651385,59.1312586279057,5.90808108241509));
#279993=CARTESIAN_POINT('Ctrl Pts',(10.0514278971315,59.2812586279051,3.26590689904295));
#279994=CARTESIAN_POINT('Ctrl Pts',(10.0514278971315,59.4312586279045,-1.23094490010826E-15));
#279995=CARTESIAN_POINT('Ctrl Pts',(10.0514278971315,59.5812586279039,-3.26590689904296));
#279996=CARTESIAN_POINT('Ctrl Pts',(8.13177598651385,59.7312586279033,-5.9080810824151));
#279997=CARTESIAN_POINT('Ctrl Pts',(6.21212407589616,59.8812586279027,-8.55025526578723));
#279998=CARTESIAN_POINT('Ctrl Pts',(3.10606203794805,60.0312586279021,-9.55947599963789));
#279999=CARTESIAN_POINT('Ctrl Pts',(-4.77833422875643E-14,60.1812586279015,
-10.5686967334885));
#280000=CARTESIAN_POINT('Ctrl Pts',(-3.10606203794815,60.3312586279009,
-9.55947599963789));
#280001=CARTESIAN_POINT('Ctrl Pts',(-6.21212407589625,60.4812586279003,
-8.55025526578723));
#280002=CARTESIAN_POINT('Ctrl Pts',(-8.13177598651394,60.6312586278997,
-5.90808108241509));
#280003=CARTESIAN_POINT('Ctrl Pts',(-10.0514278971316,60.7812586278991,
-3.26590689904296));
#280004=CARTESIAN_POINT('Ctrl Pts',(-10.0514278971316,60.9312586278985,
2.46188980021652E-15));
#280005=CARTESIAN_POINT('Ctrl Pts',(-10.0514278971316,61.0812586278979,
3.26590689904296));
#280006=CARTESIAN_POINT('Ctrl Pts',(-8.13177598651394,61.2312586278973,
5.9080810824151));
#280007=CARTESIAN_POINT('Ctrl Pts',(-6.21212407589625,61.3812586278967,
8.55025526578723));
#280008=CARTESIAN_POINT('Ctrl Pts',(-3.10606203794815,61.5312586278961,
9.55947599963789));
#280009=CARTESIAN_POINT('Ctrl Pts',(-4.60586127982301E-14,61.6812586278955,
10.5686967334885));
#280010=CARTESIAN_POINT('Ctrl Pts',(3.10606203794806,61.8312586278949,9.55947599963789));
#280011=CARTESIAN_POINT('Ctrl Pts',(6.21212407589616,61.9812586278943,8.55025526578723));
#280012=CARTESIAN_POINT('Ctrl Pts',(8.13177598651385,62.1312586278937,5.90808108241509));
#280013=CARTESIAN_POINT('Ctrl Pts',(10.0514278971315,62.2812586278931,3.26590689904295));
#280014=CARTESIAN_POINT('Ctrl Pts',(10.0514278971315,62.4312586278925,-1.23094490010826E-15));
#280015=CARTESIAN_POINT('Ctrl Pts',(10.0514278971315,62.5812586278919,-3.26590689904296));
#280016=CARTESIAN_POINT('Ctrl Pts',(8.13177598651384,62.7312586278913,-5.9080810824151));
#280017=CARTESIAN_POINT('Ctrl Pts',(6.21212407589615,62.8812586278907,-8.55025526578723));
#280018=CARTESIAN_POINT('Ctrl Pts',(3.10606203794805,63.0312586278901,-9.55947599963789));
#280019=CARTESIAN_POINT('Ctrl Pts',(-4.95110515592262E-14,63.1812586278895,
-10.5686967334885));
#280020=CARTESIAN_POINT('Ctrl Pts',(-3.10606203794815,63.3312586278889,
-9.55947599963789));
#280021=CARTESIAN_POINT('Ctrl Pts',(-6.21212407589625,63.4812586278883,
-8.55025526578723));
#280022=CARTESIAN_POINT('Ctrl Pts',(-8.13177598651395,63.6312586278877,
-5.90808108241509));
#280023=CARTESIAN_POINT('Ctrl Pts',(-10.0514278971316,63.7812586278871,
-3.26590689904296));
#280024=CARTESIAN_POINT('Ctrl Pts',(-10.0514278971316,63.9312586278865,
2.46188980021652E-15));
#280025=CARTESIAN_POINT('Ctrl Pts',(-10.0514278971316,64.0812586278859,
3.26590689904296));
#280026=CARTESIAN_POINT('Ctrl Pts',(-8.13177598651395,64.2312586278853,
5.9080810824151));
#280027=CARTESIAN_POINT('Ctrl Pts',(-6.21212407589625,64.3812586278847,
8.55025526578723));
#280028=CARTESIAN_POINT('Ctrl Pts',(-3.10606203794815,64.5312586278841,
9.55947599963789));
#280029=CARTESIAN_POINT('Ctrl Pts',(-4.77863220698919E-14,64.6812586278835,
10.5686967334885));
#280030=CARTESIAN_POINT('Ctrl Pts',(3.10606203794805,64.8312586278829,9.55947599963789));
#280031=CARTESIAN_POINT('Ctrl Pts',(6.21212407589616,64.9812586278823,8.55025526578723));
#280032=CARTESIAN_POINT('Ctrl Pts',(8.13177598651384,65.1312586278817,5.90808108241509));
#280033=CARTESIAN_POINT('Ctrl Pts',(10.0514278971315,65.2812586278811,3.26590689904295));
#280034=CARTESIAN_POINT('Ctrl Pts',(10.0514278971315,65.4312586278805,-1.23094490010826E-15));
#280035=CARTESIAN_POINT('Ctrl Pts',(10.0514278971315,65.5812586278799,-3.26590689904296));
#280036=CARTESIAN_POINT('Ctrl Pts',(8.13177598651384,65.7312586278793,-5.9080810824151));
#280037=CARTESIAN_POINT('Ctrl Pts',(6.21212407589615,65.8812586278787,-8.55025526578723));
#280038=CARTESIAN_POINT('Ctrl Pts',(3.10606203794805,66.0312586278781,-9.55947599963789));
#280039=CARTESIAN_POINT('Ctrl Pts',(-5.1238760830888E-14,66.1812586278775,
-10.5686967334885));
#280040=CARTESIAN_POINT('Ctrl Pts',(-3.10606203794815,66.3312586278769,
-9.55947599963789));
#280041=CARTESIAN_POINT('Ctrl Pts',(-6.21212407589625,66.4812586278763,
-8.55025526578723));
#280042=CARTESIAN_POINT('Ctrl Pts',(-8.13177598651395,66.6312586278757,
-5.90808108241509));
#280043=CARTESIAN_POINT('Ctrl Pts',(-10.0514278971316,66.7812586278751,
-3.26590689904296));
#280044=CARTESIAN_POINT('Ctrl Pts',(-10.0514278971316,66.9312586278745,
2.46188980021652E-15));
#280045=CARTESIAN_POINT('Ctrl Pts',(-10.0514278971316,67.0812586278739,
3.26590689904296));
#280046=CARTESIAN_POINT('Ctrl Pts',(-8.13177598651395,67.2312586278733,
5.9080810824151));
#280047=CARTESIAN_POINT('Ctrl Pts',(-6.21212407589625,67.3812586278727,
8.55025526578723));
#280048=CARTESIAN_POINT('Ctrl Pts',(-3.10606203794815,67.5312586278721,
9.55947599963789));
#280049=CARTESIAN_POINT('Ctrl Pts',(-4.95140313415538E-14,67.6812586278715,
10.5686967334885));
#280050=CARTESIAN_POINT('Ctrl Pts',(3.10606203794805,67.8312586278709,9.55947599963789));
#280051=CARTESIAN_POINT('Ctrl Pts',(6.21212407589615,67.9812586278703,8.55025526578723));
#280052=CARTESIAN_POINT('Ctrl Pts',(8.13177598651384,68.1312586278697,5.90808108241509));
#280053=CARTESIAN_POINT('Ctrl Pts',(10.0514278971315,68.2812586278691,3.26590689904295));
#280054=CARTESIAN_POINT('Ctrl Pts',(10.0514278971315,68.4312586278685,-1.23094490010826E-15));
#280055=CARTESIAN_POINT('Ctrl Pts',(10.0514278971315,68.5812586278679,-3.26590689904296));
#280056=CARTESIAN_POINT('Ctrl Pts',(8.13177598651384,68.7312586278673,-5.9080810824151));
#280057=CARTESIAN_POINT('Ctrl Pts',(6.21212407589615,68.8812586278667,-8.55025526578723));
#280058=CARTESIAN_POINT('Ctrl Pts',(3.10606203794805,69.0312586278661,-9.55947599963789));
#280059=CARTESIAN_POINT('Ctrl Pts',(-5.29664701025498E-14,69.1812586278655,
-10.5686967334885));
#280060=CARTESIAN_POINT('Ctrl Pts',(-3.10606203794816,69.3312586278649,
-9.55947599963789));
#280061=CARTESIAN_POINT('Ctrl Pts',(-6.21212407589626,69.4812586278643,
-8.55025526578723));
#280062=CARTESIAN_POINT('Ctrl Pts',(-8.13177598651395,69.6312586278637,
-5.90808108241509));
#280063=CARTESIAN_POINT('Ctrl Pts',(-10.0514278971316,69.7812586278631,
-3.26590689904296));
#280064=CARTESIAN_POINT('Ctrl Pts',(-10.0514278971316,69.9312586278625,
2.46188980021652E-15));
#280065=CARTESIAN_POINT('Ctrl Pts',(-10.0514278971316,70.0812586278619,
3.26590689904296));
#280066=CARTESIAN_POINT('Ctrl Pts',(-8.13177598651395,70.2312586278613,
5.9080810824151));
#280067=CARTESIAN_POINT('Ctrl Pts',(-6.21212407589625,70.3812586278607,
8.55025526578723));
#280068=CARTESIAN_POINT('Ctrl Pts',(-3.10606203794815,70.5312586278601,
9.55947599963789));
#280069=CARTESIAN_POINT('Ctrl Pts',(-5.12417406132156E-14,70.6812586278595,
10.5686967334885));
#280070=CARTESIAN_POINT('Ctrl Pts',(3.10606203794805,70.8312586278589,9.55947599963789));
#280071=CARTESIAN_POINT('Ctrl Pts',(6.21212407589615,70.9812586278583,8.55025526578723));
#280072=CARTESIAN_POINT('Ctrl Pts',(8.13177598651384,71.1312586278577,5.90808108241509));
#280073=CARTESIAN_POINT('Ctrl Pts',(10.0514278971315,71.2812586278571,3.26590689904295));
#280074=CARTESIAN_POINT('Ctrl Pts',(10.0514278971315,71.4312586278565,-1.23094490010826E-15));
#280075=CARTESIAN_POINT('Ctrl Pts',(10.0514278971315,71.5812586278559,-3.26590689904296));
#280076=CARTESIAN_POINT('Ctrl Pts',(8.13177598651384,71.7312586278553,-5.9080810824151));
#280077=CARTESIAN_POINT('Ctrl Pts',(6.21212407589615,71.8812586278547,-8.55025526578723));
#280078=CARTESIAN_POINT('Ctrl Pts',(3.10606203794805,72.0312586278541,-9.55947599963789));
#280079=CARTESIAN_POINT('Ctrl Pts',(-5.46941793742117E-14,72.1812586278535,
-10.5686967334885));
#280080=CARTESIAN_POINT('Ctrl Pts',(-3.10606203794816,72.3312586278529,
-9.55947599963789));
#280081=CARTESIAN_POINT('Ctrl Pts',(-6.21212407589626,72.4812586278523,
-8.55025526578723));
#280082=CARTESIAN_POINT('Ctrl Pts',(-8.13177598651395,72.6312586278517,
-5.90808108241509));
#280083=CARTESIAN_POINT('Ctrl Pts',(-10.0514278971316,72.7812586278511,
-3.26590689904296));
#280084=CARTESIAN_POINT('Ctrl Pts',(-10.0514278971316,72.9312586278505,
2.46188980021652E-15));
#280085=CARTESIAN_POINT('Ctrl Pts',(-10.0514278971316,73.0812586278499,
3.26590689904296));
#280086=CARTESIAN_POINT('Ctrl Pts',(-8.13177598651395,73.2312586278493,
5.9080810824151));
#280087=CARTESIAN_POINT('Ctrl Pts',(-6.21212407589625,73.3812586278487,
8.55025526578723));
#280088=CARTESIAN_POINT('Ctrl Pts',(-3.10606203794815,73.5312586278481,
9.55947599963789));
#280089=CARTESIAN_POINT('Ctrl Pts',(-5.29694498848774E-14,73.6812586278475,
10.5686967334885));
#280090=CARTESIAN_POINT('Ctrl Pts',(3.10606203794805,73.8312586278469,9.55947599963789));
#280091=CARTESIAN_POINT('Ctrl Pts',(6.21212407589615,73.9812586278463,8.55025526578723));
#280092=CARTESIAN_POINT('Ctrl Pts',(8.13177598651384,74.1312586278457,5.90808108241509));
#280093=CARTESIAN_POINT('Ctrl Pts',(10.0514278971315,74.2812586278451,3.26590689904295));
#280094=CARTESIAN_POINT('Ctrl Pts',(10.0514278971315,74.4312586278445,-1.23094490010826E-15));
#280095=CARTESIAN_POINT('Ctrl Pts',(10.0514278971315,74.5812586278439,-3.26590689904296));
#280096=CARTESIAN_POINT('Ctrl Pts',(8.13177598651384,74.7312586278433,-5.9080810824151));
#280097=CARTESIAN_POINT('Ctrl Pts',(6.21212407589614,74.8812586278427,-8.55025526578723));
#280098=CARTESIAN_POINT('Ctrl Pts',(3.10606203794805,75.0312586278421,-9.55947599963789));
#280099=CARTESIAN_POINT('Ctrl Pts',(-5.64218886458735E-14,75.1812586278415,
-10.5686967334885));
#280100=CARTESIAN_POINT('Ctrl Pts',(-3.10606203794816,75.3312586278409,
-9.55947599963789));
#280101=CARTESIAN_POINT('Ctrl Pts',(-6.21212407589626,75.4812586278403,
-8.55025526578723));
#280102=CARTESIAN_POINT('Ctrl Pts',(-8.13177598651395,75.6312586278397,
-5.90808108241509));
#280103=CARTESIAN_POINT('Ctrl Pts',(-10.0514278971316,75.7812586278391,
-3.26590689904296));
#280104=CARTESIAN_POINT('Ctrl Pts',(-10.0514278971316,75.9312586278385,
2.46188980021652E-15));
#280105=CARTESIAN_POINT('Ctrl Pts',(-10.0514278971316,76.0812586278379,
3.26590689904296));
#280106=CARTESIAN_POINT('Ctrl Pts',(-8.13177598651395,76.2312586278373,
5.9080810824151));
#280107=CARTESIAN_POINT('Ctrl Pts',(-6.21212407589626,76.3812586278367,
8.55025526578723));
#280108=CARTESIAN_POINT('Ctrl Pts',(-3.10606203794816,76.5312586278361,
9.55947599963789));
#280109=CARTESIAN_POINT('Ctrl Pts',(-5.46971591565393E-14,76.6812586278355,
10.5686967334885));
#280110=CARTESIAN_POINT('Ctrl Pts',(3.10606203794805,76.8312586278349,9.55947599963789));
#280111=CARTESIAN_POINT('Ctrl Pts',(6.21212407589615,76.9812586278343,8.55025526578723));
#280112=CARTESIAN_POINT('Ctrl Pts',(8.13177598651384,77.1312586278337,5.90808108241509));
#280113=CARTESIAN_POINT('Ctrl Pts',(10.0514278971315,77.2812586278331,3.26590689904295));
#280114=CARTESIAN_POINT('Ctrl Pts',(10.0514278971315,77.4312586278325,-1.23094490010826E-15));
#280115=CARTESIAN_POINT('Ctrl Pts',(10.0514278971315,77.5812586278319,-3.26590689904296));
#280116=CARTESIAN_POINT('Ctrl Pts',(8.13177598651384,77.7312586278313,-5.9080810824151));
#280117=CARTESIAN_POINT('Ctrl Pts',(6.21212407589614,77.8812586278307,-8.55025526578723));
#280118=CARTESIAN_POINT('Ctrl Pts',(3.10606203794804,78.0312586278301,-9.55947599963789));
#280119=CARTESIAN_POINT('Ctrl Pts',(-5.81495979175354E-14,78.1812586278295,
-10.5686967334885));
#280120=CARTESIAN_POINT('Ctrl Pts',(-3.10606203794816,78.3312586278289,
-9.55947599963789));
#280121=CARTESIAN_POINT('Ctrl Pts',(-6.21212407589626,78.4812586278283,
-8.55025526578723));
#280122=CARTESIAN_POINT('Ctrl Pts',(-8.13177598651395,78.6312586278277,
-5.90808108241509));
#280123=CARTESIAN_POINT('Ctrl Pts',(-10.0514278971316,78.7812586278271,
-3.26590689904296));
#280124=CARTESIAN_POINT('Ctrl Pts',(-10.0514278971316,78.9312586278265,
2.46188980021652E-15));
#280125=CARTESIAN_POINT('Ctrl Pts',(-10.0514278971316,79.0812586278259,
3.26590689904296));
#280126=CARTESIAN_POINT('Ctrl Pts',(-8.13177598651395,79.2312586278253,
5.9080810824151));
#280127=CARTESIAN_POINT('Ctrl Pts',(-6.21212407589626,79.3812586278247,
8.55025526578723));
#280128=CARTESIAN_POINT('Ctrl Pts',(-3.10606203794816,79.5312586278241,
9.55947599963789));
#280129=CARTESIAN_POINT('Ctrl Pts',(-5.64248684282011E-14,79.6812586278235,
10.5686967334885));
#280130=CARTESIAN_POINT('Ctrl Pts',(3.10606203794805,79.8312586278229,9.55947599963789));
#280131=CARTESIAN_POINT('Ctrl Pts',(6.21212407589614,79.9812586278223,8.55025526578723));
#280132=CARTESIAN_POINT('Ctrl Pts',(8.13177598651384,80.1312586278217,5.90808108241509));
#280133=CARTESIAN_POINT('Ctrl Pts',(10.0514278971315,80.2812586278211,3.26590689904295));
#280134=CARTESIAN_POINT('Ctrl Pts',(10.0514278971315,80.4312586278205,-1.23094490010826E-15));
#280135=CARTESIAN_POINT('Ctrl Pts',(10.0514278971315,80.5812586278199,-3.26590689904296));
#280136=CARTESIAN_POINT('Ctrl Pts',(8.13177598651384,80.7312586278193,-5.9080810824151));
#280137=CARTESIAN_POINT('Ctrl Pts',(6.21212407589614,80.8812586278187,-8.55025526578723));
#280138=CARTESIAN_POINT('Ctrl Pts',(3.10606203794804,81.0312586278181,-9.55947599963789));
#280139=CARTESIAN_POINT('Ctrl Pts',(-5.98773071891972E-14,81.1812586278175,
-10.5686967334885));
#280140=CARTESIAN_POINT('Ctrl Pts',(-3.10606203794816,81.3312586278169,
-9.55947599963789));
#280141=CARTESIAN_POINT('Ctrl Pts',(-6.21212407589626,81.4812586278163,
-8.55025526578723));
#280142=CARTESIAN_POINT('Ctrl Pts',(-8.13177598651396,81.6312586278157,
-5.90808108241509));
#280143=CARTESIAN_POINT('Ctrl Pts',(-10.0514278971316,81.7812586278151,
-3.26590689904296));
#280144=CARTESIAN_POINT('Ctrl Pts',(-10.0514278971316,81.9312586278145,
2.46188980021652E-15));
#280145=CARTESIAN_POINT('Ctrl Pts',(-10.0514278971316,82.0812586278139,
3.26590689904296));
#280146=CARTESIAN_POINT('Ctrl Pts',(-8.13177598651396,82.2312586278133,
5.9080810824151));
#280147=CARTESIAN_POINT('Ctrl Pts',(-6.21212407589626,82.3812586278127,
8.55025526578723));
#280148=CARTESIAN_POINT('Ctrl Pts',(-3.10606203794816,82.5312586278121,
9.55947599963789));
#280149=CARTESIAN_POINT('Ctrl Pts',(-5.8152577699863E-14,82.6812586278115,
10.5686967334885));
#280150=CARTESIAN_POINT('Ctrl Pts',(3.10606203794804,82.8312586278109,9.55947599963789));
#280151=CARTESIAN_POINT('Ctrl Pts',(6.21212407589614,82.9812586278103,8.55025526578723));
#280152=CARTESIAN_POINT('Ctrl Pts',(8.13177598651383,83.1312586278097,5.90808108241509));
#280153=CARTESIAN_POINT('Ctrl Pts',(10.0514278971315,83.2812586278091,3.26590689904295));
#280154=CARTESIAN_POINT('Ctrl Pts',(10.0514278971315,83.4312586278085,-1.23094490010826E-15));
#280155=CARTESIAN_POINT('Ctrl Pts',(10.0514278971315,83.5812586278079,-3.26590689904296));
#280156=CARTESIAN_POINT('Ctrl Pts',(8.13177598651383,83.7312586278073,-5.9080810824151));
#280157=CARTESIAN_POINT('Ctrl Pts',(6.21212407589614,83.8812586278067,-8.55025526578723));
#280158=CARTESIAN_POINT('Ctrl Pts',(3.10606203794804,84.0312586278061,-9.55947599963789));
#280159=CARTESIAN_POINT('Ctrl Pts',(-6.1605016460859E-14,84.1812586278055,
-10.5686967334885));
#280160=CARTESIAN_POINT('Ctrl Pts',(-3.10606203794816,84.3312586278049,
-9.55947599963789));
#280161=CARTESIAN_POINT('Ctrl Pts',(-6.21212407589626,84.4812586278043,
-8.55025526578723));
#280162=CARTESIAN_POINT('Ctrl Pts',(-8.13177598651396,84.6312586278037,
-5.90808108241509));
#280163=CARTESIAN_POINT('Ctrl Pts',(-10.0514278971316,84.7812586278031,
-3.26590689904296));
#280164=CARTESIAN_POINT('Ctrl Pts',(-10.0514278971316,84.9312586278025,
2.46188980021652E-15));
#280165=CARTESIAN_POINT('Ctrl Pts',(-10.0514278971316,85.0812586278019,
3.26590689904296));
#280166=CARTESIAN_POINT('Ctrl Pts',(-8.13177598651396,85.2312586278013,
5.9080810824151));
#280167=CARTESIAN_POINT('Ctrl Pts',(-6.21212407589626,85.3812586278007,
8.55025526578723));
#280168=CARTESIAN_POINT('Ctrl Pts',(-3.10606203794816,85.5312586278001,
9.55947599963789));
#280169=CARTESIAN_POINT('Ctrl Pts',(-5.98802869715248E-14,85.6812586277995,
10.5686967334885));
#280170=CARTESIAN_POINT('Ctrl Pts',(3.10606203794804,85.8312586277989,9.55947599963789));
#280171=CARTESIAN_POINT('Ctrl Pts',(6.21212407589614,85.9812586277983,8.55025526578723));
#280172=CARTESIAN_POINT('Ctrl Pts',(8.13177598651383,86.1312586277977,5.90808108241509));
#280173=CARTESIAN_POINT('Ctrl Pts',(10.0514278971315,86.2812586277971,3.26590689904295));
#280174=CARTESIAN_POINT('Ctrl Pts',(10.0514278971315,86.4312586277965,-1.23094490010826E-15));
#280175=CARTESIAN_POINT('Ctrl Pts',(10.0514278971315,86.5812586277959,-3.26590689904296));
#280176=CARTESIAN_POINT('Ctrl Pts',(8.13177598651383,86.7312586277953,-5.9080810824151));
#280177=CARTESIAN_POINT('Ctrl Pts',(6.21212407589614,86.8812586277947,-8.55025526578723));
#280178=CARTESIAN_POINT('Ctrl Pts',(3.10606203794804,87.0312586277941,-9.55947599963789));
#280179=CARTESIAN_POINT('Ctrl Pts',(-6.33327257325209E-14,87.1812586277935,
-10.5686967334885));
#280180=CARTESIAN_POINT('Ctrl Pts',(-3.10606203794817,87.3312586277929,
-9.55947599963789));
#280181=CARTESIAN_POINT('Ctrl Pts',(-6.21212407589627,87.4812586277923,
-8.55025526578723));
#280182=CARTESIAN_POINT('Ctrl Pts',(-8.13177598651396,87.6312586277917,
-5.90808108241509));
#280183=CARTESIAN_POINT('Ctrl Pts',(-10.0514278971317,87.7812586277911,
-3.26590689904296));
#280184=CARTESIAN_POINT('Ctrl Pts',(-10.0514278971317,87.9312586277905,
2.46188980021652E-15));
#280185=CARTESIAN_POINT('Ctrl Pts',(-10.0514278971317,88.0812586277899,
3.26590689904296));
#280186=CARTESIAN_POINT('Ctrl Pts',(-8.13177598651396,88.2312586277893,
5.9080810824151));
#280187=CARTESIAN_POINT('Ctrl Pts',(-6.21212407589626,88.3812586277887,
8.55025526578723));
#280188=CARTESIAN_POINT('Ctrl Pts',(-3.10606203794816,88.5312586277881,
9.55947599963789));
#280189=CARTESIAN_POINT('Ctrl Pts',(-6.16079962431866E-14,88.6812586277875,
10.5686967334885));
#280190=CARTESIAN_POINT('Ctrl Pts',(3.10606203794804,88.8312586277869,9.55947599963789));
#280191=CARTESIAN_POINT('Ctrl Pts',(6.21212407589614,88.9812586277863,8.55025526578723));
#280192=CARTESIAN_POINT('Ctrl Pts',(8.13177598651383,89.1312586277857,5.90808108241509));
#280193=CARTESIAN_POINT('Ctrl Pts',(10.0514278971315,89.2812586277851,3.26590689904295));
#280194=CARTESIAN_POINT('Ctrl Pts',(10.0514278971315,89.4312586277845,-1.23094490010826E-15));
#280195=CARTESIAN_POINT('Ctrl Pts',(10.0514278971315,89.5812586277839,-3.26590689904296));
#280196=CARTESIAN_POINT('Ctrl Pts',(8.13177598651383,89.7312586277833,-5.9080810824151));
#280197=CARTESIAN_POINT('Ctrl Pts',(6.21212407589614,89.8812586277827,-8.55025526578723));
#280198=CARTESIAN_POINT('Ctrl Pts',(3.10606203794804,90.0312586277821,-9.55947599963789));
#280199=CARTESIAN_POINT('Ctrl Pts',(-6.50604350041827E-14,90.1812586277815,
-10.5686967334885));
#280200=CARTESIAN_POINT('Ctrl Pts',(-3.10606203794817,90.3312586277809,
-9.55947599963789));
#280201=CARTESIAN_POINT('Ctrl Pts',(-6.21212407589627,90.4812586277803,
-8.55025526578723));
#280202=CARTESIAN_POINT('Ctrl Pts',(-8.13177598651396,90.6312586277797,
-5.90808108241509));
#280203=CARTESIAN_POINT('Ctrl Pts',(-10.0514278971317,90.7812586277791,
-3.26590689904296));
#280204=CARTESIAN_POINT('Ctrl Pts',(-10.0514278971317,90.9312586277785,
2.46188980021652E-15));
#280205=CARTESIAN_POINT('Ctrl Pts',(-10.0514278971317,91.0812586277779,
3.26590689904296));
#280206=CARTESIAN_POINT('Ctrl Pts',(-8.13177598651396,91.2312586277773,
5.9080810824151));
#280207=CARTESIAN_POINT('Ctrl Pts',(-6.21212407589627,91.3812586277767,
8.55025526578723));
#280208=CARTESIAN_POINT('Ctrl Pts',(-3.10606203794817,91.5312586277761,
9.55947599963789));
#280209=CARTESIAN_POINT('Ctrl Pts',(-6.33357055148485E-14,91.6812586277755,
10.5686967334885));
#280210=CARTESIAN_POINT('Ctrl Pts',(3.10606203794804,91.8312586277749,9.55947599963789));
#280211=CARTESIAN_POINT('Ctrl Pts',(6.21212407589614,91.9812586277743,8.55025526578723));
#280212=CARTESIAN_POINT('Ctrl Pts',(8.13177598651383,92.1312586277737,5.90808108241509));
#280213=CARTESIAN_POINT('Ctrl Pts',(10.0514278971315,92.2812586277731,3.26590689904295));
#280214=CARTESIAN_POINT('Ctrl Pts',(10.0514278971315,92.4312586277725,-1.23094490010826E-15));
#280215=CARTESIAN_POINT('Ctrl Pts',(10.0514278971315,92.5812586277719,-3.26590689904296));
#280216=CARTESIAN_POINT('Ctrl Pts',(8.13177598651383,92.7312586277713,-5.9080810824151));
#280217=CARTESIAN_POINT('Ctrl Pts',(6.21212407589614,92.8812586277707,-8.55025526578723));
#280218=CARTESIAN_POINT('Ctrl Pts',(3.10606203794804,93.0312586277701,-9.55947599963789));
#280219=CARTESIAN_POINT('Ctrl Pts',(-6.67881442758446E-14,93.1812586277695,
-10.5686967334885));
#280220=CARTESIAN_POINT('Ctrl Pts',(-3.10606203794817,93.3312586277689,
-9.55947599963789));
#280221=CARTESIAN_POINT('Ctrl Pts',(-6.21212407589627,93.4812586277683,
-8.55025526578723));
#280222=CARTESIAN_POINT('Ctrl Pts',(-8.13177598651396,93.6312586277677,
-5.90808108241509));
#280223=CARTESIAN_POINT('Ctrl Pts',(-10.0514278971317,93.7812586277671,
-3.26590689904296));
#280224=CARTESIAN_POINT('Ctrl Pts',(-10.0514278971317,93.9312586277665,
2.46188980021652E-15));
#280225=CARTESIAN_POINT('Ctrl Pts',(-10.0514278971317,94.0812586277659,
3.26590689904296));
#280226=CARTESIAN_POINT('Ctrl Pts',(-8.13177598651396,94.2312586277653,
5.9080810824151));
#280227=CARTESIAN_POINT('Ctrl Pts',(-6.21212407589627,94.3812586277647,
8.55025526578723));
#280228=CARTESIAN_POINT('Ctrl Pts',(-3.10606203794817,94.5312586277641,
9.55947599963789));
#280229=CARTESIAN_POINT('Ctrl Pts',(-6.50634147865103E-14,94.6812586277635,
10.5686967334885));
#280230=CARTESIAN_POINT('Ctrl Pts',(3.10606203794804,94.8312586277629,9.55947599963789));
#280231=CARTESIAN_POINT('Ctrl Pts',(6.21212407589614,94.9812586277623,8.55025526578723));
#280232=CARTESIAN_POINT('Ctrl Pts',(8.13177598651383,95.1312586277617,5.90808108241509));
#280233=CARTESIAN_POINT('Ctrl Pts',(10.0514278971315,95.2812586277611,3.26590689904295));
#280234=CARTESIAN_POINT('Ctrl Pts',(10.0514278971315,95.4312586277605,-1.23094490010826E-15));
#280235=CARTESIAN_POINT('Ctrl Pts',(10.0514278971315,95.5812586277599,-3.26590689904296));
#280236=CARTESIAN_POINT('Ctrl Pts',(8.13177598651383,95.7312586277593,-5.9080810824151));
#280237=CARTESIAN_POINT('Ctrl Pts',(6.21212407589613,95.8812586277587,-8.55025526578723));
#280238=CARTESIAN_POINT('Ctrl Pts',(3.10606203794803,96.0312586277581,-9.55947599963789));
#280239=CARTESIAN_POINT('Ctrl Pts',(-6.85158535475064E-14,96.1812586277575,
-10.5686967334885));
#280240=CARTESIAN_POINT('Ctrl Pts',(-3.10606203794817,96.3312586277569,
-9.55947599963789));
#280241=CARTESIAN_POINT('Ctrl Pts',(-6.21212407589627,96.4812586277563,
-8.55025526578723));
#280242=CARTESIAN_POINT('Ctrl Pts',(-8.13177598651396,96.6312586277557,
-5.90808108241509));
#280243=CARTESIAN_POINT('Ctrl Pts',(-10.0514278971317,96.7812586277551,
-3.26590689904296));
#280244=CARTESIAN_POINT('Ctrl Pts',(-10.0514278971317,96.9312586277545,
2.46188980021652E-15));
#280245=CARTESIAN_POINT('Ctrl Pts',(-10.0514278971317,97.0812586277539,
3.26590689904296));
#280246=CARTESIAN_POINT('Ctrl Pts',(-8.13177598651396,97.2312586277533,
5.9080810824151));
#280247=CARTESIAN_POINT('Ctrl Pts',(-6.21212407589627,97.3812586277527,
8.55025526578723));
#280248=CARTESIAN_POINT('Ctrl Pts',(-3.10606203794817,97.5312586277521,
9.55947599963789));
#280249=CARTESIAN_POINT('Ctrl Pts',(-6.67911240581722E-14,97.6812586277515,
10.5686967334885));
#280250=CARTESIAN_POINT('Ctrl Pts',(3.10606203794803,97.8312586277509,9.55947599963789));
#280251=CARTESIAN_POINT('Ctrl Pts',(6.21212407589614,97.9812586277503,8.55025526578723));
#280252=CARTESIAN_POINT('Ctrl Pts',(8.13177598651382,98.1312586277497,5.90808108241509));
#280253=CARTESIAN_POINT('Ctrl Pts',(10.0514278971315,98.2812586277491,3.26590689904295));
#280254=CARTESIAN_POINT('Ctrl Pts',(10.0514278971315,98.4312586277485,-1.23094490010826E-15));
#280255=CARTESIAN_POINT('Ctrl Pts',(10.0514278971315,98.581258627748,-3.26590689904296));
#280256=CARTESIAN_POINT('Ctrl Pts',(8.13177598651382,98.7312586277473,-5.9080810824151));
#280257=CARTESIAN_POINT('Ctrl Pts',(6.21212407589613,98.8812586277467,-8.55025526578723));
#280258=CARTESIAN_POINT('Ctrl Pts',(3.10606203794803,99.0312586277461,-9.55947599963789));
#280259=CARTESIAN_POINT('Ctrl Pts',(-7.02435628191682E-14,99.1812586277455,
-10.5686967334885));
#280260=CARTESIAN_POINT('Ctrl Pts',(-3.10606203794817,99.3312586277449,
-9.55947599963789));
#280261=CARTESIAN_POINT('Ctrl Pts',(-6.21212407589627,99.4812586277443,
-8.55025526578723));
#280262=CARTESIAN_POINT('Ctrl Pts',(-8.13177598651396,99.6312586277437,
-5.90808108241509));
#280263=CARTESIAN_POINT('Ctrl Pts',(-10.0514278971317,99.7812586277431,
-3.26590689904296));
#280264=CARTESIAN_POINT('Ctrl Pts',(-10.0514278971317,99.9312586277425,
2.46188980021652E-15));
#280265=CARTESIAN_POINT('Ctrl Pts',(-10.0514278971317,100.081258627742,
3.26590689904296));
#280266=CARTESIAN_POINT('Ctrl Pts',(-8.13177598651396,100.231258627741,
5.9080810824151));
#280267=CARTESIAN_POINT('Ctrl Pts',(-6.21212407589627,100.381258627741,
8.55025526578723));
#280268=CARTESIAN_POINT('Ctrl Pts',(-3.10606203794817,100.53125862774,9.55947599963789));
#280269=CARTESIAN_POINT('Ctrl Pts',(-6.8518833329834E-14,100.681258627739,
10.5686967334885));
#280270=CARTESIAN_POINT('Ctrl Pts',(3.10606203794803,100.831258627739,9.55947599963789));
#280271=CARTESIAN_POINT('Ctrl Pts',(6.21212407589613,100.981258627738,8.55025526578723));
#280272=CARTESIAN_POINT('Ctrl Pts',(8.13177598651382,101.131258627738,5.90808108241509));
#280273=CARTESIAN_POINT('Ctrl Pts',(10.0514278971315,101.281258627737,3.26590689904295));
#280274=CARTESIAN_POINT('Ctrl Pts',(10.0514278971315,101.431258627737,-1.23094490010826E-15));
#280275=CARTESIAN_POINT('Ctrl Pts',(10.0514278971315,101.581258627736,-3.26590689904296));
#280276=CARTESIAN_POINT('Ctrl Pts',(8.13177598651382,101.731258627735,-5.9080810824151));
#280277=CARTESIAN_POINT('Ctrl Pts',(6.21212407589613,101.881258627735,-8.55025526578723));
#280278=CARTESIAN_POINT('Ctrl Pts',(3.10606203794803,102.031258627734,-9.55947599963789));
#280279=CARTESIAN_POINT('Ctrl Pts',(-7.19712720908301E-14,102.181258627733,
-10.5686967334885));
#280280=CARTESIAN_POINT('Ctrl Pts',(-3.10606203794817,102.331258627733,
-9.55947599963789));
#280281=CARTESIAN_POINT('Ctrl Pts',(-6.21212407589628,102.481258627732,
-8.55025526578723));
#280282=CARTESIAN_POINT('Ctrl Pts',(-8.13177598651397,102.631258627732,
-5.90808108241509));
#280283=CARTESIAN_POINT('Ctrl Pts',(-10.0514278971317,102.781258627731,
-3.26590689904296));
#280284=CARTESIAN_POINT('Ctrl Pts',(-10.0514278971317,102.931258627731,
2.46188980021652E-15));
#280285=CARTESIAN_POINT('Ctrl Pts',(-10.0514278971317,103.08125862773,3.26590689904296));
#280286=CARTESIAN_POINT('Ctrl Pts',(-8.13177598651397,103.231258627729,
5.9080810824151));
#280287=CARTESIAN_POINT('Ctrl Pts',(-6.21212407589627,103.381258627729,
8.55025526578723));
#280288=CARTESIAN_POINT('Ctrl Pts',(-3.10606203794817,103.531258627728,
9.55947599963789));
#280289=CARTESIAN_POINT('Ctrl Pts',(-7.02465426014958E-14,103.681258627728,
10.5686967334885));
#280290=CARTESIAN_POINT('Ctrl Pts',(3.10606203794803,103.831258627727,9.55947599963789));
#280291=CARTESIAN_POINT('Ctrl Pts',(6.21212407589613,103.981258627726,8.55025526578723));
#280292=CARTESIAN_POINT('Ctrl Pts',(8.13177598651382,104.131258627726,5.90808108241509));
#280293=CARTESIAN_POINT('Ctrl Pts',(10.0514278971315,104.281258627725,3.26590689904295));
#280294=CARTESIAN_POINT('Ctrl Pts',(10.0514278971315,104.431258627725,-1.23094490010826E-15));
#280295=CARTESIAN_POINT('Ctrl Pts',(10.0514278971315,104.581258627724,-3.26590689904296));
#280296=CARTESIAN_POINT('Ctrl Pts',(8.13177598651382,104.731258627723,-5.9080810824151));
#280297=CARTESIAN_POINT('Ctrl Pts',(6.21212407589613,104.881258627723,-8.55025526578723));
#280298=CARTESIAN_POINT('Ctrl Pts',(3.10606203794803,105.031258627722,-9.55947599963789));
#280299=CARTESIAN_POINT('Ctrl Pts',(-7.36989813624919E-14,105.181258627722,
-10.5686967334885));
#280300=CARTESIAN_POINT('Ctrl Pts',(-3.10606203794818,105.331258627721,
-9.55947599963789));
#280301=CARTESIAN_POINT('Ctrl Pts',(-6.21212407589628,105.48125862772,-8.55025526578723));
#280302=CARTESIAN_POINT('Ctrl Pts',(-8.13177598651397,105.63125862772,-5.90808108241509));
#280303=CARTESIAN_POINT('Ctrl Pts',(-10.0514278971317,105.781258627719,
-3.26590689904296));
#280304=CARTESIAN_POINT('Ctrl Pts',(-10.0514278971317,105.931258627719,
2.46188980021652E-15));
#280305=CARTESIAN_POINT('Ctrl Pts',(-10.0514278971317,106.081258627718,
3.26590689904296));
#280306=CARTESIAN_POINT('Ctrl Pts',(-8.13177598651397,106.231258627717,
5.9080810824151));
#280307=CARTESIAN_POINT('Ctrl Pts',(-6.21212407589628,106.381258627717,
8.55025526578723));
#280308=CARTESIAN_POINT('Ctrl Pts',(-3.10606203794817,106.531258627716,
9.55947599963789));
#280309=CARTESIAN_POINT('Ctrl Pts',(-7.19742518731577E-14,106.681258627715,
10.5686967334885));
#280310=CARTESIAN_POINT('Ctrl Pts',(3.10606203794803,106.831258627715,9.55947599963789));
#280311=CARTESIAN_POINT('Ctrl Pts',(6.21212407589613,106.981258627714,8.55025526578723));
#280312=CARTESIAN_POINT('Ctrl Pts',(8.13177598651382,107.131258627714,5.90808108241509));
#280313=CARTESIAN_POINT('Ctrl Pts',(10.0514278971315,107.281258627713,3.26590689904295));
#280314=CARTESIAN_POINT('Ctrl Pts',(10.0514278971315,107.431258627713,-1.23094490010826E-15));
#280315=CARTESIAN_POINT('Ctrl Pts',(10.0514278971315,107.581258627712,-3.26590689904296));
#280316=CARTESIAN_POINT('Ctrl Pts',(8.13177598651382,107.731258627711,-5.9080810824151));
#280317=CARTESIAN_POINT('Ctrl Pts',(6.21212407589613,107.881258627711,-8.55025526578723));
#280318=CARTESIAN_POINT('Ctrl Pts',(3.10606203794803,108.03125862771,-9.55947599963789));
#280319=CARTESIAN_POINT('Ctrl Pts',(-7.54266906341537E-14,108.18125862771,
-10.5686967334885));
#280320=CARTESIAN_POINT('Ctrl Pts',(-3.10606203794818,108.331258627709,
-9.55947599963789));
#280321=CARTESIAN_POINT('Ctrl Pts',(-6.21212407589628,108.481258627708,
-8.55025526578723));
#280322=CARTESIAN_POINT('Ctrl Pts',(-8.13177598651397,108.631258627708,
-5.90808108241509));
#280323=CARTESIAN_POINT('Ctrl Pts',(-10.0514278971317,108.781258627707,
-3.26590689904296));
#280324=CARTESIAN_POINT('Ctrl Pts',(-10.0514278971317,108.931258627707,
2.46188980021652E-15));
#280325=CARTESIAN_POINT('Ctrl Pts',(-10.0514278971317,109.081258627706,
3.26590689904296));
#280326=CARTESIAN_POINT('Ctrl Pts',(-8.13177598651397,109.231258627705,
5.9080810824151));
#280327=CARTESIAN_POINT('Ctrl Pts',(-6.21212407589628,109.381258627705,
8.55025526578723));
#280328=CARTESIAN_POINT('Ctrl Pts',(-3.10606203794818,109.531258627704,
9.55947599963789));
#280329=CARTESIAN_POINT('Ctrl Pts',(-7.37019611448195E-14,109.681258627703,
10.5686967334885));
#280330=CARTESIAN_POINT('Ctrl Pts',(3.10606203794803,109.831258627703,9.55947599963789));
#280331=CARTESIAN_POINT('Ctrl Pts',(6.21212407589613,109.981258627702,8.55025526578723));
#280332=CARTESIAN_POINT('Ctrl Pts',(8.13177598651382,110.131258627702,5.90808108241509));
#280333=CARTESIAN_POINT('Ctrl Pts',(10.0514278971315,110.281258627701,3.26590689904295));
#280334=CARTESIAN_POINT('Ctrl Pts',(10.0514278971315,110.431258627701,-1.23094490010826E-15));
#280335=CARTESIAN_POINT('Ctrl Pts',(10.0514278971315,110.5812586277,-3.26590689904296));
#280336=CARTESIAN_POINT('Ctrl Pts',(8.13177598651382,110.731258627699,-5.9080810824151));
#280337=CARTESIAN_POINT('Ctrl Pts',(6.21212407589613,110.881258627699,-8.55025526578723));
#280338=CARTESIAN_POINT('Ctrl Pts',(3.10606203794803,111.031258627698,-9.55947599963789));
#280339=CARTESIAN_POINT('Ctrl Pts',(-7.71543999058156E-14,111.181258627698,
-10.5686967334885));
#280340=CARTESIAN_POINT('Ctrl Pts',(-3.10606203794818,111.331258627697,
-9.55947599963789));
#280341=CARTESIAN_POINT('Ctrl Pts',(-6.21212407589628,111.481258627696,
-8.55025526578723));
#280342=CARTESIAN_POINT('Ctrl Pts',(-8.13177598651397,111.631258627696,
-5.90808108241509));
#280343=CARTESIAN_POINT('Ctrl Pts',(-10.0514278971317,111.781258627695,
-3.26590689904296));
#280344=CARTESIAN_POINT('Ctrl Pts',(-10.0514278971317,111.931258627695,
2.46188980021652E-15));
#280345=CARTESIAN_POINT('Ctrl Pts',(-10.0514278971317,112.081258627694,
3.26590689904296));
#280346=CARTESIAN_POINT('Ctrl Pts',(-8.13177598651397,112.231258627693,
5.9080810824151));
#280347=CARTESIAN_POINT('Ctrl Pts',(-6.21212407589628,112.381258627693,
8.55025526578723));
#280348=CARTESIAN_POINT('Ctrl Pts',(-3.10606203794818,112.531258627692,
9.55947599963789));
#280349=CARTESIAN_POINT('Ctrl Pts',(-7.54296704164813E-14,112.681258627692,
10.5686967334885));
#280350=CARTESIAN_POINT('Ctrl Pts',(3.10606203794803,112.831258627691,9.55947599963789));
#280351=CARTESIAN_POINT('Ctrl Pts',(6.21212407589613,112.98125862769,8.55025526578723));
#280352=CARTESIAN_POINT('Ctrl Pts',(8.13177598651382,113.13125862769,5.90808108241509));
#280353=CARTESIAN_POINT('Ctrl Pts',(10.0514278971315,113.281258627689,3.26590689904295));
#280354=CARTESIAN_POINT('Ctrl Pts',(10.0514278971315,113.431258627689,-1.23094490010826E-15));
#280355=CARTESIAN_POINT('Ctrl Pts',(10.0514278971315,113.581258627688,-3.26590689904296));
#280356=CARTESIAN_POINT('Ctrl Pts',(8.13177598651382,113.731258627687,-5.9080810824151));
#280357=CARTESIAN_POINT('Ctrl Pts',(6.21212407589613,113.881258627687,-8.55025526578723));
#280358=CARTESIAN_POINT('Ctrl Pts',(3.10606203794802,114.031258627686,-9.55947599963789));
#280359=CARTESIAN_POINT('Ctrl Pts',(-7.88821091774774E-14,114.181258627685,
-10.5686967334885));
#280360=CARTESIAN_POINT('Ctrl Pts',(-3.10606203794818,114.331258627685,
-9.55947599963789));
#280361=CARTESIAN_POINT('Ctrl Pts',(-6.21212407589628,114.481258627684,
-8.55025526578723));
#280362=CARTESIAN_POINT('Ctrl Pts',(-8.13177598651397,114.631258627684,
-5.90808108241509));
#280363=CARTESIAN_POINT('Ctrl Pts',(-10.0514278971317,114.781258627683,
-3.26590689904296));
#280364=CARTESIAN_POINT('Ctrl Pts',(-10.0514278971317,114.931258627683,
2.46188980021652E-15));
#280365=CARTESIAN_POINT('Ctrl Pts',(-10.0514278971317,115.081258627682,
3.26590689904296));
#280366=CARTESIAN_POINT('Ctrl Pts',(-8.13177598651397,115.231258627681,
5.9080810824151));
#280367=CARTESIAN_POINT('Ctrl Pts',(-6.21212407589628,115.381258627681,
8.55025526578723));
#280368=CARTESIAN_POINT('Ctrl Pts',(-3.10606203794818,115.53125862768,9.55947599963789));
#280369=CARTESIAN_POINT('Ctrl Pts',(-7.71573796881432E-14,115.681258627679,
10.5686967334885));
#280370=CARTESIAN_POINT('Ctrl Pts',(3.10606203794802,115.831258627679,9.55947599963789));
#280371=CARTESIAN_POINT('Ctrl Pts',(6.21212407589613,115.981258627678,8.55025526578723));
#280372=CARTESIAN_POINT('Ctrl Pts',(8.13177598651382,116.131258627678,5.90808108241509));
#280373=CARTESIAN_POINT('Ctrl Pts',(10.0514278971315,116.281258627677,3.26590689904295));
#280374=CARTESIAN_POINT('Ctrl Pts',(10.0514278971315,116.431258627676,-1.23094490010826E-15));
#280375=CARTESIAN_POINT('Ctrl Pts',(10.0514278971315,116.581258627676,-3.26590689904296));
#280376=CARTESIAN_POINT('Ctrl Pts',(8.13177598651382,116.731258627675,-5.9080810824151));
#280377=CARTESIAN_POINT('Ctrl Pts',(6.21212407589612,116.881258627675,-8.55025526578723));
#280378=CARTESIAN_POINT('Ctrl Pts',(3.10606203794802,117.031258627674,-9.55947599963789));
#280379=CARTESIAN_POINT('Ctrl Pts',(-8.06098184491393E-14,117.181258627674,
-10.5686967334885));
#280380=CARTESIAN_POINT('Ctrl Pts',(-3.10606203794818,117.331258627673,
-9.55947599963789));
#280381=CARTESIAN_POINT('Ctrl Pts',(-6.21212407589629,117.481258627672,
-8.55025526578723));
#280382=CARTESIAN_POINT('Ctrl Pts',(-8.13177598651398,117.631258627672,
-5.90808108241509));
#280383=CARTESIAN_POINT('Ctrl Pts',(-10.0514278971317,117.781258627671,
-3.26590689904296));
#280384=CARTESIAN_POINT('Ctrl Pts',(-10.0514278971317,117.931258627671,
2.46188980021652E-15));
#280385=CARTESIAN_POINT('Ctrl Pts',(-10.0514278971317,118.08125862767,3.26590689904296));
#280386=CARTESIAN_POINT('Ctrl Pts',(-8.13177598651398,118.231258627669,
5.9080810824151));
#280387=CARTESIAN_POINT('Ctrl Pts',(-6.21212407589628,118.381258627669,
8.55025526578723));
#280388=CARTESIAN_POINT('Ctrl Pts',(-3.10606203794818,118.531258627668,
9.55947599963789));
#280389=CARTESIAN_POINT('Ctrl Pts',(-7.8885088959805E-14,118.681258627667,
10.5686967334885));
#280390=CARTESIAN_POINT('Ctrl Pts',(3.10606203794802,118.831258627667,9.55947599963789));
#280391=CARTESIAN_POINT('Ctrl Pts',(6.21212407589613,118.981258627666,8.55025526578723));
#280392=CARTESIAN_POINT('Ctrl Pts',(8.13177598651381,119.131258627666,5.90808108241509));
#280393=CARTESIAN_POINT('Ctrl Pts',(10.0514278971315,119.281258627665,3.26590689904295));
#280394=CARTESIAN_POINT('Ctrl Pts',(10.0514278971315,119.431258627665,-1.23094490010826E-15));
#280395=CARTESIAN_POINT('Ctrl Pts',(10.0514278971315,119.581258627664,-3.26590689904296));
#280396=CARTESIAN_POINT('Ctrl Pts',(8.13177598651381,119.731258627663,-5.9080810824151));
#280397=CARTESIAN_POINT('Ctrl Pts',(6.21212407589612,119.881258627663,-8.55025526578723));
#280398=CARTESIAN_POINT('Ctrl Pts',(3.10606203794802,120.031258627662,-9.55947599963789));
#280399=CARTESIAN_POINT('Ctrl Pts',(-8.23375277208011E-14,120.181258627662,
-10.5686967334885));
#280400=CARTESIAN_POINT('Ctrl Pts',(-3.10606203794818,120.331258627661,
-9.55947599963789));
#280401=CARTESIAN_POINT('Ctrl Pts',(-6.21212407589629,120.48125862766,-8.55025526578723));
#280402=CARTESIAN_POINT('Ctrl Pts',(-8.13177598651398,120.63125862766,-5.90808108241509));
#280403=CARTESIAN_POINT('Ctrl Pts',(-10.0514278971317,120.781258627659,
-3.26590689904296));
#280404=CARTESIAN_POINT('Ctrl Pts',(-10.0514278971317,120.931258627659,
2.46188980021652E-15));
#280405=CARTESIAN_POINT('Ctrl Pts',(-10.0514278971317,121.081258627658,
3.26590689904296));
#280406=CARTESIAN_POINT('Ctrl Pts',(-8.13177598651398,121.231258627657,
5.9080810824151));
#280407=CARTESIAN_POINT('Ctrl Pts',(-6.21212407589629,121.381258627657,
8.55025526578723));
#280408=CARTESIAN_POINT('Ctrl Pts',(-3.10606203794818,121.531258627656,
9.55947599963789));
#280409=CARTESIAN_POINT('Ctrl Pts',(-8.06127982314669E-14,121.681258627655,
10.5686967334885));
#280410=CARTESIAN_POINT('Ctrl Pts',(3.10606203794802,121.831258627655,9.55947599963789));
#280411=CARTESIAN_POINT('Ctrl Pts',(6.21212407589612,121.981258627654,8.55025526578723));
#280412=CARTESIAN_POINT('Ctrl Pts',(8.13177598651381,122.131258627654,5.90808108241509));
#280413=CARTESIAN_POINT('Ctrl Pts',(10.0514278971315,122.281258627653,3.26590689904295));
#280414=CARTESIAN_POINT('Ctrl Pts',(10.0514278971315,122.431258627653,-1.23094490010826E-15));
#280415=CARTESIAN_POINT('Ctrl Pts',(10.0514278971315,122.581258627652,-3.26590689904296));
#280416=CARTESIAN_POINT('Ctrl Pts',(8.13177598651381,122.731258627651,-5.9080810824151));
#280417=CARTESIAN_POINT('Ctrl Pts',(6.21212407589612,122.881258627651,-8.55025526578723));
#280418=CARTESIAN_POINT('Ctrl Pts',(3.10606203794802,123.03125862765,-9.55947599963789));
#280419=CARTESIAN_POINT('Ctrl Pts',(-8.40652369924629E-14,123.181258627649,
-10.5686967334885));
#280420=CARTESIAN_POINT('Ctrl Pts',(-3.10606203794819,123.331258627649,
-9.55947599963789));
#280421=CARTESIAN_POINT('Ctrl Pts',(-6.21212407589629,123.481258627648,
-8.55025526578723));
#280422=CARTESIAN_POINT('Ctrl Pts',(-8.13177598651398,123.631258627648,
-5.90808108241509));
#280423=CARTESIAN_POINT('Ctrl Pts',(-10.0514278971317,123.781258627647,
-3.26590689904296));
#280424=CARTESIAN_POINT('Ctrl Pts',(-10.0514278971317,123.931258627646,
2.46188980021652E-15));
#280425=CARTESIAN_POINT('Ctrl Pts',(-10.0514278971317,124.081258627646,
3.26590689904296));
#280426=CARTESIAN_POINT('Ctrl Pts',(-8.13177598651398,124.231258627645,
5.9080810824151));
#280427=CARTESIAN_POINT('Ctrl Pts',(-6.21212407589629,124.381258627645,
8.55025526578723));
#280428=CARTESIAN_POINT('Ctrl Pts',(-3.10606203794818,124.531258627644,
9.55947599963789));
#280429=CARTESIAN_POINT('Ctrl Pts',(-8.23405075031287E-14,124.681258627644,
10.5686967334885));
#280430=CARTESIAN_POINT('Ctrl Pts',(3.10606203794802,124.831258627643,9.55947599963789));
#280431=CARTESIAN_POINT('Ctrl Pts',(6.21212407589612,124.981258627642,8.55025526578723));
#280432=CARTESIAN_POINT('Ctrl Pts',(8.13177598651381,125.131258627642,5.90808108241509));
#280433=CARTESIAN_POINT('Ctrl Pts',(10.0514278971315,125.281258627641,3.26590689904295));
#280434=CARTESIAN_POINT('Ctrl Pts',(10.0514278971315,125.431258627641,-1.23094490010826E-15));
#280435=CARTESIAN_POINT('Ctrl Pts',(10.0514278971315,125.58125862764,-3.26590689904296));
#280436=CARTESIAN_POINT('Ctrl Pts',(8.13177598651381,125.731258627639,-5.9080810824151));
#280437=CARTESIAN_POINT('Ctrl Pts',(6.21212407589612,125.881258627639,-8.55025526578723));
#280438=CARTESIAN_POINT('Ctrl Pts',(3.10606203794802,126.031258627638,-9.55947599963789));
#280439=CARTESIAN_POINT('Ctrl Pts',(-8.57929462641248E-14,126.181258627637,
-10.5686967334885));
#280440=CARTESIAN_POINT('Ctrl Pts',(-3.10606203794819,126.331258627637,
-9.55947599963789));
#280441=CARTESIAN_POINT('Ctrl Pts',(-6.21212407589629,126.481258627636,
-8.55025526578723));
#280442=CARTESIAN_POINT('Ctrl Pts',(-8.13177598651398,126.631258627636,
-5.90808108241509));
#280443=CARTESIAN_POINT('Ctrl Pts',(-10.0514278971317,126.781258627635,
-3.26590689904296));
#280444=CARTESIAN_POINT('Ctrl Pts',(-10.0514278971317,126.931258627634,
2.46188980021652E-15));
#280445=CARTESIAN_POINT('Ctrl Pts',(-10.0514278971317,127.081258627634,
3.26590689904296));
#280446=CARTESIAN_POINT('Ctrl Pts',(-8.13177598651398,127.231258627633,
5.9080810824151));
#280447=CARTESIAN_POINT('Ctrl Pts',(-6.21212407589629,127.381258627633,
8.55025526578723));
#280448=CARTESIAN_POINT('Ctrl Pts',(-3.10606203794819,127.531258627632,
9.55947599963789));
#280449=CARTESIAN_POINT('Ctrl Pts',(-8.40682167747905E-14,127.681258627631,
10.5686967334885));
#280450=CARTESIAN_POINT('Ctrl Pts',(3.10606203794802,127.831258627631,9.55947599963789));
#280451=CARTESIAN_POINT('Ctrl Pts',(6.21212407589612,127.98125862763,8.55025526578723));
#280452=CARTESIAN_POINT('Ctrl Pts',(8.13177598651381,128.13125862763,5.90808108241509));
#280453=CARTESIAN_POINT('Ctrl Pts',(10.0514278971315,128.281258627629,3.26590689904295));
#280454=CARTESIAN_POINT('Ctrl Pts',(10.0514278971315,128.431258627629,-1.23094490010826E-15));
#280455=CARTESIAN_POINT('Ctrl Pts',(10.0514278971315,128.581258627628,-3.26590689904296));
#280456=CARTESIAN_POINT('Ctrl Pts',(8.13177598651381,128.731258627627,-5.9080810824151));
#280457=CARTESIAN_POINT('Ctrl Pts',(6.21212407589612,128.881258627627,-8.55025526578723));
#280458=CARTESIAN_POINT('Ctrl Pts',(3.10606203794801,129.031258627626,-9.55947599963789));
#280459=CARTESIAN_POINT('Ctrl Pts',(-8.75206555357867E-14,129.181258627626,
-10.5686967334885));
#280460=CARTESIAN_POINT('Ctrl Pts',(-3.10606203794819,129.331258627625,
-9.55947599963789));
#280461=CARTESIAN_POINT('Ctrl Pts',(-6.21212407589629,129.481258627624,
-8.55025526578723));
#280462=CARTESIAN_POINT('Ctrl Pts',(-8.13177598651398,129.631258627624,
-5.90808108241509));
#280463=CARTESIAN_POINT('Ctrl Pts',(-10.0514278971317,129.781258627623,
-3.26590689904296));
#280464=CARTESIAN_POINT('Ctrl Pts',(-10.0514278971317,129.931258627622,
2.46188980021652E-15));
#280465=CARTESIAN_POINT('Ctrl Pts',(-10.0514278971317,130.081258627622,
3.26590689904296));
#280466=CARTESIAN_POINT('Ctrl Pts',(-8.13177598651398,130.231258627621,
5.9080810824151));
#280467=CARTESIAN_POINT('Ctrl Pts',(-6.21212407589629,130.381258627621,
8.55025526578723));
#280468=CARTESIAN_POINT('Ctrl Pts',(-3.10606203794819,130.53125862762,9.55947599963789));
#280469=CARTESIAN_POINT('Ctrl Pts',(-8.57959260464524E-14,130.681258627619,
10.5686967334885));
#280470=CARTESIAN_POINT('Ctrl Pts',(3.10606203794802,130.831258627619,9.55947599963789));
#280471=CARTESIAN_POINT('Ctrl Pts',(6.21212407589612,130.981258627618,8.55025526578723));
#280472=CARTESIAN_POINT('Ctrl Pts',(8.13177598651381,131.131258627618,5.90808108241509));
#280473=CARTESIAN_POINT('Ctrl Pts',(10.0514278971315,131.281258627617,3.26590689904295));
#280474=CARTESIAN_POINT('Ctrl Pts',(10.0514278971315,131.431258627617,-1.23094490010826E-15));
#280475=CARTESIAN_POINT('Ctrl Pts',(10.0514278971315,131.581258627616,-3.26590689904296));
#280476=CARTESIAN_POINT('Ctrl Pts',(8.13177598651381,131.731258627615,-5.9080810824151));
#280477=CARTESIAN_POINT('Ctrl Pts',(6.21212407589611,131.881258627615,-8.55025526578723));
#280478=CARTESIAN_POINT('Ctrl Pts',(3.10606203794801,132.031258627614,-9.55947599963789));
#280479=CARTESIAN_POINT('Ctrl Pts',(-8.92483648074485E-14,132.181258627614,
-10.5686967334885));
#280480=CARTESIAN_POINT('Ctrl Pts',(-3.10606203794819,132.331258627613,
-9.55947599963789));
#280481=CARTESIAN_POINT('Ctrl Pts',(-6.21212407589629,132.481258627612,
-8.55025526578723));
#280482=CARTESIAN_POINT('Ctrl Pts',(-8.13177598651398,132.631258627612,
-5.90808108241509));
#280483=CARTESIAN_POINT('Ctrl Pts',(-10.0514278971317,132.781258627611,
-3.26590689904296));
#280484=CARTESIAN_POINT('Ctrl Pts',(-10.0514278971317,132.93125862761,2.46188980021652E-15));
#280485=CARTESIAN_POINT('Ctrl Pts',(-10.0514278971317,133.08125862761,3.26590689904296));
#280486=CARTESIAN_POINT('Ctrl Pts',(-8.13177598651398,133.231258627609,
5.9080810824151));
#280487=CARTESIAN_POINT('Ctrl Pts',(-6.21212407589629,133.381258627609,
8.55025526578723));
#280488=CARTESIAN_POINT('Ctrl Pts',(-3.10606203794819,133.531258627608,
9.55947599963789));
#280489=CARTESIAN_POINT('Ctrl Pts',(-8.75236353181142E-14,133.681258627607,
10.5686967334885));
#280490=CARTESIAN_POINT('Ctrl Pts',(3.10606203794801,133.831258627607,9.55947599963789));
#280491=CARTESIAN_POINT('Ctrl Pts',(6.21212407589612,133.981258627606,8.55025526578723));
#280492=CARTESIAN_POINT('Ctrl Pts',(8.13177598651381,134.131258627606,5.90808108241509));
#280493=CARTESIAN_POINT('Ctrl Pts',(10.0514278971315,134.281258627605,3.26590689904295));
#280494=CARTESIAN_POINT('Ctrl Pts',(10.0514278971315,134.431258627605,-1.23094490010826E-15));
#280495=CARTESIAN_POINT('Ctrl Pts',(10.0514278971315,134.581258627604,-3.26590689904296));
#280496=CARTESIAN_POINT('Ctrl Pts',(8.13177598651381,134.731258627603,-5.9080810824151));
#280497=CARTESIAN_POINT('Ctrl Pts',(6.21212407589611,134.881258627603,-8.55025526578723));
#280498=CARTESIAN_POINT('Ctrl Pts',(3.10606203794801,135.031258627602,-9.55947599963789));
#280499=CARTESIAN_POINT('Ctrl Pts',(-9.09760740791103E-14,135.181258627601,
-10.5686967334885));
#280500=CARTESIAN_POINT('Ctrl Pts',(-3.10606203794819,135.331258627601,
-9.55947599963789));
#280501=CARTESIAN_POINT('Ctrl Pts',(-6.21212407589629,135.4812586276,-8.55025526578723));
#280502=CARTESIAN_POINT('Ctrl Pts',(-8.13177598651399,135.6312586276,-5.90808108241509));
#280503=CARTESIAN_POINT('Ctrl Pts',(-10.0514278971317,135.781258627599,
-3.26590689904296));
#280504=CARTESIAN_POINT('Ctrl Pts',(-10.0514278971317,135.931258627599,
2.46188980021652E-15));
#280505=CARTESIAN_POINT('Ctrl Pts',(-10.0514278971317,136.081258627598,
3.26590689904296));
#280506=CARTESIAN_POINT('Ctrl Pts',(-8.13177598651399,136.231258627597,
5.9080810824151));
#280507=CARTESIAN_POINT('Ctrl Pts',(-6.21212407589629,136.381258627597,
8.55025526578723));
#280508=CARTESIAN_POINT('Ctrl Pts',(-3.10606203794819,136.531258627596,
9.55947599963789));
#280509=CARTESIAN_POINT('Ctrl Pts',(-8.9251344589776E-14,136.681258627595,
10.5686967334885));
#280510=CARTESIAN_POINT('Ctrl Pts',(3.10606203794801,136.831258627595,9.55947599963789));
#280511=CARTESIAN_POINT('Ctrl Pts',(6.21212407589611,136.981258627594,8.55025526578723));
#280512=CARTESIAN_POINT('Ctrl Pts',(8.1317759865138,137.131258627594,5.90808108241509));
#280513=CARTESIAN_POINT('Ctrl Pts',(10.0514278971315,137.281258627593,3.26590689904295));
#280514=CARTESIAN_POINT('Ctrl Pts',(10.0514278971315,137.431258627593,-1.23094490010826E-15));
#280515=CARTESIAN_POINT('Ctrl Pts',(10.0514278971315,137.581258627592,-3.26590689904296));
#280516=CARTESIAN_POINT('Ctrl Pts',(8.1317759865138,137.731258627591,-5.9080810824151));
#280517=CARTESIAN_POINT('Ctrl Pts',(6.21212407589611,137.881258627591,-8.55025526578723));
#280518=CARTESIAN_POINT('Ctrl Pts',(3.10606203794801,138.03125862759,-9.55947599963789));
#280519=CARTESIAN_POINT('Ctrl Pts',(-9.27037833507721E-14,138.18125862759,
-10.5686967334885));
#280520=CARTESIAN_POINT('Ctrl Pts',(-3.10606203794819,138.331258627589,
-9.55947599963789));
#280521=CARTESIAN_POINT('Ctrl Pts',(-6.2121240758963,138.481258627588,-8.55025526578723));
#280522=CARTESIAN_POINT('Ctrl Pts',(-8.13177598651399,138.631258627588,
-5.90808108241509));
#280523=CARTESIAN_POINT('Ctrl Pts',(-10.0514278971317,138.781258627587,
-3.26590689904296));
#280524=CARTESIAN_POINT('Ctrl Pts',(-10.0514278971317,138.931258627586,
2.46188980021652E-15));
#280525=CARTESIAN_POINT('Ctrl Pts',(-10.0514278971317,139.081258627586,
3.26590689904296));
#280526=CARTESIAN_POINT('Ctrl Pts',(-8.13177598651399,139.231258627585,
5.9080810824151));
#280527=CARTESIAN_POINT('Ctrl Pts',(-6.21212407589629,139.381258627585,
8.55025526578723));
#280528=CARTESIAN_POINT('Ctrl Pts',(-3.10606203794819,139.531258627584,
9.55947599963789));
#280529=CARTESIAN_POINT('Ctrl Pts',(-9.09790538614379E-14,139.681258627583,
10.5686967334885));
#280530=CARTESIAN_POINT('Ctrl Pts',(3.10606203794801,139.831258627583,9.55947599963789));
#280531=CARTESIAN_POINT('Ctrl Pts',(6.21212407589611,139.981258627582,8.55025526578723));
#280532=CARTESIAN_POINT('Ctrl Pts',(8.1317759865138,140.131258627582,5.90808108241509));
#280533=CARTESIAN_POINT('Ctrl Pts',(10.0514278971315,140.281258627581,3.26590689904295));
#280534=CARTESIAN_POINT('Ctrl Pts',(10.0514278971315,140.431258627581,-1.23094490010826E-15));
#280535=CARTESIAN_POINT('Ctrl Pts',(10.0514278971315,140.58125862758,-3.26590689904296));
#280536=CARTESIAN_POINT('Ctrl Pts',(8.1317759865138,140.731258627579,-5.9080810824151));
#280537=CARTESIAN_POINT('Ctrl Pts',(6.21212407589611,140.881258627579,-8.55025526578723));
#280538=CARTESIAN_POINT('Ctrl Pts',(3.10606203794801,141.031258627578,-9.55947599963789));
#280539=CARTESIAN_POINT('Ctrl Pts',(-9.4431492622434E-14,141.181258627577,
-10.5686967334885));
#280540=CARTESIAN_POINT('Ctrl Pts',(-3.1060620379482,141.331258627577,-9.55947599963789));
#280541=CARTESIAN_POINT('Ctrl Pts',(-6.2121240758963,141.481258627576,-8.55025526578723));
#280542=CARTESIAN_POINT('Ctrl Pts',(-8.13177598651399,141.631258627576,
-5.90808108241509));
#280543=CARTESIAN_POINT('Ctrl Pts',(-10.0514278971317,141.781258627575,
-3.26590689904296));
#280544=CARTESIAN_POINT('Ctrl Pts',(-10.0514278971317,141.931258627574,
2.46188980021652E-15));
#280545=CARTESIAN_POINT('Ctrl Pts',(-10.0514278971317,142.081258627574,
3.26590689904296));
#280546=CARTESIAN_POINT('Ctrl Pts',(-8.13177598651399,142.231258627573,
5.9080810824151));
#280547=CARTESIAN_POINT('Ctrl Pts',(-6.2121240758963,142.381258627573,8.55025526578723));
#280548=CARTESIAN_POINT('Ctrl Pts',(-3.10606203794819,142.531258627572,
9.55947599963789));
#280549=CARTESIAN_POINT('Ctrl Pts',(-9.27067631330997E-14,142.681258627572,
10.5686967334885));
#280550=CARTESIAN_POINT('Ctrl Pts',(3.10606203794801,142.831258627571,9.55947599963789));
#280551=CARTESIAN_POINT('Ctrl Pts',(6.21212407589611,142.98125862757,8.55025526578723));
#280552=CARTESIAN_POINT('Ctrl Pts',(8.1317759865138,143.13125862757,5.90808108241509));
#280553=CARTESIAN_POINT('Ctrl Pts',(10.0514278971315,143.281258627569,3.26590689904295));
#280554=CARTESIAN_POINT('Ctrl Pts',(10.0514278971315,143.431258627569,-1.23094490010826E-15));
#280555=CARTESIAN_POINT('Ctrl Pts',(10.0514278971315,143.581258627568,-3.26590689904296));
#280556=CARTESIAN_POINT('Ctrl Pts',(8.1317759865138,143.731258627567,-5.9080810824151));
#280557=CARTESIAN_POINT('Ctrl Pts',(6.21212407589611,143.881258627567,-8.55025526578723));
#280558=CARTESIAN_POINT('Ctrl Pts',(3.10606203794801,144.031258627566,-9.55947599963789));
#280559=CARTESIAN_POINT('Ctrl Pts',(-9.61592018940958E-14,144.181258627565,
-10.5686967334885));
#280560=CARTESIAN_POINT('Ctrl Pts',(-3.1060620379482,144.331258627565,-9.55947599963789));
#280561=CARTESIAN_POINT('Ctrl Pts',(-6.2121240758963,144.481258627564,-8.55025526578723));
#280562=CARTESIAN_POINT('Ctrl Pts',(-8.13177598651399,144.631258627564,
-5.90808108241509));
#280563=CARTESIAN_POINT('Ctrl Pts',(-10.0514278971317,144.781258627563,
-3.26590689904296));
#280564=CARTESIAN_POINT('Ctrl Pts',(-10.0514278971317,144.931258627562,
2.46188980021652E-15));
#280565=CARTESIAN_POINT('Ctrl Pts',(-10.0514278971317,145.081258627562,
3.26590689904296));
#280566=CARTESIAN_POINT('Ctrl Pts',(-8.13177598651399,145.231258627561,
5.9080810824151));
#280567=CARTESIAN_POINT('Ctrl Pts',(-6.2121240758963,145.381258627561,8.55025526578723));
#280568=CARTESIAN_POINT('Ctrl Pts',(-3.1060620379482,145.53125862756,9.55947599963789));
#280569=CARTESIAN_POINT('Ctrl Pts',(-9.44344724047616E-14,145.681258627559,
10.5686967334885));
#280570=CARTESIAN_POINT('Ctrl Pts',(3.10606203794801,145.831258627559,9.55947599963789));
#280571=CARTESIAN_POINT('Ctrl Pts',(6.21212407589611,145.981258627558,8.55025526578723));
#280572=CARTESIAN_POINT('Ctrl Pts',(8.1317759865138,146.131258627558,5.90808108241509));
#280573=CARTESIAN_POINT('Ctrl Pts',(10.0514278971315,146.281258627557,3.26590689904295));
#280574=CARTESIAN_POINT('Ctrl Pts',(10.0514278971315,146.431258627557,-1.23094490010826E-15));
#280575=CARTESIAN_POINT('Ctrl Pts',(10.0514278971315,146.581258627556,-3.26590689904296));
#280576=CARTESIAN_POINT('Ctrl Pts',(8.1317759865138,146.731258627555,-5.9080810824151));
#280577=CARTESIAN_POINT('Ctrl Pts',(6.2121240758961,146.881258627555,-8.55025526578723));
#280578=CARTESIAN_POINT('Ctrl Pts',(3.106062037948,147.031258627554,-9.55947599963789));
#280579=CARTESIAN_POINT('Ctrl Pts',(-9.78869111657577E-14,147.181258627553,
-10.5686967334885));
#280580=CARTESIAN_POINT('Ctrl Pts',(-3.1060620379482,147.331258627553,-9.55947599963789));
#280581=CARTESIAN_POINT('Ctrl Pts',(-6.2121240758963,147.481258627552,-8.55025526578723));
#280582=CARTESIAN_POINT('Ctrl Pts',(-8.13177598651399,147.631258627552,
-5.90808108241509));
#280583=CARTESIAN_POINT('Ctrl Pts',(-10.0514278971317,147.781258627551,
-3.26590689904296));
#280584=CARTESIAN_POINT('Ctrl Pts',(-10.0514278971317,147.931258627551,
2.46188980021652E-15));
#280585=CARTESIAN_POINT('Ctrl Pts',(-10.0514278971317,148.08125862755,3.26590689904296));
#280586=CARTESIAN_POINT('Ctrl Pts',(-8.13177598651399,148.231258627549,
5.9080810824151));
#280587=CARTESIAN_POINT('Ctrl Pts',(-6.2121240758963,148.381258627549,8.55025526578723));
#280588=CARTESIAN_POINT('Ctrl Pts',(-3.1060620379482,148.531258627548,9.55947599963789));
#280589=CARTESIAN_POINT('Ctrl Pts',(-9.61621816764234E-14,148.681258627547,
10.5686967334885));
#280590=CARTESIAN_POINT('Ctrl Pts',(3.10606203794801,148.831258627547,9.55947599963789));
#280591=CARTESIAN_POINT('Ctrl Pts',(6.21212407589611,148.981258627546,8.55025526578723));
#280592=CARTESIAN_POINT('Ctrl Pts',(8.1317759865138,149.131258627546,5.90808108241509));
#280593=CARTESIAN_POINT('Ctrl Pts',(10.0514278971315,149.281258627545,3.26590689904295));
#280594=CARTESIAN_POINT('Ctrl Pts',(10.0514278971315,149.431258627545,-1.23094490010826E-15));
#280595=CARTESIAN_POINT('Ctrl Pts',(10.0514278971315,149.581258627544,-3.26590689904296));
#280596=CARTESIAN_POINT('Ctrl Pts',(8.1317759865138,149.731258627543,-5.9080810824151));
#280597=CARTESIAN_POINT('Ctrl Pts',(6.2121240758961,149.881258627543,-8.55025526578723));
#280598=CARTESIAN_POINT('Ctrl Pts',(3.106062037948,150.031258627542,-9.55947599963789));
#280599=CARTESIAN_POINT('Ctrl Pts',(-9.96146204374195E-14,150.181258627541,
-10.5686967334885));
#280600=CARTESIAN_POINT('Ctrl Pts',(-3.1060620379482,150.331258627541,-9.55947599963789));
#280601=CARTESIAN_POINT('Ctrl Pts',(-6.2121240758963,150.48125862754,-8.55025526578723));
#280602=CARTESIAN_POINT('Ctrl Pts',(-8.131775986514,150.63125862754,-5.90808108241509));
#280603=CARTESIAN_POINT('Ctrl Pts',(-10.0514278971317,150.781258627539,
-3.26590689904296));
#280604=CARTESIAN_POINT('Ctrl Pts',(-10.0514278971317,150.931258627538,
2.46188980021652E-15));
#280605=CARTESIAN_POINT('Ctrl Pts',(-10.0514278971317,151.081258627538,
3.26590689904296));
#280606=CARTESIAN_POINT('Ctrl Pts',(-8.131775986514,151.231258627537,5.9080810824151));
#280607=CARTESIAN_POINT('Ctrl Pts',(-6.2121240758963,151.381258627537,8.55025526578723));
#280608=CARTESIAN_POINT('Ctrl Pts',(-3.1060620379482,151.531258627536,9.55947599963789));
#280609=CARTESIAN_POINT('Ctrl Pts',(-9.78898909480853E-14,151.681258627535,
10.5686967334885));
#280610=CARTESIAN_POINT('Ctrl Pts',(3.106062037948,151.831258627535,9.55947599963789));
#280611=CARTESIAN_POINT('Ctrl Pts',(6.2121240758961,151.981258627534,8.55025526578723));
#280612=CARTESIAN_POINT('Ctrl Pts',(8.13177598651379,152.131258627534,5.90808108241509));
#280613=CARTESIAN_POINT('Ctrl Pts',(10.0514278971315,152.281258627533,3.26590689904295));
#280614=CARTESIAN_POINT('Ctrl Pts',(10.0514278971315,152.431258627532,-1.23094490010826E-15));
#280615=CARTESIAN_POINT('Ctrl Pts',(10.0514278971315,152.581258627532,-3.26590689904296));
#280616=CARTESIAN_POINT('Ctrl Pts',(8.13177598651379,152.731258627531,-5.9080810824151));
#280617=CARTESIAN_POINT('Ctrl Pts',(6.2121240758961,152.881258627531,-8.55025526578723));
#280618=CARTESIAN_POINT('Ctrl Pts',(3.106062037948,153.03125862753,-9.55947599963789));
#280619=CARTESIAN_POINT('Ctrl Pts',(-1.01342329709081E-13,153.181258627529,
-10.5686967334885));
#280620=CARTESIAN_POINT('Ctrl Pts',(-3.1060620379482,153.331258627529,-9.55947599963789));
#280621=CARTESIAN_POINT('Ctrl Pts',(10.0514428414941,95.4312499996288,-1.23094673026484E-15));
#280622=CARTESIAN_POINT('Ctrl Pts',(10.0514428414941,95.5812499996282,-3.26591175476071));
#280623=CARTESIAN_POINT('Ctrl Pts',(8.13178807675712,95.7312499996276,-5.90808986649102));
#280624=CARTESIAN_POINT('Ctrl Pts',(6.21213331202015,95.8812499996269,-8.55026797822134));
#280625=CARTESIAN_POINT('Ctrl Pts',(3.10606665601004,96.0312499996264,-9.5594902125713));
#280626=CARTESIAN_POINT('Ctrl Pts',(-6.85158495407089E-14,96.1812499996257,
-10.5687124469213));
#280627=CARTESIAN_POINT('Ctrl Pts',(-3.10606665601018,96.3312499996252,
-9.5594902125713));
#280628=CARTESIAN_POINT('Ctrl Pts',(-6.21213331202028,96.4812499996245,
-8.55026797822134));
#280629=CARTESIAN_POINT('Ctrl Pts',(-8.13178807675726,96.6312499996239,
-5.90808986649102));
#280630=CARTESIAN_POINT('Ctrl Pts',(-10.0514428414942,96.7812499996234,
-3.2659117547607));
#280631=CARTESIAN_POINT('Ctrl Pts',(-10.0514428414942,96.9312499996227,
2.46189346052968E-15));
#280632=CARTESIAN_POINT('Ctrl Pts',(-10.0514428414942,97.0812499996221,
3.26591175476071));
#280633=CARTESIAN_POINT('Ctrl Pts',(-8.13178807675726,97.2312499996215,
5.90808986649102));
#280634=CARTESIAN_POINT('Ctrl Pts',(-6.21213331202028,97.381249999621,8.55026797822134));
#280635=CARTESIAN_POINT('Ctrl Pts',(-3.10606665601017,97.5312499996203,
9.5594902125713));
#280636=CARTESIAN_POINT('Ctrl Pts',(-6.67911162026936E-14,97.6812499996198,
10.5687124469213));
#280637=CARTESIAN_POINT('Ctrl Pts',(3.10606665601004,97.8312499996191,9.5594902125713));
#280638=CARTESIAN_POINT('Ctrl Pts',(6.21213331202015,97.9812499996186,8.55026797822134));
#280639=CARTESIAN_POINT('Ctrl Pts',(8.13178807675712,98.1312499996179,5.90808986649102));
#280640=CARTESIAN_POINT('Ctrl Pts',(10.0514428414941,98.2812499996173,3.2659117547607));
#280641=CARTESIAN_POINT('Ctrl Pts',(10.0514428414941,98.4312499996168,-1.23094673026484E-15));
#280642=CARTESIAN_POINT('Origin',(-3.77475828372553E-14,-1.881249999982,
2.68644078414671E-15));
#280643=CARTESIAN_POINT('Origin',(-3.77475828372553E-14,-1.881249999982,
2.68644078414671E-15));
#280644=CARTESIAN_POINT('',(10.0514428414941,17.4312499999408,1.37532313762869E-15));
#280645=CARTESIAN_POINT('',(10.0514428414941,17.8062499999393,1.37376642080824E-15));
#280646=CARTESIAN_POINT('',(10.0514428414941,-1.881249999982,4.14193483802857E-15));
#280647=CARTESIAN_POINT('',(-7.47704554734297,18.9576928414942,-6.71753623576259));
#280648=CARTESIAN_POINT('Ctrl Pts',(10.0514428414941,17.8062499999393,-1.23094673026484E-15));
#280649=CARTESIAN_POINT('Ctrl Pts',(10.0514428414941,17.9562499999387,-3.26591175476071));
#280650=CARTESIAN_POINT('Ctrl Pts',(8.13178807675717,18.1062499999381,-5.90808986649102));
#280651=CARTESIAN_POINT('Ctrl Pts',(6.21213331202019,18.2562499999375,-8.55026797822134));
#280652=CARTESIAN_POINT('Ctrl Pts',(3.10606665601008,18.4062499999369,-9.5594902125713));
#280653=CARTESIAN_POINT('Ctrl Pts',(-2.38113721364588E-14,18.5562499999362,
-10.5687124469213));
#280654=CARTESIAN_POINT('Ctrl Pts',(-3.10606665601013,18.7062499999357,
-9.5594902125713));
#280655=CARTESIAN_POINT('Ctrl Pts',(-5.67314056620243,18.8302206448612,
-8.72539733746421));
#280656=CARTESIAN_POINT('Ctrl Pts',(-7.47704554734297,18.9576928414942,
-6.71753623576259));
#280657=CARTESIAN_POINT('',(-10.0352413152989,18.9576928414942,0.570469052221818));
#280658=CARTESIAN_POINT('Origin',(-3.33066907387547E-14,18.9576928414942,
-4.01761957036229E-14));
#280659=CARTESIAN_POINT('Ctrl Pts',(10.0514428414941,17.4312499999408,-1.23094673026484E-15));
#280660=CARTESIAN_POINT('Ctrl Pts',(10.0514428414941,17.5812499999402,-3.26591175476071));
#280661=CARTESIAN_POINT('Ctrl Pts',(8.13178807675717,17.7312499999396,-5.90808986649102));
#280662=CARTESIAN_POINT('Ctrl Pts',(6.21213331202019,17.881249999939,-8.55026797822134));
#280663=CARTESIAN_POINT('Ctrl Pts',(3.10606665601008,18.0312499999384,-9.5594902125713));
#280664=CARTESIAN_POINT('Ctrl Pts',(-2.35954084775011E-14,18.1812499999378,
-10.5687124469213));
#280665=CARTESIAN_POINT('Ctrl Pts',(-3.10606665601013,18.3312499999371,
-9.5594902125713));
#280666=CARTESIAN_POINT('Ctrl Pts',(-6.21213331202024,18.4812499999365,
-8.55026797822134));
#280667=CARTESIAN_POINT('Ctrl Pts',(-8.13178807675721,18.6312499999359,
-5.90808986649102));
#280668=CARTESIAN_POINT('Ctrl Pts',(-10.0514428414942,18.7812499999353,
-3.2659117547607));
#280669=CARTESIAN_POINT('Ctrl Pts',(-10.0514428414942,18.9312499999347,
2.46189346052968E-15));
#280670=CARTESIAN_POINT('Ctrl Pts',(-10.0514428414942,18.9443610977903,
0.285464590696237));
#280671=CARTESIAN_POINT('Ctrl Pts',(-10.0352413152989,18.9576928414942,
0.570469052221818));
#280672=CARTESIAN_POINT('Origin',(-3.77475828372553E-14,-1.881249999982,
2.68644078414671E-15));
#280673=CARTESIAN_POINT('',(10.0514428414941,14.4312499999528,1.38777687219229E-15));
#280674=CARTESIAN_POINT('',(10.0514428414941,14.8062499999513,1.38622015537184E-15));
#280675=CARTESIAN_POINT('',(10.0514428414941,-1.881249999982,4.14193483802857E-15));
#280676=CARTESIAN_POINT('Ctrl Pts',(10.0514428414941,14.8062499999513,-1.23094673026484E-15));
#280677=CARTESIAN_POINT('Ctrl Pts',(10.0514428414941,14.9562499999507,-3.26591175476071));
#280678=CARTESIAN_POINT('Ctrl Pts',(8.13178807675717,15.1062499999501,-5.90808986649102));
#280679=CARTESIAN_POINT('Ctrl Pts',(6.21213331202019,15.2562499999495,-8.55026797822134));
#280680=CARTESIAN_POINT('Ctrl Pts',(3.10606665601009,15.4062499999489,-9.5594902125713));
#280681=CARTESIAN_POINT('Ctrl Pts',(-2.2083662864797E-14,15.5562499999482,
-10.5687124469213));
#280682=CARTESIAN_POINT('Ctrl Pts',(-3.10606665601013,15.7062499999477,
-9.5594902125713));
#280683=CARTESIAN_POINT('Ctrl Pts',(-6.21213331202024,15.856249999947,-8.55026797822134));
#280684=CARTESIAN_POINT('Ctrl Pts',(-8.13178807675721,16.0062499999464,
-5.90808986649102));
#280685=CARTESIAN_POINT('Ctrl Pts',(-10.0514428414942,16.1562499999458,
-3.2659117547607));
#280686=CARTESIAN_POINT('Ctrl Pts',(-10.0514428414942,16.3062499999452,
2.46189346052968E-15));
#280687=CARTESIAN_POINT('Ctrl Pts',(-10.0514428414942,16.4562499999446,
3.26591175476071));
#280688=CARTESIAN_POINT('Ctrl Pts',(-8.13178807675721,16.606249999944,5.90808986649102));
#280689=CARTESIAN_POINT('Ctrl Pts',(-6.21213331202024,16.7562499999434,
8.55026797822134));
#280690=CARTESIAN_POINT('Ctrl Pts',(-3.10606665601013,16.9062499999428,
9.5594902125713));
#280691=CARTESIAN_POINT('Ctrl Pts',(-2.03589295267817E-14,17.0562499999422,
10.5687124469213));
#280692=CARTESIAN_POINT('Ctrl Pts',(3.10606665601009,17.2062499999417,9.5594902125713));
#280693=CARTESIAN_POINT('Ctrl Pts',(6.2121333120202,17.3562499999411,8.55026797822134));
#280694=CARTESIAN_POINT('Ctrl Pts',(8.13178807675717,17.5062499999405,5.90808986649102));
#280695=CARTESIAN_POINT('Ctrl Pts',(10.0514428414941,17.6562499999399,3.2659117547607));
#280696=CARTESIAN_POINT('Ctrl Pts',(10.0514428414941,17.8062499999393,-1.23094673026484E-15));
#280697=CARTESIAN_POINT('Ctrl Pts',(10.0514428414941,14.4312499999528,-1.23094673026484E-15));
#280698=CARTESIAN_POINT('Ctrl Pts',(10.0514428414941,14.5812499999522,-3.26591175476071));
#280699=CARTESIAN_POINT('Ctrl Pts',(8.13178807675717,14.7312499999516,-5.90808986649102));
#280700=CARTESIAN_POINT('Ctrl Pts',(6.21213331202019,14.881249999951,-8.55026797822134));
#280701=CARTESIAN_POINT('Ctrl Pts',(3.10606665601009,15.0312499999504,-9.5594902125713));
#280702=CARTESIAN_POINT('Ctrl Pts',(-2.18676992058392E-14,15.1812499999498,
-10.5687124469213));
#280703=CARTESIAN_POINT('Ctrl Pts',(-3.10606665601013,15.3312499999492,
-9.5594902125713));
#280704=CARTESIAN_POINT('Ctrl Pts',(-6.21213331202024,15.4812499999485,
-8.55026797822134));
#280705=CARTESIAN_POINT('Ctrl Pts',(-8.13178807675721,15.6312499999479,
-5.90808986649102));
#280706=CARTESIAN_POINT('Ctrl Pts',(-10.0514428414942,15.7812499999473,
-3.2659117547607));
#280707=CARTESIAN_POINT('Ctrl Pts',(-10.0514428414942,15.9312499999467,
2.46189346052968E-15));
#280708=CARTESIAN_POINT('Ctrl Pts',(-10.0514428414942,16.0812499999461,
3.26591175476071));
#280709=CARTESIAN_POINT('Ctrl Pts',(-8.13178807675721,16.2312499999455,
5.90808986649102));
#280710=CARTESIAN_POINT('Ctrl Pts',(-6.21213331202024,16.3812499999449,
8.55026797822134));
#280711=CARTESIAN_POINT('Ctrl Pts',(-3.10606665601013,16.5312499999444,
9.5594902125713));
#280712=CARTESIAN_POINT('Ctrl Pts',(-2.0142965867824E-14,16.6812499999438,
10.5687124469213));
#280713=CARTESIAN_POINT('Ctrl Pts',(3.10606665601009,16.8312499999432,9.5594902125713));
#280714=CARTESIAN_POINT('Ctrl Pts',(6.2121333120202,16.9812499999426,8.55026797822134));
#280715=CARTESIAN_POINT('Ctrl Pts',(8.13178807675717,17.131249999942,5.90808986649102));
#280716=CARTESIAN_POINT('Ctrl Pts',(10.0514428414941,17.2812499999414,3.2659117547607));
#280717=CARTESIAN_POINT('Ctrl Pts',(10.0514428414941,17.4312499999408,-1.23094673026484E-15));
#280718=CARTESIAN_POINT('Origin',(-3.77475828372553E-14,-1.881249999982,
2.68644078414671E-15));
#280719=CARTESIAN_POINT('',(10.0514428414941,11.4312499999648,1.40023060675589E-15));
#280720=CARTESIAN_POINT('',(10.0514428414941,11.8062499999633,1.39867388993544E-15));
#280721=CARTESIAN_POINT('',(10.0514428414941,-1.881249999982,4.14193483802857E-15));
#280722=CARTESIAN_POINT('Ctrl Pts',(10.0514428414941,11.8062499999633,-1.23094673026484E-15));
#280723=CARTESIAN_POINT('Ctrl Pts',(10.0514428414941,11.9562499999627,-3.26591175476071));
#280724=CARTESIAN_POINT('Ctrl Pts',(8.13178807675717,12.1062499999621,-5.90808986649102));
#280725=CARTESIAN_POINT('Ctrl Pts',(6.2121333120202,12.2562499999615,-8.55026797822134));
#280726=CARTESIAN_POINT('Ctrl Pts',(3.10606665601009,12.4062499999609,-9.5594902125713));
#280727=CARTESIAN_POINT('Ctrl Pts',(-2.03559535931351E-14,12.5562499999603,
-10.5687124469213));
#280728=CARTESIAN_POINT('Ctrl Pts',(-3.10606665601013,12.7062499999597,
-9.5594902125713));
#280729=CARTESIAN_POINT('Ctrl Pts',(-6.21213331202024,12.856249999959,-8.55026797822134));
#280730=CARTESIAN_POINT('Ctrl Pts',(-8.13178807675721,13.0062499999584,
-5.90808986649102));
#280731=CARTESIAN_POINT('Ctrl Pts',(-10.0514428414942,13.1562499999578,
-3.2659117547607));
#280732=CARTESIAN_POINT('Ctrl Pts',(-10.0514428414942,13.3062499999572,
2.46189346052968E-15));
#280733=CARTESIAN_POINT('Ctrl Pts',(-10.0514428414942,13.4562499999566,
3.26591175476071));
#280734=CARTESIAN_POINT('Ctrl Pts',(-8.13178807675721,13.606249999956,5.90808986649102));
#280735=CARTESIAN_POINT('Ctrl Pts',(-6.21213331202023,13.7562499999554,
8.55026797822134));
#280736=CARTESIAN_POINT('Ctrl Pts',(-3.10606665601013,13.9062499999549,
9.5594902125713));
#280737=CARTESIAN_POINT('Ctrl Pts',(-1.86312202551199E-14,14.0562499999543,
10.5687124469213));
#280738=CARTESIAN_POINT('Ctrl Pts',(3.10606665601009,14.2062499999537,9.5594902125713));
#280739=CARTESIAN_POINT('Ctrl Pts',(6.2121333120202,14.3562499999531,8.55026797822134));
#280740=CARTESIAN_POINT('Ctrl Pts',(8.13178807675717,14.5062499999525,5.90808986649102));
#280741=CARTESIAN_POINT('Ctrl Pts',(10.0514428414941,14.6562499999519,3.2659117547607));
#280742=CARTESIAN_POINT('Ctrl Pts',(10.0514428414941,14.8062499999513,-1.23094673026484E-15));
#280743=CARTESIAN_POINT('Ctrl Pts',(10.0514428414941,11.4312499999648,-1.23094673026484E-15));
#280744=CARTESIAN_POINT('Ctrl Pts',(10.0514428414941,11.5812499999642,-3.26591175476071));
#280745=CARTESIAN_POINT('Ctrl Pts',(8.13178807675717,11.7312499999636,-5.90808986649102));
#280746=CARTESIAN_POINT('Ctrl Pts',(6.2121333120202,11.881249999963,-8.55026797822134));
#280747=CARTESIAN_POINT('Ctrl Pts',(3.10606665601009,12.0312499999624,-9.5594902125713));
#280748=CARTESIAN_POINT('Ctrl Pts',(-2.01399899341774E-14,12.1812499999618,
-10.5687124469213));
#280749=CARTESIAN_POINT('Ctrl Pts',(-3.10606665601013,12.3312499999612,
-9.5594902125713));
#280750=CARTESIAN_POINT('Ctrl Pts',(-6.21213331202024,12.4812499999605,
-8.55026797822134));
#280751=CARTESIAN_POINT('Ctrl Pts',(-8.13178807675721,12.6312499999599,
-5.90808986649102));
#280752=CARTESIAN_POINT('Ctrl Pts',(-10.0514428414942,12.7812499999593,
-3.2659117547607));
#280753=CARTESIAN_POINT('Ctrl Pts',(-10.0514428414942,12.9312499999587,
2.46189346052968E-15));
#280754=CARTESIAN_POINT('Ctrl Pts',(-10.0514428414942,13.0812499999581,
3.26591175476071));
#280755=CARTESIAN_POINT('Ctrl Pts',(-8.13178807675721,13.2312499999575,
5.90808986649102));
#280756=CARTESIAN_POINT('Ctrl Pts',(-6.21213331202023,13.3812499999569,
8.55026797822134));
#280757=CARTESIAN_POINT('Ctrl Pts',(-3.10606665601013,13.5312499999564,
9.5594902125713));
#280758=CARTESIAN_POINT('Ctrl Pts',(-1.84152565961621E-14,13.6812499999558,
10.5687124469213));
#280759=CARTESIAN_POINT('Ctrl Pts',(3.10606665601009,13.8312499999552,9.5594902125713));
#280760=CARTESIAN_POINT('Ctrl Pts',(6.2121333120202,13.9812499999546,8.55026797822134));
#280761=CARTESIAN_POINT('Ctrl Pts',(8.13178807675717,14.131249999954,5.90808986649102));
#280762=CARTESIAN_POINT('Ctrl Pts',(10.0514428414941,14.2812499999534,3.2659117547607));
#280763=CARTESIAN_POINT('Ctrl Pts',(10.0514428414941,14.4312499999528,-1.23094673026484E-15));
#280764=CARTESIAN_POINT('Origin',(-3.77475828372553E-14,-1.881249999982,
2.68644078414671E-15));
#280765=CARTESIAN_POINT('',(10.0514428414941,8.43124999997676,1.41268434131949E-15));
#280766=CARTESIAN_POINT('',(10.0514428414941,8.80624999997526,1.41112762449904E-15));
#280767=CARTESIAN_POINT('',(10.0514428414941,-1.881249999982,4.14193483802857E-15));
#280768=CARTESIAN_POINT('Ctrl Pts',(10.0514428414941,8.80624999997526,-1.23094673026484E-15));
#280769=CARTESIAN_POINT('Ctrl Pts',(10.0514428414941,8.95624999997466,-3.26591175476071));
#280770=CARTESIAN_POINT('Ctrl Pts',(8.13178807675717,9.10624999997406,-5.90808986649102));
#280771=CARTESIAN_POINT('Ctrl Pts',(6.2121333120202,9.25624999997346,-8.55026797822134));
#280772=CARTESIAN_POINT('Ctrl Pts',(3.10606665601009,9.40624999997286,-9.5594902125713));
#280773=CARTESIAN_POINT('Ctrl Pts',(-1.86282443214733E-14,9.55624999997225,
-10.5687124469213));
#280774=CARTESIAN_POINT('Ctrl Pts',(-3.10606665601013,9.70624999997165,
-9.5594902125713));
#280775=CARTESIAN_POINT('Ctrl Pts',(-6.21213331202024,9.85624999997105,
-8.55026797822134));
#280776=CARTESIAN_POINT('Ctrl Pts',(-8.13178807675721,10.0062499999704,
-5.90808986649102));
#280777=CARTESIAN_POINT('Ctrl Pts',(-10.0514428414942,10.1562499999698,
-3.2659117547607));
#280778=CARTESIAN_POINT('Ctrl Pts',(-10.0514428414942,10.3062499999692,
2.46189346052968E-15));
#280779=CARTESIAN_POINT('Ctrl Pts',(-10.0514428414942,10.4562499999686,
3.26591175476071));
#280780=CARTESIAN_POINT('Ctrl Pts',(-8.13178807675721,10.606249999968,5.90808986649102));
#280781=CARTESIAN_POINT('Ctrl Pts',(-6.21213331202023,10.7562499999674,
8.55026797822134));
#280782=CARTESIAN_POINT('Ctrl Pts',(-3.10606665601013,10.9062499999668,
9.5594902125713));
#280783=CARTESIAN_POINT('Ctrl Pts',(-1.6903510983458E-14,11.0562499999663,
10.5687124469213));
#280784=CARTESIAN_POINT('Ctrl Pts',(3.10606665601009,11.2062499999657,9.5594902125713));
#280785=CARTESIAN_POINT('Ctrl Pts',(6.2121333120202,11.3562499999651,8.55026797822134));
#280786=CARTESIAN_POINT('Ctrl Pts',(8.13178807675717,11.5062499999645,5.90808986649102));
#280787=CARTESIAN_POINT('Ctrl Pts',(10.0514428414941,11.6562499999639,3.2659117547607));
#280788=CARTESIAN_POINT('Ctrl Pts',(10.0514428414941,11.8062499999633,-1.23094673026484E-15));
#280789=CARTESIAN_POINT('Ctrl Pts',(10.0514428414941,8.43124999997676,-1.23094673026484E-15));
#280790=CARTESIAN_POINT('Ctrl Pts',(10.0514428414941,8.58124999997616,-3.26591175476071));
#280791=CARTESIAN_POINT('Ctrl Pts',(8.13178807675717,8.73124999997556,-5.90808986649102));
#280792=CARTESIAN_POINT('Ctrl Pts',(6.2121333120202,8.88124999997496,-8.55026797822134));
#280793=CARTESIAN_POINT('Ctrl Pts',(3.10606665601009,9.03124999997436,-9.5594902125713));
#280794=CARTESIAN_POINT('Ctrl Pts',(-1.84122806625156E-14,9.18124999997375,
-10.5687124469213));
#280795=CARTESIAN_POINT('Ctrl Pts',(-3.10606665601013,9.33124999997315,
-9.5594902125713));
#280796=CARTESIAN_POINT('Ctrl Pts',(-6.21213331202024,9.48124999997255,
-8.55026797822134));
#280797=CARTESIAN_POINT('Ctrl Pts',(-8.13178807675721,9.63124999997195,
-5.90808986649102));
#280798=CARTESIAN_POINT('Ctrl Pts',(-10.0514428414942,9.78124999997135,
-3.2659117547607));
#280799=CARTESIAN_POINT('Ctrl Pts',(-10.0514428414942,9.93124999997075,
2.46189346052968E-15));
#280800=CARTESIAN_POINT('Ctrl Pts',(-10.0514428414942,10.0812499999701,
3.26591175476071));
#280801=CARTESIAN_POINT('Ctrl Pts',(-8.13178807675721,10.2312499999695,
5.90808986649102));
#280802=CARTESIAN_POINT('Ctrl Pts',(-6.21213331202023,10.3812499999689,
8.55026797822134));
#280803=CARTESIAN_POINT('Ctrl Pts',(-3.10606665601012,10.5312499999684,
9.5594902125713));
#280804=CARTESIAN_POINT('Ctrl Pts',(-1.66875473245003E-14,10.6812499999678,
10.5687124469213));
#280805=CARTESIAN_POINT('Ctrl Pts',(3.10606665601009,10.8312499999672,9.5594902125713));
#280806=CARTESIAN_POINT('Ctrl Pts',(6.2121333120202,10.9812499999666,8.55026797822134));
#280807=CARTESIAN_POINT('Ctrl Pts',(8.13178807675717,11.131249999966,5.90808986649102));
#280808=CARTESIAN_POINT('Ctrl Pts',(10.0514428414941,11.2812499999654,3.2659117547607));
#280809=CARTESIAN_POINT('Ctrl Pts',(10.0514428414941,11.4312499999648,-1.23094673026484E-15));
#280810=CARTESIAN_POINT('Origin',(-3.77475828372553E-14,-1.881249999982,
2.68644078414671E-15));
#280811=CARTESIAN_POINT('',(10.0514428414941,5.43124999998876,1.42513807588309E-15));
#280812=CARTESIAN_POINT('',(10.0514428414941,5.80624999998726,1.42358135906264E-15));
#280813=CARTESIAN_POINT('',(10.0514428414941,-1.881249999982,4.14193483802857E-15));
#280814=CARTESIAN_POINT('Ctrl Pts',(10.0514428414941,5.80624999998726,-1.23094673026484E-15));
#280815=CARTESIAN_POINT('Ctrl Pts',(10.0514428414941,5.95624999998666,-3.26591175476071));
#280816=CARTESIAN_POINT('Ctrl Pts',(8.13178807675717,6.10624999998606,-5.90808986649102));
#280817=CARTESIAN_POINT('Ctrl Pts',(6.2121333120202,6.25624999998545,-8.55026797822134));
#280818=CARTESIAN_POINT('Ctrl Pts',(3.10606665601009,6.40624999998485,-9.5594902125713));
#280819=CARTESIAN_POINT('Ctrl Pts',(-1.69005350498115E-14,6.55624999998425,
-10.5687124469213));
#280820=CARTESIAN_POINT('Ctrl Pts',(-3.10606665601013,6.70624999998365,
-9.5594902125713));
#280821=CARTESIAN_POINT('Ctrl Pts',(-6.21213331202023,6.85624999998305,
-8.55026797822134));
#280822=CARTESIAN_POINT('Ctrl Pts',(-8.13178807675721,7.00624999998245,
-5.90808986649102));
#280823=CARTESIAN_POINT('Ctrl Pts',(-10.0514428414942,7.15624999998185,
-3.2659117547607));
#280824=CARTESIAN_POINT('Ctrl Pts',(-10.0514428414942,7.30624999998125,
2.46189346052968E-15));
#280825=CARTESIAN_POINT('Ctrl Pts',(-10.0514428414942,7.45624999998065,
3.26591175476071));
#280826=CARTESIAN_POINT('Ctrl Pts',(-8.13178807675721,7.60624999998005,
5.90808986649102));
#280827=CARTESIAN_POINT('Ctrl Pts',(-6.21213331202023,7.75624999997945,
8.55026797822134));
#280828=CARTESIAN_POINT('Ctrl Pts',(-3.10606665601012,7.90624999997885,
9.5594902125713));
#280829=CARTESIAN_POINT('Ctrl Pts',(-1.51758017117962E-14,8.05624999997825,
10.5687124469213));
#280830=CARTESIAN_POINT('Ctrl Pts',(3.10606665601009,8.20624999997765,9.5594902125713));
#280831=CARTESIAN_POINT('Ctrl Pts',(6.2121333120202,8.35624999997706,8.55026797822134));
#280832=CARTESIAN_POINT('Ctrl Pts',(8.13178807675717,8.50624999997646,5.90808986649102));
#280833=CARTESIAN_POINT('Ctrl Pts',(10.0514428414941,8.65624999997586,3.2659117547607));
#280834=CARTESIAN_POINT('Ctrl Pts',(10.0514428414941,8.80624999997526,-1.23094673026484E-15));
#280835=CARTESIAN_POINT('Ctrl Pts',(10.0514428414941,5.43124999998876,-1.23094673026484E-15));
#280836=CARTESIAN_POINT('Ctrl Pts',(10.0514428414941,5.58124999998816,-3.26591175476071));
#280837=CARTESIAN_POINT('Ctrl Pts',(8.13178807675717,5.73124999998756,-5.90808986649102));
#280838=CARTESIAN_POINT('Ctrl Pts',(6.2121333120202,5.88124999998695,-8.55026797822134));
#280839=CARTESIAN_POINT('Ctrl Pts',(3.10606665601009,6.03124999998635,-9.5594902125713));
#280840=CARTESIAN_POINT('Ctrl Pts',(-1.66845713908537E-14,6.18124999998575,
-10.5687124469213));
#280841=CARTESIAN_POINT('Ctrl Pts',(-3.10606665601012,6.33124999998515,
-9.5594902125713));
#280842=CARTESIAN_POINT('Ctrl Pts',(-6.21213331202023,6.48124999998455,
-8.55026797822134));
#280843=CARTESIAN_POINT('Ctrl Pts',(-8.13178807675721,6.63124999998395,
-5.90808986649102));
#280844=CARTESIAN_POINT('Ctrl Pts',(-10.0514428414942,6.78124999998335,
-3.2659117547607));
#280845=CARTESIAN_POINT('Ctrl Pts',(-10.0514428414942,6.93124999998275,
2.46189346052968E-15));
#280846=CARTESIAN_POINT('Ctrl Pts',(-10.0514428414942,7.08124999998215,
3.26591175476071));
#280847=CARTESIAN_POINT('Ctrl Pts',(-8.13178807675721,7.23124999998155,
5.90808986649102));
#280848=CARTESIAN_POINT('Ctrl Pts',(-6.21213331202023,7.38124999998095,
8.55026797822134));
#280849=CARTESIAN_POINT('Ctrl Pts',(-3.10606665601012,7.53124999998035,
9.5594902125713));
#280850=CARTESIAN_POINT('Ctrl Pts',(-1.49598380528385E-14,7.68124999997975,
10.5687124469213));
#280851=CARTESIAN_POINT('Ctrl Pts',(3.10606665601009,7.83124999997915,9.5594902125713));
#280852=CARTESIAN_POINT('Ctrl Pts',(6.2121333120202,7.98124999997856,8.55026797822134));
#280853=CARTESIAN_POINT('Ctrl Pts',(8.13178807675717,8.13124999997796,5.90808986649102));
#280854=CARTESIAN_POINT('Ctrl Pts',(10.0514428414941,8.28124999997736,3.2659117547607));
#280855=CARTESIAN_POINT('Ctrl Pts',(10.0514428414941,8.43124999997676,-1.23094673026484E-15));
#280856=CARTESIAN_POINT('Origin',(-3.77475828372553E-14,-1.881249999982,
2.68644078414671E-15));
#280857=CARTESIAN_POINT('',(10.0514428414942,2.43125000000076,-1.23094673026484E-15));
#280858=CARTESIAN_POINT('',(10.0514428414942,2.80624999999926,1.43603509362624E-15));
#280859=CARTESIAN_POINT('',(10.0514428414941,-1.881249999982,4.14193483802857E-15));
#280860=CARTESIAN_POINT('',(7.09357268597966,2.43124999999995,7.12128708482866));
#280861=CARTESIAN_POINT('Origin',(-3.77475828372553E-14,2.43125000000001,
2.65063629727636E-15));
#280862=CARTESIAN_POINT('Ctrl Pts',(7.09357268597966,2.43124999999995,7.12128708482865));
#280863=CARTESIAN_POINT('Ctrl Pts',(7.66101577103565,2.46946429917804,6.55605235674466));
#280864=CARTESIAN_POINT('Ctrl Pts',(8.13178807675718,2.50625000000046,5.90808986649102));
#280865=CARTESIAN_POINT('Ctrl Pts',(10.0514428414941,2.65624999999986,3.2659117547607));
#280866=CARTESIAN_POINT('Ctrl Pts',(10.0514428414942,2.80624999999926,-1.23094673026484E-15));
#280867=CARTESIAN_POINT('Origin',(-8.79029313101884E-14,130.96875,0.));
#280868=CARTESIAN_POINT('',(-12.,2.80625000000003,-1.96085794981161E-14));
#280869=CARTESIAN_POINT('',(-12.,2.43125,1.10010189965134E-12));
#280870=CARTESIAN_POINT('',(-12.0000000000001,130.96875,-1.46957615897682E-15));
#280871=CARTESIAN_POINT('',(-8.46872171229246,2.43125,-8.50180878165034));
#280872=CARTESIAN_POINT('Origin',(-1.38777878078145E-14,2.43125000000001,
0.));
#280873=CARTESIAN_POINT('Ctrl Pts',(-8.46872171229245,2.43125000000001,
-8.50180878165033));
#280874=CARTESIAN_POINT('Ctrl Pts',(-9.32728045918118,2.47968070262409,
-7.64659134642077));
#280875=CARTESIAN_POINT('Ctrl Pts',(-10.0513334781109,2.52543312431401,
-6.66627458127563));
#280876=CARTESIAN_POINT('Ctrl Pts',(-11.1884451683539,2.62266495898495,
-4.50834151140613));
#280877=CARTESIAN_POINT('Ctrl Pts',(-11.5906585726304,2.67259700712619,
-3.34111609539217));
#280878=CARTESIAN_POINT('Ctrl Pts',(-11.9363235172771,2.75052914174481,
-1.42769460363205));
#280879=CARTESIAN_POINT('Ctrl Pts',(-12.,2.77879127135541,-0.713750541615098));
#280880=CARTESIAN_POINT('Ctrl Pts',(-12.,2.80625000000003,-5.06539254985228E-14));
#280881=CARTESIAN_POINT('Origin',(-8.79029313101884E-14,130.96875,0.));
#280882=CARTESIAN_POINT('',(-12.,5.80624999998803,-4.62056866567646E-15));
#280883=CARTESIAN_POINT('',(-12.,5.43124999998796,-4.13484609240295E-15));
#280884=CARTESIAN_POINT('',(-12.0000000000001,130.96875,-1.46957615897682E-15));
#280885=CARTESIAN_POINT('Ctrl Pts',(-12.,5.43124999998796,4.9960036108132E-15));
#280886=CARTESIAN_POINT('Ctrl Pts',(-12.,5.40428200239846,-0.700994686785967));
#280887=CARTESIAN_POINT('Ctrl Pts',(-11.9385791761269,5.37653721513424,
-1.40222407934875));
#280888=CARTESIAN_POINT('Ctrl Pts',(-11.5422824562796,5.28562275763319,
-3.63665130268098));
#280889=CARTESIAN_POINT('Ctrl Pts',(-10.9700963138265,5.22180961683611,
-5.10946846096972));
#280890=CARTESIAN_POINT('Ctrl Pts',(-9.28827941189608,5.09885547079727,
-7.75903092660924));
#280891=CARTESIAN_POINT('Ctrl Pts',(-8.1922204615954,5.03753038515127,-8.90855617332867));
#280892=CARTESIAN_POINT('Ctrl Pts',(-5.64057798654912,4.91133636385716,
-10.7040514558091));
#280893=CARTESIAN_POINT('Ctrl Pts',(-4.21524104342245,4.85176008196607,
-11.3412762233036));
#280894=CARTESIAN_POINT('Ctrl Pts',(-1.17023092617838,4.72858683532187,
-12.0467059546444));
#280895=CARTESIAN_POINT('Ctrl Pts',(0.423111701583647,4.66413477213606,
-12.0960096253919));
#280896=CARTESIAN_POINT('Ctrl Pts',(3.51417952374597,4.53909845219181,-11.5788354443557));
#280897=CARTESIAN_POINT('Ctrl Pts',(4.98367674661455,4.48032563488727,-11.0264140689132));
#280898=CARTESIAN_POINT('Ctrl Pts',(7.63013890652938,4.35484690042301,-9.39151076963458));
#280899=CARTESIAN_POINT('Ctrl Pts',(8.78201790847445,4.29177961540221,-8.32442149108578));
#280900=CARTESIAN_POINT('Ctrl Pts',(10.635591354955,4.17064285077446,-5.78081719216585));
#280901=CARTESIAN_POINT('Ctrl Pts',(11.30784934581,4.10611725611296,-4.32053187885184));
#280902=CARTESIAN_POINT('Ctrl Pts',(12.0328413602885,3.97956051015913,-1.26643370783079));
#280903=CARTESIAN_POINT('Ctrl Pts',(12.0957398630745,3.92114872416738,0.293676045080488));
#280904=CARTESIAN_POINT('Ctrl Pts',(11.622503343012,3.79676377226967,3.37312184167239));
#280905=CARTESIAN_POINT('Ctrl Pts',(11.082537936312,3.73273968963923,4.86189128414743));
#280906=CARTESIAN_POINT('Ctrl Pts',(9.46095966411316,3.6091956348989,7.5463603035485));
#280907=CARTESIAN_POINT('Ctrl Pts',(8.39532255435243,3.54874538525415,8.71641626394015));
#280908=CARTESIAN_POINT('Ctrl Pts',(5.89011077929842,3.42271378370603,10.5689867933497));
#280909=CARTESIAN_POINT('Ctrl Pts',(4.47886390989561,3.36242385092618,11.2399520266556));
#280910=CARTESIAN_POINT('Ctrl Pts',(1.44631951535773,3.23975485335779,12.0171624969201));
#280911=CARTESIAN_POINT('Ctrl Pts',(-0.149203109815072,3.17521460742432,
12.1029588003197));
#280912=CARTESIAN_POINT('Ctrl Pts',(-3.25156538805228,3.04972141713474,
11.6548964093293));
#280913=CARTESIAN_POINT('Ctrl Pts',(-4.73023611067824,2.99125037257615,
11.1370609190304));
#280914=CARTESIAN_POINT('Ctrl Pts',(-7.41410523834579,2.86600701276808,
9.5635433962468));
#280915=CARTESIAN_POINT('Ctrl Pts',(-8.59255202546376,2.80264162533294,
8.52048379977188));
#280916=CARTESIAN_POINT('Ctrl Pts',(-10.3307866758556,2.69161560353399,
6.24337183292708));
#280917=CARTESIAN_POINT('Ctrl Pts',(-10.9484046682807,2.63994593786912,
5.08306962327767));
#280918=CARTESIAN_POINT('Ctrl Pts',(-11.7861867448544,2.53421964839238,
2.6070772122473));
#280919=CARTESIAN_POINT('Ctrl Pts',(-11.9999999999999,2.48156496040248,
1.30786573200167));
#280920=CARTESIAN_POINT('Ctrl Pts',(-12.,2.43125,1.11216591491825E-12));
#280921=CARTESIAN_POINT('Ctrl Pts',(-12.,2.80625000000003,-5.07927033766009E-14));
#280922=CARTESIAN_POINT('Ctrl Pts',(-12.,2.83809260234642,0.827703094535515));
#280923=CARTESIAN_POINT('Ctrl Pts',(-11.9143678834799,2.87099240591271,
1.65506306772216));
#280924=CARTESIAN_POINT('Ctrl Pts',(-11.4165365148981,2.96831655978162,
4.02311061157436));
#280925=CARTESIAN_POINT('Ctrl Pts',(-10.7843954258263,3.03293020718696,
5.49725525593906));
#280926=CARTESIAN_POINT('Ctrl Pts',(-9.00354985319716,3.1546886535461,8.08356084583945));
#280927=CARTESIAN_POINT('Ctrl Pts',(-7.88386994414273,3.21648924583216,
9.17893881394363));
#280928=CARTESIAN_POINT('Ctrl Pts',(-5.28285605104015,3.34221742565012,
10.8868875806367));
#280929=CARTESIAN_POINT('Ctrl Pts',(-3.82455859425111,3.40154335506105,
11.4806656367835));
#280930=CARTESIAN_POINT('Ctrl Pts',(-0.748047614205083,3.52599083837247,
12.0797140102831));
#280931=CARTESIAN_POINT('Ctrl Pts',(0.841658075829231,3.59029578433683,
12.073553287322));
#280932=CARTESIAN_POINT('Ctrl Pts',(3.90017388939111,3.71401534787315,11.4533638074065));
#280933=CARTESIAN_POINT('Ctrl Pts',(5.34198612921755,3.7729505871848,10.8560605625585));
#280934=CARTESIAN_POINT('Ctrl Pts',(7.94805013422061,3.89931422881742,9.12833611485889));
#280935=CARTESIAN_POINT('Ctrl Pts',(9.07989705968758,3.96185263740782,8.00331995449505));
#280936=CARTESIAN_POINT('Ctrl Pts',(10.831649647348,4.08407179296626,5.39558600130891));
#280937=CARTESIAN_POINT('Ctrl Pts',(11.4409454271204,4.14759848299899,3.94227237473268));
#280938=CARTESIAN_POINT('Ctrl Pts',(12.0666889074908,4.27268371788102,0.894176234594086));
#280939=CARTESIAN_POINT('Ctrl Pts',(12.0811599033549,4.33104609521448,-0.670909629289751));
#280940=CARTESIAN_POINT('Ctrl Pts',(11.507580289608,4.45679362326614,-3.7531702047656));
#280941=CARTESIAN_POINT('Ctrl Pts',(10.9119981262781,4.52137070290346,-5.23824303713071));
#280942=CARTESIAN_POINT('Ctrl Pts',(9.19762581866298,4.64372126988644,-7.86153843236569));
#280943=CARTESIAN_POINT('Ctrl Pts',(8.10690675886904,4.7045105285579,-8.98211590523337));
#280944=CARTESIAN_POINT('Ctrl Pts',(5.54721341149906,4.83043732643139,-10.755291099315));
#280945=CARTESIAN_POINT('Ctrl Pts',(4.09918917558897,4.89043431468123,-11.3861544471344));
#280946=CARTESIAN_POINT('Ctrl Pts',(1.03667757003992,5.01431551139872,-12.0578834091891));
#280947=CARTESIAN_POINT('Ctrl Pts',(-0.548840370340826,5.07845105933118,
-12.0899118051045));
#280948=CARTESIAN_POINT('Ctrl Pts',(-3.61818808824507,5.20260878260221,
-11.545579735994));
#280949=CARTESIAN_POINT('Ctrl Pts',(-5.07444191571541,5.26116025665351,
-10.9837010305141));
#280950=CARTESIAN_POINT('Ctrl Pts',(-7.72830761428462,5.38765321684513,
-9.31633102641958));
#280951=CARTESIAN_POINT('Ctrl Pts',(-8.89170266286211,5.45142329932537,
-8.21326767702354));
#280952=CARTESIAN_POINT('Ctrl Pts',(-10.7042785399836,5.57295823669527,
-5.64308168585122));
#280953=CARTESIAN_POINT('Ctrl Pts',(-11.3455634256844,5.63619905011406,
-4.20759290526078));
#280954=CARTESIAN_POINT('Ctrl Pts',(-11.8980293264065,5.73551328842991,
-1.8055677862771));
#280955=CARTESIAN_POINT('Ctrl Pts',(-12.,5.77150225280953,-0.903218196644935));
#280956=CARTESIAN_POINT('Ctrl Pts',(-12.,5.80624999998803,1.11022302462516E-15));
#280957=CARTESIAN_POINT('Origin',(-8.79029313101884E-14,130.96875,0.));
#280958=CARTESIAN_POINT('',(-12.,8.80624999997604,1.03764954113354E-13));
#280959=CARTESIAN_POINT('',(-12.,8.43124999997596,1.29348329112088E-14));
#280960=CARTESIAN_POINT('',(-12.0000000000001,130.96875,-1.46957615897682E-15));
#280961=CARTESIAN_POINT('Ctrl Pts',(-12.,8.43124999997596,3.08086889333481E-14));
#280962=CARTESIAN_POINT('Ctrl Pts',(-12.,8.39699003864453,-0.890538898304326));
#280963=CARTESIAN_POINT('Ctrl Pts',(-11.9008722571372,8.36152053074314,
-1.78030968083635));
#280964=CARTESIAN_POINT('Ctrl Pts',(-11.3587162131204,8.26272762338974,
-4.17213341949261));
#280965=CARTESIAN_POINT('Ctrl Pts',(-10.7216942676366,8.19944657225689,
-5.61005323538964));
#280966=CARTESIAN_POINT('Ctrl Pts',(-8.91725471621577,8.07781763716965,
-8.1853262158182));
#280967=CARTESIAN_POINT('Ctrl Pts',(-7.75810310432052,8.01422195318962,
-9.29136231946705));
#280968=CARTESIAN_POINT('Ctrl Pts',(-5.11065784145148,7.88774524607848,
-10.9668857151748));
#280969=CARTESIAN_POINT('Ctrl Pts',(-3.65634228967265,7.82915215245821,
-11.5335430014374));
#280970=CARTESIAN_POINT('Ctrl Pts',(-0.58839170333626,7.70505094434627,
-12.0881175813519));
#280971=CARTESIAN_POINT('Ctrl Pts',(0.997743713920646,7.64089041894949,
-12.0612333077265));
#280972=CARTESIAN_POINT('Ctrl Pts',(4.06220307058269,7.51693043404444,-11.3993078828774));
#280973=CARTESIAN_POINT('Ctrl Pts',(5.5116322884457,7.45703391637837,-10.7734680460166));
#280974=CARTESIAN_POINT('Ctrl Pts',(8.07694712039672,7.33113298492367,-9.00911806416827));
#280975=CARTESIAN_POINT('Ctrl Pts',(9.17159631988134,7.27021652447071,-7.89194794906784));
#280976=CARTESIAN_POINT('Ctrl Pts',(10.8950207952372,7.14794385508041,-5.27361861839748));
#280977=CARTESIAN_POINT('Ctrl Pts',(11.4955806208667,7.08335971465281,-3.78997959136802));
#280978=CARTESIAN_POINT('Ctrl Pts',(12.0789205324003,6.95755349607306,-0.709364752199233));
#280979=CARTESIAN_POINT('Ctrl Pts',(12.0694559833347,6.89920928618014,0.85542033665581));
#280980=CARTESIAN_POINT('Ctrl Pts',(11.4535541993981,6.77416367663518,3.90568423361148));
#280981=CARTESIAN_POINT('Ctrl Pts',(10.8486864033288,6.71060029576505,5.3613903253671));
#280982=CARTESIAN_POINT('Ctrl Pts',(9.10531241508707,6.5882901969422,7.97421059115888));
#280983=CARTESIAN_POINT('Ctrl Pts',(7.97778018551415,6.52590850488026,9.10220317724238));
#280984=CARTESIAN_POINT('Ctrl Pts',(5.37826623328161,6.39956404637928,10.8381361856232));
#280985=CARTESIAN_POINT('Ctrl Pts',(3.93843489438883,6.34056303802432,11.4402666679756));
#280986=CARTESIAN_POINT('Ctrl Pts',(0.88147954041008,6.2169065964041,12.0707786364784));
#280987=CARTESIAN_POINT('Ctrl Pts',(-0.708726898238164,6.15258139473282,
12.0821516304807));
#280988=CARTESIAN_POINT('Ctrl Pts',(-3.78706681449179,6.02805992939772,
11.4930066802789));
#280989=CARTESIAN_POINT('Ctrl Pts',(-5.24673927658173,5.9688122780238,10.9042541867205));
#280990=CARTESIAN_POINT('Ctrl Pts',(-7.85332120820976,5.84311236691359,
9.20515810671939));
#280991=CARTESIAN_POINT('Ctrl Pts',(-8.97691642983155,5.7811619479029,8.11320331071348));
#280992=CARTESIAN_POINT('Ctrl Pts',(-10.7667067410733,5.65948674729555,
5.53196789731668));
#280993=CARTESIAN_POINT('Ctrl Pts',(-11.403767689396,5.59487089658239,4.05936454027656));
#280994=CARTESIAN_POINT('Ctrl Pts',(-11.9117524522773,5.49698725924637,
1.68007305836135));
#280995=CARTESIAN_POINT('Ctrl Pts',(-12.,5.46357521179585,0.840247840106129));
#280996=CARTESIAN_POINT('Ctrl Pts',(-12.,5.43124999998796,3.88578058618805E-15));
#280997=CARTESIAN_POINT('Ctrl Pts',(-12.,5.80624999998803,1.2490009027033E-15));
#280998=CARTESIAN_POINT('Ctrl Pts',(-12.,5.83099605561787,0.643238470259273));
#280999=CARTESIAN_POINT('Ctrl Pts',(-11.9482833205872,5.85640359247076,
1.28686743499849));
#281000=CARTESIAN_POINT('Ctrl Pts',(-11.5911093748506,5.94543216321653,
3.48498547807791));
#281001=CARTESIAN_POINT('Ctrl Pts',(-11.0317226380331,6.00993836902569,
4.979976653213));
#281002=CARTESIAN_POINT('Ctrl Pts',(-9.38320563809063,6.13282993643762,
7.63873227061522));
#281003=CARTESIAN_POINT('Ctrl Pts',(-8.32095697051646,6.19279229952065,
8.78387974016299));
#281004=CARTESIAN_POINT('Ctrl Pts',(-5.80212077898664,6.31889617628815,
10.6207376555748));
#281005=CARTESIAN_POINT('Ctrl Pts',(-4.36438080392958,6.3797070879706,11.2879037183857));
#281006=CARTESIAN_POINT('Ctrl Pts',(-1.31641508298864,6.50299989129578,
12.0300843124326));
#281007=CARTESIAN_POINT('Ctrl Pts',(0.264183353965178,6.56693644113444,
12.0990064476353));
#281008=CARTESIAN_POINT('Ctrl Pts',(3.34298067884587,6.69147640903717,11.6283775643194));
#281009=CARTESIAN_POINT('Ctrl Pts',(4.81307779653889,6.74982155769761,11.100852726935));
#281010=CARTESIAN_POINT('Ctrl Pts',(7.50916246978427,6.8762478441472,9.49439635312942));
#281011=CARTESIAN_POINT('Ctrl Pts',(8.70042697128974,6.94086592426288,8.41629246571222));
#281012=CARTESIAN_POINT('Ctrl Pts',(10.570950077193,7.06219113327966,5.88809168532244));
#281013=CARTESIAN_POINT('Ctrl Pts',(11.2438606194546,7.12478980996596,4.47111460765387));
#281014=CARTESIAN_POINT('Ctrl Pts',(12.0125816948162,7.25037003020925,1.45660826479009));
#281015=CARTESIAN_POINT('Ctrl Pts',(12.1000503244365,7.30932769547842,-0.112508631886311));
#281016=CARTESIAN_POINT('Ctrl Pts',(11.667942147848,7.43414656844159,-3.21659699740878));
#281017=CARTESIAN_POINT('Ctrl Pts',(11.1446562181789,7.49854822981862,-4.72060055222581));
#281018=CARTESIAN_POINT('Ctrl Pts',(9.56191000353393,7.62193542442171,-7.41360951611981));
#281019=CARTESIAN_POINT('Ctrl Pts',(8.52789698680623,7.6812422582497,-8.58293095406429));
#281020=CARTESIAN_POINT('Ctrl Pts',(6.04981872839943,7.80750361436516,-10.4825106951619));
#281021=CARTESIAN_POINT('Ctrl Pts',(4.6224710867094,7.86926711672205,-11.1855208199272));
#281022=CARTESIAN_POINT('Ctrl Pts',(1.58966308417278,7.99194677745798,-11.9965743786724));
#281023=CARTESIAN_POINT('Ctrl Pts',(0.0146910303873457,8.05565573531663,
-12.1014221066078));
#281024=CARTESIAN_POINT('Ctrl Pts',(-3.07233371964743,8.18052850955784,
-11.703010875323));
#281025=CARTESIAN_POINT('Ctrl Pts',(-4.55582240231689,8.23882877065419,
-11.2091110657436));
#281026=CARTESIAN_POINT('Ctrl Pts',(-7.28617656375516,8.36487141394359,
-9.66595804753169));
#281027=CARTESIAN_POINT('Ctrl Pts',(-8.49939669834883,8.42947786260113,
-8.61856269810358));
#281028=CARTESIAN_POINT('Ctrl Pts',(-10.4255624419782,8.55141795323951,
-6.14108644638707));
#281029=CARTESIAN_POINT('Ctrl Pts',(-11.1312039295987,8.61289784773076,
-4.74362485061815));
#281030=CARTESIAN_POINT('Ctrl Pts',(-11.8496202008874,8.72009371706788,
-2.1906485030476));
#281031=CARTESIAN_POINT('Ctrl Pts',(-12.,8.76405334452794,-1.09684195762376));
#281032=CARTESIAN_POINT('Ctrl Pts',(-12.,8.80624999997604,2.16215934045749E-13));
#281033=CARTESIAN_POINT('Origin',(-8.79029313101884E-14,130.96875,0.));
#281034=CARTESIAN_POINT('',(-12.,11.806249999964,7.52114056987762E-14));
#281035=CARTESIAN_POINT('',(-12.,11.431249999964,9.0858611452087E-14));
#281036=CARTESIAN_POINT('',(-12.0000000000001,130.96875,-1.46957615897682E-15));
#281037=CARTESIAN_POINT('Ctrl Pts',(-12.,11.431249999964,1.57374113740616E-13));
#281038=CARTESIAN_POINT('Ctrl Pts',(-12.,11.389588144316,-1.08294059853536));
#281039=CARTESIAN_POINT('Ctrl Pts',(-11.8534082069267,11.3462030315979,
-2.16304424929612));
#281040=CARTESIAN_POINT('Ctrl Pts',(-11.1474361064258,11.2395681924447,
-4.70548077250192));
#281041=CARTESIAN_POINT('Ctrl Pts',(-10.4463866902839,11.1779409983725,
-6.10569158782984));
#281042=CARTESIAN_POINT('Ctrl Pts',(-8.52800813932628,11.0560849524982,
-8.59035119496663));
#281043=CARTESIAN_POINT('Ctrl Pts',(-7.31783574715978,10.9914747568544,
-9.64209899454808));
#281044=CARTESIAN_POINT('Ctrl Pts',(-4.59225812837821,10.8653757798519,
-11.1941956705663));
#281045=CARTESIAN_POINT('Ctrl Pts',(-3.11065270066361,10.8070785448882,
-11.6928484439898));
#281046=CARTESIAN_POINT('Ctrl Pts',(-0.024729051402356,10.6822503111089,
-12.1014704681028));
#281047=CARTESIAN_POINT('Ctrl Pts',(1.55108665626511,10.6185072267339,-12.0016879126557));
#281048=CARTESIAN_POINT('Ctrl Pts',(4.58609229101319,10.4957386699076,-11.2003626816289));
#281049=CARTESIAN_POINT('Ctrl Pts',(6.01492924344135,10.4341191736442,-10.5024374214762));
#281050=CARTESIAN_POINT('Ctrl Pts',(8.49881554186177,10.3078790847169,-8.61174622744464));
#281051=CARTESIAN_POINT('Ctrl Pts',(9.53684202246883,10.2484890722127,-7.44584929710471));
#281052=CARTESIAN_POINT('Ctrl Pts',(11.1289632812859,10.1251698186584,-4.75765250051073));
#281053=CARTESIAN_POINT('Ctrl Pts',(11.6573912043948,10.0607512188981,-3.25487939149134));
#281054=CARTESIAN_POINT('Ctrl Pts',(12.0995477628908,9.93586159518112,-0.152216878092207));
#281055=CARTESIAN_POINT('Ctrl Pts',(12.0172926245384,9.87696672724328,1.41663507310838));
#281056=CARTESIAN_POINT('Ctrl Pts',(11.2587456915536,9.75141649237194,4.43366776818686));
#281057=CARTESIAN_POINT('Ctrl Pts',(10.5903204860711,9.68865215211609,5.85330452076973));
#281058=CARTESIAN_POINT('Ctrl Pts',(8.7274459043467,9.56741403338887,8.38836970557499));
#281059=CARTESIAN_POINT('Ctrl Pts',(7.53923094341759,9.50279706761554,9.47062405795193));
#281060=CARTESIAN_POINT('Ctrl Pts',(4.84788179509845,9.37632143015218,11.0856739517181));
#281061=CARTESIAN_POINT('Ctrl Pts',(3.3796138240055,9.31795825087466,11.6177611184392));
#281062=CARTESIAN_POINT('Ctrl Pts',(0.302011016147692,9.19346660220051,
12.0981839171448));
#281063=CARTESIAN_POINT('Ctrl Pts',(-1.27928918066634,9.12950166557921,
12.0341515012749));
#281064=CARTESIAN_POINT('Ctrl Pts',(-4.32924149411119,9.0061285028992,11.3013233400185));
#281065=CARTESIAN_POINT('Ctrl Pts',(-5.76836621779356,8.94543495540061,
10.6389972126522));
#281066=CARTESIAN_POINT('Ctrl Pts',(-8.2926736112961,8.81935367750649,8.81062023518514));
#281067=CARTESIAN_POINT('Ctrl Pts',(-9.35872514961793,8.7592904954788,7.66874323005069));
#281068=CARTESIAN_POINT('Ctrl Pts',(-11.0160663846226,8.63646880844639,
5.01467122135901));
#281069=CARTESIAN_POINT('Ctrl Pts',(-11.580300837083,8.57195112870678,3.52095691603815));
#281070=CARTESIAN_POINT('Ctrl Pts',(-11.9462969687398,8.48236891808552,
1.31131429491467));
#281071=CARTESIAN_POINT('Ctrl Pts',(-12.,8.45646681014301,0.655475063957913));
#281072=CARTESIAN_POINT('Ctrl Pts',(-12.,8.43124999997596,2.81719092498633E-14));
#281073=CARTESIAN_POINT('Ctrl Pts',(-12.,8.80624999997604,2.17326157070374E-13));
#281074=CARTESIAN_POINT('Ctrl Pts',(-12.,8.82387914688782,0.458244564755818));
#281075=CARTESIAN_POINT('Ctrl Pts',(-11.9737525692637,8.84185579477114,
0.916993615098396));
#281076=CARTESIAN_POINT('Ctrl Pts',(-11.7409281292704,8.92247877912802,
2.93702401571875));
#281077=CARTESIAN_POINT('Ctrl Pts',(-11.2551207775011,8.9867366023522,4.44946623076792));
#281078=CARTESIAN_POINT('Ctrl Pts',(-9.74079553096694,9.11059263174499,
7.17689320743257));
#281079=CARTESIAN_POINT('Ctrl Pts',(-8.73596928917568,9.16939412094754,
8.37100315741494));
#281080=CARTESIAN_POINT('Ctrl Pts',(-6.30027620028189,9.29579879828115,
10.3349489533987));
#281081=CARTESIAN_POINT('Ctrl Pts',(-4.88388425520457,9.35869273192279,
11.0748315659316));
#281082=CARTESIAN_POINT('Ctrl Pts',(-1.86747266436311,9.48070914387332,
11.9560104548374));
#281083=CARTESIAN_POINT('Ctrl Pts',(-0.299057170406009,9.54415288331568,
12.0972702243737));
#281084=CARTESIAN_POINT('Ctrl Pts',(2.79530693938728,9.66932254089551,11.7725603037712));
#281085=CARTESIAN_POINT('Ctrl Pts',(4.29228928804916,9.72773524947492,11.3129655897213));
#281086=CARTESIAN_POINT('Ctrl Pts',(7.05646075467183,9.85335126957896,9.83430122549981));
#281087=CARTESIAN_POINT('Ctrl Pts',(8.29113131987403,9.9179105211198,8.81841490035983));
#281088=CARTESIAN_POINT('Ctrl Pts',(10.272736135536,10.0404294741798,6.3928979063031));
#281089=CARTESIAN_POINT('Ctrl Pts',(11.011191455937,10.1009504193315,5.01518681941377));
#281090=CARTESIAN_POINT('Ctrl Pts',(11.9231536974671,10.2261545125477,2.05699923912446));
#281091=CARTESIAN_POINT('Ctrl Pts',(12.088766400008,10.2857313049205,0.504512301282102));
#281092=CARTESIAN_POINT('Ctrl Pts',(11.8187680163681,10.4089041617859,-2.60946288488135));
#281093=CARTESIAN_POINT('Ctrl Pts',(11.3733158940114,10.4733563091391,-4.14006848777134));
#281094=CARTESIAN_POINT('Ctrl Pts',(9.92631147992378,10.5983930113062,-6.92005923599754));
#281095=CARTESIAN_POINT('Ctrl Pts',(8.94685217287931,10.6571655254461,-8.14694229711963));
#281096=CARTESIAN_POINT('Ctrl Pts',(6.57420247458641,10.7826440862918,-10.1587088160428));
#281097=CARTESIAN_POINT('Ctrl Pts',(5.20340159946979,10.8457116247515,-10.9244886456193));
#281098=CARTESIAN_POINT('Ctrl Pts',(2.21152525060571,10.966848963036,-11.9013775368152));
#281099=CARTESIAN_POINT('Ctrl Pts',(0.61498212470326,11.031373450461,-12.0895090711595));
#281100=CARTESIAN_POINT('Ctrl Pts',(-2.5136705660668,11.157930110277,-11.8353108616964));
#281101=CARTESIAN_POINT('Ctrl Pts',(-4.01686727189288,11.2163420561628,
-11.4130602011789));
#281102=CARTESIAN_POINT('Ctrl Pts',(-6.79938572972625,11.3407266944546,
-10.0114383623218));
#281103=CARTESIAN_POINT('Ctrl Pts',(-8.04845240744468,11.4047509440899,
-9.0378679579154));
#281104=CARTESIAN_POINT('Ctrl Pts',(-10.1004829868513,11.5282954884597,
-6.66614889102401));
#281105=CARTESIAN_POINT('Ctrl Pts',(-10.8839969360667,11.5887450536416,
-5.29111991055287));
#281106=CARTESIAN_POINT('Ctrl Pts',(-11.791482446841,11.7045287953537,-2.57634637217284));
#281107=CARTESIAN_POINT('Ctrl Pts',(-12.,11.7565624003826,-1.29155838100936));
#281108=CARTESIAN_POINT('Ctrl Pts',(-12.,11.806249999964,1.5931700403371E-13));
#281109=CARTESIAN_POINT('Origin',(-8.79029313101884E-14,130.96875,0.));
#281110=CARTESIAN_POINT('',(-12.,14.806249999952,7.34788079488412E-16));
#281111=CARTESIAN_POINT('',(-12.,14.431249999952,8.88810266894734E-14));
#281112=CARTESIAN_POINT('',(-12.0000000000001,130.96875,-1.46957615897682E-15));
#281113=CARTESIAN_POINT('Ctrl Pts',(-12.,14.431249999952,1.65145674912992E-13));
#281114=CARTESIAN_POINT('Ctrl Pts',(-12.,14.3823065495871,-1.27221528201616));
#281115=CARTESIAN_POINT('Ctrl Pts',(-11.7976819562748,14.3310777566137,
-2.53809767281549));
#281116=CARTESIAN_POINT('Ctrl Pts',(-10.9088722919085,14.2160239603072,
-5.23996547038095));
#281117=CARTESIAN_POINT('Ctrl Pts',(-10.1312207970015,14.1554082812044,
-6.61959498633458));
#281118=CARTESIAN_POINT('Ctrl Pts',(-8.08969908479941,14.0319810826221,
-9.00084288154191));
#281119=CARTESIAN_POINT('Ctrl Pts',(-6.84571246974124,13.9679972617242,
-9.97970502074197));
#281120=CARTESIAN_POINT('Ctrl Pts',(-4.07025897930456,13.8435387628565,
-11.3941574172112));
#281121=CARTESIAN_POINT('Ctrl Pts',(-2.56883963781858,13.7851617460955,
-11.823487409551));
#281122=CARTESIAN_POINT('Ctrl Pts',(0.558627108948717,13.6586530587222,
-12.0922194803715));
#281123=CARTESIAN_POINT('Ctrl Pts',(2.15601857273127,13.5940372166789,-11.9115809969756));
#281124=CARTESIAN_POINT('Ctrl Pts',(5.15171928337348,13.4728585774309,-10.9488291593168));
#281125=CARTESIAN_POINT('Ctrl Pts',(6.52552543835335,13.4099801485513,-10.1899618727092));
#281126=CARTESIAN_POINT('Ctrl Pts',(8.907990416113,13.2844504371692,-8.18955361272096));
#281127=CARTESIAN_POINT('Ctrl Pts',(9.89371655991383,13.2255964066297,-6.96674262794056));
#281128=CARTESIAN_POINT('Ctrl Pts',(11.3536103486055,13.100659174132,-4.19352546377302));
#281129=CARTESIAN_POINT('Ctrl Pts',(11.8060909206473,13.0362294645118,-2.6657867795321));
#281130=CARTESIAN_POINT('Ctrl Pts',(12.0910466477122,12.9129568227145,0.44592223833023));
#281131=CARTESIAN_POINT('Ctrl Pts',(11.9329895718556,12.8535084379708,1.99900816849489));
#281132=CARTESIAN_POINT('Ctrl Pts',(11.0280644293945,12.7272830031674,4.98603056075995));
#281133=CARTESIAN_POINT('Ctrl Pts',(10.2794942003153,12.6657596882479,6.38831127923374));
#281134=CARTESIAN_POINT('Ctrl Pts',(8.29003956409569,12.5429310906611,8.8160471031109));
#281135=CARTESIAN_POINT('Ctrl Pts',(7.07134536980327,12.4791651632238,9.82055700326823));
#281136=CARTESIAN_POINT('Ctrl Pts',(4.32900779517834,12.3542709355575,11.2989156424085));
#281137=CARTESIAN_POINT('Ctrl Pts',(2.8338924598131,12.2958833579715,11.7632835526384));
#281138=CARTESIAN_POINT('Ctrl Pts',(-0.259514673870521,12.1707524108885,
12.0982475553265));
#281139=CARTESIAN_POINT('Ctrl Pts',(-1.82889134293284,12.1072697910964,
11.9620377569558));
#281140=CARTESIAN_POINT('Ctrl Pts',(-4.84764043700566,11.9851588251539,
11.0906055638688));
#281141=CARTESIAN_POINT('Ctrl Pts',(-6.26557890992037,11.9224317368724,
10.3558711604917));
#281142=CARTESIAN_POINT('Ctrl Pts',(-8.70721886267572,11.7960459036551,
8.40090307546756));
#281143=CARTESIAN_POINT('Ctrl Pts',(-9.71612932779523,11.7371842182329,
7.21024969635897));
#281144=CARTESIAN_POINT('Ctrl Pts',(-11.2400537405356,11.6133911122404,
4.48757728203246));
#281145=CARTESIAN_POINT('Ctrl Pts',(-11.7311135069529,11.5491109773968,
2.97626172118548));
#281146=CARTESIAN_POINT('Ctrl Pts',(-11.9722226129965,11.4678882290064,
0.943333159935274));
#281147=CARTESIAN_POINT('Ctrl Pts',(-12.,11.4493856810174,0.471411198311356));
#281148=CARTESIAN_POINT('Ctrl Pts',(-12.,11.431249999964,1.62925228863742E-13));
#281149=CARTESIAN_POINT('Ctrl Pts',(-12.,11.806249999964,1.59178226155632E-13));
#281150=CARTESIAN_POINT('Ctrl Pts',(-12.,11.8159717771291,0.252703750665779));
#281151=CARTESIAN_POINT('Ctrl Pts',(-11.9920177414135,11.8258030097974,
0.505659048206776));
#281152=CARTESIAN_POINT('Ctrl Pts',(-11.8759839799423,11.8977356686935,
2.33774440790498));
#281153=CARTESIAN_POINT('Ctrl Pts',(-11.4645665854366,11.9622759756235,
3.88170014686002));
#281154=CARTESIAN_POINT('Ctrl Pts',(-10.0798043248063,12.0877695389606,
6.69379005208959));
#281155=CARTESIAN_POINT('Ctrl Pts',(-9.13040461137842,12.1462403905476,
7.9400858895626));
#281156=CARTESIAN_POINT('Ctrl Pts',(-6.80457932068993,12.2714835337107,
10.0063993645393));
#281157=CARTESIAN_POINT('Ctrl Pts',(-5.44842333302093,12.3348491603387,
10.8048732903662));
#281158=CARTESIAN_POINT('Ctrl Pts',(-2.48267155529713,12.4566779662627,
11.8468016530471));
#281159=CARTESIAN_POINT('Ctrl Pts',(-0.89842029146626,12.5199081357668,
12.0707791359501));
#281160=CARTESIAN_POINT('Ctrl Pts',(2.22736272105365,12.6463487146592,11.8924296877473));
#281161=CARTESIAN_POINT('Ctrl Pts',(3.73965462415031,12.7050417605495,11.5067830828562));
#281162=CARTESIAN_POINT('Ctrl Pts',(6.55807938154271,12.8290189984987,10.1717166683596));
#281163=CARTESIAN_POINT('Ctrl Pts',(7.83300587353999,12.8932308706615,9.22584812478829));
#281164=CARTESIAN_POINT('Ctrl Pts',(9.93882760285228,13.0173573477921,6.90369101150418));
#281165=CARTESIAN_POINT('Ctrl Pts',(10.7523241784602,13.0770488173305,5.55236384193603));
#281166=CARTESIAN_POINT('Ctrl Pts',(11.811475439129,13.2028932743447,2.62535552815208));
#281167=CARTESIAN_POINT('Ctrl Pts',(12.0515012216521,13.264092407653,1.07909280556291));
#281168=CARTESIAN_POINT('Ctrl Pts',(11.9286798792065,13.3861958640999,-2.05490555938842));
#281169=CARTESIAN_POINT('Ctrl Pts',(11.552914872369,13.4507928927077,-3.61191986054169));
#281170=CARTESIAN_POINT('Ctrl Pts',(10.2330810216963,13.576722174506,-6.45643216581518));
#281171=CARTESIAN_POINT('Ctrl Pts',(9.31469434867856,13.6350374464028,-7.72256004961813));
#281172=CARTESIAN_POINT('Ctrl Pts',(7.03784286455176,13.7599958252643,-9.8443034302874));
#281173=CARTESIAN_POINT('Ctrl Pts',(5.6975456848272,13.8236354433468,-10.6761287992143));
#281174=CARTESIAN_POINT('Ctrl Pts',(2.75948640105646,13.9461372360307,-11.7844774161238));
#281175=CARTESIAN_POINT('Ctrl Pts',(1.18799885877861,14.0081944366527,-12.0448164734704));
#281176=CARTESIAN_POINT('Ctrl Pts',(-1.93436825361326,14.1344968394823,
-11.9435955330094));
#281177=CARTESIAN_POINT('Ctrl Pts',(-3.45575955286439,14.1936485964835,
-11.5952143043706));
#281178=CARTESIAN_POINT('Ctrl Pts',(-6.30965930479221,14.3171679826371,
-10.3282315856791));
#281179=CARTESIAN_POINT('Ctrl Pts',(-7.61018914604508,14.3815340387382,
-9.41111828566092));
#281180=CARTESIAN_POINT('Ctrl Pts',(-9.76981475623303,14.5062104246925,
-7.13988752706686));
#281181=CARTESIAN_POINT('Ctrl Pts',(-10.613280708508,14.5653019323891,-5.81252942271048));
#281182=CARTESIAN_POINT('Ctrl Pts',(-11.7219456143113,14.6884953720743,
-2.97051848708096));
#281183=CARTESIAN_POINT('Ctrl Pts',(-12.,14.74887273433,-1.49144029733251));
#281184=CARTESIAN_POINT('Ctrl Pts',(-12.,14.806249999952,-2.77555756156289E-16));
#281185=CARTESIAN_POINT('Origin',(-8.79029313101884E-14,130.96875,0.));
#281186=CARTESIAN_POINT('',(-12.,17.80624999994,-1.4751353765381E-14));
#281187=CARTESIAN_POINT('',(-12.,17.43124999994,-5.45323593414533E-15));
#281188=CARTESIAN_POINT('',(-12.0000000000001,130.96875,-1.46957615897682E-15));
#281189=CARTESIAN_POINT('Ctrl Pts',(-12.,17.43124999994,8.32667268468867E-16));
#281190=CARTESIAN_POINT('Ctrl Pts',(-12.,17.3746355953144,-1.47161081227273));
#281191=CARTESIAN_POINT('Ctrl Pts',(-11.7292898349336,17.3150879968699,
-2.93150675551766));
#281192=CARTESIAN_POINT('Ctrl Pts',(-10.6412379837764,17.1926179533313,
-5.76141162610182));
#281193=CARTESIAN_POINT('Ctrl Pts',(-9.80367175971446,17.1334211137684,
-7.09350945191991));
#281194=CARTESIAN_POINT('Ctrl Pts',(-7.65463816373364,17.0088503852345,
-9.3748750759184));
#281195=CARTESIAN_POINT('Ctrl Pts',(-6.35912640911618,16.9445119589857,
-10.2977331098152));
#281196=CARTESIAN_POINT('Ctrl Pts',(-3.5121749371591,16.820898371858,-11.578241266071));
#281197=CARTESIAN_POINT('Ctrl Pts',(-1.99257551141557,16.7618513725082,
-11.9340128619219));
#281198=CARTESIAN_POINT('Ctrl Pts',(1.1305076194917,16.6355200061212,-12.0505218705341));
#281199=CARTESIAN_POINT('Ctrl Pts',(2.70454543356806,16.5732420527098,-11.79738307137));
#281200=CARTESIAN_POINT('Ctrl Pts',(5.64818469253235,16.450871183792,-10.7022210872036));
#281201=CARTESIAN_POINT('Ctrl Pts',(6.99170350750002,16.3872834703396,-9.87701294909237));
#281202=CARTESIAN_POINT('Ctrl Pts',(9.27837150810931,16.2622649633922,-7.76625194779492));
#281203=CARTESIAN_POINT('Ctrl Pts',(10.2029416438783,16.2039313203782,-6.50406288910224));
#281204=CARTESIAN_POINT('Ctrl Pts',(11.5357778969021,16.0780859920241,-3.66595757065916));
#281205=CARTESIAN_POINT('Ctrl Pts',(11.9186935182967,16.0134974683325,-2.11148771819885));
#281206=CARTESIAN_POINT('Ctrl Pts',(12.0565303645475,15.891277695036,1.02065530465216));
#281207=CARTESIAN_POINT('Ctrl Pts',(11.8241053985494,15.8302737912193,2.56758110483523));
#281208=CARTESIAN_POINT('Ctrl Pts',(10.7792241968896,15.7043904723188,5.50023620124078));
#281209=CARTESIAN_POINT('Ctrl Pts',(9.97171740280202,15.644559966527,6.8563211212477));
#281210=CARTESIAN_POINT('Ctrl Pts',(7.87664645564514,15.5205472616759,9.18849032656098));
#281211=CARTESIAN_POINT('Ctrl Pts',(6.60686838021293,15.4563702630232,10.1399783304692));
#281212=CARTESIAN_POINT('Ctrl Pts',(3.79558520126637,15.332307632391,11.4884657716385));
#281213=CARTESIAN_POINT('Ctrl Pts',(2.28511098038302,15.2736846808067,11.8814786023088));
#281214=CARTESIAN_POINT('Ctrl Pts',(-0.841288922901996,15.1472191481587,
12.0750852080575));
#281215=CARTESIAN_POINT('Ctrl Pts',(-2.42803402963569,15.0837396595986,
11.8583112574829));
#281216=CARTESIAN_POINT('Ctrl Pts',(-5.39912874869519,14.9620476191367,
10.8294889713357));
#281217=CARTESIAN_POINT('Ctrl Pts',(-6.75830585804143,14.8987397183168,
10.0376011230291));
#281218=CARTESIAN_POINT('Ctrl Pts',(-9.09365631450678,14.7734456974542,
7.98225807485496));
#281219=CARTESIAN_POINT('Ctrl Pts',(-10.0491372958055,14.7149257751828,
6.73987402012214));
#281220=CARTESIAN_POINT('Ctrl Pts',(-11.4465469019859,14.5895219160253,
3.93422521894999));
#281221=CARTESIAN_POINT('Ctrl Pts',(-11.8648920847047,14.5249968281946,
2.39291605364606));
#281222=CARTESIAN_POINT('Ctrl Pts',(-11.9907858489882,14.4522660510314,
0.543288455475417));
#281223=CARTESIAN_POINT('Ctrl Pts',(-12.,14.4416950587665,0.271504426974703));
#281224=CARTESIAN_POINT('Ctrl Pts',(-12.,14.431249999952,1.61329283265843E-13));
#281225=CARTESIAN_POINT('Ctrl Pts',(-12.,14.806249999952,2.93915231795365E-15));
#281226=CARTESIAN_POINT('Ctrl Pts',(-12.,14.8085776919202,0.0605050373769862));
#281227=CARTESIAN_POINT('Ctrl Pts',(-11.9995423931535,14.8109118698816,
0.121029983434178));
#281228=CARTESIAN_POINT('Ctrl Pts',(-11.9745681208275,14.8747154420508,
1.77139833348643));
#281229=CARTESIAN_POINT('Ctrl Pts',(-11.6347695110624,14.9393338131942,
3.34065359426618));
#281230=CARTESIAN_POINT('Ctrl Pts',(-10.3802032414723,15.0656598712332,
6.21668625540801));
#281231=CARTESIAN_POINT('Ctrl Pts',(-9.49265983287779,15.1239776301458,
7.50234936474159));
#281232=CARTESIAN_POINT('Ctrl Pts',(-7.2651417573986,15.2486115875892,9.67834968251244));
#281233=CARTESIAN_POINT('Ctrl Pts',(-5.94134751640508,15.3124898214874,
10.5429252185951));
#281234=CARTESIAN_POINT('Ctrl Pts',(-3.03154430393017,15.4356205591155,
11.716617455179));
#281235=CARTESIAN_POINT('Ctrl Pts',(-1.47280762426799,15.4966736800754,
12.0125075855231));
#281236=CARTESIAN_POINT('Ctrl Pts',(1.64574301659647,15.6228217033888,11.9868816261993));
#281237=CARTESIAN_POINT('Ctrl Pts',(3.17590997098518,15.6825916397591,11.6750732916029));
#281238=CARTESIAN_POINT('Ctrl Pts',(6.06355811562229,15.8056205377235,10.4751704425746));
#281239=CARTESIAN_POINT('Ctrl Pts',(7.38847734367979,15.870101979139,9.58677332163239));
#281240=CARTESIAN_POINT('Ctrl Pts',(9.59993987846,15.9952765907215,7.36593535177551));
#281241=CARTESIAN_POINT('Ctrl Pts',(10.4722897871741,16.0539449796668,6.06192650551696));
#281242=CARTESIAN_POINT('Ctrl Pts',(11.6719830965627,16.1793584728463,3.19178536257051));
#281243=CARTESIAN_POINT('Ctrl Pts',(11.9871728371349,16.2425170317467,1.65247993553365));
#281244=CARTESIAN_POINT('Ctrl Pts',(12.0123233958607,16.3638618392866,-1.49353359300221));
#281245=CARTESIAN_POINT('Ctrl Pts',(11.7090926266369,16.4279893770273,-3.06992017829334));
#281246=CARTESIAN_POINT('Ctrl Pts',(10.5221068179719,16.5545138035291,-5.97306736792306));
#281247=CARTESIAN_POINT('Ctrl Pts',(9.66546397675279,16.6129913136869,-7.27812599480033));
#281248=CARTESIAN_POINT('Ctrl Pts',(7.48795963920015,16.7372599557761,-9.50759970543453));
#281249=CARTESIAN_POINT('Ctrl Pts',(6.18140413449528,16.8013434032466,-10.4045332992438));
#281250=CARTESIAN_POINT('Ctrl Pts',(3.30059548053173,16.9250642929444,-11.6429540262693));
#281251=CARTESIAN_POINT('Ctrl Pts',(1.75466748516089,16.9852722091947,-11.9738660457127));
#281252=CARTESIAN_POINT('Ctrl Pts',(-1.35967481828507,17.1112500016836,
-12.0228895360496));
#281253=CARTESIAN_POINT('Ctrl Pts',(-2.89836992220341,17.1717929521038,
-11.7472486716372));
#281254=CARTESIAN_POINT('Ctrl Pts',(-5.81834650237366,17.2942978705331,
-10.6138798842907));
#281255=CARTESIAN_POINT('Ctrl Pts',(-7.16664128401645,17.358858746241,-9.75431556637224));
#281256=CARTESIAN_POINT('Ctrl Pts',(-9.42839959622457,17.4844859773994,
-7.58366729980175));
#281257=CARTESIAN_POINT('Ctrl Pts',(-10.3288130493131,17.5428938940208,
-6.30256531857088));
#281258=CARTESIAN_POINT('Ctrl Pts',(-11.5955599081519,17.6680565822307,
-3.46073051250532));
#281259=CARTESIAN_POINT('Ctrl Pts',(-11.9468073098174,17.7315074318097,
-1.92554324987653));
#281260=CARTESIAN_POINT('Ctrl Pts',(-11.9981396947232,17.7968373715993,
-0.244063417473451));
#281261=CARTESIAN_POINT('Ctrl Pts',(-12.,17.8015567661665,-0.121993927365321));
#281262=CARTESIAN_POINT('Ctrl Pts',(-12.,17.80624999994,8.91647866652079E-15));
#281263=CARTESIAN_POINT('Origin',(-8.79029313101884E-14,130.96875,0.));
#281264=CARTESIAN_POINT('',(-12.,20.806249999928,-1.97473573761942E-14));
#281265=CARTESIAN_POINT('',(-12.,20.431249999928,-4.05190619052819E-16));
#281266=CARTESIAN_POINT('',(-12.0000000000001,130.96875,-1.46957615897682E-15));
#281267=CARTESIAN_POINT('',(-11.7339375393676,20.90625,2.51290863785771));
#281268=CARTESIAN_POINT('Ctrl Pts',(-12.,20.806249999928,1.08246744900953E-14));
#281269=CARTESIAN_POINT('Ctrl Pts',(-12.,20.8386924218465,0.843294549988032));
#281270=CARTESIAN_POINT('Ctrl Pts',(-11.9111127257393,20.8722077061892,
1.685595404463));
#281271=CARTESIAN_POINT('Ctrl Pts',(-11.7339375393676,20.90625,2.51290863785771));
#281272=CARTESIAN_POINT('',(-6.54406206475579,20.90625,10.0585909397204));
#281273=CARTESIAN_POINT('Origin',(-1.38777878078145E-14,20.90625,0.));
#281274=CARTESIAN_POINT('Ctrl Pts',(-6.54406206475577,20.90625,10.0585909397204));
#281275=CARTESIAN_POINT('Ctrl Pts',(-7.59789374773782,20.8554613999318,
9.37297403964269));
#281276=CARTESIAN_POINT('Ctrl Pts',(-8.53748121101216,20.8045743444593,
8.52597257550313));
#281277=CARTESIAN_POINT('Ctrl Pts',(-10.1137548522019,20.7066754868414,
6.57804909368321));
#281278=CARTESIAN_POINT('Ctrl Pts',(-10.7428818779751,20.6582025322463,
5.4908453904987));
#281279=CARTESIAN_POINT('Ctrl Pts',(-11.7267322019416,20.5479783769447,
2.94539781423955));
#281280=CARTESIAN_POINT('Ctrl Pts',(-12.,20.4881310653806,1.47854228066918));
#281281=CARTESIAN_POINT('Ctrl Pts',(-12.,20.431249999928,1.30451205393456E-14));
#281282=CARTESIAN_POINT('Origin',(-8.79029313101884E-14,130.96875,0.));
#281283=CARTESIAN_POINT('Ctrl Pts',(-12.,20.431249999928,-5.18682319317065E-15));
#281284=CARTESIAN_POINT('Ctrl Pts',(-12.,20.4272741804144,-0.1033457654905));
#281285=CARTESIAN_POINT('Ctrl Pts',(-11.9986649616217,20.4232795252713,
-0.206747356078088));
#281286=CARTESIAN_POINT('Ctrl Pts',(-11.9556833500695,20.3587923509042,
-1.86903403241728));
#281287=CARTESIAN_POINT('Ctrl Pts',(-11.6119070931413,20.295399444133,-3.40514267636605));
#281288=CARTESIAN_POINT('Ctrl Pts',(-10.35902432988,20.1701813383277,-6.2529227016142));
#281289=CARTESIAN_POINT('Ctrl Pts',(-9.46441833361632,20.1117319099718,
-7.53878230791702));
#281290=CARTESIAN_POINT('Ctrl Pts',(-7.21306010861394,19.9861957242991,
-9.71991583093426));
#281291=CARTESIAN_POINT('Ctrl Pts',(-5.86957419396658,19.9216485775948,
-10.585521565293));
#281292=CARTESIAN_POINT('Ctrl Pts',(-2.95624811735045,19.7990313393556,
-11.7327679869781));
#281293=CARTESIAN_POINT('Ctrl Pts',(-1.41931771994306,19.7386626077233,
-12.0159453206607));
#281294=CARTESIAN_POINT('Ctrl Pts',(1.69593633306617,19.6126479341898,-11.9824678079457));
#281295=CARTESIAN_POINT('Ctrl Pts',(3.24454879133492,19.5522762116259,-11.6588423345282));
#281296=CARTESIAN_POINT('Ctrl Pts',(6.13148551909505,19.4286756336056,-10.4339163048501));
#281297=CARTESIAN_POINT('Ctrl Pts',(7.44170862444592,19.3646323669676,-9.54372067535896));
#281298=CARTESIAN_POINT('Ctrl Pts',(9.62973473413392,19.2402839235789,-7.3253726195877));
#281299=CARTESIAN_POINT('Ctrl Pts',(10.4928495817328,19.1818528803588,-6.02436208656314));
#281300=CARTESIAN_POINT('Ctrl Pts',(11.6946057288648,19.055306199693,-3.1254356055251));
#281301=CARTESIAN_POINT('Ctrl Pts',(12.0055053537683,18.9909082436387,-1.54894227591795));
#281302=CARTESIAN_POINT('Ctrl Pts',(11.9944702690204,18.8697051689437,1.59797350470092));
#281303=CARTESIAN_POINT('Ctrl Pts',(11.6864647086555,18.8066086521192,3.13800051799432));
#281304=CARTESIAN_POINT('Ctrl Pts',(10.5001757326045,18.681150214187,6.01366526768752));
#281305=CARTESIAN_POINT('Ctrl Pts',(9.63342952707142,18.6224118895613,7.32222245543705));
#281306=CARTESIAN_POINT('Ctrl Pts',(7.43201979404881,18.497331420033,9.55293744733466));
#281307=CARTESIAN_POINT('Ctrl Pts',(6.11180773001238,18.4328697420344,10.4469822042804));
#281308=CARTESIAN_POINT('Ctrl Pts',(3.23067082932968,18.3097418498919,11.6600105573142));
#281309=CARTESIAN_POINT('Ctrl Pts',(1.70220670810676,18.2501057076766,11.9789655069456));
#281310=CARTESIAN_POINT('Ctrl Pts',(-1.41712493239928,18.123926092264,12.0193549813857));
#281311=CARTESIAN_POINT('Ctrl Pts',(-2.97836974245961,18.0626884446831,
11.730401092986));
#281312=CARTESIAN_POINT('Ctrl Pts',(-5.89377845052369,17.9396780981733,
10.5694876277066));
#281313=CARTESIAN_POINT('Ctrl Pts',(-7.220870844797,17.8758440713655,9.71131089359237));
#281314=CARTESIAN_POINT('Ctrl Pts',(-9.45812750288978,17.7511431824503,
7.54589954829269));
#281315=CARTESIAN_POINT('Ctrl Pts',(-10.3517296478602,17.6928382996723,
6.26405976887067));
#281316=CARTESIAN_POINT('Ctrl Pts',(-11.6191706884262,17.5665872700776,
3.3941606319504));
#281317=CARTESIAN_POINT('Ctrl Pts',(-11.9660729768364,17.5019703064257,
1.82725008201508));
#281318=CARTESIAN_POINT('Ctrl Pts',(-11.9992118536821,17.4373707362562,
0.158843738507581));
#281319=CARTESIAN_POINT('Ctrl Pts',(-12.,17.4343048005603,0.0794051911696823));
#281320=CARTESIAN_POINT('Ctrl Pts',(-12.,17.43124999994,2.93915231795365E-15));
#281321=CARTESIAN_POINT('Ctrl Pts',(-12.,17.80624999994,1.41553435639707E-14));
#281322=CARTESIAN_POINT('Ctrl Pts',(-12.,17.8623465268447,1.45814931853264));
#281323=CARTESIAN_POINT('Ctrl Pts',(-11.734218240322,17.9213402806445,2.90525019506248));
#281324=CARTESIAN_POINT('Ctrl Pts',(-10.6644227558352,18.0428057517025,
5.71497448793998));
#281325=CARTESIAN_POINT('Ctrl Pts',(-9.84009188195503,18.101617930102,7.04013335853222));
#281326=CARTESIAN_POINT('Ctrl Pts',(-7.71546696621803,18.2254625856327,
9.32455711532062));
#281327=CARTESIAN_POINT('Ctrl Pts',(-6.42766033170131,18.2897245176208,
10.254803104201));
#281328=CARTESIAN_POINT('Ctrl Pts',(-3.57786992657996,18.4140201366153,
11.5600890339221));
#281329=CARTESIAN_POINT('Ctrl Pts',(-2.04534881871437,18.4735139022491,
11.9269998087708));
#281330=CARTESIAN_POINT('Ctrl Pts',(1.06421374343355,18.5992983501411,12.0529391494687));
#281331=CARTESIAN_POINT('Ctrl Pts',(2.61155160394646,18.6608047950825,11.8146224045516));
#281332=CARTESIAN_POINT('Ctrl Pts',(5.56379596545282,18.7827296562989,10.7500627379407));
#281333=CARTESIAN_POINT('Ctrl Pts',(6.93541654357681,18.8473368381549,9.92065605796218));
#281334=CARTESIAN_POINT('Ctrl Pts',(9.24804821503675,18.9733897874021,7.80212390376018));
#281335=CARTESIAN_POINT('Ctrl Pts',(10.1769150740052,19.0316892688132,6.54445894792941));
#281336=CARTESIAN_POINT('Ctrl Pts',(11.5114761381718,19.1565539965407,3.73240337121364));
#281337=CARTESIAN_POINT('Ctrl Pts',(11.8993775818987,19.2202692144908,2.20225384953143));
#281338=CARTESIAN_POINT('Ctrl Pts',(12.0670171356895,19.3429651122583,-0.932581864117961));
#281339=CARTESIAN_POINT('Ctrl Pts',(11.8404541475837,19.4047021708096,-2.50728436645661));
#281340=CARTESIAN_POINT('Ctrl Pts',(10.8014812183748,19.5309596803679,-5.45158573014176));
#281341=CARTESIAN_POINT('Ctrl Pts',(10.0097370355131,19.590281420537,-6.79683341854125));
#281342=CARTESIAN_POINT('Ctrl Pts',(7.93898916468252,19.7136563001511,-9.13565450066491));
#281343=CARTESIAN_POINT('Ctrl Pts',(6.67080256472679,19.7780610985413,-10.0989138953897));
#281344=CARTESIAN_POINT('Ctrl Pts',(3.85297940085754,19.9028929174297,-11.4707507153434));
#281345=CARTESIAN_POINT('Ctrl Pts',(2.33397058749204,19.9618389064488,-11.8733358465505));
#281346=CARTESIAN_POINT('Ctrl Pts',(-0.770408670177771,20.0874136852702,
-12.0756783444384));
#281347=CARTESIAN_POINT('Ctrl Pts',(-2.32618338058681,20.1500423328747,
-11.8744996390425));
#281348=CARTESIAN_POINT('Ctrl Pts',(-5.30942924959274,20.2713517207859,
-10.8784957640785));
#281349=CARTESIAN_POINT('Ctrl Pts',(-6.70343678962387,20.3359696460101,
-10.079450243893));
#281350=CARTESIAN_POINT('Ctrl Pts',(-9.06562792711455,20.4624049835879,
-8.01304816733746));
#281351=CARTESIAN_POINT('Ctrl Pts',(-10.0223073212644,20.5207532078552,
-6.77849117207222));
#281352=CARTESIAN_POINT('Ctrl Pts',(-11.332244142844,20.6372210020077,-4.17670102245711));
#281353=CARTESIAN_POINT('Ctrl Pts',(-11.7336475631444,20.6928494368794,
-2.86114296700866));
#281354=CARTESIAN_POINT('Ctrl Pts',(-11.9683983166688,20.7671550289339,
-1.0059500786248));
#281355=CARTESIAN_POINT('Ctrl Pts',(-12.,20.7869061651797,-0.502815432834886));
#281356=CARTESIAN_POINT('Ctrl Pts',(-12.,20.806249999928,1.63757896132211E-14));
#281357=CARTESIAN_POINT('Origin',(-3.46944695195361E-15,49.3876222290585,
0.));
#281358=CARTESIAN_POINT('',(44.1739130434783,2.43125000000001,5.40974412145092E-15));
#281359=CARTESIAN_POINT('Origin',(7.22658086056641E-16,2.43125000000001,
0.));
#281360=CARTESIAN_POINT('Origin',(0.,-9.56874999999999,0.));
#281361=CARTESIAN_POINT('',(-22.0315642065426,2.43125000000001,0.));
#281362=CARTESIAN_POINT('Origin',(4.95183270959582E-16,2.43125000000001,
0.));
#281363=CARTESIAN_POINT('',(-8.01975608296216,9.72176245732409,-13.890625));
#281364=CARTESIAN_POINT('',(-16.0395121659243,9.72176245732407,1.30104260698261E-14));
#281365=CARTESIAN_POINT('Origin',(-12.0296341244432,-9.56874999999999,-6.94531250000001));
#281366=CARTESIAN_POINT('',(8.01975608296213,9.7217624573241,-13.890625));
#281367=CARTESIAN_POINT('Origin',(6.00925839494864E-15,-9.56874999999999,
-13.890625));
#281368=CARTESIAN_POINT('',(16.0395121659243,9.7217624573241,-3.46944695195361E-15));
#281369=CARTESIAN_POINT('Origin',(12.0296341244432,-9.56874999999999,-6.94531249999999));
#281370=CARTESIAN_POINT('',(8.01975608296214,9.7217624573241,13.890625));
#281371=CARTESIAN_POINT('Origin',(12.0296341244432,-9.56874999999999,6.94531249999999));
#281372=CARTESIAN_POINT('',(-8.01975608296215,9.72176245732409,13.890625));
#281373=CARTESIAN_POINT('Origin',(0.,-9.56874999999999,13.890625));
#281374=CARTESIAN_POINT('Origin',(-12.0296341244432,-9.56874999999999,6.94531250000002));
#281375=CARTESIAN_POINT('Origin',(0.,21.43125,0.));
#281376=CARTESIAN_POINT('',(-8.01975608296215,17.0122749146482,13.890625));
#281377=CARTESIAN_POINT('',(8.01975608296214,17.0122749146482,13.890625));
#281378=CARTESIAN_POINT('Ctrl Pts',(8.01975608295684,17.012274914652,13.890625));
#281379=CARTESIAN_POINT('Ctrl Pts',(-1.37667655053519E-14,22.7389742468655,
13.890625));
#281380=CARTESIAN_POINT('Ctrl Pts',(-8.01975608295687,17.0122749146519,
13.890625));
#281381=CARTESIAN_POINT('',(16.0395121659243,17.0122749146482,-6.01981791101278E-16));
#281382=CARTESIAN_POINT('Ctrl Pts',(8.01975608296478,17.0122749146519,13.8906249999954));
#281383=CARTESIAN_POINT('Ctrl Pts',(12.0296341244432,22.7389742468655,6.9453125));
#281384=CARTESIAN_POINT('Ctrl Pts',(16.0395121659216,17.012274914652,4.58946936354325E-12));
#281385=CARTESIAN_POINT('',(8.01975608296213,17.0122749146482,-13.890625));
#281386=CARTESIAN_POINT('Ctrl Pts',(16.0395121659216,17.0122749146519,-4.58054260572454E-12));
#281387=CARTESIAN_POINT('Ctrl Pts',(12.0296341244432,22.7389742468655,-6.9453125));
#281388=CARTESIAN_POINT('Ctrl Pts',(8.01975608296477,17.0122749146519,-13.8906249999954));
#281389=CARTESIAN_POINT('',(4.73454552372624E-15,20.0812038373766,-13.890625));
#281390=CARTESIAN_POINT('Ctrl Pts',(8.01975608295685,17.0122749146519,-13.890625));
#281391=CARTESIAN_POINT('Ctrl Pts',(3.72198175111144,20.0812038373766,-13.890625));
#281392=CARTESIAN_POINT('Ctrl Pts',(7.76798010301187E-15,20.0812038373766,
-13.890625));
#281393=CARTESIAN_POINT('',(1.58534355170872E-15,21.43125,-12.9453125));
#281394=CARTESIAN_POINT('',(1.58534355170872E-15,21.43125,-12.9453125));
#281395=CARTESIAN_POINT('Origin',(0.,21.43125,0.));
#281396=CARTESIAN_POINT('',(-8.01975608296216,17.0122749146481,-13.890625));
#281397=CARTESIAN_POINT('Ctrl Pts',(7.76798010301187E-15,20.0812038373766,
-13.890625));
#281398=CARTESIAN_POINT('Ctrl Pts',(-3.72198175111144,20.0812038373766,
-13.890625));
#281399=CARTESIAN_POINT('Ctrl Pts',(-8.01975608295688,17.0122749146519,
-13.890625));
#281400=CARTESIAN_POINT('',(-16.0395121659243,17.0122749146481,1.30536815232815E-14));
#281401=CARTESIAN_POINT('Ctrl Pts',(-8.01975608296479,17.0122749146519,
-13.8906249999954));
#281402=CARTESIAN_POINT('Ctrl Pts',(-12.0296341244432,22.7389742468655,
-6.9453125));
#281403=CARTESIAN_POINT('Ctrl Pts',(-16.0395121659217,17.0122749146519,
-4.55934155590512E-12));
#281404=CARTESIAN_POINT('Ctrl Pts',(-16.0395121659217,17.0122749146519,
4.55859765942022E-12));
#281405=CARTESIAN_POINT('Ctrl Pts',(-12.0296341244432,22.7389742468655,
6.9453125));
#281406=CARTESIAN_POINT('Ctrl Pts',(-8.01975608296479,17.0122749146519,
13.8906249999954));
#281407=CARTESIAN_POINT('Origin',(-1.38777878078145E-14,20.90625,0.));
#281408=CARTESIAN_POINT('',(-1.95755827123136E-14,20.3673715931731,-11.461121593173));
#281409=CARTESIAN_POINT('Ctrl Pts',(-11.7339375393676,20.90625,2.51290863785773));
#281410=CARTESIAN_POINT('Ctrl Pts',(-11.9751037228422,20.8729010024019,
1.2275388253564));
#281411=CARTESIAN_POINT('Ctrl Pts',(-12.0064975767267,20.8411511224719,
-0.0964311651186414));
#281412=CARTESIAN_POINT('Ctrl Pts',(-11.6381351713344,20.7755984205093,
-2.65589242107953));
#281413=CARTESIAN_POINT('Ctrl Pts',(-11.254907610849,20.7423798220322,-3.8780745371738));
#281414=CARTESIAN_POINT('Ctrl Pts',(-10.0336965717947,20.6719176402762,
-6.31370393917634));
#281415=CARTESIAN_POINT('Ctrl Pts',(-9.10186287045269,20.6340528713554,
-7.57878102606151));
#281416=CARTESIAN_POINT('Ctrl Pts',(-6.72218311670212,20.5519138071734,
-9.62438013593598));
#281417=CARTESIAN_POINT('Ctrl Pts',(-5.42418150086199,20.5124695780735,
-10.3671437985956));
#281418=CARTESIAN_POINT('Ctrl Pts',(-2.63477883810742,20.4369825184929,
-11.3209167902397));
#281419=CARTESIAN_POINT('Ctrl Pts',(-1.26957078800877,20.4014603019892,
-11.4952103019892));
#281420=CARTESIAN_POINT('Ctrl Pts',(-3.4555691641458E-14,20.3673715931731,
-11.461121593173));
#281421=CARTESIAN_POINT('',(-1.54116579237465E-14,21.43125,-12.525));
#281422=CARTESIAN_POINT('',(-1.53473639667913E-14,20.90625,-12.));
#281423=CARTESIAN_POINT('Origin',(-1.38777878078145E-14,21.43125,0.));
#281424=CARTESIAN_POINT('Ctrl Pts',(-3.34454686168328E-14,20.3673715931731,
-11.461121593173));
#281425=CARTESIAN_POINT('Ctrl Pts',(0.158753063369545,20.3631089817441,
-11.456858981744));
#281426=CARTESIAN_POINT('Ctrl Pts',(0.316010936333406,20.3588817583139,
-11.4493328807581));
#281427=CARTESIAN_POINT('Ctrl Pts',(1.94465535673269,20.3150547579429,-11.3383180821017));
#281428=CARTESIAN_POINT('Ctrl Pts',(3.39261700236661,20.277278273539,-10.9535572953072));
#281429=CARTESIAN_POINT('Ctrl Pts',(6.03062359817187,20.1990638465944,-9.65839939732408));
#281430=CARTESIAN_POINT('Ctrl Pts',(7.20257467898127,20.15889608411,-8.76757326626974));
#281431=CARTESIAN_POINT('Ctrl Pts',(9.15722478991995,20.0796650678951,-6.57145272022985));
#281432=CARTESIAN_POINT('Ctrl Pts',(9.91561896638193,20.0412329954549,-5.27980368737507));
#281433=CARTESIAN_POINT('Ctrl Pts',(10.8951016967142,19.9572267702433,-2.41007461461997));
#281434=CARTESIAN_POINT('Ctrl Pts',(11.055757000172,19.9173988404041,-0.940533523605604));
#281435=CARTESIAN_POINT('Ctrl Pts',(10.8761591813622,19.8435344687281,1.79187774688301));
#281436=CARTESIAN_POINT('Ctrl Pts',(10.5287658487941,19.8047358903491,3.13038442126089));
#281437=CARTESIAN_POINT('Ctrl Pts',(9.36849149367791,19.7283234991857,5.58068678118078));
#281438=CARTESIAN_POINT('Ctrl Pts',(8.5319769564679,19.6901718697845,6.77150405317055));
#281439=CARTESIAN_POINT('Ctrl Pts',(6.35602709403731,19.6072340141407,8.71949207523714));
#281440=CARTESIAN_POINT('Ctrl Pts',(5.15415641864755,19.5670375971829,9.43423088151185));
#281441=CARTESIAN_POINT('Ctrl Pts',(3.19699827938916,19.5088390625049,10.1327998304645));
#281442=CARTESIAN_POINT('Ctrl Pts',(2.52327522205536,19.4898163385168,10.3018141492848));
#281443=CARTESIAN_POINT('Ctrl Pts',(0.50150453708759,19.4312152241487,10.5990933398486));
#281444=CARTESIAN_POINT('Ctrl Pts',(-0.858157973261501,19.3913667357374,
10.5365366445161));
#281445=CARTESIAN_POINT('Ctrl Pts',(-3.49187560718385,19.3133023101555,
9.89775066976008));
#281446=CARTESIAN_POINT('Ctrl Pts',(-4.7388067620056,19.2752321029848,9.3230150982916));
#281447=CARTESIAN_POINT('Ctrl Pts',(-6.38216076388607,19.214649651135,8.12285448752604));
#281448=CARTESIAN_POINT('Ctrl Pts',(-6.88402838863904,19.1946133285548,
7.67529956416046));
#281449=CARTESIAN_POINT('Ctrl Pts',(-8.17460081443321,19.1383957584764,
6.27619662308116));
#281450=CARTESIAN_POINT('Ctrl Pts',(-8.84515327331929,19.103594295001,5.22343353132837));
#281451=CARTESIAN_POINT('Ctrl Pts',(-9.75620235107338,19.0300319619295,
2.95820155339676));
#281452=CARTESIAN_POINT('Ctrl Pts',(-10.0025670660582,18.9932662710101,
1.7720386495763));
#281453=CARTESIAN_POINT('Ctrl Pts',(-10.0352413152989,18.9576928414942,
0.570469052221604));
#281454=CARTESIAN_POINT('Ctrl Pts',(-7.47704554734297,18.9576928414942,
-6.71753623576258));
#281455=CARTESIAN_POINT('Ctrl Pts',(-8.22914229169097,19.0695296791179,
-6.04774602181526));
#281456=CARTESIAN_POINT('Ctrl Pts',(-8.78589634872411,19.1631164093256,
-5.34312658694975));
#281457=CARTESIAN_POINT('Ctrl Pts',(-9.6773533567784,19.3393049469732,-3.99501404107446));
#281458=CARTESIAN_POINT('Ctrl Pts',(-10.0676634679168,19.4352867858775,
-3.2040722529385));
#281459=CARTESIAN_POINT('Ctrl Pts',(-10.9065983101053,19.7103902849491,
-0.775444565914872));
#281460=CARTESIAN_POINT('Ctrl Pts',(-10.9837592295337,19.8520315258032,
0.697500172039842));
#281461=CARTESIAN_POINT('Ctrl Pts',(-10.8105004116642,20.1219190682211,
3.33356522839727));
#281462=CARTESIAN_POINT('Ctrl Pts',(-10.4176784074616,20.2734600759145,
4.78318445517766));
#281463=CARTESIAN_POINT('Ctrl Pts',(-9.36828133989022,20.4995570830846,
6.8826953758291));
#281464=CARTESIAN_POINT('Ctrl Pts',(-8.89210207419248,20.5800256968209,
7.61064915299536));
#281465=CARTESIAN_POINT('Ctrl Pts',(-7.81751963755748,20.7432184861572,
8.92850556434733));
#281466=CARTESIAN_POINT('Ctrl Pts',(-7.21026201465552,20.8252469301455,
9.52852756505014));
#281467=CARTESIAN_POINT('Ctrl Pts',(-6.5440620647558,20.90625,10.0585909397204));
#281468=CARTESIAN_POINT('Origin',(0.,21.43125,0.));
#281469=CARTESIAN_POINT('Origin',(-8.01975608296216,21.43125,-13.890625));
#281470=CARTESIAN_POINT('',(-8.01975608296216,21.43125,-13.890625));
#281471=CARTESIAN_POINT('',(-16.0395121659243,21.43125,1.21746868952018E-14));
#281472=CARTESIAN_POINT('Origin',(-16.0395121659243,21.43125,1.21746868952018E-14));
#281473=CARTESIAN_POINT('',(-8.01975608296215,21.43125,13.890625));
#281474=CARTESIAN_POINT('Origin',(-8.01975608296215,21.43125,13.890625));
#281475=CARTESIAN_POINT('',(8.01975608296214,21.43125,13.890625));
#281476=CARTESIAN_POINT('Origin',(8.01975608296214,21.43125,13.890625));
#281477=CARTESIAN_POINT('',(16.0395121659243,21.43125,-2.37169225231204E-15));
#281478=CARTESIAN_POINT('Origin',(16.0395121659243,21.43125,-2.37169225231204E-15));
#281479=CARTESIAN_POINT('',(8.01975608296213,21.43125,-13.890625));
#281480=CARTESIAN_POINT('Origin',(8.01975608296213,21.43125,-13.890625));
#281481=CARTESIAN_POINT('Origin',(-44.1739130434783,2.43125000000001,0.));
#281482=CARTESIAN_POINT('Origin',(-1.38777878078145E-14,2.43125000000001,
0.));
#281483=CARTESIAN_POINT('Ctrl Pts',(10.0514428414954,2.43125000000002,1.00752739484733E-13));
#281484=CARTESIAN_POINT('Ctrl Pts',(10.1143780835885,2.43125000000002,-0.791127473640706));
#281485=CARTESIAN_POINT('Ctrl Pts',(10.0855072982437,2.43125000000002,-1.58682843497015));
#281486=CARTESIAN_POINT('Ctrl Pts',(9.84523379682252,2.43125000000002,-3.15557179232318));
#281487=CARTESIAN_POINT('Ctrl Pts',(9.63470068842676,2.43125000000002,-3.92325055631404));
#281488=CARTESIAN_POINT('Ctrl Pts',(8.67230516055593,2.43125000000002,-6.30994543448733));
#281489=CARTESIAN_POINT('Ctrl Pts',(7.71286120753459,2.43125000000002,-7.46066276667367));
#281490=CARTESIAN_POINT('Ctrl Pts',(6.06627958599162,2.43125000000002,-9.1152206243862));
#281491=CARTESIAN_POINT('Ctrl Pts',(4.9464571378071,2.43125000000001,-9.88345895797583));
#281492=CARTESIAN_POINT('Ctrl Pts',(2.75597210659317,2.43125000000001,-10.8484833593829));
#281493=CARTESIAN_POINT('Ctrl Pts',(1.37406648240357,2.43125000000002,-11.29221051564));
#281494=CARTESIAN_POINT('Ctrl Pts',(-1.98461349922251,2.43125000000001,
-11.4457083135333));
#281495=CARTESIAN_POINT('Ctrl Pts',(-3.50022085878334,2.43125000000001,
-11.1473855441023));
#281496=CARTESIAN_POINT('Ctrl Pts',(-6.14735486447011,2.43125000000001,
-10.1719281614562));
#281497=CARTESIAN_POINT('Ctrl Pts',(-7.38835529811323,2.43125000000001,
-9.4385927042382));
#281498=CARTESIAN_POINT('Ctrl Pts',(-8.46872171229246,2.43125000000001,
-8.50180878165033));
#281499=CARTESIAN_POINT('Ctrl Pts',(-12.,2.43125000000001,1.10592091040473E-12));
#281500=CARTESIAN_POINT('Ctrl Pts',(-11.8804643241478,2.43125000000001,
1.79391945396996));
#281501=CARTESIAN_POINT('Ctrl Pts',(-11.3990610613138,2.43125000000001,
3.13396898737023));
#281502=CARTESIAN_POINT('Ctrl Pts',(-10.4104157884427,2.43125000000001,
5.318570795906));
#281503=CARTESIAN_POINT('Ctrl Pts',(-9.57359601299618,2.43125000000001,
6.56829747585552));
#281504=CARTESIAN_POINT('Ctrl Pts',(-7.38873844522587,2.43125000000001,
8.65742934749614));
#281505=CARTESIAN_POINT('Ctrl Pts',(-6.14298665404833,2.43125,9.45156675706131));
#281506=CARTESIAN_POINT('Ctrl Pts',(-3.8073824930157,2.43125,10.362657594245));
#281507=CARTESIAN_POINT('Ctrl Pts',(-2.35484140538957,2.43125000000001,
10.778449175978));
#281508=CARTESIAN_POINT('Ctrl Pts',(1.15015301169903,2.43125000000001,10.6841950237441));
#281509=CARTESIAN_POINT('Ctrl Pts',(2.53388342843634,2.43125000000001,10.2413561793839));
#281510=CARTESIAN_POINT('Ctrl Pts',(4.18319669729398,2.43125000000002,9.5097960999229));
#281511=CARTESIAN_POINT('Ctrl Pts',(4.85072362354194,2.43125000000002,9.11749903031561));
#281512=CARTESIAN_POINT('Ctrl Pts',(6.06416700972034,2.43125000000002,8.20405583130882));
#281513=CARTESIAN_POINT('Ctrl Pts',(6.60953367471901,2.43125000000002,7.69028293020246));
#281514=CARTESIAN_POINT('Ctrl Pts',(7.09357268597975,2.43125000000002,7.12128708482873));
#281515=CARTESIAN_POINT('Ctrl Pts',(-10.0514365206283,-1.69375364933639,
2.46189191236404E-15));
#281516=CARTESIAN_POINT('Ctrl Pts',(-10.0514365206283,-1.54375364933699,
3.26590970098687));
#281517=CARTESIAN_POINT('Ctrl Pts',(-8.13178296306926,-1.39375364933759,
5.90808615117926));
#281518=CARTESIAN_POINT('Ctrl Pts',(-6.21212940551025,-1.24375364933819,
8.55026260137164));
#281519=CARTESIAN_POINT('Ctrl Pts',(-3.10606470275513,-1.09375364933879,
9.55948420107058));
#281520=CARTESIAN_POINT('Ctrl Pts',(-9.99267301601491E-15,-0.943753649339386,
10.5687058007695));
#281521=CARTESIAN_POINT('Ctrl Pts',(3.10606470275511,-0.793753649339984,
9.55948420107058));
#281522=CARTESIAN_POINT('Ctrl Pts',(6.21212940551023,-0.643753649340582,
8.55026260137164));
#281523=CARTESIAN_POINT('Ctrl Pts',(8.13178296306923,-0.493753649341181,
5.90808615117925));
#281524=CARTESIAN_POINT('Ctrl Pts',(10.0514365206282,-0.34375364934178,
3.26590970098687));
#281525=CARTESIAN_POINT('Ctrl Pts',(10.0514365206282,-0.19375364934238,
-1.23094595618202E-15));
#281526=CARTESIAN_POINT('Ctrl Pts',(10.0514365206282,-0.0437536493429801,
-3.26590970098687));
#281527=CARTESIAN_POINT('Ctrl Pts',(8.13178296306923,0.106246350656419,
-5.90808615117926));
#281528=CARTESIAN_POINT('Ctrl Pts',(6.21212940551023,0.256246350655818,
-8.55026260137164));
#281529=CARTESIAN_POINT('Ctrl Pts',(3.10606470275511,0.406246350655216,
-9.55948420107058));
#281530=CARTESIAN_POINT('Ctrl Pts',(-1.34451139978543E-14,0.556246350654614,
-10.5687058007695));
#281531=CARTESIAN_POINT('Ctrl Pts',(-3.10606470275513,0.706246350654012,
-9.55948420107058));
#281532=CARTESIAN_POINT('Ctrl Pts',(-6.21212940551025,0.85624635065341,
-8.55026260137164));
#281533=CARTESIAN_POINT('Ctrl Pts',(-8.13178296306926,1.00624635065281,
-5.90808615117925));
#281534=CARTESIAN_POINT('Ctrl Pts',(-10.0514365206283,1.15624635065221,
-3.26590970098687));
#281535=CARTESIAN_POINT('Ctrl Pts',(-10.0514365206283,1.30624635065161,
2.46189191236404E-15));
#281536=CARTESIAN_POINT('Ctrl Pts',(-10.0514365206283,1.45624635065101,
3.26590970098687));
#281537=CARTESIAN_POINT('Ctrl Pts',(-8.13178296306926,1.60624635065041,
5.90808615117926));
#281538=CARTESIAN_POINT('Ctrl Pts',(-6.21212940551025,1.75624635064981,
8.55026260137164));
#281539=CARTESIAN_POINT('Ctrl Pts',(-3.10606470275513,1.90624635064921,
9.55948420107058));
#281540=CARTESIAN_POINT('Ctrl Pts',(-1.17203822876767E-14,2.05624635064861,
10.5687058007695));
#281541=CARTESIAN_POINT('Ctrl Pts',(3.10606470275511,2.20624635064802,9.55948420107058));
#281542=CARTESIAN_POINT('Ctrl Pts',(6.21212940551023,2.35624635064742,8.55026260137164));
#281543=CARTESIAN_POINT('Ctrl Pts',(8.13178296306923,2.50624635064682,5.90808615117925));
#281544=CARTESIAN_POINT('Ctrl Pts',(10.0514365206282,2.65624635064622,3.26590970098687));
#281545=CARTESIAN_POINT('Ctrl Pts',(10.0514365206282,2.80624635064562,-1.23094595618202E-15));
#281546=CARTESIAN_POINT('Ctrl Pts',(10.0514365206282,2.95624635064502,-3.26590970098687));
#281547=CARTESIAN_POINT('Ctrl Pts',(8.13178296306923,3.10624635064442,-5.90808615117926));
#281548=CARTESIAN_POINT('Ctrl Pts',(6.21212940551023,3.25624635064382,-8.55026260137164));
#281549=CARTESIAN_POINT('Ctrl Pts',(3.10606470275511,3.40624635064322,-9.55948420107058));
#281550=CARTESIAN_POINT('Ctrl Pts',(-1.51728232695162E-14,3.55624635064261,
-10.5687058007695));
#281551=CARTESIAN_POINT('Ctrl Pts',(-3.10606470275514,3.70624635064201,
-9.55948420107058));
#281552=CARTESIAN_POINT('Ctrl Pts',(-6.21212940551026,3.85624635064141,
-8.55026260137164));
#281553=CARTESIAN_POINT('Ctrl Pts',(-8.13178296306926,4.00624635064081,
-5.90808615117925));
#281554=CARTESIAN_POINT('Ctrl Pts',(-10.0514365206283,4.15624635064021,
-3.26590970098687));
#281555=CARTESIAN_POINT('Ctrl Pts',(-10.0514365206283,4.30624635063961,
2.46189191236404E-15));
#281556=CARTESIAN_POINT('Ctrl Pts',(-10.0514365206283,4.45624635063901,
3.26590970098687));
#281557=CARTESIAN_POINT('Ctrl Pts',(-8.13178296306926,4.60624635063841,
5.90808615117926));
#281558=CARTESIAN_POINT('Ctrl Pts',(-6.21212940551025,4.75624635063781,
8.55026260137164));
#281559=CARTESIAN_POINT('Ctrl Pts',(-3.10606470275513,4.90624635063721,
9.55948420107058));
#281560=CARTESIAN_POINT('Ctrl Pts',(-1.34480915593386E-14,5.05624635063661,
10.5687058007695));
#281561=CARTESIAN_POINT('Ctrl Pts',(3.10606470275511,5.20624635063602,9.55948420107058));
#281562=CARTESIAN_POINT('Ctrl Pts',(6.21212940551023,5.35624635063542,8.55026260137164));
#281563=CARTESIAN_POINT('Ctrl Pts',(8.13178296306923,5.50624635063482,5.90808615117925));
#281564=CARTESIAN_POINT('Ctrl Pts',(10.0514365206282,5.65624635063422,3.26590970098687));
#281565=CARTESIAN_POINT('Ctrl Pts',(10.0514365206282,5.80624635063362,-1.23094595618202E-15));
#281566=CARTESIAN_POINT('Ctrl Pts',(10.0514365206282,5.95624635063302,-3.26590970098687));
#281567=CARTESIAN_POINT('Ctrl Pts',(8.13178296306923,6.10624635063242,-5.90808615117926));
#281568=CARTESIAN_POINT('Ctrl Pts',(6.21212940551023,6.25624635063182,-8.55026260137164));
#281569=CARTESIAN_POINT('Ctrl Pts',(3.1060647027551,6.40624635063122,-9.55948420107058));
#281570=CARTESIAN_POINT('Ctrl Pts',(-1.6900532541178E-14,6.55624635063061,
-10.5687058007695));
#281571=CARTESIAN_POINT('Ctrl Pts',(-3.10606470275514,6.70624635063001,
-9.55948420107058));
#281572=CARTESIAN_POINT('Ctrl Pts',(-6.21212940551026,6.85624635062941,
-8.55026260137164));
#281573=CARTESIAN_POINT('Ctrl Pts',(-8.13178296306926,7.00624635062881,
-5.90808615117925));
#281574=CARTESIAN_POINT('Ctrl Pts',(-10.0514365206283,7.15624635062821,
-3.26590970098687));
#281575=CARTESIAN_POINT('Ctrl Pts',(-10.0514365206283,7.30624635062761,
2.46189191236404E-15));
#281576=CARTESIAN_POINT('Ctrl Pts',(-10.0514365206283,7.45624635062701,
3.26590970098687));
#281577=CARTESIAN_POINT('Ctrl Pts',(-8.13178296306926,7.60624635062641,
5.90808615117926));
#281578=CARTESIAN_POINT('Ctrl Pts',(-6.21212940551025,7.75624635062581,
8.55026260137164));
#281579=CARTESIAN_POINT('Ctrl Pts',(-3.10606470275514,7.90624635062521,
9.55948420107058));
#281580=CARTESIAN_POINT('Ctrl Pts',(-1.51758008310004E-14,8.05624635062462,
10.5687058007695));
#281581=CARTESIAN_POINT('Ctrl Pts',(3.1060647027551,8.20624635062402,9.55948420107058));
#281582=CARTESIAN_POINT('Ctrl Pts',(6.21212940551023,8.35624635062342,8.55026260137164));
#281583=CARTESIAN_POINT('Ctrl Pts',(8.13178296306923,8.50624635062282,5.90808615117925));
#281584=CARTESIAN_POINT('Ctrl Pts',(10.0514365206282,8.65624635062222,3.26590970098687));
#281585=CARTESIAN_POINT('Ctrl Pts',(10.0514365206282,8.80624635062162,-1.23094595618202E-15));
#281586=CARTESIAN_POINT('Ctrl Pts',(10.0514365206282,8.95624635062102,-3.26590970098687));
#281587=CARTESIAN_POINT('Ctrl Pts',(8.13178296306923,9.10624635062042,-5.90808615117926));
#281588=CARTESIAN_POINT('Ctrl Pts',(6.21212940551022,9.25624635061982,-8.55026260137164));
#281589=CARTESIAN_POINT('Ctrl Pts',(3.1060647027551,9.40624635061922,-9.55948420107058));
#281590=CARTESIAN_POINT('Ctrl Pts',(-1.86282418128398E-14,9.55624635061861,
-10.5687058007695));
#281591=CARTESIAN_POINT('Ctrl Pts',(-3.10606470275514,9.70624635061801,
-9.55948420107058));
#281592=CARTESIAN_POINT('Ctrl Pts',(-6.21212940551026,9.85624635061741,
-8.55026260137164));
#281593=CARTESIAN_POINT('Ctrl Pts',(-8.13178296306926,10.0062463506168,
-5.90808615117925));
#281594=CARTESIAN_POINT('Ctrl Pts',(-10.0514365206283,10.1562463506162,
-3.26590970098687));
#281595=CARTESIAN_POINT('Ctrl Pts',(-10.0514365206283,10.3062463506156,
2.46189191236404E-15));
#281596=CARTESIAN_POINT('Ctrl Pts',(-10.0514365206283,10.456246350615,3.26590970098687));
#281597=CARTESIAN_POINT('Ctrl Pts',(-8.13178296306926,10.6062463506144,
5.90808615117926));
#281598=CARTESIAN_POINT('Ctrl Pts',(-6.21212940551026,10.7562463506138,
8.55026260137164));
#281599=CARTESIAN_POINT('Ctrl Pts',(-3.10606470275514,10.9062463506132,
9.55948420107058));
#281600=CARTESIAN_POINT('Ctrl Pts',(-1.69035101026623E-14,11.0562463506126,
10.5687058007695));
#281601=CARTESIAN_POINT('Ctrl Pts',(3.1060647027551,11.206246350612,9.55948420107058));
#281602=CARTESIAN_POINT('Ctrl Pts',(6.21212940551022,11.3562463506114,8.55026260137164));
#281603=CARTESIAN_POINT('Ctrl Pts',(8.13178296306923,11.5062463506108,5.90808615117925));
#281604=CARTESIAN_POINT('Ctrl Pts',(10.0514365206282,11.6562463506102,3.26590970098687));
#281605=CARTESIAN_POINT('Ctrl Pts',(10.0514365206282,11.8062463506096,-1.23094595618202E-15));
#281606=CARTESIAN_POINT('Ctrl Pts',(10.0514365206282,11.956246350609,-3.26590970098687));
#281607=CARTESIAN_POINT('Ctrl Pts',(8.13178296306923,12.1062463506084,-5.90808615117926));
#281608=CARTESIAN_POINT('Ctrl Pts',(6.21212940551022,12.2562463506078,-8.55026260137164));
#281609=CARTESIAN_POINT('Ctrl Pts',(3.1060647027551,12.4062463506072,-9.55948420107058));
#281610=CARTESIAN_POINT('Ctrl Pts',(-2.03559510845017E-14,12.5562463506066,
-10.5687058007695));
#281611=CARTESIAN_POINT('Ctrl Pts',(-3.10606470275514,12.706246350606,-9.55948420107058));
#281612=CARTESIAN_POINT('Ctrl Pts',(-6.21212940551026,12.8562463506054,
-8.55026260137164));
#281613=CARTESIAN_POINT('Ctrl Pts',(-8.13178296306927,13.0062463506048,
-5.90808615117925));
#281614=CARTESIAN_POINT('Ctrl Pts',(-10.0514365206283,13.1562463506042,
-3.26590970098687));
#281615=CARTESIAN_POINT('Ctrl Pts',(-10.0514365206283,13.3062463506036,
2.46189191236404E-15));
#281616=CARTESIAN_POINT('Ctrl Pts',(-10.0514365206283,13.456246350603,3.26590970098687));
#281617=CARTESIAN_POINT('Ctrl Pts',(-8.13178296306927,13.6062463506024,
5.90808615117926));
#281618=CARTESIAN_POINT('Ctrl Pts',(-6.21212940551026,13.7562463506018,
8.55026260137164));
#281619=CARTESIAN_POINT('Ctrl Pts',(-3.10606470275514,13.9062463506012,
9.55948420107058));
#281620=CARTESIAN_POINT('Ctrl Pts',(-1.86312193743241E-14,14.0562463506006,
10.5687058007695));
#281621=CARTESIAN_POINT('Ctrl Pts',(3.1060647027551,14.2062463506,9.55948420107058));
#281622=CARTESIAN_POINT('Ctrl Pts',(6.21212940551022,14.3562463505994,8.55026260137164));
#281623=CARTESIAN_POINT('Ctrl Pts',(8.13178296306923,14.5062463505988,5.90808615117925));
#281624=CARTESIAN_POINT('Ctrl Pts',(10.0514365206282,14.6562463505982,3.26590970098687));
#281625=CARTESIAN_POINT('Ctrl Pts',(10.0514365206282,14.8062463505976,-1.23094595618202E-15));
#281626=CARTESIAN_POINT('Ctrl Pts',(10.0514365206282,14.956246350597,-3.26590970098687));
#281627=CARTESIAN_POINT('Ctrl Pts',(8.13178296306922,15.1062463505964,-5.90808615117926));
#281628=CARTESIAN_POINT('Ctrl Pts',(6.21212940551022,15.2562463505958,-8.55026260137164));
#281629=CARTESIAN_POINT('Ctrl Pts',(3.1060647027551,15.4062463505952,-9.55948420107058));
#281630=CARTESIAN_POINT('Ctrl Pts',(-2.20836603561635E-14,15.5562463505946,
-10.5687058007695));
#281631=CARTESIAN_POINT('Ctrl Pts',(-3.10606470275514,15.706246350594,-9.55948420107058));
#281632=CARTESIAN_POINT('Ctrl Pts',(-6.21212940551026,15.8562463505934,
-8.55026260137164));
#281633=CARTESIAN_POINT('Ctrl Pts',(-8.13178296306927,16.0062463505928,
-5.90808615117925));
#281634=CARTESIAN_POINT('Ctrl Pts',(-10.0514365206283,16.1562463505922,
-3.26590970098687));
#281635=CARTESIAN_POINT('Ctrl Pts',(-10.0514365206283,16.3062463505916,
2.46189191236404E-15));
#281636=CARTESIAN_POINT('Ctrl Pts',(-10.0514365206283,16.456246350591,3.26590970098687));
#281637=CARTESIAN_POINT('Ctrl Pts',(-8.13178296306927,16.6062463505904,
5.90808615117926));
#281638=CARTESIAN_POINT('Ctrl Pts',(-6.21212940551026,16.7562463505898,
8.55026260137164));
#281639=CARTESIAN_POINT('Ctrl Pts',(-3.10606470275514,16.9062463505892,
9.55948420107058));
#281640=CARTESIAN_POINT('Ctrl Pts',(-2.03589286459859E-14,17.0562463505886,
10.5687058007695));
#281641=CARTESIAN_POINT('Ctrl Pts',(3.1060647027551,17.206246350588,9.55948420107058));
#281642=CARTESIAN_POINT('Ctrl Pts',(6.21212940551022,17.3562463505874,8.55026260137164));
#281643=CARTESIAN_POINT('Ctrl Pts',(8.13178296306922,17.5062463505868,5.90808615117925));
#281644=CARTESIAN_POINT('Ctrl Pts',(10.0514365206282,17.6562463505862,3.26590970098687));
#281645=CARTESIAN_POINT('Ctrl Pts',(10.0514365206282,17.8062463505856,-1.23094595618202E-15));
#281646=CARTESIAN_POINT('Ctrl Pts',(10.0514365206282,17.956246350585,-3.26590970098687));
#281647=CARTESIAN_POINT('Ctrl Pts',(8.13178296306922,18.1062463505844,-5.90808615117926));
#281648=CARTESIAN_POINT('Ctrl Pts',(6.21212940551022,18.2562463505838,-8.55026260137164));
#281649=CARTESIAN_POINT('Ctrl Pts',(3.1060647027551,18.4062463505832,-9.55948420107058));
#281650=CARTESIAN_POINT('Ctrl Pts',(-2.38113696278254E-14,18.5562463505826,
-10.5687058007695));
#281651=CARTESIAN_POINT('Ctrl Pts',(-3.10606470275514,18.706246350582,-9.55948420107058));
#281652=CARTESIAN_POINT('Ctrl Pts',(-6.21212940551027,18.8562463505814,
-8.55026260137164));
#281653=CARTESIAN_POINT('Ctrl Pts',(-8.13178296306927,19.0062463505808,
-5.90808615117925));
#281654=CARTESIAN_POINT('Ctrl Pts',(-10.0514365206283,19.1562463505802,
-3.26590970098687));
#281655=CARTESIAN_POINT('Ctrl Pts',(-10.0514365206283,19.3062463505796,
2.46189191236404E-15));
#281656=CARTESIAN_POINT('Ctrl Pts',(-10.0514365206283,19.456246350579,3.26590970098687));
#281657=CARTESIAN_POINT('Ctrl Pts',(-8.13178296306927,19.6062463505784,
5.90808615117926));
#281658=CARTESIAN_POINT('Ctrl Pts',(-6.21212940551026,19.7562463505778,
8.55026260137164));
#281659=CARTESIAN_POINT('Ctrl Pts',(-3.10606470275514,19.9062463505772,
9.55948420107058));
#281660=CARTESIAN_POINT('Ctrl Pts',(-2.20866379176478E-14,20.0562463505766,
10.5687058007695));
#281661=CARTESIAN_POINT('Ctrl Pts',(3.1060647027551,20.206246350576,9.55948420107058));
#281662=CARTESIAN_POINT('Ctrl Pts',(6.21212940551022,20.3562463505754,8.55026260137164));
#281663=CARTESIAN_POINT('Ctrl Pts',(8.13178296306922,20.5062463505748,5.90808615117925));
#281664=CARTESIAN_POINT('Ctrl Pts',(10.0514365206282,20.6562463505742,3.26590970098687));
#281665=CARTESIAN_POINT('Ctrl Pts',(10.0514365206282,20.8062463505736,-1.23094595618202E-15));
#281666=CARTESIAN_POINT('Ctrl Pts',(10.0514365206282,20.956246350573,-3.26590970098687));
#281667=CARTESIAN_POINT('Ctrl Pts',(8.13178296306922,21.1062463505724,-5.90808615117926));
#281668=CARTESIAN_POINT('Ctrl Pts',(6.21212940551022,21.2562463505718,-8.55026260137164));
#281669=CARTESIAN_POINT('Ctrl Pts',(3.1060647027551,21.4062463505712,-9.55948420107058));
#281670=CARTESIAN_POINT('Ctrl Pts',(-2.55390788994872E-14,21.5562463505706,
-10.5687058007695));
#281671=CARTESIAN_POINT('Ctrl Pts',(-3.10606470275515,21.70624635057,-9.55948420107058));
#281672=CARTESIAN_POINT('Ctrl Pts',(-6.21212940551027,21.8562463505694,
-8.55026260137164));
#281673=CARTESIAN_POINT('Ctrl Pts',(-8.13178296306927,22.0062463505688,
-5.90808615117925));
#281674=CARTESIAN_POINT('Ctrl Pts',(-10.0514365206283,22.1562463505682,
-3.26590970098687));
#281675=CARTESIAN_POINT('Ctrl Pts',(-10.0514365206283,22.3062463505676,
2.46189191236404E-15));
#281676=CARTESIAN_POINT('Ctrl Pts',(-10.0514365206283,22.456246350567,3.26590970098687));
#281677=CARTESIAN_POINT('Ctrl Pts',(-8.13178296306927,22.6062463505664,
5.90808615117926));
#281678=CARTESIAN_POINT('Ctrl Pts',(-6.21212940551027,22.7562463505658,
8.55026260137164));
#281679=CARTESIAN_POINT('Ctrl Pts',(-3.10606470275514,22.9062463505652,
9.55948420107058));
#281680=CARTESIAN_POINT('Ctrl Pts',(-2.38143471893096E-14,23.0562463505646,
10.5687058007695));
#281681=CARTESIAN_POINT('Ctrl Pts',(3.1060647027551,23.206246350564,9.55948420107058));
#281682=CARTESIAN_POINT('Ctrl Pts',(6.21212940551022,23.3562463505634,8.55026260137164));
#281683=CARTESIAN_POINT('Ctrl Pts',(8.13178296306922,23.5062463505628,5.90808615117925));
#281684=CARTESIAN_POINT('Ctrl Pts',(10.0514365206282,23.6562463505622,3.26590970098687));
#281685=CARTESIAN_POINT('Ctrl Pts',(10.0514365206282,23.8062463505616,-1.23094595618202E-15));
#281686=CARTESIAN_POINT('Ctrl Pts',(10.0514365206282,23.956246350561,-3.26590970098687));
#281687=CARTESIAN_POINT('Ctrl Pts',(8.13178296306922,24.1062463505604,-5.90808615117926));
#281688=CARTESIAN_POINT('Ctrl Pts',(6.21212940551021,24.2562463505598,-8.55026260137164));
#281689=CARTESIAN_POINT('Ctrl Pts',(3.10606470275509,24.4062463505592,-9.55948420107058));
#281690=CARTESIAN_POINT('Ctrl Pts',(-2.7266788171149E-14,24.5562463505586,
-10.5687058007695));
#281691=CARTESIAN_POINT('Ctrl Pts',(-3.10606470275515,24.706246350558,-9.55948420107058));
#281692=CARTESIAN_POINT('Ctrl Pts',(-6.21212940551027,24.8562463505574,
-8.55026260137164));
#281693=CARTESIAN_POINT('Ctrl Pts',(-8.13178296306927,25.0062463505568,
-5.90808615117925));
#281694=CARTESIAN_POINT('Ctrl Pts',(-10.0514365206283,25.1562463505562,
-3.26590970098687));
#281695=CARTESIAN_POINT('Ctrl Pts',(-10.0514365206283,25.3062463505556,
2.46189191236404E-15));
#281696=CARTESIAN_POINT('Ctrl Pts',(-10.0514365206283,25.456246350555,3.26590970098687));
#281697=CARTESIAN_POINT('Ctrl Pts',(-8.13178296306927,25.6062463505544,
5.90808615117926));
#281698=CARTESIAN_POINT('Ctrl Pts',(-6.21212940551027,25.7562463505538,
8.55026260137164));
#281699=CARTESIAN_POINT('Ctrl Pts',(-3.10606470275515,25.9062463505532,
9.55948420107058));
#281700=CARTESIAN_POINT('Ctrl Pts',(-2.55420564609715E-14,26.0562463505526,
10.5687058007695));
#281701=CARTESIAN_POINT('Ctrl Pts',(3.10606470275509,26.206246350552,9.55948420107058));
#281702=CARTESIAN_POINT('Ctrl Pts',(6.21212940551022,26.3562463505514,8.55026260137164));
#281703=CARTESIAN_POINT('Ctrl Pts',(8.13178296306922,26.5062463505508,5.90808615117925));
#281704=CARTESIAN_POINT('Ctrl Pts',(10.0514365206282,26.6562463505502,3.26590970098687));
#281705=CARTESIAN_POINT('Ctrl Pts',(10.0514365206282,26.8062463505496,-1.23094595618202E-15));
#281706=CARTESIAN_POINT('Ctrl Pts',(10.0514365206282,26.956246350549,-3.26590970098687));
#281707=CARTESIAN_POINT('Ctrl Pts',(8.13178296306922,27.1062463505484,-5.90808615117926));
#281708=CARTESIAN_POINT('Ctrl Pts',(6.21212940551021,27.2562463505478,-8.55026260137164));
#281709=CARTESIAN_POINT('Ctrl Pts',(3.10606470275509,27.4062463505472,-9.55948420107058));
#281710=CARTESIAN_POINT('Ctrl Pts',(-2.89944974428109E-14,27.5562463505466,
-10.5687058007695));
#281711=CARTESIAN_POINT('Ctrl Pts',(-3.10606470275515,27.706246350546,-9.55948420107058));
#281712=CARTESIAN_POINT('Ctrl Pts',(-6.21212940551027,27.8562463505454,
-8.55026260137164));
#281713=CARTESIAN_POINT('Ctrl Pts',(-8.13178296306928,28.0062463505448,
-5.90808615117925));
#281714=CARTESIAN_POINT('Ctrl Pts',(-10.0514365206283,28.1562463505442,
-3.26590970098687));
#281715=CARTESIAN_POINT('Ctrl Pts',(-10.0514365206283,28.3062463505436,
2.46189191236404E-15));
#281716=CARTESIAN_POINT('Ctrl Pts',(-10.0514365206283,28.456246350543,3.26590970098687));
#281717=CARTESIAN_POINT('Ctrl Pts',(-8.13178296306928,28.6062463505424,
5.90808615117926));
#281718=CARTESIAN_POINT('Ctrl Pts',(-6.21212940551027,28.7562463505418,
8.55026260137164));
#281719=CARTESIAN_POINT('Ctrl Pts',(-3.10606470275515,28.9062463505412,
9.55948420107058));
#281720=CARTESIAN_POINT('Ctrl Pts',(-2.72697657326333E-14,29.0562463505406,
10.5687058007695));
#281721=CARTESIAN_POINT('Ctrl Pts',(3.10606470275509,29.20624635054,9.55948420107058));
#281722=CARTESIAN_POINT('Ctrl Pts',(6.21212940551021,29.3562463505394,8.55026260137164));
#281723=CARTESIAN_POINT('Ctrl Pts',(8.13178296306922,29.5062463505388,5.90808615117925));
#281724=CARTESIAN_POINT('Ctrl Pts',(10.0514365206282,29.6562463505382,3.26590970098687));
#281725=CARTESIAN_POINT('Ctrl Pts',(10.0514365206282,29.8062463505376,-1.23094595618202E-15));
#281726=CARTESIAN_POINT('Ctrl Pts',(10.0514365206282,29.956246350537,-3.26590970098687));
#281727=CARTESIAN_POINT('Ctrl Pts',(8.13178296306921,30.1062463505364,-5.90808615117926));
#281728=CARTESIAN_POINT('Ctrl Pts',(6.21212940551021,30.2562463505358,-8.55026260137164));
#281729=CARTESIAN_POINT('Ctrl Pts',(3.10606470275509,30.4062463505352,-9.55948420107058));
#281730=CARTESIAN_POINT('Ctrl Pts',(-3.07222067144727E-14,30.5562463505346,
-10.5687058007695));
#281731=CARTESIAN_POINT('Ctrl Pts',(-3.10606470275515,30.706246350534,-9.55948420107058));
#281732=CARTESIAN_POINT('Ctrl Pts',(-6.21212940551027,30.8562463505334,
-8.55026260137164));
#281733=CARTESIAN_POINT('Ctrl Pts',(-8.13178296306928,31.0062463505328,
-5.90808615117925));
#281734=CARTESIAN_POINT('Ctrl Pts',(-10.0514365206283,31.1562463505322,
-3.26590970098687));
#281735=CARTESIAN_POINT('Ctrl Pts',(-10.0514365206283,31.3062463505316,
2.46189191236404E-15));
#281736=CARTESIAN_POINT('Ctrl Pts',(-10.0514365206283,31.456246350531,3.26590970098687));
#281737=CARTESIAN_POINT('Ctrl Pts',(-8.13178296306928,31.6062463505304,
5.90808615117926));
#281738=CARTESIAN_POINT('Ctrl Pts',(-6.21212940551027,31.7562463505298,
8.55026260137164));
#281739=CARTESIAN_POINT('Ctrl Pts',(-3.10606470275515,31.9062463505292,
9.55948420107058));
#281740=CARTESIAN_POINT('Ctrl Pts',(-2.89974750042951E-14,32.0562463505286,
10.5687058007695));
#281741=CARTESIAN_POINT('Ctrl Pts',(3.10606470275509,32.206246350528,9.55948420107058));
#281742=CARTESIAN_POINT('Ctrl Pts',(6.21212940551021,32.3562463505274,8.55026260137164));
#281743=CARTESIAN_POINT('Ctrl Pts',(8.13178296306921,32.5062463505268,5.90808615117925));
#281744=CARTESIAN_POINT('Ctrl Pts',(10.0514365206282,32.6562463505262,3.26590970098687));
#281745=CARTESIAN_POINT('Ctrl Pts',(10.0514365206282,32.8062463505256,-1.23094595618202E-15));
#281746=CARTESIAN_POINT('Ctrl Pts',(10.0514365206282,32.956246350525,-3.26590970098687));
#281747=CARTESIAN_POINT('Ctrl Pts',(8.13178296306921,33.1062463505244,-5.90808615117926));
#281748=CARTESIAN_POINT('Ctrl Pts',(6.21212940551021,33.2562463505238,-8.55026260137164));
#281749=CARTESIAN_POINT('Ctrl Pts',(3.10606470275509,33.4062463505232,-9.55948420107058));
#281750=CARTESIAN_POINT('Ctrl Pts',(-3.24499159861345E-14,33.5562463505226,
-10.5687058007695));
#281751=CARTESIAN_POINT('Ctrl Pts',(-3.10606470275515,33.706246350522,-9.55948420107058));
#281752=CARTESIAN_POINT('Ctrl Pts',(-6.21212940551027,33.8562463505214,
-8.55026260137164));
#281753=CARTESIAN_POINT('Ctrl Pts',(-8.13178296306928,34.0062463505208,
-5.90808615117925));
#281754=CARTESIAN_POINT('Ctrl Pts',(-10.0514365206283,34.1562463505202,
-3.26590970098687));
#281755=CARTESIAN_POINT('Ctrl Pts',(-10.0514365206283,34.3062463505196,
2.46189191236404E-15));
#281756=CARTESIAN_POINT('Ctrl Pts',(-10.0514365206283,34.456246350519,3.26590970098687));
#281757=CARTESIAN_POINT('Ctrl Pts',(-8.13178296306928,34.6062463505184,
5.90808615117926));
#281758=CARTESIAN_POINT('Ctrl Pts',(-6.21212940551027,34.7562463505178,
8.55026260137164));
#281759=CARTESIAN_POINT('Ctrl Pts',(-3.10606470275515,34.9062463505172,
9.55948420107058));
#281760=CARTESIAN_POINT('Ctrl Pts',(-3.0725184275957E-14,35.0562463505166,
10.5687058007695));
#281761=CARTESIAN_POINT('Ctrl Pts',(3.10606470275509,35.206246350516,9.55948420107058));
#281762=CARTESIAN_POINT('Ctrl Pts',(6.21212940551021,35.3562463505154,8.55026260137164));
#281763=CARTESIAN_POINT('Ctrl Pts',(8.13178296306921,35.5062463505148,5.90808615117925));
#281764=CARTESIAN_POINT('Ctrl Pts',(10.0514365206282,35.6562463505142,3.26590970098687));
#281765=CARTESIAN_POINT('Ctrl Pts',(10.0514365206282,35.8062463505136,-1.23094595618202E-15));
#281766=CARTESIAN_POINT('Ctrl Pts',(10.0514365206282,35.956246350513,-3.26590970098687));
#281767=CARTESIAN_POINT('Ctrl Pts',(8.13178296306921,36.1062463505124,-5.90808615117926));
#281768=CARTESIAN_POINT('Ctrl Pts',(6.21212940551021,36.2562463505118,-8.55026260137164));
#281769=CARTESIAN_POINT('Ctrl Pts',(3.10606470275509,36.4062463505112,-9.55948420107058));
#281770=CARTESIAN_POINT('Ctrl Pts',(-3.41776252577964E-14,36.5562463505106,
-10.5687058007695));
#281771=CARTESIAN_POINT('Ctrl Pts',(-3.10606470275516,36.70624635051,-9.55948420107058));
#281772=CARTESIAN_POINT('Ctrl Pts',(-6.21212940551028,36.8562463505094,
-8.55026260137164));
#281773=CARTESIAN_POINT('Ctrl Pts',(-8.13178296306928,37.0062463505088,
-5.90808615117925));
#281774=CARTESIAN_POINT('Ctrl Pts',(-10.0514365206283,37.1562463505082,
-3.26590970098687));
#281775=CARTESIAN_POINT('Ctrl Pts',(-10.0514365206283,37.3062463505076,
2.46189191236404E-15));
#281776=CARTESIAN_POINT('Ctrl Pts',(-10.0514365206283,37.456246350507,3.26590970098687));
#281777=CARTESIAN_POINT('Ctrl Pts',(-8.13178296306928,37.6062463505064,
5.90808615117926));
#281778=CARTESIAN_POINT('Ctrl Pts',(-6.21212940551027,37.7562463505058,
8.55026260137164));
#281779=CARTESIAN_POINT('Ctrl Pts',(-3.10606470275515,37.9062463505052,
9.55948420107058));
#281780=CARTESIAN_POINT('Ctrl Pts',(-3.24528935476188E-14,38.0562463505046,
10.5687058007695));
#281781=CARTESIAN_POINT('Ctrl Pts',(3.10606470275509,38.206246350504,9.55948420107058));
#281782=CARTESIAN_POINT('Ctrl Pts',(6.21212940551021,38.3562463505034,8.55026260137164));
#281783=CARTESIAN_POINT('Ctrl Pts',(8.13178296306921,38.5062463505028,5.90808615117925));
#281784=CARTESIAN_POINT('Ctrl Pts',(10.0514365206282,38.6562463505022,3.26590970098687));
#281785=CARTESIAN_POINT('Ctrl Pts',(10.0514365206282,38.8062463505016,-1.23094595618202E-15));
#281786=CARTESIAN_POINT('Ctrl Pts',(10.0514365206282,38.956246350501,-3.26590970098687));
#281787=CARTESIAN_POINT('Ctrl Pts',(8.13178296306921,39.1062463505004,-5.90808615117926));
#281788=CARTESIAN_POINT('Ctrl Pts',(6.2121294055102,39.2562463504998,-8.55026260137164));
#281789=CARTESIAN_POINT('Ctrl Pts',(3.10606470275508,39.4062463504992,-9.55948420107058));
#281790=CARTESIAN_POINT('Ctrl Pts',(-3.59053345294582E-14,39.5562463504986,
-10.5687058007695));
#281791=CARTESIAN_POINT('Ctrl Pts',(-3.10606470275516,39.706246350498,-9.55948420107058));
#281792=CARTESIAN_POINT('Ctrl Pts',(-6.21212940551028,39.8562463504974,
-8.55026260137164));
#281793=CARTESIAN_POINT('Ctrl Pts',(-8.13178296306928,40.0062463504968,
-5.90808615117925));
#281794=CARTESIAN_POINT('Ctrl Pts',(-10.0514365206283,40.1562463504962,
-3.26590970098687));
#281795=CARTESIAN_POINT('Ctrl Pts',(-10.0514365206283,40.3062463504956,
2.46189191236404E-15));
#281796=CARTESIAN_POINT('Ctrl Pts',(-10.0514365206283,40.456246350495,3.26590970098687));
#281797=CARTESIAN_POINT('Ctrl Pts',(-8.13178296306928,40.6062463504944,
5.90808615117926));
#281798=CARTESIAN_POINT('Ctrl Pts',(-6.21212940551028,40.7562463504938,
8.55026260137164));
#281799=CARTESIAN_POINT('Ctrl Pts',(-3.10606470275516,40.9062463504932,
9.55948420107058));
#281800=CARTESIAN_POINT('Ctrl Pts',(-3.41806028192807E-14,41.0562463504926,
10.5687058007695));
#281801=CARTESIAN_POINT('Ctrl Pts',(3.10606470275509,41.206246350492,9.55948420107058));
#281802=CARTESIAN_POINT('Ctrl Pts',(6.21212940551021,41.3562463504914,8.55026260137164));
#281803=CARTESIAN_POINT('Ctrl Pts',(8.13178296306921,41.5062463504908,5.90808615117925));
#281804=CARTESIAN_POINT('Ctrl Pts',(10.0514365206282,41.6562463504902,3.26590970098687));
#281805=CARTESIAN_POINT('Ctrl Pts',(10.0514365206282,41.8062463504896,-1.23094595618202E-15));
#281806=CARTESIAN_POINT('Ctrl Pts',(10.0514365206282,41.956246350489,-3.26590970098687));
#281807=CARTESIAN_POINT('Ctrl Pts',(8.13178296306921,42.1062463504884,-5.90808615117926));
#281808=CARTESIAN_POINT('Ctrl Pts',(6.2121294055102,42.2562463504878,-8.55026260137164));
#281809=CARTESIAN_POINT('Ctrl Pts',(3.10606470275508,42.4062463504872,-9.55948420107058));
#281810=CARTESIAN_POINT('Ctrl Pts',(-3.76330438011201E-14,42.5562463504866,
-10.5687058007695));
#281811=CARTESIAN_POINT('Ctrl Pts',(-3.10606470275516,42.706246350486,-9.55948420107058));
#281812=CARTESIAN_POINT('Ctrl Pts',(-6.21212940551028,42.8562463504854,
-8.55026260137164));
#281813=CARTESIAN_POINT('Ctrl Pts',(-8.13178296306928,43.0062463504848,
-5.90808615117925));
#281814=CARTESIAN_POINT('Ctrl Pts',(-10.0514365206283,43.1562463504842,
-3.26590970098687));
#281815=CARTESIAN_POINT('Ctrl Pts',(-10.0514365206283,43.3062463504836,
2.46189191236404E-15));
#281816=CARTESIAN_POINT('Ctrl Pts',(-10.0514365206283,43.456246350483,3.26590970098687));
#281817=CARTESIAN_POINT('Ctrl Pts',(-8.13178296306928,43.6062463504824,
5.90808615117926));
#281818=CARTESIAN_POINT('Ctrl Pts',(-6.21212940551028,43.7562463504818,
8.55026260137164));
#281819=CARTESIAN_POINT('Ctrl Pts',(-3.10606470275516,43.9062463504812,
9.55948420107058));
#281820=CARTESIAN_POINT('Ctrl Pts',(-3.59083120909425E-14,44.0562463504806,
10.5687058007695));
#281821=CARTESIAN_POINT('Ctrl Pts',(3.10606470275508,44.20624635048,9.55948420107058));
#281822=CARTESIAN_POINT('Ctrl Pts',(6.2121294055102,44.3562463504794,8.55026260137164));
#281823=CARTESIAN_POINT('Ctrl Pts',(8.13178296306921,44.5062463504788,5.90808615117925));
#281824=CARTESIAN_POINT('Ctrl Pts',(10.0514365206282,44.6562463504782,3.26590970098687));
#281825=CARTESIAN_POINT('Ctrl Pts',(10.0514365206282,44.8062463504776,-1.23094595618202E-15));
#281826=CARTESIAN_POINT('Ctrl Pts',(10.0514365206282,44.956246350477,-3.26590970098687));
#281827=CARTESIAN_POINT('Ctrl Pts',(8.13178296306921,45.1062463504764,-5.90808615117926));
#281828=CARTESIAN_POINT('Ctrl Pts',(6.2121294055102,45.2562463504758,-8.55026260137164));
#281829=CARTESIAN_POINT('Ctrl Pts',(3.10606470275508,45.4062463504752,-9.55948420107058));
#281830=CARTESIAN_POINT('Ctrl Pts',(-3.93607530727819E-14,45.5562463504746,
-10.5687058007695));
#281831=CARTESIAN_POINT('Ctrl Pts',(-3.10606470275516,45.706246350474,-9.55948420107058));
#281832=CARTESIAN_POINT('Ctrl Pts',(-6.21212940551028,45.8562463504734,
-8.55026260137164));
#281833=CARTESIAN_POINT('Ctrl Pts',(-8.13178296306928,46.0062463504728,
-5.90808615117925));
#281834=CARTESIAN_POINT('Ctrl Pts',(-10.0514365206283,46.1562463504722,
-3.26590970098687));
#281835=CARTESIAN_POINT('Ctrl Pts',(-10.0514365206283,46.3062463504716,
2.46189191236404E-15));
#281836=CARTESIAN_POINT('Ctrl Pts',(-10.0514365206283,46.456246350471,3.26590970098687));
#281837=CARTESIAN_POINT('Ctrl Pts',(-8.13178296306928,46.6062463504704,
5.90808615117926));
#281838=CARTESIAN_POINT('Ctrl Pts',(-6.21212940551028,46.7562463504698,
8.55026260137164));
#281839=CARTESIAN_POINT('Ctrl Pts',(-3.10606470275516,46.9062463504692,
9.55948420107058));
#281840=CARTESIAN_POINT('Ctrl Pts',(-3.76360213626043E-14,47.0562463504686,
10.5687058007695));
#281841=CARTESIAN_POINT('Ctrl Pts',(3.10606470275508,47.206246350468,9.55948420107058));
#281842=CARTESIAN_POINT('Ctrl Pts',(6.2121294055102,47.3562463504674,8.55026260137164));
#281843=CARTESIAN_POINT('Ctrl Pts',(8.13178296306921,47.5062463504668,5.90808615117925));
#281844=CARTESIAN_POINT('Ctrl Pts',(10.0514365206282,47.6562463504662,3.26590970098687));
#281845=CARTESIAN_POINT('Ctrl Pts',(10.0514365206282,47.8062463504656,-1.23094595618202E-15));
#281846=CARTESIAN_POINT('Ctrl Pts',(10.0514365206282,47.956246350465,-3.26590970098687));
#281847=CARTESIAN_POINT('Ctrl Pts',(8.1317829630692,48.1062463504644,-5.90808615117926));
#281848=CARTESIAN_POINT('Ctrl Pts',(6.2121294055102,48.2562463504638,-8.55026260137164));
#281849=CARTESIAN_POINT('Ctrl Pts',(3.10606470275508,48.4062463504632,-9.55948420107058));
#281850=CARTESIAN_POINT('Ctrl Pts',(-4.10884623444438E-14,48.5562463504626,
-10.5687058007695));
#281851=CARTESIAN_POINT('Ctrl Pts',(-3.10606470275516,48.706246350462,-9.55948420107058));
#281852=CARTESIAN_POINT('Ctrl Pts',(-6.21212940551028,48.8562463504614,
-8.55026260137164));
#281853=CARTESIAN_POINT('Ctrl Pts',(-8.13178296306929,49.0062463504608,
-5.90808615117925));
#281854=CARTESIAN_POINT('Ctrl Pts',(-10.0514365206283,49.1562463504602,
-3.26590970098687));
#281855=CARTESIAN_POINT('Ctrl Pts',(-10.0514365206283,49.3062463504596,
2.46189191236404E-15));
#281856=CARTESIAN_POINT('Ctrl Pts',(-10.0514365206283,49.456246350459,3.26590970098687));
#281857=CARTESIAN_POINT('Ctrl Pts',(-8.13178296306929,49.6062463504584,
5.90808615117926));
#281858=CARTESIAN_POINT('Ctrl Pts',(-6.21212940551028,49.7562463504578,
8.55026260137164));
#281859=CARTESIAN_POINT('Ctrl Pts',(-3.10606470275516,49.9062463504572,
9.55948420107058));
#281860=CARTESIAN_POINT('Ctrl Pts',(-3.93637306342662E-14,50.0562463504566,
10.5687058007695));
#281861=CARTESIAN_POINT('Ctrl Pts',(3.10606470275508,50.206246350456,9.55948420107058));
#281862=CARTESIAN_POINT('Ctrl Pts',(6.2121294055102,50.3562463504554,8.55026260137164));
#281863=CARTESIAN_POINT('Ctrl Pts',(8.1317829630692,50.5062463504548,5.90808615117925));
#281864=CARTESIAN_POINT('Ctrl Pts',(10.0514365206282,50.6562463504542,3.26590970098687));
#281865=CARTESIAN_POINT('Ctrl Pts',(10.0514365206282,50.8062463504536,-1.23094595618202E-15));
#281866=CARTESIAN_POINT('Ctrl Pts',(10.0514365206282,50.956246350453,-3.26590970098687));
#281867=CARTESIAN_POINT('Ctrl Pts',(8.1317829630692,51.1062463504524,-5.90808615117926));
#281868=CARTESIAN_POINT('Ctrl Pts',(6.2121294055102,51.2562463504518,-8.55026260137164));
#281869=CARTESIAN_POINT('Ctrl Pts',(3.10606470275508,51.4062463504512,-9.55948420107058));
#281870=CARTESIAN_POINT('Ctrl Pts',(-4.28161716161056E-14,51.5562463504506,
-10.5687058007695));
#281871=CARTESIAN_POINT('Ctrl Pts',(-3.10606470275516,51.70624635045,-9.55948420107058));
#281872=CARTESIAN_POINT('Ctrl Pts',(-6.21212940551029,51.8562463504494,
-8.55026260137164));
#281873=CARTESIAN_POINT('Ctrl Pts',(-8.13178296306929,52.0062463504488,
-5.90808615117925));
#281874=CARTESIAN_POINT('Ctrl Pts',(-10.0514365206283,52.1562463504482,
-3.26590970098687));
#281875=CARTESIAN_POINT('Ctrl Pts',(-10.0514365206283,52.3062463504476,
2.46189191236404E-15));
#281876=CARTESIAN_POINT('Ctrl Pts',(-10.0514365206283,52.456246350447,3.26590970098687));
#281877=CARTESIAN_POINT('Ctrl Pts',(-8.13178296306929,52.6062463504464,
5.90808615117926));
#281878=CARTESIAN_POINT('Ctrl Pts',(-6.21212940551028,52.7562463504458,
8.55026260137164));
#281879=CARTESIAN_POINT('Ctrl Pts',(-3.10606470275516,52.9062463504452,
9.55948420107058));
#281880=CARTESIAN_POINT('Ctrl Pts',(-4.1091439905928E-14,53.0562463504446,
10.5687058007695));
#281881=CARTESIAN_POINT('Ctrl Pts',(3.10606470275508,53.206246350444,9.55948420107058));
#281882=CARTESIAN_POINT('Ctrl Pts',(6.2121294055102,53.3562463504434,8.55026260137164));
#281883=CARTESIAN_POINT('Ctrl Pts',(8.1317829630692,53.5062463504428,5.90808615117925));
#281884=CARTESIAN_POINT('Ctrl Pts',(10.0514365206282,53.6562463504422,3.26590970098687));
#281885=CARTESIAN_POINT('Ctrl Pts',(10.0514365206282,53.8062463504416,-1.23094595618202E-15));
#281886=CARTESIAN_POINT('Ctrl Pts',(10.0514365206282,53.956246350441,-3.26590970098687));
#281887=CARTESIAN_POINT('Ctrl Pts',(8.1317829630692,54.1062463504404,-5.90808615117926));
#281888=CARTESIAN_POINT('Ctrl Pts',(6.2121294055102,54.2562463504398,-8.55026260137164));
#281889=CARTESIAN_POINT('Ctrl Pts',(3.10606470275508,54.4062463504392,-9.55948420107058));
#281890=CARTESIAN_POINT('Ctrl Pts',(-4.45438808877674E-14,54.5562463504386,
-10.5687058007695));
#281891=CARTESIAN_POINT('Ctrl Pts',(-3.10606470275517,54.706246350438,-9.55948420107058));
#281892=CARTESIAN_POINT('Ctrl Pts',(-6.21212940551029,54.8562463504374,
-8.55026260137164));
#281893=CARTESIAN_POINT('Ctrl Pts',(-8.13178296306929,55.0062463504368,
-5.90808615117925));
#281894=CARTESIAN_POINT('Ctrl Pts',(-10.0514365206283,55.1562463504362,
-3.26590970098687));
#281895=CARTESIAN_POINT('Ctrl Pts',(-10.0514365206283,55.3062463504356,
2.46189191236404E-15));
#281896=CARTESIAN_POINT('Ctrl Pts',(-10.0514365206283,55.456246350435,3.26590970098687));
#281897=CARTESIAN_POINT('Ctrl Pts',(-8.13178296306929,55.6062463504344,
5.90808615117926));
#281898=CARTESIAN_POINT('Ctrl Pts',(-6.21212940551028,55.7562463504338,
8.55026260137164));
#281899=CARTESIAN_POINT('Ctrl Pts',(-3.10606470275516,55.9062463504332,
9.55948420107058));
#281900=CARTESIAN_POINT('Ctrl Pts',(-4.28191491775899E-14,56.0562463504326,
10.5687058007695));
#281901=CARTESIAN_POINT('Ctrl Pts',(3.10606470275508,56.206246350432,9.55948420107058));
#281902=CARTESIAN_POINT('Ctrl Pts',(6.2121294055102,56.3562463504314,8.55026260137164));
#281903=CARTESIAN_POINT('Ctrl Pts',(8.1317829630692,56.5062463504308,5.90808615117925));
#281904=CARTESIAN_POINT('Ctrl Pts',(10.0514365206282,56.6562463504302,3.26590970098687));
#281905=CARTESIAN_POINT('Ctrl Pts',(10.0514365206282,56.8062463504296,-1.23094595618202E-15));
#281906=CARTESIAN_POINT('Ctrl Pts',(10.0514365206282,56.956246350429,-3.26590970098687));
#281907=CARTESIAN_POINT('Ctrl Pts',(8.1317829630692,57.1062463504284,-5.90808615117926));
#281908=CARTESIAN_POINT('Ctrl Pts',(6.2121294055102,57.2562463504278,-8.55026260137164));
#281909=CARTESIAN_POINT('Ctrl Pts',(3.10606470275507,57.4062463504272,-9.55948420107058));
#281910=CARTESIAN_POINT('Ctrl Pts',(-4.62715901594293E-14,57.5562463504266,
-10.5687058007695));
#281911=CARTESIAN_POINT('Ctrl Pts',(-3.10606470275517,57.706246350426,-9.55948420107058));
#281912=CARTESIAN_POINT('Ctrl Pts',(-6.21212940551029,57.8562463504254,
-8.55026260137164));
#281913=CARTESIAN_POINT('Ctrl Pts',(-8.13178296306929,58.0062463504248,
-5.90808615117925));
#281914=CARTESIAN_POINT('Ctrl Pts',(-10.0514365206283,58.1562463504242,
-3.26590970098687));
#281915=CARTESIAN_POINT('Ctrl Pts',(-10.0514365206283,58.3062463504236,
2.46189191236404E-15));
#281916=CARTESIAN_POINT('Ctrl Pts',(-10.0514365206283,58.456246350423,3.26590970098687));
#281917=CARTESIAN_POINT('Ctrl Pts',(-8.13178296306929,58.6062463504224,
5.90808615117926));
#281918=CARTESIAN_POINT('Ctrl Pts',(-6.21212940551029,58.7562463504218,
8.55026260137164));
#281919=CARTESIAN_POINT('Ctrl Pts',(-3.10606470275517,58.9062463504212,
9.55948420107058));
#281920=CARTESIAN_POINT('Ctrl Pts',(-4.45468584492517E-14,59.0562463504206,
10.5687058007695));
#281921=CARTESIAN_POINT('Ctrl Pts',(3.10606470275508,59.20624635042,9.55948420107058));
#281922=CARTESIAN_POINT('Ctrl Pts',(6.2121294055102,59.3562463504194,8.55026260137164));
#281923=CARTESIAN_POINT('Ctrl Pts',(8.1317829630692,59.5062463504188,5.90808615117925));
#281924=CARTESIAN_POINT('Ctrl Pts',(10.0514365206282,59.6562463504182,3.26590970098687));
#281925=CARTESIAN_POINT('Ctrl Pts',(10.0514365206282,59.8062463504176,-1.23094595618202E-15));
#281926=CARTESIAN_POINT('Ctrl Pts',(10.0514365206282,59.956246350417,-3.26590970098687));
#281927=CARTESIAN_POINT('Ctrl Pts',(8.1317829630692,60.1062463504164,-5.90808615117926));
#281928=CARTESIAN_POINT('Ctrl Pts',(6.2121294055102,60.2562463504158,-8.55026260137164));
#281929=CARTESIAN_POINT('Ctrl Pts',(3.10606470275507,60.4062463504152,-9.55948420107058));
#281930=CARTESIAN_POINT('Ctrl Pts',(-4.79992994310911E-14,60.5562463504146,
-10.5687058007695));
#281931=CARTESIAN_POINT('Ctrl Pts',(-3.10606470275517,60.706246350414,-9.55948420107058));
#281932=CARTESIAN_POINT('Ctrl Pts',(-6.21212940551029,60.8562463504134,
-8.55026260137164));
#281933=CARTESIAN_POINT('Ctrl Pts',(-8.13178296306929,61.0062463504128,
-5.90808615117925));
#281934=CARTESIAN_POINT('Ctrl Pts',(-10.0514365206283,61.1562463504122,
-3.26590970098687));
#281935=CARTESIAN_POINT('Ctrl Pts',(-10.0514365206283,61.3062463504116,
2.46189191236404E-15));
#281936=CARTESIAN_POINT('Ctrl Pts',(-10.0514365206283,61.456246350411,3.26590970098687));
#281937=CARTESIAN_POINT('Ctrl Pts',(-8.13178296306929,61.6062463504104,
5.90808615117926));
#281938=CARTESIAN_POINT('Ctrl Pts',(-6.21212940551029,61.7562463504098,
8.55026260137164));
#281939=CARTESIAN_POINT('Ctrl Pts',(-3.10606470275517,61.9062463504092,
9.55948420107058));
#281940=CARTESIAN_POINT('Ctrl Pts',(-4.62745677209135E-14,62.0562463504086,
10.5687058007695));
#281941=CARTESIAN_POINT('Ctrl Pts',(3.10606470275507,62.206246350408,9.55948420107058));
#281942=CARTESIAN_POINT('Ctrl Pts',(6.2121294055102,62.3562463504074,8.55026260137164));
#281943=CARTESIAN_POINT('Ctrl Pts',(8.1317829630692,62.5062463504068,5.90808615117925));
#281944=CARTESIAN_POINT('Ctrl Pts',(10.0514365206282,62.6562463504062,3.26590970098687));
#281945=CARTESIAN_POINT('Ctrl Pts',(10.0514365206282,62.8062463504056,-1.23094595618202E-15));
#281946=CARTESIAN_POINT('Ctrl Pts',(10.0514365206282,62.956246350405,-3.26590970098687));
#281947=CARTESIAN_POINT('Ctrl Pts',(8.1317829630692,63.1062463504044,-5.90808615117926));
#281948=CARTESIAN_POINT('Ctrl Pts',(6.21212940551019,63.2562463504038,-8.55026260137164));
#281949=CARTESIAN_POINT('Ctrl Pts',(3.10606470275507,63.4062463504032,-9.55948420107058));
#281950=CARTESIAN_POINT('Ctrl Pts',(-4.9727008702753E-14,63.5562463504026,
-10.5687058007695));
#281951=CARTESIAN_POINT('Ctrl Pts',(-3.10606470275517,63.706246350402,-9.55948420107058));
#281952=CARTESIAN_POINT('Ctrl Pts',(-6.21212940551029,63.8562463504014,
-8.55026260137164));
#281953=CARTESIAN_POINT('Ctrl Pts',(-8.1317829630693,64.0062463504008,-5.90808615117925));
#281954=CARTESIAN_POINT('Ctrl Pts',(-10.0514365206283,64.1562463504002,
-3.26590970098687));
#281955=CARTESIAN_POINT('Ctrl Pts',(-10.0514365206283,64.3062463503996,
2.46189191236404E-15));
#281956=CARTESIAN_POINT('Ctrl Pts',(-10.0514365206283,64.456246350399,3.26590970098687));
#281957=CARTESIAN_POINT('Ctrl Pts',(-8.1317829630693,64.6062463503984,5.90808615117926));
#281958=CARTESIAN_POINT('Ctrl Pts',(-6.21212940551029,64.7562463503978,
8.55026260137164));
#281959=CARTESIAN_POINT('Ctrl Pts',(-3.10606470275517,64.9062463503972,
9.55948420107058));
#281960=CARTESIAN_POINT('Ctrl Pts',(-4.80022769925754E-14,65.0562463503966,
10.5687058007695));
#281961=CARTESIAN_POINT('Ctrl Pts',(3.10606470275507,65.206246350396,9.55948420107058));
#281962=CARTESIAN_POINT('Ctrl Pts',(6.21212940551019,65.3562463503954,8.55026260137164));
#281963=CARTESIAN_POINT('Ctrl Pts',(8.1317829630692,65.5062463503948,5.90808615117925));
#281964=CARTESIAN_POINT('Ctrl Pts',(10.0514365206282,65.6562463503942,3.26590970098687));
#281965=CARTESIAN_POINT('Ctrl Pts',(10.0514365206282,65.8062463503936,-1.23094595618202E-15));
#281966=CARTESIAN_POINT('Ctrl Pts',(10.0514365206282,65.956246350393,-3.26590970098687));
#281967=CARTESIAN_POINT('Ctrl Pts',(8.13178296306919,66.1062463503924,-5.90808615117926));
#281968=CARTESIAN_POINT('Ctrl Pts',(6.21212940551019,66.2562463503918,-8.55026260137164));
#281969=CARTESIAN_POINT('Ctrl Pts',(3.10606470275507,66.4062463503912,-9.55948420107058));
#281970=CARTESIAN_POINT('Ctrl Pts',(-5.14547179744148E-14,66.5562463503906,
-10.5687058007695));
#281971=CARTESIAN_POINT('Ctrl Pts',(-3.10606470275517,66.70624635039,-9.55948420107058));
#281972=CARTESIAN_POINT('Ctrl Pts',(-6.21212940551029,66.8562463503894,
-8.55026260137164));
#281973=CARTESIAN_POINT('Ctrl Pts',(-8.1317829630693,67.0062463503888,-5.90808615117925));
#281974=CARTESIAN_POINT('Ctrl Pts',(-10.0514365206283,67.1562463503882,
-3.26590970098687));
#281975=CARTESIAN_POINT('Ctrl Pts',(-10.0514365206283,67.3062463503876,
2.46189191236404E-15));
#281976=CARTESIAN_POINT('Ctrl Pts',(-10.0514365206283,67.456246350387,3.26590970098687));
#281977=CARTESIAN_POINT('Ctrl Pts',(-8.1317829630693,67.6062463503864,5.90808615117926));
#281978=CARTESIAN_POINT('Ctrl Pts',(-6.21212940551029,67.7562463503858,
8.55026260137164));
#281979=CARTESIAN_POINT('Ctrl Pts',(-3.10606470275517,67.9062463503852,
9.55948420107058));
#281980=CARTESIAN_POINT('Ctrl Pts',(-4.97299862642372E-14,68.0562463503846,
10.5687058007695));
#281981=CARTESIAN_POINT('Ctrl Pts',(3.10606470275507,68.206246350384,9.55948420107058));
#281982=CARTESIAN_POINT('Ctrl Pts',(6.21212940551019,68.3562463503834,8.55026260137164));
#281983=CARTESIAN_POINT('Ctrl Pts',(8.13178296306919,68.5062463503828,5.90808615117925));
#281984=CARTESIAN_POINT('Ctrl Pts',(10.0514365206282,68.6562463503822,3.26590970098687));
#281985=CARTESIAN_POINT('Ctrl Pts',(10.0514365206282,68.8062463503816,-1.23094595618202E-15));
#281986=CARTESIAN_POINT('Ctrl Pts',(10.0514365206282,68.956246350381,-3.26590970098687));
#281987=CARTESIAN_POINT('Ctrl Pts',(8.13178296306919,69.1062463503804,-5.90808615117926));
#281988=CARTESIAN_POINT('Ctrl Pts',(6.21212940551019,69.2562463503798,-8.55026260137164));
#281989=CARTESIAN_POINT('Ctrl Pts',(3.10606470275507,69.4062463503792,-9.55948420107058));
#281990=CARTESIAN_POINT('Ctrl Pts',(-5.31824272460766E-14,69.5562463503786,
-10.5687058007695));
#281991=CARTESIAN_POINT('Ctrl Pts',(-3.10606470275517,69.706246350378,-9.55948420107058));
#281992=CARTESIAN_POINT('Ctrl Pts',(-6.21212940551029,69.8562463503774,
-8.55026260137164));
#281993=CARTESIAN_POINT('Ctrl Pts',(-8.1317829630693,70.0062463503768,-5.90808615117925));
#281994=CARTESIAN_POINT('Ctrl Pts',(-10.0514365206283,70.1562463503762,
-3.26590970098687));
#281995=CARTESIAN_POINT('Ctrl Pts',(-10.0514365206283,70.3062463503756,
2.46189191236404E-15));
#281996=CARTESIAN_POINT('Ctrl Pts',(-10.0514365206283,70.456246350375,3.26590970098687));
#281997=CARTESIAN_POINT('Ctrl Pts',(-8.1317829630693,70.6062463503744,5.90808615117926));
#281998=CARTESIAN_POINT('Ctrl Pts',(-6.21212940551029,70.7562463503738,
8.55026260137164));
#281999=CARTESIAN_POINT('Ctrl Pts',(-3.10606470275517,70.9062463503732,
9.55948420107058));
#282000=CARTESIAN_POINT('Ctrl Pts',(-5.1457695535899E-14,71.0562463503726,
10.5687058007695));
#282001=CARTESIAN_POINT('Ctrl Pts',(3.10606470275507,71.206246350372,9.55948420107058));
#282002=CARTESIAN_POINT('Ctrl Pts',(6.21212940551019,71.3562463503714,8.55026260137164));
#282003=CARTESIAN_POINT('Ctrl Pts',(8.13178296306919,71.5062463503708,5.90808615117925));
#282004=CARTESIAN_POINT('Ctrl Pts',(10.0514365206282,71.6562463503702,3.26590970098687));
#282005=CARTESIAN_POINT('Ctrl Pts',(10.0514365206282,71.8062463503696,-1.23094595618202E-15));
#282006=CARTESIAN_POINT('Ctrl Pts',(10.0514365206282,71.956246350369,-3.26590970098687));
#282007=CARTESIAN_POINT('Ctrl Pts',(8.13178296306919,72.1062463503684,-5.90808615117926));
#282008=CARTESIAN_POINT('Ctrl Pts',(6.21212940551019,72.2562463503678,-8.55026260137164));
#282009=CARTESIAN_POINT('Ctrl Pts',(3.10606470275507,72.4062463503672,-9.55948420107058));
#282010=CARTESIAN_POINT('Ctrl Pts',(-5.49101365177385E-14,72.5562463503666,
-10.5687058007695));
#282011=CARTESIAN_POINT('Ctrl Pts',(-3.10606470275518,72.706246350366,-9.55948420107058));
#282012=CARTESIAN_POINT('Ctrl Pts',(-6.2121294055103,72.8562463503654,-8.55026260137164));
#282013=CARTESIAN_POINT('Ctrl Pts',(-8.1317829630693,73.0062463503648,-5.90808615117925));
#282014=CARTESIAN_POINT('Ctrl Pts',(-10.0514365206283,73.1562463503642,
-3.26590970098687));
#282015=CARTESIAN_POINT('Ctrl Pts',(-10.0514365206283,73.3062463503636,
2.46189191236404E-15));
#282016=CARTESIAN_POINT('Ctrl Pts',(-10.0514365206283,73.456246350363,3.26590970098687));
#282017=CARTESIAN_POINT('Ctrl Pts',(-8.1317829630693,73.6062463503624,5.90808615117926));
#282018=CARTESIAN_POINT('Ctrl Pts',(-6.21212940551029,73.7562463503618,
8.55026260137164));
#282019=CARTESIAN_POINT('Ctrl Pts',(-3.10606470275517,73.9062463503612,
9.55948420107058));
#282020=CARTESIAN_POINT('Ctrl Pts',(-5.31854048075609E-14,74.0562463503606,
10.5687058007695));
#282021=CARTESIAN_POINT('Ctrl Pts',(3.10606470275507,74.20624635036,9.55948420107058));
#282022=CARTESIAN_POINT('Ctrl Pts',(6.21212940551019,74.3562463503594,8.55026260137164));
#282023=CARTESIAN_POINT('Ctrl Pts',(8.13178296306919,74.5062463503588,5.90808615117925));
#282024=CARTESIAN_POINT('Ctrl Pts',(10.0514365206282,74.6562463503582,3.26590970098687));
#282025=CARTESIAN_POINT('Ctrl Pts',(10.0514365206282,74.8062463503576,-1.23094595618202E-15));
#282026=CARTESIAN_POINT('Ctrl Pts',(10.0514365206282,74.956246350357,-3.26590970098687));
#282027=CARTESIAN_POINT('Ctrl Pts',(8.13178296306919,75.1062463503564,-5.90808615117926));
#282028=CARTESIAN_POINT('Ctrl Pts',(6.21212940551018,75.2562463503558,-8.55026260137164));
#282029=CARTESIAN_POINT('Ctrl Pts',(3.10606470275506,75.4062463503552,-9.55948420107058));
#282030=CARTESIAN_POINT('Ctrl Pts',(-5.66378457894003E-14,75.5562463503546,
-10.5687058007695));
#282031=CARTESIAN_POINT('Ctrl Pts',(-3.10606470275518,75.706246350354,-9.55948420107058));
#282032=CARTESIAN_POINT('Ctrl Pts',(-6.2121294055103,75.8562463503534,-8.55026260137164));
#282033=CARTESIAN_POINT('Ctrl Pts',(-8.1317829630693,76.0062463503528,-5.90808615117925));
#282034=CARTESIAN_POINT('Ctrl Pts',(-10.0514365206283,76.1562463503522,
-3.26590970098687));
#282035=CARTESIAN_POINT('Ctrl Pts',(-10.0514365206283,76.3062463503516,
2.46189191236404E-15));
#282036=CARTESIAN_POINT('Ctrl Pts',(-10.0514365206283,76.456246350351,3.26590970098687));
#282037=CARTESIAN_POINT('Ctrl Pts',(-8.1317829630693,76.6062463503504,5.90808615117926));
#282038=CARTESIAN_POINT('Ctrl Pts',(-6.21212940551029,76.7562463503498,
8.55026260137164));
#282039=CARTESIAN_POINT('Ctrl Pts',(-3.10606470275518,76.9062463503492,
9.55948420107058));
#282040=CARTESIAN_POINT('Ctrl Pts',(-5.49131140792227E-14,77.0562463503486,
10.5687058007695));
#282041=CARTESIAN_POINT('Ctrl Pts',(3.10606470275506,77.206246350348,9.55948420107058));
#282042=CARTESIAN_POINT('Ctrl Pts',(6.21212940551019,77.3562463503474,8.55026260137164));
#282043=CARTESIAN_POINT('Ctrl Pts',(8.13178296306919,77.5062463503468,5.90808615117925));
#282044=CARTESIAN_POINT('Ctrl Pts',(10.0514365206282,77.6562463503462,3.26590970098687));
#282045=CARTESIAN_POINT('Ctrl Pts',(10.0514365206282,77.8062463503456,-1.23094595618202E-15));
#282046=CARTESIAN_POINT('Ctrl Pts',(10.0514365206282,77.956246350345,-3.26590970098687));
#282047=CARTESIAN_POINT('Ctrl Pts',(8.13178296306919,78.1062463503444,-5.90808615117926));
#282048=CARTESIAN_POINT('Ctrl Pts',(6.21212940551018,78.2562463503438,-8.55026260137164));
#282049=CARTESIAN_POINT('Ctrl Pts',(3.10606470275506,78.4062463503432,-9.55948420107058));
#282050=CARTESIAN_POINT('Ctrl Pts',(-5.83655550610621E-14,78.5562463503426,
-10.5687058007695));
#282051=CARTESIAN_POINT('Ctrl Pts',(-3.10606470275518,78.706246350342,-9.55948420107058));
#282052=CARTESIAN_POINT('Ctrl Pts',(-6.2121294055103,78.8562463503414,-8.55026260137164));
#282053=CARTESIAN_POINT('Ctrl Pts',(-8.13178296306931,79.0062463503408,
-5.90808615117925));
#282054=CARTESIAN_POINT('Ctrl Pts',(-10.0514365206283,79.1562463503402,
-3.26590970098687));
#282055=CARTESIAN_POINT('Ctrl Pts',(-10.0514365206283,79.3062463503396,
2.46189191236404E-15));
#282056=CARTESIAN_POINT('Ctrl Pts',(-10.0514365206283,79.456246350339,3.26590970098687));
#282057=CARTESIAN_POINT('Ctrl Pts',(-8.13178296306931,79.6062463503384,
5.90808615117926));
#282058=CARTESIAN_POINT('Ctrl Pts',(-6.2121294055103,79.7562463503378,8.55026260137164));
#282059=CARTESIAN_POINT('Ctrl Pts',(-3.10606470275518,79.9062463503372,
9.55948420107058));
#282060=CARTESIAN_POINT('Ctrl Pts',(-5.66408233508846E-14,80.0562463503366,
10.5687058007695));
#282061=CARTESIAN_POINT('Ctrl Pts',(3.10606470275506,80.206246350336,9.55948420107058));
#282062=CARTESIAN_POINT('Ctrl Pts',(6.21212940551018,80.3562463503354,8.55026260137164));
#282063=CARTESIAN_POINT('Ctrl Pts',(8.13178296306919,80.5062463503348,5.90808615117925));
#282064=CARTESIAN_POINT('Ctrl Pts',(10.0514365206282,80.6562463503342,3.26590970098687));
#282065=CARTESIAN_POINT('Ctrl Pts',(10.0514365206282,80.8062463503336,-1.23094595618202E-15));
#282066=CARTESIAN_POINT('Ctrl Pts',(10.0514365206282,80.956246350333,-3.26590970098687));
#282067=CARTESIAN_POINT('Ctrl Pts',(8.13178296306919,81.1062463503324,-5.90808615117926));
#282068=CARTESIAN_POINT('Ctrl Pts',(6.21212940551018,81.2562463503318,-8.55026260137164));
#282069=CARTESIAN_POINT('Ctrl Pts',(3.10606470275506,81.4062463503312,-9.55948420107058));
#282070=CARTESIAN_POINT('Ctrl Pts',(-6.0093264332724E-14,81.5562463503306,
-10.5687058007695));
#282071=CARTESIAN_POINT('Ctrl Pts',(-3.10606470275518,81.70624635033,-9.55948420107058));
#282072=CARTESIAN_POINT('Ctrl Pts',(-6.2121294055103,81.8562463503294,-8.55026260137164));
#282073=CARTESIAN_POINT('Ctrl Pts',(-8.13178296306931,82.0062463503288,
-5.90808615117925));
#282074=CARTESIAN_POINT('Ctrl Pts',(-10.0514365206283,82.1562463503282,
-3.26590970098687));
#282075=CARTESIAN_POINT('Ctrl Pts',(-10.0514365206283,82.3062463503276,
2.46189191236404E-15));
#282076=CARTESIAN_POINT('Ctrl Pts',(-10.0514365206283,82.456246350327,3.26590970098687));
#282077=CARTESIAN_POINT('Ctrl Pts',(-8.13178296306931,82.6062463503264,
5.90808615117926));
#282078=CARTESIAN_POINT('Ctrl Pts',(-6.2121294055103,82.7562463503258,8.55026260137164));
#282079=CARTESIAN_POINT('Ctrl Pts',(-3.10606470275518,82.9062463503252,
9.55948420107058));
#282080=CARTESIAN_POINT('Ctrl Pts',(-5.83685326225464E-14,83.0562463503246,
10.5687058007695));
#282081=CARTESIAN_POINT('Ctrl Pts',(3.10606470275506,83.206246350324,9.55948420107058));
#282082=CARTESIAN_POINT('Ctrl Pts',(6.21212940551018,83.3562463503234,8.55026260137164));
#282083=CARTESIAN_POINT('Ctrl Pts',(8.13178296306918,83.5062463503228,5.90808615117925));
#282084=CARTESIAN_POINT('Ctrl Pts',(10.0514365206282,83.6562463503222,3.26590970098687));
#282085=CARTESIAN_POINT('Ctrl Pts',(10.0514365206282,83.8062463503216,-1.23094595618202E-15));
#282086=CARTESIAN_POINT('Ctrl Pts',(10.0514365206282,83.956246350321,-3.26590970098687));
#282087=CARTESIAN_POINT('Ctrl Pts',(8.13178296306918,84.1062463503204,-5.90808615117926));
#282088=CARTESIAN_POINT('Ctrl Pts',(6.21212940551018,84.2562463503198,-8.55026260137164));
#282089=CARTESIAN_POINT('Ctrl Pts',(3.10606470275506,84.4062463503192,-9.55948420107058));
#282090=CARTESIAN_POINT('Ctrl Pts',(-6.18209736043858E-14,84.5562463503186,
-10.5687058007695));
#282091=CARTESIAN_POINT('Ctrl Pts',(-3.10606470275518,84.706246350318,-9.55948420107058));
#282092=CARTESIAN_POINT('Ctrl Pts',(-6.2121294055103,84.8562463503174,-8.55026260137164));
#282093=CARTESIAN_POINT('Ctrl Pts',(-8.13178296306931,85.0062463503168,
-5.90808615117925));
#282094=CARTESIAN_POINT('Ctrl Pts',(-10.0514365206283,85.1562463503162,
-3.26590970098687));
#282095=CARTESIAN_POINT('Ctrl Pts',(-10.0514365206283,85.3062463503156,
2.46189191236404E-15));
#282096=CARTESIAN_POINT('Ctrl Pts',(-10.0514365206283,85.456246350315,3.26590970098687));
#282097=CARTESIAN_POINT('Ctrl Pts',(-8.13178296306931,85.6062463503144,
5.90808615117926));
#282098=CARTESIAN_POINT('Ctrl Pts',(-6.2121294055103,85.7562463503138,8.55026260137164));
#282099=CARTESIAN_POINT('Ctrl Pts',(-3.10606470275518,85.9062463503132,
9.55948420107058));
#282100=CARTESIAN_POINT('Ctrl Pts',(-6.00962418942082E-14,86.0562463503126,
10.5687058007695));
#282101=CARTESIAN_POINT('Ctrl Pts',(3.10606470275506,86.206246350312,9.55948420107058));
#282102=CARTESIAN_POINT('Ctrl Pts',(6.21212940551018,86.3562463503114,8.55026260137164));
#282103=CARTESIAN_POINT('Ctrl Pts',(8.13178296306918,86.5062463503108,5.90808615117925));
#282104=CARTESIAN_POINT('Ctrl Pts',(10.0514365206282,86.6562463503102,3.26590970098687));
#282105=CARTESIAN_POINT('Ctrl Pts',(10.0514365206282,86.8062463503096,-1.23094595618202E-15));
#282106=CARTESIAN_POINT('Ctrl Pts',(10.0514365206282,86.956246350309,-3.26590970098687));
#282107=CARTESIAN_POINT('Ctrl Pts',(8.13178296306918,87.1062463503084,-5.90808615117926));
#282108=CARTESIAN_POINT('Ctrl Pts',(6.21212940551018,87.2562463503078,-8.55026260137164));
#282109=CARTESIAN_POINT('Ctrl Pts',(3.10606470275506,87.4062463503072,-9.55948420107058));
#282110=CARTESIAN_POINT('Ctrl Pts',(-6.35486828760476E-14,87.5562463503066,
-10.5687058007695));
#282111=CARTESIAN_POINT('Ctrl Pts',(-3.10606470275518,87.706246350306,-9.55948420107058));
#282112=CARTESIAN_POINT('Ctrl Pts',(-6.21212940551031,87.8562463503054,
-8.55026260137164));
#282113=CARTESIAN_POINT('Ctrl Pts',(-8.13178296306931,88.0062463503048,
-5.90808615117925));
#282114=CARTESIAN_POINT('Ctrl Pts',(-10.0514365206283,88.1562463503042,
-3.26590970098687));
#282115=CARTESIAN_POINT('Ctrl Pts',(-10.0514365206283,88.3062463503036,
2.46189191236404E-15));
#282116=CARTESIAN_POINT('Ctrl Pts',(-10.0514365206283,88.456246350303,3.26590970098687));
#282117=CARTESIAN_POINT('Ctrl Pts',(-8.13178296306931,88.6062463503024,
5.90808615117926));
#282118=CARTESIAN_POINT('Ctrl Pts',(-6.2121294055103,88.7562463503018,8.55026260137164));
#282119=CARTESIAN_POINT('Ctrl Pts',(-3.10606470275518,88.9062463503012,
9.55948420107058));
#282120=CARTESIAN_POINT('Ctrl Pts',(-6.18239511658701E-14,89.0562463503006,
10.5687058007695));
#282121=CARTESIAN_POINT('Ctrl Pts',(3.10606470275506,89.2062463503,9.55948420107058));
#282122=CARTESIAN_POINT('Ctrl Pts',(6.21212940551018,89.3562463502994,8.55026260137164));
#282123=CARTESIAN_POINT('Ctrl Pts',(8.13178296306918,89.5062463502988,5.90808615117925));
#282124=CARTESIAN_POINT('Ctrl Pts',(10.0514365206282,89.6562463502982,3.26590970098687));
#282125=CARTESIAN_POINT('Ctrl Pts',(10.0514365206282,89.8062463502976,-1.23094595618202E-15));
#282126=CARTESIAN_POINT('Ctrl Pts',(10.0514365206282,89.956246350297,-3.26590970098687));
#282127=CARTESIAN_POINT('Ctrl Pts',(8.13178296306918,90.1062463502964,-5.90808615117926));
#282128=CARTESIAN_POINT('Ctrl Pts',(6.21212940551018,90.2562463502958,-8.55026260137164));
#282129=CARTESIAN_POINT('Ctrl Pts',(3.10606470275506,90.4062463502952,-9.55948420107058));
#282130=CARTESIAN_POINT('Ctrl Pts',(-6.52763921477095E-14,90.5562463502946,
-10.5687058007695));
#282131=CARTESIAN_POINT('Ctrl Pts',(-3.10606470275519,90.706246350294,-9.55948420107058));
#282132=CARTESIAN_POINT('Ctrl Pts',(-6.21212940551031,90.8562463502934,
-8.55026260137164));
#282133=CARTESIAN_POINT('Ctrl Pts',(-8.13178296306931,91.0062463502928,
-5.90808615117925));
#282134=CARTESIAN_POINT('Ctrl Pts',(-10.0514365206283,91.1562463502922,
-3.26590970098687));
#282135=CARTESIAN_POINT('Ctrl Pts',(-10.0514365206283,91.3062463502916,
2.46189191236404E-15));
#282136=CARTESIAN_POINT('Ctrl Pts',(-10.0514365206283,91.456246350291,3.26590970098687));
#282137=CARTESIAN_POINT('Ctrl Pts',(-8.13178296306931,91.6062463502904,
5.90808615117926));
#282138=CARTESIAN_POINT('Ctrl Pts',(-6.21212940551031,91.7562463502898,
8.55026260137164));
#282139=CARTESIAN_POINT('Ctrl Pts',(-3.10606470275518,91.9062463502892,
9.55948420107058));
#282140=CARTESIAN_POINT('Ctrl Pts',(-6.35516604375319E-14,92.0562463502886,
10.5687058007695));
#282141=CARTESIAN_POINT('Ctrl Pts',(3.10606470275506,92.206246350288,9.55948420107058));
#282142=CARTESIAN_POINT('Ctrl Pts',(6.21212940551018,92.3562463502874,8.55026260137164));
#282143=CARTESIAN_POINT('Ctrl Pts',(8.13178296306918,92.5062463502868,5.90808615117925));
#282144=CARTESIAN_POINT('Ctrl Pts',(10.0514365206282,92.6562463502862,3.26590970098687));
#282145=CARTESIAN_POINT('Ctrl Pts',(10.0514365206282,92.8062463502856,-1.23094595618202E-15));
#282146=CARTESIAN_POINT('Ctrl Pts',(10.0514365206282,92.956246350285,-3.26590970098687));
#282147=CARTESIAN_POINT('Ctrl Pts',(8.13178296306918,93.1062463502844,-5.90808615117926));
#282148=CARTESIAN_POINT('Ctrl Pts',(6.21212940551018,93.2562463502838,-8.55026260137164));
#282149=CARTESIAN_POINT('Ctrl Pts',(3.10606470275505,93.4062463502832,-9.55948420107058));
#282150=CARTESIAN_POINT('Ctrl Pts',(-6.70041014193713E-14,93.5562463502826,
-10.5687058007695));
#282151=CARTESIAN_POINT('Ctrl Pts',(-3.10606470275519,93.706246350282,-9.55948420107058));
#282152=CARTESIAN_POINT('Ctrl Pts',(-6.21212940551031,93.8562463502814,
-8.55026260137164));
#282153=CARTESIAN_POINT('Ctrl Pts',(-8.13178296306931,94.0062463502808,
-5.90808615117925));
#282154=CARTESIAN_POINT('Ctrl Pts',(-10.0514365206283,94.1562463502802,
-3.26590970098687));
#282155=CARTESIAN_POINT('Ctrl Pts',(-10.0514365206283,94.3062463502796,
2.46189191236404E-15));
#282156=CARTESIAN_POINT('Ctrl Pts',(-10.0514365206283,94.456246350279,3.26590970098687));
#282157=CARTESIAN_POINT('Ctrl Pts',(-8.13178296306931,94.6062463502784,
5.90808615117926));
#282158=CARTESIAN_POINT('Ctrl Pts',(-6.21212940551031,94.7562463502778,
8.55026260137164));
#282159=CARTESIAN_POINT('Ctrl Pts',(-3.10606470275519,94.9062463502772,
9.55948420107058));
#282160=CARTESIAN_POINT('Ctrl Pts',(-6.52793697091937E-14,95.0562463502766,
10.5687058007695));
#282161=CARTESIAN_POINT('Ctrl Pts',(3.10606470275505,95.206246350276,9.55948420107058));
#282162=CARTESIAN_POINT('Ctrl Pts',(6.21212940551018,95.3562463502754,8.55026260137164));
#282163=CARTESIAN_POINT('Ctrl Pts',(8.13178296306918,95.5062463502748,5.90808615117925));
#282164=CARTESIAN_POINT('Ctrl Pts',(10.0514365206282,95.6562463502742,3.26590970098687));
#282165=CARTESIAN_POINT('Ctrl Pts',(10.0514365206282,95.8062463502736,-1.23094595618202E-15));
#282166=CARTESIAN_POINT('Ctrl Pts',(10.0514365206282,95.956246350273,-3.26590970098687));
#282167=CARTESIAN_POINT('Ctrl Pts',(8.13178296306918,96.1062463502724,-5.90808615117926));
#282168=CARTESIAN_POINT('Ctrl Pts',(6.21212940551017,96.2562463502718,-8.55026260137164));
#282169=CARTESIAN_POINT('Ctrl Pts',(3.10606470275505,96.4062463502712,-9.55948420107058));
#282170=CARTESIAN_POINT('Ctrl Pts',(-6.87318106910331E-14,96.5562463502706,
-10.5687058007695));
#282171=CARTESIAN_POINT('Ctrl Pts',(-3.10606470275519,96.70624635027,-9.55948420107058));
#282172=CARTESIAN_POINT('Ctrl Pts',(-6.21212940551031,96.8562463502694,
-8.55026260137164));
#282173=CARTESIAN_POINT('Ctrl Pts',(-8.13178296306931,97.0062463502688,
-5.90808615117925));
#282174=CARTESIAN_POINT('Ctrl Pts',(-10.0514365206283,97.1562463502682,
-3.26590970098687));
#282175=CARTESIAN_POINT('Ctrl Pts',(-10.0514365206283,97.3062463502676,
2.46189191236404E-15));
#282176=CARTESIAN_POINT('Ctrl Pts',(-10.0514365206283,97.456246350267,3.26590970098687));
#282177=CARTESIAN_POINT('Ctrl Pts',(-8.13178296306931,97.6062463502664,
5.90808615117926));
#282178=CARTESIAN_POINT('Ctrl Pts',(-6.21212940551031,97.7562463502658,
8.55026260137164));
#282179=CARTESIAN_POINT('Ctrl Pts',(-3.10606470275519,97.9062463502652,
9.55948420107058));
#282180=CARTESIAN_POINT('Ctrl Pts',(-6.70070789808556E-14,98.0562463502646,
10.5687058007695));
#282181=CARTESIAN_POINT('Ctrl Pts',(3.10606470275505,98.206246350264,9.55948420107058));
#282182=CARTESIAN_POINT('Ctrl Pts',(6.21212940551018,98.3562463502634,8.55026260137164));
#282183=CARTESIAN_POINT('Ctrl Pts',(8.13178296306918,98.5062463502628,5.90808615117925));
#282184=CARTESIAN_POINT('Ctrl Pts',(10.0514365206282,98.6562463502622,3.26590970098687));
#282185=CARTESIAN_POINT('Ctrl Pts',(10.0514365206282,98.8062463502616,-1.23094595618202E-15));
#282186=CARTESIAN_POINT('Ctrl Pts',(10.0514365206282,98.956246350261,-3.26590970098687));
#282187=CARTESIAN_POINT('Ctrl Pts',(8.13178296306918,99.1062463502604,-5.90808615117926));
#282188=CARTESIAN_POINT('Ctrl Pts',(6.21212940551017,99.2562463502598,-8.55026260137164));
#282189=CARTESIAN_POINT('Ctrl Pts',(3.10606470275505,99.4062463502592,-9.55948420107058));
#282190=CARTESIAN_POINT('Ctrl Pts',(-7.0459519962695E-14,99.5562463502586,
-10.5687058007695));
#282191=CARTESIAN_POINT('Ctrl Pts',(-3.10606470275519,99.706246350258,-9.55948420107058));
#282192=CARTESIAN_POINT('Ctrl Pts',(-6.21212940551031,99.8562463502574,
-8.55026260137164));
#282193=CARTESIAN_POINT('Ctrl Pts',(-8.13178296306931,100.006246350257,
-5.90808615117925));
#282194=CARTESIAN_POINT('Ctrl Pts',(-10.0514365206283,100.156246350256,
-3.26590970098687));
#282195=CARTESIAN_POINT('Ctrl Pts',(-10.0514365206283,100.306246350256,
2.46189191236404E-15));
#282196=CARTESIAN_POINT('Ctrl Pts',(-10.0514365206283,100.456246350255,
3.26590970098687));
#282197=CARTESIAN_POINT('Ctrl Pts',(-8.13178296306931,100.606246350254,
5.90808615117926));
#282198=CARTESIAN_POINT('Ctrl Pts',(-6.21212940551031,100.756246350254,
8.55026260137164));
#282199=CARTESIAN_POINT('Ctrl Pts',(-3.10606470275519,100.906246350253,
9.55948420107058));
#282200=CARTESIAN_POINT('Ctrl Pts',(-6.87347882525174E-14,101.056246350253,
10.5687058007695));
#282201=CARTESIAN_POINT('Ctrl Pts',(3.10606470275505,101.206246350252,9.55948420107058));
#282202=CARTESIAN_POINT('Ctrl Pts',(6.21212940551017,101.356246350251,8.55026260137164));
#282203=CARTESIAN_POINT('Ctrl Pts',(8.13178296306917,101.506246350251,5.90808615117925));
#282204=CARTESIAN_POINT('Ctrl Pts',(10.0514365206282,101.65624635025,3.26590970098687));
#282205=CARTESIAN_POINT('Ctrl Pts',(10.0514365206282,101.80624635025,-1.23094595618202E-15));
#282206=CARTESIAN_POINT('Ctrl Pts',(10.0514365206282,101.956246350249,-3.26590970098687));
#282207=CARTESIAN_POINT('Ctrl Pts',(8.13178296306917,102.106246350248,-5.90808615117926));
#282208=CARTESIAN_POINT('Ctrl Pts',(6.21212940551017,102.256246350248,-8.55026260137164));
#282209=CARTESIAN_POINT('Ctrl Pts',(3.10606470275505,102.406246350247,-9.55948420107058));
#282210=CARTESIAN_POINT('Ctrl Pts',(-7.21872292343569E-14,102.556246350247,
-10.5687058007695));
#282211=CARTESIAN_POINT('Ctrl Pts',(-3.10606470275519,102.706246350246,
-9.55948420107058));
#282212=CARTESIAN_POINT('Ctrl Pts',(-6.21212940551031,102.856246350245,
-8.55026260137164));
#282213=CARTESIAN_POINT('Ctrl Pts',(-8.13178296306932,103.006246350245,
-5.90808615117925));
#282214=CARTESIAN_POINT('Ctrl Pts',(-10.0514365206283,103.156246350244,
-3.26590970098687));
#282215=CARTESIAN_POINT('Ctrl Pts',(-10.0514365206283,103.306246350244,
2.46189191236404E-15));
#282216=CARTESIAN_POINT('Ctrl Pts',(-10.0514365206283,103.456246350243,
3.26590970098687));
#282217=CARTESIAN_POINT('Ctrl Pts',(-8.13178296306932,103.606246350242,
5.90808615117926));
#282218=CARTESIAN_POINT('Ctrl Pts',(-6.21212940551031,103.756246350242,
8.55026260137164));
#282219=CARTESIAN_POINT('Ctrl Pts',(-3.10606470275519,103.906246350241,
9.55948420107058));
#282220=CARTESIAN_POINT('Ctrl Pts',(-7.04624975241793E-14,104.056246350241,
10.5687058007695));
#282221=CARTESIAN_POINT('Ctrl Pts',(3.10606470275505,104.20624635024,9.55948420107058));
#282222=CARTESIAN_POINT('Ctrl Pts',(6.21212940551017,104.356246350239,8.55026260137164));
#282223=CARTESIAN_POINT('Ctrl Pts',(8.13178296306917,104.506246350239,5.90808615117925));
#282224=CARTESIAN_POINT('Ctrl Pts',(10.0514365206282,104.656246350238,3.26590970098687));
#282225=CARTESIAN_POINT('Ctrl Pts',(10.0514365206282,104.806246350238,-1.23094595618202E-15));
#282226=CARTESIAN_POINT('Ctrl Pts',(10.0514365206282,104.956246350237,-3.26590970098687));
#282227=CARTESIAN_POINT('Ctrl Pts',(8.13178296306917,105.106246350236,-5.90808615117926));
#282228=CARTESIAN_POINT('Ctrl Pts',(6.21212940551017,105.256246350236,-8.55026260137164));
#282229=CARTESIAN_POINT('Ctrl Pts',(3.10606470275505,105.406246350235,-9.55948420107058));
#282230=CARTESIAN_POINT('Ctrl Pts',(-7.39149385060187E-14,105.556246350235,
-10.5687058007695));
#282231=CARTESIAN_POINT('Ctrl Pts',(-3.1060647027552,105.706246350234,-9.55948420107058));
#282232=CARTESIAN_POINT('Ctrl Pts',(-6.21212940551032,105.856246350233,
-8.55026260137164));
#282233=CARTESIAN_POINT('Ctrl Pts',(-8.13178296306932,106.006246350233,
-5.90808615117925));
#282234=CARTESIAN_POINT('Ctrl Pts',(-10.0514365206283,106.156246350232,
-3.26590970098687));
#282235=CARTESIAN_POINT('Ctrl Pts',(-10.0514365206283,106.306246350232,
2.46189191236404E-15));
#282236=CARTESIAN_POINT('Ctrl Pts',(-10.0514365206283,106.456246350231,
3.26590970098687));
#282237=CARTESIAN_POINT('Ctrl Pts',(-8.13178296306932,106.60624635023,5.90808615117926));
#282238=CARTESIAN_POINT('Ctrl Pts',(-6.21212940551031,106.75624635023,8.55026260137164));
#282239=CARTESIAN_POINT('Ctrl Pts',(-3.10606470275519,106.906246350229,
9.55948420107058));
#282240=CARTESIAN_POINT('Ctrl Pts',(-7.21902067958411E-14,107.056246350229,
10.5687058007695));
#282241=CARTESIAN_POINT('Ctrl Pts',(3.10606470275505,107.206246350228,9.55948420107058));
#282242=CARTESIAN_POINT('Ctrl Pts',(6.21212940551017,107.356246350227,8.55026260137164));
#282243=CARTESIAN_POINT('Ctrl Pts',(8.13178296306917,107.506246350227,5.90808615117925));
#282244=CARTESIAN_POINT('Ctrl Pts',(10.0514365206282,107.656246350226,3.26590970098687));
#282245=CARTESIAN_POINT('Ctrl Pts',(10.0514365206282,107.806246350226,-1.23094595618202E-15));
#282246=CARTESIAN_POINT('Ctrl Pts',(10.0514365206282,107.956246350225,-3.26590970098687));
#282247=CARTESIAN_POINT('Ctrl Pts',(8.13178296306917,108.106246350224,-5.90808615117926));
#282248=CARTESIAN_POINT('Ctrl Pts',(6.21212940551017,108.256246350224,-8.55026260137164));
#282249=CARTESIAN_POINT('Ctrl Pts',(3.10606470275505,108.406246350223,-9.55948420107058));
#282250=CARTESIAN_POINT('Ctrl Pts',(-7.56426477776805E-14,108.556246350223,
-10.5687058007695));
#282251=CARTESIAN_POINT('Ctrl Pts',(-3.1060647027552,108.706246350222,-9.55948420107058));
#282252=CARTESIAN_POINT('Ctrl Pts',(-6.21212940551032,108.856246350221,
-8.55026260137164));
#282253=CARTESIAN_POINT('Ctrl Pts',(-8.13178296306932,109.006246350221,
-5.90808615117925));
#282254=CARTESIAN_POINT('Ctrl Pts',(-10.0514365206283,109.15624635022,-3.26590970098687));
#282255=CARTESIAN_POINT('Ctrl Pts',(-10.0514365206283,109.30624635022,2.46189191236404E-15));
#282256=CARTESIAN_POINT('Ctrl Pts',(-10.0514365206283,109.456246350219,
3.26590970098687));
#282257=CARTESIAN_POINT('Ctrl Pts',(-8.13178296306932,109.606246350218,
5.90808615117926));
#282258=CARTESIAN_POINT('Ctrl Pts',(-6.21212940551032,109.756246350218,
8.55026260137164));
#282259=CARTESIAN_POINT('Ctrl Pts',(-3.10606470275519,109.906246350217,
9.55948420107058));
#282260=CARTESIAN_POINT('Ctrl Pts',(-7.39179160675029E-14,110.056246350217,
10.5687058007695));
#282261=CARTESIAN_POINT('Ctrl Pts',(3.10606470275505,110.206246350216,9.55948420107058));
#282262=CARTESIAN_POINT('Ctrl Pts',(6.21212940551017,110.356246350215,8.55026260137164));
#282263=CARTESIAN_POINT('Ctrl Pts',(8.13178296306917,110.506246350215,5.90808615117925));
#282264=CARTESIAN_POINT('Ctrl Pts',(10.0514365206282,110.656246350214,3.26590970098687));
#282265=CARTESIAN_POINT('Ctrl Pts',(10.0514365206282,110.806246350214,-1.23094595618202E-15));
#282266=CARTESIAN_POINT('Ctrl Pts',(10.0514365206282,110.956246350213,-3.26590970098687));
#282267=CARTESIAN_POINT('Ctrl Pts',(8.13178296306917,111.106246350212,-5.90808615117926));
#282268=CARTESIAN_POINT('Ctrl Pts',(6.21212940551017,111.256246350212,-8.55026260137164));
#282269=CARTESIAN_POINT('Ctrl Pts',(3.10606470275504,111.406246350211,-9.55948420107058));
#282270=CARTESIAN_POINT('Ctrl Pts',(-7.73703570493424E-14,111.556246350211,
-10.5687058007695));
#282271=CARTESIAN_POINT('Ctrl Pts',(-3.1060647027552,111.70624635021,-9.55948420107058));
#282272=CARTESIAN_POINT('Ctrl Pts',(-6.21212940551032,111.856246350209,
-8.55026260137164));
#282273=CARTESIAN_POINT('Ctrl Pts',(-8.13178296306932,112.006246350209,
-5.90808615117925));
#282274=CARTESIAN_POINT('Ctrl Pts',(-10.0514365206283,112.156246350208,
-3.26590970098687));
#282275=CARTESIAN_POINT('Ctrl Pts',(-10.0514365206283,112.306246350208,
2.46189191236404E-15));
#282276=CARTESIAN_POINT('Ctrl Pts',(-10.0514365206283,112.456246350207,
3.26590970098687));
#282277=CARTESIAN_POINT('Ctrl Pts',(-8.13178296306932,112.606246350206,
5.90808615117926));
#282278=CARTESIAN_POINT('Ctrl Pts',(-6.21212940551032,112.756246350206,
8.55026260137164));
#282279=CARTESIAN_POINT('Ctrl Pts',(-3.1060647027552,112.906246350205,9.55948420107058));
#282280=CARTESIAN_POINT('Ctrl Pts',(-7.56456253391648E-14,113.056246350205,
10.5687058007695));
#282281=CARTESIAN_POINT('Ctrl Pts',(3.10606470275504,113.206246350204,9.55948420107058));
#282282=CARTESIAN_POINT('Ctrl Pts',(6.21212940551017,113.356246350203,8.55026260137164));
#282283=CARTESIAN_POINT('Ctrl Pts',(8.13178296306917,113.506246350203,5.90808615117925));
#282284=CARTESIAN_POINT('Ctrl Pts',(10.0514365206282,113.656246350202,3.26590970098687));
#282285=CARTESIAN_POINT('Ctrl Pts',(10.0514365206282,113.806246350202,-1.23094595618202E-15));
#282286=CARTESIAN_POINT('Ctrl Pts',(10.0514365206282,113.956246350201,-3.26590970098687));
#282287=CARTESIAN_POINT('Ctrl Pts',(8.13178296306917,114.1062463502,-5.90808615117926));
#282288=CARTESIAN_POINT('Ctrl Pts',(6.21212940551016,114.2562463502,-8.55026260137164));
#282289=CARTESIAN_POINT('Ctrl Pts',(3.10606470275504,114.406246350199,-9.55948420107058));
#282290=CARTESIAN_POINT('Ctrl Pts',(-7.90980663210042E-14,114.556246350199,
-10.5687058007695));
#282291=CARTESIAN_POINT('Ctrl Pts',(-3.1060647027552,114.706246350198,-9.55948420107058));
#282292=CARTESIAN_POINT('Ctrl Pts',(-6.21212940551032,114.856246350197,
-8.55026260137164));
#282293=CARTESIAN_POINT('Ctrl Pts',(-8.13178296306932,115.006246350197,
-5.90808615117925));
#282294=CARTESIAN_POINT('Ctrl Pts',(-10.0514365206283,115.156246350196,
-3.26590970098687));
#282295=CARTESIAN_POINT('Ctrl Pts',(-10.0514365206283,115.306246350196,
2.46189191236404E-15));
#282296=CARTESIAN_POINT('Ctrl Pts',(-10.0514365206283,115.456246350195,
3.26590970098687));
#282297=CARTESIAN_POINT('Ctrl Pts',(-8.13178296306932,115.606246350194,
5.90808615117926));
#282298=CARTESIAN_POINT('Ctrl Pts',(-6.21212940551032,115.756246350194,
8.55026260137164));
#282299=CARTESIAN_POINT('Ctrl Pts',(-3.1060647027552,115.906246350193,9.55948420107058));
#282300=CARTESIAN_POINT('Ctrl Pts',(-7.73733346108267E-14,116.056246350193,
10.5687058007695));
#282301=CARTESIAN_POINT('Ctrl Pts',(3.10606470275504,116.206246350192,9.55948420107058));
#282302=CARTESIAN_POINT('Ctrl Pts',(6.21212940551017,116.356246350191,8.55026260137164));
#282303=CARTESIAN_POINT('Ctrl Pts',(8.13178296306917,116.506246350191,5.90808615117925));
#282304=CARTESIAN_POINT('Ctrl Pts',(10.0514365206282,116.65624635019,3.26590970098687));
#282305=CARTESIAN_POINT('Ctrl Pts',(10.0514365206282,116.80624635019,-1.23094595618202E-15));
#282306=CARTESIAN_POINT('Ctrl Pts',(10.0514365206282,116.956246350189,-3.26590970098687));
#282307=CARTESIAN_POINT('Ctrl Pts',(8.13178296306917,117.106246350188,-5.90808615117926));
#282308=CARTESIAN_POINT('Ctrl Pts',(6.21212940551016,117.256246350188,-8.55026260137164));
#282309=CARTESIAN_POINT('Ctrl Pts',(3.10606470275504,117.406246350187,-9.55948420107058));
#282310=CARTESIAN_POINT('Ctrl Pts',(-8.0825775592666E-14,117.556246350187,
-10.5687058007695));
#282311=CARTESIAN_POINT('Ctrl Pts',(-3.1060647027552,117.706246350186,-9.55948420107058));
#282312=CARTESIAN_POINT('Ctrl Pts',(-6.21212940551032,117.856246350185,
-8.55026260137164));
#282313=CARTESIAN_POINT('Ctrl Pts',(-8.13178296306933,118.006246350185,
-5.90808615117925));
#282314=CARTESIAN_POINT('Ctrl Pts',(-10.0514365206283,118.156246350184,
-3.26590970098687));
#282315=CARTESIAN_POINT('Ctrl Pts',(-10.0514365206283,118.306246350184,
2.46189191236404E-15));
#282316=CARTESIAN_POINT('Ctrl Pts',(-10.0514365206283,118.456246350183,
3.26590970098687));
#282317=CARTESIAN_POINT('Ctrl Pts',(-8.13178296306933,118.606246350182,
5.90808615117926));
#282318=CARTESIAN_POINT('Ctrl Pts',(-6.21212940551032,118.756246350182,
8.55026260137164));
#282319=CARTESIAN_POINT('Ctrl Pts',(-3.1060647027552,118.906246350181,9.55948420107058));
#282320=CARTESIAN_POINT('Ctrl Pts',(-7.91010438824885E-14,119.056246350181,
10.5687058007695));
#282321=CARTESIAN_POINT('Ctrl Pts',(3.10606470275504,119.20624635018,9.55948420107058));
#282322=CARTESIAN_POINT('Ctrl Pts',(6.21212940551016,119.356246350179,8.55026260137164));
#282323=CARTESIAN_POINT('Ctrl Pts',(8.13178296306916,119.506246350179,5.90808615117925));
#282324=CARTESIAN_POINT('Ctrl Pts',(10.0514365206282,119.656246350178,3.26590970098687));
#282325=CARTESIAN_POINT('Ctrl Pts',(10.0514365206282,119.806246350178,-1.23094595618202E-15));
#282326=CARTESIAN_POINT('Ctrl Pts',(10.0514365206282,119.956246350177,-3.26590970098687));
#282327=CARTESIAN_POINT('Ctrl Pts',(8.13178296306916,120.106246350176,-5.90808615117926));
#282328=CARTESIAN_POINT('Ctrl Pts',(6.21212940551016,120.256246350176,-8.55026260137164));
#282329=CARTESIAN_POINT('Ctrl Pts',(3.10606470275504,120.406246350175,-9.55948420107058));
#282330=CARTESIAN_POINT('Ctrl Pts',(-8.25534848643279E-14,120.556246350175,
-10.5687058007695));
#282331=CARTESIAN_POINT('Ctrl Pts',(-3.1060647027552,120.706246350174,-9.55948420107058));
#282332=CARTESIAN_POINT('Ctrl Pts',(-6.21212940551032,120.856246350173,
-8.55026260137164));
#282333=CARTESIAN_POINT('Ctrl Pts',(-8.13178296306933,121.006246350173,
-5.90808615117925));
#282334=CARTESIAN_POINT('Ctrl Pts',(-10.0514365206283,121.156246350172,
-3.26590970098687));
#282335=CARTESIAN_POINT('Ctrl Pts',(-10.0514365206283,121.306246350172,
2.46189191236404E-15));
#282336=CARTESIAN_POINT('Ctrl Pts',(-10.0514365206283,121.456246350171,
3.26590970098687));
#282337=CARTESIAN_POINT('Ctrl Pts',(-8.13178296306933,121.60624635017,5.90808615117926));
#282338=CARTESIAN_POINT('Ctrl Pts',(-6.21212940551032,121.75624635017,8.55026260137164));
#282339=CARTESIAN_POINT('Ctrl Pts',(-3.1060647027552,121.906246350169,9.55948420107058));
#282340=CARTESIAN_POINT('Ctrl Pts',(-8.08287531541503E-14,122.056246350169,
10.5687058007695));
#282341=CARTESIAN_POINT('Ctrl Pts',(3.10606470275504,122.206246350168,9.55948420107058));
#282342=CARTESIAN_POINT('Ctrl Pts',(6.21212940551016,122.356246350167,8.55026260137164));
#282343=CARTESIAN_POINT('Ctrl Pts',(8.13178296306916,122.506246350167,5.90808615117925));
#282344=CARTESIAN_POINT('Ctrl Pts',(10.0514365206282,122.656246350166,3.26590970098687));
#282345=CARTESIAN_POINT('Ctrl Pts',(10.0514365206282,122.806246350166,-1.23094595618202E-15));
#282346=CARTESIAN_POINT('Ctrl Pts',(10.0514365206282,122.956246350165,-3.26590970098687));
#282347=CARTESIAN_POINT('Ctrl Pts',(8.13178296306916,123.106246350164,-5.90808615117926));
#282348=CARTESIAN_POINT('Ctrl Pts',(6.21212940551016,123.256246350164,-8.55026260137164));
#282349=CARTESIAN_POINT('Ctrl Pts',(3.10606470275504,123.406246350163,-9.55948420107058));
#282350=CARTESIAN_POINT('Ctrl Pts',(-8.42811941359897E-14,123.556246350163,
-10.5687058007695));
#282351=CARTESIAN_POINT('Ctrl Pts',(-3.10606470275521,123.706246350162,
-9.55948420107058));
#282352=CARTESIAN_POINT('Ctrl Pts',(-6.21212940551032,123.856246350161,
-8.55026260137164));
#282353=CARTESIAN_POINT('Ctrl Pts',(-8.13178296306933,124.006246350161,
-5.90808615117925));
#282354=CARTESIAN_POINT('Ctrl Pts',(-10.0514365206283,124.15624635016,-3.26590970098687));
#282355=CARTESIAN_POINT('Ctrl Pts',(-10.0514365206283,124.30624635016,2.46189191236404E-15));
#282356=CARTESIAN_POINT('Ctrl Pts',(-10.0514365206283,124.456246350159,
3.26590970098687));
#282357=CARTESIAN_POINT('Ctrl Pts',(-8.13178296306933,124.606246350158,
5.90808615117926));
#282358=CARTESIAN_POINT('Ctrl Pts',(-6.21212940551032,124.756246350158,
8.55026260137164));
#282359=CARTESIAN_POINT('Ctrl Pts',(-3.1060647027552,124.906246350157,9.55948420107058));
#282360=CARTESIAN_POINT('Ctrl Pts',(-8.25564624258121E-14,125.056246350157,
10.5687058007695));
#282361=CARTESIAN_POINT('Ctrl Pts',(3.10606470275504,125.206246350156,9.55948420107058));
#282362=CARTESIAN_POINT('Ctrl Pts',(6.21212940551016,125.356246350155,8.55026260137164));
#282363=CARTESIAN_POINT('Ctrl Pts',(8.13178296306916,125.506246350155,5.90808615117925));
#282364=CARTESIAN_POINT('Ctrl Pts',(10.0514365206282,125.656246350154,3.26590970098687));
#282365=CARTESIAN_POINT('Ctrl Pts',(10.0514365206282,125.806246350154,-1.23094595618202E-15));
#282366=CARTESIAN_POINT('Ctrl Pts',(10.0514365206282,125.956246350153,-3.26590970098687));
#282367=CARTESIAN_POINT('Ctrl Pts',(8.13178296306916,126.106246350152,-5.90808615117926));
#282368=CARTESIAN_POINT('Ctrl Pts',(6.21212940551016,126.256246350152,-8.55026260137164));
#282369=CARTESIAN_POINT('Ctrl Pts',(3.10606470275503,126.406246350151,-9.55948420107058));
#282370=CARTESIAN_POINT('Ctrl Pts',(-8.60089034076516E-14,126.556246350151,
-10.5687058007695));
#282371=CARTESIAN_POINT('Ctrl Pts',(-3.10606470275521,126.70624635015,-9.55948420107058));
#282372=CARTESIAN_POINT('Ctrl Pts',(-6.21212940551033,126.856246350149,
-8.55026260137164));
#282373=CARTESIAN_POINT('Ctrl Pts',(-8.13178296306933,127.006246350149,
-5.90808615117925));
#282374=CARTESIAN_POINT('Ctrl Pts',(-10.0514365206283,127.156246350148,
-3.26590970098687));
#282375=CARTESIAN_POINT('Ctrl Pts',(-10.0514365206283,127.306246350148,
2.46189191236404E-15));
#282376=CARTESIAN_POINT('Ctrl Pts',(-10.0514365206283,127.456246350147,
3.26590970098687));
#282377=CARTESIAN_POINT('Ctrl Pts',(-8.13178296306933,127.606246350146,
5.90808615117926));
#282378=CARTESIAN_POINT('Ctrl Pts',(-6.21212940551032,127.756246350146,
8.55026260137164));
#282379=CARTESIAN_POINT('Ctrl Pts',(-3.10606470275521,127.906246350145,
9.55948420107058));
#282380=CARTESIAN_POINT('Ctrl Pts',(-8.4284171697474E-14,128.056246350145,
10.5687058007695));
#282381=CARTESIAN_POINT('Ctrl Pts',(3.10606470275504,128.206246350144,9.55948420107058));
#282382=CARTESIAN_POINT('Ctrl Pts',(6.21212940551016,128.356246350143,8.55026260137164));
#282383=CARTESIAN_POINT('Ctrl Pts',(8.13178296306916,128.506246350143,5.90808615117925));
#282384=CARTESIAN_POINT('Ctrl Pts',(10.0514365206282,128.656246350142,3.26590970098687));
#282385=CARTESIAN_POINT('Ctrl Pts',(10.0514365206282,128.806246350142,-1.23094595618202E-15));
#282386=CARTESIAN_POINT('Ctrl Pts',(10.0514365206282,128.956246350141,-3.26590970098687));
#282387=CARTESIAN_POINT('Ctrl Pts',(8.13178296306916,129.10624635014,-5.90808615117926));
#282388=CARTESIAN_POINT('Ctrl Pts',(6.21212940551015,129.25624635014,-8.55026260137164));
#282389=CARTESIAN_POINT('Ctrl Pts',(3.10606470275503,129.406246350139,-9.55948420107058));
#282390=CARTESIAN_POINT('Ctrl Pts',(-8.77366126793134E-14,129.556246350139,
-10.5687058007695));
#282391=CARTESIAN_POINT('Ctrl Pts',(-3.10606470275521,129.706246350138,
-9.55948420107058));
#282392=CARTESIAN_POINT('Ctrl Pts',(-6.21212940551033,129.856246350137,
-8.55026260137164));
#282393=CARTESIAN_POINT('Ctrl Pts',(-8.13178296306933,130.006246350137,
-5.90808615117925));
#282394=CARTESIAN_POINT('Ctrl Pts',(-10.0514365206283,130.156246350136,
-3.26590970098687));
#282395=CARTESIAN_POINT('Ctrl Pts',(-10.0514365206283,130.306246350136,
2.46189191236404E-15));
#282396=CARTESIAN_POINT('Ctrl Pts',(-10.0514365206283,130.456246350135,
3.26590970098687));
#282397=CARTESIAN_POINT('Ctrl Pts',(-8.13178296306933,130.606246350134,
5.90808615117926));
#282398=CARTESIAN_POINT('Ctrl Pts',(-6.21212940551033,130.756246350134,
8.55026260137164));
#282399=CARTESIAN_POINT('Ctrl Pts',(-3.10606470275521,130.906246350133,
9.55948420107058));
#282400=CARTESIAN_POINT('Ctrl Pts',(-8.60118809691358E-14,131.056246350133,
10.5687058007695));
#282401=CARTESIAN_POINT('Ctrl Pts',(3.10606470275503,131.206246350132,9.55948420107058));
#282402=CARTESIAN_POINT('Ctrl Pts',(6.21212940551016,131.356246350131,8.55026260137164));
#282403=CARTESIAN_POINT('Ctrl Pts',(8.13178296306916,131.506246350131,5.90808615117925));
#282404=CARTESIAN_POINT('Ctrl Pts',(10.0514365206282,131.65624635013,3.26590970098687));
#282405=CARTESIAN_POINT('Ctrl Pts',(10.0514365206282,131.80624635013,-1.23094595618202E-15));
#282406=CARTESIAN_POINT('Ctrl Pts',(10.0514365206282,131.956246350129,-3.26590970098687));
#282407=CARTESIAN_POINT('Ctrl Pts',(8.13178296306916,132.106246350128,-5.90808615117926));
#282408=CARTESIAN_POINT('Ctrl Pts',(6.21212940551015,132.256246350128,-8.55026260137164));
#282409=CARTESIAN_POINT('Ctrl Pts',(3.10606470275503,132.406246350127,-9.55948420107058));
#282410=CARTESIAN_POINT('Ctrl Pts',(-8.94643219509752E-14,132.556246350127,
-10.5687058007695));
#282411=CARTESIAN_POINT('Ctrl Pts',(-3.10606470275521,132.706246350126,
-9.55948420107058));
#282412=CARTESIAN_POINT('Ctrl Pts',(-6.21212940551033,132.856246350125,
-8.55026260137164));
#282413=CARTESIAN_POINT('Ctrl Pts',(-8.13178296306934,133.006246350125,
-5.90808615117925));
#282414=CARTESIAN_POINT('Ctrl Pts',(-10.0514365206283,133.156246350124,
-3.26590970098687));
#282415=CARTESIAN_POINT('Ctrl Pts',(-10.0514365206283,133.306246350124,
2.46189191236404E-15));
#282416=CARTESIAN_POINT('Ctrl Pts',(-10.0514365206283,133.456246350123,
3.26590970098687));
#282417=CARTESIAN_POINT('Ctrl Pts',(-8.13178296306934,133.606246350122,
5.90808615117926));
#282418=CARTESIAN_POINT('Ctrl Pts',(-6.21212940551033,133.756246350122,
8.55026260137164));
#282419=CARTESIAN_POINT('Ctrl Pts',(-3.10606470275521,133.906246350121,
9.55948420107058));
#282420=CARTESIAN_POINT('Ctrl Pts',(-8.77395902407977E-14,134.056246350121,
10.5687058007695));
#282421=CARTESIAN_POINT('Ctrl Pts',(3.10606470275503,134.20624635012,9.55948420107058));
#282422=CARTESIAN_POINT('Ctrl Pts',(6.21212940551015,134.356246350119,8.55026260137164));
#282423=CARTESIAN_POINT('Ctrl Pts',(8.13178296306915,134.506246350119,5.90808615117925));
#282424=CARTESIAN_POINT('Ctrl Pts',(10.0514365206282,134.656246350118,3.26590970098687));
#282425=CARTESIAN_POINT('Ctrl Pts',(10.0514365206282,134.806246350118,-1.23094595618202E-15));
#282426=CARTESIAN_POINT('Ctrl Pts',(10.0514365206282,134.956246350117,-3.26590970098687));
#282427=CARTESIAN_POINT('Ctrl Pts',(8.13178296306915,135.106246350116,-5.90808615117926));
#282428=CARTESIAN_POINT('Ctrl Pts',(6.21212940551015,135.256246350116,-8.55026260137164));
#282429=CARTESIAN_POINT('Ctrl Pts',(3.10606470275503,135.406246350115,-9.55948420107058));
#282430=CARTESIAN_POINT('Ctrl Pts',(-9.11920312226371E-14,135.556246350115,
-10.5687058007695));
#282431=CARTESIAN_POINT('Ctrl Pts',(-3.10606470275521,135.706246350114,
-9.55948420107058));
#282432=CARTESIAN_POINT('Ctrl Pts',(-6.21212940551033,135.856246350113,
-8.55026260137164));
#282433=CARTESIAN_POINT('Ctrl Pts',(-8.13178296306934,136.006246350113,
-5.90808615117925));
#282434=CARTESIAN_POINT('Ctrl Pts',(-10.0514365206283,136.156246350112,
-3.26590970098687));
#282435=CARTESIAN_POINT('Ctrl Pts',(-10.0514365206283,136.306246350112,
2.46189191236404E-15));
#282436=CARTESIAN_POINT('Ctrl Pts',(-10.0514365206283,136.456246350111,
3.26590970098687));
#282437=CARTESIAN_POINT('Ctrl Pts',(-8.13178296306934,136.60624635011,5.90808615117926));
#282438=CARTESIAN_POINT('Ctrl Pts',(-6.21212940551033,136.75624635011,8.55026260137164));
#282439=CARTESIAN_POINT('Ctrl Pts',(-3.10606470275521,136.906246350109,
9.55948420107058));
#282440=CARTESIAN_POINT('Ctrl Pts',(-8.94672995124595E-14,137.056246350109,
10.5687058007695));
#282441=CARTESIAN_POINT('Ctrl Pts',(3.10606470275503,137.206246350108,9.55948420107058));
#282442=CARTESIAN_POINT('Ctrl Pts',(6.21212940551015,137.356246350107,8.55026260137164));
#282443=CARTESIAN_POINT('Ctrl Pts',(8.13178296306915,137.506246350107,5.90808615117925));
#282444=CARTESIAN_POINT('Ctrl Pts',(10.0514365206282,137.656246350106,3.26590970098687));
#282445=CARTESIAN_POINT('Ctrl Pts',(10.0514365206282,137.806246350106,-1.23094595618202E-15));
#282446=CARTESIAN_POINT('Ctrl Pts',(10.0514365206282,137.956246350105,-3.26590970098687));
#282447=CARTESIAN_POINT('Ctrl Pts',(8.13178296306915,138.106246350104,-5.90808615117926));
#282448=CARTESIAN_POINT('Ctrl Pts',(6.21212940551015,138.256246350104,-8.55026260137164));
#282449=CARTESIAN_POINT('Ctrl Pts',(3.10606470275503,138.406246350103,-9.55948420107058));
#282450=CARTESIAN_POINT('Ctrl Pts',(-9.29197404942989E-14,138.556246350103,
-10.5687058007695));
#282451=CARTESIAN_POINT('Ctrl Pts',(-3.10606470275521,138.706246350102,
-9.55948420107058));
#282452=CARTESIAN_POINT('Ctrl Pts',(-6.21212940551033,138.856246350101,
-8.55026260137164));
#282453=CARTESIAN_POINT('Ctrl Pts',(-8.13178296306934,139.006246350101,
-5.90808615117925));
#282454=CARTESIAN_POINT('Ctrl Pts',(-10.0514365206283,139.1562463501,-3.26590970098687));
#282455=CARTESIAN_POINT('Ctrl Pts',(-10.0514365206283,139.3062463501,2.46189191236404E-15));
#282456=CARTESIAN_POINT('Ctrl Pts',(-10.0514365206283,139.456246350099,
3.26590970098687));
#282457=CARTESIAN_POINT('Ctrl Pts',(-8.13178296306934,139.606246350098,
5.90808615117926));
#282458=CARTESIAN_POINT('Ctrl Pts',(-6.21212940551033,139.756246350098,
8.55026260137164));
#282459=CARTESIAN_POINT('Ctrl Pts',(-3.10606470275521,139.906246350097,
9.55948420107058));
#282460=CARTESIAN_POINT('Ctrl Pts',(-9.11950087841213E-14,140.056246350097,
10.5687058007695));
#282461=CARTESIAN_POINT('Ctrl Pts',(3.10606470275503,140.206246350096,9.55948420107058));
#282462=CARTESIAN_POINT('Ctrl Pts',(6.21212940551015,140.356246350095,8.55026260137164));
#282463=CARTESIAN_POINT('Ctrl Pts',(8.13178296306915,140.506246350095,5.90808615117925));
#282464=CARTESIAN_POINT('Ctrl Pts',(10.0514365206282,140.656246350094,3.26590970098687));
#282465=CARTESIAN_POINT('Ctrl Pts',(10.0514365206282,140.806246350094,-1.23094595618202E-15));
#282466=CARTESIAN_POINT('Ctrl Pts',(10.0514365206282,140.956246350093,-3.26590970098687));
#282467=CARTESIAN_POINT('Ctrl Pts',(8.13178296306915,141.106246350092,-5.90808615117926));
#282468=CARTESIAN_POINT('Ctrl Pts',(6.21212940551015,141.256246350092,-8.55026260137164));
#282469=CARTESIAN_POINT('Ctrl Pts',(3.10606470275503,141.406246350091,-9.55948420107058));
#282470=CARTESIAN_POINT('Ctrl Pts',(-9.46474497659607E-14,141.556246350091,
-10.5687058007695));
#282471=CARTESIAN_POINT('Ctrl Pts',(-3.10606470275522,141.70624635009,-9.55948420107058));
#282472=CARTESIAN_POINT('Ctrl Pts',(-6.21212940551034,141.856246350089,
-8.55026260137164));
#282473=CARTESIAN_POINT('Ctrl Pts',(-8.13178296306934,142.006246350089,
-5.90808615117925));
#282474=CARTESIAN_POINT('Ctrl Pts',(-10.0514365206283,142.156246350088,
-3.26590970098687));
#282475=CARTESIAN_POINT('Ctrl Pts',(-10.0514365206283,142.306246350088,
2.46189191236404E-15));
#282476=CARTESIAN_POINT('Ctrl Pts',(-10.0514365206283,142.456246350087,
3.26590970098687));
#282477=CARTESIAN_POINT('Ctrl Pts',(-8.13178296306934,142.606246350086,
5.90808615117926));
#282478=CARTESIAN_POINT('Ctrl Pts',(-6.21212940551033,142.756246350086,
8.55026260137164));
#282479=CARTESIAN_POINT('Ctrl Pts',(-3.10606470275521,142.906246350085,
9.55948420107058));
#282480=CARTESIAN_POINT('Ctrl Pts',(-9.29227180557832E-14,143.056246350085,
10.5687058007695));
#282481=CARTESIAN_POINT('Ctrl Pts',(3.10606470275503,143.206246350084,9.55948420107058));
#282482=CARTESIAN_POINT('Ctrl Pts',(6.21212940551015,143.356246350083,8.55026260137164));
#282483=CARTESIAN_POINT('Ctrl Pts',(8.13178296306915,143.506246350083,5.90808615117925));
#282484=CARTESIAN_POINT('Ctrl Pts',(10.0514365206282,143.656246350082,3.26590970098687));
#282485=CARTESIAN_POINT('Ctrl Pts',(10.0514365206282,143.806246350082,-1.23094595618202E-15));
#282486=CARTESIAN_POINT('Ctrl Pts',(10.0514365206282,143.956246350081,-3.26590970098687));
#282487=CARTESIAN_POINT('Ctrl Pts',(8.13178296306915,144.10624635008,-5.90808615117926));
#282488=CARTESIAN_POINT('Ctrl Pts',(6.21212940551015,144.25624635008,-8.55026260137164));
#282489=CARTESIAN_POINT('Ctrl Pts',(3.10606470275502,144.406246350079,-9.55948420107058));
#282490=CARTESIAN_POINT('Ctrl Pts',(-9.63751590376226E-14,144.556246350079,
-10.5687058007695));
#282491=CARTESIAN_POINT('Ctrl Pts',(-3.10606470275522,144.706246350078,
-9.55948420107058));
#282492=CARTESIAN_POINT('Ctrl Pts',(-6.21212940551034,144.856246350077,
-8.55026260137164));
#282493=CARTESIAN_POINT('Ctrl Pts',(-8.13178296306934,145.006246350077,
-5.90808615117925));
#282494=CARTESIAN_POINT('Ctrl Pts',(-10.0514365206283,145.156246350076,
-3.26590970098687));
#282495=CARTESIAN_POINT('Ctrl Pts',(-10.0514365206283,145.306246350076,
2.46189191236404E-15));
#282496=CARTESIAN_POINT('Ctrl Pts',(-10.0514365206283,145.456246350075,
3.26590970098687));
#282497=CARTESIAN_POINT('Ctrl Pts',(-8.13178296306934,145.606246350074,
5.90808615117926));
#282498=CARTESIAN_POINT('Ctrl Pts',(-6.21212940551034,145.756246350074,
8.55026260137164));
#282499=CARTESIAN_POINT('Ctrl Pts',(-3.10606470275522,145.906246350073,
9.55948420107058));
#282500=CARTESIAN_POINT('Ctrl Pts',(-9.4650427327445E-14,146.056246350073,
10.5687058007695));
#282501=CARTESIAN_POINT('Ctrl Pts',(3.10606470275503,146.206246350072,9.55948420107058));
#282502=CARTESIAN_POINT('Ctrl Pts',(6.21212940551015,146.356246350071,8.55026260137164));
#282503=CARTESIAN_POINT('Ctrl Pts',(8.13178296306915,146.506246350071,5.90808615117925));
#282504=CARTESIAN_POINT('Ctrl Pts',(10.0514365206282,146.65624635007,3.26590970098687));
#282505=CARTESIAN_POINT('Ctrl Pts',(10.0514365206281,146.80624635007,-1.23094595618202E-15));
#282506=CARTESIAN_POINT('Ctrl Pts',(10.0514365206282,146.956246350069,-3.26590970098687));
#282507=CARTESIAN_POINT('Ctrl Pts',(8.13178296306915,147.106246350068,-5.90808615117926));
#282508=CARTESIAN_POINT('Ctrl Pts',(6.21212940551014,147.256246350068,-8.55026260137164));
#282509=CARTESIAN_POINT('Ctrl Pts',(3.10606470275502,147.406246350067,-9.55948420107058));
#282510=CARTESIAN_POINT('Ctrl Pts',(-9.81028683092844E-14,147.556246350067,
-10.5687058007695));
#282511=CARTESIAN_POINT('Ctrl Pts',(-3.10606470275522,147.706246350066,
-9.55948420107058));
#282512=CARTESIAN_POINT('Ctrl Pts',(-6.21212940551034,147.856246350065,
-8.55026260137164));
#282513=CARTESIAN_POINT('Ctrl Pts',(-8.13178296306934,148.006246350065,
-5.90808615117925));
#282514=CARTESIAN_POINT('Ctrl Pts',(-10.0514365206283,148.156246350064,
-3.26590970098687));
#282515=CARTESIAN_POINT('Ctrl Pts',(-10.0514365206283,148.306246350064,
2.46189191236404E-15));
#282516=CARTESIAN_POINT('Ctrl Pts',(-10.0514365206283,148.456246350063,
3.26590970098687));
#282517=CARTESIAN_POINT('Ctrl Pts',(-8.13178296306934,148.606246350062,
5.90808615117926));
#282518=CARTESIAN_POINT('Ctrl Pts',(-6.21212940551034,148.756246350062,
8.55026260137164));
#282519=CARTESIAN_POINT('Ctrl Pts',(-3.10606470275522,148.906246350061,
9.55948420107058));
#282520=CARTESIAN_POINT('Ctrl Pts',(-9.63781365991068E-14,149.056246350061,
10.5687058007695));
#282521=CARTESIAN_POINT('Ctrl Pts',(3.10606470275502,149.20624635006,9.55948420107058));
#282522=CARTESIAN_POINT('Ctrl Pts',(6.21212940551015,149.356246350059,8.55026260137164));
#282523=CARTESIAN_POINT('Ctrl Pts',(8.13178296306915,149.506246350059,5.90808615117925));
#282524=CARTESIAN_POINT('Ctrl Pts',(10.0514365206282,149.656246350058,3.26590970098687));
#282525=CARTESIAN_POINT('Ctrl Pts',(10.0514365206281,149.806246350058,-1.23094595618202E-15));
#282526=CARTESIAN_POINT('Ctrl Pts',(10.0514365206281,149.956246350057,-3.26590970098687));
#282527=CARTESIAN_POINT('Ctrl Pts',(8.13178296306915,150.106246350056,-5.90808615117926));
#282528=CARTESIAN_POINT('Ctrl Pts',(6.21212940551014,150.256246350056,-8.55026260137164));
#282529=CARTESIAN_POINT('Ctrl Pts',(3.10606470275502,150.406246350055,-9.55948420107058));
#282530=CARTESIAN_POINT('Ctrl Pts',(-9.98305775809463E-14,150.556246350055,
-10.5687058007695));
#282531=CARTESIAN_POINT('Ctrl Pts',(-3.10606470275522,150.706246350054,
-9.55948420107058));
#282532=CARTESIAN_POINT('Ctrl Pts',(-6.21212940551034,150.856246350053,
-8.55026260137164));
#282533=CARTESIAN_POINT('Ctrl Pts',(-8.13178296306935,151.006246350053,
-5.90808615117925));
#282534=CARTESIAN_POINT('Ctrl Pts',(-10.0514365206283,151.156246350052,
-3.26590970098687));
#282535=CARTESIAN_POINT('Ctrl Pts',(-10.0514365206284,151.306246350052,
2.46189191236404E-15));
#282536=CARTESIAN_POINT('Ctrl Pts',(-10.0514365206283,151.456246350051,
3.26590970098687));
#282537=CARTESIAN_POINT('Ctrl Pts',(-8.13178296306935,151.60624635005,5.90808615117926));
#282538=CARTESIAN_POINT('Ctrl Pts',(-6.21212940551034,151.75624635005,8.55026260137164));
#282539=CARTESIAN_POINT('Ctrl Pts',(-3.10606470275522,151.906246350049,
9.55948420107058));
#282540=CARTESIAN_POINT('Ctrl Pts',(-9.81058458707687E-14,152.056246350049,
10.5687058007695));
#282541=CARTESIAN_POINT('Ctrl Pts',(3.10606470275502,152.206246350048,9.55948420107058));
#282542=CARTESIAN_POINT('Ctrl Pts',(6.21212940551014,152.356246350047,8.55026260137164));
#282543=CARTESIAN_POINT('Ctrl Pts',(8.13178296306915,152.506246350047,5.90808615117925));
#282544=CARTESIAN_POINT('Ctrl Pts',(10.0514365206281,152.656246350046,3.26590970098687));
#282545=CARTESIAN_POINT('Ctrl Pts',(10.0514365206281,152.806246350046,-1.23094595618202E-15));
#282546=CARTESIAN_POINT('Ctrl Pts',(10.0514365206281,152.956246350045,-3.26590970098687));
#282547=CARTESIAN_POINT('Ctrl Pts',(8.13178296306915,153.106246350044,-5.90808615117926));
#282548=CARTESIAN_POINT('Ctrl Pts',(6.21212940551014,153.256246350044,-8.55026260137164));
#282549=CARTESIAN_POINT('Ctrl Pts',(3.10606470275502,153.406246350043,-9.55948420107058));
#282550=CARTESIAN_POINT('Ctrl Pts',(-1.01558286852608E-13,153.556246350043,
-10.5687058007695));
#282551=CARTESIAN_POINT('Ctrl Pts',(-3.10606470275522,153.706246350042,
-9.55948420107058));
#282552=CARTESIAN_POINT('Ctrl Pts',(-12.1623797632097,-0.474999999988005,
2.97892388940585E-15));
#282553=CARTESIAN_POINT('Ctrl Pts',(-12.1623797632096,-0.324999999988605,
3.95179673813133));
#282554=CARTESIAN_POINT('Ctrl Pts',(-9.83957192047856,-0.174999999989203,
7.14886745759505));
#282555=CARTESIAN_POINT('Ctrl Pts',(-7.51676407774747,-0.0249999999898023,
10.3459381770588));
#282556=CARTESIAN_POINT('Ctrl Pts',(-3.75838203887374,0.1250000000096,11.5671105274568));
#282557=CARTESIAN_POINT('Ctrl Pts',(-1.02868273148643E-14,0.275000000009002,
12.7882828778549));
#282558=CARTESIAN_POINT('Ctrl Pts',(3.75838203887372,0.425000000008404,
11.5671105274568));
#282559=CARTESIAN_POINT('Ctrl Pts',(7.51676407774745,0.575000000007806,
10.3459381770588));
#282560=CARTESIAN_POINT('Ctrl Pts',(9.83957192047854,0.725000000007208,
7.14886745759505));
#282561=CARTESIAN_POINT('Ctrl Pts',(12.1623797632096,0.875000000006609,
3.95179673813132));
#282562=CARTESIAN_POINT('Ctrl Pts',(12.1623797632096,1.02500000000601,-1.48946194470292E-15));
#282563=CARTESIAN_POINT('Ctrl Pts',(12.1623797632096,1.17500000000541,-3.95179673813132));
#282564=CARTESIAN_POINT('Ctrl Pts',(9.83957192047853,1.32500000000481,-7.14886745759505));
#282565=CARTESIAN_POINT('Ctrl Pts',(7.51676407774744,1.47500000000421,-10.3459381770588));
#282566=CARTESIAN_POINT('Ctrl Pts',(3.75838203887371,1.6250000000036,-11.5671105274568));
#282567=CARTESIAN_POINT('Ctrl Pts',(-1.42829078892864E-14,1.775000000003,
-12.7882828778549));
#282568=CARTESIAN_POINT('Ctrl Pts',(-3.75838203887374,1.9250000000024,-11.5671105274568));
#282569=CARTESIAN_POINT('Ctrl Pts',(-7.51676407774747,2.0750000000018,-10.3459381770588));
#282570=CARTESIAN_POINT('Ctrl Pts',(-9.83957192047856,2.2250000000012,-7.14886745759505));
#282571=CARTESIAN_POINT('Ctrl Pts',(-12.1623797632097,2.37500000000059,
-3.95179673813132));
#282572=CARTESIAN_POINT('Ctrl Pts',(-12.1623797632097,2.525,2.97892388940585E-15));
#282573=CARTESIAN_POINT('Ctrl Pts',(-12.1623797632097,2.6749999999994,3.95179673813133));
#282574=CARTESIAN_POINT('Ctrl Pts',(-9.83957192047856,2.8249999999988,7.14886745759505));
#282575=CARTESIAN_POINT('Ctrl Pts',(-7.51676407774747,2.9749999999982,10.3459381770588));
#282576=CARTESIAN_POINT('Ctrl Pts',(-3.75838203887374,3.1249999999976,11.5671105274568));
#282577=CARTESIAN_POINT('Ctrl Pts',(-1.20145365865262E-14,3.274999999997,
12.7882828778549));
#282578=CARTESIAN_POINT('Ctrl Pts',(3.75838203887372,3.4249999999964,11.5671105274568));
#282579=CARTESIAN_POINT('Ctrl Pts',(7.51676407774744,3.57499999999581,10.3459381770588));
#282580=CARTESIAN_POINT('Ctrl Pts',(9.83957192047853,3.72499999999521,7.14886745759505));
#282581=CARTESIAN_POINT('Ctrl Pts',(12.1623797632096,3.87499999999461,3.95179673813132));
#282582=CARTESIAN_POINT('Ctrl Pts',(12.1623797632096,4.02499999999401,-1.48946194470292E-15));
#282583=CARTESIAN_POINT('Ctrl Pts',(12.1623797632096,4.17499999999341,-3.95179673813132));
#282584=CARTESIAN_POINT('Ctrl Pts',(9.83957192047853,4.32499999999281,-7.14886745759505));
#282585=CARTESIAN_POINT('Ctrl Pts',(7.51676407774744,4.47499999999221,-10.3459381770588));
#282586=CARTESIAN_POINT('Ctrl Pts',(3.75838203887371,4.6249999999916,-11.5671105274568));
#282587=CARTESIAN_POINT('Ctrl Pts',(-1.60106171609483E-14,4.774999999991,
-12.7882828778549));
#282588=CARTESIAN_POINT('Ctrl Pts',(-3.75838203887374,4.9249999999904,-11.5671105274568));
#282589=CARTESIAN_POINT('Ctrl Pts',(-7.51676407774747,5.0749999999898,-10.3459381770588));
#282590=CARTESIAN_POINT('Ctrl Pts',(-9.83957192047857,5.2249999999892,-7.14886745759505));
#282591=CARTESIAN_POINT('Ctrl Pts',(-12.1623797632097,5.3749999999886,-3.95179673813132));
#282592=CARTESIAN_POINT('Ctrl Pts',(-12.1623797632097,5.52499999998799,
2.97892388940585E-15));
#282593=CARTESIAN_POINT('Ctrl Pts',(-12.1623797632097,5.67499999998739,
3.95179673813133));
#282594=CARTESIAN_POINT('Ctrl Pts',(-9.83957192047857,5.8249999999868,7.14886745759505));
#282595=CARTESIAN_POINT('Ctrl Pts',(-7.51676407774747,5.9749999999862,10.3459381770588));
#282596=CARTESIAN_POINT('Ctrl Pts',(-3.75838203887374,6.1249999999856,11.5671105274568));
#282597=CARTESIAN_POINT('Ctrl Pts',(-1.3742245858188E-14,6.274999999985,
12.7882828778549));
#282598=CARTESIAN_POINT('Ctrl Pts',(3.75838203887371,6.4249999999844,11.5671105274568));
#282599=CARTESIAN_POINT('Ctrl Pts',(7.51676407774744,6.57499999998381,10.3459381770588));
#282600=CARTESIAN_POINT('Ctrl Pts',(9.83957192047853,6.72499999998321,7.14886745759505));
#282601=CARTESIAN_POINT('Ctrl Pts',(12.1623797632096,6.87499999998261,3.95179673813132));
#282602=CARTESIAN_POINT('Ctrl Pts',(12.1623797632096,7.02499999998201,-1.48946194470292E-15));
#282603=CARTESIAN_POINT('Ctrl Pts',(12.1623797632096,7.17499999998141,-3.95179673813132));
#282604=CARTESIAN_POINT('Ctrl Pts',(9.83957192047853,7.32499999998081,-7.14886745759505));
#282605=CARTESIAN_POINT('Ctrl Pts',(7.51676407774744,7.47499999998021,-10.3459381770588));
#282606=CARTESIAN_POINT('Ctrl Pts',(3.75838203887371,7.6249999999796,-11.5671105274568));
#282607=CARTESIAN_POINT('Ctrl Pts',(-1.77383264326101E-14,7.774999999979,
-12.7882828778549));
#282608=CARTESIAN_POINT('Ctrl Pts',(-3.75838203887375,7.9249999999784,-11.5671105274568));
#282609=CARTESIAN_POINT('Ctrl Pts',(-7.51676407774747,8.0749999999778,-10.3459381770588));
#282610=CARTESIAN_POINT('Ctrl Pts',(-9.83957192047857,8.2249999999772,-7.14886745759505));
#282611=CARTESIAN_POINT('Ctrl Pts',(-12.1623797632097,8.3749999999766,-3.95179673813132));
#282612=CARTESIAN_POINT('Ctrl Pts',(-12.1623797632097,8.52499999997599,
2.97892388940585E-15));
#282613=CARTESIAN_POINT('Ctrl Pts',(-12.1623797632097,8.6749999999754,3.95179673813133));
#282614=CARTESIAN_POINT('Ctrl Pts',(-9.83957192047857,8.8249999999748,7.14886745759505));
#282615=CARTESIAN_POINT('Ctrl Pts',(-7.51676407774747,8.9749999999742,10.3459381770588));
#282616=CARTESIAN_POINT('Ctrl Pts',(-3.75838203887374,9.1249999999736,11.5671105274568));
#282617=CARTESIAN_POINT('Ctrl Pts',(-1.54699551298498E-14,9.274999999973,
12.7882828778549));
#282618=CARTESIAN_POINT('Ctrl Pts',(3.75838203887371,9.4249999999724,11.5671105274568));
#282619=CARTESIAN_POINT('Ctrl Pts',(7.51676407774744,9.57499999997181,10.3459381770588));
#282620=CARTESIAN_POINT('Ctrl Pts',(9.83957192047853,9.72499999997121,7.14886745759505));
#282621=CARTESIAN_POINT('Ctrl Pts',(12.1623797632096,9.87499999997061,3.95179673813132));
#282622=CARTESIAN_POINT('Ctrl Pts',(12.1623797632096,10.02499999997,-1.48946194470292E-15));
#282623=CARTESIAN_POINT('Ctrl Pts',(12.1623797632096,10.1749999999694,-3.95179673813132));
#282624=CARTESIAN_POINT('Ctrl Pts',(9.83957192047853,10.3249999999688,-7.14886745759505));
#282625=CARTESIAN_POINT('Ctrl Pts',(7.51676407774744,10.4749999999682,-10.3459381770588));
#282626=CARTESIAN_POINT('Ctrl Pts',(3.75838203887371,10.6249999999676,-11.5671105274568));
#282627=CARTESIAN_POINT('Ctrl Pts',(-1.9466035704272E-14,10.774999999967,
-12.7882828778549));
#282628=CARTESIAN_POINT('Ctrl Pts',(-3.75838203887375,10.9249999999664,
-11.5671105274568));
#282629=CARTESIAN_POINT('Ctrl Pts',(-7.51676407774748,11.0749999999658,
-10.3459381770588));
#282630=CARTESIAN_POINT('Ctrl Pts',(-9.83957192047857,11.2249999999652,
-7.14886745759505));
#282631=CARTESIAN_POINT('Ctrl Pts',(-12.1623797632097,11.3749999999646,
-3.95179673813132));
#282632=CARTESIAN_POINT('Ctrl Pts',(-12.1623797632097,11.524999999964,2.97892388940585E-15));
#282633=CARTESIAN_POINT('Ctrl Pts',(-12.1623797632097,11.6749999999634,
3.95179673813133));
#282634=CARTESIAN_POINT('Ctrl Pts',(-9.83957192047857,11.8249999999628,
7.14886745759505));
#282635=CARTESIAN_POINT('Ctrl Pts',(-7.51676407774747,11.9749999999622,
10.3459381770588));
#282636=CARTESIAN_POINT('Ctrl Pts',(-3.75838203887375,12.1249999999616,
11.5671105274568));
#282637=CARTESIAN_POINT('Ctrl Pts',(-1.71976644015117E-14,12.274999999961,
12.7882828778549));
#282638=CARTESIAN_POINT('Ctrl Pts',(3.75838203887371,12.4249999999604,11.5671105274568));
#282639=CARTESIAN_POINT('Ctrl Pts',(7.51676407774744,12.5749999999598,10.3459381770588));
#282640=CARTESIAN_POINT('Ctrl Pts',(9.83957192047853,12.7249999999592,7.14886745759505));
#282641=CARTESIAN_POINT('Ctrl Pts',(12.1623797632096,12.8749999999586,3.95179673813132));
#282642=CARTESIAN_POINT('Ctrl Pts',(12.1623797632096,13.024999999958,-1.48946194470292E-15));
#282643=CARTESIAN_POINT('Ctrl Pts',(12.1623797632096,13.1749999999574,-3.95179673813132));
#282644=CARTESIAN_POINT('Ctrl Pts',(9.83957192047853,13.3249999999568,-7.14886745759505));
#282645=CARTESIAN_POINT('Ctrl Pts',(7.51676407774743,13.4749999999562,-10.3459381770588));
#282646=CARTESIAN_POINT('Ctrl Pts',(3.75838203887371,13.6249999999556,-11.5671105274568));
#282647=CARTESIAN_POINT('Ctrl Pts',(-2.11937449759338E-14,13.774999999955,
-12.7882828778549));
#282648=CARTESIAN_POINT('Ctrl Pts',(-3.75838203887375,13.9249999999544,
-11.5671105274568));
#282649=CARTESIAN_POINT('Ctrl Pts',(-7.51676407774748,14.0749999999538,
-10.3459381770588));
#282650=CARTESIAN_POINT('Ctrl Pts',(-9.83957192047857,14.2249999999532,
-7.14886745759505));
#282651=CARTESIAN_POINT('Ctrl Pts',(-12.1623797632097,14.3749999999526,
-3.95179673813132));
#282652=CARTESIAN_POINT('Ctrl Pts',(-12.1623797632097,14.524999999952,2.97892388940585E-15));
#282653=CARTESIAN_POINT('Ctrl Pts',(-12.1623797632097,14.6749999999514,
3.95179673813133));
#282654=CARTESIAN_POINT('Ctrl Pts',(-9.83957192047857,14.8249999999508,
7.14886745759505));
#282655=CARTESIAN_POINT('Ctrl Pts',(-7.51676407774747,14.9749999999502,
10.3459381770588));
#282656=CARTESIAN_POINT('Ctrl Pts',(-3.75838203887375,15.1249999999496,
11.5671105274568));
#282657=CARTESIAN_POINT('Ctrl Pts',(-1.89253736731735E-14,15.274999999949,
12.7882828778549));
#282658=CARTESIAN_POINT('Ctrl Pts',(3.75838203887371,15.4249999999484,11.5671105274568));
#282659=CARTESIAN_POINT('Ctrl Pts',(7.51676407774744,15.5749999999478,10.3459381770588));
#282660=CARTESIAN_POINT('Ctrl Pts',(9.83957192047853,15.7249999999472,7.14886745759505));
#282661=CARTESIAN_POINT('Ctrl Pts',(12.1623797632096,15.8749999999466,3.95179673813132));
#282662=CARTESIAN_POINT('Ctrl Pts',(12.1623797632096,16.024999999946,-1.48946194470292E-15));
#282663=CARTESIAN_POINT('Ctrl Pts',(12.1623797632096,16.1749999999454,-3.95179673813132));
#282664=CARTESIAN_POINT('Ctrl Pts',(9.83957192047852,16.3249999999448,-7.14886745759505));
#282665=CARTESIAN_POINT('Ctrl Pts',(7.51676407774743,16.4749999999442,-10.3459381770588));
#282666=CARTESIAN_POINT('Ctrl Pts',(3.7583820388737,16.6249999999436,-11.5671105274568));
#282667=CARTESIAN_POINT('Ctrl Pts',(-2.29214542475956E-14,16.774999999943,
-12.7882828778549));
#282668=CARTESIAN_POINT('Ctrl Pts',(-3.75838203887375,16.9249999999424,
-11.5671105274568));
#282669=CARTESIAN_POINT('Ctrl Pts',(-7.51676407774748,17.0749999999418,
-10.3459381770588));
#282670=CARTESIAN_POINT('Ctrl Pts',(-9.83957192047857,17.2249999999412,
-7.14886745759505));
#282671=CARTESIAN_POINT('Ctrl Pts',(-12.1623797632097,17.3749999999406,
-3.95179673813132));
#282672=CARTESIAN_POINT('Ctrl Pts',(-12.1623797632097,17.52499999994,2.97892388940585E-15));
#282673=CARTESIAN_POINT('Ctrl Pts',(-12.1623797632097,17.6749999999394,
3.95179673813133));
#282674=CARTESIAN_POINT('Ctrl Pts',(-9.83957192047857,17.8249999999388,
7.14886745759505));
#282675=CARTESIAN_POINT('Ctrl Pts',(-7.51676407774748,17.9749999999382,
10.3459381770588));
#282676=CARTESIAN_POINT('Ctrl Pts',(-3.75838203887375,18.1249999999376,
11.5671105274568));
#282677=CARTESIAN_POINT('Ctrl Pts',(-2.06530829448354E-14,18.274999999937,
12.7882828778549));
#282678=CARTESIAN_POINT('Ctrl Pts',(3.75838203887371,18.4249999999364,11.5671105274568));
#282679=CARTESIAN_POINT('Ctrl Pts',(7.51676407774743,18.5749999999358,10.3459381770588));
#282680=CARTESIAN_POINT('Ctrl Pts',(9.83957192047852,18.7249999999352,7.14886745759505));
#282681=CARTESIAN_POINT('Ctrl Pts',(12.1623797632096,18.8749999999346,3.95179673813132));
#282682=CARTESIAN_POINT('Ctrl Pts',(12.1623797632096,19.024999999934,-1.48946194470292E-15));
#282683=CARTESIAN_POINT('Ctrl Pts',(12.1623797632096,19.1749999999334,-3.95179673813132));
#282684=CARTESIAN_POINT('Ctrl Pts',(9.83957192047852,19.3249999999328,-7.14886745759505));
#282685=CARTESIAN_POINT('Ctrl Pts',(7.51676407774743,19.4749999999322,-10.3459381770588));
#282686=CARTESIAN_POINT('Ctrl Pts',(3.7583820388737,19.6249999999316,-11.5671105274568));
#282687=CARTESIAN_POINT('Ctrl Pts',(-2.46491635192575E-14,19.774999999931,
-12.7882828778549));
#282688=CARTESIAN_POINT('Ctrl Pts',(-3.75838203887375,19.9249999999304,
-11.5671105274568));
#282689=CARTESIAN_POINT('Ctrl Pts',(-7.51676407774748,20.0749999999298,
-10.3459381770588));
#282690=CARTESIAN_POINT('Ctrl Pts',(-9.83957192047857,20.2249999999292,
-7.14886745759505));
#282691=CARTESIAN_POINT('Ctrl Pts',(-12.1623797632097,20.3749999999286,
-3.95179673813132));
#282692=CARTESIAN_POINT('Ctrl Pts',(-12.1623797632097,20.524999999928,2.97892388940585E-15));
#282693=CARTESIAN_POINT('Ctrl Pts',(-12.1623797632097,20.6749999999274,
3.95179673813133));
#282694=CARTESIAN_POINT('Ctrl Pts',(-9.83957192047857,20.8249999999268,
7.14886745759505));
#282695=CARTESIAN_POINT('Ctrl Pts',(-7.51676407774748,20.9749999999262,
10.3459381770588));
#282696=CARTESIAN_POINT('Ctrl Pts',(-3.75838203887375,21.1249999999256,
11.5671105274568));
#282697=CARTESIAN_POINT('Ctrl Pts',(-2.23807922164972E-14,21.274999999925,
12.7882828778549));
#282698=CARTESIAN_POINT('Ctrl Pts',(3.7583820388737,21.4249999999244,11.5671105274568));
#282699=CARTESIAN_POINT('Ctrl Pts',(7.51676407774743,21.5749999999238,10.3459381770588));
#282700=CARTESIAN_POINT('Ctrl Pts',(9.83957192047852,21.7249999999232,7.14886745759505));
#282701=CARTESIAN_POINT('Ctrl Pts',(12.1623797632096,21.8749999999226,3.95179673813132));
#282702=CARTESIAN_POINT('Ctrl Pts',(12.1623797632096,22.024999999922,-1.48946194470292E-15));
#282703=CARTESIAN_POINT('Ctrl Pts',(12.1623797632096,22.1749999999214,-3.95179673813132));
#282704=CARTESIAN_POINT('Ctrl Pts',(9.83957192047852,22.3249999999208,-7.14886745759505));
#282705=CARTESIAN_POINT('Ctrl Pts',(7.51676407774743,22.4749999999202,-10.3459381770588));
#282706=CARTESIAN_POINT('Ctrl Pts',(3.7583820388737,22.6249999999196,-11.5671105274568));
#282707=CARTESIAN_POINT('Ctrl Pts',(-2.63768727909193E-14,22.774999999919,
-12.7882828778549));
#282708=CARTESIAN_POINT('Ctrl Pts',(-3.75838203887375,22.9249999999184,
-11.5671105274568));
#282709=CARTESIAN_POINT('Ctrl Pts',(-7.51676407774748,23.0749999999178,
-10.3459381770588));
#282710=CARTESIAN_POINT('Ctrl Pts',(-9.83957192047857,23.2249999999172,
-7.14886745759505));
#282711=CARTESIAN_POINT('Ctrl Pts',(-12.1623797632097,23.3749999999166,
-3.95179673813132));
#282712=CARTESIAN_POINT('Ctrl Pts',(-12.1623797632097,23.524999999916,2.97892388940585E-15));
#282713=CARTESIAN_POINT('Ctrl Pts',(-12.1623797632097,23.6749999999154,
3.95179673813133));
#282714=CARTESIAN_POINT('Ctrl Pts',(-9.83957192047857,23.8249999999148,
7.14886745759505));
#282715=CARTESIAN_POINT('Ctrl Pts',(-7.51676407774748,23.9749999999142,
10.3459381770588));
#282716=CARTESIAN_POINT('Ctrl Pts',(-3.75838203887375,24.1249999999136,
11.5671105274568));
#282717=CARTESIAN_POINT('Ctrl Pts',(-2.4108501488159E-14,24.274999999913,
12.7882828778549));
#282718=CARTESIAN_POINT('Ctrl Pts',(3.7583820388737,24.4249999999124,11.5671105274568));
#282719=CARTESIAN_POINT('Ctrl Pts',(7.51676407774743,24.5749999999118,10.3459381770588));
#282720=CARTESIAN_POINT('Ctrl Pts',(9.83957192047852,24.7249999999112,7.14886745759505));
#282721=CARTESIAN_POINT('Ctrl Pts',(12.1623797632096,24.8749999999106,3.95179673813132));
#282722=CARTESIAN_POINT('Ctrl Pts',(12.1623797632096,25.02499999991,-1.48946194470292E-15));
#282723=CARTESIAN_POINT('Ctrl Pts',(12.1623797632096,25.1749999999094,-3.95179673813132));
#282724=CARTESIAN_POINT('Ctrl Pts',(9.83957192047852,25.3249999999088,-7.14886745759505));
#282725=CARTESIAN_POINT('Ctrl Pts',(7.51676407774743,25.4749999999082,-10.3459381770588));
#282726=CARTESIAN_POINT('Ctrl Pts',(3.7583820388737,25.6249999999076,-11.5671105274568));
#282727=CARTESIAN_POINT('Ctrl Pts',(-2.81045820625811E-14,25.774999999907,
-12.7882828778549));
#282728=CARTESIAN_POINT('Ctrl Pts',(-3.75838203887376,25.9249999999064,
-11.5671105274568));
#282729=CARTESIAN_POINT('Ctrl Pts',(-7.51676407774749,26.0749999999058,
-10.3459381770588));
#282730=CARTESIAN_POINT('Ctrl Pts',(-9.83957192047857,26.2249999999052,
-7.14886745759505));
#282731=CARTESIAN_POINT('Ctrl Pts',(-12.1623797632097,26.3749999999046,
-3.95179673813132));
#282732=CARTESIAN_POINT('Ctrl Pts',(-12.1623797632097,26.524999999904,2.97892388940585E-15));
#282733=CARTESIAN_POINT('Ctrl Pts',(-12.1623797632097,26.6749999999034,
3.95179673813133));
#282734=CARTESIAN_POINT('Ctrl Pts',(-9.83957192047857,26.8249999999028,
7.14886745759505));
#282735=CARTESIAN_POINT('Ctrl Pts',(-7.51676407774748,26.9749999999022,
10.3459381770588));
#282736=CARTESIAN_POINT('Ctrl Pts',(-3.75838203887375,27.1249999999016,
11.5671105274568));
#282737=CARTESIAN_POINT('Ctrl Pts',(-2.58362107598209E-14,27.274999999901,
12.7882828778549));
#282738=CARTESIAN_POINT('Ctrl Pts',(3.7583820388737,27.4249999999004,11.5671105274568));
#282739=CARTESIAN_POINT('Ctrl Pts',(7.51676407774743,27.5749999998998,10.3459381770588));
#282740=CARTESIAN_POINT('Ctrl Pts',(9.83957192047852,27.7249999998992,7.14886745759505));
#282741=CARTESIAN_POINT('Ctrl Pts',(12.1623797632096,27.8749999998986,3.95179673813132));
#282742=CARTESIAN_POINT('Ctrl Pts',(12.1623797632096,28.024999999898,-1.48946194470292E-15));
#282743=CARTESIAN_POINT('Ctrl Pts',(12.1623797632096,28.1749999998974,-3.95179673813132));
#282744=CARTESIAN_POINT('Ctrl Pts',(9.83957192047852,28.3249999998968,-7.14886745759505));
#282745=CARTESIAN_POINT('Ctrl Pts',(7.51676407774743,28.4749999998962,-10.3459381770588));
#282746=CARTESIAN_POINT('Ctrl Pts',(3.7583820388737,28.6249999998956,-11.5671105274568));
#282747=CARTESIAN_POINT('Ctrl Pts',(-2.9832291334243E-14,28.774999999895,
-12.7882828778549));
#282748=CARTESIAN_POINT('Ctrl Pts',(-3.75838203887376,28.9249999998944,
-11.5671105274568));
#282749=CARTESIAN_POINT('Ctrl Pts',(-7.51676407774749,29.0749999998938,
-10.3459381770588));
#282750=CARTESIAN_POINT('Ctrl Pts',(-9.83957192047858,29.2249999998932,
-7.14886745759505));
#282751=CARTESIAN_POINT('Ctrl Pts',(-12.1623797632097,29.3749999998926,
-3.95179673813132));
#282752=CARTESIAN_POINT('Ctrl Pts',(-12.1623797632097,29.524999999892,2.97892388940585E-15));
#282753=CARTESIAN_POINT('Ctrl Pts',(-12.1623797632097,29.6749999998914,
3.95179673813133));
#282754=CARTESIAN_POINT('Ctrl Pts',(-9.83957192047858,29.8249999998908,
7.14886745759505));
#282755=CARTESIAN_POINT('Ctrl Pts',(-7.51676407774748,29.9749999998902,
10.3459381770588));
#282756=CARTESIAN_POINT('Ctrl Pts',(-3.75838203887376,30.1249999998896,
11.5671105274568));
#282757=CARTESIAN_POINT('Ctrl Pts',(-2.75639200314827E-14,30.274999999889,
12.7882828778549));
#282758=CARTESIAN_POINT('Ctrl Pts',(3.7583820388737,30.4249999998884,11.5671105274568));
#282759=CARTESIAN_POINT('Ctrl Pts',(7.51676407774743,30.5749999998878,10.3459381770588));
#282760=CARTESIAN_POINT('Ctrl Pts',(9.83957192047852,30.7249999998872,7.14886745759505));
#282761=CARTESIAN_POINT('Ctrl Pts',(12.1623797632096,30.8749999998866,3.95179673813132));
#282762=CARTESIAN_POINT('Ctrl Pts',(12.1623797632096,31.024999999886,-1.48946194470292E-15));
#282763=CARTESIAN_POINT('Ctrl Pts',(12.1623797632096,31.1749999998854,-3.95179673813132));
#282764=CARTESIAN_POINT('Ctrl Pts',(9.83957192047852,31.3249999998848,-7.14886745759505));
#282765=CARTESIAN_POINT('Ctrl Pts',(7.51676407774742,31.4749999998842,-10.3459381770588));
#282766=CARTESIAN_POINT('Ctrl Pts',(3.7583820388737,31.6249999998836,-11.5671105274568));
#282767=CARTESIAN_POINT('Ctrl Pts',(-3.15600006059048E-14,31.774999999883,
-12.7882828778549));
#282768=CARTESIAN_POINT('Ctrl Pts',(-3.75838203887376,31.9249999998824,
-11.5671105274568));
#282769=CARTESIAN_POINT('Ctrl Pts',(-7.51676407774749,32.0749999998818,
-10.3459381770588));
#282770=CARTESIAN_POINT('Ctrl Pts',(-9.83957192047858,32.2249999998812,
-7.14886745759505));
#282771=CARTESIAN_POINT('Ctrl Pts',(-12.1623797632097,32.3749999998806,
-3.95179673813132));
#282772=CARTESIAN_POINT('Ctrl Pts',(-12.1623797632097,32.52499999988,2.97892388940585E-15));
#282773=CARTESIAN_POINT('Ctrl Pts',(-12.1623797632097,32.6749999998794,
3.95179673813133));
#282774=CARTESIAN_POINT('Ctrl Pts',(-9.83957192047858,32.8249999998788,
7.14886745759505));
#282775=CARTESIAN_POINT('Ctrl Pts',(-7.51676407774749,32.9749999998782,
10.3459381770588));
#282776=CARTESIAN_POINT('Ctrl Pts',(-3.75838203887376,33.1249999998776,
11.5671105274568));
#282777=CARTESIAN_POINT('Ctrl Pts',(-2.92916293031446E-14,33.274999999877,
12.7882828778549));
#282778=CARTESIAN_POINT('Ctrl Pts',(3.7583820388737,33.4249999998764,11.5671105274568));
#282779=CARTESIAN_POINT('Ctrl Pts',(7.51676407774743,33.5749999998758,10.3459381770588));
#282780=CARTESIAN_POINT('Ctrl Pts',(9.83957192047852,33.7249999998752,7.14886745759505));
#282781=CARTESIAN_POINT('Ctrl Pts',(12.1623797632096,33.8749999998746,3.95179673813132));
#282782=CARTESIAN_POINT('Ctrl Pts',(12.1623797632096,34.024999999874,-1.48946194470292E-15));
#282783=CARTESIAN_POINT('Ctrl Pts',(12.1623797632096,34.1749999998734,-3.95179673813132));
#282784=CARTESIAN_POINT('Ctrl Pts',(9.83957192047851,34.3249999998728,-7.14886745759505));
#282785=CARTESIAN_POINT('Ctrl Pts',(7.51676407774742,34.4749999998722,-10.3459381770588));
#282786=CARTESIAN_POINT('Ctrl Pts',(3.7583820388737,34.6249999998716,-11.5671105274568));
#282787=CARTESIAN_POINT('Ctrl Pts',(-3.32877098775667E-14,34.774999999871,
-12.7882828778549));
#282788=CARTESIAN_POINT('Ctrl Pts',(-3.75838203887376,34.9249999998704,
-11.5671105274568));
#282789=CARTESIAN_POINT('Ctrl Pts',(-7.51676407774749,35.0749999998698,
-10.3459381770588));
#282790=CARTESIAN_POINT('Ctrl Pts',(-9.83957192047858,35.2249999998692,
-7.14886745759505));
#282791=CARTESIAN_POINT('Ctrl Pts',(-12.1623797632097,35.3749999998686,
-3.95179673813132));
#282792=CARTESIAN_POINT('Ctrl Pts',(-12.1623797632097,35.524999999868,2.97892388940585E-15));
#282793=CARTESIAN_POINT('Ctrl Pts',(-12.1623797632097,35.6749999998674,
3.95179673813133));
#282794=CARTESIAN_POINT('Ctrl Pts',(-9.83957192047858,35.8249999998668,
7.14886745759505));
#282795=CARTESIAN_POINT('Ctrl Pts',(-7.51676407774749,35.9749999998662,
10.3459381770588));
#282796=CARTESIAN_POINT('Ctrl Pts',(-3.75838203887376,36.1249999998656,
11.5671105274568));
#282797=CARTESIAN_POINT('Ctrl Pts',(-3.10193385748064E-14,36.274999999865,
12.7882828778549));
#282798=CARTESIAN_POINT('Ctrl Pts',(3.7583820388737,36.4249999998644,11.5671105274568));
#282799=CARTESIAN_POINT('Ctrl Pts',(7.51676407774742,36.5749999998638,10.3459381770588));
#282800=CARTESIAN_POINT('Ctrl Pts',(9.83957192047851,36.7249999998632,7.14886745759505));
#282801=CARTESIAN_POINT('Ctrl Pts',(12.1623797632096,36.8749999998626,3.95179673813132));
#282802=CARTESIAN_POINT('Ctrl Pts',(12.1623797632096,37.024999999862,-1.48946194470292E-15));
#282803=CARTESIAN_POINT('Ctrl Pts',(12.1623797632096,37.1749999998614,-3.95179673813132));
#282804=CARTESIAN_POINT('Ctrl Pts',(9.83957192047851,37.3249999998608,-7.14886745759505));
#282805=CARTESIAN_POINT('Ctrl Pts',(7.51676407774742,37.4749999998602,-10.3459381770588));
#282806=CARTESIAN_POINT('Ctrl Pts',(3.75838203887369,37.6249999998596,-11.5671105274568));
#282807=CARTESIAN_POINT('Ctrl Pts',(-3.50154191492285E-14,37.774999999859,
-12.7882828778549));
#282808=CARTESIAN_POINT('Ctrl Pts',(-3.75838203887376,37.9249999998584,
-11.5671105274568));
#282809=CARTESIAN_POINT('Ctrl Pts',(-7.51676407774749,38.0749999998578,
-10.3459381770588));
#282810=CARTESIAN_POINT('Ctrl Pts',(-9.83957192047858,38.2249999998572,
-7.14886745759505));
#282811=CARTESIAN_POINT('Ctrl Pts',(-12.1623797632097,38.3749999998566,
-3.95179673813132));
#282812=CARTESIAN_POINT('Ctrl Pts',(-12.1623797632097,38.524999999856,2.97892388940585E-15));
#282813=CARTESIAN_POINT('Ctrl Pts',(-12.1623797632097,38.6749999998554,
3.95179673813133));
#282814=CARTESIAN_POINT('Ctrl Pts',(-9.83957192047858,38.8249999998548,
7.14886745759505));
#282815=CARTESIAN_POINT('Ctrl Pts',(-7.51676407774749,38.9749999998542,
10.3459381770588));
#282816=CARTESIAN_POINT('Ctrl Pts',(-3.75838203887376,39.1249999998536,
11.5671105274568));
#282817=CARTESIAN_POINT('Ctrl Pts',(-3.27470478464682E-14,39.274999999853,
12.7882828778549));
#282818=CARTESIAN_POINT('Ctrl Pts',(3.7583820388737,39.4249999998524,11.5671105274568));
#282819=CARTESIAN_POINT('Ctrl Pts',(7.51676407774742,39.5749999998518,10.3459381770588));
#282820=CARTESIAN_POINT('Ctrl Pts',(9.83957192047851,39.7249999998512,7.14886745759505));
#282821=CARTESIAN_POINT('Ctrl Pts',(12.1623797632096,39.8749999998506,3.95179673813132));
#282822=CARTESIAN_POINT('Ctrl Pts',(12.1623797632096,40.02499999985,-1.48946194470292E-15));
#282823=CARTESIAN_POINT('Ctrl Pts',(12.1623797632096,40.1749999998494,-3.95179673813132));
#282824=CARTESIAN_POINT('Ctrl Pts',(9.83957192047851,40.3249999998488,-7.14886745759505));
#282825=CARTESIAN_POINT('Ctrl Pts',(7.51676407774742,40.4749999998482,-10.3459381770588));
#282826=CARTESIAN_POINT('Ctrl Pts',(3.75838203887369,40.6249999998476,-11.5671105274568));
#282827=CARTESIAN_POINT('Ctrl Pts',(-3.67431284208903E-14,40.774999999847,
-12.7882828778549));
#282828=CARTESIAN_POINT('Ctrl Pts',(-3.75838203887376,40.9249999998464,
-11.5671105274568));
#282829=CARTESIAN_POINT('Ctrl Pts',(-7.51676407774749,41.0749999998458,
-10.3459381770588));
#282830=CARTESIAN_POINT('Ctrl Pts',(-9.83957192047858,41.2249999998452,
-7.14886745759505));
#282831=CARTESIAN_POINT('Ctrl Pts',(-12.1623797632097,41.3749999998446,
-3.95179673813132));
#282832=CARTESIAN_POINT('Ctrl Pts',(-12.1623797632097,41.524999999844,2.97892388940585E-15));
#282833=CARTESIAN_POINT('Ctrl Pts',(-12.1623797632097,41.6749999998434,
3.95179673813133));
#282834=CARTESIAN_POINT('Ctrl Pts',(-9.83957192047858,41.8249999998428,
7.14886745759505));
#282835=CARTESIAN_POINT('Ctrl Pts',(-7.51676407774749,41.9749999998422,
10.3459381770588));
#282836=CARTESIAN_POINT('Ctrl Pts',(-3.75838203887376,42.1249999998416,
11.5671105274568));
#282837=CARTESIAN_POINT('Ctrl Pts',(-3.44747571181301E-14,42.274999999841,
12.7882828778549));
#282838=CARTESIAN_POINT('Ctrl Pts',(3.75838203887369,42.4249999998404,11.5671105274568));
#282839=CARTESIAN_POINT('Ctrl Pts',(7.51676407774742,42.5749999998398,10.3459381770588));
#282840=CARTESIAN_POINT('Ctrl Pts',(9.83957192047851,42.7249999998392,7.14886745759505));
#282841=CARTESIAN_POINT('Ctrl Pts',(12.1623797632096,42.8749999998386,3.95179673813132));
#282842=CARTESIAN_POINT('Ctrl Pts',(12.1623797632096,43.024999999838,-1.48946194470292E-15));
#282843=CARTESIAN_POINT('Ctrl Pts',(12.1623797632096,43.1749999998374,-3.95179673813132));
#282844=CARTESIAN_POINT('Ctrl Pts',(9.83957192047851,43.3249999998368,-7.14886745759505));
#282845=CARTESIAN_POINT('Ctrl Pts',(7.51676407774742,43.4749999998362,-10.3459381770588));
#282846=CARTESIAN_POINT('Ctrl Pts',(3.75838203887369,43.6249999998356,-11.5671105274568));
#282847=CARTESIAN_POINT('Ctrl Pts',(-3.84708376925522E-14,43.774999999835,
-12.7882828778549));
#282848=CARTESIAN_POINT('Ctrl Pts',(-3.75838203887377,43.9249999998344,
-11.5671105274568));
#282849=CARTESIAN_POINT('Ctrl Pts',(-7.51676407774749,44.0749999998338,
-10.3459381770588));
#282850=CARTESIAN_POINT('Ctrl Pts',(-9.83957192047859,44.2249999998332,
-7.14886745759505));
#282851=CARTESIAN_POINT('Ctrl Pts',(-12.1623797632097,44.3749999998326,
-3.95179673813132));
#282852=CARTESIAN_POINT('Ctrl Pts',(-12.1623797632097,44.524999999832,2.97892388940585E-15));
#282853=CARTESIAN_POINT('Ctrl Pts',(-12.1623797632097,44.6749999998314,
3.95179673813133));
#282854=CARTESIAN_POINT('Ctrl Pts',(-9.83957192047859,44.8249999998308,
7.14886745759505));
#282855=CARTESIAN_POINT('Ctrl Pts',(-7.51676407774749,44.9749999998302,
10.3459381770588));
#282856=CARTESIAN_POINT('Ctrl Pts',(-3.75838203887376,45.1249999998296,
11.5671105274568));
#282857=CARTESIAN_POINT('Ctrl Pts',(-3.62024663897919E-14,45.274999999829,
12.7882828778549));
#282858=CARTESIAN_POINT('Ctrl Pts',(3.75838203887369,45.4249999998284,11.5671105274568));
#282859=CARTESIAN_POINT('Ctrl Pts',(7.51676407774742,45.5749999998278,10.3459381770588));
#282860=CARTESIAN_POINT('Ctrl Pts',(9.83957192047851,45.7249999998272,7.14886745759505));
#282861=CARTESIAN_POINT('Ctrl Pts',(12.1623797632096,45.8749999998266,3.95179673813132));
#282862=CARTESIAN_POINT('Ctrl Pts',(12.1623797632096,46.024999999826,-1.48946194470292E-15));
#282863=CARTESIAN_POINT('Ctrl Pts',(12.1623797632096,46.1749999998254,-3.95179673813132));
#282864=CARTESIAN_POINT('Ctrl Pts',(9.83957192047851,46.3249999998248,-7.14886745759505));
#282865=CARTESIAN_POINT('Ctrl Pts',(7.51676407774742,46.4749999998242,-10.3459381770588));
#282866=CARTESIAN_POINT('Ctrl Pts',(3.75838203887369,46.6249999998236,-11.5671105274568));
#282867=CARTESIAN_POINT('Ctrl Pts',(-4.0198546964214E-14,46.774999999823,
-12.7882828778549));
#282868=CARTESIAN_POINT('Ctrl Pts',(-3.75838203887377,46.9249999998224,
-11.5671105274568));
#282869=CARTESIAN_POINT('Ctrl Pts',(-7.5167640777475,47.0749999998218,-10.3459381770588));
#282870=CARTESIAN_POINT('Ctrl Pts',(-9.83957192047859,47.2249999998212,
-7.14886745759505));
#282871=CARTESIAN_POINT('Ctrl Pts',(-12.1623797632097,47.3749999998206,
-3.95179673813132));
#282872=CARTESIAN_POINT('Ctrl Pts',(-12.1623797632097,47.52499999982,2.97892388940585E-15));
#282873=CARTESIAN_POINT('Ctrl Pts',(-12.1623797632097,47.6749999998194,
3.95179673813133));
#282874=CARTESIAN_POINT('Ctrl Pts',(-9.83957192047859,47.8249999998188,
7.14886745759505));
#282875=CARTESIAN_POINT('Ctrl Pts',(-7.51676407774749,47.9749999998182,
10.3459381770588));
#282876=CARTESIAN_POINT('Ctrl Pts',(-3.75838203887377,48.1249999998176,
11.5671105274568));
#282877=CARTESIAN_POINT('Ctrl Pts',(-3.79301756614538E-14,48.274999999817,
12.7882828778549));
#282878=CARTESIAN_POINT('Ctrl Pts',(3.75838203887369,48.4249999998164,11.5671105274568));
#282879=CARTESIAN_POINT('Ctrl Pts',(7.51676407774742,48.5749999998158,10.3459381770588));
#282880=CARTESIAN_POINT('Ctrl Pts',(9.83957192047851,48.7249999998152,7.14886745759505));
#282881=CARTESIAN_POINT('Ctrl Pts',(12.1623797632096,48.8749999998146,3.95179673813132));
#282882=CARTESIAN_POINT('Ctrl Pts',(12.1623797632096,49.024999999814,-1.48946194470292E-15));
#282883=CARTESIAN_POINT('Ctrl Pts',(12.1623797632096,49.1749999998134,-3.95179673813132));
#282884=CARTESIAN_POINT('Ctrl Pts',(9.83957192047851,49.3249999998128,-7.14886745759505));
#282885=CARTESIAN_POINT('Ctrl Pts',(7.51676407774741,49.4749999998122,-10.3459381770588));
#282886=CARTESIAN_POINT('Ctrl Pts',(3.75838203887369,49.6249999998116,-11.5671105274568));
#282887=CARTESIAN_POINT('Ctrl Pts',(-4.19262562358759E-14,49.774999999811,
-12.7882828778549));
#282888=CARTESIAN_POINT('Ctrl Pts',(-3.75838203887377,49.9249999998104,
-11.5671105274568));
#282889=CARTESIAN_POINT('Ctrl Pts',(-7.5167640777475,50.0749999998098,-10.3459381770588));
#282890=CARTESIAN_POINT('Ctrl Pts',(-9.83957192047859,50.2249999998092,
-7.14886745759505));
#282891=CARTESIAN_POINT('Ctrl Pts',(-12.1623797632097,50.3749999998086,
-3.95179673813132));
#282892=CARTESIAN_POINT('Ctrl Pts',(-12.1623797632097,50.524999999808,2.97892388940585E-15));
#282893=CARTESIAN_POINT('Ctrl Pts',(-12.1623797632097,50.6749999998074,
3.95179673813133));
#282894=CARTESIAN_POINT('Ctrl Pts',(-9.83957192047859,50.8249999998068,
7.14886745759505));
#282895=CARTESIAN_POINT('Ctrl Pts',(-7.51676407774749,50.9749999998062,
10.3459381770588));
#282896=CARTESIAN_POINT('Ctrl Pts',(-3.75838203887377,51.1249999998056,
11.5671105274568));
#282897=CARTESIAN_POINT('Ctrl Pts',(-3.96578849331156E-14,51.274999999805,
12.7882828778549));
#282898=CARTESIAN_POINT('Ctrl Pts',(3.75838203887369,51.4249999998044,11.5671105274568));
#282899=CARTESIAN_POINT('Ctrl Pts',(7.51676407774742,51.5749999998038,10.3459381770588));
#282900=CARTESIAN_POINT('Ctrl Pts',(9.83957192047851,51.7249999998032,7.14886745759505));
#282901=CARTESIAN_POINT('Ctrl Pts',(12.1623797632096,51.8749999998026,3.95179673813132));
#282902=CARTESIAN_POINT('Ctrl Pts',(12.1623797632096,52.024999999802,-1.48946194470292E-15));
#282903=CARTESIAN_POINT('Ctrl Pts',(12.1623797632096,52.1749999998014,-3.95179673813132));
#282904=CARTESIAN_POINT('Ctrl Pts',(9.8395719204785,52.3249999998008,-7.14886745759505));
#282905=CARTESIAN_POINT('Ctrl Pts',(7.51676407774741,52.4749999998002,-10.3459381770588));
#282906=CARTESIAN_POINT('Ctrl Pts',(3.75838203887368,52.6249999997996,-11.5671105274568));
#282907=CARTESIAN_POINT('Ctrl Pts',(-4.36539655075377E-14,52.774999999799,
-12.7882828778549));
#282908=CARTESIAN_POINT('Ctrl Pts',(-3.75838203887377,52.9249999997984,
-11.5671105274568));
#282909=CARTESIAN_POINT('Ctrl Pts',(-7.5167640777475,53.0749999997978,-10.3459381770588));
#282910=CARTESIAN_POINT('Ctrl Pts',(-9.83957192047859,53.2249999997972,
-7.14886745759505));
#282911=CARTESIAN_POINT('Ctrl Pts',(-12.1623797632097,53.3749999997966,
-3.95179673813132));
#282912=CARTESIAN_POINT('Ctrl Pts',(-12.1623797632097,53.524999999796,2.97892388940585E-15));
#282913=CARTESIAN_POINT('Ctrl Pts',(-12.1623797632097,53.6749999997954,
3.95179673813133));
#282914=CARTESIAN_POINT('Ctrl Pts',(-9.83957192047859,53.8249999997948,
7.14886745759505));
#282915=CARTESIAN_POINT('Ctrl Pts',(-7.5167640777475,53.9749999997942,10.3459381770588));
#282916=CARTESIAN_POINT('Ctrl Pts',(-3.75838203887377,54.1249999997936,
11.5671105274568));
#282917=CARTESIAN_POINT('Ctrl Pts',(-4.13855942047774E-14,54.274999999793,
12.7882828778549));
#282918=CARTESIAN_POINT('Ctrl Pts',(3.75838203887369,54.4249999997924,11.5671105274568));
#282919=CARTESIAN_POINT('Ctrl Pts',(7.51676407774741,54.5749999997918,10.3459381770588));
#282920=CARTESIAN_POINT('Ctrl Pts',(9.8395719204785,54.7249999997912,7.14886745759505));
#282921=CARTESIAN_POINT('Ctrl Pts',(12.1623797632096,54.8749999997906,3.95179673813132));
#282922=CARTESIAN_POINT('Ctrl Pts',(12.1623797632096,55.02499999979,-1.48946194470292E-15));
#282923=CARTESIAN_POINT('Ctrl Pts',(12.1623797632096,55.1749999997894,-3.95179673813132));
#282924=CARTESIAN_POINT('Ctrl Pts',(9.8395719204785,55.3249999997888,-7.14886745759505));
#282925=CARTESIAN_POINT('Ctrl Pts',(7.51676407774741,55.4749999997882,-10.3459381770588));
#282926=CARTESIAN_POINT('Ctrl Pts',(3.75838203887368,55.6249999997876,-11.5671105274568));
#282927=CARTESIAN_POINT('Ctrl Pts',(-4.53816747791995E-14,55.774999999787,
-12.7882828778549));
#282928=CARTESIAN_POINT('Ctrl Pts',(-3.75838203887377,55.9249999997864,
-11.5671105274568));
#282929=CARTESIAN_POINT('Ctrl Pts',(-7.5167640777475,56.0749999997858,-10.3459381770588));
#282930=CARTESIAN_POINT('Ctrl Pts',(-9.83957192047859,56.2249999997852,
-7.14886745759505));
#282931=CARTESIAN_POINT('Ctrl Pts',(-12.1623797632097,56.3749999997846,
-3.95179673813132));
#282932=CARTESIAN_POINT('Ctrl Pts',(-12.1623797632097,56.524999999784,2.97892388940585E-15));
#282933=CARTESIAN_POINT('Ctrl Pts',(-12.1623797632097,56.6749999997834,
3.95179673813133));
#282934=CARTESIAN_POINT('Ctrl Pts',(-9.83957192047859,56.8249999997828,
7.14886745759505));
#282935=CARTESIAN_POINT('Ctrl Pts',(-7.5167640777475,56.9749999997822,10.3459381770588));
#282936=CARTESIAN_POINT('Ctrl Pts',(-3.75838203887377,57.1249999997816,
11.5671105274568));
#282937=CARTESIAN_POINT('Ctrl Pts',(-4.31133034764393E-14,57.274999999781,
12.7882828778549));
#282938=CARTESIAN_POINT('Ctrl Pts',(3.75838203887368,57.4249999997804,11.5671105274568));
#282939=CARTESIAN_POINT('Ctrl Pts',(7.51676407774741,57.5749999997798,10.3459381770588));
#282940=CARTESIAN_POINT('Ctrl Pts',(9.8395719204785,57.7249999997792,7.14886745759505));
#282941=CARTESIAN_POINT('Ctrl Pts',(12.1623797632096,57.8749999997786,3.95179673813132));
#282942=CARTESIAN_POINT('Ctrl Pts',(12.1623797632096,58.024999999778,-1.48946194470292E-15));
#282943=CARTESIAN_POINT('Ctrl Pts',(12.1623797632096,58.1749999997774,-3.95179673813132));
#282944=CARTESIAN_POINT('Ctrl Pts',(9.8395719204785,58.3249999997768,-7.14886745759505));
#282945=CARTESIAN_POINT('Ctrl Pts',(7.51676407774741,58.4749999997762,-10.3459381770588));
#282946=CARTESIAN_POINT('Ctrl Pts',(3.75838203887368,58.6249999997756,-11.5671105274568));
#282947=CARTESIAN_POINT('Ctrl Pts',(-4.71093840508614E-14,58.774999999775,
-12.7882828778549));
#282948=CARTESIAN_POINT('Ctrl Pts',(-3.75838203887377,58.9249999997744,
-11.5671105274568));
#282949=CARTESIAN_POINT('Ctrl Pts',(-7.5167640777475,59.0749999997738,-10.3459381770588));
#282950=CARTESIAN_POINT('Ctrl Pts',(-9.83957192047859,59.2249999997732,
-7.14886745759505));
#282951=CARTESIAN_POINT('Ctrl Pts',(-12.1623797632097,59.3749999997726,
-3.95179673813132));
#282952=CARTESIAN_POINT('Ctrl Pts',(-12.1623797632097,59.524999999772,2.97892388940585E-15));
#282953=CARTESIAN_POINT('Ctrl Pts',(-12.1623797632097,59.6749999997714,
3.95179673813133));
#282954=CARTESIAN_POINT('Ctrl Pts',(-9.83957192047859,59.8249999997708,
7.14886745759505));
#282955=CARTESIAN_POINT('Ctrl Pts',(-7.5167640777475,59.9749999997702,10.3459381770588));
#282956=CARTESIAN_POINT('Ctrl Pts',(-3.75838203887377,60.1249999997696,
11.5671105274568));
#282957=CARTESIAN_POINT('Ctrl Pts',(-4.48410127481011E-14,60.274999999769,
12.7882828778549));
#282958=CARTESIAN_POINT('Ctrl Pts',(3.75838203887368,60.4249999997684,11.5671105274568));
#282959=CARTESIAN_POINT('Ctrl Pts',(7.51676407774741,60.5749999997678,10.3459381770588));
#282960=CARTESIAN_POINT('Ctrl Pts',(9.8395719204785,60.7249999997672,7.14886745759505));
#282961=CARTESIAN_POINT('Ctrl Pts',(12.1623797632096,60.8749999997666,3.95179673813132));
#282962=CARTESIAN_POINT('Ctrl Pts',(12.1623797632096,61.024999999766,-1.48946194470292E-15));
#282963=CARTESIAN_POINT('Ctrl Pts',(12.1623797632096,61.1749999997654,-3.95179673813132));
#282964=CARTESIAN_POINT('Ctrl Pts',(9.8395719204785,61.3249999997648,-7.14886745759505));
#282965=CARTESIAN_POINT('Ctrl Pts',(7.51676407774741,61.4749999997642,-10.3459381770588));
#282966=CARTESIAN_POINT('Ctrl Pts',(3.75838203887368,61.6249999997636,-11.5671105274568));
#282967=CARTESIAN_POINT('Ctrl Pts',(-4.88370933225232E-14,61.774999999763,
-12.7882828778549));
#282968=CARTESIAN_POINT('Ctrl Pts',(-3.75838203887378,61.9249999997624,
-11.5671105274568));
#282969=CARTESIAN_POINT('Ctrl Pts',(-7.5167640777475,62.0749999997618,-10.3459381770588));
#282970=CARTESIAN_POINT('Ctrl Pts',(-9.8395719204786,62.2249999997612,-7.14886745759505));
#282971=CARTESIAN_POINT('Ctrl Pts',(-12.1623797632097,62.3749999997606,
-3.95179673813132));
#282972=CARTESIAN_POINT('Ctrl Pts',(-12.1623797632097,62.52499999976,2.97892388940585E-15));
#282973=CARTESIAN_POINT('Ctrl Pts',(-12.1623797632097,62.6749999997594,
3.95179673813133));
#282974=CARTESIAN_POINT('Ctrl Pts',(-9.8395719204786,62.8249999997588,7.14886745759505));
#282975=CARTESIAN_POINT('Ctrl Pts',(-7.5167640777475,62.9749999997582,10.3459381770588));
#282976=CARTESIAN_POINT('Ctrl Pts',(-3.75838203887377,63.1249999997576,
11.5671105274568));
#282977=CARTESIAN_POINT('Ctrl Pts',(-4.6568722019763E-14,63.274999999757,
12.7882828778549));
#282978=CARTESIAN_POINT('Ctrl Pts',(3.75838203887368,63.4249999997564,11.5671105274568));
#282979=CARTESIAN_POINT('Ctrl Pts',(7.51676407774741,63.5749999997558,10.3459381770588));
#282980=CARTESIAN_POINT('Ctrl Pts',(9.8395719204785,63.7249999997552,7.14886745759505));
#282981=CARTESIAN_POINT('Ctrl Pts',(12.1623797632096,63.8749999997546,3.95179673813132));
#282982=CARTESIAN_POINT('Ctrl Pts',(12.1623797632096,64.024999999754,-1.48946194470292E-15));
#282983=CARTESIAN_POINT('Ctrl Pts',(12.1623797632096,64.1749999997534,-3.95179673813132));
#282984=CARTESIAN_POINT('Ctrl Pts',(9.8395719204785,64.3249999997528,-7.14886745759505));
#282985=CARTESIAN_POINT('Ctrl Pts',(7.5167640777474,64.4749999997522,-10.3459381770588));
#282986=CARTESIAN_POINT('Ctrl Pts',(3.75838203887368,64.6249999997516,-11.5671105274568));
#282987=CARTESIAN_POINT('Ctrl Pts',(-5.05648025941851E-14,64.774999999751,
-12.7882828778549));
#282988=CARTESIAN_POINT('Ctrl Pts',(-3.75838203887378,64.9249999997504,
-11.5671105274568));
#282989=CARTESIAN_POINT('Ctrl Pts',(-7.51676407774751,65.0749999997498,
-10.3459381770588));
#282990=CARTESIAN_POINT('Ctrl Pts',(-9.8395719204786,65.2249999997492,-7.14886745759505));
#282991=CARTESIAN_POINT('Ctrl Pts',(-12.1623797632097,65.3749999997486,
-3.95179673813132));
#282992=CARTESIAN_POINT('Ctrl Pts',(-12.1623797632097,65.524999999748,2.97892388940585E-15));
#282993=CARTESIAN_POINT('Ctrl Pts',(-12.1623797632097,65.6749999997474,
3.95179673813133));
#282994=CARTESIAN_POINT('Ctrl Pts',(-9.8395719204786,65.8249999997468,7.14886745759505));
#282995=CARTESIAN_POINT('Ctrl Pts',(-7.5167640777475,65.9749999997462,10.3459381770588));
#282996=CARTESIAN_POINT('Ctrl Pts',(-3.75838203887378,66.1249999997456,
11.5671105274568));
#282997=CARTESIAN_POINT('Ctrl Pts',(-4.82964312914248E-14,66.274999999745,
12.7882828778549));
#282998=CARTESIAN_POINT('Ctrl Pts',(3.75838203887368,66.4249999997444,11.5671105274568));
#282999=CARTESIAN_POINT('Ctrl Pts',(7.51676407774741,66.5749999997438,10.3459381770588));
#283000=CARTESIAN_POINT('Ctrl Pts',(9.8395719204785,66.7249999997432,7.14886745759505));
#283001=CARTESIAN_POINT('Ctrl Pts',(12.1623797632096,66.8749999997426,3.95179673813132));
#283002=CARTESIAN_POINT('Ctrl Pts',(12.1623797632096,67.024999999742,-1.48946194470292E-15));
#283003=CARTESIAN_POINT('Ctrl Pts',(12.1623797632096,67.1749999997414,-3.95179673813132));
#283004=CARTESIAN_POINT('Ctrl Pts',(9.8395719204785,67.3249999997408,-7.14886745759505));
#283005=CARTESIAN_POINT('Ctrl Pts',(7.5167640777474,67.4749999997402,-10.3459381770588));
#283006=CARTESIAN_POINT('Ctrl Pts',(3.75838203887368,67.6249999997396,-11.5671105274568));
#283007=CARTESIAN_POINT('Ctrl Pts',(-5.22925118658469E-14,67.774999999739,
-12.7882828778549));
#283008=CARTESIAN_POINT('Ctrl Pts',(-3.75838203887378,67.9249999997384,
-11.5671105274568));
#283009=CARTESIAN_POINT('Ctrl Pts',(-7.51676407774751,68.0749999997378,
-10.3459381770588));
#283010=CARTESIAN_POINT('Ctrl Pts',(-9.8395719204786,68.2249999997372,-7.14886745759505));
#283011=CARTESIAN_POINT('Ctrl Pts',(-12.1623797632097,68.3749999997366,
-3.95179673813132));
#283012=CARTESIAN_POINT('Ctrl Pts',(-12.1623797632097,68.524999999736,2.97892388940585E-15));
#283013=CARTESIAN_POINT('Ctrl Pts',(-12.1623797632097,68.6749999997354,
3.95179673813133));
#283014=CARTESIAN_POINT('Ctrl Pts',(-9.8395719204786,68.8249999997348,7.14886745759505));
#283015=CARTESIAN_POINT('Ctrl Pts',(-7.51676407774751,68.9749999997342,
10.3459381770588));
#283016=CARTESIAN_POINT('Ctrl Pts',(-3.75838203887378,69.1249999997336,
11.5671105274568));
#283017=CARTESIAN_POINT('Ctrl Pts',(-5.00241405630866E-14,69.274999999733,
12.7882828778549));
#283018=CARTESIAN_POINT('Ctrl Pts',(3.75838203887368,69.4249999997324,11.5671105274568));
#283019=CARTESIAN_POINT('Ctrl Pts',(7.5167640777474,69.5749999997318,10.3459381770588));
#283020=CARTESIAN_POINT('Ctrl Pts',(9.8395719204785,69.7249999997312,7.14886745759505));
#283021=CARTESIAN_POINT('Ctrl Pts',(12.1623797632096,69.8749999997306,3.95179673813132));
#283022=CARTESIAN_POINT('Ctrl Pts',(12.1623797632096,70.02499999973,-1.48946194470292E-15));
#283023=CARTESIAN_POINT('Ctrl Pts',(12.1623797632096,70.1749999997294,-3.95179673813132));
#283024=CARTESIAN_POINT('Ctrl Pts',(9.83957192047849,70.3249999997288,-7.14886745759505));
#283025=CARTESIAN_POINT('Ctrl Pts',(7.5167640777474,70.4749999997282,-10.3459381770588));
#283026=CARTESIAN_POINT('Ctrl Pts',(3.75838203887367,70.6249999997276,-11.5671105274568));
#283027=CARTESIAN_POINT('Ctrl Pts',(-5.40202211375087E-14,70.774999999727,
-12.7882828778549));
#283028=CARTESIAN_POINT('Ctrl Pts',(-3.75838203887378,70.9249999997264,
-11.5671105274568));
#283029=CARTESIAN_POINT('Ctrl Pts',(-7.51676407774751,71.0749999997258,
-10.3459381770588));
#283030=CARTESIAN_POINT('Ctrl Pts',(-9.8395719204786,71.2249999997252,-7.14886745759505));
#283031=CARTESIAN_POINT('Ctrl Pts',(-12.1623797632097,71.3749999997246,
-3.95179673813132));
#283032=CARTESIAN_POINT('Ctrl Pts',(-12.1623797632097,71.524999999724,2.97892388940585E-15));
#283033=CARTESIAN_POINT('Ctrl Pts',(-12.1623797632097,71.6749999997234,
3.95179673813133));
#283034=CARTESIAN_POINT('Ctrl Pts',(-9.8395719204786,71.8249999997228,7.14886745759505));
#283035=CARTESIAN_POINT('Ctrl Pts',(-7.51676407774751,71.9749999997222,
10.3459381770588));
#283036=CARTESIAN_POINT('Ctrl Pts',(-3.75838203887378,72.1249999997216,
11.5671105274568));
#283037=CARTESIAN_POINT('Ctrl Pts',(-5.17518498347485E-14,72.274999999721,
12.7882828778549));
#283038=CARTESIAN_POINT('Ctrl Pts',(3.75838203887368,72.4249999997204,11.5671105274568));
#283039=CARTESIAN_POINT('Ctrl Pts',(7.5167640777474,72.5749999997198,10.3459381770588));
#283040=CARTESIAN_POINT('Ctrl Pts',(9.83957192047849,72.7249999997192,7.14886745759505));
#283041=CARTESIAN_POINT('Ctrl Pts',(12.1623797632096,72.8749999997186,3.95179673813132));
#283042=CARTESIAN_POINT('Ctrl Pts',(12.1623797632096,73.024999999718,-1.48946194470292E-15));
#283043=CARTESIAN_POINT('Ctrl Pts',(12.1623797632096,73.1749999997174,-3.95179673813132));
#283044=CARTESIAN_POINT('Ctrl Pts',(9.83957192047849,73.3249999997168,-7.14886745759505));
#283045=CARTESIAN_POINT('Ctrl Pts',(7.5167640777474,73.4749999997162,-10.3459381770588));
#283046=CARTESIAN_POINT('Ctrl Pts',(3.75838203887367,73.6249999997156,-11.5671105274568));
#283047=CARTESIAN_POINT('Ctrl Pts',(-5.57479304091706E-14,73.774999999715,
-12.7882828778549));
#283048=CARTESIAN_POINT('Ctrl Pts',(-3.75838203887378,73.9249999997144,
-11.5671105274568));
#283049=CARTESIAN_POINT('Ctrl Pts',(-7.51676407774751,74.0749999997138,
-10.3459381770588));
#283050=CARTESIAN_POINT('Ctrl Pts',(-9.8395719204786,74.2249999997132,-7.14886745759505));
#283051=CARTESIAN_POINT('Ctrl Pts',(-12.1623797632097,74.3749999997126,
-3.95179673813132));
#283052=CARTESIAN_POINT('Ctrl Pts',(-12.1623797632097,74.524999999712,2.97892388940585E-15));
#283053=CARTESIAN_POINT('Ctrl Pts',(-12.1623797632097,74.6749999997114,
3.95179673813133));
#283054=CARTESIAN_POINT('Ctrl Pts',(-9.8395719204786,74.8249999997108,7.14886745759505));
#283055=CARTESIAN_POINT('Ctrl Pts',(-7.51676407774751,74.9749999997102,
10.3459381770588));
#283056=CARTESIAN_POINT('Ctrl Pts',(-3.75838203887378,75.1249999997096,
11.5671105274568));
#283057=CARTESIAN_POINT('Ctrl Pts',(-5.34795591064103E-14,75.274999999709,
12.7882828778549));
#283058=CARTESIAN_POINT('Ctrl Pts',(3.75838203887367,75.4249999997084,11.5671105274568));
#283059=CARTESIAN_POINT('Ctrl Pts',(7.5167640777474,75.5749999997078,10.3459381770588));
#283060=CARTESIAN_POINT('Ctrl Pts',(9.83957192047849,75.7249999997072,7.14886745759505));
#283061=CARTESIAN_POINT('Ctrl Pts',(12.1623797632096,75.8749999997066,3.95179673813132));
#283062=CARTESIAN_POINT('Ctrl Pts',(12.1623797632096,76.024999999706,-1.48946194470292E-15));
#283063=CARTESIAN_POINT('Ctrl Pts',(12.1623797632096,76.1749999997054,-3.95179673813132));
#283064=CARTESIAN_POINT('Ctrl Pts',(9.83957192047849,76.3249999997048,-7.14886745759505));
#283065=CARTESIAN_POINT('Ctrl Pts',(7.5167640777474,76.4749999997042,-10.3459381770588));
#283066=CARTESIAN_POINT('Ctrl Pts',(3.75838203887367,76.6249999997036,-11.5671105274568));
#283067=CARTESIAN_POINT('Ctrl Pts',(-5.74756396808324E-14,76.774999999703,
-12.7882828778549));
#283068=CARTESIAN_POINT('Ctrl Pts',(-3.75838203887379,76.9249999997024,
-11.5671105274568));
#283069=CARTESIAN_POINT('Ctrl Pts',(-7.51676407774751,77.0749999997018,
-10.3459381770588));
#283070=CARTESIAN_POINT('Ctrl Pts',(-9.8395719204786,77.2249999997012,-7.14886745759505));
#283071=CARTESIAN_POINT('Ctrl Pts',(-12.1623797632097,77.3749999997006,
-3.95179673813132));
#283072=CARTESIAN_POINT('Ctrl Pts',(-12.1623797632097,77.5249999997,2.97892388940585E-15));
#283073=CARTESIAN_POINT('Ctrl Pts',(-12.1623797632097,77.6749999996994,
3.95179673813133));
#283074=CARTESIAN_POINT('Ctrl Pts',(-9.8395719204786,77.8249999996988,7.14886745759505));
#283075=CARTESIAN_POINT('Ctrl Pts',(-7.51676407774751,77.9749999996982,
10.3459381770588));
#283076=CARTESIAN_POINT('Ctrl Pts',(-3.75838203887378,78.1249999996976,
11.5671105274568));
#283077=CARTESIAN_POINT('Ctrl Pts',(-5.52072683780721E-14,78.274999999697,
12.7882828778549));
#283078=CARTESIAN_POINT('Ctrl Pts',(3.75838203887367,78.4249999996964,11.5671105274568));
#283079=CARTESIAN_POINT('Ctrl Pts',(7.5167640777474,78.5749999996958,10.3459381770588));
#283080=CARTESIAN_POINT('Ctrl Pts',(9.83957192047849,78.7249999996952,7.14886745759505));
#283081=CARTESIAN_POINT('Ctrl Pts',(12.1623797632096,78.8749999996946,3.95179673813132));
#283082=CARTESIAN_POINT('Ctrl Pts',(12.1623797632096,79.024999999694,-1.48946194470292E-15));
#283083=CARTESIAN_POINT('Ctrl Pts',(12.1623797632096,79.1749999996934,-3.95179673813132));
#283084=CARTESIAN_POINT('Ctrl Pts',(9.83957192047849,79.3249999996928,-7.14886745759505));
#283085=CARTESIAN_POINT('Ctrl Pts',(7.5167640777474,79.4749999996922,-10.3459381770588));
#283086=CARTESIAN_POINT('Ctrl Pts',(3.75838203887367,79.6249999996916,-11.5671105274568));
#283087=CARTESIAN_POINT('Ctrl Pts',(-5.92033489524943E-14,79.774999999691,
-12.7882828778549));
#283088=CARTESIAN_POINT('Ctrl Pts',(-3.75838203887379,79.9249999996904,
-11.5671105274568));
#283089=CARTESIAN_POINT('Ctrl Pts',(-7.51676407774751,80.0749999996898,
-10.3459381770588));
#283090=CARTESIAN_POINT('Ctrl Pts',(-9.83957192047861,80.2249999996892,
-7.14886745759505));
#283091=CARTESIAN_POINT('Ctrl Pts',(-12.1623797632097,80.3749999996886,
-3.95179673813132));
#283092=CARTESIAN_POINT('Ctrl Pts',(-12.1623797632097,80.524999999688,2.97892388940585E-15));
#283093=CARTESIAN_POINT('Ctrl Pts',(-12.1623797632097,80.6749999996874,
3.95179673813133));
#283094=CARTESIAN_POINT('Ctrl Pts',(-9.83957192047861,80.8249999996868,
7.14886745759505));
#283095=CARTESIAN_POINT('Ctrl Pts',(-7.51676407774751,80.9749999996862,
10.3459381770588));
#283096=CARTESIAN_POINT('Ctrl Pts',(-3.75838203887378,81.1249999996856,
11.5671105274568));
#283097=CARTESIAN_POINT('Ctrl Pts',(-5.6934977649734E-14,81.274999999685,
12.7882828778549));
#283098=CARTESIAN_POINT('Ctrl Pts',(3.75838203887367,81.4249999996844,11.5671105274568));
#283099=CARTESIAN_POINT('Ctrl Pts',(7.5167640777474,81.5749999996838,10.3459381770588));
#283100=CARTESIAN_POINT('Ctrl Pts',(9.83957192047849,81.7249999996832,7.14886745759505));
#283101=CARTESIAN_POINT('Ctrl Pts',(12.1623797632096,81.8749999996826,3.95179673813132));
#283102=CARTESIAN_POINT('Ctrl Pts',(12.1623797632096,82.024999999682,-1.48946194470292E-15));
#283103=CARTESIAN_POINT('Ctrl Pts',(12.1623797632096,82.1749999996814,-3.95179673813132));
#283104=CARTESIAN_POINT('Ctrl Pts',(9.83957192047849,82.3249999996808,-7.14886745759505));
#283105=CARTESIAN_POINT('Ctrl Pts',(7.5167640777474,82.4749999996802,-10.3459381770588));
#283106=CARTESIAN_POINT('Ctrl Pts',(3.75838203887367,82.6249999996796,-11.5671105274568));
#283107=CARTESIAN_POINT('Ctrl Pts',(-6.09310582241561E-14,82.774999999679,
-12.7882828778549));
#283108=CARTESIAN_POINT('Ctrl Pts',(-3.75838203887379,82.9249999996784,
-11.5671105274568));
#283109=CARTESIAN_POINT('Ctrl Pts',(-7.51676407774752,83.0749999996778,
-10.3459381770588));
#283110=CARTESIAN_POINT('Ctrl Pts',(-9.83957192047861,83.2249999996772,
-7.14886745759505));
#283111=CARTESIAN_POINT('Ctrl Pts',(-12.1623797632097,83.3749999996766,
-3.95179673813132));
#283112=CARTESIAN_POINT('Ctrl Pts',(-12.1623797632097,83.524999999676,2.97892388940585E-15));
#283113=CARTESIAN_POINT('Ctrl Pts',(-12.1623797632097,83.6749999996754,
3.95179673813133));
#283114=CARTESIAN_POINT('Ctrl Pts',(-9.83957192047861,83.8249999996748,
7.14886745759505));
#283115=CARTESIAN_POINT('Ctrl Pts',(-7.51676407774751,83.9749999996742,
10.3459381770588));
#283116=CARTESIAN_POINT('Ctrl Pts',(-3.75838203887379,84.1249999996736,
11.5671105274568));
#283117=CARTESIAN_POINT('Ctrl Pts',(-5.86626869213958E-14,84.274999999673,
12.7882828778549));
#283118=CARTESIAN_POINT('Ctrl Pts',(3.75838203887367,84.4249999996724,11.5671105274568));
#283119=CARTESIAN_POINT('Ctrl Pts',(7.5167640777474,84.5749999996718,10.3459381770588));
#283120=CARTESIAN_POINT('Ctrl Pts',(9.83957192047849,84.7249999996712,7.14886745759505));
#283121=CARTESIAN_POINT('Ctrl Pts',(12.1623797632096,84.8749999996706,3.95179673813132));
#283122=CARTESIAN_POINT('Ctrl Pts',(12.1623797632096,85.02499999967,-1.48946194470292E-15));
#283123=CARTESIAN_POINT('Ctrl Pts',(12.1623797632096,85.1749999996694,-3.95179673813132));
#283124=CARTESIAN_POINT('Ctrl Pts',(9.83957192047849,85.3249999996688,-7.14886745759505));
#283125=CARTESIAN_POINT('Ctrl Pts',(7.51676407774739,85.4749999996682,-10.3459381770588));
#283126=CARTESIAN_POINT('Ctrl Pts',(3.75838203887367,85.6249999996676,-11.5671105274568));
#283127=CARTESIAN_POINT('Ctrl Pts',(-6.26587674958179E-14,85.774999999667,
-12.7882828778549));
#283128=CARTESIAN_POINT('Ctrl Pts',(-3.75838203887379,85.9249999996664,
-11.5671105274568));
#283129=CARTESIAN_POINT('Ctrl Pts',(-7.51676407774752,86.0749999996658,
-10.3459381770588));
#283130=CARTESIAN_POINT('Ctrl Pts',(-9.83957192047861,86.2249999996652,
-7.14886745759505));
#283131=CARTESIAN_POINT('Ctrl Pts',(-12.1623797632097,86.3749999996646,
-3.95179673813132));
#283132=CARTESIAN_POINT('Ctrl Pts',(-12.1623797632097,86.524999999664,2.97892388940585E-15));
#283133=CARTESIAN_POINT('Ctrl Pts',(-12.1623797632097,86.6749999996634,
3.95179673813133));
#283134=CARTESIAN_POINT('Ctrl Pts',(-9.83957192047861,86.8249999996628,
7.14886745759505));
#283135=CARTESIAN_POINT('Ctrl Pts',(-7.51676407774752,86.9749999996622,
10.3459381770588));
#283136=CARTESIAN_POINT('Ctrl Pts',(-3.75838203887379,87.1249999996616,
11.5671105274568));
#283137=CARTESIAN_POINT('Ctrl Pts',(-6.03903961930577E-14,87.274999999661,
12.7882828778549));
#283138=CARTESIAN_POINT('Ctrl Pts',(3.75838203887367,87.4249999996604,11.5671105274568));
#283139=CARTESIAN_POINT('Ctrl Pts',(7.5167640777474,87.5749999996598,10.3459381770588));
#283140=CARTESIAN_POINT('Ctrl Pts',(9.83957192047849,87.7249999996592,7.14886745759505));
#283141=CARTESIAN_POINT('Ctrl Pts',(12.1623797632096,87.8749999996586,3.95179673813132));
#283142=CARTESIAN_POINT('Ctrl Pts',(12.1623797632096,88.024999999658,-1.48946194470292E-15));
#283143=CARTESIAN_POINT('Ctrl Pts',(12.1623797632096,88.1749999996574,-3.95179673813132));
#283144=CARTESIAN_POINT('Ctrl Pts',(9.83957192047849,88.3249999996568,-7.14886745759505));
#283145=CARTESIAN_POINT('Ctrl Pts',(7.51676407774739,88.4749999996562,-10.3459381770588));
#283146=CARTESIAN_POINT('Ctrl Pts',(3.75838203887366,88.6249999996556,-11.5671105274568));
#283147=CARTESIAN_POINT('Ctrl Pts',(-6.43864767674798E-14,88.774999999655,
-12.7882828778549));
#283148=CARTESIAN_POINT('Ctrl Pts',(-3.75838203887379,88.9249999996544,
-11.5671105274568));
#283149=CARTESIAN_POINT('Ctrl Pts',(-7.51676407774752,89.0749999996538,
-10.3459381770588));
#283150=CARTESIAN_POINT('Ctrl Pts',(-9.83957192047861,89.2249999996532,
-7.14886745759505));
#283151=CARTESIAN_POINT('Ctrl Pts',(-12.1623797632097,89.3749999996526,
-3.95179673813132));
#283152=CARTESIAN_POINT('Ctrl Pts',(-12.1623797632097,89.524999999652,2.97892388940585E-15));
#283153=CARTESIAN_POINT('Ctrl Pts',(-12.1623797632097,89.6749999996514,
3.95179673813133));
#283154=CARTESIAN_POINT('Ctrl Pts',(-9.83957192047861,89.8249999996508,
7.14886745759505));
#283155=CARTESIAN_POINT('Ctrl Pts',(-7.51676407774752,89.9749999996502,
10.3459381770588));
#283156=CARTESIAN_POINT('Ctrl Pts',(-3.75838203887379,90.1249999996496,
11.5671105274568));
#283157=CARTESIAN_POINT('Ctrl Pts',(-6.21181054647195E-14,90.274999999649,
12.7882828778549));
#283158=CARTESIAN_POINT('Ctrl Pts',(3.75838203887366,90.4249999996484,11.5671105274568));
#283159=CARTESIAN_POINT('Ctrl Pts',(7.51676407774739,90.5749999996478,10.3459381770588));
#283160=CARTESIAN_POINT('Ctrl Pts',(9.83957192047848,90.7249999996472,7.14886745759505));
#283161=CARTESIAN_POINT('Ctrl Pts',(12.1623797632096,90.8749999996466,3.95179673813132));
#283162=CARTESIAN_POINT('Ctrl Pts',(12.1623797632096,91.024999999646,-1.48946194470292E-15));
#283163=CARTESIAN_POINT('Ctrl Pts',(12.1623797632096,91.1749999996454,-3.95179673813132));
#283164=CARTESIAN_POINT('Ctrl Pts',(9.83957192047848,91.3249999996448,-7.14886745759505));
#283165=CARTESIAN_POINT('Ctrl Pts',(7.51676407774739,91.4749999996442,-10.3459381770588));
#283166=CARTESIAN_POINT('Ctrl Pts',(3.75838203887366,91.6249999996436,-11.5671105274568));
#283167=CARTESIAN_POINT('Ctrl Pts',(-6.61141860391416E-14,91.774999999643,
-12.7882828778549));
#283168=CARTESIAN_POINT('Ctrl Pts',(-3.75838203887379,91.9249999996424,
-11.5671105274568));
#283169=CARTESIAN_POINT('Ctrl Pts',(-7.51676407774752,92.0749999996418,
-10.3459381770588));
#283170=CARTESIAN_POINT('Ctrl Pts',(-9.83957192047861,92.2249999996412,
-7.14886745759505));
#283171=CARTESIAN_POINT('Ctrl Pts',(-12.1623797632097,92.3749999996406,
-3.95179673813132));
#283172=CARTESIAN_POINT('Ctrl Pts',(-12.1623797632097,92.52499999964,2.97892388940585E-15));
#283173=CARTESIAN_POINT('Ctrl Pts',(-12.1623797632097,92.6749999996394,
3.95179673813133));
#283174=CARTESIAN_POINT('Ctrl Pts',(-9.83957192047861,92.8249999996388,
7.14886745759505));
#283175=CARTESIAN_POINT('Ctrl Pts',(-7.51676407774752,92.9749999996382,
10.3459381770588));
#283176=CARTESIAN_POINT('Ctrl Pts',(-3.75838203887379,93.1249999996376,
11.5671105274568));
#283177=CARTESIAN_POINT('Ctrl Pts',(-6.38458147363813E-14,93.274999999637,
12.7882828778549));
#283178=CARTESIAN_POINT('Ctrl Pts',(3.75838203887366,93.4249999996364,11.5671105274568));
#283179=CARTESIAN_POINT('Ctrl Pts',(7.51676407774739,93.5749999996358,10.3459381770588));
#283180=CARTESIAN_POINT('Ctrl Pts',(9.83957192047848,93.7249999996352,7.14886745759505));
#283181=CARTESIAN_POINT('Ctrl Pts',(12.1623797632096,93.8749999996346,3.95179673813132));
#283182=CARTESIAN_POINT('Ctrl Pts',(12.1623797632096,94.024999999634,-1.48946194470292E-15));
#283183=CARTESIAN_POINT('Ctrl Pts',(12.1623797632096,94.1749999996334,-3.95179673813132));
#283184=CARTESIAN_POINT('Ctrl Pts',(9.83957192047848,94.3249999996328,-7.14886745759505));
#283185=CARTESIAN_POINT('Ctrl Pts',(7.51676407774739,94.4749999996322,-10.3459381770588));
#283186=CARTESIAN_POINT('Ctrl Pts',(3.75838203887366,94.6249999996316,-11.5671105274568));
#283187=CARTESIAN_POINT('Ctrl Pts',(-6.78418953108034E-14,94.774999999631,
-12.7882828778549));
#283188=CARTESIAN_POINT('Ctrl Pts',(-3.7583820388738,94.9249999996304,-11.5671105274568));
#283189=CARTESIAN_POINT('Ctrl Pts',(-7.51676407774752,95.0749999996298,
-10.3459381770588));
#283190=CARTESIAN_POINT('Ctrl Pts',(-9.83957192047862,95.2249999996292,
-7.14886745759505));
#283191=CARTESIAN_POINT('Ctrl Pts',(-12.1623797632097,95.3749999996286,
-3.95179673813132));
#283192=CARTESIAN_POINT('Ctrl Pts',(-12.1623797632097,95.524999999628,2.97892388940585E-15));
#283193=CARTESIAN_POINT('Ctrl Pts',(-12.1623797632097,95.6749999996274,
3.95179673813133));
#283194=CARTESIAN_POINT('Ctrl Pts',(-9.83957192047862,95.8249999996268,
7.14886745759505));
#283195=CARTESIAN_POINT('Ctrl Pts',(-7.51676407774752,95.9749999996262,
10.3459381770588));
#283196=CARTESIAN_POINT('Ctrl Pts',(-3.75838203887379,96.1249999996256,
11.5671105274568));
#283197=CARTESIAN_POINT('Ctrl Pts',(-6.55735240080432E-14,96.274999999625,
12.7882828778549));
#283198=CARTESIAN_POINT('Ctrl Pts',(3.75838203887366,96.4249999996244,11.5671105274568));
#283199=CARTESIAN_POINT('Ctrl Pts',(7.51676407774739,96.5749999996238,10.3459381770588));
#283200=CARTESIAN_POINT('Ctrl Pts',(9.83957192047848,96.7249999996232,7.14886745759505));
#283201=CARTESIAN_POINT('Ctrl Pts',(12.1623797632096,96.8749999996226,3.95179673813132));
#283202=CARTESIAN_POINT('Ctrl Pts',(12.1623797632096,97.024999999622,-1.48946194470292E-15));
#283203=CARTESIAN_POINT('Ctrl Pts',(12.1623797632096,97.1749999996214,-3.95179673813132));
#283204=CARTESIAN_POINT('Ctrl Pts',(9.83957192047848,97.3249999996208,-7.14886745759505));
#283205=CARTESIAN_POINT('Ctrl Pts',(7.51676407774739,97.4749999996202,-10.3459381770588));
#283206=CARTESIAN_POINT('Ctrl Pts',(3.75838203887366,97.6249999996196,-11.5671105274568));
#283207=CARTESIAN_POINT('Ctrl Pts',(-6.95696045824653E-14,97.774999999619,
-12.7882828778549));
#283208=CARTESIAN_POINT('Ctrl Pts',(-3.7583820388738,97.9249999996184,-11.5671105274568));
#283209=CARTESIAN_POINT('Ctrl Pts',(-7.51676407774752,98.0749999996178,
-10.3459381770588));
#283210=CARTESIAN_POINT('Ctrl Pts',(-9.83957192047862,98.2249999996172,
-7.14886745759505));
#283211=CARTESIAN_POINT('Ctrl Pts',(-12.1623797632097,98.3749999996166,
-3.95179673813132));
#283212=CARTESIAN_POINT('Ctrl Pts',(-12.1623797632097,98.524999999616,2.97892388940585E-15));
#283213=CARTESIAN_POINT('Ctrl Pts',(-12.1623797632097,98.6749999996154,
3.95179673813133));
#283214=CARTESIAN_POINT('Ctrl Pts',(-9.83957192047862,98.8249999996148,
7.14886745759505));
#283215=CARTESIAN_POINT('Ctrl Pts',(-7.51676407774752,98.9749999996142,
10.3459381770588));
#283216=CARTESIAN_POINT('Ctrl Pts',(-3.7583820388738,99.1249999996136,11.5671105274568));
#283217=CARTESIAN_POINT('Ctrl Pts',(-6.7301233279705E-14,99.274999999613,
12.7882828778549));
#283218=CARTESIAN_POINT('Ctrl Pts',(3.75838203887366,99.4249999996124,11.5671105274568));
#283219=CARTESIAN_POINT('Ctrl Pts',(7.51676407774739,99.5749999996118,10.3459381770588));
#283220=CARTESIAN_POINT('Ctrl Pts',(9.83957192047848,99.7249999996112,7.14886745759505));
#283221=CARTESIAN_POINT('Ctrl Pts',(12.1623797632096,99.8749999996106,3.95179673813132));
#283222=CARTESIAN_POINT('Ctrl Pts',(12.1623797632096,100.02499999961,-1.48946194470292E-15));
#283223=CARTESIAN_POINT('Ctrl Pts',(12.1623797632096,100.174999999609,-3.95179673813132));
#283224=CARTESIAN_POINT('Ctrl Pts',(9.83957192047848,100.324999999609,-7.14886745759505));
#283225=CARTESIAN_POINT('Ctrl Pts',(7.51676407774738,100.474999999608,-10.3459381770588));
#283226=CARTESIAN_POINT('Ctrl Pts',(3.75838203887366,100.624999999608,-11.5671105274568));
#283227=CARTESIAN_POINT('Ctrl Pts',(-7.12973138541271E-14,100.774999999607,
-12.7882828778549));
#283228=CARTESIAN_POINT('Ctrl Pts',(-3.7583820388738,100.924999999606,-11.5671105274568));
#283229=CARTESIAN_POINT('Ctrl Pts',(-7.51676407774753,101.074999999606,
-10.3459381770588));
#283230=CARTESIAN_POINT('Ctrl Pts',(-9.83957192047862,101.224999999605,
-7.14886745759505));
#283231=CARTESIAN_POINT('Ctrl Pts',(-12.1623797632097,101.374999999605,
-3.95179673813132));
#283232=CARTESIAN_POINT('Ctrl Pts',(-12.1623797632097,101.524999999604,
2.97892388940585E-15));
#283233=CARTESIAN_POINT('Ctrl Pts',(-12.1623797632097,101.674999999603,
3.95179673813133));
#283234=CARTESIAN_POINT('Ctrl Pts',(-9.83957192047862,101.824999999603,
7.14886745759505));
#283235=CARTESIAN_POINT('Ctrl Pts',(-7.51676407774752,101.974999999602,
10.3459381770588));
#283236=CARTESIAN_POINT('Ctrl Pts',(-3.7583820388738,102.124999999602,11.5671105274568));
#283237=CARTESIAN_POINT('Ctrl Pts',(-6.90289425513669E-14,102.274999999601,
12.7882828778549));
#283238=CARTESIAN_POINT('Ctrl Pts',(3.75838203887366,102.4249999996,11.5671105274568));
#283239=CARTESIAN_POINT('Ctrl Pts',(7.51676407774739,102.5749999996,10.3459381770588));
#283240=CARTESIAN_POINT('Ctrl Pts',(9.83957192047848,102.724999999599,7.14886745759505));
#283241=CARTESIAN_POINT('Ctrl Pts',(12.1623797632096,102.874999999599,3.95179673813132));
#283242=CARTESIAN_POINT('Ctrl Pts',(12.1623797632096,103.024999999598,-1.48946194470292E-15));
#283243=CARTESIAN_POINT('Ctrl Pts',(12.1623797632096,103.174999999597,-3.95179673813132));
#283244=CARTESIAN_POINT('Ctrl Pts',(9.83957192047848,103.324999999597,-7.14886745759505));
#283245=CARTESIAN_POINT('Ctrl Pts',(7.51676407774738,103.474999999596,-10.3459381770588));
#283246=CARTESIAN_POINT('Ctrl Pts',(3.75838203887366,103.624999999596,-11.5671105274568));
#283247=CARTESIAN_POINT('Ctrl Pts',(-7.3025023125789E-14,103.774999999595,
-12.7882828778549));
#283248=CARTESIAN_POINT('Ctrl Pts',(-3.7583820388738,103.924999999594,-11.5671105274568));
#283249=CARTESIAN_POINT('Ctrl Pts',(-7.51676407774753,104.074999999594,
-10.3459381770588));
#283250=CARTESIAN_POINT('Ctrl Pts',(-9.83957192047862,104.224999999593,
-7.14886745759505));
#283251=CARTESIAN_POINT('Ctrl Pts',(-12.1623797632097,104.374999999593,
-3.95179673813132));
#283252=CARTESIAN_POINT('Ctrl Pts',(-12.1623797632097,104.524999999592,
2.97892388940585E-15));
#283253=CARTESIAN_POINT('Ctrl Pts',(-12.1623797632097,104.674999999591,
3.95179673813133));
#283254=CARTESIAN_POINT('Ctrl Pts',(-9.83957192047862,104.824999999591,
7.14886745759505));
#283255=CARTESIAN_POINT('Ctrl Pts',(-7.51676407774753,104.97499999959,10.3459381770588));
#283256=CARTESIAN_POINT('Ctrl Pts',(-3.7583820388738,105.12499999959,11.5671105274568));
#283257=CARTESIAN_POINT('Ctrl Pts',(-7.07566518230287E-14,105.274999999589,
12.7882828778549));
#283258=CARTESIAN_POINT('Ctrl Pts',(3.75838203887366,105.424999999588,11.5671105274568));
#283259=CARTESIAN_POINT('Ctrl Pts',(7.51676407774738,105.574999999588,10.3459381770588));
#283260=CARTESIAN_POINT('Ctrl Pts',(9.83957192047848,105.724999999587,7.14886745759505));
#283261=CARTESIAN_POINT('Ctrl Pts',(12.1623797632096,105.874999999587,3.95179673813132));
#283262=CARTESIAN_POINT('Ctrl Pts',(12.1623797632096,106.024999999586,-1.48946194470292E-15));
#283263=CARTESIAN_POINT('Ctrl Pts',(12.1623797632096,106.174999999585,-3.95179673813132));
#283264=CARTESIAN_POINT('Ctrl Pts',(9.83957192047848,106.324999999585,-7.14886745759505));
#283265=CARTESIAN_POINT('Ctrl Pts',(7.51676407774738,106.474999999584,-10.3459381770588));
#283266=CARTESIAN_POINT('Ctrl Pts',(3.75838203887365,106.624999999584,-11.5671105274568));
#283267=CARTESIAN_POINT('Ctrl Pts',(-7.47527323974508E-14,106.774999999583,
-12.7882828778549));
#283268=CARTESIAN_POINT('Ctrl Pts',(-3.7583820388738,106.924999999582,-11.5671105274568));
#283269=CARTESIAN_POINT('Ctrl Pts',(-7.51676407774753,107.074999999582,
-10.3459381770588));
#283270=CARTESIAN_POINT('Ctrl Pts',(-9.83957192047862,107.224999999581,
-7.14886745759505));
#283271=CARTESIAN_POINT('Ctrl Pts',(-12.1623797632097,107.374999999581,
-3.95179673813132));
#283272=CARTESIAN_POINT('Ctrl Pts',(-12.1623797632097,107.52499999958,2.97892388940585E-15));
#283273=CARTESIAN_POINT('Ctrl Pts',(-12.1623797632097,107.674999999579,
3.95179673813133));
#283274=CARTESIAN_POINT('Ctrl Pts',(-9.83957192047862,107.824999999579,
7.14886745759505));
#283275=CARTESIAN_POINT('Ctrl Pts',(-7.51676407774753,107.974999999578,
10.3459381770588));
#283276=CARTESIAN_POINT('Ctrl Pts',(-3.7583820388738,108.124999999578,11.5671105274568));
#283277=CARTESIAN_POINT('Ctrl Pts',(-7.24843610946905E-14,108.274999999577,
12.7882828778549));
#283278=CARTESIAN_POINT('Ctrl Pts',(3.75838203887366,108.424999999576,11.5671105274568));
#283279=CARTESIAN_POINT('Ctrl Pts',(7.51676407774738,108.574999999576,10.3459381770588));
#283280=CARTESIAN_POINT('Ctrl Pts',(9.83957192047847,108.724999999575,7.14886745759505));
#283281=CARTESIAN_POINT('Ctrl Pts',(12.1623797632096,108.874999999575,3.95179673813132));
#283282=CARTESIAN_POINT('Ctrl Pts',(12.1623797632096,109.024999999574,-1.48946194470292E-15));
#283283=CARTESIAN_POINT('Ctrl Pts',(12.1623797632096,109.174999999573,-3.95179673813132));
#283284=CARTESIAN_POINT('Ctrl Pts',(9.83957192047847,109.324999999573,-7.14886745759505));
#283285=CARTESIAN_POINT('Ctrl Pts',(7.51676407774738,109.474999999572,-10.3459381770588));
#283286=CARTESIAN_POINT('Ctrl Pts',(3.75838203887365,109.624999999572,-11.5671105274568));
#283287=CARTESIAN_POINT('Ctrl Pts',(-7.64804416691126E-14,109.774999999571,
-12.7882828778549));
#283288=CARTESIAN_POINT('Ctrl Pts',(-3.7583820388738,109.92499999957,-11.5671105274568));
#283289=CARTESIAN_POINT('Ctrl Pts',(-7.51676407774753,110.07499999957,-10.3459381770588));
#283290=CARTESIAN_POINT('Ctrl Pts',(-9.83957192047862,110.224999999569,
-7.14886745759505));
#283291=CARTESIAN_POINT('Ctrl Pts',(-12.1623797632097,110.374999999569,
-3.95179673813132));
#283292=CARTESIAN_POINT('Ctrl Pts',(-12.1623797632097,110.524999999568,
2.97892388940585E-15));
#283293=CARTESIAN_POINT('Ctrl Pts',(-12.1623797632097,110.674999999567,
3.95179673813133));
#283294=CARTESIAN_POINT('Ctrl Pts',(-9.83957192047862,110.824999999567,
7.14886745759505));
#283295=CARTESIAN_POINT('Ctrl Pts',(-7.51676407774753,110.974999999566,
10.3459381770588));
#283296=CARTESIAN_POINT('Ctrl Pts',(-3.7583820388738,111.124999999566,11.5671105274568));
#283297=CARTESIAN_POINT('Ctrl Pts',(-7.42120703663524E-14,111.274999999565,
12.7882828778549));
#283298=CARTESIAN_POINT('Ctrl Pts',(3.75838203887365,111.424999999564,11.5671105274568));
#283299=CARTESIAN_POINT('Ctrl Pts',(7.51676407774738,111.574999999564,10.3459381770588));
#283300=CARTESIAN_POINT('Ctrl Pts',(9.83957192047847,111.724999999563,7.14886745759505));
#283301=CARTESIAN_POINT('Ctrl Pts',(12.1623797632096,111.874999999563,3.95179673813132));
#283302=CARTESIAN_POINT('Ctrl Pts',(12.1623797632096,112.024999999562,-1.48946194470292E-15));
#283303=CARTESIAN_POINT('Ctrl Pts',(12.1623797632096,112.174999999561,-3.95179673813132));
#283304=CARTESIAN_POINT('Ctrl Pts',(9.83957192047847,112.324999999561,-7.14886745759505));
#283305=CARTESIAN_POINT('Ctrl Pts',(7.51676407774738,112.47499999956,-10.3459381770588));
#283306=CARTESIAN_POINT('Ctrl Pts',(3.75838203887365,112.62499999956,-11.5671105274568));
#283307=CARTESIAN_POINT('Ctrl Pts',(-7.82081509407745E-14,112.774999999559,
-12.7882828778549));
#283308=CARTESIAN_POINT('Ctrl Pts',(-3.75838203887381,112.924999999558,
-11.5671105274568));
#283309=CARTESIAN_POINT('Ctrl Pts',(-7.51676407774753,113.074999999558,
-10.3459381770588));
#283310=CARTESIAN_POINT('Ctrl Pts',(-9.83957192047863,113.224999999557,
-7.14886745759505));
#283311=CARTESIAN_POINT('Ctrl Pts',(-12.1623797632097,113.374999999557,
-3.95179673813132));
#283312=CARTESIAN_POINT('Ctrl Pts',(-12.1623797632097,113.524999999556,
2.97892388940585E-15));
#283313=CARTESIAN_POINT('Ctrl Pts',(-12.1623797632097,113.674999999555,
3.95179673813133));
#283314=CARTESIAN_POINT('Ctrl Pts',(-9.83957192047863,113.824999999555,
7.14886745759505));
#283315=CARTESIAN_POINT('Ctrl Pts',(-7.51676407774753,113.974999999554,
10.3459381770588));
#283316=CARTESIAN_POINT('Ctrl Pts',(-3.7583820388738,114.124999999554,11.5671105274568));
#283317=CARTESIAN_POINT('Ctrl Pts',(-7.59397796380142E-14,114.274999999553,
12.7882828778549));
#283318=CARTESIAN_POINT('Ctrl Pts',(3.75838203887365,114.424999999552,11.5671105274568));
#283319=CARTESIAN_POINT('Ctrl Pts',(7.51676407774738,114.574999999552,10.3459381770588));
#283320=CARTESIAN_POINT('Ctrl Pts',(9.83957192047847,114.724999999551,7.14886745759505));
#283321=CARTESIAN_POINT('Ctrl Pts',(12.1623797632096,114.874999999551,3.95179673813132));
#283322=CARTESIAN_POINT('Ctrl Pts',(12.1623797632096,115.02499999955,-1.48946194470292E-15));
#283323=CARTESIAN_POINT('Ctrl Pts',(12.1623797632096,115.174999999549,-3.95179673813132));
#283324=CARTESIAN_POINT('Ctrl Pts',(9.83957192047847,115.324999999549,-7.14886745759505));
#283325=CARTESIAN_POINT('Ctrl Pts',(7.51676407774738,115.474999999548,-10.3459381770588));
#283326=CARTESIAN_POINT('Ctrl Pts',(3.75838203887365,115.624999999548,-11.5671105274568));
#283327=CARTESIAN_POINT('Ctrl Pts',(-7.99358602124363E-14,115.774999999547,
-12.7882828778549));
#283328=CARTESIAN_POINT('Ctrl Pts',(-3.75838203887381,115.924999999546,
-11.5671105274568));
#283329=CARTESIAN_POINT('Ctrl Pts',(-7.51676407774754,116.074999999546,
-10.3459381770588));
#283330=CARTESIAN_POINT('Ctrl Pts',(-9.83957192047863,116.224999999545,
-7.14886745759505));
#283331=CARTESIAN_POINT('Ctrl Pts',(-12.1623797632097,116.374999999545,
-3.95179673813132));
#283332=CARTESIAN_POINT('Ctrl Pts',(-12.1623797632097,116.524999999544,
2.97892388940585E-15));
#283333=CARTESIAN_POINT('Ctrl Pts',(-12.1623797632097,116.674999999543,
3.95179673813133));
#283334=CARTESIAN_POINT('Ctrl Pts',(-9.83957192047863,116.824999999543,
7.14886745759505));
#283335=CARTESIAN_POINT('Ctrl Pts',(-7.51676407774753,116.974999999542,
10.3459381770588));
#283336=CARTESIAN_POINT('Ctrl Pts',(-3.75838203887381,117.124999999542,
11.5671105274568));
#283337=CARTESIAN_POINT('Ctrl Pts',(-7.76674889096761E-14,117.274999999541,
12.7882828778549));
#283338=CARTESIAN_POINT('Ctrl Pts',(3.75838203887365,117.42499999954,11.5671105274568));
#283339=CARTESIAN_POINT('Ctrl Pts',(7.51676407774738,117.57499999954,10.3459381770588));
#283340=CARTESIAN_POINT('Ctrl Pts',(9.83957192047847,117.724999999539,7.14886745759505));
#283341=CARTESIAN_POINT('Ctrl Pts',(12.1623797632096,117.874999999539,3.95179673813132));
#283342=CARTESIAN_POINT('Ctrl Pts',(12.1623797632096,118.024999999538,-1.48946194470292E-15));
#283343=CARTESIAN_POINT('Ctrl Pts',(12.1623797632096,118.174999999537,-3.95179673813132));
#283344=CARTESIAN_POINT('Ctrl Pts',(9.83957192047847,118.324999999537,-7.14886745759505));
#283345=CARTESIAN_POINT('Ctrl Pts',(7.51676407774737,118.474999999536,-10.3459381770588));
#283346=CARTESIAN_POINT('Ctrl Pts',(3.75838203887365,118.624999999536,-11.5671105274568));
#283347=CARTESIAN_POINT('Ctrl Pts',(-8.16635694840981E-14,118.774999999535,
-12.7882828778549));
#283348=CARTESIAN_POINT('Ctrl Pts',(-3.75838203887381,118.924999999534,
-11.5671105274568));
#283349=CARTESIAN_POINT('Ctrl Pts',(-7.51676407774754,119.074999999534,
-10.3459381770588));
#283350=CARTESIAN_POINT('Ctrl Pts',(-9.83957192047863,119.224999999533,
-7.14886745759505));
#283351=CARTESIAN_POINT('Ctrl Pts',(-12.1623797632097,119.374999999533,
-3.95179673813132));
#283352=CARTESIAN_POINT('Ctrl Pts',(-12.1623797632097,119.524999999532,
2.97892388940585E-15));
#283353=CARTESIAN_POINT('Ctrl Pts',(-12.1623797632097,119.674999999531,
3.95179673813133));
#283354=CARTESIAN_POINT('Ctrl Pts',(-9.83957192047863,119.824999999531,
7.14886745759505));
#283355=CARTESIAN_POINT('Ctrl Pts',(-7.51676407774754,119.97499999953,10.3459381770588));
#283356=CARTESIAN_POINT('Ctrl Pts',(-3.75838203887381,120.12499999953,11.5671105274568));
#283357=CARTESIAN_POINT('Ctrl Pts',(-7.93951981813379E-14,120.274999999529,
12.7882828778549));
#283358=CARTESIAN_POINT('Ctrl Pts',(3.75838203887365,120.424999999528,11.5671105274568));
#283359=CARTESIAN_POINT('Ctrl Pts',(7.51676407774738,120.574999999528,10.3459381770588));
#283360=CARTESIAN_POINT('Ctrl Pts',(9.83957192047847,120.724999999527,7.14886745759505));
#283361=CARTESIAN_POINT('Ctrl Pts',(12.1623797632096,120.874999999527,3.95179673813132));
#283362=CARTESIAN_POINT('Ctrl Pts',(12.1623797632096,121.024999999526,-1.48946194470292E-15));
#283363=CARTESIAN_POINT('Ctrl Pts',(12.1623797632096,121.174999999525,-3.95179673813132));
#283364=CARTESIAN_POINT('Ctrl Pts',(9.83957192047847,121.324999999525,-7.14886745759505));
#283365=CARTESIAN_POINT('Ctrl Pts',(7.51676407774737,121.474999999524,-10.3459381770588));
#283366=CARTESIAN_POINT('Ctrl Pts',(3.75838203887364,121.624999999524,-11.5671105274568));
#283367=CARTESIAN_POINT('Ctrl Pts',(-8.339127875576E-14,121.774999999523,
-12.7882828778549));
#283368=CARTESIAN_POINT('Ctrl Pts',(-3.75838203887381,121.924999999522,
-11.5671105274568));
#283369=CARTESIAN_POINT('Ctrl Pts',(-7.51676407774754,122.074999999522,
-10.3459381770588));
#283370=CARTESIAN_POINT('Ctrl Pts',(-9.83957192047863,122.224999999521,
-7.14886745759505));
#283371=CARTESIAN_POINT('Ctrl Pts',(-12.1623797632097,122.374999999521,
-3.95179673813132));
#283372=CARTESIAN_POINT('Ctrl Pts',(-12.1623797632097,122.52499999952,2.97892388940585E-15));
#283373=CARTESIAN_POINT('Ctrl Pts',(-12.1623797632097,122.674999999519,
3.95179673813133));
#283374=CARTESIAN_POINT('Ctrl Pts',(-9.83957192047863,122.824999999519,
7.14886745759505));
#283375=CARTESIAN_POINT('Ctrl Pts',(-7.51676407774754,122.974999999518,
10.3459381770588));
#283376=CARTESIAN_POINT('Ctrl Pts',(-3.75838203887381,123.124999999518,
11.5671105274568));
#283377=CARTESIAN_POINT('Ctrl Pts',(-8.11229074529997E-14,123.274999999517,
12.7882828778549));
#283378=CARTESIAN_POINT('Ctrl Pts',(3.75838203887365,123.424999999516,11.5671105274568));
#283379=CARTESIAN_POINT('Ctrl Pts',(7.51676407774737,123.574999999516,10.3459381770588));
#283380=CARTESIAN_POINT('Ctrl Pts',(9.83957192047846,123.724999999515,7.14886745759505));
#283381=CARTESIAN_POINT('Ctrl Pts',(12.1623797632096,123.874999999515,3.95179673813132));
#283382=CARTESIAN_POINT('Ctrl Pts',(12.1623797632096,124.024999999514,-1.48946194470292E-15));
#283383=CARTESIAN_POINT('Ctrl Pts',(12.1623797632096,124.174999999513,-3.95179673813132));
#283384=CARTESIAN_POINT('Ctrl Pts',(9.83957192047846,124.324999999513,-7.14886745759505));
#283385=CARTESIAN_POINT('Ctrl Pts',(7.51676407774737,124.474999999512,-10.3459381770588));
#283386=CARTESIAN_POINT('Ctrl Pts',(3.75838203887364,124.624999999512,-11.5671105274568));
#283387=CARTESIAN_POINT('Ctrl Pts',(-8.51189880274219E-14,124.774999999511,
-12.7882828778549));
#283388=CARTESIAN_POINT('Ctrl Pts',(-3.75838203887381,124.92499999951,-11.5671105274568));
#283389=CARTESIAN_POINT('Ctrl Pts',(-7.51676407774754,125.07499999951,-10.3459381770588));
#283390=CARTESIAN_POINT('Ctrl Pts',(-9.83957192047863,125.224999999509,
-7.14886745759505));
#283391=CARTESIAN_POINT('Ctrl Pts',(-12.1623797632097,125.374999999509,
-3.95179673813132));
#283392=CARTESIAN_POINT('Ctrl Pts',(-12.1623797632097,125.524999999508,
2.97892388940585E-15));
#283393=CARTESIAN_POINT('Ctrl Pts',(-12.1623797632097,125.674999999507,
3.95179673813133));
#283394=CARTESIAN_POINT('Ctrl Pts',(-9.83957192047863,125.824999999507,
7.14886745759505));
#283395=CARTESIAN_POINT('Ctrl Pts',(-7.51676407774754,125.974999999506,
10.3459381770588));
#283396=CARTESIAN_POINT('Ctrl Pts',(-3.75838203887381,126.124999999506,
11.5671105274568));
#283397=CARTESIAN_POINT('Ctrl Pts',(-8.28506167246616E-14,126.274999999505,
12.7882828778549));
#283398=CARTESIAN_POINT('Ctrl Pts',(3.75838203887364,126.424999999504,11.5671105274568));
#283399=CARTESIAN_POINT('Ctrl Pts',(7.51676407774737,126.574999999504,10.3459381770588));
#283400=CARTESIAN_POINT('Ctrl Pts',(9.83957192047846,126.724999999503,7.14886745759505));
#283401=CARTESIAN_POINT('Ctrl Pts',(12.1623797632096,126.874999999503,3.95179673813132));
#283402=CARTESIAN_POINT('Ctrl Pts',(12.1623797632096,127.024999999502,-1.48946194470292E-15));
#283403=CARTESIAN_POINT('Ctrl Pts',(12.1623797632096,127.174999999501,-3.95179673813132));
#283404=CARTESIAN_POINT('Ctrl Pts',(9.83957192047846,127.324999999501,-7.14886745759505));
#283405=CARTESIAN_POINT('Ctrl Pts',(7.51676407774737,127.4749999995,-10.3459381770588));
#283406=CARTESIAN_POINT('Ctrl Pts',(3.75838203887364,127.6249999995,-11.5671105274568));
#283407=CARTESIAN_POINT('Ctrl Pts',(-8.68466972990837E-14,127.774999999499,
-12.7882828778549));
#283408=CARTESIAN_POINT('Ctrl Pts',(-3.75838203887381,127.924999999498,
-11.5671105274568));
#283409=CARTESIAN_POINT('Ctrl Pts',(-7.51676407774754,128.074999999498,
-10.3459381770588));
#283410=CARTESIAN_POINT('Ctrl Pts',(-9.83957192047864,128.224999999497,
-7.14886745759505));
#283411=CARTESIAN_POINT('Ctrl Pts',(-12.1623797632097,128.374999999497,
-3.95179673813132));
#283412=CARTESIAN_POINT('Ctrl Pts',(-12.1623797632097,128.524999999496,
2.97892388940585E-15));
#283413=CARTESIAN_POINT('Ctrl Pts',(-12.1623797632097,128.674999999495,
3.95179673813133));
#283414=CARTESIAN_POINT('Ctrl Pts',(-9.83957192047864,128.824999999495,
7.14886745759505));
#283415=CARTESIAN_POINT('Ctrl Pts',(-7.51676407774754,128.974999999494,
10.3459381770588));
#283416=CARTESIAN_POINT('Ctrl Pts',(-3.75838203887381,129.124999999494,
11.5671105274568));
#283417=CARTESIAN_POINT('Ctrl Pts',(-8.45783259963234E-14,129.274999999493,
12.7882828778549));
#283418=CARTESIAN_POINT('Ctrl Pts',(3.75838203887364,129.424999999492,11.5671105274568));
#283419=CARTESIAN_POINT('Ctrl Pts',(7.51676407774737,129.574999999492,10.3459381770588));
#283420=CARTESIAN_POINT('Ctrl Pts',(9.83957192047846,129.724999999491,7.14886745759505));
#283421=CARTESIAN_POINT('Ctrl Pts',(12.1623797632096,129.874999999491,3.95179673813132));
#283422=CARTESIAN_POINT('Ctrl Pts',(12.1623797632096,130.02499999949,-1.48946194470292E-15));
#283423=CARTESIAN_POINT('Ctrl Pts',(12.1623797632096,130.174999999489,-3.95179673813132));
#283424=CARTESIAN_POINT('Ctrl Pts',(9.83957192047846,130.324999999489,-7.14886745759505));
#283425=CARTESIAN_POINT('Ctrl Pts',(7.51676407774737,130.474999999488,-10.3459381770588));
#283426=CARTESIAN_POINT('Ctrl Pts',(3.75838203887364,130.624999999488,-11.5671105274568));
#283427=CARTESIAN_POINT('Ctrl Pts',(-8.85744065707455E-14,130.774999999487,
-12.7882828778549));
#283428=CARTESIAN_POINT('Ctrl Pts',(-3.75838203887382,130.924999999486,
-11.5671105274568));
#283429=CARTESIAN_POINT('Ctrl Pts',(-7.51676407774754,131.074999999486,
-10.3459381770588));
#283430=CARTESIAN_POINT('Ctrl Pts',(-9.83957192047864,131.224999999485,
-7.14886745759505));
#283431=CARTESIAN_POINT('Ctrl Pts',(-12.1623797632097,131.374999999485,
-3.95179673813132));
#283432=CARTESIAN_POINT('Ctrl Pts',(-12.1623797632097,131.524999999484,
2.97892388940585E-15));
#283433=CARTESIAN_POINT('Ctrl Pts',(-12.1623797632097,131.674999999483,
3.95179673813133));
#283434=CARTESIAN_POINT('Ctrl Pts',(-9.83957192047864,131.824999999483,
7.14886745759505));
#283435=CARTESIAN_POINT('Ctrl Pts',(-7.51676407774754,131.974999999482,
10.3459381770588));
#283436=CARTESIAN_POINT('Ctrl Pts',(-3.75838203887381,132.124999999482,
11.5671105274568));
#283437=CARTESIAN_POINT('Ctrl Pts',(-8.63060352679853E-14,132.274999999481,
12.7882828778549));
#283438=CARTESIAN_POINT('Ctrl Pts',(3.75838203887364,132.42499999948,11.5671105274568));
#283439=CARTESIAN_POINT('Ctrl Pts',(7.51676407774737,132.57499999948,10.3459381770588));
#283440=CARTESIAN_POINT('Ctrl Pts',(9.83957192047846,132.724999999479,7.14886745759505));
#283441=CARTESIAN_POINT('Ctrl Pts',(12.1623797632096,132.874999999479,3.95179673813132));
#283442=CARTESIAN_POINT('Ctrl Pts',(12.1623797632096,133.024999999478,-1.48946194470292E-15));
#283443=CARTESIAN_POINT('Ctrl Pts',(12.1623797632096,133.174999999477,-3.95179673813132));
#283444=CARTESIAN_POINT('Ctrl Pts',(9.83957192047846,133.324999999477,-7.14886745759505));
#283445=CARTESIAN_POINT('Ctrl Pts',(7.51676407774736,133.474999999476,-10.3459381770588));
#283446=CARTESIAN_POINT('Ctrl Pts',(3.75838203887364,133.624999999476,-11.5671105274568));
#283447=CARTESIAN_POINT('Ctrl Pts',(-9.03021158424074E-14,133.774999999475,
-12.7882828778549));
#283448=CARTESIAN_POINT('Ctrl Pts',(-3.75838203887382,133.924999999474,
-11.5671105274568));
#283449=CARTESIAN_POINT('Ctrl Pts',(-7.51676407774755,134.074999999474,
-10.3459381770588));
#283450=CARTESIAN_POINT('Ctrl Pts',(-9.83957192047864,134.224999999473,
-7.14886745759505));
#283451=CARTESIAN_POINT('Ctrl Pts',(-12.1623797632097,134.374999999473,
-3.95179673813132));
#283452=CARTESIAN_POINT('Ctrl Pts',(-12.1623797632097,134.524999999472,
2.97892388940585E-15));
#283453=CARTESIAN_POINT('Ctrl Pts',(-12.1623797632097,134.674999999471,
3.95179673813133));
#283454=CARTESIAN_POINT('Ctrl Pts',(-9.83957192047864,134.824999999471,
7.14886745759505));
#283455=CARTESIAN_POINT('Ctrl Pts',(-7.51676407774754,134.97499999947,10.3459381770588));
#283456=CARTESIAN_POINT('Ctrl Pts',(-3.75838203887382,135.12499999947,11.5671105274568));
#283457=CARTESIAN_POINT('Ctrl Pts',(-8.80337445396471E-14,135.274999999469,
12.7882828778549));
#283458=CARTESIAN_POINT('Ctrl Pts',(3.75838203887364,135.424999999468,11.5671105274568));
#283459=CARTESIAN_POINT('Ctrl Pts',(7.51676407774737,135.574999999468,10.3459381770588));
#283460=CARTESIAN_POINT('Ctrl Pts',(9.83957192047846,135.724999999467,7.14886745759505));
#283461=CARTESIAN_POINT('Ctrl Pts',(12.1623797632096,135.874999999467,3.95179673813132));
#283462=CARTESIAN_POINT('Ctrl Pts',(12.1623797632096,136.024999999466,-1.48946194470292E-15));
#283463=CARTESIAN_POINT('Ctrl Pts',(12.1623797632095,136.174999999465,-3.95179673813132));
#283464=CARTESIAN_POINT('Ctrl Pts',(9.83957192047846,136.324999999465,-7.14886745759505));
#283465=CARTESIAN_POINT('Ctrl Pts',(7.51676407774736,136.474999999464,-10.3459381770588));
#283466=CARTESIAN_POINT('Ctrl Pts',(3.75838203887364,136.624999999464,-11.5671105274568));
#283467=CARTESIAN_POINT('Ctrl Pts',(-9.20298251140692E-14,136.774999999463,
-12.7882828778549));
#283468=CARTESIAN_POINT('Ctrl Pts',(-3.75838203887382,136.924999999462,
-11.5671105274568));
#283469=CARTESIAN_POINT('Ctrl Pts',(-7.51676407774755,137.074999999462,
-10.3459381770588));
#283470=CARTESIAN_POINT('Ctrl Pts',(-9.83957192047864,137.224999999461,
-7.14886745759505));
#283471=CARTESIAN_POINT('Ctrl Pts',(-12.1623797632097,137.374999999461,
-3.95179673813132));
#283472=CARTESIAN_POINT('Ctrl Pts',(-12.1623797632097,137.52499999946,2.97892388940585E-15));
#283473=CARTESIAN_POINT('Ctrl Pts',(-12.1623797632097,137.674999999459,
3.95179673813133));
#283474=CARTESIAN_POINT('Ctrl Pts',(-9.83957192047864,137.824999999459,
7.14886745759505));
#283475=CARTESIAN_POINT('Ctrl Pts',(-7.51676407774755,137.974999999458,
10.3459381770588));
#283476=CARTESIAN_POINT('Ctrl Pts',(-3.75838203887382,138.124999999458,
11.5671105274568));
#283477=CARTESIAN_POINT('Ctrl Pts',(-8.97614538113089E-14,138.274999999457,
12.7882828778549));
#283478=CARTESIAN_POINT('Ctrl Pts',(3.75838203887364,138.424999999456,11.5671105274568));
#283479=CARTESIAN_POINT('Ctrl Pts',(7.51676407774736,138.574999999456,10.3459381770588));
#283480=CARTESIAN_POINT('Ctrl Pts',(9.83957192047846,138.724999999455,7.14886745759505));
#283481=CARTESIAN_POINT('Ctrl Pts',(12.1623797632096,138.874999999455,3.95179673813132));
#283482=CARTESIAN_POINT('Ctrl Pts',(12.1623797632096,139.024999999454,-1.48946194470292E-15));
#283483=CARTESIAN_POINT('Ctrl Pts',(12.1623797632095,139.174999999453,-3.95179673813132));
#283484=CARTESIAN_POINT('Ctrl Pts',(9.83957192047846,139.324999999453,-7.14886745759505));
#283485=CARTESIAN_POINT('Ctrl Pts',(7.51676407774736,139.474999999452,-10.3459381770588));
#283486=CARTESIAN_POINT('Ctrl Pts',(3.75838203887363,139.624999999452,-11.5671105274568));
#283487=CARTESIAN_POINT('Ctrl Pts',(-9.3757534385731E-14,139.774999999451,
-12.7882828778549));
#283488=CARTESIAN_POINT('Ctrl Pts',(-3.75838203887382,139.92499999945,-11.5671105274568));
#283489=CARTESIAN_POINT('Ctrl Pts',(-7.51676407774755,140.07499999945,-10.3459381770588));
#283490=CARTESIAN_POINT('Ctrl Pts',(-9.83957192047864,140.224999999449,
-7.14886745759505));
#283491=CARTESIAN_POINT('Ctrl Pts',(-12.1623797632097,140.374999999449,
-3.95179673813132));
#283492=CARTESIAN_POINT('Ctrl Pts',(-12.1623797632097,140.524999999448,
2.97892388940585E-15));
#283493=CARTESIAN_POINT('Ctrl Pts',(-12.1623797632097,140.674999999447,
3.95179673813133));
#283494=CARTESIAN_POINT('Ctrl Pts',(-9.83957192047864,140.824999999447,
7.14886745759505));
#283495=CARTESIAN_POINT('Ctrl Pts',(-7.51676407774755,140.974999999446,
10.3459381770588));
#283496=CARTESIAN_POINT('Ctrl Pts',(-3.75838203887382,141.124999999446,
11.5671105274568));
#283497=CARTESIAN_POINT('Ctrl Pts',(-9.14891630829708E-14,141.274999999445,
12.7882828778549));
#283498=CARTESIAN_POINT('Ctrl Pts',(3.75838203887364,141.424999999444,11.5671105274568));
#283499=CARTESIAN_POINT('Ctrl Pts',(7.51676407774736,141.574999999444,10.3459381770588));
#283500=CARTESIAN_POINT('Ctrl Pts',(9.83957192047845,141.724999999443,7.14886745759505));
#283501=CARTESIAN_POINT('Ctrl Pts',(12.1623797632095,141.874999999443,3.95179673813132));
#283502=CARTESIAN_POINT('Ctrl Pts',(12.1623797632095,142.024999999442,-1.48946194470292E-15));
#283503=CARTESIAN_POINT('Ctrl Pts',(12.1623797632095,142.174999999441,-3.95179673813132));
#283504=CARTESIAN_POINT('Ctrl Pts',(9.83957192047845,142.324999999441,-7.14886745759505));
#283505=CARTESIAN_POINT('Ctrl Pts',(7.51676407774736,142.47499999944,-10.3459381770588));
#283506=CARTESIAN_POINT('Ctrl Pts',(3.75838203887363,142.62499999944,-11.5671105274568));
#283507=CARTESIAN_POINT('Ctrl Pts',(-9.54852436573929E-14,142.774999999439,
-12.7882828778549));
#283508=CARTESIAN_POINT('Ctrl Pts',(-3.75838203887382,142.924999999438,
-11.5671105274568));
#283509=CARTESIAN_POINT('Ctrl Pts',(-7.51676407774755,143.074999999438,
-10.3459381770588));
#283510=CARTESIAN_POINT('Ctrl Pts',(-9.83957192047864,143.224999999437,
-7.14886745759505));
#283511=CARTESIAN_POINT('Ctrl Pts',(-12.1623797632097,143.374999999437,
-3.95179673813132));
#283512=CARTESIAN_POINT('Ctrl Pts',(-12.1623797632097,143.524999999436,
2.97892388940585E-15));
#283513=CARTESIAN_POINT('Ctrl Pts',(-12.1623797632097,143.674999999435,
3.95179673813133));
#283514=CARTESIAN_POINT('Ctrl Pts',(-9.83957192047864,143.824999999435,
7.14886745759505));
#283515=CARTESIAN_POINT('Ctrl Pts',(-7.51676407774755,143.974999999434,
10.3459381770588));
#283516=CARTESIAN_POINT('Ctrl Pts',(-3.75838203887382,144.124999999434,
11.5671105274568));
#283517=CARTESIAN_POINT('Ctrl Pts',(-9.32168723546326E-14,144.274999999433,
12.7882828778549));
#283518=CARTESIAN_POINT('Ctrl Pts',(3.75838203887363,144.424999999432,11.5671105274568));
#283519=CARTESIAN_POINT('Ctrl Pts',(7.51676407774736,144.574999999432,10.3459381770588));
#283520=CARTESIAN_POINT('Ctrl Pts',(9.83957192047845,144.724999999431,7.14886745759505));
#283521=CARTESIAN_POINT('Ctrl Pts',(12.1623797632095,144.874999999431,3.95179673813132));
#283522=CARTESIAN_POINT('Ctrl Pts',(12.1623797632095,145.02499999943,-1.48946194470292E-15));
#283523=CARTESIAN_POINT('Ctrl Pts',(12.1623797632095,145.174999999429,-3.95179673813132));
#283524=CARTESIAN_POINT('Ctrl Pts',(9.83957192047845,145.324999999429,-7.14886745759505));
#283525=CARTESIAN_POINT('Ctrl Pts',(7.51676407774736,145.474999999428,-10.3459381770588));
#283526=CARTESIAN_POINT('Ctrl Pts',(3.75838203887363,145.624999999428,-11.5671105274568));
#283527=CARTESIAN_POINT('Ctrl Pts',(-9.72129529290547E-14,145.774999999427,
-12.7882828778549));
#283528=CARTESIAN_POINT('Ctrl Pts',(-3.75838203887382,145.924999999426,
-11.5671105274568));
#283529=CARTESIAN_POINT('Ctrl Pts',(-7.51676407774755,146.074999999426,
-10.3459381770588));
#283530=CARTESIAN_POINT('Ctrl Pts',(-9.83957192047865,146.224999999425,
-7.14886745759505));
#283531=CARTESIAN_POINT('Ctrl Pts',(-12.1623797632097,146.374999999425,
-3.95179673813132));
#283532=CARTESIAN_POINT('Ctrl Pts',(-12.1623797632097,146.524999999424,
2.97892388940585E-15));
#283533=CARTESIAN_POINT('Ctrl Pts',(-12.1623797632097,146.674999999423,
3.95179673813133));
#283534=CARTESIAN_POINT('Ctrl Pts',(-9.83957192047865,146.824999999423,
7.14886745759505));
#283535=CARTESIAN_POINT('Ctrl Pts',(-7.51676407774755,146.974999999422,
10.3459381770588));
#283536=CARTESIAN_POINT('Ctrl Pts',(-3.75838203887382,147.124999999422,
11.5671105274568));
#283537=CARTESIAN_POINT('Ctrl Pts',(-9.49445816262944E-14,147.274999999421,
12.7882828778549));
#283538=CARTESIAN_POINT('Ctrl Pts',(3.75838203887363,147.42499999942,11.5671105274568));
#283539=CARTESIAN_POINT('Ctrl Pts',(7.51676407774736,147.57499999942,10.3459381770588));
#283540=CARTESIAN_POINT('Ctrl Pts',(9.83957192047845,147.724999999419,7.14886745759505));
#283541=CARTESIAN_POINT('Ctrl Pts',(12.1623797632095,147.874999999419,3.95179673813132));
#283542=CARTESIAN_POINT('Ctrl Pts',(12.1623797632095,148.024999999418,-1.48946194470292E-15));
#283543=CARTESIAN_POINT('Ctrl Pts',(12.1623797632095,148.174999999417,-3.95179673813132));
#283544=CARTESIAN_POINT('Ctrl Pts',(9.83957192047845,148.324999999417,-7.14886745759505));
#283545=CARTESIAN_POINT('Ctrl Pts',(7.51676407774736,148.474999999416,-10.3459381770588));
#283546=CARTESIAN_POINT('Ctrl Pts',(3.75838203887363,148.624999999416,-11.5671105274568));
#283547=CARTESIAN_POINT('Ctrl Pts',(-9.89406622007166E-14,148.774999999415,
-12.7882828778549));
#283548=CARTESIAN_POINT('Ctrl Pts',(-3.75838203887383,148.924999999414,
-11.5671105274568));
#283549=CARTESIAN_POINT('Ctrl Pts',(-7.51676407774756,149.074999999414,
-10.3459381770588));
#283550=CARTESIAN_POINT('Ctrl Pts',(-9.83957192047865,149.224999999413,
-7.14886745759505));
#283551=CARTESIAN_POINT('Ctrl Pts',(-12.1623797632097,149.374999999413,
-3.95179673813132));
#283552=CARTESIAN_POINT('Ctrl Pts',(-12.1623797632097,149.524999999412,
2.97892388940585E-15));
#283553=CARTESIAN_POINT('Ctrl Pts',(-12.1623797632097,149.674999999411,
3.95179673813133));
#283554=CARTESIAN_POINT('Ctrl Pts',(-9.83957192047865,149.824999999411,
7.14886745759505));
#283555=CARTESIAN_POINT('Ctrl Pts',(-7.51676407774755,149.97499999941,10.3459381770588));
#283556=CARTESIAN_POINT('Ctrl Pts',(-3.75838203887382,150.12499999941,11.5671105274568));
#283557=CARTESIAN_POINT('Ctrl Pts',(-9.66722908979563E-14,150.274999999409,
12.7882828778549));
#283558=CARTESIAN_POINT('Ctrl Pts',(3.75838203887363,150.424999999408,11.5671105274568));
#283559=CARTESIAN_POINT('Ctrl Pts',(7.51676407774736,150.574999999408,10.3459381770588));
#283560=CARTESIAN_POINT('Ctrl Pts',(9.83957192047845,150.724999999407,7.14886745759505));
#283561=CARTESIAN_POINT('Ctrl Pts',(12.1623797632095,150.874999999407,3.95179673813132));
#283562=CARTESIAN_POINT('Ctrl Pts',(12.1623797632095,151.024999999406,-1.48946194470292E-15));
#283563=CARTESIAN_POINT('Ctrl Pts',(12.1623797632095,151.174999999405,-3.95179673813132));
#283564=CARTESIAN_POINT('Ctrl Pts',(9.83957192047845,151.324999999405,-7.14886745759505));
#283565=CARTESIAN_POINT('Ctrl Pts',(7.51676407774736,151.474999999404,-10.3459381770588));
#283566=CARTESIAN_POINT('Ctrl Pts',(3.75838203887363,151.624999999404,-11.5671105274568));
#283567=CARTESIAN_POINT('Ctrl Pts',(-1.00668371472378E-13,151.774999999403,
-12.7882828778549));
#283568=CARTESIAN_POINT('Ctrl Pts',(-3.75838203887383,151.924999999402,
-11.5671105274568));
#283569=CARTESIAN_POINT('Ctrl Pts',(-7.51676407774756,152.074999999402,
-10.3459381770588));
#283570=CARTESIAN_POINT('Ctrl Pts',(-9.83957192047865,152.224999999401,
-7.14886745759505));
#283571=CARTESIAN_POINT('Ctrl Pts',(-12.1623797632097,152.374999999401,
-3.95179673813132));
#283572=CARTESIAN_POINT('Ctrl Pts',(-12.1623797632097,152.5249999994,2.97892388940585E-15));
#283573=CARTESIAN_POINT('Ctrl Pts',(-12.1623797632097,152.674999999399,
3.95179673813133));
#283574=CARTESIAN_POINT('Ctrl Pts',(-9.83957192047865,152.824999999399,
7.14886745759505));
#283575=CARTESIAN_POINT('Ctrl Pts',(-7.51676407774756,152.974999999398,
10.3459381770588));
#283576=CARTESIAN_POINT('Ctrl Pts',(-3.75838203887383,153.124999999398,
11.5671105274568));
#283577=CARTESIAN_POINT('Ctrl Pts',(-9.84000001696181E-14,153.274999999397,
12.7882828778549));
#283578=CARTESIAN_POINT('Ctrl Pts',(3.75838203887363,153.424999999396,11.5671105274568));
#283579=CARTESIAN_POINT('Ctrl Pts',(7.51676407774736,153.574999999396,10.3459381770588));
#283580=CARTESIAN_POINT('Ctrl Pts',(9.83957192047845,153.724999999395,7.14886745759505));
#283581=CARTESIAN_POINT('Ctrl Pts',(12.1623797632095,153.874999999395,3.95179673813132));
#283582=CARTESIAN_POINT('Ctrl Pts',(12.1623797632095,154.024999999394,-1.48946194470292E-15));
#283583=CARTESIAN_POINT('Ctrl Pts',(12.1623797632095,154.174999999393,-3.95179673813132));
#283584=CARTESIAN_POINT('Ctrl Pts',(9.83957192047845,154.324999999393,-7.14886745759505));
#283585=CARTESIAN_POINT('Ctrl Pts',(7.51676407774735,154.474999999392,-10.3459381770588));
#283586=CARTESIAN_POINT('Ctrl Pts',(3.75838203887363,154.624999999392,-11.5671105274568));
#283587=CARTESIAN_POINT('Ctrl Pts',(-1.0239608074404E-13,154.774999999391,
-12.7882828778549));
#283588=CARTESIAN_POINT('Ctrl Pts',(-3.75838203887383,154.92499999939,-11.5671105274568));
#283589=CARTESIAN_POINT('Ctrl Pts',(10.0514428414942,2.80624999999926,-1.23094673026484E-15));
#283590=CARTESIAN_POINT('Ctrl Pts',(10.0514428414941,2.95624999999866,-3.26591175476071));
#283591=CARTESIAN_POINT('Ctrl Pts',(8.13178807675718,3.10624999999806,-5.90808986649102));
#283592=CARTESIAN_POINT('Ctrl Pts',(6.2121333120202,3.25624999999746,-8.55026797822134));
#283593=CARTESIAN_POINT('Ctrl Pts',(3.10606665601009,3.40624999999685,-9.5594902125713));
#283594=CARTESIAN_POINT('Ctrl Pts',(-1.51728257781496E-14,3.55624999999625,
-10.5687124469213));
#283595=CARTESIAN_POINT('Ctrl Pts',(-3.10606665601012,3.70624999999565,
-9.5594902125713));
#283596=CARTESIAN_POINT('Ctrl Pts',(-6.21213331202023,3.85624999999505,
-8.55026797822134));
#283597=CARTESIAN_POINT('Ctrl Pts',(-8.13178807675721,4.00624999999445,
-5.90808986649102));
#283598=CARTESIAN_POINT('Ctrl Pts',(-10.0514428414942,4.15624999999385,
-3.2659117547607));
#283599=CARTESIAN_POINT('Ctrl Pts',(-10.0514428414942,4.30624999999325,
2.46189346052968E-15));
#283600=CARTESIAN_POINT('Ctrl Pts',(-10.0514428414942,4.45624999999265,
3.26591175476071));
#283601=CARTESIAN_POINT('Ctrl Pts',(-8.13178807675721,4.60624999999205,
5.90808986649102));
#283602=CARTESIAN_POINT('Ctrl Pts',(-6.21213331202023,4.75624999999145,
8.55026797822134));
#283603=CARTESIAN_POINT('Ctrl Pts',(-3.10606665601012,4.90624999999085,
9.5594902125713));
#283604=CARTESIAN_POINT('Ctrl Pts',(-1.34480924401344E-14,5.05624999999025,
10.5687124469213));
#283605=CARTESIAN_POINT('Ctrl Pts',(3.10606665601009,5.20624999998966,9.5594902125713));
#283606=CARTESIAN_POINT('Ctrl Pts',(6.2121333120202,5.35624999998906,8.55026797822134));
#283607=CARTESIAN_POINT('Ctrl Pts',(8.13178807675718,5.50624999998846,5.90808986649102));
#283608=CARTESIAN_POINT('Ctrl Pts',(10.0514428414941,5.65624999998786,3.2659117547607));
#283609=CARTESIAN_POINT('Ctrl Pts',(10.0514428414941,5.80624999998726,-1.23094673026484E-15));
#283610=CARTESIAN_POINT('Ctrl Pts',(-12.1623797632103,-3.28749999997638,
2.97892388940601E-15));
#283611=CARTESIAN_POINT('Ctrl Pts',(-12.1623797632103,-3.13749999997698,
3.95179673813154));
#283612=CARTESIAN_POINT('Ctrl Pts',(-9.83957192047908,-2.98749999997758,
7.14886745759543));
#283613=CARTESIAN_POINT('Ctrl Pts',(-7.51676407774787,-2.83749999997817,
10.3459381770593));
#283614=CARTESIAN_POINT('Ctrl Pts',(-3.75838203887394,-2.68749999997877,
11.5671105274575));
#283615=CARTESIAN_POINT('Ctrl Pts',(-8.66709987268145E-15,-2.53749999997937,
12.7882828778556));
#283616=CARTESIAN_POINT('Ctrl Pts',(3.75838203887392,-2.38749999997997,
11.5671105274575));
#283617=CARTESIAN_POINT('Ctrl Pts',(7.51676407774785,-2.23749999998057,
10.3459381770593));
#283618=CARTESIAN_POINT('Ctrl Pts',(9.83957192047906,-2.08749999998117,
7.14886745759543));
#283619=CARTESIAN_POINT('Ctrl Pts',(12.1623797632103,-1.93749999998176,
3.95179673813153));
#283620=CARTESIAN_POINT('Ctrl Pts',(12.1623797632103,-1.78749999998236,
-1.489461944703E-15));
#283621=CARTESIAN_POINT('Ctrl Pts',(12.1623797632103,-1.63749999998296,
-3.95179673813154));
#283622=CARTESIAN_POINT('Ctrl Pts',(9.83957192047906,-1.48749999998357,
-7.14886745759543));
#283623=CARTESIAN_POINT('Ctrl Pts',(7.51676407774784,-1.33749999998417,
-10.3459381770593));
#283624=CARTESIAN_POINT('Ctrl Pts',(3.75838203887392,-1.18749999998477,
-11.5671105274575));
#283625=CARTESIAN_POINT('Ctrl Pts',(-1.26631804471037E-14,-1.03749999998537,
-12.7882828778556));
#283626=CARTESIAN_POINT('Ctrl Pts',(-3.75838203887394,-0.887499999985973,
-11.5671105274575));
#283627=CARTESIAN_POINT('Ctrl Pts',(-7.51676407774787,-0.737499999986575,
-10.3459381770593));
#283628=CARTESIAN_POINT('Ctrl Pts',(-9.83957192047909,-0.587499999987176,
-7.14886745759543));
#283629=CARTESIAN_POINT('Ctrl Pts',(-12.1623797632103,-0.437499999987778,
-3.95179673813153));
#283630=CARTESIAN_POINT('Ctrl Pts',(-12.1623797632103,-0.287499999988378,
2.97892388940601E-15));
#283631=CARTESIAN_POINT('Ctrl Pts',(-12.1623797632103,-0.137499999988978,
3.95179673813154));
#283632=CARTESIAN_POINT('Ctrl Pts',(-9.83957192047909,0.0125000000104236,
7.14886745759543));
#283633=CARTESIAN_POINT('Ctrl Pts',(-7.51676407774787,0.162500000009825,
10.3459381770593));
#283634=CARTESIAN_POINT('Ctrl Pts',(-3.75838203887394,0.312500000009227,
11.5671105274575));
#283635=CARTESIAN_POINT('Ctrl Pts',(-1.03948091443433E-14,0.462500000008629,
12.7882828778556));
#283636=CARTESIAN_POINT('Ctrl Pts',(3.75838203887392,0.612500000008031,
11.5671105274575));
#283637=CARTESIAN_POINT('Ctrl Pts',(7.51676407774785,0.762500000007433,
10.3459381770593));
#283638=CARTESIAN_POINT('Ctrl Pts',(9.83957192047906,0.912500000006835,
7.14886745759543));
#283639=CARTESIAN_POINT('Ctrl Pts',(12.1623797632103,1.06250000000624,3.95179673813153));
#283640=CARTESIAN_POINT('Ctrl Pts',(12.1623797632103,1.21250000000564,-1.489461944703E-15));
#283641=CARTESIAN_POINT('Ctrl Pts',(12.1623797632103,1.36250000000504,-3.95179673813154));
#283642=CARTESIAN_POINT('Ctrl Pts',(9.83957192047906,1.51250000000444,-7.14886745759543));
#283643=CARTESIAN_POINT('Ctrl Pts',(7.51676407774784,1.66250000000383,-10.3459381770593));
#283644=CARTESIAN_POINT('Ctrl Pts',(3.75838203887391,1.81250000000323,-11.5671105274575));
#283645=CARTESIAN_POINT('Ctrl Pts',(-1.43908897187656E-14,1.96250000000263,
-12.7882828778556));
#283646=CARTESIAN_POINT('Ctrl Pts',(-3.75838203887394,2.11250000000203,
-11.5671105274575));
#283647=CARTESIAN_POINT('Ctrl Pts',(-7.51676407774787,2.26250000000143,
-10.3459381770593));
#283648=CARTESIAN_POINT('Ctrl Pts',(-9.83957192047909,2.41250000000082,
-7.14886745759543));
#283649=CARTESIAN_POINT('Ctrl Pts',(-12.1623797632103,2.56250000000022,
-3.95179673813153));
#283650=CARTESIAN_POINT('Ctrl Pts',(-12.1623797632103,2.71249999999962,
2.97892388940601E-15));
#283651=CARTESIAN_POINT('Ctrl Pts',(-12.1623797632103,2.86249999999902,
3.95179673813154));
#283652=CARTESIAN_POINT('Ctrl Pts',(-9.83957192047909,3.01249999999842,
7.14886745759543));
#283653=CARTESIAN_POINT('Ctrl Pts',(-7.51676407774787,3.16249999999782,
10.3459381770593));
#283654=CARTESIAN_POINT('Ctrl Pts',(-3.75838203887394,3.31249999999723,
11.5671105274575));
#283655=CARTESIAN_POINT('Ctrl Pts',(-1.21225184160051E-14,3.46249999999663,
12.7882828778556));
#283656=CARTESIAN_POINT('Ctrl Pts',(3.75838203887392,3.61249999999603,11.5671105274575));
#283657=CARTESIAN_POINT('Ctrl Pts',(7.51676407774784,3.76249999999543,10.3459381770593));
#283658=CARTESIAN_POINT('Ctrl Pts',(9.83957192047906,3.91249999999483,7.14886745759543));
#283659=CARTESIAN_POINT('Ctrl Pts',(12.1623797632103,4.06249999999424,3.95179673813153));
#283660=CARTESIAN_POINT('Ctrl Pts',(12.1623797632103,4.21249999999364,-1.489461944703E-15));
#283661=CARTESIAN_POINT('Ctrl Pts',(12.1623797632103,4.36249999999303,-3.95179673813154));
#283662=CARTESIAN_POINT('Ctrl Pts',(9.83957192047906,4.51249999999243,-7.14886745759543));
#283663=CARTESIAN_POINT('Ctrl Pts',(7.51676407774784,4.66249999999183,-10.3459381770593));
#283664=CARTESIAN_POINT('Ctrl Pts',(3.75838203887391,4.81249999999123,-11.5671105274575));
#283665=CARTESIAN_POINT('Ctrl Pts',(-1.61185989904274E-14,4.96249999999063,
-12.7882828778556));
#283666=CARTESIAN_POINT('Ctrl Pts',(-3.75838203887394,5.11249999999003,
-11.5671105274575));
#283667=CARTESIAN_POINT('Ctrl Pts',(-7.51676407774788,5.26249999998942,
-10.3459381770593));
#283668=CARTESIAN_POINT('Ctrl Pts',(-9.83957192047909,5.41249999998882,
-7.14886745759543));
#283669=CARTESIAN_POINT('Ctrl Pts',(-12.1623797632103,5.56249999998822,
-3.95179673813153));
#283670=CARTESIAN_POINT('Ctrl Pts',(-12.1623797632103,5.71249999998762,
2.97892388940601E-15));
#283671=CARTESIAN_POINT('Ctrl Pts',(-12.1623797632103,5.86249999998702,
3.95179673813154));
#283672=CARTESIAN_POINT('Ctrl Pts',(-9.83957192047909,6.01249999998642,
7.14886745759543));
#283673=CARTESIAN_POINT('Ctrl Pts',(-7.51676407774787,6.16249999998582,
10.3459381770593));
#283674=CARTESIAN_POINT('Ctrl Pts',(-3.75838203887394,6.31249999998523,
11.5671105274575));
#283675=CARTESIAN_POINT('Ctrl Pts',(-1.3850227687667E-14,6.46249999998463,
12.7882828778556));
#283676=CARTESIAN_POINT('Ctrl Pts',(3.75838203887392,6.61249999998403,11.5671105274575));
#283677=CARTESIAN_POINT('Ctrl Pts',(7.51676407774784,6.76249999998343,10.3459381770593));
#283678=CARTESIAN_POINT('Ctrl Pts',(9.83957192047906,6.91249999998283,7.14886745759543));
#283679=CARTESIAN_POINT('Ctrl Pts',(12.1623797632103,7.06249999998224,3.95179673813153));
#283680=CARTESIAN_POINT('Ctrl Pts',(12.1623797632103,7.21249999998164,-1.489461944703E-15));
#283681=CARTESIAN_POINT('Ctrl Pts',(12.1623797632103,7.36249999998104,-3.95179673813154));
#283682=CARTESIAN_POINT('Ctrl Pts',(9.83957192047906,7.51249999998044,-7.14886745759543));
#283683=CARTESIAN_POINT('Ctrl Pts',(7.51676407774784,7.66249999997983,-10.3459381770593));
#283684=CARTESIAN_POINT('Ctrl Pts',(3.75838203887391,7.81249999997923,-11.5671105274575));
#283685=CARTESIAN_POINT('Ctrl Pts',(-1.78463082620892E-14,7.96249999997863,
-12.7882828778556));
#283686=CARTESIAN_POINT('Ctrl Pts',(-3.75838203887395,8.11249999997803,
-11.5671105274575));
#283687=CARTESIAN_POINT('Ctrl Pts',(-7.51676407774788,8.26249999997743,
-10.3459381770593));
#283688=CARTESIAN_POINT('Ctrl Pts',(-9.83957192047909,8.41249999997682,
-7.14886745759543));
#283689=CARTESIAN_POINT('Ctrl Pts',(-12.1623797632103,8.56249999997622,
-3.95179673813153));
#283690=CARTESIAN_POINT('Ctrl Pts',(-12.1623797632103,8.71249999997562,
2.97892388940601E-15));
#283691=CARTESIAN_POINT('Ctrl Pts',(-12.1623797632103,8.86249999997502,
3.95179673813154));
#283692=CARTESIAN_POINT('Ctrl Pts',(-9.83957192047909,9.01249999997442,
7.14886745759543));
#283693=CARTESIAN_POINT('Ctrl Pts',(-7.51676407774787,9.16249999997382,
10.3459381770593));
#283694=CARTESIAN_POINT('Ctrl Pts',(-3.75838203887394,9.31249999997323,
11.5671105274575));
#283695=CARTESIAN_POINT('Ctrl Pts',(-1.55779369593288E-14,9.46249999997263,
12.7882828778556));
#283696=CARTESIAN_POINT('Ctrl Pts',(3.75838203887391,9.61249999997203,11.5671105274575));
#283697=CARTESIAN_POINT('Ctrl Pts',(7.51676407774784,9.76249999997144,10.3459381770593));
#283698=CARTESIAN_POINT('Ctrl Pts',(9.83957192047906,9.91249999997084,7.14886745759543));
#283699=CARTESIAN_POINT('Ctrl Pts',(12.1623797632103,10.0624999999702,3.95179673813153));
#283700=CARTESIAN_POINT('Ctrl Pts',(12.1623797632103,10.2124999999696,-1.489461944703E-15));
#283701=CARTESIAN_POINT('Ctrl Pts',(12.1623797632103,10.362499999969,-3.95179673813154));
#283702=CARTESIAN_POINT('Ctrl Pts',(9.83957192047905,10.5124999999684,-7.14886745759543));
#283703=CARTESIAN_POINT('Ctrl Pts',(7.51676407774784,10.6624999999678,-10.3459381770593));
#283704=CARTESIAN_POINT('Ctrl Pts',(3.75838203887391,10.8124999999672,-11.5671105274575));
#283705=CARTESIAN_POINT('Ctrl Pts',(-1.95740175337511E-14,10.9624999999666,
-12.7882828778556));
#283706=CARTESIAN_POINT('Ctrl Pts',(-3.75838203887395,11.112499999966,-11.5671105274575));
#283707=CARTESIAN_POINT('Ctrl Pts',(-7.51676407774788,11.2624999999654,
-10.3459381770593));
#283708=CARTESIAN_POINT('Ctrl Pts',(-9.83957192047909,11.4124999999648,
-7.14886745759543));
#283709=CARTESIAN_POINT('Ctrl Pts',(-12.1623797632103,11.5624999999642,
-3.95179673813153));
#283710=CARTESIAN_POINT('Ctrl Pts',(-12.1623797632103,11.7124999999636,
2.97892388940601E-15));
#283711=CARTESIAN_POINT('Ctrl Pts',(-12.1623797632103,11.862499999963,3.95179673813154));
#283712=CARTESIAN_POINT('Ctrl Pts',(-9.83957192047909,12.0124999999624,
7.14886745759543));
#283713=CARTESIAN_POINT('Ctrl Pts',(-7.51676407774788,12.1624999999618,
10.3459381770593));
#283714=CARTESIAN_POINT('Ctrl Pts',(-3.75838203887395,12.3124999999612,
11.5671105274575));
#283715=CARTESIAN_POINT('Ctrl Pts',(-1.73056462309906E-14,12.4624999999606,
12.7882828778556));
#283716=CARTESIAN_POINT('Ctrl Pts',(3.75838203887391,12.61249999996,11.5671105274575));
#283717=CARTESIAN_POINT('Ctrl Pts',(7.51676407774784,12.7624999999594,10.3459381770593));
#283718=CARTESIAN_POINT('Ctrl Pts',(9.83957192047906,12.9124999999588,7.14886745759543));
#283719=CARTESIAN_POINT('Ctrl Pts',(12.1623797632103,13.0624999999582,3.95179673813153));
#283720=CARTESIAN_POINT('Ctrl Pts',(12.1623797632103,13.2124999999576,-1.489461944703E-15));
#283721=CARTESIAN_POINT('Ctrl Pts',(12.1623797632103,13.362499999957,-3.95179673813154));
#283722=CARTESIAN_POINT('Ctrl Pts',(9.83957192047905,13.5124999999564,-7.14886745759543));
#283723=CARTESIAN_POINT('Ctrl Pts',(7.51676407774784,13.6624999999558,-10.3459381770593));
#283724=CARTESIAN_POINT('Ctrl Pts',(3.75838203887391,13.8124999999552,-11.5671105274575));
#283725=CARTESIAN_POINT('Ctrl Pts',(-2.13017268054129E-14,13.9624999999546,
-12.7882828778556));
#283726=CARTESIAN_POINT('Ctrl Pts',(-3.75838203887395,14.112499999954,-11.5671105274575));
#283727=CARTESIAN_POINT('Ctrl Pts',(-7.51676407774788,14.2624999999534,
-10.3459381770593));
#283728=CARTESIAN_POINT('Ctrl Pts',(-9.8395719204791,14.4124999999528,-7.14886745759543));
#283729=CARTESIAN_POINT('Ctrl Pts',(-12.1623797632103,14.5624999999522,
-3.95179673813153));
#283730=CARTESIAN_POINT('Ctrl Pts',(-12.1623797632103,14.7124999999516,
2.97892388940601E-15));
#283731=CARTESIAN_POINT('Ctrl Pts',(-12.1623797632103,14.862499999951,3.95179673813154));
#283732=CARTESIAN_POINT('Ctrl Pts',(-9.83957192047909,15.0124999999504,
7.14886745759543));
#283733=CARTESIAN_POINT('Ctrl Pts',(-7.51676407774788,15.1624999999498,
10.3459381770593));
#283734=CARTESIAN_POINT('Ctrl Pts',(-3.75838203887395,15.3124999999492,
11.5671105274575));
#283735=CARTESIAN_POINT('Ctrl Pts',(-1.90333555026525E-14,15.4624999999486,
12.7882828778556));
#283736=CARTESIAN_POINT('Ctrl Pts',(3.75838203887391,15.612499999948,11.5671105274575));
#283737=CARTESIAN_POINT('Ctrl Pts',(7.51676407774784,15.7624999999474,10.3459381770593));
#283738=CARTESIAN_POINT('Ctrl Pts',(9.83957192047905,15.9124999999468,7.14886745759543));
#283739=CARTESIAN_POINT('Ctrl Pts',(12.1623797632103,16.0624999999462,3.95179673813153));
#283740=CARTESIAN_POINT('Ctrl Pts',(12.1623797632103,16.2124999999456,-1.489461944703E-15));
#283741=CARTESIAN_POINT('Ctrl Pts',(12.1623797632103,16.362499999945,-3.95179673813154));
#283742=CARTESIAN_POINT('Ctrl Pts',(9.83957192047905,16.5124999999444,-7.14886745759543));
#283743=CARTESIAN_POINT('Ctrl Pts',(7.51676407774784,16.6624999999438,-10.3459381770593));
#283744=CARTESIAN_POINT('Ctrl Pts',(3.75838203887391,16.8124999999432,-11.5671105274575));
#283745=CARTESIAN_POINT('Ctrl Pts',(-2.30294360770748E-14,16.9624999999426,
-12.7882828778556));
#283746=CARTESIAN_POINT('Ctrl Pts',(-3.75838203887395,17.112499999942,-11.5671105274575));
#283747=CARTESIAN_POINT('Ctrl Pts',(-7.51676407774788,17.2624999999414,
-10.3459381770593));
#283748=CARTESIAN_POINT('Ctrl Pts',(-9.8395719204791,17.4124999999408,-7.14886745759543));
#283749=CARTESIAN_POINT('Ctrl Pts',(-12.1623797632103,17.5624999999402,
-3.95179673813153));
#283750=CARTESIAN_POINT('Ctrl Pts',(-12.1623797632103,17.7124999999396,
2.97892388940601E-15));
#283751=CARTESIAN_POINT('Ctrl Pts',(-12.1623797632103,17.862499999939,3.95179673813154));
#283752=CARTESIAN_POINT('Ctrl Pts',(-9.8395719204791,18.0124999999384,7.14886745759543));
#283753=CARTESIAN_POINT('Ctrl Pts',(-7.51676407774788,18.1624999999378,
10.3459381770593));
#283754=CARTESIAN_POINT('Ctrl Pts',(-3.75838203887395,18.3124999999372,
11.5671105274575));
#283755=CARTESIAN_POINT('Ctrl Pts',(-2.07610647743143E-14,18.4624999999366,
12.7882828778556));
#283756=CARTESIAN_POINT('Ctrl Pts',(3.75838203887391,18.612499999936,11.5671105274575));
#283757=CARTESIAN_POINT('Ctrl Pts',(7.51676407774784,18.7624999999354,10.3459381770593));
#283758=CARTESIAN_POINT('Ctrl Pts',(9.83957192047905,18.9124999999348,7.14886745759543));
#283759=CARTESIAN_POINT('Ctrl Pts',(12.1623797632103,19.0624999999342,3.95179673813153));
#283760=CARTESIAN_POINT('Ctrl Pts',(12.1623797632103,19.2124999999336,-1.489461944703E-15));
#283761=CARTESIAN_POINT('Ctrl Pts',(12.1623797632103,19.362499999933,-3.95179673813154));
#283762=CARTESIAN_POINT('Ctrl Pts',(9.83957192047905,19.5124999999324,-7.14886745759543));
#283763=CARTESIAN_POINT('Ctrl Pts',(7.51676407774784,19.6624999999318,-10.3459381770593));
#283764=CARTESIAN_POINT('Ctrl Pts',(3.7583820388739,19.8124999999312,-11.5671105274575));
#283765=CARTESIAN_POINT('Ctrl Pts',(-2.47571453487366E-14,19.9624999999306,
-12.7882828778556));
#283766=CARTESIAN_POINT('Ctrl Pts',(-3.75838203887395,20.11249999993,-11.5671105274575));
#283767=CARTESIAN_POINT('Ctrl Pts',(-7.51676407774788,20.2624999999294,
-10.3459381770593));
#283768=CARTESIAN_POINT('Ctrl Pts',(-9.8395719204791,20.4124999999288,-7.14886745759543));
#283769=CARTESIAN_POINT('Ctrl Pts',(-12.1623797632103,20.5624999999282,
-3.95179673813153));
#283770=CARTESIAN_POINT('Ctrl Pts',(-12.1623797632103,20.7124999999276,
2.97892388940601E-15));
#283771=CARTESIAN_POINT('Ctrl Pts',(-12.1623797632103,20.862499999927,3.95179673813154));
#283772=CARTESIAN_POINT('Ctrl Pts',(-9.8395719204791,21.0124999999264,7.14886745759543));
#283773=CARTESIAN_POINT('Ctrl Pts',(-7.51676407774788,21.1624999999258,
10.3459381770593));
#283774=CARTESIAN_POINT('Ctrl Pts',(-3.75838203887395,21.3124999999252,
11.5671105274575));
#283775=CARTESIAN_POINT('Ctrl Pts',(-2.24887740459762E-14,21.4624999999246,
12.7882828778556));
#283776=CARTESIAN_POINT('Ctrl Pts',(3.75838203887391,21.612499999924,11.5671105274575));
#283777=CARTESIAN_POINT('Ctrl Pts',(7.51676407774784,21.7624999999234,10.3459381770593));
#283778=CARTESIAN_POINT('Ctrl Pts',(9.83957192047905,21.9124999999228,7.14886745759543));
#283779=CARTESIAN_POINT('Ctrl Pts',(12.1623797632103,22.0624999999222,3.95179673813153));
#283780=CARTESIAN_POINT('Ctrl Pts',(12.1623797632103,22.2124999999216,-1.489461944703E-15));
#283781=CARTESIAN_POINT('Ctrl Pts',(12.1623797632103,22.362499999921,-3.95179673813154));
#283782=CARTESIAN_POINT('Ctrl Pts',(9.83957192047905,22.5124999999204,-7.14886745759543));
#283783=CARTESIAN_POINT('Ctrl Pts',(7.51676407774783,22.6624999999198,-10.3459381770593));
#283784=CARTESIAN_POINT('Ctrl Pts',(3.7583820388739,22.8124999999192,-11.5671105274575));
#283785=CARTESIAN_POINT('Ctrl Pts',(-2.64848546203984E-14,22.9624999999186,
-12.7882828778556));
#283786=CARTESIAN_POINT('Ctrl Pts',(-3.75838203887396,23.112499999918,-11.5671105274575));
#283787=CARTESIAN_POINT('Ctrl Pts',(-7.51676407774788,23.2624999999174,
-10.3459381770593));
#283788=CARTESIAN_POINT('Ctrl Pts',(-9.8395719204791,23.4124999999168,-7.14886745759543));
#283789=CARTESIAN_POINT('Ctrl Pts',(-12.1623797632103,23.5624999999162,
-3.95179673813153));
#283790=CARTESIAN_POINT('Ctrl Pts',(-12.1623797632103,23.7124999999156,
2.97892388940601E-15));
#283791=CARTESIAN_POINT('Ctrl Pts',(-12.1623797632103,23.862499999915,3.95179673813154));
#283792=CARTESIAN_POINT('Ctrl Pts',(-9.8395719204791,24.0124999999144,7.14886745759543));
#283793=CARTESIAN_POINT('Ctrl Pts',(-7.51676407774788,24.1624999999138,
10.3459381770593));
#283794=CARTESIAN_POINT('Ctrl Pts',(-3.75838203887395,24.3124999999132,
11.5671105274575));
#283795=CARTESIAN_POINT('Ctrl Pts',(-2.4216483317638E-14,24.4624999999126,
12.7882828778556));
#283796=CARTESIAN_POINT('Ctrl Pts',(3.7583820388739,24.612499999912,11.5671105274575));
#283797=CARTESIAN_POINT('Ctrl Pts',(7.51676407774783,24.7624999999114,10.3459381770593));
#283798=CARTESIAN_POINT('Ctrl Pts',(9.83957192047905,24.9124999999108,7.14886745759543));
#283799=CARTESIAN_POINT('Ctrl Pts',(12.1623797632103,25.0624999999102,3.95179673813153));
#283800=CARTESIAN_POINT('Ctrl Pts',(12.1623797632103,25.2124999999096,-1.489461944703E-15));
#283801=CARTESIAN_POINT('Ctrl Pts',(12.1623797632103,25.362499999909,-3.95179673813154));
#283802=CARTESIAN_POINT('Ctrl Pts',(9.83957192047905,25.5124999999084,-7.14886745759543));
#283803=CARTESIAN_POINT('Ctrl Pts',(7.51676407774783,25.6624999999078,-10.3459381770593));
#283804=CARTESIAN_POINT('Ctrl Pts',(3.7583820388739,25.8124999999072,-11.5671105274575));
#283805=CARTESIAN_POINT('Ctrl Pts',(-2.82125638920603E-14,25.9624999999066,
-12.7882828778556));
#283806=CARTESIAN_POINT('Ctrl Pts',(-3.75838203887396,26.112499999906,-11.5671105274575));
#283807=CARTESIAN_POINT('Ctrl Pts',(-7.51676407774788,26.2624999999054,
-10.3459381770593));
#283808=CARTESIAN_POINT('Ctrl Pts',(-9.8395719204791,26.4124999999048,-7.14886745759543));
#283809=CARTESIAN_POINT('Ctrl Pts',(-12.1623797632103,26.5624999999042,
-3.95179673813153));
#283810=CARTESIAN_POINT('Ctrl Pts',(-12.1623797632103,26.7124999999036,
2.97892388940601E-15));
#283811=CARTESIAN_POINT('Ctrl Pts',(-12.1623797632103,26.862499999903,3.95179673813154));
#283812=CARTESIAN_POINT('Ctrl Pts',(-9.8395719204791,27.0124999999024,7.14886745759543));
#283813=CARTESIAN_POINT('Ctrl Pts',(-7.51676407774788,27.1624999999018,
10.3459381770593));
#283814=CARTESIAN_POINT('Ctrl Pts',(-3.75838203887396,27.3124999999012,
11.5671105274575));
#283815=CARTESIAN_POINT('Ctrl Pts',(-2.59441925892998E-14,27.4624999999006,
12.7882828778556));
#283816=CARTESIAN_POINT('Ctrl Pts',(3.7583820388739,27.6124999999,11.5671105274575));
#283817=CARTESIAN_POINT('Ctrl Pts',(7.51676407774783,27.7624999998994,10.3459381770593));
#283818=CARTESIAN_POINT('Ctrl Pts',(9.83957192047905,27.9124999998988,7.14886745759543));
#283819=CARTESIAN_POINT('Ctrl Pts',(12.1623797632103,28.0624999998982,3.95179673813153));
#283820=CARTESIAN_POINT('Ctrl Pts',(12.1623797632103,28.2124999998976,-1.489461944703E-15));
#283821=CARTESIAN_POINT('Ctrl Pts',(12.1623797632103,28.362499999897,-3.95179673813154));
#283822=CARTESIAN_POINT('Ctrl Pts',(9.83957192047905,28.5124999998964,-7.14886745759543));
#283823=CARTESIAN_POINT('Ctrl Pts',(7.51676407774783,28.6624999998958,-10.3459381770593));
#283824=CARTESIAN_POINT('Ctrl Pts',(3.7583820388739,28.8124999998952,-11.5671105274575));
#283825=CARTESIAN_POINT('Ctrl Pts',(-2.99402731637221E-14,28.9624999998946,
-12.7882828778556));
#283826=CARTESIAN_POINT('Ctrl Pts',(-3.75838203887396,29.112499999894,-11.5671105274575));
#283827=CARTESIAN_POINT('Ctrl Pts',(-7.51676407774789,29.2624999998934,
-10.3459381770593));
#283828=CARTESIAN_POINT('Ctrl Pts',(-9.8395719204791,29.4124999998928,-7.14886745759543));
#283829=CARTESIAN_POINT('Ctrl Pts',(-12.1623797632103,29.5624999998922,
-3.95179673813153));
#283830=CARTESIAN_POINT('Ctrl Pts',(-12.1623797632103,29.7124999998916,
2.97892388940601E-15));
#283831=CARTESIAN_POINT('Ctrl Pts',(-12.1623797632103,29.862499999891,3.95179673813154));
#283832=CARTESIAN_POINT('Ctrl Pts',(-9.8395719204791,30.0124999998904,7.14886745759543));
#283833=CARTESIAN_POINT('Ctrl Pts',(-7.51676407774788,30.1624999998898,
10.3459381770593));
#283834=CARTESIAN_POINT('Ctrl Pts',(-3.75838203887396,30.3124999998892,
11.5671105274575));
#283835=CARTESIAN_POINT('Ctrl Pts',(-2.76719018609617E-14,30.4624999998886,
12.7882828778556));
#283836=CARTESIAN_POINT('Ctrl Pts',(3.7583820388739,30.612499999888,11.5671105274575));
#283837=CARTESIAN_POINT('Ctrl Pts',(7.51676407774783,30.7624999998874,10.3459381770593));
#283838=CARTESIAN_POINT('Ctrl Pts',(9.83957192047905,30.9124999998868,7.14886745759543));
#283839=CARTESIAN_POINT('Ctrl Pts',(12.1623797632103,31.0624999998862,3.95179673813153));
#283840=CARTESIAN_POINT('Ctrl Pts',(12.1623797632103,31.2124999998856,-1.489461944703E-15));
#283841=CARTESIAN_POINT('Ctrl Pts',(12.1623797632103,31.362499999885,-3.95179673813154));
#283842=CARTESIAN_POINT('Ctrl Pts',(9.83957192047904,31.5124999998844,-7.14886745759543));
#283843=CARTESIAN_POINT('Ctrl Pts',(7.51676407774783,31.6624999998838,-10.3459381770593));
#283844=CARTESIAN_POINT('Ctrl Pts',(3.7583820388739,31.8124999998832,-11.5671105274575));
#283845=CARTESIAN_POINT('Ctrl Pts',(-3.16679824353839E-14,31.9624999998826,
-12.7882828778556));
#283846=CARTESIAN_POINT('Ctrl Pts',(-3.75838203887396,32.112499999882,-11.5671105274575));
#283847=CARTESIAN_POINT('Ctrl Pts',(-7.51676407774789,32.2624999998814,
-10.3459381770593));
#283848=CARTESIAN_POINT('Ctrl Pts',(-9.83957192047911,32.4124999998808,
-7.14886745759543));
#283849=CARTESIAN_POINT('Ctrl Pts',(-12.1623797632103,32.5624999998802,
-3.95179673813153));
#283850=CARTESIAN_POINT('Ctrl Pts',(-12.1623797632103,32.7124999998796,
2.97892388940601E-15));
#283851=CARTESIAN_POINT('Ctrl Pts',(-12.1623797632103,32.862499999879,3.95179673813154));
#283852=CARTESIAN_POINT('Ctrl Pts',(-9.8395719204791,33.0124999998784,7.14886745759543));
#283853=CARTESIAN_POINT('Ctrl Pts',(-7.51676407774789,33.1624999998778,
10.3459381770593));
#283854=CARTESIAN_POINT('Ctrl Pts',(-3.75838203887396,33.3124999998772,
11.5671105274575));
#283855=CARTESIAN_POINT('Ctrl Pts',(-2.93996111326235E-14,33.4624999998766,
12.7882828778556));
#283856=CARTESIAN_POINT('Ctrl Pts',(3.7583820388739,33.612499999876,11.5671105274575));
#283857=CARTESIAN_POINT('Ctrl Pts',(7.51676407774783,33.7624999998754,10.3459381770593));
#283858=CARTESIAN_POINT('Ctrl Pts',(9.83957192047905,33.9124999998748,7.14886745759543));
#283859=CARTESIAN_POINT('Ctrl Pts',(12.1623797632103,34.0624999998742,3.95179673813153));
#283860=CARTESIAN_POINT('Ctrl Pts',(12.1623797632103,34.2124999998736,-1.489461944703E-15));
#283861=CARTESIAN_POINT('Ctrl Pts',(12.1623797632103,34.362499999873,-3.95179673813154));
#283862=CARTESIAN_POINT('Ctrl Pts',(9.83957192047904,34.5124999998724,-7.14886745759543));
#283863=CARTESIAN_POINT('Ctrl Pts',(7.51676407774783,34.6624999998718,-10.3459381770593));
#283864=CARTESIAN_POINT('Ctrl Pts',(3.7583820388739,34.8124999998712,-11.5671105274575));
#283865=CARTESIAN_POINT('Ctrl Pts',(-3.33956917070458E-14,34.9624999998706,
-12.7882828778556));
#283866=CARTESIAN_POINT('Ctrl Pts',(-3.75838203887396,35.11249999987,-11.5671105274575));
#283867=CARTESIAN_POINT('Ctrl Pts',(-7.51676407774789,35.2624999998694,
-10.3459381770593));
#283868=CARTESIAN_POINT('Ctrl Pts',(-9.83957192047911,35.4124999998688,
-7.14886745759543));
#283869=CARTESIAN_POINT('Ctrl Pts',(-12.1623797632103,35.5624999998682,
-3.95179673813153));
#283870=CARTESIAN_POINT('Ctrl Pts',(-12.1623797632103,35.7124999998676,
2.97892388940601E-15));
#283871=CARTESIAN_POINT('Ctrl Pts',(-12.1623797632103,35.862499999867,3.95179673813154));
#283872=CARTESIAN_POINT('Ctrl Pts',(-9.83957192047911,36.0124999998664,
7.14886745759543));
#283873=CARTESIAN_POINT('Ctrl Pts',(-7.51676407774789,36.1624999998658,
10.3459381770593));
#283874=CARTESIAN_POINT('Ctrl Pts',(-3.75838203887396,36.3124999998652,
11.5671105274575));
#283875=CARTESIAN_POINT('Ctrl Pts',(-3.11273204042854E-14,36.4624999998646,
12.7882828778556));
#283876=CARTESIAN_POINT('Ctrl Pts',(3.7583820388739,36.612499999864,11.5671105274575));
#283877=CARTESIAN_POINT('Ctrl Pts',(7.51676407774783,36.7624999998634,10.3459381770593));
#283878=CARTESIAN_POINT('Ctrl Pts',(9.83957192047904,36.9124999998628,7.14886745759543));
#283879=CARTESIAN_POINT('Ctrl Pts',(12.1623797632103,37.0624999998622,3.95179673813153));
#283880=CARTESIAN_POINT('Ctrl Pts',(12.1623797632103,37.2124999998616,-1.489461944703E-15));
#283881=CARTESIAN_POINT('Ctrl Pts',(12.1623797632103,37.362499999861,-3.95179673813154));
#283882=CARTESIAN_POINT('Ctrl Pts',(9.83957192047904,37.5124999998604,-7.14886745759543));
#283883=CARTESIAN_POINT('Ctrl Pts',(7.51676407774782,37.6624999998598,-10.3459381770593));
#283884=CARTESIAN_POINT('Ctrl Pts',(3.75838203887389,37.8124999998592,-11.5671105274575));
#283885=CARTESIAN_POINT('Ctrl Pts',(-3.51234009787076E-14,37.9624999998586,
-12.7882828778556));
#283886=CARTESIAN_POINT('Ctrl Pts',(-3.75838203887396,38.112499999858,-11.5671105274575));
#283887=CARTESIAN_POINT('Ctrl Pts',(-7.51676407774789,38.2624999998574,
-10.3459381770593));
#283888=CARTESIAN_POINT('Ctrl Pts',(-9.83957192047911,38.4124999998568,
-7.14886745759543));
#283889=CARTESIAN_POINT('Ctrl Pts',(-12.1623797632103,38.5624999998562,
-3.95179673813153));
#283890=CARTESIAN_POINT('Ctrl Pts',(-12.1623797632103,38.7124999998556,
2.97892388940601E-15));
#283891=CARTESIAN_POINT('Ctrl Pts',(-12.1623797632103,38.862499999855,3.95179673813154));
#283892=CARTESIAN_POINT('Ctrl Pts',(-9.83957192047911,39.0124999998544,
7.14886745759543));
#283893=CARTESIAN_POINT('Ctrl Pts',(-7.51676407774789,39.1624999998538,
10.3459381770593));
#283894=CARTESIAN_POINT('Ctrl Pts',(-3.75838203887396,39.3124999998532,
11.5671105274575));
#283895=CARTESIAN_POINT('Ctrl Pts',(-3.28550296759472E-14,39.4624999998526,
12.7882828778556));
#283896=CARTESIAN_POINT('Ctrl Pts',(3.7583820388739,39.612499999852,11.5671105274575));
#283897=CARTESIAN_POINT('Ctrl Pts',(7.51676407774782,39.7624999998514,10.3459381770593));
#283898=CARTESIAN_POINT('Ctrl Pts',(9.83957192047904,39.9124999998508,7.14886745759543));
#283899=CARTESIAN_POINT('Ctrl Pts',(12.1623797632103,40.0624999998502,3.95179673813153));
#283900=CARTESIAN_POINT('Ctrl Pts',(12.1623797632103,40.2124999998496,-1.489461944703E-15));
#283901=CARTESIAN_POINT('Ctrl Pts',(12.1623797632103,40.362499999849,-3.95179673813154));
#283902=CARTESIAN_POINT('Ctrl Pts',(9.83957192047904,40.5124999998484,-7.14886745759543));
#283903=CARTESIAN_POINT('Ctrl Pts',(7.51676407774782,40.6624999998478,-10.3459381770593));
#283904=CARTESIAN_POINT('Ctrl Pts',(3.75838203887389,40.8124999998472,-11.5671105274575));
#283905=CARTESIAN_POINT('Ctrl Pts',(-3.68511102503695E-14,40.9624999998466,
-12.7882828778556));
#283906=CARTESIAN_POINT('Ctrl Pts',(-3.75838203887397,41.112499999846,-11.5671105274575));
#283907=CARTESIAN_POINT('Ctrl Pts',(-7.51676407774789,41.2624999998454,
-10.3459381770593));
#283908=CARTESIAN_POINT('Ctrl Pts',(-9.83957192047911,41.4124999998448,
-7.14886745759543));
#283909=CARTESIAN_POINT('Ctrl Pts',(-12.1623797632103,41.5624999998442,
-3.95179673813153));
#283910=CARTESIAN_POINT('Ctrl Pts',(-12.1623797632103,41.7124999998436,
2.97892388940601E-15));
#283911=CARTESIAN_POINT('Ctrl Pts',(-12.1623797632103,41.862499999843,3.95179673813154));
#283912=CARTESIAN_POINT('Ctrl Pts',(-9.83957192047911,42.0124999998424,
7.14886745759543));
#283913=CARTESIAN_POINT('Ctrl Pts',(-7.51676407774789,42.1624999998418,
10.3459381770593));
#283914=CARTESIAN_POINT('Ctrl Pts',(-3.75838203887396,42.3124999998412,
11.5671105274575));
#283915=CARTESIAN_POINT('Ctrl Pts',(-3.4582738947609E-14,42.4624999998406,
12.7882828778556));
#283916=CARTESIAN_POINT('Ctrl Pts',(3.75838203887389,42.61249999984,11.5671105274575));
#283917=CARTESIAN_POINT('Ctrl Pts',(7.51676407774782,42.7624999998394,10.3459381770593));
#283918=CARTESIAN_POINT('Ctrl Pts',(9.83957192047904,42.9124999998388,7.14886745759543));
#283919=CARTESIAN_POINT('Ctrl Pts',(12.1623797632103,43.0624999998382,3.95179673813153));
#283920=CARTESIAN_POINT('Ctrl Pts',(12.1623797632103,43.2124999998376,-1.489461944703E-15));
#283921=CARTESIAN_POINT('Ctrl Pts',(12.1623797632103,43.362499999837,-3.95179673813154));
#283922=CARTESIAN_POINT('Ctrl Pts',(9.83957192047903,43.5124999998364,-7.14886745759543));
#283923=CARTESIAN_POINT('Ctrl Pts',(7.51676407774782,43.6624999998358,-10.3459381770593));
#283924=CARTESIAN_POINT('Ctrl Pts',(3.75838203887389,43.8124999998352,-11.5671105274575));
#283925=CARTESIAN_POINT('Ctrl Pts',(-3.85788195220313E-14,43.9624999998346,
-12.7882828778556));
#283926=CARTESIAN_POINT('Ctrl Pts',(-3.75838203887397,44.112499999834,-11.5671105274575));
#283927=CARTESIAN_POINT('Ctrl Pts',(-7.5167640777479,44.2624999998334,-10.3459381770593));
#283928=CARTESIAN_POINT('Ctrl Pts',(-9.83957192047911,44.4124999998328,
-7.14886745759543));
#283929=CARTESIAN_POINT('Ctrl Pts',(-12.1623797632103,44.5624999998322,
-3.95179673813153));
#283930=CARTESIAN_POINT('Ctrl Pts',(-12.1623797632103,44.7124999998316,
2.97892388940601E-15));
#283931=CARTESIAN_POINT('Ctrl Pts',(-12.1623797632103,44.862499999831,3.95179673813154));
#283932=CARTESIAN_POINT('Ctrl Pts',(-9.83957192047911,45.0124999998304,
7.14886745759543));
#283933=CARTESIAN_POINT('Ctrl Pts',(-7.51676407774789,45.1624999998298,
10.3459381770593));
#283934=CARTESIAN_POINT('Ctrl Pts',(-3.75838203887397,45.3124999998292,
11.5671105274575));
#283935=CARTESIAN_POINT('Ctrl Pts',(-3.63104482192709E-14,45.4624999998286,
12.7882828778556));
#283936=CARTESIAN_POINT('Ctrl Pts',(3.75838203887389,45.612499999828,11.5671105274575));
#283937=CARTESIAN_POINT('Ctrl Pts',(7.51676407774782,45.7624999998274,10.3459381770593));
#283938=CARTESIAN_POINT('Ctrl Pts',(9.83957192047904,45.9124999998268,7.14886745759543));
#283939=CARTESIAN_POINT('Ctrl Pts',(12.1623797632103,46.0624999998262,3.95179673813153));
#283940=CARTESIAN_POINT('Ctrl Pts',(12.1623797632103,46.2124999998256,-1.489461944703E-15));
#283941=CARTESIAN_POINT('Ctrl Pts',(12.1623797632103,46.362499999825,-3.95179673813154));
#283942=CARTESIAN_POINT('Ctrl Pts',(9.83957192047903,46.5124999998244,-7.14886745759543));
#283943=CARTESIAN_POINT('Ctrl Pts',(7.51676407774782,46.6624999998238,-10.3459381770593));
#283944=CARTESIAN_POINT('Ctrl Pts',(3.75838203887389,46.8124999998232,-11.5671105274575));
#283945=CARTESIAN_POINT('Ctrl Pts',(-4.03065287936931E-14,46.9624999998226,
-12.7882828778556));
#283946=CARTESIAN_POINT('Ctrl Pts',(-3.75838203887397,47.112499999822,-11.5671105274575));
#283947=CARTESIAN_POINT('Ctrl Pts',(-7.5167640777479,47.2624999998214,-10.3459381770593));
#283948=CARTESIAN_POINT('Ctrl Pts',(-9.83957192047912,47.4124999998208,
-7.14886745759543));
#283949=CARTESIAN_POINT('Ctrl Pts',(-12.1623797632103,47.5624999998202,
-3.95179673813153));
#283950=CARTESIAN_POINT('Ctrl Pts',(-12.1623797632103,47.7124999998196,
2.97892388940601E-15));
#283951=CARTESIAN_POINT('Ctrl Pts',(-12.1623797632103,47.862499999819,3.95179673813154));
#283952=CARTESIAN_POINT('Ctrl Pts',(-9.83957192047911,48.0124999998184,
7.14886745759543));
#283953=CARTESIAN_POINT('Ctrl Pts',(-7.51676407774789,48.1624999998178,
10.3459381770593));
#283954=CARTESIAN_POINT('Ctrl Pts',(-3.75838203887397,48.3124999998172,
11.5671105274575));
#283955=CARTESIAN_POINT('Ctrl Pts',(-3.80381574909327E-14,48.4624999998166,
12.7882828778556));
#283956=CARTESIAN_POINT('Ctrl Pts',(3.75838203887389,48.612499999816,11.5671105274575));
#283957=CARTESIAN_POINT('Ctrl Pts',(7.51676407774782,48.7624999998154,10.3459381770593));
#283958=CARTESIAN_POINT('Ctrl Pts',(9.83957192047903,48.9124999998148,7.14886745759543));
#283959=CARTESIAN_POINT('Ctrl Pts',(12.1623797632103,49.0624999998142,3.95179673813153));
#283960=CARTESIAN_POINT('Ctrl Pts',(12.1623797632103,49.2124999998136,-1.489461944703E-15));
#283961=CARTESIAN_POINT('Ctrl Pts',(12.1623797632103,49.362499999813,-3.95179673813154));
#283962=CARTESIAN_POINT('Ctrl Pts',(9.83957192047903,49.5124999998124,-7.14886745759543));
#283963=CARTESIAN_POINT('Ctrl Pts',(7.51676407774782,49.6624999998118,-10.3459381770593));
#283964=CARTESIAN_POINT('Ctrl Pts',(3.75838203887389,49.8124999998112,-11.5671105274575));
#283965=CARTESIAN_POINT('Ctrl Pts',(-4.2034238065355E-14,49.9624999998106,
-12.7882828778556));
#283966=CARTESIAN_POINT('Ctrl Pts',(-3.75838203887397,50.11249999981,-11.5671105274575));
#283967=CARTESIAN_POINT('Ctrl Pts',(-7.5167640777479,50.2624999998094,-10.3459381770593));
#283968=CARTESIAN_POINT('Ctrl Pts',(-9.83957192047912,50.4124999998088,
-7.14886745759543));
#283969=CARTESIAN_POINT('Ctrl Pts',(-12.1623797632103,50.5624999998082,
-3.95179673813153));
#283970=CARTESIAN_POINT('Ctrl Pts',(-12.1623797632103,50.7124999998076,
2.97892388940601E-15));
#283971=CARTESIAN_POINT('Ctrl Pts',(-12.1623797632103,50.862499999807,3.95179673813154));
#283972=CARTESIAN_POINT('Ctrl Pts',(-9.83957192047912,51.0124999998064,
7.14886745759543));
#283973=CARTESIAN_POINT('Ctrl Pts',(-7.5167640777479,51.1624999998058,10.3459381770593));
#283974=CARTESIAN_POINT('Ctrl Pts',(-3.75838203887397,51.3124999998052,
11.5671105274575));
#283975=CARTESIAN_POINT('Ctrl Pts',(-3.97658667625946E-14,51.4624999998046,
12.7882828778556));
#283976=CARTESIAN_POINT('Ctrl Pts',(3.75838203887389,51.612499999804,11.5671105274575));
#283977=CARTESIAN_POINT('Ctrl Pts',(7.51676407774782,51.7624999998034,10.3459381770593));
#283978=CARTESIAN_POINT('Ctrl Pts',(9.83957192047903,51.9124999998028,7.14886745759543));
#283979=CARTESIAN_POINT('Ctrl Pts',(12.1623797632103,52.0624999998022,3.95179673813153));
#283980=CARTESIAN_POINT('Ctrl Pts',(12.1623797632103,52.2124999998016,-1.489461944703E-15));
#283981=CARTESIAN_POINT('Ctrl Pts',(12.1623797632103,52.362499999801,-3.95179673813154));
#283982=CARTESIAN_POINT('Ctrl Pts',(9.83957192047903,52.5124999998004,-7.14886745759543));
#283983=CARTESIAN_POINT('Ctrl Pts',(7.51676407774781,52.6624999997998,-10.3459381770593));
#283984=CARTESIAN_POINT('Ctrl Pts',(3.75838203887388,52.8124999997992,-11.5671105274575));
#283985=CARTESIAN_POINT('Ctrl Pts',(-4.37619473370168E-14,52.9624999997986,
-12.7882828778556));
#283986=CARTESIAN_POINT('Ctrl Pts',(-3.75838203887397,53.112499999798,-11.5671105274575));
#283987=CARTESIAN_POINT('Ctrl Pts',(-7.5167640777479,53.2624999997974,-10.3459381770593));
#283988=CARTESIAN_POINT('Ctrl Pts',(-9.83957192047912,53.4124999997968,
-7.14886745759543));
#283989=CARTESIAN_POINT('Ctrl Pts',(-12.1623797632103,53.5624999997962,
-3.95179673813153));
#283990=CARTESIAN_POINT('Ctrl Pts',(-12.1623797632103,53.7124999997956,
2.97892388940601E-15));
#283991=CARTESIAN_POINT('Ctrl Pts',(-12.1623797632103,53.862499999795,3.95179673813154));
#283992=CARTESIAN_POINT('Ctrl Pts',(-9.83957192047912,54.0124999997944,
7.14886745759543));
#283993=CARTESIAN_POINT('Ctrl Pts',(-7.5167640777479,54.1624999997938,10.3459381770593));
#283994=CARTESIAN_POINT('Ctrl Pts',(-3.75838203887397,54.3124999997932,
11.5671105274575));
#283995=CARTESIAN_POINT('Ctrl Pts',(-4.14935760342564E-14,54.4624999997926,
12.7882828778556));
#283996=CARTESIAN_POINT('Ctrl Pts',(3.75838203887389,54.612499999792,11.5671105274575));
#283997=CARTESIAN_POINT('Ctrl Pts',(7.51676407774782,54.7624999997914,10.3459381770593));
#283998=CARTESIAN_POINT('Ctrl Pts',(9.83957192047903,54.9124999997908,7.14886745759543));
#283999=CARTESIAN_POINT('Ctrl Pts',(12.1623797632103,55.0624999997902,3.95179673813153));
#284000=CARTESIAN_POINT('Ctrl Pts',(12.1623797632103,55.2124999997896,-1.489461944703E-15));
#284001=CARTESIAN_POINT('Ctrl Pts',(12.1623797632103,55.362499999789,-3.95179673813154));
#284002=CARTESIAN_POINT('Ctrl Pts',(9.83957192047903,55.5124999997884,-7.14886745759543));
#284003=CARTESIAN_POINT('Ctrl Pts',(7.51676407774781,55.6624999997878,-10.3459381770593));
#284004=CARTESIAN_POINT('Ctrl Pts',(3.75838203887388,55.8124999997872,-11.5671105274575));
#284005=CARTESIAN_POINT('Ctrl Pts',(-4.54896566086787E-14,55.9624999997866,
-12.7882828778556));
#284006=CARTESIAN_POINT('Ctrl Pts',(-3.75838203887397,56.112499999786,-11.5671105274575));
#284007=CARTESIAN_POINT('Ctrl Pts',(-7.5167640777479,56.2624999997854,-10.3459381770593));
#284008=CARTESIAN_POINT('Ctrl Pts',(-9.83957192047912,56.4124999997848,
-7.14886745759543));
#284009=CARTESIAN_POINT('Ctrl Pts',(-12.1623797632103,56.5624999997842,
-3.95179673813153));
#284010=CARTESIAN_POINT('Ctrl Pts',(-12.1623797632103,56.7124999997836,
2.97892388940601E-15));
#284011=CARTESIAN_POINT('Ctrl Pts',(-12.1623797632103,56.862499999783,3.95179673813154));
#284012=CARTESIAN_POINT('Ctrl Pts',(-9.83957192047912,57.0124999997824,
7.14886745759543));
#284013=CARTESIAN_POINT('Ctrl Pts',(-7.5167640777479,57.1624999997818,10.3459381770593));
#284014=CARTESIAN_POINT('Ctrl Pts',(-3.75838203887397,57.3124999997812,
11.5671105274575));
#284015=CARTESIAN_POINT('Ctrl Pts',(-4.32212853059182E-14,57.4624999997806,
12.7882828778556));
#284016=CARTESIAN_POINT('Ctrl Pts',(3.75838203887389,57.61249999978,11.5671105274575));
#284017=CARTESIAN_POINT('Ctrl Pts',(7.51676407774781,57.7624999997794,10.3459381770593));
#284018=CARTESIAN_POINT('Ctrl Pts',(9.83957192047903,57.9124999997788,7.14886745759543));
#284019=CARTESIAN_POINT('Ctrl Pts',(12.1623797632103,58.0624999997782,3.95179673813153));
#284020=CARTESIAN_POINT('Ctrl Pts',(12.1623797632102,58.2124999997776,-1.489461944703E-15));
#284021=CARTESIAN_POINT('Ctrl Pts',(12.1623797632102,58.362499999777,-3.95179673813154));
#284022=CARTESIAN_POINT('Ctrl Pts',(9.83957192047903,58.5124999997764,-7.14886745759543));
#284023=CARTESIAN_POINT('Ctrl Pts',(7.51676407774781,58.6624999997758,-10.3459381770593));
#284024=CARTESIAN_POINT('Ctrl Pts',(3.75838203887388,58.8124999997752,-11.5671105274575));
#284025=CARTESIAN_POINT('Ctrl Pts',(-4.72173658803405E-14,58.9624999997746,
-12.7882828778556));
#284026=CARTESIAN_POINT('Ctrl Pts',(-3.75838203887398,59.112499999774,-11.5671105274575));
#284027=CARTESIAN_POINT('Ctrl Pts',(-7.51676407774791,59.2624999997734,
-10.3459381770593));
#284028=CARTESIAN_POINT('Ctrl Pts',(-9.83957192047912,59.4124999997728,
-7.14886745759543));
#284029=CARTESIAN_POINT('Ctrl Pts',(-12.1623797632103,59.5624999997722,
-3.95179673813153));
#284030=CARTESIAN_POINT('Ctrl Pts',(-12.1623797632103,59.7124999997716,
2.97892388940601E-15));
#284031=CARTESIAN_POINT('Ctrl Pts',(-12.1623797632103,59.862499999771,3.95179673813154));
#284032=CARTESIAN_POINT('Ctrl Pts',(-9.83957192047912,60.0124999997704,
7.14886745759543));
#284033=CARTESIAN_POINT('Ctrl Pts',(-7.5167640777479,60.1624999997698,10.3459381770593));
#284034=CARTESIAN_POINT('Ctrl Pts',(-3.75838203887397,60.3124999997692,
11.5671105274575));
#284035=CARTESIAN_POINT('Ctrl Pts',(-4.49489945775801E-14,60.4624999997686,
12.7882828778556));
#284036=CARTESIAN_POINT('Ctrl Pts',(3.75838203887388,60.612499999768,11.5671105274575));
#284037=CARTESIAN_POINT('Ctrl Pts',(7.51676407774781,60.7624999997674,10.3459381770593));
#284038=CARTESIAN_POINT('Ctrl Pts',(9.83957192047903,60.9124999997668,7.14886745759543));
#284039=CARTESIAN_POINT('Ctrl Pts',(12.1623797632103,61.0624999997662,3.95179673813153));
#284040=CARTESIAN_POINT('Ctrl Pts',(12.1623797632102,61.2124999997656,-1.489461944703E-15));
#284041=CARTESIAN_POINT('Ctrl Pts',(12.1623797632102,61.362499999765,-3.95179673813154));
#284042=CARTESIAN_POINT('Ctrl Pts',(9.83957192047902,61.5124999997644,-7.14886745759543));
#284043=CARTESIAN_POINT('Ctrl Pts',(7.51676407774781,61.6624999997638,-10.3459381770593));
#284044=CARTESIAN_POINT('Ctrl Pts',(3.75838203887388,61.8124999997632,-11.5671105274575));
#284045=CARTESIAN_POINT('Ctrl Pts',(-4.89450751520023E-14,61.9624999997626,
-12.7882828778556));
#284046=CARTESIAN_POINT('Ctrl Pts',(-3.75838203887398,62.112499999762,-11.5671105274575));
#284047=CARTESIAN_POINT('Ctrl Pts',(-7.51676407774791,62.2624999997614,
-10.3459381770593));
#284048=CARTESIAN_POINT('Ctrl Pts',(-9.83957192047912,62.4124999997608,
-7.14886745759543));
#284049=CARTESIAN_POINT('Ctrl Pts',(-12.1623797632103,62.5624999997602,
-3.95179673813153));
#284050=CARTESIAN_POINT('Ctrl Pts',(-12.1623797632103,62.7124999997596,
2.97892388940601E-15));
#284051=CARTESIAN_POINT('Ctrl Pts',(-12.1623797632103,62.862499999759,3.95179673813154));
#284052=CARTESIAN_POINT('Ctrl Pts',(-9.83957192047912,63.0124999997584,
7.14886745759543));
#284053=CARTESIAN_POINT('Ctrl Pts',(-7.5167640777479,63.1624999997578,10.3459381770593));
#284054=CARTESIAN_POINT('Ctrl Pts',(-3.75838203887398,63.3124999997572,
11.5671105274575));
#284055=CARTESIAN_POINT('Ctrl Pts',(-4.66767038492419E-14,63.4624999997566,
12.7882828778556));
#284056=CARTESIAN_POINT('Ctrl Pts',(3.75838203887388,63.612499999756,11.5671105274575));
#284057=CARTESIAN_POINT('Ctrl Pts',(7.51676407774781,63.7624999997554,10.3459381770593));
#284058=CARTESIAN_POINT('Ctrl Pts',(9.83957192047903,63.9124999997548,7.14886745759543));
#284059=CARTESIAN_POINT('Ctrl Pts',(12.1623797632102,64.0624999997542,3.95179673813153));
#284060=CARTESIAN_POINT('Ctrl Pts',(12.1623797632102,64.2124999997536,-1.489461944703E-15));
#284061=CARTESIAN_POINT('Ctrl Pts',(12.1623797632102,64.362499999753,-3.95179673813154));
#284062=CARTESIAN_POINT('Ctrl Pts',(9.83957192047902,64.5124999997524,-7.14886745759543));
#284063=CARTESIAN_POINT('Ctrl Pts',(7.51676407774781,64.6624999997518,-10.3459381770593));
#284064=CARTESIAN_POINT('Ctrl Pts',(3.75838203887388,64.8124999997512,-11.5671105274575));
#284065=CARTESIAN_POINT('Ctrl Pts',(-5.06727844236642E-14,64.9624999997506,
-12.7882828778556));
#284066=CARTESIAN_POINT('Ctrl Pts',(-3.75838203887398,65.11249999975,-11.5671105274575));
#284067=CARTESIAN_POINT('Ctrl Pts',(-7.51676407774791,65.2624999997494,
-10.3459381770593));
#284068=CARTESIAN_POINT('Ctrl Pts',(-9.83957192047913,65.4124999997488,
-7.14886745759543));
#284069=CARTESIAN_POINT('Ctrl Pts',(-12.1623797632103,65.5624999997482,
-3.95179673813153));
#284070=CARTESIAN_POINT('Ctrl Pts',(-12.1623797632103,65.7124999997476,
2.97892388940601E-15));
#284071=CARTESIAN_POINT('Ctrl Pts',(-12.1623797632103,65.862499999747,3.95179673813154));
#284072=CARTESIAN_POINT('Ctrl Pts',(-9.83957192047912,66.0124999997464,
7.14886745759543));
#284073=CARTESIAN_POINT('Ctrl Pts',(-7.51676407774791,66.1624999997458,
10.3459381770593));
#284074=CARTESIAN_POINT('Ctrl Pts',(-3.75838203887398,66.3124999997452,
11.5671105274575));
#284075=CARTESIAN_POINT('Ctrl Pts',(-4.84044131209037E-14,66.4624999997446,
12.7882828778556));
#284076=CARTESIAN_POINT('Ctrl Pts',(3.75838203887388,66.612499999744,11.5671105274575));
#284077=CARTESIAN_POINT('Ctrl Pts',(7.51676407774781,66.7624999997434,10.3459381770593));
#284078=CARTESIAN_POINT('Ctrl Pts',(9.83957192047902,66.9124999997428,7.14886745759543));
#284079=CARTESIAN_POINT('Ctrl Pts',(12.1623797632102,67.0624999997422,3.95179673813153));
#284080=CARTESIAN_POINT('Ctrl Pts',(12.1623797632102,67.2124999997416,-1.489461944703E-15));
#284081=CARTESIAN_POINT('Ctrl Pts',(12.1623797632102,67.362499999741,-3.95179673813154));
#284082=CARTESIAN_POINT('Ctrl Pts',(9.83957192047902,67.5124999997404,-7.14886745759543));
#284083=CARTESIAN_POINT('Ctrl Pts',(7.51676407774781,67.6624999997398,-10.3459381770593));
#284084=CARTESIAN_POINT('Ctrl Pts',(3.75838203887388,67.8124999997392,-11.5671105274575));
#284085=CARTESIAN_POINT('Ctrl Pts',(-5.2400493695326E-14,67.9624999997386,
-12.7882828778556));
#284086=CARTESIAN_POINT('Ctrl Pts',(-3.75838203887398,68.112499999738,-11.5671105274575));
#284087=CARTESIAN_POINT('Ctrl Pts',(-7.51676407774791,68.2624999997374,
-10.3459381770593));
#284088=CARTESIAN_POINT('Ctrl Pts',(-9.83957192047913,68.4124999997368,
-7.14886745759543));
#284089=CARTESIAN_POINT('Ctrl Pts',(-12.1623797632103,68.5624999997362,
-3.95179673813153));
#284090=CARTESIAN_POINT('Ctrl Pts',(-12.1623797632103,68.7124999997356,
2.97892388940601E-15));
#284091=CARTESIAN_POINT('Ctrl Pts',(-12.1623797632103,68.862499999735,3.95179673813154));
#284092=CARTESIAN_POINT('Ctrl Pts',(-9.83957192047913,69.0124999997344,
7.14886745759543));
#284093=CARTESIAN_POINT('Ctrl Pts',(-7.51676407774791,69.1624999997338,
10.3459381770593));
#284094=CARTESIAN_POINT('Ctrl Pts',(-3.75838203887398,69.3124999997332,
11.5671105274575));
#284095=CARTESIAN_POINT('Ctrl Pts',(-5.01321223925656E-14,69.4624999997326,
12.7882828778556));
#284096=CARTESIAN_POINT('Ctrl Pts',(3.75838203887388,69.612499999732,11.5671105274575));
#284097=CARTESIAN_POINT('Ctrl Pts',(7.51676407774781,69.7624999997314,10.3459381770593));
#284098=CARTESIAN_POINT('Ctrl Pts',(9.83957192047902,69.9124999997308,7.14886745759543));
#284099=CARTESIAN_POINT('Ctrl Pts',(12.1623797632102,70.0624999997302,3.95179673813153));
#284100=CARTESIAN_POINT('Ctrl Pts',(12.1623797632102,70.2124999997296,-1.489461944703E-15));
#284101=CARTESIAN_POINT('Ctrl Pts',(12.1623797632102,70.362499999729,-3.95179673813154));
#284102=CARTESIAN_POINT('Ctrl Pts',(9.83957192047902,70.5124999997284,-7.14886745759543));
#284103=CARTESIAN_POINT('Ctrl Pts',(7.5167640777478,70.6624999997278,-10.3459381770593));
#284104=CARTESIAN_POINT('Ctrl Pts',(3.75838203887388,70.8124999997272,-11.5671105274575));
#284105=CARTESIAN_POINT('Ctrl Pts',(-5.41282029669879E-14,70.9624999997266,
-12.7882828778556));
#284106=CARTESIAN_POINT('Ctrl Pts',(-3.75838203887398,71.112499999726,-11.5671105274575));
#284107=CARTESIAN_POINT('Ctrl Pts',(-7.51676407774791,71.2624999997254,
-10.3459381770593));
#284108=CARTESIAN_POINT('Ctrl Pts',(-9.83957192047913,71.4124999997248,
-7.14886745759543));
#284109=CARTESIAN_POINT('Ctrl Pts',(-12.1623797632103,71.5624999997242,
-3.95179673813153));
#284110=CARTESIAN_POINT('Ctrl Pts',(-12.1623797632103,71.7124999997236,
2.97892388940601E-15));
#284111=CARTESIAN_POINT('Ctrl Pts',(-12.1623797632103,71.862499999723,3.95179673813154));
#284112=CARTESIAN_POINT('Ctrl Pts',(-9.83957192047913,72.0124999997224,
7.14886745759543));
#284113=CARTESIAN_POINT('Ctrl Pts',(-7.51676407774791,72.1624999997218,
10.3459381770593));
#284114=CARTESIAN_POINT('Ctrl Pts',(-3.75838203887398,72.3124999997212,
11.5671105274575));
#284115=CARTESIAN_POINT('Ctrl Pts',(-5.18598316642274E-14,72.4624999997206,
12.7882828778556));
#284116=CARTESIAN_POINT('Ctrl Pts',(3.75838203887388,72.61249999972,11.5671105274575));
#284117=CARTESIAN_POINT('Ctrl Pts',(7.51676407774781,72.7624999997194,10.3459381770593));
#284118=CARTESIAN_POINT('Ctrl Pts',(9.83957192047902,72.9124999997188,7.14886745759543));
#284119=CARTESIAN_POINT('Ctrl Pts',(12.1623797632102,73.0624999997182,3.95179673813153));
#284120=CARTESIAN_POINT('Ctrl Pts',(12.1623797632102,73.2124999997176,-1.489461944703E-15));
#284121=CARTESIAN_POINT('Ctrl Pts',(12.1623797632102,73.362499999717,-3.95179673813154));
#284122=CARTESIAN_POINT('Ctrl Pts',(9.83957192047902,73.5124999997164,-7.14886745759543));
#284123=CARTESIAN_POINT('Ctrl Pts',(7.5167640777478,73.6624999997158,-10.3459381770593));
#284124=CARTESIAN_POINT('Ctrl Pts',(3.75838203887387,73.8124999997152,-11.5671105274575));
#284125=CARTESIAN_POINT('Ctrl Pts',(-5.58559122386497E-14,73.9624999997146,
-12.7882828778556));
#284126=CARTESIAN_POINT('Ctrl Pts',(-3.75838203887398,74.112499999714,-11.5671105274575));
#284127=CARTESIAN_POINT('Ctrl Pts',(-7.51676407774791,74.2624999997134,
-10.3459381770593));
#284128=CARTESIAN_POINT('Ctrl Pts',(-9.83957192047913,74.4124999997128,
-7.14886745759543));
#284129=CARTESIAN_POINT('Ctrl Pts',(-12.1623797632103,74.5624999997122,
-3.95179673813153));
#284130=CARTESIAN_POINT('Ctrl Pts',(-12.1623797632103,74.7124999997116,
2.97892388940601E-15));
#284131=CARTESIAN_POINT('Ctrl Pts',(-12.1623797632103,74.862499999711,3.95179673813154));
#284132=CARTESIAN_POINT('Ctrl Pts',(-9.83957192047913,75.0124999997104,
7.14886745759543));
#284133=CARTESIAN_POINT('Ctrl Pts',(-7.51676407774791,75.1624999997098,
10.3459381770593));
#284134=CARTESIAN_POINT('Ctrl Pts',(-3.75838203887398,75.3124999997092,
11.5671105274575));
#284135=CARTESIAN_POINT('Ctrl Pts',(-5.35875409358893E-14,75.4624999997086,
12.7882828778556));
#284136=CARTESIAN_POINT('Ctrl Pts',(3.75838203887388,75.612499999708,11.5671105274575));
#284137=CARTESIAN_POINT('Ctrl Pts',(7.5167640777478,75.7624999997074,10.3459381770593));
#284138=CARTESIAN_POINT('Ctrl Pts',(9.83957192047902,75.9124999997068,7.14886745759543));
#284139=CARTESIAN_POINT('Ctrl Pts',(12.1623797632102,76.0624999997062,3.95179673813153));
#284140=CARTESIAN_POINT('Ctrl Pts',(12.1623797632102,76.2124999997056,-1.489461944703E-15));
#284141=CARTESIAN_POINT('Ctrl Pts',(12.1623797632102,76.362499999705,-3.95179673813154));
#284142=CARTESIAN_POINT('Ctrl Pts',(9.83957192047902,76.5124999997044,-7.14886745759543));
#284143=CARTESIAN_POINT('Ctrl Pts',(7.5167640777478,76.6624999997038,-10.3459381770593));
#284144=CARTESIAN_POINT('Ctrl Pts',(3.75838203887387,76.8124999997032,-11.5671105274575));
#284145=CARTESIAN_POINT('Ctrl Pts',(-5.75836215103115E-14,76.9624999997026,
-12.7882828778556));
#284146=CARTESIAN_POINT('Ctrl Pts',(-3.75838203887399,77.112499999702,-11.5671105274575));
#284147=CARTESIAN_POINT('Ctrl Pts',(-7.51676407774791,77.2624999997014,
-10.3459381770593));
#284148=CARTESIAN_POINT('Ctrl Pts',(-9.83957192047913,77.4124999997008,
-7.14886745759543));
#284149=CARTESIAN_POINT('Ctrl Pts',(-12.1623797632103,77.5624999997002,
-3.95179673813153));
#284150=CARTESIAN_POINT('Ctrl Pts',(-12.1623797632103,77.7124999996996,
2.97892388940601E-15));
#284151=CARTESIAN_POINT('Ctrl Pts',(-12.1623797632103,77.862499999699,3.95179673813154));
#284152=CARTESIAN_POINT('Ctrl Pts',(-9.83957192047913,78.0124999996984,
7.14886745759543));
#284153=CARTESIAN_POINT('Ctrl Pts',(-7.51676407774791,78.1624999996978,
10.3459381770593));
#284154=CARTESIAN_POINT('Ctrl Pts',(-3.75838203887398,78.3124999996972,
11.5671105274575));
#284155=CARTESIAN_POINT('Ctrl Pts',(-5.53152502075511E-14,78.4624999996966,
12.7882828778556));
#284156=CARTESIAN_POINT('Ctrl Pts',(3.75838203887387,78.612499999696,11.5671105274575));
#284157=CARTESIAN_POINT('Ctrl Pts',(7.5167640777478,78.7624999996954,10.3459381770593));
#284158=CARTESIAN_POINT('Ctrl Pts',(9.83957192047902,78.9124999996948,7.14886745759543));
#284159=CARTESIAN_POINT('Ctrl Pts',(12.1623797632102,79.0624999996942,3.95179673813153));
#284160=CARTESIAN_POINT('Ctrl Pts',(12.1623797632102,79.2124999996936,-1.489461944703E-15));
#284161=CARTESIAN_POINT('Ctrl Pts',(12.1623797632102,79.362499999693,-3.95179673813154));
#284162=CARTESIAN_POINT('Ctrl Pts',(9.83957192047902,79.5124999996924,-7.14886745759543));
#284163=CARTESIAN_POINT('Ctrl Pts',(7.5167640777478,79.6624999996918,-10.3459381770593));
#284164=CARTESIAN_POINT('Ctrl Pts',(3.75838203887387,79.8124999996912,-11.5671105274575));
#284165=CARTESIAN_POINT('Ctrl Pts',(-5.93113307819734E-14,79.9624999996906,
-12.7882828778556));
#284166=CARTESIAN_POINT('Ctrl Pts',(-3.75838203887399,80.11249999969,-11.5671105274575));
#284167=CARTESIAN_POINT('Ctrl Pts',(-7.51676407774791,80.2624999996894,
-10.3459381770593));
#284168=CARTESIAN_POINT('Ctrl Pts',(-9.83957192047913,80.4124999996888,
-7.14886745759543));
#284169=CARTESIAN_POINT('Ctrl Pts',(-12.1623797632104,80.5624999996882,
-3.95179673813153));
#284170=CARTESIAN_POINT('Ctrl Pts',(-12.1623797632104,80.7124999996876,
2.97892388940601E-15));
#284171=CARTESIAN_POINT('Ctrl Pts',(-12.1623797632104,80.862499999687,3.95179673813154));
#284172=CARTESIAN_POINT('Ctrl Pts',(-9.83957192047913,81.0124999996864,
7.14886745759543));
#284173=CARTESIAN_POINT('Ctrl Pts',(-7.51676407774791,81.1624999996858,
10.3459381770593));
#284174=CARTESIAN_POINT('Ctrl Pts',(-3.75838203887399,81.3124999996852,
11.5671105274575));
#284175=CARTESIAN_POINT('Ctrl Pts',(-5.70429594792129E-14,81.4624999996846,
12.7882828778556));
#284176=CARTESIAN_POINT('Ctrl Pts',(3.75838203887387,81.612499999684,11.5671105274575));
#284177=CARTESIAN_POINT('Ctrl Pts',(7.5167640777478,81.7624999996834,10.3459381770593));
#284178=CARTESIAN_POINT('Ctrl Pts',(9.83957192047902,81.9124999996828,7.14886745759543));
#284179=CARTESIAN_POINT('Ctrl Pts',(12.1623797632102,82.0624999996822,3.95179673813153));
#284180=CARTESIAN_POINT('Ctrl Pts',(12.1623797632102,82.2124999996816,-1.489461944703E-15));
#284181=CARTESIAN_POINT('Ctrl Pts',(12.1623797632102,82.362499999681,-3.95179673813154));
#284182=CARTESIAN_POINT('Ctrl Pts',(9.83957192047902,82.5124999996804,-7.14886745759543));
#284183=CARTESIAN_POINT('Ctrl Pts',(7.5167640777478,82.6624999996798,-10.3459381770593));
#284184=CARTESIAN_POINT('Ctrl Pts',(3.75838203887387,82.8124999996792,-11.5671105274575));
#284185=CARTESIAN_POINT('Ctrl Pts',(-6.10390400536352E-14,82.9624999996786,
-12.7882828778556));
#284186=CARTESIAN_POINT('Ctrl Pts',(-3.75838203887399,83.112499999678,-11.5671105274575));
#284187=CARTESIAN_POINT('Ctrl Pts',(-7.51676407774792,83.2624999996774,
-10.3459381770593));
#284188=CARTESIAN_POINT('Ctrl Pts',(-9.83957192047914,83.4124999996768,
-7.14886745759543));
#284189=CARTESIAN_POINT('Ctrl Pts',(-12.1623797632104,83.5624999996762,
-3.95179673813153));
#284190=CARTESIAN_POINT('Ctrl Pts',(-12.1623797632104,83.7124999996756,
2.97892388940601E-15));
#284191=CARTESIAN_POINT('Ctrl Pts',(-12.1623797632104,83.862499999675,3.95179673813154));
#284192=CARTESIAN_POINT('Ctrl Pts',(-9.83957192047913,84.0124999996744,
7.14886745759543));
#284193=CARTESIAN_POINT('Ctrl Pts',(-7.51676407774791,84.1624999996738,
10.3459381770593));
#284194=CARTESIAN_POINT('Ctrl Pts',(-3.75838203887399,84.3124999996732,
11.5671105274575));
#284195=CARTESIAN_POINT('Ctrl Pts',(-5.87706687508748E-14,84.4624999996726,
12.7882828778556));
#284196=CARTESIAN_POINT('Ctrl Pts',(3.75838203887387,84.6124999996721,11.5671105274575));
#284197=CARTESIAN_POINT('Ctrl Pts',(7.5167640777478,84.7624999996714,10.3459381770593));
#284198=CARTESIAN_POINT('Ctrl Pts',(9.83957192047902,84.9124999996708,7.14886745759543));
#284199=CARTESIAN_POINT('Ctrl Pts',(12.1623797632102,85.0624999996702,3.95179673813153));
#284200=CARTESIAN_POINT('Ctrl Pts',(12.1623797632102,85.2124999996696,-1.489461944703E-15));
#284201=CARTESIAN_POINT('Ctrl Pts',(12.1623797632102,85.362499999669,-3.95179673813154));
#284202=CARTESIAN_POINT('Ctrl Pts',(9.83957192047901,85.5124999996684,-7.14886745759543));
#284203=CARTESIAN_POINT('Ctrl Pts',(7.5167640777478,85.6624999996678,-10.3459381770593));
#284204=CARTESIAN_POINT('Ctrl Pts',(3.75838203887387,85.8124999996672,-11.5671105274575));
#284205=CARTESIAN_POINT('Ctrl Pts',(-6.27667493252971E-14,85.9624999996666,
-12.7882828778556));
#284206=CARTESIAN_POINT('Ctrl Pts',(-3.75838203887399,86.112499999666,-11.5671105274575));
#284207=CARTESIAN_POINT('Ctrl Pts',(-7.51676407774792,86.2624999996654,
-10.3459381770593));
#284208=CARTESIAN_POINT('Ctrl Pts',(-9.83957192047914,86.4124999996648,
-7.14886745759543));
#284209=CARTESIAN_POINT('Ctrl Pts',(-12.1623797632104,86.5624999996642,
-3.95179673813153));
#284210=CARTESIAN_POINT('Ctrl Pts',(-12.1623797632104,86.7124999996636,
2.97892388940601E-15));
#284211=CARTESIAN_POINT('Ctrl Pts',(-12.1623797632104,86.862499999663,3.95179673813154));
#284212=CARTESIAN_POINT('Ctrl Pts',(-9.83957192047914,87.0124999996624,
7.14886745759543));
#284213=CARTESIAN_POINT('Ctrl Pts',(-7.51676407774792,87.1624999996618,
10.3459381770593));
#284214=CARTESIAN_POINT('Ctrl Pts',(-3.75838203887399,87.3124999996612,
11.5671105274575));
#284215=CARTESIAN_POINT('Ctrl Pts',(-6.04983780225366E-14,87.4624999996606,
12.7882828778556));
#284216=CARTESIAN_POINT('Ctrl Pts',(3.75838203887387,87.61249999966,11.5671105274575));
#284217=CARTESIAN_POINT('Ctrl Pts',(7.5167640777478,87.7624999996594,10.3459381770593));
#284218=CARTESIAN_POINT('Ctrl Pts',(9.83957192047901,87.9124999996588,7.14886745759543));
#284219=CARTESIAN_POINT('Ctrl Pts',(12.1623797632102,88.0624999996582,3.95179673813153));
#284220=CARTESIAN_POINT('Ctrl Pts',(12.1623797632102,88.2124999996576,-1.489461944703E-15));
#284221=CARTESIAN_POINT('Ctrl Pts',(12.1623797632102,88.362499999657,-3.95179673813154));
#284222=CARTESIAN_POINT('Ctrl Pts',(9.83957192047901,88.5124999996564,-7.14886745759543));
#284223=CARTESIAN_POINT('Ctrl Pts',(7.51676407774779,88.6624999996558,-10.3459381770593));
#284224=CARTESIAN_POINT('Ctrl Pts',(3.75838203887386,88.8124999996552,-11.5671105274575));
#284225=CARTESIAN_POINT('Ctrl Pts',(-6.44944585969589E-14,88.9624999996546,
-12.7882828778556));
#284226=CARTESIAN_POINT('Ctrl Pts',(-3.75838203887399,89.112499999654,-11.5671105274575));
#284227=CARTESIAN_POINT('Ctrl Pts',(-7.51676407774792,89.2624999996534,
-10.3459381770593));
#284228=CARTESIAN_POINT('Ctrl Pts',(-9.83957192047914,89.4124999996528,
-7.14886745759543));
#284229=CARTESIAN_POINT('Ctrl Pts',(-12.1623797632104,89.5624999996522,
-3.95179673813153));
#284230=CARTESIAN_POINT('Ctrl Pts',(-12.1623797632104,89.7124999996516,
2.97892388940601E-15));
#284231=CARTESIAN_POINT('Ctrl Pts',(-12.1623797632104,89.862499999651,3.95179673813154));
#284232=CARTESIAN_POINT('Ctrl Pts',(-9.83957192047914,90.0124999996504,
7.14886745759543));
#284233=CARTESIAN_POINT('Ctrl Pts',(-7.51676407774792,90.1624999996498,
10.3459381770593));
#284234=CARTESIAN_POINT('Ctrl Pts',(-3.75838203887399,90.3124999996492,
11.5671105274575));
#284235=CARTESIAN_POINT('Ctrl Pts',(-6.22260872941985E-14,90.4624999996486,
12.7882828778556));
#284236=CARTESIAN_POINT('Ctrl Pts',(3.75838203887387,90.612499999648,11.5671105274575));
#284237=CARTESIAN_POINT('Ctrl Pts',(7.5167640777478,90.7624999996474,10.3459381770593));
#284238=CARTESIAN_POINT('Ctrl Pts',(9.83957192047901,90.9124999996468,7.14886745759543));
#284239=CARTESIAN_POINT('Ctrl Pts',(12.1623797632102,91.0624999996462,3.95179673813153));
#284240=CARTESIAN_POINT('Ctrl Pts',(12.1623797632102,91.2124999996456,-1.489461944703E-15));
#284241=CARTESIAN_POINT('Ctrl Pts',(12.1623797632102,91.362499999645,-3.95179673813154));
#284242=CARTESIAN_POINT('Ctrl Pts',(9.83957192047901,91.5124999996444,-7.14886745759543));
#284243=CARTESIAN_POINT('Ctrl Pts',(7.51676407774779,91.6624999996438,-10.3459381770593));
#284244=CARTESIAN_POINT('Ctrl Pts',(3.75838203887386,91.8124999996432,-11.5671105274575));
#284245=CARTESIAN_POINT('Ctrl Pts',(-6.62221678686207E-14,91.9624999996426,
-12.7882828778556));
#284246=CARTESIAN_POINT('Ctrl Pts',(-3.75838203887399,92.112499999642,-11.5671105274575));
#284247=CARTESIAN_POINT('Ctrl Pts',(-7.51676407774792,92.2624999996414,
-10.3459381770593));
#284248=CARTESIAN_POINT('Ctrl Pts',(-9.83957192047914,92.4124999996408,
-7.14886745759543));
#284249=CARTESIAN_POINT('Ctrl Pts',(-12.1623797632104,92.5624999996402,
-3.95179673813153));
#284250=CARTESIAN_POINT('Ctrl Pts',(-12.1623797632104,92.7124999996396,
2.97892388940601E-15));
#284251=CARTESIAN_POINT('Ctrl Pts',(-12.1623797632104,92.862499999639,3.95179673813154));
#284252=CARTESIAN_POINT('Ctrl Pts',(-9.83957192047914,93.0124999996384,
7.14886745759543));
#284253=CARTESIAN_POINT('Ctrl Pts',(-7.51676407774792,93.1624999996378,
10.3459381770593));
#284254=CARTESIAN_POINT('Ctrl Pts',(-3.75838203887399,93.3124999996372,
11.5671105274575));
#284255=CARTESIAN_POINT('Ctrl Pts',(-6.39537965658603E-14,93.4624999996366,
12.7882828778556));
#284256=CARTESIAN_POINT('Ctrl Pts',(3.75838203887386,93.612499999636,11.5671105274575));
#284257=CARTESIAN_POINT('Ctrl Pts',(7.51676407774779,93.7624999996354,10.3459381770593));
#284258=CARTESIAN_POINT('Ctrl Pts',(9.83957192047901,93.9124999996348,7.14886745759543));
#284259=CARTESIAN_POINT('Ctrl Pts',(12.1623797632102,94.0624999996342,3.95179673813153));
#284260=CARTESIAN_POINT('Ctrl Pts',(12.1623797632102,94.2124999996336,-1.489461944703E-15));
#284261=CARTESIAN_POINT('Ctrl Pts',(12.1623797632102,94.362499999633,-3.95179673813154));
#284262=CARTESIAN_POINT('Ctrl Pts',(9.83957192047901,94.5124999996324,-7.14886745759543));
#284263=CARTESIAN_POINT('Ctrl Pts',(7.51676407774779,94.6624999996318,-10.3459381770593));
#284264=CARTESIAN_POINT('Ctrl Pts',(3.75838203887386,94.8124999996312,-11.5671105274575));
#284265=CARTESIAN_POINT('Ctrl Pts',(-6.79498771402825E-14,94.9624999996306,
-12.7882828778556));
#284266=CARTESIAN_POINT('Ctrl Pts',(-3.758382038874,95.11249999963,-11.5671105274575));
#284267=CARTESIAN_POINT('Ctrl Pts',(-7.51676407774792,95.2624999996294,
-10.3459381770593));
#284268=CARTESIAN_POINT('Ctrl Pts',(-9.83957192047914,95.4124999996288,
-7.14886745759543));
#284269=CARTESIAN_POINT('Ctrl Pts',(-12.1623797632104,95.5624999996282,
-3.95179673813153));
#284270=CARTESIAN_POINT('Ctrl Pts',(-12.1623797632104,95.7124999996276,
2.97892388940601E-15));
#284271=CARTESIAN_POINT('Ctrl Pts',(-12.1623797632104,95.862499999627,3.95179673813154));
#284272=CARTESIAN_POINT('Ctrl Pts',(-9.83957192047914,96.0124999996264,
7.14886745759543));
#284273=CARTESIAN_POINT('Ctrl Pts',(-7.51676407774792,96.1624999996258,
10.3459381770593));
#284274=CARTESIAN_POINT('Ctrl Pts',(-3.75838203887399,96.3124999996252,
11.5671105274575));
#284275=CARTESIAN_POINT('Ctrl Pts',(-6.56815058375222E-14,96.4624999996246,
12.7882828778556));
#284276=CARTESIAN_POINT('Ctrl Pts',(3.75838203887386,96.612499999624,11.5671105274575));
#284277=CARTESIAN_POINT('Ctrl Pts',(7.51676407774779,96.7624999996234,10.3459381770593));
#284278=CARTESIAN_POINT('Ctrl Pts',(9.83957192047901,96.9124999996228,7.14886745759543));
#284279=CARTESIAN_POINT('Ctrl Pts',(12.1623797632102,97.0624999996222,3.95179673813153));
#284280=CARTESIAN_POINT('Ctrl Pts',(12.1623797632102,97.2124999996216,-1.489461944703E-15));
#284281=CARTESIAN_POINT('Ctrl Pts',(12.1623797632102,97.3624999996211,-3.95179673813154));
#284282=CARTESIAN_POINT('Ctrl Pts',(9.83957192047901,97.5124999996204,-7.14886745759543));
#284283=CARTESIAN_POINT('Ctrl Pts',(7.51676407774779,97.6624999996198,-10.3459381770593));
#284284=CARTESIAN_POINT('Ctrl Pts',(3.75838203887386,97.8124999996192,-11.5671105274575));
#284285=CARTESIAN_POINT('Ctrl Pts',(-6.96775864119444E-14,97.9624999996187,
-12.7882828778556));
#284286=CARTESIAN_POINT('Ctrl Pts',(-3.758382038874,98.112499999618,-11.5671105274575));
#284287=CARTESIAN_POINT('Ctrl Pts',(-7.51676407774793,98.2624999996174,
-10.3459381770593));
#284288=CARTESIAN_POINT('Ctrl Pts',(-9.83957192047914,98.4124999996168,
-7.14886745759543));
#284289=CARTESIAN_POINT('Ctrl Pts',(-12.1623797632104,98.5624999996162,
-3.95179673813153));
#284290=CARTESIAN_POINT('Ctrl Pts',(-12.1623797632104,98.7124999996156,
2.97892388940601E-15));
#284291=CARTESIAN_POINT('Ctrl Pts',(-12.1623797632104,98.862499999615,3.95179673813154));
#284292=CARTESIAN_POINT('Ctrl Pts',(-9.83957192047914,99.0124999996144,
7.14886745759543));
#284293=CARTESIAN_POINT('Ctrl Pts',(-7.51676407774792,99.1624999996138,
10.3459381770593));
#284294=CARTESIAN_POINT('Ctrl Pts',(-3.758382038874,99.3124999996132,11.5671105274575));
#284295=CARTESIAN_POINT('Ctrl Pts',(-6.7409215109184E-14,99.4624999996126,
12.7882828778556));
#284296=CARTESIAN_POINT('Ctrl Pts',(3.75838203887386,99.612499999612,11.5671105274575));
#284297=CARTESIAN_POINT('Ctrl Pts',(7.51676407774779,99.7624999996114,10.3459381770593));
#284298=CARTESIAN_POINT('Ctrl Pts',(9.83957192047901,99.9124999996108,7.14886745759543));
#284299=CARTESIAN_POINT('Ctrl Pts',(12.1623797632102,100.06249999961,3.95179673813153));
#284300=CARTESIAN_POINT('Ctrl Pts',(12.1623797632102,100.21249999961,-1.489461944703E-15));
#284301=CARTESIAN_POINT('Ctrl Pts',(12.1623797632102,100.362499999609,-3.95179673813154));
#284302=CARTESIAN_POINT('Ctrl Pts',(9.839571920479,100.512499999608,-7.14886745759543));
#284303=CARTESIAN_POINT('Ctrl Pts',(7.51676407774779,100.662499999608,-10.3459381770593));
#284304=CARTESIAN_POINT('Ctrl Pts',(3.75838203887386,100.812499999607,-11.5671105274575));
#284305=CARTESIAN_POINT('Ctrl Pts',(-7.14052956836063E-14,100.962499999607,
-12.7882828778556));
#284306=CARTESIAN_POINT('Ctrl Pts',(-3.758382038874,101.112499999606,-11.5671105274575));
#284307=CARTESIAN_POINT('Ctrl Pts',(-7.51676407774793,101.262499999605,
-10.3459381770593));
#284308=CARTESIAN_POINT('Ctrl Pts',(-9.83957192047915,101.412499999605,
-7.14886745759543));
#284309=CARTESIAN_POINT('Ctrl Pts',(-12.1623797632104,101.562499999604,
-3.95179673813153));
#284310=CARTESIAN_POINT('Ctrl Pts',(-12.1623797632104,101.712499999604,
2.97892388940601E-15));
#284311=CARTESIAN_POINT('Ctrl Pts',(-12.1623797632104,101.862499999603,
3.95179673813154));
#284312=CARTESIAN_POINT('Ctrl Pts',(-9.83957192047914,102.012499999602,
7.14886745759543));
#284313=CARTESIAN_POINT('Ctrl Pts',(-7.51676407774793,102.162499999602,
10.3459381770593));
#284314=CARTESIAN_POINT('Ctrl Pts',(-3.758382038874,102.312499999601,11.5671105274575));
#284315=CARTESIAN_POINT('Ctrl Pts',(-6.91369243808458E-14,102.462499999601,
12.7882828778556));
#284316=CARTESIAN_POINT('Ctrl Pts',(3.75838203887386,102.6124999996,11.5671105274575));
#284317=CARTESIAN_POINT('Ctrl Pts',(7.51676407774779,102.762499999599,10.3459381770593));
#284318=CARTESIAN_POINT('Ctrl Pts',(9.839571920479,102.912499999599,7.14886745759543));
#284319=CARTESIAN_POINT('Ctrl Pts',(12.1623797632102,103.062499999598,3.95179673813153));
#284320=CARTESIAN_POINT('Ctrl Pts',(12.1623797632102,103.212499999598,-1.489461944703E-15));
#284321=CARTESIAN_POINT('Ctrl Pts',(12.1623797632102,103.362499999597,-3.95179673813154));
#284322=CARTESIAN_POINT('Ctrl Pts',(9.839571920479,103.512499999596,-7.14886745759543));
#284323=CARTESIAN_POINT('Ctrl Pts',(7.51676407774779,103.662499999596,-10.3459381770593));
#284324=CARTESIAN_POINT('Ctrl Pts',(3.75838203887386,103.812499999595,-11.5671105274575));
#284325=CARTESIAN_POINT('Ctrl Pts',(-7.31330049552681E-14,103.962499999595,
-12.7882828778556));
#284326=CARTESIAN_POINT('Ctrl Pts',(-3.758382038874,104.112499999594,-11.5671105274575));
#284327=CARTESIAN_POINT('Ctrl Pts',(-7.51676407774793,104.262499999593,
-10.3459381770593));
#284328=CARTESIAN_POINT('Ctrl Pts',(-9.83957192047915,104.412499999593,
-7.14886745759543));
#284329=CARTESIAN_POINT('Ctrl Pts',(-12.1623797632104,104.562499999592,
-3.95179673813153));
#284330=CARTESIAN_POINT('Ctrl Pts',(-12.1623797632104,104.712499999592,
2.97892388940601E-15));
#284331=CARTESIAN_POINT('Ctrl Pts',(-12.1623797632104,104.862499999591,
3.95179673813154));
#284332=CARTESIAN_POINT('Ctrl Pts',(-9.83957192047915,105.01249999959,7.14886745759543));
#284333=CARTESIAN_POINT('Ctrl Pts',(-7.51676407774793,105.16249999959,10.3459381770593));
#284334=CARTESIAN_POINT('Ctrl Pts',(-3.758382038874,105.312499999589,11.5671105274575));
#284335=CARTESIAN_POINT('Ctrl Pts',(-7.08646336525076E-14,105.462499999589,
12.7882828778556));
#284336=CARTESIAN_POINT('Ctrl Pts',(3.75838203887386,105.612499999588,11.5671105274575));
#284337=CARTESIAN_POINT('Ctrl Pts',(7.51676407774779,105.762499999587,10.3459381770593));
#284338=CARTESIAN_POINT('Ctrl Pts',(9.839571920479,105.912499999587,7.14886745759543));
#284339=CARTESIAN_POINT('Ctrl Pts',(12.1623797632102,106.062499999586,3.95179673813153));
#284340=CARTESIAN_POINT('Ctrl Pts',(12.1623797632102,106.212499999586,-1.489461944703E-15));
#284341=CARTESIAN_POINT('Ctrl Pts',(12.1623797632102,106.362499999585,-3.95179673813154));
#284342=CARTESIAN_POINT('Ctrl Pts',(9.839571920479,106.512499999584,-7.14886745759543));
#284343=CARTESIAN_POINT('Ctrl Pts',(7.51676407774778,106.662499999584,-10.3459381770593));
#284344=CARTESIAN_POINT('Ctrl Pts',(3.75838203887385,106.812499999583,-11.5671105274575));
#284345=CARTESIAN_POINT('Ctrl Pts',(-7.48607142269299E-14,106.962499999583,
-12.7882828778556));
#284346=CARTESIAN_POINT('Ctrl Pts',(-3.758382038874,107.112499999582,-11.5671105274575));
#284347=CARTESIAN_POINT('Ctrl Pts',(-7.51676407774793,107.262499999581,
-10.3459381770593));
#284348=CARTESIAN_POINT('Ctrl Pts',(-9.83957192047915,107.412499999581,
-7.14886745759543));
#284349=CARTESIAN_POINT('Ctrl Pts',(-12.1623797632104,107.56249999958,-3.95179673813153));
#284350=CARTESIAN_POINT('Ctrl Pts',(-12.1623797632104,107.71249999958,2.97892388940601E-15));
#284351=CARTESIAN_POINT('Ctrl Pts',(-12.1623797632104,107.862499999579,
3.95179673813154));
#284352=CARTESIAN_POINT('Ctrl Pts',(-9.83957192047915,108.012499999578,
7.14886745759543));
#284353=CARTESIAN_POINT('Ctrl Pts',(-7.51676407774793,108.162499999578,
10.3459381770593));
#284354=CARTESIAN_POINT('Ctrl Pts',(-3.758382038874,108.312499999577,11.5671105274575));
#284355=CARTESIAN_POINT('Ctrl Pts',(-7.25923429241695E-14,108.462499999577,
12.7882828778556));
#284356=CARTESIAN_POINT('Ctrl Pts',(3.75838203887386,108.612499999576,11.5671105274575));
#284357=CARTESIAN_POINT('Ctrl Pts',(7.51676407774779,108.762499999575,10.3459381770593));
#284358=CARTESIAN_POINT('Ctrl Pts',(9.839571920479,108.912499999575,7.14886745759543));
#284359=CARTESIAN_POINT('Ctrl Pts',(12.1623797632102,109.062499999574,3.95179673813153));
#284360=CARTESIAN_POINT('Ctrl Pts',(12.1623797632102,109.212499999574,-1.489461944703E-15));
#284361=CARTESIAN_POINT('Ctrl Pts',(12.1623797632102,109.362499999573,-3.95179673813154));
#284362=CARTESIAN_POINT('Ctrl Pts',(9.839571920479,109.512499999572,-7.14886745759543));
#284363=CARTESIAN_POINT('Ctrl Pts',(7.51676407774778,109.662499999572,-10.3459381770593));
#284364=CARTESIAN_POINT('Ctrl Pts',(3.75838203887385,109.812499999571,-11.5671105274575));
#284365=CARTESIAN_POINT('Ctrl Pts',(-7.65884234985918E-14,109.962499999571,
-12.7882828778556));
#284366=CARTESIAN_POINT('Ctrl Pts',(-3.75838203887401,110.11249999957,-11.5671105274575));
#284367=CARTESIAN_POINT('Ctrl Pts',(-7.51676407774793,110.262499999569,
-10.3459381770593));
#284368=CARTESIAN_POINT('Ctrl Pts',(-9.83957192047915,110.412499999569,
-7.14886745759543));
#284369=CARTESIAN_POINT('Ctrl Pts',(-12.1623797632104,110.562499999568,
-3.95179673813153));
#284370=CARTESIAN_POINT('Ctrl Pts',(-12.1623797632104,110.712499999568,
2.97892388940601E-15));
#284371=CARTESIAN_POINT('Ctrl Pts',(-12.1623797632104,110.862499999567,
3.95179673813154));
#284372=CARTESIAN_POINT('Ctrl Pts',(-9.83957192047915,111.012499999566,
7.14886745759543));
#284373=CARTESIAN_POINT('Ctrl Pts',(-7.51676407774793,111.162499999566,
10.3459381770593));
#284374=CARTESIAN_POINT('Ctrl Pts',(-3.758382038874,111.312499999565,11.5671105274575));
#284375=CARTESIAN_POINT('Ctrl Pts',(-7.43200521958313E-14,111.462499999565,
12.7882828778556));
#284376=CARTESIAN_POINT('Ctrl Pts',(3.75838203887385,111.612499999564,11.5671105274575));
#284377=CARTESIAN_POINT('Ctrl Pts',(7.51676407774778,111.762499999563,10.3459381770593));
#284378=CARTESIAN_POINT('Ctrl Pts',(9.839571920479,111.912499999563,7.14886745759543));
#284379=CARTESIAN_POINT('Ctrl Pts',(12.1623797632102,112.062499999562,3.95179673813153));
#284380=CARTESIAN_POINT('Ctrl Pts',(12.1623797632102,112.212499999562,-1.489461944703E-15));
#284381=CARTESIAN_POINT('Ctrl Pts',(12.1623797632102,112.362499999561,-3.95179673813154));
#284382=CARTESIAN_POINT('Ctrl Pts',(9.839571920479,112.51249999956,-7.14886745759543));
#284383=CARTESIAN_POINT('Ctrl Pts',(7.51676407774778,112.66249999956,-10.3459381770593));
#284384=CARTESIAN_POINT('Ctrl Pts',(3.75838203887385,112.812499999559,-11.5671105274575));
#284385=CARTESIAN_POINT('Ctrl Pts',(-7.83161327702536E-14,112.962499999559,
-12.7882828778556));
#284386=CARTESIAN_POINT('Ctrl Pts',(-3.75838203887401,113.112499999558,
-11.5671105274575));
#284387=CARTESIAN_POINT('Ctrl Pts',(-7.51676407774793,113.262499999557,
-10.3459381770593));
#284388=CARTESIAN_POINT('Ctrl Pts',(-9.83957192047915,113.412499999557,
-7.14886745759543));
#284389=CARTESIAN_POINT('Ctrl Pts',(-12.1623797632104,113.562499999556,
-3.95179673813153));
#284390=CARTESIAN_POINT('Ctrl Pts',(-12.1623797632104,113.712499999556,
2.97892388940601E-15));
#284391=CARTESIAN_POINT('Ctrl Pts',(-12.1623797632104,113.862499999555,
3.95179673813154));
#284392=CARTESIAN_POINT('Ctrl Pts',(-9.83957192047915,114.012499999554,
7.14886745759543));
#284393=CARTESIAN_POINT('Ctrl Pts',(-7.51676407774793,114.162499999554,
10.3459381770593));
#284394=CARTESIAN_POINT('Ctrl Pts',(-3.758382038874,114.312499999553,11.5671105274575));
#284395=CARTESIAN_POINT('Ctrl Pts',(-7.60477614674932E-14,114.462499999553,
12.7882828778556));
#284396=CARTESIAN_POINT('Ctrl Pts',(3.75838203887385,114.612499999552,11.5671105274575));
#284397=CARTESIAN_POINT('Ctrl Pts',(7.51676407774778,114.762499999551,10.3459381770593));
#284398=CARTESIAN_POINT('Ctrl Pts',(9.839571920479,114.912499999551,7.14886745759543));
#284399=CARTESIAN_POINT('Ctrl Pts',(12.1623797632102,115.06249999955,3.95179673813153));
#284400=CARTESIAN_POINT('Ctrl Pts',(12.1623797632102,115.21249999955,-1.489461944703E-15));
#284401=CARTESIAN_POINT('Ctrl Pts',(12.1623797632102,115.362499999549,-3.95179673813154));
#284402=CARTESIAN_POINT('Ctrl Pts',(9.839571920479,115.512499999548,-7.14886745759543));
#284403=CARTESIAN_POINT('Ctrl Pts',(7.51676407774778,115.662499999548,-10.3459381770593));
#284404=CARTESIAN_POINT('Ctrl Pts',(3.75838203887385,115.812499999547,-11.5671105274575));
#284405=CARTESIAN_POINT('Ctrl Pts',(-8.00438420419154E-14,115.962499999547,
-12.7882828778556));
#284406=CARTESIAN_POINT('Ctrl Pts',(-3.75838203887401,116.112499999546,
-11.5671105274575));
#284407=CARTESIAN_POINT('Ctrl Pts',(-7.51676407774794,116.262499999545,
-10.3459381770593));
#284408=CARTESIAN_POINT('Ctrl Pts',(-9.83957192047916,116.412499999545,
-7.14886745759543));
#284409=CARTESIAN_POINT('Ctrl Pts',(-12.1623797632104,116.562499999544,
-3.95179673813153));
#284410=CARTESIAN_POINT('Ctrl Pts',(-12.1623797632104,116.712499999544,
2.97892388940601E-15));
#284411=CARTESIAN_POINT('Ctrl Pts',(-12.1623797632104,116.862499999543,
3.95179673813154));
#284412=CARTESIAN_POINT('Ctrl Pts',(-9.83957192047915,117.012499999542,
7.14886745759543));
#284413=CARTESIAN_POINT('Ctrl Pts',(-7.51676407774793,117.162499999542,
10.3459381770593));
#284414=CARTESIAN_POINT('Ctrl Pts',(-3.75838203887401,117.312499999541,
11.5671105274575));
#284415=CARTESIAN_POINT('Ctrl Pts',(-7.7775470739155E-14,117.462499999541,
12.7882828778556));
#284416=CARTESIAN_POINT('Ctrl Pts',(3.75838203887385,117.61249999954,11.5671105274575));
#284417=CARTESIAN_POINT('Ctrl Pts',(7.51676407774778,117.762499999539,10.3459381770593));
#284418=CARTESIAN_POINT('Ctrl Pts',(9.839571920479,117.912499999539,7.14886745759543));
#284419=CARTESIAN_POINT('Ctrl Pts',(12.1623797632102,118.062499999538,3.95179673813153));
#284420=CARTESIAN_POINT('Ctrl Pts',(12.1623797632102,118.212499999538,-1.489461944703E-15));
#284421=CARTESIAN_POINT('Ctrl Pts',(12.1623797632102,118.362499999537,-3.95179673813154));
#284422=CARTESIAN_POINT('Ctrl Pts',(9.83957192047899,118.512499999536,-7.14886745759543));
#284423=CARTESIAN_POINT('Ctrl Pts',(7.51676407774778,118.662499999536,-10.3459381770593));
#284424=CARTESIAN_POINT('Ctrl Pts',(3.75838203887385,118.812499999535,-11.5671105274575));
#284425=CARTESIAN_POINT('Ctrl Pts',(-8.17715513135773E-14,118.962499999535,
-12.7882828778556));
#284426=CARTESIAN_POINT('Ctrl Pts',(-3.75838203887401,119.112499999534,
-11.5671105274575));
#284427=CARTESIAN_POINT('Ctrl Pts',(-7.51676407774794,119.262499999533,
-10.3459381770593));
#284428=CARTESIAN_POINT('Ctrl Pts',(-9.83957192047916,119.412499999533,
-7.14886745759543));
#284429=CARTESIAN_POINT('Ctrl Pts',(-12.1623797632104,119.562499999532,
-3.95179673813153));
#284430=CARTESIAN_POINT('Ctrl Pts',(-12.1623797632104,119.712499999532,
2.97892388940601E-15));
#284431=CARTESIAN_POINT('Ctrl Pts',(-12.1623797632104,119.862499999531,
3.95179673813154));
#284432=CARTESIAN_POINT('Ctrl Pts',(-9.83957192047916,120.01249999953,7.14886745759543));
#284433=CARTESIAN_POINT('Ctrl Pts',(-7.51676407774794,120.16249999953,10.3459381770593));
#284434=CARTESIAN_POINT('Ctrl Pts',(-3.75838203887401,120.312499999529,
11.5671105274575));
#284435=CARTESIAN_POINT('Ctrl Pts',(-7.95031800108169E-14,120.462499999529,
12.7882828778556));
#284436=CARTESIAN_POINT('Ctrl Pts',(3.75838203887385,120.612499999528,11.5671105274575));
#284437=CARTESIAN_POINT('Ctrl Pts',(7.51676407774778,120.762499999527,10.3459381770593));
#284438=CARTESIAN_POINT('Ctrl Pts',(9.83957192047899,120.912499999527,7.14886745759543));
#284439=CARTESIAN_POINT('Ctrl Pts',(12.1623797632102,121.062499999526,3.95179673813153));
#284440=CARTESIAN_POINT('Ctrl Pts',(12.1623797632102,121.212499999526,-1.489461944703E-15));
#284441=CARTESIAN_POINT('Ctrl Pts',(12.1623797632102,121.362499999525,-3.95179673813154));
#284442=CARTESIAN_POINT('Ctrl Pts',(9.83957192047899,121.512499999524,-7.14886745759543));
#284443=CARTESIAN_POINT('Ctrl Pts',(7.51676407774777,121.662499999524,-10.3459381770593));
#284444=CARTESIAN_POINT('Ctrl Pts',(3.75838203887385,121.812499999523,-11.5671105274575));
#284445=CARTESIAN_POINT('Ctrl Pts',(-8.34992605852391E-14,121.962499999523,
-12.7882828778556));
#284446=CARTESIAN_POINT('Ctrl Pts',(-3.75838203887401,122.112499999522,
-11.5671105274575));
#284447=CARTESIAN_POINT('Ctrl Pts',(-7.51676407774794,122.262499999521,
-10.3459381770593));
#284448=CARTESIAN_POINT('Ctrl Pts',(-9.83957192047916,122.412499999521,
-7.14886745759543));
#284449=CARTESIAN_POINT('Ctrl Pts',(-12.1623797632104,122.56249999952,-3.95179673813153));
#284450=CARTESIAN_POINT('Ctrl Pts',(-12.1623797632104,122.71249999952,2.97892388940601E-15));
#284451=CARTESIAN_POINT('Ctrl Pts',(-12.1623797632104,122.862499999519,
3.95179673813154));
#284452=CARTESIAN_POINT('Ctrl Pts',(-9.83957192047916,123.012499999518,
7.14886745759543));
#284453=CARTESIAN_POINT('Ctrl Pts',(-7.51676407774794,123.162499999518,
10.3459381770593));
#284454=CARTESIAN_POINT('Ctrl Pts',(-3.75838203887401,123.312499999517,
11.5671105274575));
#284455=CARTESIAN_POINT('Ctrl Pts',(-8.12308892824787E-14,123.462499999517,
12.7882828778556));
#284456=CARTESIAN_POINT('Ctrl Pts',(3.75838203887385,123.612499999516,11.5671105274575));
#284457=CARTESIAN_POINT('Ctrl Pts',(7.51676407774778,123.762499999515,10.3459381770593));
#284458=CARTESIAN_POINT('Ctrl Pts',(9.83957192047899,123.912499999515,7.14886745759543));
#284459=CARTESIAN_POINT('Ctrl Pts',(12.1623797632102,124.062499999514,3.95179673813153));
#284460=CARTESIAN_POINT('Ctrl Pts',(12.1623797632102,124.212499999514,-1.489461944703E-15));
#284461=CARTESIAN_POINT('Ctrl Pts',(12.1623797632102,124.362499999513,-3.95179673813154));
#284462=CARTESIAN_POINT('Ctrl Pts',(9.83957192047899,124.512499999512,-7.14886745759543));
#284463=CARTESIAN_POINT('Ctrl Pts',(7.51676407774777,124.662499999512,-10.3459381770593));
#284464=CARTESIAN_POINT('Ctrl Pts',(3.75838203887384,124.812499999511,-11.5671105274575));
#284465=CARTESIAN_POINT('Ctrl Pts',(-8.52269698569009E-14,124.962499999511,
-12.7882828778556));
#284466=CARTESIAN_POINT('Ctrl Pts',(-3.75838203887401,125.11249999951,-11.5671105274575));
#284467=CARTESIAN_POINT('Ctrl Pts',(-7.51676407774794,125.262499999509,
-10.3459381770593));
#284468=CARTESIAN_POINT('Ctrl Pts',(-9.83957192047916,125.412499999509,
-7.14886745759543));
#284469=CARTESIAN_POINT('Ctrl Pts',(-12.1623797632104,125.562499999508,
-3.95179673813153));
#284470=CARTESIAN_POINT('Ctrl Pts',(-12.1623797632104,125.712499999508,
2.97892388940601E-15));
#284471=CARTESIAN_POINT('Ctrl Pts',(-12.1623797632104,125.862499999507,
3.95179673813154));
#284472=CARTESIAN_POINT('Ctrl Pts',(-9.83957192047916,126.012499999506,
7.14886745759543));
#284473=CARTESIAN_POINT('Ctrl Pts',(-7.51676407774794,126.162499999506,
10.3459381770593));
#284474=CARTESIAN_POINT('Ctrl Pts',(-3.75838203887401,126.312499999505,
11.5671105274575));
#284475=CARTESIAN_POINT('Ctrl Pts',(-8.29585985541405E-14,126.462499999505,
12.7882828778556));
#284476=CARTESIAN_POINT('Ctrl Pts',(3.75838203887385,126.612499999504,11.5671105274575));
#284477=CARTESIAN_POINT('Ctrl Pts',(7.51676407774777,126.762499999503,10.3459381770593));
#284478=CARTESIAN_POINT('Ctrl Pts',(9.83957192047899,126.912499999503,7.14886745759543));
#284479=CARTESIAN_POINT('Ctrl Pts',(12.1623797632102,127.062499999502,3.95179673813153));
#284480=CARTESIAN_POINT('Ctrl Pts',(12.1623797632102,127.212499999502,-1.489461944703E-15));
#284481=CARTESIAN_POINT('Ctrl Pts',(12.1623797632102,127.362499999501,-3.95179673813154));
#284482=CARTESIAN_POINT('Ctrl Pts',(9.83957192047899,127.5124999995,-7.14886745759543));
#284483=CARTESIAN_POINT('Ctrl Pts',(7.51676407774777,127.6624999995,-10.3459381770593));
#284484=CARTESIAN_POINT('Ctrl Pts',(3.75838203887384,127.812499999499,-11.5671105274575));
#284485=CARTESIAN_POINT('Ctrl Pts',(-8.69546791285628E-14,127.962499999499,
-12.7882828778556));
#284486=CARTESIAN_POINT('Ctrl Pts',(-3.75838203887402,128.112499999498,
-11.5671105274575));
#284487=CARTESIAN_POINT('Ctrl Pts',(-7.51676407774795,128.262499999497,
-10.3459381770593));
#284488=CARTESIAN_POINT('Ctrl Pts',(-9.83957192047916,128.412499999497,
-7.14886745759543));
#284489=CARTESIAN_POINT('Ctrl Pts',(-12.1623797632104,128.562499999496,
-3.95179673813153));
#284490=CARTESIAN_POINT('Ctrl Pts',(-12.1623797632104,128.712499999496,
2.97892388940601E-15));
#284491=CARTESIAN_POINT('Ctrl Pts',(-12.1623797632104,128.862499999495,
3.95179673813154));
#284492=CARTESIAN_POINT('Ctrl Pts',(-9.83957192047916,129.012499999494,
7.14886745759543));
#284493=CARTESIAN_POINT('Ctrl Pts',(-7.51676407774794,129.162499999494,
10.3459381770593));
#284494=CARTESIAN_POINT('Ctrl Pts',(-3.75838203887401,129.312499999493,
11.5671105274575));
#284495=CARTESIAN_POINT('Ctrl Pts',(-8.46863078258024E-14,129.462499999493,
12.7882828778556));
#284496=CARTESIAN_POINT('Ctrl Pts',(3.75838203887384,129.612499999492,11.5671105274575));
#284497=CARTESIAN_POINT('Ctrl Pts',(7.51676407774777,129.762499999491,10.3459381770593));
#284498=CARTESIAN_POINT('Ctrl Pts',(9.83957192047899,129.912499999491,7.14886745759543));
#284499=CARTESIAN_POINT('Ctrl Pts',(12.1623797632102,130.06249999949,3.95179673813153));
#284500=CARTESIAN_POINT('Ctrl Pts',(12.1623797632102,130.21249999949,-1.489461944703E-15));
#284501=CARTESIAN_POINT('Ctrl Pts',(12.1623797632102,130.362499999489,-3.95179673813154));
#284502=CARTESIAN_POINT('Ctrl Pts',(9.83957192047899,130.512499999488,-7.14886745759543));
#284503=CARTESIAN_POINT('Ctrl Pts',(7.51676407774777,130.662499999488,-10.3459381770593));
#284504=CARTESIAN_POINT('Ctrl Pts',(3.75838203887384,130.812499999487,-11.5671105274575));
#284505=CARTESIAN_POINT('Ctrl Pts',(-8.86823884002247E-14,130.962499999487,
-12.7882828778556));
#284506=CARTESIAN_POINT('Ctrl Pts',(-3.75838203887402,131.112499999486,
-11.5671105274575));
#284507=CARTESIAN_POINT('Ctrl Pts',(-7.51676407774795,131.262499999485,
-10.3459381770593));
#284508=CARTESIAN_POINT('Ctrl Pts',(-9.83957192047916,131.412499999485,
-7.14886745759543));
#284509=CARTESIAN_POINT('Ctrl Pts',(-12.1623797632104,131.562499999484,
-3.95179673813153));
#284510=CARTESIAN_POINT('Ctrl Pts',(-12.1623797632104,131.712499999484,
2.97892388940601E-15));
#284511=CARTESIAN_POINT('Ctrl Pts',(-12.1623797632104,131.862499999483,
3.95179673813154));
#284512=CARTESIAN_POINT('Ctrl Pts',(-9.83957192047916,132.012499999482,
7.14886745759543));
#284513=CARTESIAN_POINT('Ctrl Pts',(-7.51676407774795,132.162499999482,
10.3459381770593));
#284514=CARTESIAN_POINT('Ctrl Pts',(-3.75838203887402,132.312499999481,
11.5671105274575));
#284515=CARTESIAN_POINT('Ctrl Pts',(-8.64140170974642E-14,132.462499999481,
12.7882828778556));
#284516=CARTESIAN_POINT('Ctrl Pts',(3.75838203887384,132.61249999948,11.5671105274575));
#284517=CARTESIAN_POINT('Ctrl Pts',(7.51676407774777,132.762499999479,10.3459381770593));
#284518=CARTESIAN_POINT('Ctrl Pts',(9.83957192047899,132.912499999479,7.14886745759543));
#284519=CARTESIAN_POINT('Ctrl Pts',(12.1623797632102,133.062499999478,3.95179673813153));
#284520=CARTESIAN_POINT('Ctrl Pts',(12.1623797632102,133.212499999478,-1.489461944703E-15));
#284521=CARTESIAN_POINT('Ctrl Pts',(12.1623797632102,133.362499999477,-3.95179673813154));
#284522=CARTESIAN_POINT('Ctrl Pts',(9.83957192047898,133.512499999476,-7.14886745759543));
#284523=CARTESIAN_POINT('Ctrl Pts',(7.51676407774777,133.662499999476,-10.3459381770593));
#284524=CARTESIAN_POINT('Ctrl Pts',(3.75838203887384,133.812499999475,-11.5671105274575));
#284525=CARTESIAN_POINT('Ctrl Pts',(-9.04100976718865E-14,133.962499999475,
-12.7882828778556));
#284526=CARTESIAN_POINT('Ctrl Pts',(-3.75838203887402,134.112499999474,
-11.5671105274575));
#284527=CARTESIAN_POINT('Ctrl Pts',(-7.51676407774795,134.262499999473,
-10.3459381770593));
#284528=CARTESIAN_POINT('Ctrl Pts',(-9.83957192047917,134.412499999473,
-7.14886745759543));
#284529=CARTESIAN_POINT('Ctrl Pts',(-12.1623797632104,134.562499999472,
-3.95179673813153));
#284530=CARTESIAN_POINT('Ctrl Pts',(-12.1623797632104,134.712499999472,
2.97892388940601E-15));
#284531=CARTESIAN_POINT('Ctrl Pts',(-12.1623797632104,134.862499999471,
3.95179673813154));
#284532=CARTESIAN_POINT('Ctrl Pts',(-9.83957192047916,135.01249999947,7.14886745759543));
#284533=CARTESIAN_POINT('Ctrl Pts',(-7.51676407774795,135.16249999947,10.3459381770593));
#284534=CARTESIAN_POINT('Ctrl Pts',(-3.75838203887402,135.312499999469,
11.5671105274575));
#284535=CARTESIAN_POINT('Ctrl Pts',(-8.8141726369126E-14,135.462499999469,
12.7882828778556));
#284536=CARTESIAN_POINT('Ctrl Pts',(3.75838203887384,135.612499999468,11.5671105274575));
#284537=CARTESIAN_POINT('Ctrl Pts',(7.51676407774777,135.762499999467,10.3459381770593));
#284538=CARTESIAN_POINT('Ctrl Pts',(9.83957192047898,135.912499999467,7.14886745759543));
#284539=CARTESIAN_POINT('Ctrl Pts',(12.1623797632102,136.062499999466,3.95179673813153));
#284540=CARTESIAN_POINT('Ctrl Pts',(12.1623797632102,136.212499999466,-1.489461944703E-15));
#284541=CARTESIAN_POINT('Ctrl Pts',(12.1623797632102,136.362499999465,-3.95179673813154));
#284542=CARTESIAN_POINT('Ctrl Pts',(9.83957192047898,136.512499999464,-7.14886745759543));
#284543=CARTESIAN_POINT('Ctrl Pts',(7.51676407774776,136.662499999464,-10.3459381770593));
#284544=CARTESIAN_POINT('Ctrl Pts',(3.75838203887384,136.812499999463,-11.5671105274575));
#284545=CARTESIAN_POINT('Ctrl Pts',(-9.21378069435483E-14,136.962499999463,
-12.7882828778556));
#284546=CARTESIAN_POINT('Ctrl Pts',(-3.75838203887402,137.112499999462,
-11.5671105274575));
#284547=CARTESIAN_POINT('Ctrl Pts',(-7.51676407774795,137.262499999461,
-10.3459381770593));
#284548=CARTESIAN_POINT('Ctrl Pts',(-9.83957192047917,137.412499999461,
-7.14886745759543));
#284549=CARTESIAN_POINT('Ctrl Pts',(-12.1623797632104,137.56249999946,-3.95179673813153));
#284550=CARTESIAN_POINT('Ctrl Pts',(-12.1623797632104,137.71249999946,2.97892388940601E-15));
#284551=CARTESIAN_POINT('Ctrl Pts',(-12.1623797632104,137.862499999459,
3.95179673813154));
#284552=CARTESIAN_POINT('Ctrl Pts',(-9.83957192047917,138.012499999458,
7.14886745759543));
#284553=CARTESIAN_POINT('Ctrl Pts',(-7.51676407774795,138.162499999458,
10.3459381770593));
#284554=CARTESIAN_POINT('Ctrl Pts',(-3.75838203887402,138.312499999457,
11.5671105274575));
#284555=CARTESIAN_POINT('Ctrl Pts',(-8.98694356407879E-14,138.462499999457,
12.7882828778556));
#284556=CARTESIAN_POINT('Ctrl Pts',(3.75838203887384,138.612499999456,11.5671105274575));
#284557=CARTESIAN_POINT('Ctrl Pts',(7.51676407774777,138.762499999455,10.3459381770593));
#284558=CARTESIAN_POINT('Ctrl Pts',(9.83957192047898,138.912499999455,7.14886745759543));
#284559=CARTESIAN_POINT('Ctrl Pts',(12.1623797632102,139.062499999454,3.95179673813153));
#284560=CARTESIAN_POINT('Ctrl Pts',(12.1623797632102,139.212499999454,-1.489461944703E-15));
#284561=CARTESIAN_POINT('Ctrl Pts',(12.1623797632102,139.362499999453,-3.95179673813154));
#284562=CARTESIAN_POINT('Ctrl Pts',(9.83957192047898,139.512499999452,-7.14886745759543));
#284563=CARTESIAN_POINT('Ctrl Pts',(7.51676407774776,139.662499999452,-10.3459381770593));
#284564=CARTESIAN_POINT('Ctrl Pts',(3.75838203887384,139.812499999451,-11.5671105274575));
#284565=CARTESIAN_POINT('Ctrl Pts',(-9.38655162152102E-14,139.962499999451,
-12.7882828778556));
#284566=CARTESIAN_POINT('Ctrl Pts',(-3.75838203887402,140.11249999945,-11.5671105274575));
#284567=CARTESIAN_POINT('Ctrl Pts',(-7.51676407774795,140.262499999449,
-10.3459381770593));
#284568=CARTESIAN_POINT('Ctrl Pts',(-9.83957192047917,140.412499999449,
-7.14886745759543));
#284569=CARTESIAN_POINT('Ctrl Pts',(-12.1623797632104,140.562499999448,
-3.95179673813153));
#284570=CARTESIAN_POINT('Ctrl Pts',(-12.1623797632104,140.712499999448,
2.97892388940601E-15));
#284571=CARTESIAN_POINT('Ctrl Pts',(-12.1623797632104,140.862499999447,
3.95179673813154));
#284572=CARTESIAN_POINT('Ctrl Pts',(-9.83957192047917,141.012499999446,
7.14886745759543));
#284573=CARTESIAN_POINT('Ctrl Pts',(-7.51676407774795,141.162499999446,
10.3459381770593));
#284574=CARTESIAN_POINT('Ctrl Pts',(-3.75838203887402,141.312499999445,
11.5671105274575));
#284575=CARTESIAN_POINT('Ctrl Pts',(-9.15971449124498E-14,141.462499999445,
12.7882828778556));
#284576=CARTESIAN_POINT('Ctrl Pts',(3.75838203887384,141.612499999444,11.5671105274575));
#284577=CARTESIAN_POINT('Ctrl Pts',(7.51676407774776,141.762499999443,10.3459381770593));
#284578=CARTESIAN_POINT('Ctrl Pts',(9.83957192047898,141.912499999443,7.14886745759543));
#284579=CARTESIAN_POINT('Ctrl Pts',(12.1623797632102,142.062499999442,3.95179673813153));
#284580=CARTESIAN_POINT('Ctrl Pts',(12.1623797632102,142.212499999442,-1.489461944703E-15));
#284581=CARTESIAN_POINT('Ctrl Pts',(12.1623797632102,142.362499999441,-3.95179673813154));
#284582=CARTESIAN_POINT('Ctrl Pts',(9.83957192047898,142.51249999944,-7.14886745759543));
#284583=CARTESIAN_POINT('Ctrl Pts',(7.51676407774776,142.66249999944,-10.3459381770593));
#284584=CARTESIAN_POINT('Ctrl Pts',(3.75838203887383,142.812499999439,-11.5671105274575));
#284585=CARTESIAN_POINT('Ctrl Pts',(-9.5593225486872E-14,142.962499999439,
-12.7882828778556));
#284586=CARTESIAN_POINT('Ctrl Pts',(-3.75838203887402,143.112499999438,
-11.5671105274575));
#284587=CARTESIAN_POINT('Ctrl Pts',(-7.51676407774795,143.262499999437,
-10.3459381770593));
#284588=CARTESIAN_POINT('Ctrl Pts',(-9.83957192047917,143.412499999437,
-7.14886745759543));
#284589=CARTESIAN_POINT('Ctrl Pts',(-12.1623797632104,143.562499999436,
-3.95179673813153));
#284590=CARTESIAN_POINT('Ctrl Pts',(-12.1623797632104,143.712499999436,
2.97892388940601E-15));
#284591=CARTESIAN_POINT('Ctrl Pts',(-12.1623797632104,143.862499999435,
3.95179673813154));
#284592=CARTESIAN_POINT('Ctrl Pts',(-9.83957192047917,144.012499999434,
7.14886745759543));
#284593=CARTESIAN_POINT('Ctrl Pts',(-7.51676407774795,144.162499999434,
10.3459381770593));
#284594=CARTESIAN_POINT('Ctrl Pts',(-3.75838203887402,144.312499999433,
11.5671105274575));
#284595=CARTESIAN_POINT('Ctrl Pts',(-9.33248541841116E-14,144.462499999433,
12.7882828778556));
#284596=CARTESIAN_POINT('Ctrl Pts',(3.75838203887384,144.612499999432,11.5671105274575));
#284597=CARTESIAN_POINT('Ctrl Pts',(7.51676407774776,144.762499999431,10.3459381770593));
#284598=CARTESIAN_POINT('Ctrl Pts',(9.83957192047898,144.912499999431,7.14886745759543));
#284599=CARTESIAN_POINT('Ctrl Pts',(12.1623797632102,145.06249999943,3.95179673813153));
#284600=CARTESIAN_POINT('Ctrl Pts',(12.1623797632102,145.21249999943,-1.489461944703E-15));
#284601=CARTESIAN_POINT('Ctrl Pts',(12.1623797632102,145.362499999429,-3.95179673813154));
#284602=CARTESIAN_POINT('Ctrl Pts',(9.83957192047898,145.512499999428,-7.14886745759543));
#284603=CARTESIAN_POINT('Ctrl Pts',(7.51676407774776,145.662499999428,-10.3459381770593));
#284604=CARTESIAN_POINT('Ctrl Pts',(3.75838203887383,145.812499999427,-11.5671105274575));
#284605=CARTESIAN_POINT('Ctrl Pts',(-9.73209347585338E-14,145.962499999427,
-12.7882828778556));
#284606=CARTESIAN_POINT('Ctrl Pts',(-3.75838203887403,146.112499999426,
-11.5671105274575));
#284607=CARTESIAN_POINT('Ctrl Pts',(-7.51676407774795,146.262499999425,
-10.3459381770593));
#284608=CARTESIAN_POINT('Ctrl Pts',(-9.83957192047917,146.412499999425,
-7.14886745759543));
#284609=CARTESIAN_POINT('Ctrl Pts',(-12.1623797632104,146.562499999424,
-3.95179673813153));
#284610=CARTESIAN_POINT('Ctrl Pts',(-12.1623797632104,146.712499999424,
2.97892388940601E-15));
#284611=CARTESIAN_POINT('Ctrl Pts',(-12.1623797632104,146.862499999423,
3.95179673813154));
#284612=CARTESIAN_POINT('Ctrl Pts',(-9.83957192047917,147.012499999422,
7.14886745759543));
#284613=CARTESIAN_POINT('Ctrl Pts',(-7.51676407774795,147.162499999422,
10.3459381770593));
#284614=CARTESIAN_POINT('Ctrl Pts',(-3.75838203887402,147.312499999421,
11.5671105274575));
#284615=CARTESIAN_POINT('Ctrl Pts',(-9.50525634557734E-14,147.462499999421,
12.7882828778556));
#284616=CARTESIAN_POINT('Ctrl Pts',(3.75838203887383,147.61249999942,11.5671105274575));
#284617=CARTESIAN_POINT('Ctrl Pts',(7.51676407774776,147.762499999419,10.3459381770593));
#284618=CARTESIAN_POINT('Ctrl Pts',(9.83957192047898,147.912499999419,7.14886745759543));
#284619=CARTESIAN_POINT('Ctrl Pts',(12.1623797632102,148.062499999418,3.95179673813153));
#284620=CARTESIAN_POINT('Ctrl Pts',(12.1623797632102,148.212499999418,-1.489461944703E-15));
#284621=CARTESIAN_POINT('Ctrl Pts',(12.1623797632102,148.362499999417,-3.95179673813154));
#284622=CARTESIAN_POINT('Ctrl Pts',(9.83957192047898,148.512499999416,-7.14886745759543));
#284623=CARTESIAN_POINT('Ctrl Pts',(7.51676407774776,148.662499999416,-10.3459381770593));
#284624=CARTESIAN_POINT('Ctrl Pts',(3.75838203887383,148.812499999415,-11.5671105274575));
#284625=CARTESIAN_POINT('Ctrl Pts',(-9.90486440301957E-14,148.962499999415,
-12.7882828778556));
#284626=CARTESIAN_POINT('Ctrl Pts',(-3.75838203887403,149.112499999414,
-11.5671105274575));
#284627=CARTESIAN_POINT('Ctrl Pts',(-7.51676407774795,149.262499999413,
-10.3459381770593));
#284628=CARTESIAN_POINT('Ctrl Pts',(-9.83957192047917,149.412499999413,
-7.14886745759543));
#284629=CARTESIAN_POINT('Ctrl Pts',(-12.1623797632104,149.562499999412,
-3.95179673813153));
#284630=CARTESIAN_POINT('Ctrl Pts',(-12.1623797632104,149.712499999412,
2.97892388940601E-15));
#284631=CARTESIAN_POINT('Ctrl Pts',(-12.1623797632104,149.862499999411,
3.95179673813154));
#284632=CARTESIAN_POINT('Ctrl Pts',(-9.83957192047917,150.01249999941,7.14886745759543));
#284633=CARTESIAN_POINT('Ctrl Pts',(-7.51676407774795,150.16249999941,10.3459381770593));
#284634=CARTESIAN_POINT('Ctrl Pts',(-3.75838203887403,150.312499999409,
11.5671105274575));
#284635=CARTESIAN_POINT('Ctrl Pts',(-9.67802727274353E-14,150.462499999409,
12.7882828778556));
#284636=CARTESIAN_POINT('Ctrl Pts',(3.75838203887383,150.612499999408,11.5671105274575));
#284637=CARTESIAN_POINT('Ctrl Pts',(7.51676407774776,150.762499999407,10.3459381770593));
#284638=CARTESIAN_POINT('Ctrl Pts',(9.83957192047898,150.912499999407,7.14886745759543));
#284639=CARTESIAN_POINT('Ctrl Pts',(12.1623797632102,151.062499999406,3.95179673813153));
#284640=CARTESIAN_POINT('Ctrl Pts',(12.1623797632102,151.212499999406,-1.489461944703E-15));
#284641=CARTESIAN_POINT('Ctrl Pts',(12.1623797632102,151.362499999405,-3.95179673813154));
#284642=CARTESIAN_POINT('Ctrl Pts',(9.83957192047897,151.512499999404,-7.14886745759543));
#284643=CARTESIAN_POINT('Ctrl Pts',(7.51676407774776,151.662499999404,-10.3459381770593));
#284644=CARTESIAN_POINT('Ctrl Pts',(3.75838203887383,151.812499999403,-11.5671105274575));
#284645=CARTESIAN_POINT('Ctrl Pts',(-1.00776353301858E-13,151.962499999403,
-12.7882828778556));
#284646=CARTESIAN_POINT('Ctrl Pts',(-3.75838203887403,152.112499999402,
-11.5671105274575));
#284647=CARTESIAN_POINT('Ctrl Pts',(-10.0514333556354,-2.06874452331816,
2.46189113716437E-15));
#284648=CARTESIAN_POINT('Ctrl Pts',(-10.0514333556354,-1.91874452331876,
3.26590867261837));
#284649=CARTESIAN_POINT('Ctrl Pts',(-8.13178040253628,-1.76874452331936,
5.90808429084315));
#284650=CARTESIAN_POINT('Ctrl Pts',(-6.21212744943711,-1.61874452331995,
8.55025990906793));
#284651=CARTESIAN_POINT('Ctrl Pts',(-3.10606372471856,-1.46874452332055,
9.55948119098353));
#284652=CARTESIAN_POINT('Ctrl Pts',(-9.77671522407829E-15,-1.31874452332115,
10.5687024728991));
#284653=CARTESIAN_POINT('Ctrl Pts',(3.10606372471854,-1.16874452332175,
9.55948119098353));
#284654=CARTESIAN_POINT('Ctrl Pts',(6.21212744943709,-1.01874452332235,
8.55025990906793));
#284655=CARTESIAN_POINT('Ctrl Pts',(8.13178040253625,-0.868744523322946,
5.90808429084315));
#284656=CARTESIAN_POINT('Ctrl Pts',(10.0514333556354,-0.718744523323545,
3.26590867261836));
#284657=CARTESIAN_POINT('Ctrl Pts',(10.0514333556354,-0.568744523324145,
-1.23094556858219E-15));
#284658=CARTESIAN_POINT('Ctrl Pts',(10.0514333556354,-0.418744523324745,
-3.26590867261837));
#284659=CARTESIAN_POINT('Ctrl Pts',(8.13178040253625,-0.268744523325346,
-5.90808429084315));
#284660=CARTESIAN_POINT('Ctrl Pts',(6.21212744943709,-0.118744523325947,
-8.55025990906793));
#284661=CARTESIAN_POINT('Ctrl Pts',(3.10606372471854,0.0312554766734513,
-9.55948119098353));
#284662=CARTESIAN_POINT('Ctrl Pts',(-1.32291553908245E-14,0.181255476672849,
-10.5687024728991));
#284663=CARTESIAN_POINT('Ctrl Pts',(-3.10606372471856,0.331255476672248,
-9.55948119098353));
#284664=CARTESIAN_POINT('Ctrl Pts',(-6.21212744943711,0.481255476671646,
-8.55025990906793));
#284665=CARTESIAN_POINT('Ctrl Pts',(-8.13178040253628,0.631255476671045,
-5.90808429084315));
#284666=CARTESIAN_POINT('Ctrl Pts',(-10.0514333556354,0.781255476670443,
-3.26590867261836));
#284667=CARTESIAN_POINT('Ctrl Pts',(-10.0514333556354,0.931255476669843,
2.46189113716437E-15));
#284668=CARTESIAN_POINT('Ctrl Pts',(-10.0514333556354,1.08125547666924,
3.26590867261837));
#284669=CARTESIAN_POINT('Ctrl Pts',(-8.13178040253628,1.23125547666864,
5.90808429084315));
#284670=CARTESIAN_POINT('Ctrl Pts',(-6.21212744943711,1.38125547666805,
8.55025990906793));
#284671=CARTESIAN_POINT('Ctrl Pts',(-3.10606372471856,1.53125547666745,
9.55948119098353));
#284672=CARTESIAN_POINT('Ctrl Pts',(-1.15044244957401E-14,1.68125547666685,
10.5687024728991));
#284673=CARTESIAN_POINT('Ctrl Pts',(3.10606372471854,1.83125547666625,9.55948119098353));
#284674=CARTESIAN_POINT('Ctrl Pts',(6.21212744943709,1.98125547666565,8.55025990906793));
#284675=CARTESIAN_POINT('Ctrl Pts',(8.13178040253625,2.13125547666505,5.90808429084315));
#284676=CARTESIAN_POINT('Ctrl Pts',(10.0514333556354,2.28125547666446,3.26590867261836));
#284677=CARTESIAN_POINT('Ctrl Pts',(10.0514333556354,2.43125547666386,-1.23094556858219E-15));
#284678=CARTESIAN_POINT('Ctrl Pts',(10.0514333556354,2.58125547666326,-3.26590867261837));
#284679=CARTESIAN_POINT('Ctrl Pts',(8.13178040253625,2.73125547666265,-5.90808429084315));
#284680=CARTESIAN_POINT('Ctrl Pts',(6.21212744943709,2.88125547666205,-8.55025990906793));
#284681=CARTESIAN_POINT('Ctrl Pts',(3.10606372471854,3.03125547666145,-9.55948119098353));
#284682=CARTESIAN_POINT('Ctrl Pts',(-1.49568646624864E-14,3.18125547666085,
-10.5687024728991));
#284683=CARTESIAN_POINT('Ctrl Pts',(-3.10606372471857,3.33125547666025,
-9.55948119098353));
#284684=CARTESIAN_POINT('Ctrl Pts',(-6.21212744943712,3.48125547665965,
-8.55025990906793));
#284685=CARTESIAN_POINT('Ctrl Pts',(-8.13178040253628,3.63125547665905,
-5.90808429084315));
#284686=CARTESIAN_POINT('Ctrl Pts',(-10.0514333556354,3.78125547665844,
-3.26590867261836));
#284687=CARTESIAN_POINT('Ctrl Pts',(-10.0514333556354,3.93125547665784,
2.46189113716437E-15));
#284688=CARTESIAN_POINT('Ctrl Pts',(-10.0514333556354,4.08125547665724,
3.26590867261837));
#284689=CARTESIAN_POINT('Ctrl Pts',(-8.13178040253628,4.23125547665664,
5.90808429084315));
#284690=CARTESIAN_POINT('Ctrl Pts',(-6.21212744943711,4.38125547665605,
8.55025990906793));
#284691=CARTESIAN_POINT('Ctrl Pts',(-3.10606372471856,4.53125547665545,
9.55948119098353));
#284692=CARTESIAN_POINT('Ctrl Pts',(-1.3232133767402E-14,4.68125547665485,
10.5687024728991));
#284693=CARTESIAN_POINT('Ctrl Pts',(3.10606372471854,4.83125547665425,9.55948119098353));
#284694=CARTESIAN_POINT('Ctrl Pts',(6.21212744943709,4.98125547665365,8.55025990906793));
#284695=CARTESIAN_POINT('Ctrl Pts',(8.13178040253625,5.13125547665306,5.90808429084315));
#284696=CARTESIAN_POINT('Ctrl Pts',(10.0514333556354,5.28125547665245,3.26590867261836));
#284697=CARTESIAN_POINT('Ctrl Pts',(10.0514333556354,5.43125547665185,-1.23094556858219E-15));
#284698=CARTESIAN_POINT('Ctrl Pts',(10.0514333556354,5.58125547665125,-3.26590867261837));
#284699=CARTESIAN_POINT('Ctrl Pts',(8.13178040253625,5.73125547665065,-5.90808429084315));
#284700=CARTESIAN_POINT('Ctrl Pts',(6.21212744943708,5.88125547665005,-8.55025990906793));
#284701=CARTESIAN_POINT('Ctrl Pts',(3.10606372471853,6.03125547664945,-9.55948119098353));
#284702=CARTESIAN_POINT('Ctrl Pts',(-1.66845739341482E-14,6.18125547664885,
-10.5687024728991));
#284703=CARTESIAN_POINT('Ctrl Pts',(-3.10606372471857,6.33125547664825,
-9.55948119098353));
#284704=CARTESIAN_POINT('Ctrl Pts',(-6.21212744943712,6.48125547664765,
-8.55025990906793));
#284705=CARTESIAN_POINT('Ctrl Pts',(-8.13178040253628,6.63125547664705,
-5.90808429084315));
#284706=CARTESIAN_POINT('Ctrl Pts',(-10.0514333556354,6.78125547664644,
-3.26590867261836));
#284707=CARTESIAN_POINT('Ctrl Pts',(-10.0514333556354,6.93125547664584,
2.46189113716437E-15));
#284708=CARTESIAN_POINT('Ctrl Pts',(-10.0514333556354,7.08125547664524,
3.26590867261837));
#284709=CARTESIAN_POINT('Ctrl Pts',(-8.13178040253628,7.23125547664465,
5.90808429084315));
#284710=CARTESIAN_POINT('Ctrl Pts',(-6.21212744943711,7.38125547664405,
8.55025990906793));
#284711=CARTESIAN_POINT('Ctrl Pts',(-3.10606372471857,7.53125547664345,
9.55948119098353));
#284712=CARTESIAN_POINT('Ctrl Pts',(-1.49598430390638E-14,7.68125547664285,
10.5687024728991));
#284713=CARTESIAN_POINT('Ctrl Pts',(3.10606372471854,7.83125547664225,9.55948119098353));
#284714=CARTESIAN_POINT('Ctrl Pts',(6.21212744943708,7.98125547664165,8.55025990906793));
#284715=CARTESIAN_POINT('Ctrl Pts',(8.13178040253625,8.13125547664105,5.90808429084315));
#284716=CARTESIAN_POINT('Ctrl Pts',(10.0514333556354,8.28125547664046,3.26590867261836));
#284717=CARTESIAN_POINT('Ctrl Pts',(10.0514333556354,8.43125547663985,-1.23094556858219E-15));
#284718=CARTESIAN_POINT('Ctrl Pts',(10.0514333556354,8.58125547663926,-3.26590867261837));
#284719=CARTESIAN_POINT('Ctrl Pts',(8.13178040253625,8.73125547663865,-5.90808429084315));
#284720=CARTESIAN_POINT('Ctrl Pts',(6.21212744943708,8.88125547663805,-8.55025990906793));
#284721=CARTESIAN_POINT('Ctrl Pts',(3.10606372471853,9.03125547663745,-9.55948119098353));
#284722=CARTESIAN_POINT('Ctrl Pts',(-1.84122832058101E-14,9.18125547663685,
-10.5687024728991));
#284723=CARTESIAN_POINT('Ctrl Pts',(-3.10606372471857,9.33125547663625,
-9.55948119098353));
#284724=CARTESIAN_POINT('Ctrl Pts',(-6.21212744943712,9.48125547663565,
-8.55025990906793));
#284725=CARTESIAN_POINT('Ctrl Pts',(-8.13178040253628,9.63125547663505,
-5.90808429084315));
#284726=CARTESIAN_POINT('Ctrl Pts',(-10.0514333556354,9.78125547663444,
-3.26590867261836));
#284727=CARTESIAN_POINT('Ctrl Pts',(-10.0514333556354,9.93125547663384,
2.46189113716437E-15));
#284728=CARTESIAN_POINT('Ctrl Pts',(-10.0514333556354,10.0812554766332,
3.26590867261837));
#284729=CARTESIAN_POINT('Ctrl Pts',(-8.13178040253628,10.2312554766326,
5.90808429084315));
#284730=CARTESIAN_POINT('Ctrl Pts',(-6.21212744943712,10.381255476632,8.55025990906793));
#284731=CARTESIAN_POINT('Ctrl Pts',(-3.10606372471857,10.5312554766314,
9.55948119098353));
#284732=CARTESIAN_POINT('Ctrl Pts',(-1.66875523107256E-14,10.6812554766309,
10.5687024728991));
#284733=CARTESIAN_POINT('Ctrl Pts',(3.10606372471853,10.8312554766303,9.55948119098353));
#284734=CARTESIAN_POINT('Ctrl Pts',(6.21212744943708,10.9812554766297,8.55025990906793));
#284735=CARTESIAN_POINT('Ctrl Pts',(8.13178040253625,11.1312554766291,5.90808429084315));
#284736=CARTESIAN_POINT('Ctrl Pts',(10.0514333556354,11.2812554766285,3.26590867261836));
#284737=CARTESIAN_POINT('Ctrl Pts',(10.0514333556354,11.4312554766279,-1.23094556858219E-15));
#284738=CARTESIAN_POINT('Ctrl Pts',(10.0514333556354,11.5812554766273,-3.26590867261837));
#284739=CARTESIAN_POINT('Ctrl Pts',(8.13178040253624,11.7312554766267,-5.90808429084315));
#284740=CARTESIAN_POINT('Ctrl Pts',(6.21212744943708,11.8812554766261,-8.55025990906793));
#284741=CARTESIAN_POINT('Ctrl Pts',(3.10606372471853,12.0312554766255,-9.55948119098353));
#284742=CARTESIAN_POINT('Ctrl Pts',(-2.01399924774719E-14,12.1812554766248,
-10.5687024728991));
#284743=CARTESIAN_POINT('Ctrl Pts',(-3.10606372471857,12.3312554766242,
-9.55948119098353));
#284744=CARTESIAN_POINT('Ctrl Pts',(-6.21212744943712,12.4812554766236,
-8.55025990906793));
#284745=CARTESIAN_POINT('Ctrl Pts',(-8.13178040253628,12.631255476623,-5.90808429084315));
#284746=CARTESIAN_POINT('Ctrl Pts',(-10.0514333556354,12.7812554766224,
-3.26590867261836));
#284747=CARTESIAN_POINT('Ctrl Pts',(-10.0514333556354,12.9312554766218,
2.46189113716437E-15));
#284748=CARTESIAN_POINT('Ctrl Pts',(-10.0514333556354,13.0812554766212,
3.26590867261837));
#284749=CARTESIAN_POINT('Ctrl Pts',(-8.13178040253628,13.2312554766206,
5.90808429084315));
#284750=CARTESIAN_POINT('Ctrl Pts',(-6.21212744943712,13.38125547662,8.55025990906793));
#284751=CARTESIAN_POINT('Ctrl Pts',(-3.10606372471857,13.5312554766194,
9.55948119098353));
#284752=CARTESIAN_POINT('Ctrl Pts',(-1.84152615823875E-14,13.6812554766188,
10.5687024728991));
#284753=CARTESIAN_POINT('Ctrl Pts',(3.10606372471853,13.8312554766182,9.55948119098353));
#284754=CARTESIAN_POINT('Ctrl Pts',(6.21212744943708,13.9812554766177,8.55025990906793));
#284755=CARTESIAN_POINT('Ctrl Pts',(8.13178040253624,14.1312554766171,5.90808429084315));
#284756=CARTESIAN_POINT('Ctrl Pts',(10.0514333556354,14.2812554766165,3.26590867261836));
#284757=CARTESIAN_POINT('Ctrl Pts',(10.0514333556354,14.4312554766159,-1.23094556858219E-15));
#284758=CARTESIAN_POINT('Ctrl Pts',(10.0514333556354,14.5812554766153,-3.26590867261837));
#284759=CARTESIAN_POINT('Ctrl Pts',(8.13178040253624,14.7312554766147,-5.90808429084315));
#284760=CARTESIAN_POINT('Ctrl Pts',(6.21212744943708,14.8812554766141,-8.55025990906793));
#284761=CARTESIAN_POINT('Ctrl Pts',(3.10606372471853,15.0312554766134,-9.55948119098353));
#284762=CARTESIAN_POINT('Ctrl Pts',(-2.18677017491337E-14,15.1812554766128,
-10.5687024728991));
#284763=CARTESIAN_POINT('Ctrl Pts',(-3.10606372471857,15.3312554766122,
-9.55948119098353));
#284764=CARTESIAN_POINT('Ctrl Pts',(-6.21212744943712,15.4812554766116,
-8.55025990906793));
#284765=CARTESIAN_POINT('Ctrl Pts',(-8.13178040253629,15.631255476611,-5.90808429084315));
#284766=CARTESIAN_POINT('Ctrl Pts',(-10.0514333556354,15.7812554766104,
-3.26590867261836));
#284767=CARTESIAN_POINT('Ctrl Pts',(-10.0514333556355,15.9312554766098,
2.46189113716437E-15));
#284768=CARTESIAN_POINT('Ctrl Pts',(-10.0514333556354,16.0812554766092,
3.26590867261837));
#284769=CARTESIAN_POINT('Ctrl Pts',(-8.13178040253629,16.2312554766086,
5.90808429084315));
#284770=CARTESIAN_POINT('Ctrl Pts',(-6.21212744943712,16.381255476608,8.55025990906793));
#284771=CARTESIAN_POINT('Ctrl Pts',(-3.10606372471857,16.5312554766074,
9.55948119098353));
#284772=CARTESIAN_POINT('Ctrl Pts',(-2.01429708540493E-14,16.6812554766069,
10.5687024728991));
#284773=CARTESIAN_POINT('Ctrl Pts',(3.10606372471853,16.8312554766063,9.55948119098353));
#284774=CARTESIAN_POINT('Ctrl Pts',(6.21212744943708,16.9812554766057,8.55025990906793));
#284775=CARTESIAN_POINT('Ctrl Pts',(8.13178040253624,17.1312554766051,5.90808429084315));
#284776=CARTESIAN_POINT('Ctrl Pts',(10.0514333556354,17.2812554766045,3.26590867261836));
#284777=CARTESIAN_POINT('Ctrl Pts',(10.0514333556354,17.4312554766039,-1.23094556858219E-15));
#284778=CARTESIAN_POINT('Ctrl Pts',(10.0514333556354,17.5812554766033,-3.26590867261837));
#284779=CARTESIAN_POINT('Ctrl Pts',(8.13178040253624,17.7312554766027,-5.90808429084315));
#284780=CARTESIAN_POINT('Ctrl Pts',(6.21212744943708,17.881255476602,-8.55025990906793));
#284781=CARTESIAN_POINT('Ctrl Pts',(3.10606372471853,18.0312554766015,-9.55948119098353));
#284782=CARTESIAN_POINT('Ctrl Pts',(-2.35954110207956E-14,18.1812554766008,
-10.5687024728991));
#284783=CARTESIAN_POINT('Ctrl Pts',(-3.10606372471857,18.3312554766002,
-9.55948119098353));
#284784=CARTESIAN_POINT('Ctrl Pts',(-6.21212744943713,18.4812554765996,
-8.55025990906793));
#284785=CARTESIAN_POINT('Ctrl Pts',(-8.13178040253629,18.631255476599,-5.90808429084315));
#284786=CARTESIAN_POINT('Ctrl Pts',(-10.0514333556354,18.7812554765984,
-3.26590867261836));
#284787=CARTESIAN_POINT('Ctrl Pts',(-10.0514333556355,18.9312554765978,
2.46189113716437E-15));
#284788=CARTESIAN_POINT('Ctrl Pts',(-10.0514333556354,19.0812554765972,
3.26590867261837));
#284789=CARTESIAN_POINT('Ctrl Pts',(-8.13178040253629,19.2312554765966,
5.90808429084315));
#284790=CARTESIAN_POINT('Ctrl Pts',(-6.21212744943712,19.381255476596,8.55025990906793));
#284791=CARTESIAN_POINT('Ctrl Pts',(-3.10606372471857,19.5312554765954,
9.55948119098353));
#284792=CARTESIAN_POINT('Ctrl Pts',(-2.18706801257112E-14,19.6812554765949,
10.5687024728991));
#284793=CARTESIAN_POINT('Ctrl Pts',(3.10606372471853,19.8312554765942,9.55948119098353));
#284794=CARTESIAN_POINT('Ctrl Pts',(6.21212744943708,19.9812554765937,8.55025990906793));
#284795=CARTESIAN_POINT('Ctrl Pts',(8.13178040253624,20.1312554765931,5.90808429084315));
#284796=CARTESIAN_POINT('Ctrl Pts',(10.0514333556354,20.2812554765925,3.26590867261836));
#284797=CARTESIAN_POINT('Ctrl Pts',(10.0514333556354,20.4312554765919,-1.23094556858219E-15));
#284798=CARTESIAN_POINT('Ctrl Pts',(10.0514333556354,20.5812554765913,-3.26590867261837));
#284799=CARTESIAN_POINT('Ctrl Pts',(8.13178040253624,20.7312554765907,-5.90808429084315));
#284800=CARTESIAN_POINT('Ctrl Pts',(6.21212744943708,20.88125547659,-8.55025990906793));
#284801=CARTESIAN_POINT('Ctrl Pts',(3.10606372471852,21.0312554765894,-9.55948119098353));
#284802=CARTESIAN_POINT('Ctrl Pts',(-2.53231202924574E-14,21.1812554765889,
-10.5687024728991));
#284803=CARTESIAN_POINT('Ctrl Pts',(-3.10606372471858,21.3312554765882,
-9.55948119098353));
#284804=CARTESIAN_POINT('Ctrl Pts',(-6.21212744943713,21.4812554765876,
-8.55025990906793));
#284805=CARTESIAN_POINT('Ctrl Pts',(-8.13178040253629,21.631255476587,-5.90808429084315));
#284806=CARTESIAN_POINT('Ctrl Pts',(-10.0514333556354,21.7812554765864,
-3.26590867261836));
#284807=CARTESIAN_POINT('Ctrl Pts',(-10.0514333556355,21.9312554765858,
2.46189113716437E-15));
#284808=CARTESIAN_POINT('Ctrl Pts',(-10.0514333556354,22.0812554765852,
3.26590867261837));
#284809=CARTESIAN_POINT('Ctrl Pts',(-8.13178040253629,22.2312554765846,
5.90808429084315));
#284810=CARTESIAN_POINT('Ctrl Pts',(-6.21212744943713,22.381255476584,8.55025990906793));
#284811=CARTESIAN_POINT('Ctrl Pts',(-3.10606372471857,22.5312554765834,
9.55948119098353));
#284812=CARTESIAN_POINT('Ctrl Pts',(-2.3598389397373E-14,22.6812554765828,
10.5687024728991));
#284813=CARTESIAN_POINT('Ctrl Pts',(3.10606372471853,22.8312554765822,9.55948119098353));
#284814=CARTESIAN_POINT('Ctrl Pts',(6.21212744943708,22.9812554765817,8.55025990906793));
#284815=CARTESIAN_POINT('Ctrl Pts',(8.13178040253624,23.1312554765811,5.90808429084315));
#284816=CARTESIAN_POINT('Ctrl Pts',(10.0514333556354,23.2812554765805,3.26590867261836));
#284817=CARTESIAN_POINT('Ctrl Pts',(10.0514333556354,23.4312554765799,-1.23094556858219E-15));
#284818=CARTESIAN_POINT('Ctrl Pts',(10.0514333556354,23.5812554765793,-3.26590867261837));
#284819=CARTESIAN_POINT('Ctrl Pts',(8.13178040253624,23.7312554765787,-5.90808429084315));
#284820=CARTESIAN_POINT('Ctrl Pts',(6.21212744943707,23.8812554765781,-8.55025990906793));
#284821=CARTESIAN_POINT('Ctrl Pts',(3.10606372471852,24.0312554765774,-9.55948119098353));
#284822=CARTESIAN_POINT('Ctrl Pts',(-2.70508295641193E-14,24.1812554765769,
-10.5687024728991));
#284823=CARTESIAN_POINT('Ctrl Pts',(-3.10606372471858,24.3312554765762,
-9.55948119098353));
#284824=CARTESIAN_POINT('Ctrl Pts',(-6.21212744943713,24.4812554765756,
-8.55025990906793));
#284825=CARTESIAN_POINT('Ctrl Pts',(-8.13178040253629,24.631255476575,-5.90808429084315));
#284826=CARTESIAN_POINT('Ctrl Pts',(-10.0514333556355,24.7812554765744,
-3.26590867261836));
#284827=CARTESIAN_POINT('Ctrl Pts',(-10.0514333556355,24.9312554765738,
2.46189113716437E-15));
#284828=CARTESIAN_POINT('Ctrl Pts',(-10.0514333556355,25.0812554765733,
3.26590867261837));
#284829=CARTESIAN_POINT('Ctrl Pts',(-8.13178040253629,25.2312554765726,
5.90808429084315));
#284830=CARTESIAN_POINT('Ctrl Pts',(-6.21212744943713,25.3812554765721,
8.55025990906793));
#284831=CARTESIAN_POINT('Ctrl Pts',(-3.10606372471858,25.5312554765715,
9.55948119098353));
#284832=CARTESIAN_POINT('Ctrl Pts',(-2.53260986690348E-14,25.6812554765709,
10.5687024728991));
#284833=CARTESIAN_POINT('Ctrl Pts',(3.10606372471852,25.8312554765702,9.55948119098353));
#284834=CARTESIAN_POINT('Ctrl Pts',(6.21212744943708,25.9812554765697,8.55025990906793));
#284835=CARTESIAN_POINT('Ctrl Pts',(8.13178040253624,26.1312554765691,5.90808429084315));
#284836=CARTESIAN_POINT('Ctrl Pts',(10.0514333556354,26.2812554765685,3.26590867261836));
#284837=CARTESIAN_POINT('Ctrl Pts',(10.0514333556354,26.4312554765679,-1.23094556858219E-15));
#284838=CARTESIAN_POINT('Ctrl Pts',(10.0514333556354,26.5812554765673,-3.26590867261837));
#284839=CARTESIAN_POINT('Ctrl Pts',(8.13178040253623,26.7312554765667,-5.90808429084315));
#284840=CARTESIAN_POINT('Ctrl Pts',(6.21212744943707,26.8812554765661,-8.55025990906793));
#284841=CARTESIAN_POINT('Ctrl Pts',(3.10606372471852,27.0312554765654,-9.55948119098353));
#284842=CARTESIAN_POINT('Ctrl Pts',(-2.87785388357811E-14,27.1812554765649,
-10.5687024728991));
#284843=CARTESIAN_POINT('Ctrl Pts',(-3.10606372471858,27.3312554765642,
-9.55948119098353));
#284844=CARTESIAN_POINT('Ctrl Pts',(-6.21212744943713,27.4812554765636,
-8.55025990906793));
#284845=CARTESIAN_POINT('Ctrl Pts',(-8.13178040253629,27.631255476563,-5.90808429084315));
#284846=CARTESIAN_POINT('Ctrl Pts',(-10.0514333556355,27.7812554765624,
-3.26590867261836));
#284847=CARTESIAN_POINT('Ctrl Pts',(-10.0514333556355,27.9312554765618,
2.46189113716437E-15));
#284848=CARTESIAN_POINT('Ctrl Pts',(-10.0514333556355,28.0812554765612,
3.26590867261837));
#284849=CARTESIAN_POINT('Ctrl Pts',(-8.13178040253629,28.2312554765606,
5.90808429084315));
#284850=CARTESIAN_POINT('Ctrl Pts',(-6.21212744943713,28.38125547656,8.55025990906793));
#284851=CARTESIAN_POINT('Ctrl Pts',(-3.10606372471858,28.5312554765595,
9.55948119098353));
#284852=CARTESIAN_POINT('Ctrl Pts',(-2.70538079406967E-14,28.6812554765589,
10.5687024728991));
#284853=CARTESIAN_POINT('Ctrl Pts',(3.10606372471852,28.8312554765583,9.55948119098353));
#284854=CARTESIAN_POINT('Ctrl Pts',(6.21212744943707,28.9812554765577,8.55025990906793));
#284855=CARTESIAN_POINT('Ctrl Pts',(8.13178040253623,29.1312554765571,5.90808429084315));
#284856=CARTESIAN_POINT('Ctrl Pts',(10.0514333556354,29.2812554765565,3.26590867261836));
#284857=CARTESIAN_POINT('Ctrl Pts',(10.0514333556354,29.4312554765559,-1.23094556858219E-15));
#284858=CARTESIAN_POINT('Ctrl Pts',(10.0514333556354,29.5812554765553,-3.26590867261837));
#284859=CARTESIAN_POINT('Ctrl Pts',(8.13178040253623,29.7312554765547,-5.90808429084315));
#284860=CARTESIAN_POINT('Ctrl Pts',(6.21212744943707,29.881255476554,-8.55025990906793));
#284861=CARTESIAN_POINT('Ctrl Pts',(3.10606372471852,30.0312554765534,-9.55948119098353));
#284862=CARTESIAN_POINT('Ctrl Pts',(-3.05062481074429E-14,30.1812554765528,
-10.5687024728991));
#284863=CARTESIAN_POINT('Ctrl Pts',(-3.10606372471858,30.3312554765522,
-9.55948119098353));
#284864=CARTESIAN_POINT('Ctrl Pts',(-6.21212744943713,30.4812554765516,
-8.55025990906793));
#284865=CARTESIAN_POINT('Ctrl Pts',(-8.13178040253629,30.631255476551,-5.90808429084315));
#284866=CARTESIAN_POINT('Ctrl Pts',(-10.0514333556355,30.7812554765504,
-3.26590867261836));
#284867=CARTESIAN_POINT('Ctrl Pts',(-10.0514333556355,30.9312554765498,
2.46189113716437E-15));
#284868=CARTESIAN_POINT('Ctrl Pts',(-10.0514333556355,31.0812554765492,
3.26590867261837));
#284869=CARTESIAN_POINT('Ctrl Pts',(-8.13178040253629,31.2312554765487,
5.90808429084315));
#284870=CARTESIAN_POINT('Ctrl Pts',(-6.21212744943713,31.381255476548,8.55025990906793));
#284871=CARTESIAN_POINT('Ctrl Pts',(-3.10606372471858,31.5312554765474,
9.55948119098353));
#284872=CARTESIAN_POINT('Ctrl Pts',(-2.87815172123585E-14,31.6812554765468,
10.5687024728991));
#284873=CARTESIAN_POINT('Ctrl Pts',(3.10606372471852,31.8312554765463,9.55948119098353));
#284874=CARTESIAN_POINT('Ctrl Pts',(6.21212744943707,31.9812554765457,8.55025990906793));
#284875=CARTESIAN_POINT('Ctrl Pts',(8.13178040253623,32.1312554765451,5.90808429084315));
#284876=CARTESIAN_POINT('Ctrl Pts',(10.0514333556354,32.2812554765445,3.26590867261836));
#284877=CARTESIAN_POINT('Ctrl Pts',(10.0514333556354,32.4312554765439,-1.23094556858219E-15));
#284878=CARTESIAN_POINT('Ctrl Pts',(10.0514333556354,32.5812554765433,-3.26590867261837));
#284879=CARTESIAN_POINT('Ctrl Pts',(8.13178040253623,32.7312554765427,-5.90808429084315));
#284880=CARTESIAN_POINT('Ctrl Pts',(6.21212744943707,32.881255476542,-8.55025990906793));
#284881=CARTESIAN_POINT('Ctrl Pts',(3.10606372471852,33.0312554765415,-9.55948119098353));
#284882=CARTESIAN_POINT('Ctrl Pts',(-3.22339573791048E-14,33.1812554765408,
-10.5687024728991));
#284883=CARTESIAN_POINT('Ctrl Pts',(-3.10606372471858,33.3312554765402,
-9.55948119098353));
#284884=CARTESIAN_POINT('Ctrl Pts',(-6.21212744943713,33.4812554765397,
-8.55025990906793));
#284885=CARTESIAN_POINT('Ctrl Pts',(-8.1317804025363,33.631255476539,-5.90808429084315));
#284886=CARTESIAN_POINT('Ctrl Pts',(-10.0514333556355,33.7812554765384,
-3.26590867261836));
#284887=CARTESIAN_POINT('Ctrl Pts',(-10.0514333556355,33.9312554765378,
2.46189113716437E-15));
#284888=CARTESIAN_POINT('Ctrl Pts',(-10.0514333556355,34.0812554765372,
3.26590867261837));
#284889=CARTESIAN_POINT('Ctrl Pts',(-8.1317804025363,34.2312554765366,5.90808429084315));
#284890=CARTESIAN_POINT('Ctrl Pts',(-6.21212744943713,34.381255476536,8.55025990906793));
#284891=CARTESIAN_POINT('Ctrl Pts',(-3.10606372471858,34.5312554765354,
9.55948119098353));
#284892=CARTESIAN_POINT('Ctrl Pts',(-3.05092264840204E-14,34.6812554765349,
10.5687024728991));
#284893=CARTESIAN_POINT('Ctrl Pts',(3.10606372471852,34.8312554765343,9.55948119098353));
#284894=CARTESIAN_POINT('Ctrl Pts',(6.21212744943707,34.9812554765337,8.55025990906793));
#284895=CARTESIAN_POINT('Ctrl Pts',(8.13178040253623,35.1312554765331,5.90808429084315));
#284896=CARTESIAN_POINT('Ctrl Pts',(10.0514333556354,35.2812554765325,3.26590867261836));
#284897=CARTESIAN_POINT('Ctrl Pts',(10.0514333556354,35.4312554765319,-1.23094556858219E-15));
#284898=CARTESIAN_POINT('Ctrl Pts',(10.0514333556354,35.5812554765313,-3.26590867261837));
#284899=CARTESIAN_POINT('Ctrl Pts',(8.13178040253623,35.7312554765307,-5.90808429084315));
#284900=CARTESIAN_POINT('Ctrl Pts',(6.21212744943707,35.8812554765301,-8.55025990906793));
#284901=CARTESIAN_POINT('Ctrl Pts',(3.10606372471852,36.0312554765295,-9.55948119098353));
#284902=CARTESIAN_POINT('Ctrl Pts',(-3.39616666507666E-14,36.1812554765289,
-10.5687024728991));
#284903=CARTESIAN_POINT('Ctrl Pts',(-3.10606372471859,36.3312554765282,
-9.55948119098353));
#284904=CARTESIAN_POINT('Ctrl Pts',(-6.21212744943714,36.4812554765277,
-8.55025990906793));
#284905=CARTESIAN_POINT('Ctrl Pts',(-8.1317804025363,36.631255476527,-5.90808429084315));
#284906=CARTESIAN_POINT('Ctrl Pts',(-10.0514333556355,36.7812554765265,
-3.26590867261836));
#284907=CARTESIAN_POINT('Ctrl Pts',(-10.0514333556355,36.9312554765258,
2.46189113716437E-15));
#284908=CARTESIAN_POINT('Ctrl Pts',(-10.0514333556355,37.0812554765252,
3.26590867261837));
#284909=CARTESIAN_POINT('Ctrl Pts',(-8.1317804025363,37.2312554765246,5.90808429084315));
#284910=CARTESIAN_POINT('Ctrl Pts',(-6.21212744943713,37.381255476524,8.55025990906793));
#284911=CARTESIAN_POINT('Ctrl Pts',(-3.10606372471858,37.5312554765234,
9.55948119098353));
#284912=CARTESIAN_POINT('Ctrl Pts',(-3.22369357556822E-14,37.6812554765228,
10.5687024728991));
#284913=CARTESIAN_POINT('Ctrl Pts',(3.10606372471852,37.8312554765223,9.55948119098353));
#284914=CARTESIAN_POINT('Ctrl Pts',(6.21212744943707,37.9812554765217,8.55025990906793));
#284915=CARTESIAN_POINT('Ctrl Pts',(8.13178040253623,38.1312554765211,5.90808429084315));
#284916=CARTESIAN_POINT('Ctrl Pts',(10.0514333556354,38.2812554765204,3.26590867261836));
#284917=CARTESIAN_POINT('Ctrl Pts',(10.0514333556354,38.4312554765199,-1.23094556858219E-15));
#284918=CARTESIAN_POINT('Ctrl Pts',(10.0514333556354,38.5812554765193,-3.26590867261837));
#284919=CARTESIAN_POINT('Ctrl Pts',(8.13178040253623,38.7312554765187,-5.90808429084315));
#284920=CARTESIAN_POINT('Ctrl Pts',(6.21212744943707,38.881255476518,-8.55025990906793));
#284921=CARTESIAN_POINT('Ctrl Pts',(3.10606372471851,39.0312554765174,-9.55948119098353));
#284922=CARTESIAN_POINT('Ctrl Pts',(-3.56893759224285E-14,39.1812554765169,
-10.5687024728991));
#284923=CARTESIAN_POINT('Ctrl Pts',(-3.10606372471859,39.3312554765162,
-9.55948119098353));
#284924=CARTESIAN_POINT('Ctrl Pts',(-6.21212744943714,39.4812554765156,
-8.55025990906793));
#284925=CARTESIAN_POINT('Ctrl Pts',(-8.1317804025363,39.631255476515,-5.90808429084315));
#284926=CARTESIAN_POINT('Ctrl Pts',(-10.0514333556355,39.7812554765145,
-3.26590867261836));
#284927=CARTESIAN_POINT('Ctrl Pts',(-10.0514333556355,39.9312554765138,
2.46189113716437E-15));
#284928=CARTESIAN_POINT('Ctrl Pts',(-10.0514333556355,40.0812554765132,
3.26590867261837));
#284929=CARTESIAN_POINT('Ctrl Pts',(-8.1317804025363,40.2312554765126,5.90808429084315));
#284930=CARTESIAN_POINT('Ctrl Pts',(-6.21212744943714,40.381255476512,8.55025990906793));
#284931=CARTESIAN_POINT('Ctrl Pts',(-3.10606372471859,40.5312554765114,
9.55948119098353));
#284932=CARTESIAN_POINT('Ctrl Pts',(-3.39646450273441E-14,40.6812554765108,
10.5687024728991));
#284933=CARTESIAN_POINT('Ctrl Pts',(3.10606372471852,40.8312554765103,9.55948119098353));
#284934=CARTESIAN_POINT('Ctrl Pts',(6.21212744943707,40.9812554765097,8.55025990906793));
#284935=CARTESIAN_POINT('Ctrl Pts',(8.13178040253623,41.1312554765091,5.90808429084315));
#284936=CARTESIAN_POINT('Ctrl Pts',(10.0514333556354,41.2812554765085,3.26590867261836));
#284937=CARTESIAN_POINT('Ctrl Pts',(10.0514333556354,41.4312554765079,-1.23094556858219E-15));
#284938=CARTESIAN_POINT('Ctrl Pts',(10.0514333556354,41.5812554765073,-3.26590867261837));
#284939=CARTESIAN_POINT('Ctrl Pts',(8.13178040253623,41.7312554765067,-5.90808429084315));
#284940=CARTESIAN_POINT('Ctrl Pts',(6.21212744943706,41.8812554765061,-8.55025990906793));
#284941=CARTESIAN_POINT('Ctrl Pts',(3.10606372471851,42.0312554765054,-9.55948119098353));
#284942=CARTESIAN_POINT('Ctrl Pts',(-3.74170851940903E-14,42.1812554765049,
-10.5687024728991));
#284943=CARTESIAN_POINT('Ctrl Pts',(-3.10606372471859,42.3312554765042,
-9.55948119098353));
#284944=CARTESIAN_POINT('Ctrl Pts',(-6.21212744943714,42.4812554765036,
-8.55025990906793));
#284945=CARTESIAN_POINT('Ctrl Pts',(-8.1317804025363,42.631255476503,-5.90808429084315));
#284946=CARTESIAN_POINT('Ctrl Pts',(-10.0514333556355,42.7812554765024,
-3.26590867261836));
#284947=CARTESIAN_POINT('Ctrl Pts',(-10.0514333556355,42.9312554765018,
2.46189113716437E-15));
#284948=CARTESIAN_POINT('Ctrl Pts',(-10.0514333556355,43.0812554765012,
3.26590867261837));
#284949=CARTESIAN_POINT('Ctrl Pts',(-8.1317804025363,43.2312554765006,5.90808429084315));
#284950=CARTESIAN_POINT('Ctrl Pts',(-6.21212744943714,43.3812554765001,
8.55025990906793));
#284951=CARTESIAN_POINT('Ctrl Pts',(-3.10606372471859,43.5312554764994,
9.55948119098353));
#284952=CARTESIAN_POINT('Ctrl Pts',(-3.56923542990059E-14,43.6812554764988,
10.5687024728991));
#284953=CARTESIAN_POINT('Ctrl Pts',(3.10606372471851,43.8312554764982,9.55948119098353));
#284954=CARTESIAN_POINT('Ctrl Pts',(6.21212744943706,43.9812554764976,8.55025990906793));
#284955=CARTESIAN_POINT('Ctrl Pts',(8.13178040253623,44.1312554764971,5.90808429084315));
#284956=CARTESIAN_POINT('Ctrl Pts',(10.0514333556354,44.2812554764965,3.26590867261836));
#284957=CARTESIAN_POINT('Ctrl Pts',(10.0514333556354,44.4312554764959,-1.23094556858219E-15));
#284958=CARTESIAN_POINT('Ctrl Pts',(10.0514333556354,44.5812554764953,-3.26590867261837));
#284959=CARTESIAN_POINT('Ctrl Pts',(8.13178040253622,44.7312554764947,-5.90808429084315));
#284960=CARTESIAN_POINT('Ctrl Pts',(6.21212744943706,44.881255476494,-8.55025990906793));
#284961=CARTESIAN_POINT('Ctrl Pts',(3.10606372471851,45.0312554764935,-9.55948119098353));
#284962=CARTESIAN_POINT('Ctrl Pts',(-3.91447944657521E-14,45.1812554764929,
-10.5687024728991));
#284963=CARTESIAN_POINT('Ctrl Pts',(-3.10606372471859,45.3312554764922,
-9.55948119098353));
#284964=CARTESIAN_POINT('Ctrl Pts',(-6.21212744943714,45.4812554764916,
-8.55025990906793));
#284965=CARTESIAN_POINT('Ctrl Pts',(-8.1317804025363,45.631255476491,-5.90808429084315));
#284966=CARTESIAN_POINT('Ctrl Pts',(-10.0514333556355,45.7812554764904,
-3.26590867261836));
#284967=CARTESIAN_POINT('Ctrl Pts',(-10.0514333556355,45.9312554764898,
2.46189113716437E-15));
#284968=CARTESIAN_POINT('Ctrl Pts',(-10.0514333556355,46.0812554764892,
3.26590867261837));
#284969=CARTESIAN_POINT('Ctrl Pts',(-8.1317804025363,46.2312554764886,5.90808429084315));
#284970=CARTESIAN_POINT('Ctrl Pts',(-6.21212744943714,46.381255476488,8.55025990906793));
#284971=CARTESIAN_POINT('Ctrl Pts',(-3.10606372471859,46.5312554764875,
9.55948119098353));
#284972=CARTESIAN_POINT('Ctrl Pts',(-3.74200635706677E-14,46.6812554764869,
10.5687024728991));
#284973=CARTESIAN_POINT('Ctrl Pts',(3.10606372471851,46.8312554764862,9.55948119098353));
#284974=CARTESIAN_POINT('Ctrl Pts',(6.21212744943706,46.9812554764857,8.55025990906793));
#284975=CARTESIAN_POINT('Ctrl Pts',(8.13178040253622,47.1312554764851,5.90808429084315));
#284976=CARTESIAN_POINT('Ctrl Pts',(10.0514333556354,47.2812554764845,3.26590867261836));
#284977=CARTESIAN_POINT('Ctrl Pts',(10.0514333556354,47.4312554764839,-1.23094556858219E-15));
#284978=CARTESIAN_POINT('Ctrl Pts',(10.0514333556354,47.5812554764833,-3.26590867261837));
#284979=CARTESIAN_POINT('Ctrl Pts',(8.13178040253622,47.7312554764826,-5.90808429084315));
#284980=CARTESIAN_POINT('Ctrl Pts',(6.21212744943706,47.8812554764821,-8.55025990906793));
#284981=CARTESIAN_POINT('Ctrl Pts',(3.10606372471851,48.0312554764814,-9.55948119098353));
#284982=CARTESIAN_POINT('Ctrl Pts',(-4.0872503737414E-14,48.1812554764809,
-10.5687024728991));
#284983=CARTESIAN_POINT('Ctrl Pts',(-3.10606372471859,48.3312554764803,
-9.55948119098353));
#284984=CARTESIAN_POINT('Ctrl Pts',(-6.21212744943714,48.4812554764797,
-8.55025990906793));
#284985=CARTESIAN_POINT('Ctrl Pts',(-8.13178040253631,48.631255476479,-5.90808429084315));
#284986=CARTESIAN_POINT('Ctrl Pts',(-10.0514333556355,48.7812554764784,
-3.26590867261836));
#284987=CARTESIAN_POINT('Ctrl Pts',(-10.0514333556355,48.9312554764778,
2.46189113716437E-15));
#284988=CARTESIAN_POINT('Ctrl Pts',(-10.0514333556355,49.0812554764772,
3.26590867261837));
#284989=CARTESIAN_POINT('Ctrl Pts',(-8.13178040253631,49.2312554764766,
5.90808429084315));
#284990=CARTESIAN_POINT('Ctrl Pts',(-6.21212744943714,49.381255476476,8.55025990906793));
#284991=CARTESIAN_POINT('Ctrl Pts',(-3.10606372471859,49.5312554764755,
9.55948119098353));
#284992=CARTESIAN_POINT('Ctrl Pts',(-3.91477728423295E-14,49.6812554764748,
10.5687024728991));
#284993=CARTESIAN_POINT('Ctrl Pts',(3.10606372471851,49.8312554764742,9.55948119098353));
#284994=CARTESIAN_POINT('Ctrl Pts',(6.21212744943706,49.9812554764736,8.55025990906793));
#284995=CARTESIAN_POINT('Ctrl Pts',(8.13178040253622,50.1312554764731,5.90808429084315));
#284996=CARTESIAN_POINT('Ctrl Pts',(10.0514333556354,50.2812554764725,3.26590867261836));
#284997=CARTESIAN_POINT('Ctrl Pts',(10.0514333556354,50.4312554764719,-1.23094556858219E-15));
#284998=CARTESIAN_POINT('Ctrl Pts',(10.0514333556354,50.5812554764713,-3.26590867261837));
#284999=CARTESIAN_POINT('Ctrl Pts',(8.13178040253622,50.7312554764707,-5.90808429084315));
#285000=CARTESIAN_POINT('Ctrl Pts',(6.21212744943706,50.88125547647,-8.55025990906793));
#285001=CARTESIAN_POINT('Ctrl Pts',(3.10606372471851,51.0312554764695,-9.55948119098353));
#285002=CARTESIAN_POINT('Ctrl Pts',(-4.26002130090758E-14,51.1812554764689,
-10.5687024728991));
#285003=CARTESIAN_POINT('Ctrl Pts',(-3.10606372471859,51.3312554764683,
-9.55948119098353));
#285004=CARTESIAN_POINT('Ctrl Pts',(-6.21212744943715,51.4812554764676,
-8.55025990906793));
#285005=CARTESIAN_POINT('Ctrl Pts',(-8.13178040253631,51.6312554764671,
-5.90808429084315));
#285006=CARTESIAN_POINT('Ctrl Pts',(-10.0514333556355,51.7812554764664,
-3.26590867261836));
#285007=CARTESIAN_POINT('Ctrl Pts',(-10.0514333556355,51.9312554764658,
2.46189113716437E-15));
#285008=CARTESIAN_POINT('Ctrl Pts',(-10.0514333556355,52.0812554764652,
3.26590867261837));
#285009=CARTESIAN_POINT('Ctrl Pts',(-8.13178040253631,52.2312554764646,
5.90808429084315));
#285010=CARTESIAN_POINT('Ctrl Pts',(-6.21212744943714,52.381255476464,8.55025990906793));
#285011=CARTESIAN_POINT('Ctrl Pts',(-3.10606372471859,52.5312554764634,
9.55948119098353));
#285012=CARTESIAN_POINT('Ctrl Pts',(-4.08754821139914E-14,52.6812554764629,
10.5687024728991));
#285013=CARTESIAN_POINT('Ctrl Pts',(3.10606372471851,52.8312554764622,9.55948119098353));
#285014=CARTESIAN_POINT('Ctrl Pts',(6.21212744943706,52.9812554764617,8.55025990906793));
#285015=CARTESIAN_POINT('Ctrl Pts',(8.13178040253622,53.1312554764611,5.90808429084315));
#285016=CARTESIAN_POINT('Ctrl Pts',(10.0514333556354,53.2812554764605,3.26590867261836));
#285017=CARTESIAN_POINT('Ctrl Pts',(10.0514333556354,53.4312554764599,-1.23094556858219E-15));
#285018=CARTESIAN_POINT('Ctrl Pts',(10.0514333556354,53.5812554764593,-3.26590867261837));
#285019=CARTESIAN_POINT('Ctrl Pts',(8.13178040253622,53.7312554764587,-5.90808429084315));
#285020=CARTESIAN_POINT('Ctrl Pts',(6.21212744943706,53.8812554764581,-8.55025990906793));
#285021=CARTESIAN_POINT('Ctrl Pts',(3.10606372471851,54.0312554764574,-9.55948119098353));
#285022=CARTESIAN_POINT('Ctrl Pts',(-4.43279222807376E-14,54.1812554764569,
-10.5687024728991));
#285023=CARTESIAN_POINT('Ctrl Pts',(-3.1060637247186,54.3312554764562,-9.55948119098353));
#285024=CARTESIAN_POINT('Ctrl Pts',(-6.21212744943715,54.4812554764556,
-8.55025990906793));
#285025=CARTESIAN_POINT('Ctrl Pts',(-8.13178040253631,54.631255476455,-5.90808429084315));
#285026=CARTESIAN_POINT('Ctrl Pts',(-10.0514333556355,54.7812554764544,
-3.26590867261836));
#285027=CARTESIAN_POINT('Ctrl Pts',(-10.0514333556355,54.9312554764538,
2.46189113716437E-15));
#285028=CARTESIAN_POINT('Ctrl Pts',(-10.0514333556355,55.0812554764532,
3.26590867261837));
#285029=CARTESIAN_POINT('Ctrl Pts',(-8.13178040253631,55.2312554764526,
5.90808429084315));
#285030=CARTESIAN_POINT('Ctrl Pts',(-6.21212744943715,55.381255476452,8.55025990906793));
#285031=CARTESIAN_POINT('Ctrl Pts',(-3.10606372471859,55.5312554764514,
9.55948119098353));
#285032=CARTESIAN_POINT('Ctrl Pts',(-4.26031913856532E-14,55.6812554764508,
10.5687024728991));
#285033=CARTESIAN_POINT('Ctrl Pts',(3.10606372471851,55.8312554764502,9.55948119098353));
#285034=CARTESIAN_POINT('Ctrl Pts',(6.21212744943706,55.9812554764496,8.55025990906793));
#285035=CARTESIAN_POINT('Ctrl Pts',(8.13178040253622,56.1312554764491,5.90808429084315));
#285036=CARTESIAN_POINT('Ctrl Pts',(10.0514333556354,56.2812554764485,3.26590867261836));
#285037=CARTESIAN_POINT('Ctrl Pts',(10.0514333556354,56.4312554764479,-1.23094556858219E-15));
#285038=CARTESIAN_POINT('Ctrl Pts',(10.0514333556354,56.5812554764473,-3.26590867261837));
#285039=CARTESIAN_POINT('Ctrl Pts',(8.13178040253622,56.7312554764467,-5.90808429084315));
#285040=CARTESIAN_POINT('Ctrl Pts',(6.21212744943706,56.881255476446,-8.55025990906793));
#285041=CARTESIAN_POINT('Ctrl Pts',(3.10606372471851,57.0312554764455,-9.55948119098353));
#285042=CARTESIAN_POINT('Ctrl Pts',(-4.60556315523995E-14,57.1812554764448,
-10.5687024728991));
#285043=CARTESIAN_POINT('Ctrl Pts',(-3.1060637247186,57.3312554764443,-9.55948119098353));
#285044=CARTESIAN_POINT('Ctrl Pts',(-6.21212744943715,57.4812554764436,
-8.55025990906793));
#285045=CARTESIAN_POINT('Ctrl Pts',(-8.13178040253631,57.631255476443,-5.90808429084315));
#285046=CARTESIAN_POINT('Ctrl Pts',(-10.0514333556355,57.7812554764424,
-3.26590867261836));
#285047=CARTESIAN_POINT('Ctrl Pts',(-10.0514333556355,57.9312554764418,
2.46189113716437E-15));
#285048=CARTESIAN_POINT('Ctrl Pts',(-10.0514333556355,58.0812554764412,
3.26590867261837));
#285049=CARTESIAN_POINT('Ctrl Pts',(-8.13178040253631,58.2312554764406,
5.90808429084315));
#285050=CARTESIAN_POINT('Ctrl Pts',(-6.21212744943715,58.38125547644,8.55025990906793));
#285051=CARTESIAN_POINT('Ctrl Pts',(-3.10606372471859,58.5312554764394,
9.55948119098353));
#285052=CARTESIAN_POINT('Ctrl Pts',(-4.43309006573151E-14,58.6812554764388,
10.5687024728991));
#285053=CARTESIAN_POINT('Ctrl Pts',(3.10606372471851,58.8312554764382,9.55948119098353));
#285054=CARTESIAN_POINT('Ctrl Pts',(6.21212744943706,58.9812554764377,8.55025990906793));
#285055=CARTESIAN_POINT('Ctrl Pts',(8.13178040253622,59.1312554764371,5.90808429084315));
#285056=CARTESIAN_POINT('Ctrl Pts',(10.0514333556354,59.2812554764365,3.26590867261836));
#285057=CARTESIAN_POINT('Ctrl Pts',(10.0514333556354,59.4312554764359,-1.23094556858219E-15));
#285058=CARTESIAN_POINT('Ctrl Pts',(10.0514333556354,59.5812554764353,-3.26590867261837));
#285059=CARTESIAN_POINT('Ctrl Pts',(8.13178040253622,59.7312554764347,-5.90808429084315));
#285060=CARTESIAN_POINT('Ctrl Pts',(6.21212744943706,59.8812554764341,-8.55025990906793));
#285061=CARTESIAN_POINT('Ctrl Pts',(3.1060637247185,60.0312554764335,-9.55948119098353));
#285062=CARTESIAN_POINT('Ctrl Pts',(-4.77833408240613E-14,60.1812554764329,
-10.5687024728991));
#285063=CARTESIAN_POINT('Ctrl Pts',(-3.1060637247186,60.3312554764322,-9.55948119098353));
#285064=CARTESIAN_POINT('Ctrl Pts',(-6.21212744943715,60.4812554764316,
-8.55025990906793));
#285065=CARTESIAN_POINT('Ctrl Pts',(-8.13178040253631,60.631255476431,-5.90808429084315));
#285066=CARTESIAN_POINT('Ctrl Pts',(-10.0514333556355,60.7812554764304,
-3.26590867261836));
#285067=CARTESIAN_POINT('Ctrl Pts',(-10.0514333556355,60.9312554764298,
2.46189113716437E-15));
#285068=CARTESIAN_POINT('Ctrl Pts',(-10.0514333556355,61.0812554764292,
3.26590867261837));
#285069=CARTESIAN_POINT('Ctrl Pts',(-8.13178040253631,61.2312554764286,
5.90808429084315));
#285070=CARTESIAN_POINT('Ctrl Pts',(-6.21212744943715,61.381255476428,8.55025990906793));
#285071=CARTESIAN_POINT('Ctrl Pts',(-3.1060637247186,61.5312554764274,9.55948119098353));
#285072=CARTESIAN_POINT('Ctrl Pts',(-4.60586099289769E-14,61.6812554764268,
10.5687024728991));
#285073=CARTESIAN_POINT('Ctrl Pts',(3.1060637247185,61.8312554764263,9.55948119098353));
#285074=CARTESIAN_POINT('Ctrl Pts',(6.21212744943706,61.9812554764256,8.55025990906793));
#285075=CARTESIAN_POINT('Ctrl Pts',(8.13178040253622,62.1312554764251,5.90808429084315));
#285076=CARTESIAN_POINT('Ctrl Pts',(10.0514333556354,62.2812554764245,3.26590867261836));
#285077=CARTESIAN_POINT('Ctrl Pts',(10.0514333556354,62.4312554764238,-1.23094556858219E-15));
#285078=CARTESIAN_POINT('Ctrl Pts',(10.0514333556354,62.5812554764233,-3.26590867261837));
#285079=CARTESIAN_POINT('Ctrl Pts',(8.13178040253621,62.7312554764227,-5.90808429084315));
#285080=CARTESIAN_POINT('Ctrl Pts',(6.21212744943705,62.8812554764221,-8.55025990906793));
#285081=CARTESIAN_POINT('Ctrl Pts',(3.1060637247185,63.0312554764215,-9.55948119098353));
#285082=CARTESIAN_POINT('Ctrl Pts',(-4.95110500957232E-14,63.1812554764208,
-10.5687024728991));
#285083=CARTESIAN_POINT('Ctrl Pts',(-3.1060637247186,63.3312554764203,-9.55948119098353));
#285084=CARTESIAN_POINT('Ctrl Pts',(-6.21212744943715,63.4812554764196,
-8.55025990906793));
#285085=CARTESIAN_POINT('Ctrl Pts',(-8.13178040253631,63.631255476419,-5.90808429084315));
#285086=CARTESIAN_POINT('Ctrl Pts',(-10.0514333556355,63.7812554764184,
-3.26590867261836));
#285087=CARTESIAN_POINT('Ctrl Pts',(-10.0514333556355,63.9312554764178,
2.46189113716437E-15));
#285088=CARTESIAN_POINT('Ctrl Pts',(-10.0514333556355,64.0812554764173,
3.26590867261837));
#285089=CARTESIAN_POINT('Ctrl Pts',(-8.13178040253631,64.2312554764166,
5.90808429084315));
#285090=CARTESIAN_POINT('Ctrl Pts',(-6.21212744943715,64.3812554764161,
8.55025990906793));
#285091=CARTESIAN_POINT('Ctrl Pts',(-3.1060637247186,64.5312554764155,9.55948119098353));
#285092=CARTESIAN_POINT('Ctrl Pts',(-4.77863192006388E-14,64.6812554764149,
10.5687024728991));
#285093=CARTESIAN_POINT('Ctrl Pts',(3.1060637247185,64.8312554764142,9.55948119098353));
#285094=CARTESIAN_POINT('Ctrl Pts',(6.21212744943705,64.9812554764137,8.55025990906793));
#285095=CARTESIAN_POINT('Ctrl Pts',(8.13178040253621,65.1312554764131,5.90808429084315));
#285096=CARTESIAN_POINT('Ctrl Pts',(10.0514333556354,65.2812554764124,3.26590867261836));
#285097=CARTESIAN_POINT('Ctrl Pts',(10.0514333556354,65.4312554764118,-1.23094556858219E-15));
#285098=CARTESIAN_POINT('Ctrl Pts',(10.0514333556354,65.5812554764112,-3.26590867261837));
#285099=CARTESIAN_POINT('Ctrl Pts',(8.13178040253621,65.7312554764107,-5.90808429084315));
#285100=CARTESIAN_POINT('Ctrl Pts',(6.21212744943705,65.8812554764101,-8.55025990906793));
#285101=CARTESIAN_POINT('Ctrl Pts',(3.1060637247185,66.0312554764095,-9.55948119098353));
#285102=CARTESIAN_POINT('Ctrl Pts',(-5.1238759367385E-14,66.1812554764089,
-10.5687024728991));
#285103=CARTESIAN_POINT('Ctrl Pts',(-3.1060637247186,66.3312554764082,-9.55948119098353));
#285104=CARTESIAN_POINT('Ctrl Pts',(-6.21212744943715,66.4812554764077,
-8.55025990906793));
#285105=CARTESIAN_POINT('Ctrl Pts',(-8.13178040253632,66.631255476407,-5.90808429084315));
#285106=CARTESIAN_POINT('Ctrl Pts',(-10.0514333556355,66.7812554764064,
-3.26590867261836));
#285107=CARTESIAN_POINT('Ctrl Pts',(-10.0514333556355,66.9312554764059,
2.46189113716437E-15));
#285108=CARTESIAN_POINT('Ctrl Pts',(-10.0514333556355,67.0812554764052,
3.26590867261837));
#285109=CARTESIAN_POINT('Ctrl Pts',(-8.13178040253632,67.2312554764047,
5.90808429084315));
#285110=CARTESIAN_POINT('Ctrl Pts',(-6.21212744943715,67.381255476404,8.55025990906793));
#285111=CARTESIAN_POINT('Ctrl Pts',(-3.1060637247186,67.5312554764035,9.55948119098353));
#285112=CARTESIAN_POINT('Ctrl Pts',(-4.95140284723006E-14,67.6812554764028,
10.5687024728991));
#285113=CARTESIAN_POINT('Ctrl Pts',(3.1060637247185,67.8312554764022,9.55948119098353));
#285114=CARTESIAN_POINT('Ctrl Pts',(6.21212744943705,67.9812554764016,8.55025990906793));
#285115=CARTESIAN_POINT('Ctrl Pts',(8.13178040253621,68.131255476401,5.90808429084315));
#285116=CARTESIAN_POINT('Ctrl Pts',(10.0514333556354,68.2812554764004,3.26590867261836));
#285117=CARTESIAN_POINT('Ctrl Pts',(10.0514333556354,68.4312554763998,-1.23094556858219E-15));
#285118=CARTESIAN_POINT('Ctrl Pts',(10.0514333556354,68.5812554763992,-3.26590867261837));
#285119=CARTESIAN_POINT('Ctrl Pts',(8.13178040253621,68.7312554763986,-5.90808429084315));
#285120=CARTESIAN_POINT('Ctrl Pts',(6.21212744943705,68.8812554763981,-8.55025990906793));
#285121=CARTESIAN_POINT('Ctrl Pts',(3.1060637247185,69.0312554763974,-9.55948119098353));
#285122=CARTESIAN_POINT('Ctrl Pts',(-5.29664686390469E-14,69.1812554763968,
-10.5687024728991));
#285123=CARTESIAN_POINT('Ctrl Pts',(-3.1060637247186,69.3312554763963,-9.55948119098353));
#285124=CARTESIAN_POINT('Ctrl Pts',(-6.21212744943715,69.4812554763957,
-8.55025990906793));
#285125=CARTESIAN_POINT('Ctrl Pts',(-8.13178040253632,69.6312554763951,
-5.90808429084315));
#285126=CARTESIAN_POINT('Ctrl Pts',(-10.0514333556355,69.7812554763944,
-3.26590867261836));
#285127=CARTESIAN_POINT('Ctrl Pts',(-10.0514333556355,69.9312554763938,
2.46189113716437E-15));
#285128=CARTESIAN_POINT('Ctrl Pts',(-10.0514333556355,70.0812554763932,
3.26590867261837));
#285129=CARTESIAN_POINT('Ctrl Pts',(-8.13178040253632,70.2312554763926,
5.90808429084315));
#285130=CARTESIAN_POINT('Ctrl Pts',(-6.21212744943715,70.381255476392,8.55025990906793));
#285131=CARTESIAN_POINT('Ctrl Pts',(-3.1060637247186,70.5312554763914,9.55948119098353));
#285132=CARTESIAN_POINT('Ctrl Pts',(-5.12417377439624E-14,70.6812554763908,
10.5687024728991));
#285133=CARTESIAN_POINT('Ctrl Pts',(3.1060637247185,70.8312554763903,9.55948119098353));
#285134=CARTESIAN_POINT('Ctrl Pts',(6.21212744943705,70.9812554763896,8.55025990906793));
#285135=CARTESIAN_POINT('Ctrl Pts',(8.13178040253621,71.131255476389,5.90808429084315));
#285136=CARTESIAN_POINT('Ctrl Pts',(10.0514333556354,71.2812554763884,3.26590867261836));
#285137=CARTESIAN_POINT('Ctrl Pts',(10.0514333556354,71.4312554763879,-1.23094556858219E-15));
#285138=CARTESIAN_POINT('Ctrl Pts',(10.0514333556354,71.5812554763872,-3.26590867261837));
#285139=CARTESIAN_POINT('Ctrl Pts',(8.13178040253621,71.7312554763867,-5.90808429084315));
#285140=CARTESIAN_POINT('Ctrl Pts',(6.21212744943705,71.881255476386,-8.55025990906793));
#285141=CARTESIAN_POINT('Ctrl Pts',(3.1060637247185,72.0312554763855,-9.55948119098353));
#285142=CARTESIAN_POINT('Ctrl Pts',(-5.46941779107087E-14,72.1812554763848,
-10.5687024728991));
#285143=CARTESIAN_POINT('Ctrl Pts',(-3.10606372471861,72.3312554763843,
-9.55948119098353));
#285144=CARTESIAN_POINT('Ctrl Pts',(-6.21212744943716,72.4812554763837,
-8.55025990906793));
#285145=CARTESIAN_POINT('Ctrl Pts',(-8.13178040253632,72.6312554763831,
-5.90808429084315));
#285146=CARTESIAN_POINT('Ctrl Pts',(-10.0514333556355,72.7812554763825,
-3.26590867261836));
#285147=CARTESIAN_POINT('Ctrl Pts',(-10.0514333556355,72.9312554763818,
2.46189113716437E-15));
#285148=CARTESIAN_POINT('Ctrl Pts',(-10.0514333556355,73.0812554763812,
3.26590867261837));
#285149=CARTESIAN_POINT('Ctrl Pts',(-8.13178040253632,73.2312554763807,
5.90808429084315));
#285150=CARTESIAN_POINT('Ctrl Pts',(-6.21212744943715,73.3812554763801,
8.55025990906793));
#285151=CARTESIAN_POINT('Ctrl Pts',(-3.1060637247186,73.5312554763795,9.55948119098353));
#285152=CARTESIAN_POINT('Ctrl Pts',(-5.29694470156243E-14,73.6812554763789,
10.5687024728991));
#285153=CARTESIAN_POINT('Ctrl Pts',(3.1060637247185,73.8312554763782,9.55948119098353));
#285154=CARTESIAN_POINT('Ctrl Pts',(6.21212744943705,73.9812554763777,8.55025990906793));
#285155=CARTESIAN_POINT('Ctrl Pts',(8.13178040253621,74.131255476377,5.90808429084315));
#285156=CARTESIAN_POINT('Ctrl Pts',(10.0514333556354,74.2812554763765,3.26590867261836));
#285157=CARTESIAN_POINT('Ctrl Pts',(10.0514333556354,74.4312554763758,-1.23094556858219E-15));
#285158=CARTESIAN_POINT('Ctrl Pts',(10.0514333556354,74.5812554763752,-3.26590867261837));
#285159=CARTESIAN_POINT('Ctrl Pts',(8.13178040253621,74.7312554763746,-5.90808429084315));
#285160=CARTESIAN_POINT('Ctrl Pts',(6.21212744943704,74.8812554763741,-8.55025990906793));
#285161=CARTESIAN_POINT('Ctrl Pts',(3.10606372471849,75.0312554763734,-9.55948119098353));
#285162=CARTESIAN_POINT('Ctrl Pts',(-5.64218871823705E-14,75.1812554763729,
-10.5687024728991));
#285163=CARTESIAN_POINT('Ctrl Pts',(-3.10606372471861,75.3312554763722,
-9.55948119098353));
#285164=CARTESIAN_POINT('Ctrl Pts',(-6.21212744943716,75.4812554763717,
-8.55025990906793));
#285165=CARTESIAN_POINT('Ctrl Pts',(-8.13178040253632,75.6312554763711,
-5.90808429084315));
#285166=CARTESIAN_POINT('Ctrl Pts',(-10.0514333556355,75.7812554763704,
-3.26590867261836));
#285167=CARTESIAN_POINT('Ctrl Pts',(-10.0514333556355,75.9312554763699,
2.46189113716437E-15));
#285168=CARTESIAN_POINT('Ctrl Pts',(-10.0514333556355,76.0812554763693,
3.26590867261837));
#285169=CARTESIAN_POINT('Ctrl Pts',(-8.13178040253632,76.2312554763686,
5.90808429084315));
#285170=CARTESIAN_POINT('Ctrl Pts',(-6.21212744943715,76.3812554763681,
8.55025990906793));
#285171=CARTESIAN_POINT('Ctrl Pts',(-3.1060637247186,76.5312554763674,9.55948119098353));
#285172=CARTESIAN_POINT('Ctrl Pts',(-5.46971562872861E-14,76.6812554763668,
10.5687024728991));
#285173=CARTESIAN_POINT('Ctrl Pts',(3.1060637247185,76.8312554763662,9.55948119098353));
#285174=CARTESIAN_POINT('Ctrl Pts',(6.21212744943705,76.9812554763656,8.55025990906793));
#285175=CARTESIAN_POINT('Ctrl Pts',(8.13178040253621,77.1312554763651,5.90808429084315));
#285176=CARTESIAN_POINT('Ctrl Pts',(10.0514333556354,77.2812554763644,3.26590867261836));
#285177=CARTESIAN_POINT('Ctrl Pts',(10.0514333556354,77.4312554763638,-1.23094556858219E-15));
#285178=CARTESIAN_POINT('Ctrl Pts',(10.0514333556354,77.5812554763632,-3.26590867261837));
#285179=CARTESIAN_POINT('Ctrl Pts',(8.13178040253621,77.7312554763626,-5.90808429084315));
#285180=CARTESIAN_POINT('Ctrl Pts',(6.21212744943704,77.881255476362,-8.55025990906793));
#285181=CARTESIAN_POINT('Ctrl Pts',(3.10606372471849,78.0312554763615,-9.55948119098353));
#285182=CARTESIAN_POINT('Ctrl Pts',(-5.81495964540324E-14,78.1812554763608,
-10.5687024728991));
#285183=CARTESIAN_POINT('Ctrl Pts',(-3.10606372471861,78.3312554763603,
-9.55948119098353));
#285184=CARTESIAN_POINT('Ctrl Pts',(-6.21212744943716,78.4812554763596,
-8.55025990906793));
#285185=CARTESIAN_POINT('Ctrl Pts',(-8.13178040253632,78.6312554763591,
-5.90808429084315));
#285186=CARTESIAN_POINT('Ctrl Pts',(-10.0514333556355,78.7812554763585,
-3.26590867261836));
#285187=CARTESIAN_POINT('Ctrl Pts',(-10.0514333556355,78.9312554763579,
2.46189113716437E-15));
#285188=CARTESIAN_POINT('Ctrl Pts',(-10.0514333556355,79.0812554763573,
3.26590867261837));
#285189=CARTESIAN_POINT('Ctrl Pts',(-8.13178040253632,79.2312554763567,
5.90808429084315));
#285190=CARTESIAN_POINT('Ctrl Pts',(-6.21212744943716,79.3812554763561,
8.55025990906793));
#285191=CARTESIAN_POINT('Ctrl Pts',(-3.10606372471861,79.5312554763554,
9.55948119098353));
#285192=CARTESIAN_POINT('Ctrl Pts',(-5.6424865558948E-14,79.6812554763548,
10.5687024728991));
#285193=CARTESIAN_POINT('Ctrl Pts',(3.10606372471849,79.8312554763542,9.55948119098353));
#285194=CARTESIAN_POINT('Ctrl Pts',(6.21212744943704,79.9812554763537,8.55025990906793));
#285195=CARTESIAN_POINT('Ctrl Pts',(8.1317804025362,80.131255476353,5.90808429084315));
#285196=CARTESIAN_POINT('Ctrl Pts',(10.0514333556354,80.2812554763524,3.26590867261836));
#285197=CARTESIAN_POINT('Ctrl Pts',(10.0514333556354,80.4312554763519,-1.23094556858219E-15));
#285198=CARTESIAN_POINT('Ctrl Pts',(10.0514333556354,80.5812554763513,-3.26590867261837));
#285199=CARTESIAN_POINT('Ctrl Pts',(8.1317804025362,80.7312554763506,-5.90808429084315));
#285200=CARTESIAN_POINT('Ctrl Pts',(6.21212744943704,80.88125547635,-8.55025990906793));
#285201=CARTESIAN_POINT('Ctrl Pts',(3.10606372471849,81.0312554763494,-9.55948119098353));
#285202=CARTESIAN_POINT('Ctrl Pts',(-5.98773057256942E-14,81.1812554763489,
-10.5687024728991));
#285203=CARTESIAN_POINT('Ctrl Pts',(-3.10606372471861,81.3312554763482,
-9.55948119098353));
#285204=CARTESIAN_POINT('Ctrl Pts',(-6.21212744943716,81.4812554763476,
-8.55025990906793));
#285205=CARTESIAN_POINT('Ctrl Pts',(-8.13178040253633,81.631255476347,-5.90808429084315));
#285206=CARTESIAN_POINT('Ctrl Pts',(-10.0514333556355,81.7812554763464,
-3.26590867261836));
#285207=CARTESIAN_POINT('Ctrl Pts',(-10.0514333556355,81.9312554763458,
2.46189113716437E-15));
#285208=CARTESIAN_POINT('Ctrl Pts',(-10.0514333556355,82.0812554763452,
3.26590867261837));
#285209=CARTESIAN_POINT('Ctrl Pts',(-8.13178040253633,82.2312554763447,
5.90808429084315));
#285210=CARTESIAN_POINT('Ctrl Pts',(-6.21212744943716,82.3812554763441,
8.55025990906793));
#285211=CARTESIAN_POINT('Ctrl Pts',(-3.10606372471861,82.5312554763435,
9.55948119098353));
#285212=CARTESIAN_POINT('Ctrl Pts',(-5.81525748306098E-14,82.6812554763429,
10.5687024728991));
#285213=CARTESIAN_POINT('Ctrl Pts',(3.10606372471849,82.8312554763423,9.55948119098353));
#285214=CARTESIAN_POINT('Ctrl Pts',(6.21212744943704,82.9812554763416,8.55025990906793));
#285215=CARTESIAN_POINT('Ctrl Pts',(8.1317804025362,83.1312554763411,5.90808429084315));
#285216=CARTESIAN_POINT('Ctrl Pts',(10.0514333556354,83.2812554763404,3.26590867261836));
#285217=CARTESIAN_POINT('Ctrl Pts',(10.0514333556354,83.4312554763399,-1.23094556858219E-15));
#285218=CARTESIAN_POINT('Ctrl Pts',(10.0514333556354,83.5812554763393,-3.26590867261837));
#285219=CARTESIAN_POINT('Ctrl Pts',(8.1317804025362,83.7312554763386,-5.90808429084315));
#285220=CARTESIAN_POINT('Ctrl Pts',(6.21212744943704,83.881255476338,-8.55025990906793));
#285221=CARTESIAN_POINT('Ctrl Pts',(3.10606372471849,84.0312554763374,-9.55948119098353));
#285222=CARTESIAN_POINT('Ctrl Pts',(-6.1605014997356E-14,84.1812554763369,
-10.5687024728991));
#285223=CARTESIAN_POINT('Ctrl Pts',(-3.10606372471861,84.3312554763362,
-9.55948119098353));
#285224=CARTESIAN_POINT('Ctrl Pts',(-6.21212744943716,84.4812554763356,
-8.55025990906793));
#285225=CARTESIAN_POINT('Ctrl Pts',(-8.13178040253633,84.631255476335,-5.90808429084315));
#285226=CARTESIAN_POINT('Ctrl Pts',(-10.0514333556355,84.7812554763345,
-3.26590867261836));
#285227=CARTESIAN_POINT('Ctrl Pts',(-10.0514333556355,84.9312554763338,
2.46189113716437E-15));
#285228=CARTESIAN_POINT('Ctrl Pts',(-10.0514333556355,85.0812554763333,
3.26590867261837));
#285229=CARTESIAN_POINT('Ctrl Pts',(-8.13178040253633,85.2312554763326,
5.90808429084315));
#285230=CARTESIAN_POINT('Ctrl Pts',(-6.21212744943716,85.3812554763321,
8.55025990906793));
#285231=CARTESIAN_POINT('Ctrl Pts',(-3.10606372471861,85.5312554763315,
9.55948119098353));
#285232=CARTESIAN_POINT('Ctrl Pts',(-5.98802841022716E-14,85.6812554763308,
10.5687024728991));
#285233=CARTESIAN_POINT('Ctrl Pts',(3.10606372471849,85.8312554763303,9.55948119098353));
#285234=CARTESIAN_POINT('Ctrl Pts',(6.21212744943704,85.9812554763297,8.55025990906793));
#285235=CARTESIAN_POINT('Ctrl Pts',(8.1317804025362,86.131255476329,5.90808429084315));
#285236=CARTESIAN_POINT('Ctrl Pts',(10.0514333556354,86.2812554763284,3.26590867261836));
#285237=CARTESIAN_POINT('Ctrl Pts',(10.0514333556354,86.4312554763278,-1.23094556858219E-15));
#285238=CARTESIAN_POINT('Ctrl Pts',(10.0514333556354,86.5812554763272,-3.26590867261837));
#285239=CARTESIAN_POINT('Ctrl Pts',(8.1317804025362,86.7312554763266,-5.90808429084315));
#285240=CARTESIAN_POINT('Ctrl Pts',(6.21212744943704,86.881255476326,-8.55025990906793));
#285241=CARTESIAN_POINT('Ctrl Pts',(3.10606372471849,87.0312554763254,-9.55948119098353));
#285242=CARTESIAN_POINT('Ctrl Pts',(-6.33327242690179E-14,87.1812554763249,
-10.5687024728991));
#285243=CARTESIAN_POINT('Ctrl Pts',(-3.10606372471861,87.3312554763242,
-9.55948119098353));
#285244=CARTESIAN_POINT('Ctrl Pts',(-6.21212744943717,87.4812554763236,
-8.55025990906793));
#285245=CARTESIAN_POINT('Ctrl Pts',(-8.13178040253633,87.631255476323,-5.90808429084315));
#285246=CARTESIAN_POINT('Ctrl Pts',(-10.0514333556355,87.7812554763225,
-3.26590867261836));
#285247=CARTESIAN_POINT('Ctrl Pts',(-10.0514333556355,87.9312554763218,
2.46189113716437E-15));
#285248=CARTESIAN_POINT('Ctrl Pts',(-10.0514333556355,88.0812554763212,
3.26590867261837));
#285249=CARTESIAN_POINT('Ctrl Pts',(-8.13178040253633,88.2312554763207,
5.90808429084315));
#285250=CARTESIAN_POINT('Ctrl Pts',(-6.21212744943716,88.38125547632,8.55025990906793));
#285251=CARTESIAN_POINT('Ctrl Pts',(-3.10606372471861,88.5312554763195,
9.55948119098353));
#285252=CARTESIAN_POINT('Ctrl Pts',(-6.16079933739335E-14,88.6812554763188,
10.5687024728991));
#285253=CARTESIAN_POINT('Ctrl Pts',(3.10606372471849,88.8312554763183,9.55948119098353));
#285254=CARTESIAN_POINT('Ctrl Pts',(6.21212744943704,88.9812554763177,8.55025990906793));
#285255=CARTESIAN_POINT('Ctrl Pts',(8.1317804025362,89.1312554763171,5.90808429084315));
#285256=CARTESIAN_POINT('Ctrl Pts',(10.0514333556354,89.2812554763164,3.26590867261836));
#285257=CARTESIAN_POINT('Ctrl Pts',(10.0514333556354,89.4312554763158,-1.23094556858219E-15));
#285258=CARTESIAN_POINT('Ctrl Pts',(10.0514333556354,89.5812554763153,-3.26590867261837));
#285259=CARTESIAN_POINT('Ctrl Pts',(8.1317804025362,89.7312554763146,-5.90808429084315));
#285260=CARTESIAN_POINT('Ctrl Pts',(6.21212744943704,89.881255476314,-8.55025990906793));
#285261=CARTESIAN_POINT('Ctrl Pts',(3.10606372471849,90.0312554763134,-9.55948119098353));
#285262=CARTESIAN_POINT('Ctrl Pts',(-6.50604335406797E-14,90.1812554763128,
-10.5687024728991));
#285263=CARTESIAN_POINT('Ctrl Pts',(-3.10606372471862,90.3312554763122,
-9.55948119098353));
#285264=CARTESIAN_POINT('Ctrl Pts',(-6.21212744943717,90.4812554763116,
-8.55025990906793));
#285265=CARTESIAN_POINT('Ctrl Pts',(-8.13178040253633,90.631255476311,-5.90808429084315));
#285266=CARTESIAN_POINT('Ctrl Pts',(-10.0514333556355,90.7812554763104,
-3.26590867261836));
#285267=CARTESIAN_POINT('Ctrl Pts',(-10.0514333556355,90.9312554763098,
2.46189113716437E-15));
#285268=CARTESIAN_POINT('Ctrl Pts',(-10.0514333556355,91.0812554763092,
3.26590867261837));
#285269=CARTESIAN_POINT('Ctrl Pts',(-8.13178040253633,91.2312554763086,
5.90808429084315));
#285270=CARTESIAN_POINT('Ctrl Pts',(-6.21212744943717,91.3812554763081,
8.55025990906793));
#285271=CARTESIAN_POINT('Ctrl Pts',(-3.10606372471861,91.5312554763075,
9.55948119098353));
#285272=CARTESIAN_POINT('Ctrl Pts',(-6.33357026455953E-14,91.6812554763069,
10.5687024728991));
#285273=CARTESIAN_POINT('Ctrl Pts',(3.10606372471849,91.8312554763063,9.55948119098353));
#285274=CARTESIAN_POINT('Ctrl Pts',(6.21212744943704,91.9812554763056,8.55025990906793));
#285275=CARTESIAN_POINT('Ctrl Pts',(8.1317804025362,92.1312554763051,5.90808429084315));
#285276=CARTESIAN_POINT('Ctrl Pts',(10.0514333556354,92.2812554763045,3.26590867261836));
#285277=CARTESIAN_POINT('Ctrl Pts',(10.0514333556354,92.4312554763039,-1.23094556858219E-15));
#285278=CARTESIAN_POINT('Ctrl Pts',(10.0514333556354,92.5812554763033,-3.26590867261837));
#285279=CARTESIAN_POINT('Ctrl Pts',(8.1317804025362,92.7312554763026,-5.90808429084315));
#285280=CARTESIAN_POINT('Ctrl Pts',(6.21212744943704,92.881255476302,-8.55025990906793));
#285281=CARTESIAN_POINT('Ctrl Pts',(3.10606372471848,93.0312554763014,-9.55948119098353));
#285282=CARTESIAN_POINT('Ctrl Pts',(-6.67881428123416E-14,93.1812554763008,
-10.5687024728991));
#285283=CARTESIAN_POINT('Ctrl Pts',(-3.10606372471862,93.3312554763002,
-9.55948119098353));
#285284=CARTESIAN_POINT('Ctrl Pts',(-6.21212744943717,93.4812554762996,
-8.55025990906793));
#285285=CARTESIAN_POINT('Ctrl Pts',(-8.13178040253633,93.631255476299,-5.90808429084315));
#285286=CARTESIAN_POINT('Ctrl Pts',(-10.0514333556355,93.7812554762984,
-3.26590867261836));
#285287=CARTESIAN_POINT('Ctrl Pts',(-10.0514333556355,93.9312554762978,
2.46189113716437E-15));
#285288=CARTESIAN_POINT('Ctrl Pts',(-10.0514333556355,94.0812554762972,
3.26590867261837));
#285289=CARTESIAN_POINT('Ctrl Pts',(-8.13178040253633,94.2312554762967,
5.90808429084315));
#285290=CARTESIAN_POINT('Ctrl Pts',(-6.21212744943717,94.3812554762961,
8.55025990906793));
#285291=CARTESIAN_POINT('Ctrl Pts',(-3.10606372471862,94.5312554762955,
9.55948119098353));
#285292=CARTESIAN_POINT('Ctrl Pts',(-6.50634119172571E-14,94.6812554762948,
10.5687024728991));
#285293=CARTESIAN_POINT('Ctrl Pts',(3.10606372471849,94.8312554762943,9.55948119098353));
#285294=CARTESIAN_POINT('Ctrl Pts',(6.21212744943704,94.9812554762937,8.55025990906793));
#285295=CARTESIAN_POINT('Ctrl Pts',(8.1317804025362,95.1312554762931,5.90808429084315));
#285296=CARTESIAN_POINT('Ctrl Pts',(10.0514333556354,95.2812554762924,3.26590867261836));
#285297=CARTESIAN_POINT('Ctrl Pts',(10.0514333556354,95.4312554762919,-1.23094556858219E-15));
#285298=CARTESIAN_POINT('Ctrl Pts',(10.0514333556354,95.5812554762912,-3.26590867261837));
#285299=CARTESIAN_POINT('Ctrl Pts',(8.1317804025362,95.7312554762906,-5.90808429084315));
#285300=CARTESIAN_POINT('Ctrl Pts',(6.21212744943703,95.88125547629,-8.55025990906793));
#285301=CARTESIAN_POINT('Ctrl Pts',(3.10606372471848,96.0312554762895,-9.55948119098353));
#285302=CARTESIAN_POINT('Ctrl Pts',(-6.85158520840034E-14,96.1812554762889,
-10.5687024728991));
#285303=CARTESIAN_POINT('Ctrl Pts',(-3.10606372471862,96.3312554762882,
-9.55948119098353));
#285304=CARTESIAN_POINT('Ctrl Pts',(-6.21212744943717,96.4812554762876,
-8.55025990906793));
#285305=CARTESIAN_POINT('Ctrl Pts',(-8.13178040253633,96.631255476287,-5.90808429084315));
#285306=CARTESIAN_POINT('Ctrl Pts',(-10.0514333556355,96.7812554762864,
-3.26590867261836));
#285307=CARTESIAN_POINT('Ctrl Pts',(-10.0514333556355,96.9312554762858,
2.46189113716437E-15));
#285308=CARTESIAN_POINT('Ctrl Pts',(-10.0514333556355,97.0812554762852,
3.26590867261837));
#285309=CARTESIAN_POINT('Ctrl Pts',(-8.13178040253633,97.2312554762846,
5.90808429084315));
#285310=CARTESIAN_POINT('Ctrl Pts',(-6.21212744943717,97.3812554762841,
8.55025990906793));
#285311=CARTESIAN_POINT('Ctrl Pts',(-3.10606372471862,97.5312554762834,
9.55948119098353));
#285312=CARTESIAN_POINT('Ctrl Pts',(-6.6791121188919E-14,97.6812554762828,
10.5687024728991));
#285313=CARTESIAN_POINT('Ctrl Pts',(3.10606372471848,97.8312554762823,9.55948119098353));
#285314=CARTESIAN_POINT('Ctrl Pts',(6.21212744943704,97.9812554762817,8.55025990906793));
#285315=CARTESIAN_POINT('Ctrl Pts',(8.13178040253619,98.1312554762811,5.90808429084315));
#285316=CARTESIAN_POINT('Ctrl Pts',(10.0514333556354,98.2812554762804,3.26590867261836));
#285317=CARTESIAN_POINT('Ctrl Pts',(10.0514333556354,98.4312554762799,-1.23094556858219E-15));
#285318=CARTESIAN_POINT('Ctrl Pts',(10.0514333556354,98.5812554762793,-3.26590867261837));
#285319=CARTESIAN_POINT('Ctrl Pts',(8.13178040253619,98.7312554762786,-5.90808429084315));
#285320=CARTESIAN_POINT('Ctrl Pts',(6.21212744943703,98.8812554762781,-8.55025990906793));
#285321=CARTESIAN_POINT('Ctrl Pts',(3.10606372471848,99.0312554762774,-9.55948119098353));
#285322=CARTESIAN_POINT('Ctrl Pts',(-7.02435613556652E-14,99.1812554762769,
-10.5687024728991));
#285323=CARTESIAN_POINT('Ctrl Pts',(-3.10606372471862,99.3312554762762,
-9.55948119098353));
#285324=CARTESIAN_POINT('Ctrl Pts',(-6.21212744943717,99.4812554762756,
-8.55025990906793));
#285325=CARTESIAN_POINT('Ctrl Pts',(-8.13178040253633,99.631255476275,-5.90808429084315));
#285326=CARTESIAN_POINT('Ctrl Pts',(-10.0514333556355,99.7812554762745,
-3.26590867261836));
#285327=CARTESIAN_POINT('Ctrl Pts',(-10.0514333556355,99.9312554762739,
2.46189113716437E-15));
#285328=CARTESIAN_POINT('Ctrl Pts',(-10.0514333556355,100.081255476273,
3.26590867261837));
#285329=CARTESIAN_POINT('Ctrl Pts',(-8.13178040253633,100.231255476273,
5.90808429084315));
#285330=CARTESIAN_POINT('Ctrl Pts',(-6.21212744943717,100.381255476272,
8.55025990906793));
#285331=CARTESIAN_POINT('Ctrl Pts',(-3.10606372471862,100.531255476271,
9.55948119098353));
#285332=CARTESIAN_POINT('Ctrl Pts',(-6.85188304605808E-14,100.681255476271,
10.5687024728991));
#285333=CARTESIAN_POINT('Ctrl Pts',(3.10606372471848,100.83125547627,9.55948119098353));
#285334=CARTESIAN_POINT('Ctrl Pts',(6.21212744943703,100.98125547627,8.55025990906793));
#285335=CARTESIAN_POINT('Ctrl Pts',(8.13178040253619,101.131255476269,5.90808429084315));
#285336=CARTESIAN_POINT('Ctrl Pts',(10.0514333556354,101.281255476268,3.26590867261836));
#285337=CARTESIAN_POINT('Ctrl Pts',(10.0514333556354,101.431255476268,-1.23094556858219E-15));
#285338=CARTESIAN_POINT('Ctrl Pts',(10.0514333556353,101.581255476267,-3.26590867261837));
#285339=CARTESIAN_POINT('Ctrl Pts',(8.13178040253619,101.731255476267,-5.90808429084315));
#285340=CARTESIAN_POINT('Ctrl Pts',(6.21212744943703,101.881255476266,-8.55025990906793));
#285341=CARTESIAN_POINT('Ctrl Pts',(3.10606372471848,102.031255476265,-9.55948119098353));
#285342=CARTESIAN_POINT('Ctrl Pts',(-7.19712706273271E-14,102.181255476265,
-10.5687024728991));
#285343=CARTESIAN_POINT('Ctrl Pts',(-3.10606372471862,102.331255476264,
-9.55948119098353));
#285344=CARTESIAN_POINT('Ctrl Pts',(-6.21212744943717,102.481255476264,
-8.55025990906793));
#285345=CARTESIAN_POINT('Ctrl Pts',(-8.13178040253634,102.631255476263,
-5.90808429084315));
#285346=CARTESIAN_POINT('Ctrl Pts',(-10.0514333556355,102.781255476262,
-3.26590867261836));
#285347=CARTESIAN_POINT('Ctrl Pts',(-10.0514333556355,102.931255476262,
2.46189113716437E-15));
#285348=CARTESIAN_POINT('Ctrl Pts',(-10.0514333556355,103.081255476261,
3.26590867261837));
#285349=CARTESIAN_POINT('Ctrl Pts',(-8.13178040253634,103.231255476261,
5.90808429084315));
#285350=CARTESIAN_POINT('Ctrl Pts',(-6.21212744943717,103.38125547626,8.55025990906793));
#285351=CARTESIAN_POINT('Ctrl Pts',(-3.10606372471862,103.531255476259,
9.55948119098353));
#285352=CARTESIAN_POINT('Ctrl Pts',(-7.02465397322427E-14,103.681255476259,
10.5687024728991));
#285353=CARTESIAN_POINT('Ctrl Pts',(3.10606372471848,103.831255476258,9.55948119098353));
#285354=CARTESIAN_POINT('Ctrl Pts',(6.21212744943703,103.981255476258,8.55025990906793));
#285355=CARTESIAN_POINT('Ctrl Pts',(8.13178040253619,104.131255476257,5.90808429084315));
#285356=CARTESIAN_POINT('Ctrl Pts',(10.0514333556353,104.281255476256,3.26590867261836));
#285357=CARTESIAN_POINT('Ctrl Pts',(10.0514333556354,104.431255476256,-1.23094556858219E-15));
#285358=CARTESIAN_POINT('Ctrl Pts',(10.0514333556353,104.581255476255,-3.26590867261837));
#285359=CARTESIAN_POINT('Ctrl Pts',(8.13178040253619,104.731255476255,-5.90808429084315));
#285360=CARTESIAN_POINT('Ctrl Pts',(6.21212744943703,104.881255476254,-8.55025990906793));
#285361=CARTESIAN_POINT('Ctrl Pts',(3.10606372471848,105.031255476253,-9.55948119098353));
#285362=CARTESIAN_POINT('Ctrl Pts',(-7.36989798989889E-14,105.181255476253,
-10.5687024728991));
#285363=CARTESIAN_POINT('Ctrl Pts',(-3.10606372471862,105.331255476252,
-9.55948119098353));
#285364=CARTESIAN_POINT('Ctrl Pts',(-6.21212744943718,105.481255476252,
-8.55025990906793));
#285365=CARTESIAN_POINT('Ctrl Pts',(-8.13178040253634,105.631255476251,
-5.90808429084315));
#285366=CARTESIAN_POINT('Ctrl Pts',(-10.0514333556355,105.78125547625,-3.26590867261836));
#285367=CARTESIAN_POINT('Ctrl Pts',(-10.0514333556355,105.93125547625,2.46189113716437E-15));
#285368=CARTESIAN_POINT('Ctrl Pts',(-10.0514333556355,106.081255476249,
3.26590867261837));
#285369=CARTESIAN_POINT('Ctrl Pts',(-8.13178040253634,106.231255476249,
5.90808429084315));
#285370=CARTESIAN_POINT('Ctrl Pts',(-6.21212744943717,106.381255476248,
8.55025990906793));
#285371=CARTESIAN_POINT('Ctrl Pts',(-3.10606372471862,106.531255476247,
9.55948119098353));
#285372=CARTESIAN_POINT('Ctrl Pts',(-7.19742490039045E-14,106.681255476247,
10.5687024728991));
#285373=CARTESIAN_POINT('Ctrl Pts',(3.10606372471848,106.831255476246,9.55948119098353));
#285374=CARTESIAN_POINT('Ctrl Pts',(6.21212744943703,106.981255476246,8.55025990906793));
#285375=CARTESIAN_POINT('Ctrl Pts',(8.13178040253619,107.131255476245,5.90808429084315));
#285376=CARTESIAN_POINT('Ctrl Pts',(10.0514333556353,107.281255476244,3.26590867261836));
#285377=CARTESIAN_POINT('Ctrl Pts',(10.0514333556354,107.431255476244,-1.23094556858219E-15));
#285378=CARTESIAN_POINT('Ctrl Pts',(10.0514333556353,107.581255476243,-3.26590867261837));
#285379=CARTESIAN_POINT('Ctrl Pts',(8.13178040253619,107.731255476243,-5.90808429084315));
#285380=CARTESIAN_POINT('Ctrl Pts',(6.21212744943703,107.881255476242,-8.55025990906793));
#285381=CARTESIAN_POINT('Ctrl Pts',(3.10606372471848,108.031255476241,-9.55948119098353));
#285382=CARTESIAN_POINT('Ctrl Pts',(-7.54266891706507E-14,108.181255476241,
-10.5687024728991));
#285383=CARTESIAN_POINT('Ctrl Pts',(-3.10606372471863,108.33125547624,-9.55948119098353));
#285384=CARTESIAN_POINT('Ctrl Pts',(-6.21212744943718,108.48125547624,-8.55025990906793));
#285385=CARTESIAN_POINT('Ctrl Pts',(-8.13178040253634,108.631255476239,
-5.90808429084315));
#285386=CARTESIAN_POINT('Ctrl Pts',(-10.0514333556355,108.781255476238,
-3.26590867261836));
#285387=CARTESIAN_POINT('Ctrl Pts',(-10.0514333556355,108.931255476238,
2.46189113716437E-15));
#285388=CARTESIAN_POINT('Ctrl Pts',(-10.0514333556355,109.081255476237,
3.26590867261837));
#285389=CARTESIAN_POINT('Ctrl Pts',(-8.13178040253634,109.231255476237,
5.90808429084315));
#285390=CARTESIAN_POINT('Ctrl Pts',(-6.21212744943718,109.381255476236,
8.55025990906793));
#285391=CARTESIAN_POINT('Ctrl Pts',(-3.10606372471862,109.531255476235,
9.55948119098353));
#285392=CARTESIAN_POINT('Ctrl Pts',(-7.37019582755663E-14,109.681255476235,
10.5687024728991));
#285393=CARTESIAN_POINT('Ctrl Pts',(3.10606372471848,109.831255476234,9.55948119098353));
#285394=CARTESIAN_POINT('Ctrl Pts',(6.21212744943703,109.981255476234,8.55025990906793));
#285395=CARTESIAN_POINT('Ctrl Pts',(8.13178040253619,110.131255476233,5.90808429084315));
#285396=CARTESIAN_POINT('Ctrl Pts',(10.0514333556353,110.281255476232,3.26590867261836));
#285397=CARTESIAN_POINT('Ctrl Pts',(10.0514333556353,110.431255476232,-1.23094556858219E-15));
#285398=CARTESIAN_POINT('Ctrl Pts',(10.0514333556353,110.581255476231,-3.26590867261837));
#285399=CARTESIAN_POINT('Ctrl Pts',(8.13178040253619,110.731255476231,-5.90808429084315));
#285400=CARTESIAN_POINT('Ctrl Pts',(6.21212744943703,110.88125547623,-8.55025990906793));
#285401=CARTESIAN_POINT('Ctrl Pts',(3.10606372471847,111.031255476229,-9.55948119098353));
#285402=CARTESIAN_POINT('Ctrl Pts',(-7.71543984423126E-14,111.181255476229,
-10.5687024728991));
#285403=CARTESIAN_POINT('Ctrl Pts',(-3.10606372471863,111.331255476228,
-9.55948119098353));
#285404=CARTESIAN_POINT('Ctrl Pts',(-6.21212744943718,111.481255476228,
-8.55025990906793));
#285405=CARTESIAN_POINT('Ctrl Pts',(-8.13178040253634,111.631255476227,
-5.90808429084315));
#285406=CARTESIAN_POINT('Ctrl Pts',(-10.0514333556355,111.781255476226,
-3.26590867261836));
#285407=CARTESIAN_POINT('Ctrl Pts',(-10.0514333556355,111.931255476226,
2.46189113716437E-15));
#285408=CARTESIAN_POINT('Ctrl Pts',(-10.0514333556355,112.081255476225,
3.26590867261837));
#285409=CARTESIAN_POINT('Ctrl Pts',(-8.13178040253634,112.231255476225,
5.90808429084315));
#285410=CARTESIAN_POINT('Ctrl Pts',(-6.21212744943718,112.381255476224,
8.55025990906793));
#285411=CARTESIAN_POINT('Ctrl Pts',(-3.10606372471863,112.531255476223,
9.55948119098353));
#285412=CARTESIAN_POINT('Ctrl Pts',(-7.54296675472282E-14,112.681255476223,
10.5687024728991));
#285413=CARTESIAN_POINT('Ctrl Pts',(3.10606372471847,112.831255476222,9.55948119098353));
#285414=CARTESIAN_POINT('Ctrl Pts',(6.21212744943703,112.981255476222,8.55025990906793));
#285415=CARTESIAN_POINT('Ctrl Pts',(8.13178040253618,113.131255476221,5.90808429084315));
#285416=CARTESIAN_POINT('Ctrl Pts',(10.0514333556353,113.28125547622,3.26590867261836));
#285417=CARTESIAN_POINT('Ctrl Pts',(10.0514333556353,113.43125547622,-1.23094556858219E-15));
#285418=CARTESIAN_POINT('Ctrl Pts',(10.0514333556353,113.581255476219,-3.26590867261837));
#285419=CARTESIAN_POINT('Ctrl Pts',(8.13178040253618,113.731255476219,-5.90808429084315));
#285420=CARTESIAN_POINT('Ctrl Pts',(6.21212744943702,113.881255476218,-8.55025990906793));
#285421=CARTESIAN_POINT('Ctrl Pts',(3.10606372471847,114.031255476217,-9.55948119098353));
#285422=CARTESIAN_POINT('Ctrl Pts',(-7.88821077139744E-14,114.181255476217,
-10.5687024728991));
#285423=CARTESIAN_POINT('Ctrl Pts',(-3.10606372471863,114.331255476216,
-9.55948119098353));
#285424=CARTESIAN_POINT('Ctrl Pts',(-6.21212744943718,114.481255476216,
-8.55025990906793));
#285425=CARTESIAN_POINT('Ctrl Pts',(-8.13178040253634,114.631255476215,
-5.90808429084315));
#285426=CARTESIAN_POINT('Ctrl Pts',(-10.0514333556355,114.781255476214,
-3.26590867261836));
#285427=CARTESIAN_POINT('Ctrl Pts',(-10.0514333556355,114.931255476214,
2.46189113716437E-15));
#285428=CARTESIAN_POINT('Ctrl Pts',(-10.0514333556355,115.081255476213,
3.26590867261837));
#285429=CARTESIAN_POINT('Ctrl Pts',(-8.13178040253634,115.231255476213,
5.90808429084315));
#285430=CARTESIAN_POINT('Ctrl Pts',(-6.21212744943718,115.381255476212,
8.55025990906793));
#285431=CARTESIAN_POINT('Ctrl Pts',(-3.10606372471863,115.531255476211,
9.55948119098353));
#285432=CARTESIAN_POINT('Ctrl Pts',(-7.715737681889E-14,115.681255476211,
10.5687024728991));
#285433=CARTESIAN_POINT('Ctrl Pts',(3.10606372471847,115.83125547621,9.55948119098353));
#285434=CARTESIAN_POINT('Ctrl Pts',(6.21212744943703,115.98125547621,8.55025990906793));
#285435=CARTESIAN_POINT('Ctrl Pts',(8.13178040253618,116.131255476209,5.90808429084315));
#285436=CARTESIAN_POINT('Ctrl Pts',(10.0514333556353,116.281255476208,3.26590867261836));
#285437=CARTESIAN_POINT('Ctrl Pts',(10.0514333556353,116.431255476208,-1.23094556858219E-15));
#285438=CARTESIAN_POINT('Ctrl Pts',(10.0514333556353,116.581255476207,-3.26590867261837));
#285439=CARTESIAN_POINT('Ctrl Pts',(8.13178040253618,116.731255476207,-5.90808429084315));
#285440=CARTESIAN_POINT('Ctrl Pts',(6.21212744943702,116.881255476206,-8.55025990906793));
#285441=CARTESIAN_POINT('Ctrl Pts',(3.10606372471847,117.031255476205,-9.55948119098353));
#285442=CARTESIAN_POINT('Ctrl Pts',(-8.06098169856363E-14,117.181255476205,
-10.5687024728991));
#285443=CARTESIAN_POINT('Ctrl Pts',(-3.10606372471863,117.331255476204,
-9.55948119098353));
#285444=CARTESIAN_POINT('Ctrl Pts',(-6.21212744943718,117.481255476204,
-8.55025990906793));
#285445=CARTESIAN_POINT('Ctrl Pts',(-8.13178040253634,117.631255476203,
-5.90808429084315));
#285446=CARTESIAN_POINT('Ctrl Pts',(-10.0514333556355,117.781255476202,
-3.26590867261836));
#285447=CARTESIAN_POINT('Ctrl Pts',(-10.0514333556355,117.931255476202,
2.46189113716437E-15));
#285448=CARTESIAN_POINT('Ctrl Pts',(-10.0514333556355,118.081255476201,
3.26590867261837));
#285449=CARTESIAN_POINT('Ctrl Pts',(-8.13178040253634,118.231255476201,
5.90808429084315));
#285450=CARTESIAN_POINT('Ctrl Pts',(-6.21212744943718,118.3812554762,8.55025990906793));
#285451=CARTESIAN_POINT('Ctrl Pts',(-3.10606372471863,118.531255476199,
9.55948119098353));
#285452=CARTESIAN_POINT('Ctrl Pts',(-7.88850860905518E-14,118.681255476199,
10.5687024728991));
#285453=CARTESIAN_POINT('Ctrl Pts',(3.10606372471847,118.831255476198,9.55948119098353));
#285454=CARTESIAN_POINT('Ctrl Pts',(6.21212744943702,118.981255476198,8.55025990906793));
#285455=CARTESIAN_POINT('Ctrl Pts',(8.13178040253618,119.131255476197,5.90808429084315));
#285456=CARTESIAN_POINT('Ctrl Pts',(10.0514333556353,119.281255476196,3.26590867261836));
#285457=CARTESIAN_POINT('Ctrl Pts',(10.0514333556353,119.431255476196,-1.23094556858219E-15));
#285458=CARTESIAN_POINT('Ctrl Pts',(10.0514333556353,119.581255476195,-3.26590867261837));
#285459=CARTESIAN_POINT('Ctrl Pts',(8.13178040253618,119.731255476195,-5.90808429084315));
#285460=CARTESIAN_POINT('Ctrl Pts',(6.21212744943702,119.881255476194,-8.55025990906793));
#285461=CARTESIAN_POINT('Ctrl Pts',(3.10606372471847,120.031255476193,-9.55948119098353));
#285462=CARTESIAN_POINT('Ctrl Pts',(-8.23375262572981E-14,120.181255476193,
-10.5687024728991));
#285463=CARTESIAN_POINT('Ctrl Pts',(-3.10606372471863,120.331255476192,
-9.55948119098353));
#285464=CARTESIAN_POINT('Ctrl Pts',(-6.21212744943718,120.481255476192,
-8.55025990906793));
#285465=CARTESIAN_POINT('Ctrl Pts',(-8.13178040253635,120.631255476191,
-5.90808429084315));
#285466=CARTESIAN_POINT('Ctrl Pts',(-10.0514333556355,120.78125547619,-3.26590867261836));
#285467=CARTESIAN_POINT('Ctrl Pts',(-10.0514333556355,120.93125547619,2.46189113716437E-15));
#285468=CARTESIAN_POINT('Ctrl Pts',(-10.0514333556355,121.081255476189,
3.26590867261837));
#285469=CARTESIAN_POINT('Ctrl Pts',(-8.13178040253635,121.231255476189,
5.90808429084315));
#285470=CARTESIAN_POINT('Ctrl Pts',(-6.21212744943718,121.381255476188,
8.55025990906793));
#285471=CARTESIAN_POINT('Ctrl Pts',(-3.10606372471863,121.531255476187,
9.55948119098353));
#285472=CARTESIAN_POINT('Ctrl Pts',(-8.06127953622137E-14,121.681255476187,
10.5687024728991));
#285473=CARTESIAN_POINT('Ctrl Pts',(3.10606372471847,121.831255476186,9.55948119098353));
#285474=CARTESIAN_POINT('Ctrl Pts',(6.21212744943702,121.981255476186,8.55025990906793));
#285475=CARTESIAN_POINT('Ctrl Pts',(8.13178040253618,122.131255476185,5.90808429084315));
#285476=CARTESIAN_POINT('Ctrl Pts',(10.0514333556353,122.281255476184,3.26590867261836));
#285477=CARTESIAN_POINT('Ctrl Pts',(10.0514333556353,122.431255476184,-1.23094556858219E-15));
#285478=CARTESIAN_POINT('Ctrl Pts',(10.0514333556353,122.581255476183,-3.26590867261837));
#285479=CARTESIAN_POINT('Ctrl Pts',(8.13178040253618,122.731255476183,-5.90808429084315));
#285480=CARTESIAN_POINT('Ctrl Pts',(6.21212744943702,122.881255476182,-8.55025990906793));
#285481=CARTESIAN_POINT('Ctrl Pts',(3.10606372471847,123.031255476181,-9.55948119098353));
#285482=CARTESIAN_POINT('Ctrl Pts',(-8.40652355289599E-14,123.181255476181,
-10.5687024728991));
#285483=CARTESIAN_POINT('Ctrl Pts',(-3.10606372471864,123.33125547618,-9.55948119098353));
#285484=CARTESIAN_POINT('Ctrl Pts',(-6.21212744943718,123.48125547618,-8.55025990906793));
#285485=CARTESIAN_POINT('Ctrl Pts',(-8.13178040253635,123.631255476179,
-5.90808429084315));
#285486=CARTESIAN_POINT('Ctrl Pts',(-10.0514333556355,123.781255476178,
-3.26590867261836));
#285487=CARTESIAN_POINT('Ctrl Pts',(-10.0514333556355,123.931255476178,
2.46189113716437E-15));
#285488=CARTESIAN_POINT('Ctrl Pts',(-10.0514333556355,124.081255476177,
3.26590867261837));
#285489=CARTESIAN_POINT('Ctrl Pts',(-8.13178040253635,124.231255476177,
5.90808429084315));
#285490=CARTESIAN_POINT('Ctrl Pts',(-6.21212744943718,124.381255476176,
8.55025990906793));
#285491=CARTESIAN_POINT('Ctrl Pts',(-3.10606372471863,124.531255476175,
9.55948119098353));
#285492=CARTESIAN_POINT('Ctrl Pts',(-8.23405046338756E-14,124.681255476175,
10.5687024728991));
#285493=CARTESIAN_POINT('Ctrl Pts',(3.10606372471847,124.831255476174,9.55948119098353));
#285494=CARTESIAN_POINT('Ctrl Pts',(6.21212744943702,124.981255476174,8.55025990906793));
#285495=CARTESIAN_POINT('Ctrl Pts',(8.13178040253618,125.131255476173,5.90808429084315));
#285496=CARTESIAN_POINT('Ctrl Pts',(10.0514333556353,125.281255476172,3.26590867261836));
#285497=CARTESIAN_POINT('Ctrl Pts',(10.0514333556353,125.431255476172,-1.23094556858219E-15));
#285498=CARTESIAN_POINT('Ctrl Pts',(10.0514333556353,125.581255476171,-3.26590867261837));
#285499=CARTESIAN_POINT('Ctrl Pts',(8.13178040253618,125.731255476171,-5.90808429084315));
#285500=CARTESIAN_POINT('Ctrl Pts',(6.21212744943702,125.88125547617,-8.55025990906793));
#285501=CARTESIAN_POINT('Ctrl Pts',(3.10606372471847,126.031255476169,-9.55948119098353));
#285502=CARTESIAN_POINT('Ctrl Pts',(-8.57929448006218E-14,126.181255476169,
-10.5687024728991));
#285503=CARTESIAN_POINT('Ctrl Pts',(-3.10606372471864,126.331255476168,
-9.55948119098353));
#285504=CARTESIAN_POINT('Ctrl Pts',(-6.21212744943719,126.481255476168,
-8.55025990906793));
#285505=CARTESIAN_POINT('Ctrl Pts',(-8.13178040253635,126.631255476167,
-5.90808429084315));
#285506=CARTESIAN_POINT('Ctrl Pts',(-10.0514333556355,126.781255476166,
-3.26590867261836));
#285507=CARTESIAN_POINT('Ctrl Pts',(-10.0514333556355,126.931255476166,
2.46189113716437E-15));
#285508=CARTESIAN_POINT('Ctrl Pts',(-10.0514333556355,127.081255476165,
3.26590867261837));
#285509=CARTESIAN_POINT('Ctrl Pts',(-8.13178040253635,127.231255476165,
5.90808429084315));
#285510=CARTESIAN_POINT('Ctrl Pts',(-6.21212744943718,127.381255476164,
8.55025990906793));
#285511=CARTESIAN_POINT('Ctrl Pts',(-3.10606372471863,127.531255476163,
9.55948119098353));
#285512=CARTESIAN_POINT('Ctrl Pts',(-8.40682139055374E-14,127.681255476163,
10.5687024728991));
#285513=CARTESIAN_POINT('Ctrl Pts',(3.10606372471847,127.831255476162,9.55948119098353));
#285514=CARTESIAN_POINT('Ctrl Pts',(6.21212744943702,127.981255476162,8.55025990906793));
#285515=CARTESIAN_POINT('Ctrl Pts',(8.13178040253618,128.131255476161,5.90808429084315));
#285516=CARTESIAN_POINT('Ctrl Pts',(10.0514333556353,128.28125547616,3.26590867261836));
#285517=CARTESIAN_POINT('Ctrl Pts',(10.0514333556353,128.43125547616,-1.23094556858219E-15));
#285518=CARTESIAN_POINT('Ctrl Pts',(10.0514333556353,128.581255476159,-3.26590867261837));
#285519=CARTESIAN_POINT('Ctrl Pts',(8.13178040253618,128.731255476159,-5.90808429084315));
#285520=CARTESIAN_POINT('Ctrl Pts',(6.21212744943701,128.881255476158,-8.55025990906793));
#285521=CARTESIAN_POINT('Ctrl Pts',(3.10606372471846,129.031255476157,-9.55948119098353));
#285522=CARTESIAN_POINT('Ctrl Pts',(-8.75206540722836E-14,129.181255476157,
-10.5687024728991));
#285523=CARTESIAN_POINT('Ctrl Pts',(-3.10606372471864,129.331255476156,
-9.55948119098353));
#285524=CARTESIAN_POINT('Ctrl Pts',(-6.21212744943719,129.481255476156,
-8.55025990906793));
#285525=CARTESIAN_POINT('Ctrl Pts',(-8.13178040253635,129.631255476155,
-5.90808429084315));
#285526=CARTESIAN_POINT('Ctrl Pts',(-10.0514333556355,129.781255476154,
-3.26590867261836));
#285527=CARTESIAN_POINT('Ctrl Pts',(-10.0514333556355,129.931255476154,
2.46189113716437E-15));
#285528=CARTESIAN_POINT('Ctrl Pts',(-10.0514333556355,130.081255476153,
3.26590867261837));
#285529=CARTESIAN_POINT('Ctrl Pts',(-8.13178040253635,130.231255476153,
5.90808429084315));
#285530=CARTESIAN_POINT('Ctrl Pts',(-6.21212744943719,130.381255476152,
8.55025990906793));
#285531=CARTESIAN_POINT('Ctrl Pts',(-3.10606372471864,130.531255476151,
9.55948119098353));
#285532=CARTESIAN_POINT('Ctrl Pts',(-8.57959231771992E-14,130.681255476151,
10.5687024728991));
#285533=CARTESIAN_POINT('Ctrl Pts',(3.10606372471846,130.83125547615,9.55948119098353));
#285534=CARTESIAN_POINT('Ctrl Pts',(6.21212744943702,130.98125547615,8.55025990906793));
#285535=CARTESIAN_POINT('Ctrl Pts',(8.13178040253618,131.131255476149,5.90808429084315));
#285536=CARTESIAN_POINT('Ctrl Pts',(10.0514333556353,131.281255476148,3.26590867261836));
#285537=CARTESIAN_POINT('Ctrl Pts',(10.0514333556353,131.431255476148,-1.23094556858219E-15));
#285538=CARTESIAN_POINT('Ctrl Pts',(10.0514333556353,131.581255476147,-3.26590867261837));
#285539=CARTESIAN_POINT('Ctrl Pts',(8.13178040253618,131.731255476147,-5.90808429084315));
#285540=CARTESIAN_POINT('Ctrl Pts',(6.21212744943701,131.881255476146,-8.55025990906793));
#285541=CARTESIAN_POINT('Ctrl Pts',(3.10606372471846,132.031255476145,-9.55948119098353));
#285542=CARTESIAN_POINT('Ctrl Pts',(-8.92483633439455E-14,132.181255476145,
-10.5687024728991));
#285543=CARTESIAN_POINT('Ctrl Pts',(-3.10606372471864,132.331255476144,
-9.55948119098353));
#285544=CARTESIAN_POINT('Ctrl Pts',(-6.21212744943719,132.481255476144,
-8.55025990906793));
#285545=CARTESIAN_POINT('Ctrl Pts',(-8.13178040253635,132.631255476143,
-5.90808429084315));
#285546=CARTESIAN_POINT('Ctrl Pts',(-10.0514333556355,132.781255476142,
-3.26590867261836));
#285547=CARTESIAN_POINT('Ctrl Pts',(-10.0514333556355,132.931255476142,
2.46189113716437E-15));
#285548=CARTESIAN_POINT('Ctrl Pts',(-10.0514333556355,133.081255476141,
3.26590867261837));
#285549=CARTESIAN_POINT('Ctrl Pts',(-8.13178040253635,133.231255476141,
5.90808429084315));
#285550=CARTESIAN_POINT('Ctrl Pts',(-6.21212744943719,133.38125547614,8.55025990906793));
#285551=CARTESIAN_POINT('Ctrl Pts',(-3.10606372471864,133.531255476139,
9.55948119098353));
#285552=CARTESIAN_POINT('Ctrl Pts',(-8.7523632448861E-14,133.681255476139,
10.5687024728991));
#285553=CARTESIAN_POINT('Ctrl Pts',(3.10606372471846,133.831255476138,9.55948119098353));
#285554=CARTESIAN_POINT('Ctrl Pts',(6.21212744943701,133.981255476138,8.55025990906793));
#285555=CARTESIAN_POINT('Ctrl Pts',(8.13178040253617,134.131255476137,5.90808429084315));
#285556=CARTESIAN_POINT('Ctrl Pts',(10.0514333556353,134.281255476136,3.26590867261836));
#285557=CARTESIAN_POINT('Ctrl Pts',(10.0514333556353,134.431255476136,-1.23094556858219E-15));
#285558=CARTESIAN_POINT('Ctrl Pts',(10.0514333556353,134.581255476135,-3.26590867261837));
#285559=CARTESIAN_POINT('Ctrl Pts',(8.13178040253617,134.731255476135,-5.90808429084315));
#285560=CARTESIAN_POINT('Ctrl Pts',(6.21212744943701,134.881255476134,-8.55025990906793));
#285561=CARTESIAN_POINT('Ctrl Pts',(3.10606372471846,135.031255476133,-9.55948119098353));
#285562=CARTESIAN_POINT('Ctrl Pts',(-9.09760726156073E-14,135.181255476133,
-10.5687024728991));
#285563=CARTESIAN_POINT('Ctrl Pts',(-3.10606372471864,135.331255476132,
-9.55948119098353));
#285564=CARTESIAN_POINT('Ctrl Pts',(-6.21212744943719,135.481255476132,
-8.55025990906793));
#285565=CARTESIAN_POINT('Ctrl Pts',(-8.13178040253636,135.631255476131,
-5.90808429084315));
#285566=CARTESIAN_POINT('Ctrl Pts',(-10.0514333556355,135.78125547613,-3.26590867261836));
#285567=CARTESIAN_POINT('Ctrl Pts',(-10.0514333556355,135.93125547613,2.46189113716437E-15));
#285568=CARTESIAN_POINT('Ctrl Pts',(-10.0514333556355,136.081255476129,
3.26590867261837));
#285569=CARTESIAN_POINT('Ctrl Pts',(-8.13178040253636,136.231255476129,
5.90808429084315));
#285570=CARTESIAN_POINT('Ctrl Pts',(-6.21212744943719,136.381255476128,
8.55025990906793));
#285571=CARTESIAN_POINT('Ctrl Pts',(-3.10606372471864,136.531255476127,
9.55948119098353));
#285572=CARTESIAN_POINT('Ctrl Pts',(-8.92513417205229E-14,136.681255476127,
10.5687024728991));
#285573=CARTESIAN_POINT('Ctrl Pts',(3.10606372471846,136.831255476126,9.55948119098353));
#285574=CARTESIAN_POINT('Ctrl Pts',(6.21212744943701,136.981255476126,8.55025990906793));
#285575=CARTESIAN_POINT('Ctrl Pts',(8.13178040253617,137.131255476125,5.90808429084315));
#285576=CARTESIAN_POINT('Ctrl Pts',(10.0514333556353,137.281255476124,3.26590867261836));
#285577=CARTESIAN_POINT('Ctrl Pts',(10.0514333556353,137.431255476124,-1.23094556858219E-15));
#285578=CARTESIAN_POINT('Ctrl Pts',(10.0514333556353,137.581255476123,-3.26590867261837));
#285579=CARTESIAN_POINT('Ctrl Pts',(8.13178040253617,137.731255476123,-5.90808429084315));
#285580=CARTESIAN_POINT('Ctrl Pts',(6.21212744943701,137.881255476122,-8.55025990906793));
#285581=CARTESIAN_POINT('Ctrl Pts',(3.10606372471846,138.031255476121,-9.55948119098353));
#285582=CARTESIAN_POINT('Ctrl Pts',(-9.27037818872691E-14,138.181255476121,
-10.5687024728991));
#285583=CARTESIAN_POINT('Ctrl Pts',(-3.10606372471864,138.33125547612,-9.55948119098353));
#285584=CARTESIAN_POINT('Ctrl Pts',(-6.21212744943719,138.48125547612,-8.55025990906793));
#285585=CARTESIAN_POINT('Ctrl Pts',(-8.13178040253636,138.631255476119,
-5.90808429084315));
#285586=CARTESIAN_POINT('Ctrl Pts',(-10.0514333556355,138.781255476118,
-3.26590867261836));
#285587=CARTESIAN_POINT('Ctrl Pts',(-10.0514333556355,138.931255476118,
2.46189113716437E-15));
#285588=CARTESIAN_POINT('Ctrl Pts',(-10.0514333556355,139.081255476117,
3.26590867261837));
#285589=CARTESIAN_POINT('Ctrl Pts',(-8.13178040253636,139.231255476117,
5.90808429084315));
#285590=CARTESIAN_POINT('Ctrl Pts',(-6.21212744943719,139.381255476116,
8.55025990906793));
#285591=CARTESIAN_POINT('Ctrl Pts',(-3.10606372471864,139.531255476115,
9.55948119098353));
#285592=CARTESIAN_POINT('Ctrl Pts',(-9.09790509921847E-14,139.681255476115,
10.5687024728991));
#285593=CARTESIAN_POINT('Ctrl Pts',(3.10606372471846,139.831255476114,9.55948119098353));
#285594=CARTESIAN_POINT('Ctrl Pts',(6.21212744943701,139.981255476114,8.55025990906793));
#285595=CARTESIAN_POINT('Ctrl Pts',(8.13178040253617,140.131255476113,5.90808429084315));
#285596=CARTESIAN_POINT('Ctrl Pts',(10.0514333556353,140.281255476112,3.26590867261836));
#285597=CARTESIAN_POINT('Ctrl Pts',(10.0514333556353,140.431255476112,-1.23094556858219E-15));
#285598=CARTESIAN_POINT('Ctrl Pts',(10.0514333556353,140.581255476111,-3.26590867261837));
#285599=CARTESIAN_POINT('Ctrl Pts',(8.13178040253617,140.731255476111,-5.90808429084315));
#285600=CARTESIAN_POINT('Ctrl Pts',(6.21212744943701,140.88125547611,-8.55025990906793));
#285601=CARTESIAN_POINT('Ctrl Pts',(3.10606372471846,141.031255476109,-9.55948119098353));
#285602=CARTESIAN_POINT('Ctrl Pts',(-9.4431491158931E-14,141.181255476109,
-10.5687024728991));
#285603=CARTESIAN_POINT('Ctrl Pts',(-3.10606372471864,141.331255476108,
-9.55948119098353));
#285604=CARTESIAN_POINT('Ctrl Pts',(-6.2121274494372,141.481255476108,-8.55025990906793));
#285605=CARTESIAN_POINT('Ctrl Pts',(-8.13178040253636,141.631255476107,
-5.90808429084315));
#285606=CARTESIAN_POINT('Ctrl Pts',(-10.0514333556355,141.781255476106,
-3.26590867261836));
#285607=CARTESIAN_POINT('Ctrl Pts',(-10.0514333556355,141.931255476106,
2.46189113716437E-15));
#285608=CARTESIAN_POINT('Ctrl Pts',(-10.0514333556355,142.081255476105,
3.26590867261837));
#285609=CARTESIAN_POINT('Ctrl Pts',(-8.13178040253636,142.231255476105,
5.90808429084315));
#285610=CARTESIAN_POINT('Ctrl Pts',(-6.21212744943719,142.381255476104,
8.55025990906793));
#285611=CARTESIAN_POINT('Ctrl Pts',(-3.10606372471864,142.531255476103,
9.55948119098353));
#285612=CARTESIAN_POINT('Ctrl Pts',(-9.27067602638466E-14,142.681255476103,
10.5687024728991));
#285613=CARTESIAN_POINT('Ctrl Pts',(3.10606372471846,142.831255476102,9.55948119098353));
#285614=CARTESIAN_POINT('Ctrl Pts',(6.21212744943701,142.981255476102,8.55025990906793));
#285615=CARTESIAN_POINT('Ctrl Pts',(8.13178040253617,143.131255476101,5.90808429084315));
#285616=CARTESIAN_POINT('Ctrl Pts',(10.0514333556353,143.2812554761,3.26590867261836));
#285617=CARTESIAN_POINT('Ctrl Pts',(10.0514333556353,143.4312554761,-1.23094556858219E-15));
#285618=CARTESIAN_POINT('Ctrl Pts',(10.0514333556353,143.581255476099,-3.26590867261837));
#285619=CARTESIAN_POINT('Ctrl Pts',(8.13178040253617,143.731255476099,-5.90808429084315));
#285620=CARTESIAN_POINT('Ctrl Pts',(6.21212744943701,143.881255476098,-8.55025990906793));
#285621=CARTESIAN_POINT('Ctrl Pts',(3.10606372471845,144.031255476097,-9.55948119098353));
#285622=CARTESIAN_POINT('Ctrl Pts',(-9.61592004305929E-14,144.181255476097,
-10.5687024728991));
#285623=CARTESIAN_POINT('Ctrl Pts',(-3.10606372471865,144.331255476096,
-9.55948119098353));
#285624=CARTESIAN_POINT('Ctrl Pts',(-6.2121274494372,144.481255476096,-8.55025990906793));
#285625=CARTESIAN_POINT('Ctrl Pts',(-8.13178040253636,144.631255476095,
-5.90808429084315));
#285626=CARTESIAN_POINT('Ctrl Pts',(-10.0514333556355,144.781255476094,
-3.26590867261836));
#285627=CARTESIAN_POINT('Ctrl Pts',(-10.0514333556355,144.931255476094,
2.46189113716437E-15));
#285628=CARTESIAN_POINT('Ctrl Pts',(-10.0514333556355,145.081255476093,
3.26590867261837));
#285629=CARTESIAN_POINT('Ctrl Pts',(-8.13178040253636,145.231255476093,
5.90808429084315));
#285630=CARTESIAN_POINT('Ctrl Pts',(-6.2121274494372,145.381255476092,8.55025990906793));
#285631=CARTESIAN_POINT('Ctrl Pts',(-3.10606372471864,145.531255476091,
9.55948119098353));
#285632=CARTESIAN_POINT('Ctrl Pts',(-9.44344695355084E-14,145.681255476091,
10.5687024728991));
#285633=CARTESIAN_POINT('Ctrl Pts',(3.10606372471846,145.83125547609,9.55948119098353));
#285634=CARTESIAN_POINT('Ctrl Pts',(6.21212744943701,145.98125547609,8.55025990906793));
#285635=CARTESIAN_POINT('Ctrl Pts',(8.13178040253617,146.131255476089,5.90808429084315));
#285636=CARTESIAN_POINT('Ctrl Pts',(10.0514333556353,146.281255476088,3.26590867261836));
#285637=CARTESIAN_POINT('Ctrl Pts',(10.0514333556353,146.431255476088,-1.23094556858219E-15));
#285638=CARTESIAN_POINT('Ctrl Pts',(10.0514333556353,146.581255476087,-3.26590867261837));
#285639=CARTESIAN_POINT('Ctrl Pts',(8.13178040253617,146.731255476087,-5.90808429084315));
#285640=CARTESIAN_POINT('Ctrl Pts',(6.212127449437,146.881255476086,-8.55025990906793));
#285641=CARTESIAN_POINT('Ctrl Pts',(3.10606372471845,147.031255476085,-9.55948119098353));
#285642=CARTESIAN_POINT('Ctrl Pts',(-9.78869097022547E-14,147.181255476085,
-10.5687024728991));
#285643=CARTESIAN_POINT('Ctrl Pts',(-3.10606372471865,147.331255476084,
-9.55948119098353));
#285644=CARTESIAN_POINT('Ctrl Pts',(-6.2121274494372,147.481255476084,-8.55025990906793));
#285645=CARTESIAN_POINT('Ctrl Pts',(-8.13178040253636,147.631255476083,
-5.90808429084315));
#285646=CARTESIAN_POINT('Ctrl Pts',(-10.0514333556355,147.781255476082,
-3.26590867261836));
#285647=CARTESIAN_POINT('Ctrl Pts',(-10.0514333556355,147.931255476082,
2.46189113716437E-15));
#285648=CARTESIAN_POINT('Ctrl Pts',(-10.0514333556355,148.081255476081,
3.26590867261837));
#285649=CARTESIAN_POINT('Ctrl Pts',(-8.13178040253636,148.231255476081,
5.90808429084315));
#285650=CARTESIAN_POINT('Ctrl Pts',(-6.2121274494372,148.38125547608,8.55025990906793));
#285651=CARTESIAN_POINT('Ctrl Pts',(-3.10606372471865,148.531255476079,
9.55948119098353));
#285652=CARTESIAN_POINT('Ctrl Pts',(-9.61621788071703E-14,148.681255476079,
10.5687024728991));
#285653=CARTESIAN_POINT('Ctrl Pts',(3.10606372471845,148.831255476078,9.55948119098353));
#285654=CARTESIAN_POINT('Ctrl Pts',(6.21212744943701,148.981255476078,8.55025990906793));
#285655=CARTESIAN_POINT('Ctrl Pts',(8.13178040253617,149.131255476077,5.90808429084315));
#285656=CARTESIAN_POINT('Ctrl Pts',(10.0514333556353,149.281255476076,3.26590867261836));
#285657=CARTESIAN_POINT('Ctrl Pts',(10.0514333556353,149.431255476076,-1.23094556858219E-15));
#285658=CARTESIAN_POINT('Ctrl Pts',(10.0514333556353,149.581255476075,-3.26590867261837));
#285659=CARTESIAN_POINT('Ctrl Pts',(8.13178040253617,149.731255476075,-5.90808429084315));
#285660=CARTESIAN_POINT('Ctrl Pts',(6.212127449437,149.881255476074,-8.55025990906793));
#285661=CARTESIAN_POINT('Ctrl Pts',(3.10606372471845,150.031255476073,-9.55948119098353));
#285662=CARTESIAN_POINT('Ctrl Pts',(-9.96146189739165E-14,150.181255476073,
-10.5687024728991));
#285663=CARTESIAN_POINT('Ctrl Pts',(-3.10606372471865,150.331255476072,
-9.55948119098353));
#285664=CARTESIAN_POINT('Ctrl Pts',(-6.2121274494372,150.481255476072,-8.55025990906793));
#285665=CARTESIAN_POINT('Ctrl Pts',(-8.13178040253636,150.631255476071,
-5.90808429084315));
#285666=CARTESIAN_POINT('Ctrl Pts',(-10.0514333556355,150.78125547607,-3.26590867261836));
#285667=CARTESIAN_POINT('Ctrl Pts',(-10.0514333556355,150.93125547607,2.46189113716437E-15));
#285668=CARTESIAN_POINT('Ctrl Pts',(-10.0514333556355,151.081255476069,
3.26590867261837));
#285669=CARTESIAN_POINT('Ctrl Pts',(-8.13178040253636,151.231255476069,
5.90808429084315));
#285670=CARTESIAN_POINT('Ctrl Pts',(-6.2121274494372,151.381255476068,8.55025990906793));
#285671=CARTESIAN_POINT('Ctrl Pts',(-3.10606372471865,151.531255476067,
9.55948119098353));
#285672=CARTESIAN_POINT('Ctrl Pts',(-9.78898880788321E-14,151.681255476067,
10.5687024728991));
#285673=CARTESIAN_POINT('Ctrl Pts',(3.10606372471845,151.831255476066,9.55948119098353));
#285674=CARTESIAN_POINT('Ctrl Pts',(6.212127449437,151.981255476066,8.55025990906793));
#285675=CARTESIAN_POINT('Ctrl Pts',(8.13178040253616,152.131255476065,5.90808429084315));
#285676=CARTESIAN_POINT('Ctrl Pts',(10.0514333556353,152.281255476064,3.26590867261836));
#285677=CARTESIAN_POINT('Ctrl Pts',(10.0514333556353,152.431255476064,-1.23094556858219E-15));
#285678=CARTESIAN_POINT('Ctrl Pts',(10.0514333556353,152.581255476063,-3.26590867261837));
#285679=CARTESIAN_POINT('Ctrl Pts',(8.13178040253616,152.731255476063,-5.90808429084315));
#285680=CARTESIAN_POINT('Ctrl Pts',(6.212127449437,152.881255476062,-8.55025990906793));
#285681=CARTESIAN_POINT('Ctrl Pts',(3.10606372471845,153.031255476061,-9.55948119098353));
#285682=CARTESIAN_POINT('Ctrl Pts',(-1.01342328245578E-13,153.181255476061,
-10.5687024728991));
#285683=CARTESIAN_POINT('Ctrl Pts',(-3.10606372471865,153.33125547606,-9.55948119098353));
#285684=CARTESIAN_POINT('Ctrl Pts',(10.0514428414942,2.43125000000076,-1.23094673026484E-15));
#285685=CARTESIAN_POINT('Ctrl Pts',(10.0514428414941,2.58125000000016,-3.26591175476071));
#285686=CARTESIAN_POINT('Ctrl Pts',(8.13178807675718,2.73124999999956,-5.90808986649102));
#285687=CARTESIAN_POINT('Ctrl Pts',(6.2121333120202,2.88124999999896,-8.55026797822134));
#285688=CARTESIAN_POINT('Ctrl Pts',(3.10606665601009,3.03124999999835,-9.5594902125713));
#285689=CARTESIAN_POINT('Ctrl Pts',(-1.49568621191919E-14,3.18124999999775,
-10.5687124469213));
#285690=CARTESIAN_POINT('Ctrl Pts',(-3.10606665601012,3.33124999999715,
-9.5594902125713));
#285691=CARTESIAN_POINT('Ctrl Pts',(-6.21213331202023,3.48124999999655,
-8.55026797822134));
#285692=CARTESIAN_POINT('Ctrl Pts',(-8.13178807675721,3.63124999999595,
-5.90808986649102));
#285693=CARTESIAN_POINT('Ctrl Pts',(-10.0514428414942,3.78124999999535,
-3.2659117547607));
#285694=CARTESIAN_POINT('Ctrl Pts',(-10.0514428414942,3.93124999999475,
2.46189346052968E-15));
#285695=CARTESIAN_POINT('Ctrl Pts',(-10.0514428414942,4.08124999999415,
3.26591175476071));
#285696=CARTESIAN_POINT('Ctrl Pts',(-8.13178807675721,4.23124999999355,
5.90808986649102));
#285697=CARTESIAN_POINT('Ctrl Pts',(-6.21213331202023,4.38124999999295,
8.55026797822134));
#285698=CARTESIAN_POINT('Ctrl Pts',(-3.10606665601012,4.53124999999235,
9.5594902125713));
#285699=CARTESIAN_POINT('Ctrl Pts',(-1.32321287811766E-14,4.68124999999175,
10.5687124469213));
#285700=CARTESIAN_POINT('Ctrl Pts',(3.10606665601009,4.83124999999115,9.5594902125713));
#285701=CARTESIAN_POINT('Ctrl Pts',(6.2121333120202,4.98124999999056,8.55026797822134));
#285702=CARTESIAN_POINT('Ctrl Pts',(8.13178807675718,5.13124999998996,5.90808986649102));
#285703=CARTESIAN_POINT('Ctrl Pts',(10.0514428414941,5.28124999998936,3.2659117547607));
#285704=CARTESIAN_POINT('Ctrl Pts',(10.0514428414941,5.43124999998876,-1.23094673026484E-15));
#285705=CARTESIAN_POINT('Origin',(-3.77475828372553E-14,-1.881249999982,
2.68644078414671E-15));
#285706=CARTESIAN_POINT('Origin',(-3.77475828372553E-14,-1.881249999982,
2.68644078414671E-15));
#285707=CARTESIAN_POINT('',(10.0514428414941,74.8062499997113,1.13714546409981E-15));
#285708=CARTESIAN_POINT('',(10.0514428414941,74.4312499997127,1.13870218092026E-15));
#285709=CARTESIAN_POINT('',(10.0514428414941,-1.881249999982,4.14193483802857E-15));
#285710=CARTESIAN_POINT('',(-9.80715114026992,73.2014428414942,-2.20256434814687));
#285711=CARTESIAN_POINT('Ctrl Pts',(-9.80715114026993,73.2014428414942,
-2.20256434814687));
#285712=CARTESIAN_POINT('Ctrl Pts',(-10.0514428414942,73.2550470089109,
-1.11482966369299));
#285713=CARTESIAN_POINT('Ctrl Pts',(-10.0514428414942,73.3062499997172,
2.46189346052968E-15));
#285714=CARTESIAN_POINT('Ctrl Pts',(-10.0514428414942,73.4562499997166,
3.26591175476071));
#285715=CARTESIAN_POINT('Ctrl Pts',(-8.13178807675725,73.606249999716,5.90808986649102));
#285716=CARTESIAN_POINT('Ctrl Pts',(-6.21213331202027,73.7562499997155,
8.55026797822134));
#285717=CARTESIAN_POINT('Ctrl Pts',(-3.10606665601016,73.9062499997148,
9.5594902125713));
#285718=CARTESIAN_POINT('Ctrl Pts',(-5.31854056883567E-14,74.0562499997142,
10.5687124469213));
#285719=CARTESIAN_POINT('Ctrl Pts',(3.10606665601005,74.2062499997136,9.5594902125713));
#285720=CARTESIAN_POINT('Ctrl Pts',(6.21213331202016,74.356249999713,8.55026797822134));
#285721=CARTESIAN_POINT('Ctrl Pts',(8.13178807675713,74.5062499997125,5.90808986649102));
#285722=CARTESIAN_POINT('Ctrl Pts',(10.0514428414941,74.6562499997118,3.2659117547607));
#285723=CARTESIAN_POINT('Ctrl Pts',(10.0514428414941,74.8062499997113,-1.23094673026484E-15));
#285724=CARTESIAN_POINT('',(-8.49270765599395,73.2014428414942,5.37637609042067));
#285725=CARTESIAN_POINT('Origin',(-3.44169137633799E-13,73.2014428414937,
6.99440505513849E-14));
#285726=CARTESIAN_POINT('Ctrl Pts',(-8.49270765599395,73.2014428414942,
5.37637609042067));
#285727=CARTESIAN_POINT('Ctrl Pts',(-8.32075096758918,73.2164846189077,
5.64800475990998));
#285728=CARTESIAN_POINT('Ctrl Pts',(-8.13178807675725,73.2312499997175,
5.90808986649102));
#285729=CARTESIAN_POINT('Ctrl Pts',(-6.21213331202027,73.381249999717,8.55026797822134));
#285730=CARTESIAN_POINT('Ctrl Pts',(-3.10606665601016,73.5312499997164,
9.5594902125713));
#285731=CARTESIAN_POINT('Ctrl Pts',(-5.29694420293989E-14,73.6812499997157,
10.5687124469213));
#285732=CARTESIAN_POINT('Ctrl Pts',(3.10606665601005,73.8312499997151,9.5594902125713));
#285733=CARTESIAN_POINT('Ctrl Pts',(6.21213331202016,73.9812499997146,8.55026797822134));
#285734=CARTESIAN_POINT('Ctrl Pts',(8.13178807675713,74.1312499997139,5.90808986649102));
#285735=CARTESIAN_POINT('Ctrl Pts',(10.0514428414941,74.2812499997134,3.2659117547607));
#285736=CARTESIAN_POINT('Ctrl Pts',(10.0514428414941,74.4312499997127,-1.23094673026484E-15));
#285737=CARTESIAN_POINT('Origin',(-5.57567406742018E-14,75.15,0.));
#285738=CARTESIAN_POINT('',(-9.00737896806879,75.15,7.92887912164091));
#285739=CARTESIAN_POINT('',(10.8311093380487,73.9811093380487,1.23959468221528E-12));
#285740=CARTESIAN_POINT('Ctrl Pts',(-9.00737896806883,75.15,7.92887912164089));
#285741=CARTESIAN_POINT('Ctrl Pts',(-9.69820351182042,75.1230722699582,
7.10333352735252));
#285742=CARTESIAN_POINT('Ctrl Pts',(-10.2770817627655,75.0969971768594,
6.18705949069743));
#285743=CARTESIAN_POINT('Ctrl Pts',(-11.1547474128912,75.0427147698165,
4.2537276641924));
#285744=CARTESIAN_POINT('Ctrl Pts',(-11.458772149512,75.0156043034968,3.25192351069933));
#285745=CARTESIAN_POINT('Ctrl Pts',(-11.8647044188623,74.9511670414305,
0.785797690073358));
#285746=CARTESIAN_POINT('Ctrl Pts',(-11.8535693691975,74.9132994586075,
-0.790228468608902));
#285747=CARTESIAN_POINT('Ctrl Pts',(-11.1272611500066,74.8311653831481,
-3.85248059592555));
#285748=CARTESIAN_POINT('Ctrl Pts',(-10.5113513970943,74.7917269214171,
-5.22009107154959));
#285749=CARTESIAN_POINT('Ctrl Pts',(-8.7026739046729,74.7115308255432,-7.78917298606851));
#285750=CARTESIAN_POINT('Ctrl Pts',(-7.5487369270328,74.6715996731515,-8.81702800061587));
#285751=CARTESIAN_POINT('Ctrl Pts',(-5.10207743581983,74.5943169629155,
-10.3505447400521));
#285752=CARTESIAN_POINT('Ctrl Pts',(-3.69969618597168,74.5565407709911,
-10.8915507233601));
#285753=CARTESIAN_POINT('Ctrl Pts',(-0.794814890740859,74.4783147165169,
-11.3946227024501));
#285754=CARTESIAN_POINT('Ctrl Pts',(0.68139788608677,74.438150792467,-11.3620602603414));
#285755=CARTESIAN_POINT('Ctrl Pts',(3.56236022636539,74.3589289937623,-10.731143902091));
#285756=CARTESIAN_POINT('Ctrl Pts',(4.93923718168667,74.3204915277411,-10.1294577658183));
#285757=CARTESIAN_POINT('Ctrl Pts',(7.40978785039317,74.2370194901842,-8.38810103154457));
#285758=CARTESIAN_POINT('Ctrl Pts',(8.35522120235473,74.1986788538341,-7.33447343383047));
#285759=CARTESIAN_POINT('Ctrl Pts',(9.82758315111317,74.1271233244885,-5.09784210187931));
#285760=CARTESIAN_POINT('Ctrl Pts',(10.3737336163218,74.0865160949434,-3.75031615897431));
#285761=CARTESIAN_POINT('Ctrl Pts',(10.7834985097843,74.0248962589012,-1.59575373885132));
#285762=CARTESIAN_POINT('Ctrl Pts',(10.8530454382111,74.0030454382112,-0.811792966467046));
#285763=CARTESIAN_POINT('Ctrl Pts',(10.8311093380487,73.9811093380488,2.51063073936938E-12));
#285764=CARTESIAN_POINT('',(13.0499999999999,76.2,1.59816407288729E-15));
#285765=CARTESIAN_POINT('',(11.9999999999999,75.15,-1.46957615897682E-15));
#285766=CARTESIAN_POINT('Origin',(-5.57567406742018E-14,76.2,-8.12023357684304E-15));
#285767=CARTESIAN_POINT('Ctrl Pts',(10.8311093380487,73.9811093380487,2.52256548982643E-12));
#285768=CARTESIAN_POINT('Ctrl Pts',(10.8143119258943,73.9643119258943,0.621624670788195));
#285769=CARTESIAN_POINT('Ctrl Pts',(10.7431385725595,73.9465278308509,1.25952363016472));
#285770=CARTESIAN_POINT('Ctrl Pts',(10.3237926143794,73.8885847118865,3.26531548950345));
#285771=CARTESIAN_POINT('Ctrl Pts',(9.77869754599333,73.8484301454163,4.55624067764685));
#285772=CARTESIAN_POINT('Ctrl Pts',(8.61389083368662,73.7901623606025,6.28474801719199));
#285773=CARTESIAN_POINT('Ctrl Pts',(8.16898248558591,73.77113065584,6.82379315457571));
#285774=CARTESIAN_POINT('Ctrl Pts',(6.71221416695348,73.712602997372,8.26680986406343));
#285775=CARTESIAN_POINT('Ctrl Pts',(5.57794501718321,73.6728079061673,9.02448648548346));
#285776=CARTESIAN_POINT('Ctrl Pts',(3.07022473208152,73.5946463655228,10.0763920380405));
#285777=CARTESIAN_POINT('Ctrl Pts',(1.71801133373339,73.5565913691597,10.3549183732943));
#285778=CARTESIAN_POINT('Ctrl Pts',(-0.326019100965161,73.495969531245,
10.3626740067965));
#285779=CARTESIAN_POINT('Ctrl Pts',(-0.997426943464804,73.4759407193955,
10.2996319059488));
#285780=CARTESIAN_POINT('Ctrl Pts',(-2.90140476360216,73.4188140988677,
9.93141432674302));
#285781=CARTESIAN_POINT('Ctrl Pts',(-4.18281817054363,73.3808750952915,
9.44793966102463));
#285782=CARTESIAN_POINT('Ctrl Pts',(-6.01121350243221,73.314726247914,8.23101639980502));
#285783=CARTESIAN_POINT('Ctrl Pts',(-6.5879521784306,73.291939229436,7.7472886059721));
#285784=CARTESIAN_POINT('Ctrl Pts',(-7.63444987216405,73.2463907888306,
6.65109656225167));
#285785=CARTESIAN_POINT('Ctrl Pts',(-8.10174935464808,73.2241898391348,
6.03647401622192));
#285786=CARTESIAN_POINT('Ctrl Pts',(-8.49270765599396,73.2014428414942,
5.37637609042066));
#285787=CARTESIAN_POINT('',(-0.772542478744793,75.15,11.975106601552));
#285788=CARTESIAN_POINT('Ctrl Pts',(-0.772542478745,75.15,11.975106601552));
#285789=CARTESIAN_POINT('Ctrl Pts',(-2.04083064796245,75.0278624546732,
11.7708948887632));
#285790=CARTESIAN_POINT('Ctrl Pts',(-3.28683095100001,74.9079915841135,
11.361657813701));
#285791=CARTESIAN_POINT('Ctrl Pts',(-5.51313922720053,74.667613993203,10.1863677934907));
#285792=CARTESIAN_POINT('Ctrl Pts',(-6.50027462213247,74.544601786977,9.43829777442363));
#285793=CARTESIAN_POINT('Ctrl Pts',(-8.13242682116904,74.3050792679408,
7.7192133645345));
#285794=CARTESIAN_POINT('Ctrl Pts',(-9.05390526764337,74.1607724922424,
6.50436427171037));
#285795=CARTESIAN_POINT('Ctrl Pts',(-10.1033813875356,73.8512496555443,
3.72785548679263));
#285796=CARTESIAN_POINT('Ctrl Pts',(-10.3342684942795,73.7200889598579,
2.52709309126293));
#285797=CARTESIAN_POINT('Ctrl Pts',(-10.3754040919887,73.4810018608485,
0.302332627258651));
#285798=CARTESIAN_POINT('Ctrl Pts',(-10.2570731251301,73.3564895116309,
-0.906797363353994));
#285799=CARTESIAN_POINT('Ctrl Pts',(-9.8071511402699,73.2014428414942,-2.20256434814686));
#285800=CARTESIAN_POINT('Origin',(-5.57567406742018E-14,75.15,0.));
#285801=CARTESIAN_POINT('Origin',(-8.79029313101884E-14,130.96875,0.));
#285802=CARTESIAN_POINT('',(10.158727500065,76.2,-6.38750777529532));
#285803=CARTESIAN_POINT('',(11.7004490057565,76.2,2.66448739229345));
#285804=CARTESIAN_POINT('Origin',(-5.63614389192858E-14,76.2,0.));
#285805=CARTESIAN_POINT('Ctrl Pts',(11.7004490057565,76.2,2.66448739229345));
#285806=CARTESIAN_POINT('Ctrl Pts',(11.1542089550934,76.1008922571332,5.06316785750065));
#285807=CARTESIAN_POINT('Ctrl Pts',(9.70820393249932,76.0062499997072,7.05342302750968));
#285808=CARTESIAN_POINT('Ctrl Pts',(7.41640786499869,75.8562499997078,10.2078097002245));
#285809=CARTESIAN_POINT('Ctrl Pts',(3.70820393249932,75.7062499997084,11.4126781955418));
#285810=CARTESIAN_POINT('Ctrl Pts',(-5.36728955793647E-14,75.556249999709,
12.6175466908592));
#285811=CARTESIAN_POINT('Ctrl Pts',(-3.70820393249942,75.4062499997096,
11.4126781955418));
#285812=CARTESIAN_POINT('Ctrl Pts',(-6.83503484848808,75.2797670322315,
10.3967092441472));
#285813=CARTESIAN_POINT('Ctrl Pts',(-9.00737896806879,75.15,7.9288791216409));
#285814=CARTESIAN_POINT('Ctrl Pts',(10.1587275000636,76.1999999999992,-6.38750777529466));
#285815=CARTESIAN_POINT('Ctrl Pts',(10.7617685920941,76.1555651822736,-5.42842790552554));
#285816=CARTESIAN_POINT('Ctrl Pts',(11.2259449173429,76.1097672665456,-4.38879634680429));
#285817=CARTESIAN_POINT('Ctrl Pts',(11.9626296774665,76.0014610227487,-1.81289318850251));
#285818=CARTESIAN_POINT('Ctrl Pts',(12.0964698979846,75.9423786381454,-0.257928135750359));
#285819=CARTESIAN_POINT('Ctrl Pts',(11.7635714974025,75.8187973732225,2.84622558177574));
#285820=CARTESIAN_POINT('Ctrl Pts',(11.2886361360743,75.7544492469013,4.36454762104216));
#285821=CARTESIAN_POINT('Ctrl Pts',(9.78747214476226,75.6298418638766,7.11578131626414));
#285822=CARTESIAN_POINT('Ctrl Pts',(8.78158044779031,75.570682135926,8.32542804683128));
#285823=CARTESIAN_POINT('Ctrl Pts',(6.41003130511432,75.4472027071465,10.2546288766467));
#285824=CARTESIAN_POINT('Ctrl Pts',(5.08061870783028,75.3867653435368,10.9741776338188));
#285825=CARTESIAN_POINT('Ctrl Pts',(2.2250043460616,75.2712533161347,11.8868781811265));
#285826=CARTESIAN_POINT('Ctrl Pts',(0.723748485605121,75.2105262409342,
12.0716358742328));
#285827=CARTESIAN_POINT('Ctrl Pts',(-0.772542478744996,75.15,11.975106601552));
#285828=CARTESIAN_POINT('Ctrl Pts',(-10.0514428414942,-1.69374999998275,
2.46189346052968E-15));
#285829=CARTESIAN_POINT('Ctrl Pts',(-10.0514428414942,-1.54374999998335,
3.26591175476071));
#285830=CARTESIAN_POINT('Ctrl Pts',(-8.1317880767572,-1.39374999998395,
5.90808986649102));
#285831=CARTESIAN_POINT('Ctrl Pts',(-6.21213331202023,-1.24374999998455,
8.55026797822134));
#285832=CARTESIAN_POINT('Ctrl Pts',(-3.10606665601012,-1.09374999998515,
9.5594902125713));
#285833=CARTESIAN_POINT('Ctrl Pts',(-9.99267389681068E-15,-0.943749999985747,
10.5687124469213));
#285834=CARTESIAN_POINT('Ctrl Pts',(3.1060666560101,-0.793749999986346,
9.5594902125713));
#285835=CARTESIAN_POINT('Ctrl Pts',(6.21213331202021,-0.643749999986944,
8.55026797822134));
#285836=CARTESIAN_POINT('Ctrl Pts',(8.13178807675718,-0.493749999987543,
5.90808986649102));
#285837=CARTESIAN_POINT('Ctrl Pts',(10.0514428414942,-0.343749999988142,
3.2659117547607));
#285838=CARTESIAN_POINT('Ctrl Pts',(10.0514428414942,-0.193749999988742,
-1.23094673026484E-15));
#285839=CARTESIAN_POINT('Ctrl Pts',(10.0514428414942,-0.0437499999893418,
-3.26591175476071));
#285840=CARTESIAN_POINT('Ctrl Pts',(8.13178807675718,0.106250000010057,
-5.90808986649102));
#285841=CARTESIAN_POINT('Ctrl Pts',(6.2121333120202,0.256250000009456,-8.55026797822134));
#285842=CARTESIAN_POINT('Ctrl Pts',(3.10606665601009,0.406250000008854,
-9.5594902125713));
#285843=CARTESIAN_POINT('Ctrl Pts',(-1.34451165064878E-14,0.556250000008252,
-10.5687124469213));
#285844=CARTESIAN_POINT('Ctrl Pts',(-3.10606665601012,0.70625000000765,
-9.5594902125713));
#285845=CARTESIAN_POINT('Ctrl Pts',(-6.21213331202023,0.856250000007049,
-8.55026797822134));
#285846=CARTESIAN_POINT('Ctrl Pts',(-8.1317880767572,1.00625000000645,-5.90808986649102));
#285847=CARTESIAN_POINT('Ctrl Pts',(-10.0514428414942,1.15625000000585,
-3.2659117547607));
#285848=CARTESIAN_POINT('Ctrl Pts',(-10.0514428414942,1.30625000000525,
2.46189346052968E-15));
#285849=CARTESIAN_POINT('Ctrl Pts',(-10.0514428414942,1.45625000000465,
3.26591175476071));
#285850=CARTESIAN_POINT('Ctrl Pts',(-8.1317880767572,1.60625000000405,5.90808986649102));
#285851=CARTESIAN_POINT('Ctrl Pts',(-6.21213331202023,1.75625000000345,
8.55026797822134));
#285852=CARTESIAN_POINT('Ctrl Pts',(-3.10606665601012,1.90625000000285,
9.5594902125713));
#285853=CARTESIAN_POINT('Ctrl Pts',(-1.17203831684725E-14,2.05625000000225,
10.5687124469213));
#285854=CARTESIAN_POINT('Ctrl Pts',(3.1060666560101,2.20625000000165,9.5594902125713));
#285855=CARTESIAN_POINT('Ctrl Pts',(6.2121333120202,2.35625000000106,8.55026797822134));
#285856=CARTESIAN_POINT('Ctrl Pts',(8.13178807675718,2.50625000000046,5.90808986649102));
#285857=CARTESIAN_POINT('Ctrl Pts',(10.0514428414942,2.65624999999986,3.2659117547607));
#285858=CARTESIAN_POINT('Ctrl Pts',(10.0514428414942,2.80624999999926,-1.23094673026484E-15));
#285859=CARTESIAN_POINT('Ctrl Pts',(10.0514428414942,2.95624999999866,-3.26591175476071));
#285860=CARTESIAN_POINT('Ctrl Pts',(8.13178807675718,3.10624999999806,-5.90808986649102));
#285861=CARTESIAN_POINT('Ctrl Pts',(6.2121333120202,3.25624999999746,-8.55026797822134));
#285862=CARTESIAN_POINT('Ctrl Pts',(3.10606665601009,3.40624999999685,-9.5594902125713));
#285863=CARTESIAN_POINT('Ctrl Pts',(-1.51728257781496E-14,3.55624999999625,
-10.5687124469213));
#285864=CARTESIAN_POINT('Ctrl Pts',(-3.10606665601012,3.70624999999565,
-9.5594902125713));
#285865=CARTESIAN_POINT('Ctrl Pts',(-6.21213331202023,3.85624999999505,
-8.55026797822134));
#285866=CARTESIAN_POINT('Ctrl Pts',(-8.13178807675721,4.00624999999445,
-5.90808986649102));
#285867=CARTESIAN_POINT('Ctrl Pts',(-10.0514428414942,4.15624999999385,
-3.2659117547607));
#285868=CARTESIAN_POINT('Ctrl Pts',(-10.0514428414942,4.30624999999325,
2.46189346052968E-15));
#285869=CARTESIAN_POINT('Ctrl Pts',(-10.0514428414942,4.45624999999265,
3.26591175476071));
#285870=CARTESIAN_POINT('Ctrl Pts',(-8.13178807675721,4.60624999999205,
5.90808986649102));
#285871=CARTESIAN_POINT('Ctrl Pts',(-6.21213331202023,4.75624999999145,
8.55026797822134));
#285872=CARTESIAN_POINT('Ctrl Pts',(-3.10606665601012,4.90624999999085,
9.5594902125713));
#285873=CARTESIAN_POINT('Ctrl Pts',(-1.34480924401344E-14,5.05624999999025,
10.5687124469213));
#285874=CARTESIAN_POINT('Ctrl Pts',(3.10606665601009,5.20624999998966,9.5594902125713));
#285875=CARTESIAN_POINT('Ctrl Pts',(6.2121333120202,5.35624999998906,8.55026797822134));
#285876=CARTESIAN_POINT('Ctrl Pts',(8.13178807675718,5.50624999998846,5.90808986649102));
#285877=CARTESIAN_POINT('Ctrl Pts',(10.0514428414942,5.65624999998786,3.2659117547607));
#285878=CARTESIAN_POINT('Ctrl Pts',(10.0514428414941,5.80624999998726,-1.23094673026484E-15));
#285879=CARTESIAN_POINT('Ctrl Pts',(10.0514428414941,5.95624999998666,-3.26591175476071));
#285880=CARTESIAN_POINT('Ctrl Pts',(8.13178807675717,6.10624999998606,-5.90808986649102));
#285881=CARTESIAN_POINT('Ctrl Pts',(6.2121333120202,6.25624999998545,-8.55026797822134));
#285882=CARTESIAN_POINT('Ctrl Pts',(3.10606665601009,6.40624999998485,-9.5594902125713));
#285883=CARTESIAN_POINT('Ctrl Pts',(-1.69005350498115E-14,6.55624999998425,
-10.5687124469213));
#285884=CARTESIAN_POINT('Ctrl Pts',(-3.10606665601013,6.70624999998365,
-9.5594902125713));
#285885=CARTESIAN_POINT('Ctrl Pts',(-6.21213331202023,6.85624999998305,
-8.55026797822134));
#285886=CARTESIAN_POINT('Ctrl Pts',(-8.13178807675721,7.00624999998245,
-5.90808986649102));
#285887=CARTESIAN_POINT('Ctrl Pts',(-10.0514428414942,7.15624999998184,
-3.2659117547607));
#285888=CARTESIAN_POINT('Ctrl Pts',(-10.0514428414942,7.30624999998125,
2.46189346052968E-15));
#285889=CARTESIAN_POINT('Ctrl Pts',(-10.0514428414942,7.45624999998065,
3.26591175476071));
#285890=CARTESIAN_POINT('Ctrl Pts',(-8.13178807675721,7.60624999998005,
5.90808986649102));
#285891=CARTESIAN_POINT('Ctrl Pts',(-6.21213331202023,7.75624999997945,
8.55026797822134));
#285892=CARTESIAN_POINT('Ctrl Pts',(-3.10606665601012,7.90624999997885,
9.5594902125713));
#285893=CARTESIAN_POINT('Ctrl Pts',(-1.51758017117962E-14,8.05624999997825,
10.5687124469213));
#285894=CARTESIAN_POINT('Ctrl Pts',(3.10606665601009,8.20624999997765,9.5594902125713));
#285895=CARTESIAN_POINT('Ctrl Pts',(6.2121333120202,8.35624999997706,8.55026797822134));
#285896=CARTESIAN_POINT('Ctrl Pts',(8.13178807675717,8.50624999997646,5.90808986649102));
#285897=CARTESIAN_POINT('Ctrl Pts',(10.0514428414942,8.65624999997586,3.2659117547607));
#285898=CARTESIAN_POINT('Ctrl Pts',(10.0514428414941,8.80624999997526,-1.23094673026484E-15));
#285899=CARTESIAN_POINT('Ctrl Pts',(10.0514428414941,8.95624999997466,-3.26591175476071));
#285900=CARTESIAN_POINT('Ctrl Pts',(8.13178807675717,9.10624999997406,-5.90808986649102));
#285901=CARTESIAN_POINT('Ctrl Pts',(6.2121333120202,9.25624999997346,-8.55026797822134));
#285902=CARTESIAN_POINT('Ctrl Pts',(3.10606665601009,9.40624999997286,-9.5594902125713));
#285903=CARTESIAN_POINT('Ctrl Pts',(-1.86282443214733E-14,9.55624999997225,
-10.5687124469213));
#285904=CARTESIAN_POINT('Ctrl Pts',(-3.10606665601013,9.70624999997165,
-9.5594902125713));
#285905=CARTESIAN_POINT('Ctrl Pts',(-6.21213331202023,9.85624999997105,
-8.55026797822134));
#285906=CARTESIAN_POINT('Ctrl Pts',(-8.13178807675721,10.0062499999704,
-5.90808986649102));
#285907=CARTESIAN_POINT('Ctrl Pts',(-10.0514428414942,10.1562499999698,
-3.2659117547607));
#285908=CARTESIAN_POINT('Ctrl Pts',(-10.0514428414942,10.3062499999692,
2.46189346052968E-15));
#285909=CARTESIAN_POINT('Ctrl Pts',(-10.0514428414942,10.4562499999686,
3.26591175476071));
#285910=CARTESIAN_POINT('Ctrl Pts',(-8.13178807675721,10.606249999968,5.90808986649102));
#285911=CARTESIAN_POINT('Ctrl Pts',(-6.21213331202023,10.7562499999674,
8.55026797822134));
#285912=CARTESIAN_POINT('Ctrl Pts',(-3.10606665601013,10.9062499999668,
9.5594902125713));
#285913=CARTESIAN_POINT('Ctrl Pts',(-1.6903510983458E-14,11.0562499999663,
10.5687124469213));
#285914=CARTESIAN_POINT('Ctrl Pts',(3.10606665601009,11.2062499999657,9.5594902125713));
#285915=CARTESIAN_POINT('Ctrl Pts',(6.2121333120202,11.3562499999651,8.55026797822134));
#285916=CARTESIAN_POINT('Ctrl Pts',(8.13178807675717,11.5062499999645,5.90808986649102));
#285917=CARTESIAN_POINT('Ctrl Pts',(10.0514428414941,11.6562499999639,3.2659117547607));
#285918=CARTESIAN_POINT('Ctrl Pts',(10.0514428414941,11.8062499999633,-1.23094673026484E-15));
#285919=CARTESIAN_POINT('Ctrl Pts',(10.0514428414941,11.9562499999627,-3.26591175476071));
#285920=CARTESIAN_POINT('Ctrl Pts',(8.13178807675717,12.1062499999621,-5.90808986649102));
#285921=CARTESIAN_POINT('Ctrl Pts',(6.2121333120202,12.2562499999615,-8.55026797822134));
#285922=CARTESIAN_POINT('Ctrl Pts',(3.10606665601009,12.4062499999609,-9.5594902125713));
#285923=CARTESIAN_POINT('Ctrl Pts',(-2.03559535931351E-14,12.5562499999603,
-10.5687124469213));
#285924=CARTESIAN_POINT('Ctrl Pts',(-3.10606665601013,12.7062499999597,
-9.5594902125713));
#285925=CARTESIAN_POINT('Ctrl Pts',(-6.21213331202024,12.856249999959,-8.55026797822134));
#285926=CARTESIAN_POINT('Ctrl Pts',(-8.13178807675721,13.0062499999584,
-5.90808986649102));
#285927=CARTESIAN_POINT('Ctrl Pts',(-10.0514428414942,13.1562499999578,
-3.2659117547607));
#285928=CARTESIAN_POINT('Ctrl Pts',(-10.0514428414942,13.3062499999572,
2.46189346052968E-15));
#285929=CARTESIAN_POINT('Ctrl Pts',(-10.0514428414942,13.4562499999566,
3.26591175476071));
#285930=CARTESIAN_POINT('Ctrl Pts',(-8.13178807675721,13.606249999956,5.90808986649102));
#285931=CARTESIAN_POINT('Ctrl Pts',(-6.21213331202023,13.7562499999554,
8.55026797822134));
#285932=CARTESIAN_POINT('Ctrl Pts',(-3.10606665601013,13.9062499999549,
9.5594902125713));
#285933=CARTESIAN_POINT('Ctrl Pts',(-1.86312202551199E-14,14.0562499999543,
10.5687124469213));
#285934=CARTESIAN_POINT('Ctrl Pts',(3.10606665601009,14.2062499999537,9.5594902125713));
#285935=CARTESIAN_POINT('Ctrl Pts',(6.2121333120202,14.3562499999531,8.55026797822134));
#285936=CARTESIAN_POINT('Ctrl Pts',(8.13178807675717,14.5062499999525,5.90808986649102));
#285937=CARTESIAN_POINT('Ctrl Pts',(10.0514428414941,14.6562499999519,3.2659117547607));
#285938=CARTESIAN_POINT('Ctrl Pts',(10.0514428414941,14.8062499999513,-1.23094673026484E-15));
#285939=CARTESIAN_POINT('Ctrl Pts',(10.0514428414941,14.9562499999507,-3.26591175476071));
#285940=CARTESIAN_POINT('Ctrl Pts',(8.13178807675717,15.1062499999501,-5.90808986649102));
#285941=CARTESIAN_POINT('Ctrl Pts',(6.21213331202019,15.2562499999495,-8.55026797822134));
#285942=CARTESIAN_POINT('Ctrl Pts',(3.10606665601009,15.4062499999489,-9.5594902125713));
#285943=CARTESIAN_POINT('Ctrl Pts',(-2.2083662864797E-14,15.5562499999482,
-10.5687124469213));
#285944=CARTESIAN_POINT('Ctrl Pts',(-3.10606665601013,15.7062499999477,
-9.5594902125713));
#285945=CARTESIAN_POINT('Ctrl Pts',(-6.21213331202024,15.856249999947,-8.55026797822134));
#285946=CARTESIAN_POINT('Ctrl Pts',(-8.13178807675721,16.0062499999464,
-5.90808986649102));
#285947=CARTESIAN_POINT('Ctrl Pts',(-10.0514428414942,16.1562499999458,
-3.2659117547607));
#285948=CARTESIAN_POINT('Ctrl Pts',(-10.0514428414942,16.3062499999452,
2.46189346052968E-15));
#285949=CARTESIAN_POINT('Ctrl Pts',(-10.0514428414942,16.4562499999446,
3.26591175476071));
#285950=CARTESIAN_POINT('Ctrl Pts',(-8.13178807675721,16.606249999944,5.90808986649102));
#285951=CARTESIAN_POINT('Ctrl Pts',(-6.21213331202024,16.7562499999434,
8.55026797822134));
#285952=CARTESIAN_POINT('Ctrl Pts',(-3.10606665601013,16.9062499999428,
9.5594902125713));
#285953=CARTESIAN_POINT('Ctrl Pts',(-2.03589295267817E-14,17.0562499999422,
10.5687124469213));
#285954=CARTESIAN_POINT('Ctrl Pts',(3.10606665601009,17.2062499999417,9.5594902125713));
#285955=CARTESIAN_POINT('Ctrl Pts',(6.21213331202019,17.3562499999411,8.55026797822134));
#285956=CARTESIAN_POINT('Ctrl Pts',(8.13178807675717,17.5062499999405,5.90808986649102));
#285957=CARTESIAN_POINT('Ctrl Pts',(10.0514428414941,17.6562499999399,3.2659117547607));
#285958=CARTESIAN_POINT('Ctrl Pts',(10.0514428414941,17.8062499999393,-1.23094673026484E-15));
#285959=CARTESIAN_POINT('Ctrl Pts',(10.0514428414941,17.9562499999387,-3.26591175476071));
#285960=CARTESIAN_POINT('Ctrl Pts',(8.13178807675717,18.1062499999381,-5.90808986649102));
#285961=CARTESIAN_POINT('Ctrl Pts',(6.21213331202019,18.2562499999375,-8.55026797822134));
#285962=CARTESIAN_POINT('Ctrl Pts',(3.10606665601008,18.4062499999369,-9.5594902125713));
#285963=CARTESIAN_POINT('Ctrl Pts',(-2.38113721364588E-14,18.5562499999362,
-10.5687124469213));
#285964=CARTESIAN_POINT('Ctrl Pts',(-3.10606665601013,18.7062499999357,
-9.5594902125713));
#285965=CARTESIAN_POINT('Ctrl Pts',(-6.21213331202024,18.856249999935,-8.55026797822134));
#285966=CARTESIAN_POINT('Ctrl Pts',(-8.13178807675721,19.0062499999344,
-5.90808986649102));
#285967=CARTESIAN_POINT('Ctrl Pts',(-10.0514428414942,19.1562499999338,
-3.2659117547607));
#285968=CARTESIAN_POINT('Ctrl Pts',(-10.0514428414942,19.3062499999332,
2.46189346052968E-15));
#285969=CARTESIAN_POINT('Ctrl Pts',(-10.0514428414942,19.4562499999326,
3.26591175476071));
#285970=CARTESIAN_POINT('Ctrl Pts',(-8.13178807675721,19.606249999932,5.90808986649102));
#285971=CARTESIAN_POINT('Ctrl Pts',(-6.21213331202024,19.7562499999314,
8.55026797822134));
#285972=CARTESIAN_POINT('Ctrl Pts',(-3.10606665601013,19.9062499999308,
9.5594902125713));
#285973=CARTESIAN_POINT('Ctrl Pts',(-2.20866387984435E-14,20.0562499999302,
10.5687124469213));
#285974=CARTESIAN_POINT('Ctrl Pts',(3.10606665601009,20.2062499999297,9.5594902125713));
#285975=CARTESIAN_POINT('Ctrl Pts',(6.21213331202019,20.356249999929,8.55026797822134));
#285976=CARTESIAN_POINT('Ctrl Pts',(8.13178807675717,20.5062499999285,5.90808986649102));
#285977=CARTESIAN_POINT('Ctrl Pts',(10.0514428414941,20.6562499999279,3.2659117547607));
#285978=CARTESIAN_POINT('Ctrl Pts',(10.0514428414941,20.8062499999273,-1.23094673026484E-15));
#285979=CARTESIAN_POINT('Ctrl Pts',(10.0514428414941,20.9562499999267,-3.26591175476071));
#285980=CARTESIAN_POINT('Ctrl Pts',(8.13178807675716,21.1062499999261,-5.90808986649102));
#285981=CARTESIAN_POINT('Ctrl Pts',(6.21213331202019,21.2562499999255,-8.55026797822134));
#285982=CARTESIAN_POINT('Ctrl Pts',(3.10606665601008,21.4062499999249,-9.5594902125713));
#285983=CARTESIAN_POINT('Ctrl Pts',(-2.55390814081207E-14,21.5562499999242,
-10.5687124469213));
#285984=CARTESIAN_POINT('Ctrl Pts',(-3.10606665601013,21.7062499999237,
-9.5594902125713));
#285985=CARTESIAN_POINT('Ctrl Pts',(-6.21213331202024,21.856249999923,-8.55026797822134));
#285986=CARTESIAN_POINT('Ctrl Pts',(-8.13178807675722,22.0062499999224,
-5.90808986649102));
#285987=CARTESIAN_POINT('Ctrl Pts',(-10.0514428414942,22.1562499999218,
-3.2659117547607));
#285988=CARTESIAN_POINT('Ctrl Pts',(-10.0514428414942,22.3062499999212,
2.46189346052968E-15));
#285989=CARTESIAN_POINT('Ctrl Pts',(-10.0514428414942,22.4562499999206,
3.26591175476071));
#285990=CARTESIAN_POINT('Ctrl Pts',(-8.13178807675722,22.60624999992,5.90808986649102));
#285991=CARTESIAN_POINT('Ctrl Pts',(-6.21213331202024,22.7562499999194,
8.55026797822134));
#285992=CARTESIAN_POINT('Ctrl Pts',(-3.10606665601013,22.9062499999188,
9.5594902125713));
#285993=CARTESIAN_POINT('Ctrl Pts',(-2.38143480701054E-14,23.0562499999182,
10.5687124469213));
#285994=CARTESIAN_POINT('Ctrl Pts',(3.10606665601008,23.2062499999177,9.5594902125713));
#285995=CARTESIAN_POINT('Ctrl Pts',(6.21213331202019,23.3562499999171,8.55026797822134));
#285996=CARTESIAN_POINT('Ctrl Pts',(8.13178807675716,23.5062499999165,5.90808986649102));
#285997=CARTESIAN_POINT('Ctrl Pts',(10.0514428414941,23.6562499999159,3.2659117547607));
#285998=CARTESIAN_POINT('Ctrl Pts',(10.0514428414941,23.8062499999153,-1.23094673026484E-15));
#285999=CARTESIAN_POINT('Ctrl Pts',(10.0514428414941,23.9562499999147,-3.26591175476071));
#286000=CARTESIAN_POINT('Ctrl Pts',(8.13178807675716,24.1062499999141,-5.90808986649102));
#286001=CARTESIAN_POINT('Ctrl Pts',(6.21213331202019,24.2562499999135,-8.55026797822134));
#286002=CARTESIAN_POINT('Ctrl Pts',(3.10606665601008,24.4062499999129,-9.5594902125713));
#286003=CARTESIAN_POINT('Ctrl Pts',(-2.72667906797825E-14,24.5562499999122,
-10.5687124469213));
#286004=CARTESIAN_POINT('Ctrl Pts',(-3.10606665601014,24.7062499999116,
-9.5594902125713));
#286005=CARTESIAN_POINT('Ctrl Pts',(-6.21213331202024,24.856249999911,-8.55026797822134));
#286006=CARTESIAN_POINT('Ctrl Pts',(-8.13178807675722,25.0062499999104,
-5.90808986649102));
#286007=CARTESIAN_POINT('Ctrl Pts',(-10.0514428414942,25.1562499999098,
-3.2659117547607));
#286008=CARTESIAN_POINT('Ctrl Pts',(-10.0514428414942,25.3062499999092,
2.46189346052968E-15));
#286009=CARTESIAN_POINT('Ctrl Pts',(-10.0514428414942,25.4562499999086,
3.26591175476071));
#286010=CARTESIAN_POINT('Ctrl Pts',(-8.13178807675722,25.6062499999081,
5.90808986649102));
#286011=CARTESIAN_POINT('Ctrl Pts',(-6.21213331202024,25.7562499999074,
8.55026797822134));
#286012=CARTESIAN_POINT('Ctrl Pts',(-3.10606665601013,25.9062499999069,
9.5594902125713));
#286013=CARTESIAN_POINT('Ctrl Pts',(-2.55420573417672E-14,26.0562499999062,
10.5687124469213));
#286014=CARTESIAN_POINT('Ctrl Pts',(3.10606665601008,26.2062499999057,9.5594902125713));
#286015=CARTESIAN_POINT('Ctrl Pts',(6.21213331202019,26.356249999905,8.55026797822134));
#286016=CARTESIAN_POINT('Ctrl Pts',(8.13178807675716,26.5062499999045,5.90808986649102));
#286017=CARTESIAN_POINT('Ctrl Pts',(10.0514428414941,26.6562499999039,3.2659117547607));
#286018=CARTESIAN_POINT('Ctrl Pts',(10.0514428414941,26.8062499999033,-1.23094673026484E-15));
#286019=CARTESIAN_POINT('Ctrl Pts',(10.0514428414941,26.9562499999027,-3.26591175476071));
#286020=CARTESIAN_POINT('Ctrl Pts',(8.13178807675716,27.1062499999021,-5.90808986649102));
#286021=CARTESIAN_POINT('Ctrl Pts',(6.21213331202019,27.2562499999015,-8.55026797822134));
#286022=CARTESIAN_POINT('Ctrl Pts',(3.10606665601008,27.4062499999009,-9.5594902125713));
#286023=CARTESIAN_POINT('Ctrl Pts',(-2.89944999514443E-14,27.5562499999002,
-10.5687124469213));
#286024=CARTESIAN_POINT('Ctrl Pts',(-3.10606665601014,27.7062499998996,
-9.5594902125713));
#286025=CARTESIAN_POINT('Ctrl Pts',(-6.21213331202024,27.856249999899,-8.55026797822134));
#286026=CARTESIAN_POINT('Ctrl Pts',(-8.13178807675722,28.0062499998984,
-5.90808986649102));
#286027=CARTESIAN_POINT('Ctrl Pts',(-10.0514428414942,28.1562499998978,
-3.2659117547607));
#286028=CARTESIAN_POINT('Ctrl Pts',(-10.0514428414942,28.3062499998973,
2.46189346052968E-15));
#286029=CARTESIAN_POINT('Ctrl Pts',(-10.0514428414942,28.4562499998966,
3.26591175476071));
#286030=CARTESIAN_POINT('Ctrl Pts',(-8.13178807675722,28.606249999896,5.90808986649102));
#286031=CARTESIAN_POINT('Ctrl Pts',(-6.21213331202024,28.7562499998954,
8.55026797822134));
#286032=CARTESIAN_POINT('Ctrl Pts',(-3.10606665601014,28.9062499998949,
9.5594902125713));
#286033=CARTESIAN_POINT('Ctrl Pts',(-2.72697666134291E-14,29.0562499998942,
10.5687124469213));
#286034=CARTESIAN_POINT('Ctrl Pts',(3.10606665601008,29.2062499998937,9.5594902125713));
#286035=CARTESIAN_POINT('Ctrl Pts',(6.21213331202019,29.356249999893,8.55026797822134));
#286036=CARTESIAN_POINT('Ctrl Pts',(8.13178807675716,29.5062499998925,5.90808986649102));
#286037=CARTESIAN_POINT('Ctrl Pts',(10.0514428414941,29.6562499998919,3.2659117547607));
#286038=CARTESIAN_POINT('Ctrl Pts',(10.0514428414941,29.8062499998913,-1.23094673026484E-15));
#286039=CARTESIAN_POINT('Ctrl Pts',(10.0514428414941,29.9562499998907,-3.26591175476071));
#286040=CARTESIAN_POINT('Ctrl Pts',(8.13178807675716,30.1062499998901,-5.90808986649102));
#286041=CARTESIAN_POINT('Ctrl Pts',(6.21213331202019,30.2562499998895,-8.55026797822134));
#286042=CARTESIAN_POINT('Ctrl Pts',(3.10606665601008,30.4062499998889,-9.5594902125713));
#286043=CARTESIAN_POINT('Ctrl Pts',(-3.07222092231062E-14,30.5562499998883,
-10.5687124469213));
#286044=CARTESIAN_POINT('Ctrl Pts',(-3.10606665601014,30.7062499998877,
-9.5594902125713));
#286045=CARTESIAN_POINT('Ctrl Pts',(-6.21213331202025,30.8562499998871,
-8.55026797822134));
#286046=CARTESIAN_POINT('Ctrl Pts',(-8.13178807675722,31.0062499998864,
-5.90808986649102));
#286047=CARTESIAN_POINT('Ctrl Pts',(-10.0514428414942,31.1562499998858,
-3.2659117547607));
#286048=CARTESIAN_POINT('Ctrl Pts',(-10.0514428414942,31.3062499998852,
2.46189346052968E-15));
#286049=CARTESIAN_POINT('Ctrl Pts',(-10.0514428414942,31.4562499998847,
3.26591175476071));
#286050=CARTESIAN_POINT('Ctrl Pts',(-8.13178807675722,31.606249999884,5.90808986649102));
#286051=CARTESIAN_POINT('Ctrl Pts',(-6.21213331202024,31.7562499998835,
8.55026797822134));
#286052=CARTESIAN_POINT('Ctrl Pts',(-3.10606665601014,31.9062499998829,
9.5594902125713));
#286053=CARTESIAN_POINT('Ctrl Pts',(-2.89974758850909E-14,32.0562499998822,
10.5687124469213));
#286054=CARTESIAN_POINT('Ctrl Pts',(3.10606665601008,32.2062499998816,9.5594902125713));
#286055=CARTESIAN_POINT('Ctrl Pts',(6.21213331202019,32.3562499998811,8.55026797822134));
#286056=CARTESIAN_POINT('Ctrl Pts',(8.13178807675716,32.5062499998805,5.90808986649102));
#286057=CARTESIAN_POINT('Ctrl Pts',(10.0514428414941,32.6562499998798,3.2659117547607));
#286058=CARTESIAN_POINT('Ctrl Pts',(10.0514428414941,32.8062499998793,-1.23094673026484E-15));
#286059=CARTESIAN_POINT('Ctrl Pts',(10.0514428414941,32.9562499998787,-3.26591175476071));
#286060=CARTESIAN_POINT('Ctrl Pts',(8.13178807675716,33.1062499998781,-5.90808986649102));
#286061=CARTESIAN_POINT('Ctrl Pts',(6.21213331202019,33.2562499998775,-8.55026797822134));
#286062=CARTESIAN_POINT('Ctrl Pts',(3.10606665601008,33.4062499998769,-9.5594902125713));
#286063=CARTESIAN_POINT('Ctrl Pts',(-3.2449918494768E-14,33.5562499998763,
-10.5687124469213));
#286064=CARTESIAN_POINT('Ctrl Pts',(-3.10606665601014,33.7062499998756,
-9.5594902125713));
#286065=CARTESIAN_POINT('Ctrl Pts',(-6.21213331202025,33.8562499998751,
-8.55026797822134));
#286066=CARTESIAN_POINT('Ctrl Pts',(-8.13178807675722,34.0062499998744,
-5.90808986649102));
#286067=CARTESIAN_POINT('Ctrl Pts',(-10.0514428414942,34.1562499998739,
-3.2659117547607));
#286068=CARTESIAN_POINT('Ctrl Pts',(-10.0514428414942,34.3062499998732,
2.46189346052968E-15));
#286069=CARTESIAN_POINT('Ctrl Pts',(-10.0514428414942,34.4562499998727,
3.26591175476071));
#286070=CARTESIAN_POINT('Ctrl Pts',(-8.13178807675722,34.606249999872,5.90808986649102));
#286071=CARTESIAN_POINT('Ctrl Pts',(-6.21213331202024,34.7562499998715,
8.55026797822134));
#286072=CARTESIAN_POINT('Ctrl Pts',(-3.10606665601014,34.9062499998708,
9.5594902125713));
#286073=CARTESIAN_POINT('Ctrl Pts',(-3.07251851567527E-14,35.0562499998703,
10.5687124469213));
#286074=CARTESIAN_POINT('Ctrl Pts',(3.10606665601008,35.2062499998697,9.5594902125713));
#286075=CARTESIAN_POINT('Ctrl Pts',(6.21213331202019,35.3562499998691,8.55026797822134));
#286076=CARTESIAN_POINT('Ctrl Pts',(8.13178807675716,35.5062499998685,5.90808986649102));
#286077=CARTESIAN_POINT('Ctrl Pts',(10.0514428414941,35.6562499998679,3.2659117547607));
#286078=CARTESIAN_POINT('Ctrl Pts',(10.0514428414941,35.8062499998673,-1.23094673026484E-15));
#286079=CARTESIAN_POINT('Ctrl Pts',(10.0514428414941,35.9562499998667,-3.26591175476071));
#286080=CARTESIAN_POINT('Ctrl Pts',(8.13178807675716,36.1062499998661,-5.90808986649102));
#286081=CARTESIAN_POINT('Ctrl Pts',(6.21213331202018,36.2562499998655,-8.55026797822134));
#286082=CARTESIAN_POINT('Ctrl Pts',(3.10606665601007,36.4062499998649,-9.5594902125713));
#286083=CARTESIAN_POINT('Ctrl Pts',(-3.41776277664299E-14,36.5562499998642,
-10.5687124469213));
#286084=CARTESIAN_POINT('Ctrl Pts',(-3.10606665601014,36.7062499998636,
-9.5594902125713));
#286085=CARTESIAN_POINT('Ctrl Pts',(-6.21213331202025,36.856249999863,-8.55026797822134));
#286086=CARTESIAN_POINT('Ctrl Pts',(-8.13178807675722,37.0062499998624,
-5.90808986649102));
#286087=CARTESIAN_POINT('Ctrl Pts',(-10.0514428414942,37.1562499998618,
-3.2659117547607));
#286088=CARTESIAN_POINT('Ctrl Pts',(-10.0514428414942,37.3062499998613,
2.46189346052968E-15));
#286089=CARTESIAN_POINT('Ctrl Pts',(-10.0514428414942,37.4562499998606,
3.26591175476071));
#286090=CARTESIAN_POINT('Ctrl Pts',(-8.13178807675722,37.60624999986,5.90808986649102));
#286091=CARTESIAN_POINT('Ctrl Pts',(-6.21213331202025,37.7562499998594,
8.55026797822134));
#286092=CARTESIAN_POINT('Ctrl Pts',(-3.10606665601014,37.9062499998588,
9.5594902125713));
#286093=CARTESIAN_POINT('Ctrl Pts',(-3.24528944284146E-14,38.0562499998583,
10.5687124469213));
#286094=CARTESIAN_POINT('Ctrl Pts',(3.10606665601007,38.2062499998577,9.5594902125713));
#286095=CARTESIAN_POINT('Ctrl Pts',(6.21213331202018,38.3562499998571,8.55026797822134));
#286096=CARTESIAN_POINT('Ctrl Pts',(8.13178807675716,38.5062499998565,5.90808986649102));
#286097=CARTESIAN_POINT('Ctrl Pts',(10.0514428414941,38.6562499998559,3.2659117547607));
#286098=CARTESIAN_POINT('Ctrl Pts',(10.0514428414941,38.8062499998553,-1.23094673026484E-15));
#286099=CARTESIAN_POINT('Ctrl Pts',(10.0514428414941,38.9562499998547,-3.26591175476071));
#286100=CARTESIAN_POINT('Ctrl Pts',(8.13178807675715,39.1062499998541,-5.90808986649102));
#286101=CARTESIAN_POINT('Ctrl Pts',(6.21213331202018,39.2562499998535,-8.55026797822134));
#286102=CARTESIAN_POINT('Ctrl Pts',(3.10606665601007,39.4062499998529,-9.5594902125713));
#286103=CARTESIAN_POINT('Ctrl Pts',(-3.59053370380917E-14,39.5562499998523,
-10.5687124469213));
#286104=CARTESIAN_POINT('Ctrl Pts',(-3.10606665601014,39.7062499998516,
-9.5594902125713));
#286105=CARTESIAN_POINT('Ctrl Pts',(-6.21213331202025,39.856249999851,-8.55026797822134));
#286106=CARTESIAN_POINT('Ctrl Pts',(-8.13178807675723,40.0062499998505,
-5.90808986649102));
#286107=CARTESIAN_POINT('Ctrl Pts',(-10.0514428414942,40.1562499998499,
-3.2659117547607));
#286108=CARTESIAN_POINT('Ctrl Pts',(-10.0514428414942,40.3062499998493,
2.46189346052968E-15));
#286109=CARTESIAN_POINT('Ctrl Pts',(-10.0514428414942,40.4562499998487,
3.26591175476071));
#286110=CARTESIAN_POINT('Ctrl Pts',(-8.13178807675723,40.606249999848,5.90808986649102));
#286111=CARTESIAN_POINT('Ctrl Pts',(-6.21213331202025,40.7562499998475,
8.55026797822134));
#286112=CARTESIAN_POINT('Ctrl Pts',(-3.10606665601014,40.9062499998468,
9.5594902125713));
#286113=CARTESIAN_POINT('Ctrl Pts',(-3.41806037000764E-14,41.0562499998463,
10.5687124469213));
#286114=CARTESIAN_POINT('Ctrl Pts',(3.10606665601007,41.2062499998457,9.5594902125713));
#286115=CARTESIAN_POINT('Ctrl Pts',(6.21213331202018,41.3562499998451,8.55026797822134));
#286116=CARTESIAN_POINT('Ctrl Pts',(8.13178807675715,41.5062499998444,5.90808986649102));
#286117=CARTESIAN_POINT('Ctrl Pts',(10.0514428414941,41.6562499998439,3.2659117547607));
#286118=CARTESIAN_POINT('Ctrl Pts',(10.0514428414941,41.8062499998433,-1.23094673026484E-15));
#286119=CARTESIAN_POINT('Ctrl Pts',(10.0514428414941,41.9562499998427,-3.26591175476071));
#286120=CARTESIAN_POINT('Ctrl Pts',(8.13178807675715,42.1062499998421,-5.90808986649102));
#286121=CARTESIAN_POINT('Ctrl Pts',(6.21213331202018,42.2562499998414,-8.55026797822134));
#286122=CARTESIAN_POINT('Ctrl Pts',(3.10606665601007,42.4062499998408,-9.5594902125713));
#286123=CARTESIAN_POINT('Ctrl Pts',(-3.76330463097535E-14,42.5562499998402,
-10.5687124469213));
#286124=CARTESIAN_POINT('Ctrl Pts',(-3.10606665601015,42.7062499998396,
-9.5594902125713));
#286125=CARTESIAN_POINT('Ctrl Pts',(-6.21213331202025,42.8562499998391,
-8.55026797822134));
#286126=CARTESIAN_POINT('Ctrl Pts',(-8.13178807675723,43.0062499998385,
-5.90808986649102));
#286127=CARTESIAN_POINT('Ctrl Pts',(-10.0514428414942,43.1562499998379,
-3.2659117547607));
#286128=CARTESIAN_POINT('Ctrl Pts',(-10.0514428414942,43.3062499998373,
2.46189346052968E-15));
#286129=CARTESIAN_POINT('Ctrl Pts',(-10.0514428414942,43.4562499998366,
3.26591175476071));
#286130=CARTESIAN_POINT('Ctrl Pts',(-8.13178807675723,43.6062499998361,
5.90808986649102));
#286131=CARTESIAN_POINT('Ctrl Pts',(-6.21213331202025,43.7562499998354,
8.55026797822134));
#286132=CARTESIAN_POINT('Ctrl Pts',(-3.10606665601014,43.9062499998348,
9.5594902125713));
#286133=CARTESIAN_POINT('Ctrl Pts',(-3.59083129717383E-14,44.0562499998343,
10.5687124469213));
#286134=CARTESIAN_POINT('Ctrl Pts',(3.10606665601007,44.2062499998337,9.5594902125713));
#286135=CARTESIAN_POINT('Ctrl Pts',(6.21213331202018,44.3562499998331,8.55026797822134));
#286136=CARTESIAN_POINT('Ctrl Pts',(8.13178807675715,44.5062499998324,5.90808986649102));
#286137=CARTESIAN_POINT('Ctrl Pts',(10.0514428414941,44.6562499998319,3.2659117547607));
#286138=CARTESIAN_POINT('Ctrl Pts',(10.0514428414941,44.8062499998313,-1.23094673026484E-15));
#286139=CARTESIAN_POINT('Ctrl Pts',(10.0514428414941,44.9562499998307,-3.26591175476071));
#286140=CARTESIAN_POINT('Ctrl Pts',(8.13178807675715,45.1062499998301,-5.90808986649102));
#286141=CARTESIAN_POINT('Ctrl Pts',(6.21213331202018,45.2562499998295,-8.55026797822134));
#286142=CARTESIAN_POINT('Ctrl Pts',(3.10606665601007,45.4062499998289,-9.5594902125713));
#286143=CARTESIAN_POINT('Ctrl Pts',(-3.93607555814154E-14,45.5562499998283,
-10.5687124469213));
#286144=CARTESIAN_POINT('Ctrl Pts',(-3.10606665601015,45.7062499998276,
-9.5594902125713));
#286145=CARTESIAN_POINT('Ctrl Pts',(-6.21213331202026,45.856249999827,-8.55026797822134));
#286146=CARTESIAN_POINT('Ctrl Pts',(-8.13178807675723,46.0062499998265,
-5.90808986649102));
#286147=CARTESIAN_POINT('Ctrl Pts',(-10.0514428414942,46.1562499998259,
-3.2659117547607));
#286148=CARTESIAN_POINT('Ctrl Pts',(-10.0514428414942,46.3062499998252,
2.46189346052968E-15));
#286149=CARTESIAN_POINT('Ctrl Pts',(-10.0514428414942,46.4562499998247,
3.26591175476071));
#286150=CARTESIAN_POINT('Ctrl Pts',(-8.13178807675723,46.606249999824,5.90808986649102));
#286151=CARTESIAN_POINT('Ctrl Pts',(-6.21213331202025,46.7562499998235,
8.55026797822134));
#286152=CARTESIAN_POINT('Ctrl Pts',(-3.10606665601015,46.9062499998228,
9.5594902125713));
#286153=CARTESIAN_POINT('Ctrl Pts',(-3.76360222434001E-14,47.0562499998223,
10.5687124469213));
#286154=CARTESIAN_POINT('Ctrl Pts',(3.10606665601007,47.2062499998217,9.5594902125713));
#286155=CARTESIAN_POINT('Ctrl Pts',(6.21213331202018,47.3562499998211,8.55026797822134));
#286156=CARTESIAN_POINT('Ctrl Pts',(8.13178807675715,47.5062499998204,5.90808986649102));
#286157=CARTESIAN_POINT('Ctrl Pts',(10.0514428414941,47.6562499998198,3.2659117547607));
#286158=CARTESIAN_POINT('Ctrl Pts',(10.0514428414941,47.8062499998193,-1.23094673026484E-15));
#286159=CARTESIAN_POINT('Ctrl Pts',(10.0514428414941,47.9562499998186,-3.26591175476071));
#286160=CARTESIAN_POINT('Ctrl Pts',(8.13178807675715,48.1062499998181,-5.90808986649102));
#286161=CARTESIAN_POINT('Ctrl Pts',(6.21213331202017,48.2562499998174,-8.55026797822134));
#286162=CARTESIAN_POINT('Ctrl Pts',(3.10606665601007,48.4062499998169,-9.5594902125713));
#286163=CARTESIAN_POINT('Ctrl Pts',(-4.10884648530772E-14,48.5562499998163,
-10.5687124469213));
#286164=CARTESIAN_POINT('Ctrl Pts',(-3.10606665601015,48.7062499998157,
-9.5594902125713));
#286165=CARTESIAN_POINT('Ctrl Pts',(-6.21213331202026,48.8562499998151,
-8.55026797822134));
#286166=CARTESIAN_POINT('Ctrl Pts',(-8.13178807675723,49.0062499998145,
-5.90808986649102));
#286167=CARTESIAN_POINT('Ctrl Pts',(-10.0514428414942,49.1562499998138,
-3.2659117547607));
#286168=CARTESIAN_POINT('Ctrl Pts',(-10.0514428414942,49.3062499998132,
2.46189346052968E-15));
#286169=CARTESIAN_POINT('Ctrl Pts',(-10.0514428414942,49.4562499998126,
3.26591175476071));
#286170=CARTESIAN_POINT('Ctrl Pts',(-8.13178807675723,49.6062499998121,
5.90808986649102));
#286171=CARTESIAN_POINT('Ctrl Pts',(-6.21213331202026,49.7562499998114,
8.55026797822134));
#286172=CARTESIAN_POINT('Ctrl Pts',(-3.10606665601015,49.9062499998109,
9.5594902125713));
#286173=CARTESIAN_POINT('Ctrl Pts',(-3.9363731515062E-14,50.0562499998103,
10.5687124469213));
#286174=CARTESIAN_POINT('Ctrl Pts',(3.10606665601007,50.2062499998097,9.5594902125713));
#286175=CARTESIAN_POINT('Ctrl Pts',(6.21213331202017,50.3562499998091,8.55026797822134));
#286176=CARTESIAN_POINT('Ctrl Pts',(8.13178807675715,50.5062499998085,5.90808986649102));
#286177=CARTESIAN_POINT('Ctrl Pts',(10.0514428414941,50.6562499998078,3.2659117547607));
#286178=CARTESIAN_POINT('Ctrl Pts',(10.0514428414941,50.8062499998072,-1.23094673026484E-15));
#286179=CARTESIAN_POINT('Ctrl Pts',(10.0514428414941,50.9562499998067,-3.26591175476071));
#286180=CARTESIAN_POINT('Ctrl Pts',(8.13178807675715,51.1062499998061,-5.90808986649102));
#286181=CARTESIAN_POINT('Ctrl Pts',(6.21213331202017,51.2562499998055,-8.55026797822134));
#286182=CARTESIAN_POINT('Ctrl Pts',(3.10606665601006,51.4062499998048,-9.5594902125713));
#286183=CARTESIAN_POINT('Ctrl Pts',(-4.2816174124739E-14,51.5562499998043,
-10.5687124469213));
#286184=CARTESIAN_POINT('Ctrl Pts',(-3.10606665601015,51.7062499998037,
-9.5594902125713));
#286185=CARTESIAN_POINT('Ctrl Pts',(-6.21213331202026,51.856249999803,-8.55026797822134));
#286186=CARTESIAN_POINT('Ctrl Pts',(-8.13178807675723,52.0062499998025,
-5.90808986649102));
#286187=CARTESIAN_POINT('Ctrl Pts',(-10.0514428414942,52.1562499998019,
-3.2659117547607));
#286188=CARTESIAN_POINT('Ctrl Pts',(-10.0514428414942,52.3062499998012,
2.46189346052968E-15));
#286189=CARTESIAN_POINT('Ctrl Pts',(-10.0514428414942,52.4562499998006,
3.26591175476071));
#286190=CARTESIAN_POINT('Ctrl Pts',(-8.13178807675723,52.6062499998,5.90808986649102));
#286191=CARTESIAN_POINT('Ctrl Pts',(-6.21213331202026,52.7562499997994,
8.55026797822134));
#286192=CARTESIAN_POINT('Ctrl Pts',(-3.10606665601015,52.9062499997988,
9.5594902125713));
#286193=CARTESIAN_POINT('Ctrl Pts',(-4.10914407867238E-14,53.0562499997983,
10.5687124469213));
#286194=CARTESIAN_POINT('Ctrl Pts',(3.10606665601007,53.2062499997976,9.5594902125713));
#286195=CARTESIAN_POINT('Ctrl Pts',(6.21213331202017,53.3562499997971,8.55026797822134));
#286196=CARTESIAN_POINT('Ctrl Pts',(8.13178807675715,53.5062499997965,5.90808986649102));
#286197=CARTESIAN_POINT('Ctrl Pts',(10.0514428414941,53.6562499997959,3.2659117547607));
#286198=CARTESIAN_POINT('Ctrl Pts',(10.0514428414941,53.8062499997953,-1.23094673026484E-15));
#286199=CARTESIAN_POINT('Ctrl Pts',(10.0514428414941,53.9562499997946,-3.26591175476071));
#286200=CARTESIAN_POINT('Ctrl Pts',(8.13178807675714,54.106249999794,-5.90808986649102));
#286201=CARTESIAN_POINT('Ctrl Pts',(6.21213331202017,54.2562499997934,-8.55026797822134));
#286202=CARTESIAN_POINT('Ctrl Pts',(3.10606665601006,54.4062499997928,-9.5594902125713));
#286203=CARTESIAN_POINT('Ctrl Pts',(-4.45438833964009E-14,54.5562499997923,
-10.5687124469213));
#286204=CARTESIAN_POINT('Ctrl Pts',(-3.10606665601015,54.7062499997917,
-9.5594902125713));
#286205=CARTESIAN_POINT('Ctrl Pts',(-6.21213331202026,54.856249999791,-8.55026797822134));
#286206=CARTESIAN_POINT('Ctrl Pts',(-8.13178807675724,55.0062499997905,
-5.90808986649102));
#286207=CARTESIAN_POINT('Ctrl Pts',(-10.0514428414942,55.1562499997898,
-3.2659117547607));
#286208=CARTESIAN_POINT('Ctrl Pts',(-10.0514428414942,55.3062499997893,
2.46189346052968E-15));
#286209=CARTESIAN_POINT('Ctrl Pts',(-10.0514428414942,55.4562499997886,
3.26591175476071));
#286210=CARTESIAN_POINT('Ctrl Pts',(-8.13178807675724,55.606249999788,5.90808986649102));
#286211=CARTESIAN_POINT('Ctrl Pts',(-6.21213331202026,55.7562499997874,
8.55026797822134));
#286212=CARTESIAN_POINT('Ctrl Pts',(-3.10606665601015,55.9062499997869,
9.5594902125713));
#286213=CARTESIAN_POINT('Ctrl Pts',(-4.28191500583856E-14,56.0562499997862,
10.5687124469213));
#286214=CARTESIAN_POINT('Ctrl Pts',(3.10606665601006,56.2062499997857,9.5594902125713));
#286215=CARTESIAN_POINT('Ctrl Pts',(6.21213331202017,56.356249999785,8.55026797822134));
#286216=CARTESIAN_POINT('Ctrl Pts',(8.13178807675714,56.5062499997845,5.90808986649102));
#286217=CARTESIAN_POINT('Ctrl Pts',(10.0514428414941,56.6562499997839,3.2659117547607));
#286218=CARTESIAN_POINT('Ctrl Pts',(10.0514428414941,56.8062499997833,-1.23094673026484E-15));
#286219=CARTESIAN_POINT('Ctrl Pts',(10.0514428414941,56.9562499997827,-3.26591175476071));
#286220=CARTESIAN_POINT('Ctrl Pts',(8.13178807675714,57.1062499997821,-5.90808986649102));
#286221=CARTESIAN_POINT('Ctrl Pts',(6.21213331202017,57.2562499997814,-8.55026797822134));
#286222=CARTESIAN_POINT('Ctrl Pts',(3.10606665601006,57.4062499997808,-9.5594902125713));
#286223=CARTESIAN_POINT('Ctrl Pts',(-4.62715926680627E-14,57.5562499997802,
-10.5687124469213));
#286224=CARTESIAN_POINT('Ctrl Pts',(-3.10606665601015,57.7062499997797,
-9.5594902125713));
#286225=CARTESIAN_POINT('Ctrl Pts',(-6.21213331202026,57.856249999779,-8.55026797822134));
#286226=CARTESIAN_POINT('Ctrl Pts',(-8.13178807675724,58.0062499997784,
-5.90808986649102));
#286227=CARTESIAN_POINT('Ctrl Pts',(-10.0514428414942,58.1562499997778,
-3.2659117547607));
#286228=CARTESIAN_POINT('Ctrl Pts',(-10.0514428414942,58.3062499997773,
2.46189346052968E-15));
#286229=CARTESIAN_POINT('Ctrl Pts',(-10.0514428414942,58.4562499997766,
3.26591175476071));
#286230=CARTESIAN_POINT('Ctrl Pts',(-8.13178807675724,58.6062499997761,
5.90808986649102));
#286231=CARTESIAN_POINT('Ctrl Pts',(-6.21213331202026,58.7562499997754,
8.55026797822134));
#286232=CARTESIAN_POINT('Ctrl Pts',(-3.10606665601015,58.9062499997749,
9.5594902125713));
#286233=CARTESIAN_POINT('Ctrl Pts',(-4.45468593300475E-14,59.0562499997743,
10.5687124469213));
#286234=CARTESIAN_POINT('Ctrl Pts',(3.10606665601006,59.2062499997736,9.5594902125713));
#286235=CARTESIAN_POINT('Ctrl Pts',(6.21213331202017,59.356249999773,8.55026797822134));
#286236=CARTESIAN_POINT('Ctrl Pts',(8.13178807675714,59.5062499997725,5.90808986649102));
#286237=CARTESIAN_POINT('Ctrl Pts',(10.0514428414941,59.6562499997718,3.2659117547607));
#286238=CARTESIAN_POINT('Ctrl Pts',(10.0514428414941,59.8062499997713,-1.23094673026484E-15));
#286239=CARTESIAN_POINT('Ctrl Pts',(10.0514428414941,59.9562499997706,-3.26591175476071));
#286240=CARTESIAN_POINT('Ctrl Pts',(8.13178807675714,60.10624999977,-5.90808986649102));
#286241=CARTESIAN_POINT('Ctrl Pts',(6.21213331202017,60.2562499997694,-8.55026797822134));
#286242=CARTESIAN_POINT('Ctrl Pts',(3.10606665601006,60.4062499997689,-9.5594902125713));
#286243=CARTESIAN_POINT('Ctrl Pts',(-4.79993019397246E-14,60.5562499997682,
-10.5687124469213));
#286244=CARTESIAN_POINT('Ctrl Pts',(-3.10606665601016,60.7062499997676,
-9.5594902125713));
#286245=CARTESIAN_POINT('Ctrl Pts',(-6.21213331202026,60.856249999767,-8.55026797822134));
#286246=CARTESIAN_POINT('Ctrl Pts',(-8.13178807675724,61.0062499997664,
-5.90808986649102));
#286247=CARTESIAN_POINT('Ctrl Pts',(-10.0514428414942,61.1562499997658,
-3.2659117547607));
#286248=CARTESIAN_POINT('Ctrl Pts',(-10.0514428414942,61.3062499997652,
2.46189346052968E-15));
#286249=CARTESIAN_POINT('Ctrl Pts',(-10.0514428414942,61.4562499997646,
3.26591175476071));
#286250=CARTESIAN_POINT('Ctrl Pts',(-8.13178807675724,61.6062499997641,
5.90808986649102));
#286251=CARTESIAN_POINT('Ctrl Pts',(-6.21213331202026,61.7562499997634,
8.55026797822134));
#286252=CARTESIAN_POINT('Ctrl Pts',(-3.10606665601015,61.9062499997628,
9.5594902125713));
#286253=CARTESIAN_POINT('Ctrl Pts',(-4.62745686017093E-14,62.0562499997622,
10.5687124469213));
#286254=CARTESIAN_POINT('Ctrl Pts',(3.10606665601006,62.2062499997617,9.5594902125713));
#286255=CARTESIAN_POINT('Ctrl Pts',(6.21213331202017,62.356249999761,8.55026797822134));
#286256=CARTESIAN_POINT('Ctrl Pts',(8.13178807675714,62.5062499997605,5.90808986649102));
#286257=CARTESIAN_POINT('Ctrl Pts',(10.0514428414941,62.6562499997599,3.2659117547607));
#286258=CARTESIAN_POINT('Ctrl Pts',(10.0514428414941,62.8062499997593,-1.23094673026484E-15));
#286259=CARTESIAN_POINT('Ctrl Pts',(10.0514428414941,62.9562499997587,-3.26591175476071));
#286260=CARTESIAN_POINT('Ctrl Pts',(8.13178807675714,63.1062499997581,-5.90808986649102));
#286261=CARTESIAN_POINT('Ctrl Pts',(6.21213331202017,63.2562499997575,-8.55026797822134));
#286262=CARTESIAN_POINT('Ctrl Pts',(3.10606665601006,63.4062499997568,-9.5594902125713));
#286263=CARTESIAN_POINT('Ctrl Pts',(-4.97270112113864E-14,63.5562499997562,
-10.5687124469213));
#286264=CARTESIAN_POINT('Ctrl Pts',(-3.10606665601016,63.7062499997556,
-9.5594902125713));
#286265=CARTESIAN_POINT('Ctrl Pts',(-6.21213331202027,63.8562499997551,
-8.55026797822134));
#286266=CARTESIAN_POINT('Ctrl Pts',(-8.13178807675724,64.0062499997544,
-5.90808986649102));
#286267=CARTESIAN_POINT('Ctrl Pts',(-10.0514428414942,64.1562499997538,
-3.2659117547607));
#286268=CARTESIAN_POINT('Ctrl Pts',(-10.0514428414942,64.3062499997532,
2.46189346052968E-15));
#286269=CARTESIAN_POINT('Ctrl Pts',(-10.0514428414942,64.4562499997526,
3.26591175476071));
#286270=CARTESIAN_POINT('Ctrl Pts',(-8.13178807675724,64.606249999752,5.90808986649102));
#286271=CARTESIAN_POINT('Ctrl Pts',(-6.21213331202026,64.7562499997514,
8.55026797822134));
#286272=CARTESIAN_POINT('Ctrl Pts',(-3.10606665601016,64.9062499997509,
9.5594902125713));
#286273=CARTESIAN_POINT('Ctrl Pts',(-4.80022778733711E-14,65.0562499997502,
10.5687124469213));
#286274=CARTESIAN_POINT('Ctrl Pts',(3.10606665601006,65.2062499997497,9.5594902125713));
#286275=CARTESIAN_POINT('Ctrl Pts',(6.21213331202017,65.3562499997491,8.55026797822134));
#286276=CARTESIAN_POINT('Ctrl Pts',(8.13178807675714,65.5062499997484,5.90808986649102));
#286277=CARTESIAN_POINT('Ctrl Pts',(10.0514428414941,65.6562499997479,3.2659117547607));
#286278=CARTESIAN_POINT('Ctrl Pts',(10.0514428414941,65.8062499997473,-1.23094673026484E-15));
#286279=CARTESIAN_POINT('Ctrl Pts',(10.0514428414941,65.9562499997467,-3.26591175476071));
#286280=CARTESIAN_POINT('Ctrl Pts',(8.13178807675714,66.1062499997461,-5.90808986649102));
#286281=CARTESIAN_POINT('Ctrl Pts',(6.21213331202016,66.2562499997454,-8.55026797822134));
#286282=CARTESIAN_POINT('Ctrl Pts',(3.10606665601006,66.4062499997449,-9.5594902125713));
#286283=CARTESIAN_POINT('Ctrl Pts',(-5.14547204830482E-14,66.5562499997443,
-10.5687124469213));
#286284=CARTESIAN_POINT('Ctrl Pts',(-3.10606665601016,66.7062499997436,
-9.5594902125713));
#286285=CARTESIAN_POINT('Ctrl Pts',(-6.21213331202027,66.8562499997431,
-8.55026797822134));
#286286=CARTESIAN_POINT('Ctrl Pts',(-8.13178807675724,67.0062499997424,
-5.90808986649102));
#286287=CARTESIAN_POINT('Ctrl Pts',(-10.0514428414942,67.1562499997418,
-3.2659117547607));
#286288=CARTESIAN_POINT('Ctrl Pts',(-10.0514428414942,67.3062499997412,
2.46189346052968E-15));
#286289=CARTESIAN_POINT('Ctrl Pts',(-10.0514428414942,67.4562499997406,
3.26591175476071));
#286290=CARTESIAN_POINT('Ctrl Pts',(-8.13178807675724,67.60624999974,5.90808986649102));
#286291=CARTESIAN_POINT('Ctrl Pts',(-6.21213331202027,67.7562499997395,
8.55026797822134));
#286292=CARTESIAN_POINT('Ctrl Pts',(-3.10606665601016,67.9062499997388,
9.5594902125713));
#286293=CARTESIAN_POINT('Ctrl Pts',(-4.9729987145033E-14,68.0562499997382,
10.5687124469213));
#286294=CARTESIAN_POINT('Ctrl Pts',(3.10606665601006,68.2062499997377,9.5594902125713));
#286295=CARTESIAN_POINT('Ctrl Pts',(6.21213331202017,68.356249999737,8.55026797822134));
#286296=CARTESIAN_POINT('Ctrl Pts',(8.13178807675714,68.5062499997365,5.90808986649102));
#286297=CARTESIAN_POINT('Ctrl Pts',(10.0514428414941,68.6562499997358,3.2659117547607));
#286298=CARTESIAN_POINT('Ctrl Pts',(10.0514428414941,68.8062499997353,-1.23094673026484E-15));
#286299=CARTESIAN_POINT('Ctrl Pts',(10.0514428414941,68.9562499997347,-3.26591175476071));
#286300=CARTESIAN_POINT('Ctrl Pts',(8.13178807675714,69.1062499997341,-5.90808986649102));
#286301=CARTESIAN_POINT('Ctrl Pts',(6.21213331202016,69.2562499997335,-8.55026797822134));
#286302=CARTESIAN_POINT('Ctrl Pts',(3.10606665601005,69.4062499997329,-9.5594902125713));
#286303=CARTESIAN_POINT('Ctrl Pts',(-5.31824297547101E-14,69.5562499997323,
-10.5687124469213));
#286304=CARTESIAN_POINT('Ctrl Pts',(-3.10606665601016,69.7062499997317,
-9.5594902125713));
#286305=CARTESIAN_POINT('Ctrl Pts',(-6.21213331202027,69.856249999731,-8.55026797822134));
#286306=CARTESIAN_POINT('Ctrl Pts',(-8.13178807675724,70.0062499997304,
-5.90808986649102));
#286307=CARTESIAN_POINT('Ctrl Pts',(-10.0514428414942,70.1562499997298,
-3.2659117547607));
#286308=CARTESIAN_POINT('Ctrl Pts',(-10.0514428414942,70.3062499997292,
2.46189346052968E-15));
#286309=CARTESIAN_POINT('Ctrl Pts',(-10.0514428414942,70.4562499997286,
3.26591175476071));
#286310=CARTESIAN_POINT('Ctrl Pts',(-8.13178807675724,70.606249999728,5.90808986649102));
#286311=CARTESIAN_POINT('Ctrl Pts',(-6.21213331202027,70.7562499997274,
8.55026797822134));
#286312=CARTESIAN_POINT('Ctrl Pts',(-3.10606665601016,70.9062499997269,
9.5594902125713));
#286313=CARTESIAN_POINT('Ctrl Pts',(-5.14576964166948E-14,71.0562499997262,
10.5687124469213));
#286314=CARTESIAN_POINT('Ctrl Pts',(3.10606665601006,71.2062499997256,9.5594902125713));
#286315=CARTESIAN_POINT('Ctrl Pts',(6.21213331202016,71.3562499997251,8.55026797822134));
#286316=CARTESIAN_POINT('Ctrl Pts',(8.13178807675714,71.5062499997244,5.90808986649102));
#286317=CARTESIAN_POINT('Ctrl Pts',(10.0514428414941,71.6562499997239,3.2659117547607));
#286318=CARTESIAN_POINT('Ctrl Pts',(10.0514428414941,71.8062499997232,-1.23094673026484E-15));
#286319=CARTESIAN_POINT('Ctrl Pts',(10.0514428414941,71.9562499997227,-3.26591175476071));
#286320=CARTESIAN_POINT('Ctrl Pts',(8.13178807675713,72.1062499997221,-5.90808986649102));
#286321=CARTESIAN_POINT('Ctrl Pts',(6.21213331202016,72.2562499997215,-8.55026797822134));
#286322=CARTESIAN_POINT('Ctrl Pts',(3.10606665601005,72.4062499997209,-9.5594902125713));
#286323=CARTESIAN_POINT('Ctrl Pts',(-5.49101390263719E-14,72.5562499997203,
-10.5687124469213));
#286324=CARTESIAN_POINT('Ctrl Pts',(-3.10606665601016,72.7062499997197,
-9.5594902125713));
#286325=CARTESIAN_POINT('Ctrl Pts',(-6.21213331202027,72.8562499997191,
-8.55026797822134));
#286326=CARTESIAN_POINT('Ctrl Pts',(-8.13178807675725,73.0062499997184,
-5.90808986649102));
#286327=CARTESIAN_POINT('Ctrl Pts',(-10.0514428414942,73.1562499997178,
-3.2659117547607));
#286328=CARTESIAN_POINT('Ctrl Pts',(-10.0514428414942,73.3062499997172,
2.46189346052968E-15));
#286329=CARTESIAN_POINT('Ctrl Pts',(-10.0514428414942,73.4562499997166,
3.26591175476071));
#286330=CARTESIAN_POINT('Ctrl Pts',(-8.13178807675725,73.606249999716,5.90808986649102));
#286331=CARTESIAN_POINT('Ctrl Pts',(-6.21213331202027,73.7562499997155,
8.55026797822134));
#286332=CARTESIAN_POINT('Ctrl Pts',(-3.10606665601016,73.9062499997148,
9.5594902125713));
#286333=CARTESIAN_POINT('Ctrl Pts',(-5.31854056883567E-14,74.0562499997143,
10.5687124469213));
#286334=CARTESIAN_POINT('Ctrl Pts',(3.10606665601005,74.2062499997136,9.5594902125713));
#286335=CARTESIAN_POINT('Ctrl Pts',(6.21213331202016,74.3562499997131,8.55026797822134));
#286336=CARTESIAN_POINT('Ctrl Pts',(8.13178807675713,74.5062499997125,5.90808986649102));
#286337=CARTESIAN_POINT('Ctrl Pts',(10.0514428414941,74.6562499997118,3.2659117547607));
#286338=CARTESIAN_POINT('Ctrl Pts',(10.0514428414941,74.8062499997113,-1.23094673026484E-15));
#286339=CARTESIAN_POINT('Ctrl Pts',(10.0514428414941,74.9562499997106,-3.26591175476071));
#286340=CARTESIAN_POINT('Ctrl Pts',(8.13178807675713,75.10624999971,-5.90808986649102));
#286341=CARTESIAN_POINT('Ctrl Pts',(6.21213331202016,75.2562499997094,-8.55026797822134));
#286342=CARTESIAN_POINT('Ctrl Pts',(3.10606665601005,75.4062499997088,-9.5594902125713));
#286343=CARTESIAN_POINT('Ctrl Pts',(-5.66378482980338E-14,75.5562499997083,
-10.5687124469213));
#286344=CARTESIAN_POINT('Ctrl Pts',(-3.10606665601016,75.7062499997077,
-9.5594902125713));
#286345=CARTESIAN_POINT('Ctrl Pts',(-6.21213331202027,75.856249999707,-8.55026797822134));
#286346=CARTESIAN_POINT('Ctrl Pts',(-8.13178807675725,76.0062499997065,
-5.90808986649102));
#286347=CARTESIAN_POINT('Ctrl Pts',(-10.0514428414942,76.1562499997058,
-3.2659117547607));
#286348=CARTESIAN_POINT('Ctrl Pts',(-10.0514428414942,76.3062499997052,
2.46189346052968E-15));
#286349=CARTESIAN_POINT('Ctrl Pts',(-10.0514428414942,76.4562499997046,
3.26591175476071));
#286350=CARTESIAN_POINT('Ctrl Pts',(-8.13178807675725,76.606249999704,5.90808986649102));
#286351=CARTESIAN_POINT('Ctrl Pts',(-6.21213331202027,76.7562499997035,
8.55026797822134));
#286352=CARTESIAN_POINT('Ctrl Pts',(-3.10606665601016,76.9062499997029,
9.5594902125713));
#286353=CARTESIAN_POINT('Ctrl Pts',(-5.49131149600185E-14,77.0562499997022,
10.5687124469213));
#286354=CARTESIAN_POINT('Ctrl Pts',(3.10606665601005,77.2062499997016,9.5594902125713));
#286355=CARTESIAN_POINT('Ctrl Pts',(6.21213331202016,77.356249999701,8.55026797822134));
#286356=CARTESIAN_POINT('Ctrl Pts',(8.13178807675713,77.5062499997004,5.90808986649102));
#286357=CARTESIAN_POINT('Ctrl Pts',(10.0514428414941,77.6562499996998,3.2659117547607));
#286358=CARTESIAN_POINT('Ctrl Pts',(10.0514428414941,77.8062499996992,-1.23094673026484E-15));
#286359=CARTESIAN_POINT('Ctrl Pts',(10.0514428414941,77.9562499996987,-3.26591175476071));
#286360=CARTESIAN_POINT('Ctrl Pts',(8.13178807675713,78.1062499996981,-5.90808986649102));
#286361=CARTESIAN_POINT('Ctrl Pts',(6.21213331202016,78.2562499996974,-8.55026797822134));
#286362=CARTESIAN_POINT('Ctrl Pts',(3.10606665601005,78.4062499996969,-9.5594902125713));
#286363=CARTESIAN_POINT('Ctrl Pts',(-5.83655575696956E-14,78.5562499996963,
-10.5687124469213));
#286364=CARTESIAN_POINT('Ctrl Pts',(-3.10606665601017,78.7062499996957,
-9.5594902125713));
#286365=CARTESIAN_POINT('Ctrl Pts',(-6.21213331202028,78.8562499996951,
-8.55026797822134));
#286366=CARTESIAN_POINT('Ctrl Pts',(-8.13178807675725,79.0062499996944,
-5.90808986649102));
#286367=CARTESIAN_POINT('Ctrl Pts',(-10.0514428414942,79.1562499996939,
-3.2659117547607));
#286368=CARTESIAN_POINT('Ctrl Pts',(-10.0514428414942,79.3062499996932,
2.46189346052968E-15));
#286369=CARTESIAN_POINT('Ctrl Pts',(-10.0514428414942,79.4562499996926,
3.26591175476071));
#286370=CARTESIAN_POINT('Ctrl Pts',(-8.13178807675725,79.606249999692,5.90808986649102));
#286371=CARTESIAN_POINT('Ctrl Pts',(-6.21213331202027,79.7562499996915,
8.55026797822134));
#286372=CARTESIAN_POINT('Ctrl Pts',(-3.10606665601016,79.9062499996908,
9.5594902125713));
#286373=CARTESIAN_POINT('Ctrl Pts',(-5.66408242316803E-14,80.0562499996902,
10.5687124469213));
#286374=CARTESIAN_POINT('Ctrl Pts',(3.10606665601005,80.2062499996896,9.5594902125713));
#286375=CARTESIAN_POINT('Ctrl Pts',(6.21213331202016,80.356249999689,8.55026797822134));
#286376=CARTESIAN_POINT('Ctrl Pts',(8.13178807675713,80.5062499996884,5.90808986649102));
#286377=CARTESIAN_POINT('Ctrl Pts',(10.0514428414941,80.6562499996878,3.2659117547607));
#286378=CARTESIAN_POINT('Ctrl Pts',(10.0514428414941,80.8062499996873,-1.23094673026484E-15));
#286379=CARTESIAN_POINT('Ctrl Pts',(10.0514428414941,80.9562499996866,-3.26591175476071));
#286380=CARTESIAN_POINT('Ctrl Pts',(8.13178807675713,81.1062499996861,-5.90808986649102));
#286381=CARTESIAN_POINT('Ctrl Pts',(6.21213331202016,81.2562499996854,-8.55026797822134));
#286382=CARTESIAN_POINT('Ctrl Pts',(3.10606665601005,81.4062499996849,-9.5594902125713));
#286383=CARTESIAN_POINT('Ctrl Pts',(-6.00932668413574E-14,81.5562499996843,
-10.5687124469213));
#286384=CARTESIAN_POINT('Ctrl Pts',(-3.10606665601017,81.7062499996837,
-9.5594902125713));
#286385=CARTESIAN_POINT('Ctrl Pts',(-6.21213331202028,81.856249999683,-8.55026797822134));
#286386=CARTESIAN_POINT('Ctrl Pts',(-8.13178807675725,82.0062499996824,
-5.90808986649102));
#286387=CARTESIAN_POINT('Ctrl Pts',(-10.0514428414942,82.1562499996818,
-3.2659117547607));
#286388=CARTESIAN_POINT('Ctrl Pts',(-10.0514428414942,82.3062499996813,
2.46189346052968E-15));
#286389=CARTESIAN_POINT('Ctrl Pts',(-10.0514428414942,82.4562499996806,
3.26591175476071));
#286390=CARTESIAN_POINT('Ctrl Pts',(-8.13178807675725,82.60624999968,5.90808986649102));
#286391=CARTESIAN_POINT('Ctrl Pts',(-6.21213331202028,82.7562499996795,
8.55026797822134));
#286392=CARTESIAN_POINT('Ctrl Pts',(-3.10606665601017,82.9062499996789,
9.5594902125713));
#286393=CARTESIAN_POINT('Ctrl Pts',(-5.83685335033422E-14,83.0562499996782,
10.5687124469213));
#286394=CARTESIAN_POINT('Ctrl Pts',(3.10606665601005,83.2062499996776,9.5594902125713));
#286395=CARTESIAN_POINT('Ctrl Pts',(6.21213331202016,83.356249999677,8.55026797822134));
#286396=CARTESIAN_POINT('Ctrl Pts',(8.13178807675713,83.5062499996764,5.90808986649102));
#286397=CARTESIAN_POINT('Ctrl Pts',(10.0514428414941,83.6562499996759,3.2659117547607));
#286398=CARTESIAN_POINT('Ctrl Pts',(10.0514428414941,83.8062499996752,-1.23094673026484E-15));
#286399=CARTESIAN_POINT('Ctrl Pts',(10.0514428414941,83.9562499996747,-3.26591175476071));
#286400=CARTESIAN_POINT('Ctrl Pts',(8.13178807675713,84.106249999674,-5.90808986649102));
#286401=CARTESIAN_POINT('Ctrl Pts',(6.21213331202016,84.2562499996734,-8.55026797822134));
#286402=CARTESIAN_POINT('Ctrl Pts',(3.10606665601005,84.4062499996729,-9.5594902125713));
#286403=CARTESIAN_POINT('Ctrl Pts',(-6.18209761130193E-14,84.5562499996723,
-10.5687124469213));
#286404=CARTESIAN_POINT('Ctrl Pts',(-3.10606665601017,84.7062499996717,
-9.5594902125713));
#286405=CARTESIAN_POINT('Ctrl Pts',(-6.21213331202028,84.856249999671,-8.55026797822134));
#286406=CARTESIAN_POINT('Ctrl Pts',(-8.13178807675725,85.0062499996704,
-5.90808986649102));
#286407=CARTESIAN_POINT('Ctrl Pts',(-10.0514428414942,85.1562499996699,
-3.2659117547607));
#286408=CARTESIAN_POINT('Ctrl Pts',(-10.0514428414942,85.3062499996692,
2.46189346052968E-15));
#286409=CARTESIAN_POINT('Ctrl Pts',(-10.0514428414942,85.4562499996686,
3.26591175476071));
#286410=CARTESIAN_POINT('Ctrl Pts',(-8.13178807675725,85.606249999668,5.90808986649102));
#286411=CARTESIAN_POINT('Ctrl Pts',(-6.21213331202028,85.7562499996675,
8.55026797822134));
#286412=CARTESIAN_POINT('Ctrl Pts',(-3.10606665601017,85.9062499996669,
9.5594902125713));
#286413=CARTESIAN_POINT('Ctrl Pts',(-6.0096242775004E-14,86.0562499996662,
10.5687124469213));
#286414=CARTESIAN_POINT('Ctrl Pts',(3.10606665601005,86.2062499996657,9.5594902125713));
#286415=CARTESIAN_POINT('Ctrl Pts',(6.21213331202016,86.3562499996651,8.55026797822134));
#286416=CARTESIAN_POINT('Ctrl Pts',(8.13178807675713,86.5062499996644,5.90808986649102));
#286417=CARTESIAN_POINT('Ctrl Pts',(10.0514428414941,86.6562499996638,3.2659117547607));
#286418=CARTESIAN_POINT('Ctrl Pts',(10.0514428414941,86.8062499996633,-1.23094673026484E-15));
#286419=CARTESIAN_POINT('Ctrl Pts',(10.0514428414941,86.9562499996626,-3.26591175476071));
#286420=CARTESIAN_POINT('Ctrl Pts',(8.13178807675713,87.1062499996621,-5.90808986649102));
#286421=CARTESIAN_POINT('Ctrl Pts',(6.21213331202015,87.2562499996614,-8.55026797822134));
#286422=CARTESIAN_POINT('Ctrl Pts',(3.10606665601004,87.4062499996609,-9.5594902125713));
#286423=CARTESIAN_POINT('Ctrl Pts',(-6.35486853846811E-14,87.5562499996603,
-10.5687124469213));
#286424=CARTESIAN_POINT('Ctrl Pts',(-3.10606665601017,87.7062499996597,
-9.5594902125713));
#286425=CARTESIAN_POINT('Ctrl Pts',(-6.21213331202028,87.856249999659,-8.55026797822134));
#286426=CARTESIAN_POINT('Ctrl Pts',(-8.13178807675726,88.0062499996585,
-5.90808986649102));
#286427=CARTESIAN_POINT('Ctrl Pts',(-10.0514428414942,88.1562499996578,
-3.2659117547607));
#286428=CARTESIAN_POINT('Ctrl Pts',(-10.0514428414942,88.3062499996572,
2.46189346052968E-15));
#286429=CARTESIAN_POINT('Ctrl Pts',(-10.0514428414942,88.4562499996566,
3.26591175476071));
#286430=CARTESIAN_POINT('Ctrl Pts',(-8.13178807675726,88.6062499996561,
5.90808986649102));
#286431=CARTESIAN_POINT('Ctrl Pts',(-6.21213331202028,88.7562499996555,
8.55026797822134));
#286432=CARTESIAN_POINT('Ctrl Pts',(-3.10606665601017,88.9062499996548,
9.5594902125713));
#286433=CARTESIAN_POINT('Ctrl Pts',(-6.18239520466659E-14,89.0562499996542,
10.5687124469213));
#286434=CARTESIAN_POINT('Ctrl Pts',(3.10606665601005,89.2062499996537,9.5594902125713));
#286435=CARTESIAN_POINT('Ctrl Pts',(6.21213331202016,89.3562499996531,8.55026797822134));
#286436=CARTESIAN_POINT('Ctrl Pts',(8.13178807675713,89.5062499996525,5.90808986649102));
#286437=CARTESIAN_POINT('Ctrl Pts',(10.0514428414941,89.6562499996518,3.2659117547607));
#286438=CARTESIAN_POINT('Ctrl Pts',(10.0514428414941,89.8062499996512,-1.23094673026484E-15));
#286439=CARTESIAN_POINT('Ctrl Pts',(10.0514428414941,89.9562499996507,-3.26591175476071));
#286440=CARTESIAN_POINT('Ctrl Pts',(8.13178807675713,90.10624999965,-5.90808986649102));
#286441=CARTESIAN_POINT('Ctrl Pts',(6.21213331202015,90.2562499996494,-8.55026797822134));
#286442=CARTESIAN_POINT('Ctrl Pts',(3.10606665601004,90.4062499996488,-9.5594902125713));
#286443=CARTESIAN_POINT('Ctrl Pts',(-6.52763946563429E-14,90.5562499996483,
-10.5687124469213));
#286444=CARTESIAN_POINT('Ctrl Pts',(-3.10606665601017,90.7062499996476,
-9.5594902125713));
#286445=CARTESIAN_POINT('Ctrl Pts',(-6.21213331202028,90.856249999647,-8.55026797822134));
#286446=CARTESIAN_POINT('Ctrl Pts',(-8.13178807675726,91.0062499996464,
-5.90808986649102));
#286447=CARTESIAN_POINT('Ctrl Pts',(-10.0514428414942,91.1562499996458,
-3.2659117547607));
#286448=CARTESIAN_POINT('Ctrl Pts',(-10.0514428414942,91.3062499996452,
2.46189346052968E-15));
#286449=CARTESIAN_POINT('Ctrl Pts',(-10.0514428414942,91.4562499996446,
3.26591175476071));
#286450=CARTESIAN_POINT('Ctrl Pts',(-8.13178807675726,91.606249999644,5.90808986649102));
#286451=CARTESIAN_POINT('Ctrl Pts',(-6.21213331202028,91.7562499996434,
8.55026797822134));
#286452=CARTESIAN_POINT('Ctrl Pts',(-3.10606665601017,91.9062499996429,
9.5594902125713));
#286453=CARTESIAN_POINT('Ctrl Pts',(-6.35516613183277E-14,92.0562499996422,
10.5687124469213));
#286454=CARTESIAN_POINT('Ctrl Pts',(3.10606665601004,92.2062499996417,9.5594902125713));
#286455=CARTESIAN_POINT('Ctrl Pts',(6.21213331202015,92.3562499996411,8.55026797822134));
#286456=CARTESIAN_POINT('Ctrl Pts',(8.13178807675712,92.5062499996404,5.90808986649102));
#286457=CARTESIAN_POINT('Ctrl Pts',(10.0514428414941,92.6562499996398,3.2659117547607));
#286458=CARTESIAN_POINT('Ctrl Pts',(10.0514428414941,92.8062499996392,-1.23094673026484E-15));
#286459=CARTESIAN_POINT('Ctrl Pts',(10.0514428414941,92.9562499996387,-3.26591175476071));
#286460=CARTESIAN_POINT('Ctrl Pts',(8.13178807675712,93.1062499996381,-5.90808986649102));
#286461=CARTESIAN_POINT('Ctrl Pts',(6.21213331202015,93.2562499996374,-8.55026797822134));
#286462=CARTESIAN_POINT('Ctrl Pts',(3.10606665601004,93.4062499996369,-9.5594902125713));
#286463=CARTESIAN_POINT('Ctrl Pts',(-6.70041039280048E-14,93.5562499996362,
-10.5687124469213));
#286464=CARTESIAN_POINT('Ctrl Pts',(-3.10606665601018,93.7062499996357,
-9.5594902125713));
#286465=CARTESIAN_POINT('Ctrl Pts',(-6.21213331202028,93.856249999635,-8.55026797822134));
#286466=CARTESIAN_POINT('Ctrl Pts',(-8.13178807675726,94.0062499996344,
-5.90808986649102));
#286467=CARTESIAN_POINT('Ctrl Pts',(-10.0514428414942,94.1562499996338,
-3.2659117547607));
#286468=CARTESIAN_POINT('Ctrl Pts',(-10.0514428414942,94.3062499996333,
2.46189346052968E-15));
#286469=CARTESIAN_POINT('Ctrl Pts',(-10.0514428414942,94.4562499996326,
3.26591175476071));
#286470=CARTESIAN_POINT('Ctrl Pts',(-8.13178807675726,94.606249999632,5.90808986649102));
#286471=CARTESIAN_POINT('Ctrl Pts',(-6.21213331202028,94.7562499996315,
8.55026797822134));
#286472=CARTESIAN_POINT('Ctrl Pts',(-3.10606665601017,94.9062499996309,
9.5594902125713));
#286473=CARTESIAN_POINT('Ctrl Pts',(-6.52793705899895E-14,95.0562499996302,
10.5687124469213));
#286474=CARTESIAN_POINT('Ctrl Pts',(3.10606665601004,95.2062499996296,9.5594902125713));
#286475=CARTESIAN_POINT('Ctrl Pts',(6.21213331202015,95.3562499996291,8.55026797822134));
#286476=CARTESIAN_POINT('Ctrl Pts',(8.13178807675712,95.5062499996285,5.90808986649102));
#286477=CARTESIAN_POINT('Ctrl Pts',(10.0514428414941,95.6562499996278,3.2659117547607));
#286478=CARTESIAN_POINT('Ctrl Pts',(10.0514428414941,95.8062499996273,-1.23094673026484E-15));
#286479=CARTESIAN_POINT('Ctrl Pts',(10.0514428414941,95.9562499996266,-3.26591175476071));
#286480=CARTESIAN_POINT('Ctrl Pts',(8.13178807675712,96.1062499996261,-5.90808986649102));
#286481=CARTESIAN_POINT('Ctrl Pts',(6.21213331202015,96.2562499996255,-8.55026797822134));
#286482=CARTESIAN_POINT('Ctrl Pts',(3.10606665601004,96.4062499996248,-9.5594902125713));
#286483=CARTESIAN_POINT('Ctrl Pts',(-6.87318131996666E-14,96.5562499996243,
-10.5687124469213));
#286484=CARTESIAN_POINT('Ctrl Pts',(-3.10606665601018,96.7062499996236,
-9.5594902125713));
#286485=CARTESIAN_POINT('Ctrl Pts',(-6.21213331202028,96.856249999623,-8.55026797822134));
#286486=CARTESIAN_POINT('Ctrl Pts',(-8.13178807675726,97.0062499996224,
-5.90808986649102));
#286487=CARTESIAN_POINT('Ctrl Pts',(-10.0514428414942,97.1562499996218,
-3.2659117547607));
#286488=CARTESIAN_POINT('Ctrl Pts',(-10.0514428414942,97.3062499996212,
2.46189346052968E-15));
#286489=CARTESIAN_POINT('Ctrl Pts',(-10.0514428414942,97.4562499996206,
3.26591175476071));
#286490=CARTESIAN_POINT('Ctrl Pts',(-8.13178807675726,97.60624999962,5.90808986649102));
#286491=CARTESIAN_POINT('Ctrl Pts',(-6.21213331202028,97.7562499996195,
8.55026797822134));
#286492=CARTESIAN_POINT('Ctrl Pts',(-3.10606665601018,97.9062499996189,
9.5594902125713));
#286493=CARTESIAN_POINT('Ctrl Pts',(-6.70070798616514E-14,98.0562499996182,
10.5687124469213));
#286494=CARTESIAN_POINT('Ctrl Pts',(3.10606665601004,98.2062499996177,9.5594902125713));
#286495=CARTESIAN_POINT('Ctrl Pts',(6.21213331202015,98.3562499996171,8.55026797822134));
#286496=CARTESIAN_POINT('Ctrl Pts',(8.13178807675712,98.5062499996165,5.90808986649102));
#286497=CARTESIAN_POINT('Ctrl Pts',(10.0514428414941,98.6562499996158,3.2659117547607));
#286498=CARTESIAN_POINT('Ctrl Pts',(10.0514428414941,98.8062499996153,-1.23094673026484E-15));
#286499=CARTESIAN_POINT('Ctrl Pts',(10.0514428414941,98.9562499996147,-3.26591175476071));
#286500=CARTESIAN_POINT('Ctrl Pts',(8.13178807675712,99.1062499996141,-5.90808986649102));
#286501=CARTESIAN_POINT('Ctrl Pts',(6.21213331202015,99.2562499996134,-8.55026797822134));
#286502=CARTESIAN_POINT('Ctrl Pts',(3.10606665601004,99.4062499996129,-9.5594902125713));
#286503=CARTESIAN_POINT('Ctrl Pts',(-7.04595224713284E-14,99.5562499996123,
-10.5687124469213));
#286504=CARTESIAN_POINT('Ctrl Pts',(-3.10606665601018,99.7062499996117,
-9.5594902125713));
#286505=CARTESIAN_POINT('Ctrl Pts',(-6.21213331202028,99.856249999611,-8.55026797822134));
#286506=CARTESIAN_POINT('Ctrl Pts',(-8.13178807675726,100.00624999961,-5.90808986649102));
#286507=CARTESIAN_POINT('Ctrl Pts',(-10.0514428414942,100.15624999961,-3.2659117547607));
#286508=CARTESIAN_POINT('Ctrl Pts',(-10.0514428414942,100.306249999609,
2.46189346052968E-15));
#286509=CARTESIAN_POINT('Ctrl Pts',(-10.0514428414942,100.456249999609,
3.26591175476071));
#286510=CARTESIAN_POINT('Ctrl Pts',(-8.13178807675726,100.606249999608,
5.90808986649102));
#286511=CARTESIAN_POINT('Ctrl Pts',(-6.21213331202028,100.756249999607,
8.55026797822134));
#286512=CARTESIAN_POINT('Ctrl Pts',(-3.10606665601018,100.906249999607,
9.5594902125713));
#286513=CARTESIAN_POINT('Ctrl Pts',(-6.87347891333132E-14,101.056249999606,
10.5687124469213));
#286514=CARTESIAN_POINT('Ctrl Pts',(3.10606665601004,101.206249999606,9.5594902125713));
#286515=CARTESIAN_POINT('Ctrl Pts',(6.21213331202015,101.356249999605,8.55026797822134));
#286516=CARTESIAN_POINT('Ctrl Pts',(8.13178807675712,101.506249999604,5.90808986649102));
#286517=CARTESIAN_POINT('Ctrl Pts',(10.0514428414941,101.656249999604,3.2659117547607));
#286518=CARTESIAN_POINT('Ctrl Pts',(10.0514428414941,101.806249999603,-1.23094673026484E-15));
#286519=CARTESIAN_POINT('Ctrl Pts',(10.0514428414941,101.956249999603,-3.26591175476071));
#286520=CARTESIAN_POINT('Ctrl Pts',(8.13178807675712,102.106249999602,-5.90808986649102));
#286521=CARTESIAN_POINT('Ctrl Pts',(6.21213331202014,102.256249999601,-8.55026797822134));
#286522=CARTESIAN_POINT('Ctrl Pts',(3.10606665601004,102.406249999601,-9.5594902125713));
#286523=CARTESIAN_POINT('Ctrl Pts',(-7.21872317429903E-14,102.5562499996,
-10.5687124469213));
#286524=CARTESIAN_POINT('Ctrl Pts',(-3.10606665601018,102.7062499996,-9.5594902125713));
#286525=CARTESIAN_POINT('Ctrl Pts',(-6.21213331202029,102.856249999599,
-8.55026797822134));
#286526=CARTESIAN_POINT('Ctrl Pts',(-8.13178807675726,103.006249999598,
-5.90808986649102));
#286527=CARTESIAN_POINT('Ctrl Pts',(-10.0514428414942,103.156249999598,
-3.2659117547607));
#286528=CARTESIAN_POINT('Ctrl Pts',(-10.0514428414942,103.306249999597,
2.46189346052968E-15));
#286529=CARTESIAN_POINT('Ctrl Pts',(-10.0514428414942,103.456249999597,
3.26591175476071));
#286530=CARTESIAN_POINT('Ctrl Pts',(-8.13178807675726,103.606249999596,
5.90808986649102));
#286531=CARTESIAN_POINT('Ctrl Pts',(-6.21213331202028,103.756249999595,
8.55026797822134));
#286532=CARTESIAN_POINT('Ctrl Pts',(-3.10606665601018,103.906249999595,
9.5594902125713));
#286533=CARTESIAN_POINT('Ctrl Pts',(-7.04624984049751E-14,104.056249999594,
10.5687124469213));
#286534=CARTESIAN_POINT('Ctrl Pts',(3.10606665601004,104.206249999594,9.5594902125713));
#286535=CARTESIAN_POINT('Ctrl Pts',(6.21213331202015,104.356249999593,8.55026797822134));
#286536=CARTESIAN_POINT('Ctrl Pts',(8.13178807675712,104.506249999592,5.90808986649102));
#286537=CARTESIAN_POINT('Ctrl Pts',(10.0514428414941,104.656249999592,3.2659117547607));
#286538=CARTESIAN_POINT('Ctrl Pts',(10.0514428414941,104.806249999591,-1.23094673026484E-15));
#286539=CARTESIAN_POINT('Ctrl Pts',(10.0514428414941,104.956249999591,-3.26591175476071));
#286540=CARTESIAN_POINT('Ctrl Pts',(8.13178807675712,105.10624999959,-5.90808986649102));
#286541=CARTESIAN_POINT('Ctrl Pts',(6.21213331202014,105.256249999589,-8.55026797822134));
#286542=CARTESIAN_POINT('Ctrl Pts',(3.10606665601003,105.406249999589,-9.5594902125713));
#286543=CARTESIAN_POINT('Ctrl Pts',(-7.39149410146522E-14,105.556249999588,
-10.5687124469213));
#286544=CARTESIAN_POINT('Ctrl Pts',(-3.10606665601018,105.706249999588,
-9.5594902125713));
#286545=CARTESIAN_POINT('Ctrl Pts',(-6.21213331202029,105.856249999587,
-8.55026797822134));
#286546=CARTESIAN_POINT('Ctrl Pts',(-8.13178807675726,106.006249999586,
-5.90808986649102));
#286547=CARTESIAN_POINT('Ctrl Pts',(-10.0514428414942,106.156249999586,
-3.2659117547607));
#286548=CARTESIAN_POINT('Ctrl Pts',(-10.0514428414942,106.306249999585,
2.46189346052968E-15));
#286549=CARTESIAN_POINT('Ctrl Pts',(-10.0514428414942,106.456249999585,
3.26591175476071));
#286550=CARTESIAN_POINT('Ctrl Pts',(-8.13178807675726,106.606249999584,
5.90808986649102));
#286551=CARTESIAN_POINT('Ctrl Pts',(-6.21213331202029,106.756249999583,
8.55026797822134));
#286552=CARTESIAN_POINT('Ctrl Pts',(-3.10606665601018,106.906249999583,
9.5594902125713));
#286553=CARTESIAN_POINT('Ctrl Pts',(-7.21902076766369E-14,107.056249999582,
10.5687124469213));
#286554=CARTESIAN_POINT('Ctrl Pts',(3.10606665601003,107.206249999582,9.5594902125713));
#286555=CARTESIAN_POINT('Ctrl Pts',(6.21213331202014,107.356249999581,8.55026797822134));
#286556=CARTESIAN_POINT('Ctrl Pts',(8.13178807675711,107.50624999958,5.90808986649102));
#286557=CARTESIAN_POINT('Ctrl Pts',(10.0514428414941,107.65624999958,3.2659117547607));
#286558=CARTESIAN_POINT('Ctrl Pts',(10.0514428414941,107.806249999579,-1.23094673026484E-15));
#286559=CARTESIAN_POINT('Ctrl Pts',(10.0514428414941,107.956249999579,-3.26591175476071));
#286560=CARTESIAN_POINT('Ctrl Pts',(8.13178807675711,108.106249999578,-5.90808986649102));
#286561=CARTESIAN_POINT('Ctrl Pts',(6.21213331202014,108.256249999577,-8.55026797822134));
#286562=CARTESIAN_POINT('Ctrl Pts',(3.10606665601003,108.406249999577,-9.5594902125713));
#286563=CARTESIAN_POINT('Ctrl Pts',(-7.5642650286314E-14,108.556249999576,
-10.5687124469213));
#286564=CARTESIAN_POINT('Ctrl Pts',(-3.10606665601018,108.706249999576,
-9.5594902125713));
#286565=CARTESIAN_POINT('Ctrl Pts',(-6.21213331202029,108.856249999575,
-8.55026797822134));
#286566=CARTESIAN_POINT('Ctrl Pts',(-8.13178807675727,109.006249999574,
-5.90808986649102));
#286567=CARTESIAN_POINT('Ctrl Pts',(-10.0514428414942,109.156249999574,
-3.2659117547607));
#286568=CARTESIAN_POINT('Ctrl Pts',(-10.0514428414942,109.306249999573,
2.46189346052968E-15));
#286569=CARTESIAN_POINT('Ctrl Pts',(-10.0514428414942,109.456249999573,
3.26591175476071));
#286570=CARTESIAN_POINT('Ctrl Pts',(-8.13178807675727,109.606249999572,
5.90808986649102));
#286571=CARTESIAN_POINT('Ctrl Pts',(-6.21213331202029,109.756249999571,
8.55026797822134));
#286572=CARTESIAN_POINT('Ctrl Pts',(-3.10606665601018,109.906249999571,
9.5594902125713));
#286573=CARTESIAN_POINT('Ctrl Pts',(-7.39179169482987E-14,110.05624999957,
10.5687124469213));
#286574=CARTESIAN_POINT('Ctrl Pts',(3.10606665601003,110.20624999957,9.5594902125713));
#286575=CARTESIAN_POINT('Ctrl Pts',(6.21213331202014,110.356249999569,8.55026797822134));
#286576=CARTESIAN_POINT('Ctrl Pts',(8.13178807675711,110.506249999568,5.90808986649102));
#286577=CARTESIAN_POINT('Ctrl Pts',(10.0514428414941,110.656249999568,3.2659117547607));
#286578=CARTESIAN_POINT('Ctrl Pts',(10.0514428414941,110.806249999567,-1.23094673026484E-15));
#286579=CARTESIAN_POINT('Ctrl Pts',(10.0514428414941,110.956249999567,-3.26591175476071));
#286580=CARTESIAN_POINT('Ctrl Pts',(8.13178807675711,111.106249999566,-5.90808986649102));
#286581=CARTESIAN_POINT('Ctrl Pts',(6.21213331202014,111.256249999565,-8.55026797822134));
#286582=CARTESIAN_POINT('Ctrl Pts',(3.10606665601003,111.406249999565,-9.5594902125713));
#286583=CARTESIAN_POINT('Ctrl Pts',(-7.73703595579758E-14,111.556249999564,
-10.5687124469213));
#286584=CARTESIAN_POINT('Ctrl Pts',(-3.10606665601019,111.706249999564,
-9.5594902125713));
#286585=CARTESIAN_POINT('Ctrl Pts',(-6.21213331202029,111.856249999563,
-8.55026797822134));
#286586=CARTESIAN_POINT('Ctrl Pts',(-8.13178807675727,112.006249999562,
-5.90808986649102));
#286587=CARTESIAN_POINT('Ctrl Pts',(-10.0514428414942,112.156249999562,
-3.2659117547607));
#286588=CARTESIAN_POINT('Ctrl Pts',(-10.0514428414942,112.306249999561,
2.46189346052968E-15));
#286589=CARTESIAN_POINT('Ctrl Pts',(-10.0514428414942,112.456249999561,
3.26591175476071));
#286590=CARTESIAN_POINT('Ctrl Pts',(-8.13178807675727,112.60624999956,5.90808986649102));
#286591=CARTESIAN_POINT('Ctrl Pts',(-6.21213331202029,112.756249999559,
8.55026797822134));
#286592=CARTESIAN_POINT('Ctrl Pts',(-3.10606665601018,112.906249999559,
9.5594902125713));
#286593=CARTESIAN_POINT('Ctrl Pts',(-7.56456262199606E-14,113.056249999558,
10.5687124469213));
#286594=CARTESIAN_POINT('Ctrl Pts',(3.10606665601003,113.206249999558,9.5594902125713));
#286595=CARTESIAN_POINT('Ctrl Pts',(6.21213331202014,113.356249999557,8.55026797822134));
#286596=CARTESIAN_POINT('Ctrl Pts',(8.13178807675711,113.506249999556,5.90808986649102));
#286597=CARTESIAN_POINT('Ctrl Pts',(10.0514428414941,113.656249999556,3.2659117547607));
#286598=CARTESIAN_POINT('Ctrl Pts',(10.0514428414941,113.806249999555,-1.23094673026484E-15));
#286599=CARTESIAN_POINT('Ctrl Pts',(10.0514428414941,113.956249999555,-3.26591175476071));
#286600=CARTESIAN_POINT('Ctrl Pts',(8.13178807675711,114.106249999554,-5.90808986649102));
#286601=CARTESIAN_POINT('Ctrl Pts',(6.21213331202014,114.256249999553,-8.55026797822134));
#286602=CARTESIAN_POINT('Ctrl Pts',(3.10606665601003,114.406249999553,-9.5594902125713));
#286603=CARTESIAN_POINT('Ctrl Pts',(-7.90980688296377E-14,114.556249999552,
-10.5687124469213));
#286604=CARTESIAN_POINT('Ctrl Pts',(-3.10606665601019,114.706249999552,
-9.5594902125713));
#286605=CARTESIAN_POINT('Ctrl Pts',(-6.2121333120203,114.856249999551,-8.55026797822134));
#286606=CARTESIAN_POINT('Ctrl Pts',(-8.13178807675727,115.00624999955,-5.90808986649102));
#286607=CARTESIAN_POINT('Ctrl Pts',(-10.0514428414942,115.15624999955,-3.2659117547607));
#286608=CARTESIAN_POINT('Ctrl Pts',(-10.0514428414942,115.306249999549,
2.46189346052968E-15));
#286609=CARTESIAN_POINT('Ctrl Pts',(-10.0514428414942,115.456249999549,
3.26591175476071));
#286610=CARTESIAN_POINT('Ctrl Pts',(-8.13178807675727,115.606249999548,
5.90808986649102));
#286611=CARTESIAN_POINT('Ctrl Pts',(-6.21213331202029,115.756249999547,
8.55026797822134));
#286612=CARTESIAN_POINT('Ctrl Pts',(-3.10606665601019,115.906249999547,
9.5594902125713));
#286613=CARTESIAN_POINT('Ctrl Pts',(-7.73733354916224E-14,116.056249999546,
10.5687124469213));
#286614=CARTESIAN_POINT('Ctrl Pts',(3.10606665601003,116.206249999546,9.5594902125713));
#286615=CARTESIAN_POINT('Ctrl Pts',(6.21213331202014,116.356249999545,8.55026797822134));
#286616=CARTESIAN_POINT('Ctrl Pts',(8.13178807675711,116.506249999544,5.90808986649102));
#286617=CARTESIAN_POINT('Ctrl Pts',(10.0514428414941,116.656249999544,3.2659117547607));
#286618=CARTESIAN_POINT('Ctrl Pts',(10.0514428414941,116.806249999543,-1.23094673026484E-15));
#286619=CARTESIAN_POINT('Ctrl Pts',(10.0514428414941,116.956249999543,-3.26591175476071));
#286620=CARTESIAN_POINT('Ctrl Pts',(8.13178807675711,117.106249999542,-5.90808986649102));
#286621=CARTESIAN_POINT('Ctrl Pts',(6.21213331202014,117.256249999541,-8.55026797822134));
#286622=CARTESIAN_POINT('Ctrl Pts',(3.10606665601003,117.406249999541,-9.5594902125713));
#286623=CARTESIAN_POINT('Ctrl Pts',(-8.08257781012995E-14,117.55624999954,
-10.5687124469213));
#286624=CARTESIAN_POINT('Ctrl Pts',(-3.10606665601019,117.70624999954,-9.5594902125713));
#286625=CARTESIAN_POINT('Ctrl Pts',(-6.2121333120203,117.856249999539,-8.55026797822134));
#286626=CARTESIAN_POINT('Ctrl Pts',(-8.13178807675727,118.006249999538,
-5.90808986649102));
#286627=CARTESIAN_POINT('Ctrl Pts',(-10.0514428414942,118.156249999538,
-3.2659117547607));
#286628=CARTESIAN_POINT('Ctrl Pts',(-10.0514428414942,118.306249999537,
2.46189346052968E-15));
#286629=CARTESIAN_POINT('Ctrl Pts',(-10.0514428414942,118.456249999537,
3.26591175476071));
#286630=CARTESIAN_POINT('Ctrl Pts',(-8.13178807675727,118.606249999536,
5.90808986649102));
#286631=CARTESIAN_POINT('Ctrl Pts',(-6.2121333120203,118.756249999535,8.55026797822134));
#286632=CARTESIAN_POINT('Ctrl Pts',(-3.10606665601019,118.906249999535,
9.5594902125713));
#286633=CARTESIAN_POINT('Ctrl Pts',(-7.91010447632842E-14,119.056249999534,
10.5687124469213));
#286634=CARTESIAN_POINT('Ctrl Pts',(3.10606665601003,119.206249999534,9.5594902125713));
#286635=CARTESIAN_POINT('Ctrl Pts',(6.21213331202014,119.356249999533,8.55026797822134));
#286636=CARTESIAN_POINT('Ctrl Pts',(8.13178807675711,119.506249999532,5.90808986649102));
#286637=CARTESIAN_POINT('Ctrl Pts',(10.0514428414941,119.656249999532,3.2659117547607));
#286638=CARTESIAN_POINT('Ctrl Pts',(10.0514428414941,119.806249999531,-1.23094673026484E-15));
#286639=CARTESIAN_POINT('Ctrl Pts',(10.0514428414941,119.956249999531,-3.26591175476071));
#286640=CARTESIAN_POINT('Ctrl Pts',(8.13178807675711,120.10624999953,-5.90808986649102));
#286641=CARTESIAN_POINT('Ctrl Pts',(6.21213331202013,120.256249999529,-8.55026797822134));
#286642=CARTESIAN_POINT('Ctrl Pts',(3.10606665601003,120.406249999529,-9.5594902125713));
#286643=CARTESIAN_POINT('Ctrl Pts',(-8.25534873729613E-14,120.556249999528,
-10.5687124469213));
#286644=CARTESIAN_POINT('Ctrl Pts',(-3.10606665601019,120.706249999528,
-9.5594902125713));
#286645=CARTESIAN_POINT('Ctrl Pts',(-6.2121333120203,120.856249999527,-8.55026797822134));
#286646=CARTESIAN_POINT('Ctrl Pts',(-8.13178807675727,121.006249999526,
-5.90808986649102));
#286647=CARTESIAN_POINT('Ctrl Pts',(-10.0514428414943,121.156249999526,
-3.2659117547607));
#286648=CARTESIAN_POINT('Ctrl Pts',(-10.0514428414943,121.306249999525,
2.46189346052968E-15));
#286649=CARTESIAN_POINT('Ctrl Pts',(-10.0514428414943,121.456249999525,
3.26591175476071));
#286650=CARTESIAN_POINT('Ctrl Pts',(-8.13178807675727,121.606249999524,
5.90808986649102));
#286651=CARTESIAN_POINT('Ctrl Pts',(-6.2121333120203,121.756249999523,8.55026797822134));
#286652=CARTESIAN_POINT('Ctrl Pts',(-3.10606665601019,121.906249999523,
9.5594902125713));
#286653=CARTESIAN_POINT('Ctrl Pts',(-8.08287540349461E-14,122.056249999522,
10.5687124469213));
#286654=CARTESIAN_POINT('Ctrl Pts',(3.10606665601003,122.206249999522,9.5594902125713));
#286655=CARTESIAN_POINT('Ctrl Pts',(6.21213331202014,122.356249999521,8.55026797822134));
#286656=CARTESIAN_POINT('Ctrl Pts',(8.13178807675711,122.50624999952,5.90808986649102));
#286657=CARTESIAN_POINT('Ctrl Pts',(10.0514428414941,122.65624999952,3.2659117547607));
#286658=CARTESIAN_POINT('Ctrl Pts',(10.0514428414941,122.806249999519,-1.23094673026484E-15));
#286659=CARTESIAN_POINT('Ctrl Pts',(10.0514428414941,122.956249999519,-3.26591175476071));
#286660=CARTESIAN_POINT('Ctrl Pts',(8.13178807675711,123.106249999518,-5.90808986649102));
#286661=CARTESIAN_POINT('Ctrl Pts',(6.21213331202013,123.256249999517,-8.55026797822134));
#286662=CARTESIAN_POINT('Ctrl Pts',(3.10606665601002,123.406249999517,-9.5594902125713));
#286663=CARTESIAN_POINT('Ctrl Pts',(-8.42811966446232E-14,123.556249999516,
-10.5687124469213));
#286664=CARTESIAN_POINT('Ctrl Pts',(-3.10606665601019,123.706249999516,
-9.5594902125713));
#286665=CARTESIAN_POINT('Ctrl Pts',(-6.2121333120203,123.856249999515,-8.55026797822134));
#286666=CARTESIAN_POINT('Ctrl Pts',(-8.13178807675727,124.006249999514,
-5.90808986649102));
#286667=CARTESIAN_POINT('Ctrl Pts',(-10.0514428414943,124.156249999514,
-3.2659117547607));
#286668=CARTESIAN_POINT('Ctrl Pts',(-10.0514428414943,124.306249999513,
2.46189346052968E-15));
#286669=CARTESIAN_POINT('Ctrl Pts',(-10.0514428414943,124.456249999513,
3.26591175476071));
#286670=CARTESIAN_POINT('Ctrl Pts',(-8.13178807675727,124.606249999512,
5.90808986649102));
#286671=CARTESIAN_POINT('Ctrl Pts',(-6.2121333120203,124.756249999511,8.55026797822134));
#286672=CARTESIAN_POINT('Ctrl Pts',(-3.10606665601019,124.906249999511,
9.5594902125713));
#286673=CARTESIAN_POINT('Ctrl Pts',(-8.25564633066079E-14,125.05624999951,
10.5687124469213));
#286674=CARTESIAN_POINT('Ctrl Pts',(3.10606665601002,125.20624999951,9.5594902125713));
#286675=CARTESIAN_POINT('Ctrl Pts',(6.21213331202013,125.356249999509,8.55026797822134));
#286676=CARTESIAN_POINT('Ctrl Pts',(8.13178807675711,125.506249999508,5.90808986649102));
#286677=CARTESIAN_POINT('Ctrl Pts',(10.0514428414941,125.656249999508,3.2659117547607));
#286678=CARTESIAN_POINT('Ctrl Pts',(10.0514428414941,125.806249999507,-1.23094673026484E-15));
#286679=CARTESIAN_POINT('Ctrl Pts',(10.0514428414941,125.956249999507,-3.26591175476071));
#286680=CARTESIAN_POINT('Ctrl Pts',(8.13178807675711,126.106249999506,-5.90808986649102));
#286681=CARTESIAN_POINT('Ctrl Pts',(6.21213331202013,126.256249999505,-8.55026797822134));
#286682=CARTESIAN_POINT('Ctrl Pts',(3.10606665601002,126.406249999505,-9.5594902125713));
#286683=CARTESIAN_POINT('Ctrl Pts',(-8.6008905916285E-14,126.556249999504,
-10.5687124469213));
#286684=CARTESIAN_POINT('Ctrl Pts',(-3.10606665601019,126.706249999504,
-9.5594902125713));
#286685=CARTESIAN_POINT('Ctrl Pts',(-6.2121333120203,126.856249999503,-8.55026797822134));
#286686=CARTESIAN_POINT('Ctrl Pts',(-8.13178807675728,127.006249999502,
-5.90808986649102));
#286687=CARTESIAN_POINT('Ctrl Pts',(-10.0514428414943,127.156249999502,
-3.2659117547607));
#286688=CARTESIAN_POINT('Ctrl Pts',(-10.0514428414943,127.306249999501,
2.46189346052968E-15));
#286689=CARTESIAN_POINT('Ctrl Pts',(-10.0514428414943,127.456249999501,
3.26591175476071));
#286690=CARTESIAN_POINT('Ctrl Pts',(-8.13178807675728,127.6062499995,5.90808986649102));
#286691=CARTESIAN_POINT('Ctrl Pts',(-6.2121333120203,127.756249999499,8.55026797822134));
#286692=CARTESIAN_POINT('Ctrl Pts',(-3.10606665601019,127.906249999499,
9.5594902125713));
#286693=CARTESIAN_POINT('Ctrl Pts',(-8.42841725782698E-14,128.056249999498,
10.5687124469213));
#286694=CARTESIAN_POINT('Ctrl Pts',(3.10606665601002,128.206249999498,9.5594902125713));
#286695=CARTESIAN_POINT('Ctrl Pts',(6.21213331202013,128.356249999497,8.55026797822134));
#286696=CARTESIAN_POINT('Ctrl Pts',(8.1317880767571,128.506249999496,5.90808986649102));
#286697=CARTESIAN_POINT('Ctrl Pts',(10.0514428414941,128.656249999496,3.2659117547607));
#286698=CARTESIAN_POINT('Ctrl Pts',(10.0514428414941,128.806249999495,-1.23094673026484E-15));
#286699=CARTESIAN_POINT('Ctrl Pts',(10.0514428414941,128.956249999495,-3.26591175476071));
#286700=CARTESIAN_POINT('Ctrl Pts',(8.1317880767571,129.106249999494,-5.90808986649102));
#286701=CARTESIAN_POINT('Ctrl Pts',(6.21213331202013,129.256249999493,-8.55026797822134));
#286702=CARTESIAN_POINT('Ctrl Pts',(3.10606665601002,129.406249999493,-9.5594902125713));
#286703=CARTESIAN_POINT('Ctrl Pts',(-8.77366151879469E-14,129.556249999492,
-10.5687124469213));
#286704=CARTESIAN_POINT('Ctrl Pts',(-3.1060666560102,129.706249999492,-9.5594902125713));
#286705=CARTESIAN_POINT('Ctrl Pts',(-6.2121333120203,129.856249999491,-8.55026797822134));
#286706=CARTESIAN_POINT('Ctrl Pts',(-8.13178807675728,130.00624999949,-5.90808986649102));
#286707=CARTESIAN_POINT('Ctrl Pts',(-10.0514428414943,130.15624999949,-3.2659117547607));
#286708=CARTESIAN_POINT('Ctrl Pts',(-10.0514428414943,130.306249999489,
2.46189346052968E-15));
#286709=CARTESIAN_POINT('Ctrl Pts',(-10.0514428414943,130.456249999489,
3.26591175476071));
#286710=CARTESIAN_POINT('Ctrl Pts',(-8.13178807675728,130.606249999488,
5.90808986649102));
#286711=CARTESIAN_POINT('Ctrl Pts',(-6.2121333120203,130.756249999487,8.55026797822134));
#286712=CARTESIAN_POINT('Ctrl Pts',(-3.10606665601019,130.906249999487,
9.5594902125713));
#286713=CARTESIAN_POINT('Ctrl Pts',(-8.60118818499316E-14,131.056249999486,
10.5687124469213));
#286714=CARTESIAN_POINT('Ctrl Pts',(3.10606665601002,131.206249999486,9.5594902125713));
#286715=CARTESIAN_POINT('Ctrl Pts',(6.21213331202013,131.356249999485,8.55026797822134));
#286716=CARTESIAN_POINT('Ctrl Pts',(8.1317880767571,131.506249999484,5.90808986649102));
#286717=CARTESIAN_POINT('Ctrl Pts',(10.0514428414941,131.656249999484,3.2659117547607));
#286718=CARTESIAN_POINT('Ctrl Pts',(10.0514428414941,131.806249999483,-1.23094673026484E-15));
#286719=CARTESIAN_POINT('Ctrl Pts',(10.0514428414941,131.956249999483,-3.26591175476071));
#286720=CARTESIAN_POINT('Ctrl Pts',(8.1317880767571,132.106249999482,-5.90808986649102));
#286721=CARTESIAN_POINT('Ctrl Pts',(6.21213331202012,132.256249999481,-8.55026797822134));
#286722=CARTESIAN_POINT('Ctrl Pts',(3.10606665601002,132.406249999481,-9.5594902125713));
#286723=CARTESIAN_POINT('Ctrl Pts',(-8.94643244596087E-14,132.55624999948,
-10.5687124469213));
#286724=CARTESIAN_POINT('Ctrl Pts',(-3.1060666560102,132.70624999948,-9.5594902125713));
#286725=CARTESIAN_POINT('Ctrl Pts',(-6.2121333120203,132.856249999479,-8.55026797822134));
#286726=CARTESIAN_POINT('Ctrl Pts',(-8.13178807675728,133.006249999478,
-5.90808986649102));
#286727=CARTESIAN_POINT('Ctrl Pts',(-10.0514428414943,133.156249999478,
-3.2659117547607));
#286728=CARTESIAN_POINT('Ctrl Pts',(-10.0514428414943,133.306249999477,
2.46189346052968E-15));
#286729=CARTESIAN_POINT('Ctrl Pts',(-10.0514428414943,133.456249999477,
3.26591175476071));
#286730=CARTESIAN_POINT('Ctrl Pts',(-8.13178807675728,133.606249999476,
5.90808986649102));
#286731=CARTESIAN_POINT('Ctrl Pts',(-6.2121333120203,133.756249999475,8.55026797822134));
#286732=CARTESIAN_POINT('Ctrl Pts',(-3.1060666560102,133.906249999475,9.5594902125713));
#286733=CARTESIAN_POINT('Ctrl Pts',(-8.77395911215934E-14,134.056249999474,
10.5687124469213));
#286734=CARTESIAN_POINT('Ctrl Pts',(3.10606665601002,134.206249999474,9.5594902125713));
#286735=CARTESIAN_POINT('Ctrl Pts',(6.21213331202013,134.356249999473,8.55026797822134));
#286736=CARTESIAN_POINT('Ctrl Pts',(8.1317880767571,134.506249999472,5.90808986649102));
#286737=CARTESIAN_POINT('Ctrl Pts',(10.0514428414941,134.656249999472,3.2659117547607));
#286738=CARTESIAN_POINT('Ctrl Pts',(10.0514428414941,134.806249999471,-1.23094673026484E-15));
#286739=CARTESIAN_POINT('Ctrl Pts',(10.0514428414941,134.956249999471,-3.26591175476071));
#286740=CARTESIAN_POINT('Ctrl Pts',(8.1317880767571,135.10624999947,-5.90808986649102));
#286741=CARTESIAN_POINT('Ctrl Pts',(6.21213331202012,135.256249999469,-8.55026797822134));
#286742=CARTESIAN_POINT('Ctrl Pts',(3.10606665601002,135.406249999469,-9.5594902125713));
#286743=CARTESIAN_POINT('Ctrl Pts',(-9.11920337312706E-14,135.556249999468,
-10.5687124469213));
#286744=CARTESIAN_POINT('Ctrl Pts',(-3.1060666560102,135.706249999468,-9.5594902125713));
#286745=CARTESIAN_POINT('Ctrl Pts',(-6.21213331202031,135.856249999467,
-8.55026797822134));
#286746=CARTESIAN_POINT('Ctrl Pts',(-8.13178807675728,136.006249999466,
-5.90808986649102));
#286747=CARTESIAN_POINT('Ctrl Pts',(-10.0514428414943,136.156249999466,
-3.2659117547607));
#286748=CARTESIAN_POINT('Ctrl Pts',(-10.0514428414943,136.306249999465,
2.46189346052968E-15));
#286749=CARTESIAN_POINT('Ctrl Pts',(-10.0514428414943,136.456249999465,
3.26591175476071));
#286750=CARTESIAN_POINT('Ctrl Pts',(-8.13178807675728,136.606249999464,
5.90808986649102));
#286751=CARTESIAN_POINT('Ctrl Pts',(-6.2121333120203,136.756249999463,8.55026797822134));
#286752=CARTESIAN_POINT('Ctrl Pts',(-3.1060666560102,136.906249999463,9.5594902125713));
#286753=CARTESIAN_POINT('Ctrl Pts',(-8.94673003932553E-14,137.056249999462,
10.5687124469213));
#286754=CARTESIAN_POINT('Ctrl Pts',(3.10606665601002,137.206249999462,9.5594902125713));
#286755=CARTESIAN_POINT('Ctrl Pts',(6.21213331202012,137.356249999461,8.55026797822134));
#286756=CARTESIAN_POINT('Ctrl Pts',(8.1317880767571,137.50624999946,5.90808986649102));
#286757=CARTESIAN_POINT('Ctrl Pts',(10.0514428414941,137.65624999946,3.2659117547607));
#286758=CARTESIAN_POINT('Ctrl Pts',(10.0514428414941,137.806249999459,-1.23094673026484E-15));
#286759=CARTESIAN_POINT('Ctrl Pts',(10.0514428414941,137.956249999459,-3.26591175476071));
#286760=CARTESIAN_POINT('Ctrl Pts',(8.1317880767571,138.106249999458,-5.90808986649102));
#286761=CARTESIAN_POINT('Ctrl Pts',(6.21213331202012,138.256249999457,-8.55026797822134));
#286762=CARTESIAN_POINT('Ctrl Pts',(3.10606665601001,138.406249999457,-9.5594902125713));
#286763=CARTESIAN_POINT('Ctrl Pts',(-9.29197430029324E-14,138.556249999456,
-10.5687124469213));
#286764=CARTESIAN_POINT('Ctrl Pts',(-3.1060666560102,138.706249999456,-9.5594902125713));
#286765=CARTESIAN_POINT('Ctrl Pts',(-6.21213331202031,138.856249999455,
-8.55026797822134));
#286766=CARTESIAN_POINT('Ctrl Pts',(-8.13178807675728,139.006249999454,
-5.90808986649102));
#286767=CARTESIAN_POINT('Ctrl Pts',(-10.0514428414943,139.156249999454,
-3.2659117547607));
#286768=CARTESIAN_POINT('Ctrl Pts',(-10.0514428414943,139.306249999453,
2.46189346052968E-15));
#286769=CARTESIAN_POINT('Ctrl Pts',(-10.0514428414943,139.456249999453,
3.26591175476071));
#286770=CARTESIAN_POINT('Ctrl Pts',(-8.13178807675728,139.606249999452,
5.90808986649102));
#286771=CARTESIAN_POINT('Ctrl Pts',(-6.21213331202031,139.756249999451,
8.55026797822134));
#286772=CARTESIAN_POINT('Ctrl Pts',(-3.1060666560102,139.906249999451,9.5594902125713));
#286773=CARTESIAN_POINT('Ctrl Pts',(-9.11950096649171E-14,140.05624999945,
10.5687124469213));
#286774=CARTESIAN_POINT('Ctrl Pts',(3.10606665601002,140.20624999945,9.5594902125713));
#286775=CARTESIAN_POINT('Ctrl Pts',(6.21213331202012,140.356249999449,8.55026797822134));
#286776=CARTESIAN_POINT('Ctrl Pts',(8.1317880767571,140.506249999448,5.90808986649102));
#286777=CARTESIAN_POINT('Ctrl Pts',(10.0514428414941,140.656249999448,3.2659117547607));
#286778=CARTESIAN_POINT('Ctrl Pts',(10.0514428414941,140.806249999447,-1.23094673026484E-15));
#286779=CARTESIAN_POINT('Ctrl Pts',(10.0514428414941,140.956249999447,-3.26591175476071));
#286780=CARTESIAN_POINT('Ctrl Pts',(8.1317880767571,141.106249999446,-5.90808986649102));
#286781=CARTESIAN_POINT('Ctrl Pts',(6.21213331202012,141.256249999445,-8.55026797822134));
#286782=CARTESIAN_POINT('Ctrl Pts',(3.10606665601001,141.406249999445,-9.5594902125713));
#286783=CARTESIAN_POINT('Ctrl Pts',(-9.46474522745942E-14,141.556249999444,
-10.5687124469213));
#286784=CARTESIAN_POINT('Ctrl Pts',(-3.1060666560102,141.706249999444,-9.5594902125713));
#286785=CARTESIAN_POINT('Ctrl Pts',(-6.21213331202031,141.856249999443,
-8.55026797822134));
#286786=CARTESIAN_POINT('Ctrl Pts',(-8.13178807675729,142.006249999442,
-5.90808986649102));
#286787=CARTESIAN_POINT('Ctrl Pts',(-10.0514428414943,142.156249999442,
-3.2659117547607));
#286788=CARTESIAN_POINT('Ctrl Pts',(-10.0514428414943,142.306249999441,
2.46189346052968E-15));
#286789=CARTESIAN_POINT('Ctrl Pts',(-10.0514428414943,142.456249999441,
3.26591175476071));
#286790=CARTESIAN_POINT('Ctrl Pts',(-8.13178807675729,142.60624999944,5.90808986649102));
#286791=CARTESIAN_POINT('Ctrl Pts',(-6.21213331202031,142.756249999439,
8.55026797822134));
#286792=CARTESIAN_POINT('Ctrl Pts',(-3.1060666560102,142.906249999439,9.5594902125713));
#286793=CARTESIAN_POINT('Ctrl Pts',(-9.29227189365789E-14,143.056249999438,
10.5687124469213));
#286794=CARTESIAN_POINT('Ctrl Pts',(3.10606665601001,143.206249999438,9.5594902125713));
#286795=CARTESIAN_POINT('Ctrl Pts',(6.21213331202012,143.356249999437,8.55026797822134));
#286796=CARTESIAN_POINT('Ctrl Pts',(8.1317880767571,143.506249999436,5.90808986649102));
#286797=CARTESIAN_POINT('Ctrl Pts',(10.0514428414941,143.656249999436,3.2659117547607));
#286798=CARTESIAN_POINT('Ctrl Pts',(10.0514428414941,143.806249999435,-1.23094673026484E-15));
#286799=CARTESIAN_POINT('Ctrl Pts',(10.0514428414941,143.956249999435,-3.26591175476071));
#286800=CARTESIAN_POINT('Ctrl Pts',(8.1317880767571,144.106249999434,-5.90808986649102));
#286801=CARTESIAN_POINT('Ctrl Pts',(6.21213331202012,144.256249999433,-8.55026797822134));
#286802=CARTESIAN_POINT('Ctrl Pts',(3.10606665601001,144.406249999433,-9.5594902125713));
#286803=CARTESIAN_POINT('Ctrl Pts',(-9.63751615462561E-14,144.556249999432,
-10.5687124469213));
#286804=CARTESIAN_POINT('Ctrl Pts',(-3.1060666560102,144.706249999432,-9.5594902125713));
#286805=CARTESIAN_POINT('Ctrl Pts',(-6.21213331202031,144.856249999431,
-8.55026797822134));
#286806=CARTESIAN_POINT('Ctrl Pts',(-8.13178807675729,145.00624999943,-5.90808986649102));
#286807=CARTESIAN_POINT('Ctrl Pts',(-10.0514428414943,145.15624999943,-3.2659117547607));
#286808=CARTESIAN_POINT('Ctrl Pts',(-10.0514428414943,145.306249999429,
2.46189346052968E-15));
#286809=CARTESIAN_POINT('Ctrl Pts',(-10.0514428414943,145.456249999429,
3.26591175476071));
#286810=CARTESIAN_POINT('Ctrl Pts',(-8.13178807675729,145.606249999428,
5.90808986649102));
#286811=CARTESIAN_POINT('Ctrl Pts',(-6.21213331202031,145.756249999427,
8.55026797822134));
#286812=CARTESIAN_POINT('Ctrl Pts',(-3.1060666560102,145.906249999427,9.5594902125713));
#286813=CARTESIAN_POINT('Ctrl Pts',(-9.46504282082408E-14,146.056249999426,
10.5687124469213));
#286814=CARTESIAN_POINT('Ctrl Pts',(3.10606665601001,146.206249999426,9.5594902125713));
#286815=CARTESIAN_POINT('Ctrl Pts',(6.21213331202012,146.356249999425,8.55026797822134));
#286816=CARTESIAN_POINT('Ctrl Pts',(8.13178807675709,146.506249999424,5.90808986649102));
#286817=CARTESIAN_POINT('Ctrl Pts',(10.0514428414941,146.656249999424,3.2659117547607));
#286818=CARTESIAN_POINT('Ctrl Pts',(10.0514428414941,146.806249999423,-1.23094673026484E-15));
#286819=CARTESIAN_POINT('Ctrl Pts',(10.0514428414941,146.956249999423,-3.26591175476071));
#286820=CARTESIAN_POINT('Ctrl Pts',(8.13178807675709,147.106249999422,-5.90808986649102));
#286821=CARTESIAN_POINT('Ctrl Pts',(6.21213331202012,147.256249999421,-8.55026797822134));
#286822=CARTESIAN_POINT('Ctrl Pts',(3.10606665601001,147.406249999421,-9.5594902125713));
#286823=CARTESIAN_POINT('Ctrl Pts',(-9.81028708179179E-14,147.55624999942,
-10.5687124469213));
#286824=CARTESIAN_POINT('Ctrl Pts',(-3.10606665601021,147.70624999942,-9.5594902125713));
#286825=CARTESIAN_POINT('Ctrl Pts',(-6.21213331202032,147.856249999419,
-8.55026797822134));
#286826=CARTESIAN_POINT('Ctrl Pts',(-8.13178807675729,148.006249999418,
-5.90808986649102));
#286827=CARTESIAN_POINT('Ctrl Pts',(-10.0514428414943,148.156249999418,
-3.2659117547607));
#286828=CARTESIAN_POINT('Ctrl Pts',(-10.0514428414943,148.306249999417,
2.46189346052968E-15));
#286829=CARTESIAN_POINT('Ctrl Pts',(-10.0514428414943,148.456249999417,
3.26591175476071));
#286830=CARTESIAN_POINT('Ctrl Pts',(-8.13178807675729,148.606249999416,
5.90808986649102));
#286831=CARTESIAN_POINT('Ctrl Pts',(-6.21213331202031,148.756249999415,
8.55026797822134));
#286832=CARTESIAN_POINT('Ctrl Pts',(-3.1060666560102,148.906249999415,9.5594902125713));
#286833=CARTESIAN_POINT('Ctrl Pts',(-9.63781374799026E-14,149.056249999414,
10.5687124469213));
#286834=CARTESIAN_POINT('Ctrl Pts',(3.10606665601001,149.206249999414,9.5594902125713));
#286835=CARTESIAN_POINT('Ctrl Pts',(6.21213331202012,149.356249999413,8.55026797822134));
#286836=CARTESIAN_POINT('Ctrl Pts',(8.13178807675709,149.506249999412,5.90808986649102));
#286837=CARTESIAN_POINT('Ctrl Pts',(10.0514428414941,149.656249999412,3.2659117547607));
#286838=CARTESIAN_POINT('Ctrl Pts',(10.0514428414941,149.806249999411,-1.23094673026484E-15));
#286839=CARTESIAN_POINT('Ctrl Pts',(10.0514428414941,149.956249999411,-3.26591175476071));
#286840=CARTESIAN_POINT('Ctrl Pts',(8.13178807675709,150.10624999941,-5.90808986649102));
#286841=CARTESIAN_POINT('Ctrl Pts',(6.21213331202012,150.256249999409,-8.55026797822134));
#286842=CARTESIAN_POINT('Ctrl Pts',(3.10606665601001,150.406249999409,-9.5594902125713));
#286843=CARTESIAN_POINT('Ctrl Pts',(-9.98305800895797E-14,150.556249999408,
-10.5687124469213));
#286844=CARTESIAN_POINT('Ctrl Pts',(-3.10606665601021,150.706249999408,
-9.5594902125713));
#286845=CARTESIAN_POINT('Ctrl Pts',(-6.21213331202032,150.856249999407,
-8.55026797822134));
#286846=CARTESIAN_POINT('Ctrl Pts',(-8.13178807675729,151.006249999406,
-5.90808986649102));
#286847=CARTESIAN_POINT('Ctrl Pts',(-10.0514428414943,151.156249999406,
-3.2659117547607));
#286848=CARTESIAN_POINT('Ctrl Pts',(-10.0514428414943,151.306249999405,
2.46189346052968E-15));
#286849=CARTESIAN_POINT('Ctrl Pts',(-10.0514428414943,151.456249999405,
3.26591175476071));
#286850=CARTESIAN_POINT('Ctrl Pts',(-8.13178807675729,151.606249999404,
5.90808986649102));
#286851=CARTESIAN_POINT('Ctrl Pts',(-6.21213331202032,151.756249999403,
8.55026797822134));
#286852=CARTESIAN_POINT('Ctrl Pts',(-3.10606665601021,151.906249999403,
9.5594902125713));
#286853=CARTESIAN_POINT('Ctrl Pts',(-9.81058467515645E-14,152.056249999402,
10.5687124469213));
#286854=CARTESIAN_POINT('Ctrl Pts',(3.10606665601001,152.206249999402,9.5594902125713));
#286855=CARTESIAN_POINT('Ctrl Pts',(6.21213331202012,152.356249999401,8.55026797822134));
#286856=CARTESIAN_POINT('Ctrl Pts',(8.13178807675709,152.5062499994,5.90808986649102));
#286857=CARTESIAN_POINT('Ctrl Pts',(10.0514428414941,152.6562499994,3.2659117547607));
#286858=CARTESIAN_POINT('Ctrl Pts',(10.0514428414941,152.806249999399,-1.23094673026484E-15));
#286859=CARTESIAN_POINT('Ctrl Pts',(10.0514428414941,152.956249999399,-3.26591175476071));
#286860=CARTESIAN_POINT('Ctrl Pts',(8.13178807675709,153.106249999398,-5.90808986649102));
#286861=CARTESIAN_POINT('Ctrl Pts',(6.21213331202012,153.256249999397,-8.55026797822134));
#286862=CARTESIAN_POINT('Ctrl Pts',(3.10606665601001,153.406249999397,-9.5594902125713));
#286863=CARTESIAN_POINT('Ctrl Pts',(-1.01558289361242E-13,153.556249999396,
-10.5687124469213));
#286864=CARTESIAN_POINT('Ctrl Pts',(-3.10606665601021,153.706249999396,
-9.5594902125713));
#286865=CARTESIAN_POINT('Ctrl Pts',(-12.1623797632097,-0.474999999988005,
2.97892388940585E-15));
#286866=CARTESIAN_POINT('Ctrl Pts',(-12.1623797632096,-0.324999999988605,
3.95179673813133));
#286867=CARTESIAN_POINT('Ctrl Pts',(-9.83957192047856,-0.174999999989203,
7.14886745759505));
#286868=CARTESIAN_POINT('Ctrl Pts',(-7.51676407774747,-0.0249999999898023,
10.3459381770588));
#286869=CARTESIAN_POINT('Ctrl Pts',(-3.75838203887374,0.1250000000096,11.5671105274568));
#286870=CARTESIAN_POINT('Ctrl Pts',(-1.02868273148643E-14,0.275000000009002,
12.7882828778549));
#286871=CARTESIAN_POINT('Ctrl Pts',(3.75838203887372,0.425000000008404,
11.5671105274568));
#286872=CARTESIAN_POINT('Ctrl Pts',(7.51676407774745,0.575000000007806,
10.3459381770588));
#286873=CARTESIAN_POINT('Ctrl Pts',(9.83957192047854,0.725000000007208,
7.14886745759505));
#286874=CARTESIAN_POINT('Ctrl Pts',(12.1623797632096,0.875000000006609,
3.95179673813132));
#286875=CARTESIAN_POINT('Ctrl Pts',(12.1623797632096,1.02500000000601,-1.48946194470292E-15));
#286876=CARTESIAN_POINT('Ctrl Pts',(12.1623797632096,1.17500000000541,-3.95179673813132));
#286877=CARTESIAN_POINT('Ctrl Pts',(9.83957192047853,1.32500000000481,-7.14886745759505));
#286878=CARTESIAN_POINT('Ctrl Pts',(7.51676407774744,1.47500000000421,-10.3459381770588));
#286879=CARTESIAN_POINT('Ctrl Pts',(3.75838203887371,1.6250000000036,-11.5671105274568));
#286880=CARTESIAN_POINT('Ctrl Pts',(-1.42829078892864E-14,1.775000000003,
-12.7882828778549));
#286881=CARTESIAN_POINT('Ctrl Pts',(-3.75838203887374,1.9250000000024,-11.5671105274568));
#286882=CARTESIAN_POINT('Ctrl Pts',(-7.51676407774747,2.0750000000018,-10.3459381770588));
#286883=CARTESIAN_POINT('Ctrl Pts',(-9.83957192047856,2.2250000000012,-7.14886745759505));
#286884=CARTESIAN_POINT('Ctrl Pts',(-12.1623797632097,2.37500000000059,
-3.95179673813132));
#286885=CARTESIAN_POINT('Ctrl Pts',(-12.1623797632097,2.525,2.97892388940585E-15));
#286886=CARTESIAN_POINT('Ctrl Pts',(-12.1623797632097,2.6749999999994,3.95179673813133));
#286887=CARTESIAN_POINT('Ctrl Pts',(-9.83957192047856,2.8249999999988,7.14886745759505));
#286888=CARTESIAN_POINT('Ctrl Pts',(-7.51676407774747,2.9749999999982,10.3459381770588));
#286889=CARTESIAN_POINT('Ctrl Pts',(-3.75838203887374,3.1249999999976,11.5671105274568));
#286890=CARTESIAN_POINT('Ctrl Pts',(-1.20145365865262E-14,3.274999999997,
12.7882828778549));
#286891=CARTESIAN_POINT('Ctrl Pts',(3.75838203887372,3.4249999999964,11.5671105274568));
#286892=CARTESIAN_POINT('Ctrl Pts',(7.51676407774744,3.57499999999581,10.3459381770588));
#286893=CARTESIAN_POINT('Ctrl Pts',(9.83957192047853,3.72499999999521,7.14886745759505));
#286894=CARTESIAN_POINT('Ctrl Pts',(12.1623797632096,3.87499999999461,3.95179673813132));
#286895=CARTESIAN_POINT('Ctrl Pts',(12.1623797632096,4.02499999999401,-1.48946194470292E-15));
#286896=CARTESIAN_POINT('Ctrl Pts',(12.1623797632096,4.17499999999341,-3.95179673813132));
#286897=CARTESIAN_POINT('Ctrl Pts',(9.83957192047853,4.32499999999281,-7.14886745759505));
#286898=CARTESIAN_POINT('Ctrl Pts',(7.51676407774744,4.47499999999221,-10.3459381770588));
#286899=CARTESIAN_POINT('Ctrl Pts',(3.75838203887371,4.6249999999916,-11.5671105274568));
#286900=CARTESIAN_POINT('Ctrl Pts',(-1.60106171609483E-14,4.774999999991,
-12.7882828778549));
#286901=CARTESIAN_POINT('Ctrl Pts',(-3.75838203887374,4.9249999999904,-11.5671105274568));
#286902=CARTESIAN_POINT('Ctrl Pts',(-7.51676407774747,5.0749999999898,-10.3459381770588));
#286903=CARTESIAN_POINT('Ctrl Pts',(-9.83957192047857,5.2249999999892,-7.14886745759505));
#286904=CARTESIAN_POINT('Ctrl Pts',(-12.1623797632097,5.3749999999886,-3.95179673813132));
#286905=CARTESIAN_POINT('Ctrl Pts',(-12.1623797632097,5.52499999998799,
2.97892388940585E-15));
#286906=CARTESIAN_POINT('Ctrl Pts',(-12.1623797632097,5.6749999999874,3.95179673813133));
#286907=CARTESIAN_POINT('Ctrl Pts',(-9.83957192047857,5.8249999999868,7.14886745759505));
#286908=CARTESIAN_POINT('Ctrl Pts',(-7.51676407774747,5.9749999999862,10.3459381770588));
#286909=CARTESIAN_POINT('Ctrl Pts',(-3.75838203887374,6.1249999999856,11.5671105274568));
#286910=CARTESIAN_POINT('Ctrl Pts',(-1.3742245858188E-14,6.274999999985,
12.7882828778549));
#286911=CARTESIAN_POINT('Ctrl Pts',(3.75838203887371,6.4249999999844,11.5671105274568));
#286912=CARTESIAN_POINT('Ctrl Pts',(7.51676407774744,6.57499999998381,10.3459381770588));
#286913=CARTESIAN_POINT('Ctrl Pts',(9.83957192047853,6.72499999998321,7.14886745759505));
#286914=CARTESIAN_POINT('Ctrl Pts',(12.1623797632096,6.87499999998261,3.95179673813132));
#286915=CARTESIAN_POINT('Ctrl Pts',(12.1623797632096,7.02499999998201,-1.48946194470292E-15));
#286916=CARTESIAN_POINT('Ctrl Pts',(12.1623797632096,7.17499999998141,-3.95179673813132));
#286917=CARTESIAN_POINT('Ctrl Pts',(9.83957192047853,7.32499999998081,-7.14886745759505));
#286918=CARTESIAN_POINT('Ctrl Pts',(7.51676407774744,7.47499999998021,-10.3459381770588));
#286919=CARTESIAN_POINT('Ctrl Pts',(3.75838203887371,7.6249999999796,-11.5671105274568));
#286920=CARTESIAN_POINT('Ctrl Pts',(-1.77383264326101E-14,7.774999999979,
-12.7882828778549));
#286921=CARTESIAN_POINT('Ctrl Pts',(-3.75838203887375,7.9249999999784,-11.5671105274568));
#286922=CARTESIAN_POINT('Ctrl Pts',(-7.51676407774747,8.0749999999778,-10.3459381770588));
#286923=CARTESIAN_POINT('Ctrl Pts',(-9.83957192047857,8.2249999999772,-7.14886745759505));
#286924=CARTESIAN_POINT('Ctrl Pts',(-12.1623797632097,8.3749999999766,-3.95179673813132));
#286925=CARTESIAN_POINT('Ctrl Pts',(-12.1623797632097,8.52499999997599,
2.97892388940585E-15));
#286926=CARTESIAN_POINT('Ctrl Pts',(-12.1623797632097,8.6749999999754,3.95179673813133));
#286927=CARTESIAN_POINT('Ctrl Pts',(-9.83957192047857,8.8249999999748,7.14886745759505));
#286928=CARTESIAN_POINT('Ctrl Pts',(-7.51676407774747,8.9749999999742,10.3459381770588));
#286929=CARTESIAN_POINT('Ctrl Pts',(-3.75838203887374,9.1249999999736,11.5671105274568));
#286930=CARTESIAN_POINT('Ctrl Pts',(-1.54699551298498E-14,9.274999999973,
12.7882828778549));
#286931=CARTESIAN_POINT('Ctrl Pts',(3.75838203887371,9.4249999999724,11.5671105274568));
#286932=CARTESIAN_POINT('Ctrl Pts',(7.51676407774744,9.57499999997181,10.3459381770588));
#286933=CARTESIAN_POINT('Ctrl Pts',(9.83957192047853,9.72499999997121,7.14886745759505));
#286934=CARTESIAN_POINT('Ctrl Pts',(12.1623797632096,9.87499999997061,3.95179673813132));
#286935=CARTESIAN_POINT('Ctrl Pts',(12.1623797632096,10.02499999997,-1.48946194470292E-15));
#286936=CARTESIAN_POINT('Ctrl Pts',(12.1623797632096,10.1749999999694,-3.95179673813132));
#286937=CARTESIAN_POINT('Ctrl Pts',(9.83957192047853,10.3249999999688,-7.14886745759505));
#286938=CARTESIAN_POINT('Ctrl Pts',(7.51676407774744,10.4749999999682,-10.3459381770588));
#286939=CARTESIAN_POINT('Ctrl Pts',(3.75838203887371,10.6249999999676,-11.5671105274568));
#286940=CARTESIAN_POINT('Ctrl Pts',(-1.9466035704272E-14,10.774999999967,
-12.7882828778549));
#286941=CARTESIAN_POINT('Ctrl Pts',(-3.75838203887375,10.9249999999664,
-11.5671105274568));
#286942=CARTESIAN_POINT('Ctrl Pts',(-7.51676407774748,11.0749999999658,
-10.3459381770588));
#286943=CARTESIAN_POINT('Ctrl Pts',(-9.83957192047857,11.2249999999652,
-7.14886745759505));
#286944=CARTESIAN_POINT('Ctrl Pts',(-12.1623797632097,11.3749999999646,
-3.95179673813132));
#286945=CARTESIAN_POINT('Ctrl Pts',(-12.1623797632097,11.524999999964,2.97892388940585E-15));
#286946=CARTESIAN_POINT('Ctrl Pts',(-12.1623797632097,11.6749999999634,
3.95179673813133));
#286947=CARTESIAN_POINT('Ctrl Pts',(-9.83957192047857,11.8249999999628,
7.14886745759505));
#286948=CARTESIAN_POINT('Ctrl Pts',(-7.51676407774747,11.9749999999622,
10.3459381770588));
#286949=CARTESIAN_POINT('Ctrl Pts',(-3.75838203887375,12.1249999999616,
11.5671105274568));
#286950=CARTESIAN_POINT('Ctrl Pts',(-1.71976644015117E-14,12.274999999961,
12.7882828778549));
#286951=CARTESIAN_POINT('Ctrl Pts',(3.75838203887371,12.4249999999604,11.5671105274568));
#286952=CARTESIAN_POINT('Ctrl Pts',(7.51676407774744,12.5749999999598,10.3459381770588));
#286953=CARTESIAN_POINT('Ctrl Pts',(9.83957192047853,12.7249999999592,7.14886745759505));
#286954=CARTESIAN_POINT('Ctrl Pts',(12.1623797632096,12.8749999999586,3.95179673813132));
#286955=CARTESIAN_POINT('Ctrl Pts',(12.1623797632096,13.024999999958,-1.48946194470292E-15));
#286956=CARTESIAN_POINT('Ctrl Pts',(12.1623797632096,13.1749999999574,-3.95179673813132));
#286957=CARTESIAN_POINT('Ctrl Pts',(9.83957192047853,13.3249999999568,-7.14886745759505));
#286958=CARTESIAN_POINT('Ctrl Pts',(7.51676407774743,13.4749999999562,-10.3459381770588));
#286959=CARTESIAN_POINT('Ctrl Pts',(3.75838203887371,13.6249999999556,-11.5671105274568));
#286960=CARTESIAN_POINT('Ctrl Pts',(-2.11937449759338E-14,13.774999999955,
-12.7882828778549));
#286961=CARTESIAN_POINT('Ctrl Pts',(-3.75838203887375,13.9249999999544,
-11.5671105274568));
#286962=CARTESIAN_POINT('Ctrl Pts',(-7.51676407774748,14.0749999999538,
-10.3459381770588));
#286963=CARTESIAN_POINT('Ctrl Pts',(-9.83957192047857,14.2249999999532,
-7.14886745759505));
#286964=CARTESIAN_POINT('Ctrl Pts',(-12.1623797632097,14.3749999999526,
-3.95179673813132));
#286965=CARTESIAN_POINT('Ctrl Pts',(-12.1623797632097,14.524999999952,2.97892388940585E-15));
#286966=CARTESIAN_POINT('Ctrl Pts',(-12.1623797632097,14.6749999999514,
3.95179673813133));
#286967=CARTESIAN_POINT('Ctrl Pts',(-9.83957192047857,14.8249999999508,
7.14886745759505));
#286968=CARTESIAN_POINT('Ctrl Pts',(-7.51676407774747,14.9749999999502,
10.3459381770588));
#286969=CARTESIAN_POINT('Ctrl Pts',(-3.75838203887375,15.1249999999496,
11.5671105274568));
#286970=CARTESIAN_POINT('Ctrl Pts',(-1.89253736731735E-14,15.274999999949,
12.7882828778549));
#286971=CARTESIAN_POINT('Ctrl Pts',(3.75838203887371,15.4249999999484,11.5671105274568));
#286972=CARTESIAN_POINT('Ctrl Pts',(7.51676407774744,15.5749999999478,10.3459381770588));
#286973=CARTESIAN_POINT('Ctrl Pts',(9.83957192047853,15.7249999999472,7.14886745759505));
#286974=CARTESIAN_POINT('Ctrl Pts',(12.1623797632096,15.8749999999466,3.95179673813132));
#286975=CARTESIAN_POINT('Ctrl Pts',(12.1623797632096,16.024999999946,-1.48946194470292E-15));
#286976=CARTESIAN_POINT('Ctrl Pts',(12.1623797632096,16.1749999999454,-3.95179673813132));
#286977=CARTESIAN_POINT('Ctrl Pts',(9.83957192047852,16.3249999999448,-7.14886745759505));
#286978=CARTESIAN_POINT('Ctrl Pts',(7.51676407774743,16.4749999999442,-10.3459381770588));
#286979=CARTESIAN_POINT('Ctrl Pts',(3.7583820388737,16.6249999999436,-11.5671105274568));
#286980=CARTESIAN_POINT('Ctrl Pts',(-2.29214542475956E-14,16.774999999943,
-12.7882828778549));
#286981=CARTESIAN_POINT('Ctrl Pts',(-3.75838203887375,16.9249999999424,
-11.5671105274568));
#286982=CARTESIAN_POINT('Ctrl Pts',(-7.51676407774748,17.0749999999418,
-10.3459381770588));
#286983=CARTESIAN_POINT('Ctrl Pts',(-9.83957192047857,17.2249999999412,
-7.14886745759505));
#286984=CARTESIAN_POINT('Ctrl Pts',(-12.1623797632097,17.3749999999406,
-3.95179673813132));
#286985=CARTESIAN_POINT('Ctrl Pts',(-12.1623797632097,17.52499999994,2.97892388940585E-15));
#286986=CARTESIAN_POINT('Ctrl Pts',(-12.1623797632097,17.6749999999394,
3.95179673813133));
#286987=CARTESIAN_POINT('Ctrl Pts',(-9.83957192047857,17.8249999999388,
7.14886745759505));
#286988=CARTESIAN_POINT('Ctrl Pts',(-7.51676407774748,17.9749999999382,
10.3459381770588));
#286989=CARTESIAN_POINT('Ctrl Pts',(-3.75838203887375,18.1249999999376,
11.5671105274568));
#286990=CARTESIAN_POINT('Ctrl Pts',(-2.06530829448354E-14,18.274999999937,
12.7882828778549));
#286991=CARTESIAN_POINT('Ctrl Pts',(3.75838203887371,18.4249999999364,11.5671105274568));
#286992=CARTESIAN_POINT('Ctrl Pts',(7.51676407774743,18.5749999999358,10.3459381770588));
#286993=CARTESIAN_POINT('Ctrl Pts',(9.83957192047852,18.7249999999352,7.14886745759505));
#286994=CARTESIAN_POINT('Ctrl Pts',(12.1623797632096,18.8749999999346,3.95179673813132));
#286995=CARTESIAN_POINT('Ctrl Pts',(12.1623797632096,19.024999999934,-1.48946194470292E-15));
#286996=CARTESIAN_POINT('Ctrl Pts',(12.1623797632096,19.1749999999334,-3.95179673813132));
#286997=CARTESIAN_POINT('Ctrl Pts',(9.83957192047852,19.3249999999328,-7.14886745759505));
#286998=CARTESIAN_POINT('Ctrl Pts',(7.51676407774743,19.4749999999322,-10.3459381770588));
#286999=CARTESIAN_POINT('Ctrl Pts',(3.7583820388737,19.6249999999316,-11.5671105274568));
#287000=CARTESIAN_POINT('Ctrl Pts',(-2.46491635192575E-14,19.774999999931,
-12.7882828778549));
#287001=CARTESIAN_POINT('Ctrl Pts',(-3.75838203887375,19.9249999999304,
-11.5671105274568));
#287002=CARTESIAN_POINT('Ctrl Pts',(-7.51676407774748,20.0749999999298,
-10.3459381770588));
#287003=CARTESIAN_POINT('Ctrl Pts',(-9.83957192047857,20.2249999999292,
-7.14886745759505));
#287004=CARTESIAN_POINT('Ctrl Pts',(-12.1623797632097,20.3749999999286,
-3.95179673813132));
#287005=CARTESIAN_POINT('Ctrl Pts',(-12.1623797632097,20.524999999928,2.97892388940585E-15));
#287006=CARTESIAN_POINT('Ctrl Pts',(-12.1623797632097,20.6749999999274,
3.95179673813133));
#287007=CARTESIAN_POINT('Ctrl Pts',(-9.83957192047857,20.8249999999268,
7.14886745759505));
#287008=CARTESIAN_POINT('Ctrl Pts',(-7.51676407774748,20.9749999999262,
10.3459381770588));
#287009=CARTESIAN_POINT('Ctrl Pts',(-3.75838203887375,21.1249999999256,
11.5671105274568));
#287010=CARTESIAN_POINT('Ctrl Pts',(-2.23807922164972E-14,21.274999999925,
12.7882828778549));
#287011=CARTESIAN_POINT('Ctrl Pts',(3.7583820388737,21.4249999999244,11.5671105274568));
#287012=CARTESIAN_POINT('Ctrl Pts',(7.51676407774743,21.5749999999238,10.3459381770588));
#287013=CARTESIAN_POINT('Ctrl Pts',(9.83957192047852,21.7249999999232,7.14886745759505));
#287014=CARTESIAN_POINT('Ctrl Pts',(12.1623797632096,21.8749999999226,3.95179673813132));
#287015=CARTESIAN_POINT('Ctrl Pts',(12.1623797632096,22.024999999922,-1.48946194470292E-15));
#287016=CARTESIAN_POINT('Ctrl Pts',(12.1623797632096,22.1749999999214,-3.95179673813132));
#287017=CARTESIAN_POINT('Ctrl Pts',(9.83957192047852,22.3249999999208,-7.14886745759505));
#287018=CARTESIAN_POINT('Ctrl Pts',(7.51676407774743,22.4749999999202,-10.3459381770588));
#287019=CARTESIAN_POINT('Ctrl Pts',(3.7583820388737,22.6249999999196,-11.5671105274568));
#287020=CARTESIAN_POINT('Ctrl Pts',(-2.63768727909193E-14,22.774999999919,
-12.7882828778549));
#287021=CARTESIAN_POINT('Ctrl Pts',(-3.75838203887375,22.9249999999184,
-11.5671105274568));
#287022=CARTESIAN_POINT('Ctrl Pts',(-7.51676407774748,23.0749999999178,
-10.3459381770588));
#287023=CARTESIAN_POINT('Ctrl Pts',(-9.83957192047857,23.2249999999172,
-7.14886745759505));
#287024=CARTESIAN_POINT('Ctrl Pts',(-12.1623797632097,23.3749999999166,
-3.95179673813132));
#287025=CARTESIAN_POINT('Ctrl Pts',(-12.1623797632097,23.524999999916,2.97892388940585E-15));
#287026=CARTESIAN_POINT('Ctrl Pts',(-12.1623797632097,23.6749999999154,
3.95179673813133));
#287027=CARTESIAN_POINT('Ctrl Pts',(-9.83957192047857,23.8249999999148,
7.14886745759505));
#287028=CARTESIAN_POINT('Ctrl Pts',(-7.51676407774748,23.9749999999142,
10.3459381770588));
#287029=CARTESIAN_POINT('Ctrl Pts',(-3.75838203887375,24.1249999999136,
11.5671105274568));
#287030=CARTESIAN_POINT('Ctrl Pts',(-2.4108501488159E-14,24.274999999913,
12.7882828778549));
#287031=CARTESIAN_POINT('Ctrl Pts',(3.7583820388737,24.4249999999124,11.5671105274568));
#287032=CARTESIAN_POINT('Ctrl Pts',(7.51676407774743,24.5749999999118,10.3459381770588));
#287033=CARTESIAN_POINT('Ctrl Pts',(9.83957192047852,24.7249999999112,7.14886745759505));
#287034=CARTESIAN_POINT('Ctrl Pts',(12.1623797632096,24.8749999999106,3.95179673813132));
#287035=CARTESIAN_POINT('Ctrl Pts',(12.1623797632096,25.02499999991,-1.48946194470292E-15));
#287036=CARTESIAN_POINT('Ctrl Pts',(12.1623797632096,25.1749999999094,-3.95179673813132));
#287037=CARTESIAN_POINT('Ctrl Pts',(9.83957192047852,25.3249999999088,-7.14886745759505));
#287038=CARTESIAN_POINT('Ctrl Pts',(7.51676407774743,25.4749999999082,-10.3459381770588));
#287039=CARTESIAN_POINT('Ctrl Pts',(3.7583820388737,25.6249999999076,-11.5671105274568));
#287040=CARTESIAN_POINT('Ctrl Pts',(-2.81045820625811E-14,25.774999999907,
-12.7882828778549));
#287041=CARTESIAN_POINT('Ctrl Pts',(-3.75838203887376,25.9249999999064,
-11.5671105274568));
#287042=CARTESIAN_POINT('Ctrl Pts',(-7.51676407774749,26.0749999999058,
-10.3459381770588));
#287043=CARTESIAN_POINT('Ctrl Pts',(-9.83957192047857,26.2249999999052,
-7.14886745759505));
#287044=CARTESIAN_POINT('Ctrl Pts',(-12.1623797632097,26.3749999999046,
-3.95179673813132));
#287045=CARTESIAN_POINT('Ctrl Pts',(-12.1623797632097,26.524999999904,2.97892388940585E-15));
#287046=CARTESIAN_POINT('Ctrl Pts',(-12.1623797632097,26.6749999999034,
3.95179673813133));
#287047=CARTESIAN_POINT('Ctrl Pts',(-9.83957192047857,26.8249999999028,
7.14886745759505));
#287048=CARTESIAN_POINT('Ctrl Pts',(-7.51676407774748,26.9749999999022,
10.3459381770588));
#287049=CARTESIAN_POINT('Ctrl Pts',(-3.75838203887375,27.1249999999016,
11.5671105274568));
#287050=CARTESIAN_POINT('Ctrl Pts',(-2.58362107598209E-14,27.274999999901,
12.7882828778549));
#287051=CARTESIAN_POINT('Ctrl Pts',(3.7583820388737,27.4249999999004,11.5671105274568));
#287052=CARTESIAN_POINT('Ctrl Pts',(7.51676407774743,27.5749999998998,10.3459381770588));
#287053=CARTESIAN_POINT('Ctrl Pts',(9.83957192047852,27.7249999998992,7.14886745759505));
#287054=CARTESIAN_POINT('Ctrl Pts',(12.1623797632096,27.8749999998986,3.95179673813132));
#287055=CARTESIAN_POINT('Ctrl Pts',(12.1623797632096,28.024999999898,-1.48946194470292E-15));
#287056=CARTESIAN_POINT('Ctrl Pts',(12.1623797632096,28.1749999998974,-3.95179673813132));
#287057=CARTESIAN_POINT('Ctrl Pts',(9.83957192047852,28.3249999998968,-7.14886745759505));
#287058=CARTESIAN_POINT('Ctrl Pts',(7.51676407774743,28.4749999998962,-10.3459381770588));
#287059=CARTESIAN_POINT('Ctrl Pts',(3.7583820388737,28.6249999998956,-11.5671105274568));
#287060=CARTESIAN_POINT('Ctrl Pts',(-2.9832291334243E-14,28.774999999895,
-12.7882828778549));
#287061=CARTESIAN_POINT('Ctrl Pts',(-3.75838203887376,28.9249999998944,
-11.5671105274568));
#287062=CARTESIAN_POINT('Ctrl Pts',(-7.51676407774749,29.0749999998938,
-10.3459381770588));
#287063=CARTESIAN_POINT('Ctrl Pts',(-9.83957192047858,29.2249999998932,
-7.14886745759505));
#287064=CARTESIAN_POINT('Ctrl Pts',(-12.1623797632097,29.3749999998926,
-3.95179673813132));
#287065=CARTESIAN_POINT('Ctrl Pts',(-12.1623797632097,29.524999999892,2.97892388940585E-15));
#287066=CARTESIAN_POINT('Ctrl Pts',(-12.1623797632097,29.6749999998914,
3.95179673813133));
#287067=CARTESIAN_POINT('Ctrl Pts',(-9.83957192047858,29.8249999998908,
7.14886745759505));
#287068=CARTESIAN_POINT('Ctrl Pts',(-7.51676407774748,29.9749999998902,
10.3459381770588));
#287069=CARTESIAN_POINT('Ctrl Pts',(-3.75838203887376,30.1249999998896,
11.5671105274568));
#287070=CARTESIAN_POINT('Ctrl Pts',(-2.75639200314827E-14,30.274999999889,
12.7882828778549));
#287071=CARTESIAN_POINT('Ctrl Pts',(3.7583820388737,30.4249999998884,11.5671105274568));
#287072=CARTESIAN_POINT('Ctrl Pts',(7.51676407774743,30.5749999998878,10.3459381770588));
#287073=CARTESIAN_POINT('Ctrl Pts',(9.83957192047852,30.7249999998872,7.14886745759505));
#287074=CARTESIAN_POINT('Ctrl Pts',(12.1623797632096,30.8749999998866,3.95179673813132));
#287075=CARTESIAN_POINT('Ctrl Pts',(12.1623797632096,31.024999999886,-1.48946194470292E-15));
#287076=CARTESIAN_POINT('Ctrl Pts',(12.1623797632096,31.1749999998854,-3.95179673813132));
#287077=CARTESIAN_POINT('Ctrl Pts',(9.83957192047852,31.3249999998848,-7.14886745759505));
#287078=CARTESIAN_POINT('Ctrl Pts',(7.51676407774742,31.4749999998842,-10.3459381770588));
#287079=CARTESIAN_POINT('Ctrl Pts',(3.7583820388737,31.6249999998836,-11.5671105274568));
#287080=CARTESIAN_POINT('Ctrl Pts',(-3.15600006059048E-14,31.774999999883,
-12.7882828778549));
#287081=CARTESIAN_POINT('Ctrl Pts',(-3.75838203887376,31.9249999998824,
-11.5671105274568));
#287082=CARTESIAN_POINT('Ctrl Pts',(-7.51676407774749,32.0749999998818,
-10.3459381770588));
#287083=CARTESIAN_POINT('Ctrl Pts',(-9.83957192047858,32.2249999998812,
-7.14886745759505));
#287084=CARTESIAN_POINT('Ctrl Pts',(-12.1623797632097,32.3749999998806,
-3.95179673813132));
#287085=CARTESIAN_POINT('Ctrl Pts',(-12.1623797632097,32.52499999988,2.97892388940585E-15));
#287086=CARTESIAN_POINT('Ctrl Pts',(-12.1623797632097,32.6749999998794,
3.95179673813133));
#287087=CARTESIAN_POINT('Ctrl Pts',(-9.83957192047858,32.8249999998788,
7.14886745759505));
#287088=CARTESIAN_POINT('Ctrl Pts',(-7.51676407774749,32.9749999998782,
10.3459381770588));
#287089=CARTESIAN_POINT('Ctrl Pts',(-3.75838203887376,33.1249999998776,
11.5671105274568));
#287090=CARTESIAN_POINT('Ctrl Pts',(-2.92916293031446E-14,33.274999999877,
12.7882828778549));
#287091=CARTESIAN_POINT('Ctrl Pts',(3.7583820388737,33.4249999998764,11.5671105274568));
#287092=CARTESIAN_POINT('Ctrl Pts',(7.51676407774743,33.5749999998758,10.3459381770588));
#287093=CARTESIAN_POINT('Ctrl Pts',(9.83957192047852,33.7249999998752,7.14886745759505));
#287094=CARTESIAN_POINT('Ctrl Pts',(12.1623797632096,33.8749999998746,3.95179673813132));
#287095=CARTESIAN_POINT('Ctrl Pts',(12.1623797632096,34.024999999874,-1.48946194470292E-15));
#287096=CARTESIAN_POINT('Ctrl Pts',(12.1623797632096,34.1749999998734,-3.95179673813132));
#287097=CARTESIAN_POINT('Ctrl Pts',(9.83957192047851,34.3249999998728,-7.14886745759505));
#287098=CARTESIAN_POINT('Ctrl Pts',(7.51676407774742,34.4749999998722,-10.3459381770588));
#287099=CARTESIAN_POINT('Ctrl Pts',(3.7583820388737,34.6249999998716,-11.5671105274568));
#287100=CARTESIAN_POINT('Ctrl Pts',(-3.32877098775667E-14,34.774999999871,
-12.7882828778549));
#287101=CARTESIAN_POINT('Ctrl Pts',(-3.75838203887376,34.9249999998704,
-11.5671105274568));
#287102=CARTESIAN_POINT('Ctrl Pts',(-7.51676407774749,35.0749999998698,
-10.3459381770588));
#287103=CARTESIAN_POINT('Ctrl Pts',(-9.83957192047858,35.2249999998692,
-7.14886745759505));
#287104=CARTESIAN_POINT('Ctrl Pts',(-12.1623797632097,35.3749999998686,
-3.95179673813132));
#287105=CARTESIAN_POINT('Ctrl Pts',(-12.1623797632097,35.524999999868,2.97892388940585E-15));
#287106=CARTESIAN_POINT('Ctrl Pts',(-12.1623797632097,35.6749999998674,
3.95179673813133));
#287107=CARTESIAN_POINT('Ctrl Pts',(-9.83957192047858,35.8249999998668,
7.14886745759505));
#287108=CARTESIAN_POINT('Ctrl Pts',(-7.51676407774749,35.9749999998662,
10.3459381770588));
#287109=CARTESIAN_POINT('Ctrl Pts',(-3.75838203887376,36.1249999998656,
11.5671105274568));
#287110=CARTESIAN_POINT('Ctrl Pts',(-3.10193385748064E-14,36.274999999865,
12.7882828778549));
#287111=CARTESIAN_POINT('Ctrl Pts',(3.7583820388737,36.4249999998644,11.5671105274568));
#287112=CARTESIAN_POINT('Ctrl Pts',(7.51676407774742,36.5749999998638,10.3459381770588));
#287113=CARTESIAN_POINT('Ctrl Pts',(9.83957192047851,36.7249999998632,7.14886745759505));
#287114=CARTESIAN_POINT('Ctrl Pts',(12.1623797632096,36.8749999998626,3.95179673813132));
#287115=CARTESIAN_POINT('Ctrl Pts',(12.1623797632096,37.024999999862,-1.48946194470292E-15));
#287116=CARTESIAN_POINT('Ctrl Pts',(12.1623797632096,37.1749999998614,-3.95179673813132));
#287117=CARTESIAN_POINT('Ctrl Pts',(9.83957192047851,37.3249999998608,-7.14886745759505));
#287118=CARTESIAN_POINT('Ctrl Pts',(7.51676407774742,37.4749999998602,-10.3459381770588));
#287119=CARTESIAN_POINT('Ctrl Pts',(3.75838203887369,37.6249999998596,-11.5671105274568));
#287120=CARTESIAN_POINT('Ctrl Pts',(-3.50154191492285E-14,37.774999999859,
-12.7882828778549));
#287121=CARTESIAN_POINT('Ctrl Pts',(-3.75838203887376,37.9249999998584,
-11.5671105274568));
#287122=CARTESIAN_POINT('Ctrl Pts',(-7.51676407774749,38.0749999998578,
-10.3459381770588));
#287123=CARTESIAN_POINT('Ctrl Pts',(-9.83957192047858,38.2249999998572,
-7.14886745759505));
#287124=CARTESIAN_POINT('Ctrl Pts',(-12.1623797632097,38.3749999998566,
-3.95179673813132));
#287125=CARTESIAN_POINT('Ctrl Pts',(-12.1623797632097,38.524999999856,2.97892388940585E-15));
#287126=CARTESIAN_POINT('Ctrl Pts',(-12.1623797632097,38.6749999998554,
3.95179673813133));
#287127=CARTESIAN_POINT('Ctrl Pts',(-9.83957192047858,38.8249999998548,
7.14886745759505));
#287128=CARTESIAN_POINT('Ctrl Pts',(-7.51676407774749,38.9749999998542,
10.3459381770588));
#287129=CARTESIAN_POINT('Ctrl Pts',(-3.75838203887376,39.1249999998536,
11.5671105274568));
#287130=CARTESIAN_POINT('Ctrl Pts',(-3.27470478464682E-14,39.274999999853,
12.7882828778549));
#287131=CARTESIAN_POINT('Ctrl Pts',(3.7583820388737,39.4249999998524,11.5671105274568));
#287132=CARTESIAN_POINT('Ctrl Pts',(7.51676407774742,39.5749999998518,10.3459381770588));
#287133=CARTESIAN_POINT('Ctrl Pts',(9.83957192047851,39.7249999998512,7.14886745759505));
#287134=CARTESIAN_POINT('Ctrl Pts',(12.1623797632096,39.8749999998506,3.95179673813132));
#287135=CARTESIAN_POINT('Ctrl Pts',(12.1623797632096,40.02499999985,-1.48946194470292E-15));
#287136=CARTESIAN_POINT('Ctrl Pts',(12.1623797632096,40.1749999998494,-3.95179673813132));
#287137=CARTESIAN_POINT('Ctrl Pts',(9.83957192047851,40.3249999998488,-7.14886745759505));
#287138=CARTESIAN_POINT('Ctrl Pts',(7.51676407774742,40.4749999998482,-10.3459381770588));
#287139=CARTESIAN_POINT('Ctrl Pts',(3.75838203887369,40.6249999998476,-11.5671105274568));
#287140=CARTESIAN_POINT('Ctrl Pts',(-3.67431284208903E-14,40.774999999847,
-12.7882828778549));
#287141=CARTESIAN_POINT('Ctrl Pts',(-3.75838203887376,40.9249999998464,
-11.5671105274568));
#287142=CARTESIAN_POINT('Ctrl Pts',(-7.51676407774749,41.0749999998458,
-10.3459381770588));
#287143=CARTESIAN_POINT('Ctrl Pts',(-9.83957192047858,41.2249999998452,
-7.14886745759505));
#287144=CARTESIAN_POINT('Ctrl Pts',(-12.1623797632097,41.3749999998446,
-3.95179673813132));
#287145=CARTESIAN_POINT('Ctrl Pts',(-12.1623797632097,41.524999999844,2.97892388940585E-15));
#287146=CARTESIAN_POINT('Ctrl Pts',(-12.1623797632097,41.6749999998434,
3.95179673813133));
#287147=CARTESIAN_POINT('Ctrl Pts',(-9.83957192047858,41.8249999998428,
7.14886745759505));
#287148=CARTESIAN_POINT('Ctrl Pts',(-7.51676407774749,41.9749999998422,
10.3459381770588));
#287149=CARTESIAN_POINT('Ctrl Pts',(-3.75838203887376,42.1249999998416,
11.5671105274568));
#287150=CARTESIAN_POINT('Ctrl Pts',(-3.44747571181301E-14,42.274999999841,
12.7882828778549));
#287151=CARTESIAN_POINT('Ctrl Pts',(3.75838203887369,42.4249999998404,11.5671105274568));
#287152=CARTESIAN_POINT('Ctrl Pts',(7.51676407774742,42.5749999998398,10.3459381770588));
#287153=CARTESIAN_POINT('Ctrl Pts',(9.83957192047851,42.7249999998392,7.14886745759505));
#287154=CARTESIAN_POINT('Ctrl Pts',(12.1623797632096,42.8749999998386,3.95179673813132));
#287155=CARTESIAN_POINT('Ctrl Pts',(12.1623797632096,43.024999999838,-1.48946194470292E-15));
#287156=CARTESIAN_POINT('Ctrl Pts',(12.1623797632096,43.1749999998374,-3.95179673813132));
#287157=CARTESIAN_POINT('Ctrl Pts',(9.83957192047851,43.3249999998368,-7.14886745759505));
#287158=CARTESIAN_POINT('Ctrl Pts',(7.51676407774742,43.4749999998362,-10.3459381770588));
#287159=CARTESIAN_POINT('Ctrl Pts',(3.75838203887369,43.6249999998356,-11.5671105274568));
#287160=CARTESIAN_POINT('Ctrl Pts',(-3.84708376925522E-14,43.774999999835,
-12.7882828778549));
#287161=CARTESIAN_POINT('Ctrl Pts',(-3.75838203887377,43.9249999998344,
-11.5671105274568));
#287162=CARTESIAN_POINT('Ctrl Pts',(-7.51676407774749,44.0749999998338,
-10.3459381770588));
#287163=CARTESIAN_POINT('Ctrl Pts',(-9.83957192047859,44.2249999998332,
-7.14886745759505));
#287164=CARTESIAN_POINT('Ctrl Pts',(-12.1623797632097,44.3749999998326,
-3.95179673813132));
#287165=CARTESIAN_POINT('Ctrl Pts',(-12.1623797632097,44.524999999832,2.97892388940585E-15));
#287166=CARTESIAN_POINT('Ctrl Pts',(-12.1623797632097,44.6749999998314,
3.95179673813133));
#287167=CARTESIAN_POINT('Ctrl Pts',(-9.83957192047859,44.8249999998308,
7.14886745759505));
#287168=CARTESIAN_POINT('Ctrl Pts',(-7.51676407774749,44.9749999998302,
10.3459381770588));
#287169=CARTESIAN_POINT('Ctrl Pts',(-3.75838203887376,45.1249999998296,
11.5671105274568));
#287170=CARTESIAN_POINT('Ctrl Pts',(-3.62024663897919E-14,45.274999999829,
12.7882828778549));
#287171=CARTESIAN_POINT('Ctrl Pts',(3.75838203887369,45.4249999998284,11.5671105274568));
#287172=CARTESIAN_POINT('Ctrl Pts',(7.51676407774742,45.5749999998278,10.3459381770588));
#287173=CARTESIAN_POINT('Ctrl Pts',(9.83957192047851,45.7249999998272,7.14886745759505));
#287174=CARTESIAN_POINT('Ctrl Pts',(12.1623797632096,45.8749999998266,3.95179673813132));
#287175=CARTESIAN_POINT('Ctrl Pts',(12.1623797632096,46.024999999826,-1.48946194470292E-15));
#287176=CARTESIAN_POINT('Ctrl Pts',(12.1623797632096,46.1749999998254,-3.95179673813132));
#287177=CARTESIAN_POINT('Ctrl Pts',(9.83957192047851,46.3249999998248,-7.14886745759505));
#287178=CARTESIAN_POINT('Ctrl Pts',(7.51676407774742,46.4749999998242,-10.3459381770588));
#287179=CARTESIAN_POINT('Ctrl Pts',(3.75838203887369,46.6249999998236,-11.5671105274568));
#287180=CARTESIAN_POINT('Ctrl Pts',(-4.0198546964214E-14,46.774999999823,
-12.7882828778549));
#287181=CARTESIAN_POINT('Ctrl Pts',(-3.75838203887377,46.9249999998224,
-11.5671105274568));
#287182=CARTESIAN_POINT('Ctrl Pts',(-7.5167640777475,47.0749999998218,-10.3459381770588));
#287183=CARTESIAN_POINT('Ctrl Pts',(-9.83957192047859,47.2249999998212,
-7.14886745759505));
#287184=CARTESIAN_POINT('Ctrl Pts',(-12.1623797632097,47.3749999998206,
-3.95179673813132));
#287185=CARTESIAN_POINT('Ctrl Pts',(-12.1623797632097,47.52499999982,2.97892388940585E-15));
#287186=CARTESIAN_POINT('Ctrl Pts',(-12.1623797632097,47.6749999998194,
3.95179673813133));
#287187=CARTESIAN_POINT('Ctrl Pts',(-9.83957192047859,47.8249999998188,
7.14886745759505));
#287188=CARTESIAN_POINT('Ctrl Pts',(-7.51676407774749,47.9749999998182,
10.3459381770588));
#287189=CARTESIAN_POINT('Ctrl Pts',(-3.75838203887377,48.1249999998176,
11.5671105274568));
#287190=CARTESIAN_POINT('Ctrl Pts',(-3.79301756614538E-14,48.274999999817,
12.7882828778549));
#287191=CARTESIAN_POINT('Ctrl Pts',(3.75838203887369,48.4249999998164,11.5671105274568));
#287192=CARTESIAN_POINT('Ctrl Pts',(7.51676407774742,48.5749999998158,10.3459381770588));
#287193=CARTESIAN_POINT('Ctrl Pts',(9.83957192047851,48.7249999998152,7.14886745759505));
#287194=CARTESIAN_POINT('Ctrl Pts',(12.1623797632096,48.8749999998146,3.95179673813132));
#287195=CARTESIAN_POINT('Ctrl Pts',(12.1623797632096,49.024999999814,-1.48946194470292E-15));
#287196=CARTESIAN_POINT('Ctrl Pts',(12.1623797632096,49.1749999998134,-3.95179673813132));
#287197=CARTESIAN_POINT('Ctrl Pts',(9.83957192047851,49.3249999998128,-7.14886745759505));
#287198=CARTESIAN_POINT('Ctrl Pts',(7.51676407774741,49.4749999998122,-10.3459381770588));
#287199=CARTESIAN_POINT('Ctrl Pts',(3.75838203887369,49.6249999998116,-11.5671105274568));
#287200=CARTESIAN_POINT('Ctrl Pts',(-4.19262562358759E-14,49.774999999811,
-12.7882828778549));
#287201=CARTESIAN_POINT('Ctrl Pts',(-3.75838203887377,49.9249999998104,
-11.5671105274568));
#287202=CARTESIAN_POINT('Ctrl Pts',(-7.5167640777475,50.0749999998098,-10.3459381770588));
#287203=CARTESIAN_POINT('Ctrl Pts',(-9.83957192047859,50.2249999998092,
-7.14886745759505));
#287204=CARTESIAN_POINT('Ctrl Pts',(-12.1623797632097,50.3749999998086,
-3.95179673813132));
#287205=CARTESIAN_POINT('Ctrl Pts',(-12.1623797632097,50.524999999808,2.97892388940585E-15));
#287206=CARTESIAN_POINT('Ctrl Pts',(-12.1623797632097,50.6749999998074,
3.95179673813133));
#287207=CARTESIAN_POINT('Ctrl Pts',(-9.83957192047859,50.8249999998068,
7.14886745759505));
#287208=CARTESIAN_POINT('Ctrl Pts',(-7.51676407774749,50.9749999998062,
10.3459381770588));
#287209=CARTESIAN_POINT('Ctrl Pts',(-3.75838203887377,51.1249999998056,
11.5671105274568));
#287210=CARTESIAN_POINT('Ctrl Pts',(-3.96578849331156E-14,51.274999999805,
12.7882828778549));
#287211=CARTESIAN_POINT('Ctrl Pts',(3.75838203887369,51.4249999998044,11.5671105274568));
#287212=CARTESIAN_POINT('Ctrl Pts',(7.51676407774742,51.5749999998038,10.3459381770588));
#287213=CARTESIAN_POINT('Ctrl Pts',(9.83957192047851,51.7249999998032,7.14886745759505));
#287214=CARTESIAN_POINT('Ctrl Pts',(12.1623797632096,51.8749999998026,3.95179673813132));
#287215=CARTESIAN_POINT('Ctrl Pts',(12.1623797632096,52.024999999802,-1.48946194470292E-15));
#287216=CARTESIAN_POINT('Ctrl Pts',(12.1623797632096,52.1749999998014,-3.95179673813132));
#287217=CARTESIAN_POINT('Ctrl Pts',(9.8395719204785,52.3249999998008,-7.14886745759505));
#287218=CARTESIAN_POINT('Ctrl Pts',(7.51676407774741,52.4749999998002,-10.3459381770588));
#287219=CARTESIAN_POINT('Ctrl Pts',(3.75838203887368,52.6249999997996,-11.5671105274568));
#287220=CARTESIAN_POINT('Ctrl Pts',(-4.36539655075377E-14,52.774999999799,
-12.7882828778549));
#287221=CARTESIAN_POINT('Ctrl Pts',(-3.75838203887377,52.9249999997984,
-11.5671105274568));
#287222=CARTESIAN_POINT('Ctrl Pts',(-7.5167640777475,53.0749999997978,-10.3459381770588));
#287223=CARTESIAN_POINT('Ctrl Pts',(-9.83957192047859,53.2249999997972,
-7.14886745759505));
#287224=CARTESIAN_POINT('Ctrl Pts',(-12.1623797632097,53.3749999997966,
-3.95179673813132));
#287225=CARTESIAN_POINT('Ctrl Pts',(-12.1623797632097,53.524999999796,2.97892388940585E-15));
#287226=CARTESIAN_POINT('Ctrl Pts',(-12.1623797632097,53.6749999997954,
3.95179673813133));
#287227=CARTESIAN_POINT('Ctrl Pts',(-9.83957192047859,53.8249999997948,
7.14886745759505));
#287228=CARTESIAN_POINT('Ctrl Pts',(-7.5167640777475,53.9749999997942,10.3459381770588));
#287229=CARTESIAN_POINT('Ctrl Pts',(-3.75838203887377,54.1249999997936,
11.5671105274568));
#287230=CARTESIAN_POINT('Ctrl Pts',(-4.13855942047774E-14,54.274999999793,
12.7882828778549));
#287231=CARTESIAN_POINT('Ctrl Pts',(3.75838203887369,54.4249999997924,11.5671105274568));
#287232=CARTESIAN_POINT('Ctrl Pts',(7.51676407774741,54.5749999997918,10.3459381770588));
#287233=CARTESIAN_POINT('Ctrl Pts',(9.8395719204785,54.7249999997912,7.14886745759505));
#287234=CARTESIAN_POINT('Ctrl Pts',(12.1623797632096,54.8749999997906,3.95179673813132));
#287235=CARTESIAN_POINT('Ctrl Pts',(12.1623797632096,55.02499999979,-1.48946194470292E-15));
#287236=CARTESIAN_POINT('Ctrl Pts',(12.1623797632096,55.1749999997894,-3.95179673813132));
#287237=CARTESIAN_POINT('Ctrl Pts',(9.8395719204785,55.3249999997888,-7.14886745759505));
#287238=CARTESIAN_POINT('Ctrl Pts',(7.51676407774741,55.4749999997882,-10.3459381770588));
#287239=CARTESIAN_POINT('Ctrl Pts',(3.75838203887368,55.6249999997876,-11.5671105274568));
#287240=CARTESIAN_POINT('Ctrl Pts',(-4.53816747791995E-14,55.774999999787,
-12.7882828778549));
#287241=CARTESIAN_POINT('Ctrl Pts',(-3.75838203887377,55.9249999997864,
-11.5671105274568));
#287242=CARTESIAN_POINT('Ctrl Pts',(-7.5167640777475,56.0749999997858,-10.3459381770588));
#287243=CARTESIAN_POINT('Ctrl Pts',(-9.83957192047859,56.2249999997852,
-7.14886745759505));
#287244=CARTESIAN_POINT('Ctrl Pts',(-12.1623797632097,56.3749999997846,
-3.95179673813132));
#287245=CARTESIAN_POINT('Ctrl Pts',(-12.1623797632097,56.524999999784,2.97892388940585E-15));
#287246=CARTESIAN_POINT('Ctrl Pts',(-12.1623797632097,56.6749999997834,
3.95179673813133));
#287247=CARTESIAN_POINT('Ctrl Pts',(-9.83957192047859,56.8249999997828,
7.14886745759505));
#287248=CARTESIAN_POINT('Ctrl Pts',(-7.5167640777475,56.9749999997822,10.3459381770588));
#287249=CARTESIAN_POINT('Ctrl Pts',(-3.75838203887377,57.1249999997816,
11.5671105274568));
#287250=CARTESIAN_POINT('Ctrl Pts',(-4.31133034764393E-14,57.274999999781,
12.7882828778549));
#287251=CARTESIAN_POINT('Ctrl Pts',(3.75838203887368,57.4249999997804,11.5671105274568));
#287252=CARTESIAN_POINT('Ctrl Pts',(7.51676407774741,57.5749999997798,10.3459381770588));
#287253=CARTESIAN_POINT('Ctrl Pts',(9.8395719204785,57.7249999997792,7.14886745759505));
#287254=CARTESIAN_POINT('Ctrl Pts',(12.1623797632096,57.8749999997786,3.95179673813132));
#287255=CARTESIAN_POINT('Ctrl Pts',(12.1623797632096,58.024999999778,-1.48946194470292E-15));
#287256=CARTESIAN_POINT('Ctrl Pts',(12.1623797632096,58.1749999997774,-3.95179673813132));
#287257=CARTESIAN_POINT('Ctrl Pts',(9.8395719204785,58.3249999997768,-7.14886745759505));
#287258=CARTESIAN_POINT('Ctrl Pts',(7.51676407774741,58.4749999997762,-10.3459381770588));
#287259=CARTESIAN_POINT('Ctrl Pts',(3.75838203887368,58.6249999997756,-11.5671105274568));
#287260=CARTESIAN_POINT('Ctrl Pts',(-4.71093840508614E-14,58.774999999775,
-12.7882828778549));
#287261=CARTESIAN_POINT('Ctrl Pts',(-3.75838203887377,58.9249999997744,
-11.5671105274568));
#287262=CARTESIAN_POINT('Ctrl Pts',(-7.5167640777475,59.0749999997738,-10.3459381770588));
#287263=CARTESIAN_POINT('Ctrl Pts',(-9.83957192047859,59.2249999997732,
-7.14886745759505));
#287264=CARTESIAN_POINT('Ctrl Pts',(-12.1623797632097,59.3749999997726,
-3.95179673813132));
#287265=CARTESIAN_POINT('Ctrl Pts',(-12.1623797632097,59.524999999772,2.97892388940585E-15));
#287266=CARTESIAN_POINT('Ctrl Pts',(-12.1623797632097,59.6749999997714,
3.95179673813133));
#287267=CARTESIAN_POINT('Ctrl Pts',(-9.83957192047859,59.8249999997708,
7.14886745759505));
#287268=CARTESIAN_POINT('Ctrl Pts',(-7.5167640777475,59.9749999997702,10.3459381770588));
#287269=CARTESIAN_POINT('Ctrl Pts',(-3.75838203887377,60.1249999997696,
11.5671105274568));
#287270=CARTESIAN_POINT('Ctrl Pts',(-4.48410127481011E-14,60.274999999769,
12.7882828778549));
#287271=CARTESIAN_POINT('Ctrl Pts',(3.75838203887368,60.4249999997684,11.5671105274568));
#287272=CARTESIAN_POINT('Ctrl Pts',(7.51676407774741,60.5749999997678,10.3459381770588));
#287273=CARTESIAN_POINT('Ctrl Pts',(9.8395719204785,60.7249999997672,7.14886745759505));
#287274=CARTESIAN_POINT('Ctrl Pts',(12.1623797632096,60.8749999997666,3.95179673813132));
#287275=CARTESIAN_POINT('Ctrl Pts',(12.1623797632096,61.024999999766,-1.48946194470292E-15));
#287276=CARTESIAN_POINT('Ctrl Pts',(12.1623797632096,61.1749999997654,-3.95179673813132));
#287277=CARTESIAN_POINT('Ctrl Pts',(9.8395719204785,61.3249999997648,-7.14886745759505));
#287278=CARTESIAN_POINT('Ctrl Pts',(7.51676407774741,61.4749999997642,-10.3459381770588));
#287279=CARTESIAN_POINT('Ctrl Pts',(3.75838203887368,61.6249999997636,-11.5671105274568));
#287280=CARTESIAN_POINT('Ctrl Pts',(-4.88370933225232E-14,61.774999999763,
-12.7882828778549));
#287281=CARTESIAN_POINT('Ctrl Pts',(-3.75838203887378,61.9249999997624,
-11.5671105274568));
#287282=CARTESIAN_POINT('Ctrl Pts',(-7.5167640777475,62.0749999997618,-10.3459381770588));
#287283=CARTESIAN_POINT('Ctrl Pts',(-9.8395719204786,62.2249999997612,-7.14886745759505));
#287284=CARTESIAN_POINT('Ctrl Pts',(-12.1623797632097,62.3749999997606,
-3.95179673813132));
#287285=CARTESIAN_POINT('Ctrl Pts',(-12.1623797632097,62.52499999976,2.97892388940585E-15));
#287286=CARTESIAN_POINT('Ctrl Pts',(-12.1623797632097,62.6749999997594,
3.95179673813133));
#287287=CARTESIAN_POINT('Ctrl Pts',(-9.8395719204786,62.8249999997588,7.14886745759505));
#287288=CARTESIAN_POINT('Ctrl Pts',(-7.5167640777475,62.9749999997582,10.3459381770588));
#287289=CARTESIAN_POINT('Ctrl Pts',(-3.75838203887377,63.1249999997576,
11.5671105274568));
#287290=CARTESIAN_POINT('Ctrl Pts',(-4.6568722019763E-14,63.274999999757,
12.7882828778549));
#287291=CARTESIAN_POINT('Ctrl Pts',(3.75838203887368,63.4249999997564,11.5671105274568));
#287292=CARTESIAN_POINT('Ctrl Pts',(7.51676407774741,63.5749999997558,10.3459381770588));
#287293=CARTESIAN_POINT('Ctrl Pts',(9.8395719204785,63.7249999997552,7.14886745759505));
#287294=CARTESIAN_POINT('Ctrl Pts',(12.1623797632096,63.8749999997546,3.95179673813132));
#287295=CARTESIAN_POINT('Ctrl Pts',(12.1623797632096,64.024999999754,-1.48946194470292E-15));
#287296=CARTESIAN_POINT('Ctrl Pts',(12.1623797632096,64.1749999997534,-3.95179673813132));
#287297=CARTESIAN_POINT('Ctrl Pts',(9.8395719204785,64.3249999997528,-7.14886745759505));
#287298=CARTESIAN_POINT('Ctrl Pts',(7.5167640777474,64.4749999997522,-10.3459381770588));
#287299=CARTESIAN_POINT('Ctrl Pts',(3.75838203887368,64.6249999997516,-11.5671105274568));
#287300=CARTESIAN_POINT('Ctrl Pts',(-5.05648025941851E-14,64.774999999751,
-12.7882828778549));
#287301=CARTESIAN_POINT('Ctrl Pts',(-3.75838203887378,64.9249999997504,
-11.5671105274568));
#287302=CARTESIAN_POINT('Ctrl Pts',(-7.51676407774751,65.0749999997498,
-10.3459381770588));
#287303=CARTESIAN_POINT('Ctrl Pts',(-9.8395719204786,65.2249999997492,-7.14886745759505));
#287304=CARTESIAN_POINT('Ctrl Pts',(-12.1623797632097,65.3749999997486,
-3.95179673813132));
#287305=CARTESIAN_POINT('Ctrl Pts',(-12.1623797632097,65.524999999748,2.97892388940585E-15));
#287306=CARTESIAN_POINT('Ctrl Pts',(-12.1623797632097,65.6749999997474,
3.95179673813133));
#287307=CARTESIAN_POINT('Ctrl Pts',(-9.8395719204786,65.8249999997468,7.14886745759505));
#287308=CARTESIAN_POINT('Ctrl Pts',(-7.5167640777475,65.9749999997462,10.3459381770588));
#287309=CARTESIAN_POINT('Ctrl Pts',(-3.75838203887378,66.1249999997456,
11.5671105274568));
#287310=CARTESIAN_POINT('Ctrl Pts',(-4.82964312914248E-14,66.274999999745,
12.7882828778549));
#287311=CARTESIAN_POINT('Ctrl Pts',(3.75838203887368,66.4249999997444,11.5671105274568));
#287312=CARTESIAN_POINT('Ctrl Pts',(7.51676407774741,66.5749999997438,10.3459381770588));
#287313=CARTESIAN_POINT('Ctrl Pts',(9.8395719204785,66.7249999997432,7.14886745759505));
#287314=CARTESIAN_POINT('Ctrl Pts',(12.1623797632096,66.8749999997426,3.95179673813132));
#287315=CARTESIAN_POINT('Ctrl Pts',(12.1623797632096,67.024999999742,-1.48946194470292E-15));
#287316=CARTESIAN_POINT('Ctrl Pts',(12.1623797632096,67.1749999997414,-3.95179673813132));
#287317=CARTESIAN_POINT('Ctrl Pts',(9.8395719204785,67.3249999997408,-7.14886745759505));
#287318=CARTESIAN_POINT('Ctrl Pts',(7.5167640777474,67.4749999997402,-10.3459381770588));
#287319=CARTESIAN_POINT('Ctrl Pts',(3.75838203887368,67.6249999997396,-11.5671105274568));
#287320=CARTESIAN_POINT('Ctrl Pts',(-5.22925118658469E-14,67.774999999739,
-12.7882828778549));
#287321=CARTESIAN_POINT('Ctrl Pts',(-3.75838203887378,67.9249999997384,
-11.5671105274568));
#287322=CARTESIAN_POINT('Ctrl Pts',(-7.51676407774751,68.0749999997378,
-10.3459381770588));
#287323=CARTESIAN_POINT('Ctrl Pts',(-9.8395719204786,68.2249999997372,-7.14886745759505));
#287324=CARTESIAN_POINT('Ctrl Pts',(-12.1623797632097,68.3749999997366,
-3.95179673813132));
#287325=CARTESIAN_POINT('Ctrl Pts',(-12.1623797632097,68.524999999736,2.97892388940585E-15));
#287326=CARTESIAN_POINT('Ctrl Pts',(-12.1623797632097,68.6749999997354,
3.95179673813133));
#287327=CARTESIAN_POINT('Ctrl Pts',(-9.8395719204786,68.8249999997348,7.14886745759505));
#287328=CARTESIAN_POINT('Ctrl Pts',(-7.51676407774751,68.9749999997342,
10.3459381770588));
#287329=CARTESIAN_POINT('Ctrl Pts',(-3.75838203887378,69.1249999997336,
11.5671105274568));
#287330=CARTESIAN_POINT('Ctrl Pts',(-5.00241405630866E-14,69.274999999733,
12.7882828778549));
#287331=CARTESIAN_POINT('Ctrl Pts',(3.75838203887368,69.4249999997324,11.5671105274568));
#287332=CARTESIAN_POINT('Ctrl Pts',(7.5167640777474,69.5749999997318,10.3459381770588));
#287333=CARTESIAN_POINT('Ctrl Pts',(9.8395719204785,69.7249999997312,7.14886745759505));
#287334=CARTESIAN_POINT('Ctrl Pts',(12.1623797632096,69.8749999997306,3.95179673813132));
#287335=CARTESIAN_POINT('Ctrl Pts',(12.1623797632096,70.02499999973,-1.48946194470292E-15));
#287336=CARTESIAN_POINT('Ctrl Pts',(12.1623797632096,70.1749999997294,-3.95179673813132));
#287337=CARTESIAN_POINT('Ctrl Pts',(9.83957192047849,70.3249999997288,-7.14886745759505));
#287338=CARTESIAN_POINT('Ctrl Pts',(7.5167640777474,70.4749999997282,-10.3459381770588));
#287339=CARTESIAN_POINT('Ctrl Pts',(3.75838203887367,70.6249999997276,-11.5671105274568));
#287340=CARTESIAN_POINT('Ctrl Pts',(-5.40202211375087E-14,70.774999999727,
-12.7882828778549));
#287341=CARTESIAN_POINT('Ctrl Pts',(-3.75838203887378,70.9249999997264,
-11.5671105274568));
#287342=CARTESIAN_POINT('Ctrl Pts',(-7.51676407774751,71.0749999997258,
-10.3459381770588));
#287343=CARTESIAN_POINT('Ctrl Pts',(-9.8395719204786,71.2249999997252,-7.14886745759505));
#287344=CARTESIAN_POINT('Ctrl Pts',(-12.1623797632097,71.3749999997246,
-3.95179673813132));
#287345=CARTESIAN_POINT('Ctrl Pts',(-12.1623797632097,71.524999999724,2.97892388940585E-15));
#287346=CARTESIAN_POINT('Ctrl Pts',(-12.1623797632097,71.6749999997234,
3.95179673813133));
#287347=CARTESIAN_POINT('Ctrl Pts',(-9.8395719204786,71.8249999997228,7.14886745759505));
#287348=CARTESIAN_POINT('Ctrl Pts',(-7.51676407774751,71.9749999997222,
10.3459381770588));
#287349=CARTESIAN_POINT('Ctrl Pts',(-3.75838203887378,72.1249999997216,
11.5671105274568));
#287350=CARTESIAN_POINT('Ctrl Pts',(-5.17518498347485E-14,72.274999999721,
12.7882828778549));
#287351=CARTESIAN_POINT('Ctrl Pts',(3.75838203887368,72.4249999997204,11.5671105274568));
#287352=CARTESIAN_POINT('Ctrl Pts',(7.5167640777474,72.5749999997198,10.3459381770588));
#287353=CARTESIAN_POINT('Ctrl Pts',(9.83957192047849,72.7249999997192,7.14886745759505));
#287354=CARTESIAN_POINT('Ctrl Pts',(12.1623797632096,72.8749999997186,3.95179673813132));
#287355=CARTESIAN_POINT('Ctrl Pts',(12.1623797632096,73.024999999718,-1.48946194470292E-15));
#287356=CARTESIAN_POINT('Ctrl Pts',(12.1623797632096,73.1749999997174,-3.95179673813132));
#287357=CARTESIAN_POINT('Ctrl Pts',(9.83957192047849,73.3249999997168,-7.14886745759505));
#287358=CARTESIAN_POINT('Ctrl Pts',(7.5167640777474,73.4749999997162,-10.3459381770588));
#287359=CARTESIAN_POINT('Ctrl Pts',(3.75838203887367,73.6249999997156,-11.5671105274568));
#287360=CARTESIAN_POINT('Ctrl Pts',(-5.57479304091706E-14,73.774999999715,
-12.7882828778549));
#287361=CARTESIAN_POINT('Ctrl Pts',(-3.75838203887378,73.9249999997144,
-11.5671105274568));
#287362=CARTESIAN_POINT('Ctrl Pts',(-7.51676407774751,74.0749999997138,
-10.3459381770588));
#287363=CARTESIAN_POINT('Ctrl Pts',(-9.8395719204786,74.2249999997132,-7.14886745759505));
#287364=CARTESIAN_POINT('Ctrl Pts',(-12.1623797632097,74.3749999997126,
-3.95179673813132));
#287365=CARTESIAN_POINT('Ctrl Pts',(-12.1623797632097,74.524999999712,2.97892388940585E-15));
#287366=CARTESIAN_POINT('Ctrl Pts',(-12.1623797632097,74.6749999997114,
3.95179673813133));
#287367=CARTESIAN_POINT('Ctrl Pts',(-9.8395719204786,74.8249999997108,7.14886745759505));
#287368=CARTESIAN_POINT('Ctrl Pts',(-7.51676407774751,74.9749999997102,
10.3459381770588));
#287369=CARTESIAN_POINT('Ctrl Pts',(-3.75838203887378,75.1249999997096,
11.5671105274568));
#287370=CARTESIAN_POINT('Ctrl Pts',(-5.34795591064103E-14,75.274999999709,
12.7882828778549));
#287371=CARTESIAN_POINT('Ctrl Pts',(3.75838203887367,75.4249999997084,11.5671105274568));
#287372=CARTESIAN_POINT('Ctrl Pts',(7.5167640777474,75.5749999997078,10.3459381770588));
#287373=CARTESIAN_POINT('Ctrl Pts',(9.83957192047849,75.7249999997072,7.14886745759505));
#287374=CARTESIAN_POINT('Ctrl Pts',(12.1623797632096,75.8749999997066,3.95179673813132));
#287375=CARTESIAN_POINT('Ctrl Pts',(12.1623797632096,76.024999999706,-1.48946194470292E-15));
#287376=CARTESIAN_POINT('Ctrl Pts',(12.1623797632096,76.1749999997054,-3.95179673813132));
#287377=CARTESIAN_POINT('Ctrl Pts',(9.83957192047849,76.3249999997048,-7.14886745759505));
#287378=CARTESIAN_POINT('Ctrl Pts',(7.5167640777474,76.4749999997042,-10.3459381770588));
#287379=CARTESIAN_POINT('Ctrl Pts',(3.75838203887367,76.6249999997036,-11.5671105274568));
#287380=CARTESIAN_POINT('Ctrl Pts',(-5.74756396808324E-14,76.774999999703,
-12.7882828778549));
#287381=CARTESIAN_POINT('Ctrl Pts',(-3.75838203887379,76.9249999997024,
-11.5671105274568));
#287382=CARTESIAN_POINT('Ctrl Pts',(-7.51676407774751,77.0749999997018,
-10.3459381770588));
#287383=CARTESIAN_POINT('Ctrl Pts',(-9.8395719204786,77.2249999997012,-7.14886745759505));
#287384=CARTESIAN_POINT('Ctrl Pts',(-12.1623797632097,77.3749999997006,
-3.95179673813132));
#287385=CARTESIAN_POINT('Ctrl Pts',(-12.1623797632097,77.5249999997,2.97892388940585E-15));
#287386=CARTESIAN_POINT('Ctrl Pts',(-12.1623797632097,77.6749999996994,
3.95179673813133));
#287387=CARTESIAN_POINT('Ctrl Pts',(-9.8395719204786,77.8249999996988,7.14886745759505));
#287388=CARTESIAN_POINT('Ctrl Pts',(-7.51676407774751,77.9749999996982,
10.3459381770588));
#287389=CARTESIAN_POINT('Ctrl Pts',(-3.75838203887378,78.1249999996976,
11.5671105274568));
#287390=CARTESIAN_POINT('Ctrl Pts',(-5.52072683780721E-14,78.274999999697,
12.7882828778549));
#287391=CARTESIAN_POINT('Ctrl Pts',(3.75838203887367,78.4249999996964,11.5671105274568));
#287392=CARTESIAN_POINT('Ctrl Pts',(7.5167640777474,78.5749999996958,10.3459381770588));
#287393=CARTESIAN_POINT('Ctrl Pts',(9.83957192047849,78.7249999996952,7.14886745759505));
#287394=CARTESIAN_POINT('Ctrl Pts',(12.1623797632096,78.8749999996946,3.95179673813132));
#287395=CARTESIAN_POINT('Ctrl Pts',(12.1623797632096,79.024999999694,-1.48946194470292E-15));
#287396=CARTESIAN_POINT('Ctrl Pts',(12.1623797632096,79.1749999996934,-3.95179673813132));
#287397=CARTESIAN_POINT('Ctrl Pts',(9.83957192047849,79.3249999996928,-7.14886745759505));
#287398=CARTESIAN_POINT('Ctrl Pts',(7.5167640777474,79.4749999996922,-10.3459381770588));
#287399=CARTESIAN_POINT('Ctrl Pts',(3.75838203887367,79.6249999996916,-11.5671105274568));
#287400=CARTESIAN_POINT('Ctrl Pts',(-5.92033489524943E-14,79.774999999691,
-12.7882828778549));
#287401=CARTESIAN_POINT('Ctrl Pts',(-3.75838203887379,79.9249999996904,
-11.5671105274568));
#287402=CARTESIAN_POINT('Ctrl Pts',(-7.51676407774751,80.0749999996898,
-10.3459381770588));
#287403=CARTESIAN_POINT('Ctrl Pts',(-9.83957192047861,80.2249999996892,
-7.14886745759505));
#287404=CARTESIAN_POINT('Ctrl Pts',(-12.1623797632097,80.3749999996886,
-3.95179673813132));
#287405=CARTESIAN_POINT('Ctrl Pts',(-12.1623797632097,80.524999999688,2.97892388940585E-15));
#287406=CARTESIAN_POINT('Ctrl Pts',(-12.1623797632097,80.6749999996874,
3.95179673813133));
#287407=CARTESIAN_POINT('Ctrl Pts',(-9.83957192047861,80.8249999996868,
7.14886745759505));
#287408=CARTESIAN_POINT('Ctrl Pts',(-7.51676407774751,80.9749999996862,
10.3459381770588));
#287409=CARTESIAN_POINT('Ctrl Pts',(-3.75838203887378,81.1249999996856,
11.5671105274568));
#287410=CARTESIAN_POINT('Ctrl Pts',(-5.6934977649734E-14,81.274999999685,
12.7882828778549));
#287411=CARTESIAN_POINT('Ctrl Pts',(3.75838203887367,81.4249999996844,11.5671105274568));
#287412=CARTESIAN_POINT('Ctrl Pts',(7.5167640777474,81.5749999996838,10.3459381770588));
#287413=CARTESIAN_POINT('Ctrl Pts',(9.83957192047849,81.7249999996832,7.14886745759505));
#287414=CARTESIAN_POINT('Ctrl Pts',(12.1623797632096,81.8749999996826,3.95179673813132));
#287415=CARTESIAN_POINT('Ctrl Pts',(12.1623797632096,82.024999999682,-1.48946194470292E-15));
#287416=CARTESIAN_POINT('Ctrl Pts',(12.1623797632096,82.1749999996814,-3.95179673813132));
#287417=CARTESIAN_POINT('Ctrl Pts',(9.83957192047849,82.3249999996808,-7.14886745759505));
#287418=CARTESIAN_POINT('Ctrl Pts',(7.5167640777474,82.4749999996802,-10.3459381770588));
#287419=CARTESIAN_POINT('Ctrl Pts',(3.75838203887367,82.6249999996796,-11.5671105274568));
#287420=CARTESIAN_POINT('Ctrl Pts',(-6.09310582241561E-14,82.774999999679,
-12.7882828778549));
#287421=CARTESIAN_POINT('Ctrl Pts',(-3.75838203887379,82.9249999996784,
-11.5671105274568));
#287422=CARTESIAN_POINT('Ctrl Pts',(-7.51676407774752,83.0749999996778,
-10.3459381770588));
#287423=CARTESIAN_POINT('Ctrl Pts',(-9.83957192047861,83.2249999996772,
-7.14886745759505));
#287424=CARTESIAN_POINT('Ctrl Pts',(-12.1623797632097,83.3749999996766,
-3.95179673813132));
#287425=CARTESIAN_POINT('Ctrl Pts',(-12.1623797632097,83.524999999676,2.97892388940585E-15));
#287426=CARTESIAN_POINT('Ctrl Pts',(-12.1623797632097,83.6749999996754,
3.95179673813133));
#287427=CARTESIAN_POINT('Ctrl Pts',(-9.83957192047861,83.8249999996748,
7.14886745759505));
#287428=CARTESIAN_POINT('Ctrl Pts',(-7.51676407774751,83.9749999996742,
10.3459381770588));
#287429=CARTESIAN_POINT('Ctrl Pts',(-3.75838203887379,84.1249999996736,
11.5671105274568));
#287430=CARTESIAN_POINT('Ctrl Pts',(-5.86626869213958E-14,84.274999999673,
12.7882828778549));
#287431=CARTESIAN_POINT('Ctrl Pts',(3.75838203887367,84.4249999996724,11.5671105274568));
#287432=CARTESIAN_POINT('Ctrl Pts',(7.5167640777474,84.5749999996718,10.3459381770588));
#287433=CARTESIAN_POINT('Ctrl Pts',(9.83957192047849,84.7249999996712,7.14886745759505));
#287434=CARTESIAN_POINT('Ctrl Pts',(12.1623797632096,84.8749999996706,3.95179673813132));
#287435=CARTESIAN_POINT('Ctrl Pts',(12.1623797632096,85.02499999967,-1.48946194470292E-15));
#287436=CARTESIAN_POINT('Ctrl Pts',(12.1623797632096,85.1749999996694,-3.95179673813132));
#287437=CARTESIAN_POINT('Ctrl Pts',(9.83957192047849,85.3249999996688,-7.14886745759505));
#287438=CARTESIAN_POINT('Ctrl Pts',(7.51676407774739,85.4749999996682,-10.3459381770588));
#287439=CARTESIAN_POINT('Ctrl Pts',(3.75838203887367,85.6249999996676,-11.5671105274568));
#287440=CARTESIAN_POINT('Ctrl Pts',(-6.26587674958179E-14,85.774999999667,
-12.7882828778549));
#287441=CARTESIAN_POINT('Ctrl Pts',(-3.75838203887379,85.9249999996664,
-11.5671105274568));
#287442=CARTESIAN_POINT('Ctrl Pts',(-7.51676407774752,86.0749999996658,
-10.3459381770588));
#287443=CARTESIAN_POINT('Ctrl Pts',(-9.83957192047861,86.2249999996652,
-7.14886745759505));
#287444=CARTESIAN_POINT('Ctrl Pts',(-12.1623797632097,86.3749999996646,
-3.95179673813132));
#287445=CARTESIAN_POINT('Ctrl Pts',(-12.1623797632097,86.524999999664,2.97892388940585E-15));
#287446=CARTESIAN_POINT('Ctrl Pts',(-12.1623797632097,86.6749999996634,
3.95179673813133));
#287447=CARTESIAN_POINT('Ctrl Pts',(-9.83957192047861,86.8249999996628,
7.14886745759505));
#287448=CARTESIAN_POINT('Ctrl Pts',(-7.51676407774752,86.9749999996622,
10.3459381770588));
#287449=CARTESIAN_POINT('Ctrl Pts',(-3.75838203887379,87.1249999996616,
11.5671105274568));
#287450=CARTESIAN_POINT('Ctrl Pts',(-6.03903961930577E-14,87.274999999661,
12.7882828778549));
#287451=CARTESIAN_POINT('Ctrl Pts',(3.75838203887367,87.4249999996604,11.5671105274568));
#287452=CARTESIAN_POINT('Ctrl Pts',(7.5167640777474,87.5749999996598,10.3459381770588));
#287453=CARTESIAN_POINT('Ctrl Pts',(9.83957192047849,87.7249999996592,7.14886745759505));
#287454=CARTESIAN_POINT('Ctrl Pts',(12.1623797632096,87.8749999996586,3.95179673813132));
#287455=CARTESIAN_POINT('Ctrl Pts',(12.1623797632096,88.024999999658,-1.48946194470292E-15));
#287456=CARTESIAN_POINT('Ctrl Pts',(12.1623797632096,88.1749999996574,-3.95179673813132));
#287457=CARTESIAN_POINT('Ctrl Pts',(9.83957192047849,88.3249999996568,-7.14886745759505));
#287458=CARTESIAN_POINT('Ctrl Pts',(7.51676407774739,88.4749999996562,-10.3459381770588));
#287459=CARTESIAN_POINT('Ctrl Pts',(3.75838203887366,88.6249999996556,-11.5671105274568));
#287460=CARTESIAN_POINT('Ctrl Pts',(-6.43864767674798E-14,88.774999999655,
-12.7882828778549));
#287461=CARTESIAN_POINT('Ctrl Pts',(-3.75838203887379,88.9249999996544,
-11.5671105274568));
#287462=CARTESIAN_POINT('Ctrl Pts',(-7.51676407774752,89.0749999996538,
-10.3459381770588));
#287463=CARTESIAN_POINT('Ctrl Pts',(-9.83957192047861,89.2249999996532,
-7.14886745759505));
#287464=CARTESIAN_POINT('Ctrl Pts',(-12.1623797632097,89.3749999996526,
-3.95179673813132));
#287465=CARTESIAN_POINT('Ctrl Pts',(-12.1623797632097,89.524999999652,2.97892388940585E-15));
#287466=CARTESIAN_POINT('Ctrl Pts',(-12.1623797632097,89.6749999996514,
3.95179673813133));
#287467=CARTESIAN_POINT('Ctrl Pts',(-9.83957192047861,89.8249999996508,
7.14886745759505));
#287468=CARTESIAN_POINT('Ctrl Pts',(-7.51676407774752,89.9749999996502,
10.3459381770588));
#287469=CARTESIAN_POINT('Ctrl Pts',(-3.75838203887379,90.1249999996496,
11.5671105274568));
#287470=CARTESIAN_POINT('Ctrl Pts',(-6.21181054647195E-14,90.274999999649,
12.7882828778549));
#287471=CARTESIAN_POINT('Ctrl Pts',(3.75838203887366,90.4249999996484,11.5671105274568));
#287472=CARTESIAN_POINT('Ctrl Pts',(7.51676407774739,90.5749999996478,10.3459381770588));
#287473=CARTESIAN_POINT('Ctrl Pts',(9.83957192047848,90.7249999996472,7.14886745759505));
#287474=CARTESIAN_POINT('Ctrl Pts',(12.1623797632096,90.8749999996466,3.95179673813132));
#287475=CARTESIAN_POINT('Ctrl Pts',(12.1623797632096,91.024999999646,-1.48946194470292E-15));
#287476=CARTESIAN_POINT('Ctrl Pts',(12.1623797632096,91.1749999996454,-3.95179673813132));
#287477=CARTESIAN_POINT('Ctrl Pts',(9.83957192047848,91.3249999996448,-7.14886745759505));
#287478=CARTESIAN_POINT('Ctrl Pts',(7.51676407774739,91.4749999996442,-10.3459381770588));
#287479=CARTESIAN_POINT('Ctrl Pts',(3.75838203887366,91.6249999996436,-11.5671105274568));
#287480=CARTESIAN_POINT('Ctrl Pts',(-6.61141860391416E-14,91.774999999643,
-12.7882828778549));
#287481=CARTESIAN_POINT('Ctrl Pts',(-3.75838203887379,91.9249999996424,
-11.5671105274568));
#287482=CARTESIAN_POINT('Ctrl Pts',(-7.51676407774752,92.0749999996418,
-10.3459381770588));
#287483=CARTESIAN_POINT('Ctrl Pts',(-9.83957192047861,92.2249999996412,
-7.14886745759505));
#287484=CARTESIAN_POINT('Ctrl Pts',(-12.1623797632097,92.3749999996406,
-3.95179673813132));
#287485=CARTESIAN_POINT('Ctrl Pts',(-12.1623797632097,92.52499999964,2.97892388940585E-15));
#287486=CARTESIAN_POINT('Ctrl Pts',(-12.1623797632097,92.6749999996394,
3.95179673813133));
#287487=CARTESIAN_POINT('Ctrl Pts',(-9.83957192047861,92.8249999996388,
7.14886745759505));
#287488=CARTESIAN_POINT('Ctrl Pts',(-7.51676407774752,92.9749999996382,
10.3459381770588));
#287489=CARTESIAN_POINT('Ctrl Pts',(-3.75838203887379,93.1249999996376,
11.5671105274568));
#287490=CARTESIAN_POINT('Ctrl Pts',(-6.38458147363813E-14,93.274999999637,
12.7882828778549));
#287491=CARTESIAN_POINT('Ctrl Pts',(3.75838203887366,93.4249999996364,11.5671105274568));
#287492=CARTESIAN_POINT('Ctrl Pts',(7.51676407774739,93.5749999996358,10.3459381770588));
#287493=CARTESIAN_POINT('Ctrl Pts',(9.83957192047848,93.7249999996352,7.14886745759505));
#287494=CARTESIAN_POINT('Ctrl Pts',(12.1623797632096,93.8749999996346,3.95179673813132));
#287495=CARTESIAN_POINT('Ctrl Pts',(12.1623797632096,94.024999999634,-1.48946194470292E-15));
#287496=CARTESIAN_POINT('Ctrl Pts',(12.1623797632096,94.1749999996334,-3.95179673813132));
#287497=CARTESIAN_POINT('Ctrl Pts',(9.83957192047848,94.3249999996328,-7.14886745759505));
#287498=CARTESIAN_POINT('Ctrl Pts',(7.51676407774739,94.4749999996322,-10.3459381770588));
#287499=CARTESIAN_POINT('Ctrl Pts',(3.75838203887366,94.6249999996316,-11.5671105274568));
#287500=CARTESIAN_POINT('Ctrl Pts',(-6.78418953108034E-14,94.774999999631,
-12.7882828778549));
#287501=CARTESIAN_POINT('Ctrl Pts',(-3.7583820388738,94.9249999996304,-11.5671105274568));
#287502=CARTESIAN_POINT('Ctrl Pts',(-7.51676407774752,95.0749999996298,
-10.3459381770588));
#287503=CARTESIAN_POINT('Ctrl Pts',(-9.83957192047862,95.2249999996292,
-7.14886745759505));
#287504=CARTESIAN_POINT('Ctrl Pts',(-12.1623797632097,95.3749999996286,
-3.95179673813132));
#287505=CARTESIAN_POINT('Ctrl Pts',(-12.1623797632097,95.524999999628,2.97892388940585E-15));
#287506=CARTESIAN_POINT('Ctrl Pts',(-12.1623797632097,95.6749999996274,
3.95179673813133));
#287507=CARTESIAN_POINT('Ctrl Pts',(-9.83957192047862,95.8249999996268,
7.14886745759505));
#287508=CARTESIAN_POINT('Ctrl Pts',(-7.51676407774752,95.9749999996262,
10.3459381770588));
#287509=CARTESIAN_POINT('Ctrl Pts',(-3.75838203887379,96.1249999996256,
11.5671105274568));
#287510=CARTESIAN_POINT('Ctrl Pts',(-6.55735240080432E-14,96.274999999625,
12.7882828778549));
#287511=CARTESIAN_POINT('Ctrl Pts',(3.75838203887366,96.4249999996244,11.5671105274568));
#287512=CARTESIAN_POINT('Ctrl Pts',(7.51676407774739,96.5749999996238,10.3459381770588));
#287513=CARTESIAN_POINT('Ctrl Pts',(9.83957192047848,96.7249999996232,7.14886745759505));
#287514=CARTESIAN_POINT('Ctrl Pts',(12.1623797632096,96.8749999996226,3.95179673813132));
#287515=CARTESIAN_POINT('Ctrl Pts',(12.1623797632096,97.024999999622,-1.48946194470292E-15));
#287516=CARTESIAN_POINT('Ctrl Pts',(12.1623797632096,97.1749999996214,-3.95179673813132));
#287517=CARTESIAN_POINT('Ctrl Pts',(9.83957192047848,97.3249999996208,-7.14886745759505));
#287518=CARTESIAN_POINT('Ctrl Pts',(7.51676407774739,97.4749999996202,-10.3459381770588));
#287519=CARTESIAN_POINT('Ctrl Pts',(3.75838203887366,97.6249999996196,-11.5671105274568));
#287520=CARTESIAN_POINT('Ctrl Pts',(-6.95696045824653E-14,97.774999999619,
-12.7882828778549));
#287521=CARTESIAN_POINT('Ctrl Pts',(-3.7583820388738,97.9249999996184,-11.5671105274568));
#287522=CARTESIAN_POINT('Ctrl Pts',(-7.51676407774752,98.0749999996178,
-10.3459381770588));
#287523=CARTESIAN_POINT('Ctrl Pts',(-9.83957192047862,98.2249999996172,
-7.14886745759505));
#287524=CARTESIAN_POINT('Ctrl Pts',(-12.1623797632097,98.3749999996166,
-3.95179673813132));
#287525=CARTESIAN_POINT('Ctrl Pts',(-12.1623797632097,98.524999999616,2.97892388940585E-15));
#287526=CARTESIAN_POINT('Ctrl Pts',(-12.1623797632097,98.6749999996154,
3.95179673813133));
#287527=CARTESIAN_POINT('Ctrl Pts',(-9.83957192047862,98.8249999996148,
7.14886745759505));
#287528=CARTESIAN_POINT('Ctrl Pts',(-7.51676407774752,98.9749999996142,
10.3459381770588));
#287529=CARTESIAN_POINT('Ctrl Pts',(-3.7583820388738,99.1249999996136,11.5671105274568));
#287530=CARTESIAN_POINT('Ctrl Pts',(-6.7301233279705E-14,99.274999999613,
12.7882828778549));
#287531=CARTESIAN_POINT('Ctrl Pts',(3.75838203887366,99.4249999996124,11.5671105274568));
#287532=CARTESIAN_POINT('Ctrl Pts',(7.51676407774739,99.5749999996118,10.3459381770588));
#287533=CARTESIAN_POINT('Ctrl Pts',(9.83957192047848,99.7249999996112,7.14886745759505));
#287534=CARTESIAN_POINT('Ctrl Pts',(12.1623797632096,99.8749999996106,3.95179673813132));
#287535=CARTESIAN_POINT('Ctrl Pts',(12.1623797632096,100.02499999961,-1.48946194470292E-15));
#287536=CARTESIAN_POINT('Ctrl Pts',(12.1623797632096,100.174999999609,-3.95179673813132));
#287537=CARTESIAN_POINT('Ctrl Pts',(9.83957192047848,100.324999999609,-7.14886745759505));
#287538=CARTESIAN_POINT('Ctrl Pts',(7.51676407774738,100.474999999608,-10.3459381770588));
#287539=CARTESIAN_POINT('Ctrl Pts',(3.75838203887366,100.624999999608,-11.5671105274568));
#287540=CARTESIAN_POINT('Ctrl Pts',(-7.12973138541271E-14,100.774999999607,
-12.7882828778549));
#287541=CARTESIAN_POINT('Ctrl Pts',(-3.7583820388738,100.924999999606,-11.5671105274568));
#287542=CARTESIAN_POINT('Ctrl Pts',(-7.51676407774753,101.074999999606,
-10.3459381770588));
#287543=CARTESIAN_POINT('Ctrl Pts',(-9.83957192047862,101.224999999605,
-7.14886745759505));
#287544=CARTESIAN_POINT('Ctrl Pts',(-12.1623797632097,101.374999999605,
-3.95179673813132));
#287545=CARTESIAN_POINT('Ctrl Pts',(-12.1623797632097,101.524999999604,
2.97892388940585E-15));
#287546=CARTESIAN_POINT('Ctrl Pts',(-12.1623797632097,101.674999999603,
3.95179673813133));
#287547=CARTESIAN_POINT('Ctrl Pts',(-9.83957192047862,101.824999999603,
7.14886745759505));
#287548=CARTESIAN_POINT('Ctrl Pts',(-7.51676407774752,101.974999999602,
10.3459381770588));
#287549=CARTESIAN_POINT('Ctrl Pts',(-3.7583820388738,102.124999999602,11.5671105274568));
#287550=CARTESIAN_POINT('Ctrl Pts',(-6.90289425513669E-14,102.274999999601,
12.7882828778549));
#287551=CARTESIAN_POINT('Ctrl Pts',(3.75838203887366,102.4249999996,11.5671105274568));
#287552=CARTESIAN_POINT('Ctrl Pts',(7.51676407774739,102.5749999996,10.3459381770588));
#287553=CARTESIAN_POINT('Ctrl Pts',(9.83957192047848,102.724999999599,7.14886745759505));
#287554=CARTESIAN_POINT('Ctrl Pts',(12.1623797632096,102.874999999599,3.95179673813132));
#287555=CARTESIAN_POINT('Ctrl Pts',(12.1623797632096,103.024999999598,-1.48946194470292E-15));
#287556=CARTESIAN_POINT('Ctrl Pts',(12.1623797632096,103.174999999597,-3.95179673813132));
#287557=CARTESIAN_POINT('Ctrl Pts',(9.83957192047848,103.324999999597,-7.14886745759505));
#287558=CARTESIAN_POINT('Ctrl Pts',(7.51676407774738,103.474999999596,-10.3459381770588));
#287559=CARTESIAN_POINT('Ctrl Pts',(3.75838203887366,103.624999999596,-11.5671105274568));
#287560=CARTESIAN_POINT('Ctrl Pts',(-7.3025023125789E-14,103.774999999595,
-12.7882828778549));
#287561=CARTESIAN_POINT('Ctrl Pts',(-3.7583820388738,103.924999999594,-11.5671105274568));
#287562=CARTESIAN_POINT('Ctrl Pts',(-7.51676407774753,104.074999999594,
-10.3459381770588));
#287563=CARTESIAN_POINT('Ctrl Pts',(-9.83957192047862,104.224999999593,
-7.14886745759505));
#287564=CARTESIAN_POINT('Ctrl Pts',(-12.1623797632097,104.374999999593,
-3.95179673813132));
#287565=CARTESIAN_POINT('Ctrl Pts',(-12.1623797632097,104.524999999592,
2.97892388940585E-15));
#287566=CARTESIAN_POINT('Ctrl Pts',(-12.1623797632097,104.674999999591,
3.95179673813133));
#287567=CARTESIAN_POINT('Ctrl Pts',(-9.83957192047862,104.824999999591,
7.14886745759505));
#287568=CARTESIAN_POINT('Ctrl Pts',(-7.51676407774753,104.97499999959,10.3459381770588));
#287569=CARTESIAN_POINT('Ctrl Pts',(-3.7583820388738,105.12499999959,11.5671105274568));
#287570=CARTESIAN_POINT('Ctrl Pts',(-7.07566518230287E-14,105.274999999589,
12.7882828778549));
#287571=CARTESIAN_POINT('Ctrl Pts',(3.75838203887366,105.424999999588,11.5671105274568));
#287572=CARTESIAN_POINT('Ctrl Pts',(7.51676407774738,105.574999999588,10.3459381770588));
#287573=CARTESIAN_POINT('Ctrl Pts',(9.83957192047848,105.724999999587,7.14886745759505));
#287574=CARTESIAN_POINT('Ctrl Pts',(12.1623797632096,105.874999999587,3.95179673813132));
#287575=CARTESIAN_POINT('Ctrl Pts',(12.1623797632096,106.024999999586,-1.48946194470292E-15));
#287576=CARTESIAN_POINT('Ctrl Pts',(12.1623797632096,106.174999999585,-3.95179673813132));
#287577=CARTESIAN_POINT('Ctrl Pts',(9.83957192047848,106.324999999585,-7.14886745759505));
#287578=CARTESIAN_POINT('Ctrl Pts',(7.51676407774738,106.474999999584,-10.3459381770588));
#287579=CARTESIAN_POINT('Ctrl Pts',(3.75838203887365,106.624999999584,-11.5671105274568));
#287580=CARTESIAN_POINT('Ctrl Pts',(-7.47527323974508E-14,106.774999999583,
-12.7882828778549));
#287581=CARTESIAN_POINT('Ctrl Pts',(-3.7583820388738,106.924999999582,-11.5671105274568));
#287582=CARTESIAN_POINT('Ctrl Pts',(-7.51676407774753,107.074999999582,
-10.3459381770588));
#287583=CARTESIAN_POINT('Ctrl Pts',(-9.83957192047862,107.224999999581,
-7.14886745759505));
#287584=CARTESIAN_POINT('Ctrl Pts',(-12.1623797632097,107.374999999581,
-3.95179673813132));
#287585=CARTESIAN_POINT('Ctrl Pts',(-12.1623797632097,107.52499999958,2.97892388940585E-15));
#287586=CARTESIAN_POINT('Ctrl Pts',(-12.1623797632097,107.674999999579,
3.95179673813133));
#287587=CARTESIAN_POINT('Ctrl Pts',(-9.83957192047862,107.824999999579,
7.14886745759505));
#287588=CARTESIAN_POINT('Ctrl Pts',(-7.51676407774753,107.974999999578,
10.3459381770588));
#287589=CARTESIAN_POINT('Ctrl Pts',(-3.7583820388738,108.124999999578,11.5671105274568));
#287590=CARTESIAN_POINT('Ctrl Pts',(-7.24843610946905E-14,108.274999999577,
12.7882828778549));
#287591=CARTESIAN_POINT('Ctrl Pts',(3.75838203887366,108.424999999576,11.5671105274568));
#287592=CARTESIAN_POINT('Ctrl Pts',(7.51676407774738,108.574999999576,10.3459381770588));
#287593=CARTESIAN_POINT('Ctrl Pts',(9.83957192047847,108.724999999575,7.14886745759505));
#287594=CARTESIAN_POINT('Ctrl Pts',(12.1623797632096,108.874999999575,3.95179673813132));
#287595=CARTESIAN_POINT('Ctrl Pts',(12.1623797632096,109.024999999574,-1.48946194470292E-15));
#287596=CARTESIAN_POINT('Ctrl Pts',(12.1623797632096,109.174999999573,-3.95179673813132));
#287597=CARTESIAN_POINT('Ctrl Pts',(9.83957192047847,109.324999999573,-7.14886745759505));
#287598=CARTESIAN_POINT('Ctrl Pts',(7.51676407774738,109.474999999572,-10.3459381770588));
#287599=CARTESIAN_POINT('Ctrl Pts',(3.75838203887365,109.624999999572,-11.5671105274568));
#287600=CARTESIAN_POINT('Ctrl Pts',(-7.64804416691126E-14,109.774999999571,
-12.7882828778549));
#287601=CARTESIAN_POINT('Ctrl Pts',(-3.7583820388738,109.92499999957,-11.5671105274568));
#287602=CARTESIAN_POINT('Ctrl Pts',(-7.51676407774753,110.07499999957,-10.3459381770588));
#287603=CARTESIAN_POINT('Ctrl Pts',(-9.83957192047862,110.224999999569,
-7.14886745759505));
#287604=CARTESIAN_POINT('Ctrl Pts',(-12.1623797632097,110.374999999569,
-3.95179673813132));
#287605=CARTESIAN_POINT('Ctrl Pts',(-12.1623797632097,110.524999999568,
2.97892388940585E-15));
#287606=CARTESIAN_POINT('Ctrl Pts',(-12.1623797632097,110.674999999567,
3.95179673813133));
#287607=CARTESIAN_POINT('Ctrl Pts',(-9.83957192047862,110.824999999567,
7.14886745759505));
#287608=CARTESIAN_POINT('Ctrl Pts',(-7.51676407774753,110.974999999566,
10.3459381770588));
#287609=CARTESIAN_POINT('Ctrl Pts',(-3.7583820388738,111.124999999566,11.5671105274568));
#287610=CARTESIAN_POINT('Ctrl Pts',(-7.42120703663524E-14,111.274999999565,
12.7882828778549));
#287611=CARTESIAN_POINT('Ctrl Pts',(3.75838203887365,111.424999999564,11.5671105274568));
#287612=CARTESIAN_POINT('Ctrl Pts',(7.51676407774738,111.574999999564,10.3459381770588));
#287613=CARTESIAN_POINT('Ctrl Pts',(9.83957192047847,111.724999999563,7.14886745759505));
#287614=CARTESIAN_POINT('Ctrl Pts',(12.1623797632096,111.874999999563,3.95179673813132));
#287615=CARTESIAN_POINT('Ctrl Pts',(12.1623797632096,112.024999999562,-1.48946194470292E-15));
#287616=CARTESIAN_POINT('Ctrl Pts',(12.1623797632096,112.174999999561,-3.95179673813132));
#287617=CARTESIAN_POINT('Ctrl Pts',(9.83957192047847,112.324999999561,-7.14886745759505));
#287618=CARTESIAN_POINT('Ctrl Pts',(7.51676407774738,112.47499999956,-10.3459381770588));
#287619=CARTESIAN_POINT('Ctrl Pts',(3.75838203887365,112.62499999956,-11.5671105274568));
#287620=CARTESIAN_POINT('Ctrl Pts',(-7.82081509407745E-14,112.774999999559,
-12.7882828778549));
#287621=CARTESIAN_POINT('Ctrl Pts',(-3.75838203887381,112.924999999558,
-11.5671105274568));
#287622=CARTESIAN_POINT('Ctrl Pts',(-7.51676407774753,113.074999999558,
-10.3459381770588));
#287623=CARTESIAN_POINT('Ctrl Pts',(-9.83957192047863,113.224999999557,
-7.14886745759505));
#287624=CARTESIAN_POINT('Ctrl Pts',(-12.1623797632097,113.374999999557,
-3.95179673813132));
#287625=CARTESIAN_POINT('Ctrl Pts',(-12.1623797632097,113.524999999556,
2.97892388940585E-15));
#287626=CARTESIAN_POINT('Ctrl Pts',(-12.1623797632097,113.674999999555,
3.95179673813133));
#287627=CARTESIAN_POINT('Ctrl Pts',(-9.83957192047863,113.824999999555,
7.14886745759505));
#287628=CARTESIAN_POINT('Ctrl Pts',(-7.51676407774753,113.974999999554,
10.3459381770588));
#287629=CARTESIAN_POINT('Ctrl Pts',(-3.7583820388738,114.124999999554,11.5671105274568));
#287630=CARTESIAN_POINT('Ctrl Pts',(-7.59397796380142E-14,114.274999999553,
12.7882828778549));
#287631=CARTESIAN_POINT('Ctrl Pts',(3.75838203887365,114.424999999552,11.5671105274568));
#287632=CARTESIAN_POINT('Ctrl Pts',(7.51676407774738,114.574999999552,10.3459381770588));
#287633=CARTESIAN_POINT('Ctrl Pts',(9.83957192047847,114.724999999551,7.14886745759505));
#287634=CARTESIAN_POINT('Ctrl Pts',(12.1623797632096,114.874999999551,3.95179673813132));
#287635=CARTESIAN_POINT('Ctrl Pts',(12.1623797632096,115.02499999955,-1.48946194470292E-15));
#287636=CARTESIAN_POINT('Ctrl Pts',(12.1623797632096,115.174999999549,-3.95179673813132));
#287637=CARTESIAN_POINT('Ctrl Pts',(9.83957192047847,115.324999999549,-7.14886745759505));
#287638=CARTESIAN_POINT('Ctrl Pts',(7.51676407774738,115.474999999548,-10.3459381770588));
#287639=CARTESIAN_POINT('Ctrl Pts',(3.75838203887365,115.624999999548,-11.5671105274568));
#287640=CARTESIAN_POINT('Ctrl Pts',(-7.99358602124363E-14,115.774999999547,
-12.7882828778549));
#287641=CARTESIAN_POINT('Ctrl Pts',(-3.75838203887381,115.924999999546,
-11.5671105274568));
#287642=CARTESIAN_POINT('Ctrl Pts',(-7.51676407774754,116.074999999546,
-10.3459381770588));
#287643=CARTESIAN_POINT('Ctrl Pts',(-9.83957192047863,116.224999999545,
-7.14886745759505));
#287644=CARTESIAN_POINT('Ctrl Pts',(-12.1623797632097,116.374999999545,
-3.95179673813132));
#287645=CARTESIAN_POINT('Ctrl Pts',(-12.1623797632097,116.524999999544,
2.97892388940585E-15));
#287646=CARTESIAN_POINT('Ctrl Pts',(-12.1623797632097,116.674999999543,
3.95179673813133));
#287647=CARTESIAN_POINT('Ctrl Pts',(-9.83957192047863,116.824999999543,
7.14886745759505));
#287648=CARTESIAN_POINT('Ctrl Pts',(-7.51676407774753,116.974999999542,
10.3459381770588));
#287649=CARTESIAN_POINT('Ctrl Pts',(-3.75838203887381,117.124999999542,
11.5671105274568));
#287650=CARTESIAN_POINT('Ctrl Pts',(-7.76674889096761E-14,117.274999999541,
12.7882828778549));
#287651=CARTESIAN_POINT('Ctrl Pts',(3.75838203887365,117.42499999954,11.5671105274568));
#287652=CARTESIAN_POINT('Ctrl Pts',(7.51676407774738,117.57499999954,10.3459381770588));
#287653=CARTESIAN_POINT('Ctrl Pts',(9.83957192047847,117.724999999539,7.14886745759505));
#287654=CARTESIAN_POINT('Ctrl Pts',(12.1623797632096,117.874999999539,3.95179673813132));
#287655=CARTESIAN_POINT('Ctrl Pts',(12.1623797632096,118.024999999538,-1.48946194470292E-15));
#287656=CARTESIAN_POINT('Ctrl Pts',(12.1623797632096,118.174999999537,-3.95179673813132));
#287657=CARTESIAN_POINT('Ctrl Pts',(9.83957192047847,118.324999999537,-7.14886745759505));
#287658=CARTESIAN_POINT('Ctrl Pts',(7.51676407774737,118.474999999536,-10.3459381770588));
#287659=CARTESIAN_POINT('Ctrl Pts',(3.75838203887365,118.624999999536,-11.5671105274568));
#287660=CARTESIAN_POINT('Ctrl Pts',(-8.16635694840981E-14,118.774999999535,
-12.7882828778549));
#287661=CARTESIAN_POINT('Ctrl Pts',(-3.75838203887381,118.924999999534,
-11.5671105274568));
#287662=CARTESIAN_POINT('Ctrl Pts',(-7.51676407774754,119.074999999534,
-10.3459381770588));
#287663=CARTESIAN_POINT('Ctrl Pts',(-9.83957192047863,119.224999999533,
-7.14886745759505));
#287664=CARTESIAN_POINT('Ctrl Pts',(-12.1623797632097,119.374999999533,
-3.95179673813132));
#287665=CARTESIAN_POINT('Ctrl Pts',(-12.1623797632097,119.524999999532,
2.97892388940585E-15));
#287666=CARTESIAN_POINT('Ctrl Pts',(-12.1623797632097,119.674999999531,
3.95179673813133));
#287667=CARTESIAN_POINT('Ctrl Pts',(-9.83957192047863,119.824999999531,
7.14886745759505));
#287668=CARTESIAN_POINT('Ctrl Pts',(-7.51676407774754,119.97499999953,10.3459381770588));
#287669=CARTESIAN_POINT('Ctrl Pts',(-3.75838203887381,120.12499999953,11.5671105274568));
#287670=CARTESIAN_POINT('Ctrl Pts',(-7.93951981813379E-14,120.274999999529,
12.7882828778549));
#287671=CARTESIAN_POINT('Ctrl Pts',(3.75838203887365,120.424999999528,11.5671105274568));
#287672=CARTESIAN_POINT('Ctrl Pts',(7.51676407774738,120.574999999528,10.3459381770588));
#287673=CARTESIAN_POINT('Ctrl Pts',(9.83957192047847,120.724999999527,7.14886745759505));
#287674=CARTESIAN_POINT('Ctrl Pts',(12.1623797632096,120.874999999527,3.95179673813132));
#287675=CARTESIAN_POINT('Ctrl Pts',(12.1623797632096,121.024999999526,-1.48946194470292E-15));
#287676=CARTESIAN_POINT('Ctrl Pts',(12.1623797632096,121.174999999525,-3.95179673813132));
#287677=CARTESIAN_POINT('Ctrl Pts',(9.83957192047847,121.324999999525,-7.14886745759505));
#287678=CARTESIAN_POINT('Ctrl Pts',(7.51676407774737,121.474999999524,-10.3459381770588));
#287679=CARTESIAN_POINT('Ctrl Pts',(3.75838203887364,121.624999999524,-11.5671105274568));
#287680=CARTESIAN_POINT('Ctrl Pts',(-8.339127875576E-14,121.774999999523,
-12.7882828778549));
#287681=CARTESIAN_POINT('Ctrl Pts',(-3.75838203887381,121.924999999522,
-11.5671105274568));
#287682=CARTESIAN_POINT('Ctrl Pts',(-7.51676407774754,122.074999999522,
-10.3459381770588));
#287683=CARTESIAN_POINT('Ctrl Pts',(-9.83957192047863,122.224999999521,
-7.14886745759505));
#287684=CARTESIAN_POINT('Ctrl Pts',(-12.1623797632097,122.374999999521,
-3.95179673813132));
#287685=CARTESIAN_POINT('Ctrl Pts',(-12.1623797632097,122.52499999952,2.97892388940585E-15));
#287686=CARTESIAN_POINT('Ctrl Pts',(-12.1623797632097,122.674999999519,
3.95179673813133));
#287687=CARTESIAN_POINT('Ctrl Pts',(-9.83957192047863,122.824999999519,
7.14886745759505));
#287688=CARTESIAN_POINT('Ctrl Pts',(-7.51676407774754,122.974999999518,
10.3459381770588));
#287689=CARTESIAN_POINT('Ctrl Pts',(-3.75838203887381,123.124999999518,
11.5671105274568));
#287690=CARTESIAN_POINT('Ctrl Pts',(-8.11229074529997E-14,123.274999999517,
12.7882828778549));
#287691=CARTESIAN_POINT('Ctrl Pts',(3.75838203887365,123.424999999516,11.5671105274568));
#287692=CARTESIAN_POINT('Ctrl Pts',(7.51676407774737,123.574999999516,10.3459381770588));
#287693=CARTESIAN_POINT('Ctrl Pts',(9.83957192047846,123.724999999515,7.14886745759505));
#287694=CARTESIAN_POINT('Ctrl Pts',(12.1623797632096,123.874999999515,3.95179673813132));
#287695=CARTESIAN_POINT('Ctrl Pts',(12.1623797632096,124.024999999514,-1.48946194470292E-15));
#287696=CARTESIAN_POINT('Ctrl Pts',(12.1623797632096,124.174999999513,-3.95179673813132));
#287697=CARTESIAN_POINT('Ctrl Pts',(9.83957192047846,124.324999999513,-7.14886745759505));
#287698=CARTESIAN_POINT('Ctrl Pts',(7.51676407774737,124.474999999512,-10.3459381770588));
#287699=CARTESIAN_POINT('Ctrl Pts',(3.75838203887364,124.624999999512,-11.5671105274568));
#287700=CARTESIAN_POINT('Ctrl Pts',(-8.51189880274219E-14,124.774999999511,
-12.7882828778549));
#287701=CARTESIAN_POINT('Ctrl Pts',(-3.75838203887381,124.92499999951,-11.5671105274568));
#287702=CARTESIAN_POINT('Ctrl Pts',(-7.51676407774754,125.07499999951,-10.3459381770588));
#287703=CARTESIAN_POINT('Ctrl Pts',(-9.83957192047863,125.224999999509,
-7.14886745759505));
#287704=CARTESIAN_POINT('Ctrl Pts',(-12.1623797632097,125.374999999509,
-3.95179673813132));
#287705=CARTESIAN_POINT('Ctrl Pts',(-12.1623797632097,125.524999999508,
2.97892388940585E-15));
#287706=CARTESIAN_POINT('Ctrl Pts',(-12.1623797632097,125.674999999507,
3.95179673813133));
#287707=CARTESIAN_POINT('Ctrl Pts',(-9.83957192047863,125.824999999507,
7.14886745759505));
#287708=CARTESIAN_POINT('Ctrl Pts',(-7.51676407774754,125.974999999506,
10.3459381770588));
#287709=CARTESIAN_POINT('Ctrl Pts',(-3.75838203887381,126.124999999506,
11.5671105274568));
#287710=CARTESIAN_POINT('Ctrl Pts',(-8.28506167246616E-14,126.274999999505,
12.7882828778549));
#287711=CARTESIAN_POINT('Ctrl Pts',(3.75838203887364,126.424999999504,11.5671105274568));
#287712=CARTESIAN_POINT('Ctrl Pts',(7.51676407774737,126.574999999504,10.3459381770588));
#287713=CARTESIAN_POINT('Ctrl Pts',(9.83957192047846,126.724999999503,7.14886745759505));
#287714=CARTESIAN_POINT('Ctrl Pts',(12.1623797632096,126.874999999503,3.95179673813132));
#287715=CARTESIAN_POINT('Ctrl Pts',(12.1623797632096,127.024999999502,-1.48946194470292E-15));
#287716=CARTESIAN_POINT('Ctrl Pts',(12.1623797632096,127.174999999501,-3.95179673813132));
#287717=CARTESIAN_POINT('Ctrl Pts',(9.83957192047846,127.324999999501,-7.14886745759505));
#287718=CARTESIAN_POINT('Ctrl Pts',(7.51676407774737,127.4749999995,-10.3459381770588));
#287719=CARTESIAN_POINT('Ctrl Pts',(3.75838203887364,127.6249999995,-11.5671105274568));
#287720=CARTESIAN_POINT('Ctrl Pts',(-8.68466972990837E-14,127.774999999499,
-12.7882828778549));
#287721=CARTESIAN_POINT('Ctrl Pts',(-3.75838203887381,127.924999999498,
-11.5671105274568));
#287722=CARTESIAN_POINT('Ctrl Pts',(-7.51676407774754,128.074999999498,
-10.3459381770588));
#287723=CARTESIAN_POINT('Ctrl Pts',(-9.83957192047864,128.224999999497,
-7.14886745759505));
#287724=CARTESIAN_POINT('Ctrl Pts',(-12.1623797632097,128.374999999497,
-3.95179673813132));
#287725=CARTESIAN_POINT('Ctrl Pts',(-12.1623797632097,128.524999999496,
2.97892388940585E-15));
#287726=CARTESIAN_POINT('Ctrl Pts',(-12.1623797632097,128.674999999495,
3.95179673813133));
#287727=CARTESIAN_POINT('Ctrl Pts',(-9.83957192047864,128.824999999495,
7.14886745759505));
#287728=CARTESIAN_POINT('Ctrl Pts',(-7.51676407774754,128.974999999494,
10.3459381770588));
#287729=CARTESIAN_POINT('Ctrl Pts',(-3.75838203887381,129.124999999494,
11.5671105274568));
#287730=CARTESIAN_POINT('Ctrl Pts',(-8.45783259963234E-14,129.274999999493,
12.7882828778549));
#287731=CARTESIAN_POINT('Ctrl Pts',(3.75838203887364,129.424999999492,11.5671105274568));
#287732=CARTESIAN_POINT('Ctrl Pts',(7.51676407774737,129.574999999492,10.3459381770588));
#287733=CARTESIAN_POINT('Ctrl Pts',(9.83957192047846,129.724999999491,7.14886745759505));
#287734=CARTESIAN_POINT('Ctrl Pts',(12.1623797632096,129.874999999491,3.95179673813132));
#287735=CARTESIAN_POINT('Ctrl Pts',(12.1623797632096,130.02499999949,-1.48946194470292E-15));
#287736=CARTESIAN_POINT('Ctrl Pts',(12.1623797632096,130.174999999489,-3.95179673813132));
#287737=CARTESIAN_POINT('Ctrl Pts',(9.83957192047846,130.324999999489,-7.14886745759505));
#287738=CARTESIAN_POINT('Ctrl Pts',(7.51676407774737,130.474999999488,-10.3459381770588));
#287739=CARTESIAN_POINT('Ctrl Pts',(3.75838203887364,130.624999999488,-11.5671105274568));
#287740=CARTESIAN_POINT('Ctrl Pts',(-8.85744065707455E-14,130.774999999487,
-12.7882828778549));
#287741=CARTESIAN_POINT('Ctrl Pts',(-3.75838203887382,130.924999999486,
-11.5671105274568));
#287742=CARTESIAN_POINT('Ctrl Pts',(-7.51676407774754,131.074999999486,
-10.3459381770588));
#287743=CARTESIAN_POINT('Ctrl Pts',(-9.83957192047864,131.224999999485,
-7.14886745759505));
#287744=CARTESIAN_POINT('Ctrl Pts',(-12.1623797632097,131.374999999485,
-3.95179673813132));
#287745=CARTESIAN_POINT('Ctrl Pts',(-12.1623797632097,131.524999999484,
2.97892388940585E-15));
#287746=CARTESIAN_POINT('Ctrl Pts',(-12.1623797632097,131.674999999483,
3.95179673813133));
#287747=CARTESIAN_POINT('Ctrl Pts',(-9.83957192047864,131.824999999483,
7.14886745759505));
#287748=CARTESIAN_POINT('Ctrl Pts',(-7.51676407774754,131.974999999482,
10.3459381770588));
#287749=CARTESIAN_POINT('Ctrl Pts',(-3.75838203887381,132.124999999482,
11.5671105274568));
#287750=CARTESIAN_POINT('Ctrl Pts',(-8.63060352679853E-14,132.274999999481,
12.7882828778549));
#287751=CARTESIAN_POINT('Ctrl Pts',(3.75838203887364,132.42499999948,11.5671105274568));
#287752=CARTESIAN_POINT('Ctrl Pts',(7.51676407774737,132.57499999948,10.3459381770588));
#287753=CARTESIAN_POINT('Ctrl Pts',(9.83957192047846,132.724999999479,7.14886745759505));
#287754=CARTESIAN_POINT('Ctrl Pts',(12.1623797632096,132.874999999479,3.95179673813132));
#287755=CARTESIAN_POINT('Ctrl Pts',(12.1623797632096,133.024999999478,-1.48946194470292E-15));
#287756=CARTESIAN_POINT('Ctrl Pts',(12.1623797632096,133.174999999477,-3.95179673813132));
#287757=CARTESIAN_POINT('Ctrl Pts',(9.83957192047846,133.324999999477,-7.14886745759505));
#287758=CARTESIAN_POINT('Ctrl Pts',(7.51676407774736,133.474999999476,-10.3459381770588));
#287759=CARTESIAN_POINT('Ctrl Pts',(3.75838203887364,133.624999999476,-11.5671105274568));
#287760=CARTESIAN_POINT('Ctrl Pts',(-9.03021158424074E-14,133.774999999475,
-12.7882828778549));
#287761=CARTESIAN_POINT('Ctrl Pts',(-3.75838203887382,133.924999999474,
-11.5671105274568));
#287762=CARTESIAN_POINT('Ctrl Pts',(-7.51676407774755,134.074999999474,
-10.3459381770588));
#287763=CARTESIAN_POINT('Ctrl Pts',(-9.83957192047864,134.224999999473,
-7.14886745759505));
#287764=CARTESIAN_POINT('Ctrl Pts',(-12.1623797632097,134.374999999473,
-3.95179673813132));
#287765=CARTESIAN_POINT('Ctrl Pts',(-12.1623797632097,134.524999999472,
2.97892388940585E-15));
#287766=CARTESIAN_POINT('Ctrl Pts',(-12.1623797632097,134.674999999471,
3.95179673813133));
#287767=CARTESIAN_POINT('Ctrl Pts',(-9.83957192047864,134.824999999471,
7.14886745759505));
#287768=CARTESIAN_POINT('Ctrl Pts',(-7.51676407774754,134.97499999947,10.3459381770588));
#287769=CARTESIAN_POINT('Ctrl Pts',(-3.75838203887382,135.12499999947,11.5671105274568));
#287770=CARTESIAN_POINT('Ctrl Pts',(-8.80337445396471E-14,135.274999999469,
12.7882828778549));
#287771=CARTESIAN_POINT('Ctrl Pts',(3.75838203887364,135.424999999468,11.5671105274568));
#287772=CARTESIAN_POINT('Ctrl Pts',(7.51676407774737,135.574999999468,10.3459381770588));
#287773=CARTESIAN_POINT('Ctrl Pts',(9.83957192047846,135.724999999467,7.14886745759505));
#287774=CARTESIAN_POINT('Ctrl Pts',(12.1623797632096,135.874999999467,3.95179673813132));
#287775=CARTESIAN_POINT('Ctrl Pts',(12.1623797632096,136.024999999466,-1.48946194470292E-15));
#287776=CARTESIAN_POINT('Ctrl Pts',(12.1623797632095,136.174999999465,-3.95179673813132));
#287777=CARTESIAN_POINT('Ctrl Pts',(9.83957192047846,136.324999999465,-7.14886745759505));
#287778=CARTESIAN_POINT('Ctrl Pts',(7.51676407774736,136.474999999464,-10.3459381770588));
#287779=CARTESIAN_POINT('Ctrl Pts',(3.75838203887364,136.624999999464,-11.5671105274568));
#287780=CARTESIAN_POINT('Ctrl Pts',(-9.20298251140692E-14,136.774999999463,
-12.7882828778549));
#287781=CARTESIAN_POINT('Ctrl Pts',(-3.75838203887382,136.924999999462,
-11.5671105274568));
#287782=CARTESIAN_POINT('Ctrl Pts',(-7.51676407774755,137.074999999462,
-10.3459381770588));
#287783=CARTESIAN_POINT('Ctrl Pts',(-9.83957192047864,137.224999999461,
-7.14886745759505));
#287784=CARTESIAN_POINT('Ctrl Pts',(-12.1623797632097,137.374999999461,
-3.95179673813132));
#287785=CARTESIAN_POINT('Ctrl Pts',(-12.1623797632097,137.52499999946,2.97892388940585E-15));
#287786=CARTESIAN_POINT('Ctrl Pts',(-12.1623797632097,137.674999999459,
3.95179673813133));
#287787=CARTESIAN_POINT('Ctrl Pts',(-9.83957192047864,137.824999999459,
7.14886745759505));
#287788=CARTESIAN_POINT('Ctrl Pts',(-7.51676407774755,137.974999999458,
10.3459381770588));
#287789=CARTESIAN_POINT('Ctrl Pts',(-3.75838203887382,138.124999999458,
11.5671105274568));
#287790=CARTESIAN_POINT('Ctrl Pts',(-8.97614538113089E-14,138.274999999457,
12.7882828778549));
#287791=CARTESIAN_POINT('Ctrl Pts',(3.75838203887364,138.424999999456,11.5671105274568));
#287792=CARTESIAN_POINT('Ctrl Pts',(7.51676407774736,138.574999999456,10.3459381770588));
#287793=CARTESIAN_POINT('Ctrl Pts',(9.83957192047846,138.724999999455,7.14886745759505));
#287794=CARTESIAN_POINT('Ctrl Pts',(12.1623797632096,138.874999999455,3.95179673813132));
#287795=CARTESIAN_POINT('Ctrl Pts',(12.1623797632096,139.024999999454,-1.48946194470292E-15));
#287796=CARTESIAN_POINT('Ctrl Pts',(12.1623797632095,139.174999999453,-3.95179673813132));
#287797=CARTESIAN_POINT('Ctrl Pts',(9.83957192047846,139.324999999453,-7.14886745759505));
#287798=CARTESIAN_POINT('Ctrl Pts',(7.51676407774736,139.474999999452,-10.3459381770588));
#287799=CARTESIAN_POINT('Ctrl Pts',(3.75838203887363,139.624999999452,-11.5671105274568));
#287800=CARTESIAN_POINT('Ctrl Pts',(-9.3757534385731E-14,139.774999999451,
-12.7882828778549));
#287801=CARTESIAN_POINT('Ctrl Pts',(-3.75838203887382,139.92499999945,-11.5671105274568));
#287802=CARTESIAN_POINT('Ctrl Pts',(-7.51676407774755,140.07499999945,-10.3459381770588));
#287803=CARTESIAN_POINT('Ctrl Pts',(-9.83957192047864,140.224999999449,
-7.14886745759505));
#287804=CARTESIAN_POINT('Ctrl Pts',(-12.1623797632097,140.374999999449,
-3.95179673813132));
#287805=CARTESIAN_POINT('Ctrl Pts',(-12.1623797632097,140.524999999448,
2.97892388940585E-15));
#287806=CARTESIAN_POINT('Ctrl Pts',(-12.1623797632097,140.674999999447,
3.95179673813133));
#287807=CARTESIAN_POINT('Ctrl Pts',(-9.83957192047864,140.824999999447,
7.14886745759505));
#287808=CARTESIAN_POINT('Ctrl Pts',(-7.51676407774755,140.974999999446,
10.3459381770588));
#287809=CARTESIAN_POINT('Ctrl Pts',(-3.75838203887382,141.124999999446,
11.5671105274568));
#287810=CARTESIAN_POINT('Ctrl Pts',(-9.14891630829708E-14,141.274999999445,
12.7882828778549));
#287811=CARTESIAN_POINT('Ctrl Pts',(3.75838203887364,141.424999999444,11.5671105274568));
#287812=CARTESIAN_POINT('Ctrl Pts',(7.51676407774736,141.574999999444,10.3459381770588));
#287813=CARTESIAN_POINT('Ctrl Pts',(9.83957192047845,141.724999999443,7.14886745759505));
#287814=CARTESIAN_POINT('Ctrl Pts',(12.1623797632095,141.874999999443,3.95179673813132));
#287815=CARTESIAN_POINT('Ctrl Pts',(12.1623797632095,142.024999999442,-1.48946194470292E-15));
#287816=CARTESIAN_POINT('Ctrl Pts',(12.1623797632095,142.174999999441,-3.95179673813132));
#287817=CARTESIAN_POINT('Ctrl Pts',(9.83957192047845,142.324999999441,-7.14886745759505));
#287818=CARTESIAN_POINT('Ctrl Pts',(7.51676407774736,142.47499999944,-10.3459381770588));
#287819=CARTESIAN_POINT('Ctrl Pts',(3.75838203887363,142.62499999944,-11.5671105274568));
#287820=CARTESIAN_POINT('Ctrl Pts',(-9.54852436573929E-14,142.774999999439,
-12.7882828778549));
#287821=CARTESIAN_POINT('Ctrl Pts',(-3.75838203887382,142.924999999438,
-11.5671105274568));
#287822=CARTESIAN_POINT('Ctrl Pts',(-7.51676407774755,143.074999999438,
-10.3459381770588));
#287823=CARTESIAN_POINT('Ctrl Pts',(-9.83957192047864,143.224999999437,
-7.14886745759505));
#287824=CARTESIAN_POINT('Ctrl Pts',(-12.1623797632097,143.374999999437,
-3.95179673813132));
#287825=CARTESIAN_POINT('Ctrl Pts',(-12.1623797632097,143.524999999436,
2.97892388940585E-15));
#287826=CARTESIAN_POINT('Ctrl Pts',(-12.1623797632097,143.674999999435,
3.95179673813133));
#287827=CARTESIAN_POINT('Ctrl Pts',(-9.83957192047864,143.824999999435,
7.14886745759505));
#287828=CARTESIAN_POINT('Ctrl Pts',(-7.51676407774755,143.974999999434,
10.3459381770588));
#287829=CARTESIAN_POINT('Ctrl Pts',(-3.75838203887382,144.124999999434,
11.5671105274568));
#287830=CARTESIAN_POINT('Ctrl Pts',(-9.32168723546326E-14,144.274999999433,
12.7882828778549));
#287831=CARTESIAN_POINT('Ctrl Pts',(3.75838203887363,144.424999999432,11.5671105274568));
#287832=CARTESIAN_POINT('Ctrl Pts',(7.51676407774736,144.574999999432,10.3459381770588));
#287833=CARTESIAN_POINT('Ctrl Pts',(9.83957192047845,144.724999999431,7.14886745759505));
#287834=CARTESIAN_POINT('Ctrl Pts',(12.1623797632095,144.874999999431,3.95179673813132));
#287835=CARTESIAN_POINT('Ctrl Pts',(12.1623797632095,145.02499999943,-1.48946194470292E-15));
#287836=CARTESIAN_POINT('Ctrl Pts',(12.1623797632095,145.174999999429,-3.95179673813132));
#287837=CARTESIAN_POINT('Ctrl Pts',(9.83957192047845,145.324999999429,-7.14886745759505));
#287838=CARTESIAN_POINT('Ctrl Pts',(7.51676407774736,145.474999999428,-10.3459381770588));
#287839=CARTESIAN_POINT('Ctrl Pts',(3.75838203887363,145.624999999428,-11.5671105274568));
#287840=CARTESIAN_POINT('Ctrl Pts',(-9.72129529290547E-14,145.774999999427,
-12.7882828778549));
#287841=CARTESIAN_POINT('Ctrl Pts',(-3.75838203887382,145.924999999426,
-11.5671105274568));
#287842=CARTESIAN_POINT('Ctrl Pts',(-7.51676407774755,146.074999999426,
-10.3459381770588));
#287843=CARTESIAN_POINT('Ctrl Pts',(-9.83957192047865,146.224999999425,
-7.14886745759505));
#287844=CARTESIAN_POINT('Ctrl Pts',(-12.1623797632097,146.374999999425,
-3.95179673813132));
#287845=CARTESIAN_POINT('Ctrl Pts',(-12.1623797632097,146.524999999424,
2.97892388940585E-15));
#287846=CARTESIAN_POINT('Ctrl Pts',(-12.1623797632097,146.674999999423,
3.95179673813133));
#287847=CARTESIAN_POINT('Ctrl Pts',(-9.83957192047865,146.824999999423,
7.14886745759505));
#287848=CARTESIAN_POINT('Ctrl Pts',(-7.51676407774755,146.974999999422,
10.3459381770588));
#287849=CARTESIAN_POINT('Ctrl Pts',(-3.75838203887382,147.124999999422,
11.5671105274568));
#287850=CARTESIAN_POINT('Ctrl Pts',(-9.49445816262944E-14,147.274999999421,
12.7882828778549));
#287851=CARTESIAN_POINT('Ctrl Pts',(3.75838203887363,147.42499999942,11.5671105274568));
#287852=CARTESIAN_POINT('Ctrl Pts',(7.51676407774736,147.57499999942,10.3459381770588));
#287853=CARTESIAN_POINT('Ctrl Pts',(9.83957192047845,147.724999999419,7.14886745759505));
#287854=CARTESIAN_POINT('Ctrl Pts',(12.1623797632095,147.874999999419,3.95179673813132));
#287855=CARTESIAN_POINT('Ctrl Pts',(12.1623797632095,148.024999999418,-1.48946194470292E-15));
#287856=CARTESIAN_POINT('Ctrl Pts',(12.1623797632095,148.174999999417,-3.95179673813132));
#287857=CARTESIAN_POINT('Ctrl Pts',(9.83957192047845,148.324999999417,-7.14886745759505));
#287858=CARTESIAN_POINT('Ctrl Pts',(7.51676407774736,148.474999999416,-10.3459381770588));
#287859=CARTESIAN_POINT('Ctrl Pts',(3.75838203887363,148.624999999416,-11.5671105274568));
#287860=CARTESIAN_POINT('Ctrl Pts',(-9.89406622007166E-14,148.774999999415,
-12.7882828778549));
#287861=CARTESIAN_POINT('Ctrl Pts',(-3.75838203887383,148.924999999414,
-11.5671105274568));
#287862=CARTESIAN_POINT('Ctrl Pts',(-7.51676407774756,149.074999999414,
-10.3459381770588));
#287863=CARTESIAN_POINT('Ctrl Pts',(-9.83957192047865,149.224999999413,
-7.14886745759505));
#287864=CARTESIAN_POINT('Ctrl Pts',(-12.1623797632097,149.374999999413,
-3.95179673813132));
#287865=CARTESIAN_POINT('Ctrl Pts',(-12.1623797632097,149.524999999412,
2.97892388940585E-15));
#287866=CARTESIAN_POINT('Ctrl Pts',(-12.1623797632097,149.674999999411,
3.95179673813133));
#287867=CARTESIAN_POINT('Ctrl Pts',(-9.83957192047865,149.824999999411,
7.14886745759505));
#287868=CARTESIAN_POINT('Ctrl Pts',(-7.51676407774755,149.97499999941,10.3459381770588));
#287869=CARTESIAN_POINT('Ctrl Pts',(-3.75838203887382,150.12499999941,11.5671105274568));
#287870=CARTESIAN_POINT('Ctrl Pts',(-9.66722908979563E-14,150.274999999409,
12.7882828778549));
#287871=CARTESIAN_POINT('Ctrl Pts',(3.75838203887363,150.424999999408,11.5671105274568));
#287872=CARTESIAN_POINT('Ctrl Pts',(7.51676407774736,150.574999999408,10.3459381770588));
#287873=CARTESIAN_POINT('Ctrl Pts',(9.83957192047845,150.724999999407,7.14886745759505));
#287874=CARTESIAN_POINT('Ctrl Pts',(12.1623797632095,150.874999999407,3.95179673813132));
#287875=CARTESIAN_POINT('Ctrl Pts',(12.1623797632095,151.024999999406,-1.48946194470292E-15));
#287876=CARTESIAN_POINT('Ctrl Pts',(12.1623797632095,151.174999999405,-3.95179673813132));
#287877=CARTESIAN_POINT('Ctrl Pts',(9.83957192047845,151.324999999405,-7.14886745759505));
#287878=CARTESIAN_POINT('Ctrl Pts',(7.51676407774736,151.474999999404,-10.3459381770588));
#287879=CARTESIAN_POINT('Ctrl Pts',(3.75838203887363,151.624999999404,-11.5671105274568));
#287880=CARTESIAN_POINT('Ctrl Pts',(-1.00668371472378E-13,151.774999999403,
-12.7882828778549));
#287881=CARTESIAN_POINT('Ctrl Pts',(-3.75838203887383,151.924999999402,
-11.5671105274568));
#287882=CARTESIAN_POINT('Ctrl Pts',(-7.51676407774756,152.074999999402,
-10.3459381770588));
#287883=CARTESIAN_POINT('Ctrl Pts',(-9.83957192047865,152.224999999401,
-7.14886745759505));
#287884=CARTESIAN_POINT('Ctrl Pts',(-12.1623797632097,152.374999999401,
-3.95179673813132));
#287885=CARTESIAN_POINT('Ctrl Pts',(-12.1623797632097,152.5249999994,2.97892388940585E-15));
#287886=CARTESIAN_POINT('Ctrl Pts',(-12.1623797632097,152.674999999399,
3.95179673813133));
#287887=CARTESIAN_POINT('Ctrl Pts',(-9.83957192047865,152.824999999399,
7.14886745759505));
#287888=CARTESIAN_POINT('Ctrl Pts',(-7.51676407774756,152.974999999398,
10.3459381770588));
#287889=CARTESIAN_POINT('Ctrl Pts',(-3.75838203887383,153.124999999398,
11.5671105274568));
#287890=CARTESIAN_POINT('Ctrl Pts',(-9.84000001696181E-14,153.274999999397,
12.7882828778549));
#287891=CARTESIAN_POINT('Ctrl Pts',(3.75838203887363,153.424999999396,11.5671105274568));
#287892=CARTESIAN_POINT('Ctrl Pts',(7.51676407774736,153.574999999396,10.3459381770588));
#287893=CARTESIAN_POINT('Ctrl Pts',(9.83957192047845,153.724999999395,7.14886745759505));
#287894=CARTESIAN_POINT('Ctrl Pts',(12.1623797632095,153.874999999395,3.95179673813132));
#287895=CARTESIAN_POINT('Ctrl Pts',(12.1623797632095,154.024999999394,-1.48946194470292E-15));
#287896=CARTESIAN_POINT('Ctrl Pts',(12.1623797632095,154.174999999393,-3.95179673813132));
#287897=CARTESIAN_POINT('Ctrl Pts',(9.83957192047845,154.324999999393,-7.14886745759505));
#287898=CARTESIAN_POINT('Ctrl Pts',(7.51676407774735,154.474999999392,-10.3459381770588));
#287899=CARTESIAN_POINT('Ctrl Pts',(3.75838203887363,154.624999999392,-11.5671105274568));
#287900=CARTESIAN_POINT('Ctrl Pts',(-1.0239608074404E-13,154.774999999391,
-12.7882828778549));
#287901=CARTESIAN_POINT('Ctrl Pts',(-3.75838203887383,154.92499999939,-11.5671105274568));
#287902=CARTESIAN_POINT('',(-9.80053286676861,76.2,-2.23182856044403));
#287903=CARTESIAN_POINT('Ctrl Pts',(10.0514428414941,74.8062499997113,-1.23094673026484E-15));
#287904=CARTESIAN_POINT('Ctrl Pts',(10.0514428414941,74.9562499997106,-3.26591175476071));
#287905=CARTESIAN_POINT('Ctrl Pts',(8.13178807675713,75.10624999971,-5.90808986649102));
#287906=CARTESIAN_POINT('Ctrl Pts',(6.21213331202016,75.2562499997095,-8.55026797822134));
#287907=CARTESIAN_POINT('Ctrl Pts',(3.10606665601005,75.4062499997088,-9.5594902125713));
#287908=CARTESIAN_POINT('Ctrl Pts',(-5.66378482980338E-14,75.5562499997083,
-10.5687124469213));
#287909=CARTESIAN_POINT('Ctrl Pts',(-3.10606665601016,75.7062499997077,
-9.5594902125713));
#287910=CARTESIAN_POINT('Ctrl Pts',(-6.21213331202027,75.8562499997071,
-8.55026797822134));
#287911=CARTESIAN_POINT('Ctrl Pts',(-8.13178807675725,76.0062499997065,
-5.90808986649102));
#287912=CARTESIAN_POINT('Ctrl Pts',(-9.34299114618875,76.1008922571328,
-4.2410118597063));
#287913=CARTESIAN_POINT('Ctrl Pts',(-9.80053286676861,76.2,-2.23182856044403));
#287914=CARTESIAN_POINT('Ctrl Pts',(-9.80053286676861,76.2,-2.23182856044404));
#287915=CARTESIAN_POINT('Ctrl Pts',(-9.6944232497338,76.2,-2.98049389998223));
#287916=CARTESIAN_POINT('Ctrl Pts',(-9.50451644375251,76.2,-3.71482315444662));
#287917=CARTESIAN_POINT('Ctrl Pts',(-8.9507720992266,76.2,-5.16268983688915));
#287918=CARTESIAN_POINT('Ctrl Pts',(-8.58384186538138,76.2,-5.86027015767421));
#287919=CARTESIAN_POINT('Ctrl Pts',(-7.36855104616312,76.2,-7.64541067699849));
#287920=CARTESIAN_POINT('Ctrl Pts',(-6.39031235163314,76.1999999999999,
-8.61475197019007));
#287921=CARTESIAN_POINT('Ctrl Pts',(-3.72933845937247,76.1999999999999,
-10.3909605175236));
#287922=CARTESIAN_POINT('Ctrl Pts',(-2.26196014736257,76.2,-10.8035407208194));
#287923=CARTESIAN_POINT('Ctrl Pts',(0.153337835077095,76.2,-11.2744264553899));
#287924=CARTESIAN_POINT('Ctrl Pts',(1.64295619773128,76.2,-11.2661126066267));
#287925=CARTESIAN_POINT('Ctrl Pts',(4.28244648061358,76.2,-10.7213720931628));
#287926=CARTESIAN_POINT('Ctrl Pts',(5.67769351012328,76.2,-10.229155280931));
#287927=CARTESIAN_POINT('Ctrl Pts',(7.64416788707506,76.2,-8.9539354014207));
#287928=CARTESIAN_POINT('Ctrl Pts',(8.19850424462796,76.2000000003225,-8.51856537485932));
#287929=CARTESIAN_POINT('Ctrl Pts',(9.24635223087657,76.2000000003225,-7.53021049871108));
#287930=CARTESIAN_POINT('Ctrl Pts',(9.73034607334846,76.2,-6.97611193267191));
#287931=CARTESIAN_POINT('Ctrl Pts',(10.1587275000649,76.2,-6.38750777529538));
#287932=CARTESIAN_POINT('Ctrl Pts',(-12.1623797632103,-3.28749999997638,
2.97892388940601E-15));
#287933=CARTESIAN_POINT('Ctrl Pts',(-12.1623797632103,-3.13749999997698,
3.95179673813154));
#287934=CARTESIAN_POINT('Ctrl Pts',(-9.83957192047908,-2.98749999997758,
7.14886745759543));
#287935=CARTESIAN_POINT('Ctrl Pts',(-7.51676407774787,-2.83749999997817,
10.3459381770593));
#287936=CARTESIAN_POINT('Ctrl Pts',(-3.75838203887394,-2.68749999997877,
11.5671105274575));
#287937=CARTESIAN_POINT('Ctrl Pts',(-8.66709987268145E-15,-2.53749999997937,
12.7882828778556));
#287938=CARTESIAN_POINT('Ctrl Pts',(3.75838203887392,-2.38749999997997,
11.5671105274575));
#287939=CARTESIAN_POINT('Ctrl Pts',(7.51676407774785,-2.23749999998057,
10.3459381770593));
#287940=CARTESIAN_POINT('Ctrl Pts',(9.83957192047906,-2.08749999998117,
7.14886745759543));
#287941=CARTESIAN_POINT('Ctrl Pts',(12.1623797632103,-1.93749999998176,
3.95179673813153));
#287942=CARTESIAN_POINT('Ctrl Pts',(12.1623797632103,-1.78749999998236,
-1.489461944703E-15));
#287943=CARTESIAN_POINT('Ctrl Pts',(12.1623797632103,-1.63749999998296,
-3.95179673813154));
#287944=CARTESIAN_POINT('Ctrl Pts',(9.83957192047906,-1.48749999998357,
-7.14886745759543));
#287945=CARTESIAN_POINT('Ctrl Pts',(7.51676407774784,-1.33749999998417,
-10.3459381770593));
#287946=CARTESIAN_POINT('Ctrl Pts',(3.75838203887392,-1.18749999998477,
-11.5671105274575));
#287947=CARTESIAN_POINT('Ctrl Pts',(-1.26631804471037E-14,-1.03749999998537,
-12.7882828778556));
#287948=CARTESIAN_POINT('Ctrl Pts',(-3.75838203887394,-0.887499999985973,
-11.5671105274575));
#287949=CARTESIAN_POINT('Ctrl Pts',(-7.51676407774787,-0.737499999986575,
-10.3459381770593));
#287950=CARTESIAN_POINT('Ctrl Pts',(-9.83957192047909,-0.587499999987176,
-7.14886745759543));
#287951=CARTESIAN_POINT('Ctrl Pts',(-12.1623797632103,-0.437499999987778,
-3.95179673813153));
#287952=CARTESIAN_POINT('Ctrl Pts',(-12.1623797632103,-0.287499999988378,
2.97892388940601E-15));
#287953=CARTESIAN_POINT('Ctrl Pts',(-12.1623797632103,-0.137499999988978,
3.95179673813154));
#287954=CARTESIAN_POINT('Ctrl Pts',(-9.83957192047909,0.0125000000104236,
7.14886745759543));
#287955=CARTESIAN_POINT('Ctrl Pts',(-7.51676407774787,0.162500000009825,
10.3459381770593));
#287956=CARTESIAN_POINT('Ctrl Pts',(-3.75838203887394,0.312500000009227,
11.5671105274575));
#287957=CARTESIAN_POINT('Ctrl Pts',(-1.03948091443433E-14,0.462500000008629,
12.7882828778556));
#287958=CARTESIAN_POINT('Ctrl Pts',(3.75838203887392,0.612500000008031,
11.5671105274575));
#287959=CARTESIAN_POINT('Ctrl Pts',(7.51676407774785,0.762500000007433,
10.3459381770593));
#287960=CARTESIAN_POINT('Ctrl Pts',(9.83957192047906,0.912500000006835,
7.14886745759543));
#287961=CARTESIAN_POINT('Ctrl Pts',(12.1623797632103,1.06250000000624,3.95179673813153));
#287962=CARTESIAN_POINT('Ctrl Pts',(12.1623797632103,1.21250000000564,-1.489461944703E-15));
#287963=CARTESIAN_POINT('Ctrl Pts',(12.1623797632103,1.36250000000504,-3.95179673813154));
#287964=CARTESIAN_POINT('Ctrl Pts',(9.83957192047906,1.51250000000444,-7.14886745759543));
#287965=CARTESIAN_POINT('Ctrl Pts',(7.51676407774784,1.66250000000383,-10.3459381770593));
#287966=CARTESIAN_POINT('Ctrl Pts',(3.75838203887391,1.81250000000323,-11.5671105274575));
#287967=CARTESIAN_POINT('Ctrl Pts',(-1.43908897187656E-14,1.96250000000263,
-12.7882828778556));
#287968=CARTESIAN_POINT('Ctrl Pts',(-3.75838203887394,2.11250000000203,
-11.5671105274575));
#287969=CARTESIAN_POINT('Ctrl Pts',(-7.51676407774787,2.26250000000143,
-10.3459381770593));
#287970=CARTESIAN_POINT('Ctrl Pts',(-9.83957192047909,2.41250000000082,
-7.14886745759543));
#287971=CARTESIAN_POINT('Ctrl Pts',(-12.1623797632103,2.56250000000022,
-3.95179673813153));
#287972=CARTESIAN_POINT('Ctrl Pts',(-12.1623797632103,2.71249999999962,
2.97892388940601E-15));
#287973=CARTESIAN_POINT('Ctrl Pts',(-12.1623797632103,2.86249999999902,
3.95179673813154));
#287974=CARTESIAN_POINT('Ctrl Pts',(-9.83957192047909,3.01249999999842,
7.14886745759543));
#287975=CARTESIAN_POINT('Ctrl Pts',(-7.51676407774787,3.16249999999782,
10.3459381770593));
#287976=CARTESIAN_POINT('Ctrl Pts',(-3.75838203887394,3.31249999999723,
11.5671105274575));
#287977=CARTESIAN_POINT('Ctrl Pts',(-1.21225184160051E-14,3.46249999999663,
12.7882828778556));
#287978=CARTESIAN_POINT('Ctrl Pts',(3.75838203887392,3.61249999999603,11.5671105274575));
#287979=CARTESIAN_POINT('Ctrl Pts',(7.51676407774784,3.76249999999543,10.3459381770593));
#287980=CARTESIAN_POINT('Ctrl Pts',(9.83957192047906,3.91249999999483,7.14886745759543));
#287981=CARTESIAN_POINT('Ctrl Pts',(12.1623797632103,4.06249999999424,3.95179673813153));
#287982=CARTESIAN_POINT('Ctrl Pts',(12.1623797632103,4.21249999999364,-1.489461944703E-15));
#287983=CARTESIAN_POINT('Ctrl Pts',(12.1623797632103,4.36249999999303,-3.95179673813154));
#287984=CARTESIAN_POINT('Ctrl Pts',(9.83957192047906,4.51249999999243,-7.14886745759543));
#287985=CARTESIAN_POINT('Ctrl Pts',(7.51676407774784,4.66249999999183,-10.3459381770593));
#287986=CARTESIAN_POINT('Ctrl Pts',(3.75838203887391,4.81249999999123,-11.5671105274575));
#287987=CARTESIAN_POINT('Ctrl Pts',(-1.61185989904274E-14,4.96249999999063,
-12.7882828778556));
#287988=CARTESIAN_POINT('Ctrl Pts',(-3.75838203887394,5.11249999999003,
-11.5671105274575));
#287989=CARTESIAN_POINT('Ctrl Pts',(-7.51676407774788,5.26249999998942,
-10.3459381770593));
#287990=CARTESIAN_POINT('Ctrl Pts',(-9.83957192047909,5.41249999998882,
-7.14886745759543));
#287991=CARTESIAN_POINT('Ctrl Pts',(-12.1623797632103,5.56249999998822,
-3.95179673813153));
#287992=CARTESIAN_POINT('Ctrl Pts',(-12.1623797632103,5.71249999998762,
2.97892388940601E-15));
#287993=CARTESIAN_POINT('Ctrl Pts',(-12.1623797632103,5.86249999998702,
3.95179673813154));
#287994=CARTESIAN_POINT('Ctrl Pts',(-9.83957192047909,6.01249999998642,
7.14886745759543));
#287995=CARTESIAN_POINT('Ctrl Pts',(-7.51676407774787,6.16249999998582,
10.3459381770593));
#287996=CARTESIAN_POINT('Ctrl Pts',(-3.75838203887394,6.31249999998523,
11.5671105274575));
#287997=CARTESIAN_POINT('Ctrl Pts',(-1.3850227687667E-14,6.46249999998463,
12.7882828778556));
#287998=CARTESIAN_POINT('Ctrl Pts',(3.75838203887392,6.61249999998403,11.5671105274575));
#287999=CARTESIAN_POINT('Ctrl Pts',(7.51676407774784,6.76249999998343,10.3459381770593));
#288000=CARTESIAN_POINT('Ctrl Pts',(9.83957192047906,6.91249999998283,7.14886745759543));
#288001=CARTESIAN_POINT('Ctrl Pts',(12.1623797632103,7.06249999998224,3.95179673813153));
#288002=CARTESIAN_POINT('Ctrl Pts',(12.1623797632103,7.21249999998164,-1.489461944703E-15));
#288003=CARTESIAN_POINT('Ctrl Pts',(12.1623797632103,7.36249999998104,-3.95179673813154));
#288004=CARTESIAN_POINT('Ctrl Pts',(9.83957192047906,7.51249999998044,-7.14886745759543));
#288005=CARTESIAN_POINT('Ctrl Pts',(7.51676407774784,7.66249999997983,-10.3459381770593));
#288006=CARTESIAN_POINT('Ctrl Pts',(3.75838203887391,7.81249999997923,-11.5671105274575));
#288007=CARTESIAN_POINT('Ctrl Pts',(-1.78463082620892E-14,7.96249999997863,
-12.7882828778556));
#288008=CARTESIAN_POINT('Ctrl Pts',(-3.75838203887395,8.11249999997803,
-11.5671105274575));
#288009=CARTESIAN_POINT('Ctrl Pts',(-7.51676407774788,8.26249999997743,
-10.3459381770593));
#288010=CARTESIAN_POINT('Ctrl Pts',(-9.83957192047909,8.41249999997682,
-7.14886745759543));
#288011=CARTESIAN_POINT('Ctrl Pts',(-12.1623797632103,8.56249999997622,
-3.95179673813153));
#288012=CARTESIAN_POINT('Ctrl Pts',(-12.1623797632103,8.71249999997562,
2.97892388940601E-15));
#288013=CARTESIAN_POINT('Ctrl Pts',(-12.1623797632103,8.86249999997502,
3.95179673813154));
#288014=CARTESIAN_POINT('Ctrl Pts',(-9.83957192047909,9.01249999997442,
7.14886745759543));
#288015=CARTESIAN_POINT('Ctrl Pts',(-7.51676407774787,9.16249999997382,
10.3459381770593));
#288016=CARTESIAN_POINT('Ctrl Pts',(-3.75838203887394,9.31249999997323,
11.5671105274575));
#288017=CARTESIAN_POINT('Ctrl Pts',(-1.55779369593288E-14,9.46249999997263,
12.7882828778556));
#288018=CARTESIAN_POINT('Ctrl Pts',(3.75838203887391,9.61249999997203,11.5671105274575));
#288019=CARTESIAN_POINT('Ctrl Pts',(7.51676407774784,9.76249999997144,10.3459381770593));
#288020=CARTESIAN_POINT('Ctrl Pts',(9.83957192047906,9.91249999997084,7.14886745759543));
#288021=CARTESIAN_POINT('Ctrl Pts',(12.1623797632103,10.0624999999702,3.95179673813153));
#288022=CARTESIAN_POINT('Ctrl Pts',(12.1623797632103,10.2124999999696,-1.489461944703E-15));
#288023=CARTESIAN_POINT('Ctrl Pts',(12.1623797632103,10.362499999969,-3.95179673813154));
#288024=CARTESIAN_POINT('Ctrl Pts',(9.83957192047905,10.5124999999684,-7.14886745759543));
#288025=CARTESIAN_POINT('Ctrl Pts',(7.51676407774784,10.6624999999678,-10.3459381770593));
#288026=CARTESIAN_POINT('Ctrl Pts',(3.75838203887391,10.8124999999672,-11.5671105274575));
#288027=CARTESIAN_POINT('Ctrl Pts',(-1.95740175337511E-14,10.9624999999666,
-12.7882828778556));
#288028=CARTESIAN_POINT('Ctrl Pts',(-3.75838203887395,11.112499999966,-11.5671105274575));
#288029=CARTESIAN_POINT('Ctrl Pts',(-7.51676407774788,11.2624999999654,
-10.3459381770593));
#288030=CARTESIAN_POINT('Ctrl Pts',(-9.83957192047909,11.4124999999648,
-7.14886745759543));
#288031=CARTESIAN_POINT('Ctrl Pts',(-12.1623797632103,11.5624999999642,
-3.95179673813153));
#288032=CARTESIAN_POINT('Ctrl Pts',(-12.1623797632103,11.7124999999636,
2.97892388940601E-15));
#288033=CARTESIAN_POINT('Ctrl Pts',(-12.1623797632103,11.862499999963,3.95179673813154));
#288034=CARTESIAN_POINT('Ctrl Pts',(-9.83957192047909,12.0124999999624,
7.14886745759543));
#288035=CARTESIAN_POINT('Ctrl Pts',(-7.51676407774788,12.1624999999618,
10.3459381770593));
#288036=CARTESIAN_POINT('Ctrl Pts',(-3.75838203887395,12.3124999999612,
11.5671105274575));
#288037=CARTESIAN_POINT('Ctrl Pts',(-1.73056462309906E-14,12.4624999999606,
12.7882828778556));
#288038=CARTESIAN_POINT('Ctrl Pts',(3.75838203887391,12.61249999996,11.5671105274575));
#288039=CARTESIAN_POINT('Ctrl Pts',(7.51676407774784,12.7624999999594,10.3459381770593));
#288040=CARTESIAN_POINT('Ctrl Pts',(9.83957192047906,12.9124999999588,7.14886745759543));
#288041=CARTESIAN_POINT('Ctrl Pts',(12.1623797632103,13.0624999999582,3.95179673813153));
#288042=CARTESIAN_POINT('Ctrl Pts',(12.1623797632103,13.2124999999576,-1.489461944703E-15));
#288043=CARTESIAN_POINT('Ctrl Pts',(12.1623797632103,13.362499999957,-3.95179673813154));
#288044=CARTESIAN_POINT('Ctrl Pts',(9.83957192047905,13.5124999999564,-7.14886745759543));
#288045=CARTESIAN_POINT('Ctrl Pts',(7.51676407774784,13.6624999999558,-10.3459381770593));
#288046=CARTESIAN_POINT('Ctrl Pts',(3.75838203887391,13.8124999999552,-11.5671105274575));
#288047=CARTESIAN_POINT('Ctrl Pts',(-2.13017268054129E-14,13.9624999999546,
-12.7882828778556));
#288048=CARTESIAN_POINT('Ctrl Pts',(-3.75838203887395,14.112499999954,-11.5671105274575));
#288049=CARTESIAN_POINT('Ctrl Pts',(-7.51676407774788,14.2624999999534,
-10.3459381770593));
#288050=CARTESIAN_POINT('Ctrl Pts',(-9.8395719204791,14.4124999999528,-7.14886745759543));
#288051=CARTESIAN_POINT('Ctrl Pts',(-12.1623797632103,14.5624999999522,
-3.95179673813153));
#288052=CARTESIAN_POINT('Ctrl Pts',(-12.1623797632103,14.7124999999516,
2.97892388940601E-15));
#288053=CARTESIAN_POINT('Ctrl Pts',(-12.1623797632103,14.862499999951,3.95179673813154));
#288054=CARTESIAN_POINT('Ctrl Pts',(-9.83957192047909,15.0124999999504,
7.14886745759543));
#288055=CARTESIAN_POINT('Ctrl Pts',(-7.51676407774788,15.1624999999498,
10.3459381770593));
#288056=CARTESIAN_POINT('Ctrl Pts',(-3.75838203887395,15.3124999999492,
11.5671105274575));
#288057=CARTESIAN_POINT('Ctrl Pts',(-1.90333555026525E-14,15.4624999999486,
12.7882828778556));
#288058=CARTESIAN_POINT('Ctrl Pts',(3.75838203887391,15.612499999948,11.5671105274575));
#288059=CARTESIAN_POINT('Ctrl Pts',(7.51676407774784,15.7624999999474,10.3459381770593));
#288060=CARTESIAN_POINT('Ctrl Pts',(9.83957192047905,15.9124999999468,7.14886745759543));
#288061=CARTESIAN_POINT('Ctrl Pts',(12.1623797632103,16.0624999999462,3.95179673813153));
#288062=CARTESIAN_POINT('Ctrl Pts',(12.1623797632103,16.2124999999456,-1.489461944703E-15));
#288063=CARTESIAN_POINT('Ctrl Pts',(12.1623797632103,16.362499999945,-3.95179673813154));
#288064=CARTESIAN_POINT('Ctrl Pts',(9.83957192047905,16.5124999999444,-7.14886745759543));
#288065=CARTESIAN_POINT('Ctrl Pts',(7.51676407774784,16.6624999999438,-10.3459381770593));
#288066=CARTESIAN_POINT('Ctrl Pts',(3.75838203887391,16.8124999999432,-11.5671105274575));
#288067=CARTESIAN_POINT('Ctrl Pts',(-2.30294360770748E-14,16.9624999999426,
-12.7882828778556));
#288068=CARTESIAN_POINT('Ctrl Pts',(-3.75838203887395,17.112499999942,-11.5671105274575));
#288069=CARTESIAN_POINT('Ctrl Pts',(-7.51676407774788,17.2624999999414,
-10.3459381770593));
#288070=CARTESIAN_POINT('Ctrl Pts',(-9.8395719204791,17.4124999999408,-7.14886745759543));
#288071=CARTESIAN_POINT('Ctrl Pts',(-12.1623797632103,17.5624999999402,
-3.95179673813153));
#288072=CARTESIAN_POINT('Ctrl Pts',(-12.1623797632103,17.7124999999396,
2.97892388940601E-15));
#288073=CARTESIAN_POINT('Ctrl Pts',(-12.1623797632103,17.862499999939,3.95179673813154));
#288074=CARTESIAN_POINT('Ctrl Pts',(-9.8395719204791,18.0124999999384,7.14886745759543));
#288075=CARTESIAN_POINT('Ctrl Pts',(-7.51676407774788,18.1624999999378,
10.3459381770593));
#288076=CARTESIAN_POINT('Ctrl Pts',(-3.75838203887395,18.3124999999372,
11.5671105274575));
#288077=CARTESIAN_POINT('Ctrl Pts',(-2.07610647743143E-14,18.4624999999366,
12.7882828778556));
#288078=CARTESIAN_POINT('Ctrl Pts',(3.75838203887391,18.612499999936,11.5671105274575));
#288079=CARTESIAN_POINT('Ctrl Pts',(7.51676407774784,18.7624999999354,10.3459381770593));
#288080=CARTESIAN_POINT('Ctrl Pts',(9.83957192047905,18.9124999999348,7.14886745759543));
#288081=CARTESIAN_POINT('Ctrl Pts',(12.1623797632103,19.0624999999342,3.95179673813153));
#288082=CARTESIAN_POINT('Ctrl Pts',(12.1623797632103,19.2124999999336,-1.489461944703E-15));
#288083=CARTESIAN_POINT('Ctrl Pts',(12.1623797632103,19.362499999933,-3.95179673813154));
#288084=CARTESIAN_POINT('Ctrl Pts',(9.83957192047905,19.5124999999324,-7.14886745759543));
#288085=CARTESIAN_POINT('Ctrl Pts',(7.51676407774784,19.6624999999318,-10.3459381770593));
#288086=CARTESIAN_POINT('Ctrl Pts',(3.7583820388739,19.8124999999312,-11.5671105274575));
#288087=CARTESIAN_POINT('Ctrl Pts',(-2.47571453487366E-14,19.9624999999306,
-12.7882828778556));
#288088=CARTESIAN_POINT('Ctrl Pts',(-3.75838203887395,20.11249999993,-11.5671105274575));
#288089=CARTESIAN_POINT('Ctrl Pts',(-7.51676407774788,20.2624999999294,
-10.3459381770593));
#288090=CARTESIAN_POINT('Ctrl Pts',(-9.8395719204791,20.4124999999288,-7.14886745759543));
#288091=CARTESIAN_POINT('Ctrl Pts',(-12.1623797632103,20.5624999999282,
-3.95179673813153));
#288092=CARTESIAN_POINT('Ctrl Pts',(-12.1623797632103,20.7124999999276,
2.97892388940601E-15));
#288093=CARTESIAN_POINT('Ctrl Pts',(-12.1623797632103,20.862499999927,3.95179673813154));
#288094=CARTESIAN_POINT('Ctrl Pts',(-9.8395719204791,21.0124999999264,7.14886745759543));
#288095=CARTESIAN_POINT('Ctrl Pts',(-7.51676407774788,21.1624999999258,
10.3459381770593));
#288096=CARTESIAN_POINT('Ctrl Pts',(-3.75838203887395,21.3124999999252,
11.5671105274575));
#288097=CARTESIAN_POINT('Ctrl Pts',(-2.24887740459762E-14,21.4624999999246,
12.7882828778556));
#288098=CARTESIAN_POINT('Ctrl Pts',(3.75838203887391,21.612499999924,11.5671105274575));
#288099=CARTESIAN_POINT('Ctrl Pts',(7.51676407774784,21.7624999999234,10.3459381770593));
#288100=CARTESIAN_POINT('Ctrl Pts',(9.83957192047905,21.9124999999228,7.14886745759543));
#288101=CARTESIAN_POINT('Ctrl Pts',(12.1623797632103,22.0624999999222,3.95179673813153));
#288102=CARTESIAN_POINT('Ctrl Pts',(12.1623797632103,22.2124999999216,-1.489461944703E-15));
#288103=CARTESIAN_POINT('Ctrl Pts',(12.1623797632103,22.362499999921,-3.95179673813154));
#288104=CARTESIAN_POINT('Ctrl Pts',(9.83957192047905,22.5124999999204,-7.14886745759543));
#288105=CARTESIAN_POINT('Ctrl Pts',(7.51676407774783,22.6624999999198,-10.3459381770593));
#288106=CARTESIAN_POINT('Ctrl Pts',(3.7583820388739,22.8124999999192,-11.5671105274575));
#288107=CARTESIAN_POINT('Ctrl Pts',(-2.64848546203984E-14,22.9624999999186,
-12.7882828778556));
#288108=CARTESIAN_POINT('Ctrl Pts',(-3.75838203887396,23.112499999918,-11.5671105274575));
#288109=CARTESIAN_POINT('Ctrl Pts',(-7.51676407774788,23.2624999999174,
-10.3459381770593));
#288110=CARTESIAN_POINT('Ctrl Pts',(-9.8395719204791,23.4124999999168,-7.14886745759543));
#288111=CARTESIAN_POINT('Ctrl Pts',(-12.1623797632103,23.5624999999162,
-3.95179673813153));
#288112=CARTESIAN_POINT('Ctrl Pts',(-12.1623797632103,23.7124999999156,
2.97892388940601E-15));
#288113=CARTESIAN_POINT('Ctrl Pts',(-12.1623797632103,23.862499999915,3.95179673813154));
#288114=CARTESIAN_POINT('Ctrl Pts',(-9.8395719204791,24.0124999999144,7.14886745759543));
#288115=CARTESIAN_POINT('Ctrl Pts',(-7.51676407774788,24.1624999999138,
10.3459381770593));
#288116=CARTESIAN_POINT('Ctrl Pts',(-3.75838203887395,24.3124999999132,
11.5671105274575));
#288117=CARTESIAN_POINT('Ctrl Pts',(-2.4216483317638E-14,24.4624999999126,
12.7882828778556));
#288118=CARTESIAN_POINT('Ctrl Pts',(3.7583820388739,24.612499999912,11.5671105274575));
#288119=CARTESIAN_POINT('Ctrl Pts',(7.51676407774783,24.7624999999114,10.3459381770593));
#288120=CARTESIAN_POINT('Ctrl Pts',(9.83957192047905,24.9124999999108,7.14886745759543));
#288121=CARTESIAN_POINT('Ctrl Pts',(12.1623797632103,25.0624999999102,3.95179673813153));
#288122=CARTESIAN_POINT('Ctrl Pts',(12.1623797632103,25.2124999999096,-1.489461944703E-15));
#288123=CARTESIAN_POINT('Ctrl Pts',(12.1623797632103,25.362499999909,-3.95179673813154));
#288124=CARTESIAN_POINT('Ctrl Pts',(9.83957192047905,25.5124999999084,-7.14886745759543));
#288125=CARTESIAN_POINT('Ctrl Pts',(7.51676407774783,25.6624999999078,-10.3459381770593));
#288126=CARTESIAN_POINT('Ctrl Pts',(3.7583820388739,25.8124999999072,-11.5671105274575));
#288127=CARTESIAN_POINT('Ctrl Pts',(-2.82125638920603E-14,25.9624999999066,
-12.7882828778556));
#288128=CARTESIAN_POINT('Ctrl Pts',(-3.75838203887396,26.112499999906,-11.5671105274575));
#288129=CARTESIAN_POINT('Ctrl Pts',(-7.51676407774788,26.2624999999054,
-10.3459381770593));
#288130=CARTESIAN_POINT('Ctrl Pts',(-9.8395719204791,26.4124999999048,-7.14886745759543));
#288131=CARTESIAN_POINT('Ctrl Pts',(-12.1623797632103,26.5624999999042,
-3.95179673813153));
#288132=CARTESIAN_POINT('Ctrl Pts',(-12.1623797632103,26.7124999999036,
2.97892388940601E-15));
#288133=CARTESIAN_POINT('Ctrl Pts',(-12.1623797632103,26.862499999903,3.95179673813154));
#288134=CARTESIAN_POINT('Ctrl Pts',(-9.8395719204791,27.0124999999024,7.14886745759543));
#288135=CARTESIAN_POINT('Ctrl Pts',(-7.51676407774788,27.1624999999018,
10.3459381770593));
#288136=CARTESIAN_POINT('Ctrl Pts',(-3.75838203887396,27.3124999999012,
11.5671105274575));
#288137=CARTESIAN_POINT('Ctrl Pts',(-2.59441925892998E-14,27.4624999999006,
12.7882828778556));
#288138=CARTESIAN_POINT('Ctrl Pts',(3.7583820388739,27.6124999999,11.5671105274575));
#288139=CARTESIAN_POINT('Ctrl Pts',(7.51676407774783,27.7624999998994,10.3459381770593));
#288140=CARTESIAN_POINT('Ctrl Pts',(9.83957192047905,27.9124999998988,7.14886745759543));
#288141=CARTESIAN_POINT('Ctrl Pts',(12.1623797632103,28.0624999998982,3.95179673813153));
#288142=CARTESIAN_POINT('Ctrl Pts',(12.1623797632103,28.2124999998976,-1.489461944703E-15));
#288143=CARTESIAN_POINT('Ctrl Pts',(12.1623797632103,28.362499999897,-3.95179673813154));
#288144=CARTESIAN_POINT('Ctrl Pts',(9.83957192047905,28.5124999998964,-7.14886745759543));
#288145=CARTESIAN_POINT('Ctrl Pts',(7.51676407774783,28.6624999998958,-10.3459381770593));
#288146=CARTESIAN_POINT('Ctrl Pts',(3.7583820388739,28.8124999998952,-11.5671105274575));
#288147=CARTESIAN_POINT('Ctrl Pts',(-2.99402731637221E-14,28.9624999998946,
-12.7882828778556));
#288148=CARTESIAN_POINT('Ctrl Pts',(-3.75838203887396,29.112499999894,-11.5671105274575));
#288149=CARTESIAN_POINT('Ctrl Pts',(-7.51676407774789,29.2624999998934,
-10.3459381770593));
#288150=CARTESIAN_POINT('Ctrl Pts',(-9.8395719204791,29.4124999998928,-7.14886745759543));
#288151=CARTESIAN_POINT('Ctrl Pts',(-12.1623797632103,29.5624999998922,
-3.95179673813153));
#288152=CARTESIAN_POINT('Ctrl Pts',(-12.1623797632103,29.7124999998916,
2.97892388940601E-15));
#288153=CARTESIAN_POINT('Ctrl Pts',(-12.1623797632103,29.862499999891,3.95179673813154));
#288154=CARTESIAN_POINT('Ctrl Pts',(-9.8395719204791,30.0124999998904,7.14886745759543));
#288155=CARTESIAN_POINT('Ctrl Pts',(-7.51676407774788,30.1624999998898,
10.3459381770593));
#288156=CARTESIAN_POINT('Ctrl Pts',(-3.75838203887396,30.3124999998892,
11.5671105274575));
#288157=CARTESIAN_POINT('Ctrl Pts',(-2.76719018609617E-14,30.4624999998886,
12.7882828778556));
#288158=CARTESIAN_POINT('Ctrl Pts',(3.7583820388739,30.612499999888,11.5671105274575));
#288159=CARTESIAN_POINT('Ctrl Pts',(7.51676407774783,30.7624999998874,10.3459381770593));
#288160=CARTESIAN_POINT('Ctrl Pts',(9.83957192047905,30.9124999998868,7.14886745759543));
#288161=CARTESIAN_POINT('Ctrl Pts',(12.1623797632103,31.0624999998862,3.95179673813153));
#288162=CARTESIAN_POINT('Ctrl Pts',(12.1623797632103,31.2124999998856,-1.489461944703E-15));
#288163=CARTESIAN_POINT('Ctrl Pts',(12.1623797632103,31.362499999885,-3.95179673813154));
#288164=CARTESIAN_POINT('Ctrl Pts',(9.83957192047904,31.5124999998844,-7.14886745759543));
#288165=CARTESIAN_POINT('Ctrl Pts',(7.51676407774783,31.6624999998838,-10.3459381770593));
#288166=CARTESIAN_POINT('Ctrl Pts',(3.7583820388739,31.8124999998832,-11.5671105274575));
#288167=CARTESIAN_POINT('Ctrl Pts',(-3.16679824353839E-14,31.9624999998826,
-12.7882828778556));
#288168=CARTESIAN_POINT('Ctrl Pts',(-3.75838203887396,32.112499999882,-11.5671105274575));
#288169=CARTESIAN_POINT('Ctrl Pts',(-7.51676407774789,32.2624999998814,
-10.3459381770593));
#288170=CARTESIAN_POINT('Ctrl Pts',(-9.83957192047911,32.4124999998808,
-7.14886745759543));
#288171=CARTESIAN_POINT('Ctrl Pts',(-12.1623797632103,32.5624999998802,
-3.95179673813153));
#288172=CARTESIAN_POINT('Ctrl Pts',(-12.1623797632103,32.7124999998796,
2.97892388940601E-15));
#288173=CARTESIAN_POINT('Ctrl Pts',(-12.1623797632103,32.862499999879,3.95179673813154));
#288174=CARTESIAN_POINT('Ctrl Pts',(-9.8395719204791,33.0124999998784,7.14886745759543));
#288175=CARTESIAN_POINT('Ctrl Pts',(-7.51676407774789,33.1624999998778,
10.3459381770593));
#288176=CARTESIAN_POINT('Ctrl Pts',(-3.75838203887396,33.3124999998772,
11.5671105274575));
#288177=CARTESIAN_POINT('Ctrl Pts',(-2.93996111326235E-14,33.4624999998766,
12.7882828778556));
#288178=CARTESIAN_POINT('Ctrl Pts',(3.7583820388739,33.612499999876,11.5671105274575));
#288179=CARTESIAN_POINT('Ctrl Pts',(7.51676407774783,33.7624999998754,10.3459381770593));
#288180=CARTESIAN_POINT('Ctrl Pts',(9.83957192047905,33.9124999998748,7.14886745759543));
#288181=CARTESIAN_POINT('Ctrl Pts',(12.1623797632103,34.0624999998742,3.95179673813153));
#288182=CARTESIAN_POINT('Ctrl Pts',(12.1623797632103,34.2124999998736,-1.489461944703E-15));
#288183=CARTESIAN_POINT('Ctrl Pts',(12.1623797632103,34.362499999873,-3.95179673813154));
#288184=CARTESIAN_POINT('Ctrl Pts',(9.83957192047904,34.5124999998724,-7.14886745759543));
#288185=CARTESIAN_POINT('Ctrl Pts',(7.51676407774783,34.6624999998718,-10.3459381770593));
#288186=CARTESIAN_POINT('Ctrl Pts',(3.7583820388739,34.8124999998712,-11.5671105274575));
#288187=CARTESIAN_POINT('Ctrl Pts',(-3.33956917070458E-14,34.9624999998706,
-12.7882828778556));
#288188=CARTESIAN_POINT('Ctrl Pts',(-3.75838203887396,35.11249999987,-11.5671105274575));
#288189=CARTESIAN_POINT('Ctrl Pts',(-7.51676407774789,35.2624999998694,
-10.3459381770593));
#288190=CARTESIAN_POINT('Ctrl Pts',(-9.83957192047911,35.4124999998688,
-7.14886745759543));
#288191=CARTESIAN_POINT('Ctrl Pts',(-12.1623797632103,35.5624999998682,
-3.95179673813153));
#288192=CARTESIAN_POINT('Ctrl Pts',(-12.1623797632103,35.7124999998676,
2.97892388940601E-15));
#288193=CARTESIAN_POINT('Ctrl Pts',(-12.1623797632103,35.862499999867,3.95179673813154));
#288194=CARTESIAN_POINT('Ctrl Pts',(-9.83957192047911,36.0124999998664,
7.14886745759543));
#288195=CARTESIAN_POINT('Ctrl Pts',(-7.51676407774789,36.1624999998658,
10.3459381770593));
#288196=CARTESIAN_POINT('Ctrl Pts',(-3.75838203887396,36.3124999998652,
11.5671105274575));
#288197=CARTESIAN_POINT('Ctrl Pts',(-3.11273204042854E-14,36.4624999998646,
12.7882828778556));
#288198=CARTESIAN_POINT('Ctrl Pts',(3.7583820388739,36.612499999864,11.5671105274575));
#288199=CARTESIAN_POINT('Ctrl Pts',(7.51676407774783,36.7624999998634,10.3459381770593));
#288200=CARTESIAN_POINT('Ctrl Pts',(9.83957192047904,36.9124999998628,7.14886745759543));
#288201=CARTESIAN_POINT('Ctrl Pts',(12.1623797632103,37.0624999998622,3.95179673813153));
#288202=CARTESIAN_POINT('Ctrl Pts',(12.1623797632103,37.2124999998616,-1.489461944703E-15));
#288203=CARTESIAN_POINT('Ctrl Pts',(12.1623797632103,37.362499999861,-3.95179673813154));
#288204=CARTESIAN_POINT('Ctrl Pts',(9.83957192047904,37.5124999998604,-7.14886745759543));
#288205=CARTESIAN_POINT('Ctrl Pts',(7.51676407774782,37.6624999998598,-10.3459381770593));
#288206=CARTESIAN_POINT('Ctrl Pts',(3.75838203887389,37.8124999998592,-11.5671105274575));
#288207=CARTESIAN_POINT('Ctrl Pts',(-3.51234009787076E-14,37.9624999998586,
-12.7882828778556));
#288208=CARTESIAN_POINT('Ctrl Pts',(-3.75838203887396,38.112499999858,-11.5671105274575));
#288209=CARTESIAN_POINT('Ctrl Pts',(-7.51676407774789,38.2624999998574,
-10.3459381770593));
#288210=CARTESIAN_POINT('Ctrl Pts',(-9.83957192047911,38.4124999998568,
-7.14886745759543));
#288211=CARTESIAN_POINT('Ctrl Pts',(-12.1623797632103,38.5624999998562,
-3.95179673813153));
#288212=CARTESIAN_POINT('Ctrl Pts',(-12.1623797632103,38.7124999998556,
2.97892388940601E-15));
#288213=CARTESIAN_POINT('Ctrl Pts',(-12.1623797632103,38.862499999855,3.95179673813154));
#288214=CARTESIAN_POINT('Ctrl Pts',(-9.83957192047911,39.0124999998544,
7.14886745759543));
#288215=CARTESIAN_POINT('Ctrl Pts',(-7.51676407774789,39.1624999998538,
10.3459381770593));
#288216=CARTESIAN_POINT('Ctrl Pts',(-3.75838203887396,39.3124999998532,
11.5671105274575));
#288217=CARTESIAN_POINT('Ctrl Pts',(-3.28550296759472E-14,39.4624999998526,
12.7882828778556));
#288218=CARTESIAN_POINT('Ctrl Pts',(3.7583820388739,39.612499999852,11.5671105274575));
#288219=CARTESIAN_POINT('Ctrl Pts',(7.51676407774782,39.7624999998514,10.3459381770593));
#288220=CARTESIAN_POINT('Ctrl Pts',(9.83957192047904,39.9124999998508,7.14886745759543));
#288221=CARTESIAN_POINT('Ctrl Pts',(12.1623797632103,40.0624999998502,3.95179673813153));
#288222=CARTESIAN_POINT('Ctrl Pts',(12.1623797632103,40.2124999998496,-1.489461944703E-15));
#288223=CARTESIAN_POINT('Ctrl Pts',(12.1623797632103,40.362499999849,-3.95179673813154));
#288224=CARTESIAN_POINT('Ctrl Pts',(9.83957192047904,40.5124999998484,-7.14886745759543));
#288225=CARTESIAN_POINT('Ctrl Pts',(7.51676407774782,40.6624999998478,-10.3459381770593));
#288226=CARTESIAN_POINT('Ctrl Pts',(3.75838203887389,40.8124999998472,-11.5671105274575));
#288227=CARTESIAN_POINT('Ctrl Pts',(-3.68511102503695E-14,40.9624999998466,
-12.7882828778556));
#288228=CARTESIAN_POINT('Ctrl Pts',(-3.75838203887397,41.112499999846,-11.5671105274575));
#288229=CARTESIAN_POINT('Ctrl Pts',(-7.51676407774789,41.2624999998454,
-10.3459381770593));
#288230=CARTESIAN_POINT('Ctrl Pts',(-9.83957192047911,41.4124999998448,
-7.14886745759543));
#288231=CARTESIAN_POINT('Ctrl Pts',(-12.1623797632103,41.5624999998442,
-3.95179673813153));
#288232=CARTESIAN_POINT('Ctrl Pts',(-12.1623797632103,41.7124999998436,
2.97892388940601E-15));
#288233=CARTESIAN_POINT('Ctrl Pts',(-12.1623797632103,41.862499999843,3.95179673813154));
#288234=CARTESIAN_POINT('Ctrl Pts',(-9.83957192047911,42.0124999998424,
7.14886745759543));
#288235=CARTESIAN_POINT('Ctrl Pts',(-7.51676407774789,42.1624999998418,
10.3459381770593));
#288236=CARTESIAN_POINT('Ctrl Pts',(-3.75838203887396,42.3124999998412,
11.5671105274575));
#288237=CARTESIAN_POINT('Ctrl Pts',(-3.4582738947609E-14,42.4624999998406,
12.7882828778556));
#288238=CARTESIAN_POINT('Ctrl Pts',(3.75838203887389,42.61249999984,11.5671105274575));
#288239=CARTESIAN_POINT('Ctrl Pts',(7.51676407774782,42.7624999998394,10.3459381770593));
#288240=CARTESIAN_POINT('Ctrl Pts',(9.83957192047904,42.9124999998388,7.14886745759543));
#288241=CARTESIAN_POINT('Ctrl Pts',(12.1623797632103,43.0624999998382,3.95179673813153));
#288242=CARTESIAN_POINT('Ctrl Pts',(12.1623797632103,43.2124999998376,-1.489461944703E-15));
#288243=CARTESIAN_POINT('Ctrl Pts',(12.1623797632103,43.362499999837,-3.95179673813154));
#288244=CARTESIAN_POINT('Ctrl Pts',(9.83957192047903,43.5124999998364,-7.14886745759543));
#288245=CARTESIAN_POINT('Ctrl Pts',(7.51676407774782,43.6624999998358,-10.3459381770593));
#288246=CARTESIAN_POINT('Ctrl Pts',(3.75838203887389,43.8124999998352,-11.5671105274575));
#288247=CARTESIAN_POINT('Ctrl Pts',(-3.85788195220313E-14,43.9624999998346,
-12.7882828778556));
#288248=CARTESIAN_POINT('Ctrl Pts',(-3.75838203887397,44.112499999834,-11.5671105274575));
#288249=CARTESIAN_POINT('Ctrl Pts',(-7.5167640777479,44.2624999998334,-10.3459381770593));
#288250=CARTESIAN_POINT('Ctrl Pts',(-9.83957192047911,44.4124999998328,
-7.14886745759543));
#288251=CARTESIAN_POINT('Ctrl Pts',(-12.1623797632103,44.5624999998322,
-3.95179673813153));
#288252=CARTESIAN_POINT('Ctrl Pts',(-12.1623797632103,44.7124999998316,
2.97892388940601E-15));
#288253=CARTESIAN_POINT('Ctrl Pts',(-12.1623797632103,44.862499999831,3.95179673813154));
#288254=CARTESIAN_POINT('Ctrl Pts',(-9.83957192047911,45.0124999998304,
7.14886745759543));
#288255=CARTESIAN_POINT('Ctrl Pts',(-7.51676407774789,45.1624999998298,
10.3459381770593));
#288256=CARTESIAN_POINT('Ctrl Pts',(-3.75838203887397,45.3124999998292,
11.5671105274575));
#288257=CARTESIAN_POINT('Ctrl Pts',(-3.63104482192709E-14,45.4624999998286,
12.7882828778556));
#288258=CARTESIAN_POINT('Ctrl Pts',(3.75838203887389,45.612499999828,11.5671105274575));
#288259=CARTESIAN_POINT('Ctrl Pts',(7.51676407774782,45.7624999998274,10.3459381770593));
#288260=CARTESIAN_POINT('Ctrl Pts',(9.83957192047904,45.9124999998268,7.14886745759543));
#288261=CARTESIAN_POINT('Ctrl Pts',(12.1623797632103,46.0624999998262,3.95179673813153));
#288262=CARTESIAN_POINT('Ctrl Pts',(12.1623797632103,46.2124999998256,-1.489461944703E-15));
#288263=CARTESIAN_POINT('Ctrl Pts',(12.1623797632103,46.362499999825,-3.95179673813154));
#288264=CARTESIAN_POINT('Ctrl Pts',(9.83957192047903,46.5124999998244,-7.14886745759543));
#288265=CARTESIAN_POINT('Ctrl Pts',(7.51676407774782,46.6624999998238,-10.3459381770593));
#288266=CARTESIAN_POINT('Ctrl Pts',(3.75838203887389,46.8124999998232,-11.5671105274575));
#288267=CARTESIAN_POINT('Ctrl Pts',(-4.03065287936931E-14,46.9624999998226,
-12.7882828778556));
#288268=CARTESIAN_POINT('Ctrl Pts',(-3.75838203887397,47.112499999822,-11.5671105274575));
#288269=CARTESIAN_POINT('Ctrl Pts',(-7.5167640777479,47.2624999998214,-10.3459381770593));
#288270=CARTESIAN_POINT('Ctrl Pts',(-9.83957192047912,47.4124999998208,
-7.14886745759543));
#288271=CARTESIAN_POINT('Ctrl Pts',(-12.1623797632103,47.5624999998202,
-3.95179673813153));
#288272=CARTESIAN_POINT('Ctrl Pts',(-12.1623797632103,47.7124999998196,
2.97892388940601E-15));
#288273=CARTESIAN_POINT('Ctrl Pts',(-12.1623797632103,47.862499999819,3.95179673813154));
#288274=CARTESIAN_POINT('Ctrl Pts',(-9.83957192047911,48.0124999998184,
7.14886745759543));
#288275=CARTESIAN_POINT('Ctrl Pts',(-7.51676407774789,48.1624999998178,
10.3459381770593));
#288276=CARTESIAN_POINT('Ctrl Pts',(-3.75838203887397,48.3124999998172,
11.5671105274575));
#288277=CARTESIAN_POINT('Ctrl Pts',(-3.80381574909327E-14,48.4624999998166,
12.7882828778556));
#288278=CARTESIAN_POINT('Ctrl Pts',(3.75838203887389,48.612499999816,11.5671105274575));
#288279=CARTESIAN_POINT('Ctrl Pts',(7.51676407774782,48.7624999998154,10.3459381770593));
#288280=CARTESIAN_POINT('Ctrl Pts',(9.83957192047903,48.9124999998148,7.14886745759543));
#288281=CARTESIAN_POINT('Ctrl Pts',(12.1623797632103,49.0624999998142,3.95179673813153));
#288282=CARTESIAN_POINT('Ctrl Pts',(12.1623797632103,49.2124999998136,-1.489461944703E-15));
#288283=CARTESIAN_POINT('Ctrl Pts',(12.1623797632103,49.362499999813,-3.95179673813154));
#288284=CARTESIAN_POINT('Ctrl Pts',(9.83957192047903,49.5124999998124,-7.14886745759543));
#288285=CARTESIAN_POINT('Ctrl Pts',(7.51676407774782,49.6624999998118,-10.3459381770593));
#288286=CARTESIAN_POINT('Ctrl Pts',(3.75838203887389,49.8124999998112,-11.5671105274575));
#288287=CARTESIAN_POINT('Ctrl Pts',(-4.2034238065355E-14,49.9624999998106,
-12.7882828778556));
#288288=CARTESIAN_POINT('Ctrl Pts',(-3.75838203887397,50.11249999981,-11.5671105274575));
#288289=CARTESIAN_POINT('Ctrl Pts',(-7.5167640777479,50.2624999998094,-10.3459381770593));
#288290=CARTESIAN_POINT('Ctrl Pts',(-9.83957192047912,50.4124999998088,
-7.14886745759543));
#288291=CARTESIAN_POINT('Ctrl Pts',(-12.1623797632103,50.5624999998082,
-3.95179673813153));
#288292=CARTESIAN_POINT('Ctrl Pts',(-12.1623797632103,50.7124999998076,
2.97892388940601E-15));
#288293=CARTESIAN_POINT('Ctrl Pts',(-12.1623797632103,50.862499999807,3.95179673813154));
#288294=CARTESIAN_POINT('Ctrl Pts',(-9.83957192047912,51.0124999998064,
7.14886745759543));
#288295=CARTESIAN_POINT('Ctrl Pts',(-7.5167640777479,51.1624999998058,10.3459381770593));
#288296=CARTESIAN_POINT('Ctrl Pts',(-3.75838203887397,51.3124999998052,
11.5671105274575));
#288297=CARTESIAN_POINT('Ctrl Pts',(-3.97658667625946E-14,51.4624999998046,
12.7882828778556));
#288298=CARTESIAN_POINT('Ctrl Pts',(3.75838203887389,51.612499999804,11.5671105274575));
#288299=CARTESIAN_POINT('Ctrl Pts',(7.51676407774782,51.7624999998034,10.3459381770593));
#288300=CARTESIAN_POINT('Ctrl Pts',(9.83957192047903,51.9124999998028,7.14886745759543));
#288301=CARTESIAN_POINT('Ctrl Pts',(12.1623797632103,52.0624999998022,3.95179673813153));
#288302=CARTESIAN_POINT('Ctrl Pts',(12.1623797632103,52.2124999998016,-1.489461944703E-15));
#288303=CARTESIAN_POINT('Ctrl Pts',(12.1623797632103,52.362499999801,-3.95179673813154));
#288304=CARTESIAN_POINT('Ctrl Pts',(9.83957192047903,52.5124999998004,-7.14886745759543));
#288305=CARTESIAN_POINT('Ctrl Pts',(7.51676407774781,52.6624999997998,-10.3459381770593));
#288306=CARTESIAN_POINT('Ctrl Pts',(3.75838203887388,52.8124999997992,-11.5671105274575));
#288307=CARTESIAN_POINT('Ctrl Pts',(-4.37619473370168E-14,52.9624999997986,
-12.7882828778556));
#288308=CARTESIAN_POINT('Ctrl Pts',(-3.75838203887397,53.112499999798,-11.5671105274575));
#288309=CARTESIAN_POINT('Ctrl Pts',(-7.5167640777479,53.2624999997974,-10.3459381770593));
#288310=CARTESIAN_POINT('Ctrl Pts',(-9.83957192047912,53.4124999997968,
-7.14886745759543));
#288311=CARTESIAN_POINT('Ctrl Pts',(-12.1623797632103,53.5624999997962,
-3.95179673813153));
#288312=CARTESIAN_POINT('Ctrl Pts',(-12.1623797632103,53.7124999997956,
2.97892388940601E-15));
#288313=CARTESIAN_POINT('Ctrl Pts',(-12.1623797632103,53.862499999795,3.95179673813154));
#288314=CARTESIAN_POINT('Ctrl Pts',(-9.83957192047912,54.0124999997944,
7.14886745759543));
#288315=CARTESIAN_POINT('Ctrl Pts',(-7.5167640777479,54.1624999997938,10.3459381770593));
#288316=CARTESIAN_POINT('Ctrl Pts',(-3.75838203887397,54.3124999997932,
11.5671105274575));
#288317=CARTESIAN_POINT('Ctrl Pts',(-4.14935760342564E-14,54.4624999997926,
12.7882828778556));
#288318=CARTESIAN_POINT('Ctrl Pts',(3.75838203887389,54.612499999792,11.5671105274575));
#288319=CARTESIAN_POINT('Ctrl Pts',(7.51676407774782,54.7624999997914,10.3459381770593));
#288320=CARTESIAN_POINT('Ctrl Pts',(9.83957192047903,54.9124999997908,7.14886745759543));
#288321=CARTESIAN_POINT('Ctrl Pts',(12.1623797632103,55.0624999997902,3.95179673813153));
#288322=CARTESIAN_POINT('Ctrl Pts',(12.1623797632103,55.2124999997896,-1.489461944703E-15));
#288323=CARTESIAN_POINT('Ctrl Pts',(12.1623797632103,55.362499999789,-3.95179673813154));
#288324=CARTESIAN_POINT('Ctrl Pts',(9.83957192047903,55.5124999997884,-7.14886745759543));
#288325=CARTESIAN_POINT('Ctrl Pts',(7.51676407774781,55.6624999997878,-10.3459381770593));
#288326=CARTESIAN_POINT('Ctrl Pts',(3.75838203887388,55.8124999997872,-11.5671105274575));
#288327=CARTESIAN_POINT('Ctrl Pts',(-4.54896566086787E-14,55.9624999997866,
-12.7882828778556));
#288328=CARTESIAN_POINT('Ctrl Pts',(-3.75838203887397,56.112499999786,-11.5671105274575));
#288329=CARTESIAN_POINT('Ctrl Pts',(-7.5167640777479,56.2624999997854,-10.3459381770593));
#288330=CARTESIAN_POINT('Ctrl Pts',(-9.83957192047912,56.4124999997848,
-7.14886745759543));
#288331=CARTESIAN_POINT('Ctrl Pts',(-12.1623797632103,56.5624999997842,
-3.95179673813153));
#288332=CARTESIAN_POINT('Ctrl Pts',(-12.1623797632103,56.7124999997836,
2.97892388940601E-15));
#288333=CARTESIAN_POINT('Ctrl Pts',(-12.1623797632103,56.862499999783,3.95179673813154));
#288334=CARTESIAN_POINT('Ctrl Pts',(-9.83957192047912,57.0124999997824,
7.14886745759543));
#288335=CARTESIAN_POINT('Ctrl Pts',(-7.5167640777479,57.1624999997818,10.3459381770593));
#288336=CARTESIAN_POINT('Ctrl Pts',(-3.75838203887397,57.3124999997812,
11.5671105274575));
#288337=CARTESIAN_POINT('Ctrl Pts',(-4.32212853059182E-14,57.4624999997806,
12.7882828778556));
#288338=CARTESIAN_POINT('Ctrl Pts',(3.75838203887389,57.61249999978,11.5671105274575));
#288339=CARTESIAN_POINT('Ctrl Pts',(7.51676407774781,57.7624999997794,10.3459381770593));
#288340=CARTESIAN_POINT('Ctrl Pts',(9.83957192047903,57.9124999997788,7.14886745759543));
#288341=CARTESIAN_POINT('Ctrl Pts',(12.1623797632103,58.0624999997782,3.95179673813153));
#288342=CARTESIAN_POINT('Ctrl Pts',(12.1623797632102,58.2124999997776,-1.489461944703E-15));
#288343=CARTESIAN_POINT('Ctrl Pts',(12.1623797632102,58.362499999777,-3.95179673813154));
#288344=CARTESIAN_POINT('Ctrl Pts',(9.83957192047903,58.5124999997764,-7.14886745759543));
#288345=CARTESIAN_POINT('Ctrl Pts',(7.51676407774781,58.6624999997758,-10.3459381770593));
#288346=CARTESIAN_POINT('Ctrl Pts',(3.75838203887388,58.8124999997752,-11.5671105274575));
#288347=CARTESIAN_POINT('Ctrl Pts',(-4.72173658803405E-14,58.9624999997746,
-12.7882828778556));
#288348=CARTESIAN_POINT('Ctrl Pts',(-3.75838203887398,59.112499999774,-11.5671105274575));
#288349=CARTESIAN_POINT('Ctrl Pts',(-7.51676407774791,59.2624999997734,
-10.3459381770593));
#288350=CARTESIAN_POINT('Ctrl Pts',(-9.83957192047912,59.4124999997728,
-7.14886745759543));
#288351=CARTESIAN_POINT('Ctrl Pts',(-12.1623797632103,59.5624999997722,
-3.95179673813153));
#288352=CARTESIAN_POINT('Ctrl Pts',(-12.1623797632103,59.7124999997716,
2.97892388940601E-15));
#288353=CARTESIAN_POINT('Ctrl Pts',(-12.1623797632103,59.862499999771,3.95179673813154));
#288354=CARTESIAN_POINT('Ctrl Pts',(-9.83957192047912,60.0124999997704,
7.14886745759543));
#288355=CARTESIAN_POINT('Ctrl Pts',(-7.5167640777479,60.1624999997698,10.3459381770593));
#288356=CARTESIAN_POINT('Ctrl Pts',(-3.75838203887397,60.3124999997692,
11.5671105274575));
#288357=CARTESIAN_POINT('Ctrl Pts',(-4.49489945775801E-14,60.4624999997686,
12.7882828778556));
#288358=CARTESIAN_POINT('Ctrl Pts',(3.75838203887388,60.612499999768,11.5671105274575));
#288359=CARTESIAN_POINT('Ctrl Pts',(7.51676407774781,60.7624999997674,10.3459381770593));
#288360=CARTESIAN_POINT('Ctrl Pts',(9.83957192047903,60.9124999997668,7.14886745759543));
#288361=CARTESIAN_POINT('Ctrl Pts',(12.1623797632103,61.0624999997662,3.95179673813153));
#288362=CARTESIAN_POINT('Ctrl Pts',(12.1623797632102,61.2124999997656,-1.489461944703E-15));
#288363=CARTESIAN_POINT('Ctrl Pts',(12.1623797632102,61.362499999765,-3.95179673813154));
#288364=CARTESIAN_POINT('Ctrl Pts',(9.83957192047902,61.5124999997644,-7.14886745759543));
#288365=CARTESIAN_POINT('Ctrl Pts',(7.51676407774781,61.6624999997638,-10.3459381770593));
#288366=CARTESIAN_POINT('Ctrl Pts',(3.75838203887388,61.8124999997632,-11.5671105274575));
#288367=CARTESIAN_POINT('Ctrl Pts',(-4.89450751520023E-14,61.9624999997626,
-12.7882828778556));
#288368=CARTESIAN_POINT('Ctrl Pts',(-3.75838203887398,62.112499999762,-11.5671105274575));
#288369=CARTESIAN_POINT('Ctrl Pts',(-7.51676407774791,62.2624999997614,
-10.3459381770593));
#288370=CARTESIAN_POINT('Ctrl Pts',(-9.83957192047912,62.4124999997608,
-7.14886745759543));
#288371=CARTESIAN_POINT('Ctrl Pts',(-12.1623797632103,62.5624999997602,
-3.95179673813153));
#288372=CARTESIAN_POINT('Ctrl Pts',(-12.1623797632103,62.7124999997596,
2.97892388940601E-15));
#288373=CARTESIAN_POINT('Ctrl Pts',(-12.1623797632103,62.862499999759,3.95179673813154));
#288374=CARTESIAN_POINT('Ctrl Pts',(-9.83957192047912,63.0124999997584,
7.14886745759543));
#288375=CARTESIAN_POINT('Ctrl Pts',(-7.5167640777479,63.1624999997578,10.3459381770593));
#288376=CARTESIAN_POINT('Ctrl Pts',(-3.75838203887398,63.3124999997572,
11.5671105274575));
#288377=CARTESIAN_POINT('Ctrl Pts',(-4.66767038492419E-14,63.4624999997566,
12.7882828778556));
#288378=CARTESIAN_POINT('Ctrl Pts',(3.75838203887388,63.612499999756,11.5671105274575));
#288379=CARTESIAN_POINT('Ctrl Pts',(7.51676407774781,63.7624999997554,10.3459381770593));
#288380=CARTESIAN_POINT('Ctrl Pts',(9.83957192047903,63.9124999997548,7.14886745759543));
#288381=CARTESIAN_POINT('Ctrl Pts',(12.1623797632102,64.0624999997542,3.95179673813153));
#288382=CARTESIAN_POINT('Ctrl Pts',(12.1623797632102,64.2124999997536,-1.489461944703E-15));
#288383=CARTESIAN_POINT('Ctrl Pts',(12.1623797632102,64.362499999753,-3.95179673813154));
#288384=CARTESIAN_POINT('Ctrl Pts',(9.83957192047902,64.5124999997524,-7.14886745759543));
#288385=CARTESIAN_POINT('Ctrl Pts',(7.51676407774781,64.6624999997518,-10.3459381770593));
#288386=CARTESIAN_POINT('Ctrl Pts',(3.75838203887388,64.8124999997512,-11.5671105274575));
#288387=CARTESIAN_POINT('Ctrl Pts',(-5.06727844236642E-14,64.9624999997506,
-12.7882828778556));
#288388=CARTESIAN_POINT('Ctrl Pts',(-3.75838203887398,65.11249999975,-11.5671105274575));
#288389=CARTESIAN_POINT('Ctrl Pts',(-7.51676407774791,65.2624999997494,
-10.3459381770593));
#288390=CARTESIAN_POINT('Ctrl Pts',(-9.83957192047913,65.4124999997488,
-7.14886745759543));
#288391=CARTESIAN_POINT('Ctrl Pts',(-12.1623797632103,65.5624999997482,
-3.95179673813153));
#288392=CARTESIAN_POINT('Ctrl Pts',(-12.1623797632103,65.7124999997476,
2.97892388940601E-15));
#288393=CARTESIAN_POINT('Ctrl Pts',(-12.1623797632103,65.862499999747,3.95179673813154));
#288394=CARTESIAN_POINT('Ctrl Pts',(-9.83957192047912,66.0124999997464,
7.14886745759543));
#288395=CARTESIAN_POINT('Ctrl Pts',(-7.51676407774791,66.1624999997458,
10.3459381770593));
#288396=CARTESIAN_POINT('Ctrl Pts',(-3.75838203887398,66.3124999997452,
11.5671105274575));
#288397=CARTESIAN_POINT('Ctrl Pts',(-4.84044131209037E-14,66.4624999997446,
12.7882828778556));
#288398=CARTESIAN_POINT('Ctrl Pts',(3.75838203887388,66.612499999744,11.5671105274575));
#288399=CARTESIAN_POINT('Ctrl Pts',(7.51676407774781,66.7624999997434,10.3459381770593));
#288400=CARTESIAN_POINT('Ctrl Pts',(9.83957192047902,66.9124999997428,7.14886745759543));
#288401=CARTESIAN_POINT('Ctrl Pts',(12.1623797632102,67.0624999997422,3.95179673813153));
#288402=CARTESIAN_POINT('Ctrl Pts',(12.1623797632102,67.2124999997416,-1.489461944703E-15));
#288403=CARTESIAN_POINT('Ctrl Pts',(12.1623797632102,67.362499999741,-3.95179673813154));
#288404=CARTESIAN_POINT('Ctrl Pts',(9.83957192047902,67.5124999997404,-7.14886745759543));
#288405=CARTESIAN_POINT('Ctrl Pts',(7.51676407774781,67.6624999997398,-10.3459381770593));
#288406=CARTESIAN_POINT('Ctrl Pts',(3.75838203887388,67.8124999997392,-11.5671105274575));
#288407=CARTESIAN_POINT('Ctrl Pts',(-5.2400493695326E-14,67.9624999997386,
-12.7882828778556));
#288408=CARTESIAN_POINT('Ctrl Pts',(-3.75838203887398,68.112499999738,-11.5671105274575));
#288409=CARTESIAN_POINT('Ctrl Pts',(-7.51676407774791,68.2624999997374,
-10.3459381770593));
#288410=CARTESIAN_POINT('Ctrl Pts',(-9.83957192047913,68.4124999997368,
-7.14886745759543));
#288411=CARTESIAN_POINT('Ctrl Pts',(-12.1623797632103,68.5624999997362,
-3.95179673813153));
#288412=CARTESIAN_POINT('Ctrl Pts',(-12.1623797632103,68.7124999997356,
2.97892388940601E-15));
#288413=CARTESIAN_POINT('Ctrl Pts',(-12.1623797632103,68.862499999735,3.95179673813154));
#288414=CARTESIAN_POINT('Ctrl Pts',(-9.83957192047913,69.0124999997344,
7.14886745759543));
#288415=CARTESIAN_POINT('Ctrl Pts',(-7.51676407774791,69.1624999997338,
10.3459381770593));
#288416=CARTESIAN_POINT('Ctrl Pts',(-3.75838203887398,69.3124999997332,
11.5671105274575));
#288417=CARTESIAN_POINT('Ctrl Pts',(-5.01321223925656E-14,69.4624999997326,
12.7882828778556));
#288418=CARTESIAN_POINT('Ctrl Pts',(3.75838203887388,69.612499999732,11.5671105274575));
#288419=CARTESIAN_POINT('Ctrl Pts',(7.51676407774781,69.7624999997314,10.3459381770593));
#288420=CARTESIAN_POINT('Ctrl Pts',(9.83957192047902,69.9124999997308,7.14886745759543));
#288421=CARTESIAN_POINT('Ctrl Pts',(12.1623797632102,70.0624999997302,3.95179673813153));
#288422=CARTESIAN_POINT('Ctrl Pts',(12.1623797632102,70.2124999997296,-1.489461944703E-15));
#288423=CARTESIAN_POINT('Ctrl Pts',(12.1623797632102,70.362499999729,-3.95179673813154));
#288424=CARTESIAN_POINT('Ctrl Pts',(9.83957192047902,70.5124999997284,-7.14886745759543));
#288425=CARTESIAN_POINT('Ctrl Pts',(7.5167640777478,70.6624999997278,-10.3459381770593));
#288426=CARTESIAN_POINT('Ctrl Pts',(3.75838203887388,70.8124999997272,-11.5671105274575));
#288427=CARTESIAN_POINT('Ctrl Pts',(-5.41282029669879E-14,70.9624999997266,
-12.7882828778556));
#288428=CARTESIAN_POINT('Ctrl Pts',(-3.75838203887398,71.112499999726,-11.5671105274575));
#288429=CARTESIAN_POINT('Ctrl Pts',(-7.51676407774791,71.2624999997254,
-10.3459381770593));
#288430=CARTESIAN_POINT('Ctrl Pts',(-9.83957192047913,71.4124999997248,
-7.14886745759543));
#288431=CARTESIAN_POINT('Ctrl Pts',(-12.1623797632103,71.5624999997242,
-3.95179673813153));
#288432=CARTESIAN_POINT('Ctrl Pts',(-12.1623797632103,71.7124999997236,
2.97892388940601E-15));
#288433=CARTESIAN_POINT('Ctrl Pts',(-12.1623797632103,71.862499999723,3.95179673813154));
#288434=CARTESIAN_POINT('Ctrl Pts',(-9.83957192047913,72.0124999997224,
7.14886745759543));
#288435=CARTESIAN_POINT('Ctrl Pts',(-7.51676407774791,72.1624999997218,
10.3459381770593));
#288436=CARTESIAN_POINT('Ctrl Pts',(-3.75838203887398,72.3124999997212,
11.5671105274575));
#288437=CARTESIAN_POINT('Ctrl Pts',(-5.18598316642274E-14,72.4624999997206,
12.7882828778556));
#288438=CARTESIAN_POINT('Ctrl Pts',(3.75838203887388,72.61249999972,11.5671105274575));
#288439=CARTESIAN_POINT('Ctrl Pts',(7.51676407774781,72.7624999997194,10.3459381770593));
#288440=CARTESIAN_POINT('Ctrl Pts',(9.83957192047902,72.9124999997188,7.14886745759543));
#288441=CARTESIAN_POINT('Ctrl Pts',(12.1623797632102,73.0624999997182,3.95179673813153));
#288442=CARTESIAN_POINT('Ctrl Pts',(12.1623797632102,73.2124999997176,-1.489461944703E-15));
#288443=CARTESIAN_POINT('Ctrl Pts',(12.1623797632102,73.362499999717,-3.95179673813154));
#288444=CARTESIAN_POINT('Ctrl Pts',(9.83957192047902,73.5124999997164,-7.14886745759543));
#288445=CARTESIAN_POINT('Ctrl Pts',(7.5167640777478,73.6624999997158,-10.3459381770593));
#288446=CARTESIAN_POINT('Ctrl Pts',(3.75838203887387,73.8124999997152,-11.5671105274575));
#288447=CARTESIAN_POINT('Ctrl Pts',(-5.58559122386497E-14,73.9624999997146,
-12.7882828778556));
#288448=CARTESIAN_POINT('Ctrl Pts',(-3.75838203887398,74.112499999714,-11.5671105274575));
#288449=CARTESIAN_POINT('Ctrl Pts',(-7.51676407774791,74.2624999997134,
-10.3459381770593));
#288450=CARTESIAN_POINT('Ctrl Pts',(-9.83957192047913,74.4124999997128,
-7.14886745759543));
#288451=CARTESIAN_POINT('Ctrl Pts',(-12.1623797632103,74.5624999997122,
-3.95179673813153));
#288452=CARTESIAN_POINT('Ctrl Pts',(-12.1623797632103,74.7124999997116,
2.97892388940601E-15));
#288453=CARTESIAN_POINT('Ctrl Pts',(-12.1623797632103,74.862499999711,3.95179673813154));
#288454=CARTESIAN_POINT('Ctrl Pts',(-9.83957192047913,75.0124999997104,
7.14886745759543));
#288455=CARTESIAN_POINT('Ctrl Pts',(-7.51676407774791,75.1624999997098,
10.3459381770593));
#288456=CARTESIAN_POINT('Ctrl Pts',(-3.75838203887398,75.3124999997092,
11.5671105274575));
#288457=CARTESIAN_POINT('Ctrl Pts',(-5.35875409358893E-14,75.4624999997086,
12.7882828778556));
#288458=CARTESIAN_POINT('Ctrl Pts',(3.75838203887388,75.612499999708,11.5671105274575));
#288459=CARTESIAN_POINT('Ctrl Pts',(7.5167640777478,75.7624999997074,10.3459381770593));
#288460=CARTESIAN_POINT('Ctrl Pts',(9.83957192047902,75.9124999997068,7.14886745759543));
#288461=CARTESIAN_POINT('Ctrl Pts',(12.1623797632102,76.0624999997062,3.95179673813153));
#288462=CARTESIAN_POINT('Ctrl Pts',(12.1623797632102,76.2124999997056,-1.489461944703E-15));
#288463=CARTESIAN_POINT('Ctrl Pts',(12.1623797632102,76.362499999705,-3.95179673813154));
#288464=CARTESIAN_POINT('Ctrl Pts',(9.83957192047902,76.5124999997044,-7.14886745759543));
#288465=CARTESIAN_POINT('Ctrl Pts',(7.5167640777478,76.6624999997038,-10.3459381770593));
#288466=CARTESIAN_POINT('Ctrl Pts',(3.75838203887387,76.8124999997032,-11.5671105274575));
#288467=CARTESIAN_POINT('Ctrl Pts',(-5.75836215103115E-14,76.9624999997026,
-12.7882828778556));
#288468=CARTESIAN_POINT('Ctrl Pts',(-3.75838203887399,77.112499999702,-11.5671105274575));
#288469=CARTESIAN_POINT('Ctrl Pts',(-7.51676407774791,77.2624999997014,
-10.3459381770593));
#288470=CARTESIAN_POINT('Ctrl Pts',(-9.83957192047913,77.4124999997008,
-7.14886745759543));
#288471=CARTESIAN_POINT('Ctrl Pts',(-12.1623797632103,77.5624999997002,
-3.95179673813153));
#288472=CARTESIAN_POINT('Ctrl Pts',(-12.1623797632103,77.7124999996996,
2.97892388940601E-15));
#288473=CARTESIAN_POINT('Ctrl Pts',(-12.1623797632103,77.862499999699,3.95179673813154));
#288474=CARTESIAN_POINT('Ctrl Pts',(-9.83957192047913,78.0124999996984,
7.14886745759543));
#288475=CARTESIAN_POINT('Ctrl Pts',(-7.51676407774791,78.1624999996978,
10.3459381770593));
#288476=CARTESIAN_POINT('Ctrl Pts',(-3.75838203887398,78.3124999996972,
11.5671105274575));
#288477=CARTESIAN_POINT('Ctrl Pts',(-5.53152502075511E-14,78.4624999996966,
12.7882828778556));
#288478=CARTESIAN_POINT('Ctrl Pts',(3.75838203887387,78.612499999696,11.5671105274575));
#288479=CARTESIAN_POINT('Ctrl Pts',(7.5167640777478,78.7624999996954,10.3459381770593));
#288480=CARTESIAN_POINT('Ctrl Pts',(9.83957192047902,78.9124999996948,7.14886745759543));
#288481=CARTESIAN_POINT('Ctrl Pts',(12.1623797632102,79.0624999996942,3.95179673813153));
#288482=CARTESIAN_POINT('Ctrl Pts',(12.1623797632102,79.2124999996936,-1.489461944703E-15));
#288483=CARTESIAN_POINT('Ctrl Pts',(12.1623797632102,79.362499999693,-3.95179673813154));
#288484=CARTESIAN_POINT('Ctrl Pts',(9.83957192047902,79.5124999996924,-7.14886745759543));
#288485=CARTESIAN_POINT('Ctrl Pts',(7.5167640777478,79.6624999996918,-10.3459381770593));
#288486=CARTESIAN_POINT('Ctrl Pts',(3.75838203887387,79.8124999996912,-11.5671105274575));
#288487=CARTESIAN_POINT('Ctrl Pts',(-5.93113307819734E-14,79.9624999996906,
-12.7882828778556));
#288488=CARTESIAN_POINT('Ctrl Pts',(-3.75838203887399,80.11249999969,-11.5671105274575));
#288489=CARTESIAN_POINT('Ctrl Pts',(-7.51676407774791,80.2624999996894,
-10.3459381770593));
#288490=CARTESIAN_POINT('Ctrl Pts',(-9.83957192047913,80.4124999996888,
-7.14886745759543));
#288491=CARTESIAN_POINT('Ctrl Pts',(-12.1623797632104,80.5624999996882,
-3.95179673813153));
#288492=CARTESIAN_POINT('Ctrl Pts',(-12.1623797632104,80.7124999996876,
2.97892388940601E-15));
#288493=CARTESIAN_POINT('Ctrl Pts',(-12.1623797632104,80.862499999687,3.95179673813154));
#288494=CARTESIAN_POINT('Ctrl Pts',(-9.83957192047913,81.0124999996864,
7.14886745759543));
#288495=CARTESIAN_POINT('Ctrl Pts',(-7.51676407774791,81.1624999996858,
10.3459381770593));
#288496=CARTESIAN_POINT('Ctrl Pts',(-3.75838203887399,81.3124999996852,
11.5671105274575));
#288497=CARTESIAN_POINT('Ctrl Pts',(-5.70429594792129E-14,81.4624999996846,
12.7882828778556));
#288498=CARTESIAN_POINT('Ctrl Pts',(3.75838203887387,81.612499999684,11.5671105274575));
#288499=CARTESIAN_POINT('Ctrl Pts',(7.5167640777478,81.7624999996834,10.3459381770593));
#288500=CARTESIAN_POINT('Ctrl Pts',(9.83957192047902,81.9124999996828,7.14886745759543));
#288501=CARTESIAN_POINT('Ctrl Pts',(12.1623797632102,82.0624999996822,3.95179673813153));
#288502=CARTESIAN_POINT('Ctrl Pts',(12.1623797632102,82.2124999996816,-1.489461944703E-15));
#288503=CARTESIAN_POINT('Ctrl Pts',(12.1623797632102,82.362499999681,-3.95179673813154));
#288504=CARTESIAN_POINT('Ctrl Pts',(9.83957192047902,82.5124999996804,-7.14886745759543));
#288505=CARTESIAN_POINT('Ctrl Pts',(7.5167640777478,82.6624999996798,-10.3459381770593));
#288506=CARTESIAN_POINT('Ctrl Pts',(3.75838203887387,82.8124999996792,-11.5671105274575));
#288507=CARTESIAN_POINT('Ctrl Pts',(-6.10390400536352E-14,82.9624999996786,
-12.7882828778556));
#288508=CARTESIAN_POINT('Ctrl Pts',(-3.75838203887399,83.112499999678,-11.5671105274575));
#288509=CARTESIAN_POINT('Ctrl Pts',(-7.51676407774792,83.2624999996774,
-10.3459381770593));
#288510=CARTESIAN_POINT('Ctrl Pts',(-9.83957192047914,83.4124999996768,
-7.14886745759543));
#288511=CARTESIAN_POINT('Ctrl Pts',(-12.1623797632104,83.5624999996762,
-3.95179673813153));
#288512=CARTESIAN_POINT('Ctrl Pts',(-12.1623797632104,83.7124999996756,
2.97892388940601E-15));
#288513=CARTESIAN_POINT('Ctrl Pts',(-12.1623797632104,83.862499999675,3.95179673813154));
#288514=CARTESIAN_POINT('Ctrl Pts',(-9.83957192047913,84.0124999996744,
7.14886745759543));
#288515=CARTESIAN_POINT('Ctrl Pts',(-7.51676407774791,84.1624999996738,
10.3459381770593));
#288516=CARTESIAN_POINT('Ctrl Pts',(-3.75838203887399,84.3124999996732,
11.5671105274575));
#288517=CARTESIAN_POINT('Ctrl Pts',(-5.87706687508748E-14,84.4624999996726,
12.7882828778556));
#288518=CARTESIAN_POINT('Ctrl Pts',(3.75838203887387,84.6124999996721,11.5671105274575));
#288519=CARTESIAN_POINT('Ctrl Pts',(7.5167640777478,84.7624999996714,10.3459381770593));
#288520=CARTESIAN_POINT('Ctrl Pts',(9.83957192047902,84.9124999996708,7.14886745759543));
#288521=CARTESIAN_POINT('Ctrl Pts',(12.1623797632102,85.0624999996702,3.95179673813153));
#288522=CARTESIAN_POINT('Ctrl Pts',(12.1623797632102,85.2124999996696,-1.489461944703E-15));
#288523=CARTESIAN_POINT('Ctrl Pts',(12.1623797632102,85.362499999669,-3.95179673813154));
#288524=CARTESIAN_POINT('Ctrl Pts',(9.83957192047901,85.5124999996684,-7.14886745759543));
#288525=CARTESIAN_POINT('Ctrl Pts',(7.5167640777478,85.6624999996678,-10.3459381770593));
#288526=CARTESIAN_POINT('Ctrl Pts',(3.75838203887387,85.8124999996672,-11.5671105274575));
#288527=CARTESIAN_POINT('Ctrl Pts',(-6.27667493252971E-14,85.9624999996666,
-12.7882828778556));
#288528=CARTESIAN_POINT('Ctrl Pts',(-3.75838203887399,86.112499999666,-11.5671105274575));
#288529=CARTESIAN_POINT('Ctrl Pts',(-7.51676407774792,86.2624999996654,
-10.3459381770593));
#288530=CARTESIAN_POINT('Ctrl Pts',(-9.83957192047914,86.4124999996648,
-7.14886745759543));
#288531=CARTESIAN_POINT('Ctrl Pts',(-12.1623797632104,86.5624999996642,
-3.95179673813153));
#288532=CARTESIAN_POINT('Ctrl Pts',(-12.1623797632104,86.7124999996636,
2.97892388940601E-15));
#288533=CARTESIAN_POINT('Ctrl Pts',(-12.1623797632104,86.862499999663,3.95179673813154));
#288534=CARTESIAN_POINT('Ctrl Pts',(-9.83957192047914,87.0124999996624,
7.14886745759543));
#288535=CARTESIAN_POINT('Ctrl Pts',(-7.51676407774792,87.1624999996618,
10.3459381770593));
#288536=CARTESIAN_POINT('Ctrl Pts',(-3.75838203887399,87.3124999996612,
11.5671105274575));
#288537=CARTESIAN_POINT('Ctrl Pts',(-6.04983780225366E-14,87.4624999996606,
12.7882828778556));
#288538=CARTESIAN_POINT('Ctrl Pts',(3.75838203887387,87.61249999966,11.5671105274575));
#288539=CARTESIAN_POINT('Ctrl Pts',(7.5167640777478,87.7624999996594,10.3459381770593));
#288540=CARTESIAN_POINT('Ctrl Pts',(9.83957192047901,87.9124999996588,7.14886745759543));
#288541=CARTESIAN_POINT('Ctrl Pts',(12.1623797632102,88.0624999996582,3.95179673813153));
#288542=CARTESIAN_POINT('Ctrl Pts',(12.1623797632102,88.2124999996576,-1.489461944703E-15));
#288543=CARTESIAN_POINT('Ctrl Pts',(12.1623797632102,88.362499999657,-3.95179673813154));
#288544=CARTESIAN_POINT('Ctrl Pts',(9.83957192047901,88.5124999996564,-7.14886745759543));
#288545=CARTESIAN_POINT('Ctrl Pts',(7.51676407774779,88.6624999996558,-10.3459381770593));
#288546=CARTESIAN_POINT('Ctrl Pts',(3.75838203887386,88.8124999996552,-11.5671105274575));
#288547=CARTESIAN_POINT('Ctrl Pts',(-6.44944585969589E-14,88.9624999996546,
-12.7882828778556));
#288548=CARTESIAN_POINT('Ctrl Pts',(-3.75838203887399,89.112499999654,-11.5671105274575));
#288549=CARTESIAN_POINT('Ctrl Pts',(-7.51676407774792,89.2624999996534,
-10.3459381770593));
#288550=CARTESIAN_POINT('Ctrl Pts',(-9.83957192047914,89.4124999996528,
-7.14886745759543));
#288551=CARTESIAN_POINT('Ctrl Pts',(-12.1623797632104,89.5624999996522,
-3.95179673813153));
#288552=CARTESIAN_POINT('Ctrl Pts',(-12.1623797632104,89.7124999996516,
2.97892388940601E-15));
#288553=CARTESIAN_POINT('Ctrl Pts',(-12.1623797632104,89.862499999651,3.95179673813154));
#288554=CARTESIAN_POINT('Ctrl Pts',(-9.83957192047914,90.0124999996504,
7.14886745759543));
#288555=CARTESIAN_POINT('Ctrl Pts',(-7.51676407774792,90.1624999996498,
10.3459381770593));
#288556=CARTESIAN_POINT('Ctrl Pts',(-3.75838203887399,90.3124999996492,
11.5671105274575));
#288557=CARTESIAN_POINT('Ctrl Pts',(-6.22260872941985E-14,90.4624999996486,
12.7882828778556));
#288558=CARTESIAN_POINT('Ctrl Pts',(3.75838203887387,90.612499999648,11.5671105274575));
#288559=CARTESIAN_POINT('Ctrl Pts',(7.5167640777478,90.7624999996474,10.3459381770593));
#288560=CARTESIAN_POINT('Ctrl Pts',(9.83957192047901,90.9124999996468,7.14886745759543));
#288561=CARTESIAN_POINT('Ctrl Pts',(12.1623797632102,91.0624999996462,3.95179673813153));
#288562=CARTESIAN_POINT('Ctrl Pts',(12.1623797632102,91.2124999996456,-1.489461944703E-15));
#288563=CARTESIAN_POINT('Ctrl Pts',(12.1623797632102,91.362499999645,-3.95179673813154));
#288564=CARTESIAN_POINT('Ctrl Pts',(9.83957192047901,91.5124999996444,-7.14886745759543));
#288565=CARTESIAN_POINT('Ctrl Pts',(7.51676407774779,91.6624999996438,-10.3459381770593));
#288566=CARTESIAN_POINT('Ctrl Pts',(3.75838203887386,91.8124999996432,-11.5671105274575));
#288567=CARTESIAN_POINT('Ctrl Pts',(-6.62221678686207E-14,91.9624999996426,
-12.7882828778556));
#288568=CARTESIAN_POINT('Ctrl Pts',(-3.75838203887399,92.112499999642,-11.5671105274575));
#288569=CARTESIAN_POINT('Ctrl Pts',(-7.51676407774792,92.2624999996414,
-10.3459381770593));
#288570=CARTESIAN_POINT('Ctrl Pts',(-9.83957192047914,92.4124999996408,
-7.14886745759543));
#288571=CARTESIAN_POINT('Ctrl Pts',(-12.1623797632104,92.5624999996402,
-3.95179673813153));
#288572=CARTESIAN_POINT('Ctrl Pts',(-12.1623797632104,92.7124999996396,
2.97892388940601E-15));
#288573=CARTESIAN_POINT('Ctrl Pts',(-12.1623797632104,92.862499999639,3.95179673813154));
#288574=CARTESIAN_POINT('Ctrl Pts',(-9.83957192047914,93.0124999996384,
7.14886745759543));
#288575=CARTESIAN_POINT('Ctrl Pts',(-7.51676407774792,93.1624999996378,
10.3459381770593));
#288576=CARTESIAN_POINT('Ctrl Pts',(-3.75838203887399,93.3124999996372,
11.5671105274575));
#288577=CARTESIAN_POINT('Ctrl Pts',(-6.39537965658603E-14,93.4624999996366,
12.7882828778556));
#288578=CARTESIAN_POINT('Ctrl Pts',(3.75838203887386,93.612499999636,11.5671105274575));
#288579=CARTESIAN_POINT('Ctrl Pts',(7.51676407774779,93.7624999996354,10.3459381770593));
#288580=CARTESIAN_POINT('Ctrl Pts',(9.83957192047901,93.9124999996348,7.14886745759543));
#288581=CARTESIAN_POINT('Ctrl Pts',(12.1623797632102,94.0624999996342,3.95179673813153));
#288582=CARTESIAN_POINT('Ctrl Pts',(12.1623797632102,94.2124999996336,-1.489461944703E-15));
#288583=CARTESIAN_POINT('Ctrl Pts',(12.1623797632102,94.362499999633,-3.95179673813154));
#288584=CARTESIAN_POINT('Ctrl Pts',(9.83957192047901,94.5124999996324,-7.14886745759543));
#288585=CARTESIAN_POINT('Ctrl Pts',(7.51676407774779,94.6624999996318,-10.3459381770593));
#288586=CARTESIAN_POINT('Ctrl Pts',(3.75838203887386,94.8124999996312,-11.5671105274575));
#288587=CARTESIAN_POINT('Ctrl Pts',(-6.79498771402825E-14,94.9624999996306,
-12.7882828778556));
#288588=CARTESIAN_POINT('Ctrl Pts',(-3.758382038874,95.11249999963,-11.5671105274575));
#288589=CARTESIAN_POINT('Ctrl Pts',(-7.51676407774792,95.2624999996294,
-10.3459381770593));
#288590=CARTESIAN_POINT('Ctrl Pts',(-9.83957192047914,95.4124999996288,
-7.14886745759543));
#288591=CARTESIAN_POINT('Ctrl Pts',(-12.1623797632104,95.5624999996282,
-3.95179673813153));
#288592=CARTESIAN_POINT('Ctrl Pts',(-12.1623797632104,95.7124999996276,
2.97892388940601E-15));
#288593=CARTESIAN_POINT('Ctrl Pts',(-12.1623797632104,95.862499999627,3.95179673813154));
#288594=CARTESIAN_POINT('Ctrl Pts',(-9.83957192047914,96.0124999996264,
7.14886745759543));
#288595=CARTESIAN_POINT('Ctrl Pts',(-7.51676407774792,96.1624999996258,
10.3459381770593));
#288596=CARTESIAN_POINT('Ctrl Pts',(-3.75838203887399,96.3124999996252,
11.5671105274575));
#288597=CARTESIAN_POINT('Ctrl Pts',(-6.56815058375222E-14,96.4624999996246,
12.7882828778556));
#288598=CARTESIAN_POINT('Ctrl Pts',(3.75838203887386,96.612499999624,11.5671105274575));
#288599=CARTESIAN_POINT('Ctrl Pts',(7.51676407774779,96.7624999996234,10.3459381770593));
#288600=CARTESIAN_POINT('Ctrl Pts',(9.83957192047901,96.9124999996228,7.14886745759543));
#288601=CARTESIAN_POINT('Ctrl Pts',(12.1623797632102,97.0624999996222,3.95179673813153));
#288602=CARTESIAN_POINT('Ctrl Pts',(12.1623797632102,97.2124999996216,-1.489461944703E-15));
#288603=CARTESIAN_POINT('Ctrl Pts',(12.1623797632102,97.3624999996211,-3.95179673813154));
#288604=CARTESIAN_POINT('Ctrl Pts',(9.83957192047901,97.5124999996204,-7.14886745759543));
#288605=CARTESIAN_POINT('Ctrl Pts',(7.51676407774779,97.6624999996198,-10.3459381770593));
#288606=CARTESIAN_POINT('Ctrl Pts',(3.75838203887386,97.8124999996192,-11.5671105274575));
#288607=CARTESIAN_POINT('Ctrl Pts',(-6.96775864119444E-14,97.9624999996187,
-12.7882828778556));
#288608=CARTESIAN_POINT('Ctrl Pts',(-3.758382038874,98.112499999618,-11.5671105274575));
#288609=CARTESIAN_POINT('Ctrl Pts',(-7.51676407774793,98.2624999996174,
-10.3459381770593));
#288610=CARTESIAN_POINT('Ctrl Pts',(-9.83957192047914,98.4124999996168,
-7.14886745759543));
#288611=CARTESIAN_POINT('Ctrl Pts',(-12.1623797632104,98.5624999996162,
-3.95179673813153));
#288612=CARTESIAN_POINT('Ctrl Pts',(-12.1623797632104,98.7124999996156,
2.97892388940601E-15));
#288613=CARTESIAN_POINT('Ctrl Pts',(-12.1623797632104,98.862499999615,3.95179673813154));
#288614=CARTESIAN_POINT('Ctrl Pts',(-9.83957192047914,99.0124999996144,
7.14886745759543));
#288615=CARTESIAN_POINT('Ctrl Pts',(-7.51676407774792,99.1624999996138,
10.3459381770593));
#288616=CARTESIAN_POINT('Ctrl Pts',(-3.758382038874,99.3124999996132,11.5671105274575));
#288617=CARTESIAN_POINT('Ctrl Pts',(-6.7409215109184E-14,99.4624999996126,
12.7882828778556));
#288618=CARTESIAN_POINT('Ctrl Pts',(3.75838203887386,99.612499999612,11.5671105274575));
#288619=CARTESIAN_POINT('Ctrl Pts',(7.51676407774779,99.7624999996114,10.3459381770593));
#288620=CARTESIAN_POINT('Ctrl Pts',(9.83957192047901,99.9124999996108,7.14886745759543));
#288621=CARTESIAN_POINT('Ctrl Pts',(12.1623797632102,100.06249999961,3.95179673813153));
#288622=CARTESIAN_POINT('Ctrl Pts',(12.1623797632102,100.21249999961,-1.489461944703E-15));
#288623=CARTESIAN_POINT('Ctrl Pts',(12.1623797632102,100.362499999609,-3.95179673813154));
#288624=CARTESIAN_POINT('Ctrl Pts',(9.839571920479,100.512499999608,-7.14886745759543));
#288625=CARTESIAN_POINT('Ctrl Pts',(7.51676407774779,100.662499999608,-10.3459381770593));
#288626=CARTESIAN_POINT('Ctrl Pts',(3.75838203887386,100.812499999607,-11.5671105274575));
#288627=CARTESIAN_POINT('Ctrl Pts',(-7.14052956836063E-14,100.962499999607,
-12.7882828778556));
#288628=CARTESIAN_POINT('Ctrl Pts',(-3.758382038874,101.112499999606,-11.5671105274575));
#288629=CARTESIAN_POINT('Ctrl Pts',(-7.51676407774793,101.262499999605,
-10.3459381770593));
#288630=CARTESIAN_POINT('Ctrl Pts',(-9.83957192047915,101.412499999605,
-7.14886745759543));
#288631=CARTESIAN_POINT('Ctrl Pts',(-12.1623797632104,101.562499999604,
-3.95179673813153));
#288632=CARTESIAN_POINT('Ctrl Pts',(-12.1623797632104,101.712499999604,
2.97892388940601E-15));
#288633=CARTESIAN_POINT('Ctrl Pts',(-12.1623797632104,101.862499999603,
3.95179673813154));
#288634=CARTESIAN_POINT('Ctrl Pts',(-9.83957192047914,102.012499999602,
7.14886745759543));
#288635=CARTESIAN_POINT('Ctrl Pts',(-7.51676407774793,102.162499999602,
10.3459381770593));
#288636=CARTESIAN_POINT('Ctrl Pts',(-3.758382038874,102.312499999601,11.5671105274575));
#288637=CARTESIAN_POINT('Ctrl Pts',(-6.91369243808458E-14,102.462499999601,
12.7882828778556));
#288638=CARTESIAN_POINT('Ctrl Pts',(3.75838203887386,102.6124999996,11.5671105274575));
#288639=CARTESIAN_POINT('Ctrl Pts',(7.51676407774779,102.762499999599,10.3459381770593));
#288640=CARTESIAN_POINT('Ctrl Pts',(9.839571920479,102.912499999599,7.14886745759543));
#288641=CARTESIAN_POINT('Ctrl Pts',(12.1623797632102,103.062499999598,3.95179673813153));
#288642=CARTESIAN_POINT('Ctrl Pts',(12.1623797632102,103.212499999598,-1.489461944703E-15));
#288643=CARTESIAN_POINT('Ctrl Pts',(12.1623797632102,103.362499999597,-3.95179673813154));
#288644=CARTESIAN_POINT('Ctrl Pts',(9.839571920479,103.512499999596,-7.14886745759543));
#288645=CARTESIAN_POINT('Ctrl Pts',(7.51676407774779,103.662499999596,-10.3459381770593));
#288646=CARTESIAN_POINT('Ctrl Pts',(3.75838203887386,103.812499999595,-11.5671105274575));
#288647=CARTESIAN_POINT('Ctrl Pts',(-7.31330049552681E-14,103.962499999595,
-12.7882828778556));
#288648=CARTESIAN_POINT('Ctrl Pts',(-3.758382038874,104.112499999594,-11.5671105274575));
#288649=CARTESIAN_POINT('Ctrl Pts',(-7.51676407774793,104.262499999593,
-10.3459381770593));
#288650=CARTESIAN_POINT('Ctrl Pts',(-9.83957192047915,104.412499999593,
-7.14886745759543));
#288651=CARTESIAN_POINT('Ctrl Pts',(-12.1623797632104,104.562499999592,
-3.95179673813153));
#288652=CARTESIAN_POINT('Ctrl Pts',(-12.1623797632104,104.712499999592,
2.97892388940601E-15));
#288653=CARTESIAN_POINT('Ctrl Pts',(-12.1623797632104,104.862499999591,
3.95179673813154));
#288654=CARTESIAN_POINT('Ctrl Pts',(-9.83957192047915,105.01249999959,7.14886745759543));
#288655=CARTESIAN_POINT('Ctrl Pts',(-7.51676407774793,105.16249999959,10.3459381770593));
#288656=CARTESIAN_POINT('Ctrl Pts',(-3.758382038874,105.312499999589,11.5671105274575));
#288657=CARTESIAN_POINT('Ctrl Pts',(-7.08646336525076E-14,105.462499999589,
12.7882828778556));
#288658=CARTESIAN_POINT('Ctrl Pts',(3.75838203887386,105.612499999588,11.5671105274575));
#288659=CARTESIAN_POINT('Ctrl Pts',(7.51676407774779,105.762499999587,10.3459381770593));
#288660=CARTESIAN_POINT('Ctrl Pts',(9.839571920479,105.912499999587,7.14886745759543));
#288661=CARTESIAN_POINT('Ctrl Pts',(12.1623797632102,106.062499999586,3.95179673813153));
#288662=CARTESIAN_POINT('Ctrl Pts',(12.1623797632102,106.212499999586,-1.489461944703E-15));
#288663=CARTESIAN_POINT('Ctrl Pts',(12.1623797632102,106.362499999585,-3.95179673813154));
#288664=CARTESIAN_POINT('Ctrl Pts',(9.839571920479,106.512499999584,-7.14886745759543));
#288665=CARTESIAN_POINT('Ctrl Pts',(7.51676407774778,106.662499999584,-10.3459381770593));
#288666=CARTESIAN_POINT('Ctrl Pts',(3.75838203887385,106.812499999583,-11.5671105274575));
#288667=CARTESIAN_POINT('Ctrl Pts',(-7.48607142269299E-14,106.962499999583,
-12.7882828778556));
#288668=CARTESIAN_POINT('Ctrl Pts',(-3.758382038874,107.112499999582,-11.5671105274575));
#288669=CARTESIAN_POINT('Ctrl Pts',(-7.51676407774793,107.262499999581,
-10.3459381770593));
#288670=CARTESIAN_POINT('Ctrl Pts',(-9.83957192047915,107.412499999581,
-7.14886745759543));
#288671=CARTESIAN_POINT('Ctrl Pts',(-12.1623797632104,107.56249999958,-3.95179673813153));
#288672=CARTESIAN_POINT('Ctrl Pts',(-12.1623797632104,107.71249999958,2.97892388940601E-15));
#288673=CARTESIAN_POINT('Ctrl Pts',(-12.1623797632104,107.862499999579,
3.95179673813154));
#288674=CARTESIAN_POINT('Ctrl Pts',(-9.83957192047915,108.012499999578,
7.14886745759543));
#288675=CARTESIAN_POINT('Ctrl Pts',(-7.51676407774793,108.162499999578,
10.3459381770593));
#288676=CARTESIAN_POINT('Ctrl Pts',(-3.758382038874,108.312499999577,11.5671105274575));
#288677=CARTESIAN_POINT('Ctrl Pts',(-7.25923429241695E-14,108.462499999577,
12.7882828778556));
#288678=CARTESIAN_POINT('Ctrl Pts',(3.75838203887386,108.612499999576,11.5671105274575));
#288679=CARTESIAN_POINT('Ctrl Pts',(7.51676407774779,108.762499999575,10.3459381770593));
#288680=CARTESIAN_POINT('Ctrl Pts',(9.839571920479,108.912499999575,7.14886745759543));
#288681=CARTESIAN_POINT('Ctrl Pts',(12.1623797632102,109.062499999574,3.95179673813153));
#288682=CARTESIAN_POINT('Ctrl Pts',(12.1623797632102,109.212499999574,-1.489461944703E-15));
#288683=CARTESIAN_POINT('Ctrl Pts',(12.1623797632102,109.362499999573,-3.95179673813154));
#288684=CARTESIAN_POINT('Ctrl Pts',(9.839571920479,109.512499999572,-7.14886745759543));
#288685=CARTESIAN_POINT('Ctrl Pts',(7.51676407774778,109.662499999572,-10.3459381770593));
#288686=CARTESIAN_POINT('Ctrl Pts',(3.75838203887385,109.812499999571,-11.5671105274575));
#288687=CARTESIAN_POINT('Ctrl Pts',(-7.65884234985918E-14,109.962499999571,
-12.7882828778556));
#288688=CARTESIAN_POINT('Ctrl Pts',(-3.75838203887401,110.11249999957,-11.5671105274575));
#288689=CARTESIAN_POINT('Ctrl Pts',(-7.51676407774793,110.262499999569,
-10.3459381770593));
#288690=CARTESIAN_POINT('Ctrl Pts',(-9.83957192047915,110.412499999569,
-7.14886745759543));
#288691=CARTESIAN_POINT('Ctrl Pts',(-12.1623797632104,110.562499999568,
-3.95179673813153));
#288692=CARTESIAN_POINT('Ctrl Pts',(-12.1623797632104,110.712499999568,
2.97892388940601E-15));
#288693=CARTESIAN_POINT('Ctrl Pts',(-12.1623797632104,110.862499999567,
3.95179673813154));
#288694=CARTESIAN_POINT('Ctrl Pts',(-9.83957192047915,111.012499999566,
7.14886745759543));
#288695=CARTESIAN_POINT('Ctrl Pts',(-7.51676407774793,111.162499999566,
10.3459381770593));
#288696=CARTESIAN_POINT('Ctrl Pts',(-3.758382038874,111.312499999565,11.5671105274575));
#288697=CARTESIAN_POINT('Ctrl Pts',(-7.43200521958313E-14,111.462499999565,
12.7882828778556));
#288698=CARTESIAN_POINT('Ctrl Pts',(3.75838203887385,111.612499999564,11.5671105274575));
#288699=CARTESIAN_POINT('Ctrl Pts',(7.51676407774778,111.762499999563,10.3459381770593));
#288700=CARTESIAN_POINT('Ctrl Pts',(9.839571920479,111.912499999563,7.14886745759543));
#288701=CARTESIAN_POINT('Ctrl Pts',(12.1623797632102,112.062499999562,3.95179673813153));
#288702=CARTESIAN_POINT('Ctrl Pts',(12.1623797632102,112.212499999562,-1.489461944703E-15));
#288703=CARTESIAN_POINT('Ctrl Pts',(12.1623797632102,112.362499999561,-3.95179673813154));
#288704=CARTESIAN_POINT('Ctrl Pts',(9.839571920479,112.51249999956,-7.14886745759543));
#288705=CARTESIAN_POINT('Ctrl Pts',(7.51676407774778,112.66249999956,-10.3459381770593));
#288706=CARTESIAN_POINT('Ctrl Pts',(3.75838203887385,112.812499999559,-11.5671105274575));
#288707=CARTESIAN_POINT('Ctrl Pts',(-7.83161327702536E-14,112.962499999559,
-12.7882828778556));
#288708=CARTESIAN_POINT('Ctrl Pts',(-3.75838203887401,113.112499999558,
-11.5671105274575));
#288709=CARTESIAN_POINT('Ctrl Pts',(-7.51676407774793,113.262499999557,
-10.3459381770593));
#288710=CARTESIAN_POINT('Ctrl Pts',(-9.83957192047915,113.412499999557,
-7.14886745759543));
#288711=CARTESIAN_POINT('Ctrl Pts',(-12.1623797632104,113.562499999556,
-3.95179673813153));
#288712=CARTESIAN_POINT('Ctrl Pts',(-12.1623797632104,113.712499999556,
2.97892388940601E-15));
#288713=CARTESIAN_POINT('Ctrl Pts',(-12.1623797632104,113.862499999555,
3.95179673813154));
#288714=CARTESIAN_POINT('Ctrl Pts',(-9.83957192047915,114.012499999554,
7.14886745759543));
#288715=CARTESIAN_POINT('Ctrl Pts',(-7.51676407774793,114.162499999554,
10.3459381770593));
#288716=CARTESIAN_POINT('Ctrl Pts',(-3.758382038874,114.312499999553,11.5671105274575));
#288717=CARTESIAN_POINT('Ctrl Pts',(-7.60477614674932E-14,114.462499999553,
12.7882828778556));
#288718=CARTESIAN_POINT('Ctrl Pts',(3.75838203887385,114.612499999552,11.5671105274575));
#288719=CARTESIAN_POINT('Ctrl Pts',(7.51676407774778,114.762499999551,10.3459381770593));
#288720=CARTESIAN_POINT('Ctrl Pts',(9.839571920479,114.912499999551,7.14886745759543));
#288721=CARTESIAN_POINT('Ctrl Pts',(12.1623797632102,115.06249999955,3.95179673813153));
#288722=CARTESIAN_POINT('Ctrl Pts',(12.1623797632102,115.21249999955,-1.489461944703E-15));
#288723=CARTESIAN_POINT('Ctrl Pts',(12.1623797632102,115.362499999549,-3.95179673813154));
#288724=CARTESIAN_POINT('Ctrl Pts',(9.839571920479,115.512499999548,-7.14886745759543));
#288725=CARTESIAN_POINT('Ctrl Pts',(7.51676407774778,115.662499999548,-10.3459381770593));
#288726=CARTESIAN_POINT('Ctrl Pts',(3.75838203887385,115.812499999547,-11.5671105274575));
#288727=CARTESIAN_POINT('Ctrl Pts',(-8.00438420419154E-14,115.962499999547,
-12.7882828778556));
#288728=CARTESIAN_POINT('Ctrl Pts',(-3.75838203887401,116.112499999546,
-11.5671105274575));
#288729=CARTESIAN_POINT('Ctrl Pts',(-7.51676407774794,116.262499999545,
-10.3459381770593));
#288730=CARTESIAN_POINT('Ctrl Pts',(-9.83957192047916,116.412499999545,
-7.14886745759543));
#288731=CARTESIAN_POINT('Ctrl Pts',(-12.1623797632104,116.562499999544,
-3.95179673813153));
#288732=CARTESIAN_POINT('Ctrl Pts',(-12.1623797632104,116.712499999544,
2.97892388940601E-15));
#288733=CARTESIAN_POINT('Ctrl Pts',(-12.1623797632104,116.862499999543,
3.95179673813154));
#288734=CARTESIAN_POINT('Ctrl Pts',(-9.83957192047915,117.012499999542,
7.14886745759543));
#288735=CARTESIAN_POINT('Ctrl Pts',(-7.51676407774793,117.162499999542,
10.3459381770593));
#288736=CARTESIAN_POINT('Ctrl Pts',(-3.75838203887401,117.312499999541,
11.5671105274575));
#288737=CARTESIAN_POINT('Ctrl Pts',(-7.7775470739155E-14,117.462499999541,
12.7882828778556));
#288738=CARTESIAN_POINT('Ctrl Pts',(3.75838203887385,117.61249999954,11.5671105274575));
#288739=CARTESIAN_POINT('Ctrl Pts',(7.51676407774778,117.762499999539,10.3459381770593));
#288740=CARTESIAN_POINT('Ctrl Pts',(9.839571920479,117.912499999539,7.14886745759543));
#288741=CARTESIAN_POINT('Ctrl Pts',(12.1623797632102,118.062499999538,3.95179673813153));
#288742=CARTESIAN_POINT('Ctrl Pts',(12.1623797632102,118.212499999538,-1.489461944703E-15));
#288743=CARTESIAN_POINT('Ctrl Pts',(12.1623797632102,118.362499999537,-3.95179673813154));
#288744=CARTESIAN_POINT('Ctrl Pts',(9.83957192047899,118.512499999536,-7.14886745759543));
#288745=CARTESIAN_POINT('Ctrl Pts',(7.51676407774778,118.662499999536,-10.3459381770593));
#288746=CARTESIAN_POINT('Ctrl Pts',(3.75838203887385,118.812499999535,-11.5671105274575));
#288747=CARTESIAN_POINT('Ctrl Pts',(-8.17715513135773E-14,118.962499999535,
-12.7882828778556));
#288748=CARTESIAN_POINT('Ctrl Pts',(-3.75838203887401,119.112499999534,
-11.5671105274575));
#288749=CARTESIAN_POINT('Ctrl Pts',(-7.51676407774794,119.262499999533,
-10.3459381770593));
#288750=CARTESIAN_POINT('Ctrl Pts',(-9.83957192047916,119.412499999533,
-7.14886745759543));
#288751=CARTESIAN_POINT('Ctrl Pts',(-12.1623797632104,119.562499999532,
-3.95179673813153));
#288752=CARTESIAN_POINT('Ctrl Pts',(-12.1623797632104,119.712499999532,
2.97892388940601E-15));
#288753=CARTESIAN_POINT('Ctrl Pts',(-12.1623797632104,119.862499999531,
3.95179673813154));
#288754=CARTESIAN_POINT('Ctrl Pts',(-9.83957192047916,120.01249999953,7.14886745759543));
#288755=CARTESIAN_POINT('Ctrl Pts',(-7.51676407774794,120.16249999953,10.3459381770593));
#288756=CARTESIAN_POINT('Ctrl Pts',(-3.75838203887401,120.312499999529,
11.5671105274575));
#288757=CARTESIAN_POINT('Ctrl Pts',(-7.95031800108169E-14,120.462499999529,
12.7882828778556));
#288758=CARTESIAN_POINT('Ctrl Pts',(3.75838203887385,120.612499999528,11.5671105274575));
#288759=CARTESIAN_POINT('Ctrl Pts',(7.51676407774778,120.762499999527,10.3459381770593));
#288760=CARTESIAN_POINT('Ctrl Pts',(9.83957192047899,120.912499999527,7.14886745759543));
#288761=CARTESIAN_POINT('Ctrl Pts',(12.1623797632102,121.062499999526,3.95179673813153));
#288762=CARTESIAN_POINT('Ctrl Pts',(12.1623797632102,121.212499999526,-1.489461944703E-15));
#288763=CARTESIAN_POINT('Ctrl Pts',(12.1623797632102,121.362499999525,-3.95179673813154));
#288764=CARTESIAN_POINT('Ctrl Pts',(9.83957192047899,121.512499999524,-7.14886745759543));
#288765=CARTESIAN_POINT('Ctrl Pts',(7.51676407774777,121.662499999524,-10.3459381770593));
#288766=CARTESIAN_POINT('Ctrl Pts',(3.75838203887385,121.812499999523,-11.5671105274575));
#288767=CARTESIAN_POINT('Ctrl Pts',(-8.34992605852391E-14,121.962499999523,
-12.7882828778556));
#288768=CARTESIAN_POINT('Ctrl Pts',(-3.75838203887401,122.112499999522,
-11.5671105274575));
#288769=CARTESIAN_POINT('Ctrl Pts',(-7.51676407774794,122.262499999521,
-10.3459381770593));
#288770=CARTESIAN_POINT('Ctrl Pts',(-9.83957192047916,122.412499999521,
-7.14886745759543));
#288771=CARTESIAN_POINT('Ctrl Pts',(-12.1623797632104,122.56249999952,-3.95179673813153));
#288772=CARTESIAN_POINT('Ctrl Pts',(-12.1623797632104,122.71249999952,2.97892388940601E-15));
#288773=CARTESIAN_POINT('Ctrl Pts',(-12.1623797632104,122.862499999519,
3.95179673813154));
#288774=CARTESIAN_POINT('Ctrl Pts',(-9.83957192047916,123.012499999518,
7.14886745759543));
#288775=CARTESIAN_POINT('Ctrl Pts',(-7.51676407774794,123.162499999518,
10.3459381770593));
#288776=CARTESIAN_POINT('Ctrl Pts',(-3.75838203887401,123.312499999517,
11.5671105274575));
#288777=CARTESIAN_POINT('Ctrl Pts',(-8.12308892824787E-14,123.462499999517,
12.7882828778556));
#288778=CARTESIAN_POINT('Ctrl Pts',(3.75838203887385,123.612499999516,11.5671105274575));
#288779=CARTESIAN_POINT('Ctrl Pts',(7.51676407774778,123.762499999515,10.3459381770593));
#288780=CARTESIAN_POINT('Ctrl Pts',(9.83957192047899,123.912499999515,7.14886745759543));
#288781=CARTESIAN_POINT('Ctrl Pts',(12.1623797632102,124.062499999514,3.95179673813153));
#288782=CARTESIAN_POINT('Ctrl Pts',(12.1623797632102,124.212499999514,-1.489461944703E-15));
#288783=CARTESIAN_POINT('Ctrl Pts',(12.1623797632102,124.362499999513,-3.95179673813154));
#288784=CARTESIAN_POINT('Ctrl Pts',(9.83957192047899,124.512499999512,-7.14886745759543));
#288785=CARTESIAN_POINT('Ctrl Pts',(7.51676407774777,124.662499999512,-10.3459381770593));
#288786=CARTESIAN_POINT('Ctrl Pts',(3.75838203887384,124.812499999511,-11.5671105274575));
#288787=CARTESIAN_POINT('Ctrl Pts',(-8.52269698569009E-14,124.962499999511,
-12.7882828778556));
#288788=CARTESIAN_POINT('Ctrl Pts',(-3.75838203887401,125.11249999951,-11.5671105274575));
#288789=CARTESIAN_POINT('Ctrl Pts',(-7.51676407774794,125.262499999509,
-10.3459381770593));
#288790=CARTESIAN_POINT('Ctrl Pts',(-9.83957192047916,125.412499999509,
-7.14886745759543));
#288791=CARTESIAN_POINT('Ctrl Pts',(-12.1623797632104,125.562499999508,
-3.95179673813153));
#288792=CARTESIAN_POINT('Ctrl Pts',(-12.1623797632104,125.712499999508,
2.97892388940601E-15));
#288793=CARTESIAN_POINT('Ctrl Pts',(-12.1623797632104,125.862499999507,
3.95179673813154));
#288794=CARTESIAN_POINT('Ctrl Pts',(-9.83957192047916,126.012499999506,
7.14886745759543));
#288795=CARTESIAN_POINT('Ctrl Pts',(-7.51676407774794,126.162499999506,
10.3459381770593));
#288796=CARTESIAN_POINT('Ctrl Pts',(-3.75838203887401,126.312499999505,
11.5671105274575));
#288797=CARTESIAN_POINT('Ctrl Pts',(-8.29585985541405E-14,126.462499999505,
12.7882828778556));
#288798=CARTESIAN_POINT('Ctrl Pts',(3.75838203887385,126.612499999504,11.5671105274575));
#288799=CARTESIAN_POINT('Ctrl Pts',(7.51676407774777,126.762499999503,10.3459381770593));
#288800=CARTESIAN_POINT('Ctrl Pts',(9.83957192047899,126.912499999503,7.14886745759543));
#288801=CARTESIAN_POINT('Ctrl Pts',(12.1623797632102,127.062499999502,3.95179673813153));
#288802=CARTESIAN_POINT('Ctrl Pts',(12.1623797632102,127.212499999502,-1.489461944703E-15));
#288803=CARTESIAN_POINT('Ctrl Pts',(12.1623797632102,127.362499999501,-3.95179673813154));
#288804=CARTESIAN_POINT('Ctrl Pts',(9.83957192047899,127.5124999995,-7.14886745759543));
#288805=CARTESIAN_POINT('Ctrl Pts',(7.51676407774777,127.6624999995,-10.3459381770593));
#288806=CARTESIAN_POINT('Ctrl Pts',(3.75838203887384,127.812499999499,-11.5671105274575));
#288807=CARTESIAN_POINT('Ctrl Pts',(-8.69546791285628E-14,127.962499999499,
-12.7882828778556));
#288808=CARTESIAN_POINT('Ctrl Pts',(-3.75838203887402,128.112499999498,
-11.5671105274575));
#288809=CARTESIAN_POINT('Ctrl Pts',(-7.51676407774795,128.262499999497,
-10.3459381770593));
#288810=CARTESIAN_POINT('Ctrl Pts',(-9.83957192047916,128.412499999497,
-7.14886745759543));
#288811=CARTESIAN_POINT('Ctrl Pts',(-12.1623797632104,128.562499999496,
-3.95179673813153));
#288812=CARTESIAN_POINT('Ctrl Pts',(-12.1623797632104,128.712499999496,
2.97892388940601E-15));
#288813=CARTESIAN_POINT('Ctrl Pts',(-12.1623797632104,128.862499999495,
3.95179673813154));
#288814=CARTESIAN_POINT('Ctrl Pts',(-9.83957192047916,129.012499999494,
7.14886745759543));
#288815=CARTESIAN_POINT('Ctrl Pts',(-7.51676407774794,129.162499999494,
10.3459381770593));
#288816=CARTESIAN_POINT('Ctrl Pts',(-3.75838203887401,129.312499999493,
11.5671105274575));
#288817=CARTESIAN_POINT('Ctrl Pts',(-8.46863078258024E-14,129.462499999493,
12.7882828778556));
#288818=CARTESIAN_POINT('Ctrl Pts',(3.75838203887384,129.612499999492,11.5671105274575));
#288819=CARTESIAN_POINT('Ctrl Pts',(7.51676407774777,129.762499999491,10.3459381770593));
#288820=CARTESIAN_POINT('Ctrl Pts',(9.83957192047899,129.912499999491,7.14886745759543));
#288821=CARTESIAN_POINT('Ctrl Pts',(12.1623797632102,130.06249999949,3.95179673813153));
#288822=CARTESIAN_POINT('Ctrl Pts',(12.1623797632102,130.21249999949,-1.489461944703E-15));
#288823=CARTESIAN_POINT('Ctrl Pts',(12.1623797632102,130.362499999489,-3.95179673813154));
#288824=CARTESIAN_POINT('Ctrl Pts',(9.83957192047899,130.512499999488,-7.14886745759543));
#288825=CARTESIAN_POINT('Ctrl Pts',(7.51676407774777,130.662499999488,-10.3459381770593));
#288826=CARTESIAN_POINT('Ctrl Pts',(3.75838203887384,130.812499999487,-11.5671105274575));
#288827=CARTESIAN_POINT('Ctrl Pts',(-8.86823884002247E-14,130.962499999487,
-12.7882828778556));
#288828=CARTESIAN_POINT('Ctrl Pts',(-3.75838203887402,131.112499999486,
-11.5671105274575));
#288829=CARTESIAN_POINT('Ctrl Pts',(-7.51676407774795,131.262499999485,
-10.3459381770593));
#288830=CARTESIAN_POINT('Ctrl Pts',(-9.83957192047916,131.412499999485,
-7.14886745759543));
#288831=CARTESIAN_POINT('Ctrl Pts',(-12.1623797632104,131.562499999484,
-3.95179673813153));
#288832=CARTESIAN_POINT('Ctrl Pts',(-12.1623797632104,131.712499999484,
2.97892388940601E-15));
#288833=CARTESIAN_POINT('Ctrl Pts',(-12.1623797632104,131.862499999483,
3.95179673813154));
#288834=CARTESIAN_POINT('Ctrl Pts',(-9.83957192047916,132.012499999482,
7.14886745759543));
#288835=CARTESIAN_POINT('Ctrl Pts',(-7.51676407774795,132.162499999482,
10.3459381770593));
#288836=CARTESIAN_POINT('Ctrl Pts',(-3.75838203887402,132.312499999481,
11.5671105274575));
#288837=CARTESIAN_POINT('Ctrl Pts',(-8.64140170974642E-14,132.462499999481,
12.7882828778556));
#288838=CARTESIAN_POINT('Ctrl Pts',(3.75838203887384,132.61249999948,11.5671105274575));
#288839=CARTESIAN_POINT('Ctrl Pts',(7.51676407774777,132.762499999479,10.3459381770593));
#288840=CARTESIAN_POINT('Ctrl Pts',(9.83957192047899,132.912499999479,7.14886745759543));
#288841=CARTESIAN_POINT('Ctrl Pts',(12.1623797632102,133.062499999478,3.95179673813153));
#288842=CARTESIAN_POINT('Ctrl Pts',(12.1623797632102,133.212499999478,-1.489461944703E-15));
#288843=CARTESIAN_POINT('Ctrl Pts',(12.1623797632102,133.362499999477,-3.95179673813154));
#288844=CARTESIAN_POINT('Ctrl Pts',(9.83957192047898,133.512499999476,-7.14886745759543));
#288845=CARTESIAN_POINT('Ctrl Pts',(7.51676407774777,133.662499999476,-10.3459381770593));
#288846=CARTESIAN_POINT('Ctrl Pts',(3.75838203887384,133.812499999475,-11.5671105274575));
#288847=CARTESIAN_POINT('Ctrl Pts',(-9.04100976718865E-14,133.962499999475,
-12.7882828778556));
#288848=CARTESIAN_POINT('Ctrl Pts',(-3.75838203887402,134.112499999474,
-11.5671105274575));
#288849=CARTESIAN_POINT('Ctrl Pts',(-7.51676407774795,134.262499999473,
-10.3459381770593));
#288850=CARTESIAN_POINT('Ctrl Pts',(-9.83957192047917,134.412499999473,
-7.14886745759543));
#288851=CARTESIAN_POINT('Ctrl Pts',(-12.1623797632104,134.562499999472,
-3.95179673813153));
#288852=CARTESIAN_POINT('Ctrl Pts',(-12.1623797632104,134.712499999472,
2.97892388940601E-15));
#288853=CARTESIAN_POINT('Ctrl Pts',(-12.1623797632104,134.862499999471,
3.95179673813154));
#288854=CARTESIAN_POINT('Ctrl Pts',(-9.83957192047916,135.01249999947,7.14886745759543));
#288855=CARTESIAN_POINT('Ctrl Pts',(-7.51676407774795,135.16249999947,10.3459381770593));
#288856=CARTESIAN_POINT('Ctrl Pts',(-3.75838203887402,135.312499999469,
11.5671105274575));
#288857=CARTESIAN_POINT('Ctrl Pts',(-8.8141726369126E-14,135.462499999469,
12.7882828778556));
#288858=CARTESIAN_POINT('Ctrl Pts',(3.75838203887384,135.612499999468,11.5671105274575));
#288859=CARTESIAN_POINT('Ctrl Pts',(7.51676407774777,135.762499999467,10.3459381770593));
#288860=CARTESIAN_POINT('Ctrl Pts',(9.83957192047898,135.912499999467,7.14886745759543));
#288861=CARTESIAN_POINT('Ctrl Pts',(12.1623797632102,136.062499999466,3.95179673813153));
#288862=CARTESIAN_POINT('Ctrl Pts',(12.1623797632102,136.212499999466,-1.489461944703E-15));
#288863=CARTESIAN_POINT('Ctrl Pts',(12.1623797632102,136.362499999465,-3.95179673813154));
#288864=CARTESIAN_POINT('Ctrl Pts',(9.83957192047898,136.512499999464,-7.14886745759543));
#288865=CARTESIAN_POINT('Ctrl Pts',(7.51676407774777,136.662499999464,-10.3459381770593));
#288866=CARTESIAN_POINT('Ctrl Pts',(3.75838203887384,136.812499999463,-11.5671105274575));
#288867=CARTESIAN_POINT('Ctrl Pts',(-9.21378069435483E-14,136.962499999463,
-12.7882828778556));
#288868=CARTESIAN_POINT('Ctrl Pts',(-3.75838203887402,137.112499999462,
-11.5671105274575));
#288869=CARTESIAN_POINT('Ctrl Pts',(-7.51676407774795,137.262499999461,
-10.3459381770593));
#288870=CARTESIAN_POINT('Ctrl Pts',(-9.83957192047917,137.412499999461,
-7.14886745759543));
#288871=CARTESIAN_POINT('Ctrl Pts',(-12.1623797632104,137.56249999946,-3.95179673813153));
#288872=CARTESIAN_POINT('Ctrl Pts',(-12.1623797632104,137.71249999946,2.97892388940601E-15));
#288873=CARTESIAN_POINT('Ctrl Pts',(-12.1623797632104,137.862499999459,
3.95179673813154));
#288874=CARTESIAN_POINT('Ctrl Pts',(-9.83957192047917,138.012499999458,
7.14886745759543));
#288875=CARTESIAN_POINT('Ctrl Pts',(-7.51676407774795,138.162499999458,
10.3459381770593));
#288876=CARTESIAN_POINT('Ctrl Pts',(-3.75838203887402,138.312499999457,
11.5671105274575));
#288877=CARTESIAN_POINT('Ctrl Pts',(-8.98694356407879E-14,138.462499999457,
12.7882828778556));
#288878=CARTESIAN_POINT('Ctrl Pts',(3.75838203887384,138.612499999456,11.5671105274575));
#288879=CARTESIAN_POINT('Ctrl Pts',(7.51676407774777,138.762499999455,10.3459381770593));
#288880=CARTESIAN_POINT('Ctrl Pts',(9.83957192047898,138.912499999455,7.14886745759543));
#288881=CARTESIAN_POINT('Ctrl Pts',(12.1623797632102,139.062499999454,3.95179673813153));
#288882=CARTESIAN_POINT('Ctrl Pts',(12.1623797632102,139.212499999454,-1.489461944703E-15));
#288883=CARTESIAN_POINT('Ctrl Pts',(12.1623797632102,139.362499999453,-3.95179673813154));
#288884=CARTESIAN_POINT('Ctrl Pts',(9.83957192047898,139.512499999452,-7.14886745759543));
#288885=CARTESIAN_POINT('Ctrl Pts',(7.51676407774776,139.662499999452,-10.3459381770593));
#288886=CARTESIAN_POINT('Ctrl Pts',(3.75838203887384,139.812499999451,-11.5671105274575));
#288887=CARTESIAN_POINT('Ctrl Pts',(-9.38655162152102E-14,139.962499999451,
-12.7882828778556));
#288888=CARTESIAN_POINT('Ctrl Pts',(-3.75838203887402,140.11249999945,-11.5671105274575));
#288889=CARTESIAN_POINT('Ctrl Pts',(-7.51676407774795,140.262499999449,
-10.3459381770593));
#288890=CARTESIAN_POINT('Ctrl Pts',(-9.83957192047917,140.412499999449,
-7.14886745759543));
#288891=CARTESIAN_POINT('Ctrl Pts',(-12.1623797632104,140.562499999448,
-3.95179673813153));
#288892=CARTESIAN_POINT('Ctrl Pts',(-12.1623797632104,140.712499999448,
2.97892388940601E-15));
#288893=CARTESIAN_POINT('Ctrl Pts',(-12.1623797632104,140.862499999447,
3.95179673813154));
#288894=CARTESIAN_POINT('Ctrl Pts',(-9.83957192047917,141.012499999446,
7.14886745759543));
#288895=CARTESIAN_POINT('Ctrl Pts',(-7.51676407774795,141.162499999446,
10.3459381770593));
#288896=CARTESIAN_POINT('Ctrl Pts',(-3.75838203887402,141.312499999445,
11.5671105274575));
#288897=CARTESIAN_POINT('Ctrl Pts',(-9.15971449124498E-14,141.462499999445,
12.7882828778556));
#288898=CARTESIAN_POINT('Ctrl Pts',(3.75838203887384,141.612499999444,11.5671105274575));
#288899=CARTESIAN_POINT('Ctrl Pts',(7.51676407774777,141.762499999443,10.3459381770593));
#288900=CARTESIAN_POINT('Ctrl Pts',(9.83957192047898,141.912499999443,7.14886745759543));
#288901=CARTESIAN_POINT('Ctrl Pts',(12.1623797632102,142.062499999442,3.95179673813153));
#288902=CARTESIAN_POINT('Ctrl Pts',(12.1623797632102,142.212499999442,-1.489461944703E-15));
#288903=CARTESIAN_POINT('Ctrl Pts',(12.1623797632102,142.362499999441,-3.95179673813154));
#288904=CARTESIAN_POINT('Ctrl Pts',(9.83957192047898,142.51249999944,-7.14886745759543));
#288905=CARTESIAN_POINT('Ctrl Pts',(7.51676407774776,142.66249999944,-10.3459381770593));
#288906=CARTESIAN_POINT('Ctrl Pts',(3.75838203887383,142.812499999439,-11.5671105274575));
#288907=CARTESIAN_POINT('Ctrl Pts',(-9.5593225486872E-14,142.962499999439,
-12.7882828778556));
#288908=CARTESIAN_POINT('Ctrl Pts',(-3.75838203887402,143.112499999438,
-11.5671105274575));
#288909=CARTESIAN_POINT('Ctrl Pts',(-7.51676407774795,143.262499999437,
-10.3459381770593));
#288910=CARTESIAN_POINT('Ctrl Pts',(-9.83957192047917,143.412499999437,
-7.14886745759543));
#288911=CARTESIAN_POINT('Ctrl Pts',(-12.1623797632104,143.562499999436,
-3.95179673813153));
#288912=CARTESIAN_POINT('Ctrl Pts',(-12.1623797632104,143.712499999436,
2.97892388940601E-15));
#288913=CARTESIAN_POINT('Ctrl Pts',(-12.1623797632104,143.862499999435,
3.95179673813154));
#288914=CARTESIAN_POINT('Ctrl Pts',(-9.83957192047917,144.012499999434,
7.14886745759543));
#288915=CARTESIAN_POINT('Ctrl Pts',(-7.51676407774795,144.162499999434,
10.3459381770593));
#288916=CARTESIAN_POINT('Ctrl Pts',(-3.75838203887402,144.312499999433,
11.5671105274575));
#288917=CARTESIAN_POINT('Ctrl Pts',(-9.33248541841116E-14,144.462499999433,
12.7882828778556));
#288918=CARTESIAN_POINT('Ctrl Pts',(3.75838203887384,144.612499999432,11.5671105274575));
#288919=CARTESIAN_POINT('Ctrl Pts',(7.51676407774776,144.762499999431,10.3459381770593));
#288920=CARTESIAN_POINT('Ctrl Pts',(9.83957192047898,144.912499999431,7.14886745759543));
#288921=CARTESIAN_POINT('Ctrl Pts',(12.1623797632102,145.06249999943,3.95179673813153));
#288922=CARTESIAN_POINT('Ctrl Pts',(12.1623797632102,145.21249999943,-1.489461944703E-15));
#288923=CARTESIAN_POINT('Ctrl Pts',(12.1623797632102,145.362499999429,-3.95179673813154));
#288924=CARTESIAN_POINT('Ctrl Pts',(9.83957192047898,145.512499999428,-7.14886745759543));
#288925=CARTESIAN_POINT('Ctrl Pts',(7.51676407774776,145.662499999428,-10.3459381770593));
#288926=CARTESIAN_POINT('Ctrl Pts',(3.75838203887383,145.812499999427,-11.5671105274575));
#288927=CARTESIAN_POINT('Ctrl Pts',(-9.73209347585338E-14,145.962499999427,
-12.7882828778556));
#288928=CARTESIAN_POINT('Ctrl Pts',(-3.75838203887403,146.112499999426,
-11.5671105274575));
#288929=CARTESIAN_POINT('Ctrl Pts',(-7.51676407774795,146.262499999425,
-10.3459381770593));
#288930=CARTESIAN_POINT('Ctrl Pts',(-9.83957192047917,146.412499999425,
-7.14886745759543));
#288931=CARTESIAN_POINT('Ctrl Pts',(-12.1623797632104,146.562499999424,
-3.95179673813153));
#288932=CARTESIAN_POINT('Ctrl Pts',(-12.1623797632104,146.712499999424,
2.97892388940601E-15));
#288933=CARTESIAN_POINT('Ctrl Pts',(-12.1623797632104,146.862499999423,
3.95179673813154));
#288934=CARTESIAN_POINT('Ctrl Pts',(-9.83957192047917,147.012499999422,
7.14886745759543));
#288935=CARTESIAN_POINT('Ctrl Pts',(-7.51676407774795,147.162499999422,
10.3459381770593));
#288936=CARTESIAN_POINT('Ctrl Pts',(-3.75838203887402,147.312499999421,
11.5671105274575));
#288937=CARTESIAN_POINT('Ctrl Pts',(-9.50525634557734E-14,147.462499999421,
12.7882828778556));
#288938=CARTESIAN_POINT('Ctrl Pts',(3.75838203887383,147.61249999942,11.5671105274575));
#288939=CARTESIAN_POINT('Ctrl Pts',(7.51676407774776,147.762499999419,10.3459381770593));
#288940=CARTESIAN_POINT('Ctrl Pts',(9.83957192047898,147.912499999419,7.14886745759543));
#288941=CARTESIAN_POINT('Ctrl Pts',(12.1623797632102,148.062499999418,3.95179673813153));
#288942=CARTESIAN_POINT('Ctrl Pts',(12.1623797632102,148.212499999418,-1.489461944703E-15));
#288943=CARTESIAN_POINT('Ctrl Pts',(12.1623797632102,148.362499999417,-3.95179673813154));
#288944=CARTESIAN_POINT('Ctrl Pts',(9.83957192047898,148.512499999416,-7.14886745759543));
#288945=CARTESIAN_POINT('Ctrl Pts',(7.51676407774776,148.662499999416,-10.3459381770593));
#288946=CARTESIAN_POINT('Ctrl Pts',(3.75838203887383,148.812499999415,-11.5671105274575));
#288947=CARTESIAN_POINT('Ctrl Pts',(-9.90486440301957E-14,148.962499999415,
-12.7882828778556));
#288948=CARTESIAN_POINT('Ctrl Pts',(-3.75838203887403,149.112499999414,
-11.5671105274575));
#288949=CARTESIAN_POINT('Ctrl Pts',(-7.51676407774795,149.262499999413,
-10.3459381770593));
#288950=CARTESIAN_POINT('Ctrl Pts',(-9.83957192047917,149.412499999413,
-7.14886745759543));
#288951=CARTESIAN_POINT('Ctrl Pts',(-12.1623797632104,149.562499999412,
-3.95179673813153));
#288952=CARTESIAN_POINT('Ctrl Pts',(-12.1623797632104,149.712499999412,
2.97892388940601E-15));
#288953=CARTESIAN_POINT('Ctrl Pts',(-12.1623797632104,149.862499999411,
3.95179673813154));
#288954=CARTESIAN_POINT('Ctrl Pts',(-9.83957192047917,150.01249999941,7.14886745759543));
#288955=CARTESIAN_POINT('Ctrl Pts',(-7.51676407774795,150.16249999941,10.3459381770593));
#288956=CARTESIAN_POINT('Ctrl Pts',(-3.75838203887403,150.312499999409,
11.5671105274575));
#288957=CARTESIAN_POINT('Ctrl Pts',(-9.67802727274353E-14,150.462499999409,
12.7882828778556));
#288958=CARTESIAN_POINT('Ctrl Pts',(3.75838203887383,150.612499999408,11.5671105274575));
#288959=CARTESIAN_POINT('Ctrl Pts',(7.51676407774776,150.762499999407,10.3459381770593));
#288960=CARTESIAN_POINT('Ctrl Pts',(9.83957192047898,150.912499999407,7.14886745759543));
#288961=CARTESIAN_POINT('Ctrl Pts',(12.1623797632102,151.062499999406,3.95179673813153));
#288962=CARTESIAN_POINT('Ctrl Pts',(12.1623797632102,151.212499999406,-1.489461944703E-15));
#288963=CARTESIAN_POINT('Ctrl Pts',(12.1623797632102,151.362499999405,-3.95179673813154));
#288964=CARTESIAN_POINT('Ctrl Pts',(9.83957192047897,151.512499999404,-7.14886745759543));
#288965=CARTESIAN_POINT('Ctrl Pts',(7.51676407774776,151.662499999404,-10.3459381770593));
#288966=CARTESIAN_POINT('Ctrl Pts',(3.75838203887383,151.812499999403,-11.5671105274575));
#288967=CARTESIAN_POINT('Ctrl Pts',(-1.00776353301858E-13,151.962499999403,
-12.7882828778556));
#288968=CARTESIAN_POINT('Ctrl Pts',(-3.75838203887403,152.112499999402,
-11.5671105274575));
#288969=CARTESIAN_POINT('Ctrl Pts',(-10.0514428414942,-2.06874999998125,
2.46189346052968E-15));
#288970=CARTESIAN_POINT('Ctrl Pts',(-10.0514428414942,-1.91874999998185,
3.26591175476071));
#288971=CARTESIAN_POINT('Ctrl Pts',(-8.1317880767572,-1.76874999998245,
5.90808986649102));
#288972=CARTESIAN_POINT('Ctrl Pts',(-6.21213331202023,-1.61874999998305,
8.55026797822134));
#288973=CARTESIAN_POINT('Ctrl Pts',(-3.10606665601012,-1.46874999998365,
9.5594902125713));
#288974=CARTESIAN_POINT('Ctrl Pts',(-9.77671023785295E-15,-1.31874999998425,
10.5687124469213));
#288975=CARTESIAN_POINT('Ctrl Pts',(3.1060666560101,-1.16874999998485,9.5594902125713));
#288976=CARTESIAN_POINT('Ctrl Pts',(6.21213331202021,-1.01874999998544,
8.55026797822134));
#288977=CARTESIAN_POINT('Ctrl Pts',(8.13178807675718,-0.868749999986043,
5.90808986649102));
#288978=CARTESIAN_POINT('Ctrl Pts',(10.0514428414942,-0.718749999986641,
3.2659117547607));
#288979=CARTESIAN_POINT('Ctrl Pts',(10.0514428414942,-0.568749999987242,
-1.23094673026484E-15));
#288980=CARTESIAN_POINT('Ctrl Pts',(10.0514428414942,-0.418749999987842,
-3.26591175476071));
#288981=CARTESIAN_POINT('Ctrl Pts',(8.13178807675718,-0.268749999988443,
-5.90808986649102));
#288982=CARTESIAN_POINT('Ctrl Pts',(6.2121333120202,-0.118749999989044,
-8.55026797822134));
#288983=CARTESIAN_POINT('Ctrl Pts',(3.10606665601009,0.0312500000103543,
-9.5594902125713));
#288984=CARTESIAN_POINT('Ctrl Pts',(-1.322915284753E-14,0.181250000009752,
-10.5687124469213));
#288985=CARTESIAN_POINT('Ctrl Pts',(-3.10606665601012,0.331250000009151,
-9.5594902125713));
#288986=CARTESIAN_POINT('Ctrl Pts',(-6.21213331202023,0.481250000008549,
-8.55026797822134));
#288987=CARTESIAN_POINT('Ctrl Pts',(-8.1317880767572,0.631250000007948,
-5.90808986649102));
#288988=CARTESIAN_POINT('Ctrl Pts',(-10.0514428414942,0.781250000007346,
-3.2659117547607));
#288989=CARTESIAN_POINT('Ctrl Pts',(-10.0514428414942,0.931250000006746,
2.46189346052968E-15));
#288990=CARTESIAN_POINT('Ctrl Pts',(-10.0514428414942,1.08125000000615,
3.26591175476071));
#288991=CARTESIAN_POINT('Ctrl Pts',(-8.1317880767572,1.23125000000555,5.90808986649102));
#288992=CARTESIAN_POINT('Ctrl Pts',(-6.21213331202023,1.38125000000495,
8.55026797822134));
#288993=CARTESIAN_POINT('Ctrl Pts',(-3.10606665601012,1.53125000000435,
9.5594902125713));
#288994=CARTESIAN_POINT('Ctrl Pts',(-1.15044195095148E-14,1.68125000000375,
10.5687124469213));
#288995=CARTESIAN_POINT('Ctrl Pts',(3.1060666560101,1.83125000000315,9.5594902125713));
#288996=CARTESIAN_POINT('Ctrl Pts',(6.2121333120202,1.98125000000256,8.55026797822134));
#288997=CARTESIAN_POINT('Ctrl Pts',(8.13178807675718,2.13125000000196,5.90808986649102));
#288998=CARTESIAN_POINT('Ctrl Pts',(10.0514428414942,2.28125000000136,3.2659117547607));
#288999=CARTESIAN_POINT('Ctrl Pts',(10.0514428414942,2.43125000000076,-1.23094673026484E-15));
#289000=CARTESIAN_POINT('Ctrl Pts',(10.0514428414942,2.58125000000016,-3.26591175476071));
#289001=CARTESIAN_POINT('Ctrl Pts',(8.13178807675718,2.73124999999956,-5.90808986649102));
#289002=CARTESIAN_POINT('Ctrl Pts',(6.2121333120202,2.88124999999896,-8.55026797822134));
#289003=CARTESIAN_POINT('Ctrl Pts',(3.10606665601009,3.03124999999835,-9.5594902125713));
#289004=CARTESIAN_POINT('Ctrl Pts',(-1.49568621191919E-14,3.18124999999775,
-10.5687124469213));
#289005=CARTESIAN_POINT('Ctrl Pts',(-3.10606665601012,3.33124999999715,
-9.5594902125713));
#289006=CARTESIAN_POINT('Ctrl Pts',(-6.21213331202023,3.48124999999655,
-8.55026797822134));
#289007=CARTESIAN_POINT('Ctrl Pts',(-8.13178807675721,3.63124999999595,
-5.90808986649102));
#289008=CARTESIAN_POINT('Ctrl Pts',(-10.0514428414942,3.78124999999535,
-3.2659117547607));
#289009=CARTESIAN_POINT('Ctrl Pts',(-10.0514428414942,3.93124999999475,
2.46189346052968E-15));
#289010=CARTESIAN_POINT('Ctrl Pts',(-10.0514428414942,4.08124999999415,
3.26591175476071));
#289011=CARTESIAN_POINT('Ctrl Pts',(-8.13178807675721,4.23124999999355,
5.90808986649102));
#289012=CARTESIAN_POINT('Ctrl Pts',(-6.21213331202023,4.38124999999295,
8.55026797822134));
#289013=CARTESIAN_POINT('Ctrl Pts',(-3.10606665601012,4.53124999999235,
9.5594902125713));
#289014=CARTESIAN_POINT('Ctrl Pts',(-1.32321287811766E-14,4.68124999999175,
10.5687124469213));
#289015=CARTESIAN_POINT('Ctrl Pts',(3.10606665601009,4.83124999999115,9.5594902125713));
#289016=CARTESIAN_POINT('Ctrl Pts',(6.2121333120202,4.98124999999055,8.55026797822134));
#289017=CARTESIAN_POINT('Ctrl Pts',(8.13178807675718,5.13124999998996,5.90808986649102));
#289018=CARTESIAN_POINT('Ctrl Pts',(10.0514428414942,5.28124999998936,3.2659117547607));
#289019=CARTESIAN_POINT('Ctrl Pts',(10.0514428414941,5.43124999998876,-1.23094673026484E-15));
#289020=CARTESIAN_POINT('Ctrl Pts',(10.0514428414941,5.58124999998816,-3.26591175476071));
#289021=CARTESIAN_POINT('Ctrl Pts',(8.13178807675717,5.73124999998756,-5.90808986649102));
#289022=CARTESIAN_POINT('Ctrl Pts',(6.2121333120202,5.88124999998695,-8.55026797822134));
#289023=CARTESIAN_POINT('Ctrl Pts',(3.10606665601009,6.03124999998635,-9.5594902125713));
#289024=CARTESIAN_POINT('Ctrl Pts',(-1.66845713908537E-14,6.18124999998575,
-10.5687124469213));
#289025=CARTESIAN_POINT('Ctrl Pts',(-3.10606665601012,6.33124999998515,
-9.5594902125713));
#289026=CARTESIAN_POINT('Ctrl Pts',(-6.21213331202023,6.48124999998455,
-8.55026797822134));
#289027=CARTESIAN_POINT('Ctrl Pts',(-8.13178807675721,6.63124999998395,
-5.90808986649102));
#289028=CARTESIAN_POINT('Ctrl Pts',(-10.0514428414942,6.78124999998335,
-3.2659117547607));
#289029=CARTESIAN_POINT('Ctrl Pts',(-10.0514428414942,6.93124999998275,
2.46189346052968E-15));
#289030=CARTESIAN_POINT('Ctrl Pts',(-10.0514428414942,7.08124999998215,
3.26591175476071));
#289031=CARTESIAN_POINT('Ctrl Pts',(-8.13178807675721,7.23124999998155,
5.90808986649102));
#289032=CARTESIAN_POINT('Ctrl Pts',(-6.21213331202023,7.38124999998095,
8.55026797822134));
#289033=CARTESIAN_POINT('Ctrl Pts',(-3.10606665601012,7.53124999998035,
9.5594902125713));
#289034=CARTESIAN_POINT('Ctrl Pts',(-1.49598380528385E-14,7.68124999997975,
10.5687124469213));
#289035=CARTESIAN_POINT('Ctrl Pts',(3.10606665601009,7.83124999997915,9.5594902125713));
#289036=CARTESIAN_POINT('Ctrl Pts',(6.2121333120202,7.98124999997856,8.55026797822134));
#289037=CARTESIAN_POINT('Ctrl Pts',(8.13178807675717,8.13124999997796,5.90808986649102));
#289038=CARTESIAN_POINT('Ctrl Pts',(10.0514428414942,8.28124999997736,3.2659117547607));
#289039=CARTESIAN_POINT('Ctrl Pts',(10.0514428414941,8.43124999997676,-1.23094673026484E-15));
#289040=CARTESIAN_POINT('Ctrl Pts',(10.0514428414941,8.58124999997616,-3.26591175476071));
#289041=CARTESIAN_POINT('Ctrl Pts',(8.13178807675717,8.73124999997556,-5.90808986649102));
#289042=CARTESIAN_POINT('Ctrl Pts',(6.2121333120202,8.88124999997496,-8.55026797822134));
#289043=CARTESIAN_POINT('Ctrl Pts',(3.10606665601009,9.03124999997436,-9.5594902125713));
#289044=CARTESIAN_POINT('Ctrl Pts',(-1.84122806625156E-14,9.18124999997375,
-10.5687124469213));
#289045=CARTESIAN_POINT('Ctrl Pts',(-3.10606665601013,9.33124999997315,
-9.5594902125713));
#289046=CARTESIAN_POINT('Ctrl Pts',(-6.21213331202023,9.48124999997255,
-8.55026797822134));
#289047=CARTESIAN_POINT('Ctrl Pts',(-8.13178807675721,9.63124999997195,
-5.90808986649102));
#289048=CARTESIAN_POINT('Ctrl Pts',(-10.0514428414942,9.78124999997135,
-3.2659117547607));
#289049=CARTESIAN_POINT('Ctrl Pts',(-10.0514428414942,9.93124999997075,
2.46189346052968E-15));
#289050=CARTESIAN_POINT('Ctrl Pts',(-10.0514428414942,10.0812499999701,
3.26591175476071));
#289051=CARTESIAN_POINT('Ctrl Pts',(-8.13178807675721,10.2312499999695,
5.90808986649102));
#289052=CARTESIAN_POINT('Ctrl Pts',(-6.21213331202023,10.3812499999689,
8.55026797822134));
#289053=CARTESIAN_POINT('Ctrl Pts',(-3.10606665601012,10.5312499999684,
9.5594902125713));
#289054=CARTESIAN_POINT('Ctrl Pts',(-1.66875473245003E-14,10.6812499999678,
10.5687124469213));
#289055=CARTESIAN_POINT('Ctrl Pts',(3.10606665601009,10.8312499999672,9.5594902125713));
#289056=CARTESIAN_POINT('Ctrl Pts',(6.2121333120202,10.9812499999666,8.55026797822134));
#289057=CARTESIAN_POINT('Ctrl Pts',(8.13178807675717,11.131249999966,5.90808986649102));
#289058=CARTESIAN_POINT('Ctrl Pts',(10.0514428414941,11.2812499999654,3.2659117547607));
#289059=CARTESIAN_POINT('Ctrl Pts',(10.0514428414941,11.4312499999648,-1.23094673026484E-15));
#289060=CARTESIAN_POINT('Ctrl Pts',(10.0514428414941,11.5812499999642,-3.26591175476071));
#289061=CARTESIAN_POINT('Ctrl Pts',(8.13178807675717,11.7312499999636,-5.90808986649102));
#289062=CARTESIAN_POINT('Ctrl Pts',(6.2121333120202,11.881249999963,-8.55026797822134));
#289063=CARTESIAN_POINT('Ctrl Pts',(3.10606665601009,12.0312499999624,-9.5594902125713));
#289064=CARTESIAN_POINT('Ctrl Pts',(-2.01399899341774E-14,12.1812499999618,
-10.5687124469213));
#289065=CARTESIAN_POINT('Ctrl Pts',(-3.10606665601013,12.3312499999612,
-9.5594902125713));
#289066=CARTESIAN_POINT('Ctrl Pts',(-6.21213331202024,12.4812499999605,
-8.55026797822134));
#289067=CARTESIAN_POINT('Ctrl Pts',(-8.13178807675721,12.6312499999599,
-5.90808986649102));
#289068=CARTESIAN_POINT('Ctrl Pts',(-10.0514428414942,12.7812499999593,
-3.2659117547607));
#289069=CARTESIAN_POINT('Ctrl Pts',(-10.0514428414942,12.9312499999587,
2.46189346052968E-15));
#289070=CARTESIAN_POINT('Ctrl Pts',(-10.0514428414942,13.0812499999581,
3.26591175476071));
#289071=CARTESIAN_POINT('Ctrl Pts',(-8.13178807675721,13.2312499999575,
5.90808986649102));
#289072=CARTESIAN_POINT('Ctrl Pts',(-6.21213331202023,13.3812499999569,
8.55026797822134));
#289073=CARTESIAN_POINT('Ctrl Pts',(-3.10606665601013,13.5312499999564,
9.5594902125713));
#289074=CARTESIAN_POINT('Ctrl Pts',(-1.84152565961621E-14,13.6812499999558,
10.5687124469213));
#289075=CARTESIAN_POINT('Ctrl Pts',(3.10606665601009,13.8312499999552,9.5594902125713));
#289076=CARTESIAN_POINT('Ctrl Pts',(6.2121333120202,13.9812499999546,8.55026797822134));
#289077=CARTESIAN_POINT('Ctrl Pts',(8.13178807675717,14.131249999954,5.90808986649102));
#289078=CARTESIAN_POINT('Ctrl Pts',(10.0514428414941,14.2812499999534,3.2659117547607));
#289079=CARTESIAN_POINT('Ctrl Pts',(10.0514428414941,14.4312499999528,-1.23094673026484E-15));
#289080=CARTESIAN_POINT('Ctrl Pts',(10.0514428414941,14.5812499999522,-3.26591175476071));
#289081=CARTESIAN_POINT('Ctrl Pts',(8.13178807675717,14.7312499999516,-5.90808986649102));
#289082=CARTESIAN_POINT('Ctrl Pts',(6.21213331202019,14.881249999951,-8.55026797822134));
#289083=CARTESIAN_POINT('Ctrl Pts',(3.10606665601009,15.0312499999504,-9.5594902125713));
#289084=CARTESIAN_POINT('Ctrl Pts',(-2.18676992058392E-14,15.1812499999498,
-10.5687124469213));
#289085=CARTESIAN_POINT('Ctrl Pts',(-3.10606665601013,15.3312499999492,
-9.5594902125713));
#289086=CARTESIAN_POINT('Ctrl Pts',(-6.21213331202024,15.4812499999485,
-8.55026797822134));
#289087=CARTESIAN_POINT('Ctrl Pts',(-8.13178807675721,15.6312499999479,
-5.90808986649102));
#289088=CARTESIAN_POINT('Ctrl Pts',(-10.0514428414942,15.7812499999473,
-3.2659117547607));
#289089=CARTESIAN_POINT('Ctrl Pts',(-10.0514428414942,15.9312499999467,
2.46189346052968E-15));
#289090=CARTESIAN_POINT('Ctrl Pts',(-10.0514428414942,16.0812499999461,
3.26591175476071));
#289091=CARTESIAN_POINT('Ctrl Pts',(-8.13178807675721,16.2312499999455,
5.90808986649102));
#289092=CARTESIAN_POINT('Ctrl Pts',(-6.21213331202024,16.3812499999449,
8.55026797822134));
#289093=CARTESIAN_POINT('Ctrl Pts',(-3.10606665601013,16.5312499999444,
9.5594902125713));
#289094=CARTESIAN_POINT('Ctrl Pts',(-2.0142965867824E-14,16.6812499999438,
10.5687124469213));
#289095=CARTESIAN_POINT('Ctrl Pts',(3.10606665601009,16.8312499999432,9.5594902125713));
#289096=CARTESIAN_POINT('Ctrl Pts',(6.21213331202019,16.9812499999426,8.55026797822134));
#289097=CARTESIAN_POINT('Ctrl Pts',(8.13178807675717,17.131249999942,5.90808986649102));
#289098=CARTESIAN_POINT('Ctrl Pts',(10.0514428414941,17.2812499999414,3.2659117547607));
#289099=CARTESIAN_POINT('Ctrl Pts',(10.0514428414941,17.4312499999408,-1.23094673026484E-15));
#289100=CARTESIAN_POINT('Ctrl Pts',(10.0514428414941,17.5812499999402,-3.26591175476071));
#289101=CARTESIAN_POINT('Ctrl Pts',(8.13178807675717,17.7312499999396,-5.90808986649102));
#289102=CARTESIAN_POINT('Ctrl Pts',(6.21213331202019,17.881249999939,-8.55026797822134));
#289103=CARTESIAN_POINT('Ctrl Pts',(3.10606665601008,18.0312499999384,-9.5594902125713));
#289104=CARTESIAN_POINT('Ctrl Pts',(-2.35954084775011E-14,18.1812499999378,
-10.5687124469213));
#289105=CARTESIAN_POINT('Ctrl Pts',(-3.10606665601013,18.3312499999371,
-9.5594902125713));
#289106=CARTESIAN_POINT('Ctrl Pts',(-6.21213331202024,18.4812499999365,
-8.55026797822134));
#289107=CARTESIAN_POINT('Ctrl Pts',(-8.13178807675721,18.6312499999359,
-5.90808986649102));
#289108=CARTESIAN_POINT('Ctrl Pts',(-10.0514428414942,18.7812499999353,
-3.2659117547607));
#289109=CARTESIAN_POINT('Ctrl Pts',(-10.0514428414942,18.9312499999347,
2.46189346052968E-15));
#289110=CARTESIAN_POINT('Ctrl Pts',(-10.0514428414942,19.0812499999341,
3.26591175476071));
#289111=CARTESIAN_POINT('Ctrl Pts',(-8.13178807675721,19.2312499999335,
5.90808986649102));
#289112=CARTESIAN_POINT('Ctrl Pts',(-6.21213331202024,19.381249999933,8.55026797822134));
#289113=CARTESIAN_POINT('Ctrl Pts',(-3.10606665601013,19.5312499999323,
9.5594902125713));
#289114=CARTESIAN_POINT('Ctrl Pts',(-2.18706751394858E-14,19.6812499999318,
10.5687124469213));
#289115=CARTESIAN_POINT('Ctrl Pts',(3.10606665601009,19.8312499999312,9.5594902125713));
#289116=CARTESIAN_POINT('Ctrl Pts',(6.21213331202019,19.9812499999306,8.55026797822134));
#289117=CARTESIAN_POINT('Ctrl Pts',(8.13178807675717,20.13124999993,5.90808986649102));
#289118=CARTESIAN_POINT('Ctrl Pts',(10.0514428414941,20.2812499999294,3.2659117547607));
#289119=CARTESIAN_POINT('Ctrl Pts',(10.0514428414941,20.4312499999288,-1.23094673026484E-15));
#289120=CARTESIAN_POINT('Ctrl Pts',(10.0514428414941,20.5812499999282,-3.26591175476071));
#289121=CARTESIAN_POINT('Ctrl Pts',(8.13178807675716,20.7312499999276,-5.90808986649102));
#289122=CARTESIAN_POINT('Ctrl Pts',(6.21213331202019,20.881249999927,-8.55026797822134));
#289123=CARTESIAN_POINT('Ctrl Pts',(3.10606665601008,21.0312499999264,-9.5594902125713));
#289124=CARTESIAN_POINT('Ctrl Pts',(-2.53231177491629E-14,21.1812499999258,
-10.5687124469213));
#289125=CARTESIAN_POINT('Ctrl Pts',(-3.10606665601013,21.3312499999251,
-9.5594902125713));
#289126=CARTESIAN_POINT('Ctrl Pts',(-6.21213331202024,21.4812499999245,
-8.55026797822134));
#289127=CARTESIAN_POINT('Ctrl Pts',(-8.13178807675722,21.6312499999239,
-5.90808986649102));
#289128=CARTESIAN_POINT('Ctrl Pts',(-10.0514428414942,21.7812499999233,
-3.2659117547607));
#289129=CARTESIAN_POINT('Ctrl Pts',(-10.0514428414942,21.9312499999227,
2.46189346052968E-15));
#289130=CARTESIAN_POINT('Ctrl Pts',(-10.0514428414942,22.0812499999221,
3.26591175476071));
#289131=CARTESIAN_POINT('Ctrl Pts',(-8.13178807675722,22.2312499999215,
5.90808986649102));
#289132=CARTESIAN_POINT('Ctrl Pts',(-6.21213331202024,22.3812499999209,
8.55026797822134));
#289133=CARTESIAN_POINT('Ctrl Pts',(-3.10606665601013,22.5312499999204,
9.5594902125713));
#289134=CARTESIAN_POINT('Ctrl Pts',(-2.35983844111477E-14,22.6812499999198,
10.5687124469213));
#289135=CARTESIAN_POINT('Ctrl Pts',(3.10606665601008,22.8312499999192,9.5594902125713));
#289136=CARTESIAN_POINT('Ctrl Pts',(6.21213331202019,22.9812499999186,8.55026797822134));
#289137=CARTESIAN_POINT('Ctrl Pts',(8.13178807675716,23.131249999918,5.90808986649102));
#289138=CARTESIAN_POINT('Ctrl Pts',(10.0514428414941,23.2812499999174,3.2659117547607));
#289139=CARTESIAN_POINT('Ctrl Pts',(10.0514428414941,23.4312499999168,-1.23094673026484E-15));
#289140=CARTESIAN_POINT('Ctrl Pts',(10.0514428414941,23.5812499999162,-3.26591175476071));
#289141=CARTESIAN_POINT('Ctrl Pts',(8.13178807675716,23.7312499999156,-5.90808986649102));
#289142=CARTESIAN_POINT('Ctrl Pts',(6.21213331202019,23.881249999915,-8.55026797822134));
#289143=CARTESIAN_POINT('Ctrl Pts',(3.10606665601008,24.0312499999144,-9.5594902125713));
#289144=CARTESIAN_POINT('Ctrl Pts',(-2.70508270208248E-14,24.1812499999138,
-10.5687124469213));
#289145=CARTESIAN_POINT('Ctrl Pts',(-3.10606665601014,24.3312499999131,
-9.5594902125713));
#289146=CARTESIAN_POINT('Ctrl Pts',(-6.21213331202024,24.4812499999125,
-8.55026797822134));
#289147=CARTESIAN_POINT('Ctrl Pts',(-8.13178807675722,24.6312499999119,
-5.90808986649102));
#289148=CARTESIAN_POINT('Ctrl Pts',(-10.0514428414942,24.7812499999113,
-3.2659117547607));
#289149=CARTESIAN_POINT('Ctrl Pts',(-10.0514428414942,24.9312499999107,
2.46189346052968E-15));
#289150=CARTESIAN_POINT('Ctrl Pts',(-10.0514428414942,25.0812499999101,
3.26591175476071));
#289151=CARTESIAN_POINT('Ctrl Pts',(-8.13178807675722,25.2312499999095,
5.90808986649102));
#289152=CARTESIAN_POINT('Ctrl Pts',(-6.21213331202024,25.381249999909,8.55026797822134));
#289153=CARTESIAN_POINT('Ctrl Pts',(-3.10606665601013,25.5312499999084,
9.5594902125713));
#289154=CARTESIAN_POINT('Ctrl Pts',(-2.53260936828095E-14,25.6812499999078,
10.5687124469213));
#289155=CARTESIAN_POINT('Ctrl Pts',(3.10606665601008,25.8312499999072,9.5594902125713));
#289156=CARTESIAN_POINT('Ctrl Pts',(6.21213331202019,25.9812499999066,8.55026797822134));
#289157=CARTESIAN_POINT('Ctrl Pts',(8.13178807675716,26.131249999906,5.90808986649102));
#289158=CARTESIAN_POINT('Ctrl Pts',(10.0514428414941,26.2812499999054,3.2659117547607));
#289159=CARTESIAN_POINT('Ctrl Pts',(10.0514428414941,26.4312499999048,-1.23094673026484E-15));
#289160=CARTESIAN_POINT('Ctrl Pts',(10.0514428414941,26.5812499999042,-3.26591175476071));
#289161=CARTESIAN_POINT('Ctrl Pts',(8.13178807675716,26.7312499999036,-5.90808986649102));
#289162=CARTESIAN_POINT('Ctrl Pts',(6.21213331202019,26.881249999903,-8.55026797822134));
#289163=CARTESIAN_POINT('Ctrl Pts',(3.10606665601008,27.0312499999024,-9.5594902125713));
#289164=CARTESIAN_POINT('Ctrl Pts',(-2.87785362924866E-14,27.1812499999018,
-10.5687124469213));
#289165=CARTESIAN_POINT('Ctrl Pts',(-3.10606665601014,27.3312499999011,
-9.5594902125713));
#289166=CARTESIAN_POINT('Ctrl Pts',(-6.21213331202024,27.4812499999005,
-8.55026797822134));
#289167=CARTESIAN_POINT('Ctrl Pts',(-8.13178807675722,27.6312499998999,
-5.90808986649102));
#289168=CARTESIAN_POINT('Ctrl Pts',(-10.0514428414942,27.7812499998993,
-3.2659117547607));
#289169=CARTESIAN_POINT('Ctrl Pts',(-10.0514428414942,27.9312499998987,
2.46189346052968E-15));
#289170=CARTESIAN_POINT('Ctrl Pts',(-10.0514428414942,28.0812499998981,
3.26591175476071));
#289171=CARTESIAN_POINT('Ctrl Pts',(-8.13178807675722,28.2312499998975,
5.90808986649102));
#289172=CARTESIAN_POINT('Ctrl Pts',(-6.21213331202024,28.3812499998969,
8.55026797822134));
#289173=CARTESIAN_POINT('Ctrl Pts',(-3.10606665601014,28.5312499998964,
9.5594902125713));
#289174=CARTESIAN_POINT('Ctrl Pts',(-2.70538029544713E-14,28.6812499998958,
10.5687124469213));
#289175=CARTESIAN_POINT('Ctrl Pts',(3.10606665601008,28.8312499998952,9.5594902125713));
#289176=CARTESIAN_POINT('Ctrl Pts',(6.21213331202019,28.9812499998946,8.55026797822134));
#289177=CARTESIAN_POINT('Ctrl Pts',(8.13178807675716,29.131249999894,5.90808986649102));
#289178=CARTESIAN_POINT('Ctrl Pts',(10.0514428414941,29.2812499998934,3.2659117547607));
#289179=CARTESIAN_POINT('Ctrl Pts',(10.0514428414941,29.4312499998928,-1.23094673026484E-15));
#289180=CARTESIAN_POINT('Ctrl Pts',(10.0514428414941,29.5812499998922,-3.26591175476071));
#289181=CARTESIAN_POINT('Ctrl Pts',(8.13178807675716,29.7312499998916,-5.90808986649102));
#289182=CARTESIAN_POINT('Ctrl Pts',(6.21213331202019,29.881249999891,-8.55026797822134));
#289183=CARTESIAN_POINT('Ctrl Pts',(3.10606665601008,30.0312499998904,-9.5594902125713));
#289184=CARTESIAN_POINT('Ctrl Pts',(-3.05062455641484E-14,30.1812499998898,
-10.5687124469213));
#289185=CARTESIAN_POINT('Ctrl Pts',(-3.10606665601014,30.3312499998892,
-9.5594902125713));
#289186=CARTESIAN_POINT('Ctrl Pts',(-6.21213331202025,30.4812499998885,
-8.55026797822134));
#289187=CARTESIAN_POINT('Ctrl Pts',(-8.13178807675722,30.6312499998879,
-5.90808986649102));
#289188=CARTESIAN_POINT('Ctrl Pts',(-10.0514428414942,30.7812499998873,
-3.2659117547607));
#289189=CARTESIAN_POINT('Ctrl Pts',(-10.0514428414942,30.9312499998867,
2.46189346052968E-15));
#289190=CARTESIAN_POINT('Ctrl Pts',(-10.0514428414942,31.0812499998861,
3.26591175476071));
#289191=CARTESIAN_POINT('Ctrl Pts',(-8.13178807675722,31.2312499998855,
5.90808986649102));
#289192=CARTESIAN_POINT('Ctrl Pts',(-6.21213331202024,31.381249999885,8.55026797822134));
#289193=CARTESIAN_POINT('Ctrl Pts',(-3.10606665601014,31.5312499998843,
9.5594902125713));
#289194=CARTESIAN_POINT('Ctrl Pts',(-2.87815122261332E-14,31.6812499998838,
10.5687124469213));
#289195=CARTESIAN_POINT('Ctrl Pts',(3.10606665601008,31.8312499998832,9.5594902125713));
#289196=CARTESIAN_POINT('Ctrl Pts',(6.21213331202019,31.9812499998826,8.55026797822134));
#289197=CARTESIAN_POINT('Ctrl Pts',(8.13178807675716,32.131249999882,5.90808986649102));
#289198=CARTESIAN_POINT('Ctrl Pts',(10.0514428414941,32.2812499998814,3.2659117547607));
#289199=CARTESIAN_POINT('Ctrl Pts',(10.0514428414941,32.4312499998808,-1.23094673026484E-15));
#289200=CARTESIAN_POINT('Ctrl Pts',(10.0514428414941,32.5812499998802,-3.26591175476071));
#289201=CARTESIAN_POINT('Ctrl Pts',(8.13178807675716,32.7312499998796,-5.90808986649102));
#289202=CARTESIAN_POINT('Ctrl Pts',(6.21213331202019,32.8812499998789,-8.55026797822134));
#289203=CARTESIAN_POINT('Ctrl Pts',(3.10606665601008,33.0312499998784,-9.5594902125713));
#289204=CARTESIAN_POINT('Ctrl Pts',(-3.22339548358103E-14,33.1812499998777,
-10.5687124469213));
#289205=CARTESIAN_POINT('Ctrl Pts',(-3.10606665601014,33.3312499998772,
-9.5594902125713));
#289206=CARTESIAN_POINT('Ctrl Pts',(-6.21213331202025,33.4812499998766,
-8.55026797822134));
#289207=CARTESIAN_POINT('Ctrl Pts',(-8.13178807675722,33.6312499998759,
-5.90808986649102));
#289208=CARTESIAN_POINT('Ctrl Pts',(-10.0514428414942,33.7812499998753,
-3.2659117547607));
#289209=CARTESIAN_POINT('Ctrl Pts',(-10.0514428414942,33.9312499998747,
2.46189346052968E-15));
#289210=CARTESIAN_POINT('Ctrl Pts',(-10.0514428414942,34.0812499998741,
3.26591175476071));
#289211=CARTESIAN_POINT('Ctrl Pts',(-8.13178807675722,34.2312499998735,
5.90808986649102));
#289212=CARTESIAN_POINT('Ctrl Pts',(-6.21213331202024,34.3812499998729,
8.55026797822134));
#289213=CARTESIAN_POINT('Ctrl Pts',(-3.10606665601014,34.5312499998724,
9.5594902125713));
#289214=CARTESIAN_POINT('Ctrl Pts',(-3.0509221497795E-14,34.6812499998718,
10.5687124469213));
#289215=CARTESIAN_POINT('Ctrl Pts',(3.10606665601008,34.8312499998712,9.5594902125713));
#289216=CARTESIAN_POINT('Ctrl Pts',(6.21213331202019,34.9812499998706,8.55026797822134));
#289217=CARTESIAN_POINT('Ctrl Pts',(8.13178807675716,35.13124999987,5.90808986649102));
#289218=CARTESIAN_POINT('Ctrl Pts',(10.0514428414941,35.2812499998694,3.2659117547607));
#289219=CARTESIAN_POINT('Ctrl Pts',(10.0514428414941,35.4312499998688,-1.23094673026484E-15));
#289220=CARTESIAN_POINT('Ctrl Pts',(10.0514428414941,35.5812499998682,-3.26591175476071));
#289221=CARTESIAN_POINT('Ctrl Pts',(8.13178807675716,35.7312499998676,-5.90808986649102));
#289222=CARTESIAN_POINT('Ctrl Pts',(6.21213331202018,35.881249999867,-8.55026797822134));
#289223=CARTESIAN_POINT('Ctrl Pts',(3.10606665601007,36.0312499998664,-9.5594902125713));
#289224=CARTESIAN_POINT('Ctrl Pts',(-3.39616641074721E-14,36.1812499998658,
-10.5687124469213));
#289225=CARTESIAN_POINT('Ctrl Pts',(-3.10606665601014,36.3312499998652,
-9.5594902125713));
#289226=CARTESIAN_POINT('Ctrl Pts',(-6.21213331202025,36.4812499998646,
-8.55026797822134));
#289227=CARTESIAN_POINT('Ctrl Pts',(-8.13178807675722,36.6312499998639,
-5.90808986649102));
#289228=CARTESIAN_POINT('Ctrl Pts',(-10.0514428414942,36.7812499998634,
-3.2659117547607));
#289229=CARTESIAN_POINT('Ctrl Pts',(-10.0514428414942,36.9312499998627,
2.46189346052968E-15));
#289230=CARTESIAN_POINT('Ctrl Pts',(-10.0514428414942,37.0812499998621,
3.26591175476071));
#289231=CARTESIAN_POINT('Ctrl Pts',(-8.13178807675722,37.2312499998615,
5.90808986649102));
#289232=CARTESIAN_POINT('Ctrl Pts',(-6.21213331202025,37.3812499998609,
8.55026797822134));
#289233=CARTESIAN_POINT('Ctrl Pts',(-3.10606665601014,37.5312499998603,
9.5594902125713));
#289234=CARTESIAN_POINT('Ctrl Pts',(-3.22369307694568E-14,37.6812499998598,
10.5687124469213));
#289235=CARTESIAN_POINT('Ctrl Pts',(3.10606665601008,37.8312499998592,9.5594902125713));
#289236=CARTESIAN_POINT('Ctrl Pts',(6.21213331202018,37.9812499998586,8.55026797822134));
#289237=CARTESIAN_POINT('Ctrl Pts',(8.13178807675716,38.131249999858,5.90808986649102));
#289238=CARTESIAN_POINT('Ctrl Pts',(10.0514428414941,38.2812499998574,3.2659117547607));
#289239=CARTESIAN_POINT('Ctrl Pts',(10.0514428414941,38.4312499998568,-1.23094673026484E-15));
#289240=CARTESIAN_POINT('Ctrl Pts',(10.0514428414941,38.5812499998562,-3.26591175476071));
#289241=CARTESIAN_POINT('Ctrl Pts',(8.13178807675715,38.7312499998556,-5.90808986649102));
#289242=CARTESIAN_POINT('Ctrl Pts',(6.21213331202018,38.881249999855,-8.55026797822134));
#289243=CARTESIAN_POINT('Ctrl Pts',(3.10606665601007,39.0312499998544,-9.5594902125713));
#289244=CARTESIAN_POINT('Ctrl Pts',(-3.5689373379134E-14,39.1812499998538,
-10.5687124469213));
#289245=CARTESIAN_POINT('Ctrl Pts',(-3.10606665601014,39.3312499998532,
-9.5594902125713));
#289246=CARTESIAN_POINT('Ctrl Pts',(-6.21213331202025,39.4812499998525,
-8.55026797822134));
#289247=CARTESIAN_POINT('Ctrl Pts',(-8.13178807675723,39.6312499998519,
-5.90808986649102));
#289248=CARTESIAN_POINT('Ctrl Pts',(-10.0514428414942,39.7812499998513,
-3.2659117547607));
#289249=CARTESIAN_POINT('Ctrl Pts',(-10.0514428414942,39.9312499998507,
2.46189346052968E-15));
#289250=CARTESIAN_POINT('Ctrl Pts',(-10.0514428414942,40.0812499998502,
3.26591175476071));
#289251=CARTESIAN_POINT('Ctrl Pts',(-8.13178807675723,40.2312499998495,
5.90808986649102));
#289252=CARTESIAN_POINT('Ctrl Pts',(-6.21213331202025,40.3812499998489,
8.55026797822134));
#289253=CARTESIAN_POINT('Ctrl Pts',(-3.10606665601014,40.5312499998483,
9.5594902125713));
#289254=CARTESIAN_POINT('Ctrl Pts',(-3.39646400411187E-14,40.6812499998478,
10.5687124469213));
#289255=CARTESIAN_POINT('Ctrl Pts',(3.10606665601007,40.8312499998472,9.5594902125713));
#289256=CARTESIAN_POINT('Ctrl Pts',(6.21213331202018,40.9812499998466,8.55026797822134));
#289257=CARTESIAN_POINT('Ctrl Pts',(8.13178807675715,41.131249999846,5.90808986649102));
#289258=CARTESIAN_POINT('Ctrl Pts',(10.0514428414941,41.2812499998454,3.2659117547607));
#289259=CARTESIAN_POINT('Ctrl Pts',(10.0514428414941,41.4312499998448,-1.23094673026484E-15));
#289260=CARTESIAN_POINT('Ctrl Pts',(10.0514428414941,41.5812499998442,-3.26591175476071));
#289261=CARTESIAN_POINT('Ctrl Pts',(8.13178807675715,41.7312499998436,-5.90808986649102));
#289262=CARTESIAN_POINT('Ctrl Pts',(6.21213331202018,41.881249999843,-8.55026797822134));
#289263=CARTESIAN_POINT('Ctrl Pts',(3.10606665601007,42.0312499998423,-9.5594902125713));
#289264=CARTESIAN_POINT('Ctrl Pts',(-3.74170826507958E-14,42.1812499998418,
-10.5687124469213));
#289265=CARTESIAN_POINT('Ctrl Pts',(-3.10606665601015,42.3312499998411,
-9.5594902125713));
#289266=CARTESIAN_POINT('Ctrl Pts',(-6.21213331202025,42.4812499998406,
-8.55026797822134));
#289267=CARTESIAN_POINT('Ctrl Pts',(-8.13178807675723,42.6312499998399,
-5.90808986649102));
#289268=CARTESIAN_POINT('Ctrl Pts',(-10.0514428414942,42.7812499998393,
-3.2659117547607));
#289269=CARTESIAN_POINT('Ctrl Pts',(-10.0514428414942,42.9312499998387,
2.46189346052968E-15));
#289270=CARTESIAN_POINT('Ctrl Pts',(-10.0514428414942,43.0812499998381,
3.26591175476071));
#289271=CARTESIAN_POINT('Ctrl Pts',(-8.13178807675723,43.2312499998375,
5.90808986649102));
#289272=CARTESIAN_POINT('Ctrl Pts',(-6.21213331202025,43.3812499998369,
8.55026797822134));
#289273=CARTESIAN_POINT('Ctrl Pts',(-3.10606665601014,43.5312499998363,
9.5594902125713));
#289274=CARTESIAN_POINT('Ctrl Pts',(-3.56923493127805E-14,43.6812499998357,
10.5687124469213));
#289275=CARTESIAN_POINT('Ctrl Pts',(3.10606665601007,43.8312499998352,9.5594902125713));
#289276=CARTESIAN_POINT('Ctrl Pts',(6.21213331202018,43.9812499998345,8.55026797822134));
#289277=CARTESIAN_POINT('Ctrl Pts',(8.13178807675715,44.131249999834,5.90808986649102));
#289278=CARTESIAN_POINT('Ctrl Pts',(10.0514428414941,44.2812499998334,3.2659117547607));
#289279=CARTESIAN_POINT('Ctrl Pts',(10.0514428414941,44.4312499998328,-1.23094673026484E-15));
#289280=CARTESIAN_POINT('Ctrl Pts',(10.0514428414941,44.5812499998322,-3.26591175476071));
#289281=CARTESIAN_POINT('Ctrl Pts',(8.13178807675715,44.7312499998316,-5.90808986649102));
#289282=CARTESIAN_POINT('Ctrl Pts',(6.21213331202018,44.881249999831,-8.55026797822134));
#289283=CARTESIAN_POINT('Ctrl Pts',(3.10606665601007,45.0312499998304,-9.5594902125713));
#289284=CARTESIAN_POINT('Ctrl Pts',(-3.91447919224576E-14,45.1812499998297,
-10.5687124469213));
#289285=CARTESIAN_POINT('Ctrl Pts',(-3.10606665601015,45.3312499998292,
-9.5594902125713));
#289286=CARTESIAN_POINT('Ctrl Pts',(-6.21213331202026,45.4812499998285,
-8.55026797822134));
#289287=CARTESIAN_POINT('Ctrl Pts',(-8.13178807675723,45.6312499998279,
-5.90808986649102));
#289288=CARTESIAN_POINT('Ctrl Pts',(-10.0514428414942,45.7812499998273,
-3.2659117547607));
#289289=CARTESIAN_POINT('Ctrl Pts',(-10.0514428414942,45.9312499998267,
2.46189346052968E-15));
#289290=CARTESIAN_POINT('Ctrl Pts',(-10.0514428414942,46.0812499998261,
3.26591175476071));
#289291=CARTESIAN_POINT('Ctrl Pts',(-8.13178807675723,46.2312499998255,
5.90808986649102));
#289292=CARTESIAN_POINT('Ctrl Pts',(-6.21213331202025,46.3812499998249,
8.55026797822134));
#289293=CARTESIAN_POINT('Ctrl Pts',(-3.10606665601015,46.5312499998244,
9.5594902125713));
#289294=CARTESIAN_POINT('Ctrl Pts',(-3.74200585844424E-14,46.6812499998238,
10.5687124469213));
#289295=CARTESIAN_POINT('Ctrl Pts',(3.10606665601007,46.8312499998232,9.5594902125713));
#289296=CARTESIAN_POINT('Ctrl Pts',(6.21213331202018,46.9812499998226,8.55026797822134));
#289297=CARTESIAN_POINT('Ctrl Pts',(8.13178807675715,47.131249999822,5.90808986649102));
#289298=CARTESIAN_POINT('Ctrl Pts',(10.0514428414941,47.2812499998214,3.2659117547607));
#289299=CARTESIAN_POINT('Ctrl Pts',(10.0514428414941,47.4312499998208,-1.23094673026484E-15));
#289300=CARTESIAN_POINT('Ctrl Pts',(10.0514428414941,47.5812499998202,-3.26591175476071));
#289301=CARTESIAN_POINT('Ctrl Pts',(8.13178807675715,47.7312499998196,-5.90808986649102));
#289302=CARTESIAN_POINT('Ctrl Pts',(6.21213331202017,47.881249999819,-8.55026797822134));
#289303=CARTESIAN_POINT('Ctrl Pts',(3.10606665601007,48.0312499998184,-9.5594902125713));
#289304=CARTESIAN_POINT('Ctrl Pts',(-4.08725011941195E-14,48.1812499998178,
-10.5687124469213));
#289305=CARTESIAN_POINT('Ctrl Pts',(-3.10606665601015,48.3312499998172,
-9.5594902125713));
#289306=CARTESIAN_POINT('Ctrl Pts',(-6.21213331202026,48.4812499998166,
-8.55026797822134));
#289307=CARTESIAN_POINT('Ctrl Pts',(-8.13178807675723,48.6312499998159,
-5.90808986649102));
#289308=CARTESIAN_POINT('Ctrl Pts',(-10.0514428414942,48.7812499998153,
-3.2659117547607));
#289309=CARTESIAN_POINT('Ctrl Pts',(-10.0514428414942,48.9312499998147,
2.46189346052968E-15));
#289310=CARTESIAN_POINT('Ctrl Pts',(-10.0514428414942,49.0812499998141,
3.26591175476071));
#289311=CARTESIAN_POINT('Ctrl Pts',(-8.13178807675723,49.2312499998135,
5.90808986649102));
#289312=CARTESIAN_POINT('Ctrl Pts',(-6.21213331202026,49.3812499998129,
8.55026797822134));
#289313=CARTESIAN_POINT('Ctrl Pts',(-3.10606665601015,49.5312499998124,
9.5594902125713));
#289314=CARTESIAN_POINT('Ctrl Pts',(-3.91477678561042E-14,49.6812499998117,
10.5687124469213));
#289315=CARTESIAN_POINT('Ctrl Pts',(3.10606665601007,49.8312499998111,9.5594902125713));
#289316=CARTESIAN_POINT('Ctrl Pts',(6.21213331202017,49.9812499998106,8.55026797822134));
#289317=CARTESIAN_POINT('Ctrl Pts',(8.13178807675715,50.13124999981,5.90808986649102));
#289318=CARTESIAN_POINT('Ctrl Pts',(10.0514428414941,50.2812499998094,3.2659117547607));
#289319=CARTESIAN_POINT('Ctrl Pts',(10.0514428414941,50.4312499998088,-1.23094673026484E-15));
#289320=CARTESIAN_POINT('Ctrl Pts',(10.0514428414941,50.5812499998082,-3.26591175476071));
#289321=CARTESIAN_POINT('Ctrl Pts',(8.13178807675715,50.7312499998076,-5.90808986649102));
#289322=CARTESIAN_POINT('Ctrl Pts',(6.21213331202017,50.881249999807,-8.55026797822134));
#289323=CARTESIAN_POINT('Ctrl Pts',(3.10606665601007,51.0312499998064,-9.5594902125713));
#289324=CARTESIAN_POINT('Ctrl Pts',(-4.26002104657813E-14,51.1812499998058,
-10.5687124469213));
#289325=CARTESIAN_POINT('Ctrl Pts',(-3.10606665601015,51.3312499998052,
-9.5594902125713));
#289326=CARTESIAN_POINT('Ctrl Pts',(-6.21213331202026,51.4812499998045,
-8.55026797822134));
#289327=CARTESIAN_POINT('Ctrl Pts',(-8.13178807675723,51.631249999804,-5.90808986649102));
#289328=CARTESIAN_POINT('Ctrl Pts',(-10.0514428414942,51.7812499998034,
-3.2659117547607));
#289329=CARTESIAN_POINT('Ctrl Pts',(-10.0514428414942,51.9312499998027,
2.46189346052968E-15));
#289330=CARTESIAN_POINT('Ctrl Pts',(-10.0514428414942,52.0812499998021,
3.26591175476071));
#289331=CARTESIAN_POINT('Ctrl Pts',(-8.13178807675723,52.2312499998015,
5.90808986649102));
#289332=CARTESIAN_POINT('Ctrl Pts',(-6.21213331202026,52.3812499998009,
8.55026797822134));
#289333=CARTESIAN_POINT('Ctrl Pts',(-3.10606665601015,52.5312499998004,
9.5594902125713));
#289334=CARTESIAN_POINT('Ctrl Pts',(-4.08754771277661E-14,52.6812499997998,
10.5687124469213));
#289335=CARTESIAN_POINT('Ctrl Pts',(3.10606665601007,52.8312499997991,9.5594902125713));
#289336=CARTESIAN_POINT('Ctrl Pts',(6.21213331202017,52.9812499997986,8.55026797822134));
#289337=CARTESIAN_POINT('Ctrl Pts',(8.13178807675715,53.131249999798,5.90808986649102));
#289338=CARTESIAN_POINT('Ctrl Pts',(10.0514428414941,53.2812499997974,3.2659117547607));
#289339=CARTESIAN_POINT('Ctrl Pts',(10.0514428414941,53.4312499997968,-1.23094673026484E-15));
#289340=CARTESIAN_POINT('Ctrl Pts',(10.0514428414941,53.5812499997962,-3.26591175476071));
#289341=CARTESIAN_POINT('Ctrl Pts',(8.13178807675714,53.7312499997956,-5.90808986649102));
#289342=CARTESIAN_POINT('Ctrl Pts',(6.21213331202017,53.881249999795,-8.55026797822134));
#289343=CARTESIAN_POINT('Ctrl Pts',(3.10606665601006,54.0312499997944,-9.5594902125713));
#289344=CARTESIAN_POINT('Ctrl Pts',(-4.43279197374432E-14,54.1812499997938,
-10.5687124469213));
#289345=CARTESIAN_POINT('Ctrl Pts',(-3.10606665601015,54.3312499997932,
-9.5594902125713));
#289346=CARTESIAN_POINT('Ctrl Pts',(-6.21213331202026,54.4812499997926,
-8.55026797822134));
#289347=CARTESIAN_POINT('Ctrl Pts',(-8.13178807675724,54.6312499997919,
-5.90808986649102));
#289348=CARTESIAN_POINT('Ctrl Pts',(-10.0514428414942,54.7812499997914,
-3.2659117547607));
#289349=CARTESIAN_POINT('Ctrl Pts',(-10.0514428414942,54.9312499997907,
2.46189346052968E-15));
#289350=CARTESIAN_POINT('Ctrl Pts',(-10.0514428414942,55.0812499997901,
3.26591175476071));
#289351=CARTESIAN_POINT('Ctrl Pts',(-8.13178807675724,55.2312499997895,
5.90808986649102));
#289352=CARTESIAN_POINT('Ctrl Pts',(-6.21213331202026,55.3812499997889,
8.55026797822134));
#289353=CARTESIAN_POINT('Ctrl Pts',(-3.10606665601015,55.5312499997884,
9.5594902125713));
#289354=CARTESIAN_POINT('Ctrl Pts',(-4.26031863994279E-14,55.6812499997877,
10.5687124469213));
#289355=CARTESIAN_POINT('Ctrl Pts',(3.10606665601006,55.8312499997871,9.5594902125713));
#289356=CARTESIAN_POINT('Ctrl Pts',(6.21213331202017,55.9812499997865,8.55026797822134));
#289357=CARTESIAN_POINT('Ctrl Pts',(8.13178807675714,56.131249999786,5.90808986649102));
#289358=CARTESIAN_POINT('Ctrl Pts',(10.0514428414941,56.2812499997854,3.2659117547607));
#289359=CARTESIAN_POINT('Ctrl Pts',(10.0514428414941,56.4312499997848,-1.23094673026484E-15));
#289360=CARTESIAN_POINT('Ctrl Pts',(10.0514428414941,56.5812499997842,-3.26591175476071));
#289361=CARTESIAN_POINT('Ctrl Pts',(8.13178807675714,56.7312499997836,-5.90808986649102));
#289362=CARTESIAN_POINT('Ctrl Pts',(6.21213331202017,56.881249999783,-8.55026797822134));
#289363=CARTESIAN_POINT('Ctrl Pts',(3.10606665601006,57.0312499997824,-9.5594902125713));
#289364=CARTESIAN_POINT('Ctrl Pts',(-4.6055629009105E-14,57.1812499997818,
-10.5687124469213));
#289365=CARTESIAN_POINT('Ctrl Pts',(-3.10606665601015,57.3312499997812,
-9.5594902125713));
#289366=CARTESIAN_POINT('Ctrl Pts',(-6.21213331202026,57.4812499997805,
-8.55026797822134));
#289367=CARTESIAN_POINT('Ctrl Pts',(-8.13178807675724,57.6312499997799,
-5.90808986649102));
#289368=CARTESIAN_POINT('Ctrl Pts',(-10.0514428414942,57.7812499997793,
-3.2659117547607));
#289369=CARTESIAN_POINT('Ctrl Pts',(-10.0514428414942,57.9312499997787,
2.46189346052968E-15));
#289370=CARTESIAN_POINT('Ctrl Pts',(-10.0514428414942,58.0812499997781,
3.26591175476071));
#289371=CARTESIAN_POINT('Ctrl Pts',(-8.13178807675724,58.2312499997775,
5.90808986649102));
#289372=CARTESIAN_POINT('Ctrl Pts',(-6.21213331202026,58.3812499997769,
8.55026797822134));
#289373=CARTESIAN_POINT('Ctrl Pts',(-3.10606665601015,58.5312499997763,
9.5594902125713));
#289374=CARTESIAN_POINT('Ctrl Pts',(-4.43308956710897E-14,58.6812499997758,
10.5687124469213));
#289375=CARTESIAN_POINT('Ctrl Pts',(3.10606665601006,58.8312499997751,9.5594902125713));
#289376=CARTESIAN_POINT('Ctrl Pts',(6.21213331202017,58.9812499997745,8.55026797822134));
#289377=CARTESIAN_POINT('Ctrl Pts',(8.13178807675714,59.131249999774,5.90808986649102));
#289378=CARTESIAN_POINT('Ctrl Pts',(10.0514428414941,59.2812499997734,3.2659117547607));
#289379=CARTESIAN_POINT('Ctrl Pts',(10.0514428414941,59.4312499997728,-1.23094673026484E-15));
#289380=CARTESIAN_POINT('Ctrl Pts',(10.0514428414941,59.5812499997722,-3.26591175476071));
#289381=CARTESIAN_POINT('Ctrl Pts',(8.13178807675714,59.7312499997716,-5.90808986649102));
#289382=CARTESIAN_POINT('Ctrl Pts',(6.21213331202017,59.881249999771,-8.55026797822134));
#289383=CARTESIAN_POINT('Ctrl Pts',(3.10606665601006,60.0312499997704,-9.5594902125713));
#289384=CARTESIAN_POINT('Ctrl Pts',(-4.77833382807668E-14,60.1812499997698,
-10.5687124469213));
#289385=CARTESIAN_POINT('Ctrl Pts',(-3.10606665601016,60.3312499997692,
-9.5594902125713));
#289386=CARTESIAN_POINT('Ctrl Pts',(-6.21213331202026,60.4812499997686,
-8.55026797822134));
#289387=CARTESIAN_POINT('Ctrl Pts',(-8.13178807675724,60.6312499997679,
-5.90808986649102));
#289388=CARTESIAN_POINT('Ctrl Pts',(-10.0514428414942,60.7812499997674,
-3.2659117547607));
#289389=CARTESIAN_POINT('Ctrl Pts',(-10.0514428414942,60.9312499997667,
2.46189346052968E-15));
#289390=CARTESIAN_POINT('Ctrl Pts',(-10.0514428414942,61.0812499997661,
3.26591175476071));
#289391=CARTESIAN_POINT('Ctrl Pts',(-8.13178807675724,61.2312499997655,
5.90808986649102));
#289392=CARTESIAN_POINT('Ctrl Pts',(-6.21213331202026,61.3812499997649,
8.55026797822134));
#289393=CARTESIAN_POINT('Ctrl Pts',(-3.10606665601015,61.5312499997643,
9.5594902125713));
#289394=CARTESIAN_POINT('Ctrl Pts',(-4.60586049427516E-14,61.6812499997638,
10.5687124469213));
#289395=CARTESIAN_POINT('Ctrl Pts',(3.10606665601006,61.8312499997632,9.5594902125713));
#289396=CARTESIAN_POINT('Ctrl Pts',(6.21213331202017,61.9812499997625,8.55026797822134));
#289397=CARTESIAN_POINT('Ctrl Pts',(8.13178807675714,62.131249999762,5.90808986649102));
#289398=CARTESIAN_POINT('Ctrl Pts',(10.0514428414941,62.2812499997614,3.2659117547607));
#289399=CARTESIAN_POINT('Ctrl Pts',(10.0514428414941,62.4312499997608,-1.23094673026484E-15));
#289400=CARTESIAN_POINT('Ctrl Pts',(10.0514428414941,62.5812499997602,-3.26591175476071));
#289401=CARTESIAN_POINT('Ctrl Pts',(8.13178807675714,62.7312499997596,-5.90808986649102));
#289402=CARTESIAN_POINT('Ctrl Pts',(6.21213331202017,62.881249999759,-8.55026797822134));
#289403=CARTESIAN_POINT('Ctrl Pts',(3.10606665601006,63.0312499997584,-9.5594902125713));
#289404=CARTESIAN_POINT('Ctrl Pts',(-4.95110475524287E-14,63.1812499997578,
-10.5687124469213));
#289405=CARTESIAN_POINT('Ctrl Pts',(-3.10606665601016,63.3312499997572,
-9.5594902125713));
#289406=CARTESIAN_POINT('Ctrl Pts',(-6.21213331202027,63.4812499997565,
-8.55026797822134));
#289407=CARTESIAN_POINT('Ctrl Pts',(-8.13178807675724,63.631249999756,-5.90808986649102));
#289408=CARTESIAN_POINT('Ctrl Pts',(-10.0514428414942,63.7812499997553,
-3.2659117547607));
#289409=CARTESIAN_POINT('Ctrl Pts',(-10.0514428414942,63.9312499997548,
2.46189346052968E-15));
#289410=CARTESIAN_POINT('Ctrl Pts',(-10.0514428414942,64.0812499997541,
3.26591175476071));
#289411=CARTESIAN_POINT('Ctrl Pts',(-8.13178807675724,64.2312499997535,
5.90808986649102));
#289412=CARTESIAN_POINT('Ctrl Pts',(-6.21213331202026,64.381249999753,8.55026797822134));
#289413=CARTESIAN_POINT('Ctrl Pts',(-3.10606665601016,64.5312499997523,
9.5594902125713));
#289414=CARTESIAN_POINT('Ctrl Pts',(-4.77863142144134E-14,64.6812499997518,
10.5687124469213));
#289415=CARTESIAN_POINT('Ctrl Pts',(3.10606665601006,64.8312499997512,9.5594902125713));
#289416=CARTESIAN_POINT('Ctrl Pts',(6.21213331202017,64.9812499997506,8.55026797822134));
#289417=CARTESIAN_POINT('Ctrl Pts',(8.13178807675714,65.13124999975,5.90808986649102));
#289418=CARTESIAN_POINT('Ctrl Pts',(10.0514428414941,65.2812499997493,3.2659117547607));
#289419=CARTESIAN_POINT('Ctrl Pts',(10.0514428414941,65.4312499997488,-1.23094673026484E-15));
#289420=CARTESIAN_POINT('Ctrl Pts',(10.0514428414941,65.5812499997482,-3.26591175476071));
#289421=CARTESIAN_POINT('Ctrl Pts',(8.13178807675714,65.7312499997475,-5.90808986649102));
#289422=CARTESIAN_POINT('Ctrl Pts',(6.21213331202016,65.881249999747,-8.55026797822134));
#289423=CARTESIAN_POINT('Ctrl Pts',(3.10606665601006,66.0312499997464,-9.5594902125713));
#289424=CARTESIAN_POINT('Ctrl Pts',(-5.12387568240905E-14,66.1812499997457,
-10.5687124469213));
#289425=CARTESIAN_POINT('Ctrl Pts',(-3.10606665601016,66.3312499997451,
-9.5594902125713));
#289426=CARTESIAN_POINT('Ctrl Pts',(-6.21213331202027,66.4812499997445,
-8.55026797822134));
#289427=CARTESIAN_POINT('Ctrl Pts',(-8.13178807675724,66.6312499997439,
-5.90808986649102));
#289428=CARTESIAN_POINT('Ctrl Pts',(-10.0514428414942,66.7812499997433,
-3.2659117547607));
#289429=CARTESIAN_POINT('Ctrl Pts',(-10.0514428414942,66.9312499997427,
2.46189346052968E-15));
#289430=CARTESIAN_POINT('Ctrl Pts',(-10.0514428414942,67.0812499997421,
3.26591175476071));
#289431=CARTESIAN_POINT('Ctrl Pts',(-8.13178807675724,67.2312499997416,
5.90808986649102));
#289432=CARTESIAN_POINT('Ctrl Pts',(-6.21213331202027,67.3812499997409,
8.55026797822134));
#289433=CARTESIAN_POINT('Ctrl Pts',(-3.10606665601016,67.5312499997404,
9.5594902125713));
#289434=CARTESIAN_POINT('Ctrl Pts',(-4.95140234860752E-14,67.6812499997397,
10.5687124469213));
#289435=CARTESIAN_POINT('Ctrl Pts',(3.10606665601006,67.8312499997391,9.5594902125713));
#289436=CARTESIAN_POINT('Ctrl Pts',(6.21213331202017,67.9812499997385,8.55026797822134));
#289437=CARTESIAN_POINT('Ctrl Pts',(8.13178807675714,68.1312499997379,5.90808986649102));
#289438=CARTESIAN_POINT('Ctrl Pts',(10.0514428414941,68.2812499997374,3.2659117547607));
#289439=CARTESIAN_POINT('Ctrl Pts',(10.0514428414941,68.4312499997367,-1.23094673026484E-15));
#289440=CARTESIAN_POINT('Ctrl Pts',(10.0514428414941,68.5812499997361,-3.26591175476071));
#289441=CARTESIAN_POINT('Ctrl Pts',(8.13178807675714,68.7312499997356,-5.90808986649102));
#289442=CARTESIAN_POINT('Ctrl Pts',(6.21213331202016,68.881249999735,-8.55026797822134));
#289443=CARTESIAN_POINT('Ctrl Pts',(3.10606665601006,69.0312499997344,-9.5594902125713));
#289444=CARTESIAN_POINT('Ctrl Pts',(-5.29664660957524E-14,69.1812499997337,
-10.5687124469213));
#289445=CARTESIAN_POINT('Ctrl Pts',(-3.10606665601016,69.3312499997332,
-9.5594902125713));
#289446=CARTESIAN_POINT('Ctrl Pts',(-6.21213331202027,69.4812499997326,
-8.55026797822134));
#289447=CARTESIAN_POINT('Ctrl Pts',(-8.13178807675724,69.6312499997319,
-5.90808986649102));
#289448=CARTESIAN_POINT('Ctrl Pts',(-10.0514428414942,69.7812499997313,
-3.2659117547607));
#289449=CARTESIAN_POINT('Ctrl Pts',(-10.0514428414942,69.9312499997307,
2.46189346052968E-15));
#289450=CARTESIAN_POINT('Ctrl Pts',(-10.0514428414942,70.0812499997301,
3.26591175476071));
#289451=CARTESIAN_POINT('Ctrl Pts',(-8.13178807675724,70.2312499997295,
5.90808986649102));
#289452=CARTESIAN_POINT('Ctrl Pts',(-6.21213331202027,70.3812499997289,
8.55026797822134));
#289453=CARTESIAN_POINT('Ctrl Pts',(-3.10606665601016,70.5312499997283,
9.5594902125713));
#289454=CARTESIAN_POINT('Ctrl Pts',(-5.12417327577371E-14,70.6812499997277,
10.5687124469213));
#289455=CARTESIAN_POINT('Ctrl Pts',(3.10606665601006,70.8312499997271,9.5594902125713));
#289456=CARTESIAN_POINT('Ctrl Pts',(6.21213331202016,70.9812499997265,8.55026797822134));
#289457=CARTESIAN_POINT('Ctrl Pts',(8.13178807675714,71.131249999726,5.90808986649102));
#289458=CARTESIAN_POINT('Ctrl Pts',(10.0514428414941,71.2812499997253,3.2659117547607));
#289459=CARTESIAN_POINT('Ctrl Pts',(10.0514428414941,71.4312499997248,-1.23094673026484E-15));
#289460=CARTESIAN_POINT('Ctrl Pts',(10.0514428414941,71.5812499997242,-3.26591175476071));
#289461=CARTESIAN_POINT('Ctrl Pts',(8.13178807675713,71.7312499997236,-5.90808986649102));
#289462=CARTESIAN_POINT('Ctrl Pts',(6.21213331202016,71.881249999723,-8.55026797822134));
#289463=CARTESIAN_POINT('Ctrl Pts',(3.10606665601005,72.0312499997223,-9.5594902125713));
#289464=CARTESIAN_POINT('Ctrl Pts',(-5.46941753674142E-14,72.1812499997217,
-10.5687124469213));
#289465=CARTESIAN_POINT('Ctrl Pts',(-3.10606665601016,72.3312499997212,
-9.5594902125713));
#289466=CARTESIAN_POINT('Ctrl Pts',(-6.21213331202027,72.4812499997205,
-8.55026797822134));
#289467=CARTESIAN_POINT('Ctrl Pts',(-8.13178807675725,72.63124999972,-5.90808986649102));
#289468=CARTESIAN_POINT('Ctrl Pts',(-10.0514428414942,72.7812499997193,
-3.2659117547607));
#289469=CARTESIAN_POINT('Ctrl Pts',(-10.0514428414942,72.9312499997187,
2.46189346052968E-15));
#289470=CARTESIAN_POINT('Ctrl Pts',(-10.0514428414942,73.0812499997181,
3.26591175476071));
#289471=CARTESIAN_POINT('Ctrl Pts',(-8.13178807675725,73.2312499997175,
5.90808986649102));
#289472=CARTESIAN_POINT('Ctrl Pts',(-6.21213331202027,73.381249999717,8.55026797822134));
#289473=CARTESIAN_POINT('Ctrl Pts',(-3.10606665601016,73.5312499997164,
9.5594902125713));
#289474=CARTESIAN_POINT('Ctrl Pts',(-5.29694420293989E-14,73.6812499997157,
10.5687124469213));
#289475=CARTESIAN_POINT('Ctrl Pts',(3.10606665601005,73.8312499997151,9.5594902125713));
#289476=CARTESIAN_POINT('Ctrl Pts',(6.21213331202016,73.9812499997146,8.55026797822134));
#289477=CARTESIAN_POINT('Ctrl Pts',(8.13178807675713,74.1312499997139,5.90808986649102));
#289478=CARTESIAN_POINT('Ctrl Pts',(10.0514428414941,74.2812499997134,3.2659117547607));
#289479=CARTESIAN_POINT('Ctrl Pts',(10.0514428414941,74.4312499997127,-1.23094673026484E-15));
#289480=CARTESIAN_POINT('Ctrl Pts',(10.0514428414941,74.5812499997122,-3.26591175476071));
#289481=CARTESIAN_POINT('Ctrl Pts',(8.13178807675713,74.7312499997116,-5.90808986649102));
#289482=CARTESIAN_POINT('Ctrl Pts',(6.21213331202016,74.8812499997109,-8.55026797822134));
#289483=CARTESIAN_POINT('Ctrl Pts',(3.10606665601005,75.0312499997104,-9.5594902125713));
#289484=CARTESIAN_POINT('Ctrl Pts',(-5.6421884639076E-14,75.1812499997098,
-10.5687124469213));
#289485=CARTESIAN_POINT('Ctrl Pts',(-3.10606665601016,75.3312499997092,
-9.5594902125713));
#289486=CARTESIAN_POINT('Ctrl Pts',(-6.21213331202027,75.4812499997086,
-8.55026797822134));
#289487=CARTESIAN_POINT('Ctrl Pts',(-8.13178807675725,75.6312499997079,
-5.90808986649102));
#289488=CARTESIAN_POINT('Ctrl Pts',(-10.0514428414942,75.7812499997073,
-3.2659117547607));
#289489=CARTESIAN_POINT('Ctrl Pts',(-10.0514428414942,75.9312499997068,
2.46189346052968E-15));
#289490=CARTESIAN_POINT('Ctrl Pts',(-10.0514428414942,76.0812499997061,
3.26591175476071));
#289491=CARTESIAN_POINT('Ctrl Pts',(-8.13178807675725,76.2312499997055,
5.90808986649102));
#289492=CARTESIAN_POINT('Ctrl Pts',(-6.21213331202027,76.3812499997049,
8.55026797822134));
#289493=CARTESIAN_POINT('Ctrl Pts',(-3.10606665601016,76.5312499997043,
9.5594902125713));
#289494=CARTESIAN_POINT('Ctrl Pts',(-5.46971513010608E-14,76.6812499997037,
10.5687124469213));
#289495=CARTESIAN_POINT('Ctrl Pts',(3.10606665601005,76.8312499997031,9.5594902125713));
#289496=CARTESIAN_POINT('Ctrl Pts',(6.21213331202016,76.9812499997025,8.55026797822134));
#289497=CARTESIAN_POINT('Ctrl Pts',(8.13178807675713,77.131249999702,5.90808986649102));
#289498=CARTESIAN_POINT('Ctrl Pts',(10.0514428414941,77.2812499997013,3.2659117547607));
#289499=CARTESIAN_POINT('Ctrl Pts',(10.0514428414941,77.4312499997008,-1.23094673026484E-15));
#289500=CARTESIAN_POINT('Ctrl Pts',(10.0514428414941,77.5812499997001,-3.26591175476071));
#289501=CARTESIAN_POINT('Ctrl Pts',(8.13178807675713,77.7312499996995,-5.90808986649102));
#289502=CARTESIAN_POINT('Ctrl Pts',(6.21213331202016,77.881249999699,-8.55026797822134));
#289503=CARTESIAN_POINT('Ctrl Pts',(3.10606665601005,78.0312499996984,-9.5594902125713));
#289504=CARTESIAN_POINT('Ctrl Pts',(-5.81495939107379E-14,78.1812499996978,
-10.5687124469213));
#289505=CARTESIAN_POINT('Ctrl Pts',(-3.10606665601017,78.3312499996971,
-9.5594902125713));
#289506=CARTESIAN_POINT('Ctrl Pts',(-6.21213331202028,78.4812499996966,
-8.55026797822134));
#289507=CARTESIAN_POINT('Ctrl Pts',(-8.13178807675725,78.631249999696,-5.90808986649102));
#289508=CARTESIAN_POINT('Ctrl Pts',(-10.0514428414942,78.7812499996954,
-3.2659117547607));
#289509=CARTESIAN_POINT('Ctrl Pts',(-10.0514428414942,78.9312499996948,
2.46189346052968E-15));
#289510=CARTESIAN_POINT('Ctrl Pts',(-10.0514428414942,79.0812499996942,
3.26591175476071));
#289511=CARTESIAN_POINT('Ctrl Pts',(-8.13178807675725,79.2312499996936,
5.90808986649102));
#289512=CARTESIAN_POINT('Ctrl Pts',(-6.21213331202027,79.381249999693,8.55026797822134));
#289513=CARTESIAN_POINT('Ctrl Pts',(-3.10606665601016,79.5312499996923,
9.5594902125713));
#289514=CARTESIAN_POINT('Ctrl Pts',(-5.64248605727226E-14,79.6812499996917,
10.5687124469213));
#289515=CARTESIAN_POINT('Ctrl Pts',(3.10606665601005,79.8312499996911,9.5594902125713));
#289516=CARTESIAN_POINT('Ctrl Pts',(6.21213331202016,79.9812499996905,8.55026797822134));
#289517=CARTESIAN_POINT('Ctrl Pts',(8.13178807675713,80.1312499996899,5.90808986649102));
#289518=CARTESIAN_POINT('Ctrl Pts',(10.0514428414941,80.2812499996894,3.2659117547607));
#289519=CARTESIAN_POINT('Ctrl Pts',(10.0514428414941,80.4312499996887,-1.23094673026484E-15));
#289520=CARTESIAN_POINT('Ctrl Pts',(10.0514428414941,80.5812499996882,-3.26591175476071));
#289521=CARTESIAN_POINT('Ctrl Pts',(8.13178807675713,80.7312499996875,-5.90808986649102));
#289522=CARTESIAN_POINT('Ctrl Pts',(6.21213331202016,80.881249999687,-8.55026797822134));
#289523=CARTESIAN_POINT('Ctrl Pts',(3.10606665601005,81.0312499996864,-9.5594902125713));
#289524=CARTESIAN_POINT('Ctrl Pts',(-5.98773031823997E-14,81.1812499996858,
-10.5687124469213));
#289525=CARTESIAN_POINT('Ctrl Pts',(-3.10606665601017,81.3312499996851,
-9.5594902125713));
#289526=CARTESIAN_POINT('Ctrl Pts',(-6.21213331202028,81.4812499996845,
-8.55026797822134));
#289527=CARTESIAN_POINT('Ctrl Pts',(-8.13178807675725,81.6312499996839,
-5.90808986649102));
#289528=CARTESIAN_POINT('Ctrl Pts',(-10.0514428414942,81.7812499996834,
-3.2659117547607));
#289529=CARTESIAN_POINT('Ctrl Pts',(-10.0514428414942,81.9312499996827,
2.46189346052968E-15));
#289530=CARTESIAN_POINT('Ctrl Pts',(-10.0514428414942,82.0812499996821,
3.26591175476071));
#289531=CARTESIAN_POINT('Ctrl Pts',(-8.13178807675725,82.2312499996816,
5.90808986649102));
#289532=CARTESIAN_POINT('Ctrl Pts',(-6.21213331202028,82.381249999681,8.55026797822134));
#289533=CARTESIAN_POINT('Ctrl Pts',(-3.10606665601017,82.5312499996804,
9.5594902125713));
#289534=CARTESIAN_POINT('Ctrl Pts',(-5.81525698443845E-14,82.6812499996797,
10.5687124469213));
#289535=CARTESIAN_POINT('Ctrl Pts',(3.10606665601005,82.8312499996792,9.5594902125713));
#289536=CARTESIAN_POINT('Ctrl Pts',(6.21213331202016,82.9812499996786,8.55026797822134));
#289537=CARTESIAN_POINT('Ctrl Pts',(8.13178807675713,83.131249999678,5.90808986649102));
#289538=CARTESIAN_POINT('Ctrl Pts',(10.0514428414941,83.2812499996773,3.2659117547607));
#289539=CARTESIAN_POINT('Ctrl Pts',(10.0514428414941,83.4312499996767,-1.23094673026484E-15));
#289540=CARTESIAN_POINT('Ctrl Pts',(10.0514428414941,83.5812499996761,-3.26591175476071));
#289541=CARTESIAN_POINT('Ctrl Pts',(8.13178807675713,83.7312499996756,-5.90808986649102));
#289542=CARTESIAN_POINT('Ctrl Pts',(6.21213331202016,83.8812499996749,-8.55026797822134));
#289543=CARTESIAN_POINT('Ctrl Pts',(3.10606665601005,84.0312499996743,-9.5594902125713));
#289544=CARTESIAN_POINT('Ctrl Pts',(-6.16050124540615E-14,84.1812499996738,
-10.5687124469213));
#289545=CARTESIAN_POINT('Ctrl Pts',(-3.10606665601017,84.3312499996732,
-9.5594902125713));
#289546=CARTESIAN_POINT('Ctrl Pts',(-6.21213331202028,84.4812499996725,
-8.55026797822134));
#289547=CARTESIAN_POINT('Ctrl Pts',(-8.13178807675725,84.631249999672,-5.90808986649102));
#289548=CARTESIAN_POINT('Ctrl Pts',(-10.0514428414942,84.7812499996714,
-3.2659117547607));
#289549=CARTESIAN_POINT('Ctrl Pts',(-10.0514428414942,84.9312499996708,
2.46189346052968E-15));
#289550=CARTESIAN_POINT('Ctrl Pts',(-10.0514428414942,85.0812499996701,
3.26591175476071));
#289551=CARTESIAN_POINT('Ctrl Pts',(-8.13178807675725,85.2312499996695,
5.90808986649102));
#289552=CARTESIAN_POINT('Ctrl Pts',(-6.21213331202028,85.381249999669,8.55026797822134));
#289553=CARTESIAN_POINT('Ctrl Pts',(-3.10606665601017,85.5312499996683,
9.5594902125713));
#289554=CARTESIAN_POINT('Ctrl Pts',(-5.98802791160463E-14,85.6812499996678,
10.5687124469213));
#289555=CARTESIAN_POINT('Ctrl Pts',(3.10606665601005,85.8312499996672,9.5594902125713));
#289556=CARTESIAN_POINT('Ctrl Pts',(6.21213331202016,85.9812499996666,8.55026797822134));
#289557=CARTESIAN_POINT('Ctrl Pts',(8.13178807675713,86.1312499996659,5.90808986649102));
#289558=CARTESIAN_POINT('Ctrl Pts',(10.0514428414941,86.2812499996653,3.2659117547607));
#289559=CARTESIAN_POINT('Ctrl Pts',(10.0514428414941,86.4312499996647,-1.23094673026484E-15));
#289560=CARTESIAN_POINT('Ctrl Pts',(10.0514428414941,86.5812499996642,-3.26591175476071));
#289561=CARTESIAN_POINT('Ctrl Pts',(8.13178807675713,86.7312499996635,-5.90808986649102));
#289562=CARTESIAN_POINT('Ctrl Pts',(6.21213331202015,86.8812499996629,-8.55026797822134));
#289563=CARTESIAN_POINT('Ctrl Pts',(3.10606665601004,87.0312499996624,-9.5594902125713));
#289564=CARTESIAN_POINT('Ctrl Pts',(-6.33327217257234E-14,87.1812499996618,
-10.5687124469213));
#289565=CARTESIAN_POINT('Ctrl Pts',(-3.10606665601017,87.3312499996611,
-9.5594902125713));
#289566=CARTESIAN_POINT('Ctrl Pts',(-6.21213331202028,87.4812499996605,
-8.55026797822134));
#289567=CARTESIAN_POINT('Ctrl Pts',(-8.13178807675726,87.6312499996599,
-5.90808986649102));
#289568=CARTESIAN_POINT('Ctrl Pts',(-10.0514428414942,87.7812499996594,
-3.2659117547607));
#289569=CARTESIAN_POINT('Ctrl Pts',(-10.0514428414942,87.9312499996587,
2.46189346052968E-15));
#289570=CARTESIAN_POINT('Ctrl Pts',(-10.0514428414942,88.0812499996581,
3.26591175476071));
#289571=CARTESIAN_POINT('Ctrl Pts',(-8.13178807675726,88.2312499996575,
5.90808986649102));
#289572=CARTESIAN_POINT('Ctrl Pts',(-6.21213331202028,88.3812499996569,
8.55026797822134));
#289573=CARTESIAN_POINT('Ctrl Pts',(-3.10606665601017,88.5312499996564,
9.5594902125713));
#289574=CARTESIAN_POINT('Ctrl Pts',(-6.16079883877081E-14,88.6812499996557,
10.5687124469213));
#289575=CARTESIAN_POINT('Ctrl Pts',(3.10606665601005,88.8312499996552,9.5594902125713));
#289576=CARTESIAN_POINT('Ctrl Pts',(6.21213331202016,88.9812499996546,8.55026797822134));
#289577=CARTESIAN_POINT('Ctrl Pts',(8.13178807675713,89.131249999654,5.90808986649102));
#289578=CARTESIAN_POINT('Ctrl Pts',(10.0514428414941,89.2812499996533,3.2659117547607));
#289579=CARTESIAN_POINT('Ctrl Pts',(10.0514428414941,89.4312499996527,-1.23094673026484E-15));
#289580=CARTESIAN_POINT('Ctrl Pts',(10.0514428414941,89.5812499996521,-3.26591175476071));
#289581=CARTESIAN_POINT('Ctrl Pts',(8.13178807675713,89.7312499996515,-5.90808986649102));
#289582=CARTESIAN_POINT('Ctrl Pts',(6.21213331202015,89.8812499996509,-8.55026797822134));
#289583=CARTESIAN_POINT('Ctrl Pts',(3.10606665601004,90.0312499996504,-9.5594902125713));
#289584=CARTESIAN_POINT('Ctrl Pts',(-6.50604309973852E-14,90.1812499996498,
-10.5687124469213));
#289585=CARTESIAN_POINT('Ctrl Pts',(-3.10606665601017,90.3312499996491,
-9.5594902125713));
#289586=CARTESIAN_POINT('Ctrl Pts',(-6.21213331202028,90.4812499996485,
-8.55026797822134));
#289587=CARTESIAN_POINT('Ctrl Pts',(-8.13178807675726,90.631249999648,-5.90808986649102));
#289588=CARTESIAN_POINT('Ctrl Pts',(-10.0514428414942,90.7812499996473,
-3.2659117547607));
#289589=CARTESIAN_POINT('Ctrl Pts',(-10.0514428414942,90.9312499996468,
2.46189346052968E-15));
#289590=CARTESIAN_POINT('Ctrl Pts',(-10.0514428414942,91.0812499996461,
3.26591175476071));
#289591=CARTESIAN_POINT('Ctrl Pts',(-8.13178807675726,91.2312499996455,
5.90808986649102));
#289592=CARTESIAN_POINT('Ctrl Pts',(-6.21213331202028,91.381249999645,8.55026797822134));
#289593=CARTESIAN_POINT('Ctrl Pts',(-3.10606665601017,91.5312499996443,
9.5594902125713));
#289594=CARTESIAN_POINT('Ctrl Pts',(-6.333569765937E-14,91.6812499996438,
10.5687124469213));
#289595=CARTESIAN_POINT('Ctrl Pts',(3.10606665601004,91.8312499996431,9.5594902125713));
#289596=CARTESIAN_POINT('Ctrl Pts',(6.21213331202015,91.9812499996426,8.55026797822134));
#289597=CARTESIAN_POINT('Ctrl Pts',(8.13178807675712,92.131249999642,5.90808986649102));
#289598=CARTESIAN_POINT('Ctrl Pts',(10.0514428414941,92.2812499996414,3.2659117547607));
#289599=CARTESIAN_POINT('Ctrl Pts',(10.0514428414941,92.4312499996408,-1.23094673026484E-15));
#289600=CARTESIAN_POINT('Ctrl Pts',(10.0514428414941,92.5812499996402,-3.26591175476071));
#289601=CARTESIAN_POINT('Ctrl Pts',(8.13178807675712,92.7312499996396,-5.90808986649102));
#289602=CARTESIAN_POINT('Ctrl Pts',(6.21213331202015,92.8812499996389,-8.55026797822134));
#289603=CARTESIAN_POINT('Ctrl Pts',(3.10606665601004,93.0312499996383,-9.5594902125713));
#289604=CARTESIAN_POINT('Ctrl Pts',(-6.67881402690471E-14,93.1812499996377,
-10.5687124469213));
#289605=CARTESIAN_POINT('Ctrl Pts',(-3.10606665601018,93.3312499996371,
-9.5594902125713));
#289606=CARTESIAN_POINT('Ctrl Pts',(-6.21213331202028,93.4812499996365,
-8.55026797822134));
#289607=CARTESIAN_POINT('Ctrl Pts',(-8.13178807675726,93.6312499996359,
-5.90808986649102));
#289608=CARTESIAN_POINT('Ctrl Pts',(-10.0514428414942,93.7812499996353,
-3.2659117547607));
#289609=CARTESIAN_POINT('Ctrl Pts',(-10.0514428414942,93.9312499996347,
2.46189346052968E-15));
#289610=CARTESIAN_POINT('Ctrl Pts',(-10.0514428414942,94.0812499996341,
3.26591175476071));
#289611=CARTESIAN_POINT('Ctrl Pts',(-8.13178807675726,94.2312499996335,
5.90808986649102));
#289612=CARTESIAN_POINT('Ctrl Pts',(-6.21213331202028,94.381249999633,8.55026797822134));
#289613=CARTESIAN_POINT('Ctrl Pts',(-3.10606665601017,94.5312499996324,
9.5594902125713));
#289614=CARTESIAN_POINT('Ctrl Pts',(-6.50634069310318E-14,94.6812499996317,
10.5687124469213));
#289615=CARTESIAN_POINT('Ctrl Pts',(3.10606665601004,94.8312499996312,9.5594902125713));
#289616=CARTESIAN_POINT('Ctrl Pts',(6.21213331202015,94.9812499996306,8.55026797822134));
#289617=CARTESIAN_POINT('Ctrl Pts',(8.13178807675712,95.13124999963,5.90808986649102));
#289618=CARTESIAN_POINT('Ctrl Pts',(10.0514428414941,95.2812499996293,3.2659117547607));
#289619=CARTESIAN_POINT('Ctrl Pts',(10.0514428414941,95.4312499996288,-1.23094673026484E-15));
#289620=CARTESIAN_POINT('Ctrl Pts',(10.0514428414941,95.5812499996282,-3.26591175476071));
#289621=CARTESIAN_POINT('Ctrl Pts',(8.13178807675712,95.7312499996276,-5.90808986649102));
#289622=CARTESIAN_POINT('Ctrl Pts',(6.21213331202015,95.8812499996269,-8.55026797822134));
#289623=CARTESIAN_POINT('Ctrl Pts',(3.10606665601004,96.0312499996264,-9.5594902125713));
#289624=CARTESIAN_POINT('Ctrl Pts',(-6.85158495407089E-14,96.1812499996257,
-10.5687124469213));
#289625=CARTESIAN_POINT('Ctrl Pts',(-3.10606665601018,96.3312499996252,
-9.5594902125713));
#289626=CARTESIAN_POINT('Ctrl Pts',(-6.21213331202028,96.4812499996245,
-8.55026797822134));
#289627=CARTESIAN_POINT('Ctrl Pts',(-8.13178807675726,96.6312499996239,
-5.90808986649102));
#289628=CARTESIAN_POINT('Ctrl Pts',(-10.0514428414942,96.7812499996234,
-3.2659117547607));
#289629=CARTESIAN_POINT('Ctrl Pts',(-10.0514428414942,96.9312499996227,
2.46189346052968E-15));
#289630=CARTESIAN_POINT('Ctrl Pts',(-10.0514428414942,97.0812499996221,
3.26591175476071));
#289631=CARTESIAN_POINT('Ctrl Pts',(-8.13178807675726,97.2312499996215,
5.90808986649102));
#289632=CARTESIAN_POINT('Ctrl Pts',(-6.21213331202028,97.381249999621,8.55026797822134));
#289633=CARTESIAN_POINT('Ctrl Pts',(-3.10606665601017,97.5312499996203,
9.5594902125713));
#289634=CARTESIAN_POINT('Ctrl Pts',(-6.67911162026936E-14,97.6812499996197,
10.5687124469213));
#289635=CARTESIAN_POINT('Ctrl Pts',(3.10606665601004,97.8312499996191,9.5594902125713));
#289636=CARTESIAN_POINT('Ctrl Pts',(6.21213331202015,97.9812499996186,8.55026797822134));
#289637=CARTESIAN_POINT('Ctrl Pts',(8.13178807675712,98.1312499996179,5.90808986649102));
#289638=CARTESIAN_POINT('Ctrl Pts',(10.0514428414941,98.2812499996173,3.2659117547607));
#289639=CARTESIAN_POINT('Ctrl Pts',(10.0514428414941,98.4312499996168,-1.23094673026484E-15));
#289640=CARTESIAN_POINT('Ctrl Pts',(10.0514428414941,98.5812499996162,-3.26591175476071));
#289641=CARTESIAN_POINT('Ctrl Pts',(8.13178807675712,98.7312499996156,-5.90808986649102));
#289642=CARTESIAN_POINT('Ctrl Pts',(6.21213331202015,98.8812499996149,-8.55026797822134));
#289643=CARTESIAN_POINT('Ctrl Pts',(3.10606665601004,99.0312499996143,-9.5594902125713));
#289644=CARTESIAN_POINT('Ctrl Pts',(-7.02435588123707E-14,99.1812499996138,
-10.5687124469213));
#289645=CARTESIAN_POINT('Ctrl Pts',(-3.10606665601018,99.3312499996131,
-9.5594902125713));
#289646=CARTESIAN_POINT('Ctrl Pts',(-6.21213331202028,99.4812499996125,
-8.55026797822134));
#289647=CARTESIAN_POINT('Ctrl Pts',(-8.13178807675726,99.631249999612,-5.90808986649102));
#289648=CARTESIAN_POINT('Ctrl Pts',(-10.0514428414942,99.7812499996113,
-3.2659117547607));
#289649=CARTESIAN_POINT('Ctrl Pts',(-10.0514428414942,99.9312499996108,
2.46189346052968E-15));
#289650=CARTESIAN_POINT('Ctrl Pts',(-10.0514428414942,100.08124999961,3.26591175476071));
#289651=CARTESIAN_POINT('Ctrl Pts',(-8.13178807675726,100.23124999961,5.90808986649102));
#289652=CARTESIAN_POINT('Ctrl Pts',(-6.21213331202028,100.381249999609,
8.55026797822134));
#289653=CARTESIAN_POINT('Ctrl Pts',(-3.10606665601018,100.531249999608,
9.5594902125713));
#289654=CARTESIAN_POINT('Ctrl Pts',(-6.85188254743555E-14,100.681249999608,
10.5687124469213));
#289655=CARTESIAN_POINT('Ctrl Pts',(3.10606665601004,100.831249999607,9.5594902125713));
#289656=CARTESIAN_POINT('Ctrl Pts',(6.21213331202015,100.981249999607,8.55026797822134));
#289657=CARTESIAN_POINT('Ctrl Pts',(8.13178807675712,101.131249999606,5.90808986649102));
#289658=CARTESIAN_POINT('Ctrl Pts',(10.0514428414941,101.281249999605,3.2659117547607));
#289659=CARTESIAN_POINT('Ctrl Pts',(10.0514428414941,101.431249999605,-1.23094673026484E-15));
#289660=CARTESIAN_POINT('Ctrl Pts',(10.0514428414941,101.581249999604,-3.26591175476071));
#289661=CARTESIAN_POINT('Ctrl Pts',(8.13178807675712,101.731249999604,-5.90808986649102));
#289662=CARTESIAN_POINT('Ctrl Pts',(6.21213331202014,101.881249999603,-8.55026797822134));
#289663=CARTESIAN_POINT('Ctrl Pts',(3.10606665601004,102.031249999602,-9.5594902125713));
#289664=CARTESIAN_POINT('Ctrl Pts',(-7.19712680840326E-14,102.181249999602,
-10.5687124469213));
#289665=CARTESIAN_POINT('Ctrl Pts',(-3.10606665601018,102.331249999601,
-9.5594902125713));
#289666=CARTESIAN_POINT('Ctrl Pts',(-6.21213331202029,102.481249999601,
-8.55026797822134));
#289667=CARTESIAN_POINT('Ctrl Pts',(-8.13178807675726,102.6312499996,-5.90808986649102));
#289668=CARTESIAN_POINT('Ctrl Pts',(-10.0514428414942,102.781249999599,
-3.2659117547607));
#289669=CARTESIAN_POINT('Ctrl Pts',(-10.0514428414942,102.931249999599,
2.46189346052968E-15));
#289670=CARTESIAN_POINT('Ctrl Pts',(-10.0514428414942,103.081249999598,
3.26591175476071));
#289671=CARTESIAN_POINT('Ctrl Pts',(-8.13178807675726,103.231249999598,
5.90808986649102));
#289672=CARTESIAN_POINT('Ctrl Pts',(-6.21213331202028,103.381249999597,
8.55026797822134));
#289673=CARTESIAN_POINT('Ctrl Pts',(-3.10606665601018,103.531249999596,
9.5594902125713));
#289674=CARTESIAN_POINT('Ctrl Pts',(-7.02465347460173E-14,103.681249999596,
10.5687124469213));
#289675=CARTESIAN_POINT('Ctrl Pts',(3.10606665601004,103.831249999595,9.5594902125713));
#289676=CARTESIAN_POINT('Ctrl Pts',(6.21213331202015,103.981249999595,8.55026797822134));
#289677=CARTESIAN_POINT('Ctrl Pts',(8.13178807675712,104.131249999594,5.90808986649102));
#289678=CARTESIAN_POINT('Ctrl Pts',(10.0514428414941,104.281249999593,3.2659117547607));
#289679=CARTESIAN_POINT('Ctrl Pts',(10.0514428414941,104.431249999593,-1.23094673026484E-15));
#289680=CARTESIAN_POINT('Ctrl Pts',(10.0514428414941,104.581249999592,-3.26591175476071));
#289681=CARTESIAN_POINT('Ctrl Pts',(8.13178807675712,104.731249999592,-5.90808986649102));
#289682=CARTESIAN_POINT('Ctrl Pts',(6.21213331202014,104.881249999591,-8.55026797822134));
#289683=CARTESIAN_POINT('Ctrl Pts',(3.10606665601003,105.03124999959,-9.5594902125713));
#289684=CARTESIAN_POINT('Ctrl Pts',(-7.36989773556944E-14,105.18124999959,
-10.5687124469213));
#289685=CARTESIAN_POINT('Ctrl Pts',(-3.10606665601018,105.331249999589,
-9.5594902125713));
#289686=CARTESIAN_POINT('Ctrl Pts',(-6.21213331202029,105.481249999589,
-8.55026797822134));
#289687=CARTESIAN_POINT('Ctrl Pts',(-8.13178807675726,105.631249999588,
-5.90808986649102));
#289688=CARTESIAN_POINT('Ctrl Pts',(-10.0514428414942,105.781249999587,
-3.2659117547607));
#289689=CARTESIAN_POINT('Ctrl Pts',(-10.0514428414942,105.931249999587,
2.46189346052968E-15));
#289690=CARTESIAN_POINT('Ctrl Pts',(-10.0514428414942,106.081249999586,
3.26591175476071));
#289691=CARTESIAN_POINT('Ctrl Pts',(-8.13178807675726,106.231249999586,
5.90808986649102));
#289692=CARTESIAN_POINT('Ctrl Pts',(-6.21213331202029,106.381249999585,
8.55026797822134));
#289693=CARTESIAN_POINT('Ctrl Pts',(-3.10606665601018,106.531249999584,
9.5594902125713));
#289694=CARTESIAN_POINT('Ctrl Pts',(-7.19742440176792E-14,106.681249999584,
10.5687124469213));
#289695=CARTESIAN_POINT('Ctrl Pts',(3.10606665601004,106.831249999583,9.5594902125713));
#289696=CARTESIAN_POINT('Ctrl Pts',(6.21213331202014,106.981249999583,8.55026797822134));
#289697=CARTESIAN_POINT('Ctrl Pts',(8.13178807675711,107.131249999582,5.90808986649102));
#289698=CARTESIAN_POINT('Ctrl Pts',(10.0514428414941,107.281249999581,3.2659117547607));
#289699=CARTESIAN_POINT('Ctrl Pts',(10.0514428414941,107.431249999581,-1.23094673026484E-15));
#289700=CARTESIAN_POINT('Ctrl Pts',(10.0514428414941,107.58124999958,-3.26591175476071));
#289701=CARTESIAN_POINT('Ctrl Pts',(8.13178807675711,107.73124999958,-5.90808986649102));
#289702=CARTESIAN_POINT('Ctrl Pts',(6.21213331202014,107.881249999579,-8.55026797822134));
#289703=CARTESIAN_POINT('Ctrl Pts',(3.10606665601003,108.031249999578,-9.5594902125713));
#289704=CARTESIAN_POINT('Ctrl Pts',(-7.54266866273562E-14,108.181249999578,
-10.5687124469213));
#289705=CARTESIAN_POINT('Ctrl Pts',(-3.10606665601018,108.331249999577,
-9.5594902125713));
#289706=CARTESIAN_POINT('Ctrl Pts',(-6.21213331202029,108.481249999577,
-8.55026797822134));
#289707=CARTESIAN_POINT('Ctrl Pts',(-8.13178807675727,108.631249999576,
-5.90808986649102));
#289708=CARTESIAN_POINT('Ctrl Pts',(-10.0514428414942,108.781249999575,
-3.2659117547607));
#289709=CARTESIAN_POINT('Ctrl Pts',(-10.0514428414942,108.931249999575,
2.46189346052968E-15));
#289710=CARTESIAN_POINT('Ctrl Pts',(-10.0514428414942,109.081249999574,
3.26591175476071));
#289711=CARTESIAN_POINT('Ctrl Pts',(-8.13178807675727,109.231249999574,
5.90808986649102));
#289712=CARTESIAN_POINT('Ctrl Pts',(-6.21213331202029,109.381249999573,
8.55026797822134));
#289713=CARTESIAN_POINT('Ctrl Pts',(-3.10606665601018,109.531249999572,
9.5594902125713));
#289714=CARTESIAN_POINT('Ctrl Pts',(-7.3701953289341E-14,109.681249999572,
10.5687124469213));
#289715=CARTESIAN_POINT('Ctrl Pts',(3.10606665601003,109.831249999571,9.5594902125713));
#289716=CARTESIAN_POINT('Ctrl Pts',(6.21213331202014,109.981249999571,8.55026797822134));
#289717=CARTESIAN_POINT('Ctrl Pts',(8.13178807675711,110.13124999957,5.90808986649102));
#289718=CARTESIAN_POINT('Ctrl Pts',(10.0514428414941,110.281249999569,3.2659117547607));
#289719=CARTESIAN_POINT('Ctrl Pts',(10.0514428414941,110.431249999569,-1.23094673026484E-15));
#289720=CARTESIAN_POINT('Ctrl Pts',(10.0514428414941,110.581249999568,-3.26591175476071));
#289721=CARTESIAN_POINT('Ctrl Pts',(8.13178807675711,110.731249999568,-5.90808986649102));
#289722=CARTESIAN_POINT('Ctrl Pts',(6.21213331202014,110.881249999567,-8.55026797822134));
#289723=CARTESIAN_POINT('Ctrl Pts',(3.10606665601003,111.031249999566,-9.5594902125713));
#289724=CARTESIAN_POINT('Ctrl Pts',(-7.71543958990181E-14,111.181249999566,
-10.5687124469213));
#289725=CARTESIAN_POINT('Ctrl Pts',(-3.10606665601019,111.331249999565,
-9.5594902125713));
#289726=CARTESIAN_POINT('Ctrl Pts',(-6.21213331202029,111.481249999565,
-8.55026797822134));
#289727=CARTESIAN_POINT('Ctrl Pts',(-8.13178807675727,111.631249999564,
-5.90808986649102));
#289728=CARTESIAN_POINT('Ctrl Pts',(-10.0514428414942,111.781249999563,
-3.2659117547607));
#289729=CARTESIAN_POINT('Ctrl Pts',(-10.0514428414942,111.931249999563,
2.46189346052968E-15));
#289730=CARTESIAN_POINT('Ctrl Pts',(-10.0514428414942,112.081249999562,
3.26591175476071));
#289731=CARTESIAN_POINT('Ctrl Pts',(-8.13178807675727,112.231249999562,
5.90808986649102));
#289732=CARTESIAN_POINT('Ctrl Pts',(-6.21213331202029,112.381249999561,
8.55026797822134));
#289733=CARTESIAN_POINT('Ctrl Pts',(-3.10606665601018,112.53124999956,9.5594902125713));
#289734=CARTESIAN_POINT('Ctrl Pts',(-7.54296625610028E-14,112.68124999956,
10.5687124469213));
#289735=CARTESIAN_POINT('Ctrl Pts',(3.10606665601003,112.831249999559,9.5594902125713));
#289736=CARTESIAN_POINT('Ctrl Pts',(6.21213331202014,112.981249999559,8.55026797822134));
#289737=CARTESIAN_POINT('Ctrl Pts',(8.13178807675711,113.131249999558,5.90808986649102));
#289738=CARTESIAN_POINT('Ctrl Pts',(10.0514428414941,113.281249999557,3.2659117547607));
#289739=CARTESIAN_POINT('Ctrl Pts',(10.0514428414941,113.431249999557,-1.23094673026484E-15));
#289740=CARTESIAN_POINT('Ctrl Pts',(10.0514428414941,113.581249999556,-3.26591175476071));
#289741=CARTESIAN_POINT('Ctrl Pts',(8.13178807675711,113.731249999556,-5.90808986649102));
#289742=CARTESIAN_POINT('Ctrl Pts',(6.21213331202014,113.881249999555,-8.55026797822134));
#289743=CARTESIAN_POINT('Ctrl Pts',(3.10606665601003,114.031249999554,-9.5594902125713));
#289744=CARTESIAN_POINT('Ctrl Pts',(-7.88821051706799E-14,114.181249999554,
-10.5687124469213));
#289745=CARTESIAN_POINT('Ctrl Pts',(-3.10606665601019,114.331249999553,
-9.5594902125713));
#289746=CARTESIAN_POINT('Ctrl Pts',(-6.2121333120203,114.481249999553,-8.55026797822134));
#289747=CARTESIAN_POINT('Ctrl Pts',(-8.13178807675727,114.631249999552,
-5.90808986649102));
#289748=CARTESIAN_POINT('Ctrl Pts',(-10.0514428414942,114.781249999551,
-3.2659117547607));
#289749=CARTESIAN_POINT('Ctrl Pts',(-10.0514428414942,114.931249999551,
2.46189346052968E-15));
#289750=CARTESIAN_POINT('Ctrl Pts',(-10.0514428414942,115.08124999955,3.26591175476071));
#289751=CARTESIAN_POINT('Ctrl Pts',(-8.13178807675727,115.23124999955,5.90808986649102));
#289752=CARTESIAN_POINT('Ctrl Pts',(-6.21213331202029,115.381249999549,
8.55026797822134));
#289753=CARTESIAN_POINT('Ctrl Pts',(-3.10606665601018,115.531249999548,
9.5594902125713));
#289754=CARTESIAN_POINT('Ctrl Pts',(-7.71573718326647E-14,115.681249999548,
10.5687124469213));
#289755=CARTESIAN_POINT('Ctrl Pts',(3.10606665601003,115.831249999547,9.5594902125713));
#289756=CARTESIAN_POINT('Ctrl Pts',(6.21213331202014,115.981249999547,8.55026797822134));
#289757=CARTESIAN_POINT('Ctrl Pts',(8.13178807675711,116.131249999546,5.90808986649102));
#289758=CARTESIAN_POINT('Ctrl Pts',(10.0514428414941,116.281249999545,3.2659117547607));
#289759=CARTESIAN_POINT('Ctrl Pts',(10.0514428414941,116.431249999545,-1.23094673026484E-15));
#289760=CARTESIAN_POINT('Ctrl Pts',(10.0514428414941,116.581249999544,-3.26591175476071));
#289761=CARTESIAN_POINT('Ctrl Pts',(8.13178807675711,116.731249999544,-5.90808986649102));
#289762=CARTESIAN_POINT('Ctrl Pts',(6.21213331202014,116.881249999543,-8.55026797822134));
#289763=CARTESIAN_POINT('Ctrl Pts',(3.10606665601003,117.031249999542,-9.5594902125713));
#289764=CARTESIAN_POINT('Ctrl Pts',(-8.06098144423418E-14,117.181249999542,
-10.5687124469213));
#289765=CARTESIAN_POINT('Ctrl Pts',(-3.10606665601019,117.331249999541,
-9.5594902125713));
#289766=CARTESIAN_POINT('Ctrl Pts',(-6.2121333120203,117.481249999541,-8.55026797822134));
#289767=CARTESIAN_POINT('Ctrl Pts',(-8.13178807675727,117.63124999954,-5.90808986649102));
#289768=CARTESIAN_POINT('Ctrl Pts',(-10.0514428414942,117.781249999539,
-3.2659117547607));
#289769=CARTESIAN_POINT('Ctrl Pts',(-10.0514428414942,117.931249999539,
2.46189346052968E-15));
#289770=CARTESIAN_POINT('Ctrl Pts',(-10.0514428414942,118.081249999538,
3.26591175476071));
#289771=CARTESIAN_POINT('Ctrl Pts',(-8.13178807675727,118.231249999538,
5.90808986649102));
#289772=CARTESIAN_POINT('Ctrl Pts',(-6.2121333120203,118.381249999537,8.55026797822134));
#289773=CARTESIAN_POINT('Ctrl Pts',(-3.10606665601019,118.531249999536,
9.5594902125713));
#289774=CARTESIAN_POINT('Ctrl Pts',(-7.88850811043265E-14,118.681249999536,
10.5687124469213));
#289775=CARTESIAN_POINT('Ctrl Pts',(3.10606665601003,118.831249999535,9.5594902125713));
#289776=CARTESIAN_POINT('Ctrl Pts',(6.21213331202014,118.981249999535,8.55026797822134));
#289777=CARTESIAN_POINT('Ctrl Pts',(8.13178807675711,119.131249999534,5.90808986649102));
#289778=CARTESIAN_POINT('Ctrl Pts',(10.0514428414941,119.281249999533,3.2659117547607));
#289779=CARTESIAN_POINT('Ctrl Pts',(10.0514428414941,119.431249999533,-1.23094673026484E-15));
#289780=CARTESIAN_POINT('Ctrl Pts',(10.0514428414941,119.581249999532,-3.26591175476071));
#289781=CARTESIAN_POINT('Ctrl Pts',(8.13178807675711,119.731249999532,-5.90808986649102));
#289782=CARTESIAN_POINT('Ctrl Pts',(6.21213331202013,119.881249999531,-8.55026797822134));
#289783=CARTESIAN_POINT('Ctrl Pts',(3.10606665601003,120.03124999953,-9.5594902125713));
#289784=CARTESIAN_POINT('Ctrl Pts',(-8.23375237140036E-14,120.18124999953,
-10.5687124469213));
#289785=CARTESIAN_POINT('Ctrl Pts',(-3.10606665601019,120.331249999529,
-9.5594902125713));
#289786=CARTESIAN_POINT('Ctrl Pts',(-6.2121333120203,120.481249999529,-8.55026797822134));
#289787=CARTESIAN_POINT('Ctrl Pts',(-8.13178807675727,120.631249999528,
-5.90808986649102));
#289788=CARTESIAN_POINT('Ctrl Pts',(-10.0514428414943,120.781249999527,
-3.2659117547607));
#289789=CARTESIAN_POINT('Ctrl Pts',(-10.0514428414943,120.931249999527,
2.46189346052968E-15));
#289790=CARTESIAN_POINT('Ctrl Pts',(-10.0514428414943,121.081249999526,
3.26591175476071));
#289791=CARTESIAN_POINT('Ctrl Pts',(-8.13178807675727,121.231249999526,
5.90808986649102));
#289792=CARTESIAN_POINT('Ctrl Pts',(-6.2121333120203,121.381249999525,8.55026797822134));
#289793=CARTESIAN_POINT('Ctrl Pts',(-3.10606665601019,121.531249999524,
9.5594902125713));
#289794=CARTESIAN_POINT('Ctrl Pts',(-8.06127903759884E-14,121.681249999524,
10.5687124469213));
#289795=CARTESIAN_POINT('Ctrl Pts',(3.10606665601003,121.831249999523,9.5594902125713));
#289796=CARTESIAN_POINT('Ctrl Pts',(6.21213331202014,121.981249999523,8.55026797822134));
#289797=CARTESIAN_POINT('Ctrl Pts',(8.13178807675711,122.131249999522,5.90808986649102));
#289798=CARTESIAN_POINT('Ctrl Pts',(10.0514428414941,122.281249999521,3.2659117547607));
#289799=CARTESIAN_POINT('Ctrl Pts',(10.0514428414941,122.431249999521,-1.23094673026484E-15));
#289800=CARTESIAN_POINT('Ctrl Pts',(10.0514428414941,122.58124999952,-3.26591175476071));
#289801=CARTESIAN_POINT('Ctrl Pts',(8.13178807675711,122.73124999952,-5.90808986649102));
#289802=CARTESIAN_POINT('Ctrl Pts',(6.21213331202013,122.881249999519,-8.55026797822134));
#289803=CARTESIAN_POINT('Ctrl Pts',(3.10606665601002,123.031249999518,-9.5594902125713));
#289804=CARTESIAN_POINT('Ctrl Pts',(-8.40652329856655E-14,123.181249999518,
-10.5687124469213));
#289805=CARTESIAN_POINT('Ctrl Pts',(-3.10606665601019,123.331249999517,
-9.5594902125713));
#289806=CARTESIAN_POINT('Ctrl Pts',(-6.2121333120203,123.481249999517,-8.55026797822134));
#289807=CARTESIAN_POINT('Ctrl Pts',(-8.13178807675727,123.631249999516,
-5.90808986649102));
#289808=CARTESIAN_POINT('Ctrl Pts',(-10.0514428414943,123.781249999515,
-3.2659117547607));
#289809=CARTESIAN_POINT('Ctrl Pts',(-10.0514428414943,123.931249999515,
2.46189346052968E-15));
#289810=CARTESIAN_POINT('Ctrl Pts',(-10.0514428414943,124.081249999514,
3.26591175476071));
#289811=CARTESIAN_POINT('Ctrl Pts',(-8.13178807675727,124.231249999514,
5.90808986649102));
#289812=CARTESIAN_POINT('Ctrl Pts',(-6.2121333120203,124.381249999513,8.55026797822134));
#289813=CARTESIAN_POINT('Ctrl Pts',(-3.10606665601019,124.531249999512,
9.5594902125713));
#289814=CARTESIAN_POINT('Ctrl Pts',(-8.23404996476502E-14,124.681249999512,
10.5687124469213));
#289815=CARTESIAN_POINT('Ctrl Pts',(3.10606665601002,124.831249999511,9.5594902125713));
#289816=CARTESIAN_POINT('Ctrl Pts',(6.21213331202013,124.981249999511,8.55026797822134));
#289817=CARTESIAN_POINT('Ctrl Pts',(8.13178807675711,125.13124999951,5.90808986649102));
#289818=CARTESIAN_POINT('Ctrl Pts',(10.0514428414941,125.281249999509,3.2659117547607));
#289819=CARTESIAN_POINT('Ctrl Pts',(10.0514428414941,125.431249999509,-1.23094673026484E-15));
#289820=CARTESIAN_POINT('Ctrl Pts',(10.0514428414941,125.581249999508,-3.26591175476071));
#289821=CARTESIAN_POINT('Ctrl Pts',(8.13178807675711,125.731249999508,-5.90808986649102));
#289822=CARTESIAN_POINT('Ctrl Pts',(6.21213331202013,125.881249999507,-8.55026797822134));
#289823=CARTESIAN_POINT('Ctrl Pts',(3.10606665601002,126.031249999506,-9.5594902125713));
#289824=CARTESIAN_POINT('Ctrl Pts',(-8.57929422573273E-14,126.181249999506,
-10.5687124469213));
#289825=CARTESIAN_POINT('Ctrl Pts',(-3.10606665601019,126.331249999505,
-9.5594902125713));
#289826=CARTESIAN_POINT('Ctrl Pts',(-6.2121333120203,126.481249999505,-8.55026797822134));
#289827=CARTESIAN_POINT('Ctrl Pts',(-8.13178807675728,126.631249999504,
-5.90808986649102));
#289828=CARTESIAN_POINT('Ctrl Pts',(-10.0514428414943,126.781249999503,
-3.2659117547607));
#289829=CARTESIAN_POINT('Ctrl Pts',(-10.0514428414943,126.931249999503,
2.46189346052968E-15));
#289830=CARTESIAN_POINT('Ctrl Pts',(-10.0514428414943,127.081249999502,
3.26591175476071));
#289831=CARTESIAN_POINT('Ctrl Pts',(-8.13178807675728,127.231249999502,
5.90808986649102));
#289832=CARTESIAN_POINT('Ctrl Pts',(-6.2121333120203,127.381249999501,8.55026797822134));
#289833=CARTESIAN_POINT('Ctrl Pts',(-3.10606665601019,127.5312499995,9.5594902125713));
#289834=CARTESIAN_POINT('Ctrl Pts',(-8.4068208919312E-14,127.6812499995,
10.5687124469213));
#289835=CARTESIAN_POINT('Ctrl Pts',(3.10606665601002,127.831249999499,9.5594902125713));
#289836=CARTESIAN_POINT('Ctrl Pts',(6.21213331202013,127.981249999499,8.55026797822134));
#289837=CARTESIAN_POINT('Ctrl Pts',(8.1317880767571,128.131249999498,5.90808986649102));
#289838=CARTESIAN_POINT('Ctrl Pts',(10.0514428414941,128.281249999497,3.2659117547607));
#289839=CARTESIAN_POINT('Ctrl Pts',(10.0514428414941,128.431249999497,-1.23094673026484E-15));
#289840=CARTESIAN_POINT('Ctrl Pts',(10.0514428414941,128.581249999496,-3.26591175476071));
#289841=CARTESIAN_POINT('Ctrl Pts',(8.1317880767571,128.731249999496,-5.90808986649102));
#289842=CARTESIAN_POINT('Ctrl Pts',(6.21213331202013,128.881249999495,-8.55026797822134));
#289843=CARTESIAN_POINT('Ctrl Pts',(3.10606665601002,129.031249999494,-9.5594902125713));
#289844=CARTESIAN_POINT('Ctrl Pts',(-8.75206515289892E-14,129.181249999494,
-10.5687124469213));
#289845=CARTESIAN_POINT('Ctrl Pts',(-3.1060666560102,129.331249999493,-9.5594902125713));
#289846=CARTESIAN_POINT('Ctrl Pts',(-6.2121333120203,129.481249999493,-8.55026797822134));
#289847=CARTESIAN_POINT('Ctrl Pts',(-8.13178807675728,129.631249999492,
-5.90808986649102));
#289848=CARTESIAN_POINT('Ctrl Pts',(-10.0514428414943,129.781249999491,
-3.2659117547607));
#289849=CARTESIAN_POINT('Ctrl Pts',(-10.0514428414943,129.931249999491,
2.46189346052968E-15));
#289850=CARTESIAN_POINT('Ctrl Pts',(-10.0514428414943,130.08124999949,3.26591175476071));
#289851=CARTESIAN_POINT('Ctrl Pts',(-8.13178807675728,130.23124999949,5.90808986649102));
#289852=CARTESIAN_POINT('Ctrl Pts',(-6.2121333120203,130.381249999489,8.55026797822134));
#289853=CARTESIAN_POINT('Ctrl Pts',(-3.10606665601019,130.531249999488,
9.5594902125713));
#289854=CARTESIAN_POINT('Ctrl Pts',(-8.57959181909739E-14,130.681249999488,
10.5687124469213));
#289855=CARTESIAN_POINT('Ctrl Pts',(3.10606665601002,130.831249999487,9.5594902125713));
#289856=CARTESIAN_POINT('Ctrl Pts',(6.21213331202013,130.981249999487,8.55026797822134));
#289857=CARTESIAN_POINT('Ctrl Pts',(8.1317880767571,131.131249999486,5.90808986649102));
#289858=CARTESIAN_POINT('Ctrl Pts',(10.0514428414941,131.281249999485,3.2659117547607));
#289859=CARTESIAN_POINT('Ctrl Pts',(10.0514428414941,131.431249999485,-1.23094673026484E-15));
#289860=CARTESIAN_POINT('Ctrl Pts',(10.0514428414941,131.581249999484,-3.26591175476071));
#289861=CARTESIAN_POINT('Ctrl Pts',(8.1317880767571,131.731249999484,-5.90808986649102));
#289862=CARTESIAN_POINT('Ctrl Pts',(6.21213331202012,131.881249999483,-8.55026797822134));
#289863=CARTESIAN_POINT('Ctrl Pts',(3.10606665601002,132.031249999482,-9.5594902125713));
#289864=CARTESIAN_POINT('Ctrl Pts',(-8.9248360800651E-14,132.181249999482,
-10.5687124469213));
#289865=CARTESIAN_POINT('Ctrl Pts',(-3.1060666560102,132.331249999481,-9.5594902125713));
#289866=CARTESIAN_POINT('Ctrl Pts',(-6.2121333120203,132.48124999948,-8.55026797822134));
#289867=CARTESIAN_POINT('Ctrl Pts',(-8.13178807675728,132.63124999948,-5.90808986649102));
#289868=CARTESIAN_POINT('Ctrl Pts',(-10.0514428414943,132.781249999479,
-3.2659117547607));
#289869=CARTESIAN_POINT('Ctrl Pts',(-10.0514428414943,132.931249999479,
2.46189346052968E-15));
#289870=CARTESIAN_POINT('Ctrl Pts',(-10.0514428414943,133.081249999478,
3.26591175476071));
#289871=CARTESIAN_POINT('Ctrl Pts',(-8.13178807675728,133.231249999478,
5.90808986649102));
#289872=CARTESIAN_POINT('Ctrl Pts',(-6.2121333120203,133.381249999477,8.55026797822134));
#289873=CARTESIAN_POINT('Ctrl Pts',(-3.1060666560102,133.531249999476,9.5594902125713));
#289874=CARTESIAN_POINT('Ctrl Pts',(-8.75236274626357E-14,133.681249999476,
10.5687124469213));
#289875=CARTESIAN_POINT('Ctrl Pts',(3.10606665601002,133.831249999475,9.5594902125713));
#289876=CARTESIAN_POINT('Ctrl Pts',(6.21213331202013,133.981249999475,8.55026797822134));
#289877=CARTESIAN_POINT('Ctrl Pts',(8.1317880767571,134.131249999474,5.90808986649102));
#289878=CARTESIAN_POINT('Ctrl Pts',(10.0514428414941,134.281249999473,3.2659117547607));
#289879=CARTESIAN_POINT('Ctrl Pts',(10.0514428414941,134.431249999473,-1.23094673026484E-15));
#289880=CARTESIAN_POINT('Ctrl Pts',(10.0514428414941,134.581249999472,-3.26591175476071));
#289881=CARTESIAN_POINT('Ctrl Pts',(8.1317880767571,134.731249999472,-5.90808986649102));
#289882=CARTESIAN_POINT('Ctrl Pts',(6.21213331202012,134.881249999471,-8.55026797822134));
#289883=CARTESIAN_POINT('Ctrl Pts',(3.10606665601002,135.03124999947,-9.5594902125713));
#289884=CARTESIAN_POINT('Ctrl Pts',(-9.09760700723128E-14,135.18124999947,
-10.5687124469213));
#289885=CARTESIAN_POINT('Ctrl Pts',(-3.1060666560102,135.331249999469,-9.5594902125713));
#289886=CARTESIAN_POINT('Ctrl Pts',(-6.21213331202031,135.481249999469,
-8.55026797822134));
#289887=CARTESIAN_POINT('Ctrl Pts',(-8.13178807675728,135.631249999468,
-5.90808986649102));
#289888=CARTESIAN_POINT('Ctrl Pts',(-10.0514428414943,135.781249999467,
-3.2659117547607));
#289889=CARTESIAN_POINT('Ctrl Pts',(-10.0514428414943,135.931249999467,
2.46189346052968E-15));
#289890=CARTESIAN_POINT('Ctrl Pts',(-10.0514428414943,136.081249999466,
3.26591175476071));
#289891=CARTESIAN_POINT('Ctrl Pts',(-8.13178807675728,136.231249999466,
5.90808986649102));
#289892=CARTESIAN_POINT('Ctrl Pts',(-6.2121333120203,136.381249999465,8.55026797822134));
#289893=CARTESIAN_POINT('Ctrl Pts',(-3.1060666560102,136.531249999464,9.5594902125713));
#289894=CARTESIAN_POINT('Ctrl Pts',(-8.92513367342975E-14,136.681249999464,
10.5687124469213));
#289895=CARTESIAN_POINT('Ctrl Pts',(3.10606665601002,136.831249999463,9.5594902125713));
#289896=CARTESIAN_POINT('Ctrl Pts',(6.21213331202012,136.981249999463,8.55026797822134));
#289897=CARTESIAN_POINT('Ctrl Pts',(8.1317880767571,137.131249999462,5.90808986649102));
#289898=CARTESIAN_POINT('Ctrl Pts',(10.0514428414941,137.281249999461,3.2659117547607));
#289899=CARTESIAN_POINT('Ctrl Pts',(10.0514428414941,137.431249999461,-1.23094673026484E-15));
#289900=CARTESIAN_POINT('Ctrl Pts',(10.0514428414941,137.58124999946,-3.26591175476071));
#289901=CARTESIAN_POINT('Ctrl Pts',(8.1317880767571,137.73124999946,-5.90808986649102));
#289902=CARTESIAN_POINT('Ctrl Pts',(6.21213331202012,137.881249999459,-8.55026797822134));
#289903=CARTESIAN_POINT('Ctrl Pts',(3.10606665601002,138.031249999458,-9.5594902125713));
#289904=CARTESIAN_POINT('Ctrl Pts',(-9.27037793439746E-14,138.181249999458,
-10.5687124469213));
#289905=CARTESIAN_POINT('Ctrl Pts',(-3.1060666560102,138.331249999457,-9.5594902125713));
#289906=CARTESIAN_POINT('Ctrl Pts',(-6.21213331202031,138.481249999456,
-8.55026797822134));
#289907=CARTESIAN_POINT('Ctrl Pts',(-8.13178807675728,138.631249999456,
-5.90808986649102));
#289908=CARTESIAN_POINT('Ctrl Pts',(-10.0514428414943,138.781249999455,
-3.2659117547607));
#289909=CARTESIAN_POINT('Ctrl Pts',(-10.0514428414943,138.931249999455,
2.46189346052968E-15));
#289910=CARTESIAN_POINT('Ctrl Pts',(-10.0514428414943,139.081249999454,
3.26591175476071));
#289911=CARTESIAN_POINT('Ctrl Pts',(-8.13178807675728,139.231249999454,
5.90808986649102));
#289912=CARTESIAN_POINT('Ctrl Pts',(-6.21213331202031,139.381249999453,
8.55026797822134));
#289913=CARTESIAN_POINT('Ctrl Pts',(-3.1060666560102,139.531249999452,9.5594902125713));
#289914=CARTESIAN_POINT('Ctrl Pts',(-9.09790460059594E-14,139.681249999452,
10.5687124469213));
#289915=CARTESIAN_POINT('Ctrl Pts',(3.10606665601002,139.831249999451,9.5594902125713));
#289916=CARTESIAN_POINT('Ctrl Pts',(6.21213331202012,139.981249999451,8.55026797822134));
#289917=CARTESIAN_POINT('Ctrl Pts',(8.1317880767571,140.13124999945,5.90808986649102));
#289918=CARTESIAN_POINT('Ctrl Pts',(10.0514428414941,140.281249999449,3.2659117547607));
#289919=CARTESIAN_POINT('Ctrl Pts',(10.0514428414941,140.431249999449,-1.23094673026484E-15));
#289920=CARTESIAN_POINT('Ctrl Pts',(10.0514428414941,140.581249999448,-3.26591175476071));
#289921=CARTESIAN_POINT('Ctrl Pts',(8.1317880767571,140.731249999448,-5.90808986649102));
#289922=CARTESIAN_POINT('Ctrl Pts',(6.21213331202012,140.881249999447,-8.55026797822134));
#289923=CARTESIAN_POINT('Ctrl Pts',(3.10606665601001,141.031249999446,-9.5594902125713));
#289924=CARTESIAN_POINT('Ctrl Pts',(-9.44314886156365E-14,141.181249999446,
-10.5687124469213));
#289925=CARTESIAN_POINT('Ctrl Pts',(-3.1060666560102,141.331249999445,-9.5594902125713));
#289926=CARTESIAN_POINT('Ctrl Pts',(-6.21213331202031,141.481249999445,
-8.55026797822134));
#289927=CARTESIAN_POINT('Ctrl Pts',(-8.13178807675729,141.631249999444,
-5.90808986649102));
#289928=CARTESIAN_POINT('Ctrl Pts',(-10.0514428414943,141.781249999443,
-3.2659117547607));
#289929=CARTESIAN_POINT('Ctrl Pts',(-10.0514428414943,141.931249999443,
2.46189346052968E-15));
#289930=CARTESIAN_POINT('Ctrl Pts',(-10.0514428414943,142.081249999442,
3.26591175476071));
#289931=CARTESIAN_POINT('Ctrl Pts',(-8.13178807675729,142.231249999442,
5.90808986649102));
#289932=CARTESIAN_POINT('Ctrl Pts',(-6.21213331202031,142.381249999441,
8.55026797822134));
#289933=CARTESIAN_POINT('Ctrl Pts',(-3.1060666560102,142.53124999944,9.5594902125713));
#289934=CARTESIAN_POINT('Ctrl Pts',(-9.27067552776212E-14,142.68124999944,
10.5687124469213));
#289935=CARTESIAN_POINT('Ctrl Pts',(3.10606665601001,142.831249999439,9.5594902125713));
#289936=CARTESIAN_POINT('Ctrl Pts',(6.21213331202012,142.981249999439,8.55026797822134));
#289937=CARTESIAN_POINT('Ctrl Pts',(8.1317880767571,143.131249999438,5.90808986649102));
#289938=CARTESIAN_POINT('Ctrl Pts',(10.0514428414941,143.281249999437,3.2659117547607));
#289939=CARTESIAN_POINT('Ctrl Pts',(10.0514428414941,143.431249999437,-1.23094673026484E-15));
#289940=CARTESIAN_POINT('Ctrl Pts',(10.0514428414941,143.581249999436,-3.26591175476071));
#289941=CARTESIAN_POINT('Ctrl Pts',(8.1317880767571,143.731249999436,-5.90808986649102));
#289942=CARTESIAN_POINT('Ctrl Pts',(6.21213331202012,143.881249999435,-8.55026797822134));
#289943=CARTESIAN_POINT('Ctrl Pts',(3.10606665601001,144.031249999434,-9.5594902125713));
#289944=CARTESIAN_POINT('Ctrl Pts',(-9.61591978872984E-14,144.181249999434,
-10.5687124469213));
#289945=CARTESIAN_POINT('Ctrl Pts',(-3.1060666560102,144.331249999433,-9.5594902125713));
#289946=CARTESIAN_POINT('Ctrl Pts',(-6.21213331202031,144.481249999432,
-8.55026797822134));
#289947=CARTESIAN_POINT('Ctrl Pts',(-8.13178807675729,144.631249999432,
-5.90808986649102));
#289948=CARTESIAN_POINT('Ctrl Pts',(-10.0514428414943,144.781249999431,
-3.2659117547607));
#289949=CARTESIAN_POINT('Ctrl Pts',(-10.0514428414943,144.931249999431,
2.46189346052968E-15));
#289950=CARTESIAN_POINT('Ctrl Pts',(-10.0514428414943,145.08124999943,3.26591175476071));
#289951=CARTESIAN_POINT('Ctrl Pts',(-8.13178807675729,145.23124999943,5.90808986649102));
#289952=CARTESIAN_POINT('Ctrl Pts',(-6.21213331202031,145.381249999429,
8.55026797822134));
#289953=CARTESIAN_POINT('Ctrl Pts',(-3.1060666560102,145.531249999428,9.5594902125713));
#289954=CARTESIAN_POINT('Ctrl Pts',(-9.44344645492831E-14,145.681249999428,
10.5687124469213));
#289955=CARTESIAN_POINT('Ctrl Pts',(3.10606665601001,145.831249999427,9.5594902125713));
#289956=CARTESIAN_POINT('Ctrl Pts',(6.21213331202012,145.981249999427,8.55026797822134));
#289957=CARTESIAN_POINT('Ctrl Pts',(8.13178807675709,146.131249999426,5.90808986649102));
#289958=CARTESIAN_POINT('Ctrl Pts',(10.0514428414941,146.281249999425,3.2659117547607));
#289959=CARTESIAN_POINT('Ctrl Pts',(10.0514428414941,146.431249999425,-1.23094673026484E-15));
#289960=CARTESIAN_POINT('Ctrl Pts',(10.0514428414941,146.581249999424,-3.26591175476071));
#289961=CARTESIAN_POINT('Ctrl Pts',(8.13178807675709,146.731249999424,-5.90808986649102));
#289962=CARTESIAN_POINT('Ctrl Pts',(6.21213331202012,146.881249999423,-8.55026797822134));
#289963=CARTESIAN_POINT('Ctrl Pts',(3.10606665601001,147.031249999422,-9.5594902125713));
#289964=CARTESIAN_POINT('Ctrl Pts',(-9.78869071589602E-14,147.181249999422,
-10.5687124469213));
#289965=CARTESIAN_POINT('Ctrl Pts',(-3.10606665601021,147.331249999421,
-9.5594902125713));
#289966=CARTESIAN_POINT('Ctrl Pts',(-6.21213331202032,147.481249999421,
-8.55026797822134));
#289967=CARTESIAN_POINT('Ctrl Pts',(-8.13178807675729,147.63124999942,-5.90808986649102));
#289968=CARTESIAN_POINT('Ctrl Pts',(-10.0514428414943,147.781249999419,
-3.2659117547607));
#289969=CARTESIAN_POINT('Ctrl Pts',(-10.0514428414943,147.931249999419,
2.46189346052968E-15));
#289970=CARTESIAN_POINT('Ctrl Pts',(-10.0514428414943,148.081249999418,
3.26591175476071));
#289971=CARTESIAN_POINT('Ctrl Pts',(-8.13178807675729,148.231249999418,
5.90808986649102));
#289972=CARTESIAN_POINT('Ctrl Pts',(-6.21213331202031,148.381249999417,
8.55026797822134));
#289973=CARTESIAN_POINT('Ctrl Pts',(-3.1060666560102,148.531249999416,9.5594902125713));
#289974=CARTESIAN_POINT('Ctrl Pts',(-9.61621738209449E-14,148.681249999416,
10.5687124469213));
#289975=CARTESIAN_POINT('Ctrl Pts',(3.10606665601001,148.831249999415,9.5594902125713));
#289976=CARTESIAN_POINT('Ctrl Pts',(6.21213331202012,148.981249999415,8.55026797822134));
#289977=CARTESIAN_POINT('Ctrl Pts',(8.13178807675709,149.131249999414,5.90808986649102));
#289978=CARTESIAN_POINT('Ctrl Pts',(10.0514428414941,149.281249999413,3.2659117547607));
#289979=CARTESIAN_POINT('Ctrl Pts',(10.0514428414941,149.431249999413,-1.23094673026484E-15));
#289980=CARTESIAN_POINT('Ctrl Pts',(10.0514428414941,149.581249999412,-3.26591175476071));
#289981=CARTESIAN_POINT('Ctrl Pts',(8.13178807675709,149.731249999412,-5.90808986649102));
#289982=CARTESIAN_POINT('Ctrl Pts',(6.21213331202012,149.881249999411,-8.55026797822134));
#289983=CARTESIAN_POINT('Ctrl Pts',(3.10606665601001,150.03124999941,-9.5594902125713));
#289984=CARTESIAN_POINT('Ctrl Pts',(-9.9614616430622E-14,150.18124999941,
-10.5687124469213));
#289985=CARTESIAN_POINT('Ctrl Pts',(-3.10606665601021,150.331249999409,
-9.5594902125713));
#289986=CARTESIAN_POINT('Ctrl Pts',(-6.21213331202032,150.481249999409,
-8.55026797822134));
#289987=CARTESIAN_POINT('Ctrl Pts',(-8.13178807675729,150.631249999408,
-5.90808986649102));
#289988=CARTESIAN_POINT('Ctrl Pts',(-10.0514428414943,150.781249999407,
-3.2659117547607));
#289989=CARTESIAN_POINT('Ctrl Pts',(-10.0514428414943,150.931249999407,
2.46189346052968E-15));
#289990=CARTESIAN_POINT('Ctrl Pts',(-10.0514428414943,151.081249999406,
3.26591175476071));
#289991=CARTESIAN_POINT('Ctrl Pts',(-8.13178807675729,151.231249999406,
5.90808986649102));
#289992=CARTESIAN_POINT('Ctrl Pts',(-6.21213331202032,151.381249999405,
8.55026797822134));
#289993=CARTESIAN_POINT('Ctrl Pts',(-3.10606665601021,151.531249999404,
9.5594902125713));
#289994=CARTESIAN_POINT('Ctrl Pts',(-9.78898830926068E-14,151.681249999404,
10.5687124469213));
#289995=CARTESIAN_POINT('Ctrl Pts',(3.10606665601001,151.831249999403,9.5594902125713));
#289996=CARTESIAN_POINT('Ctrl Pts',(6.21213331202012,151.981249999403,8.55026797822134));
#289997=CARTESIAN_POINT('Ctrl Pts',(8.13178807675709,152.131249999402,5.90808986649102));
#289998=CARTESIAN_POINT('Ctrl Pts',(10.0514428414941,152.281249999401,3.2659117547607));
#289999=CARTESIAN_POINT('Ctrl Pts',(10.0514428414941,152.431249999401,-1.23094673026484E-15));
#290000=CARTESIAN_POINT('Ctrl Pts',(10.0514428414941,152.5812499994,-3.26591175476071));
#290001=CARTESIAN_POINT('Ctrl Pts',(8.13178807675709,152.7312499994,-5.90808986649102));
#290002=CARTESIAN_POINT('Ctrl Pts',(6.21213331202012,152.881249999399,-8.55026797822134));
#290003=CARTESIAN_POINT('Ctrl Pts',(3.10606665601001,153.031249999398,-9.5594902125713));
#290004=CARTESIAN_POINT('Ctrl Pts',(-1.01342325702284E-13,153.181249999398,
-10.5687124469213));
#290005=CARTESIAN_POINT('Ctrl Pts',(-3.10606665601021,153.331249999397,
-9.5594902125713));
#290006=CARTESIAN_POINT('',(-8.5091557340996,76.2,5.35030577524922));
#290007=CARTESIAN_POINT('Ctrl Pts',(11.7004490057565,76.2,2.66448739229326));
#290008=CARTESIAN_POINT('Ctrl Pts',(11.2736065385016,76.2,4.07643912420469));
#290009=CARTESIAN_POINT('Ctrl Pts',(10.5879289871897,76.2,5.39657685789075));
#290010=CARTESIAN_POINT('Ctrl Pts',(8.52767436642338,76.2,8.0266839054084));
#290011=CARTESIAN_POINT('Ctrl Pts',(7.30982467417011,76.2,8.87851993633569));
#290012=CARTESIAN_POINT('Ctrl Pts',(5.2040775105915,76.2,10.1043730632371));
#290013=CARTESIAN_POINT('Ctrl Pts',(3.83447247941545,76.2,10.5921419577076));
#290014=CARTESIAN_POINT('Ctrl Pts',(1.06742512277072,76.2,11.0007660700567));
#290015=CARTESIAN_POINT('Ctrl Pts',(-0.312663875595359,76.2,10.9428078138237));
#290016=CARTESIAN_POINT('Ctrl Pts',(-2.60282640207458,76.2,10.4049192800778));
#290017=CARTESIAN_POINT('Ctrl Pts',(-4.01317621566336,76.2,9.94321112964606));
#290018=CARTESIAN_POINT('Ctrl Pts',(-6.08753010305324,76.2,8.42910175872524));
#290019=CARTESIAN_POINT('Ctrl Pts',(-6.66541282594047,76.2,7.89712047013574));
#290020=CARTESIAN_POINT('Ctrl Pts',(-7.69093052494506,76.2,6.71162715330518));
#290021=CARTESIAN_POINT('Ctrl Pts',(-8.14368210712128,76.2,6.05166491645592));
#290022=CARTESIAN_POINT('Ctrl Pts',(-8.50915573409961,76.2,5.35030577524915));
#290023=CARTESIAN_POINT('Ctrl Pts',(10.0514428414941,74.4312499997127,-1.23094673026484E-15));
#290024=CARTESIAN_POINT('Ctrl Pts',(10.0514428414941,74.5812499997121,-3.26591175476071));
#290025=CARTESIAN_POINT('Ctrl Pts',(8.13178807675713,74.7312499997116,-5.90808986649102));
#290026=CARTESIAN_POINT('Ctrl Pts',(6.21213331202016,74.8812499997109,-8.55026797822134));
#290027=CARTESIAN_POINT('Ctrl Pts',(3.10606665601005,75.0312499997104,-9.5594902125713));
#290028=CARTESIAN_POINT('Ctrl Pts',(-5.6421884639076E-14,75.1812499997097,
-10.5687124469213));
#290029=CARTESIAN_POINT('Ctrl Pts',(-3.10606665601016,75.3312499997092,
-9.5594902125713));
#290030=CARTESIAN_POINT('Ctrl Pts',(-6.21213331202027,75.4812499997086,
-8.55026797822134));
#290031=CARTESIAN_POINT('Ctrl Pts',(-8.13178807675725,75.6312499997079,
-5.90808986649102));
#290032=CARTESIAN_POINT('Ctrl Pts',(-10.0514428414942,75.7812499997073,
-3.2659117547607));
#290033=CARTESIAN_POINT('Ctrl Pts',(-10.0514428414942,75.9312499997068,
2.46189346052968E-15));
#290034=CARTESIAN_POINT('Ctrl Pts',(-10.0514428414942,76.0643266453995,
2.89744387635823));
#290035=CARTESIAN_POINT('Ctrl Pts',(-8.5091557340996,76.2,5.35030577524922));
#290036=CARTESIAN_POINT('Origin',(-3.77475828372553E-14,-1.881249999982,
2.68644078414671E-15));
#290037=CARTESIAN_POINT('Origin',(-3.77475828372553E-14,76.2,2.03817200954814E-15));
#290038=CARTESIAN_POINT('Origin',(0.,76.2,0.));
#290039=CARTESIAN_POINT('Origin',(-3.77475828372553E-14,-1.881249999982,
2.68644078414671E-15));
#290040=CARTESIAN_POINT('',(10.0514428414942,2.80624999999926,1.43603509362624E-15));
#290041=CARTESIAN_POINT('',(10.0514428414942,2.43125000000076,-1.23094673026484E-15));
#290042=CARTESIAN_POINT('',(10.0514428414941,-1.881249999982,4.14193483802857E-15));
#290043=CARTESIAN_POINT('',(7.09357268597966,2.43124999999995,7.12128708482866));
#290044=CARTESIAN_POINT('Ctrl Pts',(7.09357268597966,2.43124999999995,7.12128708482865));
#290045=CARTESIAN_POINT('Ctrl Pts',(7.66101577103565,2.46946429917804,6.55605235674466));
#290046=CARTESIAN_POINT('Ctrl Pts',(8.13178807675718,2.50625000000046,5.90808986649102));
#290047=CARTESIAN_POINT('Ctrl Pts',(10.0514428414941,2.65624999999986,3.2659117547607));
#290048=CARTESIAN_POINT('Ctrl Pts',(10.0514428414942,2.80624999999926,-1.23094673026484E-15));
#290049=CARTESIAN_POINT('Origin',(-3.77475828372553E-14,2.43125000000001,
2.65063629727636E-15));
#290050=CARTESIAN_POINT('Origin',(-3.77475828372553E-14,-1.881249999982,
2.68644078414671E-15));
#290051=CARTESIAN_POINT('',(10.0514428414941,5.80624999998726,1.42358135906264E-15));
#290052=CARTESIAN_POINT('',(10.0514428414941,5.43124999998876,1.42513807588309E-15));
#290053=CARTESIAN_POINT('',(10.0514428414941,-1.881249999982,4.14193483802857E-15));
#290054=CARTESIAN_POINT('Ctrl Pts',(10.0514428414942,2.80624999999926,-1.23094673026484E-15));
#290055=CARTESIAN_POINT('Ctrl Pts',(10.0514428414941,2.95624999999866,-3.26591175476071));
#290056=CARTESIAN_POINT('Ctrl Pts',(8.13178807675718,3.10624999999806,-5.90808986649102));
#290057=CARTESIAN_POINT('Ctrl Pts',(6.2121333120202,3.25624999999746,-8.55026797822134));
#290058=CARTESIAN_POINT('Ctrl Pts',(3.10606665601009,3.40624999999685,-9.5594902125713));
#290059=CARTESIAN_POINT('Ctrl Pts',(-1.51728257781496E-14,3.55624999999625,
-10.5687124469213));
#290060=CARTESIAN_POINT('Ctrl Pts',(-3.10606665601012,3.70624999999565,
-9.5594902125713));
#290061=CARTESIAN_POINT('Ctrl Pts',(-6.21213331202023,3.85624999999505,
-8.55026797822134));
#290062=CARTESIAN_POINT('Ctrl Pts',(-8.13178807675721,4.00624999999445,
-5.90808986649102));
#290063=CARTESIAN_POINT('Ctrl Pts',(-10.0514428414942,4.15624999999385,
-3.2659117547607));
#290064=CARTESIAN_POINT('Ctrl Pts',(-10.0514428414942,4.30624999999325,
2.46189346052968E-15));
#290065=CARTESIAN_POINT('Ctrl Pts',(-10.0514428414942,4.45624999999265,
3.26591175476071));
#290066=CARTESIAN_POINT('Ctrl Pts',(-8.13178807675721,4.60624999999205,
5.90808986649102));
#290067=CARTESIAN_POINT('Ctrl Pts',(-6.21213331202023,4.75624999999145,
8.55026797822134));
#290068=CARTESIAN_POINT('Ctrl Pts',(-3.10606665601012,4.90624999999085,
9.5594902125713));
#290069=CARTESIAN_POINT('Ctrl Pts',(-1.34480924401344E-14,5.05624999999025,
10.5687124469213));
#290070=CARTESIAN_POINT('Ctrl Pts',(3.10606665601009,5.20624999998966,9.5594902125713));
#290071=CARTESIAN_POINT('Ctrl Pts',(6.2121333120202,5.35624999998906,8.55026797822134));
#290072=CARTESIAN_POINT('Ctrl Pts',(8.13178807675718,5.50624999998846,5.90808986649102));
#290073=CARTESIAN_POINT('Ctrl Pts',(10.0514428414941,5.65624999998786,3.2659117547607));
#290074=CARTESIAN_POINT('Ctrl Pts',(10.0514428414941,5.80624999998726,-1.23094673026484E-15));
#290075=CARTESIAN_POINT('Ctrl Pts',(10.0514428414942,2.43125000000076,-1.23094673026484E-15));
#290076=CARTESIAN_POINT('Ctrl Pts',(10.0514428414941,2.58125000000016,-3.26591175476071));
#290077=CARTESIAN_POINT('Ctrl Pts',(8.13178807675718,2.73124999999956,-5.90808986649102));
#290078=CARTESIAN_POINT('Ctrl Pts',(6.2121333120202,2.88124999999896,-8.55026797822134));
#290079=CARTESIAN_POINT('Ctrl Pts',(3.10606665601009,3.03124999999835,-9.5594902125713));
#290080=CARTESIAN_POINT('Ctrl Pts',(-1.49568621191919E-14,3.18124999999775,
-10.5687124469213));
#290081=CARTESIAN_POINT('Ctrl Pts',(-3.10606665601012,3.33124999999715,
-9.5594902125713));
#290082=CARTESIAN_POINT('Ctrl Pts',(-6.21213331202023,3.48124999999655,
-8.55026797822134));
#290083=CARTESIAN_POINT('Ctrl Pts',(-8.13178807675721,3.63124999999595,
-5.90808986649102));
#290084=CARTESIAN_POINT('Ctrl Pts',(-10.0514428414942,3.78124999999535,
-3.2659117547607));
#290085=CARTESIAN_POINT('Ctrl Pts',(-10.0514428414942,3.93124999999475,
2.46189346052968E-15));
#290086=CARTESIAN_POINT('Ctrl Pts',(-10.0514428414942,4.08124999999415,
3.26591175476071));
#290087=CARTESIAN_POINT('Ctrl Pts',(-8.13178807675721,4.23124999999355,
5.90808986649102));
#290088=CARTESIAN_POINT('Ctrl Pts',(-6.21213331202023,4.38124999999295,
8.55026797822134));
#290089=CARTESIAN_POINT('Ctrl Pts',(-3.10606665601012,4.53124999999235,
9.5594902125713));
#290090=CARTESIAN_POINT('Ctrl Pts',(-1.32321287811766E-14,4.68124999999175,
10.5687124469213));
#290091=CARTESIAN_POINT('Ctrl Pts',(3.10606665601009,4.83124999999115,9.5594902125713));
#290092=CARTESIAN_POINT('Ctrl Pts',(6.2121333120202,4.98124999999056,8.55026797822134));
#290093=CARTESIAN_POINT('Ctrl Pts',(8.13178807675718,5.13124999998996,5.90808986649102));
#290094=CARTESIAN_POINT('Ctrl Pts',(10.0514428414941,5.28124999998936,3.2659117547607));
#290095=CARTESIAN_POINT('Ctrl Pts',(10.0514428414941,5.43124999998876,-1.23094673026484E-15));
#290096=CARTESIAN_POINT('Origin',(-3.77475828372553E-14,-1.881249999982,
2.68644078414671E-15));
#290097=CARTESIAN_POINT('',(10.0514428414941,8.80624999997526,1.41112762449904E-15));
#290098=CARTESIAN_POINT('',(10.0514428414941,8.43124999997676,1.41268434131949E-15));
#290099=CARTESIAN_POINT('',(10.0514428414941,-1.881249999982,4.14193483802857E-15));
#290100=CARTESIAN_POINT('Ctrl Pts',(10.0514428414941,5.80624999998726,-1.23094673026484E-15));
#290101=CARTESIAN_POINT('Ctrl Pts',(10.0514428414941,5.95624999998666,-3.26591175476071));
#290102=CARTESIAN_POINT('Ctrl Pts',(8.13178807675717,6.10624999998606,-5.90808986649102));
#290103=CARTESIAN_POINT('Ctrl Pts',(6.2121333120202,6.25624999998545,-8.55026797822134));
#290104=CARTESIAN_POINT('Ctrl Pts',(3.10606665601009,6.40624999998485,-9.5594902125713));
#290105=CARTESIAN_POINT('Ctrl Pts',(-1.69005350498115E-14,6.55624999998425,
-10.5687124469213));
#290106=CARTESIAN_POINT('Ctrl Pts',(-3.10606665601013,6.70624999998365,
-9.5594902125713));
#290107=CARTESIAN_POINT('Ctrl Pts',(-6.21213331202023,6.85624999998305,
-8.55026797822134));
#290108=CARTESIAN_POINT('Ctrl Pts',(-8.13178807675721,7.00624999998245,
-5.90808986649102));
#290109=CARTESIAN_POINT('Ctrl Pts',(-10.0514428414942,7.15624999998185,
-3.2659117547607));
#290110=CARTESIAN_POINT('Ctrl Pts',(-10.0514428414942,7.30624999998125,
2.46189346052968E-15));
#290111=CARTESIAN_POINT('Ctrl Pts',(-10.0514428414942,7.45624999998065,
3.26591175476071));
#290112=CARTESIAN_POINT('Ctrl Pts',(-8.13178807675721,7.60624999998005,
5.90808986649102));
#290113=CARTESIAN_POINT('Ctrl Pts',(-6.21213331202023,7.75624999997945,
8.55026797822134));
#290114=CARTESIAN_POINT('Ctrl Pts',(-3.10606665601012,7.90624999997885,
9.5594902125713));
#290115=CARTESIAN_POINT('Ctrl Pts',(-1.51758017117962E-14,8.05624999997825,
10.5687124469213));
#290116=CARTESIAN_POINT('Ctrl Pts',(3.10606665601009,8.20624999997765,9.5594902125713));
#290117=CARTESIAN_POINT('Ctrl Pts',(6.2121333120202,8.35624999997706,8.55026797822134));
#290118=CARTESIAN_POINT('Ctrl Pts',(8.13178807675717,8.50624999997646,5.90808986649102));
#290119=CARTESIAN_POINT('Ctrl Pts',(10.0514428414941,8.65624999997586,3.2659117547607));
#290120=CARTESIAN_POINT('Ctrl Pts',(10.0514428414941,8.80624999997526,-1.23094673026484E-15));
#290121=CARTESIAN_POINT('Ctrl Pts',(10.0514428414941,5.43124999998876,-1.23094673026484E-15));
#290122=CARTESIAN_POINT('Ctrl Pts',(10.0514428414941,5.58124999998816,-3.26591175476071));
#290123=CARTESIAN_POINT('Ctrl Pts',(8.13178807675717,5.73124999998756,-5.90808986649102));
#290124=CARTESIAN_POINT('Ctrl Pts',(6.2121333120202,5.88124999998695,-8.55026797822134));
#290125=CARTESIAN_POINT('Ctrl Pts',(3.10606665601009,6.03124999998635,-9.5594902125713));
#290126=CARTESIAN_POINT('Ctrl Pts',(-1.66845713908537E-14,6.18124999998575,
-10.5687124469213));
#290127=CARTESIAN_POINT('Ctrl Pts',(-3.10606665601012,6.33124999998515,
-9.5594902125713));
#290128=CARTESIAN_POINT('Ctrl Pts',(-6.21213331202023,6.48124999998455,
-8.55026797822134));
#290129=CARTESIAN_POINT('Ctrl Pts',(-8.13178807675721,6.63124999998395,
-5.90808986649102));
#290130=CARTESIAN_POINT('Ctrl Pts',(-10.0514428414942,6.78124999998335,
-3.2659117547607));
#290131=CARTESIAN_POINT('Ctrl Pts',(-10.0514428414942,6.93124999998275,
2.46189346052968E-15));
#290132=CARTESIAN_POINT('Ctrl Pts',(-10.0514428414942,7.08124999998215,
3.26591175476071));
#290133=CARTESIAN_POINT('Ctrl Pts',(-8.13178807675721,7.23124999998155,
5.90808986649102));
#290134=CARTESIAN_POINT('Ctrl Pts',(-6.21213331202023,7.38124999998095,
8.55026797822134));
#290135=CARTESIAN_POINT('Ctrl Pts',(-3.10606665601012,7.53124999998035,
9.5594902125713));
#290136=CARTESIAN_POINT('Ctrl Pts',(-1.49598380528385E-14,7.68124999997975,
10.5687124469213));
#290137=CARTESIAN_POINT('Ctrl Pts',(3.10606665601009,7.83124999997915,9.5594902125713));
#290138=CARTESIAN_POINT('Ctrl Pts',(6.2121333120202,7.98124999997856,8.55026797822134));
#290139=CARTESIAN_POINT('Ctrl Pts',(8.13178807675717,8.13124999997796,5.90808986649102));
#290140=CARTESIAN_POINT('Ctrl Pts',(10.0514428414941,8.28124999997736,3.2659117547607));
#290141=CARTESIAN_POINT('Ctrl Pts',(10.0514428414941,8.43124999997676,-1.23094673026484E-15));
#290142=CARTESIAN_POINT('Origin',(-3.77475828372553E-14,-1.881249999982,
2.68644078414671E-15));
#290143=CARTESIAN_POINT('',(10.0514428414941,11.8062499999633,1.39867388993544E-15));
#290144=CARTESIAN_POINT('',(10.0514428414941,11.4312499999648,1.40023060675589E-15));
#290145=CARTESIAN_POINT('',(10.0514428414941,-1.881249999982,4.14193483802857E-15));
#290146=CARTESIAN_POINT('Ctrl Pts',(10.0514428414941,8.80624999997526,-1.23094673026484E-15));
#290147=CARTESIAN_POINT('Ctrl Pts',(10.0514428414941,8.95624999997466,-3.26591175476071));
#290148=CARTESIAN_POINT('Ctrl Pts',(8.13178807675717,9.10624999997406,-5.90808986649102));
#290149=CARTESIAN_POINT('Ctrl Pts',(6.2121333120202,9.25624999997346,-8.55026797822134));
#290150=CARTESIAN_POINT('Ctrl Pts',(3.10606665601009,9.40624999997286,-9.5594902125713));
#290151=CARTESIAN_POINT('Ctrl Pts',(-1.86282443214733E-14,9.55624999997225,
-10.5687124469213));
#290152=CARTESIAN_POINT('Ctrl Pts',(-3.10606665601013,9.70624999997165,
-9.5594902125713));
#290153=CARTESIAN_POINT('Ctrl Pts',(-6.21213331202024,9.85624999997105,
-8.55026797822134));
#290154=CARTESIAN_POINT('Ctrl Pts',(-8.13178807675721,10.0062499999704,
-5.90808986649102));
#290155=CARTESIAN_POINT('Ctrl Pts',(-10.0514428414942,10.1562499999698,
-3.2659117547607));
#290156=CARTESIAN_POINT('Ctrl Pts',(-10.0514428414942,10.3062499999692,
2.46189346052968E-15));
#290157=CARTESIAN_POINT('Ctrl Pts',(-10.0514428414942,10.4562499999686,
3.26591175476071));
#290158=CARTESIAN_POINT('Ctrl Pts',(-8.13178807675721,10.606249999968,5.90808986649102));
#290159=CARTESIAN_POINT('Ctrl Pts',(-6.21213331202023,10.7562499999674,
8.55026797822134));
#290160=CARTESIAN_POINT('Ctrl Pts',(-3.10606665601013,10.9062499999668,
9.5594902125713));
#290161=CARTESIAN_POINT('Ctrl Pts',(-1.6903510983458E-14,11.0562499999663,
10.5687124469213));
#290162=CARTESIAN_POINT('Ctrl Pts',(3.10606665601009,11.2062499999657,9.5594902125713));
#290163=CARTESIAN_POINT('Ctrl Pts',(6.2121333120202,11.3562499999651,8.55026797822134));
#290164=CARTESIAN_POINT('Ctrl Pts',(8.13178807675717,11.5062499999645,5.90808986649102));
#290165=CARTESIAN_POINT('Ctrl Pts',(10.0514428414941,11.6562499999639,3.2659117547607));
#290166=CARTESIAN_POINT('Ctrl Pts',(10.0514428414941,11.8062499999633,-1.23094673026484E-15));
#290167=CARTESIAN_POINT('Ctrl Pts',(10.0514428414941,8.43124999997676,-1.23094673026484E-15));
#290168=CARTESIAN_POINT('Ctrl Pts',(10.0514428414941,8.58124999997616,-3.26591175476071));
#290169=CARTESIAN_POINT('Ctrl Pts',(8.13178807675717,8.73124999997556,-5.90808986649102));
#290170=CARTESIAN_POINT('Ctrl Pts',(6.2121333120202,8.88124999997496,-8.55026797822134));
#290171=CARTESIAN_POINT('Ctrl Pts',(3.10606665601009,9.03124999997436,-9.5594902125713));
#290172=CARTESIAN_POINT('Ctrl Pts',(-1.84122806625156E-14,9.18124999997375,
-10.5687124469213));
#290173=CARTESIAN_POINT('Ctrl Pts',(-3.10606665601013,9.33124999997315,
-9.5594902125713));
#290174=CARTESIAN_POINT('Ctrl Pts',(-6.21213331202024,9.48124999997255,
-8.55026797822134));
#290175=CARTESIAN_POINT('Ctrl Pts',(-8.13178807675721,9.63124999997195,
-5.90808986649102));
#290176=CARTESIAN_POINT('Ctrl Pts',(-10.0514428414942,9.78124999997135,
-3.2659117547607));
#290177=CARTESIAN_POINT('Ctrl Pts',(-10.0514428414942,9.93124999997075,
2.46189346052968E-15));
#290178=CARTESIAN_POINT('Ctrl Pts',(-10.0514428414942,10.0812499999701,
3.26591175476071));
#290179=CARTESIAN_POINT('Ctrl Pts',(-8.13178807675721,10.2312499999695,
5.90808986649102));
#290180=CARTESIAN_POINT('Ctrl Pts',(-6.21213331202023,10.3812499999689,
8.55026797822134));
#290181=CARTESIAN_POINT('Ctrl Pts',(-3.10606665601012,10.5312499999684,
9.5594902125713));
#290182=CARTESIAN_POINT('Ctrl Pts',(-1.66875473245003E-14,10.6812499999678,
10.5687124469213));
#290183=CARTESIAN_POINT('Ctrl Pts',(3.10606665601009,10.8312499999672,9.5594902125713));
#290184=CARTESIAN_POINT('Ctrl Pts',(6.2121333120202,10.9812499999666,8.55026797822134));
#290185=CARTESIAN_POINT('Ctrl Pts',(8.13178807675717,11.131249999966,5.90808986649102));
#290186=CARTESIAN_POINT('Ctrl Pts',(10.0514428414941,11.2812499999654,3.2659117547607));
#290187=CARTESIAN_POINT('Ctrl Pts',(10.0514428414941,11.4312499999648,-1.23094673026484E-15));
#290188=CARTESIAN_POINT('Origin',(-3.77475828372553E-14,-1.881249999982,
2.68644078414671E-15));
#290189=CARTESIAN_POINT('',(10.0514428414941,14.8062499999513,1.38622015537184E-15));
#290190=CARTESIAN_POINT('',(10.0514428414941,14.4312499999528,1.38777687219229E-15));
#290191=CARTESIAN_POINT('',(10.0514428414941,-1.881249999982,4.14193483802857E-15));
#290192=CARTESIAN_POINT('Ctrl Pts',(10.0514428414941,11.8062499999633,-1.23094673026484E-15));
#290193=CARTESIAN_POINT('Ctrl Pts',(10.0514428414941,11.9562499999627,-3.26591175476071));
#290194=CARTESIAN_POINT('Ctrl Pts',(8.13178807675717,12.1062499999621,-5.90808986649102));
#290195=CARTESIAN_POINT('Ctrl Pts',(6.2121333120202,12.2562499999615,-8.55026797822134));
#290196=CARTESIAN_POINT('Ctrl Pts',(3.10606665601009,12.4062499999609,-9.5594902125713));
#290197=CARTESIAN_POINT('Ctrl Pts',(-2.03559535931351E-14,12.5562499999603,
-10.5687124469213));
#290198=CARTESIAN_POINT('Ctrl Pts',(-3.10606665601013,12.7062499999597,
-9.5594902125713));
#290199=CARTESIAN_POINT('Ctrl Pts',(-6.21213331202024,12.856249999959,-8.55026797822134));
#290200=CARTESIAN_POINT('Ctrl Pts',(-8.13178807675721,13.0062499999584,
-5.90808986649102));
#290201=CARTESIAN_POINT('Ctrl Pts',(-10.0514428414942,13.1562499999578,
-3.2659117547607));
#290202=CARTESIAN_POINT('Ctrl Pts',(-10.0514428414942,13.3062499999572,
2.46189346052968E-15));
#290203=CARTESIAN_POINT('Ctrl Pts',(-10.0514428414942,13.4562499999566,
3.26591175476071));
#290204=CARTESIAN_POINT('Ctrl Pts',(-8.13178807675721,13.606249999956,5.90808986649102));
#290205=CARTESIAN_POINT('Ctrl Pts',(-6.21213331202023,13.7562499999554,
8.55026797822134));
#290206=CARTESIAN_POINT('Ctrl Pts',(-3.10606665601013,13.9062499999549,
9.5594902125713));
#290207=CARTESIAN_POINT('Ctrl Pts',(-1.86312202551199E-14,14.0562499999543,
10.5687124469213));
#290208=CARTESIAN_POINT('Ctrl Pts',(3.10606665601009,14.2062499999537,9.5594902125713));
#290209=CARTESIAN_POINT('Ctrl Pts',(6.2121333120202,14.3562499999531,8.55026797822134));
#290210=CARTESIAN_POINT('Ctrl Pts',(8.13178807675717,14.5062499999525,5.90808986649102));
#290211=CARTESIAN_POINT('Ctrl Pts',(10.0514428414941,14.6562499999519,3.2659117547607));
#290212=CARTESIAN_POINT('Ctrl Pts',(10.0514428414941,14.8062499999513,-1.23094673026484E-15));
#290213=CARTESIAN_POINT('Ctrl Pts',(10.0514428414941,11.4312499999648,-1.23094673026484E-15));
#290214=CARTESIAN_POINT('Ctrl Pts',(10.0514428414941,11.5812499999642,-3.26591175476071));
#290215=CARTESIAN_POINT('Ctrl Pts',(8.13178807675717,11.7312499999636,-5.90808986649102));
#290216=CARTESIAN_POINT('Ctrl Pts',(6.2121333120202,11.881249999963,-8.55026797822134));
#290217=CARTESIAN_POINT('Ctrl Pts',(3.10606665601009,12.0312499999624,-9.5594902125713));
#290218=CARTESIAN_POINT('Ctrl Pts',(-2.01399899341774E-14,12.1812499999618,
-10.5687124469213));
#290219=CARTESIAN_POINT('Ctrl Pts',(-3.10606665601013,12.3312499999612,
-9.5594902125713));
#290220=CARTESIAN_POINT('Ctrl Pts',(-6.21213331202024,12.4812499999605,
-8.55026797822134));
#290221=CARTESIAN_POINT('Ctrl Pts',(-8.13178807675721,12.6312499999599,
-5.90808986649102));
#290222=CARTESIAN_POINT('Ctrl Pts',(-10.0514428414942,12.7812499999593,
-3.2659117547607));
#290223=CARTESIAN_POINT('Ctrl Pts',(-10.0514428414942,12.9312499999587,
2.46189346052968E-15));
#290224=CARTESIAN_POINT('Ctrl Pts',(-10.0514428414942,13.0812499999581,
3.26591175476071));
#290225=CARTESIAN_POINT('Ctrl Pts',(-8.13178807675721,13.2312499999575,
5.90808986649102));
#290226=CARTESIAN_POINT('Ctrl Pts',(-6.21213331202023,13.3812499999569,
8.55026797822134));
#290227=CARTESIAN_POINT('Ctrl Pts',(-3.10606665601013,13.5312499999564,
9.5594902125713));
#290228=CARTESIAN_POINT('Ctrl Pts',(-1.84152565961621E-14,13.6812499999558,
10.5687124469213));
#290229=CARTESIAN_POINT('Ctrl Pts',(3.10606665601009,13.8312499999552,9.5594902125713));
#290230=CARTESIAN_POINT('Ctrl Pts',(6.2121333120202,13.9812499999546,8.55026797822134));
#290231=CARTESIAN_POINT('Ctrl Pts',(8.13178807675717,14.131249999954,5.90808986649102));
#290232=CARTESIAN_POINT('Ctrl Pts',(10.0514428414941,14.2812499999534,3.2659117547607));
#290233=CARTESIAN_POINT('Ctrl Pts',(10.0514428414941,14.4312499999528,-1.23094673026484E-15));
#290234=CARTESIAN_POINT('Origin',(-3.77475828372553E-14,-1.881249999982,
2.68644078414671E-15));
#290235=CARTESIAN_POINT('',(10.0514428414941,17.8062499999393,1.37376642080824E-15));
#290236=CARTESIAN_POINT('',(10.0514428414941,17.4312499999408,1.37532313762869E-15));
#290237=CARTESIAN_POINT('',(10.0514428414941,-1.881249999982,4.14193483802857E-15));
#290238=CARTESIAN_POINT('Ctrl Pts',(10.0514428414941,14.8062499999513,-1.23094673026484E-15));
#290239=CARTESIAN_POINT('Ctrl Pts',(10.0514428414941,14.9562499999507,-3.26591175476071));
#290240=CARTESIAN_POINT('Ctrl Pts',(8.13178807675717,15.1062499999501,-5.90808986649102));
#290241=CARTESIAN_POINT('Ctrl Pts',(6.21213331202019,15.2562499999495,-8.55026797822134));
#290242=CARTESIAN_POINT('Ctrl Pts',(3.10606665601009,15.4062499999489,-9.5594902125713));
#290243=CARTESIAN_POINT('Ctrl Pts',(-2.2083662864797E-14,15.5562499999482,
-10.5687124469213));
#290244=CARTESIAN_POINT('Ctrl Pts',(-3.10606665601013,15.7062499999477,
-9.5594902125713));
#290245=CARTESIAN_POINT('Ctrl Pts',(-6.21213331202024,15.856249999947,-8.55026797822134));
#290246=CARTESIAN_POINT('Ctrl Pts',(-8.13178807675721,16.0062499999464,
-5.90808986649102));
#290247=CARTESIAN_POINT('Ctrl Pts',(-10.0514428414942,16.1562499999458,
-3.2659117547607));
#290248=CARTESIAN_POINT('Ctrl Pts',(-10.0514428414942,16.3062499999452,
2.46189346052968E-15));
#290249=CARTESIAN_POINT('Ctrl Pts',(-10.0514428414942,16.4562499999446,
3.26591175476071));
#290250=CARTESIAN_POINT('Ctrl Pts',(-8.13178807675721,16.606249999944,5.90808986649102));
#290251=CARTESIAN_POINT('Ctrl Pts',(-6.21213331202024,16.7562499999434,
8.55026797822134));
#290252=CARTESIAN_POINT('Ctrl Pts',(-3.10606665601013,16.9062499999428,
9.5594902125713));
#290253=CARTESIAN_POINT('Ctrl Pts',(-2.03589295267817E-14,17.0562499999422,
10.5687124469213));
#290254=CARTESIAN_POINT('Ctrl Pts',(3.10606665601009,17.2062499999417,9.5594902125713));
#290255=CARTESIAN_POINT('Ctrl Pts',(6.2121333120202,17.3562499999411,8.55026797822134));
#290256=CARTESIAN_POINT('Ctrl Pts',(8.13178807675717,17.5062499999405,5.90808986649102));
#290257=CARTESIAN_POINT('Ctrl Pts',(10.0514428414941,17.6562499999399,3.2659117547607));
#290258=CARTESIAN_POINT('Ctrl Pts',(10.0514428414941,17.8062499999393,-1.23094673026484E-15));
#290259=CARTESIAN_POINT('Ctrl Pts',(10.0514428414941,14.4312499999528,-1.23094673026484E-15));
#290260=CARTESIAN_POINT('Ctrl Pts',(10.0514428414941,14.5812499999522,-3.26591175476071));
#290261=CARTESIAN_POINT('Ctrl Pts',(8.13178807675717,14.7312499999516,-5.90808986649102));
#290262=CARTESIAN_POINT('Ctrl Pts',(6.21213331202019,14.881249999951,-8.55026797822134));
#290263=CARTESIAN_POINT('Ctrl Pts',(3.10606665601009,15.0312499999504,-9.5594902125713));
#290264=CARTESIAN_POINT('Ctrl Pts',(-2.18676992058392E-14,15.1812499999498,
-10.5687124469213));
#290265=CARTESIAN_POINT('Ctrl Pts',(-3.10606665601013,15.3312499999492,
-9.5594902125713));
#290266=CARTESIAN_POINT('Ctrl Pts',(-6.21213331202024,15.4812499999485,
-8.55026797822134));
#290267=CARTESIAN_POINT('Ctrl Pts',(-8.13178807675721,15.6312499999479,
-5.90808986649102));
#290268=CARTESIAN_POINT('Ctrl Pts',(-10.0514428414942,15.7812499999473,
-3.2659117547607));
#290269=CARTESIAN_POINT('Ctrl Pts',(-10.0514428414942,15.9312499999467,
2.46189346052968E-15));
#290270=CARTESIAN_POINT('Ctrl Pts',(-10.0514428414942,16.0812499999461,
3.26591175476071));
#290271=CARTESIAN_POINT('Ctrl Pts',(-8.13178807675721,16.2312499999455,
5.90808986649102));
#290272=CARTESIAN_POINT('Ctrl Pts',(-6.21213331202024,16.3812499999449,
8.55026797822134));
#290273=CARTESIAN_POINT('Ctrl Pts',(-3.10606665601013,16.5312499999444,
9.5594902125713));
#290274=CARTESIAN_POINT('Ctrl Pts',(-2.0142965867824E-14,16.6812499999438,
10.5687124469213));
#290275=CARTESIAN_POINT('Ctrl Pts',(3.10606665601009,16.8312499999432,9.5594902125713));
#290276=CARTESIAN_POINT('Ctrl Pts',(6.2121333120202,16.9812499999426,8.55026797822134));
#290277=CARTESIAN_POINT('Ctrl Pts',(8.13178807675717,17.131249999942,5.90808986649102));
#290278=CARTESIAN_POINT('Ctrl Pts',(10.0514428414941,17.2812499999414,3.2659117547607));
#290279=CARTESIAN_POINT('Ctrl Pts',(10.0514428414941,17.4312499999408,-1.23094673026484E-15));
#290280=CARTESIAN_POINT('Origin',(-3.77475828372553E-14,-1.881249999982,
2.68644078414671E-15));
#290281=CARTESIAN_POINT('',(10.0514428414941,20.8062499999273,1.36131268624463E-15));
#290282=CARTESIAN_POINT('',(10.0514428414941,20.4312499999288,1.36286940306508E-15));
#290283=CARTESIAN_POINT('',(10.0514428414941,-1.881249999982,4.14193483802857E-15));
#290284=CARTESIAN_POINT('Ctrl Pts',(10.0514428414941,17.8062499999393,-1.23094673026484E-15));
#290285=CARTESIAN_POINT('Ctrl Pts',(10.0514428414941,17.9562499999387,-3.26591175476071));
#290286=CARTESIAN_POINT('Ctrl Pts',(8.13178807675717,18.1062499999381,-5.90808986649102));
#290287=CARTESIAN_POINT('Ctrl Pts',(6.21213331202019,18.2562499999375,-8.55026797822134));
#290288=CARTESIAN_POINT('Ctrl Pts',(3.10606665601008,18.4062499999369,-9.5594902125713));
#290289=CARTESIAN_POINT('Ctrl Pts',(-2.38113721364588E-14,18.5562499999362,
-10.5687124469213));
#290290=CARTESIAN_POINT('Ctrl Pts',(-3.10606665601013,18.7062499999357,
-9.5594902125713));
#290291=CARTESIAN_POINT('Ctrl Pts',(-6.21213331202024,18.856249999935,-8.55026797822134));
#290292=CARTESIAN_POINT('Ctrl Pts',(-8.13178807675721,19.0062499999344,
-5.90808986649102));
#290293=CARTESIAN_POINT('Ctrl Pts',(-10.0514428414942,19.1562499999338,
-3.2659117547607));
#290294=CARTESIAN_POINT('Ctrl Pts',(-10.0514428414942,19.3062499999332,
2.46189346052968E-15));
#290295=CARTESIAN_POINT('Ctrl Pts',(-10.0514428414942,19.4562499999326,
3.26591175476071));
#290296=CARTESIAN_POINT('Ctrl Pts',(-8.13178807675721,19.606249999932,5.90808986649102));
#290297=CARTESIAN_POINT('Ctrl Pts',(-6.21213331202024,19.7562499999314,
8.55026797822134));
#290298=CARTESIAN_POINT('Ctrl Pts',(-3.10606665601013,19.9062499999308,
9.5594902125713));
#290299=CARTESIAN_POINT('Ctrl Pts',(-2.20866387984436E-14,20.0562499999302,
10.5687124469213));
#290300=CARTESIAN_POINT('Ctrl Pts',(3.10606665601009,20.2062499999297,9.5594902125713));
#290301=CARTESIAN_POINT('Ctrl Pts',(6.21213331202019,20.356249999929,8.55026797822134));
#290302=CARTESIAN_POINT('Ctrl Pts',(8.13178807675717,20.5062499999285,5.90808986649102));
#290303=CARTESIAN_POINT('Ctrl Pts',(10.0514428414941,20.6562499999279,3.2659117547607));
#290304=CARTESIAN_POINT('Ctrl Pts',(10.0514428414941,20.8062499999273,-1.23094673026484E-15));
#290305=CARTESIAN_POINT('Ctrl Pts',(10.0514428414941,17.4312499999408,-1.23094673026484E-15));
#290306=CARTESIAN_POINT('Ctrl Pts',(10.0514428414941,17.5812499999402,-3.26591175476071));
#290307=CARTESIAN_POINT('Ctrl Pts',(8.13178807675717,17.7312499999396,-5.90808986649102));
#290308=CARTESIAN_POINT('Ctrl Pts',(6.21213331202019,17.881249999939,-8.55026797822134));
#290309=CARTESIAN_POINT('Ctrl Pts',(3.10606665601008,18.0312499999384,-9.5594902125713));
#290310=CARTESIAN_POINT('Ctrl Pts',(-2.35954084775011E-14,18.1812499999378,
-10.5687124469213));
#290311=CARTESIAN_POINT('Ctrl Pts',(-3.10606665601013,18.3312499999371,
-9.5594902125713));
#290312=CARTESIAN_POINT('Ctrl Pts',(-6.21213331202024,18.4812499999365,
-8.55026797822134));
#290313=CARTESIAN_POINT('Ctrl Pts',(-8.13178807675721,18.6312499999359,
-5.90808986649102));
#290314=CARTESIAN_POINT('Ctrl Pts',(-10.0514428414942,18.7812499999353,
-3.2659117547607));
#290315=CARTESIAN_POINT('Ctrl Pts',(-10.0514428414942,18.9312499999347,
2.46189346052968E-15));
#290316=CARTESIAN_POINT('Ctrl Pts',(-10.0514428414942,19.0812499999341,
3.26591175476071));
#290317=CARTESIAN_POINT('Ctrl Pts',(-8.13178807675721,19.2312499999335,
5.90808986649102));
#290318=CARTESIAN_POINT('Ctrl Pts',(-6.21213331202024,19.3812499999329,
8.55026797822134));
#290319=CARTESIAN_POINT('Ctrl Pts',(-3.10606665601013,19.5312499999323,
9.5594902125713));
#290320=CARTESIAN_POINT('Ctrl Pts',(-2.18706751394858E-14,19.6812499999318,
10.5687124469213));
#290321=CARTESIAN_POINT('Ctrl Pts',(3.10606665601009,19.8312499999312,9.5594902125713));
#290322=CARTESIAN_POINT('Ctrl Pts',(6.21213331202019,19.9812499999306,8.55026797822134));
#290323=CARTESIAN_POINT('Ctrl Pts',(8.13178807675717,20.13124999993,5.90808986649102));
#290324=CARTESIAN_POINT('Ctrl Pts',(10.0514428414941,20.2812499999294,3.2659117547607));
#290325=CARTESIAN_POINT('Ctrl Pts',(10.0514428414941,20.4312499999288,-1.23094673026484E-15));
#290326=CARTESIAN_POINT('Origin',(-3.77475828372553E-14,-1.881249999982,
2.68644078414671E-15));
#290327=CARTESIAN_POINT('',(10.0514428414941,23.8062499999153,1.34885895168103E-15));
#290328=CARTESIAN_POINT('',(10.0514428414941,23.4312499999168,1.35041566850148E-15));
#290329=CARTESIAN_POINT('',(10.0514428414941,-1.881249999982,4.14193483802857E-15));
#290330=CARTESIAN_POINT('Ctrl Pts',(10.0514428414941,20.8062499999273,-1.23094673026484E-15));
#290331=CARTESIAN_POINT('Ctrl Pts',(10.0514428414941,20.9562499999267,-3.26591175476071));
#290332=CARTESIAN_POINT('Ctrl Pts',(8.13178807675716,21.1062499999261,-5.90808986649102));
#290333=CARTESIAN_POINT('Ctrl Pts',(6.21213331202019,21.2562499999255,-8.55026797822134));
#290334=CARTESIAN_POINT('Ctrl Pts',(3.10606665601008,21.4062499999249,-9.5594902125713));
#290335=CARTESIAN_POINT('Ctrl Pts',(-2.55390814081206E-14,21.5562499999242,
-10.5687124469213));
#290336=CARTESIAN_POINT('Ctrl Pts',(-3.10606665601013,21.7062499999237,
-9.5594902125713));
#290337=CARTESIAN_POINT('Ctrl Pts',(-6.21213331202024,21.856249999923,-8.55026797822134));
#290338=CARTESIAN_POINT('Ctrl Pts',(-8.13178807675722,22.0062499999224,
-5.90808986649102));
#290339=CARTESIAN_POINT('Ctrl Pts',(-10.0514428414942,22.1562499999218,
-3.2659117547607));
#290340=CARTESIAN_POINT('Ctrl Pts',(-10.0514428414942,22.3062499999212,
2.46189346052968E-15));
#290341=CARTESIAN_POINT('Ctrl Pts',(-10.0514428414942,22.4562499999206,
3.26591175476071));
#290342=CARTESIAN_POINT('Ctrl Pts',(-8.13178807675722,22.60624999992,5.90808986649102));
#290343=CARTESIAN_POINT('Ctrl Pts',(-6.21213331202024,22.7562499999194,
8.55026797822134));
#290344=CARTESIAN_POINT('Ctrl Pts',(-3.10606665601013,22.9062499999188,
9.5594902125713));
#290345=CARTESIAN_POINT('Ctrl Pts',(-2.38143480701054E-14,23.0562499999182,
10.5687124469213));
#290346=CARTESIAN_POINT('Ctrl Pts',(3.10606665601008,23.2062499999177,9.5594902125713));
#290347=CARTESIAN_POINT('Ctrl Pts',(6.21213331202019,23.3562499999171,8.55026797822134));
#290348=CARTESIAN_POINT('Ctrl Pts',(8.13178807675716,23.5062499999165,5.90808986649102));
#290349=CARTESIAN_POINT('Ctrl Pts',(10.0514428414941,23.6562499999159,3.2659117547607));
#290350=CARTESIAN_POINT('Ctrl Pts',(10.0514428414941,23.8062499999153,-1.23094673026484E-15));
#290351=CARTESIAN_POINT('Ctrl Pts',(10.0514428414941,20.4312499999288,-1.23094673026484E-15));
#290352=CARTESIAN_POINT('Ctrl Pts',(10.0514428414941,20.5812499999282,-3.26591175476071));
#290353=CARTESIAN_POINT('Ctrl Pts',(8.13178807675716,20.7312499999276,-5.90808986649102));
#290354=CARTESIAN_POINT('Ctrl Pts',(6.21213331202019,20.881249999927,-8.55026797822134));
#290355=CARTESIAN_POINT('Ctrl Pts',(3.10606665601008,21.0312499999264,-9.5594902125713));
#290356=CARTESIAN_POINT('Ctrl Pts',(-2.53231177491629E-14,21.1812499999258,
-10.5687124469213));
#290357=CARTESIAN_POINT('Ctrl Pts',(-3.10606665601013,21.3312499999251,
-9.5594902125713));
#290358=CARTESIAN_POINT('Ctrl Pts',(-6.21213331202024,21.4812499999245,
-8.55026797822134));
#290359=CARTESIAN_POINT('Ctrl Pts',(-8.13178807675722,21.6312499999239,
-5.90808986649102));
#290360=CARTESIAN_POINT('Ctrl Pts',(-10.0514428414942,21.7812499999233,
-3.2659117547607));
#290361=CARTESIAN_POINT('Ctrl Pts',(-10.0514428414942,21.9312499999227,
2.46189346052968E-15));
#290362=CARTESIAN_POINT('Ctrl Pts',(-10.0514428414942,22.0812499999221,
3.26591175476071));
#290363=CARTESIAN_POINT('Ctrl Pts',(-8.13178807675722,22.2312499999215,
5.90808986649102));
#290364=CARTESIAN_POINT('Ctrl Pts',(-6.21213331202024,22.3812499999209,
8.55026797822134));
#290365=CARTESIAN_POINT('Ctrl Pts',(-3.10606665601013,22.5312499999204,
9.5594902125713));
#290366=CARTESIAN_POINT('Ctrl Pts',(-2.35983844111477E-14,22.6812499999198,
10.5687124469213));
#290367=CARTESIAN_POINT('Ctrl Pts',(3.10606665601008,22.8312499999192,9.5594902125713));
#290368=CARTESIAN_POINT('Ctrl Pts',(6.21213331202019,22.9812499999186,8.55026797822134));
#290369=CARTESIAN_POINT('Ctrl Pts',(8.13178807675716,23.131249999918,5.90808986649102));
#290370=CARTESIAN_POINT('Ctrl Pts',(10.0514428414941,23.2812499999174,3.2659117547607));
#290371=CARTESIAN_POINT('Ctrl Pts',(10.0514428414941,23.4312499999168,-1.23094673026484E-15));
#290372=CARTESIAN_POINT('Origin',(-3.77475828372553E-14,-1.881249999982,
2.68644078414671E-15));
#290373=CARTESIAN_POINT('',(10.0514428414941,26.8062499999033,1.33640521711743E-15));
#290374=CARTESIAN_POINT('',(10.0514428414941,26.4312499999048,1.33796193393788E-15));
#290375=CARTESIAN_POINT('',(10.0514428414941,-1.881249999982,4.14193483802857E-15));
#290376=CARTESIAN_POINT('Ctrl Pts',(10.0514428414941,23.8062499999153,-1.23094673026484E-15));
#290377=CARTESIAN_POINT('Ctrl Pts',(10.0514428414941,23.9562499999147,-3.26591175476071));
#290378=CARTESIAN_POINT('Ctrl Pts',(8.13178807675716,24.1062499999141,-5.90808986649102));
#290379=CARTESIAN_POINT('Ctrl Pts',(6.21213331202019,24.2562499999135,-8.55026797822134));
#290380=CARTESIAN_POINT('Ctrl Pts',(3.10606665601008,24.4062499999129,-9.5594902125713));
#290381=CARTESIAN_POINT('Ctrl Pts',(-2.72667906797825E-14,24.5562499999122,
-10.5687124469213));
#290382=CARTESIAN_POINT('Ctrl Pts',(-3.10606665601014,24.7062499999116,
-9.5594902125713));
#290383=CARTESIAN_POINT('Ctrl Pts',(-6.21213331202024,24.856249999911,-8.55026797822134));
#290384=CARTESIAN_POINT('Ctrl Pts',(-8.13178807675722,25.0062499999104,
-5.90808986649102));
#290385=CARTESIAN_POINT('Ctrl Pts',(-10.0514428414942,25.1562499999098,
-3.2659117547607));
#290386=CARTESIAN_POINT('Ctrl Pts',(-10.0514428414942,25.3062499999092,
2.46189346052968E-15));
#290387=CARTESIAN_POINT('Ctrl Pts',(-10.0514428414942,25.4562499999086,
3.26591175476071));
#290388=CARTESIAN_POINT('Ctrl Pts',(-8.13178807675722,25.6062499999081,
5.90808986649102));
#290389=CARTESIAN_POINT('Ctrl Pts',(-6.21213331202024,25.7562499999074,
8.55026797822134));
#290390=CARTESIAN_POINT('Ctrl Pts',(-3.10606665601013,25.9062499999069,
9.5594902125713));
#290391=CARTESIAN_POINT('Ctrl Pts',(-2.55420573417672E-14,26.0562499999062,
10.5687124469213));
#290392=CARTESIAN_POINT('Ctrl Pts',(3.10606665601008,26.2062499999057,9.5594902125713));
#290393=CARTESIAN_POINT('Ctrl Pts',(6.21213331202019,26.356249999905,8.55026797822134));
#290394=CARTESIAN_POINT('Ctrl Pts',(8.13178807675716,26.5062499999045,5.90808986649102));
#290395=CARTESIAN_POINT('Ctrl Pts',(10.0514428414941,26.6562499999039,3.2659117547607));
#290396=CARTESIAN_POINT('Ctrl Pts',(10.0514428414941,26.8062499999033,-1.23094673026484E-15));
#290397=CARTESIAN_POINT('Ctrl Pts',(10.0514428414941,23.4312499999168,-1.23094673026484E-15));
#290398=CARTESIAN_POINT('Ctrl Pts',(10.0514428414941,23.5812499999162,-3.26591175476071));
#290399=CARTESIAN_POINT('Ctrl Pts',(8.13178807675716,23.7312499999156,-5.90808986649102));
#290400=CARTESIAN_POINT('Ctrl Pts',(6.21213331202019,23.881249999915,-8.55026797822134));
#290401=CARTESIAN_POINT('Ctrl Pts',(3.10606665601008,24.0312499999144,-9.5594902125713));
#290402=CARTESIAN_POINT('Ctrl Pts',(-2.70508270208248E-14,24.1812499999138,
-10.5687124469213));
#290403=CARTESIAN_POINT('Ctrl Pts',(-3.10606665601014,24.3312499999131,
-9.5594902125713));
#290404=CARTESIAN_POINT('Ctrl Pts',(-6.21213331202024,24.4812499999125,
-8.55026797822134));
#290405=CARTESIAN_POINT('Ctrl Pts',(-8.13178807675722,24.6312499999119,
-5.90808986649102));
#290406=CARTESIAN_POINT('Ctrl Pts',(-10.0514428414942,24.7812499999113,
-3.2659117547607));
#290407=CARTESIAN_POINT('Ctrl Pts',(-10.0514428414942,24.9312499999107,
2.46189346052968E-15));
#290408=CARTESIAN_POINT('Ctrl Pts',(-10.0514428414942,25.0812499999101,
3.26591175476071));
#290409=CARTESIAN_POINT('Ctrl Pts',(-8.13178807675722,25.2312499999095,
5.90808986649102));
#290410=CARTESIAN_POINT('Ctrl Pts',(-6.21213331202024,25.381249999909,8.55026797822134));
#290411=CARTESIAN_POINT('Ctrl Pts',(-3.10606665601013,25.5312499999084,
9.5594902125713));
#290412=CARTESIAN_POINT('Ctrl Pts',(-2.53260936828095E-14,25.6812499999078,
10.5687124469213));
#290413=CARTESIAN_POINT('Ctrl Pts',(3.10606665601008,25.8312499999072,9.5594902125713));
#290414=CARTESIAN_POINT('Ctrl Pts',(6.21213331202019,25.9812499999066,8.55026797822134));
#290415=CARTESIAN_POINT('Ctrl Pts',(8.13178807675716,26.131249999906,5.90808986649102));
#290416=CARTESIAN_POINT('Ctrl Pts',(10.0514428414941,26.2812499999054,3.2659117547607));
#290417=CARTESIAN_POINT('Ctrl Pts',(10.0514428414941,26.4312499999048,-1.23094673026484E-15));
#290418=CARTESIAN_POINT('Origin',(-3.77475828372553E-14,-1.881249999982,
2.68644078414671E-15));
#290419=CARTESIAN_POINT('',(10.0514428414941,29.8062499998913,1.32395148255383E-15));
#290420=CARTESIAN_POINT('',(10.0514428414941,29.4312499998928,1.32550819937428E-15));
#290421=CARTESIAN_POINT('',(10.0514428414941,-1.881249999982,4.14193483802857E-15));
#290422=CARTESIAN_POINT('Ctrl Pts',(10.0514428414941,26.8062499999033,-1.23094673026484E-15));
#290423=CARTESIAN_POINT('Ctrl Pts',(10.0514428414941,26.9562499999027,-3.26591175476071));
#290424=CARTESIAN_POINT('Ctrl Pts',(8.13178807675716,27.1062499999021,-5.90808986649102));
#290425=CARTESIAN_POINT('Ctrl Pts',(6.21213331202019,27.2562499999015,-8.55026797822134));
#290426=CARTESIAN_POINT('Ctrl Pts',(3.10606665601008,27.4062499999009,-9.5594902125713));
#290427=CARTESIAN_POINT('Ctrl Pts',(-2.89944999514443E-14,27.5562499999003,
-10.5687124469213));
#290428=CARTESIAN_POINT('Ctrl Pts',(-3.10606665601014,27.7062499998996,
-9.5594902125713));
#290429=CARTESIAN_POINT('Ctrl Pts',(-6.21213331202024,27.856249999899,-8.55026797822134));
#290430=CARTESIAN_POINT('Ctrl Pts',(-8.13178807675722,28.0062499998984,
-5.90808986649102));
#290431=CARTESIAN_POINT('Ctrl Pts',(-10.0514428414942,28.1562499998978,
-3.2659117547607));
#290432=CARTESIAN_POINT('Ctrl Pts',(-10.0514428414942,28.3062499998973,
2.46189346052968E-15));
#290433=CARTESIAN_POINT('Ctrl Pts',(-10.0514428414942,28.4562499998966,
3.26591175476071));
#290434=CARTESIAN_POINT('Ctrl Pts',(-8.13178807675722,28.606249999896,5.90808986649102));
#290435=CARTESIAN_POINT('Ctrl Pts',(-6.21213331202024,28.7562499998954,
8.55026797822134));
#290436=CARTESIAN_POINT('Ctrl Pts',(-3.10606665601014,28.9062499998949,
9.5594902125713));
#290437=CARTESIAN_POINT('Ctrl Pts',(-2.72697666134291E-14,29.0562499998942,
10.5687124469213));
#290438=CARTESIAN_POINT('Ctrl Pts',(3.10606665601008,29.2062499998937,9.5594902125713));
#290439=CARTESIAN_POINT('Ctrl Pts',(6.21213331202019,29.356249999893,8.55026797822134));
#290440=CARTESIAN_POINT('Ctrl Pts',(8.13178807675716,29.5062499998925,5.90808986649102));
#290441=CARTESIAN_POINT('Ctrl Pts',(10.0514428414941,29.6562499998919,3.2659117547607));
#290442=CARTESIAN_POINT('Ctrl Pts',(10.0514428414941,29.8062499998913,-1.23094673026484E-15));
#290443=CARTESIAN_POINT('Ctrl Pts',(10.0514428414941,26.4312499999048,-1.23094673026484E-15));
#290444=CARTESIAN_POINT('Ctrl Pts',(10.0514428414941,26.5812499999042,-3.26591175476071));
#290445=CARTESIAN_POINT('Ctrl Pts',(8.13178807675716,26.7312499999036,-5.90808986649102));
#290446=CARTESIAN_POINT('Ctrl Pts',(6.21213331202019,26.881249999903,-8.55026797822134));
#290447=CARTESIAN_POINT('Ctrl Pts',(3.10606665601008,27.0312499999024,-9.5594902125713));
#290448=CARTESIAN_POINT('Ctrl Pts',(-2.87785362924866E-14,27.1812499999018,
-10.5687124469213));
#290449=CARTESIAN_POINT('Ctrl Pts',(-3.10606665601014,27.3312499999011,
-9.5594902125713));
#290450=CARTESIAN_POINT('Ctrl Pts',(-6.21213331202024,27.4812499999005,
-8.55026797822134));
#290451=CARTESIAN_POINT('Ctrl Pts',(-8.13178807675722,27.6312499998999,
-5.90808986649102));
#290452=CARTESIAN_POINT('Ctrl Pts',(-10.0514428414942,27.7812499998993,
-3.2659117547607));
#290453=CARTESIAN_POINT('Ctrl Pts',(-10.0514428414942,27.9312499998987,
2.46189346052968E-15));
#290454=CARTESIAN_POINT('Ctrl Pts',(-10.0514428414942,28.0812499998981,
3.26591175476071));
#290455=CARTESIAN_POINT('Ctrl Pts',(-8.13178807675722,28.2312499998975,
5.90808986649102));
#290456=CARTESIAN_POINT('Ctrl Pts',(-6.21213331202024,28.3812499998969,
8.55026797822134));
#290457=CARTESIAN_POINT('Ctrl Pts',(-3.10606665601014,28.5312499998964,
9.5594902125713));
#290458=CARTESIAN_POINT('Ctrl Pts',(-2.70538029544713E-14,28.6812499998958,
10.5687124469213));
#290459=CARTESIAN_POINT('Ctrl Pts',(3.10606665601008,28.8312499998952,9.5594902125713));
#290460=CARTESIAN_POINT('Ctrl Pts',(6.21213331202019,28.9812499998946,8.55026797822134));
#290461=CARTESIAN_POINT('Ctrl Pts',(8.13178807675716,29.131249999894,5.90808986649102));
#290462=CARTESIAN_POINT('Ctrl Pts',(10.0514428414941,29.2812499998934,3.2659117547607));
#290463=CARTESIAN_POINT('Ctrl Pts',(10.0514428414941,29.4312499998928,-1.23094673026484E-15));
#290464=CARTESIAN_POINT('Origin',(-3.77475828372553E-14,-1.881249999982,
2.68644078414671E-15));
#290465=CARTESIAN_POINT('',(10.0514428414941,32.8062499998793,1.31149774799023E-15));
#290466=CARTESIAN_POINT('',(10.0514428414941,32.4312499998808,1.31305446481068E-15));
#290467=CARTESIAN_POINT('',(10.0514428414941,-1.881249999982,4.14193483802857E-15));
#290468=CARTESIAN_POINT('Ctrl Pts',(10.0514428414941,29.8062499998913,-1.23094673026484E-15));
#290469=CARTESIAN_POINT('Ctrl Pts',(10.0514428414941,29.9562499998907,-3.26591175476071));
#290470=CARTESIAN_POINT('Ctrl Pts',(8.13178807675716,30.1062499998901,-5.90808986649102));
#290471=CARTESIAN_POINT('Ctrl Pts',(6.21213331202019,30.2562499998894,-8.55026797822134));
#290472=CARTESIAN_POINT('Ctrl Pts',(3.10606665601008,30.4062499998889,-9.5594902125713));
#290473=CARTESIAN_POINT('Ctrl Pts',(-3.07222092231062E-14,30.5562499998883,
-10.5687124469213));
#290474=CARTESIAN_POINT('Ctrl Pts',(-3.10606665601014,30.7062499998877,
-9.5594902125713));
#290475=CARTESIAN_POINT('Ctrl Pts',(-6.21213331202025,30.8562499998871,
-8.55026797822134));
#290476=CARTESIAN_POINT('Ctrl Pts',(-8.13178807675722,31.0062499998864,
-5.90808986649102));
#290477=CARTESIAN_POINT('Ctrl Pts',(-10.0514428414942,31.1562499998858,
-3.2659117547607));
#290478=CARTESIAN_POINT('Ctrl Pts',(-10.0514428414942,31.3062499998852,
2.46189346052968E-15));
#290479=CARTESIAN_POINT('Ctrl Pts',(-10.0514428414942,31.4562499998847,
3.26591175476071));
#290480=CARTESIAN_POINT('Ctrl Pts',(-8.13178807675722,31.606249999884,5.90808986649102));
#290481=CARTESIAN_POINT('Ctrl Pts',(-6.21213331202024,31.7562499998835,
8.55026797822134));
#290482=CARTESIAN_POINT('Ctrl Pts',(-3.10606665601014,31.9062499998829,
9.5594902125713));
#290483=CARTESIAN_POINT('Ctrl Pts',(-2.89974758850909E-14,32.0562499998822,
10.5687124469213));
#290484=CARTESIAN_POINT('Ctrl Pts',(3.10606665601008,32.2062499998816,9.5594902125713));
#290485=CARTESIAN_POINT('Ctrl Pts',(6.21213331202019,32.3562499998811,8.55026797822134));
#290486=CARTESIAN_POINT('Ctrl Pts',(8.13178807675716,32.5062499998805,5.90808986649102));
#290487=CARTESIAN_POINT('Ctrl Pts',(10.0514428414941,32.6562499998799,3.2659117547607));
#290488=CARTESIAN_POINT('Ctrl Pts',(10.0514428414941,32.8062499998793,-1.23094673026484E-15));
#290489=CARTESIAN_POINT('Ctrl Pts',(10.0514428414941,29.4312499998928,-1.23094673026484E-15));
#290490=CARTESIAN_POINT('Ctrl Pts',(10.0514428414941,29.5812499998922,-3.26591175476071));
#290491=CARTESIAN_POINT('Ctrl Pts',(8.13178807675716,29.7312499998916,-5.90808986649102));
#290492=CARTESIAN_POINT('Ctrl Pts',(6.21213331202019,29.881249999891,-8.55026797822134));
#290493=CARTESIAN_POINT('Ctrl Pts',(3.10606665601008,30.0312499998904,-9.5594902125713));
#290494=CARTESIAN_POINT('Ctrl Pts',(-3.05062455641484E-14,30.1812499998898,
-10.5687124469213));
#290495=CARTESIAN_POINT('Ctrl Pts',(-3.10606665601014,30.3312499998892,
-9.5594902125713));
#290496=CARTESIAN_POINT('Ctrl Pts',(-6.21213331202025,30.4812499998885,
-8.55026797822134));
#290497=CARTESIAN_POINT('Ctrl Pts',(-8.13178807675722,30.6312499998879,
-5.90808986649102));
#290498=CARTESIAN_POINT('Ctrl Pts',(-10.0514428414942,30.7812499998873,
-3.2659117547607));
#290499=CARTESIAN_POINT('Ctrl Pts',(-10.0514428414942,30.9312499998867,
2.46189346052968E-15));
#290500=CARTESIAN_POINT('Ctrl Pts',(-10.0514428414942,31.0812499998861,
3.26591175476071));
#290501=CARTESIAN_POINT('Ctrl Pts',(-8.13178807675722,31.2312499998855,
5.90808986649102));
#290502=CARTESIAN_POINT('Ctrl Pts',(-6.21213331202024,31.381249999885,8.55026797822134));
#290503=CARTESIAN_POINT('Ctrl Pts',(-3.10606665601014,31.5312499998843,
9.5594902125713));
#290504=CARTESIAN_POINT('Ctrl Pts',(-2.87815122261332E-14,31.6812499998838,
10.5687124469213));
#290505=CARTESIAN_POINT('Ctrl Pts',(3.10606665601008,31.8312499998832,9.5594902125713));
#290506=CARTESIAN_POINT('Ctrl Pts',(6.21213331202019,31.9812499998826,8.55026797822134));
#290507=CARTESIAN_POINT('Ctrl Pts',(8.13178807675716,32.131249999882,5.90808986649102));
#290508=CARTESIAN_POINT('Ctrl Pts',(10.0514428414941,32.2812499998814,3.2659117547607));
#290509=CARTESIAN_POINT('Ctrl Pts',(10.0514428414941,32.4312499998808,-1.23094673026484E-15));
#290510=CARTESIAN_POINT('Origin',(-3.77475828372553E-14,-1.881249999982,
2.68644078414671E-15));
#290511=CARTESIAN_POINT('',(10.0514428414941,35.8062499998673,1.29904401342663E-15));
#290512=CARTESIAN_POINT('',(10.0514428414941,35.4312499998688,1.30060073024708E-15));
#290513=CARTESIAN_POINT('',(10.0514428414941,-1.881249999982,4.14193483802857E-15));
#290514=CARTESIAN_POINT('Ctrl Pts',(10.0514428414941,32.8062499998793,-1.23094673026484E-15));
#290515=CARTESIAN_POINT('Ctrl Pts',(10.0514428414941,32.9562499998787,-3.26591175476071));
#290516=CARTESIAN_POINT('Ctrl Pts',(8.13178807675716,33.1062499998781,-5.90808986649102));
#290517=CARTESIAN_POINT('Ctrl Pts',(6.21213331202018,33.2562499998775,-8.55026797822134));
#290518=CARTESIAN_POINT('Ctrl Pts',(3.10606665601008,33.4062499998769,-9.5594902125713));
#290519=CARTESIAN_POINT('Ctrl Pts',(-3.2449918494768E-14,33.5562499998763,
-10.5687124469213));
#290520=CARTESIAN_POINT('Ctrl Pts',(-3.10606665601014,33.7062499998756,
-9.5594902125713));
#290521=CARTESIAN_POINT('Ctrl Pts',(-6.21213331202025,33.856249999875,-8.55026797822134));
#290522=CARTESIAN_POINT('Ctrl Pts',(-8.13178807675722,34.0062499998744,
-5.90808986649102));
#290523=CARTESIAN_POINT('Ctrl Pts',(-10.0514428414942,34.1562499998739,
-3.2659117547607));
#290524=CARTESIAN_POINT('Ctrl Pts',(-10.0514428414942,34.3062499998732,
2.46189346052968E-15));
#290525=CARTESIAN_POINT('Ctrl Pts',(-10.0514428414942,34.4562499998727,
3.26591175476071));
#290526=CARTESIAN_POINT('Ctrl Pts',(-8.13178807675722,34.606249999872,5.90808986649102));
#290527=CARTESIAN_POINT('Ctrl Pts',(-6.21213331202024,34.7562499998714,
8.55026797822134));
#290528=CARTESIAN_POINT('Ctrl Pts',(-3.10606665601014,34.9062499998708,
9.5594902125713));
#290529=CARTESIAN_POINT('Ctrl Pts',(-3.07251851567527E-14,35.0562499998703,
10.5687124469213));
#290530=CARTESIAN_POINT('Ctrl Pts',(3.10606665601008,35.2062499998697,9.5594902125713));
#290531=CARTESIAN_POINT('Ctrl Pts',(6.21213331202019,35.3562499998691,8.55026797822134));
#290532=CARTESIAN_POINT('Ctrl Pts',(8.13178807675716,35.5062499998685,5.90808986649102));
#290533=CARTESIAN_POINT('Ctrl Pts',(10.0514428414941,35.6562499998679,3.2659117547607));
#290534=CARTESIAN_POINT('Ctrl Pts',(10.0514428414941,35.8062499998673,-1.23094673026484E-15));
#290535=CARTESIAN_POINT('Ctrl Pts',(10.0514428414941,32.4312499998808,-1.23094673026484E-15));
#290536=CARTESIAN_POINT('Ctrl Pts',(10.0514428414941,32.5812499998802,-3.26591175476071));
#290537=CARTESIAN_POINT('Ctrl Pts',(8.13178807675716,32.7312499998796,-5.90808986649102));
#290538=CARTESIAN_POINT('Ctrl Pts',(6.21213331202018,32.8812499998789,-8.55026797822134));
#290539=CARTESIAN_POINT('Ctrl Pts',(3.10606665601008,33.0312499998784,-9.5594902125713));
#290540=CARTESIAN_POINT('Ctrl Pts',(-3.22339548358103E-14,33.1812499998777,
-10.5687124469213));
#290541=CARTESIAN_POINT('Ctrl Pts',(-3.10606665601014,33.3312499998772,
-9.5594902125713));
#290542=CARTESIAN_POINT('Ctrl Pts',(-6.21213331202025,33.4812499998765,
-8.55026797822134));
#290543=CARTESIAN_POINT('Ctrl Pts',(-8.13178807675722,33.6312499998759,
-5.90808986649102));
#290544=CARTESIAN_POINT('Ctrl Pts',(-10.0514428414942,33.7812499998753,
-3.2659117547607));
#290545=CARTESIAN_POINT('Ctrl Pts',(-10.0514428414942,33.9312499998747,
2.46189346052968E-15));
#290546=CARTESIAN_POINT('Ctrl Pts',(-10.0514428414942,34.0812499998741,
3.26591175476071));
#290547=CARTESIAN_POINT('Ctrl Pts',(-8.13178807675722,34.2312499998735,
5.90808986649102));
#290548=CARTESIAN_POINT('Ctrl Pts',(-6.21213331202024,34.3812499998729,
8.55026797822134));
#290549=CARTESIAN_POINT('Ctrl Pts',(-3.10606665601014,34.5312499998724,
9.5594902125713));
#290550=CARTESIAN_POINT('Ctrl Pts',(-3.0509221497795E-14,34.6812499998718,
10.5687124469213));
#290551=CARTESIAN_POINT('Ctrl Pts',(3.10606665601008,34.8312499998712,9.5594902125713));
#290552=CARTESIAN_POINT('Ctrl Pts',(6.21213331202019,34.9812499998706,8.55026797822134));
#290553=CARTESIAN_POINT('Ctrl Pts',(8.13178807675716,35.13124999987,5.90808986649102));
#290554=CARTESIAN_POINT('Ctrl Pts',(10.0514428414941,35.2812499998694,3.2659117547607));
#290555=CARTESIAN_POINT('Ctrl Pts',(10.0514428414941,35.4312499998688,-1.23094673026484E-15));
#290556=CARTESIAN_POINT('Origin',(-3.77475828372553E-14,-1.881249999982,
2.68644078414671E-15));
#290557=CARTESIAN_POINT('',(10.0514428414941,38.8062499998553,1.28659027886303E-15));
#290558=CARTESIAN_POINT('',(10.0514428414941,38.4312499998568,1.28814699568348E-15));
#290559=CARTESIAN_POINT('',(10.0514428414941,-1.881249999982,4.14193483802857E-15));
#290560=CARTESIAN_POINT('Ctrl Pts',(10.0514428414941,35.8062499998673,-1.23094673026484E-15));
#290561=CARTESIAN_POINT('Ctrl Pts',(10.0514428414941,35.9562499998667,-3.26591175476071));
#290562=CARTESIAN_POINT('Ctrl Pts',(8.13178807675716,36.1062499998661,-5.90808986649102));
#290563=CARTESIAN_POINT('Ctrl Pts',(6.21213331202018,36.2562499998655,-8.55026797822134));
#290564=CARTESIAN_POINT('Ctrl Pts',(3.10606665601007,36.4062499998649,-9.5594902125713));
#290565=CARTESIAN_POINT('Ctrl Pts',(-3.41776277664299E-14,36.5562499998642,
-10.5687124469213));
#290566=CARTESIAN_POINT('Ctrl Pts',(-3.10606665601014,36.7062499998636,
-9.5594902125713));
#290567=CARTESIAN_POINT('Ctrl Pts',(-6.21213331202025,36.856249999863,-8.55026797822134));
#290568=CARTESIAN_POINT('Ctrl Pts',(-8.13178807675722,37.0062499998624,
-5.90808986649102));
#290569=CARTESIAN_POINT('Ctrl Pts',(-10.0514428414942,37.1562499998618,
-3.2659117547607));
#290570=CARTESIAN_POINT('Ctrl Pts',(-10.0514428414942,37.3062499998613,
2.46189346052968E-15));
#290571=CARTESIAN_POINT('Ctrl Pts',(-10.0514428414942,37.4562499998606,
3.26591175476071));
#290572=CARTESIAN_POINT('Ctrl Pts',(-8.13178807675722,37.60624999986,5.90808986649102));
#290573=CARTESIAN_POINT('Ctrl Pts',(-6.21213331202025,37.7562499998594,
8.55026797822134));
#290574=CARTESIAN_POINT('Ctrl Pts',(-3.10606665601014,37.9062499998588,
9.5594902125713));
#290575=CARTESIAN_POINT('Ctrl Pts',(-3.24528944284146E-14,38.0562499998583,
10.5687124469213));
#290576=CARTESIAN_POINT('Ctrl Pts',(3.10606665601007,38.2062499998577,9.5594902125713));
#290577=CARTESIAN_POINT('Ctrl Pts',(6.21213331202018,38.3562499998571,8.55026797822134));
#290578=CARTESIAN_POINT('Ctrl Pts',(8.13178807675716,38.5062499998565,5.90808986649102));
#290579=CARTESIAN_POINT('Ctrl Pts',(10.0514428414941,38.6562499998559,3.2659117547607));
#290580=CARTESIAN_POINT('Ctrl Pts',(10.0514428414941,38.8062499998553,-1.23094673026484E-15));
#290581=CARTESIAN_POINT('Ctrl Pts',(10.0514428414941,35.4312499998688,-1.23094673026484E-15));
#290582=CARTESIAN_POINT('Ctrl Pts',(10.0514428414941,35.5812499998681,-3.26591175476071));
#290583=CARTESIAN_POINT('Ctrl Pts',(8.13178807675716,35.7312499998676,-5.90808986649102));
#290584=CARTESIAN_POINT('Ctrl Pts',(6.21213331202018,35.881249999867,-8.55026797822134));
#290585=CARTESIAN_POINT('Ctrl Pts',(3.10606665601007,36.0312499998664,-9.5594902125713));
#290586=CARTESIAN_POINT('Ctrl Pts',(-3.39616641074721E-14,36.1812499998658,
-10.5687124469213));
#290587=CARTESIAN_POINT('Ctrl Pts',(-3.10606665601014,36.3312499998652,
-9.5594902125713));
#290588=CARTESIAN_POINT('Ctrl Pts',(-6.21213331202025,36.4812499998645,
-8.55026797822134));
#290589=CARTESIAN_POINT('Ctrl Pts',(-8.13178807675722,36.6312499998639,
-5.90808986649102));
#290590=CARTESIAN_POINT('Ctrl Pts',(-10.0514428414942,36.7812499998633,
-3.2659117547607));
#290591=CARTESIAN_POINT('Ctrl Pts',(-10.0514428414942,36.9312499998627,
2.46189346052968E-15));
#290592=CARTESIAN_POINT('Ctrl Pts',(-10.0514428414942,37.0812499998621,
3.26591175476071));
#290593=CARTESIAN_POINT('Ctrl Pts',(-8.13178807675722,37.2312499998615,
5.90808986649102));
#290594=CARTESIAN_POINT('Ctrl Pts',(-6.21213331202025,37.3812499998609,
8.55026797822134));
#290595=CARTESIAN_POINT('Ctrl Pts',(-3.10606665601014,37.5312499998603,
9.5594902125713));
#290596=CARTESIAN_POINT('Ctrl Pts',(-3.22369307694568E-14,37.6812499998598,
10.5687124469213));
#290597=CARTESIAN_POINT('Ctrl Pts',(3.10606665601008,37.8312499998592,9.5594902125713));
#290598=CARTESIAN_POINT('Ctrl Pts',(6.21213331202018,37.9812499998586,8.55026797822134));
#290599=CARTESIAN_POINT('Ctrl Pts',(8.13178807675716,38.131249999858,5.90808986649102));
#290600=CARTESIAN_POINT('Ctrl Pts',(10.0514428414941,38.2812499998574,3.2659117547607));
#290601=CARTESIAN_POINT('Ctrl Pts',(10.0514428414941,38.4312499998568,-1.23094673026484E-15));
#290602=CARTESIAN_POINT('Origin',(-3.77475828372553E-14,-1.881249999982,
2.68644078414671E-15));
#290603=CARTESIAN_POINT('',(10.0514428414941,41.8062499998433,1.27413654429943E-15));
#290604=CARTESIAN_POINT('',(10.0514428414941,41.4312499998448,1.27569326111988E-15));
#290605=CARTESIAN_POINT('',(10.0514428414941,-1.881249999982,4.14193483802857E-15));
#290606=CARTESIAN_POINT('Ctrl Pts',(10.0514428414941,38.8062499998553,-1.23094673026484E-15));
#290607=CARTESIAN_POINT('Ctrl Pts',(10.0514428414941,38.9562499998547,-3.26591175476071));
#290608=CARTESIAN_POINT('Ctrl Pts',(8.13178807675715,39.1062499998541,-5.90808986649102));
#290609=CARTESIAN_POINT('Ctrl Pts',(6.21213331202018,39.2562499998535,-8.55026797822134));
#290610=CARTESIAN_POINT('Ctrl Pts',(3.10606665601007,39.4062499998529,-9.5594902125713));
#290611=CARTESIAN_POINT('Ctrl Pts',(-3.59053370380917E-14,39.5562499998522,
-10.5687124469213));
#290612=CARTESIAN_POINT('Ctrl Pts',(-3.10606665601014,39.7062499998516,
-9.5594902125713));
#290613=CARTESIAN_POINT('Ctrl Pts',(-6.21213331202025,39.856249999851,-8.55026797822134));
#290614=CARTESIAN_POINT('Ctrl Pts',(-8.13178807675723,40.0062499998505,
-5.90808986649102));
#290615=CARTESIAN_POINT('Ctrl Pts',(-10.0514428414942,40.1562499998499,
-3.2659117547607));
#290616=CARTESIAN_POINT('Ctrl Pts',(-10.0514428414942,40.3062499998493,
2.46189346052968E-15));
#290617=CARTESIAN_POINT('Ctrl Pts',(-10.0514428414942,40.4562499998487,
3.26591175476071));
#290618=CARTESIAN_POINT('Ctrl Pts',(-8.13178807675723,40.606249999848,5.90808986649102));
#290619=CARTESIAN_POINT('Ctrl Pts',(-6.21213331202025,40.7562499998474,
8.55026797822134));
#290620=CARTESIAN_POINT('Ctrl Pts',(-3.10606665601014,40.9062499998468,
9.5594902125713));
#290621=CARTESIAN_POINT('Ctrl Pts',(-3.41806037000764E-14,41.0562499998463,
10.5687124469213));
#290622=CARTESIAN_POINT('Ctrl Pts',(3.10606665601007,41.2062499998457,9.5594902125713));
#290623=CARTESIAN_POINT('Ctrl Pts',(6.21213331202018,41.3562499998451,8.55026797822134));
#290624=CARTESIAN_POINT('Ctrl Pts',(8.13178807675715,41.5062499998444,5.90808986649102));
#290625=CARTESIAN_POINT('Ctrl Pts',(10.0514428414941,41.6562499998439,3.2659117547607));
#290626=CARTESIAN_POINT('Ctrl Pts',(10.0514428414941,41.8062499998433,-1.23094673026484E-15));
#290627=CARTESIAN_POINT('Ctrl Pts',(10.0514428414941,38.4312499998568,-1.23094673026484E-15));
#290628=CARTESIAN_POINT('Ctrl Pts',(10.0514428414941,38.5812499998562,-3.26591175476071));
#290629=CARTESIAN_POINT('Ctrl Pts',(8.13178807675715,38.7312499998556,-5.90808986649102));
#290630=CARTESIAN_POINT('Ctrl Pts',(6.21213331202018,38.881249999855,-8.55026797822134));
#290631=CARTESIAN_POINT('Ctrl Pts',(3.10606665601007,39.0312499998544,-9.5594902125713));
#290632=CARTESIAN_POINT('Ctrl Pts',(-3.5689373379134E-14,39.1812499998537,
-10.5687124469213));
#290633=CARTESIAN_POINT('Ctrl Pts',(-3.10606665601014,39.3312499998532,
-9.5594902125713));
#290634=CARTESIAN_POINT('Ctrl Pts',(-6.21213331202025,39.4812499998525,
-8.55026797822134));
#290635=CARTESIAN_POINT('Ctrl Pts',(-8.13178807675723,39.6312499998519,
-5.90808986649102));
#290636=CARTESIAN_POINT('Ctrl Pts',(-10.0514428414942,39.7812499998513,
-3.2659117547607));
#290637=CARTESIAN_POINT('Ctrl Pts',(-10.0514428414942,39.9312499998507,
2.46189346052968E-15));
#290638=CARTESIAN_POINT('Ctrl Pts',(-10.0514428414942,40.0812499998501,
3.26591175476071));
#290639=CARTESIAN_POINT('Ctrl Pts',(-8.13178807675723,40.2312499998495,
5.90808986649102));
#290640=CARTESIAN_POINT('Ctrl Pts',(-6.21213331202025,40.3812499998489,
8.55026797822134));
#290641=CARTESIAN_POINT('Ctrl Pts',(-3.10606665601014,40.5312499998483,
9.5594902125713));
#290642=CARTESIAN_POINT('Ctrl Pts',(-3.39646400411187E-14,40.6812499998478,
10.5687124469213));
#290643=CARTESIAN_POINT('Ctrl Pts',(3.10606665601007,40.8312499998472,9.5594902125713));
#290644=CARTESIAN_POINT('Ctrl Pts',(6.21213331202018,40.9812499998465,8.55026797822134));
#290645=CARTESIAN_POINT('Ctrl Pts',(8.13178807675715,41.131249999846,5.90808986649102));
#290646=CARTESIAN_POINT('Ctrl Pts',(10.0514428414941,41.2812499998454,3.2659117547607));
#290647=CARTESIAN_POINT('Ctrl Pts',(10.0514428414941,41.4312499998448,-1.23094673026484E-15));
#290648=CARTESIAN_POINT('Origin',(-3.77475828372553E-14,-1.881249999982,
2.68644078414671E-15));
#290649=CARTESIAN_POINT('',(10.0514428414941,44.8062499998313,1.26168280973582E-15));
#290650=CARTESIAN_POINT('',(10.0514428414941,44.4312499998328,1.26323952655627E-15));
#290651=CARTESIAN_POINT('',(10.0514428414941,-1.881249999982,4.14193483802857E-15));
#290652=CARTESIAN_POINT('Ctrl Pts',(10.0514428414941,41.8062499998433,-1.23094673026484E-15));
#290653=CARTESIAN_POINT('Ctrl Pts',(10.0514428414941,41.9562499998427,-3.26591175476071));
#290654=CARTESIAN_POINT('Ctrl Pts',(8.13178807675715,42.1062499998421,-5.90808986649102));
#290655=CARTESIAN_POINT('Ctrl Pts',(6.21213331202018,42.2562499998415,-8.55026797822134));
#290656=CARTESIAN_POINT('Ctrl Pts',(3.10606665601007,42.4062499998408,-9.5594902125713));
#290657=CARTESIAN_POINT('Ctrl Pts',(-3.76330463097535E-14,42.5562499998402,
-10.5687124469213));
#290658=CARTESIAN_POINT('Ctrl Pts',(-3.10606665601015,42.7062499998396,
-9.5594902125713));
#290659=CARTESIAN_POINT('Ctrl Pts',(-6.21213331202025,42.8562499998391,
-8.55026797822134));
#290660=CARTESIAN_POINT('Ctrl Pts',(-8.13178807675723,43.0062499998385,
-5.90808986649102));
#290661=CARTESIAN_POINT('Ctrl Pts',(-10.0514428414942,43.1562499998379,
-3.2659117547607));
#290662=CARTESIAN_POINT('Ctrl Pts',(-10.0514428414942,43.3062499998373,
2.46189346052968E-15));
#290663=CARTESIAN_POINT('Ctrl Pts',(-10.0514428414942,43.4562499998366,
3.26591175476071));
#290664=CARTESIAN_POINT('Ctrl Pts',(-8.13178807675723,43.6062499998361,
5.90808986649102));
#290665=CARTESIAN_POINT('Ctrl Pts',(-6.21213331202025,43.7562499998354,
8.55026797822134));
#290666=CARTESIAN_POINT('Ctrl Pts',(-3.10606665601014,43.9062499998348,
9.5594902125713));
#290667=CARTESIAN_POINT('Ctrl Pts',(-3.59083129717383E-14,44.0562499998343,
10.5687124469213));
#290668=CARTESIAN_POINT('Ctrl Pts',(3.10606665601007,44.2062499998337,9.5594902125713));
#290669=CARTESIAN_POINT('Ctrl Pts',(6.21213331202018,44.356249999833,8.55026797822134));
#290670=CARTESIAN_POINT('Ctrl Pts',(8.13178807675715,44.5062499998324,5.90808986649102));
#290671=CARTESIAN_POINT('Ctrl Pts',(10.0514428414941,44.6562499998319,3.2659117547607));
#290672=CARTESIAN_POINT('Ctrl Pts',(10.0514428414941,44.8062499998313,-1.23094673026484E-15));
#290673=CARTESIAN_POINT('Ctrl Pts',(10.0514428414941,41.4312499998448,-1.23094673026484E-15));
#290674=CARTESIAN_POINT('Ctrl Pts',(10.0514428414941,41.5812499998442,-3.26591175476071));
#290675=CARTESIAN_POINT('Ctrl Pts',(8.13178807675715,41.7312499998436,-5.90808986649102));
#290676=CARTESIAN_POINT('Ctrl Pts',(6.21213331202018,41.881249999843,-8.55026797822134));
#290677=CARTESIAN_POINT('Ctrl Pts',(3.10606665601007,42.0312499998423,-9.5594902125713));
#290678=CARTESIAN_POINT('Ctrl Pts',(-3.74170826507958E-14,42.1812499998418,
-10.5687124469213));
#290679=CARTESIAN_POINT('Ctrl Pts',(-3.10606665601015,42.3312499998411,
-9.5594902125713));
#290680=CARTESIAN_POINT('Ctrl Pts',(-6.21213331202025,42.4812499998405,
-8.55026797822134));
#290681=CARTESIAN_POINT('Ctrl Pts',(-8.13178807675723,42.6312499998399,
-5.90808986649102));
#290682=CARTESIAN_POINT('Ctrl Pts',(-10.0514428414942,42.7812499998393,
-3.2659117547607));
#290683=CARTESIAN_POINT('Ctrl Pts',(-10.0514428414942,42.9312499998387,
2.46189346052968E-15));
#290684=CARTESIAN_POINT('Ctrl Pts',(-10.0514428414942,43.0812499998381,
3.26591175476071));
#290685=CARTESIAN_POINT('Ctrl Pts',(-8.13178807675723,43.2312499998375,
5.90808986649102));
#290686=CARTESIAN_POINT('Ctrl Pts',(-6.21213331202025,43.3812499998369,
8.55026797822134));
#290687=CARTESIAN_POINT('Ctrl Pts',(-3.10606665601014,43.5312499998363,
9.5594902125713));
#290688=CARTESIAN_POINT('Ctrl Pts',(-3.56923493127805E-14,43.6812499998357,
10.5687124469213));
#290689=CARTESIAN_POINT('Ctrl Pts',(3.10606665601007,43.8312499998352,9.5594902125713));
#290690=CARTESIAN_POINT('Ctrl Pts',(6.21213331202018,43.9812499998345,8.55026797822134));
#290691=CARTESIAN_POINT('Ctrl Pts',(8.13178807675715,44.131249999834,5.90808986649102));
#290692=CARTESIAN_POINT('Ctrl Pts',(10.0514428414941,44.2812499998334,3.2659117547607));
#290693=CARTESIAN_POINT('Ctrl Pts',(10.0514428414941,44.4312499998328,-1.23094673026484E-15));
#290694=CARTESIAN_POINT('Origin',(-3.77475828372553E-14,-1.881249999982,
2.68644078414671E-15));
#290695=CARTESIAN_POINT('',(10.0514428414941,47.8062499998193,1.24922907517222E-15));
#290696=CARTESIAN_POINT('',(10.0514428414941,47.4312499998208,1.25078579199267E-15));
#290697=CARTESIAN_POINT('',(10.0514428414941,-1.881249999982,4.14193483802857E-15));
#290698=CARTESIAN_POINT('Ctrl Pts',(10.0514428414941,44.8062499998313,-1.23094673026484E-15));
#290699=CARTESIAN_POINT('Ctrl Pts',(10.0514428414941,44.9562499998307,-3.26591175476071));
#290700=CARTESIAN_POINT('Ctrl Pts',(8.13178807675715,45.1062499998301,-5.90808986649102));
#290701=CARTESIAN_POINT('Ctrl Pts',(6.21213331202018,45.2562499998295,-8.55026797822134));
#290702=CARTESIAN_POINT('Ctrl Pts',(3.10606665601007,45.4062499998289,-9.5594902125713));
#290703=CARTESIAN_POINT('Ctrl Pts',(-3.93607555814154E-14,45.5562499998282,
-10.5687124469213));
#290704=CARTESIAN_POINT('Ctrl Pts',(-3.10606665601015,45.7062499998276,
-9.5594902125713));
#290705=CARTESIAN_POINT('Ctrl Pts',(-6.21213331202026,45.856249999827,-8.55026797822134));
#290706=CARTESIAN_POINT('Ctrl Pts',(-8.13178807675723,46.0062499998265,
-5.90808986649102));
#290707=CARTESIAN_POINT('Ctrl Pts',(-10.0514428414942,46.1562499998259,
-3.2659117547607));
#290708=CARTESIAN_POINT('Ctrl Pts',(-10.0514428414942,46.3062499998252,
2.46189346052968E-15));
#290709=CARTESIAN_POINT('Ctrl Pts',(-10.0514428414942,46.4562499998246,
3.26591175476071));
#290710=CARTESIAN_POINT('Ctrl Pts',(-8.13178807675723,46.606249999824,5.90808986649102));
#290711=CARTESIAN_POINT('Ctrl Pts',(-6.21213331202025,46.7562499998235,
8.55026797822134));
#290712=CARTESIAN_POINT('Ctrl Pts',(-3.10606665601015,46.9062499998228,
9.5594902125713));
#290713=CARTESIAN_POINT('Ctrl Pts',(-3.76360222434001E-14,47.0562499998223,
10.5687124469213));
#290714=CARTESIAN_POINT('Ctrl Pts',(3.10606665601007,47.2062499998217,9.5594902125713));
#290715=CARTESIAN_POINT('Ctrl Pts',(6.21213331202018,47.356249999821,8.55026797822134));
#290716=CARTESIAN_POINT('Ctrl Pts',(8.13178807675715,47.5062499998204,5.90808986649102));
#290717=CARTESIAN_POINT('Ctrl Pts',(10.0514428414941,47.6562499998198,3.2659117547607));
#290718=CARTESIAN_POINT('Ctrl Pts',(10.0514428414941,47.8062499998193,-1.23094673026484E-15));
#290719=CARTESIAN_POINT('Ctrl Pts',(10.0514428414941,44.4312499998328,-1.23094673026484E-15));
#290720=CARTESIAN_POINT('Ctrl Pts',(10.0514428414941,44.5812499998322,-3.26591175476071));
#290721=CARTESIAN_POINT('Ctrl Pts',(8.13178807675715,44.7312499998316,-5.90808986649102));
#290722=CARTESIAN_POINT('Ctrl Pts',(6.21213331202018,44.881249999831,-8.55026797822134));
#290723=CARTESIAN_POINT('Ctrl Pts',(3.10606665601007,45.0312499998304,-9.5594902125713));
#290724=CARTESIAN_POINT('Ctrl Pts',(-3.91447919224576E-14,45.1812499998297,
-10.5687124469213));
#290725=CARTESIAN_POINT('Ctrl Pts',(-3.10606665601015,45.3312499998292,
-9.5594902125713));
#290726=CARTESIAN_POINT('Ctrl Pts',(-6.21213331202026,45.4812499998285,
-8.55026797822134));
#290727=CARTESIAN_POINT('Ctrl Pts',(-8.13178807675723,45.6312499998279,
-5.90808986649102));
#290728=CARTESIAN_POINT('Ctrl Pts',(-10.0514428414942,45.7812499998273,
-3.2659117547607));
#290729=CARTESIAN_POINT('Ctrl Pts',(-10.0514428414942,45.9312499998267,
2.46189346052968E-15));
#290730=CARTESIAN_POINT('Ctrl Pts',(-10.0514428414942,46.0812499998261,
3.26591175476071));
#290731=CARTESIAN_POINT('Ctrl Pts',(-8.13178807675723,46.2312499998255,
5.90808986649102));
#290732=CARTESIAN_POINT('Ctrl Pts',(-6.21213331202025,46.3812499998249,
8.55026797822134));
#290733=CARTESIAN_POINT('Ctrl Pts',(-3.10606665601015,46.5312499998244,
9.5594902125713));
#290734=CARTESIAN_POINT('Ctrl Pts',(-3.74200585844424E-14,46.6812499998238,
10.5687124469213));
#290735=CARTESIAN_POINT('Ctrl Pts',(3.10606665601007,46.8312499998232,9.5594902125713));
#290736=CARTESIAN_POINT('Ctrl Pts',(6.21213331202018,46.9812499998225,8.55026797822134));
#290737=CARTESIAN_POINT('Ctrl Pts',(8.13178807675715,47.131249999822,5.90808986649102));
#290738=CARTESIAN_POINT('Ctrl Pts',(10.0514428414941,47.2812499998214,3.2659117547607));
#290739=CARTESIAN_POINT('Ctrl Pts',(10.0514428414941,47.4312499998208,-1.23094673026484E-15));
#290740=CARTESIAN_POINT('Origin',(-3.77475828372553E-14,-1.881249999982,
2.68644078414671E-15));
#290741=CARTESIAN_POINT('',(10.0514428414941,50.8062499998072,1.23677534060862E-15));
#290742=CARTESIAN_POINT('',(10.0514428414941,50.4312499998088,1.23833205742907E-15));
#290743=CARTESIAN_POINT('',(10.0514428414941,-1.881249999982,4.14193483802857E-15));
#290744=CARTESIAN_POINT('Ctrl Pts',(10.0514428414941,47.8062499998193,-1.23094673026484E-15));
#290745=CARTESIAN_POINT('Ctrl Pts',(10.0514428414941,47.9562499998187,-3.26591175476071));
#290746=CARTESIAN_POINT('Ctrl Pts',(8.13178807675715,48.1062499998181,-5.90808986649102));
#290747=CARTESIAN_POINT('Ctrl Pts',(6.21213331202018,48.2562499998174,-8.55026797822134));
#290748=CARTESIAN_POINT('Ctrl Pts',(3.10606665601007,48.4062499998169,-9.5594902125713));
#290749=CARTESIAN_POINT('Ctrl Pts',(-4.10884648530772E-14,48.5562499998163,
-10.5687124469213));
#290750=CARTESIAN_POINT('Ctrl Pts',(-3.10606665601015,48.7062499998157,
-9.5594902125713));
#290751=CARTESIAN_POINT('Ctrl Pts',(-6.21213331202026,48.8562499998151,
-8.55026797822134));
#290752=CARTESIAN_POINT('Ctrl Pts',(-8.13178807675723,49.0062499998145,
-5.90808986649102));
#290753=CARTESIAN_POINT('Ctrl Pts',(-10.0514428414942,49.1562499998139,
-3.2659117547607));
#290754=CARTESIAN_POINT('Ctrl Pts',(-10.0514428414942,49.3062499998132,
2.46189346052968E-15));
#290755=CARTESIAN_POINT('Ctrl Pts',(-10.0514428414942,49.4562499998126,
3.26591175476071));
#290756=CARTESIAN_POINT('Ctrl Pts',(-8.13178807675723,49.6062499998121,
5.90808986649102));
#290757=CARTESIAN_POINT('Ctrl Pts',(-6.21213331202025,49.7562499998114,
8.55026797822134));
#290758=CARTESIAN_POINT('Ctrl Pts',(-3.10606665601015,49.9062499998109,
9.5594902125713));
#290759=CARTESIAN_POINT('Ctrl Pts',(-3.9363731515062E-14,50.0562499998103,
10.5687124469213));
#290760=CARTESIAN_POINT('Ctrl Pts',(3.10606665601007,50.2062499998097,9.5594902125713));
#290761=CARTESIAN_POINT('Ctrl Pts',(6.21213331202018,50.3562499998091,8.55026797822134));
#290762=CARTESIAN_POINT('Ctrl Pts',(8.13178807675715,50.5062499998085,5.90808986649102));
#290763=CARTESIAN_POINT('Ctrl Pts',(10.0514428414941,50.6562499998078,3.2659117547607));
#290764=CARTESIAN_POINT('Ctrl Pts',(10.0514428414941,50.8062499998072,-1.23094673026484E-15));
#290765=CARTESIAN_POINT('Ctrl Pts',(10.0514428414941,47.4312499998208,-1.23094673026484E-15));
#290766=CARTESIAN_POINT('Ctrl Pts',(10.0514428414941,47.5812499998202,-3.26591175476071));
#290767=CARTESIAN_POINT('Ctrl Pts',(8.13178807675715,47.7312499998196,-5.90808986649102));
#290768=CARTESIAN_POINT('Ctrl Pts',(6.21213331202018,47.881249999819,-8.55026797822134));
#290769=CARTESIAN_POINT('Ctrl Pts',(3.10606665601007,48.0312499998184,-9.5594902125713));
#290770=CARTESIAN_POINT('Ctrl Pts',(-4.08725011941195E-14,48.1812499998178,
-10.5687124469213));
#290771=CARTESIAN_POINT('Ctrl Pts',(-3.10606665601015,48.3312499998172,
-9.5594902125713));
#290772=CARTESIAN_POINT('Ctrl Pts',(-6.21213331202026,48.4812499998166,
-8.55026797822134));
#290773=CARTESIAN_POINT('Ctrl Pts',(-8.13178807675723,48.6312499998159,
-5.90808986649102));
#290774=CARTESIAN_POINT('Ctrl Pts',(-10.0514428414942,48.7812499998153,
-3.2659117547607));
#290775=CARTESIAN_POINT('Ctrl Pts',(-10.0514428414942,48.9312499998147,
2.46189346052968E-15));
#290776=CARTESIAN_POINT('Ctrl Pts',(-10.0514428414942,49.0812499998141,
3.26591175476071));
#290777=CARTESIAN_POINT('Ctrl Pts',(-8.13178807675723,49.2312499998135,
5.90808986649102));
#290778=CARTESIAN_POINT('Ctrl Pts',(-6.21213331202025,49.3812499998129,
8.55026797822134));
#290779=CARTESIAN_POINT('Ctrl Pts',(-3.10606665601015,49.5312499998124,
9.5594902125713));
#290780=CARTESIAN_POINT('Ctrl Pts',(-3.91477678561042E-14,49.6812499998118,
10.5687124469213));
#290781=CARTESIAN_POINT('Ctrl Pts',(3.10606665601007,49.8312499998111,9.5594902125713));
#290782=CARTESIAN_POINT('Ctrl Pts',(6.21213331202018,49.9812499998106,8.55026797822134));
#290783=CARTESIAN_POINT('Ctrl Pts',(8.13178807675715,50.13124999981,5.90808986649102));
#290784=CARTESIAN_POINT('Ctrl Pts',(10.0514428414941,50.2812499998094,3.2659117547607));
#290785=CARTESIAN_POINT('Ctrl Pts',(10.0514428414941,50.4312499998088,-1.23094673026484E-15));
#290786=CARTESIAN_POINT('Origin',(-3.77475828372553E-14,-1.881249999982,
2.68644078414671E-15));
#290787=CARTESIAN_POINT('',(10.0514428414941,53.8062499997953,1.22432160604502E-15));
#290788=CARTESIAN_POINT('',(10.0514428414941,53.4312499997968,1.22587832286547E-15));
#290789=CARTESIAN_POINT('',(10.0514428414941,-1.881249999982,4.14193483802857E-15));
#290790=CARTESIAN_POINT('Ctrl Pts',(10.0514428414941,50.8062499998072,-1.23094673026484E-15));
#290791=CARTESIAN_POINT('Ctrl Pts',(10.0514428414941,50.9562499998067,-3.26591175476071));
#290792=CARTESIAN_POINT('Ctrl Pts',(8.13178807675715,51.1062499998061,-5.90808986649102));
#290793=CARTESIAN_POINT('Ctrl Pts',(6.21213331202017,51.2562499998054,-8.55026797822134));
#290794=CARTESIAN_POINT('Ctrl Pts',(3.10606665601006,51.4062499998048,-9.5594902125713));
#290795=CARTESIAN_POINT('Ctrl Pts',(-4.2816174124739E-14,51.5562499998043,
-10.5687124469213));
#290796=CARTESIAN_POINT('Ctrl Pts',(-3.10606665601015,51.7062499998037,
-9.5594902125713));
#290797=CARTESIAN_POINT('Ctrl Pts',(-6.21213331202026,51.856249999803,-8.55026797822134));
#290798=CARTESIAN_POINT('Ctrl Pts',(-8.13178807675723,52.0062499998025,
-5.90808986649102));
#290799=CARTESIAN_POINT('Ctrl Pts',(-10.0514428414942,52.1562499998019,
-3.2659117547607));
#290800=CARTESIAN_POINT('Ctrl Pts',(-10.0514428414942,52.3062499998012,
2.46189346052968E-15));
#290801=CARTESIAN_POINT('Ctrl Pts',(-10.0514428414942,52.4562499998006,
3.26591175476071));
#290802=CARTESIAN_POINT('Ctrl Pts',(-8.13178807675723,52.6062499998,5.90808986649102));
#290803=CARTESIAN_POINT('Ctrl Pts',(-6.21213331202026,52.7562499997994,
8.55026797822134));
#290804=CARTESIAN_POINT('Ctrl Pts',(-3.10606665601015,52.9062499997988,
9.5594902125713));
#290805=CARTESIAN_POINT('Ctrl Pts',(-4.10914407867238E-14,53.0562499997983,
10.5687124469213));
#290806=CARTESIAN_POINT('Ctrl Pts',(3.10606665601007,53.2062499997976,9.5594902125713));
#290807=CARTESIAN_POINT('Ctrl Pts',(6.21213331202018,53.356249999797,8.55026797822134));
#290808=CARTESIAN_POINT('Ctrl Pts',(8.13178807675715,53.5062499997965,5.90808986649102));
#290809=CARTESIAN_POINT('Ctrl Pts',(10.0514428414941,53.6562499997959,3.2659117547607));
#290810=CARTESIAN_POINT('Ctrl Pts',(10.0514428414941,53.8062499997953,-1.23094673026484E-15));
#290811=CARTESIAN_POINT('Ctrl Pts',(10.0514428414941,50.4312499998088,-1.23094673026484E-15));
#290812=CARTESIAN_POINT('Ctrl Pts',(10.0514428414941,50.5812499998082,-3.26591175476071));
#290813=CARTESIAN_POINT('Ctrl Pts',(8.13178807675715,50.7312499998076,-5.90808986649102));
#290814=CARTESIAN_POINT('Ctrl Pts',(6.21213331202017,50.881249999807,-8.55026797822134));
#290815=CARTESIAN_POINT('Ctrl Pts',(3.10606665601007,51.0312499998064,-9.5594902125713));
#290816=CARTESIAN_POINT('Ctrl Pts',(-4.26002104657813E-14,51.1812499998058,
-10.5687124469213));
#290817=CARTESIAN_POINT('Ctrl Pts',(-3.10606665601015,51.3312499998052,
-9.5594902125713));
#290818=CARTESIAN_POINT('Ctrl Pts',(-6.21213331202026,51.4812499998045,
-8.55026797822134));
#290819=CARTESIAN_POINT('Ctrl Pts',(-8.13178807675723,51.631249999804,-5.90808986649102));
#290820=CARTESIAN_POINT('Ctrl Pts',(-10.0514428414942,51.7812499998033,
-3.2659117547607));
#290821=CARTESIAN_POINT('Ctrl Pts',(-10.0514428414942,51.9312499998027,
2.46189346052968E-15));
#290822=CARTESIAN_POINT('Ctrl Pts',(-10.0514428414942,52.0812499998021,
3.26591175476071));
#290823=CARTESIAN_POINT('Ctrl Pts',(-8.13178807675723,52.2312499998015,
5.90808986649102));
#290824=CARTESIAN_POINT('Ctrl Pts',(-6.21213331202026,52.3812499998009,
8.55026797822134));
#290825=CARTESIAN_POINT('Ctrl Pts',(-3.10606665601015,52.5312499998004,
9.5594902125713));
#290826=CARTESIAN_POINT('Ctrl Pts',(-4.08754771277661E-14,52.6812499997997,
10.5687124469213));
#290827=CARTESIAN_POINT('Ctrl Pts',(3.10606665601007,52.8312499997991,9.5594902125713));
#290828=CARTESIAN_POINT('Ctrl Pts',(6.21213331202018,52.9812499997985,8.55026797822134));
#290829=CARTESIAN_POINT('Ctrl Pts',(8.13178807675715,53.131249999798,5.90808986649102));
#290830=CARTESIAN_POINT('Ctrl Pts',(10.0514428414941,53.2812499997974,3.2659117547607));
#290831=CARTESIAN_POINT('Ctrl Pts',(10.0514428414941,53.4312499997968,-1.23094673026484E-15));
#290832=CARTESIAN_POINT('Origin',(-3.77475828372553E-14,-1.881249999982,
2.68644078414671E-15));
#290833=CARTESIAN_POINT('',(10.0514428414941,56.8062499997833,1.21186787148142E-15));
#290834=CARTESIAN_POINT('',(10.0514428414941,56.4312499997848,1.21342458830187E-15));
#290835=CARTESIAN_POINT('',(10.0514428414941,-1.881249999982,4.14193483802857E-15));
#290836=CARTESIAN_POINT('Ctrl Pts',(10.0514428414941,53.8062499997953,-1.23094673026484E-15));
#290837=CARTESIAN_POINT('Ctrl Pts',(10.0514428414941,53.9562499997946,-3.26591175476071));
#290838=CARTESIAN_POINT('Ctrl Pts',(8.13178807675714,54.106249999794,-5.90808986649102));
#290839=CARTESIAN_POINT('Ctrl Pts',(6.21213331202017,54.2562499997934,-8.55026797822134));
#290840=CARTESIAN_POINT('Ctrl Pts',(3.10606665601006,54.4062499997928,-9.5594902125713));
#290841=CARTESIAN_POINT('Ctrl Pts',(-4.45438833964009E-14,54.5562499997923,
-10.5687124469213));
#290842=CARTESIAN_POINT('Ctrl Pts',(-3.10606665601015,54.7062499997917,
-9.5594902125713));
#290843=CARTESIAN_POINT('Ctrl Pts',(-6.21213331202026,54.856249999791,-8.55026797822134));
#290844=CARTESIAN_POINT('Ctrl Pts',(-8.13178807675724,55.0062499997905,
-5.90808986649102));
#290845=CARTESIAN_POINT('Ctrl Pts',(-10.0514428414942,55.1562499997898,
-3.2659117547607));
#290846=CARTESIAN_POINT('Ctrl Pts',(-10.0514428414942,55.3062499997893,
2.46189346052968E-15));
#290847=CARTESIAN_POINT('Ctrl Pts',(-10.0514428414942,55.4562499997886,
3.26591175476071));
#290848=CARTESIAN_POINT('Ctrl Pts',(-8.13178807675724,55.606249999788,5.90808986649102));
#290849=CARTESIAN_POINT('Ctrl Pts',(-6.21213331202026,55.7562499997874,
8.55026797822134));
#290850=CARTESIAN_POINT('Ctrl Pts',(-3.10606665601015,55.9062499997869,
9.5594902125713));
#290851=CARTESIAN_POINT('Ctrl Pts',(-4.28191500583856E-14,56.0562499997862,
10.5687124469213));
#290852=CARTESIAN_POINT('Ctrl Pts',(3.10606665601006,56.2062499997857,9.5594902125713));
#290853=CARTESIAN_POINT('Ctrl Pts',(6.21213331202017,56.356249999785,8.55026797822134));
#290854=CARTESIAN_POINT('Ctrl Pts',(8.13178807675714,56.5062499997845,5.90808986649102));
#290855=CARTESIAN_POINT('Ctrl Pts',(10.0514428414941,56.6562499997839,3.2659117547607));
#290856=CARTESIAN_POINT('Ctrl Pts',(10.0514428414941,56.8062499997833,-1.23094673026484E-15));
#290857=CARTESIAN_POINT('Ctrl Pts',(10.0514428414941,53.4312499997968,-1.23094673026484E-15));
#290858=CARTESIAN_POINT('Ctrl Pts',(10.0514428414941,53.5812499997962,-3.26591175476071));
#290859=CARTESIAN_POINT('Ctrl Pts',(8.13178807675714,53.7312499997956,-5.90808986649102));
#290860=CARTESIAN_POINT('Ctrl Pts',(6.21213331202017,53.881249999795,-8.55026797822134));
#290861=CARTESIAN_POINT('Ctrl Pts',(3.10606665601006,54.0312499997944,-9.5594902125713));
#290862=CARTESIAN_POINT('Ctrl Pts',(-4.43279197374432E-14,54.1812499997938,
-10.5687124469213));
#290863=CARTESIAN_POINT('Ctrl Pts',(-3.10606665601015,54.3312499997932,
-9.5594902125713));
#290864=CARTESIAN_POINT('Ctrl Pts',(-6.21213331202026,54.4812499997926,
-8.55026797822134));
#290865=CARTESIAN_POINT('Ctrl Pts',(-8.13178807675724,54.6312499997919,
-5.90808986649102));
#290866=CARTESIAN_POINT('Ctrl Pts',(-10.0514428414942,54.7812499997913,
-3.2659117547607));
#290867=CARTESIAN_POINT('Ctrl Pts',(-10.0514428414942,54.9312499997907,
2.46189346052968E-15));
#290868=CARTESIAN_POINT('Ctrl Pts',(-10.0514428414942,55.0812499997901,
3.26591175476071));
#290869=CARTESIAN_POINT('Ctrl Pts',(-8.13178807675724,55.2312499997895,
5.90808986649102));
#290870=CARTESIAN_POINT('Ctrl Pts',(-6.21213331202026,55.3812499997889,
8.55026797822134));
#290871=CARTESIAN_POINT('Ctrl Pts',(-3.10606665601015,55.5312499997884,
9.5594902125713));
#290872=CARTESIAN_POINT('Ctrl Pts',(-4.26031863994279E-14,55.6812499997877,
10.5687124469213));
#290873=CARTESIAN_POINT('Ctrl Pts',(3.10606665601006,55.8312499997871,9.5594902125713));
#290874=CARTESIAN_POINT('Ctrl Pts',(6.21213331202017,55.9812499997865,8.55026797822134));
#290875=CARTESIAN_POINT('Ctrl Pts',(8.13178807675714,56.131249999786,5.90808986649102));
#290876=CARTESIAN_POINT('Ctrl Pts',(10.0514428414941,56.2812499997854,3.2659117547607));
#290877=CARTESIAN_POINT('Ctrl Pts',(10.0514428414941,56.4312499997848,-1.23094673026484E-15));
#290878=CARTESIAN_POINT('Origin',(-3.77475828372553E-14,-1.881249999982,
2.68644078414671E-15));
#290879=CARTESIAN_POINT('',(10.0514428414941,59.8062499997713,1.19941413691782E-15));
#290880=CARTESIAN_POINT('',(10.0514428414941,59.4312499997728,1.20097085373827E-15));
#290881=CARTESIAN_POINT('',(10.0514428414941,-1.881249999982,4.14193483802857E-15));
#290882=CARTESIAN_POINT('Ctrl Pts',(10.0514428414941,56.8062499997833,-1.23094673026484E-15));
#290883=CARTESIAN_POINT('Ctrl Pts',(10.0514428414941,56.9562499997827,-3.26591175476071));
#290884=CARTESIAN_POINT('Ctrl Pts',(8.13178807675714,57.1062499997821,-5.90808986649102));
#290885=CARTESIAN_POINT('Ctrl Pts',(6.21213331202017,57.2562499997814,-8.55026797822134));
#290886=CARTESIAN_POINT('Ctrl Pts',(3.10606665601006,57.4062499997808,-9.5594902125713));
#290887=CARTESIAN_POINT('Ctrl Pts',(-4.62715926680627E-14,57.5562499997802,
-10.5687124469213));
#290888=CARTESIAN_POINT('Ctrl Pts',(-3.10606665601015,57.7062499997797,
-9.5594902125713));
#290889=CARTESIAN_POINT('Ctrl Pts',(-6.21213331202026,57.856249999779,-8.55026797822134));
#290890=CARTESIAN_POINT('Ctrl Pts',(-8.13178807675724,58.0062499997784,
-5.90808986649102));
#290891=CARTESIAN_POINT('Ctrl Pts',(-10.0514428414942,58.1562499997778,
-3.2659117547607));
#290892=CARTESIAN_POINT('Ctrl Pts',(-10.0514428414942,58.3062499997773,
2.46189346052968E-15));
#290893=CARTESIAN_POINT('Ctrl Pts',(-10.0514428414942,58.4562499997766,
3.26591175476071));
#290894=CARTESIAN_POINT('Ctrl Pts',(-8.13178807675724,58.6062499997761,
5.90808986649102));
#290895=CARTESIAN_POINT('Ctrl Pts',(-6.21213331202026,58.7562499997754,
8.55026797822134));
#290896=CARTESIAN_POINT('Ctrl Pts',(-3.10606665601015,58.9062499997749,
9.5594902125713));
#290897=CARTESIAN_POINT('Ctrl Pts',(-4.45468593300475E-14,59.0562499997742,
10.5687124469213));
#290898=CARTESIAN_POINT('Ctrl Pts',(3.10606665601006,59.2062499997736,9.5594902125713));
#290899=CARTESIAN_POINT('Ctrl Pts',(6.21213331202017,59.356249999773,8.55026797822134));
#290900=CARTESIAN_POINT('Ctrl Pts',(8.13178807675714,59.5062499997725,5.90808986649102));
#290901=CARTESIAN_POINT('Ctrl Pts',(10.0514428414941,59.6562499997719,3.2659117547607));
#290902=CARTESIAN_POINT('Ctrl Pts',(10.0514428414941,59.8062499997713,-1.23094673026484E-15));
#290903=CARTESIAN_POINT('Ctrl Pts',(10.0514428414941,56.4312499997848,-1.23094673026484E-15));
#290904=CARTESIAN_POINT('Ctrl Pts',(10.0514428414941,56.5812499997842,-3.26591175476071));
#290905=CARTESIAN_POINT('Ctrl Pts',(8.13178807675714,56.7312499997836,-5.90808986649102));
#290906=CARTESIAN_POINT('Ctrl Pts',(6.21213331202017,56.881249999783,-8.55026797822134));
#290907=CARTESIAN_POINT('Ctrl Pts',(3.10606665601006,57.0312499997824,-9.5594902125713));
#290908=CARTESIAN_POINT('Ctrl Pts',(-4.6055629009105E-14,57.1812499997818,
-10.5687124469213));
#290909=CARTESIAN_POINT('Ctrl Pts',(-3.10606665601015,57.3312499997812,
-9.5594902125713));
#290910=CARTESIAN_POINT('Ctrl Pts',(-6.21213331202026,57.4812499997805,
-8.55026797822134));
#290911=CARTESIAN_POINT('Ctrl Pts',(-8.13178807675724,57.6312499997799,
-5.90808986649102));
#290912=CARTESIAN_POINT('Ctrl Pts',(-10.0514428414942,57.7812499997793,
-3.2659117547607));
#290913=CARTESIAN_POINT('Ctrl Pts',(-10.0514428414942,57.9312499997787,
2.46189346052968E-15));
#290914=CARTESIAN_POINT('Ctrl Pts',(-10.0514428414942,58.0812499997781,
3.26591175476071));
#290915=CARTESIAN_POINT('Ctrl Pts',(-8.13178807675724,58.2312499997775,
5.90808986649102));
#290916=CARTESIAN_POINT('Ctrl Pts',(-6.21213331202026,58.3812499997769,
8.55026797822134));
#290917=CARTESIAN_POINT('Ctrl Pts',(-3.10606665601015,58.5312499997763,
9.5594902125713));
#290918=CARTESIAN_POINT('Ctrl Pts',(-4.43308956710897E-14,58.6812499997757,
10.5687124469213));
#290919=CARTESIAN_POINT('Ctrl Pts',(3.10606665601006,58.8312499997751,9.5594902125713));
#290920=CARTESIAN_POINT('Ctrl Pts',(6.21213331202017,58.9812499997745,8.55026797822134));
#290921=CARTESIAN_POINT('Ctrl Pts',(8.13178807675714,59.131249999774,5.90808986649102));
#290922=CARTESIAN_POINT('Ctrl Pts',(10.0514428414941,59.2812499997734,3.2659117547607));
#290923=CARTESIAN_POINT('Ctrl Pts',(10.0514428414941,59.4312499997728,-1.23094673026484E-15));
#290924=CARTESIAN_POINT('Origin',(-3.77475828372553E-14,-1.881249999982,
2.68644078414671E-15));
#290925=CARTESIAN_POINT('',(10.0514428414941,92.8062499996392,1.0624230567182E-15));
#290926=CARTESIAN_POINT('',(10.0514428414941,92.4312499996408,1.06397977353865E-15));
#290927=CARTESIAN_POINT('',(10.0514428414941,-1.881249999982,4.14193483802857E-15));
#290928=CARTESIAN_POINT('',(-9.73188510064473,91.186,-2.51434197826683));
#290929=CARTESIAN_POINT('Ctrl Pts',(-9.73188510064473,91.186,-2.51434197826683));
#290930=CARTESIAN_POINT('Ctrl Pts',(-10.0514428414942,91.2475767399999,
-1.27747792244231));
#290931=CARTESIAN_POINT('Ctrl Pts',(-10.0514428414942,91.3062499996452,
2.46189346052968E-15));
#290932=CARTESIAN_POINT('Ctrl Pts',(-10.0514428414942,91.4562499996446,
3.26591175476071));
#290933=CARTESIAN_POINT('Ctrl Pts',(-8.13178807675726,91.606249999644,5.90808986649102));
#290934=CARTESIAN_POINT('Ctrl Pts',(-6.21213331202028,91.7562499996434,
8.55026797822134));
#290935=CARTESIAN_POINT('Ctrl Pts',(-3.10606665601017,91.9062499996429,
9.5594902125713));
#290936=CARTESIAN_POINT('Ctrl Pts',(-6.35516613183277E-14,92.0562499996422,
10.5687124469213));
#290937=CARTESIAN_POINT('Ctrl Pts',(3.10606665601004,92.2062499996417,9.5594902125713));
#290938=CARTESIAN_POINT('Ctrl Pts',(6.21213331202015,92.3562499996411,8.55026797822134));
#290939=CARTESIAN_POINT('Ctrl Pts',(8.13178807675712,92.5062499996404,5.90808986649102));
#290940=CARTESIAN_POINT('Ctrl Pts',(10.0514428414941,92.6562499996398,3.2659117547607));
#290941=CARTESIAN_POINT('Ctrl Pts',(10.0514428414941,92.8062499996392,-1.23094673026484E-15));
#290942=CARTESIAN_POINT('',(-8.66397270809404,91.1859999999999,5.09579043026958));
#290943=CARTESIAN_POINT('Origin',(-3.77475828372553E-14,91.186,1.91375089876756E-15));
#290944=CARTESIAN_POINT('Ctrl Pts',(-8.66397270809405,91.1859999999999,
5.09579043026958));
#290945=CARTESIAN_POINT('Ctrl Pts',(-8.41752315772121,91.2089229318145,
5.51480926700787));
#290946=CARTESIAN_POINT('Ctrl Pts',(-8.13178807675726,91.2312499996455,
5.90808986649102));
#290947=CARTESIAN_POINT('Ctrl Pts',(-6.21213331202028,91.381249999645,8.55026797822134));
#290948=CARTESIAN_POINT('Ctrl Pts',(-3.10606665601017,91.5312499996443,
9.5594902125713));
#290949=CARTESIAN_POINT('Ctrl Pts',(-6.333569765937E-14,91.6812499996438,
10.5687124469213));
#290950=CARTESIAN_POINT('Ctrl Pts',(3.10606665601004,91.8312499996431,9.5594902125713));
#290951=CARTESIAN_POINT('Ctrl Pts',(6.21213331202015,91.9812499996426,8.55026797822134));
#290952=CARTESIAN_POINT('Ctrl Pts',(8.13178807675712,92.131249999642,5.90808986649102));
#290953=CARTESIAN_POINT('Ctrl Pts',(10.0514428414941,92.2812499996413,3.2659117547607));
#290954=CARTESIAN_POINT('Ctrl Pts',(10.0514428414941,92.4312499996408,-1.23094673026484E-15));
#290955=CARTESIAN_POINT('Origin',(-3.77475828372553E-14,-1.881249999982,
2.68644078414671E-15));
#290956=CARTESIAN_POINT('',(10.0514428414941,95.8062499996273,1.0499693221546E-15));
#290957=CARTESIAN_POINT('',(10.0514428414941,95.4312499996288,1.05152603897505E-15));
#290958=CARTESIAN_POINT('',(10.0514428414941,-1.881249999982,4.14193483802857E-15));
#290959=CARTESIAN_POINT('Ctrl Pts',(10.0514428414941,92.8062499996392,-1.23094673026484E-15));
#290960=CARTESIAN_POINT('Ctrl Pts',(10.0514428414941,92.9562499996387,-3.26591175476071));
#290961=CARTESIAN_POINT('Ctrl Pts',(8.13178807675712,93.1062499996381,-5.90808986649102));
#290962=CARTESIAN_POINT('Ctrl Pts',(6.21213331202015,93.2562499996374,-8.55026797822134));
#290963=CARTESIAN_POINT('Ctrl Pts',(3.10606665601004,93.4062499996369,-9.5594902125713));
#290964=CARTESIAN_POINT('Ctrl Pts',(-6.70041039280048E-14,93.5562499996362,
-10.5687124469213));
#290965=CARTESIAN_POINT('Ctrl Pts',(-3.10606665601018,93.7062499996357,
-9.5594902125713));
#290966=CARTESIAN_POINT('Ctrl Pts',(-6.21213331202028,93.856249999635,-8.55026797822134));
#290967=CARTESIAN_POINT('Ctrl Pts',(-8.13178807675726,94.0062499996344,
-5.90808986649102));
#290968=CARTESIAN_POINT('Ctrl Pts',(-10.0514428414942,94.1562499996338,
-3.2659117547607));
#290969=CARTESIAN_POINT('Ctrl Pts',(-10.0514428414942,94.3062499996333,
2.46189346052968E-15));
#290970=CARTESIAN_POINT('Ctrl Pts',(-10.0514428414942,94.4562499996326,
3.26591175476071));
#290971=CARTESIAN_POINT('Ctrl Pts',(-8.13178807675726,94.606249999632,5.90808986649102));
#290972=CARTESIAN_POINT('Ctrl Pts',(-6.21213331202028,94.7562499996315,
8.55026797822134));
#290973=CARTESIAN_POINT('Ctrl Pts',(-3.10606665601017,94.9062499996309,
9.5594902125713));
#290974=CARTESIAN_POINT('Ctrl Pts',(-6.52793705899895E-14,95.0562499996302,
10.5687124469213));
#290975=CARTESIAN_POINT('Ctrl Pts',(3.10606665601004,95.2062499996296,9.5594902125713));
#290976=CARTESIAN_POINT('Ctrl Pts',(6.21213331202015,95.3562499996291,8.55026797822134));
#290977=CARTESIAN_POINT('Ctrl Pts',(8.13178807675712,95.5062499996285,5.90808986649102));
#290978=CARTESIAN_POINT('Ctrl Pts',(10.0514428414941,95.6562499996278,3.2659117547607));
#290979=CARTESIAN_POINT('Ctrl Pts',(10.0514428414941,95.8062499996273,-1.23094673026484E-15));
#290980=CARTESIAN_POINT('Ctrl Pts',(10.0514428414941,92.4312499996408,-1.23094673026484E-15));
#290981=CARTESIAN_POINT('Ctrl Pts',(10.0514428414941,92.5812499996402,-3.26591175476071));
#290982=CARTESIAN_POINT('Ctrl Pts',(8.13178807675712,92.7312499996396,-5.90808986649102));
#290983=CARTESIAN_POINT('Ctrl Pts',(6.21213331202015,92.8812499996389,-8.55026797822134));
#290984=CARTESIAN_POINT('Ctrl Pts',(3.10606665601004,93.0312499996383,-9.5594902125713));
#290985=CARTESIAN_POINT('Ctrl Pts',(-6.67881402690471E-14,93.1812499996377,
-10.5687124469213));
#290986=CARTESIAN_POINT('Ctrl Pts',(-3.10606665601018,93.3312499996371,
-9.5594902125713));
#290987=CARTESIAN_POINT('Ctrl Pts',(-6.21213331202028,93.4812499996365,
-8.55026797822134));
#290988=CARTESIAN_POINT('Ctrl Pts',(-8.13178807675726,93.6312499996359,
-5.90808986649102));
#290989=CARTESIAN_POINT('Ctrl Pts',(-10.0514428414942,93.7812499996353,
-3.2659117547607));
#290990=CARTESIAN_POINT('Ctrl Pts',(-10.0514428414942,93.9312499996347,
2.46189346052968E-15));
#290991=CARTESIAN_POINT('Ctrl Pts',(-10.0514428414942,94.0812499996341,
3.26591175476071));
#290992=CARTESIAN_POINT('Ctrl Pts',(-8.13178807675726,94.2312499996335,
5.90808986649102));
#290993=CARTESIAN_POINT('Ctrl Pts',(-6.21213331202028,94.3812499996329,
8.55026797822134));
#290994=CARTESIAN_POINT('Ctrl Pts',(-3.10606665601017,94.5312499996324,
9.5594902125713));
#290995=CARTESIAN_POINT('Ctrl Pts',(-6.50634069310318E-14,94.6812499996317,
10.5687124469213));
#290996=CARTESIAN_POINT('Ctrl Pts',(3.10606665601004,94.8312499996312,9.5594902125713));
#290997=CARTESIAN_POINT('Ctrl Pts',(6.21213331202015,94.9812499996305,8.55026797822134));
#290998=CARTESIAN_POINT('Ctrl Pts',(8.13178807675712,95.13124999963,5.90808986649102));
#290999=CARTESIAN_POINT('Ctrl Pts',(10.0514428414941,95.2812499996293,3.2659117547607));
#291000=CARTESIAN_POINT('Ctrl Pts',(10.0514428414941,95.4312499996288,-1.23094673026484E-15));
#291001=CARTESIAN_POINT('Origin',(-3.77475828372553E-14,-1.881249999982,
2.68644078414671E-15));
#291002=CARTESIAN_POINT('',(10.0514428414941,98.8062499996153,1.037515587591E-15));
#291003=CARTESIAN_POINT('',(10.0514428414941,98.4312499996168,1.03907230441145E-15));
#291004=CARTESIAN_POINT('',(10.0514428414941,-1.881249999982,4.14193483802857E-15));
#291005=CARTESIAN_POINT('Ctrl Pts',(10.0514428414941,95.8062499996273,-1.23094673026484E-15));
#291006=CARTESIAN_POINT('Ctrl Pts',(10.0514428414941,95.9562499996266,-3.26591175476071));
#291007=CARTESIAN_POINT('Ctrl Pts',(8.13178807675712,96.1062499996261,-5.90808986649102));
#291008=CARTESIAN_POINT('Ctrl Pts',(6.21213331202015,96.2562499996255,-8.55026797822134));
#291009=CARTESIAN_POINT('Ctrl Pts',(3.10606665601004,96.4062499996248,-9.5594902125713));
#291010=CARTESIAN_POINT('Ctrl Pts',(-6.87318131996666E-14,96.5562499996243,
-10.5687124469213));
#291011=CARTESIAN_POINT('Ctrl Pts',(-3.10606665601018,96.7062499996236,
-9.5594902125713));
#291012=CARTESIAN_POINT('Ctrl Pts',(-6.21213331202028,96.856249999623,-8.55026797822134));
#291013=CARTESIAN_POINT('Ctrl Pts',(-8.13178807675726,97.0062499996224,
-5.90808986649102));
#291014=CARTESIAN_POINT('Ctrl Pts',(-10.0514428414942,97.1562499996218,
-3.2659117547607));
#291015=CARTESIAN_POINT('Ctrl Pts',(-10.0514428414942,97.3062499996212,
2.46189346052968E-15));
#291016=CARTESIAN_POINT('Ctrl Pts',(-10.0514428414942,97.4562499996206,
3.26591175476071));
#291017=CARTESIAN_POINT('Ctrl Pts',(-8.13178807675726,97.60624999962,5.90808986649102));
#291018=CARTESIAN_POINT('Ctrl Pts',(-6.21213331202028,97.7562499996194,
8.55026797822134));
#291019=CARTESIAN_POINT('Ctrl Pts',(-3.10606665601018,97.9062499996189,
9.5594902125713));
#291020=CARTESIAN_POINT('Ctrl Pts',(-6.70070798616514E-14,98.0562499996182,
10.5687124469213));
#291021=CARTESIAN_POINT('Ctrl Pts',(3.10606665601004,98.2062499996177,9.5594902125713));
#291022=CARTESIAN_POINT('Ctrl Pts',(6.21213331202015,98.3562499996171,8.55026797822134));
#291023=CARTESIAN_POINT('Ctrl Pts',(8.13178807675712,98.5062499996165,5.90808986649102));
#291024=CARTESIAN_POINT('Ctrl Pts',(10.0514428414941,98.6562499996158,3.2659117547607));
#291025=CARTESIAN_POINT('Ctrl Pts',(10.0514428414941,98.8062499996153,-1.23094673026484E-15));
#291026=CARTESIAN_POINT('Ctrl Pts',(10.0514428414941,95.4312499996288,-1.23094673026484E-15));
#291027=CARTESIAN_POINT('Ctrl Pts',(10.0514428414941,95.5812499996282,-3.26591175476071));
#291028=CARTESIAN_POINT('Ctrl Pts',(8.13178807675712,95.7312499996276,-5.90808986649102));
#291029=CARTESIAN_POINT('Ctrl Pts',(6.21213331202015,95.8812499996269,-8.55026797822134));
#291030=CARTESIAN_POINT('Ctrl Pts',(3.10606665601004,96.0312499996264,-9.5594902125713));
#291031=CARTESIAN_POINT('Ctrl Pts',(-6.85158495407089E-14,96.1812499996257,
-10.5687124469213));
#291032=CARTESIAN_POINT('Ctrl Pts',(-3.10606665601018,96.3312499996252,
-9.5594902125713));
#291033=CARTESIAN_POINT('Ctrl Pts',(-6.21213331202028,96.4812499996245,
-8.55026797822134));
#291034=CARTESIAN_POINT('Ctrl Pts',(-8.13178807675726,96.6312499996239,
-5.90808986649102));
#291035=CARTESIAN_POINT('Ctrl Pts',(-10.0514428414942,96.7812499996234,
-3.2659117547607));
#291036=CARTESIAN_POINT('Ctrl Pts',(-10.0514428414942,96.9312499996227,
2.46189346052968E-15));
#291037=CARTESIAN_POINT('Ctrl Pts',(-10.0514428414942,97.0812499996221,
3.26591175476071));
#291038=CARTESIAN_POINT('Ctrl Pts',(-8.13178807675726,97.2312499996215,
5.90808986649102));
#291039=CARTESIAN_POINT('Ctrl Pts',(-6.21213331202028,97.381249999621,8.55026797822134));
#291040=CARTESIAN_POINT('Ctrl Pts',(-3.10606665601017,97.5312499996203,
9.5594902125713));
#291041=CARTESIAN_POINT('Ctrl Pts',(-6.67911162026936E-14,97.6812499996198,
10.5687124469213));
#291042=CARTESIAN_POINT('Ctrl Pts',(3.10606665601004,97.8312499996191,9.5594902125713));
#291043=CARTESIAN_POINT('Ctrl Pts',(6.21213331202015,97.9812499996186,8.55026797822134));
#291044=CARTESIAN_POINT('Ctrl Pts',(8.13178807675712,98.1312499996179,5.90808986649102));
#291045=CARTESIAN_POINT('Ctrl Pts',(10.0514428414941,98.2812499996173,3.2659117547607));
#291046=CARTESIAN_POINT('Ctrl Pts',(10.0514428414941,98.4312499996168,-1.23094673026484E-15));
#291047=CARTESIAN_POINT('Origin',(-3.77475828372553E-14,-1.881249999982,
2.68644078414671E-15));
#291048=CARTESIAN_POINT('',(10.0514428414941,101.806249999603,1.0250618530274E-15));
#291049=CARTESIAN_POINT('',(10.0514428414941,101.431249999605,1.02661856984785E-15));
#291050=CARTESIAN_POINT('',(10.0514428414941,-1.881249999982,4.14193483802857E-15));
#291051=CARTESIAN_POINT('Ctrl Pts',(10.0514428414941,98.8062499996153,-1.23094673026484E-15));
#291052=CARTESIAN_POINT('Ctrl Pts',(10.0514428414941,98.9562499996147,-3.26591175476071));
#291053=CARTESIAN_POINT('Ctrl Pts',(8.13178807675712,99.1062499996141,-5.90808986649102));
#291054=CARTESIAN_POINT('Ctrl Pts',(6.21213331202014,99.2562499996134,-8.55026797822134));
#291055=CARTESIAN_POINT('Ctrl Pts',(3.10606665601004,99.4062499996129,-9.5594902125713));
#291056=CARTESIAN_POINT('Ctrl Pts',(-7.04595224713285E-14,99.5562499996122,
-10.5687124469213));
#291057=CARTESIAN_POINT('Ctrl Pts',(-3.10606665601018,99.7062499996117,
-9.5594902125713));
#291058=CARTESIAN_POINT('Ctrl Pts',(-6.21213331202029,99.856249999611,-8.55026797822134));
#291059=CARTESIAN_POINT('Ctrl Pts',(-8.13178807675726,100.00624999961,-5.90808986649102));
#291060=CARTESIAN_POINT('Ctrl Pts',(-10.0514428414942,100.15624999961,-3.2659117547607));
#291061=CARTESIAN_POINT('Ctrl Pts',(-10.0514428414942,100.306249999609,
2.46189346052968E-15));
#291062=CARTESIAN_POINT('Ctrl Pts',(-10.0514428414942,100.456249999609,
3.26591175476071));
#291063=CARTESIAN_POINT('Ctrl Pts',(-8.13178807675726,100.606249999608,
5.90808986649102));
#291064=CARTESIAN_POINT('Ctrl Pts',(-6.21213331202028,100.756249999607,
8.55026797822134));
#291065=CARTESIAN_POINT('Ctrl Pts',(-3.10606665601018,100.906249999607,
9.5594902125713));
#291066=CARTESIAN_POINT('Ctrl Pts',(-6.87347891333132E-14,101.056249999606,
10.5687124469213));
#291067=CARTESIAN_POINT('Ctrl Pts',(3.10606665601004,101.206249999606,9.5594902125713));
#291068=CARTESIAN_POINT('Ctrl Pts',(6.21213331202015,101.356249999605,8.55026797822134));
#291069=CARTESIAN_POINT('Ctrl Pts',(8.13178807675712,101.506249999604,5.90808986649102));
#291070=CARTESIAN_POINT('Ctrl Pts',(10.0514428414941,101.656249999604,3.2659117547607));
#291071=CARTESIAN_POINT('Ctrl Pts',(10.0514428414941,101.806249999603,-1.23094673026484E-15));
#291072=CARTESIAN_POINT('Ctrl Pts',(10.0514428414941,98.4312499996168,-1.23094673026484E-15));
#291073=CARTESIAN_POINT('Ctrl Pts',(10.0514428414941,98.5812499996162,-3.26591175476071));
#291074=CARTESIAN_POINT('Ctrl Pts',(8.13178807675712,98.7312499996156,-5.90808986649102));
#291075=CARTESIAN_POINT('Ctrl Pts',(6.21213331202014,98.8812499996149,-8.55026797822134));
#291076=CARTESIAN_POINT('Ctrl Pts',(3.10606665601004,99.0312499996143,-9.5594902125713));
#291077=CARTESIAN_POINT('Ctrl Pts',(-7.02435588123707E-14,99.1812499996138,
-10.5687124469213));
#291078=CARTESIAN_POINT('Ctrl Pts',(-3.10606665601018,99.3312499996131,
-9.5594902125713));
#291079=CARTESIAN_POINT('Ctrl Pts',(-6.21213331202029,99.4812499996125,
-8.55026797822134));
#291080=CARTESIAN_POINT('Ctrl Pts',(-8.13178807675726,99.631249999612,-5.90808986649102));
#291081=CARTESIAN_POINT('Ctrl Pts',(-10.0514428414942,99.7812499996114,
-3.2659117547607));
#291082=CARTESIAN_POINT('Ctrl Pts',(-10.0514428414942,99.9312499996108,
2.46189346052968E-15));
#291083=CARTESIAN_POINT('Ctrl Pts',(-10.0514428414942,100.08124999961,3.26591175476071));
#291084=CARTESIAN_POINT('Ctrl Pts',(-8.13178807675726,100.23124999961,5.90808986649102));
#291085=CARTESIAN_POINT('Ctrl Pts',(-6.21213331202028,100.381249999609,
8.55026797822134));
#291086=CARTESIAN_POINT('Ctrl Pts',(-3.10606665601018,100.531249999608,
9.5594902125713));
#291087=CARTESIAN_POINT('Ctrl Pts',(-6.85188254743555E-14,100.681249999608,
10.5687124469213));
#291088=CARTESIAN_POINT('Ctrl Pts',(3.10606665601004,100.831249999607,9.5594902125713));
#291089=CARTESIAN_POINT('Ctrl Pts',(6.21213331202015,100.981249999607,8.55026797822134));
#291090=CARTESIAN_POINT('Ctrl Pts',(8.13178807675712,101.131249999606,5.90808986649102));
#291091=CARTESIAN_POINT('Ctrl Pts',(10.0514428414941,101.281249999605,3.2659117547607));
#291092=CARTESIAN_POINT('Ctrl Pts',(10.0514428414941,101.431249999605,-1.23094673026484E-15));
#291093=CARTESIAN_POINT('Origin',(-3.77475828372553E-14,-1.881249999982,
2.68644078414671E-15));
#291094=CARTESIAN_POINT('',(10.0514428414941,104.806249999591,1.0126081184638E-15));
#291095=CARTESIAN_POINT('',(10.0514428414941,104.431249999593,1.01416483528425E-15));
#291096=CARTESIAN_POINT('',(10.0514428414941,-1.881249999982,4.14193483802857E-15));
#291097=CARTESIAN_POINT('Ctrl Pts',(10.0514428414941,101.806249999603,-1.23094673026484E-15));
#291098=CARTESIAN_POINT('Ctrl Pts',(10.0514428414941,101.956249999603,-3.26591175476071));
#291099=CARTESIAN_POINT('Ctrl Pts',(8.13178807675712,102.106249999602,-5.90808986649102));
#291100=CARTESIAN_POINT('Ctrl Pts',(6.21213331202014,102.256249999601,-8.55026797822134));
#291101=CARTESIAN_POINT('Ctrl Pts',(3.10606665601004,102.406249999601,-9.5594902125713));
#291102=CARTESIAN_POINT('Ctrl Pts',(-7.21872317429903E-14,102.5562499996,
-10.5687124469213));
#291103=CARTESIAN_POINT('Ctrl Pts',(-3.10606665601018,102.7062499996,-9.5594902125713));
#291104=CARTESIAN_POINT('Ctrl Pts',(-6.21213331202029,102.856249999599,
-8.55026797822134));
#291105=CARTESIAN_POINT('Ctrl Pts',(-8.13178807675726,103.006249999598,
-5.90808986649102));
#291106=CARTESIAN_POINT('Ctrl Pts',(-10.0514428414942,103.156249999598,
-3.2659117547607));
#291107=CARTESIAN_POINT('Ctrl Pts',(-10.0514428414942,103.306249999597,
2.46189346052968E-15));
#291108=CARTESIAN_POINT('Ctrl Pts',(-10.0514428414942,103.456249999597,
3.26591175476071));
#291109=CARTESIAN_POINT('Ctrl Pts',(-8.13178807675726,103.606249999596,
5.90808986649102));
#291110=CARTESIAN_POINT('Ctrl Pts',(-6.21213331202029,103.756249999595,
8.55026797822134));
#291111=CARTESIAN_POINT('Ctrl Pts',(-3.10606665601018,103.906249999595,
9.5594902125713));
#291112=CARTESIAN_POINT('Ctrl Pts',(-7.0462498404975E-14,104.056249999594,
10.5687124469213));
#291113=CARTESIAN_POINT('Ctrl Pts',(3.10606665601004,104.206249999594,9.5594902125713));
#291114=CARTESIAN_POINT('Ctrl Pts',(6.21213331202014,104.356249999593,8.55026797822134));
#291115=CARTESIAN_POINT('Ctrl Pts',(8.13178807675712,104.506249999592,5.90808986649102));
#291116=CARTESIAN_POINT('Ctrl Pts',(10.0514428414941,104.656249999592,3.2659117547607));
#291117=CARTESIAN_POINT('Ctrl Pts',(10.0514428414941,104.806249999591,-1.23094673026484E-15));
#291118=CARTESIAN_POINT('Ctrl Pts',(10.0514428414941,101.431249999605,-1.23094673026484E-15));
#291119=CARTESIAN_POINT('Ctrl Pts',(10.0514428414941,101.581249999604,-3.26591175476071));
#291120=CARTESIAN_POINT('Ctrl Pts',(8.13178807675712,101.731249999604,-5.90808986649102));
#291121=CARTESIAN_POINT('Ctrl Pts',(6.21213331202014,101.881249999603,-8.55026797822134));
#291122=CARTESIAN_POINT('Ctrl Pts',(3.10606665601004,102.031249999602,-9.5594902125713));
#291123=CARTESIAN_POINT('Ctrl Pts',(-7.19712680840326E-14,102.181249999602,
-10.5687124469213));
#291124=CARTESIAN_POINT('Ctrl Pts',(-3.10606665601018,102.331249999601,
-9.5594902125713));
#291125=CARTESIAN_POINT('Ctrl Pts',(-6.21213331202029,102.481249999601,
-8.55026797822134));
#291126=CARTESIAN_POINT('Ctrl Pts',(-8.13178807675726,102.6312499996,-5.90808986649102));
#291127=CARTESIAN_POINT('Ctrl Pts',(-10.0514428414942,102.781249999599,
-3.2659117547607));
#291128=CARTESIAN_POINT('Ctrl Pts',(-10.0514428414942,102.931249999599,
2.46189346052968E-15));
#291129=CARTESIAN_POINT('Ctrl Pts',(-10.0514428414942,103.081249999598,
3.26591175476071));
#291130=CARTESIAN_POINT('Ctrl Pts',(-8.13178807675726,103.231249999598,
5.90808986649102));
#291131=CARTESIAN_POINT('Ctrl Pts',(-6.21213331202029,103.381249999597,
8.55026797822134));
#291132=CARTESIAN_POINT('Ctrl Pts',(-3.10606665601018,103.531249999596,
9.5594902125713));
#291133=CARTESIAN_POINT('Ctrl Pts',(-7.02465347460173E-14,103.681249999596,
10.5687124469213));
#291134=CARTESIAN_POINT('Ctrl Pts',(3.10606665601004,103.831249999595,9.5594902125713));
#291135=CARTESIAN_POINT('Ctrl Pts',(6.21213331202014,103.981249999595,8.55026797822134));
#291136=CARTESIAN_POINT('Ctrl Pts',(8.13178807675712,104.131249999594,5.90808986649102));
#291137=CARTESIAN_POINT('Ctrl Pts',(10.0514428414941,104.281249999593,3.2659117547607));
#291138=CARTESIAN_POINT('Ctrl Pts',(10.0514428414941,104.431249999593,-1.23094673026484E-15));
#291139=CARTESIAN_POINT('Origin',(-3.77475828372553E-14,-1.881249999982,
2.68644078414671E-15));
#291140=CARTESIAN_POINT('',(10.0514428414941,107.806249999579,1.0001543839002E-15));
#291141=CARTESIAN_POINT('',(10.0514428414941,107.431249999581,1.00171110072065E-15));
#291142=CARTESIAN_POINT('',(10.0514428414941,-1.881249999982,4.14193483802857E-15));
#291143=CARTESIAN_POINT('Ctrl Pts',(10.0514428414941,104.806249999591,-1.23094673026484E-15));
#291144=CARTESIAN_POINT('Ctrl Pts',(10.0514428414941,104.956249999591,-3.26591175476071));
#291145=CARTESIAN_POINT('Ctrl Pts',(8.13178807675712,105.10624999959,-5.90808986649102));
#291146=CARTESIAN_POINT('Ctrl Pts',(6.21213331202014,105.256249999589,-8.55026797822134));
#291147=CARTESIAN_POINT('Ctrl Pts',(3.10606665601003,105.406249999589,-9.5594902125713));
#291148=CARTESIAN_POINT('Ctrl Pts',(-7.39149410146522E-14,105.556249999588,
-10.5687124469213));
#291149=CARTESIAN_POINT('Ctrl Pts',(-3.10606665601018,105.706249999588,
-9.5594902125713));
#291150=CARTESIAN_POINT('Ctrl Pts',(-6.21213331202029,105.856249999587,
-8.55026797822134));
#291151=CARTESIAN_POINT('Ctrl Pts',(-8.13178807675726,106.006249999586,
-5.90808986649102));
#291152=CARTESIAN_POINT('Ctrl Pts',(-10.0514428414942,106.156249999586,
-3.2659117547607));
#291153=CARTESIAN_POINT('Ctrl Pts',(-10.0514428414942,106.306249999585,
2.46189346052968E-15));
#291154=CARTESIAN_POINT('Ctrl Pts',(-10.0514428414942,106.456249999585,
3.26591175476071));
#291155=CARTESIAN_POINT('Ctrl Pts',(-8.13178807675726,106.606249999584,
5.90808986649102));
#291156=CARTESIAN_POINT('Ctrl Pts',(-6.21213331202029,106.756249999583,
8.55026797822134));
#291157=CARTESIAN_POINT('Ctrl Pts',(-3.10606665601018,106.906249999583,
9.5594902125713));
#291158=CARTESIAN_POINT('Ctrl Pts',(-7.21902076766369E-14,107.056249999582,
10.5687124469213));
#291159=CARTESIAN_POINT('Ctrl Pts',(3.10606665601003,107.206249999582,9.5594902125713));
#291160=CARTESIAN_POINT('Ctrl Pts',(6.21213331202014,107.356249999581,8.55026797822134));
#291161=CARTESIAN_POINT('Ctrl Pts',(8.13178807675711,107.50624999958,5.90808986649102));
#291162=CARTESIAN_POINT('Ctrl Pts',(10.0514428414941,107.65624999958,3.2659117547607));
#291163=CARTESIAN_POINT('Ctrl Pts',(10.0514428414941,107.806249999579,-1.23094673026484E-15));
#291164=CARTESIAN_POINT('Ctrl Pts',(10.0514428414941,104.431249999593,-1.23094673026484E-15));
#291165=CARTESIAN_POINT('Ctrl Pts',(10.0514428414941,104.581249999592,-3.26591175476071));
#291166=CARTESIAN_POINT('Ctrl Pts',(8.13178807675712,104.731249999592,-5.90808986649102));
#291167=CARTESIAN_POINT('Ctrl Pts',(6.21213331202014,104.881249999591,-8.55026797822134));
#291168=CARTESIAN_POINT('Ctrl Pts',(3.10606665601003,105.03124999959,-9.5594902125713));
#291169=CARTESIAN_POINT('Ctrl Pts',(-7.36989773556944E-14,105.18124999959,
-10.5687124469213));
#291170=CARTESIAN_POINT('Ctrl Pts',(-3.10606665601018,105.331249999589,
-9.5594902125713));
#291171=CARTESIAN_POINT('Ctrl Pts',(-6.21213331202029,105.481249999589,
-8.55026797822134));
#291172=CARTESIAN_POINT('Ctrl Pts',(-8.13178807675726,105.631249999588,
-5.90808986649102));
#291173=CARTESIAN_POINT('Ctrl Pts',(-10.0514428414942,105.781249999587,
-3.2659117547607));
#291174=CARTESIAN_POINT('Ctrl Pts',(-10.0514428414942,105.931249999587,
2.46189346052968E-15));
#291175=CARTESIAN_POINT('Ctrl Pts',(-10.0514428414942,106.081249999586,
3.26591175476071));
#291176=CARTESIAN_POINT('Ctrl Pts',(-8.13178807675726,106.231249999586,
5.90808986649102));
#291177=CARTESIAN_POINT('Ctrl Pts',(-6.21213331202029,106.381249999585,
8.55026797822134));
#291178=CARTESIAN_POINT('Ctrl Pts',(-3.10606665601018,106.531249999584,
9.5594902125713));
#291179=CARTESIAN_POINT('Ctrl Pts',(-7.19742440176792E-14,106.681249999584,
10.5687124469213));
#291180=CARTESIAN_POINT('Ctrl Pts',(3.10606665601004,106.831249999583,9.5594902125713));
#291181=CARTESIAN_POINT('Ctrl Pts',(6.21213331202014,106.981249999583,8.55026797822134));
#291182=CARTESIAN_POINT('Ctrl Pts',(8.13178807675711,107.131249999582,5.90808986649102));
#291183=CARTESIAN_POINT('Ctrl Pts',(10.0514428414941,107.281249999581,3.2659117547607));
#291184=CARTESIAN_POINT('Ctrl Pts',(10.0514428414941,107.431249999581,-1.23094673026484E-15));
#291185=CARTESIAN_POINT('Origin',(-3.77475828372553E-14,-1.881249999982,
2.68644078414671E-15));
#291186=CARTESIAN_POINT('',(10.0514428414941,110.806249999567,9.87700649336596E-16));
#291187=CARTESIAN_POINT('',(10.0514428414941,110.431249999569,9.89257366157046E-16));
#291188=CARTESIAN_POINT('',(10.0514428414941,-1.881249999982,4.14193483802857E-15));
#291189=CARTESIAN_POINT('Ctrl Pts',(10.0514428414941,107.806249999579,-1.23094673026484E-15));
#291190=CARTESIAN_POINT('Ctrl Pts',(10.0514428414941,107.956249999579,-3.26591175476071));
#291191=CARTESIAN_POINT('Ctrl Pts',(8.13178807675711,108.106249999578,-5.90808986649102));
#291192=CARTESIAN_POINT('Ctrl Pts',(6.21213331202014,108.256249999577,-8.55026797822134));
#291193=CARTESIAN_POINT('Ctrl Pts',(3.10606665601003,108.406249999577,-9.5594902125713));
#291194=CARTESIAN_POINT('Ctrl Pts',(-7.5642650286314E-14,108.556249999576,
-10.5687124469213));
#291195=CARTESIAN_POINT('Ctrl Pts',(-3.10606665601018,108.706249999576,
-9.5594902125713));
#291196=CARTESIAN_POINT('Ctrl Pts',(-6.21213331202029,108.856249999575,
-8.55026797822134));
#291197=CARTESIAN_POINT('Ctrl Pts',(-8.13178807675727,109.006249999574,
-5.90808986649102));
#291198=CARTESIAN_POINT('Ctrl Pts',(-10.0514428414942,109.156249999574,
-3.2659117547607));
#291199=CARTESIAN_POINT('Ctrl Pts',(-10.0514428414942,109.306249999573,
2.46189346052968E-15));
#291200=CARTESIAN_POINT('Ctrl Pts',(-10.0514428414942,109.456249999573,
3.26591175476071));
#291201=CARTESIAN_POINT('Ctrl Pts',(-8.13178807675727,109.606249999572,
5.90808986649102));
#291202=CARTESIAN_POINT('Ctrl Pts',(-6.21213331202029,109.756249999571,
8.55026797822134));
#291203=CARTESIAN_POINT('Ctrl Pts',(-3.10606665601018,109.906249999571,
9.5594902125713));
#291204=CARTESIAN_POINT('Ctrl Pts',(-7.39179169482987E-14,110.05624999957,
10.5687124469213));
#291205=CARTESIAN_POINT('Ctrl Pts',(3.10606665601003,110.20624999957,9.5594902125713));
#291206=CARTESIAN_POINT('Ctrl Pts',(6.21213331202014,110.356249999569,8.55026797822134));
#291207=CARTESIAN_POINT('Ctrl Pts',(8.13178807675711,110.506249999568,5.90808986649102));
#291208=CARTESIAN_POINT('Ctrl Pts',(10.0514428414941,110.656249999568,3.2659117547607));
#291209=CARTESIAN_POINT('Ctrl Pts',(10.0514428414941,110.806249999567,-1.23094673026484E-15));
#291210=CARTESIAN_POINT('Ctrl Pts',(10.0514428414941,107.431249999581,-1.23094673026484E-15));
#291211=CARTESIAN_POINT('Ctrl Pts',(10.0514428414941,107.58124999958,-3.26591175476071));
#291212=CARTESIAN_POINT('Ctrl Pts',(8.13178807675711,107.73124999958,-5.90808986649102));
#291213=CARTESIAN_POINT('Ctrl Pts',(6.21213331202014,107.881249999579,-8.55026797822134));
#291214=CARTESIAN_POINT('Ctrl Pts',(3.10606665601003,108.031249999578,-9.5594902125713));
#291215=CARTESIAN_POINT('Ctrl Pts',(-7.54266866273562E-14,108.181249999578,
-10.5687124469213));
#291216=CARTESIAN_POINT('Ctrl Pts',(-3.10606665601018,108.331249999577,
-9.5594902125713));
#291217=CARTESIAN_POINT('Ctrl Pts',(-6.21213331202029,108.481249999577,
-8.55026797822134));
#291218=CARTESIAN_POINT('Ctrl Pts',(-8.13178807675727,108.631249999576,
-5.90808986649102));
#291219=CARTESIAN_POINT('Ctrl Pts',(-10.0514428414942,108.781249999575,
-3.2659117547607));
#291220=CARTESIAN_POINT('Ctrl Pts',(-10.0514428414942,108.931249999575,
2.46189346052968E-15));
#291221=CARTESIAN_POINT('Ctrl Pts',(-10.0514428414942,109.081249999574,
3.26591175476071));
#291222=CARTESIAN_POINT('Ctrl Pts',(-8.13178807675727,109.231249999574,
5.90808986649102));
#291223=CARTESIAN_POINT('Ctrl Pts',(-6.21213331202029,109.381249999573,
8.55026797822134));
#291224=CARTESIAN_POINT('Ctrl Pts',(-3.10606665601018,109.531249999572,
9.5594902125713));
#291225=CARTESIAN_POINT('Ctrl Pts',(-7.3701953289341E-14,109.681249999572,
10.5687124469213));
#291226=CARTESIAN_POINT('Ctrl Pts',(3.10606665601003,109.831249999571,9.5594902125713));
#291227=CARTESIAN_POINT('Ctrl Pts',(6.21213331202014,109.981249999571,8.55026797822134));
#291228=CARTESIAN_POINT('Ctrl Pts',(8.13178807675711,110.13124999957,5.90808986649102));
#291229=CARTESIAN_POINT('Ctrl Pts',(10.0514428414941,110.281249999569,3.2659117547607));
#291230=CARTESIAN_POINT('Ctrl Pts',(10.0514428414941,110.431249999569,-1.23094673026484E-15));
#291231=CARTESIAN_POINT('Origin',(-3.77475828372553E-14,-1.881249999982,
2.68644078414671E-15));
#291232=CARTESIAN_POINT('',(10.0514428414941,113.806249999555,9.75246914772995E-16));
#291233=CARTESIAN_POINT('',(10.0514428414941,113.431249999557,9.76803631593445E-16));
#291234=CARTESIAN_POINT('',(10.0514428414941,-1.881249999982,4.14193483802857E-15));
#291235=CARTESIAN_POINT('Ctrl Pts',(10.0514428414941,110.806249999567,-1.23094673026484E-15));
#291236=CARTESIAN_POINT('Ctrl Pts',(10.0514428414941,110.956249999567,-3.26591175476071));
#291237=CARTESIAN_POINT('Ctrl Pts',(8.13178807675711,111.106249999566,-5.90808986649102));
#291238=CARTESIAN_POINT('Ctrl Pts',(6.21213331202014,111.256249999565,-8.55026797822134));
#291239=CARTESIAN_POINT('Ctrl Pts',(3.10606665601003,111.406249999565,-9.5594902125713));
#291240=CARTESIAN_POINT('Ctrl Pts',(-7.73703595579758E-14,111.556249999564,
-10.5687124469213));
#291241=CARTESIAN_POINT('Ctrl Pts',(-3.10606665601019,111.706249999564,
-9.5594902125713));
#291242=CARTESIAN_POINT('Ctrl Pts',(-6.21213331202029,111.856249999563,
-8.55026797822134));
#291243=CARTESIAN_POINT('Ctrl Pts',(-8.13178807675727,112.006249999562,
-5.90808986649102));
#291244=CARTESIAN_POINT('Ctrl Pts',(-10.0514428414942,112.156249999562,
-3.2659117547607));
#291245=CARTESIAN_POINT('Ctrl Pts',(-10.0514428414942,112.306249999561,
2.46189346052968E-15));
#291246=CARTESIAN_POINT('Ctrl Pts',(-10.0514428414942,112.456249999561,
3.26591175476071));
#291247=CARTESIAN_POINT('Ctrl Pts',(-8.13178807675727,112.60624999956,5.90808986649102));
#291248=CARTESIAN_POINT('Ctrl Pts',(-6.21213331202029,112.756249999559,
8.55026797822134));
#291249=CARTESIAN_POINT('Ctrl Pts',(-3.10606665601018,112.906249999559,
9.5594902125713));
#291250=CARTESIAN_POINT('Ctrl Pts',(-7.56456262199606E-14,113.056249999558,
10.5687124469213));
#291251=CARTESIAN_POINT('Ctrl Pts',(3.10606665601003,113.206249999558,9.5594902125713));
#291252=CARTESIAN_POINT('Ctrl Pts',(6.21213331202014,113.356249999557,8.55026797822134));
#291253=CARTESIAN_POINT('Ctrl Pts',(8.13178807675711,113.506249999556,5.90808986649102));
#291254=CARTESIAN_POINT('Ctrl Pts',(10.0514428414941,113.656249999556,3.2659117547607));
#291255=CARTESIAN_POINT('Ctrl Pts',(10.0514428414941,113.806249999555,-1.23094673026484E-15));
#291256=CARTESIAN_POINT('Ctrl Pts',(10.0514428414941,110.431249999569,-1.23094673026484E-15));
#291257=CARTESIAN_POINT('Ctrl Pts',(10.0514428414941,110.581249999568,-3.26591175476071));
#291258=CARTESIAN_POINT('Ctrl Pts',(8.13178807675711,110.731249999568,-5.90808986649102));
#291259=CARTESIAN_POINT('Ctrl Pts',(6.21213331202014,110.881249999567,-8.55026797822134));
#291260=CARTESIAN_POINT('Ctrl Pts',(3.10606665601003,111.031249999566,-9.5594902125713));
#291261=CARTESIAN_POINT('Ctrl Pts',(-7.71543958990181E-14,111.181249999566,
-10.5687124469213));
#291262=CARTESIAN_POINT('Ctrl Pts',(-3.10606665601019,111.331249999565,
-9.5594902125713));
#291263=CARTESIAN_POINT('Ctrl Pts',(-6.21213331202029,111.481249999565,
-8.55026797822134));
#291264=CARTESIAN_POINT('Ctrl Pts',(-8.13178807675727,111.631249999564,
-5.90808986649102));
#291265=CARTESIAN_POINT('Ctrl Pts',(-10.0514428414942,111.781249999563,
-3.2659117547607));
#291266=CARTESIAN_POINT('Ctrl Pts',(-10.0514428414942,111.931249999563,
2.46189346052968E-15));
#291267=CARTESIAN_POINT('Ctrl Pts',(-10.0514428414942,112.081249999562,
3.26591175476071));
#291268=CARTESIAN_POINT('Ctrl Pts',(-8.13178807675727,112.231249999562,
5.90808986649102));
#291269=CARTESIAN_POINT('Ctrl Pts',(-6.21213331202029,112.381249999561,
8.55026797822134));
#291270=CARTESIAN_POINT('Ctrl Pts',(-3.10606665601018,112.53124999956,9.5594902125713));
#291271=CARTESIAN_POINT('Ctrl Pts',(-7.54296625610028E-14,112.68124999956,
10.5687124469213));
#291272=CARTESIAN_POINT('Ctrl Pts',(3.10606665601003,112.831249999559,9.5594902125713));
#291273=CARTESIAN_POINT('Ctrl Pts',(6.21213331202014,112.981249999559,8.55026797822134));
#291274=CARTESIAN_POINT('Ctrl Pts',(8.13178807675711,113.131249999558,5.90808986649102));
#291275=CARTESIAN_POINT('Ctrl Pts',(10.0514428414941,113.281249999557,3.2659117547607));
#291276=CARTESIAN_POINT('Ctrl Pts',(10.0514428414941,113.431249999557,-1.23094673026484E-15));
#291277=CARTESIAN_POINT('Origin',(-3.77475828372553E-14,-1.881249999982,
2.68644078414671E-15));
#291278=CARTESIAN_POINT('',(10.0514428414941,116.806249999543,9.62793180209394E-16));
#291279=CARTESIAN_POINT('',(10.0514428414941,116.431249999545,9.64349897029844E-16));
#291280=CARTESIAN_POINT('',(10.0514428414941,-1.881249999982,4.14193483802857E-15));
#291281=CARTESIAN_POINT('Ctrl Pts',(10.0514428414941,113.806249999555,-1.23094673026484E-15));
#291282=CARTESIAN_POINT('Ctrl Pts',(10.0514428414941,113.956249999555,-3.26591175476071));
#291283=CARTESIAN_POINT('Ctrl Pts',(8.13178807675711,114.106249999554,-5.90808986649102));
#291284=CARTESIAN_POINT('Ctrl Pts',(6.21213331202014,114.256249999553,-8.55026797822134));
#291285=CARTESIAN_POINT('Ctrl Pts',(3.10606665601003,114.406249999553,-9.5594902125713));
#291286=CARTESIAN_POINT('Ctrl Pts',(-7.90980688296377E-14,114.556249999552,
-10.5687124469213));
#291287=CARTESIAN_POINT('Ctrl Pts',(-3.10606665601019,114.706249999552,
-9.5594902125713));
#291288=CARTESIAN_POINT('Ctrl Pts',(-6.21213331202029,114.856249999551,
-8.55026797822134));
#291289=CARTESIAN_POINT('Ctrl Pts',(-8.13178807675727,115.00624999955,-5.90808986649102));
#291290=CARTESIAN_POINT('Ctrl Pts',(-10.0514428414942,115.15624999955,-3.2659117547607));
#291291=CARTESIAN_POINT('Ctrl Pts',(-10.0514428414942,115.306249999549,
2.46189346052968E-15));
#291292=CARTESIAN_POINT('Ctrl Pts',(-10.0514428414942,115.456249999549,
3.26591175476071));
#291293=CARTESIAN_POINT('Ctrl Pts',(-8.13178807675727,115.606249999548,
5.90808986649102));
#291294=CARTESIAN_POINT('Ctrl Pts',(-6.21213331202029,115.756249999547,
8.55026797822134));
#291295=CARTESIAN_POINT('Ctrl Pts',(-3.10606665601019,115.906249999547,
9.5594902125713));
#291296=CARTESIAN_POINT('Ctrl Pts',(-7.73733354916224E-14,116.056249999546,
10.5687124469213));
#291297=CARTESIAN_POINT('Ctrl Pts',(3.10606665601003,116.206249999546,9.5594902125713));
#291298=CARTESIAN_POINT('Ctrl Pts',(6.21213331202014,116.356249999545,8.55026797822134));
#291299=CARTESIAN_POINT('Ctrl Pts',(8.13178807675711,116.506249999544,5.90808986649102));
#291300=CARTESIAN_POINT('Ctrl Pts',(10.0514428414941,116.656249999544,3.2659117547607));
#291301=CARTESIAN_POINT('Ctrl Pts',(10.0514428414941,116.806249999543,-1.23094673026484E-15));
#291302=CARTESIAN_POINT('Ctrl Pts',(10.0514428414941,113.431249999557,-1.23094673026484E-15));
#291303=CARTESIAN_POINT('Ctrl Pts',(10.0514428414941,113.581249999556,-3.26591175476071));
#291304=CARTESIAN_POINT('Ctrl Pts',(8.13178807675711,113.731249999556,-5.90808986649102));
#291305=CARTESIAN_POINT('Ctrl Pts',(6.21213331202014,113.881249999555,-8.55026797822134));
#291306=CARTESIAN_POINT('Ctrl Pts',(3.10606665601003,114.031249999554,-9.5594902125713));
#291307=CARTESIAN_POINT('Ctrl Pts',(-7.88821051706799E-14,114.181249999554,
-10.5687124469213));
#291308=CARTESIAN_POINT('Ctrl Pts',(-3.10606665601019,114.331249999553,
-9.5594902125713));
#291309=CARTESIAN_POINT('Ctrl Pts',(-6.21213331202029,114.481249999553,
-8.55026797822134));
#291310=CARTESIAN_POINT('Ctrl Pts',(-8.13178807675727,114.631249999552,
-5.90808986649102));
#291311=CARTESIAN_POINT('Ctrl Pts',(-10.0514428414942,114.781249999551,
-3.2659117547607));
#291312=CARTESIAN_POINT('Ctrl Pts',(-10.0514428414942,114.931249999551,
2.46189346052968E-15));
#291313=CARTESIAN_POINT('Ctrl Pts',(-10.0514428414942,115.08124999955,3.26591175476071));
#291314=CARTESIAN_POINT('Ctrl Pts',(-8.13178807675727,115.23124999955,5.90808986649102));
#291315=CARTESIAN_POINT('Ctrl Pts',(-6.21213331202029,115.381249999549,
8.55026797822134));
#291316=CARTESIAN_POINT('Ctrl Pts',(-3.10606665601018,115.531249999548,
9.5594902125713));
#291317=CARTESIAN_POINT('Ctrl Pts',(-7.71573718326647E-14,115.681249999548,
10.5687124469213));
#291318=CARTESIAN_POINT('Ctrl Pts',(3.10606665601003,115.831249999547,9.5594902125713));
#291319=CARTESIAN_POINT('Ctrl Pts',(6.21213331202014,115.981249999547,8.55026797822134));
#291320=CARTESIAN_POINT('Ctrl Pts',(8.13178807675711,116.131249999546,5.90808986649102));
#291321=CARTESIAN_POINT('Ctrl Pts',(10.0514428414941,116.281249999545,3.2659117547607));
#291322=CARTESIAN_POINT('Ctrl Pts',(10.0514428414941,116.431249999545,-1.23094673026484E-15));
#291323=CARTESIAN_POINT('Origin',(-3.77475828372553E-14,-1.881249999982,
2.68644078414671E-15));
#291324=CARTESIAN_POINT('',(10.0514428414941,119.806249999531,9.50339445645792E-16));
#291325=CARTESIAN_POINT('',(10.0514428414941,119.431249999533,9.51896162466242E-16));
#291326=CARTESIAN_POINT('',(10.0514428414941,-1.881249999982,4.14193483802857E-15));
#291327=CARTESIAN_POINT('Ctrl Pts',(10.0514428414941,116.806249999543,-1.23094673026484E-15));
#291328=CARTESIAN_POINT('Ctrl Pts',(10.0514428414941,116.956249999543,-3.26591175476071));
#291329=CARTESIAN_POINT('Ctrl Pts',(8.13178807675711,117.106249999542,-5.90808986649102));
#291330=CARTESIAN_POINT('Ctrl Pts',(6.21213331202014,117.256249999541,-8.55026797822134));
#291331=CARTESIAN_POINT('Ctrl Pts',(3.10606665601003,117.406249999541,-9.5594902125713));
#291332=CARTESIAN_POINT('Ctrl Pts',(-8.08257781012995E-14,117.55624999954,
-10.5687124469213));
#291333=CARTESIAN_POINT('Ctrl Pts',(-3.10606665601019,117.70624999954,-9.5594902125713));
#291334=CARTESIAN_POINT('Ctrl Pts',(-6.2121333120203,117.856249999539,-8.55026797822134));
#291335=CARTESIAN_POINT('Ctrl Pts',(-8.13178807675727,118.006249999538,
-5.90808986649102));
#291336=CARTESIAN_POINT('Ctrl Pts',(-10.0514428414942,118.156249999538,
-3.2659117547607));
#291337=CARTESIAN_POINT('Ctrl Pts',(-10.0514428414942,118.306249999537,
2.46189346052968E-15));
#291338=CARTESIAN_POINT('Ctrl Pts',(-10.0514428414942,118.456249999537,
3.26591175476071));
#291339=CARTESIAN_POINT('Ctrl Pts',(-8.13178807675727,118.606249999536,
5.90808986649102));
#291340=CARTESIAN_POINT('Ctrl Pts',(-6.21213331202029,118.756249999535,
8.55026797822134));
#291341=CARTESIAN_POINT('Ctrl Pts',(-3.10606665601019,118.906249999535,
9.5594902125713));
#291342=CARTESIAN_POINT('Ctrl Pts',(-7.91010447632842E-14,119.056249999534,
10.5687124469213));
#291343=CARTESIAN_POINT('Ctrl Pts',(3.10606665601003,119.206249999534,9.5594902125713));
#291344=CARTESIAN_POINT('Ctrl Pts',(6.21213331202014,119.356249999533,8.55026797822134));
#291345=CARTESIAN_POINT('Ctrl Pts',(8.13178807675711,119.506249999532,5.90808986649102));
#291346=CARTESIAN_POINT('Ctrl Pts',(10.0514428414941,119.656249999532,3.2659117547607));
#291347=CARTESIAN_POINT('Ctrl Pts',(10.0514428414941,119.806249999531,-1.23094673026484E-15));
#291348=CARTESIAN_POINT('Ctrl Pts',(10.0514428414941,116.431249999545,-1.23094673026484E-15));
#291349=CARTESIAN_POINT('Ctrl Pts',(10.0514428414941,116.581249999544,-3.26591175476071));
#291350=CARTESIAN_POINT('Ctrl Pts',(8.13178807675711,116.731249999544,-5.90808986649102));
#291351=CARTESIAN_POINT('Ctrl Pts',(6.21213331202014,116.881249999543,-8.55026797822134));
#291352=CARTESIAN_POINT('Ctrl Pts',(3.10606665601003,117.031249999542,-9.5594902125713));
#291353=CARTESIAN_POINT('Ctrl Pts',(-8.06098144423418E-14,117.181249999542,
-10.5687124469213));
#291354=CARTESIAN_POINT('Ctrl Pts',(-3.10606665601019,117.331249999541,
-9.5594902125713));
#291355=CARTESIAN_POINT('Ctrl Pts',(-6.2121333120203,117.481249999541,-8.55026797822134));
#291356=CARTESIAN_POINT('Ctrl Pts',(-8.13178807675727,117.63124999954,-5.90808986649102));
#291357=CARTESIAN_POINT('Ctrl Pts',(-10.0514428414942,117.781249999539,
-3.2659117547607));
#291358=CARTESIAN_POINT('Ctrl Pts',(-10.0514428414942,117.931249999539,
2.46189346052968E-15));
#291359=CARTESIAN_POINT('Ctrl Pts',(-10.0514428414942,118.081249999538,
3.26591175476071));
#291360=CARTESIAN_POINT('Ctrl Pts',(-8.13178807675727,118.231249999538,
5.90808986649102));
#291361=CARTESIAN_POINT('Ctrl Pts',(-6.21213331202029,118.381249999537,
8.55026797822134));
#291362=CARTESIAN_POINT('Ctrl Pts',(-3.10606665601019,118.531249999536,
9.5594902125713));
#291363=CARTESIAN_POINT('Ctrl Pts',(-7.88850811043265E-14,118.681249999536,
10.5687124469213));
#291364=CARTESIAN_POINT('Ctrl Pts',(3.10606665601003,118.831249999535,9.5594902125713));
#291365=CARTESIAN_POINT('Ctrl Pts',(6.21213331202014,118.981249999535,8.55026797822134));
#291366=CARTESIAN_POINT('Ctrl Pts',(8.13178807675711,119.131249999534,5.90808986649102));
#291367=CARTESIAN_POINT('Ctrl Pts',(10.0514428414941,119.281249999533,3.2659117547607));
#291368=CARTESIAN_POINT('Ctrl Pts',(10.0514428414941,119.431249999533,-1.23094673026484E-15));
#291369=CARTESIAN_POINT('Origin',(-3.77475828372553E-14,-1.881249999982,
2.68644078414671E-15));
#291370=CARTESIAN_POINT('',(10.0514428414941,122.806249999519,9.37885711082191E-16));
#291371=CARTESIAN_POINT('',(10.0514428414941,122.431249999521,9.39442427902641E-16));
#291372=CARTESIAN_POINT('',(10.0514428414941,-1.881249999982,4.14193483802857E-15));
#291373=CARTESIAN_POINT('Ctrl Pts',(10.0514428414941,119.806249999531,-1.23094673026484E-15));
#291374=CARTESIAN_POINT('Ctrl Pts',(10.0514428414941,119.956249999531,-3.26591175476071));
#291375=CARTESIAN_POINT('Ctrl Pts',(8.13178807675711,120.10624999953,-5.90808986649102));
#291376=CARTESIAN_POINT('Ctrl Pts',(6.21213331202013,120.256249999529,-8.55026797822134));
#291377=CARTESIAN_POINT('Ctrl Pts',(3.10606665601003,120.406249999529,-9.5594902125713));
#291378=CARTESIAN_POINT('Ctrl Pts',(-8.25534873729613E-14,120.556249999528,
-10.5687124469213));
#291379=CARTESIAN_POINT('Ctrl Pts',(-3.10606665601019,120.706249999528,
-9.5594902125713));
#291380=CARTESIAN_POINT('Ctrl Pts',(-6.2121333120203,120.856249999527,-8.55026797822134));
#291381=CARTESIAN_POINT('Ctrl Pts',(-8.13178807675727,121.006249999526,
-5.90808986649102));
#291382=CARTESIAN_POINT('Ctrl Pts',(-10.0514428414943,121.156249999526,
-3.2659117547607));
#291383=CARTESIAN_POINT('Ctrl Pts',(-10.0514428414943,121.306249999525,
2.46189346052968E-15));
#291384=CARTESIAN_POINT('Ctrl Pts',(-10.0514428414943,121.456249999525,
3.26591175476071));
#291385=CARTESIAN_POINT('Ctrl Pts',(-8.13178807675727,121.606249999524,
5.90808986649102));
#291386=CARTESIAN_POINT('Ctrl Pts',(-6.2121333120203,121.756249999523,8.55026797822134));
#291387=CARTESIAN_POINT('Ctrl Pts',(-3.10606665601019,121.906249999523,
9.5594902125713));
#291388=CARTESIAN_POINT('Ctrl Pts',(-8.08287540349461E-14,122.056249999522,
10.5687124469213));
#291389=CARTESIAN_POINT('Ctrl Pts',(3.10606665601003,122.206249999522,9.5594902125713));
#291390=CARTESIAN_POINT('Ctrl Pts',(6.21213331202014,122.356249999521,8.55026797822134));
#291391=CARTESIAN_POINT('Ctrl Pts',(8.13178807675711,122.50624999952,5.90808986649102));
#291392=CARTESIAN_POINT('Ctrl Pts',(10.0514428414941,122.65624999952,3.2659117547607));
#291393=CARTESIAN_POINT('Ctrl Pts',(10.0514428414941,122.806249999519,-1.23094673026484E-15));
#291394=CARTESIAN_POINT('Ctrl Pts',(10.0514428414941,119.431249999533,-1.23094673026484E-15));
#291395=CARTESIAN_POINT('Ctrl Pts',(10.0514428414941,119.581249999532,-3.26591175476071));
#291396=CARTESIAN_POINT('Ctrl Pts',(8.13178807675711,119.731249999532,-5.90808986649102));
#291397=CARTESIAN_POINT('Ctrl Pts',(6.21213331202013,119.881249999531,-8.55026797822134));
#291398=CARTESIAN_POINT('Ctrl Pts',(3.10606665601003,120.03124999953,-9.5594902125713));
#291399=CARTESIAN_POINT('Ctrl Pts',(-8.23375237140036E-14,120.18124999953,
-10.5687124469213));
#291400=CARTESIAN_POINT('Ctrl Pts',(-3.10606665601019,120.331249999529,
-9.5594902125713));
#291401=CARTESIAN_POINT('Ctrl Pts',(-6.2121333120203,120.481249999529,-8.55026797822134));
#291402=CARTESIAN_POINT('Ctrl Pts',(-8.13178807675727,120.631249999528,
-5.90808986649102));
#291403=CARTESIAN_POINT('Ctrl Pts',(-10.0514428414943,120.781249999527,
-3.2659117547607));
#291404=CARTESIAN_POINT('Ctrl Pts',(-10.0514428414943,120.931249999527,
2.46189346052968E-15));
#291405=CARTESIAN_POINT('Ctrl Pts',(-10.0514428414943,121.081249999526,
3.26591175476071));
#291406=CARTESIAN_POINT('Ctrl Pts',(-8.13178807675727,121.231249999526,
5.90808986649102));
#291407=CARTESIAN_POINT('Ctrl Pts',(-6.2121333120203,121.381249999525,8.55026797822134));
#291408=CARTESIAN_POINT('Ctrl Pts',(-3.10606665601019,121.531249999524,
9.5594902125713));
#291409=CARTESIAN_POINT('Ctrl Pts',(-8.06127903759884E-14,121.681249999524,
10.5687124469213));
#291410=CARTESIAN_POINT('Ctrl Pts',(3.10606665601003,121.831249999523,9.5594902125713));
#291411=CARTESIAN_POINT('Ctrl Pts',(6.21213331202014,121.981249999523,8.55026797822134));
#291412=CARTESIAN_POINT('Ctrl Pts',(8.13178807675711,122.131249999522,5.90808986649102));
#291413=CARTESIAN_POINT('Ctrl Pts',(10.0514428414941,122.281249999521,3.2659117547607));
#291414=CARTESIAN_POINT('Ctrl Pts',(10.0514428414941,122.431249999521,-1.23094673026484E-15));
#291415=CARTESIAN_POINT('Origin',(-3.77475828372553E-14,-1.881249999982,
2.68644078414671E-15));
#291416=CARTESIAN_POINT('',(10.0514428414941,125.806249999507,9.2543197651859E-16));
#291417=CARTESIAN_POINT('',(10.0514428414941,125.431249999509,9.2698869333904E-16));
#291418=CARTESIAN_POINT('',(10.0514428414941,-1.881249999982,4.14193483802857E-15));
#291419=CARTESIAN_POINT('Ctrl Pts',(10.0514428414941,122.806249999519,-1.23094673026484E-15));
#291420=CARTESIAN_POINT('Ctrl Pts',(10.0514428414941,122.956249999519,-3.26591175476071));
#291421=CARTESIAN_POINT('Ctrl Pts',(8.13178807675711,123.106249999518,-5.90808986649102));
#291422=CARTESIAN_POINT('Ctrl Pts',(6.21213331202013,123.256249999517,-8.55026797822134));
#291423=CARTESIAN_POINT('Ctrl Pts',(3.10606665601002,123.406249999517,-9.5594902125713));
#291424=CARTESIAN_POINT('Ctrl Pts',(-8.42811966446232E-14,123.556249999516,
-10.5687124469213));
#291425=CARTESIAN_POINT('Ctrl Pts',(-3.10606665601019,123.706249999516,
-9.5594902125713));
#291426=CARTESIAN_POINT('Ctrl Pts',(-6.2121333120203,123.856249999515,-8.55026797822134));
#291427=CARTESIAN_POINT('Ctrl Pts',(-8.13178807675727,124.006249999514,
-5.90808986649102));
#291428=CARTESIAN_POINT('Ctrl Pts',(-10.0514428414943,124.156249999514,
-3.2659117547607));
#291429=CARTESIAN_POINT('Ctrl Pts',(-10.0514428414943,124.306249999513,
2.46189346052968E-15));
#291430=CARTESIAN_POINT('Ctrl Pts',(-10.0514428414943,124.456249999513,
3.26591175476071));
#291431=CARTESIAN_POINT('Ctrl Pts',(-8.13178807675727,124.606249999512,
5.90808986649102));
#291432=CARTESIAN_POINT('Ctrl Pts',(-6.2121333120203,124.756249999511,8.55026797822134));
#291433=CARTESIAN_POINT('Ctrl Pts',(-3.10606665601019,124.906249999511,
9.5594902125713));
#291434=CARTESIAN_POINT('Ctrl Pts',(-8.25564633066079E-14,125.05624999951,
10.5687124469213));
#291435=CARTESIAN_POINT('Ctrl Pts',(3.10606665601002,125.20624999951,9.5594902125713));
#291436=CARTESIAN_POINT('Ctrl Pts',(6.21213331202013,125.356249999509,8.55026797822134));
#291437=CARTESIAN_POINT('Ctrl Pts',(8.13178807675711,125.506249999508,5.90808986649102));
#291438=CARTESIAN_POINT('Ctrl Pts',(10.0514428414941,125.656249999508,3.2659117547607));
#291439=CARTESIAN_POINT('Ctrl Pts',(10.0514428414941,125.806249999507,-1.23094673026484E-15));
#291440=CARTESIAN_POINT('Ctrl Pts',(10.0514428414941,122.431249999521,-1.23094673026484E-15));
#291441=CARTESIAN_POINT('Ctrl Pts',(10.0514428414941,122.58124999952,-3.26591175476071));
#291442=CARTESIAN_POINT('Ctrl Pts',(8.13178807675711,122.73124999952,-5.90808986649102));
#291443=CARTESIAN_POINT('Ctrl Pts',(6.21213331202013,122.881249999519,-8.55026797822134));
#291444=CARTESIAN_POINT('Ctrl Pts',(3.10606665601002,123.031249999518,-9.5594902125713));
#291445=CARTESIAN_POINT('Ctrl Pts',(-8.40652329856655E-14,123.181249999518,
-10.5687124469213));
#291446=CARTESIAN_POINT('Ctrl Pts',(-3.10606665601019,123.331249999517,
-9.5594902125713));
#291447=CARTESIAN_POINT('Ctrl Pts',(-6.2121333120203,123.481249999517,-8.55026797822134));
#291448=CARTESIAN_POINT('Ctrl Pts',(-8.13178807675727,123.631249999516,
-5.90808986649102));
#291449=CARTESIAN_POINT('Ctrl Pts',(-10.0514428414943,123.781249999515,
-3.2659117547607));
#291450=CARTESIAN_POINT('Ctrl Pts',(-10.0514428414943,123.931249999515,
2.46189346052968E-15));
#291451=CARTESIAN_POINT('Ctrl Pts',(-10.0514428414943,124.081249999514,
3.26591175476071));
#291452=CARTESIAN_POINT('Ctrl Pts',(-8.13178807675727,124.231249999514,
5.90808986649102));
#291453=CARTESIAN_POINT('Ctrl Pts',(-6.2121333120203,124.381249999513,8.55026797822134));
#291454=CARTESIAN_POINT('Ctrl Pts',(-3.10606665601019,124.531249999512,
9.5594902125713));
#291455=CARTESIAN_POINT('Ctrl Pts',(-8.23404996476502E-14,124.681249999512,
10.5687124469213));
#291456=CARTESIAN_POINT('Ctrl Pts',(3.10606665601002,124.831249999511,9.5594902125713));
#291457=CARTESIAN_POINT('Ctrl Pts',(6.21213331202013,124.981249999511,8.55026797822134));
#291458=CARTESIAN_POINT('Ctrl Pts',(8.13178807675711,125.13124999951,5.90808986649102));
#291459=CARTESIAN_POINT('Ctrl Pts',(10.0514428414941,125.281249999509,3.2659117547607));
#291460=CARTESIAN_POINT('Ctrl Pts',(10.0514428414941,125.431249999509,-1.23094673026484E-15));
#291461=CARTESIAN_POINT('Origin',(-3.77475828372553E-14,-1.881249999982,
2.68644078414671E-15));
#291462=CARTESIAN_POINT('',(10.0514428414941,128.806249999495,9.12978241954989E-16));
#291463=CARTESIAN_POINT('',(10.0514428414941,128.431249999497,9.14534958775439E-16));
#291464=CARTESIAN_POINT('',(10.0514428414941,-1.881249999982,4.14193483802857E-15));
#291465=CARTESIAN_POINT('Ctrl Pts',(10.0514428414941,125.806249999507,-1.23094673026484E-15));
#291466=CARTESIAN_POINT('Ctrl Pts',(10.0514428414941,125.956249999507,-3.26591175476071));
#291467=CARTESIAN_POINT('Ctrl Pts',(8.13178807675711,126.106249999506,-5.90808986649102));
#291468=CARTESIAN_POINT('Ctrl Pts',(6.21213331202013,126.256249999505,-8.55026797822134));
#291469=CARTESIAN_POINT('Ctrl Pts',(3.10606665601002,126.406249999505,-9.5594902125713));
#291470=CARTESIAN_POINT('Ctrl Pts',(-8.6008905916285E-14,126.556249999504,
-10.5687124469213));
#291471=CARTESIAN_POINT('Ctrl Pts',(-3.10606665601019,126.706249999504,
-9.5594902125713));
#291472=CARTESIAN_POINT('Ctrl Pts',(-6.2121333120203,126.856249999503,-8.55026797822134));
#291473=CARTESIAN_POINT('Ctrl Pts',(-8.13178807675728,127.006249999502,
-5.90808986649102));
#291474=CARTESIAN_POINT('Ctrl Pts',(-10.0514428414943,127.156249999502,
-3.2659117547607));
#291475=CARTESIAN_POINT('Ctrl Pts',(-10.0514428414943,127.306249999501,
2.46189346052968E-15));
#291476=CARTESIAN_POINT('Ctrl Pts',(-10.0514428414943,127.456249999501,
3.26591175476071));
#291477=CARTESIAN_POINT('Ctrl Pts',(-8.13178807675728,127.6062499995,5.90808986649102));
#291478=CARTESIAN_POINT('Ctrl Pts',(-6.2121333120203,127.756249999499,8.55026797822134));
#291479=CARTESIAN_POINT('Ctrl Pts',(-3.10606665601019,127.906249999499,
9.5594902125713));
#291480=CARTESIAN_POINT('Ctrl Pts',(-8.42841725782698E-14,128.056249999498,
10.5687124469213));
#291481=CARTESIAN_POINT('Ctrl Pts',(3.10606665601002,128.206249999498,9.5594902125713));
#291482=CARTESIAN_POINT('Ctrl Pts',(6.21213331202013,128.356249999497,8.55026797822134));
#291483=CARTESIAN_POINT('Ctrl Pts',(8.1317880767571,128.506249999496,5.90808986649102));
#291484=CARTESIAN_POINT('Ctrl Pts',(10.0514428414941,128.656249999496,3.2659117547607));
#291485=CARTESIAN_POINT('Ctrl Pts',(10.0514428414941,128.806249999495,-1.23094673026484E-15));
#291486=CARTESIAN_POINT('Ctrl Pts',(10.0514428414941,125.431249999509,-1.23094673026484E-15));
#291487=CARTESIAN_POINT('Ctrl Pts',(10.0514428414941,125.581249999508,-3.26591175476071));
#291488=CARTESIAN_POINT('Ctrl Pts',(8.13178807675711,125.731249999508,-5.90808986649102));
#291489=CARTESIAN_POINT('Ctrl Pts',(6.21213331202013,125.881249999507,-8.55026797822134));
#291490=CARTESIAN_POINT('Ctrl Pts',(3.10606665601002,126.031249999506,-9.5594902125713));
#291491=CARTESIAN_POINT('Ctrl Pts',(-8.57929422573273E-14,126.181249999506,
-10.5687124469213));
#291492=CARTESIAN_POINT('Ctrl Pts',(-3.10606665601019,126.331249999505,
-9.5594902125713));
#291493=CARTESIAN_POINT('Ctrl Pts',(-6.2121333120203,126.481249999505,-8.55026797822134));
#291494=CARTESIAN_POINT('Ctrl Pts',(-8.13178807675728,126.631249999504,
-5.90808986649102));
#291495=CARTESIAN_POINT('Ctrl Pts',(-10.0514428414943,126.781249999503,
-3.2659117547607));
#291496=CARTESIAN_POINT('Ctrl Pts',(-10.0514428414943,126.931249999503,
2.46189346052968E-15));
#291497=CARTESIAN_POINT('Ctrl Pts',(-10.0514428414943,127.081249999502,
3.26591175476071));
#291498=CARTESIAN_POINT('Ctrl Pts',(-8.13178807675728,127.231249999502,
5.90808986649102));
#291499=CARTESIAN_POINT('Ctrl Pts',(-6.2121333120203,127.381249999501,8.55026797822134));
#291500=CARTESIAN_POINT('Ctrl Pts',(-3.10606665601019,127.5312499995,9.5594902125713));
#291501=CARTESIAN_POINT('Ctrl Pts',(-8.4068208919312E-14,127.6812499995,
10.5687124469213));
#291502=CARTESIAN_POINT('Ctrl Pts',(3.10606665601002,127.831249999499,9.5594902125713));
#291503=CARTESIAN_POINT('Ctrl Pts',(6.21213331202013,127.981249999499,8.55026797822134));
#291504=CARTESIAN_POINT('Ctrl Pts',(8.1317880767571,128.131249999498,5.90808986649102));
#291505=CARTESIAN_POINT('Ctrl Pts',(10.0514428414941,128.281249999497,3.2659117547607));
#291506=CARTESIAN_POINT('Ctrl Pts',(10.0514428414941,128.431249999497,-1.23094673026484E-15));
#291507=CARTESIAN_POINT('Origin',(-8.79029313101884E-14,130.96875,0.));
#291508=CARTESIAN_POINT('',(-12.0000000000001,128.431249999496,-7.19625340030961E-14));
#291509=CARTESIAN_POINT('',(-12.0000000000001,128.806249999496,-1.6694244058475E-14));
#291510=CARTESIAN_POINT('',(-12.0000000000001,130.96875,-1.46957615897682E-15));
#291511=CARTESIAN_POINT('',(-7.3010839424065,128.868749999999,9.52334884722529));
#291512=CARTESIAN_POINT('Ctrl Pts',(-12.0000000000001,128.431249999496,
-3.80251385934116E-14));
#291513=CARTESIAN_POINT('Ctrl Pts',(-12.0000000000001,128.481970002,1.31839422452174));
#291514=CARTESIAN_POINT('Ctrl Pts',(-11.7827260639574,128.53512719973,2.62954328634065));
#291515=CARTESIAN_POINT('Ctrl Pts',(-10.9745647540102,128.636212850368,
4.99453327094218));
#291516=CARTESIAN_POINT('Ctrl Pts',(-10.4318751626277,128.683474543101,
6.04670312147143));
#291517=CARTESIAN_POINT('Ctrl Pts',(-9.05815403570474,128.774185332047,
7.95825182936078));
#291518=CARTESIAN_POINT('Ctrl Pts',(-8.23482414938436,128.821172544027,
8.8074960793686));
#291519=CARTESIAN_POINT('Ctrl Pts',(-7.30108394240603,128.868749999998,
9.52334884722502));
#291520=CARTESIAN_POINT('',(-11.8941677855641,128.86875,1.59021152330489));
#291521=CARTESIAN_POINT('Origin',(-8.66935348200203E-14,128.86875,0.));
#291522=CARTESIAN_POINT('Ctrl Pts',(-11.8941677855641,128.86875,1.59021152330492));
#291523=CARTESIAN_POINT('Ctrl Pts',(-11.9646919997276,128.84757520719,1.06271764974586));
#291524=CARTESIAN_POINT('Ctrl Pts',(-12.0000000000001,128.826697189287,
0.531495575654397));
#291525=CARTESIAN_POINT('Ctrl Pts',(-12.0000000000001,128.806249999496,
3.24740234702858E-14));
#291526=CARTESIAN_POINT('Origin',(-8.79029313101884E-14,130.96875,0.));
#291527=CARTESIAN_POINT('',(-12.0000000000001,125.431249999508,-2.53890049450429E-15));
#291528=CARTESIAN_POINT('',(-12.0000000000001,125.806249999508,7.85073803031321E-14));
#291529=CARTESIAN_POINT('',(-12.0000000000001,130.96875,-1.46957615897682E-15));
#291530=CARTESIAN_POINT('Ctrl Pts',(-12.0000000000001,125.431249999508,
-1.0547118733939E-14));
#291531=CARTESIAN_POINT('Ctrl Pts',(-12.0000000000001,125.489596886951,
1.51664423554858));
#291532=CARTESIAN_POINT('Ctrl Pts',(-11.7124672914376,125.55104013437,3.02034889816076));
#291533=CARTESIAN_POINT('Ctrl Pts',(-10.5808995167431,125.674745188536,
5.86821693033722));
#291534=CARTESIAN_POINT('Ctrl Pts',(-9.73743272163847,125.733338542766,
7.1814939780729));
#291535=CARTESIAN_POINT('Ctrl Pts',(-7.58142249067642,125.857439407559,
9.43349532883263));
#291536=CARTESIAN_POINT('Ctrl Pts',(-6.28242507135789,125.921600081592,
10.3440797672615));
#291537=CARTESIAN_POINT('Ctrl Pts',(-3.41418066711554,126.045560539419,
11.6098695739462));
#291538=CARTESIAN_POINT('Ctrl Pts',(-1.87371932800542,126.105456460553,
11.9555370942489));
#291539=CARTESIAN_POINT('Ctrl Pts',(1.23871898742655,126.231357235109,12.0360651439063));
#291540=CARTESIAN_POINT('Ctrl Pts',(2.7809719944347,126.292274471604,11.7757047301857));
#291541=CARTESIAN_POINT('Ctrl Pts',(5.71429353463594,126.414546669267,10.6704915883421));
#291542=CARTESIAN_POINT('Ctrl Pts',(7.07223692666379,126.47913085024,9.82322725908423));
#291543=CARTESIAN_POINT('Ctrl Pts',(9.35495050356998,126.604937420233,7.67387871961371));
#291544=CARTESIAN_POINT('Ctrl Pts',(10.2670744395895,126.663281529632,6.40239705975796));
#291545=CARTESIAN_POINT('Ctrl Pts',(11.561755155871,126.788326898164,3.57268807209495));
#291546=CARTESIAN_POINT('Ctrl Pts',(11.9280794377078,126.851890498091,2.03946880008667));
#291547=CARTESIAN_POINT('Ctrl Pts',(12.053496278001,126.974201142343,-1.0990717883848));
#291548=CARTESIAN_POINT('Ctrl Pts',(11.8043524772866,127.036581899792,-2.67438299002925));
#291549=CARTESIAN_POINT('Ctrl Pts',(10.7217182551911,127.162926241768,-5.60675502470455));
#291550=CARTESIAN_POINT('Ctrl Pts',(9.9108203693828,127.22192765558,-6.94021692903948));
#291551=CARTESIAN_POINT('Ctrl Pts',(7.80834131296282,127.345583714989,-9.24718977833398));
#291552=CARTESIAN_POINT('Ctrl Pts',(6.52853819589473,127.409909036468,-10.191117730139));
#291553=CARTESIAN_POINT('Ctrl Pts',(3.69184433991172,127.534430944573,-11.52394689137));
#291554=CARTESIAN_POINT('Ctrl Pts',(2.16489556008747,127.593678134542,-11.9056393604222));
#291555=CARTESIAN_POINT('Ctrl Pts',(-0.942572912478038,127.719377874731,
-12.0632149041181));
#291556=CARTESIAN_POINT('Ctrl Pts',(-2.49342240453255,127.781329203651,
-11.8402681046257));
#291557=CARTESIAN_POINT('Ctrl Pts',(-5.45863081898636,127.903003901638,
-10.8040734135506));
#291558=CARTESIAN_POINT('Ctrl Pts',(-6.83961692526329,127.967619763625,
-9.98719220398577));
#291559=CARTESIAN_POINT('Ctrl Pts',(-9.17288875238684,128.093835926364,
-7.89020427402746));
#291560=CARTESIAN_POINT('Ctrl Pts',(-10.1133256482652,128.152136931153,
-6.64212901323631));
#291561=CARTESIAN_POINT('Ctrl Pts',(-11.4754003004398,128.27686797732,-3.84248800492933));
#291562=CARTESIAN_POINT('Ctrl Pts',(-11.8782216827375,128.340681306605,
-2.31463600074324));
#291563=CARTESIAN_POINT('Ctrl Pts',(-11.9921423568023,128.411850799235,
-0.501701477445237));
#291564=CARTESIAN_POINT('Ctrl Pts',(-12.0000000000001,128.421604405312,
-0.250723482590127));
#291565=CARTESIAN_POINT('Ctrl Pts',(-12.0000000000001,128.431249999496,
1.73472347597681E-15));
#291566=CARTESIAN_POINT('Ctrl Pts',(-12.0000000000001,128.806249999496,
-4.57273108267486E-14));
#291567=CARTESIAN_POINT('Ctrl Pts',(-12.0000000000001,128.794332493682,
-0.309778589508634));
#291568=CARTESIAN_POINT('Ctrl Pts',(-11.9880049278405,128.78226205016,-0.619635141726521));
#291569=CARTESIAN_POINT('Ctrl Pts',(-11.8980136235725,128.736545834021,
-1.778723119345));
#291570=CARTESIAN_POINT('Ctrl Pts',(-11.7416705872724,128.702261315831,
-2.61910140635539));
#291571=CARTESIAN_POINT('Ctrl Pts',(-11.0465766482761,128.604085546726,
-4.94519098084889));
#291572=CARTESIAN_POINT('Ctrl Pts',(-10.3026821784156,128.542403594453,
-6.35108656262286));
#291573=CARTESIAN_POINT('Ctrl Pts',(-8.32158736574728,128.419673735816,
-8.78617588549032));
#291574=CARTESIAN_POINT('Ctrl Pts',(-7.10697201666228,128.355945463055,
-9.79471613563536));
#291575=CARTESIAN_POINT('Ctrl Pts',(-4.37245333378446,128.231097693156,
-11.281882612525));
#291576=CARTESIAN_POINT('Ctrl Pts',(-2.88126249839227,128.172799515821,
-11.751490889311));
#291577=CARTESIAN_POINT('Ctrl Pts',(0.235470080245203,128.04672503467,-12.1022565541906));
#291578=CARTESIAN_POINT('Ctrl Pts',(1.83268362734837,127.982116389507,-11.9650152362571));
#291579=CARTESIAN_POINT('Ctrl Pts',(4.84604017671202,127.860223556581,-11.0870123571411));
#291580=CARTESIAN_POINT('Ctrl Pts',(6.23714114056861,127.798661069928,-10.3684338391067));
#291581=CARTESIAN_POINT('Ctrl Pts',(8.67617998441893,127.672887425654,-8.43563337672419));
#291582=CARTESIAN_POINT('Ctrl Pts',(9.69864245837801,127.613427163644,-7.23687647571405));
#291583=CARTESIAN_POINT('Ctrl Pts',(11.2334836328764,127.489101896387,-4.50391835817245));
#291584=CARTESIAN_POINT('Ctrl Pts',(11.7266830329195,127.424831418766,-2.99354903217779));
#291585=CARTESIAN_POINT('Ctrl Pts',(12.0987618481939,127.301010723956,0.104097835807391));
#291586=CARTESIAN_POINT('Ctrl Pts',(11.9847153130956,127.242175748738,1.66055259173718));
#291587=CARTESIAN_POINT('Ctrl Pts',(11.1628945228536,127.115781636673,4.67896175004949));
#291588=CARTESIAN_POINT('Ctrl Pts',(10.4494920965024,127.052982022215,6.10824039252744));
#291589=CARTESIAN_POINT('Ctrl Pts',(8.52281591676635,126.930912282871,8.59046691788869));
#291590=CARTESIAN_POINT('Ctrl Pts',(7.33486129463653,126.867446574144,9.6246594640949));
#291591=CARTESIAN_POINT('Ctrl Pts',(4.63764878122555,126.742298608303,11.1757992658842));
#291592=CARTESIAN_POINT('Ctrl Pts',(3.15569205951511,126.683900424763,11.6810916275616));
#291593=CARTESIAN_POINT('Ctrl Pts',(0.0494360069800742,126.558249727994,
12.1039500516553));
#291594=CARTESIAN_POINT('Ctrl Pts',(-1.54667912891781,126.493685514498,
12.0048332356448));
#291595=CARTESIAN_POINT('Ctrl Pts',(-4.57443637444229,126.371210161175,
11.2014841669797));
#291596=CARTESIAN_POINT('Ctrl Pts',(-5.98050056719766,126.310620638141,
10.5181997613387));
#291597=CARTESIAN_POINT('Ctrl Pts',(-8.46866339045471,126.184652585968,
8.64483615362303));
#291598=CARTESIAN_POINT('Ctrl Pts',(-9.52315613199515,126.124486320596,
7.46732454508722));
#291599=CARTESIAN_POINT('Ctrl Pts',(-11.1224854645179,126.000734282678,
4.77022018048739));
#291600=CARTESIAN_POINT('Ctrl Pts',(-11.650494800803,125.936640580968,3.27575632643063));
#291601=CARTESIAN_POINT('Ctrl Pts',(-11.9586682352639,125.851029796291,
1.15055753302113));
#291602=CARTESIAN_POINT('Ctrl Pts',(-12.0000000000001,125.828372379491,
0.575039758716343));
#291603=CARTESIAN_POINT('Ctrl Pts',(-12.0000000000001,125.806249999508,
-9.29811783123569E-15));
#291604=CARTESIAN_POINT('Origin',(-8.79029313101884E-14,130.96875,0.));
#291605=CARTESIAN_POINT('',(-12.0000000000001,122.43124999952,-1.91922458638816E-14));
#291606=CARTESIAN_POINT('',(-12.0000000000001,122.80624999952,1.20810221360561E-15));
#291607=CARTESIAN_POINT('',(-12.0000000000001,130.96875,-1.46957615897682E-15));
#291608=CARTESIAN_POINT('Ctrl Pts',(-12.0000000000001,122.43124999952,2.62637134262889E-14));
#291609=CARTESIAN_POINT('Ctrl Pts',(-12.0000000000001,122.435732938321,
0.116527609076827));
#291610=CARTESIAN_POINT('Ctrl Pts',(-11.9983026721942,122.440239705659,
0.233123111782995));
#291611=CARTESIAN_POINT('Ctrl Pts',(-11.9486246694461,122.506405303043,
1.93686221448914));
#291612=CARTESIAN_POINT('Ctrl Pts',(-11.5878069745041,122.571015519303,
3.49907598592701));
#291613=CARTESIAN_POINT('Ctrl Pts',(-10.295123242127,122.697114835668,6.35682970576345));
#291614=CARTESIAN_POINT('Ctrl Pts',(-9.38960619474072,122.755412061665,
7.63113068561021));
#291615=CARTESIAN_POINT('Ctrl Pts',(-7.13326534584562,122.880240022951,
9.77561936761895));
#291616=CARTESIAN_POINT('Ctrl Pts',(-5.79976689993488,122.94398331222,10.621162644329));
#291617=CARTESIAN_POINT('Ctrl Pts',(-2.87341254255409,123.06675240564,11.75686397533));
#291618=CARTESIAN_POINT('Ctrl Pts',(-1.30723980981329,123.128371038424,
12.0321100813843));
#291619=CARTESIAN_POINT('Ctrl Pts',(1.81358360631128,123.254610997428,11.9625647420134));
#291620=CARTESIAN_POINT('Ctrl Pts',(3.33866915744452,123.314001523729,11.6295020408271));
#291621=CARTESIAN_POINT('Ctrl Pts',(6.20683349161236,123.437320363311,10.3905875210183));
#291622=CARTESIAN_POINT('Ctrl Pts',(7.51766930637064,123.501739063548,9.48544504376199));
#291623=CARTESIAN_POINT('Ctrl Pts',(9.69912485336729,123.626629113384,7.23527423550305));
#291624=CARTESIAN_POINT('Ctrl Pts',(10.5547516636117,123.685523610693,5.91771783856675));
#291625=CARTESIAN_POINT('Ctrl Pts',(11.7145004189305,123.811073663117,3.0310482601749));
#291626=CARTESIAN_POINT('Ctrl Pts',(12.0082060367235,123.873839015107,1.48965046616972));
#291627=CARTESIAN_POINT('Ctrl Pts',(11.9912446250076,123.995076604622,-1.65623689768775));
#291628=CARTESIAN_POINT('Ctrl Pts',(11.6661213753513,124.059693561683,-3.23022371496439));
#291629=CARTESIAN_POINT('Ctrl Pts',(10.4381304385326,124.186169495528,-6.11878703324379));
#291630=CARTESIAN_POINT('Ctrl Pts',(9.56305485397843,124.244532792525,-7.41229666342868));
#291631=CARTESIAN_POINT('Ctrl Pts',(7.35564800647638,124.36902414678,-9.60998003718757));
#291632=CARTESIAN_POINT('Ctrl Pts',(6.038725950634,124.432989253204,-10.4876680518474));
#291633=CARTESIAN_POINT('Ctrl Pts',(3.14054067387461,124.556362899663,-11.6875673834738));
#291634=CARTESIAN_POINT('Ctrl Pts',(1.58696921632692,124.617055746233,-11.9976591489136));
#291635=CARTESIAN_POINT('Ctrl Pts',(-1.52992798780065,124.743136886626,
-12.0022826425887));
#291636=CARTESIAN_POINT('Ctrl Pts',(-3.06356722876761,124.803200686683,
-11.7051236054165));
#291637=CARTESIAN_POINT('Ctrl Pts',(-5.96443528226193,124.926021949361,
-10.5321492263498));
#291638=CARTESIAN_POINT('Ctrl Pts',(-7.29891290370308,124.990539696528,
-9.6553811402027));
#291639=CARTESIAN_POINT('Ctrl Pts',(-9.53086438296879,125.115902420437,
-7.45483206289494));
#291640=CARTESIAN_POINT('Ctrl Pts',(-10.4146403136237,125.174446596594,
-6.16012410562965));
#291641=CARTESIAN_POINT('Ctrl Pts',(-11.6416510156975,125.299763148066,
-3.30137878322185));
#291642=CARTESIAN_POINT('Ctrl Pts',(-11.9715069422521,125.363044440324,
-1.76364841004787));
#291643=CARTESIAN_POINT('Ctrl Pts',(-11.9994118426542,125.425963812243,
-0.137215804927733));
#291644=CARTESIAN_POINT('Ctrl Pts',(-12.0000000000001,125.428611080214,
-0.0685949484236192));
#291645=CARTESIAN_POINT('Ctrl Pts',(-12.0000000000001,125.431249999508,
2.73285667600019E-15));
#291646=CARTESIAN_POINT('Ctrl Pts',(-12.0000000000001,125.806249999508,
-1.0547118733939E-14));
#291647=CARTESIAN_POINT('Ctrl Pts',(-12.0000000000001,125.769125942516,
-0.964986985673901));
#291648=CARTESIAN_POINT('Ctrl Pts',(-11.8836046085516,125.730603060961,
-1.92851526825847));
#291649=CARTESIAN_POINT('Ctrl Pts',(-11.2718009128407,125.627383811719,
-4.41276556604046));
#291650=CARTESIAN_POINT('Ctrl Pts',(-10.5889399812926,125.56332599208,-5.86512219781751));
#291651=CARTESIAN_POINT('Ctrl Pts',(-8.71656853591449,125.441944357557,
-8.39315212868226));
#291652=CARTESIAN_POINT('Ctrl Pts',(-7.55538743852935,125.378769778022,
-9.45195081641037));
#291653=CARTESIAN_POINT('Ctrl Pts',(-4.89580690723992,125.253368317505,
-11.0655482010172));
#291654=CARTESIAN_POINT('Ctrl Pts',(-3.42309837976009,125.194717237643,
-11.6059347670923));
#291655=CARTESIAN_POINT('Ctrl Pts',(-0.328008361997646,125.069518216469,
-12.0991251932609));
#291656=CARTESIAN_POINT('Ctrl Pts',(1.26618304560651,125.005031819417,-12.0371639804595));
#291657=CARTESIAN_POINT('Ctrl Pts',(4.30697724794929,124.882029110113,-11.3068065663843));
#291658=CARTESIAN_POINT('Ctrl Pts',(5.72744418487154,124.822223078081,-10.6578786238672));
#291659=CARTESIAN_POINT('Ctrl Pts',(8.26302605911904,124.696083445389,-8.842565323223));
#291660=CARTESIAN_POINT('Ctrl Pts',(9.34855021222853,124.635077726409,-7.68590015126261));
#291661=CARTESIAN_POINT('Ctrl Pts',(11.0095892765376,124.51191564796,-5.02418165010607));
#291662=CARTESIAN_POINT('Ctrl Pts',(11.5706872712687,124.448026028093,-3.54577376973066));
#291663=CARTESIAN_POINT('Ctrl Pts',(12.0900654713141,124.323409893459,-0.475311047824805));
#291664=CARTESIAN_POINT('Ctrl Pts',(12.0505338417015,124.265087752431,1.08637342597683));
#291665=CARTESIAN_POINT('Ctrl Pts',(11.3713292922706,124.138742241242,4.14985809937313));
#291666=CARTESIAN_POINT('Ctrl Pts',(10.7219775170637,124.074123727343,5.61853715041643));
#291667=CARTESIAN_POINT('Ctrl Pts',(8.90984038756518,123.952660229812,8.18700872245728));
#291668=CARTESIAN_POINT('Ctrl Pts',(7.77644366969167,123.8903211212,9.27037657699587));
#291669=CARTESIAN_POINT('Ctrl Pts',(5.15594158714334,123.764693450601,10.9472748861876));
#291670=CARTESIAN_POINT('Ctrl Pts',(3.69284093342787,123.70562855315,11.5234342032408));
#291671=CARTESIAN_POINT('Ctrl Pts',(0.609990526536278,123.580924634636,
12.087706928294));
#291672=CARTESIAN_POINT('Ctrl Pts',(-0.981399707504531,123.516551547435,
12.0632353700333));
#291673=CARTESIAN_POINT('Ctrl Pts',(-4.03434702382668,123.393057234344,
11.4068132083855));
#291674=CARTESIAN_POINT('Ctrl Pts',(-5.46918910028784,123.333876771955,
10.792557749552));
#291675=CARTESIAN_POINT('Ctrl Pts',(-8.05221336441863,123.207582119441,
9.03602339714975));
#291676=CARTESIAN_POINT('Ctrl Pts',(-9.16889223660466,123.145582038152,
7.90057035870083));
#291677=CARTESIAN_POINT('Ctrl Pts',(-10.8911261633591,123.023045994957,
5.27500816840282));
#291678=CARTESIAN_POINT('Ctrl Pts',(-11.4847996170347,122.959392917648,
3.81333328315813));
#291679=CARTESIAN_POINT('Ctrl Pts',(-11.9272030519174,122.865878822449,
1.52631316037461));
#291680=CARTESIAN_POINT('Ctrl Pts',(-12.0000000000001,122.835609410272,
0.763156065843486));
#291681=CARTESIAN_POINT('Ctrl Pts',(-12.0000000000001,122.80624999952,-9.43689570931383E-15));
#291682=CARTESIAN_POINT('Origin',(-8.79029313101884E-14,130.96875,0.));
#291683=CARTESIAN_POINT('',(-12.0000000000001,119.431249999532,8.29482724016328E-14));
#291684=CARTESIAN_POINT('',(-12.0000000000001,119.806249999532,-5.81888296038403E-14));
#291685=CARTESIAN_POINT('',(-12.0000000000001,130.96875,-1.46957615897682E-15));
#291686=CARTESIAN_POINT('Ctrl Pts',(-12.0000000000001,119.431249999532,
4.51721993144361E-14));
#291687=CARTESIAN_POINT('Ctrl Pts',(-12.0000000000001,119.443085102611,
0.307636647781991));
#291688=CARTESIAN_POINT('Ctrl Pts',(-11.9881702429117,119.455080866568,
0.615605725182721));
#291689=CARTESIAN_POINT('Ctrl Pts',(-11.8428535024459,119.529346228598,
2.4988117637302));
#291690=CARTESIAN_POINT('Ctrl Pts',(-11.4112356703933,119.593838282962,
4.03494972594653));
#291691=CARTESIAN_POINT('Ctrl Pts',(-9.9895647574198,119.719065609207,6.82812682905568));
#291692=CARTESIAN_POINT('Ctrl Pts',(-9.02238025756206,119.777697052648,
8.06296059190003));
#291693=CARTESIAN_POINT('Ctrl Pts',(-6.66877251628973,119.903084360385,
10.0970981483154));
#291694=CARTESIAN_POINT('Ctrl Pts',(-5.30386420471749,119.966277482577,
10.8762702578697));
#291695=CARTESIAN_POINT('Ctrl Pts',(-2.32256894648718,120.087701862772,
11.8797953199349));
#291696=CARTESIAN_POINT('Ctrl Pts',(-0.731034154377956,120.151679046811,
12.0826371615092));
#291697=CARTESIAN_POINT('Ctrl Pts',(2.39650174146898,120.278190531324,11.8595432877569));
#291698=CARTESIAN_POINT('Ctrl Pts',(3.90344614359641,120.336697353249,11.4522985786249));
#291699=CARTESIAN_POINT('Ctrl Pts',(6.70081111332831,120.460920120084,10.0779192792414));
#291700=CARTESIAN_POINT('Ctrl Pts',(7.96056234169184,120.525025626629,9.11563735429559));
#291701=CARTESIAN_POINT('Ctrl Pts',(10.034755997471,120.648813760085,6.76417815612786));
#291702=CARTESIAN_POINT('Ctrl Pts',(10.8306278056746,120.708932157215,5.39888360513246));
#291703=CARTESIAN_POINT('Ctrl Pts',(11.8478136055881,120.834888821484,2.45532321880896));
#291704=CARTESIAN_POINT('Ctrl Pts',(12.0654965891985,120.895533083184,0.907129236787544));
#291705=CARTESIAN_POINT('Ctrl Pts',(11.8985223670227,121.01797392093,-2.22129273422858));
#291706=CARTESIAN_POINT('Ctrl Pts',(11.5017561957471,121.08254188909,-3.77072795845864));
#291707=CARTESIAN_POINT('Ctrl Pts',(10.1437069246306,121.20821972362,-6.59628730733561));
#291708=CARTESIAN_POINT('Ctrl Pts',(9.20710805602347,121.266607157818,-7.85079237476785));
#291709=CARTESIAN_POINT('Ctrl Pts',(6.90141739958207,121.391737867082,-9.94008999640738));
#291710=CARTESIAN_POINT('Ctrl Pts',(5.55171625469305,121.455220721204,-10.7523786624008));
#291711=CARTESIAN_POINT('Ctrl Pts',(2.59730531844547,121.57733225951,-11.8218076510319));
#291712=CARTESIAN_POINT('Ctrl Pts',(1.01831374391615,121.640058343302,-12.0608691629107));
#291713=CARTESIAN_POINT('Ctrl Pts',(-2.10611302272581,121.766444060896,
-11.9144920478712));
#291714=CARTESIAN_POINT('Ctrl Pts',(-3.62219495019258,121.825306122227,
-11.5442874849623));
#291715=CARTESIAN_POINT('Ctrl Pts',(-6.45545251682648,121.949098843524,
-10.237397172522));
#291716=CARTESIAN_POINT('Ctrl Pts',(-7.74107895185393,122.013379111644,
-9.30337920646476));
#291717=CARTESIAN_POINT('Ctrl Pts',(-9.8693148984103,122.137738651117,-7.00227036660378));
#291718=CARTESIAN_POINT('Ctrl Pts',(-10.6952971812211,122.197160624728,
-5.66089624038417));
#291719=CARTESIAN_POINT('Ctrl Pts',(-11.7433895056935,122.318206030773,
-2.85503915504212));
#291720=CARTESIAN_POINT('Ctrl Pts',(-12.0000000000001,122.376129690943,
-1.43277391352303));
#291721=CARTESIAN_POINT('Ctrl Pts',(-12.0000000000001,122.43124999952,1.02695629777827E-14));
#291722=CARTESIAN_POINT('Ctrl Pts',(-12.0000000000001,122.80624999952,3.87190279838023E-14));
#291723=CARTESIAN_POINT('Ctrl Pts',(-12.0000000000001,122.776270810373,
-0.77926632248526));
#291724=CARTESIAN_POINT('Ctrl Pts',(-11.9240970835404,122.745345702254,
-1.55845810881199));
#291725=CARTESIAN_POINT('Ctrl Pts',(-11.4647743595056,122.650188016398,
-3.88270361944645));
#291726=CARTESIAN_POINT('Ctrl Pts',(-10.8516651212801,122.585588979386,
-5.36265231065594));
#291727=CARTESIAN_POINT('Ctrl Pts',(-9.10542162693431,122.463516494878,
-7.96836377170369));
#291728=CARTESIAN_POINT('Ctrl Pts',(-8.00084636519117,122.402264711622,
-9.07691102421512));
#291729=CARTESIAN_POINT('Ctrl Pts',(-5.42135353959798,122.276430632389,
-10.818934968515));
#291730=CARTESIAN_POINT('Ctrl Pts',(-3.9683912202721,122.216774796399,-11.4320744239647));
#291731=CARTESIAN_POINT('Ctrl Pts',(-0.899079105758544,122.092618513315,
-12.0691561732302));
#291732=CARTESIAN_POINT('Ctrl Pts',(0.688547655362349,122.028397661792,
-12.0829942621337));
#291733=CARTESIAN_POINT('Ctrl Pts',(3.75286824811511,121.904443290005,-11.5024782379153));
#291734=CARTESIAN_POINT('Ctrl Pts',(5.20225852444924,121.845730570123,-10.9237121701835));
#291735=CARTESIAN_POINT('Ctrl Pts',(7.83339548366492,121.719296722212,-9.22754491337953));
#291736=CARTESIAN_POINT('Ctrl Pts',(8.98177696327284,121.656131531625,-8.11399197794614));
#291737=CARTESIAN_POINT('Ctrl Pts',(10.765503539707,121.53426676251,-5.52585877431411));
#291738=CARTESIAN_POINT('Ctrl Pts',(11.3916501947226,121.470886064425,-4.08181518174822));
#291739=CARTESIAN_POINT('Ctrl Pts',(12.0549842028282,121.345656672567,-1.04218578921163));
#291740=CARTESIAN_POINT('Ctrl Pts',(12.0885988775717,121.287197801041,0.524022283936685));
#291741=CARTESIAN_POINT('Ctrl Pts',(11.552275802476,121.161680708871,3.61239839010473));
#291742=CARTESIAN_POINT('Ctrl Pts',(10.9757082466759,121.097136594324,5.10279256238657));
#291743=CARTESIAN_POINT('Ctrl Pts',(9.29592360412163,120.974496271202,7.74485796939733));
#291744=CARTESIAN_POINT('Ctrl Pts',(8.22018348407914,120.914162802098,8.87838696232961));
#291745=CARTESIAN_POINT('Ctrl Pts',(5.68195640921952,120.788140573221,10.6851216295968));
#291746=CARTESIAN_POINT('Ctrl Pts',(4.23931932328379,120.727734068384,11.335104213746));
#291747=CARTESIAN_POINT('Ctrl Pts',(1.18436608857568,120.60415861419,12.0440240616632));
#291748=CARTESIAN_POINT('Ctrl Pts',(-0.398660321286915,120.540123850784,
12.0955451771913));
#291749=CARTESIAN_POINT('Ctrl Pts',(-3.47312595407421,120.415759103507,
11.5900991948286));
#291750=CARTESIAN_POINT('Ctrl Pts',(-4.9367061390559,120.357336819557,11.0463519815541));
#291751=CARTESIAN_POINT('Ctrl Pts',(-7.6148521868453,120.230785634668,9.40995216834716));
#291752=CARTESIAN_POINT('Ctrl Pts',(-8.79431168759276,120.166330990559,
8.3182012252389));
#291753=CARTESIAN_POINT('Ctrl Pts',(-10.6375639830793,120.045157411401,
5.76737559864589));
#291754=CARTESIAN_POINT('Ctrl Pts',(-11.2948745591418,119.982073881331,
4.34118223713426));
#291755=CARTESIAN_POINT('Ctrl Pts',(-11.8869206891821,119.880796684097,
1.90099319300707));
#291756=CARTESIAN_POINT('Ctrl Pts',(-12.0000000000001,119.842841437673,
0.951142317236447));
#291757=CARTESIAN_POINT('Ctrl Pts',(-12.0000000000001,119.806249999532,
3.05311331771918E-14));
#291758=CARTESIAN_POINT('Origin',(-8.79029313101884E-14,130.96875,0.));
#291759=CARTESIAN_POINT('',(-12.0000000000001,116.431249999544,5.60947529935118E-14));
#291760=CARTESIAN_POINT('',(-12.0000000000001,116.806249999544,-9.27792157148178E-14));
#291761=CARTESIAN_POINT('',(-12.0000000000001,130.96875,-1.46957615897682E-15));
#291762=CARTESIAN_POINT('Ctrl Pts',(-12.0000000000001,116.431249999544,
-1.13797860024079E-14));
#291763=CARTESIAN_POINT('Ctrl Pts',(-12.0000000000001,116.450519136619,
0.500873773198305));
#291764=CARTESIAN_POINT('Ctrl Pts',(-11.9686420792505,116.470199718424,
1.00225366006863));
#291765=CARTESIAN_POINT('Ctrl Pts',(-11.7089771942863,116.552670958819,
3.06160585470905));
#291766=CARTESIAN_POINT('Ctrl Pts',(-11.2073618931561,116.616902187071,
4.56822045722642));
#291767=CARTESIAN_POINT('Ctrl Pts',(-9.6569671432679,116.741093193354,7.29263498896614));
#291768=CARTESIAN_POINT('Ctrl Pts',(-8.62681581704463,116.800707940273,
8.48631601045096));
#291769=CARTESIAN_POINT('Ctrl Pts',(-6.17596786986063,116.926529824619,
10.4048915410279));
#291770=CARTESIAN_POINT('Ctrl Pts',(-4.78126553006508,116.98784374612,11.1150124322844));
#291771=CARTESIAN_POINT('Ctrl Pts',(-1.7643663240107,117.10987988252,11.9751588681878));
#291772=CARTESIAN_POINT('Ctrl Pts',(-0.167335355273029,117.174481142232,
12.1032712798306));
#291773=CARTESIAN_POINT('Ctrl Pts',(2.94697813853509,117.300457769347,11.7352472424878));
#291774=CARTESIAN_POINT('Ctrl Pts',(4.43598025015591,117.3587653613,11.2571218222671));
#291775=CARTESIAN_POINT('Ctrl Pts',(7.1616829743892,117.483688624386,9.75464608989288));
#291776=CARTESIAN_POINT('Ctrl Pts',(8.36998823367536,117.547357307896,8.73992698006901));
#291777=CARTESIAN_POINT('Ctrl Pts',(10.3381688774826,117.669933227142,6.29353728685221));
#291778=CARTESIAN_POINT('Ctrl Pts',(11.0748361719961,117.731867143341,4.88206941562071));
#291779=CARTESIAN_POINT('Ctrl Pts',(11.9515988639792,117.858152680848,1.88433420432893));
#291780=CARTESIAN_POINT('Ctrl Pts',(12.0947296000952,117.917367252942,0.330082711652782));
#291781=CARTESIAN_POINT('Ctrl Pts',(11.7802236931385,118.040832147053,-2.77702219578679));
#291782=CARTESIAN_POINT('Ctrl Pts',(11.3138892864885,118.105213315824,-4.29899774607966));
#291783=CARTESIAN_POINT('Ctrl Pts',(9.82855002991664,118.229949232127,-7.05871424878508));
#291784=CARTESIAN_POINT('Ctrl Pts',(8.8304088319451,118.288983648681,-8.27343176695405));
#291785=CARTESIAN_POINT('Ctrl Pts',(6.42879631823223,118.414598265921,-10.2510567167147));
#291786=CARTESIAN_POINT('Ctrl Pts',(5.04912863955706,118.477008455727,-10.9963301642431));
#291787=CARTESIAN_POINT('Ctrl Pts',(2.04732776269366,118.598433851882,-11.9305466432727));
#291788=CARTESIAN_POINT('Ctrl Pts',(0.44986907729023,118.663052413097,-12.0965614184918));
#291789=CARTESIAN_POINT('Ctrl Pts',(-2.67412136042386,118.789420480815,
-11.8001856782115));
#291790=CARTESIAN_POINT('Ctrl Pts',(-4.17212545624418,118.847748257556,
-11.3573195903235));
#291791=CARTESIAN_POINT('Ctrl Pts',(-6.93396204596735,118.972343476991,
-9.91837487743489));
#291792=CARTESIAN_POINT('Ctrl Pts',(-8.16816599184413,119.036246259063,
-8.92945641981678));
#291793=CARTESIAN_POINT('Ctrl Pts',(-10.1895003983347,119.159444745716,
-6.5300423601243));
#291794=CARTESIAN_POINT('Ctrl Pts',(-10.9558841274651,119.22039573402,-5.14160249984191));
#291795=CARTESIAN_POINT('Ctrl Pts',(-11.80930185404,119.334044878749,-2.46474708173146));
#291796=CARTESIAN_POINT('Ctrl Pts',(-12.0000000000001,119.383732705891,
-1.23514436925128));
#291797=CARTESIAN_POINT('Ctrl Pts',(-12.0000000000001,119.431249999532,
-3.27515792264421E-14));
#291798=CARTESIAN_POINT('Ctrl Pts',(-12.0000000000001,119.806249999532,
2.692290834716E-14));
#291799=CARTESIAN_POINT('Ctrl Pts',(-12.0000000000001,119.783277972883,
-0.597125113647374));
#291800=CARTESIAN_POINT('Ctrl Pts',(-11.9554325127281,119.759730929568,
-1.19471611211129));
#291801=CARTESIAN_POINT('Ctrl Pts',(-11.6308449637883,119.672791989272,
-3.34910515005578));
#291802=CARTESIAN_POINT('Ctrl Pts',(-11.0897504983799,119.608334559506,
-4.84877198070028));
#291803=CARTESIAN_POINT('Ctrl Pts',(-9.47454580744222,119.485186418556,
-7.52502068711062));
#291804=CARTESIAN_POINT('Ctrl Pts',(-8.42662162912825,119.42557711517,-8.68245593268385));
#291805=CARTESIAN_POINT('Ctrl Pts',(-5.92843279303923,119.299391062744,
-10.5511886788847));
#291806=CARTESIAN_POINT('Ctrl Pts',(-4.49594034728034,119.238114606867,
-11.2365595976314));
#291807=CARTESIAN_POINT('Ctrl Pts',(-1.4555755876238,119.115129268884,-12.0138062962249));
#291808=CARTESIAN_POINT('Ctrl Pts',(0.122259056921303,119.051304516797,
-12.1010385489323));
#291809=CARTESIAN_POINT('Ctrl Pts',(3.20537086773915,118.926590024272,-11.6671580584952));
#291810=CARTESIAN_POINT('Ctrl Pts',(4.68230336517048,118.868287043019,-11.1567464555144));
#291811=CARTESIAN_POINT('Ctrl Pts',(7.3959683167439,118.742051657471,-9.58251626242619));
#291812=CARTESIAN_POINT('Ctrl Pts',(8.59852163498118,118.677435153814,-8.5200164017129));
#291813=CARTESIAN_POINT('Ctrl Pts',(10.4975241771352,118.555791084917,-6.01760343772505));
#291814=CARTESIAN_POINT('Ctrl Pts',(11.1871642645573,118.493784188957,-4.6105778085268));
#291815=CARTESIAN_POINT('Ctrl Pts',(11.9938522491681,118.368094869886,-1.60557179364514));
#291816=CARTESIAN_POINT('Ctrl Pts',(12.1007908177156,118.308875546012,-0.0354984191383897));
#291817=CARTESIAN_POINT('Ctrl Pts',(11.7061277760934,118.184326743795,3.07373650387339));
#291818=CARTESIAN_POINT('Ctrl Pts',(11.2020091660397,118.119994177238,4.5821718769257));
#291819=CARTESIAN_POINT('Ctrl Pts',(9.6542340162482,117.996361433865,7.29292631911161));
#291820=CARTESIAN_POINT('Ctrl Pts',(8.63516107596953,117.937335124396,8.47496175593411));
#291821=CARTESIAN_POINT('Ctrl Pts',(6.17874626117698,117.81099789906,10.4075496139555));
#291822=CARTESIAN_POINT('Ctrl Pts',(4.75697882722234,117.748673835196,11.1294576150518));
#291823=CARTESIAN_POINT('Ctrl Pts',(1.73247376269937,117.626330035357,11.9765439283481));
#291824=CARTESIAN_POINT('Ctrl Pts',(0.160766521532632,117.562753141943,
12.100123861986));
#291825=CARTESIAN_POINT('Ctrl Pts',(-2.93016092852451,117.43772250017,11.7395612500877));
#291826=CARTESIAN_POINT('Ctrl Pts',(-4.42060094658391,117.379384307779,
11.2632781652628));
#291827=CARTESIAN_POINT('Ctrl Pts',(-7.16846560687761,117.253556389344,
9.75325728399708));
#291828=CARTESIAN_POINT('Ctrl Pts',(-8.39282136547194,117.188969784549,
8.72202340899157));
#291829=CARTESIAN_POINT('Ctrl Pts',(-10.3476250584071,117.06672636511,6.27120636193096));
#291830=CARTESIAN_POINT('Ctrl Pts',(-11.0701893390789,117.005761656376,
4.88390755713557));
#291831=CARTESIAN_POINT('Ctrl Pts',(-11.8352255782078,116.896502075798,
2.29243572099499));
#291832=CARTESIAN_POINT('Ctrl Pts',(-12.0000000000001,116.850419884796,
1.14813325590528));
#291833=CARTESIAN_POINT('Ctrl Pts',(-12.0000000000001,116.806249999544,
1.63757896132211E-14));
#291834=CARTESIAN_POINT('Origin',(-8.79029313101884E-14,130.96875,0.));
#291835=CARTESIAN_POINT('',(-12.0000000000001,113.431249999556,-1.70623322603542E-15));
#291836=CARTESIAN_POINT('',(-12.0000000000001,113.806249999556,-1.1130606243825E-13));
#291837=CARTESIAN_POINT('',(-12.0000000000001,130.96875,-1.46957615897682E-15));
#291838=CARTESIAN_POINT('Ctrl Pts',(-12.0000000000001,113.431249999556,
5.82867087928207E-15));
#291839=CARTESIAN_POINT('Ctrl Pts',(-12.0000000000001,113.457825190305,
0.690784232431625));
#291840=CARTESIAN_POINT('Ctrl Pts',(-11.9403554096789,113.485156143997,
1.38183374397962));
#291841=CARTESIAN_POINT('Ctrl Pts',(-11.5514681472104,113.575642332941,
3.60753621479684));
#291842=CARTESIAN_POINT('Ctrl Pts',(-10.9828317388839,113.63948040642,5.08215484118498));
#291843=CARTESIAN_POINT('Ctrl Pts',(-9.30767226272974,113.762501690871,
7.73562560296991));
#291844=CARTESIAN_POINT('Ctrl Pts',(-8.21499357640178,113.823722415958,
8.88744539519899));
#291845=CARTESIAN_POINT('Ctrl Pts',(-5.66850236442309,113.949899202563,
10.6893059180563));
#291846=CARTESIAN_POINT('Ctrl Pts',(-4.24472700301189,114.009547185458,
11.3302881273245));
#291847=CARTESIAN_POINT('Ctrl Pts',(-1.20105788221068,114.132666187656,
12.0437244646561));
#291848=CARTESIAN_POINT('Ctrl Pts',(0.392567991437235,114.197129708379,
12.0970917713889));
#291849=CARTESIAN_POINT('Ctrl Pts',(3.48493930206807,114.322218755539,11.587619026558));
#291850=CARTESIAN_POINT('Ctrl Pts',(4.95547101554945,114.38095050263,11.0390659981908));
#291851=CARTESIAN_POINT('Ctrl Pts',(7.6061616336417,114.506404940095,9.41100456735867));
#291852=CARTESIAN_POINT('Ctrl Pts',(8.76103716219917,114.569507126276,8.34657176380249));
#291853=CARTESIAN_POINT('Ctrl Pts',(10.6206625015808,114.690723095543,5.80796595342873));
#291854=CARTESIAN_POINT('Ctrl Pts',(11.2963358913733,114.755096313423,4.35022984652544));
#291855=CARTESIAN_POINT('Ctrl Pts',(12.0293491926827,114.881641011308,1.29905112196894));
#291856=CARTESIAN_POINT('Ctrl Pts',(12.0964796858635,114.94007598164,-0.260766983788003));
#291857=CARTESIAN_POINT('Ctrl Pts',(11.6316057612974,115.064417264866,-3.34179484746409));
#291858=CARTESIAN_POINT('Ctrl Pts',(11.0954841507373,115.128464233674,-4.83240810857913));
#291859=CARTESIAN_POINT('Ctrl Pts',(9.48106461331453,115.252075785788,-7.52095764001368));
#291860=CARTESIAN_POINT('Ctrl Pts',(8.41901860617005,115.312432377127,-8.69341978411619));
#291861=CARTESIAN_POINT('Ctrl Pts',(5.9192982166187,115.438443734786,-10.5526971298546));
#291862=CARTESIAN_POINT('Ctrl Pts',(4.50972010974552,115.498827989115,-11.2276343318953));
#291863=CARTESIAN_POINT('Ctrl Pts',(1.47870553517511,115.621435104166,-12.0132767706304));
#291864=CARTESIAN_POINT('Ctrl Pts',(-0.117019989849763,115.68598355757,
-12.1033683611737));
#291865=CARTESIAN_POINT('Ctrl Pts',(-3.22065113350542,115.811528074544,
-11.6634342756433));
#291866=CARTESIAN_POINT('Ctrl Pts',(-4.7003849565096,115.869973461379,-11.1496479264714));
#291867=CARTESIAN_POINT('Ctrl Pts',(-7.38857458390202,115.995186606646,
-9.58334783932789));
#291868=CARTESIAN_POINT('Ctrl Pts',(-8.57009823916183,116.05858483444,-8.54314197267345));
#291869=CARTESIAN_POINT('Ctrl Pts',(-10.4837014045556,116.180491570798,
-6.04977764603272));
#291870=CARTESIAN_POINT('Ctrl Pts',(-11.1897627199188,116.243581245614,
-4.61491991065847));
#291871=CARTESIAN_POINT('Ctrl Pts',(-11.8650162131259,116.349694596727,
-2.07605764573233));
#291872=CARTESIAN_POINT('Ctrl Pts',(-12.0000000000001,116.391271532176,
-1.03918331784912));
#291873=CARTESIAN_POINT('Ctrl Pts',(-12.0000000000001,116.431249999544,
4.16333634234434E-15));
#291874=CARTESIAN_POINT('Ctrl Pts',(-12.0000000000001,116.806249999544,
2.76861866765898E-14));
#291875=CARTESIAN_POINT('Ctrl Pts',(-12.0000000000001,116.79048398263,-0.40981515411806));
#291876=CARTESIAN_POINT('Ctrl Pts',(-11.979007200241,116.774437557422,-0.82009814833851));
#291877=CARTESIAN_POINT('Ctrl Pts',(-11.7759002586227,116.696021448289,
-2.79241977131035));
#291878=CARTESIAN_POINT('Ctrl Pts',(-11.309428417977,116.631851765499,-4.30885338971805));
#291879=CARTESIAN_POINT('Ctrl Pts',(-9.83047366907497,116.50777186963,-7.05359202791613));
#291880=CARTESIAN_POINT('Ctrl Pts',(-8.84066915635196,116.449162423424,
-8.26038103683867));
#291881=CARTESIAN_POINT('Ctrl Pts',(-6.42689296455462,116.322691881841,
-10.2572630045548));
#291882=CARTESIAN_POINT('Ctrl Pts',(-5.01622766426787,116.259160670949,
-11.0160469934526));
#291883=CARTESIAN_POINT('Ctrl Pts',(-2.00853060107773,116.137496769046,
-11.9328865761613));
#291884=CARTESIAN_POINT('Ctrl Pts',(-0.443768785237827,116.074200823988,
-12.0925909409474));
#291885=CARTESIAN_POINT('Ctrl Pts',(2.65392175167885,115.948896609605,-11.80542678572));
#291886=CARTESIAN_POINT('Ctrl Pts',(4.15771200471099,115.890365913736,-11.3633123313233));
#291887=CARTESIAN_POINT('Ctrl Pts',(6.9386714237031,115.764980553746,-9.91745581711915));
#291888=CARTESIAN_POINT('Ctrl Pts',(8.18390177819024,115.700458739542,-8.91767835283168));
#291889=CARTESIAN_POINT('Ctrl Pts',(10.1932370278195,115.577663391961,-6.51870429084006));
#291890=CARTESIAN_POINT('Ctrl Pts',(10.9481940148213,115.517561718441,-5.15099467981093));
#291891=CARTESIAN_POINT('Ctrl Pts',(11.9033774238926,115.391488981224,-2.18427134454457));
#291892=CARTESIAN_POINT('Ctrl Pts',(12.0866899624146,115.330838674002,-0.610980294446826));
#291893=CARTESIAN_POINT('Ctrl Pts',(11.8376023441408,115.207435578478,2.51577393725414));
#291894=CARTESIAN_POINT('Ctrl Pts',(11.4080289538783,115.143460160531,4.03914695105162));
#291895=CARTESIAN_POINT('Ctrl Pts',(9.99673848720598,115.018986808815,6.81609837161942));
#291896=CARTESIAN_POINT('Ctrl Pts',(9.03556009573234,114.960616136635,8.04689953179336));
#291897=CARTESIAN_POINT('Ctrl Pts',(6.66537138938319,114.834122177736,10.1047594233466));
#291898=CARTESIAN_POINT('Ctrl Pts',(5.26778424110486,114.769505796758,10.8988130867691));
#291899=CARTESIAN_POINT('Ctrl Pts',(2.27957664384873,114.648300534033,11.883608380707));
#291900=CARTESIAN_POINT('Ctrl Pts',(0.722438874997024,114.585473265916,
12.0787176302905));
#291901=CARTESIAN_POINT('Ctrl Pts',(-2.38105346608099,114.459934363625,
11.863901263394));
#291902=CARTESIAN_POINT('Ctrl Pts',(-3.89783877408231,114.401062257605,
11.4554995754585));
#291903=CARTESIAN_POINT('Ctrl Pts',(-6.71033303018463,114.276146264562,
10.0727879054382));
#291904=CARTESIAN_POINT('Ctrl Pts',(-7.97522204452457,114.21172148225,9.10414927996976));
#291905=CARTESIAN_POINT('Ctrl Pts',(-10.0370462972033,114.08842795567,6.75646747682689));
#291906=CARTESIAN_POINT('Ctrl Pts',(-10.8234227591233,114.029005854449,
5.40792805678477));
#291907=CARTESIAN_POINT('Ctrl Pts',(-11.7747831448269,113.912041481627,
2.67672150532812));
#291908=CARTESIAN_POINT('Ctrl Pts',(-12.0000000000001,113.857888696239,
1.34227437121494));
#291909=CARTESIAN_POINT('Ctrl Pts',(-12.0000000000001,113.806249999556,
9.71445146547012E-15));
#291910=CARTESIAN_POINT('Origin',(-8.79029313101884E-14,130.96875,0.));
#291911=CARTESIAN_POINT('',(-12.0000000000001,110.431249999568,-1.01716837888022E-14));
#291912=CARTESIAN_POINT('',(-12.0000000000001,110.806249999568,3.54084502355313E-16));
#291913=CARTESIAN_POINT('',(-12.0000000000001,130.96875,-1.46957615897682E-15));
#291914=CARTESIAN_POINT('Ctrl Pts',(-12.0000000000001,110.431249999568,
-1.74860126378462E-14));
#291915=CARTESIAN_POINT('Ctrl Pts',(-12.0000000000001,110.465115924226,
0.880296476203017));
#291916=CARTESIAN_POINT('Ctrl Pts',(-11.9031394395545,110.500166049423,
1.75990265488635));
#291917=CARTESIAN_POINT('Ctrl Pts',(-11.3692619648579,110.598537238417,
4.14345429566384));
#291918=CARTESIAN_POINT('Ctrl Pts',(-10.7356906174076,110.661850372262,
5.58332922324425));
#291919=CARTESIAN_POINT('Ctrl Pts',(-8.93782980140339,110.783554748739,
8.16270075587147));
#291920=CARTESIAN_POINT('Ctrl Pts',(-7.78210399224986,110.847011607531,
9.27113220442497));
#291921=CARTESIAN_POINT('Ctrl Pts',(-5.13984413787133,110.973474930871,
10.9532298014104));
#291922=CARTESIAN_POINT('Ctrl Pts',(-3.68709432736107,111.032103901031,
11.523741709725));
#291923=CARTESIAN_POINT('Ctrl Pts',(-0.620285349530542,111.156158930108,
12.0865763507926));
#291924=CARTESIAN_POINT('Ctrl Pts',(0.966336225591075,111.220339121004,
12.0638434327127));
#291925=CARTESIAN_POINT('Ctrl Pts',(4.03235325847998,111.344362115236,11.4098263448967));
#291926=CARTESIAN_POINT('Ctrl Pts',(5.48291136998425,111.404179853104,10.7880339859718));
#291927=CARTESIAN_POINT('Ctrl Pts',(8.05274987745621,111.530059705669,9.03079685556067));
#291928=CARTESIAN_POINT('Ctrl Pts',(9.15056396922682,111.591080896714,7.91637343568581));
#291929=CARTESIAN_POINT('Ctrl Pts',(10.8812710005861,111.713290272981,5.30205556549628));
#291930=CARTESIAN_POINT('Ctrl Pts',(11.4858356836687,111.777879619812,3.81958246250681));
#291931=CARTESIAN_POINT('Ctrl Pts',(12.0770307530136,111.903732565958,0.740305302302331));
#291932=CARTESIAN_POINT('Ctrl Pts',(12.0715928814009,111.962064297098,-0.824235712880048));
#291933=CARTESIAN_POINT('Ctrl Pts',(11.4636098970648,112.08707745876,-3.87622914728557));
#291934=CARTESIAN_POINT('Ctrl Pts',(10.8623097381496,112.150669900599,-5.33384983312881));
#291935=CARTESIAN_POINT('Ctrl Pts',(9.12567953174611,112.273052622388,-7.95074901703718));
#291936=CARTESIAN_POINT('Ctrl Pts',(8.00161470651909,112.335310435219,-9.08112915652761));
#291937=CARTESIAN_POINT('Ctrl Pts',(5.40736674584077,112.461639222265,-10.8236510627333));
#291938=CARTESIAN_POINT('Ctrl Pts',(3.96912835756686,112.520695384853,-11.4296579216072));
#291939=CARTESIAN_POINT('Ctrl Pts',(0.91344063540796,112.644300549689,-12.0684562331533));
#291940=CARTESIAN_POINT('Ctrl Pts',(-0.677155773912495,112.708641526006,
-12.0840159153029));
#291941=CARTESIAN_POINT('Ctrl Pts',(-3.75695067726136,112.833221846805,
-11.5028231922881));
#291942=CARTESIAN_POINT('Ctrl Pts',(-5.21772308801828,112.892408916726,
-10.9181014267066));
#291943=CARTESIAN_POINT('Ctrl Pts',(-7.82876549740021,113.018085923719,
-9.22610798019146));
#291944=CARTESIAN_POINT('Ctrl Pts',(-8.955499396414,113.080158694416,-8.13690020602289));
#291945=CARTESIAN_POINT('Ctrl Pts',(-10.752452768734,113.201766616298,-5.55974102688885));
#291946=CARTESIAN_POINT('Ctrl Pts',(-11.3934535376065,113.266383763236,
-4.08838410163288));
#291947=CARTESIAN_POINT('Ctrl Pts',(-11.909628104702,113.364715251788,-1.70011239393634));
#291948=CARTESIAN_POINT('Ctrl Pts',(-12.0000000000001,113.398538036134,
-0.850300897476276));
#291949=CARTESIAN_POINT('Ctrl Pts',(-12.0000000000001,113.431249999556,
-6.21724893790088E-14));
#291950=CARTESIAN_POINT('Ctrl Pts',(-12.0000000000001,113.806249999556,
6.10622663543836E-14));
#291951=CARTESIAN_POINT('Ctrl Pts',(-12.0000000000001,113.797455107568,
-0.228610690666172));
#291952=CARTESIAN_POINT('Ctrl Pts',(-11.9934672441515,113.788570061458,
-0.45744218831683));
#291953=CARTESIAN_POINT('Ctrl Pts',(-11.8898190120987,113.717659267,-2.26698993984803));
#291954=CARTESIAN_POINT('Ctrl Pts',(-11.4872988731828,113.653101432803,
-3.81429216865722));
#291955=CARTESIAN_POINT('Ctrl Pts',(-10.1187640137248,113.527495091212,
-6.63458618622984));
#291956=CARTESIAN_POINT('Ctrl Pts',(-9.17714746409585,113.469078172581,
-7.88587738051025));
#291957=CARTESIAN_POINT('Ctrl Pts',(-6.86355088241269,113.343902531598,
-9.96618318978778));
#291958=CARTESIAN_POINT('Ctrl Pts',(-5.51130420365368,113.280464935998,
-10.7730647239246));
#291959=CARTESIAN_POINT('Ctrl Pts',(-2.55243275192805,113.15846339173,-11.8317281566572));
#291960=CARTESIAN_POINT('Ctrl Pts',(-0.97137790623552,113.095543061264,
-12.064889759129));
#291961=CARTESIAN_POINT('Ctrl Pts',(2.15358968078377,112.969135467026,-11.9060031991555));
#291962=CARTESIAN_POINT('Ctrl Pts',(3.66819178657938,112.910343101329,-11.5297558769136));
#291963=CARTESIAN_POINT('Ctrl Pts',(6.49566732729766,112.786477290939,-10.2118332717201));
#291964=CARTESIAN_POINT('Ctrl Pts',(7.77712174052835,112.722223028237,-9.27316675891725));
#291965=CARTESIAN_POINT('Ctrl Pts',(9.89660650128791,112.597953813618,-6.96381187199637));
#291966=CARTESIAN_POINT('Ctrl Pts',(10.7177142680202,112.538429915866,-5.61854633965747));
#291967=CARTESIAN_POINT('Ctrl Pts',(11.7950102695258,112.412635919089,-2.69874525153756));
#291968=CARTESIAN_POINT('Ctrl Pts',(12.0447056237293,112.351178829674,-1.15333520888798));
#291969=CARTESIAN_POINT('Ctrl Pts',(11.9409784320375,112.229225628947,1.98296153828977));
#291970=CARTESIAN_POINT('Ctrl Pts',(11.574318636668,112.164619830901,3.54316225105717));
#291971=CARTESIAN_POINT('Ctrl Pts',(10.2710279476328,112.038586094515,6.39576490361487));
#291972=CARTESIAN_POINT('Ctrl Pts',(9.36048981331488,111.980285079213,7.66688091650389));
#291973=CARTESIAN_POINT('Ctrl Pts',(7.09613388102823,111.855405387036,9.80251350578982));
#291974=CARTESIAN_POINT('Ctrl Pts',(5.75996790521609,111.791701845441,10.6427135154324));
#291975=CARTESIAN_POINT('Ctrl Pts',(2.82903220130612,111.66903620831,11.7677579487339));
#291976=CARTESIAN_POINT('Ctrl Pts',(1.26078481853545,111.607249816787,12.0372005843419));
#291977=CARTESIAN_POINT('Ctrl Pts',(-1.86064935753329,111.480985152024,
11.9553197569415));
#291978=CARTESIAN_POINT('Ctrl Pts',(-3.38429918801148,111.421691090299,
11.6162905055771));
#291979=CARTESIAN_POINT('Ctrl Pts',(-6.24692957529679,111.298293293233,
10.3664383288339));
#291980=CARTESIAN_POINT('Ctrl Pts',(-7.55376660389433,111.233894356657,
9.45662322434075));
#291981=CARTESIAN_POINT('Ctrl Pts',(-9.72673952276036,111.109086673137,
7.19824128289136));
#291982=CARTESIAN_POINT('Ctrl Pts',(-10.5776405378452,111.050118849626,
5.87687081016613));
#291983=CARTESIAN_POINT('Ctrl Pts',(-11.7125327347171,110.926016024765,
3.0197434655804));
#291984=CARTESIAN_POINT('Ctrl Pts',(-12.0000000000001,110.864590449283,
1.51647689596978));
#291985=CARTESIAN_POINT('Ctrl Pts',(-12.0000000000001,110.806249999568,
-2.22044604925031E-14));
#291986=CARTESIAN_POINT('Origin',(-8.79029313101884E-14,130.96875,0.));
#291987=CARTESIAN_POINT('',(-12.0000000000001,107.43124999958,-1.00342610070077E-13));
#291988=CARTESIAN_POINT('',(-12.0000000000001,107.80624999958,1.16164430694665E-14));
#291989=CARTESIAN_POINT('',(-12.0000000000001,130.96875,-1.46957615897682E-15));
#291990=CARTESIAN_POINT('Ctrl Pts',(-12.0000000000001,107.43124999958,-2.35922392732846E-14));
#291991=CARTESIAN_POINT('Ctrl Pts',(-12.0000000000001,107.472475829027,
1.0716067184754));
#291992=CARTESIAN_POINT('Ctrl Pts',(-11.8564608278089,107.515392780944,
2.14053305265728));
#291993=CARTESIAN_POINT('Ctrl Pts',(-11.1605739263003,107.621569699177,
4.6743434535674));
#291994=CARTESIAN_POINT('Ctrl Pts',(-10.4632702917257,107.683319400101,
6.0767941236516));
#291995=CARTESIAN_POINT('Ctrl Pts',(-8.5512486899399,107.805106347455,8.56729714134744));
#291996=CARTESIAN_POINT('Ctrl Pts',(-7.34357041189055,107.869719085032,
9.62258470436895));
#291997=CARTESIAN_POINT('Ctrl Pts',(-4.62189680058411,107.995863404523,
11.1819618222427));
#291998=CARTESIAN_POINT('Ctrl Pts',(-3.14182651482416,108.054160447384,
11.6844830099114));
#291999=CARTESIAN_POINT('Ctrl Pts',(-0.0568141277773715,108.178951819832,
12.1014150897439));
#292000=CARTESIAN_POINT('Ctrl Pts',(1.51967651284923,108.242722205819,12.0057583846512));
#292001=CARTESIAN_POINT('Ctrl Pts',(4.5564574303511,108.365562574341,11.2123528821052));
#292002=CARTESIAN_POINT('Ctrl Pts',(5.98650151062605,108.427067136739,10.5185617850649));
#292003=CARTESIAN_POINT('Ctrl Pts',(8.47510348932741,108.553289670874,8.63509949614269));
#292004=CARTESIAN_POINT('Ctrl Pts',(9.51639107407667,108.612749709332,7.47198794670194));
#292005=CARTESIAN_POINT('Ctrl Pts',(11.116123688399,108.736013143636,4.78771517132547));
#292006=CARTESIAN_POINT('Ctrl Pts',(11.6487272945608,108.800444999749,3.28595424396765));
#292007=CARTESIAN_POINT('Ctrl Pts',(12.0990450148902,108.92539154911,0.184463751769529));
#292008=CARTESIAN_POINT('Ctrl Pts',(12.0210207858086,108.984237724039,-1.38417049431514));
#292009=CARTESIAN_POINT('Ctrl Pts',(11.2707328709427,109.10976338588,-4.40324796613719));
#292010=CARTESIAN_POINT('Ctrl Pts',(10.6059494256205,109.17266439157,-5.82504154546219));
#292011=CARTESIAN_POINT('Ctrl Pts',(8.74928869642534,109.293831307012,-8.36566466196085));
#292012=CARTESIAN_POINT('Ctrl Pts',(7.56355668864608,109.358446893393,-9.45127849098679));
#292013=CARTESIAN_POINT('Ctrl Pts',(4.87605914739465,109.48496203341,-11.073291084806));
#292014=CARTESIAN_POINT('Ctrl Pts',(3.40927519642272,109.543341920951,-11.609074510916));
#292015=CARTESIAN_POINT('Ctrl Pts',(0.332653773135498,109.667793871786,
-12.0974309104079));
#292016=CARTESIAN_POINT('Ctrl Pts',(-1.24920411698429,109.731781367575,
-12.0373623932641));
#292017=CARTESIAN_POINT('Ctrl Pts',(-4.30075360512462,109.855219137329,
-11.3121123245655));
#292018=CARTESIAN_POINT('Ctrl Pts',(-5.74099588501373,109.915819683157,
-10.6537031827515));
#292019=CARTESIAN_POINT('Ctrl Pts',(-8.26972566093404,110.041882442436,
-8.83219195748779));
#292020=CARTESIAN_POINT('Ctrl Pts',(-9.33885324364083,110.10202934897,-7.69296290720051));
#292021=CARTESIAN_POINT('Ctrl Pts',(-11.0033260464683,110.224793971897,
-5.04269138549187));
#292022=CARTESIAN_POINT('Ctrl Pts',(-11.5714789179734,110.289320479752,
-3.55002077741768));
#292023=CARTESIAN_POINT('Ctrl Pts',(-11.9446631888315,110.379350140444,
-1.33108289701475));
#292024=CARTESIAN_POINT('Ctrl Pts',(-12.0000000000001,110.405652480965,
-0.665371037497507));
#292025=CARTESIAN_POINT('Ctrl Pts',(-12.0000000000001,110.431249999568,
-5.02375918642883E-14));
#292026=CARTESIAN_POINT('Ctrl Pts',(-12.0000000000001,110.806249999568,
2.17774516368745E-15));
#292027=CARTESIAN_POINT('Ctrl Pts',(-12.0000000000001,110.804838357927,
-0.0366936138490478));
#292028=CARTESIAN_POINT('Ctrl Pts',(-11.999831697421,110.803424321145,-0.073394801155502));
#292029=CARTESIAN_POINT('Ctrl Pts',(-11.9848975174662,110.740622205456,
-1.70099394016176));
#292030=CARTESIAN_POINT('Ctrl Pts',(-11.6540662341939,110.676004008975,
-3.27315832183884));
#292031=CARTESIAN_POINT('Ctrl Pts',(-10.4157421801185,110.54958555311,-6.15687014859585));
#292032=CARTESIAN_POINT('Ctrl Pts',(-9.53582486973339,110.491242982813,
-7.44733605075462));
#292033=CARTESIAN_POINT('Ctrl Pts',(-7.32059686431816,110.366695474867,
-9.63661626355309));
#292034=CARTESIAN_POINT('Ctrl Pts',(-6.00099254844588,110.302763449472,
-10.5092211258972));
#292035=CARTESIAN_POINT('Ctrl Pts',(-3.09828244396946,110.179483361799,
-11.6989576253021));
#292036=CARTESIAN_POINT('Ctrl Pts',(-1.54270457224186,110.118653710383,
-12.0035458220116));
#292037=CARTESIAN_POINT('Ctrl Pts',(1.57484202992488,109.992546301288,-11.9964432460054));
#292038=CARTESIAN_POINT('Ctrl Pts',(3.10713791958133,109.932599558695,-11.6936044440958));
#292039=CARTESIAN_POINT('Ctrl Pts',(6.00290068011063,109.809697043666,-10.5101858809725));
#292040=CARTESIAN_POINT('Ctrl Pts',(7.33368685836178,109.745192702931,-9.6289008134264));
#292041=CARTESIAN_POINT('Ctrl Pts',(9.55771326639455,109.619902138368,-7.42047872440394));
#292042=CARTESIAN_POINT('Ctrl Pts',(10.4370687726621,109.561312846305,-6.12216827482664));
#292043=CARTESIAN_POINT('Ctrl Pts',(11.6535135321669,109.435957947521,-3.25899308580099));
#292044=CARTESIAN_POINT('Ctrl Pts',(11.9776928605359,109.372723534638,-1.72063683666438));
#292045=CARTESIAN_POINT('Ctrl Pts',(12.0204952786623,109.251203487661,1.42419635463371));
#292046=CARTESIAN_POINT('Ctrl Pts',(11.726835375321,109.187405635287,3.00043341259854));
#292047=CARTESIAN_POINT('Ctrl Pts',(10.5582919242157,109.06091014305,5.90882078243624));
#292048=CARTESIAN_POINT('Ctrl Pts',(9.70973094131579,109.002364951962,7.21892400700678));
#292049=CARTESIAN_POINT('Ctrl Pts',(7.54539904661067,108.878198378943,9.46223515898262));
#292050=CARTESIAN_POINT('Ctrl Pts',(6.24346505458509,108.814066835585,10.3675525596455));
#292051=CARTESIAN_POINT('Ctrl Pts',(3.37034905226605,108.690198148285,11.6227774571493));
#292052=CARTESIAN_POINT('Ctrl Pts',(1.82777399968561,108.630185010958,11.962752625575));
#292053=CARTESIAN_POINT('Ctrl Pts',(-1.28540795349743,108.504254155623,
12.0311231925084));
#292054=CARTESIAN_POINT('Ctrl Pts',(-2.82629089884275,108.44348471512,11.7648649134983));
#292055=CARTESIAN_POINT('Ctrl Pts',(-5.75448372048115,108.32112190543,10.6487816912335));
#292056=CARTESIAN_POINT('Ctrl Pts',(-7.1087191713167,108.256546002343,9.79676197411502));
#292057=CARTESIAN_POINT('Ctrl Pts',(-9.38336545307885,108.130807819236,
7.63918600453096));
#292058=CARTESIAN_POINT('Ctrl Pts',(-10.290979608285,108.072442298752,6.36399529241569));
#292059=CARTESIAN_POINT('Ctrl Pts',(-11.5749065627175,107.947350868096,
3.52959487641761));
#292060=CARTESIAN_POINT('Ctrl Pts',(-11.9354229698167,107.883830039254,
1.99560028495009));
#292061=CARTESIAN_POINT('Ctrl Pts',(-11.9973672522598,107.817453322316,
0.290358986012273));
#292062=CARTESIAN_POINT('Ctrl Pts',(-12.0000000000001,107.811833224361,
0.145127975993206));
#292063=CARTESIAN_POINT('Ctrl Pts',(-12.0000000000001,107.80624999958,3.19189119579733E-14));
#292064=CARTESIAN_POINT('Origin',(-8.79029313101884E-14,130.96875,0.));
#292065=CARTESIAN_POINT('',(-12.0000000000001,104.431249999592,-1.27681852051471E-13));
#292066=CARTESIAN_POINT('',(-12.0000000000001,104.806249999592,1.19342770927626E-13));
#292067=CARTESIAN_POINT('',(-12.0000000000001,130.96875,-1.46957615897682E-15));
#292068=CARTESIAN_POINT('Ctrl Pts',(-12.0000000000001,104.431249999592,
-3.8441472227646E-13));
#292069=CARTESIAN_POINT('Ctrl Pts',(-12.0000000000001,104.478870965931,
1.23783919338978));
#292070=CARTESIAN_POINT('Ctrl Pts',(-11.8084687407335,104.528670746041,
2.4700812688676));
#292071=CARTESIAN_POINT('Ctrl Pts',(-10.9524960498144,104.642422247347,
5.14876714220476));
#292072=CARTESIAN_POINT('Ctrl Pts',(-10.1852917659291,104.703348111406,
6.53656683948058));
#292073=CARTESIAN_POINT('Ctrl Pts',(-8.16248778483741,104.826563392885,
8.93466456822427));
#292074=CARTESIAN_POINT('Ctrl Pts',(-6.92757065129571,104.890472222916,
9.92285577526435));
#292075=CARTESIAN_POINT('Ctrl Pts',(-4.16474079504433,105.015057717378,
11.3600243563759));
#292076=CARTESIAN_POINT('Ctrl Pts',(-2.66648802844724,105.073388293074,
11.8019078210812));
#292077=CARTESIAN_POINT('Ctrl Pts',(0.457759258577007,105.199766750565,
12.096279340879));
#292078=CARTESIAN_POINT('Ctrl Pts',(2.05521741175009,105.264385290251,11.9292042769213));
#292079=CARTESIAN_POINT('Ctrl Pts',(5.05658115232668,105.385793003872,10.9929181357832));
#292080=CARTESIAN_POINT('Ctrl Pts',(6.4358250306347,105.448236295316,10.2466597324239));
#292081=CARTESIAN_POINT('Ctrl Pts',(8.83605220345876,105.573844849345,8.26738303399802));
#292082=CARTESIAN_POINT('Ctrl Pts',(9.83329452454308,105.632865363677,7.05207833591719));
#292083=CARTESIAN_POINT('Ctrl Pts',(11.3167954709383,105.757616045139,4.29138073074682));
#292084=CARTESIAN_POINT('Ctrl Pts',(11.7821299805779,105.82200091017,2.76898421521227));
#292085=CARTESIAN_POINT('Ctrl Pts',(12.094500037319,105.945452126676,-0.338459142171763));
#292086=CARTESIAN_POINT('Ctrl Pts',(11.9502904496381,106.004682712918,-1.89262718076547));
#292087=CARTESIAN_POINT('Ctrl Pts',(11.0714914325709,106.130964004916,-4.88959039396011));
#292088=CARTESIAN_POINT('Ctrl Pts',(10.3339629765012,106.192867469903,-6.3003952609892));
#292089=CARTESIAN_POINT('Ctrl Pts',(8.36424401652176,106.315461815542,-8.74544262989015));
#292090=CARTESIAN_POINT('Ctrl Pts',(7.15518653768962,106.379137687194,-9.75942872072018));
#292091=CARTESIAN_POINT('Ctrl Pts',(4.42843243854746,106.504052097933,-11.2600850432998));
#292092=CARTESIAN_POINT('Ctrl Pts',(2.93916954508338,106.562358094017,-11.7371975382882));
#292093=CARTESIAN_POINT('Ctrl Pts',(-0.175434345152722,106.688346467914,
-12.1031707379278));
#292094=CARTESIAN_POINT('Ctrl Pts',(-1.77248965636175,106.7529487123,-11.9739735782117));
#292095=CARTESIAN_POINT('Ctrl Pts',(-4.81797147125956,106.876141039515,
-11.1034148887432));
#292096=CARTESIAN_POINT('Ctrl Pts',(-6.23716913870021,106.938733989896,
-10.3728859618237));
#292097=CARTESIAN_POINT('Ctrl Pts',(-8.68365988620488,107.065104145652,
-8.42525379333561));
#292098=CARTESIAN_POINT('Ctrl Pts',(-9.6959044275387,107.12401750548,-7.23742505899842));
#292099=CARTESIAN_POINT('Ctrl Pts',(-11.2276591634751,107.247758596914,
-4.51864891526425));
#292100=CARTESIAN_POINT('Ctrl Pts',(-11.7230049203476,107.31205641737,-3.00826624484089));
#292101=CARTESIAN_POINT('Ctrl Pts',(-11.9709415925415,107.393768648943,
-0.96483267613689));
#292102=CARTESIAN_POINT('Ctrl Pts',(-12.0000000000001,107.41270083742,-0.482159050745271));
#292103=CARTESIAN_POINT('Ctrl Pts',(-12.0000000000001,107.43124999958,-2.77555756156289E-16));
#292104=CARTESIAN_POINT('Ctrl Pts',(-12.0000000000001,107.80624999958,-3.46944695195361E-14));
#292105=CARTESIAN_POINT('Ctrl Pts',(-12.0000000000001,107.751124737303,
-1.43290267791645));
#292106=CARTESIAN_POINT('Ctrl Pts',(-11.7433421899126,107.693187065922,
-2.85551674708468));
#292107=CARTESIAN_POINT('Ctrl Pts',(-10.6998000168058,107.572695216503,
-5.6484633501225));
#292108=CARTESIAN_POINT('Ctrl Pts',(-9.88373255926775,107.513770095995,
-6.97873356384564));
#292109=CARTESIAN_POINT('Ctrl Pts',(-7.77272003673247,107.390040611035,
-9.27704927235111));
#292110=CARTESIAN_POINT('Ctrl Pts',(-6.4898226139486,107.32573893502,-10.2157237852365));
#292111=CARTESIAN_POINT('Ctrl Pts',(-3.64807500368188,107.201303237798,
-11.5379711509711));
#292112=CARTESIAN_POINT('Ctrl Pts',(-2.11898203155151,107.141964623298,
-11.9139876813583));
#292113=CARTESIAN_POINT('Ctrl Pts',(0.989299535718332,107.016231992737,
-12.0594117922852));
#292114=CARTESIAN_POINT('Ctrl Pts',(2.53880322870443,106.954454867829,-11.8305601284356));
#292115=CARTESIAN_POINT('Ctrl Pts',(5.4990534278353,106.832683293425,-10.7834665636903));
#292116=CARTESIAN_POINT('Ctrl Pts',(6.87645816728897,106.768070055141,-9.96176637459719));
#292117=CARTESIAN_POINT('Ctrl Pts',(9.201821943112,106.641915764979,-7.85649621287418));
#292118=CARTESIAN_POINT('Ctrl Pts',(10.1378238393358,106.583618488968,-6.60474111275065));
#292119=CARTESIAN_POINT('Ctrl Pts',(11.4893568080365,106.458835346254,-3.80032072830849));
#292120=CARTESIAN_POINT('Ctrl Pts',(11.8864585551809,106.395058977097,-2.27157102790158));
#292121=CARTESIAN_POINT('Ctrl Pts',(12.0720896196125,106.27220278525,0.861585505856075));
#292122=CARTESIAN_POINT('Ctrl Pts',(11.8551147849263,106.210723377283,2.43600242799914));
#292123=CARTESIAN_POINT('Ctrl Pts',(10.8346985368866,106.08450475685,5.38532235547232));
#292124=CARTESIAN_POINT('Ctrl Pts',(10.0510979590871,106.025028943484,6.73556216159971));
#292125=CARTESIAN_POINT('Ctrl Pts',(7.99389367644074,105.901777922586,9.08781508319591));
#292126=CARTESIAN_POINT('Ctrl Pts',(6.73071709669543,105.837343197422,10.0592288540481));
#292127=CARTESIAN_POINT('Ctrl Pts',(3.92098548417948,105.712384132381,11.4475545198986));
#292128=CARTESIAN_POINT('Ctrl Pts',(2.40534971244001,105.653548439328,11.8589576328111));
#292129=CARTESIAN_POINT('Ctrl Pts',(-0.697680398376329,105.528028234643,
12.0802124876522));
#292130=CARTESIAN_POINT('Ctrl Pts',(-2.25552011584,105.46509677064,11.8882367252435));
#292131=CARTESIAN_POINT('Ctrl Pts',(-5.24627778918792,105.343945647858,
10.9092283541567));
#292132=CARTESIAN_POINT('Ctrl Pts',(-6.64570423226648,105.2793304235,10.1177549085152));
#292133=CARTESIAN_POINT('Ctrl Pts',(-9.02001057303937,105.152806623237,
8.06430737183463));
#292134=CARTESIAN_POINT('Ctrl Pts',(-9.98350661690994,105.094422794686,
6.83544294611026));
#292135=CARTESIAN_POINT('Ctrl Pts',(-11.4002871497796,104.969979671626,
4.0610611070136));
#292136=CARTESIAN_POINT('Ctrl Pts',(-11.8328494888336,104.905987249946,
2.53821727375672));
#292137=CARTESIAN_POINT('Ctrl Pts',(-11.9867964501751,104.831436008067,
0.650384324452592));
#292138=CARTESIAN_POINT('Ctrl Pts',(-12.0000000000001,104.818753455413,
0.325009525372273));
#292139=CARTESIAN_POINT('Ctrl Pts',(-12.0000000000001,104.806249999592,
4.41244263349461E-13));
#292140=CARTESIAN_POINT('Origin',(-8.79029313101884E-14,130.96875,0.));
#292141=CARTESIAN_POINT('',(-12.0000000000001,101.431249999604,-3.74068423616381E-14));
#292142=CARTESIAN_POINT('',(-12.0000000000001,101.806249999604,8.20462161941248E-14));
#292143=CARTESIAN_POINT('',(-12.0000000000001,130.96875,-1.46957615897682E-15));
#292144=CARTESIAN_POINT('Ctrl Pts',(-12.0000000000001,101.431249999604,
-2.08166817117217E-14));
#292145=CARTESIAN_POINT('Ctrl Pts',(-12.0000000000001,101.486480368325,
1.43563477022792));
#292146=CARTESIAN_POINT('Ctrl Pts',(-11.7423637223291,101.544523597783,
2.86067474786727));
#292147=CARTESIAN_POINT('Ctrl Pts',(-10.6913465639717,101.665674294721,
5.66831838384956));
#292148=CARTESIAN_POINT('Ctrl Pts',(-9.864509629537,101.725078834577,7.00900948680852));
#292149=CARTESIAN_POINT('Ctrl Pts',(-7.7347392825375,101.849454122691,9.30866876971111));
#292150=CARTESIAN_POINT('Ctrl Pts',(-6.44838210482864,101.913738856922,
10.2418687926062));
#292151=CARTESIAN_POINT('Ctrl Pts',(-3.61411194849174,102.037518624373,
11.5468205756838));
#292152=CARTESIAN_POINT('Ctrl Pts',(-2.09777054167503,102.096393398676,
11.9159637947213));
#292153=CARTESIAN_POINT('Ctrl Pts',(1.02655990456309,102.222775220028,12.0601440246069));
#292154=CARTESIAN_POINT('Ctrl Pts',(2.60518842577862,102.285467588493,11.8200466266539));
#292155=CARTESIAN_POINT('Ctrl Pts',(5.55881291589413,102.407598360007,10.7487262681341));
#292156=CARTESIAN_POINT('Ctrl Pts',(6.90806435611422,102.4710890811,9.93548776383274));
#292157=CARTESIAN_POINT('Ctrl Pts',(9.21236286066618,102.596211774256,7.84461115492276));
#292158=CARTESIAN_POINT('Ctrl Pts',(10.1480793037009,102.654594451917,6.58954141103041));
#292159=CARTESIAN_POINT('Ctrl Pts',(11.5042826036013,102.780284760786,3.76305801707942));
#292160=CARTESIAN_POINT('Ctrl Pts',(11.9000354126918,102.844854416412,2.2132496682374));
#292161=CARTESIAN_POINT('Ctrl Pts',(12.0648754059926,102.9672792705,-0.915450283366411));
#292162=CARTESIAN_POINT('Ctrl Pts',(11.8461129143289,103.027949013678,-2.46355219734727));
#292163=CARTESIAN_POINT('Ctrl Pts',(10.8268982536332,103.153900398374,-5.40631613185324));
#292164=CARTESIAN_POINT('Ctrl Pts',(10.0301736577837,103.213996901955,-6.77093711946924));
#292165=CARTESIAN_POINT('Ctrl Pts',(7.95445010979591,103.337801653831,-9.12098954731558));
#292166=CARTESIAN_POINT('Ctrl Pts',(6.69396284264352,103.401912566859,-10.0824857902304));
#292167=CARTESIAN_POINT('Ctrl Pts',(3.89557572687022,103.526123852328,-11.4549753373937));
#292168=CARTESIAN_POINT('Ctrl Pts',(2.3883726505594,103.584638296435,-11.8611803475485));
#292169=CARTESIAN_POINT('Ctrl Pts',(-0.739082770733267,103.711146525683,
-12.0821196279082));
#292170=CARTESIAN_POINT('Ctrl Pts',(-2.33026894912346,103.775086642228,
-11.8782593431249));
#292171=CARTESIAN_POINT('Ctrl Pts',(-5.31082446606679,103.896530727792,
-10.8728873364844));
#292172=CARTESIAN_POINT('Ctrl Pts',(-6.67531879768973,103.959732378726,
-10.0927867264592));
#292173=CARTESIAN_POINT('Ctrl Pts',(-9.02759927654267,104.085113094283,
-8.05709960715809));
#292174=CARTESIAN_POINT('Ctrl Pts',(-9.99393082580769,104.143735651335,
-6.82171458919567));
#292175=CARTESIAN_POINT('Ctrl Pts',(-11.4138370934978,104.268976015867,
-4.02762520637223));
#292176=CARTESIAN_POINT('Ctrl Pts',(-11.8444903102128,104.333470643599,
-2.49110693061898));
#292177=CARTESIAN_POINT('Ctrl Pts',(-11.9883717226644,104.407624235863,
-0.610339821600662));
#292178=CARTESIAN_POINT('Ctrl Pts',(-12.0000000000001,104.419516116535,
-0.305005577473783));
#292179=CARTESIAN_POINT('Ctrl Pts',(-12.0000000000001,104.431249999592,
-4.09186573513409E-13));
#292180=CARTESIAN_POINT('Ctrl Pts',(-12.0000000000001,104.806249999592,
4.56856774633252E-13));
#292181=CARTESIAN_POINT('Ctrl Pts',(-12.0000000000001,104.758601490836,
-1.23855511927143));
#292182=CARTESIAN_POINT('Ctrl Pts',(-11.8082468123864,104.708767224827,
-2.47162149771696));
#292183=CARTESIAN_POINT('Ctrl Pts',(-10.9583504590709,104.595896362933,
-5.12939072557227));
#292184=CARTESIAN_POINT('Ctrl Pts',(-10.2060230595981,104.535730732699,
-6.49869718555533));
#292185=CARTESIAN_POINT('Ctrl Pts',(-8.20109956593658,104.412978757805,
-8.90191931904317));
#292186=CARTESIAN_POINT('Ctrl Pts',(-6.95754137383397,104.348450357766,
-9.90427530766931));
#292187=CARTESIAN_POINT('Ctrl Pts',(-4.17924700902458,104.223027513568,
-11.3553764834465));
#292188=CARTESIAN_POINT('Ctrl Pts',(-2.67654250396623,104.164518418188,
-11.8002868100017));
#292189=CARTESIAN_POINT('Ctrl Pts',(0.420634824484783,104.039234963523,
-12.0934553377146));
#292190=CARTESIAN_POINT('Ctrl Pts',(1.98599508233998,103.975914810977,-11.9366957236708));
#292191=CARTESIAN_POINT('Ctrl Pts',(4.99510223067139,103.854193869933,-11.0255561725828));
#292192=CARTESIAN_POINT('Ctrl Pts',(6.40669019810106,103.790767354196,-10.2698003364113));
#292193=CARTESIAN_POINT('Ctrl Pts',(8.8239865738571,103.664307010339,-8.27819238721138));
#292194=CARTESIAN_POINT('Ctrl Pts',(9.81620057244571,103.605669864452,-7.07343347616651));
#292195=CARTESIAN_POINT('Ctrl Pts',(11.3008354362689,103.481625073801,-4.33145292931322));
#292196=CARTESIAN_POINT('Ctrl Pts',(11.7704103186201,103.4174406109,-2.81564336233957));
#292197=CARTESIAN_POINT('Ctrl Pts',(12.097616008431,103.293403808774,0.30220106981476));
#292198=CARTESIAN_POINT('Ctrl Pts',(11.9554270961315,103.233603145005,1.87386889975548));
#292199=CARTESIAN_POINT('Ctrl Pts',(11.0801151872735,103.10772795905,4.86140899493031));
#292200=CARTESIAN_POINT('Ctrl Pts',(10.3602688336532,103.046683455066,6.25034332769341));
#292201=CARTESIAN_POINT('Ctrl Pts',(8.41005808803819,102.924488069061,8.70546181073995));
#292202=CARTESIAN_POINT('Ctrl Pts',(7.18748045059645,102.859897634335,9.7393041406602));
#292203=CARTESIAN_POINT('Ctrl Pts',(4.44241821737085,102.734034473329,11.2546644811422));
#292204=CARTESIAN_POINT('Ctrl Pts',(2.95309570322389,102.675705230097,11.733787715922));
#292205=CARTESIAN_POINT('Ctrl Pts',(-0.137221574066131,102.55069927033,
12.1004522758571));
#292206=CARTESIAN_POINT('Ctrl Pts',(-1.70946979472838,102.487100493836,
11.9798876915772));
#292207=CARTESIAN_POINT('Ctrl Pts',(-4.73533018511225,102.364701869915,
11.1386076462919));
#292208=CARTESIAN_POINT('Ctrl Pts',(-6.15800372262147,102.302471030129,
10.4197516925769));
#292209=CARTESIAN_POINT('Ctrl Pts',(-8.61792563958917,102.176145716897,
8.49249195173133));
#292210=CARTESIAN_POINT('Ctrl Pts',(-9.63941404855684,102.1170771611,7.31250848129084));
#292211=CARTESIAN_POINT('Ctrl Pts',(-11.1928508050391,101.993483328734,
4.60460504283106));
#292212=CARTESIAN_POINT('Ctrl Pts',(-11.7000709570479,101.929138946295,
3.09687028481685));
#292213=CARTESIAN_POINT('Ctrl Pts',(-11.9672392841743,101.846070331329,
1.02442820521571));
#292214=CARTESIAN_POINT('Ctrl Pts',(-12.0000000000001,101.825945438085,
0.511954871078143));
#292215=CARTESIAN_POINT('Ctrl Pts',(-12.0000000000001,101.806249999604,
3.75394160201381E-13));
#292216=CARTESIAN_POINT('Origin',(-8.79029313101884E-14,130.96875,0.));
#292217=CARTESIAN_POINT('',(-12.0000000000001,98.431249999616,-7.39612622723935E-15));
#292218=CARTESIAN_POINT('',(-12.0000000000001,98.806249999616,-1.70623322603542E-15));
#292219=CARTESIAN_POINT('',(-12.0000000000001,130.96875,-1.46957615897682E-15));
#292220=CARTESIAN_POINT('Ctrl Pts',(-12.0000000000001,98.431249999616,2.73285667600019E-15));
#292221=CARTESIAN_POINT('Ctrl Pts',(-12.0000000000001,98.4339838995247,
0.0710638342315633));
#292222=CARTESIAN_POINT('Ctrl Pts',(-11.999368742607,98.4367267560416,0.142155374774367));
#292223=CARTESIAN_POINT('Ctrl Pts',(-11.970413553221,98.499757391063,1.77113884620319));
#292224=CARTESIAN_POINT('Ctrl Pts',(-11.6395687683053,98.5630467688966,
3.30875809283163));
#292225=CARTESIAN_POINT('Ctrl Pts',(-10.4107184215545,98.6883565337207,
6.16672926919503));
#292226=CARTESIAN_POINT('Ctrl Pts',(-9.52617270723465,98.746893233943,7.4608093385413));
#292227=CARTESIAN_POINT('Ctrl Pts',(-7.29284135606745,98.872268443788,9.6599843247105));
#292228=CARTESIAN_POINT('Ctrl Pts',(-5.95772174749821,98.9367884426156,
10.5359634928269));
#292229=CARTESIAN_POINT('Ctrl Pts',(-3.05596584100162,99.0595954362412,
11.7071157123083));
#292230=CARTESIAN_POINT('Ctrl Pts',(-1.52209266533542,99.1196800579496,
12.0032840633594));
#292231=CARTESIAN_POINT('Ctrl Pts',(1.59469019289135,99.2457565729532,11.9966155425732));
#292232=CARTESIAN_POINT('Ctrl Pts',(3.14791120094077,99.3064259324189,11.6855641658905));
#292233=CARTESIAN_POINT('Ctrl Pts',(6.04530459772022,99.4298158168412,10.4838919607646));
#292234=CARTESIAN_POINT('Ctrl Pts',(7.36175649343294,99.4937866150215,9.60531743954377));
#292235=CARTESIAN_POINT('Ctrl Pts',(9.56779607296812,99.6182680624296,7.40616884991388));
#292236=CARTESIAN_POINT('Ctrl Pts',(10.4420261374425,99.676635375023,6.11212812404449));
#292237=CARTESIAN_POINT('Ctrl Pts',(11.6682109103662,99.803121251764,3.22271949610166));
#292238=CARTESIAN_POINT('Ctrl Pts',(11.9923361918725,99.8677379023339,1.64841638612066));
#292239=CARTESIAN_POINT('Ctrl Pts',(12.0072192913573,99.9889576944574,-1.49768364446297));
#292240=CARTESIAN_POINT('Ctrl Pts',(11.7124578522839,100.051757106291,-3.03898249246358));
#292241=CARTESIAN_POINT('Ctrl Pts',(10.5507336771395,100.177301021367,-5.92485068641402));
#292242=CARTESIAN_POINT('Ctrl Pts',(9.69428116035566,100.236183130822,-7.24174002038604));
#292243=CARTESIAN_POINT('Ctrl Pts',(7.5113436058091,100.361087484542,-9.49047261996084));
#292244=CARTESIAN_POINT('Ctrl Pts',(6.19980993931202,100.425509546752,-10.3947959861688));
#292245=CARTESIAN_POINT('Ctrl Pts',(3.33067993774254,100.548814456576,-11.6317955142732));
#292246=CARTESIAN_POINT('Ctrl Pts',(1.80534352002713,100.608222320188,-11.9638139311181));
#292247=CARTESIAN_POINT('Ctrl Pts',(-1.31537176120697,100.734457905044,
-12.0312005576569));
#292248=CARTESIAN_POINT('Ctrl Pts',(-2.88118079495719,100.796047579945,
-11.7549390802658));
#292249=CARTESIAN_POINT('Ctrl Pts',(-5.80673038534638,100.918834693939,
-10.6173721643633));
#292250=CARTESIAN_POINT('Ctrl Pts',(-7.13975940039004,100.982584856503,
-9.77089369112507));
#292251=CARTESIAN_POINT('Ctrl Pts',(-9.39469398919182,101.107403640946,
-7.62485542228049));
#292252=CARTESIAN_POINT('Ctrl Pts',(-10.2993311285907,101.165700631305,
-6.34999679352737));
#292253=CARTESIAN_POINT('Ctrl Pts',(-11.5901541926833,101.291811339783,
-3.49134238417836));
#292254=CARTESIAN_POINT('Ctrl Pts',(-11.9499467466854,101.356422234309,
-1.92877789368869));
#292255=CARTESIAN_POINT('Ctrl Pts',(-11.9983815360636,101.422472161457,
-0.227641529534562));
#292256=CARTESIAN_POINT('Ctrl Pts',(-12.0000000000001,101.42687244655,-0.113788256692766));
#292257=CARTESIAN_POINT('Ctrl Pts',(-12.0000000000001,101.431249999604,
1.59594559789866E-14));
#292258=CARTESIAN_POINT('Ctrl Pts',(-12.0000000000001,101.806249999604,
4.54081217071689E-13));
#292259=CARTESIAN_POINT('Ctrl Pts',(-12.0000000000001,101.766230467423,
-1.04025073916514));
#292260=CARTESIAN_POINT('Ctrl Pts',(-11.8647387182924,101.724607547189,
-2.07823021252408));
#292261=CARTESIAN_POINT('Ctrl Pts',(-11.1964684722288,101.619699777096,
-4.58802411045548));
#292262=CARTESIAN_POINT('Ctrl Pts',(-10.5095366854714,101.557599891377,
-5.99666408431447));
#292263=CARTESIAN_POINT('Ctrl Pts',(-8.6151392416733,101.436006797544,-8.50327148822433));
#292264=CARTESIAN_POINT('Ctrl Pts',(-7.41440413156253,101.371389422096,
-9.56831056394794));
#292265=CARTESIAN_POINT('Ctrl Pts',(-4.70357623074547,101.245122398749,
-11.1477762603995));
#292266=CARTESIAN_POINT('Ctrl Pts',(-3.22775165344605,101.186815296669,
-11.6609686402055));
#292267=CARTESIAN_POINT('Ctrl Pts',(-0.145323019961658,101.062128439248,
-12.1008215457449));
#292268=CARTESIAN_POINT('Ctrl Pts',(1.43297481961014,100.998284950528,-12.0165610469654));
#292269=CARTESIAN_POINT('Ctrl Pts',(4.47459070255941,100.875249003546,-11.2450105826866));
#292270=CARTESIAN_POINT('Ctrl Pts',(5.90794163155401,100.814050914446,-10.562603188016));
#292271=CARTESIAN_POINT('Ctrl Pts',(8.40949900348915,100.687877932815,-8.69905657155727));
#292272=CARTESIAN_POINT('Ctrl Pts',(9.45975726268865,100.628213979255,-7.54362017860402));
#292273=CARTESIAN_POINT('Ctrl Pts',(11.0803977678472,100.505106926566,-4.87020570611372));
#292274=CARTESIAN_POINT('Ctrl Pts',(11.6244761419959,100.440640950313,-3.371286252466));
#292275=CARTESIAN_POINT('Ctrl Pts',(12.0972265307051,100.315540412315,-0.273081860755084));
#292276=CARTESIAN_POINT('Ctrl Pts',(12.030816350728,100.256817412875,1.29494252459816));
#292277=CARTESIAN_POINT('Ctrl Pts',(11.3032575658423,100.131368363954,4.31941369468196));
#292278=CARTESIAN_POINT('Ctrl Pts',(10.6485546742428,100.068258588068,5.7471365668539));
#292279=CARTESIAN_POINT('Ctrl Pts',(8.81030383113319,99.947025338931,8.30113829994723));
#292280=CARTESIAN_POINT('Ctrl Pts',(7.63347054879219,99.8826852300756,9.39474500493053));
#292281=CARTESIAN_POINT('Ctrl Pts',(4.95929109759016,99.7561432023647,11.0362192328815));
#292282=CARTESIAN_POINT('Ctrl Pts',(3.49690740949452,99.6977028757142,11.5829351373832));
#292283=CARTESIAN_POINT('Ctrl Pts',(0.423259818640735,99.5733712189287,
12.0947502380544));
#292284=CARTESIAN_POINT('Ctrl Pts',(-1.16019061442988,99.5093193034237,
12.046417704419));
#292285=CARTESIAN_POINT('Ctrl Pts',(-4.21639957800431,99.3856930539296,
11.3435862127409));
#292286=CARTESIAN_POINT('Ctrl Pts',(-5.65992487123753,99.3253566684579,
10.696740333296));
#292287=CARTESIAN_POINT('Ctrl Pts',(-8.20168150789831,99.1993497667033,
8.89550832667992));
#292288=CARTESIAN_POINT('Ctrl Pts',(-9.27988138373904,99.1389446082995,
7.76410238086659));
#292289=CARTESIAN_POINT('Ctrl Pts',(-10.9653551504483,99.0163510890256,
5.12510208173164));
#292290=CARTESIAN_POINT('Ctrl Pts',(-11.5450497092688,98.951800902559,3.63556610340489));
#292291=CARTESIAN_POINT('Ctrl Pts',(-11.9397038585928,98.8604536395862,
1.38935501476442));
#292292=CARTESIAN_POINT('Ctrl Pts',(-12.0000000000001,98.8329699508869,
0.694547076025101));
#292293=CARTESIAN_POINT('Ctrl Pts',(-12.0000000000001,98.806249999616,1.94289029309402E-15));
#292294=CARTESIAN_POINT('Origin',(-8.79029313101884E-14,130.96875,0.));
#292295=CARTESIAN_POINT('',(-12.0000000000001,95.431249999628,6.27560911412627E-14));
#292296=CARTESIAN_POINT('',(-12.0000000000001,95.806249999628,-2.51596946212419E-14));
#292297=CARTESIAN_POINT('',(-12.0000000000001,130.96875,-1.46957615897682E-15));
#292298=CARTESIAN_POINT('Ctrl Pts',(-12.0000000000001,95.431249999628,-8.60422844084496E-15));
#292299=CARTESIAN_POINT('Ctrl Pts',(-12.0000000000001,95.4409906235063,
0.253193644134754));
#292300=CARTESIAN_POINT('Ctrl Pts',(-11.9919867672329,95.4508413495118,
0.506645579091207));
#292301=CARTESIAN_POINT('Ctrl Pts',(-11.8767809487482,95.5221231903685,
2.32208286579897));
#292302=CARTESIAN_POINT('Ctrl Pts',(-11.4729702276523,95.5859428304934,
3.84977745561648));
#292303=CARTESIAN_POINT('Ctrl Pts',(-10.1090728697394,95.7106647582825,
6.6485892116695));
#292304=CARTESIAN_POINT('Ctrl Pts',(-9.16786888107841,95.7689668056092,
7.89602750012452));
#292305=CARTESIAN_POINT('Ctrl Pts',(-6.83322973383029,95.8951935824947,
9.99157989034653));
#292306=CARTESIAN_POINT('Ctrl Pts',(-5.45162528538409,95.9598098091461,
10.8076253621462));
#292307=CARTESIAN_POINT('Ctrl Pts',(-2.48556070131359,96.0814676265569,
11.8419316653302));
#292308=CARTESIAN_POINT('Ctrl Pts',(-0.934478472913705,96.1434495513518,
12.063855455804));
#292309=CARTESIAN_POINT('Ctrl Pts',(2.17284804789866,96.2691435494718,11.9041750318455));
#292310=CARTESIAN_POINT('Ctrl Pts',(3.6994249245477,96.3283753205453,11.5214995860526));
#292311=CARTESIAN_POINT('Ctrl Pts',(6.53524039790862,96.4529120720883,10.1868371422895));
#292312=CARTESIAN_POINT('Ctrl Pts',(7.81450496390696,96.5172414001135,9.24199942925195));
#292313=CARTESIAN_POINT('Ctrl Pts',(9.91550239210979,96.640884615364,6.93352749959648));
#292314=CARTESIAN_POINT('Ctrl Pts',(10.7255035305225,96.6998997042907,5.59951240890465));
#292315=CARTESIAN_POINT('Ctrl Pts',(11.8060931249998,96.8262401279026,2.66657788672909));
#292316=CARTESIAN_POINT('Ctrl Pts',(12.0541788218455,96.8885895765476,1.09129317018687));
#292317=CARTESIAN_POINT('Ctrl Pts',(11.9267881891096,97.0109185137701,-2.0470815939593));
#292318=CARTESIAN_POINT('Ctrl Pts',(11.5594557310219,97.0744894536273,-3.58016408067849));
#292319=CARTESIAN_POINT('Ctrl Pts',(10.2629091491639,97.1995267154807,-6.40905609030048));
#292320=CARTESIAN_POINT('Ctrl Pts',(9.35000251967587,97.2578675135338,-7.67989349432511));
#292321=CARTESIAN_POINT('Ctrl Pts',(7.06588919238247,97.3836858653614,-9.82781096885908));
#292322=CARTESIAN_POINT('Ctrl Pts',(5.70730328442144,97.448271393592,-10.6742476144214));
#292323=CARTESIAN_POINT('Ctrl Pts',(2.77309298937273,97.5705277384726,-11.7775707460928));
#292324=CARTESIAN_POINT('Ctrl Pts',(1.23060221857106,97.6314710942121,-12.036905859078));
#292325=CARTESIAN_POINT('Ctrl Pts',(-1.88170570409498,97.7573665942699,
-11.9542646404877));
#292326=CARTESIAN_POINT('Ctrl Pts',(-3.42179911890718,97.8172425508346,
-11.6076079183399));
#292327=CARTESIAN_POINT('Ctrl Pts',(-6.28919379484739,97.9412188725106,
-10.3399813514453));
#292328=CARTESIAN_POINT('Ctrl Pts',(-7.58767823178803,98.0053845234396,
-9.42848153263456));
#292329=CARTESIAN_POINT('Ctrl Pts',(-9.74223853888837,98.1294738432075,
-7.17497009917505));
#292330=CARTESIAN_POINT('Ctrl Pts',(-10.5848186442503,98.1880760149103,
-5.86114108318552));
#292331=CARTESIAN_POINT('Ctrl Pts',(-11.7134943203517,98.3116777809989,
-3.01501817768779));
#292332=CARTESIAN_POINT('Ctrl Pts',(-12.0000000000001,98.3730074168523,
-1.5139329839569));
#292333=CARTESIAN_POINT('Ctrl Pts',(-12.0000000000001,98.431249999616,-3.80251385934116E-14));
#292334=CARTESIAN_POINT('Ctrl Pts',(-12.0000000000001,98.806249999616,-7.21644966006352E-15));
#292335=CARTESIAN_POINT('Ctrl Pts',(-12.0000000000001,98.7735434882751,
-0.850159178381908));
#292336=CARTESIAN_POINT('Ctrl Pts',(-11.909658234483,98.7397261048303,-1.69984007587557));
#292337=CARTESIAN_POINT('Ctrl Pts',(-11.3998801877238,98.6425987099933,
-4.05889143789282));
#292338=CARTESIAN_POINT('Ctrl Pts',(-10.776497725326,98.5791933670716,-5.50447377851174));
#292339=CARTESIAN_POINT('Ctrl Pts',(-8.99802596747649,98.457269553505,-8.09584915261635));
#292340=CARTESIAN_POINT('Ctrl Pts',(-7.85236943941162,98.3942105106125,
-9.21129759630602));
#292341=CARTESIAN_POINT('Ctrl Pts',(-5.22536157044818,98.2677878683712,
-10.9126767647559));
#292342=CARTESIAN_POINT('Ctrl Pts',(-3.77721877718979,98.2090417087292,
-11.4945021231782));
#292343=CARTESIAN_POINT('Ctrl Pts',(-0.713835593063138,98.0851252559177,
-12.0815691625026));
#292344=CARTESIAN_POINT('Ctrl Pts',(0.87415130039543,98.0208898367353,-12.0710295258403));
#292345=CARTESIAN_POINT('Ctrl Pts',(3.94467066967295,97.8966847191707,-11.4402247482499));
#292346=CARTESIAN_POINT('Ctrl Pts',(5.39851955746572,97.8370865391971,-10.8302874243549));
#292347=CARTESIAN_POINT('Ctrl Pts',(7.98157939540233,97.7112696433552,-9.09389575881817));
#292348=CARTESIAN_POINT('Ctrl Pts',(9.08865504458853,97.6499302204276,-7.98752451712976));
#292349=CARTESIAN_POINT('Ctrl Pts',(10.8406367502923,97.5279089383564,-5.38500844837757));
#292350=CARTESIAN_POINT('Ctrl Pts',(11.4569020000997,97.46330681163,-3.90600489478107));
#292351=CARTESIAN_POINT('Ctrl Pts',(12.071059380927,97.3373198579925,-0.830705307969824));
#292352=CARTESIAN_POINT('Ctrl Pts',(12.0773796214608,97.2790136755807,0.73311161381929));
#292353=CARTESIAN_POINT('Ctrl Pts',(11.4925352314639,97.1540981915476,3.79008424243644));
#292354=CARTESIAN_POINT('Ctrl Pts',(10.9016839261066,97.0904231884907,5.25324602785943));
#292355=CARTESIAN_POINT('Ctrl Pts',(9.18477025462278,96.9678310714679,7.88199443316276));
#292356=CARTESIAN_POINT('Ctrl Pts',(8.07081539852554,96.9059239276573,9.01931404370743));
#292357=CARTESIAN_POINT('Ctrl Pts',(5.49193281263632,96.7796421210471,10.7810086478598));
#292358=CARTESIAN_POINT('Ctrl Pts',(4.0583444278431,96.7204134801818,11.3983034025011));
#292359=CARTESIAN_POINT('Ctrl Pts',(1.0064215525226,96.5969606065995,12.0612161585608));
#292360=CARTESIAN_POINT('Ctrl Pts',(-0.585248825613923,96.532576187332,
12.0889723081148));
#292361=CARTESIAN_POINT('Ctrl Pts',(-3.66921114597413,96.4078272909733,
11.5309332747356));
#292362=CARTESIAN_POINT('Ctrl Pts',(-5.13316546952277,96.3488051013711,
10.9579238728703));
#292363=CARTESIAN_POINT('Ctrl Pts',(-7.75714219069866,96.2231958129574,
9.28658112039682));
#292364=CARTESIAN_POINT('Ctrl Pts',(-8.89298840814305,96.1607565336721,
8.20536316575725));
#292365=CARTESIAN_POINT('Ctrl Pts',(-10.7107000481564,96.0393466788323,
5.64009722731743));
#292366=CARTESIAN_POINT('Ctrl Pts',(-11.3631176146055,95.9747281350808,
4.17241353627881));
#292367=CARTESIAN_POINT('Ctrl Pts',(-11.9033212497446,95.8750998425117,
1.75824077268344));
#292368=CARTESIAN_POINT('Ctrl Pts',(-12.0000000000001,95.8400841254468,
0.87946991067202));
#292369=CARTESIAN_POINT('Ctrl Pts',(-12.0000000000001,95.806249999628,1.83186799063151E-14));
#292370=CARTESIAN_POINT('Origin',(-8.79029313101884E-14,130.96875,0.));
#292371=CARTESIAN_POINT('',(-12.0000000000001,92.43124999964,6.31640258511681E-16));
#292372=CARTESIAN_POINT('',(-12.0000000000001,92.80624999964,-6.20746101900283E-14));
#292373=CARTESIAN_POINT('',(-12.0000000000001,130.96875,-1.46957615897682E-15));
#292374=CARTESIAN_POINT('Ctrl Pts',(-12.0000000000001,92.43124999964,-1.42941214420489E-14));
#292375=CARTESIAN_POINT('Ctrl Pts',(-12.0000000000001,92.4479877578223,
0.435074184339853));
#292376=CARTESIAN_POINT('Ctrl Pts',(-11.9763397243295,92.4650400989585,
0.870637814920657));
#292377=CARTESIAN_POINT('Ctrl Pts',(-11.7578816109529,92.5446073612302,
2.86789412608426));
#292378=CARTESIAN_POINT('Ctrl Pts',(-11.2813220363684,92.60882420549,4.38227593627422));
#292379=CARTESIAN_POINT('Ctrl Pts',(-9.7839069954388,92.7327888285159,7.11802010863116));
#292380=CARTESIAN_POINT('Ctrl Pts',(-8.78626776826647,92.7914926820686,
8.31820295371068));
#292381=CARTESIAN_POINT('Ctrl Pts',(-6.36105190107423,92.9179295500625,
10.2979232987543));
#292382=CARTESIAN_POINT('Ctrl Pts',(-4.94739221745984,92.9811237805496,
11.0468557946528));
#292383=CARTESIAN_POINT('Ctrl Pts',(-1.93512718985598,93.1029724604937,
11.9451331339142));
#292384=CARTESIAN_POINT('Ctrl Pts',(-0.368436712215726,93.1663464215603,
12.095243007058));
#292385=CARTESIAN_POINT('Ctrl Pts',(2.72755667704737,93.2915819848791,11.7885297563894));
#292386=CARTESIAN_POINT('Ctrl Pts',(4.2278077709974,93.3500461678424,11.3373130914935));
#292387=CARTESIAN_POINT('Ctrl Pts',(7.00006279564588,93.4755527368303,9.87437813894915));
#292388=CARTESIAN_POINT('Ctrl Pts',(8.2398257586959,93.5400951580834,8.86620875460888));
#292389=CARTESIAN_POINT('Ctrl Pts',(10.2347651696407,93.6627481361002,6.4534083692514));
#292390=CARTESIAN_POINT('Ctrl Pts',(10.9811476841064,93.7230623550284,5.08049611460835));
#292391=CARTESIAN_POINT('Ctrl Pts',(11.9168157767857,93.8490887220024,2.10863719708276));
#292392=CARTESIAN_POINT('Ctrl Pts',(12.0900709513035,93.9095144585482,0.535718606429136));
#292393=CARTESIAN_POINT('Ctrl Pts',(11.8219379208979,94.0330760816248,-2.58896809368176));
#292394=CARTESIAN_POINT('Ctrl Pts',(11.3826137977506,94.0971061475619,-4.11059339897155));
#292395=CARTESIAN_POINT('Ctrl Pts',(9.95341939221315,94.2214798181759,-6.87913640890142));
#292396=CARTESIAN_POINT('Ctrl Pts',(8.98467968699075,94.2798974166537,-8.10361418915103));
#292397=CARTESIAN_POINT('Ctrl Pts',(6.60175557235523,94.4064510604421,-10.1464555512627));
#292398=CARTESIAN_POINT('Ctrl Pts',(5.19922467694068,94.4709369435709,-10.9316516553147));
#292399=CARTESIAN_POINT('Ctrl Pts',(2.20405011418617,94.5920942996898,-11.8979958893954));
#292400=CARTESIAN_POINT('Ctrl Pts',(0.644716337823207,94.6551706759385,
-12.083217628931));
#292401=CARTESIAN_POINT('Ctrl Pts',(-2.45713397727001,94.7806431568839,
-11.8482499914944));
#292402=CARTESIAN_POINT('Ctrl Pts',(-3.97031478326955,94.8394051439292,
-11.4304497851616));
#292403=CARTESIAN_POINT('Ctrl Pts',(-6.77412900177955,94.964455180782,-10.0301533882426));
#292404=CARTESIAN_POINT('Ctrl Pts',(-8.03363115892578,95.028910254409,-9.05282638295034));
#292405=CARTESIAN_POINT('Ctrl Pts',(-10.0809540083812,95.1520694815291,
-6.6908335429643));
#292406=CARTESIAN_POINT('Ctrl Pts',(-10.8586243610838,95.2116641683148,
-5.33696550272215));
#292407=CARTESIAN_POINT('Ctrl Pts',(-11.7836034241284,95.3275863308543,
-2.6242779117785));
#292408=CARTESIAN_POINT('Ctrl Pts',(-12.0000000000001,95.3806324966463,
-1.31572989543491));
#292409=CARTESIAN_POINT('Ctrl Pts',(-12.0000000000001,95.431249999628,1.11022302462516E-15));
#292410=CARTESIAN_POINT('Ctrl Pts',(-12.0000000000001,95.806249999628,-3.30291349825984E-14));
#292411=CARTESIAN_POINT('Ctrl Pts',(-12.0000000000001,95.780812263331,-0.661217724041314));
#292412=CARTESIAN_POINT('Ctrl Pts',(-11.9453518514414,95.7546782580322,
-1.3227777092535));
#292413=CARTESIAN_POINT('Ctrl Pts',(-11.5776573376204,95.6654340297677,
-3.52308312258341));
#292414=CARTESIAN_POINT('Ctrl Pts',(-11.019331674726,95.601525930069,-5.00287214507789));
#292415=CARTESIAN_POINT('Ctrl Pts',(-9.36347959868558,95.4783126788969,
-7.66760616295407));
#292416=CARTESIAN_POINT('Ctrl Pts',(-8.28057849027473,95.4173837817315,
-8.82604402484954));
#292417=CARTESIAN_POINT('Ctrl Pts',(-5.74899845438352,95.2912579992088,
-10.6462828662507));
#292418=CARTESIAN_POINT('Ctrl Pts',(-4.32974559250291,95.2313918879129,
-11.2981215440558));
#292419=CARTESIAN_POINT('Ctrl Pts',(-1.29001781704521,95.1084323164824,
-12.0346740357956));
#292420=CARTESIAN_POINT('Ctrl Pts',(0.30436940379332,95.0439379986191,-12.0997835588058));
#292421=CARTESIAN_POINT('Ctrl Pts',(3.40044253566307,94.9186992096441,-11.6125564471109));
#292422=CARTESIAN_POINT('Ctrl Pts',(4.87394485420319,94.8600755841093,-11.075156778205));
#292423=CARTESIAN_POINT('Ctrl Pts',(7.53676439822538,94.7346940694898,-9.46685640644819));
#292424=CARTESIAN_POINT('Ctrl Pts',(8.70024479373768,94.6714934487501,-8.41012717739552));
#292425=CARTESIAN_POINT('Ctrl Pts',(10.5772679268381,94.5500517449144,-5.88597332086489));
#292426=CARTESIAN_POINT('Ctrl Pts',(11.2627500519815,94.4861071516647,-4.43558346711482));
#292427=CARTESIAN_POINT('Ctrl Pts',(12.0188163963501,94.3595985278966,-1.39283282560082));
#292428=CARTESIAN_POINT('Ctrl Pts',(12.0981145963205,94.3010850127693,0.16613584188054));
#292429=CARTESIAN_POINT('Ctrl Pts',(11.6572931019273,94.1768723370203,3.25163584565223));
#292430=CARTESIAN_POINT('Ctrl Pts',(11.1322499388105,94.1127620762655,4.74749389657754));
#292431=CARTESIAN_POINT('Ctrl Pts',(9.53843214039509,93.9889593322919,7.44770709885618));
#292432=CARTESIAN_POINT('Ctrl Pts',(8.48669257446584,93.928860188331,8.62705540376232));
#292433=CARTESIAN_POINT('Ctrl Pts',(6.00274500242889,93.8029081645055,10.5055466789873));
#292434=CARTESIAN_POINT('Ctrl Pts',(4.59796298894832,93.7422415095144,11.1918712782594));
#292435=CARTESIAN_POINT('Ctrl Pts',(1.57140633397644,93.6198147210993,12.0016647936709));
#292436=CARTESIAN_POINT('Ctrl Pts',(-0.0248383326823098,93.5552452679742,
12.1040681564932));
#292437=CARTESIAN_POINT('Ctrl Pts',(-3.13203640672852,93.4295564656351,
11.687426784496));
#292438=CARTESIAN_POINT('Ctrl Pts',(-4.61479899631361,93.371173219743,11.1852228902824));
#292439=CARTESIAN_POINT('Ctrl Pts',(-7.31527872105174,93.2460495556566,
9.63960211418373));
#292440=CARTESIAN_POINT('Ctrl Pts',(-8.5055637399146,93.1825597841818,8.60760504109358));
#292441=CARTESIAN_POINT('Ctrl Pts',(-10.4369820617429,93.0604313361305,
6.12943631487414));
#292442=CARTESIAN_POINT('Ctrl Pts',(-11.1530457820141,92.9977348986901,
4.70218511139591));
#292443=CARTESIAN_POINT('Ctrl Pts',(-11.8565225469263,92.8903720861421,
2.14001517296361));
#292444=CARTESIAN_POINT('Ctrl Pts',(-12.0000000000001,92.8474669725009,
1.07137650413103));
#292445=CARTESIAN_POINT('Ctrl Pts',(-12.0000000000001,92.80624999964,-2.63677968348475E-14));
#292446=CARTESIAN_POINT('Origin',(-8.79029313101884E-14,130.96875,0.));
#292447=CARTESIAN_POINT('',(-12.,56.4312499997839,-1.48567922702232E-13));
#292448=CARTESIAN_POINT('',(-12.,56.806249999784,-3.42843401048799E-14));
#292449=CARTESIAN_POINT('',(-12.0000000000001,130.96875,-1.46957615897682E-15));
#292450=CARTESIAN_POINT('',(9.41568944744514,58.25,-7.43940805637581));
#292451=CARTESIAN_POINT('Ctrl Pts',(-12.,56.4312499997839,-2.08444372873373E-13));
#292452=CARTESIAN_POINT('Ctrl Pts',(-12.0000000000001,56.4796005831921,
1.25680454989647));
#292453=CARTESIAN_POINT('Ctrl Pts',(-11.8025538465919,56.5301936043954,
2.5077439321711));
#292454=CARTESIAN_POINT('Ctrl Pts',(-10.9351216314112,56.643788730521,5.17864163026471));
#292455=CARTESIAN_POINT('Ctrl Pts',(-10.1767968959666,56.7038100819498,
6.54430442895148));
#292456=CARTESIAN_POINT('Ctrl Pts',(-8.16181553223068,56.8266606028225,
8.93782778686641));
#292457=CARTESIAN_POINT('Ctrl Pts',(-6.91444955693021,56.8911736378425,
9.93429658204381));
#292458=CARTESIAN_POINT('Ctrl Pts',(-4.13008267255682,57.0165105871442,
11.3734270421349));
#292459=CARTESIAN_POINT('Ctrl Pts',(-2.62490142548079,57.0750705066934,
11.8119550341771));
#292460=CARTESIAN_POINT('Ctrl Pts',(0.47343692183443,57.200400925558,12.0914175547538));
#292461=CARTESIAN_POINT('Ctrl Pts',(2.03742327080079,57.2636655023219,11.9279388370427));
#292462=CARTESIAN_POINT('Ctrl Pts',(5.04330248025586,57.3852558704958,11.0037895935951));
#292463=CARTESIAN_POINT('Ctrl Pts',(6.45278041867523,57.4489229198579,10.2411184393772));
#292464=CARTESIAN_POINT('Ctrl Pts',(8.86203277851051,57.5754063519648,8.2374677951918));
#292465=CARTESIAN_POINT('Ctrl Pts',(9.8487426438822,57.6339819585794,7.02807344505916));
#292466=CARTESIAN_POINT('Ctrl Pts',(11.3203984451319,57.758106490958,4.27980297250595));
#292467=CARTESIAN_POINT('Ctrl Pts',(11.7828840712243,57.8222568315178,2.76257692820836));
#292468=CARTESIAN_POINT('Ctrl Pts',(12.093882992487,57.9452495710872,-0.333394483159807));
#292469=CARTESIAN_POINT('Ctrl Pts',(11.9512678995239,58.0042455402168,-1.88158108678264));
#292470=CARTESIAN_POINT('Ctrl Pts',(11.0874436001478,58.1289659147518,-4.84283605448112));
#292471=CARTESIAN_POINT('Ctrl Pts',(10.3729381859985,58.1898675005961,-6.22786585061494));
#292472=CARTESIAN_POINT('Ctrl Pts',(9.41568944744502,58.25,-7.43940805637597));
#292473=CARTESIAN_POINT('',(11.9139873655789,58.25,1.43419142823616));
#292474=CARTESIAN_POINT('Origin',(-4.60239784438011E-14,58.25,0.));
#292475=CARTESIAN_POINT('Ctrl Pts',(11.9139873655789,58.25,1.43419142823616));
#292476=CARTESIAN_POINT('Ctrl Pts',(11.7419322810054,58.1928633911005,2.86347211101975));
#292477=CARTESIAN_POINT('Ctrl Pts',(11.3140783609753,58.1341670582794,4.25018151571504));
#292478=CARTESIAN_POINT('Ctrl Pts',(9.99471722983137,58.0198787276206,6.7922574722224));
#292479=CARTESIAN_POINT('Ctrl Pts',(9.11862808992739,57.9661217678065,7.92967429883511));
#292480=CARTESIAN_POINT('Ctrl Pts',(6.88763929437055,57.8449802717658,9.95400993085742));
#292481=CARTESIAN_POINT('Ctrl Pts',(5.51132648159584,57.7803680058085,10.7771721335172));
#292482=CARTESIAN_POINT('Ctrl Pts',(2.55258779755992,57.6585671957128,11.8275757293221));
#292483=CARTESIAN_POINT('Ctrl Pts',(1.00349369270896,57.5968421723381,12.058220919922));
#292484=CARTESIAN_POINT('Ctrl Pts',(-2.10503272518202,57.4710996373618,
11.9164883058773));
#292485=CARTESIAN_POINT('Ctrl Pts',(-3.63477613369994,57.4117324362029,
11.5421964925761));
#292486=CARTESIAN_POINT('Ctrl Pts',(-6.47805324817245,57.2873231041572,
10.223163188254));
#292487=CARTESIAN_POINT('Ctrl Pts',(-7.76188571802245,57.2230287850605,
9.28608507812353));
#292488=CARTESIAN_POINT('Ctrl Pts',(-9.87548389609288,57.0992772380319,
6.99040032187376));
#292489=CARTESIAN_POINT('Ctrl Pts',(-10.6931193539723,57.0403744014441,
5.66109909495666));
#292490=CARTESIAN_POINT('Ctrl Pts',(-11.7416233824511,56.9196975169164,
2.86495497233163));
#292491=CARTESIAN_POINT('Ctrl Pts',(-12.,56.8615595351003,1.43769259310665));
#292492=CARTESIAN_POINT('Ctrl Pts',(-12.,56.806249999784,-1.0547118733939E-14));
#292493=CARTESIAN_POINT('Origin',(-8.79029313101884E-14,130.96875,0.));
#292494=CARTESIAN_POINT('',(-12.,53.431249999796,4.29975907498869E-14));
#292495=CARTESIAN_POINT('',(-12.,53.806249999796,7.34788079488412E-16));
#292496=CARTESIAN_POINT('',(-12.0000000000001,130.96875,-1.46957615897682E-15));
#292497=CARTESIAN_POINT('Ctrl Pts',(-12.,53.431249999796,3.88578058618805E-15));
#292498=CARTESIAN_POINT('Ctrl Pts',(-12.,53.4871296062859,1.45251078131059));
#292499=CARTESIAN_POINT('Ctrl Pts',(-11.7362697676557,53.545887435454,2.8941457146946));
#292500=CARTESIAN_POINT('Ctrl Pts',(-10.6723591125893,53.6671358170952,
5.7001391743692));
#292501=CARTESIAN_POINT('Ctrl Pts',(-9.84987352654367,53.725972253639,7.02644046693785));
#292502=CARTESIAN_POINT('Ctrl Pts',(-7.72828533595836,53.8497914258214,
9.31397212620167));
#292503=CARTESIAN_POINT('Ctrl Pts',(-6.44157098951665,53.9140624414862,
10.2461035663569));
#292504=CARTESIAN_POINT('Ctrl Pts',(-3.59357279785099,54.038389583625,11.5551820820907));
#292505=CARTESIAN_POINT('Ctrl Pts',(-2.06181728169446,54.0978477387845,
11.9241297682562));
#292506=CARTESIAN_POINT('Ctrl Pts',(1.04746123863136,54.2236206969434,12.0544267391436));
#292507=CARTESIAN_POINT('Ctrl Pts',(2.59528430838765,54.2851867498183,11.8182264369422));
#292508=CARTESIAN_POINT('Ctrl Pts',(5.54932503645201,54.4070775499409,10.7575718149213));
#292509=CARTESIAN_POINT('Ctrl Pts',(6.9222436218604,54.471686284401,9.92988638851982));
#292510=CARTESIAN_POINT('Ctrl Pts',(9.23772823991195,54.5977621257001,7.8143181733086));
#292511=CARTESIAN_POINT('Ctrl Pts',(10.1681933239522,54.6560602355255,6.55797590019966));
#292512=CARTESIAN_POINT('Ctrl Pts',(11.5065573354667,54.7809069275133,3.74762478934861));
#292513=CARTESIAN_POINT('Ctrl Pts',(11.8965194259829,54.8446360238262,2.21778406412077));
#292514=CARTESIAN_POINT('Ctrl Pts',(12.0681892059812,54.9673680294498,-0.916680721945098));
#292515=CARTESIAN_POINT('Ctrl Pts',(11.8437757627918,55.0290465072021,-2.49132058677692));
#292516=CARTESIAN_POINT('Ctrl Pts',(10.8089621012139,55.1552954021812,-5.43674945472044));
#292517=CARTESIAN_POINT('Ctrl Pts',(10.0190430503885,55.2146507485608,-6.78311694484928));
#292518=CARTESIAN_POINT('Ctrl Pts',(7.95132789589228,55.3379980910645,-9.12495403364958));
#292519=CARTESIAN_POINT('Ctrl Pts',(6.6842604992068,55.4024097965215,-10.0900443803154));
#292520=CARTESIAN_POINT('Ctrl Pts',(3.86824730793014,55.5272703674442,-11.4655816809358));
#292521=CARTESIAN_POINT('Ctrl Pts',(2.34999462310856,55.5861907204487,-11.8701464395861));
#292522=CARTESIAN_POINT('Ctrl Pts',(-0.754084089986135,55.7117533419867,
-12.0767338211216));
#292523=CARTESIAN_POINT('Ctrl Pts',(-2.31032311118788,55.774449098957,-11.8776203671417));
#292524=CARTESIAN_POINT('Ctrl Pts',(-5.29526061035131,55.895723166354,-10.8854303487974));
#292525=CARTESIAN_POINT('Ctrl Pts',(-6.6904886906033,55.9603406693356,-10.088082516988));
#292526=CARTESIAN_POINT('Ctrl Pts',(-9.05540439012356,56.0867960754365,
-8.02458642659485));
#292527=CARTESIAN_POINT('Ctrl Pts',(-10.0136161072456,56.1451514874907,
-6.79130808557009));
#292528=CARTESIAN_POINT('Ctrl Pts',(-11.4178762637581,56.26966311311,-4.01107750314829));
#292529=CARTESIAN_POINT('Ctrl Pts',(-11.8436234943505,56.333616439539,-2.48703553226478));
#292530=CARTESIAN_POINT('Ctrl Pts',(-11.9881437725539,56.4073920033214,
-0.61630231526467));
#292531=CARTESIAN_POINT('Ctrl Pts',(-12.,56.4194016589986,-0.307980743108728));
#292532=CARTESIAN_POINT('Ctrl Pts',(-12.,56.431249999784,-1.83880688453542E-13));
#292533=CARTESIAN_POINT('Ctrl Pts',(-12.,56.806249999784,-1.2490009027033E-15));
#292534=CARTESIAN_POINT('Ctrl Pts',(-12.,56.8008357843213,-0.14073481947853));
#292535=CARTESIAN_POINT('Ctrl Pts',(-11.9975242302304,56.7953868674467,
-0.281567226368526));
#292536=CARTESIAN_POINT('Ctrl Pts',(-11.9376166255646,56.7292090376622,
-1.98230049374114));
#292537=CARTESIAN_POINT('Ctrl Pts',(-11.5788604387752,56.6657013356079,
-3.51652580330893));
#292538=CARTESIAN_POINT('Ctrl Pts',(-10.2981943560748,56.5405961595996,
-6.35234303161689));
#292539=CARTESIAN_POINT('Ctrl Pts',(-9.3919473084131,56.482223365065,-7.62865707923812));
#292540=CARTESIAN_POINT('Ctrl Pts',(-7.1197472580277,56.3565060811356,-9.78872100964218));
#292541=CARTESIAN_POINT('Ctrl Pts',(-5.76663779028911,56.2919328603437,
-10.6421776962415));
#292542=CARTESIAN_POINT('Ctrl Pts',(-2.84000231878984,56.1695428275062,
-11.7615493915576));
#292543=CARTESIAN_POINT('Ctrl Pts',(-1.29953472732787,56.1088172837461,
-12.0295922776977));
#292544=CARTESIAN_POINT('Ctrl Pts',(1.8138700773441,55.9828774138792,-11.9649010019541));
#292545=CARTESIAN_POINT('Ctrl Pts',(3.35708379228035,55.9228280131136,-11.6266489732502));
#292546=CARTESIAN_POINT('Ctrl Pts',(6.23166838906527,55.7989872672075,-10.3746205954368));
#292547=CARTESIAN_POINT('Ctrl Pts',(7.53448615261147,55.7348647064474,-9.47089739641282));
#292548=CARTESIAN_POINT('Ctrl Pts',(9.70132975098782,55.6106784867606,-7.2302169988211));
#292549=CARTESIAN_POINT('Ctrl Pts',(10.5514300340919,55.5521470124149,-5.92107369846786));
#292550=CARTESIAN_POINT('Ctrl Pts',(11.7234859051004,55.425645911933,-3.01368180469527));
#292551=CARTESIAN_POINT('Ctrl Pts',(12.018968228371,55.3617859544397,-1.43741489019202));
#292552=CARTESIAN_POINT('Ctrl Pts',(11.9795299887659,55.2402991338749,1.70764771572582));
#292553=CARTESIAN_POINT('Ctrl Pts',(11.6570644007191,55.1770790288273,3.24618888105004));
#292554=CARTESIAN_POINT('Ctrl Pts',(10.4438112629329,55.0517127580189,6.11069669039277));
#292555=CARTESIAN_POINT('Ctrl Pts',(9.5657907603954,54.9931091100837,7.41009407699998));
#292556=CARTESIAN_POINT('Ctrl Pts',(7.34415819072201,54.8678404916379,9.62088798132063));
#292557=CARTESIAN_POINT('Ctrl Pts',(6.01448847362389,54.8033403588107,10.503532747568));
#292558=CARTESIAN_POINT('Ctrl Pts',(3.12026983466767,54.6804135344638,11.6900990248898));
#292559=CARTESIAN_POINT('Ctrl Pts',(1.58837964561655,54.6205013061338,11.9946500945103));
#292560=CARTESIAN_POINT('Ctrl Pts',(-1.52936066374502,54.4943860614182,
12.0052882362664));
#292561=CARTESIAN_POINT('Ctrl Pts',(-3.08554247314003,54.4335144510827,
11.7023598441195));
#292562=CARTESIAN_POINT('Ctrl Pts',(-5.98961160773956,54.3102627229801,
10.5156866498795));
#292563=CARTESIAN_POINT('Ctrl Pts',(-7.31002011518611,54.2463408201135,
9.64461440052666));
#292564=CARTESIAN_POINT('Ctrl Pts',(-9.5276000616501,54.1217765985134,7.45786840585217));
#292565=CARTESIAN_POINT('Ctrl Pts',(-10.4089750696479,54.0634395118941,
6.16831971457848));
#292566=CARTESIAN_POINT('Ctrl Pts',(-11.6504069111924,53.9370385412999,
3.28607217389276));
#292567=CARTESIAN_POINT('Ctrl Pts',(-11.9829544758109,53.8724201434715,
1.7144602120856));
#292568=CARTESIAN_POINT('Ctrl Pts',(-11.999787336411,53.8094266493438,0.0825033819025622));
#292569=CARTESIAN_POINT('Ctrl Pts',(-12.,53.8078368125135,0.0412469364927481));
#292570=CARTESIAN_POINT('Ctrl Pts',(-12.,53.806249999796,2.93915231795365E-15));
#292571=CARTESIAN_POINT('Origin',(-8.79029313101884E-14,130.96875,0.));
#292572=CARTESIAN_POINT('',(-12.,50.431249999808,-4.62056866567646E-15));
#292573=CARTESIAN_POINT('',(-12.,50.806249999808,6.52193984771498E-14));
#292574=CARTESIAN_POINT('',(-12.0000000000001,130.96875,-1.46957615897682E-15));
#292575=CARTESIAN_POINT('Ctrl Pts',(-12.,50.431249999808,2.93915231795365E-15));
#292576=CARTESIAN_POINT('Ctrl Pts',(-12.,50.4333746432347,0.0552270797444227));
#292577=CARTESIAN_POINT('Ctrl Pts',(-11.9996187466256,50.4355046952934,
0.110470872436941));
#292578=CARTESIAN_POINT('Ctrl Pts',(-11.9768936043853,50.4990861513974,
1.75579641839743));
#292579=CARTESIAN_POINT('Ctrl Pts',(-11.6390809684786,50.5637046711776,
3.32570082480313));
#292580=CARTESIAN_POINT('Ctrl Pts',(-10.3881127909486,50.6900514144101,
6.20344025906615));
#292581=CARTESIAN_POINT('Ctrl Pts',(-9.50226042672603,50.7483738478049,
7.49016928165803));
#292582=CARTESIAN_POINT('Ctrl Pts',(-7.27746453080368,50.8729888469884,
9.66911900238871));
#292583=CARTESIAN_POINT('Ctrl Pts',(-5.95459568647555,50.936879186898,10.5354773982616));
#292584=CARTESIAN_POINT('Ctrl Pts',(-3.04636173817073,51.060043252087,11.7127312485299));
#292585=CARTESIAN_POINT('Ctrl Pts',(-1.48832533954868,51.1210459751629,
12.0105532498137));
#292586=CARTESIAN_POINT('Ctrl Pts',(1.63000466665062,51.2471850736166,11.9890404478604));
#292587=CARTESIAN_POINT('Ctrl Pts',(3.16064508284471,51.3069934116536,11.6792235396826));
#292588=CARTESIAN_POINT('Ctrl Pts',(6.05010037198389,51.4299944549249,10.4829795379728));
#292589=CARTESIAN_POINT('Ctrl Pts',(7.37632612828183,51.4944811634555,9.59615917197936));
#292590=CARTESIAN_POINT('Ctrl Pts',(9.59058322802632,51.6196817306165,7.37807593840257));
#292591=CARTESIAN_POINT('Ctrl Pts',(10.4644911620606,51.6783317258522,6.07533323433215));
#292592=CARTESIAN_POINT('Ctrl Pts',(11.6679105771596,51.8037324189243,3.20673549708131));
#292593=CARTESIAN_POINT('Ctrl Pts',(11.9850988204085,51.8669080122012,1.66763663857078));
#292594=CARTESIAN_POINT('Ctrl Pts',(12.0141746424869,51.9882919802791,-1.47811941699711));
#292595=CARTESIAN_POINT('Ctrl Pts',(11.7130740031476,52.0523453898995,-3.05447428151856));
#292596=CARTESIAN_POINT('Ctrl Pts',(10.530191958422,52.1788634877723,-5.95879036118455));
#292597=CARTESIAN_POINT('Ctrl Pts',(9.67534739336931,52.2373551303859,-7.26497244843828));
#292598=CARTESIAN_POINT('Ctrl Pts',(7.50077083482246,52.3616012930252,-9.49753044946365));
#292599=CARTESIAN_POINT('Ctrl Pts',(6.19523966964062,52.4256956418871,-10.3963324217276));
#292600=CARTESIAN_POINT('Ctrl Pts',(3.31613883858384,52.5494496519484,-11.6384967577646));
#292601=CARTESIAN_POINT('Ctrl Pts',(1.7709568382787,52.6096132908761,-11.9714288361293));
#292602=CARTESIAN_POINT('Ctrl Pts',(-1.34312935883758,52.7355807236463,
-12.0247635155693));
#292603=CARTESIAN_POINT('Ctrl Pts',(-2.88231279120065,52.7961732160391,
-11.7512130832305));
#292604=CARTESIAN_POINT('Ctrl Pts',(-5.80412602816963,52.918646690625,-10.6216947176347));
#292605=CARTESIAN_POINT('Ctrl Pts',(-7.1537488290025,52.9832111124131,-9.76380911854804));
#292606=CARTESIAN_POINT('Ctrl Pts',(-9.41838431356261,53.1088632934264,
-7.59607158678609));
#292607=CARTESIAN_POINT('Ctrl Pts',(-10.3204048871767,53.1672608749328,
-6.31628776693271));
#292608=CARTESIAN_POINT('Ctrl Pts',(-11.5909871582565,53.292407903375,-3.4761062152077));
#292609=CARTESIAN_POINT('Ctrl Pts',(-11.9443028041032,53.3558745509222,
-1.9411803201662));
#292610=CARTESIAN_POINT('Ctrl Pts',(-11.9979789277012,53.421437949922,-0.254393574972973));
#292611=CARTESIAN_POINT('Ctrl Pts',(-12.,53.4263581727884,-0.127156075625299));
#292612=CARTESIAN_POINT('Ctrl Pts',(-12.,53.431249999796,2.34187669256869E-14));
#292613=CARTESIAN_POINT('Ctrl Pts',(-12.,53.806249999796,1.4432899320127E-14));
#292614=CARTESIAN_POINT('Ctrl Pts',(-12.,53.7480939148037,-1.51168459759066));
#292615=CARTESIAN_POINT('Ctrl Pts',(-11.7143465683857,53.6868690266145,
-3.01032393715114));
#292616=CARTESIAN_POINT('Ctrl Pts',(-10.5844918994098,53.562939921336,-5.86457248065474));
#292617=CARTESIAN_POINT('Ctrl Pts',(-9.73501285958027,53.5039492278736,
-7.18708934061602));
#292618=CARTESIAN_POINT('Ctrl Pts',(-7.56459251217115,53.3791664941359,
-9.44793524513585));
#292619=CARTESIAN_POINT('Ctrl Pts',(-6.25896026340131,53.3147736776583,
-10.3591511846968));
#292620=CARTESIAN_POINT('Ctrl Pts',(-3.39799737004919,53.1913523776906,
-11.6122869664658));
#292621=CARTESIAN_POINT('Ctrl Pts',(-1.87477951714514,53.1320864243024,
-11.9531081269277));
#292622=CARTESIAN_POINT('Ctrl Pts',(1.24683572774671,53.0058144351521,-12.0386941530778));
#292623=CARTESIAN_POINT('Ctrl Pts',(2.81570505813728,52.9439768965327,-11.7709951509428));
#292624=CARTESIAN_POINT('Ctrl Pts',(5.74801110444513,52.8213424941071,-10.6491505166484));
#292625=CARTESIAN_POINT('Ctrl Pts',(7.08497336545378,52.7576510477283,-9.81055520606376));
#292626=CARTESIAN_POINT('Ctrl Pts',(9.35172990701891,52.6327560522224,-7.67758313712671));
#292627=CARTESIAN_POINT('Ctrl Pts',(10.263773913544,52.5744530895322,-6.40742326293614));
#292628=CARTESIAN_POINT('Ctrl Pts',(11.5702421647988,52.4484392107677,-3.55636923351588));
#292629=CARTESIAN_POINT('Ctrl Pts',(11.9386514798297,52.3838349192808,-1.99677613501637));
#292630=CARTESIAN_POINT('Ctrl Pts',(12.0460453155768,52.2618526617759,1.13908453685275));
#292631=CARTESIAN_POINT('Ctrl Pts',(11.7982071860678,52.200445948804,2.68465914904394));
#292632=CARTESIAN_POINT('Ctrl Pts',(10.7243954194677,52.0746421717493,5.60584655808609));
#292633=CARTESIAN_POINT('Ctrl Pts',(9.90474876030528,52.0150868999077,6.95227710948971));
#292634=CARTESIAN_POINT('Ctrl Pts',(7.78788701011688,51.8908449260673,9.26409655473338));
#292635=CARTESIAN_POINT('Ctrl Pts',(6.50768448347384,51.8265986328547,10.2041509569471));
#292636=CARTESIAN_POINT('Ctrl Pts',(3.68194428913401,51.702711177516,11.5253724153568));
#292637=CARTESIAN_POINT('Ctrl Pts',(2.16778571004633,51.6439387737841,11.9034275032323));
#292638=CARTESIAN_POINT('Ctrl Pts',(-0.957341155162895,51.517524736608,
12.0660569027066));
#292639=CARTESIAN_POINT('Ctrl Pts',(-2.53901199783854,51.4545455404943,
11.8346610204564));
#292640=CARTESIAN_POINT('Ctrl Pts',(-5.49921221111154,51.3325770637309,
10.7792172403802));
#292641=CARTESIAN_POINT('Ctrl Pts',(-6.85221550876325,51.2691531618878,
9.97395304151869));
#292642=CARTESIAN_POINT('Ctrl Pts',(-9.1681705344409,51.1439643127511,7.8963378369432));
#292643=CARTESIAN_POINT('Ctrl Pts',(-10.1112860675465,51.0855377818822,
6.64600774787707));
#292644=CARTESIAN_POINT('Ctrl Pts',(-11.4829497441587,50.959952982895,3.82729031393066));
#292645=CARTESIAN_POINT('Ctrl Pts',(-11.887186090446,50.8953983536027,2.2806290215588));
#292646=CARTESIAN_POINT('Ctrl Pts',(-11.9931989855778,50.8242908749857,
0.466737071064205));
#292647=CARTESIAN_POINT('Ctrl Pts',(-12.,50.8152236502517,0.233257262100788));
#292648=CARTESIAN_POINT('Ctrl Pts',(-12.,50.806249999808,2.15313877838241E-13));
#292649=CARTESIAN_POINT('Origin',(-8.79029313101884E-14,130.96875,0.));
#292650=CARTESIAN_POINT('',(-12.,47.43124999982,8.60360801888715E-14));
#292651=CARTESIAN_POINT('',(-12.,47.80624999982,1.14936573298645E-13));
#292652=CARTESIAN_POINT('',(-12.0000000000001,130.96875,-1.46957615897682E-15));
#292653=CARTESIAN_POINT('Ctrl Pts',(-12.,47.43124999982,2.31065167000111E-13));
#292654=CARTESIAN_POINT('Ctrl Pts',(-12.,47.4407678727725,0.247403551082924));
#292655=CARTESIAN_POINT('Ctrl Pts',(-11.9923490646664,47.4503907550039,
0.495050729214709));
#292656=CARTESIAN_POINT('Ctrl Pts',(-11.8790644606491,47.5220984700527,
2.32218224939318));
#292657=CARTESIAN_POINT('Ctrl Pts',(-11.4696027511409,47.5866428237261,
3.86687861825634));
#292658=CARTESIAN_POINT('Ctrl Pts',(-10.0884088594892,47.7121614098843,
6.68077838944382));
#292659=CARTESIAN_POINT('Ctrl Pts',(-9.14072251871325,47.7706195334804,
7.92817496660893));
#292660=CARTESIAN_POINT('Ctrl Pts',(-6.81758560523962,47.89584804637,9.99757334818262));
#292661=CARTESIAN_POINT('Ctrl Pts',(-5.46228610104156,47.9592297004385,
10.7979002123034));
#292662=CARTESIAN_POINT('Ctrl Pts',(-2.49804490039839,48.0810967543812,
11.8435163598417));
#292663=CARTESIAN_POINT('Ctrl Pts',(-0.914496854331955,48.1442578249945,
12.0695190218114));
#292664=CARTESIAN_POINT('Ctrl Pts',(2.21110912803724,48.2706912428669,11.8954602673166));
#292665=CARTESIAN_POINT('Ctrl Pts',(3.72391114734811,48.3294052303618,11.5118855378486));
#292666=CARTESIAN_POINT('Ctrl Pts',(6.54433692350144,48.4533581435511,10.1805963520437));
#292667=CARTESIAN_POINT('Ctrl Pts',(7.82070636620124,48.5175795628426,9.23631232192927));
#292668=CARTESIAN_POINT('Ctrl Pts',(9.9295451305108,48.6417377379988,6.91697463000914));
#292669=CARTESIAN_POINT('Ctrl Pts',(10.7447224853498,48.7013913232631,5.5669845201973));
#292670=CARTESIAN_POINT('Ctrl Pts',(11.8078795147673,48.8272247409165,2.64156471203725));
#292671=CARTESIAN_POINT('Ctrl Pts',(12.0500395478662,48.8884798877763,1.09548931021175));
#292672=CARTESIAN_POINT('Ctrl Pts',(11.9314334482903,49.0105503990855,-2.03902230824284));
#292673=CARTESIAN_POINT('Ctrl Pts',(11.5576773465329,49.0751495604682,-3.59674478067195));
#292674=CARTESIAN_POINT('Ctrl Pts',(10.2414947097431,49.2011021244793,-6.44304862520994));
#292675=CARTESIAN_POINT('Ctrl Pts',(9.32484211207299,49.2594133717901,-7.71027961852137));
#292676=CARTESIAN_POINT('Ctrl Pts',(7.05074793878167,49.3843545943596,-9.8350965442519));
#292677=CARTESIAN_POINT('Ctrl Pts',(5.71135946361982,49.4480085240933,-10.6687745641359));
#292678=CARTESIAN_POINT('Ctrl Pts',(2.77487011449975,49.5705467408296,-11.7808159513214));
#292679=CARTESIAN_POINT('Ctrl Pts',(1.2040981552789,49.6325432062857,-12.043169752985));
#292680=CARTESIAN_POINT('Ctrl Pts',(-1.91806513933708,49.7588373645131,
-11.9462280010008));
#292681=CARTESIAN_POINT('Ctrl Pts',(-3.43995695565266,49.8180196669659,
-11.5999157144062));
#292682=CARTESIAN_POINT('Ctrl Pts',(-6.29579415143742,49.941512382835,-10.3367213702745));
#292683=CARTESIAN_POINT('Ctrl Pts',(-7.59772347007663,50.0058859134419,
-9.42121991920977));
#292684=CARTESIAN_POINT('Ctrl Pts',(-9.76030732451788,50.1305915776529,
-7.15282943528729));
#292685=CARTESIAN_POINT('Ctrl Pts',(-10.6054210782084,50.1896547997765,
-5.82679696083733));
#292686=CARTESIAN_POINT('Ctrl Pts',(-11.7198746329126,50.3130500057532,
-2.98142224388078));
#292687=CARTESIAN_POINT('Ctrl Pts',(-12.,50.3736594394224,-1.49698459091494));
#292688=CARTESIAN_POINT('Ctrl Pts',(-12.,50.431249999808,-3.60822483003176E-15));
#292689=CARTESIAN_POINT('Ctrl Pts',(-12.,50.806249999808,2.11775041947249E-13));
#292690=CARTESIAN_POINT('Ctrl Pts',(-12.,50.7557911893547,-1.31160490918796));
#292691=CARTESIAN_POINT('Ctrl Pts',(-11.784958795216,50.7029229735181,-2.61596775665401));
#292692=CARTESIAN_POINT('Ctrl Pts',(-10.8579681788226,50.586384972594,-5.34400959596382));
#292693=CARTESIAN_POINT('Ctrl Pts',(-10.0683905445584,50.526101142349,-6.71426830879258));
#292694=CARTESIAN_POINT('Ctrl Pts',(-8.00548678663434,50.4024364306604,
-9.07607578521367));
#292695=CARTESIAN_POINT('Ctrl Pts',(-6.75117323967514,50.3383716329531,
-10.0441298842934));
#292696=CARTESIAN_POINT('Ctrl Pts',(-3.96136200713807,50.2140653698115,
-11.4324177395091));
#292697=CARTESIAN_POINT('Ctrl Pts',(-2.45632658584548,50.1556104973947,
-11.8473194713069));
#292698=CARTESIAN_POINT('Ctrl Pts',(0.6717896556587,50.0290755374074,-12.086283174021));
#292699=CARTESIAN_POINT('Ctrl Pts',(2.26588548555627,49.9648219505577,-11.8909449059983));
#292700=CARTESIAN_POINT('Ctrl Pts',(5.25260223989149,49.8435434241694,-10.9010162838714));
#292701=CARTESIAN_POINT('Ctrl Pts',(6.62053656282354,49.7804138038033,-10.1286799125176));
#292702=CARTESIAN_POINT('Ctrl Pts',(8.98388750296656,49.6549790246415,-8.10595614246599));
#292703=CARTESIAN_POINT('Ctrl Pts',(9.95734378372957,49.5962785807417,-6.87518063584317));
#292704=CARTESIAN_POINT('Ctrl Pts',(11.3919731722414,49.4711479557705,-4.08872760854805));
#292705=CARTESIAN_POINT('Ctrl Pts',(11.8306707335156,49.406675621401,-2.5554025829876));
#292706=CARTESIAN_POINT('Ctrl Pts',(12.0863157245536,49.2836000769814,0.560706804715852));
#292707=CARTESIAN_POINT('Ctrl Pts',(11.9134519368995,49.2238937129125,2.11261320746752));
#292708=CARTESIAN_POINT('Ctrl Pts',(10.9806134950917,49.0977307783428,5.08894141443361));
#292709=CARTESIAN_POINT('Ctrl Pts',(10.2202603227565,49.0365917722932,6.48207908223318));
#292710=CARTESIAN_POINT('Ctrl Pts',(8.20972359130218,48.9135173804856,8.89113562490776));
#292711=CARTESIAN_POINT('Ctrl Pts',(6.98076465471862,48.8496597446431,9.88537443630402));
#292712=CARTESIAN_POINT('Ctrl Pts',(4.2262356362271,48.7249941615828,11.3373365458814));
#292713=CARTESIAN_POINT('Ctrl Pts',(2.7300589348449,48.6666832035132,11.7874093317986));
#292714=CARTESIAN_POINT('Ctrl Pts',(-0.392026331067906,48.5403922016132,
12.0984721210039));
#292715=CARTESIAN_POINT('Ctrl Pts',(-1.98946818663386,48.4757743211795,
11.9402272870843));
#292716=CARTESIAN_POINT('Ctrl Pts',(-4.99444789369535,48.3542203386418,
11.0211812157372));
#292717=CARTESIAN_POINT('Ctrl Pts',(-6.37721571212599,48.2920486779669,
10.2831227191624));
#292718=CARTESIAN_POINT('Ctrl Pts',(-8.78896645640985,48.1663900703293,
8.31760167700385));
#292719=CARTESIAN_POINT('Ctrl Pts',(-9.79368884331946,48.1072498720136,
7.1071890123526));
#292720=CARTESIAN_POINT('Ctrl Pts',(-11.292468355393,47.9826229572552,4.35467285326218));
#292721=CARTESIAN_POINT('Ctrl Pts',(-11.7661084694716,47.9182697115858,
2.83579689248597));
#292722=CARTESIAN_POINT('Ctrl Pts',(-11.9776268652391,47.8390998979341,
0.846616841177166));
#292723=CARTESIAN_POINT('Ctrl Pts',(-12.,47.8225261014706,0.423074080334272));
#292724=CARTESIAN_POINT('Ctrl Pts',(-12.,47.80624999982,1.73611125475759E-13));
#292725=CARTESIAN_POINT('Origin',(-8.79029313101884E-14,130.96875,0.));
#292726=CARTESIAN_POINT('',(-12.,44.431249999832,4.71435798574715E-14));
#292727=CARTESIAN_POINT('',(-12.,44.806249999832,4.32577992712834E-14));
#292728=CARTESIAN_POINT('',(-12.0000000000001,130.96875,-1.46957615897682E-15));
#292729=CARTESIAN_POINT('Ctrl Pts',(-12.,44.431249999832,2.12191375581483E-13));
#292730=CARTESIAN_POINT('Ctrl Pts',(-12.,44.4480633973018,0.437040319885026));
#292731=CARTESIAN_POINT('Ctrl Pts',(-11.9761253853199,44.4651936746564,
0.874560148487268));
#292732=CARTESIAN_POINT('Ctrl Pts',(-11.7561719971819,44.5449565599248,
2.87641555660222));
#292733=CARTESIAN_POINT('Ctrl Pts',(-11.2774887994135,44.6092895857453,
4.39312733398706));
#292734=CARTESIAN_POINT('Ctrl Pts',(-9.769422444749,44.7338401007517,7.14064011226523));
#292735=CARTESIAN_POINT('Ctrl Pts',(-8.76014300197083,44.7930576606372,
8.3480659234863));
#292736=CARTESIAN_POINT('Ctrl Pts',(-6.34137693634925,44.9187463133987,
10.3051948567027));
#292737=CARTESIAN_POINT('Ctrl Pts',(-4.95646526673096,44.9807567681892,
11.0382537859001));
#292738=CARTESIAN_POINT('Ctrl Pts',(-1.9493068899536,45.1023988797682,11.9467775902144));
#292739=CARTESIAN_POINT('Ctrl Pts',(-0.351898131209509,45.1670154214074,
12.0996351633707));
#292740=CARTESIAN_POINT('Ctrl Pts',(2.76884245591405,45.2932520299078,11.7783891778682));
#292741=CARTESIAN_POINT('Ctrl Pts',(4.26374680592003,45.3515551502874,11.323313415966));
#292742=CARTESIAN_POINT('Ctrl Pts',(7.01317923842076,45.4762685836509,9.86232394612193));
#292743=CARTESIAN_POINT('Ctrl Pts',(8.23848222451373,45.5400940614743,8.86440566825877));
#292744=CARTESIAN_POINT('Ctrl Pts',(10.2415028621997,45.6630813533292,6.44866740241013));
#292745=CARTESIAN_POINT('Ctrl Pts',(10.9976565736167,45.7243547713553,5.05226566134454));
#292746=CARTESIAN_POINT('Ctrl Pts',(11.92054272461,45.8505403224076,2.07211587581859));
#292747=CARTESIAN_POINT('Ctrl Pts',(12.0881258529366,45.9101517109846,0.519786142751066));
#292748=CARTESIAN_POINT('Ctrl Pts',(11.8220280136357,46.0332982737874,-2.59477293038869));
#292749=CARTESIAN_POINT('Ctrl Pts',(11.3784104957874,46.0977560372114,-4.12612061417768));
#292750=CARTESIAN_POINT('Ctrl Pts',(9.93476841314932,46.2228184111249,-6.90787115060338));
#292751=CARTESIAN_POINT('Ctrl Pts',(8.95694147161195,46.28157074466,-8.13581345040347));
#292752=CARTESIAN_POINT('Ctrl Pts',(6.58681770431223,46.4070375608798,-10.1505626538572));
#292753=CARTESIAN_POINT('Ctrl Pts',(5.21679342013365,46.4701221067991,-10.9181266772137));
#292754=CARTESIAN_POINT('Ctrl Pts',(2.22631721205064,46.5912979910622,-11.8985638824829));
#292755=CARTESIAN_POINT('Ctrl Pts',(0.63043916516099,46.6557481998966,-12.0886574981134));
#292756=CARTESIAN_POINT('Ctrl Pts',(-2.49806951449905,46.7822990343408,
-11.8386062570599));
#292757=CARTESIAN_POINT('Ctrl Pts',(-4.00176733541213,46.8407219916465,
-11.4183558921771));
#292758=CARTESIAN_POINT('Ctrl Pts',(-6.78627496913661,46.9650854684867,
-10.0203619377339));
#292759=CARTESIAN_POINT('Ctrl Pts',(-8.03677248548348,47.0291208981668,
-9.04829069795741));
#292760=CARTESIAN_POINT('Ctrl Pts',(-10.0917662518949,47.1526983168778,
-6.67926746296542));
#292761=CARTESIAN_POINT('Ctrl Pts',(-10.8769328846958,47.2131020949138,
-5.30553745375233));
#292762=CARTESIAN_POINT('Ctrl Pts',(-11.7897156391528,47.3290914917053,
-2.58713938330585));
#292763=CARTESIAN_POINT('Ctrl Pts',(-12.,47.3813523556844,-1.29701819002632));
#292764=CARTESIAN_POINT('Ctrl Pts',(-12.,47.43124999982,2.16771045558062E-13));
#292765=CARTESIAN_POINT('Ctrl Pts',(-12.,47.80624999982,2.04003480774873E-13));
#292766=CARTESIAN_POINT('Ctrl Pts',(-12.,47.7632541030443,-1.11761709757617));
#292767=CARTESIAN_POINT('Ctrl Pts',(-11.8438691418875,47.7184381854061,
-2.23181305421852));
#292768=CARTESIAN_POINT('Ctrl Pts',(-11.0991279573074,47.6092880553311,
-4.82703414338412));
#292769=CARTESIAN_POINT('Ctrl Pts',(-10.3687627631493,47.5471277954344,
-6.24334594351771));
#292770=CARTESIAN_POINT('Ctrl Pts',(-8.41183557330947,47.4246874049577,
-8.69952455205501));
#292771=CARTESIAN_POINT('Ctrl Pts',(-7.20903772274042,47.3610720405269,
-9.71958143976674));
#292772=CARTESIAN_POINT('Ctrl Pts',(-4.49103627275375,47.2360851638739,
-11.2353325572595));
#292773=CARTESIAN_POINT('Ctrl Pts',(-3.00394262343975,47.177762031447,-11.720854706413));
#292774=CARTESIAN_POINT('Ctrl Pts',(0.108228352968689,47.0518720709817,
-12.103841048153));
#292775=CARTESIAN_POINT('Ctrl Pts',(1.70506011519628,46.987278869342,-11.9836421050193));
#292776=CARTESIAN_POINT('Ctrl Pts',(4.72498218786174,46.8651204554188,-11.1389841017771));
#292777=CARTESIAN_POINT('Ctrl Pts',(6.12279678628232,46.804014061626,-10.436191065797));
#292778=CARTESIAN_POINT('Ctrl Pts',(8.58385739181458,46.678151220751,-8.52994948380035));
#292779=CARTESIAN_POINT('Ctrl Pts',(9.62066378834719,46.618395094874,-7.34067395799302));
#292780=CARTESIAN_POINT('Ctrl Pts',(11.1844836000381,46.4943220083027,-4.6236866482046));
#292781=CARTESIAN_POINT('Ctrl Pts',(11.6933529492508,46.430126384601,-3.12035451835472));
#292782=CARTESIAN_POINT('Ctrl Pts',(12.0991883805569,46.3061087047262,-0.0285554936068377));
#292783=CARTESIAN_POINT('Ctrl Pts',(12.0022010561016,46.2474495293521,1.52914964686318));
#292784=CARTESIAN_POINT('Ctrl Pts',(11.2126464649974,46.1209970957569,4.55955871390806));
#292785=CARTESIAN_POINT('Ctrl Pts',(10.5129341842395,46.0576501769004,5.99922541638793));
#292786=CARTESIAN_POINT('Ctrl Pts',(8.61062745985699,45.9358856515147,8.50215678159028));
#292787=CARTESIAN_POINT('Ctrl Pts',(7.43466838544492,45.8725470762023,9.54751274348946));
#292788=CARTESIAN_POINT('Ctrl Pts',(4.75429418025336,45.7472797427785,11.1268489084341));
#292789=CARTESIAN_POINT('Ctrl Pts',(3.27648282411912,45.688786514153,11.6479513487885));
#292790=CARTESIAN_POINT('Ctrl Pts',(0.175152526872331,45.5633350683713,
12.1025662801572));
#292791=CARTESIAN_POINT('Ctrl Pts',(-1.42019834163361,45.498801770141,12.0202321282542));
#292792=CARTESIAN_POINT('Ctrl Pts',(-4.45396624172863,45.3760832807332,
11.249820552242));
#292793=CARTESIAN_POINT('Ctrl Pts',(-5.86655654536747,45.315867792378,10.582056634735));
#292794=CARTESIAN_POINT('Ctrl Pts',(-8.37619037859286,45.1898200456127,
8.73489350280551));
#292795=CARTESIAN_POINT('Ctrl Pts',(-9.44472037212808,45.1292928650767,
7.56677849119635));
#292796=CARTESIAN_POINT('Ctrl Pts',(-11.0720581406693,45.0058035139223,
4.88560278740076));
#292797=CARTESIAN_POINT('Ctrl Pts',(-11.6151138397186,44.9417981794053,
3.39832477228253));
#292798=CARTESIAN_POINT('Ctrl Pts',(-11.9523124591163,44.8543875745271,
1.23577307049343));
#292799=CARTESIAN_POINT('Ctrl Pts',(-12.,44.8300125392067,0.617673366029319));
#292800=CARTESIAN_POINT('Ctrl Pts',(-12.,44.806249999832,-3.46944695195361E-15));
#292801=CARTESIAN_POINT('Origin',(-8.79029313101884E-14,130.96875,0.));
#292802=CARTESIAN_POINT('',(-12.,41.431249999844,-1.46125758873029E-14));
#292803=CARTESIAN_POINT('',(-12.,41.806249999844,-1.69717998146313E-14));
#292804=CARTESIAN_POINT('',(-12.0000000000001,130.96875,-1.46957615897682E-15));
#292805=CARTESIAN_POINT('Ctrl Pts',(-12.,41.431249999844,9.43689570931383E-15));
#292806=CARTESIAN_POINT('Ctrl Pts',(-12.,41.4555295818647,0.631113153188752));
#292807=CARTESIAN_POINT('Ctrl Pts',(-11.9502146704977,41.480447020204,1.26263023873752));
#292808=CARTESIAN_POINT('Ctrl Pts',(-11.6036949894875,41.5684241015784,
3.43687809370616));
#292809=CARTESIAN_POINT('Ctrl Pts',(-11.0559156247007,41.6324001760595,
4.92186072382863));
#292810=CARTESIAN_POINT('Ctrl Pts',(-9.41976702018347,41.7558051513705,
7.59798038360397));
#292811=CARTESIAN_POINT('Ctrl Pts',(-8.34680511181584,41.8164527518273,
8.76311730869326));
#292812=CARTESIAN_POINT('Ctrl Pts',(-5.83039947901914,41.9425249504412,
10.6019882659294));
#292813=CARTESIAN_POINT('Ctrl Pts',(-4.41575251688016,42.0026290583863,
11.2648449144665));
#292814=CARTESIAN_POINT('Ctrl Pts',(-1.38012561054793,42.1254227461761,
12.0248295578064));
#292815=CARTESIAN_POINT('Ctrl Pts',(0.214947713004328,42.1899448174772,
12.1018562767893));
#292816=CARTESIAN_POINT('Ctrl Pts',(3.31467996834863,42.315331621106,11.6371948376792));
#292817=CARTESIAN_POINT('Ctrl Pts',(4.79116959092115,42.3738614683273,11.1110785709522));
#292818=CARTESIAN_POINT('Ctrl Pts',(7.46616442758904,42.4991648908377,9.52282048797467));
#292819=CARTESIAN_POINT('Ctrl Pts',(8.63829657933997,42.5624617695215,8.47395091611032));
#292820=CARTESIAN_POINT('Ctrl Pts',(10.5328423833091,42.6841278665148,5.96447730981581));
#292821=CARTESIAN_POINT('Ctrl Pts',(11.2281896251307,42.7476550373785,4.52151316204852));
#292822=CARTESIAN_POINT('Ctrl Pts',(12.0074663393262,42.8741251897373,1.48730403633692));
#292823=CARTESIAN_POINT('Ctrl Pts',(12.0990229616799,42.9327356783733,-0.0707926080980731));
#292824=CARTESIAN_POINT('Ctrl Pts',(11.6824444101056,43.0568142310699,-3.16068328377196));
#292825=CARTESIAN_POINT('Ctrl Pts',(11.1686012325138,43.1209844862839,-4.66173990110958));
#292826=CARTESIAN_POINT('Ctrl Pts',(9.59556606119807,43.2449755342907,-7.37360048341212));
#292827=CARTESIAN_POINT('Ctrl Pts',(8.55418145173455,43.3048330375685,-8.55983872995765));
#292828=CARTESIAN_POINT('Ctrl Pts',(6.08609991188275,43.4307236214075,-10.4575836520369));
#292829=CARTESIAN_POINT('Ctrl Pts',(4.68614689785719,43.4916913759107,-11.1553316022767));
#292830=CARTESIAN_POINT('Ctrl Pts',(1.66416888938256,43.6139329541844,-11.9893170423389));
#292831=CARTESIAN_POINT('Ctrl Pts',(0.067496458510527,43.6785197107354,
-12.104065813472));
#292832=CARTESIAN_POINT('Ctrl Pts',(-3.04317437145658,43.8043489890024,
-11.7107734300768));
#292833=CARTESIAN_POINT('Ctrl Pts',(-4.52894729934066,43.8626868170876,
-11.2201494953272));
#292834=CARTESIAN_POINT('Ctrl Pts',(-7.24161258390349,43.9877165151098,
-9.69525277413838));
#292835=CARTESIAN_POINT('Ctrl Pts',(-8.4405970497795,44.0512942543223,-8.67152967250919));
#292836=CARTESIAN_POINT('Ctrl Pts',(-10.3897417120076,44.1736401674515,
-6.20861290814931));
#292837=CARTESIAN_POINT('Ctrl Pts',(-11.115746097572,44.2359606257585,-4.78895761877185));
#292838=CARTESIAN_POINT('Ctrl Pts',(-11.8477912822414,44.3445657147565,
-2.20377891566744));
#292839=CARTESIAN_POINT('Ctrl Pts',(-12.,44.3887975354914,-1.10349134543309));
#292840=CARTESIAN_POINT('Ctrl Pts',(-12.,44.431249999832,2.11775041947249E-13));
#292841=CARTESIAN_POINT('Ctrl Pts',(-12.,44.806249999832,1.2490009027033E-14));
#292842=CARTESIAN_POINT('Ctrl Pts',(-12.,44.7707571013409,-0.922587343696966));
#292843=CARTESIAN_POINT('Ctrl Pts',(-11.8936087828564,44.7339748643673,
-1.84412060288041));
#292844=CARTESIAN_POINT('Ctrl Pts',(-11.3171654079714,44.6324372407734,
-4.29614870177773));
#292845=CARTESIAN_POINT('Ctrl Pts',(-10.6479128705179,44.5678230724129,
-5.75824864709434));
#292846=CARTESIAN_POINT('Ctrl Pts',(-8.79958584391621,44.4467137796665,
-8.30575435989554));
#292847=CARTESIAN_POINT('Ctrl Pts',(-7.65025428745581,44.383701387247,-9.37510781353939));
#292848=CARTESIAN_POINT('Ctrl Pts',(-5.00717796024875,44.2581956490076,
-11.0158070497208));
#292849=CARTESIAN_POINT('Ctrl Pts',(-3.53854538320666,44.1993871673535,
-11.5714554134028));
#292850=CARTESIAN_POINT('Ctrl Pts',(-0.448572613682795,44.074395143219,
-12.0950485754387));
#292851=CARTESIAN_POINT('Ctrl Pts',(1.14452620374632,44.0099529423683,-12.0491312232276));
#292852=CARTESIAN_POINT('Ctrl Pts',(4.19064476565769,43.8867348581954,-11.3503763214298));
#292853=CARTESIAN_POINT('Ctrl Pts',(5.61728165907052,43.8272168385556,-10.716282921232));
#292854=CARTESIAN_POINT('Ctrl Pts',(8.17321331619008,43.7010086192829,-8.92609404588821));
#292855=CARTESIAN_POINT('Ctrl Pts',(9.27208779579082,43.6395952508958,-7.77848261244147));
#292856=CARTESIAN_POINT('Ctrl Pts',(10.9594430391363,43.5166973288171,-5.13218112477692));
#292857=CARTESIAN_POINT('Ctrl Pts',(11.5345800225846,43.4529052377067,-3.66086990947338));
#292858=CARTESIAN_POINT('Ctrl Pts',(12.084772499407,43.3281439874099,-0.59664727805155));
#292859=CARTESIAN_POINT('Ctrl Pts',(12.0608636000957,43.269845613111,0.966055964610005));
#292860=CARTESIAN_POINT('Ctrl Pts',(11.4122909633861,43.1436650635112,4.0352056082348));
#292861=CARTESIAN_POINT('Ctrl Pts',(10.7785087786671,43.0790506090707,5.50883800602957));
#292862=CARTESIAN_POINT('Ctrl Pts',(8.99467956134047,42.9573198358976,8.09345482594726));
#292863=CARTESIAN_POINT('Ctrl Pts',(7.87369414154674,42.895469631438,9.18769182077571));
#292864=CARTESIAN_POINT('Ctrl Pts',(5.27082318036897,42.7697508400841,10.8926896879356));
#292865=CARTESIAN_POINT('Ctrl Pts',(3.81206688801357,42.7104513446453,11.4847923470224));
#292866=CARTESIAN_POINT('Ctrl Pts',(0.734944359608439,42.5859791236831,
12.080540589554));
#292867=CARTESIAN_POINT('Ctrl Pts',(-0.854930055522513,42.5216673526452,
12.0726431855703));
#292868=CARTESIAN_POINT('Ctrl Pts',(-3.91292811989484,42.3979687325035,
11.4490135627046));
#292869=CARTESIAN_POINT('Ctrl Pts',(-5.35408061776081,42.3390119364223,
10.850101759793));
#292870=CARTESIAN_POINT('Ctrl Pts',(-7.95796292680611,42.2126546460276,
9.11964158869093));
#292871=CARTESIAN_POINT('Ctrl Pts',(-9.08837248934058,42.1501687604152,
7.99363321081445));
#292872=CARTESIAN_POINT('Ctrl Pts',(-10.837335509043,42.0279192380799,5.38420353094394));
#292873=CARTESIAN_POINT('Ctrl Pts',(-11.445157596175,41.9643802601783,3.93009166695208));
#292874=CARTESIAN_POINT('Ctrl Pts',(-11.9191153548007,41.8691479620093,
1.60866192649058));
#292875=CARTESIAN_POINT('Ctrl Pts',(-12.,41.8371973529385,0.804432365335873));
#292876=CARTESIAN_POINT('Ctrl Pts',(-12.,41.806249999844,-1.30451205393456E-14));
#292877=CARTESIAN_POINT('Origin',(-8.79029313101884E-14,130.96875,0.));
#292878=CARTESIAN_POINT('',(-12.,38.431249999856,1.32817776064042E-14));
#292879=CARTESIAN_POINT('',(-12.,38.806249999856,-4.22293736248536E-14));
#292880=CARTESIAN_POINT('',(-12.0000000000001,130.96875,-1.46957615897682E-15));
#292881=CARTESIAN_POINT('Ctrl Pts',(-12.,38.431249999856,3.19189119579733E-15));
#292882=CARTESIAN_POINT('Ctrl Pts',(-12.,38.4627470412595,0.818720730010485));
#292883=CARTESIAN_POINT('Ctrl Pts',(-11.9162164291614,38.4952804862953,
1.63715836389978));
#292884=CARTESIAN_POINT('Ctrl Pts',(-11.4311628703194,38.5911059325512,
3.97040090002212));
#292885=CARTESIAN_POINT('Ctrl Pts',(-10.8184656394873,38.6546039678113,
5.42186448815198));
#292886=CARTESIAN_POINT('Ctrl Pts',(-9.06027034794767,38.7767526520915,
8.02567327944428));
#292887=CARTESIAN_POINT('Ctrl Pts',(-7.92510055901498,38.8394136877261,
9.14839305516659));
#292888=CARTESIAN_POINT('Ctrl Pts',(-5.31399423879045,38.9657918611721,
10.8697885374707));
#292889=CARTESIAN_POINT('Ctrl Pts',(-3.87065742753112,39.0246786179399,
11.4633714113522));
#292890=CARTESIAN_POINT('Ctrl Pts',(-0.810952705910088,39.1484462738174,
12.0756027183795));
#292891=CARTESIAN_POINT('Ctrl Pts',(0.778355614096445,39.2127351458265,
12.077747465541));
#292892=CARTESIAN_POINT('Ctrl Pts',(3.85344412602932,39.3371250890941,11.4710661599005));
#292893=CARTESIAN_POINT('Ctrl Pts',(5.31067786234046,39.3965134969212,10.8734102690138));
#292894=CARTESIAN_POINT('Ctrl Pts',(7.90739026213174,39.5222632701861,9.15863281694728));
#292895=CARTESIAN_POINT('Ctrl Pts',(9.02404753124986,39.5839503239638,8.06061484314743));
#292896=CARTESIAN_POINT('Ctrl Pts',(10.7979807496565,39.7057725186941,5.47040624510141));
#292897=CARTESIAN_POINT('Ctrl Pts',(11.4263198233243,39.7703840195296,3.99508204807151));
#292898=CARTESIAN_POINT('Ctrl Pts',(12.0641932735035,39.8965053178702,0.923996180099739));
#292899=CARTESIAN_POINT('Ctrl Pts',(12.0826383631988,39.9548022036435,-0.63905682404472));
#292900=CARTESIAN_POINT('Ctrl Pts',(11.5216766930976,40.07961240592,-3.7010527694457));
#292901=CARTESIAN_POINT('Ctrl Pts',(10.9416475861037,40.1433689492677,-5.16985042399155));
#292902=CARTESIAN_POINT('Ctrl Pts',(9.24510211101141,40.2661728281079,-7.81072130431282));
#292903=CARTESIAN_POINT('Ctrl Pts',(8.14154860183542,40.3277356340467,-8.95514693641855));
#292904=CARTESIAN_POINT('Ctrl Pts',(5.57849184352484,40.4539671305243,-10.7365079553709));
#292905=CARTESIAN_POINT('Ctrl Pts',(4.14969608175823,40.5133912672661,-11.365394034471));
#292906=CARTESIAN_POINT('Ctrl Pts',(1.10175261287963,40.6366831704764,-12.0530444689562));
#292907=CARTESIAN_POINT('Ctrl Pts',(-0.490925135201216,40.7011083387142,
-12.0933310903339));
#292908=CARTESIAN_POINT('Ctrl Pts',(-3.57905925800803,40.8260259880267,
-11.5590620019779));
#292909=CARTESIAN_POINT('Ctrl Pts',(-5.04624884960544,40.8848966761853,
-10.9980408831662));
#292910=CARTESIAN_POINT('Ctrl Pts',(-7.68342360485882,41.0104348637905,
-9.34785405875282));
#292911=CARTESIAN_POINT('Ctrl Pts',(-8.82858459186161,41.0732661061744,
-8.27482610799069));
#292912=CARTESIAN_POINT('Ctrl Pts',(-10.6674568021903,41.194469297909,-5.72180756870018));
#292913=CARTESIAN_POINT('Ctrl Pts',(-11.3315107912658,41.2590856390456,
-4.25796203440441));
#292914=CARTESIAN_POINT('Ctrl Pts',(-11.896660693456,41.360034065031,-1.81757981643005));
#292915=CARTESIAN_POINT('Ctrl Pts',(-12.,41.3962698521127,-0.909259118006817));
#292916=CARTESIAN_POINT('Ctrl Pts',(-12.,41.431249999844,-2.692290834716E-14));
#292917=CARTESIAN_POINT('Ctrl Pts',(-12.,41.806249999844,-1.51267887105178E-14));
#292918=CARTESIAN_POINT('Ctrl Pts',(-12.,41.7778205860545,-0.738982119407512));
#292919=CARTESIAN_POINT('Ctrl Pts',(-11.9317419193925,41.7485339036576,
-1.47806932044144));
#292920=CARTESIAN_POINT('Ctrl Pts',(-11.5035983705324,41.655184985873,-3.76542920943106));
#292921=CARTESIAN_POINT('Ctrl Pts',(-10.9063587082155,41.5906054825755,
-5.25002648732262));
#292922=CARTESIAN_POINT('Ctrl Pts',(-9.18897205810974,41.4682807599009,
-7.87167067732582));
#292923=CARTESIAN_POINT('Ctrl Pts',(-8.09694473926842,41.407449509464,-8.99111433965235));
#292924=CARTESIAN_POINT('Ctrl Pts',(-5.5353796252676,41.281531283893,-10.7613527298956));
#292925=CARTESIAN_POINT('Ctrl Pts',(-4.08688731425502,41.2215680644128,
-11.3905441816188));
#292926=CARTESIAN_POINT('Ctrl Pts',(-1.02372569601573,41.0976605741296,
-12.0590118479223));
#292927=CARTESIAN_POINT('Ctrl Pts',(0.561999477521797,41.0335166434399,
-12.0893292334744));
#292928=CARTESIAN_POINT('Ctrl Pts',(3.63088463893472,40.909377630972,-11.5415894732783));
#292929=CARTESIAN_POINT('Ctrl Pts',(5.08649399878036,40.8508126621997,-10.9781210699601));
#292930=CARTESIAN_POINT('Ctrl Pts',(7.73822477815293,40.7243250672075,-9.30803825386205));
#292931=CARTESIAN_POINT('Ctrl Pts',(8.90020859356382,40.6606132834455,-8.20398555482632));
#292932=CARTESIAN_POINT('Ctrl Pts',(10.7100801257288,40.5390470177957,-5.63210653469817));
#292933=CARTESIAN_POINT('Ctrl Pts',(11.3499486695057,40.475792761556,-4.19580812973791));
#292934=CARTESIAN_POINT('Ctrl Pts',(12.0440596481023,40.3504538888403,-1.16333298212337));
#292935=CARTESIAN_POINT('Ctrl Pts',(12.0933754581578,40.2918840575548,0.403761734034306));
#292936=CARTESIAN_POINT('Ctrl Pts',(11.5875293687639,40.1665629969046,3.49694485298569));
#292937=CARTESIAN_POINT('Ctrl Pts',(11.0265311623774,40.1020529092557,4.99151333281217));
#292938=CARTESIAN_POINT('Ctrl Pts',(9.37508065496285,39.9791844834636,7.64871426241236));
#292939=CARTESIAN_POINT('Ctrl Pts',(8.31156816845547,39.9191889447782,8.79277523687751));
#292940=CARTESIAN_POINT('Ctrl Pts',(5.79091324092277,39.7930925420681,10.6268155293752));
#292941=CARTESIAN_POINT('Ctrl Pts',(4.35271268300412,39.7323209264614,11.2923734401967));
#292942=CARTESIAN_POINT('Ctrl Pts',(1.30408528138926,39.6090013575907,12.0314479104659));
#292943=CARTESIAN_POINT('Ctrl Pts',(-0.276747876045521,39.5450553131092,
12.0987463589307));
#292944=CARTESIAN_POINT('Ctrl Pts',(-3.35515052035818,39.4205313103708,
11.6248643914831));
#292945=CARTESIAN_POINT('Ctrl Pts',(-4.82464042947219,39.3621804905949,
11.095824236271));
#292946=CARTESIAN_POINT('Ctrl Pts',(-7.51915453353781,39.2357377403919,
9.48651371884892));
#292947=CARTESIAN_POINT('Ctrl Pts',(-8.7094080333007,39.1711199584178,8.40703084629784));
#292948=CARTESIAN_POINT('Ctrl Pts',(-10.5773933932437,39.0498235777697,
5.87654963587647));
#292949=CARTESIAN_POINT('Ctrl Pts',(-11.2488153785026,38.9871702481793,
4.45868949119449));
#292950=CARTESIAN_POINT('Ctrl Pts',(-11.8766392410368,38.8841629732154,
1.98515443060089));
#292951=CARTESIAN_POINT('Ctrl Pts',(-12.,38.8444686416769,0.993439159275016));
#292952=CARTESIAN_POINT('Ctrl Pts',(-12.,38.806249999856,1.66533453693773E-14));
#292953=CARTESIAN_POINT('Origin',(-8.79029313101884E-14,130.96875,0.));
#292954=CARTESIAN_POINT('',(-12.,35.431249999868,-5.15968803951284E-14));
#292955=CARTESIAN_POINT('',(-12.,35.806249999868,-1.33406439522195E-13));
#292956=CARTESIAN_POINT('',(-12.0000000000001,130.96875,-1.46957615897682E-15));
#292957=CARTESIAN_POINT('Ctrl Pts',(-12.,35.431249999868,-1.04360964314765E-13));
#292958=CARTESIAN_POINT('Ctrl Pts',(-12.,35.4700381716479,1.00824327937616));
#292959=CARTESIAN_POINT('Ctrl Pts',(-11.8729349682393,35.51034198472,2.01459756389213));
#292960=CARTESIAN_POINT('Ctrl Pts',(-11.2324217201602,35.6139509957666,
4.49965086560238));
#292961=CARTESIAN_POINT('Ctrl Pts',(-10.5560913389816,35.6764253426343,
5.91459768290572));
#292962=CARTESIAN_POINT('Ctrl Pts',(-8.67974020180297,35.7978165013443,
8.43755061085998));
#292963=CARTESIAN_POINT('Ctrl Pts',(-7.48615700668944,35.8624349960771,
9.51248052848435));
#292964=CARTESIAN_POINT('Ctrl Pts',(-4.78646793873384,35.9888231360038,
11.1123714934671));
#292965=CARTESIAN_POINT('Ctrl Pts',(-3.31497518795321,36.0471564367163,
11.6364104546645));
#292966=CARTESIAN_POINT('Ctrl Pts',(-0.235277726382621,36.171732815913,
12.099555273878));
#292967=CARTESIAN_POINT('Ctrl Pts',(1.34477456587885,36.2356472737348,12.0268993925935));
#292968=CARTESIAN_POINT('Ctrl Pts',(4.39121111942935,36.3588782209397,11.277574042516));
#292969=CARTESIAN_POINT('Ctrl Pts',(5.82788906599174,36.4197807200876,10.6067061703878));
#292970=CARTESIAN_POINT('Ctrl Pts',(8.34253553350199,36.5459016694114,8.76336354866154));
#292971=CARTESIAN_POINT('Ctrl Pts',(9.40187406344104,36.6057888893765,7.61571572231948));
#292972=CARTESIAN_POINT('Ctrl Pts',(11.0436327369964,36.7287334334172,4.9533871395502));
#292973=CARTESIAN_POINT('Ctrl Pts',(11.5993072771692,36.7932304407386,3.45742890019772));
#292974=CARTESIAN_POINT('Ctrl Pts',(12.0947375415577,36.9184829563752,0.362643204550438));
#292975=CARTESIAN_POINT('Ctrl Pts',(12.0400468780078,36.9770973226748,-1.20474787555495));
#292976=CARTESIAN_POINT('Ctrl Pts',(11.335412173293,37.1024718528658,-4.2347305225582));
#292977=CARTESIAN_POINT('Ctrl Pts',(10.6908673865189,37.1656814449742,-5.66834854358663));
#292978=CARTESIAN_POINT('Ctrl Pts',(8.87206294573137,37.2871439038344,-8.23462677611558));
#292979=CARTESIAN_POINT('Ctrl Pts',(7.70541453987611,37.3510495185937,-9.33540665419294));
#292980=CARTESIAN_POINT('Ctrl Pts',(5.04662834355365,37.4775546945405,-10.9965179503444));
#292981=CARTESIAN_POINT('Ctrl Pts',(3.58888934073206,37.5360763764805,-11.5547299900151));
#292982=CARTESIAN_POINT('Ctrl Pts',(0.518483215847364,37.6602769132132,
-12.0912010592991));
#292983=CARTESIAN_POINT('Ctrl Pts',(-1.0665498363905,37.7243928470083,-12.0552273362314));
#292984=CARTESIAN_POINT('Ctrl Pts',(-4.12755437962205,37.8482130817744,
-11.375976411187));
#292985=CARTESIAN_POINT('Ctrl Pts',(-5.57449640280557,37.9082892707063,
-10.7412540867963));
#292986=CARTESIAN_POINT('Ctrl Pts',(-8.1298661695661,38.0342357156939,-8.96130166659882));
#292987=CARTESIAN_POINT('Ctrl Pts',(-9.21756461347896,38.0949293589744,
-7.83810797722948));
#292988=CARTESIAN_POINT('Ctrl Pts',(-10.9249731035212,38.2173392686393,
-5.21100737200903));
#292989=CARTESIAN_POINT('Ctrl Pts',(-11.5167262601255,38.2819104729188,
-3.72484314150043));
#292990=CARTESIAN_POINT('Ctrl Pts',(-11.9342867633289,38.3746336494357,
-1.45030986554002));
#292991=CARTESIAN_POINT('Ctrl Pts',(-12.,38.4033555800282,-0.725075713364724));
#292992=CARTESIAN_POINT('Ctrl Pts',(-12.,38.431249999856,1.13797860024079E-14));
#292993=CARTESIAN_POINT('Ctrl Pts',(-12.,38.806249999856,1.95676808090184E-14));
#292994=CARTESIAN_POINT('Ctrl Pts',(-12.,38.7848368006228,-0.556605615219962));
#292995=CARTESIAN_POINT('Ctrl Pts',(-11.9612756878353,38.7629201691543,
-1.11371494261193));
#292996=CARTESIAN_POINT('Ctrl Pts',(-11.6644552582536,38.6778210346364,
-3.22930293378464));
#292997=CARTESIAN_POINT('Ctrl Pts',(-11.1394629688195,38.6134136771892,
-4.73290011993798));
#292998=CARTESIAN_POINT('Ctrl Pts',(-9.55360537494578,38.4900489314371,
-7.42431460952982));
#292999=CARTESIAN_POINT('Ctrl Pts',(-8.5182607742844,38.4307148678992,-8.59250029243608));
#293000=CARTESIAN_POINT('Ctrl Pts',(-6.03825498759269,38.3044605264228,
-10.4891319933311));
#293001=CARTESIAN_POINT('Ctrl Pts',(-4.61041277056975,38.242745113982,-11.1904554442826));
#293002=CARTESIAN_POINT('Ctrl Pts',(-1.57687408184143,38.1200358963687,
-11.9982836169922));
#293003=CARTESIAN_POINT('Ctrl Pts',(-0.00162053623311592,38.0563155519266,
-12.1014523639863));
#293004=CARTESIAN_POINT('Ctrl Pts',(3.08504138152381,37.9314574545594,-11.6996554205751));
#293005=CARTESIAN_POINT('Ctrl Pts',(4.56790597917435,37.8731585374633,-11.20417964339));
#293006=CARTESIAN_POINT('Ctrl Pts',(7.29667881694916,37.7470971393136,-9.65806131879168));
#293007=CARTESIAN_POINT('Ctrl Pts',(8.50889043244637,37.6824893721698,-8.60922240837434));
#293008=CARTESIAN_POINT('Ctrl Pts',(10.4324769840663,37.560577044529,-6.12936387313183));
#293009=CARTESIAN_POINT('Ctrl Pts',(11.1365970977192,37.4990487018181,-4.7309910451774));
#293010=CARTESIAN_POINT('Ctrl Pts',(11.9761702450188,37.373268480201,-1.73430718515646));
#293011=CARTESIAN_POINT('Ctrl Pts',(12.0999915756348,37.3137878947727,-0.163447609588439));
#293012=CARTESIAN_POINT('Ctrl Pts',(11.7376918656824,37.1894806492918,2.9500238740173));
#293013=CARTESIAN_POINT('Ctrl Pts',(11.2501446104752,37.1252153578106,4.46209488687447));
#293014=CARTESIAN_POINT('Ctrl Pts',(9.73263915500905,37.0013800721998,7.18794934595158));
#293015=CARTESIAN_POINT('Ctrl Pts',(8.72646017235344,36.9425590237925,8.38091488005002));
#293016=CARTESIAN_POINT('Ctrl Pts',(6.28879684496449,36.8161605437619,10.341888226191));
#293017=CARTESIAN_POINT('Ctrl Pts',(4.87189218036381,36.7533221782981,11.0800661200621));
#293018=CARTESIAN_POINT('Ctrl Pts',(1.85470485672127,36.6312743872966,11.9580191975185));
#293019=CARTESIAN_POINT('Ctrl Pts',(0.285969466989008,36.5678177077983,
12.097608011535));
#293020=CARTESIAN_POINT('Ctrl Pts',(-2.80808018452431,36.4426607703231,
11.7695039807635));
#293021=CARTESIAN_POINT('Ctrl Pts',(-4.30444491654658,36.3842567180682,
11.3083293063412));
#293022=CARTESIAN_POINT('Ctrl Pts',(-7.06708425206928,36.2586202861418,
9.82669765417226));
#293023=CARTESIAN_POINT('Ctrl Pts',(-8.30078803454533,36.1940580917055,
8.80935689303109));
#293024=CARTESIAN_POINT('Ctrl Pts',(-10.2798691440691,36.0715647349362,
6.38144285677968));
#293025=CARTESIAN_POINT('Ctrl Pts',(-11.016825756956,36.0110036067955,5.00282570486589));
#293026=CARTESIAN_POINT('Ctrl Pts',(-11.8224444004248,35.8999944688486,
2.37906263930499));
#293027=CARTESIAN_POINT('Ctrl Pts',(-12.0000000000001,35.8521007994926,
1.19182623088897));
#293028=CARTESIAN_POINT('Ctrl Pts',(-12.,35.806249999868,-2.27873275804313E-13));
#293029=CARTESIAN_POINT('Origin',(-8.79029313101884E-14,130.96875,0.));
#293030=CARTESIAN_POINT('',(-12.,32.43124999988,-1.15434704311075E-13));
#293031=CARTESIAN_POINT('',(-12.,32.80624999988,-5.31445805606718E-15));
#293032=CARTESIAN_POINT('',(-12.0000000000001,130.96875,-1.46957615897682E-15));
#293033=CARTESIAN_POINT('Ctrl Pts',(-12.,32.43124999988,-2.18158824338843E-13));
#293034=CARTESIAN_POINT('Ctrl Pts',(-12.0000000000001,32.4776762727195,
1.20678483746527));
#293035=CARTESIAN_POINT('Ctrl Pts',(-11.8179589645538,32.5261907975428,
2.40870209300642));
#293036=CARTESIAN_POINT('Ctrl Pts',(-10.9982644188703,32.6377969953442,
5.0434113412201));
#293037=CARTESIAN_POINT('Ctrl Pts',(-10.2563850742601,32.698227446797,6.41905095562799));
#293038=CARTESIAN_POINT('Ctrl Pts',(-8.26901764732399,32.8208045715522,
8.83908300931383));
#293039=CARTESIAN_POINT('Ctrl Pts',(-7.03214309924002,32.8853568146657,
9.85164104839903));
#293040=CARTESIAN_POINT('Ctrl Pts',(-4.26447583888615,33.0109258659356,
11.3235184271393));
#293041=CARTESIAN_POINT('Ctrl Pts',(-2.76608200565986,33.0693596323568,
11.7794987318951));
#293042=CARTESIAN_POINT('Ctrl Pts',(0.328992884834674,33.1945580416199,
12.0964443517389));
#293043=CARTESIAN_POINT('Ctrl Pts',(1.89667010069928,33.2579719170862,11.9513643438712));
#293044=CARTESIAN_POINT('Ctrl Pts',(4.91129963068495,33.3799162431608,11.0628074664535));
#293045=CARTESIAN_POINT('Ctrl Pts',(6.3265156265557,33.4429385666294,10.3190227205775));
#293046=CARTESIAN_POINT('Ctrl Pts',(8.75769482069915,33.5693572706409,8.34827414059132));
#293047=CARTESIAN_POINT('Ctrl Pts',(9.75942334147266,33.6281153813829,7.15154516538066));
#293048=CARTESIAN_POINT('Ctrl Pts',(11.2664628787054,33.7520185502841,4.42052559388299));
#293049=CARTESIAN_POINT('Ctrl Pts',(11.7482850488903,33.816258979221,2.90724065456717));
#293050=CARTESIAN_POINT('Ctrl Pts',(12.0994052463512,33.9404810327821,-0.207648830224786));
#293051=CARTESIAN_POINT('Ctrl Pts',(11.9697396871303,34.0000594305946,-1.77877097455616));
#293052=CARTESIAN_POINT('Ctrl Pts',(11.1187907608595,34.125870314321,-4.77255563778874));
#293053=CARTESIAN_POINT('Ctrl Pts',(10.4096637930931,34.1872405346318,-6.16792808916501));
#293054=CARTESIAN_POINT('Ctrl Pts',(8.47759190364955,34.3092439253597,-8.63993753467918));
#293055=CARTESIAN_POINT('Ctrl Pts',(7.26206580242804,34.3738470647927,-9.68401981234569));
#293056=CARTESIAN_POINT('Ctrl Pts',(4.52809320359843,34.499846399196,-11.2203709724452));
#293057=CARTESIAN_POINT('Ctrl Pts',(3.04317416810518,34.5581510189295,-11.7106554039441));
#293058=CARTESIAN_POINT('Ctrl Pts',(-0.0446744412204195,34.6830571189791,
-12.1012993876648));
#293059=CARTESIAN_POINT('Ctrl Pts',(-1.61899415642968,34.746739689188,-11.9926018972619));
#293060=CARTESIAN_POINT('Ctrl Pts',(-4.65011840450887,34.8693512406255,
-11.1741502096888));
#293061=CARTESIAN_POINT('Ctrl Pts',(-6.07632860852273,34.9312263422972,
-10.4672682898571));
#293062=CARTESIAN_POINT('Ctrl Pts',(-8.54997851100817,35.0575036507789,
-8.56092250731231));
#293063=CARTESIAN_POINT('Ctrl Pts',(-9.5809337182492,35.1167493351784,-7.38899455347827));
#293064=CARTESIAN_POINT('Ctrl Pts',(-11.1565315742162,35.2401877322821,
-4.69233201097822));
#293065=CARTESIAN_POINT('Ctrl Pts',(-11.675897777898,35.3045760268348,-3.18740231154562));
#293066=CARTESIAN_POINT('Ctrl Pts',(-11.9632185252926,35.3890323308912,
-1.08543714878296));
#293067=CARTESIAN_POINT('Ctrl Pts',(-12.,35.4103808839011,-0.542462945650476));
#293068=CARTESIAN_POINT('Ctrl Pts',(-12.,35.431249999868,-1.13103970633688E-13));
#293069=CARTESIAN_POINT('Ctrl Pts',(-12.,35.806249999868,-2.04627981226224E-13));
#293070=CARTESIAN_POINT('Ctrl Pts',(-12.,35.7920639646029,-0.368745781529345));
#293071=CARTESIAN_POINT('Ctrl Pts',(-11.9830038542012,35.7776492037367,
-0.737914576754738));
#293072=CARTESIAN_POINT('Ctrl Pts',(-11.8041633160057,35.7011049692098,
-2.66946411788623));
#293073=CARTESIAN_POINT('Ctrl Pts',(-11.354105989905,35.6370174959843,-4.18909421482921));
#293074=CARTESIAN_POINT('Ctrl Pts',(-9.90522339156164,35.5127571124111,
-6.94829540786313));
#293075=CARTESIAN_POINT('Ctrl Pts',(-8.92815820661399,35.4542744622871,
-8.1657947673545));
#293076=CARTESIAN_POINT('Ctrl Pts',(-6.53302381849094,35.3277523578375,
-10.1905036328583));
#293077=CARTESIAN_POINT('Ctrl Pts',(-5.12726325995961,35.2636521554673,
-10.9652742067382));
#293078=CARTESIAN_POINT('Ctrl Pts',(-2.12709803906788,35.1422929229861,
-11.912123170417));
#293079=CARTESIAN_POINT('Ctrl Pts',(-0.565577341076917,35.0791280839252,
-12.0873085786455));
#293080=CARTESIAN_POINT('Ctrl Pts',(2.52752654738964,34.9540094033686,-11.8323663023729));
#293081=CARTESIAN_POINT('Ctrl Pts',(4.03027763949432,34.8956068183643,-11.4083384908807));
#293082=CARTESIAN_POINT('Ctrl Pts',(6.81102621451258,34.7712034870444,-10.0034944167991));
#293083=CARTESIAN_POINT('Ctrl Pts',(8.05881998447991,34.7071892601766,-9.02859354763777));
#293084=CARTESIAN_POINT('Ctrl Pts',(10.1082156653494,34.5836740271163,-6.65448064341902));
#293085=CARTESIAN_POINT('Ctrl Pts',(10.8902599029851,34.5231833580987,-5.27829725337419));
#293086=CARTESIAN_POINT('Ctrl Pts',(11.8745727165592,34.3971432211835,-2.32188603377452));
#293087=CARTESIAN_POINT('Ctrl Pts',(12.0747742808167,34.3368927320492,-0.772218541801659));
#293088=CARTESIAN_POINT('Ctrl Pts',(11.873227379025,34.214197585593,2.35158047736658));
#293089=CARTESIAN_POINT('Ctrl Pts',(11.4600717986303,34.1496609674394,3.8948755610043));
#293090=CARTESIAN_POINT('Ctrl Pts',(10.0721373165819,34.024189754806,6.70535377430503));
#293091=CARTESIAN_POINT('Ctrl Pts',(9.12121355161991,33.9657071760561,7.95066998817524));
#293092=CARTESIAN_POINT('Ctrl Pts',(6.79299867096633,33.8404511283386,10.0142372207861));
#293093=CARTESIAN_POINT('Ctrl Pts',(5.43608279131537,33.7770998455958,10.8110619628864));
#293094=CARTESIAN_POINT('Ctrl Pts',(2.46898927635769,33.6553051667091,11.8497082510787));
#293095=CARTESIAN_POINT('Ctrl Pts',(0.884112711395966,33.5920131103,12.0718827108435));
#293096=CARTESIAN_POINT('Ctrl Pts',(-2.2418265845094,33.4655662096119,11.8897137412496));
#293097=CARTESIAN_POINT('Ctrl Pts',(-3.75366399717397,33.4068913516675,
11.5022228938451));
#293098=CARTESIAN_POINT('Ctrl Pts',(-6.57030474952821,33.2828925745752,
10.1637951032527));
#293099=CARTESIAN_POINT('Ctrl Pts',(-7.84394492687112,33.2186892972338,
9.21651758465373));
#293100=CARTESIAN_POINT('Ctrl Pts',(-9.94707858033792,33.0945911471668,
6.89185204586521));
#293101=CARTESIAN_POINT('Ctrl Pts',(-10.75907758468,33.0348655046159,5.53933429402285));
#293102=CARTESIAN_POINT('Ctrl Pts',(-11.7598464659617,32.915546560012,2.76297779607306));
#293103=CARTESIAN_POINT('Ctrl Pts',(-12.,32.8595735697097,1.38607024889398));
#293104=CARTESIAN_POINT('Ctrl Pts',(-12.,32.80624999988,3.88578058618805E-15));
#293105=CARTESIAN_POINT('Origin',(-8.79029313101884E-14,130.96875,0.));
#293106=CARTESIAN_POINT('',(-12.,29.431249999892,-5.31060898192282E-14));
#293107=CARTESIAN_POINT('',(-12.,29.806249999892,-2.57148061335544E-14));
#293108=CARTESIAN_POINT('',(-12.0000000000001,130.96875,-1.46957615897682E-15));
#293109=CARTESIAN_POINT('Ctrl Pts',(-12.,29.431249999892,-9.32587340685131E-14));
#293110=CARTESIAN_POINT('Ctrl Pts',(-12.,29.4851488241481,1.40102316837458));
#293111=CARTESIAN_POINT('Ctrl Pts',(-11.7546358261363,29.541753991599,2.79267022061044));
#293112=CARTESIAN_POINT('Ctrl Pts',(-10.7438889970809,29.6610106605539,
5.56416592000471));
#293113=CARTESIAN_POINT('Ctrl Pts',(-9.93826035902713,29.7200942929683,
6.90087635712038));
#293114=CARTESIAN_POINT('Ctrl Pts',(-7.8444929696234,29.8436744278595,9.2166465168711));
#293115=CARTESIAN_POINT('Ctrl Pts',(-6.56786190030818,29.9080228891066,
10.1659136415296));
#293116=CARTESIAN_POINT('Ctrl Pts',(-3.73633664274598,30.0326315459472,
11.5095052889258));
#293117=CARTESIAN_POINT('Ctrl Pts',(-2.21157294657299,30.0917899949855,
11.8969668898356));
#293118=CARTESIAN_POINT('Ctrl Pts',(0.895057612379632,30.2174558408568,
12.0668979865983));
#293119=CARTESIAN_POINT('Ctrl Pts',(2.4472716297175,30.2795885355239,11.8499569001875));
#293120=CARTESIAN_POINT('Ctrl Pts',(5.41749433871223,30.4011637263426,10.8248489145821));
#293121=CARTESIAN_POINT('Ctrl Pts',(6.80210151923264,30.4657813504751,10.0128775729825));
#293122=CARTESIAN_POINT('Ctrl Pts',(9.14338880188783,30.5920593815452,7.92431988258037));
#293123=CARTESIAN_POINT('Ctrl Pts',(10.0883236951527,30.6503681744823,6.67998170676279));
#293124=CARTESIAN_POINT('Ctrl Pts',(11.4610834689155,30.7750453012285,3.88521406347696));
#293125=CARTESIAN_POINT('Ctrl Pts',(11.8697061866883,30.8388952901868,2.35829411145753));
#293126=CARTESIAN_POINT('Ctrl Pts',(12.0778585345691,30.9619488763262,-0.772675797213721));
#293127=CARTESIAN_POINT('Ctrl Pts',(11.8728581235085,31.0231198087666,-2.34671393167774));
#293128=CARTESIAN_POINT('Ctrl Pts',(10.8756316476451,31.1492881933354,-5.30226286314234));
#293129=CARTESIAN_POINT('Ctrl Pts',(10.1022106565283,31.2089715090149,-6.65872709649208));
#293130=CARTESIAN_POINT('Ctrl Pts',(8.06197802432647,31.3320641370475,-9.02767772633765));
#293131=CARTESIAN_POINT('Ctrl Pts',(6.8051221704812,31.3965330449699,-10.0092289052083));
#293132=CARTESIAN_POINT('Ctrl Pts',(4.00556095415405,31.5216473949094,-11.4180839686849));
#293133=CARTESIAN_POINT('Ctrl Pts',(2.49413853287218,31.5803599769125,-11.840455574618));
#293134=CARTESIAN_POINT('Ctrl Pts',(-0.606971283075425,31.7058025040382,
-12.0852335809304));
#293135=CARTESIAN_POINT('Ctrl Pts',(-2.16735607895474,31.7689213949195,
-11.9047965025742));
#293136=CARTESIAN_POINT('Ctrl Pts',(-5.16492051548911,31.8901754234635,
-10.9477503712494));
#293137=CARTESIAN_POINT('Ctrl Pts',(-6.56899609687767,31.9544757824724,
-10.1675305909724));
#293138=CARTESIAN_POINT('Ctrl Pts',(-8.95775373601538,32.0810145793702,
-8.13334282430559));
#293139=CARTESIAN_POINT('Ctrl Pts',(-9.93046914074174,32.1394614895692,
-6.91219539265034));
#293140=CARTESIAN_POINT('Ctrl Pts',(-11.3690686936999,32.2637815229155,
-4.14810252474221));
#293141=CARTESIAN_POINT('Ctrl Pts',(-11.8135187518015,32.3278393648193,
-2.6274207399871));
#293142=CARTESIAN_POINT('Ctrl Pts',(-11.9842718072799,32.4037445737492,
-0.709853976657044));
#293143=CARTESIAN_POINT('Ctrl Pts',(-12.,32.4176033869892,-0.354724265208347));
#293144=CARTESIAN_POINT('Ctrl Pts',(-12.,32.43124999988,-2.08791317568569E-13));
#293145=CARTESIAN_POINT('Ctrl Pts',(-12.,32.80624999988,4.5102810375397E-16));
#293146=CARTESIAN_POINT('Ctrl Pts',(-12.,32.8000424641438,-0.161356050061035));
#293147=CARTESIAN_POINT('Ctrl Pts',(-11.9967455546346,32.7937895901545,
-0.322833170037546));
#293148=CARTESIAN_POINT('Ctrl Pts',(-11.9262084743953,32.7257288838371,
-2.06905540512378));
#293149=CARTESIAN_POINT('Ctrl Pts',(-11.5486544106732,32.6611338492227,
-3.62543657544074));
#293150=CARTESIAN_POINT('Ctrl Pts',(-10.2255683019167,32.535225413725,-6.4683502881123));
#293151=CARTESIAN_POINT('Ctrl Pts',(-9.30563617959406,32.4769061387655,
-7.73349450970906));
#293152=CARTESIAN_POINT('Ctrl Pts',(-7.02632893219277,32.3519325782973,
-9.85249633764293));
#293153=CARTESIAN_POINT('Ctrl Pts',(-5.685223823736,32.2883058052959,-10.6826694433699));
#293154=CARTESIAN_POINT('Ctrl Pts',(-2.74576725643883,32.1658365822708,
-11.7877250338585));
#293155=CARTESIAN_POINT('Ctrl Pts',(-1.17364211102602,32.1037248205395,
-12.0462668531426));
#293156=CARTESIAN_POINT('Ctrl Pts',(1.94890553891517,31.9774151148127,-11.941229191595));
#293157=CARTESIAN_POINT('Ctrl Pts',(3.46985003208625,31.9182901507538,-11.5910027489076));
#293158=CARTESIAN_POINT('Ctrl Pts',(6.32201899278502,31.7947470883891,-10.3206420147937));
#293159=CARTESIAN_POINT('Ctrl Pts',(7.62129871611257,31.7303877946302,-9.40209248895725));
#293160=CARTESIAN_POINT('Ctrl Pts',(9.77828338826287,31.6057376318048,-7.12832969617556));
#293161=CARTESIAN_POINT('Ctrl Pts',(10.6202783134745,31.5466204539994,-5.79978884346416));
#293162=CARTESIAN_POINT('Ctrl Pts',(11.7474348874117,31.4209711163855,-2.8999486463113));
#293163=CARTESIAN_POINT('Ctrl Pts',(12.0237302200211,31.3587494337806,-1.35693759319928));
#293164=CARTESIAN_POINT('Ctrl Pts',(11.972474690382,31.2372225916453,1.78532564615453));
#293165=CARTESIAN_POINT('Ctrl Pts',(11.63090385625,31.1726044433631,3.35399928337155));
#293166=CARTESIAN_POINT('Ctrl Pts',(10.3731262802374,31.0462969511876,6.22850593462641));
#293167=CARTESIAN_POINT('Ctrl Pts',(9.48407280831626,30.9879829679234,7.51321676272817));
#293168=CARTESIAN_POINT('Ctrl Pts',(7.2541253814875,30.8633321832837,9.68658109167525));
#293169=CARTESIAN_POINT('Ctrl Pts',(5.92950656980374,30.7994648455449,10.5495634275673));
#293170=CARTESIAN_POINT('Ctrl Pts',(3.01830377911047,30.6763639699012,11.7200733600513));
#293171=CARTESIAN_POINT('Ctrl Pts',(1.45894185072004,30.6152654374406,12.0142368666767));
#293172=CARTESIAN_POINT('Ctrl Pts',(-1.65980483796559,30.4891094838263,
11.9849352026845));
#293173=CARTESIAN_POINT('Ctrl Pts',(-3.18954833416544,30.4293734498415,
11.6713473717854));
#293174=CARTESIAN_POINT('Ctrl Pts',(-6.07557898484373,30.3063197608035,
10.4681755582203));
#293175=CARTESIAN_POINT('Ctrl Pts',(-7.39932882970642,30.2418431144289,
9.57837059156762));
#293176=CARTESIAN_POINT('Ctrl Pts',(-9.60829173472751,30.1166917984454,
7.35507195419466));
#293177=CARTESIAN_POINT('Ctrl Pts',(-10.4792481496153,30.0580065703022,
6.04993124133885));
#293178=CARTESIAN_POINT('Ctrl Pts',(-11.6756085493199,29.9325817407516,
3.17841249757036));
#293179=CARTESIAN_POINT('Ctrl Pts',(-11.9890112143639,29.869438496906,1.63892450753172));
#293180=CARTESIAN_POINT('Ctrl Pts',(-11.9999054182355,29.8083678250883,
0.0550191180779561));
#293181=CARTESIAN_POINT('Ctrl Pts',(-12.,29.807308236395,0.027507350646264));
#293182=CARTESIAN_POINT('Ctrl Pts',(-12.,29.806249999892,-1.04101115714572E-13));
#293183=CARTESIAN_POINT('Origin',(-8.79029313101884E-14,130.96875,0.));
#293184=CARTESIAN_POINT('',(-12.,26.4312499994205,-6.28404526952038E-9));
#293185=CARTESIAN_POINT('',(-12.,26.806249999904,3.01779842624183E-14));
#293186=CARTESIAN_POINT('',(-12.0000000000001,130.96875,-1.46957615897682E-15));
#293187=CARTESIAN_POINT('Ctrl Pts',(-12.,26.4312499994205,-1.25681301308442E-8));
#293188=CARTESIAN_POINT('Ctrl Pts',(-12.0000000000063,26.4314790020448,
0.005952584484202));
#293189=CARTESIAN_POINT('Ctrl Pts',(-11.9999955708361,26.4317080680303,
0.0119053893945655));
#293190=CARTESIAN_POINT('Ctrl Pts',(-11.9976172228562,26.4932197505189,
1.61004119241557));
#293191=CARTESIAN_POINT('Ctrl Pts',(-11.678391503657,26.5578345097249,3.18588710337945));
#293192=CARTESIAN_POINT('Ctrl Pts',(-10.4610723416985,26.6843687439975,
6.0794333281055));
#293193=CARTESIAN_POINT('Ctrl Pts',(-9.59098918588322,26.7427574557944,
7.37607697614277));
#293194=CARTESIAN_POINT('Ctrl Pts',(-7.39166162622063,26.8671898824307,
9.58240212898549));
#293195=CARTESIAN_POINT('Ctrl Pts',(-6.07752317006222,26.931188229299,10.4653194827716));
#293196=CARTESIAN_POINT('Ctrl Pts',(-3.18402088459822,27.0546573220819,
11.6756787271243));
#293197=CARTESIAN_POINT('Ctrl Pts',(-1.63251893587116,27.1152132217633,
11.9914301900934));
#293198=CARTESIAN_POINT('Ctrl Pts',(1.4836990924161,27.2412668889159,12.0081169930264));
#293199=CARTESIAN_POINT('Ctrl Pts',(3.01871679408634,27.3014552565358,11.716802448988));
#293200=CARTESIAN_POINT('Ctrl Pts',(5.92481138151768,27.4241919260214,10.5545796385704));
#293201=CARTESIAN_POINT('Ctrl Pts',(7.26306823652372,27.488722584878,9.6824701750163));
#293202=CARTESIAN_POINT('Ctrl Pts',(9.50314964785391,27.6141585383666,7.49003106375069));
#293203=CARTESIAN_POINT('Ctrl Pts',(10.3914615484667,27.6726602946857,6.1990252522971));
#293204=CARTESIAN_POINT('Ctrl Pts',(11.6293109061408,27.7979363907583,3.34485320306925));
#293205=CARTESIAN_POINT('Ctrl Pts',(11.9649950199946,27.8612649924479,1.80778678146149));
#293206=CARTESIAN_POINT('Ctrl Pts',(12.0303715249327,27.9830059032825,-1.33545268582758));
#293207=CARTESIAN_POINT('Ctrl Pts',(11.7489204696593,28.0463959052348,-2.91147312204396));
#293208=CARTESIAN_POINT('Ctrl Pts',(10.6039167708586,28.172852637454,-5.82650150959838));
#293209=CARTESIAN_POINT('Ctrl Pts',(9.76567299451591,28.2314997836282,-7.14302793176961));
#293210=CARTESIAN_POINT('Ctrl Pts',(7.61820968020575,28.3555321834124,-9.40391356928499));
#293211=CARTESIAN_POINT('Ctrl Pts',(6.32224180580404,28.4197217744015,-10.3198840220338));
#293212=CARTESIAN_POINT('Ctrl Pts',(3.45901026767688,28.5437752099896,-11.5964839511652));
#293213=CARTESIAN_POINT('Ctrl Pts',(1.92071620599176,28.6035553972944,-11.9479715018053));
#293214=CARTESIAN_POINT('Ctrl Pts',(-1.1909499873322,28.7294249388549,-12.040934522847));
#293215=CARTESIAN_POINT('Ctrl Pts',(-2.7346005176524,28.7904977009883,-11.7866081716702));
#293216=CARTESIAN_POINT('Ctrl Pts',(-5.67314045061089,28.9126761759063,
-10.6925193683012));
#293217=CARTESIAN_POINT('Ctrl Pts',(-7.03485626457987,28.9772678956048,
-9.85013026499296));
#293218=CARTESIAN_POINT('Ctrl Pts',(-9.32579612279864,29.1031433497616,
-7.70920706652483));
#293219=CARTESIAN_POINT('Ctrl Pts',(-10.2425208237552,29.1614697147043,
-6.4415146649703));
#293220=CARTESIAN_POINT('Ctrl Pts',(-11.5481671297799,29.2864669548987,
-3.61661964098504));
#293221=CARTESIAN_POINT('Ctrl Pts',(-11.9204183427465,29.3500733461147,
-2.08421384703015));
#293222=CARTESIAN_POINT('Ctrl Pts',(-11.9961974439967,29.4177771295152,
-0.348972550675605));
#293223=CARTESIAN_POINT('Ctrl Pts',(-12.,29.4245400561049,-0.174415431763315));
#293224=CARTESIAN_POINT('Ctrl Pts',(-12.,29.431249999892,-1.0842021724855E-13));
#293225=CARTESIAN_POINT('Ctrl Pts',(-12.,29.806249999892,-1.08801856413265E-13));
#293226=CARTESIAN_POINT('Ctrl Pts',(-12.,29.7461635566442,-1.56186151103106));
#293227=CARTESIAN_POINT('Ctrl Pts',(-11.6950686578715,29.6828245025684,
-3.1091918087787));
#293228=CARTESIAN_POINT('Ctrl Pts',(-10.5148572656756,29.5574045423193,
-5.98583111260254));
#293229=CARTESIAN_POINT('Ctrl Pts',(-9.65660561959846,29.4989392255624,
-7.28988416406018));
#293230=CARTESIAN_POINT('Ctrl Pts',(-7.47648354397054,29.3746505852464,
-9.51659596253284));
#293231=CARTESIAN_POINT('Ctrl Pts',(-6.16901356837322,29.3105769874857,
-10.4118566312308));
#293232=CARTESIAN_POINT('Ctrl Pts',(-3.28667891078174,29.1868858422458,
-11.6469259874971));
#293233=CARTESIAN_POINT('Ctrl Pts',(-1.74008355600073,29.1266378583166,
-11.9760291153752));
#293234=CARTESIAN_POINT('Ctrl Pts',(1.37448685209422,29.0006508388008,-12.0211925873615));
#293235=CARTESIAN_POINT('Ctrl Pts',(2.91274434176103,28.9401517936605,-11.743680215496));
#293236=CARTESIAN_POINT('Ctrl Pts',(5.83107365352603,28.8176188307369,-10.6068646486473));
#293237=CARTESIAN_POINT('Ctrl Pts',(7.17817733977478,28.7530612262002,-9.74579850908251));
#293238=CARTESIAN_POINT('Ctrl Pts',(9.43735700957167,28.6274564438988,-7.57254521072166));
#293239=CARTESIAN_POINT('Ctrl Pts',(10.3363302801933,28.5690388406801,-6.29026256566099));
#293240=CARTESIAN_POINT('Ctrl Pts',(11.5996396563453,28.4438622385919,-3.44694918231876));
#293241=CARTESIAN_POINT('Ctrl Pts',(11.9490339098776,28.3804256333046,-1.91153005543417));
#293242=CARTESIAN_POINT('Ctrl Pts',(12.0412893187095,28.2584264836826,1.22968847603223));
#293243=CARTESIAN_POINT('Ctrl Pts',(11.7743308323104,28.195501897565,2.80541482406902));
#293244=CARTESIAN_POINT('Ctrl Pts',(10.6572910223695,28.0690938346845,5.72826413975934));
#293245=CARTESIAN_POINT('Ctrl Pts',(9.83130606094285,28.0103029298356,7.05239846244492));
#293246=CARTESIAN_POINT('Ctrl Pts',(7.7039605726298,27.886435546933,9.33403355125254));
#293247=CARTESIAN_POINT('Ctrl Pts',(6.41517677553145,27.8221818590215,10.2625878578183));
#293248=CARTESIAN_POINT('Ctrl Pts',(3.56378173465436,27.6979146157577,11.5644717555374));
#293249=CARTESIAN_POINT('Ctrl Pts',(2.0305743381716,27.6383884572968,11.9295549490862));
#293250=CARTESIAN_POINT('Ctrl Pts',(-1.07924184233729,27.5125937503266,
12.0515849848931));
#293251=CARTESIAN_POINT('Ctrl Pts',(-2.62614400459274,27.4511403249807,
11.811369716088));
#293252=CARTESIAN_POINT('Ctrl Pts',(-5.57677391434579,27.3291850153474,
10.7433073328657));
#293253=CARTESIAN_POINT('Ctrl Pts',(-6.94722786573379,27.2645793236449,
9.91235760254589));
#293254=CARTESIAN_POINT('Ctrl Pts',(-9.25729741802083,27.1385470230812,
7.79116744626057));
#293255=CARTESIAN_POINT('Ctrl Pts',(-10.184729240557,27.0802458792577,6.53231540738293));
#293256=CARTESIAN_POINT('Ctrl Pts',(-11.5158750392046,26.9553650750171,
3.71873225757449));
#293257=CARTESIAN_POINT('Ctrl Pts',(-11.9019263496545,26.8916624070597,
2.18830781033492));
#293258=CARTESIAN_POINT('Ctrl Pts',(-11.9945473038564,26.8223955724385,
0.417909473500312));
#293259=CARTESIAN_POINT('Ctrl Pts',(-12.,26.8142850295081,0.208859150254401));
#293260=CARTESIAN_POINT('Ctrl Pts',(-12.,26.806249999904,1.13312137450805E-13));
#293261=CARTESIAN_POINT('Origin',(-8.79029313101884E-14,130.96875,0.));
#293262=CARTESIAN_POINT('',(-12.,23.431249999916,7.61134619062841E-14));
#293263=CARTESIAN_POINT('',(-12.,23.806249999916,1.38875757267125E-13));
#293264=CARTESIAN_POINT('',(-12.0000000000001,130.96875,-1.46957615897682E-15));
#293265=CARTESIAN_POINT('Ctrl Pts',(-12.,23.431249999916,1.11577413974828E-13));
#293266=CARTESIAN_POINT('Ctrl Pts',(-12.,23.4398130406759,0.22258404820464));
#293267=CARTESIAN_POINT('Ctrl Pts',(-11.9938071335293,23.4484616365627,
0.445379795782725));
#293268=CARTESIAN_POINT('Ctrl Pts',(-11.8943033853353,23.518351927683,2.22974764099004));
#293269=CARTESIAN_POINT('Ctrl Pts',(-11.5027536396383,23.5820916451671,
3.75934858799651));
#293270=CARTESIAN_POINT('Ctrl Pts',(-10.1614602463391,23.7069243478206,
6.56838425218786));
#293271=CARTESIAN_POINT('Ctrl Pts',(-9.22976384960113,23.7652217461412,
7.82370706132516));
#293272=CARTESIAN_POINT('Ctrl Pts',(-6.91208163660612,23.8913151486123,
9.93698914294296));
#293273=CARTESIAN_POINT('Ctrl Pts',(-5.53816396297601,23.9559250022048,
10.7633465114));
#293274=CARTESIAN_POINT('Ctrl Pts',(-2.58274047876639,24.0777894527795,
11.8209897106908));
#293275=CARTESIAN_POINT('Ctrl Pts',(-1.03454361812171,24.139401831489,12.0555579958973));
#293276=CARTESIAN_POINT('Ctrl Pts',(2.07451493030272,24.2651658915976,11.9219010856576));
#293277=CARTESIAN_POINT('Ctrl Pts',(3.60567970990701,24.3245969477269,11.5513830311112));
#293278=CARTESIAN_POINT('Ctrl Pts',(6.45229346006646,24.44894831872,10.2393799661171));
#293279=CARTESIAN_POINT('Ctrl Pts',(7.73816339564967,24.5132262620019,9.3057949290138));
#293280=CARTESIAN_POINT('Ctrl Pts',(9.85740713840747,24.6370256775676,7.01586734759232));
#293281=CARTESIAN_POINT('Ctrl Pts',(10.6784688336598,24.695881211199,5.68868492135024));
#293282=CARTESIAN_POINT('Ctrl Pts',(11.7842800249469,24.8222689400477,2.76271576049254));
#293283=CARTESIAN_POINT('Ctrl Pts',(12.045422510488,24.8850125296937,1.18711851387509));
#293284=CARTESIAN_POINT('Ctrl Pts',(11.9423554273777,25.0071140984816,-1.95324933201141));
#293285=CARTESIAN_POINT('Ctrl Pts',(11.5874432158204,25.0705928692317,-3.48797159679797));
#293286=CARTESIAN_POINT('Ctrl Pts',(10.3139009873652,25.1957277148076,-6.3268747238173));
#293287=CARTESIAN_POINT('Ctrl Pts',(9.41063996641178,25.2541176617196,-7.605640666435));
#293288=CARTESIAN_POINT('Ctrl Pts',(7.14378402625019,25.3797890270167,-9.77112886524276));
#293289=CARTESIAN_POINT('Ctrl Pts',(5.79313702996344,25.4443561104804,-10.6277167262761));
#293290=CARTESIAN_POINT('Ctrl Pts',(2.86990730503427,25.5668052080308,-11.7542602021739));
#293291=CARTESIAN_POINT('Ctrl Pts',(1.3303469679492,25.6274363345891,-12.0261957086734));
#293292=CARTESIAN_POINT('Ctrl Pts',(-1.76483950428071,25.7526392574292,
-11.9698710723832));
#293293=CARTESIAN_POINT('Ctrl Pts',(-3.29140693331789,25.8121342827434,
-11.6429845208071));
#293294=CARTESIAN_POINT('Ctrl Pts',(-6.16526988915022,25.9353702621123,
-10.4153984561717));
#293295=CARTESIAN_POINT('Ctrl Pts',(-7.48022415333472,25.9998084258097,
-9.51510593454787));
#293296=CARTESIAN_POINT('Ctrl Pts',(-9.67043315155746,26.1247825872557,
-7.27344561108007));
#293297=CARTESIAN_POINT('Ctrl Pts',(-10.5309372747227,26.1836057457594,
-5.95983225202021));
#293298=CARTESIAN_POINT('Ctrl Pts',(-11.7001145821,26.3088791217704,-3.08341800519752));
#293299=CARTESIAN_POINT('Ctrl Pts',(-11.9999999983778,26.3716626034119,
-1.54888950087861));
#293300=CARTESIAN_POINT('Ctrl Pts',(-12.,26.4312499994205,-1.25681384743892E-8));
#293301=CARTESIAN_POINT('Ctrl Pts',(-12.,26.806249999904,1.29896093881143E-13));
#293302=CARTESIAN_POINT('Ctrl Pts',(-12.,26.7537890016525,-1.36364892928156));
#293303=CARTESIAN_POINT('Ctrl Pts',(-11.7675527535486,26.6987444641245,
-2.71892659361115));
#293304=CARTESIAN_POINT('Ctrl Pts',(-10.7947443658577,26.5809437486461,
-5.46490380294277));
#293305=CARTESIAN_POINT('Ctrl Pts',(-10.0013609216683,26.5216517362606,
-6.80914524864304));
#293306=CARTESIAN_POINT('Ctrl Pts',(-7.92789050622467,26.398252233563,-9.14525467926901));
#293307=CARTESIAN_POINT('Ctrl Pts',(-6.65870048348816,26.3338537374135,
-10.1068679183002));
#293308=CARTESIAN_POINT('Ctrl Pts',(-3.83925340538554,26.2090478577536,
-11.4753786473057));
#293309=CARTESIAN_POINT('Ctrl Pts',(-2.31956538971854,26.1500783908989,
-11.8761840996725));
#293310=CARTESIAN_POINT('Ctrl Pts',(0.785082900623845,26.0244927294772,
-12.0747109172162));
#293311=CARTESIAN_POINT('Ctrl Pts',(2.34043984396086,25.9619239810052,-11.8716759525006));
#293312=CARTESIAN_POINT('Ctrl Pts',(5.32216235716819,25.8405829440187,-10.8722442458735));
#293313=CARTESIAN_POINT('Ctrl Pts',(6.71507066342784,25.7759647302934,-10.0716736262776));
#293314=CARTESIAN_POINT('Ctrl Pts',(9.0748101075305,25.6495475374532,-8.00266022351069));
#293315=CARTESIAN_POINT('Ctrl Pts',(10.0301109621315,25.5912053758984,-6.7669533887209));
#293316=CARTESIAN_POINT('Ctrl Pts',(11.4274700267537,25.4666566549912,-3.98351626644247));
#293317=CARTESIAN_POINT('Ctrl Pts',(11.8494629126326,25.4027253598738,-2.45882710758252));
#293318=CARTESIAN_POINT('Ctrl Pts',(12.0837415350844,25.2794473222752,0.66948815588767));
#293319=CARTESIAN_POINT('Ctrl Pts',(11.8925943782014,25.2186146452849,2.24305802232372));
#293320=CARTESIAN_POINT('Ctrl Pts',(10.9222168551947,25.0925066677988,5.20576051131627));
#293321=CARTESIAN_POINT('Ctrl Pts',(10.1605857816088,25.0325624351741,6.56941195749918));
#293322=CARTESIAN_POINT('Ctrl Pts',(8.14006577677286,24.909658157909,8.95757294257594));
#293323=CARTESIAN_POINT('Ctrl Pts',(6.89060965781988,24.8451541191261,9.95078653368017));
#293324=CARTESIAN_POINT('Ctrl Pts',(4.10290371893131,24.7198651398814,11.383303631392));
#293325=CARTESIAN_POINT('Ctrl Pts',(2.59635635370549,24.6612748205926,11.8183042639752));
#293326=CARTESIAN_POINT('Ctrl Pts',(-0.50260758961881,24.5359190958379,
12.0901927815865));
#293327=CARTESIAN_POINT('Ctrl Pts',(-2.06582271479834,24.4726857157314,
11.9230053433905));
#293328=CARTESIAN_POINT('Ctrl Pts',(-5.06990412957124,24.35116806988,10.9916693343548));
#293329=CARTESIAN_POINT('Ctrl Pts',(-6.47821009372995,24.2873657358891,
10.22517208831));
#293330=CARTESIAN_POINT('Ctrl Pts',(-8.8830041082046,24.1608698364378,8.21486070050412));
#293331=CARTESIAN_POINT('Ctrl Pts',(-9.86666611749828,24.1023256506135,
7.00290264189264));
#293332=CARTESIAN_POINT('Ctrl Pts',(-11.3311293953531,23.9781576531616,
4.25116536415171));
#293333=CARTESIAN_POINT('Ctrl Pts',(-11.7896882704929,23.9140267567717,
2.7331688646281));
#293334=CARTESIAN_POINT('Ctrl Pts',(-11.9809869533892,23.8365132364504,
0.780472016417012));
#293335=CARTESIAN_POINT('Ctrl Pts',(-12.,23.8212541772838,0.390012220207713));
#293336=CARTESIAN_POINT('Ctrl Pts',(-12.,23.806249999916,3.25017790459015E-13));
#293337=CARTESIAN_POINT('Origin',(-8.79029313101884E-14,130.96875,0.));
#293338=CARTESIAN_POINT('',(-12.,20.431249999928,1.34330781760066E-13));
#293339=CARTESIAN_POINT('',(-12.,20.806249999928,2.71595654142186E-14));
#293340=CARTESIAN_POINT('',(-12.0000000000001,130.96875,-1.46957615897682E-15));
#293341=CARTESIAN_POINT('Ctrl Pts',(-12.,20.431249999928,3.23074900165921E-13));
#293342=CARTESIAN_POINT('Ctrl Pts',(-12.,20.4467848257397,0.403805670704763));
#293343=CARTESIAN_POINT('Ctrl Pts',(-11.9796183449311,20.4625921950636,
0.808073320648967));
#293344=CARTESIAN_POINT('Ctrl Pts',(-11.7801159006779,20.5407344048709,
2.77444649295645));
#293345=CARTESIAN_POINT('Ctrl Pts',(-11.3160449848468,20.604892485555,4.29135863890174));
#293346=CARTESIAN_POINT('Ctrl Pts',(-9.84148614536275,20.7289993282602,
7.03822603928776));
#293347=CARTESIAN_POINT('Ctrl Pts',(-8.85354564014989,20.7875881579817,
8.24658460486558));
#293348=CARTESIAN_POINT('Ctrl Pts',(-6.44249394372589,20.9140664918751,
10.2475442515478));
#293349=CARTESIAN_POINT('Ctrl Pts',(-5.03254351667025,20.9776793384299,
11.0086698879463));
#293350=CARTESIAN_POINT('Ctrl Pts',(-2.02594049367394,21.0992989854766,
11.9299138331781));
#293351=CARTESIAN_POINT('Ctrl Pts',(-0.461644847179159,21.1625760735884,
12.0918926621046));
#293352=CARTESIAN_POINT('Ctrl Pts',(2.63643741123524,21.2878961334393,11.8093688217767));
#293353=CARTESIAN_POINT('Ctrl Pts',(4.14106597654989,21.3464442328503,11.3694152091123));
#293354=CARTESIAN_POINT('Ctrl Pts',(6.92407989691486,21.4718004693551,9.92761136320372));
#293355=CARTESIAN_POINT('Ctrl Pts',(8.17059822423941,21.5363170385871,8.92982723706064));
#293356=CARTESIAN_POINT('Ctrl Pts',(10.1833370256642,21.659145690427,6.53413703540161));
#293357=CARTESIAN_POINT('Ctrl Pts',(10.940323806214,21.719198738833,5.16766084013816));
#293358=CARTESIAN_POINT('Ctrl Pts',(11.9001278424061,21.8452822730432,2.20215818516315));
#293359=CARTESIAN_POINT('Ctrl Pts',(12.0858225482307,21.9059873448058,0.628781301812343));
#293360=CARTESIAN_POINT('Ctrl Pts',(11.8412402405099,22.0293525601758,-2.49845215337111));
#293361=CARTESIAN_POINT('Ctrl Pts',(11.4139731840186,22.0933147054619,-4.0222295365126));
#293362=CARTESIAN_POINT('Ctrl Pts',(10.0069201157794,22.2178111846298,-6.80115893647389));
#293363=CARTESIAN_POINT('Ctrl Pts',(9.04752999575144,22.2761724459011,-8.03345356440084));
#293364=CARTESIAN_POINT('Ctrl Pts',(6.68051948207383,22.4026432132964,-10.0947124632924));
#293365=CARTESIAN_POINT('Ctrl Pts',(5.28435371861963,22.4672603187263,-10.8907529644727));
#293366=CARTESIAN_POINT('Ctrl Pts',(2.29811650048091,22.588507122638,-11.8800074121184));
#293367=CARTESIAN_POINT('Ctrl Pts',(0.741520454552576,22.6512548674486,
-12.0775312505332));
#293368=CARTESIAN_POINT('Ctrl Pts',(-2.36232605474743,22.7768080961458,
-11.8676768837343));
#293369=CARTESIAN_POINT('Ctrl Pts',(-3.87999642471441,22.8357090654822,
-11.4615887160664));
#293370=CARTESIAN_POINT('Ctrl Pts',(-6.69461417398888,22.9605916894066,
-10.0832032383739));
#293371=CARTESIAN_POINT('Ctrl Pts',(-7.96081811139866,23.0250086359743,
-9.11670400877424));
#293372=CARTESIAN_POINT('Ctrl Pts',(-10.0261963824355,23.14833468153,-6.77254619328493));
#293373=CARTESIAN_POINT('Ctrl Pts',(-10.8147096955589,23.2077162761768,
-5.42531660356751));
#293374=CARTESIAN_POINT('Ctrl Pts',(-11.7725905894236,23.3249359390307,
-2.6895927928564));
#293375=CARTESIAN_POINT('Ctrl Pts',(-12.,23.3793605712179,-1.34879179282623));
#293376=CARTESIAN_POINT('Ctrl Pts',(-12.,23.431249999916,1.08246744900953E-13));
#293377=CARTESIAN_POINT('Ctrl Pts',(-12.,23.806249999916,3.29458682557515E-13));
#293378=CARTESIAN_POINT('Ctrl Pts',(-12.,23.761270474463,-1.16917869975571));
#293379=CARTESIAN_POINT('Ctrl Pts',(-11.8291289136152,23.7143161307078,
-2.33417060705515));
#293380=CARTESIAN_POINT('Ctrl Pts',(-11.0446447532021,23.6042128314296,
-4.94125469642478));
#293381=CARTESIAN_POINT('Ctrl Pts',(-10.3151456048164,23.5434465782065,
-6.32437469437398));
#293382=CARTESIAN_POINT('Ctrl Pts',(-8.34863463534201,23.4210817968168,
-8.76418235793767));
#293383=CARTESIAN_POINT('Ctrl Pts',(-7.11976024704336,23.3565060849324,
-9.78873873335731));
#293384=CARTESIAN_POINT('Ctrl Pts',(-4.36476270921836,23.2307694099466,
-11.2851044893288));
#293385=CARTESIAN_POINT('Ctrl Pts',(-2.87146936935017,23.17240337585,-11.7541221595676));
#293386=CARTESIAN_POINT('Ctrl Pts',(0.220985512029197,23.0473109481819,
-12.099075516286));
#293387=CARTESIAN_POINT('Ctrl Pts',(1.7912833647821,22.9837910657267,-11.9677904024354));
#293388=CARTESIAN_POINT('Ctrl Pts',(4.81229210353979,22.8615886952367,-11.1058563450733));
#293389=CARTESIAN_POINT('Ctrl Pts',(6.23173012211203,22.799021172219,-10.3761315516819));
#293390=CARTESIAN_POINT('Ctrl Pts',(8.67914767360568,22.6726540431373,-8.42990231678871));
#293391=CARTESIAN_POINT('Ctrl Pts',(9.69202949891002,22.6137305466513,-7.24261379317035));
#293392=CARTESIAN_POINT('Ctrl Pts',(11.2252803437536,22.4899994638192,-4.52458392404308));
#293393=CARTESIAN_POINT('Ctrl Pts',(11.721445154911,22.4256983166613,-3.0143809076004));
#293394=CARTESIAN_POINT('Ctrl Pts',(12.1005737742388,22.3012645216902,0.0969120056357209));
#293395=CARTESIAN_POINT('Ctrl Pts',(11.9855379923338,22.2419238543774,1.66736754248129));
#293396=CARTESIAN_POINT('Ctrl Pts',(11.1630735659662,22.1161905068203,4.66839193848627));
#293397=CARTESIAN_POINT('Ctrl Pts',(10.4664856162945,22.0544171592613,6.07127028798239));
#293398=CARTESIAN_POINT('Ctrl Pts',(8.55567909165914,21.9326434694289,8.56288812457291));
#293399=CARTESIAN_POINT('Ctrl Pts',(7.34847816608553,21.8680302986595,9.61885092633913));
#293400=CARTESIAN_POINT('Ctrl Pts',(4.62755125718015,21.7418773780287,11.1796175428449));
#293401=CARTESIAN_POINT('Ctrl Pts',(3.1477741743481,21.6835801399995,11.6828769675529));
#293402=CARTESIAN_POINT('Ctrl Pts',(0.0629372260864292,21.558795864199,
12.1013948602857));
#293403=CARTESIAN_POINT('Ctrl Pts',(-1.51368102089066,21.495020316427,12.0065258535606));
#293404=CARTESIAN_POINT('Ctrl Pts',(-4.55079936511367,21.3721662987073,
11.2146319147188));
#293405=CARTESIAN_POINT('Ctrl Pts',(-5.98107330162838,21.3106834381994,
10.5216293205749));
#293406=CARTESIAN_POINT('Ctrl Pts',(-8.47057404200132,21.1844642790414,
8.63954601741154));
#293407=CARTESIAN_POINT('Ctrl Pts',(-9.51248341293276,21.1249906405834,
7.47696583729867));
#293408=CARTESIAN_POINT('Ctrl Pts',(-11.1136666219519,21.0017379116272,
4.79344265898674));
#293409=CARTESIAN_POINT('Ctrl Pts',(-11.6470661436893,20.9373035795534,
3.29187598120315));
#293410=CARTESIAN_POINT('Ctrl Pts',(-11.9582772315793,20.8512438335824,
1.15599407183253));
#293411=CARTESIAN_POINT('Ctrl Pts',(-12.,20.8284767802287,0.577753496285518));
#293412=CARTESIAN_POINT('Ctrl Pts',(-12.,20.806249999928,9.57567358739198E-15));
#293413=CARTESIAN_POINT('Origin',(-8.79029313101884E-14,130.96875,0.));
#293414=CARTESIAN_POINT('',(-12.,17.43124999994,2.44533967916948E-14));
#293415=CARTESIAN_POINT('',(-12.,17.80624999994,-2.19195579930893E-15));
#293416=CARTESIAN_POINT('',(-12.0000000000001,130.96875,-1.46957615897682E-15));
#293417=CARTESIAN_POINT('Ctrl Pts',(-12.,17.43124999994,5.35682609381638E-14));
#293418=CARTESIAN_POINT('Ctrl Pts',(-12.,17.4539971128015,0.591278800092865));
#293419=CARTESIAN_POINT('Ctrl Pts',(-11.9563009265847,17.4773086571402,
1.18303050285719));
#293420=CARTESIAN_POINT('Ctrl Pts',(-11.6357699188653,17.5639823368467,
3.331842519734));
#293421=CARTESIAN_POINT('Ctrl Pts',(-11.0969971356305,17.6284329581875,
4.83208673531864));
#293422=CARTESIAN_POINT('Ctrl Pts',(-9.48602239365201,17.7516128629079,
7.51053548942931));
#293423=CARTESIAN_POINT('Ctrl Pts',(-8.43991362594118,17.8111804351853,
8.66952450881498));
#293424=CARTESIAN_POINT('Ctrl Pts',(-5.94434591436069,17.937376567561,10.5422888708228));
#293425=CARTESIAN_POINT('Ctrl Pts',(-4.5125221168834,17.9987146459351,11.2299639974067));
#293426=CARTESIAN_POINT('Ctrl Pts',(-1.47313381954063,18.1216604851874,
12.0116363905843));
#293427=CARTESIAN_POINT('Ctrl Pts',(0.104337134805024,18.185470525697,12.1011768361982));
#293428=CARTESIAN_POINT('Ctrl Pts',(3.18797499635399,18.3102062974211,11.6719373989125));
#293429=CARTESIAN_POINT('Ctrl Pts',(4.66576764457087,18.3685068068196,11.163686575192));
#293430=CARTESIAN_POINT('Ctrl Pts',(7.38163184806853,18.4947174440379,9.59352427003675));
#293431=CARTESIAN_POINT('Ctrl Pts',(8.58559365724217,18.5593331061441,8.53299842515826));
#293432=CARTESIAN_POINT('Ctrl Pts',(10.4881684878408,18.6810165610806,6.0338457770933));
#293433=CARTESIAN_POINT('Ctrl Pts',(11.179910341594,18.7429520460265,4.62807383611877));
#293434=CARTESIAN_POINT('Ctrl Pts',(11.9913702643163,18.8686547636934,1.62427004050253));
#293435=CARTESIAN_POINT('Ctrl Pts',(12.1007575921369,18.9279100116668,0.0540801116266604));
#293436=CARTESIAN_POINT('Ctrl Pts',(11.7107948809275,19.0524241989025,-3.05578227418279));
#293437=CARTESIAN_POINT('Ctrl Pts',(11.2090827886063,19.1167474287713,-4.56475687833112));
#293438=CARTESIAN_POINT('Ctrl Pts',(9.66570132517863,19.2404101454037,-7.27771802796008));
#293439=CARTESIAN_POINT('Ctrl Pts',(8.64850206774641,19.2994045093754,-8.46134422340063));
#293440=CARTESIAN_POINT('Ctrl Pts',(6.19480894882948,19.4257508803272,-10.3980628251768));
#293441=CARTESIAN_POINT('Ctrl Pts',(4.77374542976002,19.488147940957,-11.1223374114215));
#293442=CARTESIAN_POINT('Ctrl Pts',(1.75029509261386,19.6104490761765,-11.9739224784792));
#293443=CARTESIAN_POINT('Ctrl Pts',(0.179010938886157,19.6740088553441,
-12.0998378860898));
#293444=CARTESIAN_POINT('Ctrl Pts',(-2.91238430867471,19.7990584199239,
-11.7440039397611));
#293445=CARTESIAN_POINT('Ctrl Pts',(-4.40368952208624,19.8574042958986,
-11.2699218185076));
#293446=CARTESIAN_POINT('Ctrl Pts',(-7.15372046582846,19.9832047383442,
-9.7640381692274));
#293447=CARTESIAN_POINT('Ctrl Pts',(-8.37944964047272,20.047788209345,-8.73482644189239));
#293448=CARTESIAN_POINT('Ctrl Pts',(-10.3378062779058,20.1700686233113,
-6.28734366947722));
#293449=CARTESIAN_POINT('Ctrl Pts',(-11.062474098562,20.2309723528992,-4.90131154770073));
#293450=CARTESIAN_POINT('Ctrl Pts',(-11.8333884458573,20.3404879887831,
-2.30509383170136));
#293451=CARTESIAN_POINT('Ctrl Pts',(-12.,20.3868345884464,-1.15451536053513));
#293452=CARTESIAN_POINT('Ctrl Pts',(-12.,20.431249999928,3.34177130412172E-13));
#293453=CARTESIAN_POINT('Ctrl Pts',(-12.,20.806249999928,3.88578058618805E-15));
#293454=CARTESIAN_POINT('Ctrl Pts',(-12.,20.7688814633124,-0.971341885268998));
#293455=CARTESIAN_POINT('Ctrl Pts',(-11.8820664283109,20.7300961104164,
-1.94119295148273));
#293456=CARTESIAN_POINT('Ctrl Pts',(-11.2730074993954,20.6279881502184,
-4.39744870216082));
#293457=CARTESIAN_POINT('Ctrl Pts',(-10.6089181380125,20.5650608786088,
-5.81965308324059));
#293458=CARTESIAN_POINT('Ctrl Pts',(-8.75344208941597,20.4439075836876,
-8.36133391417179));
#293459=CARTESIAN_POINT('Ctrl Pts',(-7.56818400896899,20.3792923083396,
-9.44758696664805));
#293460=CARTESIAN_POINT('Ctrl Pts',(-4.88142122317779,20.2527696970531,
-11.070925094903));
#293461=CARTESIAN_POINT('Ctrl Pts',(-3.41491999798804,20.1943864155705,
-11.6074121784866));
#293462=CARTESIAN_POINT('Ctrl Pts',(-0.338486781005807,20.0699420778411,
-12.0972787778748));
#293463=CARTESIAN_POINT('Ctrl Pts',(1.24347617575282,20.0059503320169,-12.0379651060085));
#293464=CARTESIAN_POINT('Ctrl Pts',(4.29532847004766,19.8825003134971,-11.3141577789942));
#293465=CARTESIAN_POINT('Ctrl Pts',(5.7357830630127,19.8219172611387,-10.6564938888015));
#293466=CARTESIAN_POINT('Ctrl Pts',(8.26535369452417,19.6958580483938,-8.83628916380843));
#293467=CARTESIAN_POINT('Ctrl Pts',(9.3350663651124,19.6356949967075,-7.69756403507541));
#293468=CARTESIAN_POINT('Ctrl Pts',(11.0008950231688,19.512941282377,-5.04801661087702));
#293469=CARTESIAN_POINT('Ctrl Pts',(11.5697929225376,19.4484131411879,-3.55554562082969));
#293470=CARTESIAN_POINT('Ctrl Pts',(12.0910996598554,19.3229917907181,-0.464779079887096));
#293471=CARTESIAN_POINT('Ctrl Pts',(12.0497536139095,19.2644818519719,1.10186944496459));
#293472=CARTESIAN_POINT('Ctrl Pts',(11.3712584209357,19.1391975620908,4.13799966585378));
#293473=CARTESIAN_POINT('Ctrl Pts',(10.7383436427877,19.0758783728349,5.57824532750321));
#293474=CARTESIAN_POINT('Ctrl Pts',(8.94173389183376,18.9541597065169,8.15839479986107));
#293475=CARTESIAN_POINT('Ctrl Pts',(7.78665902721745,18.8907290269032,9.26728093053828));
#293476=CARTESIAN_POINT('Ctrl Pts',(5.14538467415531,18.7642682730146,10.9506268864999));
#293477=CARTESIAN_POINT('Ctrl Pts',(3.69293246893586,18.7056322562587,11.5218708993174));
#293478=CARTESIAN_POINT('Ctrl Pts',(0.626341788480967,18.5815860574952,
12.0862741549164));
#293479=CARTESIAN_POINT('Ctrl Pts',(-0.960370917922583,18.5174021802619,
12.0643298816322));
#293480=CARTESIAN_POINT('Ctrl Pts',(-4.02668243917191,18.3933672737255,
11.4118148451283));
#293481=CARTESIAN_POINT('Ctrl Pts',(-5.47745451590982,18.3335642700473,
10.7907907424887));
#293482=CARTESIAN_POINT('Ctrl Pts',(-8.0481511058204,18.2076884424295,9.03490394444749));
#293483=CARTESIAN_POINT('Ctrl Pts',(-9.14656576390013,18.146647146687,7.92100201639144));
#293484=CARTESIAN_POINT('Ctrl Pts',(-10.8786540110187,18.0244498374781,
5.30744659638946));
#293485=CARTESIAN_POINT('Ctrl Pts',(-11.48397828387,17.9598595509646,3.82519587335654));
#293486=CARTESIAN_POINT('Ctrl Pts',(-11.9279001944013,17.8655889419805,
1.51900463488298));
#293487=CARTESIAN_POINT('Ctrl Pts',(-12.,17.8354684935126,0.759493124481815));
#293488=CARTESIAN_POINT('Ctrl Pts',(-12.,17.80624999994,1.04083408558608E-14));
#293489=CARTESIAN_POINT('Origin',(-8.79029313101884E-14,130.96875,0.));
#293490=CARTESIAN_POINT('',(-12.,14.431249999952,-1.35928853084006E-15));
#293491=CARTESIAN_POINT('',(-12.,14.806249999952,-4.36865413446742E-14));
#293492=CARTESIAN_POINT('',(-12.0000000000001,130.96875,-1.46957615897682E-15));
#293493=CARTESIAN_POINT('Ctrl Pts',(-12.,14.431249999952,4.16333634234434E-16));
#293494=CARTESIAN_POINT('Ctrl Pts',(-12.,14.460987767858,0.772990921177218));
#293495=CARTESIAN_POINT('Ctrl Pts',(-11.9253146601718,14.4916574086311,
1.54593781233599));
#293496=CARTESIAN_POINT('Ctrl Pts',(-11.4708998428656,14.5865337222738,
3.86446412862074));
#293497=CARTESIAN_POINT('Ctrl Pts',(-10.8602603601541,14.6511301570846,
5.34514765151272));
#293498=CARTESIAN_POINT('Ctrl Pts',(-9.1185074465202,14.7732424691752,7.95335345197746));
#293499=CARTESIAN_POINT('Ctrl Pts',(-8.01588770460201,14.834426599361,9.06360143593913));
#293500=CARTESIAN_POINT('Ctrl Pts',(-5.43918583426702,14.9602740213547,
10.8100279769507));
#293501=CARTESIAN_POINT('Ctrl Pts',(-3.98691784246459,15.0199757854631,
11.4256709688868));
#293502=CARTESIAN_POINT('Ctrl Pts',(-0.918554175498763,15.1440937030375,
12.0676565860704));
#293503=CARTESIAN_POINT('Ctrl Pts',(0.66878655424738,15.2083029843487,12.0840709717991));
#293504=CARTESIAN_POINT('Ctrl Pts',(3.73383381415189,15.3322867504394,11.508673841105));
#293505=CARTESIAN_POINT('Ctrl Pts',(5.18419781753589,15.3909742483674,10.9322978502764));
#293506=CARTESIAN_POINT('Ctrl Pts',(7.81855818192678,15.5174167452044,9.24020346931188));
#293507=CARTESIAN_POINT('Ctrl Pts',(8.9690674588818,15.5806656015378,8.12813241825711));
#293508=CARTESIAN_POINT('Ctrl Pts',(10.7568932976436,15.702484090034,5.54253414447198));
#293509=CARTESIAN_POINT('Ctrl Pts',(11.3851948471033,15.765845384446,4.09969509039685));
#293510=CARTESIAN_POINT('Ctrl Pts',(12.0533520147543,15.8910924437712,1.0611735967341));
#293511=CARTESIAN_POINT('Ctrl Pts',(12.0894255701802,15.9495668040691,-0.505175363631084));
#293512=CARTESIAN_POINT('Ctrl Pts',(11.5578801980134,16.0750536126133,-3.59431665985857));
#293513=CARTESIAN_POINT('Ctrl Pts',(10.9837525372396,16.1395928120628,-5.08537584114874));
#293514=CARTESIAN_POINT('Ctrl Pts',(9.30840727074358,16.2622694239057,-7.72982696247656));
#293515=CARTESIAN_POINT('Ctrl Pts',(8.23458548037391,16.3225478455797,-8.86501066592352));
#293516=CARTESIAN_POINT('Ctrl Pts',(5.69911229414429,16.448581933702,-10.6760345176555));
#293517=CARTESIAN_POINT('Ctrl Pts',(4.25716889207649,16.5090439008629,-11.3284625629591));
#293518=CARTESIAN_POINT('Ctrl Pts',(1.20319891082697,16.6325795816195,-12.0421254554265));
#293519=CARTESIAN_POINT('Ctrl Pts',(-0.379492791011095,16.6966008058014,
-12.096129889922));
#293520=CARTESIAN_POINT('Ctrl Pts',(-3.45459032687708,16.8209911140947,
-11.5956465592013));
#293521=CARTESIAN_POINT('Ctrl Pts',(-4.91910185381263,16.8794001840513,
-11.0542122147388));
#293522=CARTESIAN_POINT('Ctrl Pts',(-7.60033579695139,17.005958400366,-9.42176679373339));
#293523=CARTESIAN_POINT('Ctrl Pts',(-8.78184023446649,17.0705029359655,
-8.3314626220704));
#293524=CARTESIAN_POINT('Ctrl Pts',(-10.6289833189954,17.1916298915339,
-5.78311310327076));
#293525=CARTESIAN_POINT('Ctrl Pts',(-11.2883210946912,17.2546928414801,
-4.35811336985312));
#293526=CARTESIAN_POINT('Ctrl Pts',(-11.8854674394808,17.3562186805609,
-1.91311839528264));
#293527=CARTESIAN_POINT('Ctrl Pts',(-12.,17.3944241966078,-0.957234306581829));
#293528=CARTESIAN_POINT('Ctrl Pts',(-12.,17.43124999994,5.60662627435704E-14));
#293529=CARTESIAN_POINT('Ctrl Pts',(-12.,17.80624999994,1.13797860024079E-14));
#293530=CARTESIAN_POINT('Ctrl Pts',(-12.,17.7761119753235,-0.783395024280319));
#293531=CARTESIAN_POINT('Ctrl Pts',(-11.9232906485854,17.7450186926119,
-1.56669624300091));
#293532=CARTESIAN_POINT('Ctrl Pts',(-11.465508196661,17.6506612618365,-3.87064072738115));
#293533=CARTESIAN_POINT('Ctrl Pts',(-10.8648852070875,17.5870633542603,
-5.32862351292106));
#293534=CARTESIAN_POINT('Ctrl Pts',(-9.12953434449562,17.4646669131686,
-7.94629499456211));
#293535=CARTESIAN_POINT('Ctrl Pts',(-8.0061267671257,17.4024323741593,-9.07712725864556));
#293536=CARTESIAN_POINT('Ctrl Pts',(-5.4128771983687,17.276106583186,-10.8208973231749));
#293537=CARTESIAN_POINT('Ctrl Pts',(-3.97494086041983,17.2170397353279,
-11.4276386605344));
#293538=CARTESIAN_POINT('Ctrl Pts',(-0.919494781300424,17.0934443451582,
-12.0680067393541));
#293539=CARTESIAN_POINT('Ctrl Pts',(0.671174299028302,17.0291004292379,
-12.0843598021253));
#293540=CARTESIAN_POINT('Ctrl Pts',(3.75124351266482,16.9045090123542,-11.5046737807013));
#293541=CARTESIAN_POINT('Ctrl Pts',(5.21222391654724,16.8453331927415,-10.9207152458411));
#293542=CARTESIAN_POINT('Ctrl Pts',(7.82411039744174,16.719660545862,-9.23006694389104));
#293543=CARTESIAN_POINT('Ctrl Pts',(8.95143845658941,16.6575643890469,-8.14137947652282));
#293544=CARTESIAN_POINT('Ctrl Pts',(10.7497470693045,16.535969257765,-5.56499311512457));
#293545=CARTESIAN_POINT('Ctrl Pts',(11.3914932367514,16.471351912502,-4.09387322936519));
#293546=CARTESIAN_POINT('Ctrl Pts',(12.0557290891391,16.3450861452902,-1.02759776257042));
#293547=CARTESIAN_POINT('Ctrl Pts',(12.087630137356,16.2867792276593,0.53458775095372));
#293548=CARTESIAN_POINT('Ctrl Pts',(11.5531974907912,16.1620912636547,3.60202608884916));
#293549=CARTESIAN_POINT('Ctrl Pts',(10.9852331632466,16.0982485173233,5.076984551652));
#293550=CARTESIAN_POINT('Ctrl Pts',(9.31133355087314,15.9752145821935,7.7311935043871));
#293551=CARTESIAN_POINT('Ctrl Pts',(8.21929404044133,15.9140133905269,8.8834467907717));
#293552=CARTESIAN_POINT('Ctrl Pts',(5.67377710036676,15.7878398859371,10.6865102472551));
#293553=CARTESIAN_POINT('Ctrl Pts',(4.2502971290847,15.7281781303768,11.3282027085803));
#293554=CARTESIAN_POINT('Ctrl Pts',(1.20688282896854,15.6050694358914,12.043152154094));
#293555=CARTESIAN_POINT('Ctrl Pts',(-0.386795444128867,15.5406037955665,
12.09728761924));
#293556=CARTESIAN_POINT('Ctrl Pts',(-3.47941185947045,15.4155048337123,
11.5892705222127));
#293557=CARTESIAN_POINT('Ctrl Pts',(-4.95013874828265,15.3567806387341,
11.0414482393785));
#293558=CARTESIAN_POINT('Ctrl Pts',(-7.60162688164875,15.231330848694,9.41467995783229));
#293559=CARTESIAN_POINT('Ctrl Pts',(-8.75706777119083,15.1682221135034,
8.35074986546862));
#293560=CARTESIAN_POINT('Ctrl Pts',(-10.6178353111347,15.046991234969,5.81308909801941));
#293561=CARTESIAN_POINT('Ctrl Pts',(-11.2941531048397,14.9826465868061,
4.35583447463269));
#293562=CARTESIAN_POINT('Ctrl Pts',(-11.8885694328649,14.8802421012849,
1.88711330108603));
#293563=CARTESIAN_POINT('Ctrl Pts',(-12.,14.8425737134021,0.944183195223962));
#293564=CARTESIAN_POINT('Ctrl Pts',(-12.,14.806249999952,-1.00475183728577E-13));
#293565=CARTESIAN_POINT('Origin',(-8.79029313101884E-14,130.96875,0.));
#293566=CARTESIAN_POINT('',(-12.,11.431249999964,-3.88293156119391E-14));
#293567=CARTESIAN_POINT('',(-12.,11.806249999964,-8.49382656034026E-14));
#293568=CARTESIAN_POINT('',(-12.0000000000001,130.96875,-1.46957615897682E-15));
#293569=CARTESIAN_POINT('Ctrl Pts',(-12.,11.431249999964,-5.07927033766009E-14));
#293570=CARTESIAN_POINT('Ctrl Pts',(-12.,11.468121395742,0.958419417275447));
#293571=CARTESIAN_POINT('Ctrl Pts',(-11.8851836503325,11.5063744328613,
1.91544653988381));
#293572=CARTESIAN_POINT('Ctrl Pts',(-11.2788881633895,11.6093366144611,
4.39480445595943));
#293573=CARTESIAN_POINT('Ctrl Pts',(-10.5980910112658,11.6734842595123,
5.84870775642085));
#293574=CARTESIAN_POINT('Ctrl Pts',(-8.72938078653482,11.7948184680951,
8.37978226182653));
#293575=CARTESIAN_POINT('Ctrl Pts',(-7.57001013475369,11.8579724084575,
9.44020476171866));
#293576=CARTESIAN_POINT('Ctrl Pts',(-4.91298096368815,11.9833893373363,
11.0579643683581));
#293577=CARTESIAN_POINT('Ctrl Pts',(-3.44089744373657,12.0420627745674,
11.6006993699913));
#293578=CARTESIAN_POINT('Ctrl Pts',(-0.34658463568243,12.1672303569483,
12.0985754145678));
#293579=CARTESIAN_POINT('Ctrl Pts',(1.24744865956387,12.2317103582207,12.0390876488422));
#293580=CARTESIAN_POINT('Ctrl Pts',(4.28907572010713,12.3547467573467,11.3135987775732));
#293581=CARTESIAN_POINT('Ctrl Pts',(5.71049570567009,12.4145064081564,10.6669576658726));
#293582=CARTESIAN_POINT('Ctrl Pts',(8.24921959246757,12.5406568322771,8.85551510332783));
#293583=CARTESIAN_POINT('Ctrl Pts',(9.33680374771899,12.6017236380238,7.70024351636594));
#293584=CARTESIAN_POINT('Ctrl Pts',(11.0019126150717,12.7248453601402,5.04089637975034));
#293585=CARTESIAN_POINT('Ctrl Pts',(11.5651846431726,12.78872030928,3.56357623029895));
#293586=CARTESIAN_POINT('Ctrl Pts',(12.0893260345269,12.913359362794,0.494065419426067));
#293587=CARTESIAN_POINT('Ctrl Pts',(12.0522083116166,12.9716759408897,-1.06777826455158));
#293588=CARTESIAN_POINT('Ctrl Pts',(11.3777405180559,13.0979963969138,-4.13215072990994));
#293589=CARTESIAN_POINT('Ctrl Pts',(10.7307949238898,13.162614709663,-5.60160636794518));
#293590=CARTESIAN_POINT('Ctrl Pts',(8.9230328122269,13.2841200741918,-8.17258774244646));
#293591=CARTESIAN_POINT('Ctrl Pts',(7.79155726353775,13.3463814656007,-9.25764068226929));
#293592=CARTESIAN_POINT('Ctrl Pts',(5.17378153763854,13.4720234616693,-10.9388940070764));
#293593=CARTESIAN_POINT('Ctrl Pts',(3.7113512800567,13.5311226870725,-11.517523069066));
#293594=CARTESIAN_POINT('Ctrl Pts',(0.629377258875286,13.6557911550399,
-12.0866799579317));
#293595=CARTESIAN_POINT('Ctrl Pts',(-0.961788845064329,13.7201551759877,
-12.064781443821));
#293596=CARTESIAN_POINT('Ctrl Pts',(-4.01553325036617,13.8436817320055,
-11.4134456384658));
#293597=CARTESIAN_POINT('Ctrl Pts',(-5.45135669482629,13.9028253429919,
-10.8015713665829));
#293598=CARTESIAN_POINT('Ctrl Pts',(-8.0376235095307,14.0291299589728,-9.0490809538014));
#293599=CARTESIAN_POINT('Ctrl Pts',(-9.15643559500131,14.0912036179821,
-7.91509128812461));
#293600=CARTESIAN_POINT('Ctrl Pts',(-10.8828318353858,14.2136955710466,
-5.29202757565925));
#293601=CARTESIAN_POINT('Ctrl Pts',(-11.4787118397578,14.2773313132461,
-3.83152024366495));
#293602=CARTESIAN_POINT('Ctrl Pts',(-11.9259733144817,14.3711130450116,
-1.53912176236354));
#293603=CARTESIAN_POINT('Ctrl Pts',(-12.,14.4016436505551,-0.769574884210652));
#293604=CARTESIAN_POINT('Ctrl Pts',(-12.,14.431249999952,8.46545056276682E-15));
#293605=CARTESIAN_POINT('Ctrl Pts',(-12.,14.806249999952,-1.08524300657109E-13));
#293606=CARTESIAN_POINT('Ctrl Pts',(-12.,14.7833237431069,-0.595935392792773));
#293607=CARTESIAN_POINT('Ctrl Pts',(-11.9556099107365,14.7598250575928,
-1.19232703919809));
#293608=CARTESIAN_POINT('Ctrl Pts',(-11.6333140357018,14.6733316268826,
-3.33588029999469));
#293609=CARTESIAN_POINT('Ctrl Pts',(-11.0979184575167,14.6092803890216,
-4.82684043130409));
#293610=CARTESIAN_POINT('Ctrl Pts',(-9.48485046374418,14.4856561552388,
-7.51615874779507));
#293611=CARTESIAN_POINT('Ctrl Pts',(-8.42348187457655,14.4253170025921,
-8.68907439094324));
#293612=CARTESIAN_POINT('Ctrl Pts',(-5.92479762126047,14.2993094887007,
-10.5496161928145));
#293613=CARTESIAN_POINT('Ctrl Pts',(-4.51553444132652,14.23890720504,-11.2253024111993));
#293614=CARTESIAN_POINT('Ctrl Pts',(-1.48480981289121,14.1163118185567,
-12.0125344581499));
#293615=CARTESIAN_POINT('Ctrl Pts',(0.110952708358791,14.0517618686231,
-12.1034359909647));
#293616=CARTESIAN_POINT('Ctrl Pts',(3.21482169659992,13.9262077306336,-11.6650344976422));
#293617=CARTESIAN_POINT('Ctrl Pts',(4.69475560629124,13.8677669508926,-11.1520111884328));
#293618=CARTESIAN_POINT('Ctrl Pts',(7.38375802076941,13.7425595614282,-9.58707188710994));
#293619=CARTESIAN_POINT('Ctrl Pts',(8.56586069103511,13.6791551935694,-8.54740472438333));
#293620=CARTESIAN_POINT('Ctrl Pts',(10.4806400999911,13.557233721765,-6.05503960750681));
#293621=CARTESIAN_POINT('Ctrl Pts',(11.1873622091499,13.494170481708,-4.62068324356806));
#293622=CARTESIAN_POINT('Ctrl Pts',(11.993432245557,13.3677473913579,-1.59640310585493));
#293623=CARTESIAN_POINT('Ctrl Pts',(12.0991493850008,13.3090025850949,-0.0393339420722724));
#293624=CARTESIAN_POINT('Ctrl Pts',(11.7105867762451,13.1850846193959,3.05548543495258));
#293625=CARTESIAN_POINT('Ctrl Pts',(11.2097277761212,13.1208497738241,4.56243980164547));
#293626=CARTESIAN_POINT('Ctrl Pts',(9.66073170363857,12.9966465906864,7.28762531122103));
#293627=CARTESIAN_POINT('Ctrl Pts',(8.6312727436616,12.9370461441711,8.48176401491606));
#293628=CARTESIAN_POINT('Ctrl Pts',(6.1814877412528,12.8112285633671,10.4016215629996));
#293629=CARTESIAN_POINT('Ctrl Pts',(4.78710944777118,12.749892644819,11.1125044187706));
#293630=CARTESIAN_POINT('Ctrl Pts',(1.7705270509074,12.6278693236197,11.9742604606147));
#293631=CARTESIAN_POINT('Ctrl Pts',(0.173477555825857,12.563267314501,12.1031955259798));
#293632=CARTESIAN_POINT('Ctrl Pts',(-2.94105624238201,12.4372817758863,
11.7367268103642));
#293633=CARTESIAN_POINT('Ctrl Pts',(-4.43025614388931,12.378975406019,11.2593695964559));
#293634=CARTESIAN_POINT('Ctrl Pts',(-7.15675630678309,12.2540588534684,
9.75827367924247));
#293635=CARTESIAN_POINT('Ctrl Pts',(-8.36563209591937,12.1903847159397,
8.74411044859983));
#293636=CARTESIAN_POINT('Ctrl Pts',(-10.3349794652727,12.0677948191106,
6.29873873932138));
#293637=CARTESIAN_POINT('Ctrl Pts',(-11.0722999088359,12.0058840092412,
4.88777370037917));
#293638=CARTESIAN_POINT('Ctrl Pts',(-11.8374969081264,11.8958645770464,
2.27660283786094));
#293639=CARTESIAN_POINT('Ctrl Pts',(-12.,11.8501144449795,1.14019377199156));
#293640=CARTESIAN_POINT('Ctrl Pts',(-12.,11.806249999964,-1.58206781009085E-13));
#293641=CARTESIAN_POINT('Origin',(-8.79029313101884E-14,130.96875,0.));
#293642=CARTESIAN_POINT('',(-12.,8.43124999997595,-1.13942842121735E-13));
#293643=CARTESIAN_POINT('',(-12.,8.80624999997602,-8.17810688771248E-14));
#293644=CARTESIAN_POINT('',(-12.0000000000001,130.96875,-1.46957615897682E-15));
#293645=CARTESIAN_POINT('Ctrl Pts',(-12.,8.43124999997595,-2.38142838782096E-13));
#293646=CARTESIAN_POINT('Ctrl Pts',(-12.,8.47567904276991,1.15486968708691));
#293647=CARTESIAN_POINT('Ctrl Pts',(-11.8332862861018,8.52203689564963,
2.30570747586626));
#293648=CARTESIAN_POINT('Ctrl Pts',(-11.0546840741179,8.63262018149063,
4.92717929318519));
#293649=CARTESIAN_POINT('Ctrl Pts',(-10.3128518110714,8.6943731952545,6.33466675125794));
#293650=CARTESIAN_POINT('Ctrl Pts',(-8.33544286534331,8.81705929161092,
8.772988659322));
#293651=CARTESIAN_POINT('Ctrl Pts',(-7.12262737739931,8.88077073210684,
9.78329826619002));
#293652=CARTESIAN_POINT('Ctrl Pts',(-4.39062248372888,9.00564032179357,
11.2748423843938));
#293653=CARTESIAN_POINT('Ctrl Pts',(-2.90005621554315,9.06394026182268,
11.7468847293909));
#293654=CARTESIAN_POINT('Ctrl Pts',(0.215990291541665,9.18998699079689,
12.1025858000625));
#293655=CARTESIAN_POINT('Ctrl Pts',(1.81315678618581,9.25459373264729,11.9679551876436));
#293656=CARTESIAN_POINT('Ctrl Pts',(4.82753254542353,9.37652779347956,11.0950577850757));
#293657=CARTESIAN_POINT('Ctrl Pts',(6.21966467391305,9.43801819258929,10.378898502507));
#293658=CARTESIAN_POINT('Ctrl Pts',(8.66208380791205,9.5638057413359,8.45016580927124));
#293659=CARTESIAN_POINT('Ctrl Pts',(9.68674645413114,9.62330923814904,7.25285986368789));
#293660=CARTESIAN_POINT('Ctrl Pts',(11.2260430133152,9.74759630337008,4.52234239591337));
#293661=CARTESIAN_POINT('Ctrl Pts',(11.7216544504217,9.81185575689031,3.01304334406987));
#293662=CARTESIAN_POINT('Ctrl Pts',(12.0989206745883,9.93570728451623,-0.0837194877233916));
#293663=CARTESIAN_POINT('Ctrl Pts',(11.9874952273135,9.99451299425393,-1.64036838390401));
#293664=CARTESIAN_POINT('Ctrl Pts',(11.1706301135791,10.1209163279355,-4.66062744191089));
#293665=CARTESIAN_POINT('Ctrl Pts',(10.4593290033012,10.1837981545383,-6.0915050773422));
#293666=CARTESIAN_POINT('Ctrl Pts',(8.53639605876238,10.3058213938744,-8.57692800386591));
#293667=CARTESIAN_POINT('Ctrl Pts',(7.35028185501117,10.3692679518947,-9.61284821886774));
#293668=CARTESIAN_POINT('Ctrl Pts',(4.6556505078725,10.4944348524845,-11.1683370581618));
#293669=CARTESIAN_POINT('Ctrl Pts',(3.1743300758674,10.5528456511109,-11.6760645492037));
#293670=CARTESIAN_POINT('Ctrl Pts',(0.0688214425628372,10.6784661141365,
-12.1038217757956));
#293671=CARTESIAN_POINT('Ctrl Pts',(-1.52718699512888,10.7430260115992,
-12.0072944293978));
#293672=CARTESIAN_POINT('Ctrl Pts',(-4.55588475974131,10.8655394097185,
-11.2090242181891));
#293673=CARTESIAN_POINT('Ctrl Pts',(-5.96295820240637,10.9260690566215,
-10.5281349593043));
#293674=CARTESIAN_POINT('Ctrl Pts',(-8.45443974112375,11.0520496403179,
-8.65881211458809));
#293675=CARTESIAN_POINT('Ctrl Pts',(-9.51110070527266,11.1122696139857,
-7.48274840654294));
#293676=CARTESIAN_POINT('Ctrl Pts',(-11.1147663784201,11.2359815304433,
-4.78809590464511));
#293677=CARTESIAN_POINT('Ctrl Pts',(-11.6451082116492,11.3000620123745,
-3.29473355410627));
#293678=CARTESIAN_POINT('Ctrl Pts',(-11.9577152330903,11.3859513408221,
-1.16373497183783));
#293679=CARTESIAN_POINT('Ctrl Pts',(-12.,11.4088740267595,-0.581631553322767));
#293680=CARTESIAN_POINT('Ctrl Pts',(-12.,11.431249999964,-4.94049245958195E-14));
#293681=CARTESIAN_POINT('Ctrl Pts',(-12.,11.806249999964,-1.61745616900077E-13));
#293682=CARTESIAN_POINT('Ctrl Pts',(-12.,11.7908310580493,-0.400793433853994));
#293683=CARTESIAN_POINT('Ctrl Pts',(-11.9799212696319,11.7751438853602,
-0.802035169667738));
#293684=CARTESIAN_POINT('Ctrl Pts',(-11.7816700157317,11.6969204614742,
-2.77092592266831));
#293685=CARTESIAN_POINT('Ctrl Pts',(-11.316093947334,11.6325364866386,-4.29322081162527));
#293686=CARTESIAN_POINT('Ctrl Pts',(-9.83214892128302,11.5077893688272,
-7.05368149456638));
#293687=CARTESIAN_POINT('Ctrl Pts',(-8.83468948695932,11.448765508599,-8.26884438344096));
#293688=CARTESIAN_POINT('Ctrl Pts',(-6.43412768719993,11.3231554888659,
-10.2477221527081));
#293689=CARTESIAN_POINT('Ctrl Pts',(-5.0547814365477,11.2607202042168,-10.9937426620182));
#293690=CARTESIAN_POINT('Ctrl Pts',(-2.05331204574442,11.1393082169545,
-11.9295289522943));
#293691=CARTESIAN_POINT('Ctrl Pts',(-0.455853701824085,11.0746896695529,
-12.0963479369981));
#293692=CARTESIAN_POINT('Ctrl Pts',(2.66833162018204,10.9483137185994,-11.8014923603382));
#293693=CARTESIAN_POINT('Ctrl Pts',(4.1665243434072,10.8899838299704,-11.3593715915035));
#293694=CARTESIAN_POINT('Ctrl Pts',(6.92911439357375,10.7653959840471,-9.92177404670185));
#293695=CARTESIAN_POINT('Ctrl Pts',(8.16385933511844,10.7014886122352,-8.93340716820374));
#293696=CARTESIAN_POINT('Ctrl Pts',(10.1863084718864,10.5782773839634,-6.53499150991227));
#293697=CARTESIAN_POINT('Ctrl Pts',(10.9533146286252,10.5173454636238,-5.14703722123551));
#293698=CARTESIAN_POINT('Ctrl Pts',(11.9019288490941,10.391219130035,-2.17678626584642));
#293699=CARTESIAN_POINT('Ctrl Pts',(12.0831664937677,10.3313554208171,-0.625557225353349));
#293700=CARTESIAN_POINT('Ctrl Pts',(11.8440955525672,10.2083941351607,2.49296740377523));
#293701=CARTESIAN_POINT('Ctrl Pts',(11.4132093961979,10.1439001263703,4.02939390434652));
#293702=CARTESIAN_POINT('Ctrl Pts',(9.99287701464981,10.0186629073762,6.82326307060616));
#293703=CARTESIAN_POINT('Ctrl Pts',(9.02633952552437,9.96003821567332,8.05851500568563));
#293704=CARTESIAN_POINT('Ctrl Pts',(6.67373853886068,9.83465590549268,10.0938280512869));
#293705=CARTESIAN_POINT('Ctrl Pts',(5.30914420066387,9.77145631141753,10.873704505715));
#293706=CARTESIAN_POINT('Ctrl Pts',(2.32841002448062,9.65001698073936,11.8786306257011));
#293707=CARTESIAN_POINT('Ctrl Pts',(0.737139668560564,9.58606792592722,
12.0822450578068));
#293708=CARTESIAN_POINT('Ctrl Pts',(-2.39033521655523,9.45955890935075,
11.8607856440462));
#293709=CARTESIAN_POINT('Ctrl Pts',(-3.89747585812195,9.40104631775012,
11.4543296406377));
#293710=CARTESIAN_POINT('Ctrl Pts',(-6.69561629539186,9.27683225742513,
10.0813838633756));
#293711=CARTESIAN_POINT('Ctrl Pts',(-7.95592592650306,9.21272264692234,
9.11969790764957));
#293712=CARTESIAN_POINT('Ctrl Pts',(-10.031280211762,9.08892190382184,6.76930583631912));
#293713=CARTESIAN_POINT('Ctrl Pts',(-10.8277989771356,9.02882012738768,
5.40452225488909));
#293714=CARTESIAN_POINT('Ctrl Pts',(-11.777351614017,8.91141976316705,2.66139535479353));
#293715=CARTESIAN_POINT('Ctrl Pts',(-12.,8.85759349064843,1.33460091143043));
#293716=CARTESIAN_POINT('Ctrl Pts',(-12.,8.80624999997602,-1.55708779203678E-13));
#293717=CARTESIAN_POINT('Origin',(-8.79029313101884E-14,130.96875,0.));
#293718=CARTESIAN_POINT('',(-12.,5.43124999998795,-4.9081531354962E-14));
#293719=CARTESIAN_POINT('',(-12.,5.80624999998803,-4.33395966494788E-14));
#293720=CARTESIAN_POINT('',(-12.0000000000001,130.96875,-1.46957615897682E-15));
#293721=CARTESIAN_POINT('Ctrl Pts',(-12.,5.43124999998796,-1.0547118733939E-13));
#293722=CARTESIAN_POINT('Ctrl Pts',(-12.,5.48316066100001,1.34934369658807));
#293723=CARTESIAN_POINT('Ctrl Pts',(-11.772405113539,5.53760150108826,2.69050573314737));
#293724=CARTESIAN_POINT('Ctrl Pts',(-10.808283298763,5.65555307592163,5.44322675517562));
#293725=CARTESIAN_POINT('Ctrl Pts',(-10.0073226821317,5.71554268054446,
6.80449854506295));
#293726=CARTESIAN_POINT('Ctrl Pts',(-7.92399898072301,5.83942961064025,
9.14754655087858));
#293727=CARTESIAN_POINT('Ctrl Pts',(-6.65985819086981,5.90356699044507,
10.1051273038608));
#293728=CARTESIAN_POINT('Ctrl Pts',(-3.85639847296629,6.0277206464562,11.4682112052612));
#293729=CARTESIAN_POINT('Ctrl Pts',(-2.34791038983903,6.08627502965305,
11.8692437344367));
#293730=CARTESIAN_POINT('Ctrl Pts',(0.779138761520414,6.21276682493733,
12.0794649387276));
#293731=CARTESIAN_POINT('Ctrl Pts',(2.36858754625643,6.27652418701721,11.8705394221944));
#293732=CARTESIAN_POINT('Ctrl Pts',(5.34545009884912,6.39806595211044,10.8559762327792));
#293733=CARTESIAN_POINT('Ctrl Pts',(6.70787386690365,6.46130969798621,10.0712552868311));
#293734=CARTESIAN_POINT('Ctrl Pts',(9.05353598797736,6.58665709630091,8.02786005241167));
#293735=CARTESIAN_POINT('Ctrl Pts',(10.0156193450479,6.64523716971519,6.78973179473641));
#293736=CARTESIAN_POINT('Ctrl Pts',(11.42672840657,6.77054206895559,3.99110653852963));
#293737=CARTESIAN_POINT('Ctrl Pts',(11.8525709468448,6.83504912565561,2.45270210592386));
#293738=CARTESIAN_POINT('Ctrl Pts',(12.08095445666,6.95793566212947,-0.667352081631377));
#293739=CARTESIAN_POINT('Ctrl Pts',(11.8943164326147,7.01790521951554,-2.21814033602071));
#293740=CARTESIAN_POINT('Ctrl Pts',(10.9355322908033,7.14400747227379,-5.18446093676301));
#293741=CARTESIAN_POINT('Ctrl Pts',(10.1642396821313,7.20480980455327,-6.56906772064067));
#293742=CARTESIAN_POINT('Ctrl Pts',(8.13411242723517,7.32810843972088,-8.96059155792173));
#293743=CARTESIAN_POINT('Ctrl Pts',(6.89564370264464,7.39204706166707,-9.94514742218858));
#293744=CARTESIAN_POINT('Ctrl Pts',(4.12786880580135,7.51658356185018,-11.3734491135158));
#293745=CARTESIAN_POINT('Ctrl Pts',(2.62837697546685,7.57492991794071,-11.8104294769704));
#293746=CARTESIAN_POINT('Ctrl Pts',(-0.497141444118381,7.70135979382401,
-12.0947944144799));
#293747=CARTESIAN_POINT('Ctrl Pts',(-2.09458678244572,7.76597781513833,
-11.9224256637474));
#293748=CARTESIAN_POINT('Ctrl Pts',(-5.09375598834702,7.88729675796684,
-10.9758080629586));
#293749=CARTESIAN_POINT('Ctrl Pts',(-6.47088121212119,7.94990729844587,
-10.2246305765451));
#293750=CARTESIAN_POINT('Ctrl Pts',(-8.86418498157722,8.07548536384248,
-8.23710693670026));
#293751=CARTESIAN_POINT('Ctrl Pts',(-9.85693654644579,8.13443839020935,
-7.01887152039891));
#293752=CARTESIAN_POINT('Ctrl Pts',(-11.3312440069665,8.25926239558325,
-4.25328081991911));
#293753=CARTESIAN_POINT('Ctrl Pts',(-11.7915756778617,8.32366530262542,
-2.72878980717319));
#293754=CARTESIAN_POINT('Ctrl Pts',(-11.9813435805726,8.40127455381076,
-0.773107190868359));
#293755=CARTESIAN_POINT('Ctrl Pts',(-12.,8.41638721319939,-0.386336973170943));
#293756=CARTESIAN_POINT('Ctrl Pts',(-12.,8.43124999997595,-2.37795894086901E-13));
#293757=CARTESIAN_POINT('Ctrl Pts',(-12.,8.80624999997602,-1.66255897937617E-13));
#293758=CARTESIAN_POINT('Ctrl Pts',(-12.,8.79813272939646,-0.21099688727731));
#293759=CARTESIAN_POINT('Ctrl Pts',(-11.9944351114046,8.7899385956393,-0.422183581457404));
#293760=CARTESIAN_POINT('Ctrl Pts',(-11.8996707215412,8.71977517169762,
-2.21519103619965));
#293761=CARTESIAN_POINT('Ctrl Pts',(-11.5036732986091,8.65520592074364,
-3.76490938631468));
#293762=CARTESIAN_POINT('Ctrl Pts',(-10.1470244217602,8.529518619843,-6.59116981568474));
#293763=CARTESIAN_POINT('Ctrl Pts',(-9.21109500593409,8.47113480593771,
-7.84610328964277));
#293764=CARTESIAN_POINT('Ctrl Pts',(-6.90646045764588,8.3460101749747,-9.93659887528159));
#293765=CARTESIAN_POINT('Ctrl Pts',(-5.55710042579121,8.28252135004021,
-10.7496081664373));
#293766=CARTESIAN_POINT('Ctrl Pts',(-2.60328607266364,8.16039521741785,
-11.8204720961739));
#293767=CARTESIAN_POINT('Ctrl Pts',(-1.02456992343103,8.09769472397751,
-12.0603195299831));
#293768=CARTESIAN_POINT('Ctrl Pts',(2.09978380262065,7.9713119609373,-11.9156091672496));
#293769=CARTESIAN_POINT('Ctrl Pts',(3.6160626052177,7.9124402673541,-11.5462098306494));
#293770=CARTESIAN_POINT('Ctrl Pts',(6.45008849028493,7.78865737076106,-10.2407902300069));
#293771=CARTESIAN_POINT('Ctrl Pts',(7.73626938443166,7.72437371151312,-9.30739278575468));
#293772=CARTESIAN_POINT('Ctrl Pts',(9.86566953124602,7.60000222059313,-7.00738367027481));
#293773=CARTESIAN_POINT('Ctrl Pts',(10.6923002669755,7.54059348651161,-5.66652775660526));
#293774=CARTESIAN_POINT('Ctrl Pts',(11.7827709730715,7.41483685997714,-2.75197877573901));
#293775=CARTESIAN_POINT('Ctrl Pts',(12.0394907776967,7.35318567197567,-1.20719461145544));
#293776=CARTESIAN_POINT('Ctrl Pts',(11.9496282804079,7.23134321534966,1.93072841285107));
#293777=CARTESIAN_POINT('Ctrl Pts',(11.5895883716215,7.16673248183404,3.49320834764535));
#293778=CARTESIAN_POINT('Ctrl Pts',(10.2983163653039,7.0406245189931,6.35164551791823));
#293779=CARTESIAN_POINT('Ctrl Pts',(9.39346694581025,6.98232748347902,7.6263696258289));
#293780=CARTESIAN_POINT('Ctrl Pts',(7.13819304752949,6.85750648206278,9.77203411777655));
#293781=CARTESIAN_POINT('Ctrl Pts',(5.8050507275199,6.79375797518282,10.6182870045464));
#293782=CARTESIAN_POINT('Ctrl Pts',(2.87930693272437,6.67097520571558,11.755403896766));
#293783=CARTESIAN_POINT('Ctrl Pts',(1.31341015214886,6.60937855666803,12.0314204579715));
#293784=CARTESIAN_POINT('Ctrl Pts',(-1.80733124687646,6.48314191532549,
11.963513117834));
#293785=CARTESIAN_POINT('Ctrl Pts',(-3.33260716233041,6.42373824615532,
11.6312428003402));
#293786=CARTESIAN_POINT('Ctrl Pts',(-6.20150430623542,6.30042997321308,
10.3937813234885));
#293787=CARTESIAN_POINT('Ctrl Pts',(-7.51286969343425,6.23600871932628,
9.489260337549));
#293788=CARTESIAN_POINT('Ctrl Pts',(-9.69544983274317,6.111107812912,7.24018078654216));
#293789=CARTESIAN_POINT('Ctrl Pts',(-10.5517032124387,6.05222272741964,
5.92313055806081));
#293790=CARTESIAN_POINT('Ctrl Pts',(-11.7056476605019,5.92746690877289,
3.0552200217429));
#293791=CARTESIAN_POINT('Ctrl Pts',(-12.,5.86528504658153,1.53453195250642));
#293792=CARTESIAN_POINT('Ctrl Pts',(-12.,5.80624999998803,-7.82707232360735E-14));
#293793=CARTESIAN_POINT('Origin',(-8.79029313101884E-14,130.96875,0.));
#293794=CARTESIAN_POINT('',(-12.,2.43125,1.10010189965134E-12));
#293795=CARTESIAN_POINT('',(-12.,2.80625000000003,2.67779262495037E-14));
#293796=CARTESIAN_POINT('',(-12.0000000000001,130.96875,-1.46957615897682E-15));
#293797=CARTESIAN_POINT('Ctrl Pts',(-12.,2.43125,9.00945984483315E-13));
#293798=CARTESIAN_POINT('Ctrl Pts',(-11.9999999999999,2.4911350116956,1.55662558473029));
#293799=CARTESIAN_POINT('Ctrl Pts',(-11.6971144483733,2.55424279958433,
3.09860916496787));
#293800=CARTESIAN_POINT('Ctrl Pts',(-10.5224531068447,2.67950010145453,
5.97282371668433));
#293801=CARTESIAN_POINT('Ctrl Pts',(-9.66497642460032,2.73802981152558,
7.27907409547783));
#293802=CARTESIAN_POINT('Ctrl Pts',(-7.48003477965859,2.86270132352826,
9.51525533049624));
#293803=CARTESIAN_POINT('Ctrl Pts',(-6.16505976325898,2.92713958298818,
10.4155233167743));
#293804=CARTESIAN_POINT('Ctrl Pts',(-3.29116809533114,3.05037514083823,
11.6430521341568));
#293805=CARTESIAN_POINT('Ctrl Pts',(-1.76459319119719,3.10987070600563,
11.9699074843356));
#293806=CARTESIAN_POINT('Ctrl Pts',(1.35558206429589,3.23608444636122,12.0266224287251));
#293807=CARTESIAN_POINT('Ctrl Pts',(2.91959038239198,3.29753272360557,11.7453424601158));
#293808=CARTESIAN_POINT('Ctrl Pts',(5.84114830094354,3.42040855260187,10.5985502603361));
#293809=CARTESIAN_POINT('Ctrl Pts',(7.17184521901149,3.48419233047212,9.74744812198967));
#293810=CARTESIAN_POINT('Ctrl Pts',(9.41981206730866,3.60896520534576,7.59375046821348));
#293811=CARTESIAN_POINT('Ctrl Pts',(10.3200940077531,3.66726291054294,6.31613384843947));
#293812=CARTESIAN_POINT('Ctrl Pts',(11.601699280568,3.79342956421014,3.453030181618));
#293813=CARTESIAN_POINT('Ctrl Pts',(11.9564118807405,3.85804339370619,1.88873882372495));
#293814=CARTESIAN_POINT('Ctrl Pts',(12.0351273056935,3.97979581503355,-1.25046576458793));
#293815=CARTESIAN_POINT('Ctrl Pts',(11.7727578542884,4.04160719230054,-2.7947425831598));
#293816=CARTESIAN_POINT('Ctrl Pts',(10.6716949431582,4.16733332880825,-5.70505740316497));
#293817=CARTESIAN_POINT('Ctrl Pts',(9.84062591668189,4.22665346776733,-7.0423630525007));
#293818=CARTESIAN_POINT('Ctrl Pts',(7.7032573569002,4.35110634929211,-9.33482775429073));
#293819=CARTESIAN_POINT('Ctrl Pts',(6.41328493131931,4.41541278903545,-10.2639647164412));
#293820=CARTESIAN_POINT('Ctrl Pts',(3.57400587694271,4.53912779617043,-11.5592986217982));
#293821=CARTESIAN_POINT('Ctrl Pts',(2.05637948023744,4.59806770267168,-11.9231780273746));
#293822=CARTESIAN_POINT('Ctrl Pts',(-1.06746740839951,4.7244299637078,-12.0564638092353));
#293823=CARTESIAN_POINT('Ctrl Pts',(-2.64429244292222,4.78695690058136,
-11.8112304892412));
#293824=CARTESIAN_POINT('Ctrl Pts',(-5.59400321749938,4.90918267913456,
-10.730527510895));
#293825=CARTESIAN_POINT('Ctrl Pts',(-6.94101277916468,4.9727120522437,-9.91257768011027));
#293826=CARTESIAN_POINT('Ctrl Pts',(-9.23839107840673,5.0977944387425,-7.81387146280667));
#293827=CARTESIAN_POINT('Ctrl Pts',(-10.1697260942533,5.15615539903364,
-6.55600029274628));
#293828=CARTESIAN_POINT('Ctrl Pts',(-11.5167551841335,5.28190720769102,
-3.72493741785824));
#293829=CARTESIAN_POINT('Ctrl Pts',(-11.9074700526976,5.34648482152274,
-2.17328528068706));
#293830=CARTESIAN_POINT('Ctrl Pts',(-11.9951611270702,5.4160444741397,-0.393673742057767));
#293831=CARTESIAN_POINT('Ctrl Pts',(-12.,5.42368073729527,-0.196752202786124));
#293832=CARTESIAN_POINT('Ctrl Pts',(-12.,5.43124999998796,-1.03528297046296E-13));
#293833=CARTESIAN_POINT('Ctrl Pts',(-12.,5.80624999998803,-7.73410487064402E-14));
#293834=CARTESIAN_POINT('Ctrl Pts',(-12.,5.80549759002151,-0.0195578254213006));
#293835=CARTESIAN_POINT('Ctrl Pts',(-11.9999521864408,5.80474449763365,
-0.0391178538336524));
#293836=CARTESIAN_POINT('Ctrl Pts',(-11.9920734110103,5.74266205787834,
-1.65030248185612));
#293837=CARTESIAN_POINT('Ctrl Pts',(-11.6677074305612,5.67804533094413,
-3.22452936898916));
#293838=CARTESIAN_POINT('Ctrl Pts',(-10.4410870423967,5.55156184943048,
-6.11373419643874));
#293839=CARTESIAN_POINT('Ctrl Pts',(-9.56665307445172,5.49319551600094,
-7.40764685647228));
#293840=CARTESIAN_POINT('Ctrl Pts',(-7.36028372895381,5.36871167674947,
-9.60644215951102));
#293841=CARTESIAN_POINT('Ctrl Pts',(-6.04371840307873,5.30474224885963,
-10.4848029251598));
#293842=CARTESIAN_POINT('Ctrl Pts',(-3.14613399240567,5.18135627761357,
-11.686047639939));
#293843=CARTESIAN_POINT('Ctrl Pts',(-1.59282846915494,5.12068126502382,
-11.9968676396392));
#293844=CARTESIAN_POINT('Ctrl Pts',(1.52398198989469,4.99460363354349,-12.0030430608051));
#293845=CARTESIAN_POINT('Ctrl Pts',(3.05779876832007,4.93452404342637,-11.7066358305338));
#293846=CARTESIAN_POINT('Ctrl Pts',(5.95934066276901,4.81171360655184,-10.5350442308914));
#293847=CARTESIAN_POINT('Ctrl Pts',(7.29430552357991,4.74719414830042,-9.65887480657748));
#293848=CARTESIAN_POINT('Ctrl Pts',(9.52730421974323,4.62182194640091,-7.4593684697147));
#293849=CARTESIAN_POINT('Ctrl Pts',(10.4116643536932,4.56328345421739,-6.16513701376164));
#293850=CARTESIAN_POINT('Ctrl Pts',(11.6400712060169,4.43797205030929,-3.30697913166894));
#293851=CARTESIAN_POINT('Ctrl Pts',(11.9706775872629,4.37468461963252,-1.76933303656079));
#293852=CARTESIAN_POINT('Ctrl Pts',(12.0260930463176,4.25304071884541,1.37462133271613));
#293853=CARTESIAN_POINT('Ctrl Pts',(11.7392589524117,4.18947265612799,2.95074082568823));
#293854=CARTESIAN_POINT('Ctrl Pts',(10.5838743001801,4.06299857987467,5.86284707047165));
#293855=CARTESIAN_POINT('Ctrl Pts',(9.74108044214217,4.00439854555643,7.17654303706032));
#293856=CARTESIAN_POINT('Ctrl Pts',(7.58617056509479,3.88030643972879,9.42969050622614));
#293857=CARTESIAN_POINT('Ctrl Pts',(6.28756241453168,3.81614198603421,10.340969693975));
#293858=CARTESIAN_POINT('Ctrl Pts',(3.41996284795624,3.69216948565523,11.608153535125));
#293859=CARTESIAN_POINT('Ctrl Pts',(1.8797807380391,3.63228872813482,11.9545718356335));
#293860=CARTESIAN_POINT('Ctrl Pts',(-1.23255864397486,3.50639195551972,
12.0367037164367));
#293861=CARTESIAN_POINT('Ctrl Pts',(-2.77499211667185,3.44545490694412,
11.7771214706575));
#293862=CARTESIAN_POINT('Ctrl Pts',(-5.70898826801489,3.32319473827851,
10.6733427728421));
#293863=CARTESIAN_POINT('Ctrl Pts',(-7.0674193640055,3.25860953229914,9.82670660028009));
#293864=CARTESIAN_POINT('Ctrl Pts',(-9.35119537620759,3.13279401741017,
7.67844416870611));
#293865=CARTESIAN_POINT('Ctrl Pts',(-10.2639133847422,3.07445243231789,
6.40745149139112));
#293866=CARTESIAN_POINT('Ctrl Pts',(-11.5600103262491,2.94941321380034,
3.57836252406713));
#293867=CARTESIAN_POINT('Ctrl Pts',(-11.9270998194105,2.88584404053605,
2.04524701332363));
#293868=CARTESIAN_POINT('Ctrl Pts',(-11.9967384171378,2.81872422872653,
0.323190056187629));
#293869=CARTESIAN_POINT('Ctrl Pts',(-12.,2.81246434007284,0.161532919100313));
#293870=CARTESIAN_POINT('Ctrl Pts',(-12.,2.80625000000003,5.24927323830582E-14));
#293871=CARTESIAN_POINT('Origin',(-8.79029313101884E-14,130.96875,0.));
#293872=CARTESIAN_POINT('',(-8.46872171229246,2.43125,-8.50180878165034));
#293873=CARTESIAN_POINT('Ctrl Pts',(-12.,2.80625000000003,5.77315972805081E-14));
#293874=CARTESIAN_POINT('Ctrl Pts',(-12.,2.75181214583704,-1.41503448306261));
#293875=CARTESIAN_POINT('Ctrl Pts',(-11.7497034409074,2.69462147714694,
-2.82029817695595));
#293876=CARTESIAN_POINT('Ctrl Pts',(-10.9573405555813,2.60202148529659,
-4.96984876681417));
#293877=CARTESIAN_POINT('Ctrl Pts',(-10.5667212506353,2.56697606517402,
-5.75388464177398));
#293878=CARTESIAN_POINT('Ctrl Pts',(-9.6267115219977,2.49896581374268,-7.21628658515935));
#293879=CARTESIAN_POINT('Ctrl Pts',(-9.08163925424091,2.46582425285662,
-7.89127657272241));
#293880=CARTESIAN_POINT('Ctrl Pts',(-8.4687217122924,2.43125000000001,-8.50180878165037));
#293881=CARTESIAN_POINT('Origin',(-1.38777878078145E-14,2.43125000000001,
0.));
#293882=CARTESIAN_POINT('Origin',(-4.54192801987171E-14,57.2,0.));
#293883=CARTESIAN_POINT('',(-11.251117508365,58.9988824916351,-9.57071644917375E-15));
#293884=CARTESIAN_POINT('Ctrl Pts',(9.41568944744522,58.25,-7.43940805637572));
#293885=CARTESIAN_POINT('Ctrl Pts',(8.79573603498597,58.2739415406423,-8.18543385222336));
#293886=CARTESIAN_POINT('Ctrl Pts',(8.08700707828182,58.2986811839343,-8.85294058875071));
#293887=CARTESIAN_POINT('Ctrl Pts',(6.53424618639461,58.348352376611,-9.99336249557727));
#293888=CARTESIAN_POINT('Ctrl Pts',(5.6978562173087,58.3730962739907,-10.4646913423123));
#293889=CARTESIAN_POINT('Ctrl Pts',(4.21229181931588,58.4139168883336,-11.0803254365483));
#293890=CARTESIAN_POINT('Ctrl Pts',(3.58715467640316,58.4299857748698,-11.281544084094));
#293891=CARTESIAN_POINT('Ctrl Pts',(1.45628305848908,58.4851817311957,-11.7744414883963));
#293892=CARTESIAN_POINT('Ctrl Pts',(-0.090158574616811,58.5256317479014,
-11.8236949834757));
#293893=CARTESIAN_POINT('Ctrl Pts',(-3.02394526826764,58.6031803869245,
-11.3392745716886));
#293894=CARTESIAN_POINT('Ctrl Pts',(-4.49506113981352,58.6411124276446,
-10.8282548234504));
#293895=CARTESIAN_POINT('Ctrl Pts',(-7.12494968894065,58.723324568187,-9.17826743218203));
#293896=CARTESIAN_POINT('Ctrl Pts',(-8.20553019239892,58.7626401442854,
-8.17129870321612));
#293897=CARTESIAN_POINT('Ctrl Pts',(-10.0520993471377,58.8433462973028,
-5.64304338821277));
#293898=CARTESIAN_POINT('Ctrl Pts',(-10.6336060765998,58.8835565622676,
-4.23613498781373));
#293899=CARTESIAN_POINT('Ctrl Pts',(-11.1741358391133,58.9468224589001,
-1.96620905423901));
#293900=CARTESIAN_POINT('Ctrl Pts',(-11.2766767876284,58.9733232123716,
-0.982555718105193));
#293901=CARTESIAN_POINT('Ctrl Pts',(-11.251117508365,58.9988824916351,1.77635683940025E-14));
#293902=CARTESIAN_POINT('',(-13.05,57.2,-1.59816407288729E-15));
#293903=CARTESIAN_POINT('',(-13.05,57.2,-1.59816407288729E-15));
#293904=CARTESIAN_POINT('Origin',(-4.54192801987171E-14,57.2,0.));
#293905=CARTESIAN_POINT('',(6.83270577527258,60.1985571585059,-7.37194919844001));
#293906=CARTESIAN_POINT('Ctrl Pts',(-11.251117508365,58.9988824916351,3.27515792264421E-14));
#293907=CARTESIAN_POINT('Ctrl Pts',(-11.2385726688954,59.0114273311046,
0.482251616975299));
#293908=CARTESIAN_POINT('Ctrl Pts',(-11.1947127197006,59.0242689258418,
0.964213182637807));
#293909=CARTESIAN_POINT('Ctrl Pts',(-10.895798509458,59.0761575489079,2.86503292607173));
#293910=CARTESIAN_POINT('Ctrl Pts',(-10.3986941703556,59.1162399397277,
4.23081678926045));
#293911=CARTESIAN_POINT('Ctrl Pts',(-9.28561894190705,59.1748510495143,
6.07866846337327));
#293912=CARTESIAN_POINT('Ctrl Pts',(-8.85456618599315,59.1937120748971,
6.66018982610041));
#293913=CARTESIAN_POINT('Ctrl Pts',(-7.40967389241113,59.2520150973381,
8.25170914496314));
#293914=CARTESIAN_POINT('Ctrl Pts',(-6.25222753197104,59.2923785121678,
9.11138079427429));
#293915=CARTESIAN_POINT('Ctrl Pts',(-3.74760729768966,59.369570655975,10.3028052876729));
#293916=CARTESIAN_POINT('Ctrl Pts',(-2.34928610066821,59.4075104184351,
10.6948750747753));
#293917=CARTESIAN_POINT('Ctrl Pts',(0.779711812100376,59.4964841752171,
10.8441374514475));
#293918=CARTESIAN_POINT('Ctrl Pts',(2.19507014871295,59.5372684261364,10.5537953412713));
#293919=CARTESIAN_POINT('Ctrl Pts',(4.5699429723945,59.6064277448452,9.70309149882849));
#293920=CARTESIAN_POINT('Ctrl Pts',(5.72066828246454,59.6447411400348,9.02739600905606));
#293921=CARTESIAN_POINT('Ctrl Pts',(7.76853464378474,59.7237483857297,7.23875024917893));
#293922=CARTESIAN_POINT('Ctrl Pts',(8.63524372650229,59.7622453507951,6.1148459525091));
#293923=CARTESIAN_POINT('Ctrl Pts',(9.83658164315294,59.8417129538795,3.65453270819226));
#293924=CARTESIAN_POINT('Ctrl Pts',(10.1857205813106,59.8816061800705,2.35290905826649));
#293925=CARTESIAN_POINT('Ctrl Pts',(10.3729006217155,59.9595796521074,-0.320720838433725));
#293926=CARTESIAN_POINT('Ctrl Pts',(10.205314917492,59.9976670280176,-1.66555307451394));
#293927=CARTESIAN_POINT('Ctrl Pts',(9.49559971070312,60.0651115369737,-3.78971049737241));
#293928=CARTESIAN_POINT('Ctrl Pts',(9.1027240403221,60.0920685051517,-4.59569513239433));
#293929=CARTESIAN_POINT('Ctrl Pts',(8.11140739263744,60.1450250918943,-6.09351276754362));
#293930=CARTESIAN_POINT('Ctrl Pts',(7.51526380442641,60.1710414084933,-6.77683587343302));
#293931=CARTESIAN_POINT('Ctrl Pts',(6.83270577527257,60.1985571585058,-7.37194919844003));
#293932=CARTESIAN_POINT('',(-0.358381257737887,60.1985571585059,-10.0450518201713));
#293933=CARTESIAN_POINT('Origin',(-8.10462807976364E-14,60.1985571585057,
6.21724893790088E-14));
#293934=CARTESIAN_POINT('Ctrl Pts',(-0.358381257737859,60.1985571585059,
-10.0450518201713));
#293935=CARTESIAN_POINT('Ctrl Pts',(0.569600497855516,60.0920908389641,
-10.1846938468385));
#293936=CARTESIAN_POINT('Ctrl Pts',(1.86768826672467,59.9489768555399,-10.2622313963477));
#293937=CARTESIAN_POINT('Ctrl Pts',(4.82229184539531,59.6316500051715,-9.5602844533037));
#293938=CARTESIAN_POINT('Ctrl Pts',(6.09703360509207,59.4828126471393,-8.98125348648291));
#293939=CARTESIAN_POINT('Ctrl Pts',(8.64359555920175,59.1568934783279,-7.16524174281715));
#293940=CARTESIAN_POINT('Ctrl Pts',(9.58558008715325,59.0150265477672,-5.97673601271509));
#293941=CARTESIAN_POINT('Ctrl Pts',(10.7798566334032,58.7884331321821,-4.04272726160383));
#293942=CARTESIAN_POINT('Ctrl Pts',(11.2179091250566,58.6795346125953,-3.03593820382734));
#293943=CARTESIAN_POINT('Ctrl Pts',(11.8513180753988,58.4474576877315,-0.725960973686208));
#293944=CARTESIAN_POINT('Ctrl Pts',(11.9400790733319,58.3432212931802,0.43745433545044));
#293945=CARTESIAN_POINT('Ctrl Pts',(11.9139873655789,58.25,1.43419142823615));
#293946=CARTESIAN_POINT('Origin',(-8.79029313101884E-14,130.96875,0.));
#293947=CARTESIAN_POINT('',(-4.83831102398129,130.817307158506,8.81034900733485));
#293948=CARTESIAN_POINT('',(-10.3754400975249,130.493309902475,-3.34148109778276E-15));
#293949=CARTESIAN_POINT('Ctrl Pts',(-10.3754400975249,130.493309902475,
-4.85722573273506E-15));
#293950=CARTESIAN_POINT('Ctrl Pts',(-10.3638450429889,130.504904957011,
0.411047722935234));
#293951=CARTESIAN_POINT('Ctrl Pts',(-10.3275450278176,130.516761565068,
0.822042306381597));
#293952=CARTESIAN_POINT('Ctrl Pts',(-10.0721499446089,130.567155272434,
2.52967838917212));
#293953=CARTESIAN_POINT('Ctrl Pts',(-9.63043563877547,130.606815619881,
3.77975573956643));
#293954=CARTESIAN_POINT('Ctrl Pts',(-8.47232889963708,130.674443677503,
5.75246532316119));
#293955=CARTESIAN_POINT('Ctrl Pts',(-7.85961320778648,130.702096724505,
6.52278639205452));
#293956=CARTESIAN_POINT('Ctrl Pts',(-6.45488736456084,130.759774236249,
7.83679328916589));
#293957=CARTESIAN_POINT('Ctrl Pts',(-5.67876562648238,130.788661778153,
8.38148366250018));
#293958=CARTESIAN_POINT('Ctrl Pts',(-4.83831102398136,130.817307158506,
8.81034900733487));
#293959=CARTESIAN_POINT('',(2.81735069959344,130.817307158506,9.64852518426128));
#293960=CARTESIAN_POINT('Origin',(1.77635683940025E-14,130.817307158505,
-7.7715611723761E-13));
#293961=CARTESIAN_POINT('Ctrl Pts',(-11.894167785564,128.86875,1.59021152330507));
#293962=CARTESIAN_POINT('Ctrl Pts',(-11.6160944182043,128.984669600074,
2.79534433683652));
#293963=CARTESIAN_POINT('Ctrl Pts',(-11.1495590589446,129.104808940769,
3.9486436044955));
#293964=CARTESIAN_POINT('Ctrl Pts',(-9.99474123522102,129.322681085237,
5.86611791592308));
#293965=CARTESIAN_POINT('Ctrl Pts',(-9.24106914132451,129.438710702818,
6.87629466505421));
#293966=CARTESIAN_POINT('Ctrl Pts',(-7.60212862518274,129.653506500676,
8.27681501381399));
#293967=CARTESIAN_POINT('Ctrl Pts',(-7.00852279237346,129.727188567012,
8.69083371192293));
#293968=CARTESIAN_POINT('Ctrl Pts',(-5.75231106181202,129.87582352063,9.39498084136462));
#293969=CARTESIAN_POINT('Ctrl Pts',(-5.09304579581803,129.9504191299,9.68406859338561));
#293970=CARTESIAN_POINT('Ctrl Pts',(-3.1915580491957,130.156529510499,10.3049448070743));
#293971=CARTESIAN_POINT('Ctrl Pts',(-1.94706281547003,130.282347955964,
10.4821475592344));
#293972=CARTESIAN_POINT('Ctrl Pts',(0.523645534039794,130.552019108861,
10.3725726766803));
#293973=CARTESIAN_POINT('Ctrl Pts',(1.70640129850129,130.686168481297,10.1095352252478));
#293974=CARTESIAN_POINT('Ctrl Pts',(2.8173506995935,130.817307158506,9.64852518426143));
#293975=CARTESIAN_POINT('Ctrl Pts',(-7.30108394240721,128.868749999999,
9.52334884722601));
#293976=CARTESIAN_POINT('Ctrl Pts',(-6.30302171533989,128.90036926442,10.248671949143));
#293977=CARTESIAN_POINT('Ctrl Pts',(-5.19895338212386,128.932055884534,
10.8155858694633));
#293978=CARTESIAN_POINT('Ctrl Pts',(-2.84939595618331,128.993471671357,
11.5949956950555));
#293979=CARTESIAN_POINT('Ctrl Pts',(-1.6294605374271,129.024443351536,11.7964401725797));
#293980=CARTESIAN_POINT('Ctrl Pts',(1.19446780691268,129.097950041924,11.8173195636497));
#293981=CARTESIAN_POINT('Ctrl Pts',(2.66422769795,129.136066177321,11.508354646803));
#293982=CARTESIAN_POINT('Ctrl Pts',(5.36881592504784,129.209269604011,10.4617874232397));
#293983=CARTESIAN_POINT('Ctrl Pts',(6.67010341062351,129.249841492879,9.63525664930798));
#293984=CARTESIAN_POINT('Ctrl Pts',(8.80069211440203,129.327673228521,7.59990649152918));
#293985=CARTESIAN_POINT('Ctrl Pts',(9.71750054011973,129.365467783131,6.36547005128502));
#293986=CARTESIAN_POINT('Ctrl Pts',(10.6671105988966,129.428419178648,4.20075858084496));
#293987=CARTESIAN_POINT('Ctrl Pts',(10.8985785326509,129.448468661738,3.49231250117377));
#293988=CARTESIAN_POINT('Ctrl Pts',(11.3798900320565,129.50832678461,1.32145897720948));
#293989=CARTESIAN_POINT('Ctrl Pts',(11.4183347881864,129.546093788355,-0.181457365732128));
#293990=CARTESIAN_POINT('Ctrl Pts',(11.035404631011,129.605797053053,-2.36908459971864));
#293991=CARTESIAN_POINT('Ctrl Pts',(10.838193172437,129.625864165925,-3.07808845028999));
#293992=CARTESIAN_POINT('Ctrl Pts',(10.0527919462299,129.685481946684,-5.10722353689452));
#293993=CARTESIAN_POINT('Ctrl Pts',(9.27574806257917,129.723282730156,-6.34546975494142));
#293994=CARTESIAN_POINT('Ctrl Pts',(7.30265479182673,129.801149008045,-8.43888275379305));
#293995=CARTESIAN_POINT('Ctrl Pts',(6.12615848216244,129.84141096262,-9.28030131521465));
#293996=CARTESIAN_POINT('Ctrl Pts',(3.51132031891206,129.92061366261,-10.4691433409554));
#293997=CARTESIAN_POINT('Ctrl Pts',(2.09323021142943,129.958633060114,-10.8045158956757));
#293998=CARTESIAN_POINT('Ctrl Pts',(-0.910552320525702,130.043534699612,
-10.898914083415));
#293999=CARTESIAN_POINT('Ctrl Pts',(-2.33181430589621,130.083835312678,
-10.6070904248003));
#294000=CARTESIAN_POINT('Ctrl Pts',(-4.77795410356712,130.155467557091,
-9.68150441188508));
#294001=CARTESIAN_POINT('Ctrl Pts',(-5.92816571815587,130.194022804729,
-8.97732226984948));
#294002=CARTESIAN_POINT('Ctrl Pts',(-7.89717510050072,130.270679844274,
-7.19030195250223));
#294003=CARTESIAN_POINT('Ctrl Pts',(-8.77341371877538,130.308974063784,
-6.06403251894919));
#294004=CARTESIAN_POINT('Ctrl Pts',(-9.9732821988043,130.391291620567,-3.48310903998621));
#294005=CARTESIAN_POINT('Ctrl Pts',(-10.300207709712,130.431340575298,-2.16021817703969));
#294006=CARTESIAN_POINT('Ctrl Pts',(-10.3801921577127,130.477950105763,
-0.541661562394141));
#294007=CARTESIAN_POINT('Ctrl Pts',(-10.383079668429,130.485670331571,-0.270824791260495));
#294008=CARTESIAN_POINT('Ctrl Pts',(-10.3754400975249,130.493309902475,
4.42701431069281E-14));
#294009=CARTESIAN_POINT('',(-9.9000000000001,130.96875,-1.21240033115588E-15));
#294010=CARTESIAN_POINT('',(-9.9000000000001,130.96875,-1.21240033115588E-15));
#294011=CARTESIAN_POINT('Origin',(-8.79029313101884E-14,130.96875,0.));
#294012=CARTESIAN_POINT('Origin',(-8.79029313101884E-14,130.96875,0.));
#294013=CARTESIAN_POINT('',(11.6184932898974,91.186,3.00176842421407));
#294014=CARTESIAN_POINT('Ctrl Pts',(-12.0000000000001,92.80624999964,-3.4555691641458E-14));
#294015=CARTESIAN_POINT('Ctrl Pts',(-12.0000000000001,92.7882122178229,
-0.468866447099216));
#294016=CARTESIAN_POINT('Ctrl Pts',(-11.972521673645,92.769811805124,-0.938230718020533));
#294017=CARTESIAN_POINT('Ctrl Pts',(-11.733006065977,92.6886980402866,-2.96884416604449));
#294018=CARTESIAN_POINT('Ctrl Pts',(-11.2428649939964,92.6244138443026,
-4.48056379236747));
#294019=CARTESIAN_POINT('Ctrl Pts',(-9.71367031873571,92.5000404579741,
-7.21660735543917));
#294020=CARTESIAN_POINT('Ctrl Pts',(-8.69399354379183,92.440633818221,-8.41719962742405));
#294021=CARTESIAN_POINT('Ctrl Pts',(-6.25923585411257,92.3148778940627,
-10.3551473117068));
#294022=CARTESIAN_POINT('Ctrl Pts',(-4.8694412051415,92.2532230340454,-11.0767878398891));
#294023=CARTESIAN_POINT('Ctrl Pts',(-1.85738137910691,92.1313826546791,
-11.9612501088246));
#294024=CARTESIAN_POINT('Ctrl Pts',(-0.260114213238191,92.0667718405922,
-12.1017951164519));
#294025=CARTESIAN_POINT('Ctrl Pts',(2.85747996146335,91.9406625071477,-11.7572747332122));
#294026=CARTESIAN_POINT('Ctrl Pts',(4.34945959390987,91.8823654951006,-11.2907447234468));
#294027=CARTESIAN_POINT('Ctrl Pts',(7.08715085155504,91.7575455999654,-9.80911729155921));
#294028=CARTESIAN_POINT('Ctrl Pts',(8.30403841759875,91.6937962665103,-8.80281869876389));
#294029=CARTESIAN_POINT('Ctrl Pts',(10.289789073564,91.5710113283916,-6.37182103468252));
#294030=CARTESIAN_POINT('Ctrl Pts',(11.0362878674002,91.5094181611936,-4.96793793338489));
#294031=CARTESIAN_POINT('Ctrl Pts',(11.8058222286519,91.4014840499907,-2.41238131425744));
#294032=CARTESIAN_POINT('Ctrl Pts',(11.976544227546,91.3575745868965,-1.32648830144042));
#294033=CARTESIAN_POINT('Ctrl Pts',(12.0188779046423,91.2730160899065,0.85773434553886));
#294034=CARTESIAN_POINT('Ctrl Pts',(11.8913002682865,91.2300321596809,1.94585550891945));
#294035=CARTESIAN_POINT('Ctrl Pts',(11.6184932898973,91.186,3.00176842421425));
#294036=CARTESIAN_POINT('',(10.3435570531169,91.185999999999,-6.08365247930179));
#294037=CARTESIAN_POINT('Origin',(-6.49919226343618E-14,91.186,0.));
#294038=CARTESIAN_POINT('Ctrl Pts',(10.343557053117,91.185999999999,-6.08365247930161));
#294039=CARTESIAN_POINT('Ctrl Pts',(9.55890855690799,91.2471314138738,-7.41772876238869));
#294040=CARTESIAN_POINT('Ctrl Pts',(8.52353606068608,91.3064930697652,-8.58747742168945));
#294041=CARTESIAN_POINT('Ctrl Pts',(6.06330327988208,91.4317877484173,-10.4709623620909));
#294042=CARTESIAN_POINT('Ctrl Pts',(4.66089813768456,91.4927127095218,-11.1660411123352));
#294043=CARTESIAN_POINT('Ctrl Pts',(1.65780900183523,91.6141902168476,-11.9872326559139));
#294044=CARTESIAN_POINT('Ctrl Pts',(0.0843670061797239,91.6778372825548,
-12.101022716674));
#294045=CARTESIAN_POINT('Ctrl Pts',(-3.00455409179326,91.8027867656814,
-11.7206623108048));
#294046=CARTESIAN_POINT('Ctrl Pts',(-4.49136392438059,91.8610998850578,
-11.2351643727108));
#294047=CARTESIAN_POINT('Ctrl Pts',(-7.23010729887462,91.9870412753891,
-9.70781666209722));
#294048=CARTESIAN_POINT('Ctrl Pts',(-8.44866993703788,92.0516394256888,
-8.66812365438208));
#294049=CARTESIAN_POINT('Ctrl Pts',(-10.3885381900297,92.1737257864082,
-6.20335539022936));
#294050=CARTESIAN_POINT('Ctrl Pts',(-11.1022697317196,92.2349539470959,
-4.8107460550984));
#294051=CARTESIAN_POINT('Ctrl Pts',(-11.8428241618736,92.343137182588,-2.23929765448896));
#294052=CARTESIAN_POINT('Ctrl Pts',(-12.0000000000001,92.3881104835417,
-1.1213502773074));
#294053=CARTESIAN_POINT('Ctrl Pts',(-12.0000000000001,92.43124999964,1.0547118733939E-14));
#294054=CARTESIAN_POINT('Ctrl Pts',(-10.0514428414942,-1.69374999998275,
2.46189346052968E-15));
#294055=CARTESIAN_POINT('Ctrl Pts',(-10.0514428414942,-1.54374999998335,
3.26591175476071));
#294056=CARTESIAN_POINT('Ctrl Pts',(-8.1317880767572,-1.39374999998395,
5.90808986649102));
#294057=CARTESIAN_POINT('Ctrl Pts',(-6.21213331202023,-1.24374999998455,
8.55026797822134));
#294058=CARTESIAN_POINT('Ctrl Pts',(-3.10606665601012,-1.09374999998515,
9.5594902125713));
#294059=CARTESIAN_POINT('Ctrl Pts',(-9.99267389681068E-15,-0.943749999985747,
10.5687124469213));
#294060=CARTESIAN_POINT('Ctrl Pts',(3.1060666560101,-0.793749999986346,
9.5594902125713));
#294061=CARTESIAN_POINT('Ctrl Pts',(6.21213331202021,-0.643749999986944,
8.55026797822134));
#294062=CARTESIAN_POINT('Ctrl Pts',(8.13178807675718,-0.493749999987543,
5.90808986649102));
#294063=CARTESIAN_POINT('Ctrl Pts',(10.0514428414942,-0.343749999988142,
3.2659117547607));
#294064=CARTESIAN_POINT('Ctrl Pts',(10.0514428414942,-0.193749999988742,
-1.23094673026484E-15));
#294065=CARTESIAN_POINT('Ctrl Pts',(10.0514428414942,-0.0437499999893418,
-3.26591175476071));
#294066=CARTESIAN_POINT('Ctrl Pts',(8.13178807675718,0.106250000010057,
-5.90808986649102));
#294067=CARTESIAN_POINT('Ctrl Pts',(6.2121333120202,0.256250000009456,-8.55026797822134));
#294068=CARTESIAN_POINT('Ctrl Pts',(3.10606665601009,0.406250000008854,
-9.5594902125713));
#294069=CARTESIAN_POINT('Ctrl Pts',(-1.34451165064878E-14,0.556250000008252,
-10.5687124469213));
#294070=CARTESIAN_POINT('Ctrl Pts',(-3.10606665601012,0.70625000000765,
-9.5594902125713));
#294071=CARTESIAN_POINT('Ctrl Pts',(-6.21213331202023,0.856250000007049,
-8.55026797822134));
#294072=CARTESIAN_POINT('Ctrl Pts',(-8.1317880767572,1.00625000000645,-5.90808986649102));
#294073=CARTESIAN_POINT('Ctrl Pts',(-10.0514428414942,1.15625000000585,
-3.2659117547607));
#294074=CARTESIAN_POINT('Ctrl Pts',(-10.0514428414942,1.30625000000525,
2.46189346052968E-15));
#294075=CARTESIAN_POINT('Ctrl Pts',(-10.0514428414942,1.45625000000465,
3.26591175476071));
#294076=CARTESIAN_POINT('Ctrl Pts',(-8.1317880767572,1.60625000000405,5.90808986649102));
#294077=CARTESIAN_POINT('Ctrl Pts',(-6.21213331202023,1.75625000000345,
8.55026797822134));
#294078=CARTESIAN_POINT('Ctrl Pts',(-3.10606665601012,1.90625000000285,
9.5594902125713));
#294079=CARTESIAN_POINT('Ctrl Pts',(-1.17203831684725E-14,2.05625000000225,
10.5687124469213));
#294080=CARTESIAN_POINT('Ctrl Pts',(3.1060666560101,2.20625000000165,9.5594902125713));
#294081=CARTESIAN_POINT('Ctrl Pts',(6.2121333120202,2.35625000000106,8.55026797822134));
#294082=CARTESIAN_POINT('Ctrl Pts',(8.13178807675718,2.50625000000046,5.90808986649102));
#294083=CARTESIAN_POINT('Ctrl Pts',(10.0514428414942,2.65624999999986,3.2659117547607));
#294084=CARTESIAN_POINT('Ctrl Pts',(10.0514428414942,2.80624999999926,-1.23094673026484E-15));
#294085=CARTESIAN_POINT('Ctrl Pts',(10.0514428414942,2.95624999999866,-3.26591175476071));
#294086=CARTESIAN_POINT('Ctrl Pts',(8.13178807675718,3.10624999999806,-5.90808986649102));
#294087=CARTESIAN_POINT('Ctrl Pts',(6.2121333120202,3.25624999999746,-8.55026797822134));
#294088=CARTESIAN_POINT('Ctrl Pts',(3.10606665601009,3.40624999999685,-9.5594902125713));
#294089=CARTESIAN_POINT('Ctrl Pts',(-1.51728257781496E-14,3.55624999999625,
-10.5687124469213));
#294090=CARTESIAN_POINT('Ctrl Pts',(-3.10606665601012,3.70624999999565,
-9.5594902125713));
#294091=CARTESIAN_POINT('Ctrl Pts',(-6.21213331202023,3.85624999999505,
-8.55026797822134));
#294092=CARTESIAN_POINT('Ctrl Pts',(-8.13178807675721,4.00624999999445,
-5.90808986649102));
#294093=CARTESIAN_POINT('Ctrl Pts',(-10.0514428414942,4.15624999999385,
-3.2659117547607));
#294094=CARTESIAN_POINT('Ctrl Pts',(-10.0514428414942,4.30624999999325,
2.46189346052968E-15));
#294095=CARTESIAN_POINT('Ctrl Pts',(-10.0514428414942,4.45624999999265,
3.26591175476071));
#294096=CARTESIAN_POINT('Ctrl Pts',(-8.13178807675721,4.60624999999205,
5.90808986649102));
#294097=CARTESIAN_POINT('Ctrl Pts',(-6.21213331202023,4.75624999999145,
8.55026797822134));
#294098=CARTESIAN_POINT('Ctrl Pts',(-3.10606665601012,4.90624999999085,
9.5594902125713));
#294099=CARTESIAN_POINT('Ctrl Pts',(-1.34480924401344E-14,5.05624999999025,
10.5687124469213));
#294100=CARTESIAN_POINT('Ctrl Pts',(3.10606665601009,5.20624999998966,9.5594902125713));
#294101=CARTESIAN_POINT('Ctrl Pts',(6.2121333120202,5.35624999998906,8.55026797822134));
#294102=CARTESIAN_POINT('Ctrl Pts',(8.13178807675718,5.50624999998846,5.90808986649102));
#294103=CARTESIAN_POINT('Ctrl Pts',(10.0514428414942,5.65624999998786,3.2659117547607));
#294104=CARTESIAN_POINT('Ctrl Pts',(10.0514428414941,5.80624999998726,-1.23094673026484E-15));
#294105=CARTESIAN_POINT('Ctrl Pts',(10.0514428414941,5.95624999998666,-3.26591175476071));
#294106=CARTESIAN_POINT('Ctrl Pts',(8.13178807675717,6.10624999998606,-5.90808986649102));
#294107=CARTESIAN_POINT('Ctrl Pts',(6.2121333120202,6.25624999998545,-8.55026797822134));
#294108=CARTESIAN_POINT('Ctrl Pts',(3.10606665601009,6.40624999998485,-9.5594902125713));
#294109=CARTESIAN_POINT('Ctrl Pts',(-1.69005350498115E-14,6.55624999998425,
-10.5687124469213));
#294110=CARTESIAN_POINT('Ctrl Pts',(-3.10606665601013,6.70624999998365,
-9.5594902125713));
#294111=CARTESIAN_POINT('Ctrl Pts',(-6.21213331202023,6.85624999998305,
-8.55026797822134));
#294112=CARTESIAN_POINT('Ctrl Pts',(-8.13178807675721,7.00624999998245,
-5.90808986649102));
#294113=CARTESIAN_POINT('Ctrl Pts',(-10.0514428414942,7.15624999998184,
-3.2659117547607));
#294114=CARTESIAN_POINT('Ctrl Pts',(-10.0514428414942,7.30624999998125,
2.46189346052968E-15));
#294115=CARTESIAN_POINT('Ctrl Pts',(-10.0514428414942,7.45624999998065,
3.26591175476071));
#294116=CARTESIAN_POINT('Ctrl Pts',(-8.13178807675721,7.60624999998005,
5.90808986649102));
#294117=CARTESIAN_POINT('Ctrl Pts',(-6.21213331202023,7.75624999997945,
8.55026797822134));
#294118=CARTESIAN_POINT('Ctrl Pts',(-3.10606665601012,7.90624999997885,
9.5594902125713));
#294119=CARTESIAN_POINT('Ctrl Pts',(-1.51758017117962E-14,8.05624999997825,
10.5687124469213));
#294120=CARTESIAN_POINT('Ctrl Pts',(3.10606665601009,8.20624999997765,9.5594902125713));
#294121=CARTESIAN_POINT('Ctrl Pts',(6.2121333120202,8.35624999997706,8.55026797822134));
#294122=CARTESIAN_POINT('Ctrl Pts',(8.13178807675717,8.50624999997646,5.90808986649102));
#294123=CARTESIAN_POINT('Ctrl Pts',(10.0514428414942,8.65624999997586,3.2659117547607));
#294124=CARTESIAN_POINT('Ctrl Pts',(10.0514428414941,8.80624999997526,-1.23094673026484E-15));
#294125=CARTESIAN_POINT('Ctrl Pts',(10.0514428414941,8.95624999997466,-3.26591175476071));
#294126=CARTESIAN_POINT('Ctrl Pts',(8.13178807675717,9.10624999997406,-5.90808986649102));
#294127=CARTESIAN_POINT('Ctrl Pts',(6.2121333120202,9.25624999997346,-8.55026797822134));
#294128=CARTESIAN_POINT('Ctrl Pts',(3.10606665601009,9.40624999997286,-9.5594902125713));
#294129=CARTESIAN_POINT('Ctrl Pts',(-1.86282443214733E-14,9.55624999997225,
-10.5687124469213));
#294130=CARTESIAN_POINT('Ctrl Pts',(-3.10606665601013,9.70624999997165,
-9.5594902125713));
#294131=CARTESIAN_POINT('Ctrl Pts',(-6.21213331202023,9.85624999997105,
-8.55026797822134));
#294132=CARTESIAN_POINT('Ctrl Pts',(-8.13178807675721,10.0062499999704,
-5.90808986649102));
#294133=CARTESIAN_POINT('Ctrl Pts',(-10.0514428414942,10.1562499999698,
-3.2659117547607));
#294134=CARTESIAN_POINT('Ctrl Pts',(-10.0514428414942,10.3062499999692,
2.46189346052968E-15));
#294135=CARTESIAN_POINT('Ctrl Pts',(-10.0514428414942,10.4562499999686,
3.26591175476071));
#294136=CARTESIAN_POINT('Ctrl Pts',(-8.13178807675721,10.606249999968,5.90808986649102));
#294137=CARTESIAN_POINT('Ctrl Pts',(-6.21213331202023,10.7562499999674,
8.55026797822134));
#294138=CARTESIAN_POINT('Ctrl Pts',(-3.10606665601013,10.9062499999668,
9.5594902125713));
#294139=CARTESIAN_POINT('Ctrl Pts',(-1.6903510983458E-14,11.0562499999663,
10.5687124469213));
#294140=CARTESIAN_POINT('Ctrl Pts',(3.10606665601009,11.2062499999657,9.5594902125713));
#294141=CARTESIAN_POINT('Ctrl Pts',(6.2121333120202,11.3562499999651,8.55026797822134));
#294142=CARTESIAN_POINT('Ctrl Pts',(8.13178807675717,11.5062499999645,5.90808986649102));
#294143=CARTESIAN_POINT('Ctrl Pts',(10.0514428414941,11.6562499999639,3.2659117547607));
#294144=CARTESIAN_POINT('Ctrl Pts',(10.0514428414941,11.8062499999633,-1.23094673026484E-15));
#294145=CARTESIAN_POINT('Ctrl Pts',(10.0514428414941,11.9562499999627,-3.26591175476071));
#294146=CARTESIAN_POINT('Ctrl Pts',(8.13178807675717,12.1062499999621,-5.90808986649102));
#294147=CARTESIAN_POINT('Ctrl Pts',(6.2121333120202,12.2562499999615,-8.55026797822134));
#294148=CARTESIAN_POINT('Ctrl Pts',(3.10606665601009,12.4062499999609,-9.5594902125713));
#294149=CARTESIAN_POINT('Ctrl Pts',(-2.03559535931351E-14,12.5562499999603,
-10.5687124469213));
#294150=CARTESIAN_POINT('Ctrl Pts',(-3.10606665601013,12.7062499999597,
-9.5594902125713));
#294151=CARTESIAN_POINT('Ctrl Pts',(-6.21213331202024,12.856249999959,-8.55026797822134));
#294152=CARTESIAN_POINT('Ctrl Pts',(-8.13178807675721,13.0062499999584,
-5.90808986649102));
#294153=CARTESIAN_POINT('Ctrl Pts',(-10.0514428414942,13.1562499999578,
-3.2659117547607));
#294154=CARTESIAN_POINT('Ctrl Pts',(-10.0514428414942,13.3062499999572,
2.46189346052968E-15));
#294155=CARTESIAN_POINT('Ctrl Pts',(-10.0514428414942,13.4562499999566,
3.26591175476071));
#294156=CARTESIAN_POINT('Ctrl Pts',(-8.13178807675721,13.606249999956,5.90808986649102));
#294157=CARTESIAN_POINT('Ctrl Pts',(-6.21213331202023,13.7562499999554,
8.55026797822134));
#294158=CARTESIAN_POINT('Ctrl Pts',(-3.10606665601013,13.9062499999549,
9.5594902125713));
#294159=CARTESIAN_POINT('Ctrl Pts',(-1.86312202551199E-14,14.0562499999543,
10.5687124469213));
#294160=CARTESIAN_POINT('Ctrl Pts',(3.10606665601009,14.2062499999537,9.5594902125713));
#294161=CARTESIAN_POINT('Ctrl Pts',(6.2121333120202,14.3562499999531,8.55026797822134));
#294162=CARTESIAN_POINT('Ctrl Pts',(8.13178807675717,14.5062499999525,5.90808986649102));
#294163=CARTESIAN_POINT('Ctrl Pts',(10.0514428414941,14.6562499999519,3.2659117547607));
#294164=CARTESIAN_POINT('Ctrl Pts',(10.0514428414941,14.8062499999513,-1.23094673026484E-15));
#294165=CARTESIAN_POINT('Ctrl Pts',(10.0514428414941,14.9562499999507,-3.26591175476071));
#294166=CARTESIAN_POINT('Ctrl Pts',(8.13178807675717,15.1062499999501,-5.90808986649102));
#294167=CARTESIAN_POINT('Ctrl Pts',(6.21213331202019,15.2562499999495,-8.55026797822134));
#294168=CARTESIAN_POINT('Ctrl Pts',(3.10606665601009,15.4062499999489,-9.5594902125713));
#294169=CARTESIAN_POINT('Ctrl Pts',(-2.2083662864797E-14,15.5562499999482,
-10.5687124469213));
#294170=CARTESIAN_POINT('Ctrl Pts',(-3.10606665601013,15.7062499999477,
-9.5594902125713));
#294171=CARTESIAN_POINT('Ctrl Pts',(-6.21213331202024,15.856249999947,-8.55026797822134));
#294172=CARTESIAN_POINT('Ctrl Pts',(-8.13178807675721,16.0062499999464,
-5.90808986649102));
#294173=CARTESIAN_POINT('Ctrl Pts',(-10.0514428414942,16.1562499999458,
-3.2659117547607));
#294174=CARTESIAN_POINT('Ctrl Pts',(-10.0514428414942,16.3062499999452,
2.46189346052968E-15));
#294175=CARTESIAN_POINT('Ctrl Pts',(-10.0514428414942,16.4562499999446,
3.26591175476071));
#294176=CARTESIAN_POINT('Ctrl Pts',(-8.13178807675721,16.606249999944,5.90808986649102));
#294177=CARTESIAN_POINT('Ctrl Pts',(-6.21213331202024,16.7562499999434,
8.55026797822134));
#294178=CARTESIAN_POINT('Ctrl Pts',(-3.10606665601013,16.9062499999428,
9.5594902125713));
#294179=CARTESIAN_POINT('Ctrl Pts',(-2.03589295267817E-14,17.0562499999422,
10.5687124469213));
#294180=CARTESIAN_POINT('Ctrl Pts',(3.10606665601009,17.2062499999417,9.5594902125713));
#294181=CARTESIAN_POINT('Ctrl Pts',(6.21213331202019,17.3562499999411,8.55026797822134));
#294182=CARTESIAN_POINT('Ctrl Pts',(8.13178807675717,17.5062499999405,5.90808986649102));
#294183=CARTESIAN_POINT('Ctrl Pts',(10.0514428414941,17.6562499999399,3.2659117547607));
#294184=CARTESIAN_POINT('Ctrl Pts',(10.0514428414941,17.8062499999393,-1.23094673026484E-15));
#294185=CARTESIAN_POINT('Ctrl Pts',(10.0514428414941,17.9562499999387,-3.26591175476071));
#294186=CARTESIAN_POINT('Ctrl Pts',(8.13178807675717,18.1062499999381,-5.90808986649102));
#294187=CARTESIAN_POINT('Ctrl Pts',(6.21213331202019,18.2562499999375,-8.55026797822134));
#294188=CARTESIAN_POINT('Ctrl Pts',(3.10606665601008,18.4062499999369,-9.5594902125713));
#294189=CARTESIAN_POINT('Ctrl Pts',(-2.38113721364588E-14,18.5562499999362,
-10.5687124469213));
#294190=CARTESIAN_POINT('Ctrl Pts',(-3.10606665601013,18.7062499999357,
-9.5594902125713));
#294191=CARTESIAN_POINT('Ctrl Pts',(-6.21213331202024,18.856249999935,-8.55026797822134));
#294192=CARTESIAN_POINT('Ctrl Pts',(-8.13178807675721,19.0062499999344,
-5.90808986649102));
#294193=CARTESIAN_POINT('Ctrl Pts',(-10.0514428414942,19.1562499999338,
-3.2659117547607));
#294194=CARTESIAN_POINT('Ctrl Pts',(-10.0514428414942,19.3062499999332,
2.46189346052968E-15));
#294195=CARTESIAN_POINT('Ctrl Pts',(-10.0514428414942,19.4562499999326,
3.26591175476071));
#294196=CARTESIAN_POINT('Ctrl Pts',(-8.13178807675721,19.606249999932,5.90808986649102));
#294197=CARTESIAN_POINT('Ctrl Pts',(-6.21213331202024,19.7562499999314,
8.55026797822134));
#294198=CARTESIAN_POINT('Ctrl Pts',(-3.10606665601013,19.9062499999308,
9.5594902125713));
#294199=CARTESIAN_POINT('Ctrl Pts',(-2.20866387984435E-14,20.0562499999302,
10.5687124469213));
#294200=CARTESIAN_POINT('Ctrl Pts',(3.10606665601009,20.2062499999297,9.5594902125713));
#294201=CARTESIAN_POINT('Ctrl Pts',(6.21213331202019,20.356249999929,8.55026797822134));
#294202=CARTESIAN_POINT('Ctrl Pts',(8.13178807675717,20.5062499999285,5.90808986649102));
#294203=CARTESIAN_POINT('Ctrl Pts',(10.0514428414941,20.6562499999279,3.2659117547607));
#294204=CARTESIAN_POINT('Ctrl Pts',(10.0514428414941,20.8062499999273,-1.23094673026484E-15));
#294205=CARTESIAN_POINT('Ctrl Pts',(10.0514428414941,20.9562499999267,-3.26591175476071));
#294206=CARTESIAN_POINT('Ctrl Pts',(8.13178807675716,21.1062499999261,-5.90808986649102));
#294207=CARTESIAN_POINT('Ctrl Pts',(6.21213331202019,21.2562499999255,-8.55026797822134));
#294208=CARTESIAN_POINT('Ctrl Pts',(3.10606665601008,21.4062499999249,-9.5594902125713));
#294209=CARTESIAN_POINT('Ctrl Pts',(-2.55390814081207E-14,21.5562499999242,
-10.5687124469213));
#294210=CARTESIAN_POINT('Ctrl Pts',(-3.10606665601013,21.7062499999237,
-9.5594902125713));
#294211=CARTESIAN_POINT('Ctrl Pts',(-6.21213331202024,21.856249999923,-8.55026797822134));
#294212=CARTESIAN_POINT('Ctrl Pts',(-8.13178807675722,22.0062499999224,
-5.90808986649102));
#294213=CARTESIAN_POINT('Ctrl Pts',(-10.0514428414942,22.1562499999218,
-3.2659117547607));
#294214=CARTESIAN_POINT('Ctrl Pts',(-10.0514428414942,22.3062499999212,
2.46189346052968E-15));
#294215=CARTESIAN_POINT('Ctrl Pts',(-10.0514428414942,22.4562499999206,
3.26591175476071));
#294216=CARTESIAN_POINT('Ctrl Pts',(-8.13178807675722,22.60624999992,5.90808986649102));
#294217=CARTESIAN_POINT('Ctrl Pts',(-6.21213331202024,22.7562499999194,
8.55026797822134));
#294218=CARTESIAN_POINT('Ctrl Pts',(-3.10606665601013,22.9062499999188,
9.5594902125713));
#294219=CARTESIAN_POINT('Ctrl Pts',(-2.38143480701054E-14,23.0562499999182,
10.5687124469213));
#294220=CARTESIAN_POINT('Ctrl Pts',(3.10606665601008,23.2062499999177,9.5594902125713));
#294221=CARTESIAN_POINT('Ctrl Pts',(6.21213331202019,23.3562499999171,8.55026797822134));
#294222=CARTESIAN_POINT('Ctrl Pts',(8.13178807675716,23.5062499999165,5.90808986649102));
#294223=CARTESIAN_POINT('Ctrl Pts',(10.0514428414941,23.6562499999159,3.2659117547607));
#294224=CARTESIAN_POINT('Ctrl Pts',(10.0514428414941,23.8062499999153,-1.23094673026484E-15));
#294225=CARTESIAN_POINT('Ctrl Pts',(10.0514428414941,23.9562499999147,-3.26591175476071));
#294226=CARTESIAN_POINT('Ctrl Pts',(8.13178807675716,24.1062499999141,-5.90808986649102));
#294227=CARTESIAN_POINT('Ctrl Pts',(6.21213331202019,24.2562499999135,-8.55026797822134));
#294228=CARTESIAN_POINT('Ctrl Pts',(3.10606665601008,24.4062499999129,-9.5594902125713));
#294229=CARTESIAN_POINT('Ctrl Pts',(-2.72667906797825E-14,24.5562499999122,
-10.5687124469213));
#294230=CARTESIAN_POINT('Ctrl Pts',(-3.10606665601014,24.7062499999116,
-9.5594902125713));
#294231=CARTESIAN_POINT('Ctrl Pts',(-6.21213331202024,24.856249999911,-8.55026797822134));
#294232=CARTESIAN_POINT('Ctrl Pts',(-8.13178807675722,25.0062499999104,
-5.90808986649102));
#294233=CARTESIAN_POINT('Ctrl Pts',(-10.0514428414942,25.1562499999098,
-3.2659117547607));
#294234=CARTESIAN_POINT('Ctrl Pts',(-10.0514428414942,25.3062499999092,
2.46189346052968E-15));
#294235=CARTESIAN_POINT('Ctrl Pts',(-10.0514428414942,25.4562499999086,
3.26591175476071));
#294236=CARTESIAN_POINT('Ctrl Pts',(-8.13178807675722,25.6062499999081,
5.90808986649102));
#294237=CARTESIAN_POINT('Ctrl Pts',(-6.21213331202024,25.7562499999074,
8.55026797822134));
#294238=CARTESIAN_POINT('Ctrl Pts',(-3.10606665601013,25.9062499999069,
9.5594902125713));
#294239=CARTESIAN_POINT('Ctrl Pts',(-2.55420573417672E-14,26.0562499999062,
10.5687124469213));
#294240=CARTESIAN_POINT('Ctrl Pts',(3.10606665601008,26.2062499999057,9.5594902125713));
#294241=CARTESIAN_POINT('Ctrl Pts',(6.21213331202019,26.356249999905,8.55026797822134));
#294242=CARTESIAN_POINT('Ctrl Pts',(8.13178807675716,26.5062499999045,5.90808986649102));
#294243=CARTESIAN_POINT('Ctrl Pts',(10.0514428414941,26.6562499999039,3.2659117547607));
#294244=CARTESIAN_POINT('Ctrl Pts',(10.0514428414941,26.8062499999033,-1.23094673026484E-15));
#294245=CARTESIAN_POINT('Ctrl Pts',(10.0514428414941,26.9562499999027,-3.26591175476071));
#294246=CARTESIAN_POINT('Ctrl Pts',(8.13178807675716,27.1062499999021,-5.90808986649102));
#294247=CARTESIAN_POINT('Ctrl Pts',(6.21213331202019,27.2562499999015,-8.55026797822134));
#294248=CARTESIAN_POINT('Ctrl Pts',(3.10606665601008,27.4062499999009,-9.5594902125713));
#294249=CARTESIAN_POINT('Ctrl Pts',(-2.89944999514443E-14,27.5562499999002,
-10.5687124469213));
#294250=CARTESIAN_POINT('Ctrl Pts',(-3.10606665601014,27.7062499998996,
-9.5594902125713));
#294251=CARTESIAN_POINT('Ctrl Pts',(-6.21213331202024,27.856249999899,-8.55026797822134));
#294252=CARTESIAN_POINT('Ctrl Pts',(-8.13178807675722,28.0062499998984,
-5.90808986649102));
#294253=CARTESIAN_POINT('Ctrl Pts',(-10.0514428414942,28.1562499998978,
-3.2659117547607));
#294254=CARTESIAN_POINT('Ctrl Pts',(-10.0514428414942,28.3062499998973,
2.46189346052968E-15));
#294255=CARTESIAN_POINT('Ctrl Pts',(-10.0514428414942,28.4562499998966,
3.26591175476071));
#294256=CARTESIAN_POINT('Ctrl Pts',(-8.13178807675722,28.606249999896,5.90808986649102));
#294257=CARTESIAN_POINT('Ctrl Pts',(-6.21213331202024,28.7562499998954,
8.55026797822134));
#294258=CARTESIAN_POINT('Ctrl Pts',(-3.10606665601014,28.9062499998949,
9.5594902125713));
#294259=CARTESIAN_POINT('Ctrl Pts',(-2.72697666134291E-14,29.0562499998942,
10.5687124469213));
#294260=CARTESIAN_POINT('Ctrl Pts',(3.10606665601008,29.2062499998937,9.5594902125713));
#294261=CARTESIAN_POINT('Ctrl Pts',(6.21213331202019,29.356249999893,8.55026797822134));
#294262=CARTESIAN_POINT('Ctrl Pts',(8.13178807675716,29.5062499998925,5.90808986649102));
#294263=CARTESIAN_POINT('Ctrl Pts',(10.0514428414941,29.6562499998919,3.2659117547607));
#294264=CARTESIAN_POINT('Ctrl Pts',(10.0514428414941,29.8062499998913,-1.23094673026484E-15));
#294265=CARTESIAN_POINT('Ctrl Pts',(10.0514428414941,29.9562499998907,-3.26591175476071));
#294266=CARTESIAN_POINT('Ctrl Pts',(8.13178807675716,30.1062499998901,-5.90808986649102));
#294267=CARTESIAN_POINT('Ctrl Pts',(6.21213331202019,30.2562499998895,-8.55026797822134));
#294268=CARTESIAN_POINT('Ctrl Pts',(3.10606665601008,30.4062499998889,-9.5594902125713));
#294269=CARTESIAN_POINT('Ctrl Pts',(-3.07222092231062E-14,30.5562499998883,
-10.5687124469213));
#294270=CARTESIAN_POINT('Ctrl Pts',(-3.10606665601014,30.7062499998877,
-9.5594902125713));
#294271=CARTESIAN_POINT('Ctrl Pts',(-6.21213331202025,30.8562499998871,
-8.55026797822134));
#294272=CARTESIAN_POINT('Ctrl Pts',(-8.13178807675722,31.0062499998864,
-5.90808986649102));
#294273=CARTESIAN_POINT('Ctrl Pts',(-10.0514428414942,31.1562499998858,
-3.2659117547607));
#294274=CARTESIAN_POINT('Ctrl Pts',(-10.0514428414942,31.3062499998852,
2.46189346052968E-15));
#294275=CARTESIAN_POINT('Ctrl Pts',(-10.0514428414942,31.4562499998847,
3.26591175476071));
#294276=CARTESIAN_POINT('Ctrl Pts',(-8.13178807675722,31.606249999884,5.90808986649102));
#294277=CARTESIAN_POINT('Ctrl Pts',(-6.21213331202024,31.7562499998835,
8.55026797822134));
#294278=CARTESIAN_POINT('Ctrl Pts',(-3.10606665601014,31.9062499998829,
9.5594902125713));
#294279=CARTESIAN_POINT('Ctrl Pts',(-2.89974758850909E-14,32.0562499998822,
10.5687124469213));
#294280=CARTESIAN_POINT('Ctrl Pts',(3.10606665601008,32.2062499998816,9.5594902125713));
#294281=CARTESIAN_POINT('Ctrl Pts',(6.21213331202019,32.3562499998811,8.55026797822134));
#294282=CARTESIAN_POINT('Ctrl Pts',(8.13178807675716,32.5062499998805,5.90808986649102));
#294283=CARTESIAN_POINT('Ctrl Pts',(10.0514428414941,32.6562499998798,3.2659117547607));
#294284=CARTESIAN_POINT('Ctrl Pts',(10.0514428414941,32.8062499998793,-1.23094673026484E-15));
#294285=CARTESIAN_POINT('Ctrl Pts',(10.0514428414941,32.9562499998787,-3.26591175476071));
#294286=CARTESIAN_POINT('Ctrl Pts',(8.13178807675716,33.1062499998781,-5.90808986649102));
#294287=CARTESIAN_POINT('Ctrl Pts',(6.21213331202019,33.2562499998775,-8.55026797822134));
#294288=CARTESIAN_POINT('Ctrl Pts',(3.10606665601008,33.4062499998769,-9.5594902125713));
#294289=CARTESIAN_POINT('Ctrl Pts',(-3.2449918494768E-14,33.5562499998763,
-10.5687124469213));
#294290=CARTESIAN_POINT('Ctrl Pts',(-3.10606665601014,33.7062499998756,
-9.5594902125713));
#294291=CARTESIAN_POINT('Ctrl Pts',(-6.21213331202025,33.8562499998751,
-8.55026797822134));
#294292=CARTESIAN_POINT('Ctrl Pts',(-8.13178807675722,34.0062499998744,
-5.90808986649102));
#294293=CARTESIAN_POINT('Ctrl Pts',(-10.0514428414942,34.1562499998739,
-3.2659117547607));
#294294=CARTESIAN_POINT('Ctrl Pts',(-10.0514428414942,34.3062499998732,
2.46189346052968E-15));
#294295=CARTESIAN_POINT('Ctrl Pts',(-10.0514428414942,34.4562499998727,
3.26591175476071));
#294296=CARTESIAN_POINT('Ctrl Pts',(-8.13178807675722,34.606249999872,5.90808986649102));
#294297=CARTESIAN_POINT('Ctrl Pts',(-6.21213331202024,34.7562499998715,
8.55026797822134));
#294298=CARTESIAN_POINT('Ctrl Pts',(-3.10606665601014,34.9062499998708,
9.5594902125713));
#294299=CARTESIAN_POINT('Ctrl Pts',(-3.07251851567527E-14,35.0562499998703,
10.5687124469213));
#294300=CARTESIAN_POINT('Ctrl Pts',(3.10606665601008,35.2062499998697,9.5594902125713));
#294301=CARTESIAN_POINT('Ctrl Pts',(6.21213331202019,35.3562499998691,8.55026797822134));
#294302=CARTESIAN_POINT('Ctrl Pts',(8.13178807675716,35.5062499998685,5.90808986649102));
#294303=CARTESIAN_POINT('Ctrl Pts',(10.0514428414941,35.6562499998679,3.2659117547607));
#294304=CARTESIAN_POINT('Ctrl Pts',(10.0514428414941,35.8062499998673,-1.23094673026484E-15));
#294305=CARTESIAN_POINT('Ctrl Pts',(10.0514428414941,35.9562499998667,-3.26591175476071));
#294306=CARTESIAN_POINT('Ctrl Pts',(8.13178807675716,36.1062499998661,-5.90808986649102));
#294307=CARTESIAN_POINT('Ctrl Pts',(6.21213331202018,36.2562499998655,-8.55026797822134));
#294308=CARTESIAN_POINT('Ctrl Pts',(3.10606665601007,36.4062499998649,-9.5594902125713));
#294309=CARTESIAN_POINT('Ctrl Pts',(-3.41776277664299E-14,36.5562499998642,
-10.5687124469213));
#294310=CARTESIAN_POINT('Ctrl Pts',(-3.10606665601014,36.7062499998636,
-9.5594902125713));
#294311=CARTESIAN_POINT('Ctrl Pts',(-6.21213331202025,36.856249999863,-8.55026797822134));
#294312=CARTESIAN_POINT('Ctrl Pts',(-8.13178807675722,37.0062499998624,
-5.90808986649102));
#294313=CARTESIAN_POINT('Ctrl Pts',(-10.0514428414942,37.1562499998618,
-3.2659117547607));
#294314=CARTESIAN_POINT('Ctrl Pts',(-10.0514428414942,37.3062499998613,
2.46189346052968E-15));
#294315=CARTESIAN_POINT('Ctrl Pts',(-10.0514428414942,37.4562499998606,
3.26591175476071));
#294316=CARTESIAN_POINT('Ctrl Pts',(-8.13178807675722,37.60624999986,5.90808986649102));
#294317=CARTESIAN_POINT('Ctrl Pts',(-6.21213331202025,37.7562499998594,
8.55026797822134));
#294318=CARTESIAN_POINT('Ctrl Pts',(-3.10606665601014,37.9062499998588,
9.5594902125713));
#294319=CARTESIAN_POINT('Ctrl Pts',(-3.24528944284146E-14,38.0562499998583,
10.5687124469213));
#294320=CARTESIAN_POINT('Ctrl Pts',(3.10606665601007,38.2062499998577,9.5594902125713));
#294321=CARTESIAN_POINT('Ctrl Pts',(6.21213331202018,38.3562499998571,8.55026797822134));
#294322=CARTESIAN_POINT('Ctrl Pts',(8.13178807675716,38.5062499998565,5.90808986649102));
#294323=CARTESIAN_POINT('Ctrl Pts',(10.0514428414941,38.6562499998559,3.2659117547607));
#294324=CARTESIAN_POINT('Ctrl Pts',(10.0514428414941,38.8062499998553,-1.23094673026484E-15));
#294325=CARTESIAN_POINT('Ctrl Pts',(10.0514428414941,38.9562499998547,-3.26591175476071));
#294326=CARTESIAN_POINT('Ctrl Pts',(8.13178807675715,39.1062499998541,-5.90808986649102));
#294327=CARTESIAN_POINT('Ctrl Pts',(6.21213331202018,39.2562499998535,-8.55026797822134));
#294328=CARTESIAN_POINT('Ctrl Pts',(3.10606665601007,39.4062499998529,-9.5594902125713));
#294329=CARTESIAN_POINT('Ctrl Pts',(-3.59053370380917E-14,39.5562499998523,
-10.5687124469213));
#294330=CARTESIAN_POINT('Ctrl Pts',(-3.10606665601014,39.7062499998516,
-9.5594902125713));
#294331=CARTESIAN_POINT('Ctrl Pts',(-6.21213331202025,39.856249999851,-8.55026797822134));
#294332=CARTESIAN_POINT('Ctrl Pts',(-8.13178807675723,40.0062499998505,
-5.90808986649102));
#294333=CARTESIAN_POINT('Ctrl Pts',(-10.0514428414942,40.1562499998499,
-3.2659117547607));
#294334=CARTESIAN_POINT('Ctrl Pts',(-10.0514428414942,40.3062499998493,
2.46189346052968E-15));
#294335=CARTESIAN_POINT('Ctrl Pts',(-10.0514428414942,40.4562499998487,
3.26591175476071));
#294336=CARTESIAN_POINT('Ctrl Pts',(-8.13178807675723,40.606249999848,5.90808986649102));
#294337=CARTESIAN_POINT('Ctrl Pts',(-6.21213331202025,40.7562499998475,
8.55026797822134));
#294338=CARTESIAN_POINT('Ctrl Pts',(-3.10606665601014,40.9062499998468,
9.5594902125713));
#294339=CARTESIAN_POINT('Ctrl Pts',(-3.41806037000764E-14,41.0562499998463,
10.5687124469213));
#294340=CARTESIAN_POINT('Ctrl Pts',(3.10606665601007,41.2062499998457,9.5594902125713));
#294341=CARTESIAN_POINT('Ctrl Pts',(6.21213331202018,41.3562499998451,8.55026797822134));
#294342=CARTESIAN_POINT('Ctrl Pts',(8.13178807675715,41.5062499998444,5.90808986649102));
#294343=CARTESIAN_POINT('Ctrl Pts',(10.0514428414941,41.6562499998439,3.2659117547607));
#294344=CARTESIAN_POINT('Ctrl Pts',(10.0514428414941,41.8062499998433,-1.23094673026484E-15));
#294345=CARTESIAN_POINT('Ctrl Pts',(10.0514428414941,41.9562499998427,-3.26591175476071));
#294346=CARTESIAN_POINT('Ctrl Pts',(8.13178807675715,42.1062499998421,-5.90808986649102));
#294347=CARTESIAN_POINT('Ctrl Pts',(6.21213331202018,42.2562499998414,-8.55026797822134));
#294348=CARTESIAN_POINT('Ctrl Pts',(3.10606665601007,42.4062499998408,-9.5594902125713));
#294349=CARTESIAN_POINT('Ctrl Pts',(-3.76330463097535E-14,42.5562499998402,
-10.5687124469213));
#294350=CARTESIAN_POINT('Ctrl Pts',(-3.10606665601015,42.7062499998396,
-9.5594902125713));
#294351=CARTESIAN_POINT('Ctrl Pts',(-6.21213331202025,42.8562499998391,
-8.55026797822134));
#294352=CARTESIAN_POINT('Ctrl Pts',(-8.13178807675723,43.0062499998385,
-5.90808986649102));
#294353=CARTESIAN_POINT('Ctrl Pts',(-10.0514428414942,43.1562499998379,
-3.2659117547607));
#294354=CARTESIAN_POINT('Ctrl Pts',(-10.0514428414942,43.3062499998373,
2.46189346052968E-15));
#294355=CARTESIAN_POINT('Ctrl Pts',(-10.0514428414942,43.4562499998366,
3.26591175476071));
#294356=CARTESIAN_POINT('Ctrl Pts',(-8.13178807675723,43.6062499998361,
5.90808986649102));
#294357=CARTESIAN_POINT('Ctrl Pts',(-6.21213331202025,43.7562499998354,
8.55026797822134));
#294358=CARTESIAN_POINT('Ctrl Pts',(-3.10606665601014,43.9062499998348,
9.5594902125713));
#294359=CARTESIAN_POINT('Ctrl Pts',(-3.59083129717383E-14,44.0562499998343,
10.5687124469213));
#294360=CARTESIAN_POINT('Ctrl Pts',(3.10606665601007,44.2062499998337,9.5594902125713));
#294361=CARTESIAN_POINT('Ctrl Pts',(6.21213331202018,44.3562499998331,8.55026797822134));
#294362=CARTESIAN_POINT('Ctrl Pts',(8.13178807675715,44.5062499998324,5.90808986649102));
#294363=CARTESIAN_POINT('Ctrl Pts',(10.0514428414941,44.6562499998319,3.2659117547607));
#294364=CARTESIAN_POINT('Ctrl Pts',(10.0514428414941,44.8062499998313,-1.23094673026484E-15));
#294365=CARTESIAN_POINT('Ctrl Pts',(10.0514428414941,44.9562499998307,-3.26591175476071));
#294366=CARTESIAN_POINT('Ctrl Pts',(8.13178807675715,45.1062499998301,-5.90808986649102));
#294367=CARTESIAN_POINT('Ctrl Pts',(6.21213331202018,45.2562499998295,-8.55026797822134));
#294368=CARTESIAN_POINT('Ctrl Pts',(3.10606665601007,45.4062499998289,-9.5594902125713));
#294369=CARTESIAN_POINT('Ctrl Pts',(-3.93607555814154E-14,45.5562499998283,
-10.5687124469213));
#294370=CARTESIAN_POINT('Ctrl Pts',(-3.10606665601015,45.7062499998276,
-9.5594902125713));
#294371=CARTESIAN_POINT('Ctrl Pts',(-6.21213331202026,45.856249999827,-8.55026797822134));
#294372=CARTESIAN_POINT('Ctrl Pts',(-8.13178807675723,46.0062499998265,
-5.90808986649102));
#294373=CARTESIAN_POINT('Ctrl Pts',(-10.0514428414942,46.1562499998259,
-3.2659117547607));
#294374=CARTESIAN_POINT('Ctrl Pts',(-10.0514428414942,46.3062499998252,
2.46189346052968E-15));
#294375=CARTESIAN_POINT('Ctrl Pts',(-10.0514428414942,46.4562499998247,
3.26591175476071));
#294376=CARTESIAN_POINT('Ctrl Pts',(-8.13178807675723,46.606249999824,5.90808986649102));
#294377=CARTESIAN_POINT('Ctrl Pts',(-6.21213331202025,46.7562499998235,
8.55026797822134));
#294378=CARTESIAN_POINT('Ctrl Pts',(-3.10606665601015,46.9062499998228,
9.5594902125713));
#294379=CARTESIAN_POINT('Ctrl Pts',(-3.76360222434001E-14,47.0562499998223,
10.5687124469213));
#294380=CARTESIAN_POINT('Ctrl Pts',(3.10606665601007,47.2062499998217,9.5594902125713));
#294381=CARTESIAN_POINT('Ctrl Pts',(6.21213331202018,47.3562499998211,8.55026797822134));
#294382=CARTESIAN_POINT('Ctrl Pts',(8.13178807675715,47.5062499998204,5.90808986649102));
#294383=CARTESIAN_POINT('Ctrl Pts',(10.0514428414941,47.6562499998198,3.2659117547607));
#294384=CARTESIAN_POINT('Ctrl Pts',(10.0514428414941,47.8062499998193,-1.23094673026484E-15));
#294385=CARTESIAN_POINT('Ctrl Pts',(10.0514428414941,47.9562499998186,-3.26591175476071));
#294386=CARTESIAN_POINT('Ctrl Pts',(8.13178807675715,48.1062499998181,-5.90808986649102));
#294387=CARTESIAN_POINT('Ctrl Pts',(6.21213331202017,48.2562499998174,-8.55026797822134));
#294388=CARTESIAN_POINT('Ctrl Pts',(3.10606665601007,48.4062499998169,-9.5594902125713));
#294389=CARTESIAN_POINT('Ctrl Pts',(-4.10884648530772E-14,48.5562499998163,
-10.5687124469213));
#294390=CARTESIAN_POINT('Ctrl Pts',(-3.10606665601015,48.7062499998157,
-9.5594902125713));
#294391=CARTESIAN_POINT('Ctrl Pts',(-6.21213331202026,48.8562499998151,
-8.55026797822134));
#294392=CARTESIAN_POINT('Ctrl Pts',(-8.13178807675723,49.0062499998145,
-5.90808986649102));
#294393=CARTESIAN_POINT('Ctrl Pts',(-10.0514428414942,49.1562499998138,
-3.2659117547607));
#294394=CARTESIAN_POINT('Ctrl Pts',(-10.0514428414942,49.3062499998132,
2.46189346052968E-15));
#294395=CARTESIAN_POINT('Ctrl Pts',(-10.0514428414942,49.4562499998126,
3.26591175476071));
#294396=CARTESIAN_POINT('Ctrl Pts',(-8.13178807675723,49.6062499998121,
5.90808986649102));
#294397=CARTESIAN_POINT('Ctrl Pts',(-6.21213331202026,49.7562499998114,
8.55026797822134));
#294398=CARTESIAN_POINT('Ctrl Pts',(-3.10606665601015,49.9062499998109,
9.5594902125713));
#294399=CARTESIAN_POINT('Ctrl Pts',(-3.9363731515062E-14,50.0562499998103,
10.5687124469213));
#294400=CARTESIAN_POINT('Ctrl Pts',(3.10606665601007,50.2062499998097,9.5594902125713));
#294401=CARTESIAN_POINT('Ctrl Pts',(6.21213331202017,50.3562499998091,8.55026797822134));
#294402=CARTESIAN_POINT('Ctrl Pts',(8.13178807675715,50.5062499998085,5.90808986649102));
#294403=CARTESIAN_POINT('Ctrl Pts',(10.0514428414941,50.6562499998078,3.2659117547607));
#294404=CARTESIAN_POINT('Ctrl Pts',(10.0514428414941,50.8062499998072,-1.23094673026484E-15));
#294405=CARTESIAN_POINT('Ctrl Pts',(10.0514428414941,50.9562499998067,-3.26591175476071));
#294406=CARTESIAN_POINT('Ctrl Pts',(8.13178807675715,51.1062499998061,-5.90808986649102));
#294407=CARTESIAN_POINT('Ctrl Pts',(6.21213331202017,51.2562499998055,-8.55026797822134));
#294408=CARTESIAN_POINT('Ctrl Pts',(3.10606665601006,51.4062499998048,-9.5594902125713));
#294409=CARTESIAN_POINT('Ctrl Pts',(-4.2816174124739E-14,51.5562499998043,
-10.5687124469213));
#294410=CARTESIAN_POINT('Ctrl Pts',(-3.10606665601015,51.7062499998037,
-9.5594902125713));
#294411=CARTESIAN_POINT('Ctrl Pts',(-6.21213331202026,51.856249999803,-8.55026797822134));
#294412=CARTESIAN_POINT('Ctrl Pts',(-8.13178807675723,52.0062499998025,
-5.90808986649102));
#294413=CARTESIAN_POINT('Ctrl Pts',(-10.0514428414942,52.1562499998019,
-3.2659117547607));
#294414=CARTESIAN_POINT('Ctrl Pts',(-10.0514428414942,52.3062499998012,
2.46189346052968E-15));
#294415=CARTESIAN_POINT('Ctrl Pts',(-10.0514428414942,52.4562499998006,
3.26591175476071));
#294416=CARTESIAN_POINT('Ctrl Pts',(-8.13178807675723,52.6062499998,5.90808986649102));
#294417=CARTESIAN_POINT('Ctrl Pts',(-6.21213331202026,52.7562499997994,
8.55026797822134));
#294418=CARTESIAN_POINT('Ctrl Pts',(-3.10606665601015,52.9062499997988,
9.5594902125713));
#294419=CARTESIAN_POINT('Ctrl Pts',(-4.10914407867238E-14,53.0562499997983,
10.5687124469213));
#294420=CARTESIAN_POINT('Ctrl Pts',(3.10606665601007,53.2062499997976,9.5594902125713));
#294421=CARTESIAN_POINT('Ctrl Pts',(6.21213331202017,53.3562499997971,8.55026797822134));
#294422=CARTESIAN_POINT('Ctrl Pts',(8.13178807675715,53.5062499997965,5.90808986649102));
#294423=CARTESIAN_POINT('Ctrl Pts',(10.0514428414941,53.6562499997959,3.2659117547607));
#294424=CARTESIAN_POINT('Ctrl Pts',(10.0514428414941,53.8062499997953,-1.23094673026484E-15));
#294425=CARTESIAN_POINT('Ctrl Pts',(10.0514428414941,53.9562499997946,-3.26591175476071));
#294426=CARTESIAN_POINT('Ctrl Pts',(8.13178807675714,54.106249999794,-5.90808986649102));
#294427=CARTESIAN_POINT('Ctrl Pts',(6.21213331202017,54.2562499997934,-8.55026797822134));
#294428=CARTESIAN_POINT('Ctrl Pts',(3.10606665601006,54.4062499997928,-9.5594902125713));
#294429=CARTESIAN_POINT('Ctrl Pts',(-4.45438833964009E-14,54.5562499997923,
-10.5687124469213));
#294430=CARTESIAN_POINT('Ctrl Pts',(-3.10606665601015,54.7062499997917,
-9.5594902125713));
#294431=CARTESIAN_POINT('Ctrl Pts',(-6.21213331202026,54.856249999791,-8.55026797822134));
#294432=CARTESIAN_POINT('Ctrl Pts',(-8.13178807675724,55.0062499997905,
-5.90808986649102));
#294433=CARTESIAN_POINT('Ctrl Pts',(-10.0514428414942,55.1562499997898,
-3.2659117547607));
#294434=CARTESIAN_POINT('Ctrl Pts',(-10.0514428414942,55.3062499997893,
2.46189346052968E-15));
#294435=CARTESIAN_POINT('Ctrl Pts',(-10.0514428414942,55.4562499997886,
3.26591175476071));
#294436=CARTESIAN_POINT('Ctrl Pts',(-8.13178807675724,55.606249999788,5.90808986649102));
#294437=CARTESIAN_POINT('Ctrl Pts',(-6.21213331202026,55.7562499997874,
8.55026797822134));
#294438=CARTESIAN_POINT('Ctrl Pts',(-3.10606665601015,55.9062499997869,
9.5594902125713));
#294439=CARTESIAN_POINT('Ctrl Pts',(-4.28191500583856E-14,56.0562499997862,
10.5687124469213));
#294440=CARTESIAN_POINT('Ctrl Pts',(3.10606665601006,56.2062499997857,9.5594902125713));
#294441=CARTESIAN_POINT('Ctrl Pts',(6.21213331202017,56.356249999785,8.55026797822134));
#294442=CARTESIAN_POINT('Ctrl Pts',(8.13178807675714,56.5062499997845,5.90808986649102));
#294443=CARTESIAN_POINT('Ctrl Pts',(10.0514428414941,56.6562499997839,3.2659117547607));
#294444=CARTESIAN_POINT('Ctrl Pts',(10.0514428414941,56.8062499997833,-1.23094673026484E-15));
#294445=CARTESIAN_POINT('Ctrl Pts',(10.0514428414941,56.9562499997827,-3.26591175476071));
#294446=CARTESIAN_POINT('Ctrl Pts',(8.13178807675714,57.1062499997821,-5.90808986649102));
#294447=CARTESIAN_POINT('Ctrl Pts',(6.21213331202017,57.2562499997814,-8.55026797822134));
#294448=CARTESIAN_POINT('Ctrl Pts',(3.10606665601006,57.4062499997808,-9.5594902125713));
#294449=CARTESIAN_POINT('Ctrl Pts',(-4.62715926680627E-14,57.5562499997802,
-10.5687124469213));
#294450=CARTESIAN_POINT('Ctrl Pts',(-3.10606665601015,57.7062499997797,
-9.5594902125713));
#294451=CARTESIAN_POINT('Ctrl Pts',(-6.21213331202026,57.856249999779,-8.55026797822134));
#294452=CARTESIAN_POINT('Ctrl Pts',(-8.13178807675724,58.0062499997784,
-5.90808986649102));
#294453=CARTESIAN_POINT('Ctrl Pts',(-10.0514428414942,58.1562499997778,
-3.2659117547607));
#294454=CARTESIAN_POINT('Ctrl Pts',(-10.0514428414942,58.3062499997773,
2.46189346052968E-15));
#294455=CARTESIAN_POINT('Ctrl Pts',(-10.0514428414942,58.4562499997766,
3.26591175476071));
#294456=CARTESIAN_POINT('Ctrl Pts',(-8.13178807675724,58.6062499997761,
5.90808986649102));
#294457=CARTESIAN_POINT('Ctrl Pts',(-6.21213331202026,58.7562499997754,
8.55026797822134));
#294458=CARTESIAN_POINT('Ctrl Pts',(-3.10606665601015,58.9062499997749,
9.5594902125713));
#294459=CARTESIAN_POINT('Ctrl Pts',(-4.45468593300475E-14,59.0562499997743,
10.5687124469213));
#294460=CARTESIAN_POINT('Ctrl Pts',(3.10606665601006,59.2062499997736,9.5594902125713));
#294461=CARTESIAN_POINT('Ctrl Pts',(6.21213331202017,59.356249999773,8.55026797822134));
#294462=CARTESIAN_POINT('Ctrl Pts',(8.13178807675714,59.5062499997725,5.90808986649102));
#294463=CARTESIAN_POINT('Ctrl Pts',(10.0514428414941,59.6562499997718,3.2659117547607));
#294464=CARTESIAN_POINT('Ctrl Pts',(10.0514428414941,59.8062499997713,-1.23094673026484E-15));
#294465=CARTESIAN_POINT('Ctrl Pts',(10.0514428414941,59.9562499997706,-3.26591175476071));
#294466=CARTESIAN_POINT('Ctrl Pts',(8.13178807675714,60.10624999977,-5.90808986649102));
#294467=CARTESIAN_POINT('Ctrl Pts',(6.21213331202017,60.2562499997694,-8.55026797822134));
#294468=CARTESIAN_POINT('Ctrl Pts',(3.10606665601006,60.4062499997689,-9.5594902125713));
#294469=CARTESIAN_POINT('Ctrl Pts',(-4.79993019397246E-14,60.5562499997682,
-10.5687124469213));
#294470=CARTESIAN_POINT('Ctrl Pts',(-3.10606665601016,60.7062499997676,
-9.5594902125713));
#294471=CARTESIAN_POINT('Ctrl Pts',(-6.21213331202026,60.856249999767,-8.55026797822134));
#294472=CARTESIAN_POINT('Ctrl Pts',(-8.13178807675724,61.0062499997664,
-5.90808986649102));
#294473=CARTESIAN_POINT('Ctrl Pts',(-10.0514428414942,61.1562499997658,
-3.2659117547607));
#294474=CARTESIAN_POINT('Ctrl Pts',(-10.0514428414942,61.3062499997652,
2.46189346052968E-15));
#294475=CARTESIAN_POINT('Ctrl Pts',(-10.0514428414942,61.4562499997646,
3.26591175476071));
#294476=CARTESIAN_POINT('Ctrl Pts',(-8.13178807675724,61.6062499997641,
5.90808986649102));
#294477=CARTESIAN_POINT('Ctrl Pts',(-6.21213331202026,61.7562499997634,
8.55026797822134));
#294478=CARTESIAN_POINT('Ctrl Pts',(-3.10606665601015,61.9062499997628,
9.5594902125713));
#294479=CARTESIAN_POINT('Ctrl Pts',(-4.62745686017093E-14,62.0562499997622,
10.5687124469213));
#294480=CARTESIAN_POINT('Ctrl Pts',(3.10606665601006,62.2062499997617,9.5594902125713));
#294481=CARTESIAN_POINT('Ctrl Pts',(6.21213331202017,62.356249999761,8.55026797822134));
#294482=CARTESIAN_POINT('Ctrl Pts',(8.13178807675714,62.5062499997605,5.90808986649102));
#294483=CARTESIAN_POINT('Ctrl Pts',(10.0514428414941,62.6562499997599,3.2659117547607));
#294484=CARTESIAN_POINT('Ctrl Pts',(10.0514428414941,62.8062499997593,-1.23094673026484E-15));
#294485=CARTESIAN_POINT('Ctrl Pts',(10.0514428414941,62.9562499997587,-3.26591175476071));
#294486=CARTESIAN_POINT('Ctrl Pts',(8.13178807675714,63.1062499997581,-5.90808986649102));
#294487=CARTESIAN_POINT('Ctrl Pts',(6.21213331202017,63.2562499997575,-8.55026797822134));
#294488=CARTESIAN_POINT('Ctrl Pts',(3.10606665601006,63.4062499997568,-9.5594902125713));
#294489=CARTESIAN_POINT('Ctrl Pts',(-4.97270112113864E-14,63.5562499997562,
-10.5687124469213));
#294490=CARTESIAN_POINT('Ctrl Pts',(-3.10606665601016,63.7062499997556,
-9.5594902125713));
#294491=CARTESIAN_POINT('Ctrl Pts',(-6.21213331202027,63.8562499997551,
-8.55026797822134));
#294492=CARTESIAN_POINT('Ctrl Pts',(-8.13178807675724,64.0062499997544,
-5.90808986649102));
#294493=CARTESIAN_POINT('Ctrl Pts',(-10.0514428414942,64.1562499997538,
-3.2659117547607));
#294494=CARTESIAN_POINT('Ctrl Pts',(-10.0514428414942,64.3062499997532,
2.46189346052968E-15));
#294495=CARTESIAN_POINT('Ctrl Pts',(-10.0514428414942,64.4562499997526,
3.26591175476071));
#294496=CARTESIAN_POINT('Ctrl Pts',(-8.13178807675724,64.606249999752,5.90808986649102));
#294497=CARTESIAN_POINT('Ctrl Pts',(-6.21213331202026,64.7562499997514,
8.55026797822134));
#294498=CARTESIAN_POINT('Ctrl Pts',(-3.10606665601016,64.9062499997509,
9.5594902125713));
#294499=CARTESIAN_POINT('Ctrl Pts',(-4.80022778733711E-14,65.0562499997502,
10.5687124469213));
#294500=CARTESIAN_POINT('Ctrl Pts',(3.10606665601006,65.2062499997497,9.5594902125713));
#294501=CARTESIAN_POINT('Ctrl Pts',(6.21213331202017,65.3562499997491,8.55026797822134));
#294502=CARTESIAN_POINT('Ctrl Pts',(8.13178807675714,65.5062499997484,5.90808986649102));
#294503=CARTESIAN_POINT('Ctrl Pts',(10.0514428414941,65.6562499997479,3.2659117547607));
#294504=CARTESIAN_POINT('Ctrl Pts',(10.0514428414941,65.8062499997473,-1.23094673026484E-15));
#294505=CARTESIAN_POINT('Ctrl Pts',(10.0514428414941,65.9562499997467,-3.26591175476071));
#294506=CARTESIAN_POINT('Ctrl Pts',(8.13178807675714,66.1062499997461,-5.90808986649102));
#294507=CARTESIAN_POINT('Ctrl Pts',(6.21213331202016,66.2562499997454,-8.55026797822134));
#294508=CARTESIAN_POINT('Ctrl Pts',(3.10606665601006,66.4062499997449,-9.5594902125713));
#294509=CARTESIAN_POINT('Ctrl Pts',(-5.14547204830482E-14,66.5562499997443,
-10.5687124469213));
#294510=CARTESIAN_POINT('Ctrl Pts',(-3.10606665601016,66.7062499997436,
-9.5594902125713));
#294511=CARTESIAN_POINT('Ctrl Pts',(-6.21213331202027,66.8562499997431,
-8.55026797822134));
#294512=CARTESIAN_POINT('Ctrl Pts',(-8.13178807675724,67.0062499997424,
-5.90808986649102));
#294513=CARTESIAN_POINT('Ctrl Pts',(-10.0514428414942,67.1562499997418,
-3.2659117547607));
#294514=CARTESIAN_POINT('Ctrl Pts',(-10.0514428414942,67.3062499997412,
2.46189346052968E-15));
#294515=CARTESIAN_POINT('Ctrl Pts',(-10.0514428414942,67.4562499997406,
3.26591175476071));
#294516=CARTESIAN_POINT('Ctrl Pts',(-8.13178807675724,67.60624999974,5.90808986649102));
#294517=CARTESIAN_POINT('Ctrl Pts',(-6.21213331202027,67.7562499997395,
8.55026797822134));
#294518=CARTESIAN_POINT('Ctrl Pts',(-3.10606665601016,67.9062499997388,
9.5594902125713));
#294519=CARTESIAN_POINT('Ctrl Pts',(-4.9729987145033E-14,68.0562499997382,
10.5687124469213));
#294520=CARTESIAN_POINT('Ctrl Pts',(3.10606665601006,68.2062499997377,9.5594902125713));
#294521=CARTESIAN_POINT('Ctrl Pts',(6.21213331202017,68.356249999737,8.55026797822134));
#294522=CARTESIAN_POINT('Ctrl Pts',(8.13178807675714,68.5062499997365,5.90808986649102));
#294523=CARTESIAN_POINT('Ctrl Pts',(10.0514428414941,68.6562499997358,3.2659117547607));
#294524=CARTESIAN_POINT('Ctrl Pts',(10.0514428414941,68.8062499997353,-1.23094673026484E-15));
#294525=CARTESIAN_POINT('Ctrl Pts',(10.0514428414941,68.9562499997347,-3.26591175476071));
#294526=CARTESIAN_POINT('Ctrl Pts',(8.13178807675714,69.1062499997341,-5.90808986649102));
#294527=CARTESIAN_POINT('Ctrl Pts',(6.21213331202016,69.2562499997335,-8.55026797822134));
#294528=CARTESIAN_POINT('Ctrl Pts',(3.10606665601005,69.4062499997329,-9.5594902125713));
#294529=CARTESIAN_POINT('Ctrl Pts',(-5.31824297547101E-14,69.5562499997323,
-10.5687124469213));
#294530=CARTESIAN_POINT('Ctrl Pts',(-3.10606665601016,69.7062499997317,
-9.5594902125713));
#294531=CARTESIAN_POINT('Ctrl Pts',(-6.21213331202027,69.856249999731,-8.55026797822134));
#294532=CARTESIAN_POINT('Ctrl Pts',(-8.13178807675724,70.0062499997304,
-5.90808986649102));
#294533=CARTESIAN_POINT('Ctrl Pts',(-10.0514428414942,70.1562499997298,
-3.2659117547607));
#294534=CARTESIAN_POINT('Ctrl Pts',(-10.0514428414942,70.3062499997292,
2.46189346052968E-15));
#294535=CARTESIAN_POINT('Ctrl Pts',(-10.0514428414942,70.4562499997286,
3.26591175476071));
#294536=CARTESIAN_POINT('Ctrl Pts',(-8.13178807675724,70.606249999728,5.90808986649102));
#294537=CARTESIAN_POINT('Ctrl Pts',(-6.21213331202027,70.7562499997274,
8.55026797822134));
#294538=CARTESIAN_POINT('Ctrl Pts',(-3.10606665601016,70.9062499997269,
9.5594902125713));
#294539=CARTESIAN_POINT('Ctrl Pts',(-5.14576964166948E-14,71.0562499997262,
10.5687124469213));
#294540=CARTESIAN_POINT('Ctrl Pts',(3.10606665601006,71.2062499997256,9.5594902125713));
#294541=CARTESIAN_POINT('Ctrl Pts',(6.21213331202016,71.3562499997251,8.55026797822134));
#294542=CARTESIAN_POINT('Ctrl Pts',(8.13178807675714,71.5062499997244,5.90808986649102));
#294543=CARTESIAN_POINT('Ctrl Pts',(10.0514428414941,71.6562499997239,3.2659117547607));
#294544=CARTESIAN_POINT('Ctrl Pts',(10.0514428414941,71.8062499997232,-1.23094673026484E-15));
#294545=CARTESIAN_POINT('Ctrl Pts',(10.0514428414941,71.9562499997227,-3.26591175476071));
#294546=CARTESIAN_POINT('Ctrl Pts',(8.13178807675713,72.1062499997221,-5.90808986649102));
#294547=CARTESIAN_POINT('Ctrl Pts',(6.21213331202016,72.2562499997215,-8.55026797822134));
#294548=CARTESIAN_POINT('Ctrl Pts',(3.10606665601005,72.4062499997209,-9.5594902125713));
#294549=CARTESIAN_POINT('Ctrl Pts',(-5.49101390263719E-14,72.5562499997203,
-10.5687124469213));
#294550=CARTESIAN_POINT('Ctrl Pts',(-3.10606665601016,72.7062499997197,
-9.5594902125713));
#294551=CARTESIAN_POINT('Ctrl Pts',(-6.21213331202027,72.8562499997191,
-8.55026797822134));
#294552=CARTESIAN_POINT('Ctrl Pts',(-8.13178807675725,73.0062499997184,
-5.90808986649102));
#294553=CARTESIAN_POINT('Ctrl Pts',(-10.0514428414942,73.1562499997178,
-3.2659117547607));
#294554=CARTESIAN_POINT('Ctrl Pts',(-10.0514428414942,73.3062499997172,
2.46189346052968E-15));
#294555=CARTESIAN_POINT('Ctrl Pts',(-10.0514428414942,73.4562499997166,
3.26591175476071));
#294556=CARTESIAN_POINT('Ctrl Pts',(-8.13178807675725,73.606249999716,5.90808986649102));
#294557=CARTESIAN_POINT('Ctrl Pts',(-6.21213331202027,73.7562499997155,
8.55026797822134));
#294558=CARTESIAN_POINT('Ctrl Pts',(-3.10606665601016,73.9062499997148,
9.5594902125713));
#294559=CARTESIAN_POINT('Ctrl Pts',(-5.31854056883567E-14,74.0562499997143,
10.5687124469213));
#294560=CARTESIAN_POINT('Ctrl Pts',(3.10606665601005,74.2062499997136,9.5594902125713));
#294561=CARTESIAN_POINT('Ctrl Pts',(6.21213331202016,74.3562499997131,8.55026797822134));
#294562=CARTESIAN_POINT('Ctrl Pts',(8.13178807675713,74.5062499997125,5.90808986649102));
#294563=CARTESIAN_POINT('Ctrl Pts',(10.0514428414941,74.6562499997118,3.2659117547607));
#294564=CARTESIAN_POINT('Ctrl Pts',(10.0514428414941,74.8062499997113,-1.23094673026484E-15));
#294565=CARTESIAN_POINT('Ctrl Pts',(10.0514428414941,74.9562499997106,-3.26591175476071));
#294566=CARTESIAN_POINT('Ctrl Pts',(8.13178807675713,75.10624999971,-5.90808986649102));
#294567=CARTESIAN_POINT('Ctrl Pts',(6.21213331202016,75.2562499997094,-8.55026797822134));
#294568=CARTESIAN_POINT('Ctrl Pts',(3.10606665601005,75.4062499997088,-9.5594902125713));
#294569=CARTESIAN_POINT('Ctrl Pts',(-5.66378482980338E-14,75.5562499997083,
-10.5687124469213));
#294570=CARTESIAN_POINT('Ctrl Pts',(-3.10606665601016,75.7062499997077,
-9.5594902125713));
#294571=CARTESIAN_POINT('Ctrl Pts',(-6.21213331202027,75.856249999707,-8.55026797822134));
#294572=CARTESIAN_POINT('Ctrl Pts',(-8.13178807675725,76.0062499997065,
-5.90808986649102));
#294573=CARTESIAN_POINT('Ctrl Pts',(-10.0514428414942,76.1562499997058,
-3.2659117547607));
#294574=CARTESIAN_POINT('Ctrl Pts',(-10.0514428414942,76.3062499997052,
2.46189346052968E-15));
#294575=CARTESIAN_POINT('Ctrl Pts',(-10.0514428414942,76.4562499997046,
3.26591175476071));
#294576=CARTESIAN_POINT('Ctrl Pts',(-8.13178807675725,76.606249999704,5.90808986649102));
#294577=CARTESIAN_POINT('Ctrl Pts',(-6.21213331202027,76.7562499997035,
8.55026797822134));
#294578=CARTESIAN_POINT('Ctrl Pts',(-3.10606665601016,76.9062499997029,
9.5594902125713));
#294579=CARTESIAN_POINT('Ctrl Pts',(-5.49131149600185E-14,77.0562499997022,
10.5687124469213));
#294580=CARTESIAN_POINT('Ctrl Pts',(3.10606665601005,77.2062499997016,9.5594902125713));
#294581=CARTESIAN_POINT('Ctrl Pts',(6.21213331202016,77.356249999701,8.55026797822134));
#294582=CARTESIAN_POINT('Ctrl Pts',(8.13178807675713,77.5062499997004,5.90808986649102));
#294583=CARTESIAN_POINT('Ctrl Pts',(10.0514428414941,77.6562499996998,3.2659117547607));
#294584=CARTESIAN_POINT('Ctrl Pts',(10.0514428414941,77.8062499996992,-1.23094673026484E-15));
#294585=CARTESIAN_POINT('Ctrl Pts',(10.0514428414941,77.9562499996987,-3.26591175476071));
#294586=CARTESIAN_POINT('Ctrl Pts',(8.13178807675713,78.1062499996981,-5.90808986649102));
#294587=CARTESIAN_POINT('Ctrl Pts',(6.21213331202016,78.2562499996974,-8.55026797822134));
#294588=CARTESIAN_POINT('Ctrl Pts',(3.10606665601005,78.4062499996969,-9.5594902125713));
#294589=CARTESIAN_POINT('Ctrl Pts',(-5.83655575696956E-14,78.5562499996963,
-10.5687124469213));
#294590=CARTESIAN_POINT('Ctrl Pts',(-3.10606665601017,78.7062499996957,
-9.5594902125713));
#294591=CARTESIAN_POINT('Ctrl Pts',(-6.21213331202028,78.8562499996951,
-8.55026797822134));
#294592=CARTESIAN_POINT('Ctrl Pts',(-8.13178807675725,79.0062499996944,
-5.90808986649102));
#294593=CARTESIAN_POINT('Ctrl Pts',(-10.0514428414942,79.1562499996939,
-3.2659117547607));
#294594=CARTESIAN_POINT('Ctrl Pts',(-10.0514428414942,79.3062499996932,
2.46189346052968E-15));
#294595=CARTESIAN_POINT('Ctrl Pts',(-10.0514428414942,79.4562499996926,
3.26591175476071));
#294596=CARTESIAN_POINT('Ctrl Pts',(-8.13178807675725,79.606249999692,5.90808986649102));
#294597=CARTESIAN_POINT('Ctrl Pts',(-6.21213331202027,79.7562499996915,
8.55026797822134));
#294598=CARTESIAN_POINT('Ctrl Pts',(-3.10606665601016,79.9062499996908,
9.5594902125713));
#294599=CARTESIAN_POINT('Ctrl Pts',(-5.66408242316803E-14,80.0562499996902,
10.5687124469213));
#294600=CARTESIAN_POINT('Ctrl Pts',(3.10606665601005,80.2062499996896,9.5594902125713));
#294601=CARTESIAN_POINT('Ctrl Pts',(6.21213331202016,80.356249999689,8.55026797822134));
#294602=CARTESIAN_POINT('Ctrl Pts',(8.13178807675713,80.5062499996884,5.90808986649102));
#294603=CARTESIAN_POINT('Ctrl Pts',(10.0514428414941,80.6562499996878,3.2659117547607));
#294604=CARTESIAN_POINT('Ctrl Pts',(10.0514428414941,80.8062499996873,-1.23094673026484E-15));
#294605=CARTESIAN_POINT('Ctrl Pts',(10.0514428414941,80.9562499996866,-3.26591175476071));
#294606=CARTESIAN_POINT('Ctrl Pts',(8.13178807675713,81.1062499996861,-5.90808986649102));
#294607=CARTESIAN_POINT('Ctrl Pts',(6.21213331202016,81.2562499996854,-8.55026797822134));
#294608=CARTESIAN_POINT('Ctrl Pts',(3.10606665601005,81.4062499996849,-9.5594902125713));
#294609=CARTESIAN_POINT('Ctrl Pts',(-6.00932668413574E-14,81.5562499996843,
-10.5687124469213));
#294610=CARTESIAN_POINT('Ctrl Pts',(-3.10606665601017,81.7062499996837,
-9.5594902125713));
#294611=CARTESIAN_POINT('Ctrl Pts',(-6.21213331202028,81.856249999683,-8.55026797822134));
#294612=CARTESIAN_POINT('Ctrl Pts',(-8.13178807675725,82.0062499996824,
-5.90808986649102));
#294613=CARTESIAN_POINT('Ctrl Pts',(-10.0514428414942,82.1562499996818,
-3.2659117547607));
#294614=CARTESIAN_POINT('Ctrl Pts',(-10.0514428414942,82.3062499996813,
2.46189346052968E-15));
#294615=CARTESIAN_POINT('Ctrl Pts',(-10.0514428414942,82.4562499996806,
3.26591175476071));
#294616=CARTESIAN_POINT('Ctrl Pts',(-8.13178807675725,82.60624999968,5.90808986649102));
#294617=CARTESIAN_POINT('Ctrl Pts',(-6.21213331202028,82.7562499996795,
8.55026797822134));
#294618=CARTESIAN_POINT('Ctrl Pts',(-3.10606665601017,82.9062499996789,
9.5594902125713));
#294619=CARTESIAN_POINT('Ctrl Pts',(-5.83685335033422E-14,83.0562499996782,
10.5687124469213));
#294620=CARTESIAN_POINT('Ctrl Pts',(3.10606665601005,83.2062499996776,9.5594902125713));
#294621=CARTESIAN_POINT('Ctrl Pts',(6.21213331202016,83.356249999677,8.55026797822134));
#294622=CARTESIAN_POINT('Ctrl Pts',(8.13178807675713,83.5062499996764,5.90808986649102));
#294623=CARTESIAN_POINT('Ctrl Pts',(10.0514428414941,83.6562499996759,3.2659117547607));
#294624=CARTESIAN_POINT('Ctrl Pts',(10.0514428414941,83.8062499996752,-1.23094673026484E-15));
#294625=CARTESIAN_POINT('Ctrl Pts',(10.0514428414941,83.9562499996747,-3.26591175476071));
#294626=CARTESIAN_POINT('Ctrl Pts',(8.13178807675713,84.106249999674,-5.90808986649102));
#294627=CARTESIAN_POINT('Ctrl Pts',(6.21213331202016,84.2562499996734,-8.55026797822134));
#294628=CARTESIAN_POINT('Ctrl Pts',(3.10606665601005,84.4062499996729,-9.5594902125713));
#294629=CARTESIAN_POINT('Ctrl Pts',(-6.18209761130193E-14,84.5562499996723,
-10.5687124469213));
#294630=CARTESIAN_POINT('Ctrl Pts',(-3.10606665601017,84.7062499996717,
-9.5594902125713));
#294631=CARTESIAN_POINT('Ctrl Pts',(-6.21213331202028,84.856249999671,-8.55026797822134));
#294632=CARTESIAN_POINT('Ctrl Pts',(-8.13178807675725,85.0062499996704,
-5.90808986649102));
#294633=CARTESIAN_POINT('Ctrl Pts',(-10.0514428414942,85.1562499996699,
-3.2659117547607));
#294634=CARTESIAN_POINT('Ctrl Pts',(-10.0514428414942,85.3062499996692,
2.46189346052968E-15));
#294635=CARTESIAN_POINT('Ctrl Pts',(-10.0514428414942,85.4562499996686,
3.26591175476071));
#294636=CARTESIAN_POINT('Ctrl Pts',(-8.13178807675725,85.606249999668,5.90808986649102));
#294637=CARTESIAN_POINT('Ctrl Pts',(-6.21213331202028,85.7562499996675,
8.55026797822134));
#294638=CARTESIAN_POINT('Ctrl Pts',(-3.10606665601017,85.9062499996669,
9.5594902125713));
#294639=CARTESIAN_POINT('Ctrl Pts',(-6.0096242775004E-14,86.0562499996662,
10.5687124469213));
#294640=CARTESIAN_POINT('Ctrl Pts',(3.10606665601005,86.2062499996657,9.5594902125713));
#294641=CARTESIAN_POINT('Ctrl Pts',(6.21213331202016,86.3562499996651,8.55026797822134));
#294642=CARTESIAN_POINT('Ctrl Pts',(8.13178807675713,86.5062499996644,5.90808986649102));
#294643=CARTESIAN_POINT('Ctrl Pts',(10.0514428414941,86.6562499996638,3.2659117547607));
#294644=CARTESIAN_POINT('Ctrl Pts',(10.0514428414941,86.8062499996633,-1.23094673026484E-15));
#294645=CARTESIAN_POINT('Ctrl Pts',(10.0514428414941,86.9562499996626,-3.26591175476071));
#294646=CARTESIAN_POINT('Ctrl Pts',(8.13178807675713,87.1062499996621,-5.90808986649102));
#294647=CARTESIAN_POINT('Ctrl Pts',(6.21213331202015,87.2562499996614,-8.55026797822134));
#294648=CARTESIAN_POINT('Ctrl Pts',(3.10606665601004,87.4062499996609,-9.5594902125713));
#294649=CARTESIAN_POINT('Ctrl Pts',(-6.35486853846811E-14,87.5562499996603,
-10.5687124469213));
#294650=CARTESIAN_POINT('Ctrl Pts',(-3.10606665601017,87.7062499996597,
-9.5594902125713));
#294651=CARTESIAN_POINT('Ctrl Pts',(-6.21213331202028,87.856249999659,-8.55026797822134));
#294652=CARTESIAN_POINT('Ctrl Pts',(-8.13178807675726,88.0062499996585,
-5.90808986649102));
#294653=CARTESIAN_POINT('Ctrl Pts',(-10.0514428414942,88.1562499996578,
-3.2659117547607));
#294654=CARTESIAN_POINT('Ctrl Pts',(-10.0514428414942,88.3062499996572,
2.46189346052968E-15));
#294655=CARTESIAN_POINT('Ctrl Pts',(-10.0514428414942,88.4562499996566,
3.26591175476071));
#294656=CARTESIAN_POINT('Ctrl Pts',(-8.13178807675726,88.6062499996561,
5.90808986649102));
#294657=CARTESIAN_POINT('Ctrl Pts',(-6.21213331202028,88.7562499996555,
8.55026797822134));
#294658=CARTESIAN_POINT('Ctrl Pts',(-3.10606665601017,88.9062499996548,
9.5594902125713));
#294659=CARTESIAN_POINT('Ctrl Pts',(-6.18239520466659E-14,89.0562499996542,
10.5687124469213));
#294660=CARTESIAN_POINT('Ctrl Pts',(3.10606665601005,89.2062499996537,9.5594902125713));
#294661=CARTESIAN_POINT('Ctrl Pts',(6.21213331202016,89.3562499996531,8.55026797822134));
#294662=CARTESIAN_POINT('Ctrl Pts',(8.13178807675713,89.5062499996525,5.90808986649102));
#294663=CARTESIAN_POINT('Ctrl Pts',(10.0514428414941,89.6562499996518,3.2659117547607));
#294664=CARTESIAN_POINT('Ctrl Pts',(10.0514428414941,89.8062499996512,-1.23094673026484E-15));
#294665=CARTESIAN_POINT('Ctrl Pts',(10.0514428414941,89.9562499996507,-3.26591175476071));
#294666=CARTESIAN_POINT('Ctrl Pts',(8.13178807675713,90.10624999965,-5.90808986649102));
#294667=CARTESIAN_POINT('Ctrl Pts',(6.21213331202015,90.2562499996494,-8.55026797822134));
#294668=CARTESIAN_POINT('Ctrl Pts',(3.10606665601004,90.4062499996488,-9.5594902125713));
#294669=CARTESIAN_POINT('Ctrl Pts',(-6.52763946563429E-14,90.5562499996483,
-10.5687124469213));
#294670=CARTESIAN_POINT('Ctrl Pts',(-3.10606665601017,90.7062499996476,
-9.5594902125713));
#294671=CARTESIAN_POINT('Ctrl Pts',(-6.21213331202028,90.856249999647,-8.55026797822134));
#294672=CARTESIAN_POINT('Ctrl Pts',(-8.13178807675726,91.0062499996464,
-5.90808986649102));
#294673=CARTESIAN_POINT('Ctrl Pts',(-10.0514428414942,91.1562499996458,
-3.2659117547607));
#294674=CARTESIAN_POINT('Ctrl Pts',(-10.0514428414942,91.3062499996452,
2.46189346052968E-15));
#294675=CARTESIAN_POINT('Ctrl Pts',(-10.0514428414942,91.4562499996446,
3.26591175476071));
#294676=CARTESIAN_POINT('Ctrl Pts',(-8.13178807675726,91.606249999644,5.90808986649102));
#294677=CARTESIAN_POINT('Ctrl Pts',(-6.21213331202028,91.7562499996434,
8.55026797822134));
#294678=CARTESIAN_POINT('Ctrl Pts',(-3.10606665601017,91.9062499996429,
9.5594902125713));
#294679=CARTESIAN_POINT('Ctrl Pts',(-6.35516613183277E-14,92.0562499996422,
10.5687124469213));
#294680=CARTESIAN_POINT('Ctrl Pts',(3.10606665601004,92.2062499996417,9.5594902125713));
#294681=CARTESIAN_POINT('Ctrl Pts',(6.21213331202015,92.3562499996411,8.55026797822134));
#294682=CARTESIAN_POINT('Ctrl Pts',(8.13178807675712,92.5062499996404,5.90808986649102));
#294683=CARTESIAN_POINT('Ctrl Pts',(10.0514428414941,92.6562499996398,3.2659117547607));
#294684=CARTESIAN_POINT('Ctrl Pts',(10.0514428414941,92.8062499996392,-1.23094673026484E-15));
#294685=CARTESIAN_POINT('Ctrl Pts',(10.0514428414941,92.9562499996387,-3.26591175476071));
#294686=CARTESIAN_POINT('Ctrl Pts',(8.13178807675712,93.1062499996381,-5.90808986649102));
#294687=CARTESIAN_POINT('Ctrl Pts',(6.21213331202015,93.2562499996374,-8.55026797822134));
#294688=CARTESIAN_POINT('Ctrl Pts',(3.10606665601004,93.4062499996369,-9.5594902125713));
#294689=CARTESIAN_POINT('Ctrl Pts',(-6.70041039280048E-14,93.5562499996362,
-10.5687124469213));
#294690=CARTESIAN_POINT('Ctrl Pts',(-3.10606665601018,93.7062499996357,
-9.5594902125713));
#294691=CARTESIAN_POINT('Ctrl Pts',(-6.21213331202028,93.856249999635,-8.55026797822134));
#294692=CARTESIAN_POINT('Ctrl Pts',(-8.13178807675726,94.0062499996344,
-5.90808986649102));
#294693=CARTESIAN_POINT('Ctrl Pts',(-10.0514428414942,94.1562499996338,
-3.2659117547607));
#294694=CARTESIAN_POINT('Ctrl Pts',(-10.0514428414942,94.3062499996333,
2.46189346052968E-15));
#294695=CARTESIAN_POINT('Ctrl Pts',(-10.0514428414942,94.4562499996326,
3.26591175476071));
#294696=CARTESIAN_POINT('Ctrl Pts',(-8.13178807675726,94.606249999632,5.90808986649102));
#294697=CARTESIAN_POINT('Ctrl Pts',(-6.21213331202028,94.7562499996315,
8.55026797822134));
#294698=CARTESIAN_POINT('Ctrl Pts',(-3.10606665601017,94.9062499996309,
9.5594902125713));
#294699=CARTESIAN_POINT('Ctrl Pts',(-6.52793705899895E-14,95.0562499996302,
10.5687124469213));
#294700=CARTESIAN_POINT('Ctrl Pts',(3.10606665601004,95.2062499996296,9.5594902125713));
#294701=CARTESIAN_POINT('Ctrl Pts',(6.21213331202015,95.3562499996291,8.55026797822134));
#294702=CARTESIAN_POINT('Ctrl Pts',(8.13178807675712,95.5062499996285,5.90808986649102));
#294703=CARTESIAN_POINT('Ctrl Pts',(10.0514428414941,95.6562499996278,3.2659117547607));
#294704=CARTESIAN_POINT('Ctrl Pts',(10.0514428414941,95.8062499996273,-1.23094673026484E-15));
#294705=CARTESIAN_POINT('Ctrl Pts',(10.0514428414941,95.9562499996266,-3.26591175476071));
#294706=CARTESIAN_POINT('Ctrl Pts',(8.13178807675712,96.1062499996261,-5.90808986649102));
#294707=CARTESIAN_POINT('Ctrl Pts',(6.21213331202015,96.2562499996255,-8.55026797822134));
#294708=CARTESIAN_POINT('Ctrl Pts',(3.10606665601004,96.4062499996248,-9.5594902125713));
#294709=CARTESIAN_POINT('Ctrl Pts',(-6.87318131996666E-14,96.5562499996243,
-10.5687124469213));
#294710=CARTESIAN_POINT('Ctrl Pts',(-3.10606665601018,96.7062499996236,
-9.5594902125713));
#294711=CARTESIAN_POINT('Ctrl Pts',(-6.21213331202028,96.856249999623,-8.55026797822134));
#294712=CARTESIAN_POINT('Ctrl Pts',(-8.13178807675726,97.0062499996224,
-5.90808986649102));
#294713=CARTESIAN_POINT('Ctrl Pts',(-10.0514428414942,97.1562499996218,
-3.2659117547607));
#294714=CARTESIAN_POINT('Ctrl Pts',(-10.0514428414942,97.3062499996212,
2.46189346052968E-15));
#294715=CARTESIAN_POINT('Ctrl Pts',(-10.0514428414942,97.4562499996206,
3.26591175476071));
#294716=CARTESIAN_POINT('Ctrl Pts',(-8.13178807675726,97.60624999962,5.90808986649102));
#294717=CARTESIAN_POINT('Ctrl Pts',(-6.21213331202028,97.7562499996195,
8.55026797822134));
#294718=CARTESIAN_POINT('Ctrl Pts',(-3.10606665601018,97.9062499996189,
9.5594902125713));
#294719=CARTESIAN_POINT('Ctrl Pts',(-6.70070798616514E-14,98.0562499996182,
10.5687124469213));
#294720=CARTESIAN_POINT('Ctrl Pts',(3.10606665601004,98.2062499996177,9.5594902125713));
#294721=CARTESIAN_POINT('Ctrl Pts',(6.21213331202015,98.3562499996171,8.55026797822134));
#294722=CARTESIAN_POINT('Ctrl Pts',(8.13178807675712,98.5062499996165,5.90808986649102));
#294723=CARTESIAN_POINT('Ctrl Pts',(10.0514428414941,98.6562499996158,3.2659117547607));
#294724=CARTESIAN_POINT('Ctrl Pts',(10.0514428414941,98.8062499996153,-1.23094673026484E-15));
#294725=CARTESIAN_POINT('Ctrl Pts',(10.0514428414941,98.9562499996147,-3.26591175476071));
#294726=CARTESIAN_POINT('Ctrl Pts',(8.13178807675712,99.1062499996141,-5.90808986649102));
#294727=CARTESIAN_POINT('Ctrl Pts',(6.21213331202015,99.2562499996134,-8.55026797822134));
#294728=CARTESIAN_POINT('Ctrl Pts',(3.10606665601004,99.4062499996129,-9.5594902125713));
#294729=CARTESIAN_POINT('Ctrl Pts',(-7.04595224713284E-14,99.5562499996123,
-10.5687124469213));
#294730=CARTESIAN_POINT('Ctrl Pts',(-3.10606665601018,99.7062499996117,
-9.5594902125713));
#294731=CARTESIAN_POINT('Ctrl Pts',(-6.21213331202028,99.856249999611,-8.55026797822134));
#294732=CARTESIAN_POINT('Ctrl Pts',(-8.13178807675726,100.00624999961,-5.90808986649102));
#294733=CARTESIAN_POINT('Ctrl Pts',(-10.0514428414942,100.15624999961,-3.2659117547607));
#294734=CARTESIAN_POINT('Ctrl Pts',(-10.0514428414942,100.306249999609,
2.46189346052968E-15));
#294735=CARTESIAN_POINT('Ctrl Pts',(-10.0514428414942,100.456249999609,
3.26591175476071));
#294736=CARTESIAN_POINT('Ctrl Pts',(-8.13178807675726,100.606249999608,
5.90808986649102));
#294737=CARTESIAN_POINT('Ctrl Pts',(-6.21213331202028,100.756249999607,
8.55026797822134));
#294738=CARTESIAN_POINT('Ctrl Pts',(-3.10606665601018,100.906249999607,
9.5594902125713));
#294739=CARTESIAN_POINT('Ctrl Pts',(-6.87347891333132E-14,101.056249999606,
10.5687124469213));
#294740=CARTESIAN_POINT('Ctrl Pts',(3.10606665601004,101.206249999606,9.5594902125713));
#294741=CARTESIAN_POINT('Ctrl Pts',(6.21213331202015,101.356249999605,8.55026797822134));
#294742=CARTESIAN_POINT('Ctrl Pts',(8.13178807675712,101.506249999604,5.90808986649102));
#294743=CARTESIAN_POINT('Ctrl Pts',(10.0514428414941,101.656249999604,3.2659117547607));
#294744=CARTESIAN_POINT('Ctrl Pts',(10.0514428414941,101.806249999603,-1.23094673026484E-15));
#294745=CARTESIAN_POINT('Ctrl Pts',(10.0514428414941,101.956249999603,-3.26591175476071));
#294746=CARTESIAN_POINT('Ctrl Pts',(8.13178807675712,102.106249999602,-5.90808986649102));
#294747=CARTESIAN_POINT('Ctrl Pts',(6.21213331202014,102.256249999601,-8.55026797822134));
#294748=CARTESIAN_POINT('Ctrl Pts',(3.10606665601004,102.406249999601,-9.5594902125713));
#294749=CARTESIAN_POINT('Ctrl Pts',(-7.21872317429903E-14,102.5562499996,
-10.5687124469213));
#294750=CARTESIAN_POINT('Ctrl Pts',(-3.10606665601018,102.7062499996,-9.5594902125713));
#294751=CARTESIAN_POINT('Ctrl Pts',(-6.21213331202029,102.856249999599,
-8.55026797822134));
#294752=CARTESIAN_POINT('Ctrl Pts',(-8.13178807675726,103.006249999598,
-5.90808986649102));
#294753=CARTESIAN_POINT('Ctrl Pts',(-10.0514428414942,103.156249999598,
-3.2659117547607));
#294754=CARTESIAN_POINT('Ctrl Pts',(-10.0514428414942,103.306249999597,
2.46189346052968E-15));
#294755=CARTESIAN_POINT('Ctrl Pts',(-10.0514428414942,103.456249999597,
3.26591175476071));
#294756=CARTESIAN_POINT('Ctrl Pts',(-8.13178807675726,103.606249999596,
5.90808986649102));
#294757=CARTESIAN_POINT('Ctrl Pts',(-6.21213331202028,103.756249999595,
8.55026797822134));
#294758=CARTESIAN_POINT('Ctrl Pts',(-3.10606665601018,103.906249999595,
9.5594902125713));
#294759=CARTESIAN_POINT('Ctrl Pts',(-7.04624984049751E-14,104.056249999594,
10.5687124469213));
#294760=CARTESIAN_POINT('Ctrl Pts',(3.10606665601004,104.206249999594,9.5594902125713));
#294761=CARTESIAN_POINT('Ctrl Pts',(6.21213331202015,104.356249999593,8.55026797822134));
#294762=CARTESIAN_POINT('Ctrl Pts',(8.13178807675712,104.506249999592,5.90808986649102));
#294763=CARTESIAN_POINT('Ctrl Pts',(10.0514428414941,104.656249999592,3.2659117547607));
#294764=CARTESIAN_POINT('Ctrl Pts',(10.0514428414941,104.806249999591,-1.23094673026484E-15));
#294765=CARTESIAN_POINT('Ctrl Pts',(10.0514428414941,104.956249999591,-3.26591175476071));
#294766=CARTESIAN_POINT('Ctrl Pts',(8.13178807675712,105.10624999959,-5.90808986649102));
#294767=CARTESIAN_POINT('Ctrl Pts',(6.21213331202014,105.256249999589,-8.55026797822134));
#294768=CARTESIAN_POINT('Ctrl Pts',(3.10606665601003,105.406249999589,-9.5594902125713));
#294769=CARTESIAN_POINT('Ctrl Pts',(-7.39149410146522E-14,105.556249999588,
-10.5687124469213));
#294770=CARTESIAN_POINT('Ctrl Pts',(-3.10606665601018,105.706249999588,
-9.5594902125713));
#294771=CARTESIAN_POINT('Ctrl Pts',(-6.21213331202029,105.856249999587,
-8.55026797822134));
#294772=CARTESIAN_POINT('Ctrl Pts',(-8.13178807675726,106.006249999586,
-5.90808986649102));
#294773=CARTESIAN_POINT('Ctrl Pts',(-10.0514428414942,106.156249999586,
-3.2659117547607));
#294774=CARTESIAN_POINT('Ctrl Pts',(-10.0514428414942,106.306249999585,
2.46189346052968E-15));
#294775=CARTESIAN_POINT('Ctrl Pts',(-10.0514428414942,106.456249999585,
3.26591175476071));
#294776=CARTESIAN_POINT('Ctrl Pts',(-8.13178807675726,106.606249999584,
5.90808986649102));
#294777=CARTESIAN_POINT('Ctrl Pts',(-6.21213331202029,106.756249999583,
8.55026797822134));
#294778=CARTESIAN_POINT('Ctrl Pts',(-3.10606665601018,106.906249999583,
9.5594902125713));
#294779=CARTESIAN_POINT('Ctrl Pts',(-7.21902076766369E-14,107.056249999582,
10.5687124469213));
#294780=CARTESIAN_POINT('Ctrl Pts',(3.10606665601003,107.206249999582,9.5594902125713));
#294781=CARTESIAN_POINT('Ctrl Pts',(6.21213331202014,107.356249999581,8.55026797822134));
#294782=CARTESIAN_POINT('Ctrl Pts',(8.13178807675711,107.50624999958,5.90808986649102));
#294783=CARTESIAN_POINT('Ctrl Pts',(10.0514428414941,107.65624999958,3.2659117547607));
#294784=CARTESIAN_POINT('Ctrl Pts',(10.0514428414941,107.806249999579,-1.23094673026484E-15));
#294785=CARTESIAN_POINT('Ctrl Pts',(10.0514428414941,107.956249999579,-3.26591175476071));
#294786=CARTESIAN_POINT('Ctrl Pts',(8.13178807675711,108.106249999578,-5.90808986649102));
#294787=CARTESIAN_POINT('Ctrl Pts',(6.21213331202014,108.256249999577,-8.55026797822134));
#294788=CARTESIAN_POINT('Ctrl Pts',(3.10606665601003,108.406249999577,-9.5594902125713));
#294789=CARTESIAN_POINT('Ctrl Pts',(-7.5642650286314E-14,108.556249999576,
-10.5687124469213));
#294790=CARTESIAN_POINT('Ctrl Pts',(-3.10606665601018,108.706249999576,
-9.5594902125713));
#294791=CARTESIAN_POINT('Ctrl Pts',(-6.21213331202029,108.856249999575,
-8.55026797822134));
#294792=CARTESIAN_POINT('Ctrl Pts',(-8.13178807675727,109.006249999574,
-5.90808986649102));
#294793=CARTESIAN_POINT('Ctrl Pts',(-10.0514428414942,109.156249999574,
-3.2659117547607));
#294794=CARTESIAN_POINT('Ctrl Pts',(-10.0514428414942,109.306249999573,
2.46189346052968E-15));
#294795=CARTESIAN_POINT('Ctrl Pts',(-10.0514428414942,109.456249999573,
3.26591175476071));
#294796=CARTESIAN_POINT('Ctrl Pts',(-8.13178807675727,109.606249999572,
5.90808986649102));
#294797=CARTESIAN_POINT('Ctrl Pts',(-6.21213331202029,109.756249999571,
8.55026797822134));
#294798=CARTESIAN_POINT('Ctrl Pts',(-3.10606665601018,109.906249999571,
9.5594902125713));
#294799=CARTESIAN_POINT('Ctrl Pts',(-7.39179169482987E-14,110.05624999957,
10.5687124469213));
#294800=CARTESIAN_POINT('Ctrl Pts',(3.10606665601003,110.20624999957,9.5594902125713));
#294801=CARTESIAN_POINT('Ctrl Pts',(6.21213331202014,110.356249999569,8.55026797822134));
#294802=CARTESIAN_POINT('Ctrl Pts',(8.13178807675711,110.506249999568,5.90808986649102));
#294803=CARTESIAN_POINT('Ctrl Pts',(10.0514428414941,110.656249999568,3.2659117547607));
#294804=CARTESIAN_POINT('Ctrl Pts',(10.0514428414941,110.806249999567,-1.23094673026484E-15));
#294805=CARTESIAN_POINT('Ctrl Pts',(10.0514428414941,110.956249999567,-3.26591175476071));
#294806=CARTESIAN_POINT('Ctrl Pts',(8.13178807675711,111.106249999566,-5.90808986649102));
#294807=CARTESIAN_POINT('Ctrl Pts',(6.21213331202014,111.256249999565,-8.55026797822134));
#294808=CARTESIAN_POINT('Ctrl Pts',(3.10606665601003,111.406249999565,-9.5594902125713));
#294809=CARTESIAN_POINT('Ctrl Pts',(-7.73703595579758E-14,111.556249999564,
-10.5687124469213));
#294810=CARTESIAN_POINT('Ctrl Pts',(-3.10606665601019,111.706249999564,
-9.5594902125713));
#294811=CARTESIAN_POINT('Ctrl Pts',(-6.21213331202029,111.856249999563,
-8.55026797822134));
#294812=CARTESIAN_POINT('Ctrl Pts',(-8.13178807675727,112.006249999562,
-5.90808986649102));
#294813=CARTESIAN_POINT('Ctrl Pts',(-10.0514428414942,112.156249999562,
-3.2659117547607));
#294814=CARTESIAN_POINT('Ctrl Pts',(-10.0514428414942,112.306249999561,
2.46189346052968E-15));
#294815=CARTESIAN_POINT('Ctrl Pts',(-10.0514428414942,112.456249999561,
3.26591175476071));
#294816=CARTESIAN_POINT('Ctrl Pts',(-8.13178807675727,112.60624999956,5.90808986649102));
#294817=CARTESIAN_POINT('Ctrl Pts',(-6.21213331202029,112.756249999559,
8.55026797822134));
#294818=CARTESIAN_POINT('Ctrl Pts',(-3.10606665601018,112.906249999559,
9.5594902125713));
#294819=CARTESIAN_POINT('Ctrl Pts',(-7.56456262199606E-14,113.056249999558,
10.5687124469213));
#294820=CARTESIAN_POINT('Ctrl Pts',(3.10606665601003,113.206249999558,9.5594902125713));
#294821=CARTESIAN_POINT('Ctrl Pts',(6.21213331202014,113.356249999557,8.55026797822134));
#294822=CARTESIAN_POINT('Ctrl Pts',(8.13178807675711,113.506249999556,5.90808986649102));
#294823=CARTESIAN_POINT('Ctrl Pts',(10.0514428414941,113.656249999556,3.2659117547607));
#294824=CARTESIAN_POINT('Ctrl Pts',(10.0514428414941,113.806249999555,-1.23094673026484E-15));
#294825=CARTESIAN_POINT('Ctrl Pts',(10.0514428414941,113.956249999555,-3.26591175476071));
#294826=CARTESIAN_POINT('Ctrl Pts',(8.13178807675711,114.106249999554,-5.90808986649102));
#294827=CARTESIAN_POINT('Ctrl Pts',(6.21213331202014,114.256249999553,-8.55026797822134));
#294828=CARTESIAN_POINT('Ctrl Pts',(3.10606665601003,114.406249999553,-9.5594902125713));
#294829=CARTESIAN_POINT('Ctrl Pts',(-7.90980688296377E-14,114.556249999552,
-10.5687124469213));
#294830=CARTESIAN_POINT('Ctrl Pts',(-3.10606665601019,114.706249999552,
-9.5594902125713));
#294831=CARTESIAN_POINT('Ctrl Pts',(-6.2121333120203,114.856249999551,-8.55026797822134));
#294832=CARTESIAN_POINT('Ctrl Pts',(-8.13178807675727,115.00624999955,-5.90808986649102));
#294833=CARTESIAN_POINT('Ctrl Pts',(-10.0514428414942,115.15624999955,-3.2659117547607));
#294834=CARTESIAN_POINT('Ctrl Pts',(-10.0514428414942,115.306249999549,
2.46189346052968E-15));
#294835=CARTESIAN_POINT('Ctrl Pts',(-10.0514428414942,115.456249999549,
3.26591175476071));
#294836=CARTESIAN_POINT('Ctrl Pts',(-8.13178807675727,115.606249999548,
5.90808986649102));
#294837=CARTESIAN_POINT('Ctrl Pts',(-6.21213331202029,115.756249999547,
8.55026797822134));
#294838=CARTESIAN_POINT('Ctrl Pts',(-3.10606665601019,115.906249999547,
9.5594902125713));
#294839=CARTESIAN_POINT('Ctrl Pts',(-7.73733354916224E-14,116.056249999546,
10.5687124469213));
#294840=CARTESIAN_POINT('Ctrl Pts',(3.10606665601003,116.206249999546,9.5594902125713));
#294841=CARTESIAN_POINT('Ctrl Pts',(6.21213331202014,116.356249999545,8.55026797822134));
#294842=CARTESIAN_POINT('Ctrl Pts',(8.13178807675711,116.506249999544,5.90808986649102));
#294843=CARTESIAN_POINT('Ctrl Pts',(10.0514428414941,116.656249999544,3.2659117547607));
#294844=CARTESIAN_POINT('Ctrl Pts',(10.0514428414941,116.806249999543,-1.23094673026484E-15));
#294845=CARTESIAN_POINT('Ctrl Pts',(10.0514428414941,116.956249999543,-3.26591175476071));
#294846=CARTESIAN_POINT('Ctrl Pts',(8.13178807675711,117.106249999542,-5.90808986649102));
#294847=CARTESIAN_POINT('Ctrl Pts',(6.21213331202014,117.256249999541,-8.55026797822134));
#294848=CARTESIAN_POINT('Ctrl Pts',(3.10606665601003,117.406249999541,-9.5594902125713));
#294849=CARTESIAN_POINT('Ctrl Pts',(-8.08257781012995E-14,117.55624999954,
-10.5687124469213));
#294850=CARTESIAN_POINT('Ctrl Pts',(-3.10606665601019,117.70624999954,-9.5594902125713));
#294851=CARTESIAN_POINT('Ctrl Pts',(-6.2121333120203,117.856249999539,-8.55026797822134));
#294852=CARTESIAN_POINT('Ctrl Pts',(-8.13178807675727,118.006249999538,
-5.90808986649102));
#294853=CARTESIAN_POINT('Ctrl Pts',(-10.0514428414942,118.156249999538,
-3.2659117547607));
#294854=CARTESIAN_POINT('Ctrl Pts',(-10.0514428414942,118.306249999537,
2.46189346052968E-15));
#294855=CARTESIAN_POINT('Ctrl Pts',(-10.0514428414942,118.456249999537,
3.26591175476071));
#294856=CARTESIAN_POINT('Ctrl Pts',(-8.13178807675727,118.606249999536,
5.90808986649102));
#294857=CARTESIAN_POINT('Ctrl Pts',(-6.2121333120203,118.756249999535,8.55026797822134));
#294858=CARTESIAN_POINT('Ctrl Pts',(-3.10606665601019,118.906249999535,
9.5594902125713));
#294859=CARTESIAN_POINT('Ctrl Pts',(-7.91010447632842E-14,119.056249999534,
10.5687124469213));
#294860=CARTESIAN_POINT('Ctrl Pts',(3.10606665601003,119.206249999534,9.5594902125713));
#294861=CARTESIAN_POINT('Ctrl Pts',(6.21213331202014,119.356249999533,8.55026797822134));
#294862=CARTESIAN_POINT('Ctrl Pts',(8.13178807675711,119.506249999532,5.90808986649102));
#294863=CARTESIAN_POINT('Ctrl Pts',(10.0514428414941,119.656249999532,3.2659117547607));
#294864=CARTESIAN_POINT('Ctrl Pts',(10.0514428414941,119.806249999531,-1.23094673026484E-15));
#294865=CARTESIAN_POINT('Ctrl Pts',(10.0514428414941,119.956249999531,-3.26591175476071));
#294866=CARTESIAN_POINT('Ctrl Pts',(8.13178807675711,120.10624999953,-5.90808986649102));
#294867=CARTESIAN_POINT('Ctrl Pts',(6.21213331202013,120.256249999529,-8.55026797822134));
#294868=CARTESIAN_POINT('Ctrl Pts',(3.10606665601003,120.406249999529,-9.5594902125713));
#294869=CARTESIAN_POINT('Ctrl Pts',(-8.25534873729613E-14,120.556249999528,
-10.5687124469213));
#294870=CARTESIAN_POINT('Ctrl Pts',(-3.10606665601019,120.706249999528,
-9.5594902125713));
#294871=CARTESIAN_POINT('Ctrl Pts',(-6.2121333120203,120.856249999527,-8.55026797822134));
#294872=CARTESIAN_POINT('Ctrl Pts',(-8.13178807675727,121.006249999526,
-5.90808986649102));
#294873=CARTESIAN_POINT('Ctrl Pts',(-10.0514428414943,121.156249999526,
-3.2659117547607));
#294874=CARTESIAN_POINT('Ctrl Pts',(-10.0514428414943,121.306249999525,
2.46189346052968E-15));
#294875=CARTESIAN_POINT('Ctrl Pts',(-10.0514428414943,121.456249999525,
3.26591175476071));
#294876=CARTESIAN_POINT('Ctrl Pts',(-8.13178807675727,121.606249999524,
5.90808986649102));
#294877=CARTESIAN_POINT('Ctrl Pts',(-6.2121333120203,121.756249999523,8.55026797822134));
#294878=CARTESIAN_POINT('Ctrl Pts',(-3.10606665601019,121.906249999523,
9.5594902125713));
#294879=CARTESIAN_POINT('Ctrl Pts',(-8.08287540349461E-14,122.056249999522,
10.5687124469213));
#294880=CARTESIAN_POINT('Ctrl Pts',(3.10606665601003,122.206249999522,9.5594902125713));
#294881=CARTESIAN_POINT('Ctrl Pts',(6.21213331202014,122.356249999521,8.55026797822134));
#294882=CARTESIAN_POINT('Ctrl Pts',(8.13178807675711,122.50624999952,5.90808986649102));
#294883=CARTESIAN_POINT('Ctrl Pts',(10.0514428414941,122.65624999952,3.2659117547607));
#294884=CARTESIAN_POINT('Ctrl Pts',(10.0514428414941,122.806249999519,-1.23094673026484E-15));
#294885=CARTESIAN_POINT('Ctrl Pts',(10.0514428414941,122.956249999519,-3.26591175476071));
#294886=CARTESIAN_POINT('Ctrl Pts',(8.13178807675711,123.106249999518,-5.90808986649102));
#294887=CARTESIAN_POINT('Ctrl Pts',(6.21213331202013,123.256249999517,-8.55026797822134));
#294888=CARTESIAN_POINT('Ctrl Pts',(3.10606665601002,123.406249999517,-9.5594902125713));
#294889=CARTESIAN_POINT('Ctrl Pts',(-8.42811966446232E-14,123.556249999516,
-10.5687124469213));
#294890=CARTESIAN_POINT('Ctrl Pts',(-3.10606665601019,123.706249999516,
-9.5594902125713));
#294891=CARTESIAN_POINT('Ctrl Pts',(-6.2121333120203,123.856249999515,-8.55026797822134));
#294892=CARTESIAN_POINT('Ctrl Pts',(-8.13178807675727,124.006249999514,
-5.90808986649102));
#294893=CARTESIAN_POINT('Ctrl Pts',(-10.0514428414943,124.156249999514,
-3.2659117547607));
#294894=CARTESIAN_POINT('Ctrl Pts',(-10.0514428414943,124.306249999513,
2.46189346052968E-15));
#294895=CARTESIAN_POINT('Ctrl Pts',(-10.0514428414943,124.456249999513,
3.26591175476071));
#294896=CARTESIAN_POINT('Ctrl Pts',(-8.13178807675727,124.606249999512,
5.90808986649102));
#294897=CARTESIAN_POINT('Ctrl Pts',(-6.2121333120203,124.756249999511,8.55026797822134));
#294898=CARTESIAN_POINT('Ctrl Pts',(-3.10606665601019,124.906249999511,
9.5594902125713));
#294899=CARTESIAN_POINT('Ctrl Pts',(-8.25564633066079E-14,125.05624999951,
10.5687124469213));
#294900=CARTESIAN_POINT('Ctrl Pts',(3.10606665601002,125.20624999951,9.5594902125713));
#294901=CARTESIAN_POINT('Ctrl Pts',(6.21213331202013,125.356249999509,8.55026797822134));
#294902=CARTESIAN_POINT('Ctrl Pts',(8.13178807675711,125.506249999508,5.90808986649102));
#294903=CARTESIAN_POINT('Ctrl Pts',(10.0514428414941,125.656249999508,3.2659117547607));
#294904=CARTESIAN_POINT('Ctrl Pts',(10.0514428414941,125.806249999507,-1.23094673026484E-15));
#294905=CARTESIAN_POINT('Ctrl Pts',(10.0514428414941,125.956249999507,-3.26591175476071));
#294906=CARTESIAN_POINT('Ctrl Pts',(8.13178807675711,126.106249999506,-5.90808986649102));
#294907=CARTESIAN_POINT('Ctrl Pts',(6.21213331202013,126.256249999505,-8.55026797822134));
#294908=CARTESIAN_POINT('Ctrl Pts',(3.10606665601002,126.406249999505,-9.5594902125713));
#294909=CARTESIAN_POINT('Ctrl Pts',(-8.6008905916285E-14,126.556249999504,
-10.5687124469213));
#294910=CARTESIAN_POINT('Ctrl Pts',(-3.10606665601019,126.706249999504,
-9.5594902125713));
#294911=CARTESIAN_POINT('Ctrl Pts',(-6.2121333120203,126.856249999503,-8.55026797822134));
#294912=CARTESIAN_POINT('Ctrl Pts',(-8.13178807675728,127.006249999502,
-5.90808986649102));
#294913=CARTESIAN_POINT('Ctrl Pts',(-10.0514428414943,127.156249999502,
-3.2659117547607));
#294914=CARTESIAN_POINT('Ctrl Pts',(-10.0514428414943,127.306249999501,
2.46189346052968E-15));
#294915=CARTESIAN_POINT('Ctrl Pts',(-10.0514428414943,127.456249999501,
3.26591175476071));
#294916=CARTESIAN_POINT('Ctrl Pts',(-8.13178807675728,127.6062499995,5.90808986649102));
#294917=CARTESIAN_POINT('Ctrl Pts',(-6.2121333120203,127.756249999499,8.55026797822134));
#294918=CARTESIAN_POINT('Ctrl Pts',(-3.10606665601019,127.906249999499,
9.5594902125713));
#294919=CARTESIAN_POINT('Ctrl Pts',(-8.42841725782698E-14,128.056249999498,
10.5687124469213));
#294920=CARTESIAN_POINT('Ctrl Pts',(3.10606665601002,128.206249999498,9.5594902125713));
#294921=CARTESIAN_POINT('Ctrl Pts',(6.21213331202013,128.356249999497,8.55026797822134));
#294922=CARTESIAN_POINT('Ctrl Pts',(8.1317880767571,128.506249999496,5.90808986649102));
#294923=CARTESIAN_POINT('Ctrl Pts',(10.0514428414941,128.656249999496,3.2659117547607));
#294924=CARTESIAN_POINT('Ctrl Pts',(10.0514428414941,128.806249999495,-1.23094673026484E-15));
#294925=CARTESIAN_POINT('Ctrl Pts',(10.0514428414941,128.956249999495,-3.26591175476071));
#294926=CARTESIAN_POINT('Ctrl Pts',(8.1317880767571,129.106249999494,-5.90808986649102));
#294927=CARTESIAN_POINT('Ctrl Pts',(6.21213331202013,129.256249999493,-8.55026797822134));
#294928=CARTESIAN_POINT('Ctrl Pts',(3.10606665601002,129.406249999493,-9.5594902125713));
#294929=CARTESIAN_POINT('Ctrl Pts',(-8.77366151879469E-14,129.556249999492,
-10.5687124469213));
#294930=CARTESIAN_POINT('Ctrl Pts',(-3.1060666560102,129.706249999492,-9.5594902125713));
#294931=CARTESIAN_POINT('Ctrl Pts',(-6.2121333120203,129.856249999491,-8.55026797822134));
#294932=CARTESIAN_POINT('Ctrl Pts',(-8.13178807675728,130.00624999949,-5.90808986649102));
#294933=CARTESIAN_POINT('Ctrl Pts',(-10.0514428414943,130.15624999949,-3.2659117547607));
#294934=CARTESIAN_POINT('Ctrl Pts',(-10.0514428414943,130.306249999489,
2.46189346052968E-15));
#294935=CARTESIAN_POINT('Ctrl Pts',(-10.0514428414943,130.456249999489,
3.26591175476071));
#294936=CARTESIAN_POINT('Ctrl Pts',(-8.13178807675728,130.606249999488,
5.90808986649102));
#294937=CARTESIAN_POINT('Ctrl Pts',(-6.2121333120203,130.756249999487,8.55026797822134));
#294938=CARTESIAN_POINT('Ctrl Pts',(-3.10606665601019,130.906249999487,
9.5594902125713));
#294939=CARTESIAN_POINT('Ctrl Pts',(-8.60118818499316E-14,131.056249999486,
10.5687124469213));
#294940=CARTESIAN_POINT('Ctrl Pts',(3.10606665601002,131.206249999486,9.5594902125713));
#294941=CARTESIAN_POINT('Ctrl Pts',(6.21213331202013,131.356249999485,8.55026797822134));
#294942=CARTESIAN_POINT('Ctrl Pts',(8.1317880767571,131.506249999484,5.90808986649102));
#294943=CARTESIAN_POINT('Ctrl Pts',(10.0514428414941,131.656249999484,3.2659117547607));
#294944=CARTESIAN_POINT('Ctrl Pts',(10.0514428414941,131.806249999483,-1.23094673026484E-15));
#294945=CARTESIAN_POINT('Ctrl Pts',(10.0514428414941,131.956249999483,-3.26591175476071));
#294946=CARTESIAN_POINT('Ctrl Pts',(8.1317880767571,132.106249999482,-5.90808986649102));
#294947=CARTESIAN_POINT('Ctrl Pts',(6.21213331202012,132.256249999481,-8.55026797822134));
#294948=CARTESIAN_POINT('Ctrl Pts',(3.10606665601002,132.406249999481,-9.5594902125713));
#294949=CARTESIAN_POINT('Ctrl Pts',(-8.94643244596087E-14,132.55624999948,
-10.5687124469213));
#294950=CARTESIAN_POINT('Ctrl Pts',(-3.1060666560102,132.70624999948,-9.5594902125713));
#294951=CARTESIAN_POINT('Ctrl Pts',(-6.2121333120203,132.856249999479,-8.55026797822134));
#294952=CARTESIAN_POINT('Ctrl Pts',(-8.13178807675728,133.006249999478,
-5.90808986649102));
#294953=CARTESIAN_POINT('Ctrl Pts',(-10.0514428414943,133.156249999478,
-3.2659117547607));
#294954=CARTESIAN_POINT('Ctrl Pts',(-10.0514428414943,133.306249999477,
2.46189346052968E-15));
#294955=CARTESIAN_POINT('Ctrl Pts',(-10.0514428414943,133.456249999477,
3.26591175476071));
#294956=CARTESIAN_POINT('Ctrl Pts',(-8.13178807675728,133.606249999476,
5.90808986649102));
#294957=CARTESIAN_POINT('Ctrl Pts',(-6.2121333120203,133.756249999475,8.55026797822134));
#294958=CARTESIAN_POINT('Ctrl Pts',(-3.1060666560102,133.906249999475,9.5594902125713));
#294959=CARTESIAN_POINT('Ctrl Pts',(-8.77395911215934E-14,134.056249999474,
10.5687124469213));
#294960=CARTESIAN_POINT('Ctrl Pts',(3.10606665601002,134.206249999474,9.5594902125713));
#294961=CARTESIAN_POINT('Ctrl Pts',(6.21213331202013,134.356249999473,8.55026797822134));
#294962=CARTESIAN_POINT('Ctrl Pts',(8.1317880767571,134.506249999472,5.90808986649102));
#294963=CARTESIAN_POINT('Ctrl Pts',(10.0514428414941,134.656249999472,3.2659117547607));
#294964=CARTESIAN_POINT('Ctrl Pts',(10.0514428414941,134.806249999471,-1.23094673026484E-15));
#294965=CARTESIAN_POINT('Ctrl Pts',(10.0514428414941,134.956249999471,-3.26591175476071));
#294966=CARTESIAN_POINT('Ctrl Pts',(8.1317880767571,135.10624999947,-5.90808986649102));
#294967=CARTESIAN_POINT('Ctrl Pts',(6.21213331202012,135.256249999469,-8.55026797822134));
#294968=CARTESIAN_POINT('Ctrl Pts',(3.10606665601002,135.406249999469,-9.5594902125713));
#294969=CARTESIAN_POINT('Ctrl Pts',(-9.11920337312706E-14,135.556249999468,
-10.5687124469213));
#294970=CARTESIAN_POINT('Ctrl Pts',(-3.1060666560102,135.706249999468,-9.5594902125713));
#294971=CARTESIAN_POINT('Ctrl Pts',(-6.21213331202031,135.856249999467,
-8.55026797822134));
#294972=CARTESIAN_POINT('Ctrl Pts',(-8.13178807675728,136.006249999466,
-5.90808986649102));
#294973=CARTESIAN_POINT('Ctrl Pts',(-10.0514428414943,136.156249999466,
-3.2659117547607));
#294974=CARTESIAN_POINT('Ctrl Pts',(-10.0514428414943,136.306249999465,
2.46189346052968E-15));
#294975=CARTESIAN_POINT('Ctrl Pts',(-10.0514428414943,136.456249999465,
3.26591175476071));
#294976=CARTESIAN_POINT('Ctrl Pts',(-8.13178807675728,136.606249999464,
5.90808986649102));
#294977=CARTESIAN_POINT('Ctrl Pts',(-6.2121333120203,136.756249999463,8.55026797822134));
#294978=CARTESIAN_POINT('Ctrl Pts',(-3.1060666560102,136.906249999463,9.5594902125713));
#294979=CARTESIAN_POINT('Ctrl Pts',(-8.94673003932553E-14,137.056249999462,
10.5687124469213));
#294980=CARTESIAN_POINT('Ctrl Pts',(3.10606665601002,137.206249999462,9.5594902125713));
#294981=CARTESIAN_POINT('Ctrl Pts',(6.21213331202012,137.356249999461,8.55026797822134));
#294982=CARTESIAN_POINT('Ctrl Pts',(8.1317880767571,137.50624999946,5.90808986649102));
#294983=CARTESIAN_POINT('Ctrl Pts',(10.0514428414941,137.65624999946,3.2659117547607));
#294984=CARTESIAN_POINT('Ctrl Pts',(10.0514428414941,137.806249999459,-1.23094673026484E-15));
#294985=CARTESIAN_POINT('Ctrl Pts',(10.0514428414941,137.956249999459,-3.26591175476071));
#294986=CARTESIAN_POINT('Ctrl Pts',(8.1317880767571,138.106249999458,-5.90808986649102));
#294987=CARTESIAN_POINT('Ctrl Pts',(6.21213331202012,138.256249999457,-8.55026797822134));
#294988=CARTESIAN_POINT('Ctrl Pts',(3.10606665601001,138.406249999457,-9.5594902125713));
#294989=CARTESIAN_POINT('Ctrl Pts',(-9.29197430029324E-14,138.556249999456,
-10.5687124469213));
#294990=CARTESIAN_POINT('Ctrl Pts',(-3.1060666560102,138.706249999456,-9.5594902125713));
#294991=CARTESIAN_POINT('Ctrl Pts',(-6.21213331202031,138.856249999455,
-8.55026797822134));
#294992=CARTESIAN_POINT('Ctrl Pts',(-8.13178807675728,139.006249999454,
-5.90808986649102));
#294993=CARTESIAN_POINT('Ctrl Pts',(-10.0514428414943,139.156249999454,
-3.2659117547607));
#294994=CARTESIAN_POINT('Ctrl Pts',(-10.0514428414943,139.306249999453,
2.46189346052968E-15));
#294995=CARTESIAN_POINT('Ctrl Pts',(-10.0514428414943,139.456249999453,
3.26591175476071));
#294996=CARTESIAN_POINT('Ctrl Pts',(-8.13178807675728,139.606249999452,
5.90808986649102));
#294997=CARTESIAN_POINT('Ctrl Pts',(-6.21213331202031,139.756249999451,
8.55026797822134));
#294998=CARTESIAN_POINT('Ctrl Pts',(-3.1060666560102,139.906249999451,9.5594902125713));
#294999=CARTESIAN_POINT('Ctrl Pts',(-9.11950096649171E-14,140.05624999945,
10.5687124469213));
#295000=CARTESIAN_POINT('Ctrl Pts',(3.10606665601002,140.20624999945,9.5594902125713));
#295001=CARTESIAN_POINT('Ctrl Pts',(6.21213331202012,140.356249999449,8.55026797822134));
#295002=CARTESIAN_POINT('Ctrl Pts',(8.1317880767571,140.506249999448,5.90808986649102));
#295003=CARTESIAN_POINT('Ctrl Pts',(10.0514428414941,140.656249999448,3.2659117547607));
#295004=CARTESIAN_POINT('Ctrl Pts',(10.0514428414941,140.806249999447,-1.23094673026484E-15));
#295005=CARTESIAN_POINT('Ctrl Pts',(10.0514428414941,140.956249999447,-3.26591175476071));
#295006=CARTESIAN_POINT('Ctrl Pts',(8.1317880767571,141.106249999446,-5.90808986649102));
#295007=CARTESIAN_POINT('Ctrl Pts',(6.21213331202012,141.256249999445,-8.55026797822134));
#295008=CARTESIAN_POINT('Ctrl Pts',(3.10606665601001,141.406249999445,-9.5594902125713));
#295009=CARTESIAN_POINT('Ctrl Pts',(-9.46474522745942E-14,141.556249999444,
-10.5687124469213));
#295010=CARTESIAN_POINT('Ctrl Pts',(-3.1060666560102,141.706249999444,-9.5594902125713));
#295011=CARTESIAN_POINT('Ctrl Pts',(-6.21213331202031,141.856249999443,
-8.55026797822134));
#295012=CARTESIAN_POINT('Ctrl Pts',(-8.13178807675729,142.006249999442,
-5.90808986649102));
#295013=CARTESIAN_POINT('Ctrl Pts',(-10.0514428414943,142.156249999442,
-3.2659117547607));
#295014=CARTESIAN_POINT('Ctrl Pts',(-10.0514428414943,142.306249999441,
2.46189346052968E-15));
#295015=CARTESIAN_POINT('Ctrl Pts',(-10.0514428414943,142.456249999441,
3.26591175476071));
#295016=CARTESIAN_POINT('Ctrl Pts',(-8.13178807675729,142.60624999944,5.90808986649102));
#295017=CARTESIAN_POINT('Ctrl Pts',(-6.21213331202031,142.756249999439,
8.55026797822134));
#295018=CARTESIAN_POINT('Ctrl Pts',(-3.1060666560102,142.906249999439,9.5594902125713));
#295019=CARTESIAN_POINT('Ctrl Pts',(-9.29227189365789E-14,143.056249999438,
10.5687124469213));
#295020=CARTESIAN_POINT('Ctrl Pts',(3.10606665601001,143.206249999438,9.5594902125713));
#295021=CARTESIAN_POINT('Ctrl Pts',(6.21213331202012,143.356249999437,8.55026797822134));
#295022=CARTESIAN_POINT('Ctrl Pts',(8.1317880767571,143.506249999436,5.90808986649102));
#295023=CARTESIAN_POINT('Ctrl Pts',(10.0514428414941,143.656249999436,3.2659117547607));
#295024=CARTESIAN_POINT('Ctrl Pts',(10.0514428414941,143.806249999435,-1.23094673026484E-15));
#295025=CARTESIAN_POINT('Ctrl Pts',(10.0514428414941,143.956249999435,-3.26591175476071));
#295026=CARTESIAN_POINT('Ctrl Pts',(8.1317880767571,144.106249999434,-5.90808986649102));
#295027=CARTESIAN_POINT('Ctrl Pts',(6.21213331202012,144.256249999433,-8.55026797822134));
#295028=CARTESIAN_POINT('Ctrl Pts',(3.10606665601001,144.406249999433,-9.5594902125713));
#295029=CARTESIAN_POINT('Ctrl Pts',(-9.63751615462561E-14,144.556249999432,
-10.5687124469213));
#295030=CARTESIAN_POINT('Ctrl Pts',(-3.1060666560102,144.706249999432,-9.5594902125713));
#295031=CARTESIAN_POINT('Ctrl Pts',(-6.21213331202031,144.856249999431,
-8.55026797822134));
#295032=CARTESIAN_POINT('Ctrl Pts',(-8.13178807675729,145.00624999943,-5.90808986649102));
#295033=CARTESIAN_POINT('Ctrl Pts',(-10.0514428414943,145.15624999943,-3.2659117547607));
#295034=CARTESIAN_POINT('Ctrl Pts',(-10.0514428414943,145.306249999429,
2.46189346052968E-15));
#295035=CARTESIAN_POINT('Ctrl Pts',(-10.0514428414943,145.456249999429,
3.26591175476071));
#295036=CARTESIAN_POINT('Ctrl Pts',(-8.13178807675729,145.606249999428,
5.90808986649102));
#295037=CARTESIAN_POINT('Ctrl Pts',(-6.21213331202031,145.756249999427,
8.55026797822134));
#295038=CARTESIAN_POINT('Ctrl Pts',(-3.1060666560102,145.906249999427,9.5594902125713));
#295039=CARTESIAN_POINT('Ctrl Pts',(-9.46504282082408E-14,146.056249999426,
10.5687124469213));
#295040=CARTESIAN_POINT('Ctrl Pts',(3.10606665601001,146.206249999426,9.5594902125713));
#295041=CARTESIAN_POINT('Ctrl Pts',(6.21213331202012,146.356249999425,8.55026797822134));
#295042=CARTESIAN_POINT('Ctrl Pts',(8.13178807675709,146.506249999424,5.90808986649102));
#295043=CARTESIAN_POINT('Ctrl Pts',(10.0514428414941,146.656249999424,3.2659117547607));
#295044=CARTESIAN_POINT('Ctrl Pts',(10.0514428414941,146.806249999423,-1.23094673026484E-15));
#295045=CARTESIAN_POINT('Ctrl Pts',(10.0514428414941,146.956249999423,-3.26591175476071));
#295046=CARTESIAN_POINT('Ctrl Pts',(8.13178807675709,147.106249999422,-5.90808986649102));
#295047=CARTESIAN_POINT('Ctrl Pts',(6.21213331202012,147.256249999421,-8.55026797822134));
#295048=CARTESIAN_POINT('Ctrl Pts',(3.10606665601001,147.406249999421,-9.5594902125713));
#295049=CARTESIAN_POINT('Ctrl Pts',(-9.81028708179179E-14,147.55624999942,
-10.5687124469213));
#295050=CARTESIAN_POINT('Ctrl Pts',(-3.10606665601021,147.70624999942,-9.5594902125713));
#295051=CARTESIAN_POINT('Ctrl Pts',(-6.21213331202032,147.856249999419,
-8.55026797822134));
#295052=CARTESIAN_POINT('Ctrl Pts',(-8.13178807675729,148.006249999418,
-5.90808986649102));
#295053=CARTESIAN_POINT('Ctrl Pts',(-10.0514428414943,148.156249999418,
-3.2659117547607));
#295054=CARTESIAN_POINT('Ctrl Pts',(-10.0514428414943,148.306249999417,
2.46189346052968E-15));
#295055=CARTESIAN_POINT('Ctrl Pts',(-10.0514428414943,148.456249999417,
3.26591175476071));
#295056=CARTESIAN_POINT('Ctrl Pts',(-8.13178807675729,148.606249999416,
5.90808986649102));
#295057=CARTESIAN_POINT('Ctrl Pts',(-6.21213331202031,148.756249999415,
8.55026797822134));
#295058=CARTESIAN_POINT('Ctrl Pts',(-3.1060666560102,148.906249999415,9.5594902125713));
#295059=CARTESIAN_POINT('Ctrl Pts',(-9.63781374799026E-14,149.056249999414,
10.5687124469213));
#295060=CARTESIAN_POINT('Ctrl Pts',(3.10606665601001,149.206249999414,9.5594902125713));
#295061=CARTESIAN_POINT('Ctrl Pts',(6.21213331202012,149.356249999413,8.55026797822134));
#295062=CARTESIAN_POINT('Ctrl Pts',(8.13178807675709,149.506249999412,5.90808986649102));
#295063=CARTESIAN_POINT('Ctrl Pts',(10.0514428414941,149.656249999412,3.2659117547607));
#295064=CARTESIAN_POINT('Ctrl Pts',(10.0514428414941,149.806249999411,-1.23094673026484E-15));
#295065=CARTESIAN_POINT('Ctrl Pts',(10.0514428414941,149.956249999411,-3.26591175476071));
#295066=CARTESIAN_POINT('Ctrl Pts',(8.13178807675709,150.10624999941,-5.90808986649102));
#295067=CARTESIAN_POINT('Ctrl Pts',(6.21213331202012,150.256249999409,-8.55026797822134));
#295068=CARTESIAN_POINT('Ctrl Pts',(3.10606665601001,150.406249999409,-9.5594902125713));
#295069=CARTESIAN_POINT('Ctrl Pts',(-9.98305800895797E-14,150.556249999408,
-10.5687124469213));
#295070=CARTESIAN_POINT('Ctrl Pts',(-3.10606665601021,150.706249999408,
-9.5594902125713));
#295071=CARTESIAN_POINT('Ctrl Pts',(-6.21213331202032,150.856249999407,
-8.55026797822134));
#295072=CARTESIAN_POINT('Ctrl Pts',(-8.13178807675729,151.006249999406,
-5.90808986649102));
#295073=CARTESIAN_POINT('Ctrl Pts',(-10.0514428414943,151.156249999406,
-3.2659117547607));
#295074=CARTESIAN_POINT('Ctrl Pts',(-10.0514428414943,151.306249999405,
2.46189346052968E-15));
#295075=CARTESIAN_POINT('Ctrl Pts',(-10.0514428414943,151.456249999405,
3.26591175476071));
#295076=CARTESIAN_POINT('Ctrl Pts',(-8.13178807675729,151.606249999404,
5.90808986649102));
#295077=CARTESIAN_POINT('Ctrl Pts',(-6.21213331202032,151.756249999403,
8.55026797822134));
#295078=CARTESIAN_POINT('Ctrl Pts',(-3.10606665601021,151.906249999403,
9.5594902125713));
#295079=CARTESIAN_POINT('Ctrl Pts',(-9.81058467515645E-14,152.056249999402,
10.5687124469213));
#295080=CARTESIAN_POINT('Ctrl Pts',(3.10606665601001,152.206249999402,9.5594902125713));
#295081=CARTESIAN_POINT('Ctrl Pts',(6.21213331202012,152.356249999401,8.55026797822134));
#295082=CARTESIAN_POINT('Ctrl Pts',(8.13178807675709,152.5062499994,5.90808986649102));
#295083=CARTESIAN_POINT('Ctrl Pts',(10.0514428414941,152.6562499994,3.2659117547607));
#295084=CARTESIAN_POINT('Ctrl Pts',(10.0514428414941,152.806249999399,-1.23094673026484E-15));
#295085=CARTESIAN_POINT('Ctrl Pts',(10.0514428414941,152.956249999399,-3.26591175476071));
#295086=CARTESIAN_POINT('Ctrl Pts',(8.13178807675709,153.106249999398,-5.90808986649102));
#295087=CARTESIAN_POINT('Ctrl Pts',(6.21213331202012,153.256249999397,-8.55026797822134));
#295088=CARTESIAN_POINT('Ctrl Pts',(3.10606665601001,153.406249999397,-9.5594902125713));
#295089=CARTESIAN_POINT('Ctrl Pts',(-1.01558289361242E-13,153.556249999396,
-10.5687124469213));
#295090=CARTESIAN_POINT('Ctrl Pts',(-3.10606665601021,153.706249999396,
-9.5594902125713));
#295091=CARTESIAN_POINT('Ctrl Pts',(-12.1623797632097,-0.474999999988005,
2.97892388940585E-15));
#295092=CARTESIAN_POINT('Ctrl Pts',(-12.1623797632096,-0.324999999988605,
3.95179673813133));
#295093=CARTESIAN_POINT('Ctrl Pts',(-9.83957192047856,-0.174999999989203,
7.14886745759505));
#295094=CARTESIAN_POINT('Ctrl Pts',(-7.51676407774747,-0.0249999999898023,
10.3459381770588));
#295095=CARTESIAN_POINT('Ctrl Pts',(-3.75838203887374,0.1250000000096,11.5671105274568));
#295096=CARTESIAN_POINT('Ctrl Pts',(-1.02868273148643E-14,0.275000000009002,
12.7882828778549));
#295097=CARTESIAN_POINT('Ctrl Pts',(3.75838203887372,0.425000000008404,
11.5671105274568));
#295098=CARTESIAN_POINT('Ctrl Pts',(7.51676407774745,0.575000000007806,
10.3459381770588));
#295099=CARTESIAN_POINT('Ctrl Pts',(9.83957192047854,0.725000000007208,
7.14886745759505));
#295100=CARTESIAN_POINT('Ctrl Pts',(12.1623797632096,0.875000000006609,
3.95179673813132));
#295101=CARTESIAN_POINT('Ctrl Pts',(12.1623797632096,1.02500000000601,-1.48946194470292E-15));
#295102=CARTESIAN_POINT('Ctrl Pts',(12.1623797632096,1.17500000000541,-3.95179673813132));
#295103=CARTESIAN_POINT('Ctrl Pts',(9.83957192047853,1.32500000000481,-7.14886745759505));
#295104=CARTESIAN_POINT('Ctrl Pts',(7.51676407774744,1.47500000000421,-10.3459381770588));
#295105=CARTESIAN_POINT('Ctrl Pts',(3.75838203887371,1.6250000000036,-11.5671105274568));
#295106=CARTESIAN_POINT('Ctrl Pts',(-1.42829078892864E-14,1.775000000003,
-12.7882828778549));
#295107=CARTESIAN_POINT('Ctrl Pts',(-3.75838203887374,1.9250000000024,-11.5671105274568));
#295108=CARTESIAN_POINT('Ctrl Pts',(-7.51676407774747,2.0750000000018,-10.3459381770588));
#295109=CARTESIAN_POINT('Ctrl Pts',(-9.83957192047856,2.2250000000012,-7.14886745759505));
#295110=CARTESIAN_POINT('Ctrl Pts',(-12.1623797632097,2.37500000000059,
-3.95179673813132));
#295111=CARTESIAN_POINT('Ctrl Pts',(-12.1623797632097,2.525,2.97892388940585E-15));
#295112=CARTESIAN_POINT('Ctrl Pts',(-12.1623797632097,2.6749999999994,3.95179673813133));
#295113=CARTESIAN_POINT('Ctrl Pts',(-9.83957192047856,2.8249999999988,7.14886745759505));
#295114=CARTESIAN_POINT('Ctrl Pts',(-7.51676407774747,2.9749999999982,10.3459381770588));
#295115=CARTESIAN_POINT('Ctrl Pts',(-3.75838203887374,3.1249999999976,11.5671105274568));
#295116=CARTESIAN_POINT('Ctrl Pts',(-1.20145365865262E-14,3.274999999997,
12.7882828778549));
#295117=CARTESIAN_POINT('Ctrl Pts',(3.75838203887372,3.4249999999964,11.5671105274568));
#295118=CARTESIAN_POINT('Ctrl Pts',(7.51676407774744,3.57499999999581,10.3459381770588));
#295119=CARTESIAN_POINT('Ctrl Pts',(9.83957192047853,3.72499999999521,7.14886745759505));
#295120=CARTESIAN_POINT('Ctrl Pts',(12.1623797632096,3.87499999999461,3.95179673813132));
#295121=CARTESIAN_POINT('Ctrl Pts',(12.1623797632096,4.02499999999401,-1.48946194470292E-15));
#295122=CARTESIAN_POINT('Ctrl Pts',(12.1623797632096,4.17499999999341,-3.95179673813132));
#295123=CARTESIAN_POINT('Ctrl Pts',(9.83957192047853,4.32499999999281,-7.14886745759505));
#295124=CARTESIAN_POINT('Ctrl Pts',(7.51676407774744,4.47499999999221,-10.3459381770588));
#295125=CARTESIAN_POINT('Ctrl Pts',(3.75838203887371,4.6249999999916,-11.5671105274568));
#295126=CARTESIAN_POINT('Ctrl Pts',(-1.60106171609483E-14,4.774999999991,
-12.7882828778549));
#295127=CARTESIAN_POINT('Ctrl Pts',(-3.75838203887374,4.9249999999904,-11.5671105274568));
#295128=CARTESIAN_POINT('Ctrl Pts',(-7.51676407774747,5.0749999999898,-10.3459381770588));
#295129=CARTESIAN_POINT('Ctrl Pts',(-9.83957192047857,5.2249999999892,-7.14886745759505));
#295130=CARTESIAN_POINT('Ctrl Pts',(-12.1623797632097,5.3749999999886,-3.95179673813132));
#295131=CARTESIAN_POINT('Ctrl Pts',(-12.1623797632097,5.52499999998799,
2.97892388940585E-15));
#295132=CARTESIAN_POINT('Ctrl Pts',(-12.1623797632097,5.6749999999874,3.95179673813133));
#295133=CARTESIAN_POINT('Ctrl Pts',(-9.83957192047857,5.8249999999868,7.14886745759505));
#295134=CARTESIAN_POINT('Ctrl Pts',(-7.51676407774747,5.9749999999862,10.3459381770588));
#295135=CARTESIAN_POINT('Ctrl Pts',(-3.75838203887374,6.1249999999856,11.5671105274568));
#295136=CARTESIAN_POINT('Ctrl Pts',(-1.3742245858188E-14,6.274999999985,
12.7882828778549));
#295137=CARTESIAN_POINT('Ctrl Pts',(3.75838203887371,6.4249999999844,11.5671105274568));
#295138=CARTESIAN_POINT('Ctrl Pts',(7.51676407774744,6.57499999998381,10.3459381770588));
#295139=CARTESIAN_POINT('Ctrl Pts',(9.83957192047853,6.72499999998321,7.14886745759505));
#295140=CARTESIAN_POINT('Ctrl Pts',(12.1623797632096,6.87499999998261,3.95179673813132));
#295141=CARTESIAN_POINT('Ctrl Pts',(12.1623797632096,7.02499999998201,-1.48946194470292E-15));
#295142=CARTESIAN_POINT('Ctrl Pts',(12.1623797632096,7.17499999998141,-3.95179673813132));
#295143=CARTESIAN_POINT('Ctrl Pts',(9.83957192047853,7.32499999998081,-7.14886745759505));
#295144=CARTESIAN_POINT('Ctrl Pts',(7.51676407774744,7.47499999998021,-10.3459381770588));
#295145=CARTESIAN_POINT('Ctrl Pts',(3.75838203887371,7.6249999999796,-11.5671105274568));
#295146=CARTESIAN_POINT('Ctrl Pts',(-1.77383264326101E-14,7.774999999979,
-12.7882828778549));
#295147=CARTESIAN_POINT('Ctrl Pts',(-3.75838203887375,7.9249999999784,-11.5671105274568));
#295148=CARTESIAN_POINT('Ctrl Pts',(-7.51676407774747,8.0749999999778,-10.3459381770588));
#295149=CARTESIAN_POINT('Ctrl Pts',(-9.83957192047857,8.2249999999772,-7.14886745759505));
#295150=CARTESIAN_POINT('Ctrl Pts',(-12.1623797632097,8.3749999999766,-3.95179673813132));
#295151=CARTESIAN_POINT('Ctrl Pts',(-12.1623797632097,8.52499999997599,
2.97892388940585E-15));
#295152=CARTESIAN_POINT('Ctrl Pts',(-12.1623797632097,8.6749999999754,3.95179673813133));
#295153=CARTESIAN_POINT('Ctrl Pts',(-9.83957192047857,8.8249999999748,7.14886745759505));
#295154=CARTESIAN_POINT('Ctrl Pts',(-7.51676407774747,8.9749999999742,10.3459381770588));
#295155=CARTESIAN_POINT('Ctrl Pts',(-3.75838203887374,9.1249999999736,11.5671105274568));
#295156=CARTESIAN_POINT('Ctrl Pts',(-1.54699551298498E-14,9.274999999973,
12.7882828778549));
#295157=CARTESIAN_POINT('Ctrl Pts',(3.75838203887371,9.4249999999724,11.5671105274568));
#295158=CARTESIAN_POINT('Ctrl Pts',(7.51676407774744,9.57499999997181,10.3459381770588));
#295159=CARTESIAN_POINT('Ctrl Pts',(9.83957192047853,9.72499999997121,7.14886745759505));
#295160=CARTESIAN_POINT('Ctrl Pts',(12.1623797632096,9.87499999997061,3.95179673813132));
#295161=CARTESIAN_POINT('Ctrl Pts',(12.1623797632096,10.02499999997,-1.48946194470292E-15));
#295162=CARTESIAN_POINT('Ctrl Pts',(12.1623797632096,10.1749999999694,-3.95179673813132));
#295163=CARTESIAN_POINT('Ctrl Pts',(9.83957192047853,10.3249999999688,-7.14886745759505));
#295164=CARTESIAN_POINT('Ctrl Pts',(7.51676407774744,10.4749999999682,-10.3459381770588));
#295165=CARTESIAN_POINT('Ctrl Pts',(3.75838203887371,10.6249999999676,-11.5671105274568));
#295166=CARTESIAN_POINT('Ctrl Pts',(-1.9466035704272E-14,10.774999999967,
-12.7882828778549));
#295167=CARTESIAN_POINT('Ctrl Pts',(-3.75838203887375,10.9249999999664,
-11.5671105274568));
#295168=CARTESIAN_POINT('Ctrl Pts',(-7.51676407774748,11.0749999999658,
-10.3459381770588));
#295169=CARTESIAN_POINT('Ctrl Pts',(-9.83957192047857,11.2249999999652,
-7.14886745759505));
#295170=CARTESIAN_POINT('Ctrl Pts',(-12.1623797632097,11.3749999999646,
-3.95179673813132));
#295171=CARTESIAN_POINT('Ctrl Pts',(-12.1623797632097,11.524999999964,2.97892388940585E-15));
#295172=CARTESIAN_POINT('Ctrl Pts',(-12.1623797632097,11.6749999999634,
3.95179673813133));
#295173=CARTESIAN_POINT('Ctrl Pts',(-9.83957192047857,11.8249999999628,
7.14886745759505));
#295174=CARTESIAN_POINT('Ctrl Pts',(-7.51676407774747,11.9749999999622,
10.3459381770588));
#295175=CARTESIAN_POINT('Ctrl Pts',(-3.75838203887375,12.1249999999616,
11.5671105274568));
#295176=CARTESIAN_POINT('Ctrl Pts',(-1.71976644015117E-14,12.274999999961,
12.7882828778549));
#295177=CARTESIAN_POINT('Ctrl Pts',(3.75838203887371,12.4249999999604,11.5671105274568));
#295178=CARTESIAN_POINT('Ctrl Pts',(7.51676407774744,12.5749999999598,10.3459381770588));
#295179=CARTESIAN_POINT('Ctrl Pts',(9.83957192047853,12.7249999999592,7.14886745759505));
#295180=CARTESIAN_POINT('Ctrl Pts',(12.1623797632096,12.8749999999586,3.95179673813132));
#295181=CARTESIAN_POINT('Ctrl Pts',(12.1623797632096,13.024999999958,-1.48946194470292E-15));
#295182=CARTESIAN_POINT('Ctrl Pts',(12.1623797632096,13.1749999999574,-3.95179673813132));
#295183=CARTESIAN_POINT('Ctrl Pts',(9.83957192047853,13.3249999999568,-7.14886745759505));
#295184=CARTESIAN_POINT('Ctrl Pts',(7.51676407774743,13.4749999999562,-10.3459381770588));
#295185=CARTESIAN_POINT('Ctrl Pts',(3.75838203887371,13.6249999999556,-11.5671105274568));
#295186=CARTESIAN_POINT('Ctrl Pts',(-2.11937449759338E-14,13.774999999955,
-12.7882828778549));
#295187=CARTESIAN_POINT('Ctrl Pts',(-3.75838203887375,13.9249999999544,
-11.5671105274568));
#295188=CARTESIAN_POINT('Ctrl Pts',(-7.51676407774748,14.0749999999538,
-10.3459381770588));
#295189=CARTESIAN_POINT('Ctrl Pts',(-9.83957192047857,14.2249999999532,
-7.14886745759505));
#295190=CARTESIAN_POINT('Ctrl Pts',(-12.1623797632097,14.3749999999526,
-3.95179673813132));
#295191=CARTESIAN_POINT('Ctrl Pts',(-12.1623797632097,14.524999999952,2.97892388940585E-15));
#295192=CARTESIAN_POINT('Ctrl Pts',(-12.1623797632097,14.6749999999514,
3.95179673813133));
#295193=CARTESIAN_POINT('Ctrl Pts',(-9.83957192047857,14.8249999999508,
7.14886745759505));
#295194=CARTESIAN_POINT('Ctrl Pts',(-7.51676407774747,14.9749999999502,
10.3459381770588));
#295195=CARTESIAN_POINT('Ctrl Pts',(-3.75838203887375,15.1249999999496,
11.5671105274568));
#295196=CARTESIAN_POINT('Ctrl Pts',(-1.89253736731735E-14,15.274999999949,
12.7882828778549));
#295197=CARTESIAN_POINT('Ctrl Pts',(3.75838203887371,15.4249999999484,11.5671105274568));
#295198=CARTESIAN_POINT('Ctrl Pts',(7.51676407774744,15.5749999999478,10.3459381770588));
#295199=CARTESIAN_POINT('Ctrl Pts',(9.83957192047853,15.7249999999472,7.14886745759505));
#295200=CARTESIAN_POINT('Ctrl Pts',(12.1623797632096,15.8749999999466,3.95179673813132));
#295201=CARTESIAN_POINT('Ctrl Pts',(12.1623797632096,16.024999999946,-1.48946194470292E-15));
#295202=CARTESIAN_POINT('Ctrl Pts',(12.1623797632096,16.1749999999454,-3.95179673813132));
#295203=CARTESIAN_POINT('Ctrl Pts',(9.83957192047852,16.3249999999448,-7.14886745759505));
#295204=CARTESIAN_POINT('Ctrl Pts',(7.51676407774743,16.4749999999442,-10.3459381770588));
#295205=CARTESIAN_POINT('Ctrl Pts',(3.7583820388737,16.6249999999436,-11.5671105274568));
#295206=CARTESIAN_POINT('Ctrl Pts',(-2.29214542475956E-14,16.774999999943,
-12.7882828778549));
#295207=CARTESIAN_POINT('Ctrl Pts',(-3.75838203887375,16.9249999999424,
-11.5671105274568));
#295208=CARTESIAN_POINT('Ctrl Pts',(-7.51676407774748,17.0749999999418,
-10.3459381770588));
#295209=CARTESIAN_POINT('Ctrl Pts',(-9.83957192047857,17.2249999999412,
-7.14886745759505));
#295210=CARTESIAN_POINT('Ctrl Pts',(-12.1623797632097,17.3749999999406,
-3.95179673813132));
#295211=CARTESIAN_POINT('Ctrl Pts',(-12.1623797632097,17.52499999994,2.97892388940585E-15));
#295212=CARTESIAN_POINT('Ctrl Pts',(-12.1623797632097,17.6749999999394,
3.95179673813133));
#295213=CARTESIAN_POINT('Ctrl Pts',(-9.83957192047857,17.8249999999388,
7.14886745759505));
#295214=CARTESIAN_POINT('Ctrl Pts',(-7.51676407774748,17.9749999999382,
10.3459381770588));
#295215=CARTESIAN_POINT('Ctrl Pts',(-3.75838203887375,18.1249999999376,
11.5671105274568));
#295216=CARTESIAN_POINT('Ctrl Pts',(-2.06530829448354E-14,18.274999999937,
12.7882828778549));
#295217=CARTESIAN_POINT('Ctrl Pts',(3.75838203887371,18.4249999999364,11.5671105274568));
#295218=CARTESIAN_POINT('Ctrl Pts',(7.51676407774743,18.5749999999358,10.3459381770588));
#295219=CARTESIAN_POINT('Ctrl Pts',(9.83957192047852,18.7249999999352,7.14886745759505));
#295220=CARTESIAN_POINT('Ctrl Pts',(12.1623797632096,18.8749999999346,3.95179673813132));
#295221=CARTESIAN_POINT('Ctrl Pts',(12.1623797632096,19.024999999934,-1.48946194470292E-15));
#295222=CARTESIAN_POINT('Ctrl Pts',(12.1623797632096,19.1749999999334,-3.95179673813132));
#295223=CARTESIAN_POINT('Ctrl Pts',(9.83957192047852,19.3249999999328,-7.14886745759505));
#295224=CARTESIAN_POINT('Ctrl Pts',(7.51676407774743,19.4749999999322,-10.3459381770588));
#295225=CARTESIAN_POINT('Ctrl Pts',(3.7583820388737,19.6249999999316,-11.5671105274568));
#295226=CARTESIAN_POINT('Ctrl Pts',(-2.46491635192575E-14,19.774999999931,
-12.7882828778549));
#295227=CARTESIAN_POINT('Ctrl Pts',(-3.75838203887375,19.9249999999304,
-11.5671105274568));
#295228=CARTESIAN_POINT('Ctrl Pts',(-7.51676407774748,20.0749999999298,
-10.3459381770588));
#295229=CARTESIAN_POINT('Ctrl Pts',(-9.83957192047857,20.2249999999292,
-7.14886745759505));
#295230=CARTESIAN_POINT('Ctrl Pts',(-12.1623797632097,20.3749999999286,
-3.95179673813132));
#295231=CARTESIAN_POINT('Ctrl Pts',(-12.1623797632097,20.524999999928,2.97892388940585E-15));
#295232=CARTESIAN_POINT('Ctrl Pts',(-12.1623797632097,20.6749999999274,
3.95179673813133));
#295233=CARTESIAN_POINT('Ctrl Pts',(-9.83957192047857,20.8249999999268,
7.14886745759505));
#295234=CARTESIAN_POINT('Ctrl Pts',(-7.51676407774748,20.9749999999262,
10.3459381770588));
#295235=CARTESIAN_POINT('Ctrl Pts',(-3.75838203887375,21.1249999999256,
11.5671105274568));
#295236=CARTESIAN_POINT('Ctrl Pts',(-2.23807922164972E-14,21.274999999925,
12.7882828778549));
#295237=CARTESIAN_POINT('Ctrl Pts',(3.7583820388737,21.4249999999244,11.5671105274568));
#295238=CARTESIAN_POINT('Ctrl Pts',(7.51676407774743,21.5749999999238,10.3459381770588));
#295239=CARTESIAN_POINT('Ctrl Pts',(9.83957192047852,21.7249999999232,7.14886745759505));
#295240=CARTESIAN_POINT('Ctrl Pts',(12.1623797632096,21.8749999999226,3.95179673813132));
#295241=CARTESIAN_POINT('Ctrl Pts',(12.1623797632096,22.024999999922,-1.48946194470292E-15));
#295242=CARTESIAN_POINT('Ctrl Pts',(12.1623797632096,22.1749999999214,-3.95179673813132));
#295243=CARTESIAN_POINT('Ctrl Pts',(9.83957192047852,22.3249999999208,-7.14886745759505));
#295244=CARTESIAN_POINT('Ctrl Pts',(7.51676407774743,22.4749999999202,-10.3459381770588));
#295245=CARTESIAN_POINT('Ctrl Pts',(3.7583820388737,22.6249999999196,-11.5671105274568));
#295246=CARTESIAN_POINT('Ctrl Pts',(-2.63768727909193E-14,22.774999999919,
-12.7882828778549));
#295247=CARTESIAN_POINT('Ctrl Pts',(-3.75838203887375,22.9249999999184,
-11.5671105274568));
#295248=CARTESIAN_POINT('Ctrl Pts',(-7.51676407774748,23.0749999999178,
-10.3459381770588));
#295249=CARTESIAN_POINT('Ctrl Pts',(-9.83957192047857,23.2249999999172,
-7.14886745759505));
#295250=CARTESIAN_POINT('Ctrl Pts',(-12.1623797632097,23.3749999999166,
-3.95179673813132));
#295251=CARTESIAN_POINT('Ctrl Pts',(-12.1623797632097,23.524999999916,2.97892388940585E-15));
#295252=CARTESIAN_POINT('Ctrl Pts',(-12.1623797632097,23.6749999999154,
3.95179673813133));
#295253=CARTESIAN_POINT('Ctrl Pts',(-9.83957192047857,23.8249999999148,
7.14886745759505));
#295254=CARTESIAN_POINT('Ctrl Pts',(-7.51676407774748,23.9749999999142,
10.3459381770588));
#295255=CARTESIAN_POINT('Ctrl Pts',(-3.75838203887375,24.1249999999136,
11.5671105274568));
#295256=CARTESIAN_POINT('Ctrl Pts',(-2.4108501488159E-14,24.274999999913,
12.7882828778549));
#295257=CARTESIAN_POINT('Ctrl Pts',(3.7583820388737,24.4249999999124,11.5671105274568));
#295258=CARTESIAN_POINT('Ctrl Pts',(7.51676407774743,24.5749999999118,10.3459381770588));
#295259=CARTESIAN_POINT('Ctrl Pts',(9.83957192047852,24.7249999999112,7.14886745759505));
#295260=CARTESIAN_POINT('Ctrl Pts',(12.1623797632096,24.8749999999106,3.95179673813132));
#295261=CARTESIAN_POINT('Ctrl Pts',(12.1623797632096,25.02499999991,-1.48946194470292E-15));
#295262=CARTESIAN_POINT('Ctrl Pts',(12.1623797632096,25.1749999999094,-3.95179673813132));
#295263=CARTESIAN_POINT('Ctrl Pts',(9.83957192047852,25.3249999999088,-7.14886745759505));
#295264=CARTESIAN_POINT('Ctrl Pts',(7.51676407774743,25.4749999999082,-10.3459381770588));
#295265=CARTESIAN_POINT('Ctrl Pts',(3.7583820388737,25.6249999999076,-11.5671105274568));
#295266=CARTESIAN_POINT('Ctrl Pts',(-2.81045820625811E-14,25.774999999907,
-12.7882828778549));
#295267=CARTESIAN_POINT('Ctrl Pts',(-3.75838203887376,25.9249999999064,
-11.5671105274568));
#295268=CARTESIAN_POINT('Ctrl Pts',(-7.51676407774749,26.0749999999058,
-10.3459381770588));
#295269=CARTESIAN_POINT('Ctrl Pts',(-9.83957192047857,26.2249999999052,
-7.14886745759505));
#295270=CARTESIAN_POINT('Ctrl Pts',(-12.1623797632097,26.3749999999046,
-3.95179673813132));
#295271=CARTESIAN_POINT('Ctrl Pts',(-12.1623797632097,26.524999999904,2.97892388940585E-15));
#295272=CARTESIAN_POINT('Ctrl Pts',(-12.1623797632097,26.6749999999034,
3.95179673813133));
#295273=CARTESIAN_POINT('Ctrl Pts',(-9.83957192047857,26.8249999999028,
7.14886745759505));
#295274=CARTESIAN_POINT('Ctrl Pts',(-7.51676407774748,26.9749999999022,
10.3459381770588));
#295275=CARTESIAN_POINT('Ctrl Pts',(-3.75838203887375,27.1249999999016,
11.5671105274568));
#295276=CARTESIAN_POINT('Ctrl Pts',(-2.58362107598209E-14,27.274999999901,
12.7882828778549));
#295277=CARTESIAN_POINT('Ctrl Pts',(3.7583820388737,27.4249999999004,11.5671105274568));
#295278=CARTESIAN_POINT('Ctrl Pts',(7.51676407774743,27.5749999998998,10.3459381770588));
#295279=CARTESIAN_POINT('Ctrl Pts',(9.83957192047852,27.7249999998992,7.14886745759505));
#295280=CARTESIAN_POINT('Ctrl Pts',(12.1623797632096,27.8749999998986,3.95179673813132));
#295281=CARTESIAN_POINT('Ctrl Pts',(12.1623797632096,28.024999999898,-1.48946194470292E-15));
#295282=CARTESIAN_POINT('Ctrl Pts',(12.1623797632096,28.1749999998974,-3.95179673813132));
#295283=CARTESIAN_POINT('Ctrl Pts',(9.83957192047852,28.3249999998968,-7.14886745759505));
#295284=CARTESIAN_POINT('Ctrl Pts',(7.51676407774743,28.4749999998962,-10.3459381770588));
#295285=CARTESIAN_POINT('Ctrl Pts',(3.7583820388737,28.6249999998956,-11.5671105274568));
#295286=CARTESIAN_POINT('Ctrl Pts',(-2.9832291334243E-14,28.774999999895,
-12.7882828778549));
#295287=CARTESIAN_POINT('Ctrl Pts',(-3.75838203887376,28.9249999998944,
-11.5671105274568));
#295288=CARTESIAN_POINT('Ctrl Pts',(-7.51676407774749,29.0749999998938,
-10.3459381770588));
#295289=CARTESIAN_POINT('Ctrl Pts',(-9.83957192047858,29.2249999998932,
-7.14886745759505));
#295290=CARTESIAN_POINT('Ctrl Pts',(-12.1623797632097,29.3749999998926,
-3.95179673813132));
#295291=CARTESIAN_POINT('Ctrl Pts',(-12.1623797632097,29.524999999892,2.97892388940585E-15));
#295292=CARTESIAN_POINT('Ctrl Pts',(-12.1623797632097,29.6749999998914,
3.95179673813133));
#295293=CARTESIAN_POINT('Ctrl Pts',(-9.83957192047858,29.8249999998908,
7.14886745759505));
#295294=CARTESIAN_POINT('Ctrl Pts',(-7.51676407774748,29.9749999998902,
10.3459381770588));
#295295=CARTESIAN_POINT('Ctrl Pts',(-3.75838203887376,30.1249999998896,
11.5671105274568));
#295296=CARTESIAN_POINT('Ctrl Pts',(-2.75639200314827E-14,30.274999999889,
12.7882828778549));
#295297=CARTESIAN_POINT('Ctrl Pts',(3.7583820388737,30.4249999998884,11.5671105274568));
#295298=CARTESIAN_POINT('Ctrl Pts',(7.51676407774743,30.5749999998878,10.3459381770588));
#295299=CARTESIAN_POINT('Ctrl Pts',(9.83957192047852,30.7249999998872,7.14886745759505));
#295300=CARTESIAN_POINT('Ctrl Pts',(12.1623797632096,30.8749999998866,3.95179673813132));
#295301=CARTESIAN_POINT('Ctrl Pts',(12.1623797632096,31.024999999886,-1.48946194470292E-15));
#295302=CARTESIAN_POINT('Ctrl Pts',(12.1623797632096,31.1749999998854,-3.95179673813132));
#295303=CARTESIAN_POINT('Ctrl Pts',(9.83957192047852,31.3249999998848,-7.14886745759505));
#295304=CARTESIAN_POINT('Ctrl Pts',(7.51676407774742,31.4749999998842,-10.3459381770588));
#295305=CARTESIAN_POINT('Ctrl Pts',(3.7583820388737,31.6249999998836,-11.5671105274568));
#295306=CARTESIAN_POINT('Ctrl Pts',(-3.15600006059048E-14,31.774999999883,
-12.7882828778549));
#295307=CARTESIAN_POINT('Ctrl Pts',(-3.75838203887376,31.9249999998824,
-11.5671105274568));
#295308=CARTESIAN_POINT('Ctrl Pts',(-7.51676407774749,32.0749999998818,
-10.3459381770588));
#295309=CARTESIAN_POINT('Ctrl Pts',(-9.83957192047858,32.2249999998812,
-7.14886745759505));
#295310=CARTESIAN_POINT('Ctrl Pts',(-12.1623797632097,32.3749999998806,
-3.95179673813132));
#295311=CARTESIAN_POINT('Ctrl Pts',(-12.1623797632097,32.52499999988,2.97892388940585E-15));
#295312=CARTESIAN_POINT('Ctrl Pts',(-12.1623797632097,32.6749999998794,
3.95179673813133));
#295313=CARTESIAN_POINT('Ctrl Pts',(-9.83957192047858,32.8249999998788,
7.14886745759505));
#295314=CARTESIAN_POINT('Ctrl Pts',(-7.51676407774749,32.9749999998782,
10.3459381770588));
#295315=CARTESIAN_POINT('Ctrl Pts',(-3.75838203887376,33.1249999998776,
11.5671105274568));
#295316=CARTESIAN_POINT('Ctrl Pts',(-2.92916293031446E-14,33.274999999877,
12.7882828778549));
#295317=CARTESIAN_POINT('Ctrl Pts',(3.7583820388737,33.4249999998764,11.5671105274568));
#295318=CARTESIAN_POINT('Ctrl Pts',(7.51676407774743,33.5749999998758,10.3459381770588));
#295319=CARTESIAN_POINT('Ctrl Pts',(9.83957192047852,33.7249999998752,7.14886745759505));
#295320=CARTESIAN_POINT('Ctrl Pts',(12.1623797632096,33.8749999998746,3.95179673813132));
#295321=CARTESIAN_POINT('Ctrl Pts',(12.1623797632096,34.024999999874,-1.48946194470292E-15));
#295322=CARTESIAN_POINT('Ctrl Pts',(12.1623797632096,34.1749999998734,-3.95179673813132));
#295323=CARTESIAN_POINT('Ctrl Pts',(9.83957192047851,34.3249999998728,-7.14886745759505));
#295324=CARTESIAN_POINT('Ctrl Pts',(7.51676407774742,34.4749999998722,-10.3459381770588));
#295325=CARTESIAN_POINT('Ctrl Pts',(3.7583820388737,34.6249999998716,-11.5671105274568));
#295326=CARTESIAN_POINT('Ctrl Pts',(-3.32877098775667E-14,34.774999999871,
-12.7882828778549));
#295327=CARTESIAN_POINT('Ctrl Pts',(-3.75838203887376,34.9249999998704,
-11.5671105274568));
#295328=CARTESIAN_POINT('Ctrl Pts',(-7.51676407774749,35.0749999998698,
-10.3459381770588));
#295329=CARTESIAN_POINT('Ctrl Pts',(-9.83957192047858,35.2249999998692,
-7.14886745759505));
#295330=CARTESIAN_POINT('Ctrl Pts',(-12.1623797632097,35.3749999998686,
-3.95179673813132));
#295331=CARTESIAN_POINT('Ctrl Pts',(-12.1623797632097,35.524999999868,2.97892388940585E-15));
#295332=CARTESIAN_POINT('Ctrl Pts',(-12.1623797632097,35.6749999998674,
3.95179673813133));
#295333=CARTESIAN_POINT('Ctrl Pts',(-9.83957192047858,35.8249999998668,
7.14886745759505));
#295334=CARTESIAN_POINT('Ctrl Pts',(-7.51676407774749,35.9749999998662,
10.3459381770588));
#295335=CARTESIAN_POINT('Ctrl Pts',(-3.75838203887376,36.1249999998656,
11.5671105274568));
#295336=CARTESIAN_POINT('Ctrl Pts',(-3.10193385748064E-14,36.274999999865,
12.7882828778549));
#295337=CARTESIAN_POINT('Ctrl Pts',(3.7583820388737,36.4249999998644,11.5671105274568));
#295338=CARTESIAN_POINT('Ctrl Pts',(7.51676407774742,36.5749999998638,10.3459381770588));
#295339=CARTESIAN_POINT('Ctrl Pts',(9.83957192047851,36.7249999998632,7.14886745759505));
#295340=CARTESIAN_POINT('Ctrl Pts',(12.1623797632096,36.8749999998626,3.95179673813132));
#295341=CARTESIAN_POINT('Ctrl Pts',(12.1623797632096,37.024999999862,-1.48946194470292E-15));
#295342=CARTESIAN_POINT('Ctrl Pts',(12.1623797632096,37.1749999998614,-3.95179673813132));
#295343=CARTESIAN_POINT('Ctrl Pts',(9.83957192047851,37.3249999998608,-7.14886745759505));
#295344=CARTESIAN_POINT('Ctrl Pts',(7.51676407774742,37.4749999998602,-10.3459381770588));
#295345=CARTESIAN_POINT('Ctrl Pts',(3.75838203887369,37.6249999998596,-11.5671105274568));
#295346=CARTESIAN_POINT('Ctrl Pts',(-3.50154191492285E-14,37.774999999859,
-12.7882828778549));
#295347=CARTESIAN_POINT('Ctrl Pts',(-3.75838203887376,37.9249999998584,
-11.5671105274568));
#295348=CARTESIAN_POINT('Ctrl Pts',(-7.51676407774749,38.0749999998578,
-10.3459381770588));
#295349=CARTESIAN_POINT('Ctrl Pts',(-9.83957192047858,38.2249999998572,
-7.14886745759505));
#295350=CARTESIAN_POINT('Ctrl Pts',(-12.1623797632097,38.3749999998566,
-3.95179673813132));
#295351=CARTESIAN_POINT('Ctrl Pts',(-12.1623797632097,38.524999999856,2.97892388940585E-15));
#295352=CARTESIAN_POINT('Ctrl Pts',(-12.1623797632097,38.6749999998554,
3.95179673813133));
#295353=CARTESIAN_POINT('Ctrl Pts',(-9.83957192047858,38.8249999998548,
7.14886745759505));
#295354=CARTESIAN_POINT('Ctrl Pts',(-7.51676407774749,38.9749999998542,
10.3459381770588));
#295355=CARTESIAN_POINT('Ctrl Pts',(-3.75838203887376,39.1249999998536,
11.5671105274568));
#295356=CARTESIAN_POINT('Ctrl Pts',(-3.27470478464682E-14,39.274999999853,
12.7882828778549));
#295357=CARTESIAN_POINT('Ctrl Pts',(3.7583820388737,39.4249999998524,11.5671105274568));
#295358=CARTESIAN_POINT('Ctrl Pts',(7.51676407774742,39.5749999998518,10.3459381770588));
#295359=CARTESIAN_POINT('Ctrl Pts',(9.83957192047851,39.7249999998512,7.14886745759505));
#295360=CARTESIAN_POINT('Ctrl Pts',(12.1623797632096,39.8749999998506,3.95179673813132));
#295361=CARTESIAN_POINT('Ctrl Pts',(12.1623797632096,40.02499999985,-1.48946194470292E-15));
#295362=CARTESIAN_POINT('Ctrl Pts',(12.1623797632096,40.1749999998494,-3.95179673813132));
#295363=CARTESIAN_POINT('Ctrl Pts',(9.83957192047851,40.3249999998488,-7.14886745759505));
#295364=CARTESIAN_POINT('Ctrl Pts',(7.51676407774742,40.4749999998482,-10.3459381770588));
#295365=CARTESIAN_POINT('Ctrl Pts',(3.75838203887369,40.6249999998476,-11.5671105274568));
#295366=CARTESIAN_POINT('Ctrl Pts',(-3.67431284208903E-14,40.774999999847,
-12.7882828778549));
#295367=CARTESIAN_POINT('Ctrl Pts',(-3.75838203887376,40.9249999998464,
-11.5671105274568));
#295368=CARTESIAN_POINT('Ctrl Pts',(-7.51676407774749,41.0749999998458,
-10.3459381770588));
#295369=CARTESIAN_POINT('Ctrl Pts',(-9.83957192047858,41.2249999998452,
-7.14886745759505));
#295370=CARTESIAN_POINT('Ctrl Pts',(-12.1623797632097,41.3749999998446,
-3.95179673813132));
#295371=CARTESIAN_POINT('Ctrl Pts',(-12.1623797632097,41.524999999844,2.97892388940585E-15));
#295372=CARTESIAN_POINT('Ctrl Pts',(-12.1623797632097,41.6749999998434,
3.95179673813133));
#295373=CARTESIAN_POINT('Ctrl Pts',(-9.83957192047858,41.8249999998428,
7.14886745759505));
#295374=CARTESIAN_POINT('Ctrl Pts',(-7.51676407774749,41.9749999998422,
10.3459381770588));
#295375=CARTESIAN_POINT('Ctrl Pts',(-3.75838203887376,42.1249999998416,
11.5671105274568));
#295376=CARTESIAN_POINT('Ctrl Pts',(-3.44747571181301E-14,42.274999999841,
12.7882828778549));
#295377=CARTESIAN_POINT('Ctrl Pts',(3.75838203887369,42.4249999998404,11.5671105274568));
#295378=CARTESIAN_POINT('Ctrl Pts',(7.51676407774742,42.5749999998398,10.3459381770588));
#295379=CARTESIAN_POINT('Ctrl Pts',(9.83957192047851,42.7249999998392,7.14886745759505));
#295380=CARTESIAN_POINT('Ctrl Pts',(12.1623797632096,42.8749999998386,3.95179673813132));
#295381=CARTESIAN_POINT('Ctrl Pts',(12.1623797632096,43.024999999838,-1.48946194470292E-15));
#295382=CARTESIAN_POINT('Ctrl Pts',(12.1623797632096,43.1749999998374,-3.95179673813132));
#295383=CARTESIAN_POINT('Ctrl Pts',(9.83957192047851,43.3249999998368,-7.14886745759505));
#295384=CARTESIAN_POINT('Ctrl Pts',(7.51676407774742,43.4749999998362,-10.3459381770588));
#295385=CARTESIAN_POINT('Ctrl Pts',(3.75838203887369,43.6249999998356,-11.5671105274568));
#295386=CARTESIAN_POINT('Ctrl Pts',(-3.84708376925522E-14,43.774999999835,
-12.7882828778549));
#295387=CARTESIAN_POINT('Ctrl Pts',(-3.75838203887377,43.9249999998344,
-11.5671105274568));
#295388=CARTESIAN_POINT('Ctrl Pts',(-7.51676407774749,44.0749999998338,
-10.3459381770588));
#295389=CARTESIAN_POINT('Ctrl Pts',(-9.83957192047859,44.2249999998332,
-7.14886745759505));
#295390=CARTESIAN_POINT('Ctrl Pts',(-12.1623797632097,44.3749999998326,
-3.95179673813132));
#295391=CARTESIAN_POINT('Ctrl Pts',(-12.1623797632097,44.524999999832,2.97892388940585E-15));
#295392=CARTESIAN_POINT('Ctrl Pts',(-12.1623797632097,44.6749999998314,
3.95179673813133));
#295393=CARTESIAN_POINT('Ctrl Pts',(-9.83957192047859,44.8249999998308,
7.14886745759505));
#295394=CARTESIAN_POINT('Ctrl Pts',(-7.51676407774749,44.9749999998302,
10.3459381770588));
#295395=CARTESIAN_POINT('Ctrl Pts',(-3.75838203887376,45.1249999998296,
11.5671105274568));
#295396=CARTESIAN_POINT('Ctrl Pts',(-3.62024663897919E-14,45.274999999829,
12.7882828778549));
#295397=CARTESIAN_POINT('Ctrl Pts',(3.75838203887369,45.4249999998284,11.5671105274568));
#295398=CARTESIAN_POINT('Ctrl Pts',(7.51676407774742,45.5749999998278,10.3459381770588));
#295399=CARTESIAN_POINT('Ctrl Pts',(9.83957192047851,45.7249999998272,7.14886745759505));
#295400=CARTESIAN_POINT('Ctrl Pts',(12.1623797632096,45.8749999998266,3.95179673813132));
#295401=CARTESIAN_POINT('Ctrl Pts',(12.1623797632096,46.024999999826,-1.48946194470292E-15));
#295402=CARTESIAN_POINT('Ctrl Pts',(12.1623797632096,46.1749999998254,-3.95179673813132));
#295403=CARTESIAN_POINT('Ctrl Pts',(9.83957192047851,46.3249999998248,-7.14886745759505));
#295404=CARTESIAN_POINT('Ctrl Pts',(7.51676407774742,46.4749999998242,-10.3459381770588));
#295405=CARTESIAN_POINT('Ctrl Pts',(3.75838203887369,46.6249999998236,-11.5671105274568));
#295406=CARTESIAN_POINT('Ctrl Pts',(-4.0198546964214E-14,46.774999999823,
-12.7882828778549));
#295407=CARTESIAN_POINT('Ctrl Pts',(-3.75838203887377,46.9249999998224,
-11.5671105274568));
#295408=CARTESIAN_POINT('Ctrl Pts',(-7.5167640777475,47.0749999998218,-10.3459381770588));
#295409=CARTESIAN_POINT('Ctrl Pts',(-9.83957192047859,47.2249999998212,
-7.14886745759505));
#295410=CARTESIAN_POINT('Ctrl Pts',(-12.1623797632097,47.3749999998206,
-3.95179673813132));
#295411=CARTESIAN_POINT('Ctrl Pts',(-12.1623797632097,47.52499999982,2.97892388940585E-15));
#295412=CARTESIAN_POINT('Ctrl Pts',(-12.1623797632097,47.6749999998194,
3.95179673813133));
#295413=CARTESIAN_POINT('Ctrl Pts',(-9.83957192047859,47.8249999998188,
7.14886745759505));
#295414=CARTESIAN_POINT('Ctrl Pts',(-7.51676407774749,47.9749999998182,
10.3459381770588));
#295415=CARTESIAN_POINT('Ctrl Pts',(-3.75838203887377,48.1249999998176,
11.5671105274568));
#295416=CARTESIAN_POINT('Ctrl Pts',(-3.79301756614538E-14,48.274999999817,
12.7882828778549));
#295417=CARTESIAN_POINT('Ctrl Pts',(3.75838203887369,48.4249999998164,11.5671105274568));
#295418=CARTESIAN_POINT('Ctrl Pts',(7.51676407774742,48.5749999998158,10.3459381770588));
#295419=CARTESIAN_POINT('Ctrl Pts',(9.83957192047851,48.7249999998152,7.14886745759505));
#295420=CARTESIAN_POINT('Ctrl Pts',(12.1623797632096,48.8749999998146,3.95179673813132));
#295421=CARTESIAN_POINT('Ctrl Pts',(12.1623797632096,49.024999999814,-1.48946194470292E-15));
#295422=CARTESIAN_POINT('Ctrl Pts',(12.1623797632096,49.1749999998134,-3.95179673813132));
#295423=CARTESIAN_POINT('Ctrl Pts',(9.83957192047851,49.3249999998128,-7.14886745759505));
#295424=CARTESIAN_POINT('Ctrl Pts',(7.51676407774741,49.4749999998122,-10.3459381770588));
#295425=CARTESIAN_POINT('Ctrl Pts',(3.75838203887369,49.6249999998116,-11.5671105274568));
#295426=CARTESIAN_POINT('Ctrl Pts',(-4.19262562358759E-14,49.774999999811,
-12.7882828778549));
#295427=CARTESIAN_POINT('Ctrl Pts',(-3.75838203887377,49.9249999998104,
-11.5671105274568));
#295428=CARTESIAN_POINT('Ctrl Pts',(-7.5167640777475,50.0749999998098,-10.3459381770588));
#295429=CARTESIAN_POINT('Ctrl Pts',(-9.83957192047859,50.2249999998092,
-7.14886745759505));
#295430=CARTESIAN_POINT('Ctrl Pts',(-12.1623797632097,50.3749999998086,
-3.95179673813132));
#295431=CARTESIAN_POINT('Ctrl Pts',(-12.1623797632097,50.524999999808,2.97892388940585E-15));
#295432=CARTESIAN_POINT('Ctrl Pts',(-12.1623797632097,50.6749999998074,
3.95179673813133));
#295433=CARTESIAN_POINT('Ctrl Pts',(-9.83957192047859,50.8249999998068,
7.14886745759505));
#295434=CARTESIAN_POINT('Ctrl Pts',(-7.51676407774749,50.9749999998062,
10.3459381770588));
#295435=CARTESIAN_POINT('Ctrl Pts',(-3.75838203887377,51.1249999998056,
11.5671105274568));
#295436=CARTESIAN_POINT('Ctrl Pts',(-3.96578849331156E-14,51.274999999805,
12.7882828778549));
#295437=CARTESIAN_POINT('Ctrl Pts',(3.75838203887369,51.4249999998044,11.5671105274568));
#295438=CARTESIAN_POINT('Ctrl Pts',(7.51676407774742,51.5749999998038,10.3459381770588));
#295439=CARTESIAN_POINT('Ctrl Pts',(9.83957192047851,51.7249999998032,7.14886745759505));
#295440=CARTESIAN_POINT('Ctrl Pts',(12.1623797632096,51.8749999998026,3.95179673813132));
#295441=CARTESIAN_POINT('Ctrl Pts',(12.1623797632096,52.024999999802,-1.48946194470292E-15));
#295442=CARTESIAN_POINT('Ctrl Pts',(12.1623797632096,52.1749999998014,-3.95179673813132));
#295443=CARTESIAN_POINT('Ctrl Pts',(9.8395719204785,52.3249999998008,-7.14886745759505));
#295444=CARTESIAN_POINT('Ctrl Pts',(7.51676407774741,52.4749999998002,-10.3459381770588));
#295445=CARTESIAN_POINT('Ctrl Pts',(3.75838203887368,52.6249999997996,-11.5671105274568));
#295446=CARTESIAN_POINT('Ctrl Pts',(-4.36539655075377E-14,52.774999999799,
-12.7882828778549));
#295447=CARTESIAN_POINT('Ctrl Pts',(-3.75838203887377,52.9249999997984,
-11.5671105274568));
#295448=CARTESIAN_POINT('Ctrl Pts',(-7.5167640777475,53.0749999997978,-10.3459381770588));
#295449=CARTESIAN_POINT('Ctrl Pts',(-9.83957192047859,53.2249999997972,
-7.14886745759505));
#295450=CARTESIAN_POINT('Ctrl Pts',(-12.1623797632097,53.3749999997966,
-3.95179673813132));
#295451=CARTESIAN_POINT('Ctrl Pts',(-12.1623797632097,53.524999999796,2.97892388940585E-15));
#295452=CARTESIAN_POINT('Ctrl Pts',(-12.1623797632097,53.6749999997954,
3.95179673813133));
#295453=CARTESIAN_POINT('Ctrl Pts',(-9.83957192047859,53.8249999997948,
7.14886745759505));
#295454=CARTESIAN_POINT('Ctrl Pts',(-7.5167640777475,53.9749999997942,10.3459381770588));
#295455=CARTESIAN_POINT('Ctrl Pts',(-3.75838203887377,54.1249999997936,
11.5671105274568));
#295456=CARTESIAN_POINT('Ctrl Pts',(-4.13855942047774E-14,54.274999999793,
12.7882828778549));
#295457=CARTESIAN_POINT('Ctrl Pts',(3.75838203887369,54.4249999997924,11.5671105274568));
#295458=CARTESIAN_POINT('Ctrl Pts',(7.51676407774741,54.5749999997918,10.3459381770588));
#295459=CARTESIAN_POINT('Ctrl Pts',(9.8395719204785,54.7249999997912,7.14886745759505));
#295460=CARTESIAN_POINT('Ctrl Pts',(12.1623797632096,54.8749999997906,3.95179673813132));
#295461=CARTESIAN_POINT('Ctrl Pts',(12.1623797632096,55.02499999979,-1.48946194470292E-15));
#295462=CARTESIAN_POINT('Ctrl Pts',(12.1623797632096,55.1749999997894,-3.95179673813132));
#295463=CARTESIAN_POINT('Ctrl Pts',(9.8395719204785,55.3249999997888,-7.14886745759505));
#295464=CARTESIAN_POINT('Ctrl Pts',(7.51676407774741,55.4749999997882,-10.3459381770588));
#295465=CARTESIAN_POINT('Ctrl Pts',(3.75838203887368,55.6249999997876,-11.5671105274568));
#295466=CARTESIAN_POINT('Ctrl Pts',(-4.53816747791995E-14,55.774999999787,
-12.7882828778549));
#295467=CARTESIAN_POINT('Ctrl Pts',(-3.75838203887377,55.9249999997864,
-11.5671105274568));
#295468=CARTESIAN_POINT('Ctrl Pts',(-7.5167640777475,56.0749999997858,-10.3459381770588));
#295469=CARTESIAN_POINT('Ctrl Pts',(-9.83957192047859,56.2249999997852,
-7.14886745759505));
#295470=CARTESIAN_POINT('Ctrl Pts',(-12.1623797632097,56.3749999997846,
-3.95179673813132));
#295471=CARTESIAN_POINT('Ctrl Pts',(-12.1623797632097,56.524999999784,2.97892388940585E-15));
#295472=CARTESIAN_POINT('Ctrl Pts',(-12.1623797632097,56.6749999997834,
3.95179673813133));
#295473=CARTESIAN_POINT('Ctrl Pts',(-9.83957192047859,56.8249999997828,
7.14886745759505));
#295474=CARTESIAN_POINT('Ctrl Pts',(-7.5167640777475,56.9749999997822,10.3459381770588));
#295475=CARTESIAN_POINT('Ctrl Pts',(-3.75838203887377,57.1249999997816,
11.5671105274568));
#295476=CARTESIAN_POINT('Ctrl Pts',(-4.31133034764393E-14,57.274999999781,
12.7882828778549));
#295477=CARTESIAN_POINT('Ctrl Pts',(3.75838203887368,57.4249999997804,11.5671105274568));
#295478=CARTESIAN_POINT('Ctrl Pts',(7.51676407774741,57.5749999997798,10.3459381770588));
#295479=CARTESIAN_POINT('Ctrl Pts',(9.8395719204785,57.7249999997792,7.14886745759505));
#295480=CARTESIAN_POINT('Ctrl Pts',(12.1623797632096,57.8749999997786,3.95179673813132));
#295481=CARTESIAN_POINT('Ctrl Pts',(12.1623797632096,58.024999999778,-1.48946194470292E-15));
#295482=CARTESIAN_POINT('Ctrl Pts',(12.1623797632096,58.1749999997774,-3.95179673813132));
#295483=CARTESIAN_POINT('Ctrl Pts',(9.8395719204785,58.3249999997768,-7.14886745759505));
#295484=CARTESIAN_POINT('Ctrl Pts',(7.51676407774741,58.4749999997762,-10.3459381770588));
#295485=CARTESIAN_POINT('Ctrl Pts',(3.75838203887368,58.6249999997756,-11.5671105274568));
#295486=CARTESIAN_POINT('Ctrl Pts',(-4.71093840508614E-14,58.774999999775,
-12.7882828778549));
#295487=CARTESIAN_POINT('Ctrl Pts',(-3.75838203887377,58.9249999997744,
-11.5671105274568));
#295488=CARTESIAN_POINT('Ctrl Pts',(-7.5167640777475,59.0749999997738,-10.3459381770588));
#295489=CARTESIAN_POINT('Ctrl Pts',(-9.83957192047859,59.2249999997732,
-7.14886745759505));
#295490=CARTESIAN_POINT('Ctrl Pts',(-12.1623797632097,59.3749999997726,
-3.95179673813132));
#295491=CARTESIAN_POINT('Ctrl Pts',(-12.1623797632097,59.524999999772,2.97892388940585E-15));
#295492=CARTESIAN_POINT('Ctrl Pts',(-12.1623797632097,59.6749999997714,
3.95179673813133));
#295493=CARTESIAN_POINT('Ctrl Pts',(-9.83957192047859,59.8249999997708,
7.14886745759505));
#295494=CARTESIAN_POINT('Ctrl Pts',(-7.5167640777475,59.9749999997702,10.3459381770588));
#295495=CARTESIAN_POINT('Ctrl Pts',(-3.75838203887377,60.1249999997696,
11.5671105274568));
#295496=CARTESIAN_POINT('Ctrl Pts',(-4.48410127481011E-14,60.274999999769,
12.7882828778549));
#295497=CARTESIAN_POINT('Ctrl Pts',(3.75838203887368,60.4249999997684,11.5671105274568));
#295498=CARTESIAN_POINT('Ctrl Pts',(7.51676407774741,60.5749999997678,10.3459381770588));
#295499=CARTESIAN_POINT('Ctrl Pts',(9.8395719204785,60.7249999997672,7.14886745759505));
#295500=CARTESIAN_POINT('Ctrl Pts',(12.1623797632096,60.8749999997666,3.95179673813132));
#295501=CARTESIAN_POINT('Ctrl Pts',(12.1623797632096,61.024999999766,-1.48946194470292E-15));
#295502=CARTESIAN_POINT('Ctrl Pts',(12.1623797632096,61.1749999997654,-3.95179673813132));
#295503=CARTESIAN_POINT('Ctrl Pts',(9.8395719204785,61.3249999997648,-7.14886745759505));
#295504=CARTESIAN_POINT('Ctrl Pts',(7.51676407774741,61.4749999997642,-10.3459381770588));
#295505=CARTESIAN_POINT('Ctrl Pts',(3.75838203887368,61.6249999997636,-11.5671105274568));
#295506=CARTESIAN_POINT('Ctrl Pts',(-4.88370933225232E-14,61.774999999763,
-12.7882828778549));
#295507=CARTESIAN_POINT('Ctrl Pts',(-3.75838203887378,61.9249999997624,
-11.5671105274568));
#295508=CARTESIAN_POINT('Ctrl Pts',(-7.5167640777475,62.0749999997618,-10.3459381770588));
#295509=CARTESIAN_POINT('Ctrl Pts',(-9.8395719204786,62.2249999997612,-7.14886745759505));
#295510=CARTESIAN_POINT('Ctrl Pts',(-12.1623797632097,62.3749999997606,
-3.95179673813132));
#295511=CARTESIAN_POINT('Ctrl Pts',(-12.1623797632097,62.52499999976,2.97892388940585E-15));
#295512=CARTESIAN_POINT('Ctrl Pts',(-12.1623797632097,62.6749999997594,
3.95179673813133));
#295513=CARTESIAN_POINT('Ctrl Pts',(-9.8395719204786,62.8249999997588,7.14886745759505));
#295514=CARTESIAN_POINT('Ctrl Pts',(-7.5167640777475,62.9749999997582,10.3459381770588));
#295515=CARTESIAN_POINT('Ctrl Pts',(-3.75838203887377,63.1249999997576,
11.5671105274568));
#295516=CARTESIAN_POINT('Ctrl Pts',(-4.6568722019763E-14,63.274999999757,
12.7882828778549));
#295517=CARTESIAN_POINT('Ctrl Pts',(3.75838203887368,63.4249999997564,11.5671105274568));
#295518=CARTESIAN_POINT('Ctrl Pts',(7.51676407774741,63.5749999997558,10.3459381770588));
#295519=CARTESIAN_POINT('Ctrl Pts',(9.8395719204785,63.7249999997552,7.14886745759505));
#295520=CARTESIAN_POINT('Ctrl Pts',(12.1623797632096,63.8749999997546,3.95179673813132));
#295521=CARTESIAN_POINT('Ctrl Pts',(12.1623797632096,64.024999999754,-1.48946194470292E-15));
#295522=CARTESIAN_POINT('Ctrl Pts',(12.1623797632096,64.1749999997534,-3.95179673813132));
#295523=CARTESIAN_POINT('Ctrl Pts',(9.8395719204785,64.3249999997528,-7.14886745759505));
#295524=CARTESIAN_POINT('Ctrl Pts',(7.5167640777474,64.4749999997522,-10.3459381770588));
#295525=CARTESIAN_POINT('Ctrl Pts',(3.75838203887368,64.6249999997516,-11.5671105274568));
#295526=CARTESIAN_POINT('Ctrl Pts',(-5.05648025941851E-14,64.774999999751,
-12.7882828778549));
#295527=CARTESIAN_POINT('Ctrl Pts',(-3.75838203887378,64.9249999997504,
-11.5671105274568));
#295528=CARTESIAN_POINT('Ctrl Pts',(-7.51676407774751,65.0749999997498,
-10.3459381770588));
#295529=CARTESIAN_POINT('Ctrl Pts',(-9.8395719204786,65.2249999997492,-7.14886745759505));
#295530=CARTESIAN_POINT('Ctrl Pts',(-12.1623797632097,65.3749999997486,
-3.95179673813132));
#295531=CARTESIAN_POINT('Ctrl Pts',(-12.1623797632097,65.524999999748,2.97892388940585E-15));
#295532=CARTESIAN_POINT('Ctrl Pts',(-12.1623797632097,65.6749999997474,
3.95179673813133));
#295533=CARTESIAN_POINT('Ctrl Pts',(-9.8395719204786,65.8249999997468,7.14886745759505));
#295534=CARTESIAN_POINT('Ctrl Pts',(-7.5167640777475,65.9749999997462,10.3459381770588));
#295535=CARTESIAN_POINT('Ctrl Pts',(-3.75838203887378,66.1249999997456,
11.5671105274568));
#295536=CARTESIAN_POINT('Ctrl Pts',(-4.82964312914248E-14,66.274999999745,
12.7882828778549));
#295537=CARTESIAN_POINT('Ctrl Pts',(3.75838203887368,66.4249999997444,11.5671105274568));
#295538=CARTESIAN_POINT('Ctrl Pts',(7.51676407774741,66.5749999997438,10.3459381770588));
#295539=CARTESIAN_POINT('Ctrl Pts',(9.8395719204785,66.7249999997432,7.14886745759505));
#295540=CARTESIAN_POINT('Ctrl Pts',(12.1623797632096,66.8749999997426,3.95179673813132));
#295541=CARTESIAN_POINT('Ctrl Pts',(12.1623797632096,67.024999999742,-1.48946194470292E-15));
#295542=CARTESIAN_POINT('Ctrl Pts',(12.1623797632096,67.1749999997414,-3.95179673813132));
#295543=CARTESIAN_POINT('Ctrl Pts',(9.8395719204785,67.3249999997408,-7.14886745759505));
#295544=CARTESIAN_POINT('Ctrl Pts',(7.5167640777474,67.4749999997402,-10.3459381770588));
#295545=CARTESIAN_POINT('Ctrl Pts',(3.75838203887368,67.6249999997396,-11.5671105274568));
#295546=CARTESIAN_POINT('Ctrl Pts',(-5.22925118658469E-14,67.774999999739,
-12.7882828778549));
#295547=CARTESIAN_POINT('Ctrl Pts',(-3.75838203887378,67.9249999997384,
-11.5671105274568));
#295548=CARTESIAN_POINT('Ctrl Pts',(-7.51676407774751,68.0749999997378,
-10.3459381770588));
#295549=CARTESIAN_POINT('Ctrl Pts',(-9.8395719204786,68.2249999997372,-7.14886745759505));
#295550=CARTESIAN_POINT('Ctrl Pts',(-12.1623797632097,68.3749999997366,
-3.95179673813132));
#295551=CARTESIAN_POINT('Ctrl Pts',(-12.1623797632097,68.524999999736,2.97892388940585E-15));
#295552=CARTESIAN_POINT('Ctrl Pts',(-12.1623797632097,68.6749999997354,
3.95179673813133));
#295553=CARTESIAN_POINT('Ctrl Pts',(-9.8395719204786,68.8249999997348,7.14886745759505));
#295554=CARTESIAN_POINT('Ctrl Pts',(-7.51676407774751,68.9749999997342,
10.3459381770588));
#295555=CARTESIAN_POINT('Ctrl Pts',(-3.75838203887378,69.1249999997336,
11.5671105274568));
#295556=CARTESIAN_POINT('Ctrl Pts',(-5.00241405630866E-14,69.274999999733,
12.7882828778549));
#295557=CARTESIAN_POINT('Ctrl Pts',(3.75838203887368,69.4249999997324,11.5671105274568));
#295558=CARTESIAN_POINT('Ctrl Pts',(7.5167640777474,69.5749999997318,10.3459381770588));
#295559=CARTESIAN_POINT('Ctrl Pts',(9.8395719204785,69.7249999997312,7.14886745759505));
#295560=CARTESIAN_POINT('Ctrl Pts',(12.1623797632096,69.8749999997306,3.95179673813132));
#295561=CARTESIAN_POINT('Ctrl Pts',(12.1623797632096,70.02499999973,-1.48946194470292E-15));
#295562=CARTESIAN_POINT('Ctrl Pts',(12.1623797632096,70.1749999997294,-3.95179673813132));
#295563=CARTESIAN_POINT('Ctrl Pts',(9.83957192047849,70.3249999997288,-7.14886745759505));
#295564=CARTESIAN_POINT('Ctrl Pts',(7.5167640777474,70.4749999997282,-10.3459381770588));
#295565=CARTESIAN_POINT('Ctrl Pts',(3.75838203887367,70.6249999997276,-11.5671105274568));
#295566=CARTESIAN_POINT('Ctrl Pts',(-5.40202211375087E-14,70.774999999727,
-12.7882828778549));
#295567=CARTESIAN_POINT('Ctrl Pts',(-3.75838203887378,70.9249999997264,
-11.5671105274568));
#295568=CARTESIAN_POINT('Ctrl Pts',(-7.51676407774751,71.0749999997258,
-10.3459381770588));
#295569=CARTESIAN_POINT('Ctrl Pts',(-9.8395719204786,71.2249999997252,-7.14886745759505));
#295570=CARTESIAN_POINT('Ctrl Pts',(-12.1623797632097,71.3749999997246,
-3.95179673813132));
#295571=CARTESIAN_POINT('Ctrl Pts',(-12.1623797632097,71.524999999724,2.97892388940585E-15));
#295572=CARTESIAN_POINT('Ctrl Pts',(-12.1623797632097,71.6749999997234,
3.95179673813133));
#295573=CARTESIAN_POINT('Ctrl Pts',(-9.8395719204786,71.8249999997228,7.14886745759505));
#295574=CARTESIAN_POINT('Ctrl Pts',(-7.51676407774751,71.9749999997222,
10.3459381770588));
#295575=CARTESIAN_POINT('Ctrl Pts',(-3.75838203887378,72.1249999997216,
11.5671105274568));
#295576=CARTESIAN_POINT('Ctrl Pts',(-5.17518498347485E-14,72.274999999721,
12.7882828778549));
#295577=CARTESIAN_POINT('Ctrl Pts',(3.75838203887368,72.4249999997204,11.5671105274568));
#295578=CARTESIAN_POINT('Ctrl Pts',(7.5167640777474,72.5749999997198,10.3459381770588));
#295579=CARTESIAN_POINT('Ctrl Pts',(9.83957192047849,72.7249999997192,7.14886745759505));
#295580=CARTESIAN_POINT('Ctrl Pts',(12.1623797632096,72.8749999997186,3.95179673813132));
#295581=CARTESIAN_POINT('Ctrl Pts',(12.1623797632096,73.024999999718,-1.48946194470292E-15));
#295582=CARTESIAN_POINT('Ctrl Pts',(12.1623797632096,73.1749999997174,-3.95179673813132));
#295583=CARTESIAN_POINT('Ctrl Pts',(9.83957192047849,73.3249999997168,-7.14886745759505));
#295584=CARTESIAN_POINT('Ctrl Pts',(7.5167640777474,73.4749999997162,-10.3459381770588));
#295585=CARTESIAN_POINT('Ctrl Pts',(3.75838203887367,73.6249999997156,-11.5671105274568));
#295586=CARTESIAN_POINT('Ctrl Pts',(-5.57479304091706E-14,73.774999999715,
-12.7882828778549));
#295587=CARTESIAN_POINT('Ctrl Pts',(-3.75838203887378,73.9249999997144,
-11.5671105274568));
#295588=CARTESIAN_POINT('Ctrl Pts',(-7.51676407774751,74.0749999997138,
-10.3459381770588));
#295589=CARTESIAN_POINT('Ctrl Pts',(-9.8395719204786,74.2249999997132,-7.14886745759505));
#295590=CARTESIAN_POINT('Ctrl Pts',(-12.1623797632097,74.3749999997126,
-3.95179673813132));
#295591=CARTESIAN_POINT('Ctrl Pts',(-12.1623797632097,74.524999999712,2.97892388940585E-15));
#295592=CARTESIAN_POINT('Ctrl Pts',(-12.1623797632097,74.6749999997114,
3.95179673813133));
#295593=CARTESIAN_POINT('Ctrl Pts',(-9.8395719204786,74.8249999997108,7.14886745759505));
#295594=CARTESIAN_POINT('Ctrl Pts',(-7.51676407774751,74.9749999997102,
10.3459381770588));
#295595=CARTESIAN_POINT('Ctrl Pts',(-3.75838203887378,75.1249999997096,
11.5671105274568));
#295596=CARTESIAN_POINT('Ctrl Pts',(-5.34795591064103E-14,75.274999999709,
12.7882828778549));
#295597=CARTESIAN_POINT('Ctrl Pts',(3.75838203887367,75.4249999997084,11.5671105274568));
#295598=CARTESIAN_POINT('Ctrl Pts',(7.5167640777474,75.5749999997078,10.3459381770588));
#295599=CARTESIAN_POINT('Ctrl Pts',(9.83957192047849,75.7249999997072,7.14886745759505));
#295600=CARTESIAN_POINT('Ctrl Pts',(12.1623797632096,75.8749999997066,3.95179673813132));
#295601=CARTESIAN_POINT('Ctrl Pts',(12.1623797632096,76.024999999706,-1.48946194470292E-15));
#295602=CARTESIAN_POINT('Ctrl Pts',(12.1623797632096,76.1749999997054,-3.95179673813132));
#295603=CARTESIAN_POINT('Ctrl Pts',(9.83957192047849,76.3249999997048,-7.14886745759505));
#295604=CARTESIAN_POINT('Ctrl Pts',(7.5167640777474,76.4749999997042,-10.3459381770588));
#295605=CARTESIAN_POINT('Ctrl Pts',(3.75838203887367,76.6249999997036,-11.5671105274568));
#295606=CARTESIAN_POINT('Ctrl Pts',(-5.74756396808324E-14,76.774999999703,
-12.7882828778549));
#295607=CARTESIAN_POINT('Ctrl Pts',(-3.75838203887379,76.9249999997024,
-11.5671105274568));
#295608=CARTESIAN_POINT('Ctrl Pts',(-7.51676407774751,77.0749999997018,
-10.3459381770588));
#295609=CARTESIAN_POINT('Ctrl Pts',(-9.8395719204786,77.2249999997012,-7.14886745759505));
#295610=CARTESIAN_POINT('Ctrl Pts',(-12.1623797632097,77.3749999997006,
-3.95179673813132));
#295611=CARTESIAN_POINT('Ctrl Pts',(-12.1623797632097,77.5249999997,2.97892388940585E-15));
#295612=CARTESIAN_POINT('Ctrl Pts',(-12.1623797632097,77.6749999996994,
3.95179673813133));
#295613=CARTESIAN_POINT('Ctrl Pts',(-9.8395719204786,77.8249999996988,7.14886745759505));
#295614=CARTESIAN_POINT('Ctrl Pts',(-7.51676407774751,77.9749999996982,
10.3459381770588));
#295615=CARTESIAN_POINT('Ctrl Pts',(-3.75838203887378,78.1249999996976,
11.5671105274568));
#295616=CARTESIAN_POINT('Ctrl Pts',(-5.52072683780721E-14,78.274999999697,
12.7882828778549));
#295617=CARTESIAN_POINT('Ctrl Pts',(3.75838203887367,78.4249999996964,11.5671105274568));
#295618=CARTESIAN_POINT('Ctrl Pts',(7.5167640777474,78.5749999996958,10.3459381770588));
#295619=CARTESIAN_POINT('Ctrl Pts',(9.83957192047849,78.7249999996952,7.14886745759505));
#295620=CARTESIAN_POINT('Ctrl Pts',(12.1623797632096,78.8749999996946,3.95179673813132));
#295621=CARTESIAN_POINT('Ctrl Pts',(12.1623797632096,79.024999999694,-1.48946194470292E-15));
#295622=CARTESIAN_POINT('Ctrl Pts',(12.1623797632096,79.1749999996934,-3.95179673813132));
#295623=CARTESIAN_POINT('Ctrl Pts',(9.83957192047849,79.3249999996928,-7.14886745759505));
#295624=CARTESIAN_POINT('Ctrl Pts',(7.5167640777474,79.4749999996922,-10.3459381770588));
#295625=CARTESIAN_POINT('Ctrl Pts',(3.75838203887367,79.6249999996916,-11.5671105274568));
#295626=CARTESIAN_POINT('Ctrl Pts',(-5.92033489524943E-14,79.774999999691,
-12.7882828778549));
#295627=CARTESIAN_POINT('Ctrl Pts',(-3.75838203887379,79.9249999996904,
-11.5671105274568));
#295628=CARTESIAN_POINT('Ctrl Pts',(-7.51676407774751,80.0749999996898,
-10.3459381770588));
#295629=CARTESIAN_POINT('Ctrl Pts',(-9.83957192047861,80.2249999996892,
-7.14886745759505));
#295630=CARTESIAN_POINT('Ctrl Pts',(-12.1623797632097,80.3749999996886,
-3.95179673813132));
#295631=CARTESIAN_POINT('Ctrl Pts',(-12.1623797632097,80.524999999688,2.97892388940585E-15));
#295632=CARTESIAN_POINT('Ctrl Pts',(-12.1623797632097,80.6749999996874,
3.95179673813133));
#295633=CARTESIAN_POINT('Ctrl Pts',(-9.83957192047861,80.8249999996868,
7.14886745759505));
#295634=CARTESIAN_POINT('Ctrl Pts',(-7.51676407774751,80.9749999996862,
10.3459381770588));
#295635=CARTESIAN_POINT('Ctrl Pts',(-3.75838203887378,81.1249999996856,
11.5671105274568));
#295636=CARTESIAN_POINT('Ctrl Pts',(-5.6934977649734E-14,81.274999999685,
12.7882828778549));
#295637=CARTESIAN_POINT('Ctrl Pts',(3.75838203887367,81.4249999996844,11.5671105274568));
#295638=CARTESIAN_POINT('Ctrl Pts',(7.5167640777474,81.5749999996838,10.3459381770588));
#295639=CARTESIAN_POINT('Ctrl Pts',(9.83957192047849,81.7249999996832,7.14886745759505));
#295640=CARTESIAN_POINT('Ctrl Pts',(12.1623797632096,81.8749999996826,3.95179673813132));
#295641=CARTESIAN_POINT('Ctrl Pts',(12.1623797632096,82.024999999682,-1.48946194470292E-15));
#295642=CARTESIAN_POINT('Ctrl Pts',(12.1623797632096,82.1749999996814,-3.95179673813132));
#295643=CARTESIAN_POINT('Ctrl Pts',(9.83957192047849,82.3249999996808,-7.14886745759505));
#295644=CARTESIAN_POINT('Ctrl Pts',(7.5167640777474,82.4749999996802,-10.3459381770588));
#295645=CARTESIAN_POINT('Ctrl Pts',(3.75838203887367,82.6249999996796,-11.5671105274568));
#295646=CARTESIAN_POINT('Ctrl Pts',(-6.09310582241561E-14,82.774999999679,
-12.7882828778549));
#295647=CARTESIAN_POINT('Ctrl Pts',(-3.75838203887379,82.9249999996784,
-11.5671105274568));
#295648=CARTESIAN_POINT('Ctrl Pts',(-7.51676407774752,83.0749999996778,
-10.3459381770588));
#295649=CARTESIAN_POINT('Ctrl Pts',(-9.83957192047861,83.2249999996772,
-7.14886745759505));
#295650=CARTESIAN_POINT('Ctrl Pts',(-12.1623797632097,83.3749999996766,
-3.95179673813132));
#295651=CARTESIAN_POINT('Ctrl Pts',(-12.1623797632097,83.524999999676,2.97892388940585E-15));
#295652=CARTESIAN_POINT('Ctrl Pts',(-12.1623797632097,83.6749999996754,
3.95179673813133));
#295653=CARTESIAN_POINT('Ctrl Pts',(-9.83957192047861,83.8249999996748,
7.14886745759505));
#295654=CARTESIAN_POINT('Ctrl Pts',(-7.51676407774751,83.9749999996742,
10.3459381770588));
#295655=CARTESIAN_POINT('Ctrl Pts',(-3.75838203887379,84.1249999996736,
11.5671105274568));
#295656=CARTESIAN_POINT('Ctrl Pts',(-5.86626869213958E-14,84.274999999673,
12.7882828778549));
#295657=CARTESIAN_POINT('Ctrl Pts',(3.75838203887367,84.4249999996724,11.5671105274568));
#295658=CARTESIAN_POINT('Ctrl Pts',(7.5167640777474,84.5749999996718,10.3459381770588));
#295659=CARTESIAN_POINT('Ctrl Pts',(9.83957192047849,84.7249999996712,7.14886745759505));
#295660=CARTESIAN_POINT('Ctrl Pts',(12.1623797632096,84.8749999996706,3.95179673813132));
#295661=CARTESIAN_POINT('Ctrl Pts',(12.1623797632096,85.02499999967,-1.48946194470292E-15));
#295662=CARTESIAN_POINT('Ctrl Pts',(12.1623797632096,85.1749999996694,-3.95179673813132));
#295663=CARTESIAN_POINT('Ctrl Pts',(9.83957192047849,85.3249999996688,-7.14886745759505));
#295664=CARTESIAN_POINT('Ctrl Pts',(7.51676407774739,85.4749999996682,-10.3459381770588));
#295665=CARTESIAN_POINT('Ctrl Pts',(3.75838203887367,85.6249999996676,-11.5671105274568));
#295666=CARTESIAN_POINT('Ctrl Pts',(-6.26587674958179E-14,85.774999999667,
-12.7882828778549));
#295667=CARTESIAN_POINT('Ctrl Pts',(-3.75838203887379,85.9249999996664,
-11.5671105274568));
#295668=CARTESIAN_POINT('Ctrl Pts',(-7.51676407774752,86.0749999996658,
-10.3459381770588));
#295669=CARTESIAN_POINT('Ctrl Pts',(-9.83957192047861,86.2249999996652,
-7.14886745759505));
#295670=CARTESIAN_POINT('Ctrl Pts',(-12.1623797632097,86.3749999996646,
-3.95179673813132));
#295671=CARTESIAN_POINT('Ctrl Pts',(-12.1623797632097,86.524999999664,2.97892388940585E-15));
#295672=CARTESIAN_POINT('Ctrl Pts',(-12.1623797632097,86.6749999996634,
3.95179673813133));
#295673=CARTESIAN_POINT('Ctrl Pts',(-9.83957192047861,86.8249999996628,
7.14886745759505));
#295674=CARTESIAN_POINT('Ctrl Pts',(-7.51676407774752,86.9749999996622,
10.3459381770588));
#295675=CARTESIAN_POINT('Ctrl Pts',(-3.75838203887379,87.1249999996616,
11.5671105274568));
#295676=CARTESIAN_POINT('Ctrl Pts',(-6.03903961930577E-14,87.274999999661,
12.7882828778549));
#295677=CARTESIAN_POINT('Ctrl Pts',(3.75838203887367,87.4249999996604,11.5671105274568));
#295678=CARTESIAN_POINT('Ctrl Pts',(7.5167640777474,87.5749999996598,10.3459381770588));
#295679=CARTESIAN_POINT('Ctrl Pts',(9.83957192047849,87.7249999996592,7.14886745759505));
#295680=CARTESIAN_POINT('Ctrl Pts',(12.1623797632096,87.8749999996586,3.95179673813132));
#295681=CARTESIAN_POINT('Ctrl Pts',(12.1623797632096,88.024999999658,-1.48946194470292E-15));
#295682=CARTESIAN_POINT('Ctrl Pts',(12.1623797632096,88.1749999996574,-3.95179673813132));
#295683=CARTESIAN_POINT('Ctrl Pts',(9.83957192047849,88.3249999996568,-7.14886745759505));
#295684=CARTESIAN_POINT('Ctrl Pts',(7.51676407774739,88.4749999996562,-10.3459381770588));
#295685=CARTESIAN_POINT('Ctrl Pts',(3.75838203887366,88.6249999996556,-11.5671105274568));
#295686=CARTESIAN_POINT('Ctrl Pts',(-6.43864767674798E-14,88.774999999655,
-12.7882828778549));
#295687=CARTESIAN_POINT('Ctrl Pts',(-3.75838203887379,88.9249999996544,
-11.5671105274568));
#295688=CARTESIAN_POINT('Ctrl Pts',(-7.51676407774752,89.0749999996538,
-10.3459381770588));
#295689=CARTESIAN_POINT('Ctrl Pts',(-9.83957192047861,89.2249999996532,
-7.14886745759505));
#295690=CARTESIAN_POINT('Ctrl Pts',(-12.1623797632097,89.3749999996526,
-3.95179673813132));
#295691=CARTESIAN_POINT('Ctrl Pts',(-12.1623797632097,89.524999999652,2.97892388940585E-15));
#295692=CARTESIAN_POINT('Ctrl Pts',(-12.1623797632097,89.6749999996514,
3.95179673813133));
#295693=CARTESIAN_POINT('Ctrl Pts',(-9.83957192047861,89.8249999996508,
7.14886745759505));
#295694=CARTESIAN_POINT('Ctrl Pts',(-7.51676407774752,89.9749999996502,
10.3459381770588));
#295695=CARTESIAN_POINT('Ctrl Pts',(-3.75838203887379,90.1249999996496,
11.5671105274568));
#295696=CARTESIAN_POINT('Ctrl Pts',(-6.21181054647195E-14,90.274999999649,
12.7882828778549));
#295697=CARTESIAN_POINT('Ctrl Pts',(3.75838203887366,90.4249999996484,11.5671105274568));
#295698=CARTESIAN_POINT('Ctrl Pts',(7.51676407774739,90.5749999996478,10.3459381770588));
#295699=CARTESIAN_POINT('Ctrl Pts',(9.83957192047848,90.7249999996472,7.14886745759505));
#295700=CARTESIAN_POINT('Ctrl Pts',(12.1623797632096,90.8749999996466,3.95179673813132));
#295701=CARTESIAN_POINT('Ctrl Pts',(12.1623797632096,91.024999999646,-1.48946194470292E-15));
#295702=CARTESIAN_POINT('Ctrl Pts',(12.1623797632096,91.1749999996454,-3.95179673813132));
#295703=CARTESIAN_POINT('Ctrl Pts',(9.83957192047848,91.3249999996448,-7.14886745759505));
#295704=CARTESIAN_POINT('Ctrl Pts',(7.51676407774739,91.4749999996442,-10.3459381770588));
#295705=CARTESIAN_POINT('Ctrl Pts',(3.75838203887366,91.6249999996436,-11.5671105274568));
#295706=CARTESIAN_POINT('Ctrl Pts',(-6.61141860391416E-14,91.774999999643,
-12.7882828778549));
#295707=CARTESIAN_POINT('Ctrl Pts',(-3.75838203887379,91.9249999996424,
-11.5671105274568));
#295708=CARTESIAN_POINT('Ctrl Pts',(-7.51676407774752,92.0749999996418,
-10.3459381770588));
#295709=CARTESIAN_POINT('Ctrl Pts',(-9.83957192047861,92.2249999996412,
-7.14886745759505));
#295710=CARTESIAN_POINT('Ctrl Pts',(-12.1623797632097,92.3749999996406,
-3.95179673813132));
#295711=CARTESIAN_POINT('Ctrl Pts',(-12.1623797632097,92.52499999964,2.97892388940585E-15));
#295712=CARTESIAN_POINT('Ctrl Pts',(-12.1623797632097,92.6749999996394,
3.95179673813133));
#295713=CARTESIAN_POINT('Ctrl Pts',(-9.83957192047861,92.8249999996388,
7.14886745759505));
#295714=CARTESIAN_POINT('Ctrl Pts',(-7.51676407774752,92.9749999996382,
10.3459381770588));
#295715=CARTESIAN_POINT('Ctrl Pts',(-3.75838203887379,93.1249999996376,
11.5671105274568));
#295716=CARTESIAN_POINT('Ctrl Pts',(-6.38458147363813E-14,93.274999999637,
12.7882828778549));
#295717=CARTESIAN_POINT('Ctrl Pts',(3.75838203887366,93.4249999996364,11.5671105274568));
#295718=CARTESIAN_POINT('Ctrl Pts',(7.51676407774739,93.5749999996358,10.3459381770588));
#295719=CARTESIAN_POINT('Ctrl Pts',(9.83957192047848,93.7249999996352,7.14886745759505));
#295720=CARTESIAN_POINT('Ctrl Pts',(12.1623797632096,93.8749999996346,3.95179673813132));
#295721=CARTESIAN_POINT('Ctrl Pts',(12.1623797632096,94.024999999634,-1.48946194470292E-15));
#295722=CARTESIAN_POINT('Ctrl Pts',(12.1623797632096,94.1749999996334,-3.95179673813132));
#295723=CARTESIAN_POINT('Ctrl Pts',(9.83957192047848,94.3249999996328,-7.14886745759505));
#295724=CARTESIAN_POINT('Ctrl Pts',(7.51676407774739,94.4749999996322,-10.3459381770588));
#295725=CARTESIAN_POINT('Ctrl Pts',(3.75838203887366,94.6249999996316,-11.5671105274568));
#295726=CARTESIAN_POINT('Ctrl Pts',(-6.78418953108034E-14,94.774999999631,
-12.7882828778549));
#295727=CARTESIAN_POINT('Ctrl Pts',(-3.7583820388738,94.9249999996304,-11.5671105274568));
#295728=CARTESIAN_POINT('Ctrl Pts',(-7.51676407774752,95.0749999996298,
-10.3459381770588));
#295729=CARTESIAN_POINT('Ctrl Pts',(-9.83957192047862,95.2249999996292,
-7.14886745759505));
#295730=CARTESIAN_POINT('Ctrl Pts',(-12.1623797632097,95.3749999996286,
-3.95179673813132));
#295731=CARTESIAN_POINT('Ctrl Pts',(-12.1623797632097,95.524999999628,2.97892388940585E-15));
#295732=CARTESIAN_POINT('Ctrl Pts',(-12.1623797632097,95.6749999996274,
3.95179673813133));
#295733=CARTESIAN_POINT('Ctrl Pts',(-9.83957192047862,95.8249999996268,
7.14886745759505));
#295734=CARTESIAN_POINT('Ctrl Pts',(-7.51676407774752,95.9749999996262,
10.3459381770588));
#295735=CARTESIAN_POINT('Ctrl Pts',(-3.75838203887379,96.1249999996256,
11.5671105274568));
#295736=CARTESIAN_POINT('Ctrl Pts',(-6.55735240080432E-14,96.274999999625,
12.7882828778549));
#295737=CARTESIAN_POINT('Ctrl Pts',(3.75838203887366,96.4249999996244,11.5671105274568));
#295738=CARTESIAN_POINT('Ctrl Pts',(7.51676407774739,96.5749999996238,10.3459381770588));
#295739=CARTESIAN_POINT('Ctrl Pts',(9.83957192047848,96.7249999996232,7.14886745759505));
#295740=CARTESIAN_POINT('Ctrl Pts',(12.1623797632096,96.8749999996226,3.95179673813132));
#295741=CARTESIAN_POINT('Ctrl Pts',(12.1623797632096,97.024999999622,-1.48946194470292E-15));
#295742=CARTESIAN_POINT('Ctrl Pts',(12.1623797632096,97.1749999996214,-3.95179673813132));
#295743=CARTESIAN_POINT('Ctrl Pts',(9.83957192047848,97.3249999996208,-7.14886745759505));
#295744=CARTESIAN_POINT('Ctrl Pts',(7.51676407774739,97.4749999996202,-10.3459381770588));
#295745=CARTESIAN_POINT('Ctrl Pts',(3.75838203887366,97.6249999996196,-11.5671105274568));
#295746=CARTESIAN_POINT('Ctrl Pts',(-6.95696045824653E-14,97.774999999619,
-12.7882828778549));
#295747=CARTESIAN_POINT('Ctrl Pts',(-3.7583820388738,97.9249999996184,-11.5671105274568));
#295748=CARTESIAN_POINT('Ctrl Pts',(-7.51676407774752,98.0749999996178,
-10.3459381770588));
#295749=CARTESIAN_POINT('Ctrl Pts',(-9.83957192047862,98.2249999996172,
-7.14886745759505));
#295750=CARTESIAN_POINT('Ctrl Pts',(-12.1623797632097,98.3749999996166,
-3.95179673813132));
#295751=CARTESIAN_POINT('Ctrl Pts',(-12.1623797632097,98.524999999616,2.97892388940585E-15));
#295752=CARTESIAN_POINT('Ctrl Pts',(-12.1623797632097,98.6749999996154,
3.95179673813133));
#295753=CARTESIAN_POINT('Ctrl Pts',(-9.83957192047862,98.8249999996148,
7.14886745759505));
#295754=CARTESIAN_POINT('Ctrl Pts',(-7.51676407774752,98.9749999996142,
10.3459381770588));
#295755=CARTESIAN_POINT('Ctrl Pts',(-3.7583820388738,99.1249999996136,11.5671105274568));
#295756=CARTESIAN_POINT('Ctrl Pts',(-6.7301233279705E-14,99.274999999613,
12.7882828778549));
#295757=CARTESIAN_POINT('Ctrl Pts',(3.75838203887366,99.4249999996124,11.5671105274568));
#295758=CARTESIAN_POINT('Ctrl Pts',(7.51676407774739,99.5749999996118,10.3459381770588));
#295759=CARTESIAN_POINT('Ctrl Pts',(9.83957192047848,99.7249999996112,7.14886745759505));
#295760=CARTESIAN_POINT('Ctrl Pts',(12.1623797632096,99.8749999996106,3.95179673813132));
#295761=CARTESIAN_POINT('Ctrl Pts',(12.1623797632096,100.02499999961,-1.48946194470292E-15));
#295762=CARTESIAN_POINT('Ctrl Pts',(12.1623797632096,100.174999999609,-3.95179673813132));
#295763=CARTESIAN_POINT('Ctrl Pts',(9.83957192047848,100.324999999609,-7.14886745759505));
#295764=CARTESIAN_POINT('Ctrl Pts',(7.51676407774738,100.474999999608,-10.3459381770588));
#295765=CARTESIAN_POINT('Ctrl Pts',(3.75838203887366,100.624999999608,-11.5671105274568));
#295766=CARTESIAN_POINT('Ctrl Pts',(-7.12973138541271E-14,100.774999999607,
-12.7882828778549));
#295767=CARTESIAN_POINT('Ctrl Pts',(-3.7583820388738,100.924999999606,-11.5671105274568));
#295768=CARTESIAN_POINT('Ctrl Pts',(-7.51676407774753,101.074999999606,
-10.3459381770588));
#295769=CARTESIAN_POINT('Ctrl Pts',(-9.83957192047862,101.224999999605,
-7.14886745759505));
#295770=CARTESIAN_POINT('Ctrl Pts',(-12.1623797632097,101.374999999605,
-3.95179673813132));
#295771=CARTESIAN_POINT('Ctrl Pts',(-12.1623797632097,101.524999999604,
2.97892388940585E-15));
#295772=CARTESIAN_POINT('Ctrl Pts',(-12.1623797632097,101.674999999603,
3.95179673813133));
#295773=CARTESIAN_POINT('Ctrl Pts',(-9.83957192047862,101.824999999603,
7.14886745759505));
#295774=CARTESIAN_POINT('Ctrl Pts',(-7.51676407774752,101.974999999602,
10.3459381770588));
#295775=CARTESIAN_POINT('Ctrl Pts',(-3.7583820388738,102.124999999602,11.5671105274568));
#295776=CARTESIAN_POINT('Ctrl Pts',(-6.90289425513669E-14,102.274999999601,
12.7882828778549));
#295777=CARTESIAN_POINT('Ctrl Pts',(3.75838203887366,102.4249999996,11.5671105274568));
#295778=CARTESIAN_POINT('Ctrl Pts',(7.51676407774739,102.5749999996,10.3459381770588));
#295779=CARTESIAN_POINT('Ctrl Pts',(9.83957192047848,102.724999999599,7.14886745759505));
#295780=CARTESIAN_POINT('Ctrl Pts',(12.1623797632096,102.874999999599,3.95179673813132));
#295781=CARTESIAN_POINT('Ctrl Pts',(12.1623797632096,103.024999999598,-1.48946194470292E-15));
#295782=CARTESIAN_POINT('Ctrl Pts',(12.1623797632096,103.174999999597,-3.95179673813132));
#295783=CARTESIAN_POINT('Ctrl Pts',(9.83957192047848,103.324999999597,-7.14886745759505));
#295784=CARTESIAN_POINT('Ctrl Pts',(7.51676407774738,103.474999999596,-10.3459381770588));
#295785=CARTESIAN_POINT('Ctrl Pts',(3.75838203887366,103.624999999596,-11.5671105274568));
#295786=CARTESIAN_POINT('Ctrl Pts',(-7.3025023125789E-14,103.774999999595,
-12.7882828778549));
#295787=CARTESIAN_POINT('Ctrl Pts',(-3.7583820388738,103.924999999594,-11.5671105274568));
#295788=CARTESIAN_POINT('Ctrl Pts',(-7.51676407774753,104.074999999594,
-10.3459381770588));
#295789=CARTESIAN_POINT('Ctrl Pts',(-9.83957192047862,104.224999999593,
-7.14886745759505));
#295790=CARTESIAN_POINT('Ctrl Pts',(-12.1623797632097,104.374999999593,
-3.95179673813132));
#295791=CARTESIAN_POINT('Ctrl Pts',(-12.1623797632097,104.524999999592,
2.97892388940585E-15));
#295792=CARTESIAN_POINT('Ctrl Pts',(-12.1623797632097,104.674999999591,
3.95179673813133));
#295793=CARTESIAN_POINT('Ctrl Pts',(-9.83957192047862,104.824999999591,
7.14886745759505));
#295794=CARTESIAN_POINT('Ctrl Pts',(-7.51676407774753,104.97499999959,10.3459381770588));
#295795=CARTESIAN_POINT('Ctrl Pts',(-3.7583820388738,105.12499999959,11.5671105274568));
#295796=CARTESIAN_POINT('Ctrl Pts',(-7.07566518230287E-14,105.274999999589,
12.7882828778549));
#295797=CARTESIAN_POINT('Ctrl Pts',(3.75838203887366,105.424999999588,11.5671105274568));
#295798=CARTESIAN_POINT('Ctrl Pts',(7.51676407774738,105.574999999588,10.3459381770588));
#295799=CARTESIAN_POINT('Ctrl Pts',(9.83957192047848,105.724999999587,7.14886745759505));
#295800=CARTESIAN_POINT('Ctrl Pts',(12.1623797632096,105.874999999587,3.95179673813132));
#295801=CARTESIAN_POINT('Ctrl Pts',(12.1623797632096,106.024999999586,-1.48946194470292E-15));
#295802=CARTESIAN_POINT('Ctrl Pts',(12.1623797632096,106.174999999585,-3.95179673813132));
#295803=CARTESIAN_POINT('Ctrl Pts',(9.83957192047848,106.324999999585,-7.14886745759505));
#295804=CARTESIAN_POINT('Ctrl Pts',(7.51676407774738,106.474999999584,-10.3459381770588));
#295805=CARTESIAN_POINT('Ctrl Pts',(3.75838203887365,106.624999999584,-11.5671105274568));
#295806=CARTESIAN_POINT('Ctrl Pts',(-7.47527323974508E-14,106.774999999583,
-12.7882828778549));
#295807=CARTESIAN_POINT('Ctrl Pts',(-3.7583820388738,106.924999999582,-11.5671105274568));
#295808=CARTESIAN_POINT('Ctrl Pts',(-7.51676407774753,107.074999999582,
-10.3459381770588));
#295809=CARTESIAN_POINT('Ctrl Pts',(-9.83957192047862,107.224999999581,
-7.14886745759505));
#295810=CARTESIAN_POINT('Ctrl Pts',(-12.1623797632097,107.374999999581,
-3.95179673813132));
#295811=CARTESIAN_POINT('Ctrl Pts',(-12.1623797632097,107.52499999958,2.97892388940585E-15));
#295812=CARTESIAN_POINT('Ctrl Pts',(-12.1623797632097,107.674999999579,
3.95179673813133));
#295813=CARTESIAN_POINT('Ctrl Pts',(-9.83957192047862,107.824999999579,
7.14886745759505));
#295814=CARTESIAN_POINT('Ctrl Pts',(-7.51676407774753,107.974999999578,
10.3459381770588));
#295815=CARTESIAN_POINT('Ctrl Pts',(-3.7583820388738,108.124999999578,11.5671105274568));
#295816=CARTESIAN_POINT('Ctrl Pts',(-7.24843610946905E-14,108.274999999577,
12.7882828778549));
#295817=CARTESIAN_POINT('Ctrl Pts',(3.75838203887366,108.424999999576,11.5671105274568));
#295818=CARTESIAN_POINT('Ctrl Pts',(7.51676407774738,108.574999999576,10.3459381770588));
#295819=CARTESIAN_POINT('Ctrl Pts',(9.83957192047847,108.724999999575,7.14886745759505));
#295820=CARTESIAN_POINT('Ctrl Pts',(12.1623797632096,108.874999999575,3.95179673813132));
#295821=CARTESIAN_POINT('Ctrl Pts',(12.1623797632096,109.024999999574,-1.48946194470292E-15));
#295822=CARTESIAN_POINT('Ctrl Pts',(12.1623797632096,109.174999999573,-3.95179673813132));
#295823=CARTESIAN_POINT('Ctrl Pts',(9.83957192047847,109.324999999573,-7.14886745759505));
#295824=CARTESIAN_POINT('Ctrl Pts',(7.51676407774738,109.474999999572,-10.3459381770588));
#295825=CARTESIAN_POINT('Ctrl Pts',(3.75838203887365,109.624999999572,-11.5671105274568));
#295826=CARTESIAN_POINT('Ctrl Pts',(-7.64804416691126E-14,109.774999999571,
-12.7882828778549));
#295827=CARTESIAN_POINT('Ctrl Pts',(-3.7583820388738,109.92499999957,-11.5671105274568));
#295828=CARTESIAN_POINT('Ctrl Pts',(-7.51676407774753,110.07499999957,-10.3459381770588));
#295829=CARTESIAN_POINT('Ctrl Pts',(-9.83957192047862,110.224999999569,
-7.14886745759505));
#295830=CARTESIAN_POINT('Ctrl Pts',(-12.1623797632097,110.374999999569,
-3.95179673813132));
#295831=CARTESIAN_POINT('Ctrl Pts',(-12.1623797632097,110.524999999568,
2.97892388940585E-15));
#295832=CARTESIAN_POINT('Ctrl Pts',(-12.1623797632097,110.674999999567,
3.95179673813133));
#295833=CARTESIAN_POINT('Ctrl Pts',(-9.83957192047862,110.824999999567,
7.14886745759505));
#295834=CARTESIAN_POINT('Ctrl Pts',(-7.51676407774753,110.974999999566,
10.3459381770588));
#295835=CARTESIAN_POINT('Ctrl Pts',(-3.7583820388738,111.124999999566,11.5671105274568));
#295836=CARTESIAN_POINT('Ctrl Pts',(-7.42120703663524E-14,111.274999999565,
12.7882828778549));
#295837=CARTESIAN_POINT('Ctrl Pts',(3.75838203887365,111.424999999564,11.5671105274568));
#295838=CARTESIAN_POINT('Ctrl Pts',(7.51676407774738,111.574999999564,10.3459381770588));
#295839=CARTESIAN_POINT('Ctrl Pts',(9.83957192047847,111.724999999563,7.14886745759505));
#295840=CARTESIAN_POINT('Ctrl Pts',(12.1623797632096,111.874999999563,3.95179673813132));
#295841=CARTESIAN_POINT('Ctrl Pts',(12.1623797632096,112.024999999562,-1.48946194470292E-15));
#295842=CARTESIAN_POINT('Ctrl Pts',(12.1623797632096,112.174999999561,-3.95179673813132));
#295843=CARTESIAN_POINT('Ctrl Pts',(9.83957192047847,112.324999999561,-7.14886745759505));
#295844=CARTESIAN_POINT('Ctrl Pts',(7.51676407774738,112.47499999956,-10.3459381770588));
#295845=CARTESIAN_POINT('Ctrl Pts',(3.75838203887365,112.62499999956,-11.5671105274568));
#295846=CARTESIAN_POINT('Ctrl Pts',(-7.82081509407745E-14,112.774999999559,
-12.7882828778549));
#295847=CARTESIAN_POINT('Ctrl Pts',(-3.75838203887381,112.924999999558,
-11.5671105274568));
#295848=CARTESIAN_POINT('Ctrl Pts',(-7.51676407774753,113.074999999558,
-10.3459381770588));
#295849=CARTESIAN_POINT('Ctrl Pts',(-9.83957192047863,113.224999999557,
-7.14886745759505));
#295850=CARTESIAN_POINT('Ctrl Pts',(-12.1623797632097,113.374999999557,
-3.95179673813132));
#295851=CARTESIAN_POINT('Ctrl Pts',(-12.1623797632097,113.524999999556,
2.97892388940585E-15));
#295852=CARTESIAN_POINT('Ctrl Pts',(-12.1623797632097,113.674999999555,
3.95179673813133));
#295853=CARTESIAN_POINT('Ctrl Pts',(-9.83957192047863,113.824999999555,
7.14886745759505));
#295854=CARTESIAN_POINT('Ctrl Pts',(-7.51676407774753,113.974999999554,
10.3459381770588));
#295855=CARTESIAN_POINT('Ctrl Pts',(-3.7583820388738,114.124999999554,11.5671105274568));
#295856=CARTESIAN_POINT('Ctrl Pts',(-7.59397796380142E-14,114.274999999553,
12.7882828778549));
#295857=CARTESIAN_POINT('Ctrl Pts',(3.75838203887365,114.424999999552,11.5671105274568));
#295858=CARTESIAN_POINT('Ctrl Pts',(7.51676407774738,114.574999999552,10.3459381770588));
#295859=CARTESIAN_POINT('Ctrl Pts',(9.83957192047847,114.724999999551,7.14886745759505));
#295860=CARTESIAN_POINT('Ctrl Pts',(12.1623797632096,114.874999999551,3.95179673813132));
#295861=CARTESIAN_POINT('Ctrl Pts',(12.1623797632096,115.02499999955,-1.48946194470292E-15));
#295862=CARTESIAN_POINT('Ctrl Pts',(12.1623797632096,115.174999999549,-3.95179673813132));
#295863=CARTESIAN_POINT('Ctrl Pts',(9.83957192047847,115.324999999549,-7.14886745759505));
#295864=CARTESIAN_POINT('Ctrl Pts',(7.51676407774738,115.474999999548,-10.3459381770588));
#295865=CARTESIAN_POINT('Ctrl Pts',(3.75838203887365,115.624999999548,-11.5671105274568));
#295866=CARTESIAN_POINT('Ctrl Pts',(-7.99358602124363E-14,115.774999999547,
-12.7882828778549));
#295867=CARTESIAN_POINT('Ctrl Pts',(-3.75838203887381,115.924999999546,
-11.5671105274568));
#295868=CARTESIAN_POINT('Ctrl Pts',(-7.51676407774754,116.074999999546,
-10.3459381770588));
#295869=CARTESIAN_POINT('Ctrl Pts',(-9.83957192047863,116.224999999545,
-7.14886745759505));
#295870=CARTESIAN_POINT('Ctrl Pts',(-12.1623797632097,116.374999999545,
-3.95179673813132));
#295871=CARTESIAN_POINT('Ctrl Pts',(-12.1623797632097,116.524999999544,
2.97892388940585E-15));
#295872=CARTESIAN_POINT('Ctrl Pts',(-12.1623797632097,116.674999999543,
3.95179673813133));
#295873=CARTESIAN_POINT('Ctrl Pts',(-9.83957192047863,116.824999999543,
7.14886745759505));
#295874=CARTESIAN_POINT('Ctrl Pts',(-7.51676407774753,116.974999999542,
10.3459381770588));
#295875=CARTESIAN_POINT('Ctrl Pts',(-3.75838203887381,117.124999999542,
11.5671105274568));
#295876=CARTESIAN_POINT('Ctrl Pts',(-7.76674889096761E-14,117.274999999541,
12.7882828778549));
#295877=CARTESIAN_POINT('Ctrl Pts',(3.75838203887365,117.42499999954,11.5671105274568));
#295878=CARTESIAN_POINT('Ctrl Pts',(7.51676407774738,117.57499999954,10.3459381770588));
#295879=CARTESIAN_POINT('Ctrl Pts',(9.83957192047847,117.724999999539,7.14886745759505));
#295880=CARTESIAN_POINT('Ctrl Pts',(12.1623797632096,117.874999999539,3.95179673813132));
#295881=CARTESIAN_POINT('Ctrl Pts',(12.1623797632096,118.024999999538,-1.48946194470292E-15));
#295882=CARTESIAN_POINT('Ctrl Pts',(12.1623797632096,118.174999999537,-3.95179673813132));
#295883=CARTESIAN_POINT('Ctrl Pts',(9.83957192047847,118.324999999537,-7.14886745759505));
#295884=CARTESIAN_POINT('Ctrl Pts',(7.51676407774737,118.474999999536,-10.3459381770588));
#295885=CARTESIAN_POINT('Ctrl Pts',(3.75838203887365,118.624999999536,-11.5671105274568));
#295886=CARTESIAN_POINT('Ctrl Pts',(-8.16635694840981E-14,118.774999999535,
-12.7882828778549));
#295887=CARTESIAN_POINT('Ctrl Pts',(-3.75838203887381,118.924999999534,
-11.5671105274568));
#295888=CARTESIAN_POINT('Ctrl Pts',(-7.51676407774754,119.074999999534,
-10.3459381770588));
#295889=CARTESIAN_POINT('Ctrl Pts',(-9.83957192047863,119.224999999533,
-7.14886745759505));
#295890=CARTESIAN_POINT('Ctrl Pts',(-12.1623797632097,119.374999999533,
-3.95179673813132));
#295891=CARTESIAN_POINT('Ctrl Pts',(-12.1623797632097,119.524999999532,
2.97892388940585E-15));
#295892=CARTESIAN_POINT('Ctrl Pts',(-12.1623797632097,119.674999999531,
3.95179673813133));
#295893=CARTESIAN_POINT('Ctrl Pts',(-9.83957192047863,119.824999999531,
7.14886745759505));
#295894=CARTESIAN_POINT('Ctrl Pts',(-7.51676407774754,119.97499999953,10.3459381770588));
#295895=CARTESIAN_POINT('Ctrl Pts',(-3.75838203887381,120.12499999953,11.5671105274568));
#295896=CARTESIAN_POINT('Ctrl Pts',(-7.93951981813379E-14,120.274999999529,
12.7882828778549));
#295897=CARTESIAN_POINT('Ctrl Pts',(3.75838203887365,120.424999999528,11.5671105274568));
#295898=CARTESIAN_POINT('Ctrl Pts',(7.51676407774738,120.574999999528,10.3459381770588));
#295899=CARTESIAN_POINT('Ctrl Pts',(9.83957192047847,120.724999999527,7.14886745759505));
#295900=CARTESIAN_POINT('Ctrl Pts',(12.1623797632096,120.874999999527,3.95179673813132));
#295901=CARTESIAN_POINT('Ctrl Pts',(12.1623797632096,121.024999999526,-1.48946194470292E-15));
#295902=CARTESIAN_POINT('Ctrl Pts',(12.1623797632096,121.174999999525,-3.95179673813132));
#295903=CARTESIAN_POINT('Ctrl Pts',(9.83957192047847,121.324999999525,-7.14886745759505));
#295904=CARTESIAN_POINT('Ctrl Pts',(7.51676407774737,121.474999999524,-10.3459381770588));
#295905=CARTESIAN_POINT('Ctrl Pts',(3.75838203887364,121.624999999524,-11.5671105274568));
#295906=CARTESIAN_POINT('Ctrl Pts',(-8.339127875576E-14,121.774999999523,
-12.7882828778549));
#295907=CARTESIAN_POINT('Ctrl Pts',(-3.75838203887381,121.924999999522,
-11.5671105274568));
#295908=CARTESIAN_POINT('Ctrl Pts',(-7.51676407774754,122.074999999522,
-10.3459381770588));
#295909=CARTESIAN_POINT('Ctrl Pts',(-9.83957192047863,122.224999999521,
-7.14886745759505));
#295910=CARTESIAN_POINT('Ctrl Pts',(-12.1623797632097,122.374999999521,
-3.95179673813132));
#295911=CARTESIAN_POINT('Ctrl Pts',(-12.1623797632097,122.52499999952,2.97892388940585E-15));
#295912=CARTESIAN_POINT('Ctrl Pts',(-12.1623797632097,122.674999999519,
3.95179673813133));
#295913=CARTESIAN_POINT('Ctrl Pts',(-9.83957192047863,122.824999999519,
7.14886745759505));
#295914=CARTESIAN_POINT('Ctrl Pts',(-7.51676407774754,122.974999999518,
10.3459381770588));
#295915=CARTESIAN_POINT('Ctrl Pts',(-3.75838203887381,123.124999999518,
11.5671105274568));
#295916=CARTESIAN_POINT('Ctrl Pts',(-8.11229074529997E-14,123.274999999517,
12.7882828778549));
#295917=CARTESIAN_POINT('Ctrl Pts',(3.75838203887365,123.424999999516,11.5671105274568));
#295918=CARTESIAN_POINT('Ctrl Pts',(7.51676407774737,123.574999999516,10.3459381770588));
#295919=CARTESIAN_POINT('Ctrl Pts',(9.83957192047846,123.724999999515,7.14886745759505));
#295920=CARTESIAN_POINT('Ctrl Pts',(12.1623797632096,123.874999999515,3.95179673813132));
#295921=CARTESIAN_POINT('Ctrl Pts',(12.1623797632096,124.024999999514,-1.48946194470292E-15));
#295922=CARTESIAN_POINT('Ctrl Pts',(12.1623797632096,124.174999999513,-3.95179673813132));
#295923=CARTESIAN_POINT('Ctrl Pts',(9.83957192047846,124.324999999513,-7.14886745759505));
#295924=CARTESIAN_POINT('Ctrl Pts',(7.51676407774737,124.474999999512,-10.3459381770588));
#295925=CARTESIAN_POINT('Ctrl Pts',(3.75838203887364,124.624999999512,-11.5671105274568));
#295926=CARTESIAN_POINT('Ctrl Pts',(-8.51189880274219E-14,124.774999999511,
-12.7882828778549));
#295927=CARTESIAN_POINT('Ctrl Pts',(-3.75838203887381,124.92499999951,-11.5671105274568));
#295928=CARTESIAN_POINT('Ctrl Pts',(-7.51676407774754,125.07499999951,-10.3459381770588));
#295929=CARTESIAN_POINT('Ctrl Pts',(-9.83957192047863,125.224999999509,
-7.14886745759505));
#295930=CARTESIAN_POINT('Ctrl Pts',(-12.1623797632097,125.374999999509,
-3.95179673813132));
#295931=CARTESIAN_POINT('Ctrl Pts',(-12.1623797632097,125.524999999508,
2.97892388940585E-15));
#295932=CARTESIAN_POINT('Ctrl Pts',(-12.1623797632097,125.674999999507,
3.95179673813133));
#295933=CARTESIAN_POINT('Ctrl Pts',(-9.83957192047863,125.824999999507,
7.14886745759505));
#295934=CARTESIAN_POINT('Ctrl Pts',(-7.51676407774754,125.974999999506,
10.3459381770588));
#295935=CARTESIAN_POINT('Ctrl Pts',(-3.75838203887381,126.124999999506,
11.5671105274568));
#295936=CARTESIAN_POINT('Ctrl Pts',(-8.28506167246616E-14,126.274999999505,
12.7882828778549));
#295937=CARTESIAN_POINT('Ctrl Pts',(3.75838203887364,126.424999999504,11.5671105274568));
#295938=CARTESIAN_POINT('Ctrl Pts',(7.51676407774737,126.574999999504,10.3459381770588));
#295939=CARTESIAN_POINT('Ctrl Pts',(9.83957192047846,126.724999999503,7.14886745759505));
#295940=CARTESIAN_POINT('Ctrl Pts',(12.1623797632096,126.874999999503,3.95179673813132));
#295941=CARTESIAN_POINT('Ctrl Pts',(12.1623797632096,127.024999999502,-1.48946194470292E-15));
#295942=CARTESIAN_POINT('Ctrl Pts',(12.1623797632096,127.174999999501,-3.95179673813132));
#295943=CARTESIAN_POINT('Ctrl Pts',(9.83957192047846,127.324999999501,-7.14886745759505));
#295944=CARTESIAN_POINT('Ctrl Pts',(7.51676407774737,127.4749999995,-10.3459381770588));
#295945=CARTESIAN_POINT('Ctrl Pts',(3.75838203887364,127.6249999995,-11.5671105274568));
#295946=CARTESIAN_POINT('Ctrl Pts',(-8.68466972990837E-14,127.774999999499,
-12.7882828778549));
#295947=CARTESIAN_POINT('Ctrl Pts',(-3.75838203887381,127.924999999498,
-11.5671105274568));
#295948=CARTESIAN_POINT('Ctrl Pts',(-7.51676407774754,128.074999999498,
-10.3459381770588));
#295949=CARTESIAN_POINT('Ctrl Pts',(-9.83957192047864,128.224999999497,
-7.14886745759505));
#295950=CARTESIAN_POINT('Ctrl Pts',(-12.1623797632097,128.374999999497,
-3.95179673813132));
#295951=CARTESIAN_POINT('Ctrl Pts',(-12.1623797632097,128.524999999496,
2.97892388940585E-15));
#295952=CARTESIAN_POINT('Ctrl Pts',(-12.1623797632097,128.674999999495,
3.95179673813133));
#295953=CARTESIAN_POINT('Ctrl Pts',(-9.83957192047864,128.824999999495,
7.14886745759505));
#295954=CARTESIAN_POINT('Ctrl Pts',(-7.51676407774754,128.974999999494,
10.3459381770588));
#295955=CARTESIAN_POINT('Ctrl Pts',(-3.75838203887381,129.124999999494,
11.5671105274568));
#295956=CARTESIAN_POINT('Ctrl Pts',(-8.45783259963234E-14,129.274999999493,
12.7882828778549));
#295957=CARTESIAN_POINT('Ctrl Pts',(3.75838203887364,129.424999999492,11.5671105274568));
#295958=CARTESIAN_POINT('Ctrl Pts',(7.51676407774737,129.574999999492,10.3459381770588));
#295959=CARTESIAN_POINT('Ctrl Pts',(9.83957192047846,129.724999999491,7.14886745759505));
#295960=CARTESIAN_POINT('Ctrl Pts',(12.1623797632096,129.874999999491,3.95179673813132));
#295961=CARTESIAN_POINT('Ctrl Pts',(12.1623797632096,130.02499999949,-1.48946194470292E-15));
#295962=CARTESIAN_POINT('Ctrl Pts',(12.1623797632096,130.174999999489,-3.95179673813132));
#295963=CARTESIAN_POINT('Ctrl Pts',(9.83957192047846,130.324999999489,-7.14886745759505));
#295964=CARTESIAN_POINT('Ctrl Pts',(7.51676407774737,130.474999999488,-10.3459381770588));
#295965=CARTESIAN_POINT('Ctrl Pts',(3.75838203887364,130.624999999488,-11.5671105274568));
#295966=CARTESIAN_POINT('Ctrl Pts',(-8.85744065707455E-14,130.774999999487,
-12.7882828778549));
#295967=CARTESIAN_POINT('Ctrl Pts',(-3.75838203887382,130.924999999486,
-11.5671105274568));
#295968=CARTESIAN_POINT('Ctrl Pts',(-7.51676407774754,131.074999999486,
-10.3459381770588));
#295969=CARTESIAN_POINT('Ctrl Pts',(-9.83957192047864,131.224999999485,
-7.14886745759505));
#295970=CARTESIAN_POINT('Ctrl Pts',(-12.1623797632097,131.374999999485,
-3.95179673813132));
#295971=CARTESIAN_POINT('Ctrl Pts',(-12.1623797632097,131.524999999484,
2.97892388940585E-15));
#295972=CARTESIAN_POINT('Ctrl Pts',(-12.1623797632097,131.674999999483,
3.95179673813133));
#295973=CARTESIAN_POINT('Ctrl Pts',(-9.83957192047864,131.824999999483,
7.14886745759505));
#295974=CARTESIAN_POINT('Ctrl Pts',(-7.51676407774754,131.974999999482,
10.3459381770588));
#295975=CARTESIAN_POINT('Ctrl Pts',(-3.75838203887381,132.124999999482,
11.5671105274568));
#295976=CARTESIAN_POINT('Ctrl Pts',(-8.63060352679853E-14,132.274999999481,
12.7882828778549));
#295977=CARTESIAN_POINT('Ctrl Pts',(3.75838203887364,132.42499999948,11.5671105274568));
#295978=CARTESIAN_POINT('Ctrl Pts',(7.51676407774737,132.57499999948,10.3459381770588));
#295979=CARTESIAN_POINT('Ctrl Pts',(9.83957192047846,132.724999999479,7.14886745759505));
#295980=CARTESIAN_POINT('Ctrl Pts',(12.1623797632096,132.874999999479,3.95179673813132));
#295981=CARTESIAN_POINT('Ctrl Pts',(12.1623797632096,133.024999999478,-1.48946194470292E-15));
#295982=CARTESIAN_POINT('Ctrl Pts',(12.1623797632096,133.174999999477,-3.95179673813132));
#295983=CARTESIAN_POINT('Ctrl Pts',(9.83957192047846,133.324999999477,-7.14886745759505));
#295984=CARTESIAN_POINT('Ctrl Pts',(7.51676407774736,133.474999999476,-10.3459381770588));
#295985=CARTESIAN_POINT('Ctrl Pts',(3.75838203887364,133.624999999476,-11.5671105274568));
#295986=CARTESIAN_POINT('Ctrl Pts',(-9.03021158424074E-14,133.774999999475,
-12.7882828778549));
#295987=CARTESIAN_POINT('Ctrl Pts',(-3.75838203887382,133.924999999474,
-11.5671105274568));
#295988=CARTESIAN_POINT('Ctrl Pts',(-7.51676407774755,134.074999999474,
-10.3459381770588));
#295989=CARTESIAN_POINT('Ctrl Pts',(-9.83957192047864,134.224999999473,
-7.14886745759505));
#295990=CARTESIAN_POINT('Ctrl Pts',(-12.1623797632097,134.374999999473,
-3.95179673813132));
#295991=CARTESIAN_POINT('Ctrl Pts',(-12.1623797632097,134.524999999472,
2.97892388940585E-15));
#295992=CARTESIAN_POINT('Ctrl Pts',(-12.1623797632097,134.674999999471,
3.95179673813133));
#295993=CARTESIAN_POINT('Ctrl Pts',(-9.83957192047864,134.824999999471,
7.14886745759505));
#295994=CARTESIAN_POINT('Ctrl Pts',(-7.51676407774754,134.97499999947,10.3459381770588));
#295995=CARTESIAN_POINT('Ctrl Pts',(-3.75838203887382,135.12499999947,11.5671105274568));
#295996=CARTESIAN_POINT('Ctrl Pts',(-8.80337445396471E-14,135.274999999469,
12.7882828778549));
#295997=CARTESIAN_POINT('Ctrl Pts',(3.75838203887364,135.424999999468,11.5671105274568));
#295998=CARTESIAN_POINT('Ctrl Pts',(7.51676407774737,135.574999999468,10.3459381770588));
#295999=CARTESIAN_POINT('Ctrl Pts',(9.83957192047846,135.724999999467,7.14886745759505));
#296000=CARTESIAN_POINT('Ctrl Pts',(12.1623797632096,135.874999999467,3.95179673813132));
#296001=CARTESIAN_POINT('Ctrl Pts',(12.1623797632096,136.024999999466,-1.48946194470292E-15));
#296002=CARTESIAN_POINT('Ctrl Pts',(12.1623797632095,136.174999999465,-3.95179673813132));
#296003=CARTESIAN_POINT('Ctrl Pts',(9.83957192047846,136.324999999465,-7.14886745759505));
#296004=CARTESIAN_POINT('Ctrl Pts',(7.51676407774736,136.474999999464,-10.3459381770588));
#296005=CARTESIAN_POINT('Ctrl Pts',(3.75838203887364,136.624999999464,-11.5671105274568));
#296006=CARTESIAN_POINT('Ctrl Pts',(-9.20298251140692E-14,136.774999999463,
-12.7882828778549));
#296007=CARTESIAN_POINT('Ctrl Pts',(-3.75838203887382,136.924999999462,
-11.5671105274568));
#296008=CARTESIAN_POINT('Ctrl Pts',(-7.51676407774755,137.074999999462,
-10.3459381770588));
#296009=CARTESIAN_POINT('Ctrl Pts',(-9.83957192047864,137.224999999461,
-7.14886745759505));
#296010=CARTESIAN_POINT('Ctrl Pts',(-12.1623797632097,137.374999999461,
-3.95179673813132));
#296011=CARTESIAN_POINT('Ctrl Pts',(-12.1623797632097,137.52499999946,2.97892388940585E-15));
#296012=CARTESIAN_POINT('Ctrl Pts',(-12.1623797632097,137.674999999459,
3.95179673813133));
#296013=CARTESIAN_POINT('Ctrl Pts',(-9.83957192047864,137.824999999459,
7.14886745759505));
#296014=CARTESIAN_POINT('Ctrl Pts',(-7.51676407774755,137.974999999458,
10.3459381770588));
#296015=CARTESIAN_POINT('Ctrl Pts',(-3.75838203887382,138.124999999458,
11.5671105274568));
#296016=CARTESIAN_POINT('Ctrl Pts',(-8.97614538113089E-14,138.274999999457,
12.7882828778549));
#296017=CARTESIAN_POINT('Ctrl Pts',(3.75838203887364,138.424999999456,11.5671105274568));
#296018=CARTESIAN_POINT('Ctrl Pts',(7.51676407774736,138.574999999456,10.3459381770588));
#296019=CARTESIAN_POINT('Ctrl Pts',(9.83957192047846,138.724999999455,7.14886745759505));
#296020=CARTESIAN_POINT('Ctrl Pts',(12.1623797632096,138.874999999455,3.95179673813132));
#296021=CARTESIAN_POINT('Ctrl Pts',(12.1623797632096,139.024999999454,-1.48946194470292E-15));
#296022=CARTESIAN_POINT('Ctrl Pts',(12.1623797632095,139.174999999453,-3.95179673813132));
#296023=CARTESIAN_POINT('Ctrl Pts',(9.83957192047846,139.324999999453,-7.14886745759505));
#296024=CARTESIAN_POINT('Ctrl Pts',(7.51676407774736,139.474999999452,-10.3459381770588));
#296025=CARTESIAN_POINT('Ctrl Pts',(3.75838203887363,139.624999999452,-11.5671105274568));
#296026=CARTESIAN_POINT('Ctrl Pts',(-9.3757534385731E-14,139.774999999451,
-12.7882828778549));
#296027=CARTESIAN_POINT('Ctrl Pts',(-3.75838203887382,139.92499999945,-11.5671105274568));
#296028=CARTESIAN_POINT('Ctrl Pts',(-7.51676407774755,140.07499999945,-10.3459381770588));
#296029=CARTESIAN_POINT('Ctrl Pts',(-9.83957192047864,140.224999999449,
-7.14886745759505));
#296030=CARTESIAN_POINT('Ctrl Pts',(-12.1623797632097,140.374999999449,
-3.95179673813132));
#296031=CARTESIAN_POINT('Ctrl Pts',(-12.1623797632097,140.524999999448,
2.97892388940585E-15));
#296032=CARTESIAN_POINT('Ctrl Pts',(-12.1623797632097,140.674999999447,
3.95179673813133));
#296033=CARTESIAN_POINT('Ctrl Pts',(-9.83957192047864,140.824999999447,
7.14886745759505));
#296034=CARTESIAN_POINT('Ctrl Pts',(-7.51676407774755,140.974999999446,
10.3459381770588));
#296035=CARTESIAN_POINT('Ctrl Pts',(-3.75838203887382,141.124999999446,
11.5671105274568));
#296036=CARTESIAN_POINT('Ctrl Pts',(-9.14891630829708E-14,141.274999999445,
12.7882828778549));
#296037=CARTESIAN_POINT('Ctrl Pts',(3.75838203887364,141.424999999444,11.5671105274568));
#296038=CARTESIAN_POINT('Ctrl Pts',(7.51676407774736,141.574999999444,10.3459381770588));
#296039=CARTESIAN_POINT('Ctrl Pts',(9.83957192047845,141.724999999443,7.14886745759505));
#296040=CARTESIAN_POINT('Ctrl Pts',(12.1623797632095,141.874999999443,3.95179673813132));
#296041=CARTESIAN_POINT('Ctrl Pts',(12.1623797632095,142.024999999442,-1.48946194470292E-15));
#296042=CARTESIAN_POINT('Ctrl Pts',(12.1623797632095,142.174999999441,-3.95179673813132));
#296043=CARTESIAN_POINT('Ctrl Pts',(9.83957192047845,142.324999999441,-7.14886745759505));
#296044=CARTESIAN_POINT('Ctrl Pts',(7.51676407774736,142.47499999944,-10.3459381770588));
#296045=CARTESIAN_POINT('Ctrl Pts',(3.75838203887363,142.62499999944,-11.5671105274568));
#296046=CARTESIAN_POINT('Ctrl Pts',(-9.54852436573929E-14,142.774999999439,
-12.7882828778549));
#296047=CARTESIAN_POINT('Ctrl Pts',(-3.75838203887382,142.924999999438,
-11.5671105274568));
#296048=CARTESIAN_POINT('Ctrl Pts',(-7.51676407774755,143.074999999438,
-10.3459381770588));
#296049=CARTESIAN_POINT('Ctrl Pts',(-9.83957192047864,143.224999999437,
-7.14886745759505));
#296050=CARTESIAN_POINT('Ctrl Pts',(-12.1623797632097,143.374999999437,
-3.95179673813132));
#296051=CARTESIAN_POINT('Ctrl Pts',(-12.1623797632097,143.524999999436,
2.97892388940585E-15));
#296052=CARTESIAN_POINT('Ctrl Pts',(-12.1623797632097,143.674999999435,
3.95179673813133));
#296053=CARTESIAN_POINT('Ctrl Pts',(-9.83957192047864,143.824999999435,
7.14886745759505));
#296054=CARTESIAN_POINT('Ctrl Pts',(-7.51676407774755,143.974999999434,
10.3459381770588));
#296055=CARTESIAN_POINT('Ctrl Pts',(-3.75838203887382,144.124999999434,
11.5671105274568));
#296056=CARTESIAN_POINT('Ctrl Pts',(-9.32168723546326E-14,144.274999999433,
12.7882828778549));
#296057=CARTESIAN_POINT('Ctrl Pts',(3.75838203887363,144.424999999432,11.5671105274568));
#296058=CARTESIAN_POINT('Ctrl Pts',(7.51676407774736,144.574999999432,10.3459381770588));
#296059=CARTESIAN_POINT('Ctrl Pts',(9.83957192047845,144.724999999431,7.14886745759505));
#296060=CARTESIAN_POINT('Ctrl Pts',(12.1623797632095,144.874999999431,3.95179673813132));
#296061=CARTESIAN_POINT('Ctrl Pts',(12.1623797632095,145.02499999943,-1.48946194470292E-15));
#296062=CARTESIAN_POINT('Ctrl Pts',(12.1623797632095,145.174999999429,-3.95179673813132));
#296063=CARTESIAN_POINT('Ctrl Pts',(9.83957192047845,145.324999999429,-7.14886745759505));
#296064=CARTESIAN_POINT('Ctrl Pts',(7.51676407774736,145.474999999428,-10.3459381770588));
#296065=CARTESIAN_POINT('Ctrl Pts',(3.75838203887363,145.624999999428,-11.5671105274568));
#296066=CARTESIAN_POINT('Ctrl Pts',(-9.72129529290547E-14,145.774999999427,
-12.7882828778549));
#296067=CARTESIAN_POINT('Ctrl Pts',(-3.75838203887382,145.924999999426,
-11.5671105274568));
#296068=CARTESIAN_POINT('Ctrl Pts',(-7.51676407774755,146.074999999426,
-10.3459381770588));
#296069=CARTESIAN_POINT('Ctrl Pts',(-9.83957192047865,146.224999999425,
-7.14886745759505));
#296070=CARTESIAN_POINT('Ctrl Pts',(-12.1623797632097,146.374999999425,
-3.95179673813132));
#296071=CARTESIAN_POINT('Ctrl Pts',(-12.1623797632097,146.524999999424,
2.97892388940585E-15));
#296072=CARTESIAN_POINT('Ctrl Pts',(-12.1623797632097,146.674999999423,
3.95179673813133));
#296073=CARTESIAN_POINT('Ctrl Pts',(-9.83957192047865,146.824999999423,
7.14886745759505));
#296074=CARTESIAN_POINT('Ctrl Pts',(-7.51676407774755,146.974999999422,
10.3459381770588));
#296075=CARTESIAN_POINT('Ctrl Pts',(-3.75838203887382,147.124999999422,
11.5671105274568));
#296076=CARTESIAN_POINT('Ctrl Pts',(-9.49445816262944E-14,147.274999999421,
12.7882828778549));
#296077=CARTESIAN_POINT('Ctrl Pts',(3.75838203887363,147.42499999942,11.5671105274568));
#296078=CARTESIAN_POINT('Ctrl Pts',(7.51676407774736,147.57499999942,10.3459381770588));
#296079=CARTESIAN_POINT('Ctrl Pts',(9.83957192047845,147.724999999419,7.14886745759505));
#296080=CARTESIAN_POINT('Ctrl Pts',(12.1623797632095,147.874999999419,3.95179673813132));
#296081=CARTESIAN_POINT('Ctrl Pts',(12.1623797632095,148.024999999418,-1.48946194470292E-15));
#296082=CARTESIAN_POINT('Ctrl Pts',(12.1623797632095,148.174999999417,-3.95179673813132));
#296083=CARTESIAN_POINT('Ctrl Pts',(9.83957192047845,148.324999999417,-7.14886745759505));
#296084=CARTESIAN_POINT('Ctrl Pts',(7.51676407774736,148.474999999416,-10.3459381770588));
#296085=CARTESIAN_POINT('Ctrl Pts',(3.75838203887363,148.624999999416,-11.5671105274568));
#296086=CARTESIAN_POINT('Ctrl Pts',(-9.89406622007166E-14,148.774999999415,
-12.7882828778549));
#296087=CARTESIAN_POINT('Ctrl Pts',(-3.75838203887383,148.924999999414,
-11.5671105274568));
#296088=CARTESIAN_POINT('Ctrl Pts',(-7.51676407774756,149.074999999414,
-10.3459381770588));
#296089=CARTESIAN_POINT('Ctrl Pts',(-9.83957192047865,149.224999999413,
-7.14886745759505));
#296090=CARTESIAN_POINT('Ctrl Pts',(-12.1623797632097,149.374999999413,
-3.95179673813132));
#296091=CARTESIAN_POINT('Ctrl Pts',(-12.1623797632097,149.524999999412,
2.97892388940585E-15));
#296092=CARTESIAN_POINT('Ctrl Pts',(-12.1623797632097,149.674999999411,
3.95179673813133));
#296093=CARTESIAN_POINT('Ctrl Pts',(-9.83957192047865,149.824999999411,
7.14886745759505));
#296094=CARTESIAN_POINT('Ctrl Pts',(-7.51676407774755,149.97499999941,10.3459381770588));
#296095=CARTESIAN_POINT('Ctrl Pts',(-3.75838203887382,150.12499999941,11.5671105274568));
#296096=CARTESIAN_POINT('Ctrl Pts',(-9.66722908979563E-14,150.274999999409,
12.7882828778549));
#296097=CARTESIAN_POINT('Ctrl Pts',(3.75838203887363,150.424999999408,11.5671105274568));
#296098=CARTESIAN_POINT('Ctrl Pts',(7.51676407774736,150.574999999408,10.3459381770588));
#296099=CARTESIAN_POINT('Ctrl Pts',(9.83957192047845,150.724999999407,7.14886745759505));
#296100=CARTESIAN_POINT('Ctrl Pts',(12.1623797632095,150.874999999407,3.95179673813132));
#296101=CARTESIAN_POINT('Ctrl Pts',(12.1623797632095,151.024999999406,-1.48946194470292E-15));
#296102=CARTESIAN_POINT('Ctrl Pts',(12.1623797632095,151.174999999405,-3.95179673813132));
#296103=CARTESIAN_POINT('Ctrl Pts',(9.83957192047845,151.324999999405,-7.14886745759505));
#296104=CARTESIAN_POINT('Ctrl Pts',(7.51676407774736,151.474999999404,-10.3459381770588));
#296105=CARTESIAN_POINT('Ctrl Pts',(3.75838203887363,151.624999999404,-11.5671105274568));
#296106=CARTESIAN_POINT('Ctrl Pts',(-1.00668371472378E-13,151.774999999403,
-12.7882828778549));
#296107=CARTESIAN_POINT('Ctrl Pts',(-3.75838203887383,151.924999999402,
-11.5671105274568));
#296108=CARTESIAN_POINT('Ctrl Pts',(-7.51676407774756,152.074999999402,
-10.3459381770588));
#296109=CARTESIAN_POINT('Ctrl Pts',(-9.83957192047865,152.224999999401,
-7.14886745759505));
#296110=CARTESIAN_POINT('Ctrl Pts',(-12.1623797632097,152.374999999401,
-3.95179673813132));
#296111=CARTESIAN_POINT('Ctrl Pts',(-12.1623797632097,152.5249999994,2.97892388940585E-15));
#296112=CARTESIAN_POINT('Ctrl Pts',(-12.1623797632097,152.674999999399,
3.95179673813133));
#296113=CARTESIAN_POINT('Ctrl Pts',(-9.83957192047865,152.824999999399,
7.14886745759505));
#296114=CARTESIAN_POINT('Ctrl Pts',(-7.51676407774756,152.974999999398,
10.3459381770588));
#296115=CARTESIAN_POINT('Ctrl Pts',(-3.75838203887383,153.124999999398,
11.5671105274568));
#296116=CARTESIAN_POINT('Ctrl Pts',(-9.84000001696181E-14,153.274999999397,
12.7882828778549));
#296117=CARTESIAN_POINT('Ctrl Pts',(3.75838203887363,153.424999999396,11.5671105274568));
#296118=CARTESIAN_POINT('Ctrl Pts',(7.51676407774736,153.574999999396,10.3459381770588));
#296119=CARTESIAN_POINT('Ctrl Pts',(9.83957192047845,153.724999999395,7.14886745759505));
#296120=CARTESIAN_POINT('Ctrl Pts',(12.1623797632095,153.874999999395,3.95179673813132));
#296121=CARTESIAN_POINT('Ctrl Pts',(12.1623797632095,154.024999999394,-1.48946194470292E-15));
#296122=CARTESIAN_POINT('Ctrl Pts',(12.1623797632095,154.174999999393,-3.95179673813132));
#296123=CARTESIAN_POINT('Ctrl Pts',(9.83957192047845,154.324999999393,-7.14886745759505));
#296124=CARTESIAN_POINT('Ctrl Pts',(7.51676407774735,154.474999999392,-10.3459381770588));
#296125=CARTESIAN_POINT('Ctrl Pts',(3.75838203887363,154.624999999392,-11.5671105274568));
#296126=CARTESIAN_POINT('Ctrl Pts',(-1.0239608074404E-13,154.774999999391,
-12.7882828778549));
#296127=CARTESIAN_POINT('Ctrl Pts',(-3.75838203887383,154.92499999939,-11.5671105274568));
#296128=CARTESIAN_POINT('Ctrl Pts',(-9.73188510064477,91.186,-2.51434197826682));
#296129=CARTESIAN_POINT('Ctrl Pts',(-9.60478494878794,91.186,-3.25683227280792));
#296130=CARTESIAN_POINT('Ctrl Pts',(-9.39476270715683,91.186,-3.98267472639531));
#296131=CARTESIAN_POINT('Ctrl Pts',(-8.80110729028426,91.186,-5.41178772721597));
#296132=CARTESIAN_POINT('Ctrl Pts',(-8.4113556697725,91.186,-6.10153554674208));
#296133=CARTESIAN_POINT('Ctrl Pts',(-7.1594638773909,91.186,-7.83754033530839));
#296134=CARTESIAN_POINT('Ctrl Pts',(-6.16336234352202,91.1859999986483,
-8.77422666970583));
#296135=CARTESIAN_POINT('Ctrl Pts',(-3.45643278380831,91.1859999986483,
-10.4839899487996));
#296136=CARTESIAN_POINT('Ctrl Pts',(-1.95983265628982,91.186,-10.8625608372954));
#296137=CARTESIAN_POINT('Ctrl Pts',(0.487656647838607,91.186,-11.266528763347));
#296138=CARTESIAN_POINT('Ctrl Pts',(1.98204486733221,91.186,-11.2131410528978));
#296139=CARTESIAN_POINT('Ctrl Pts',(4.44770027945387,91.186,-10.6233745503084));
#296140=CARTESIAN_POINT('Ctrl Pts',(5.84635722463119,91.186,-10.1391958336611));
#296141=CARTESIAN_POINT('Ctrl Pts',(8.49239651382177,91.186,-8.32644545870485));
#296142=CARTESIAN_POINT('Ctrl Pts',(9.52161704638934,91.186,-7.28514894739878));
#296143=CARTESIAN_POINT('Ctrl Pts',(10.3435570531184,91.186,-6.08365247930268));
#296144=CARTESIAN_POINT('Ctrl Pts',(10.0514428414941,128.806249999495,-1.23094673026484E-15));
#296145=CARTESIAN_POINT('Ctrl Pts',(10.0514428414941,128.956249999495,-3.26591175476071));
#296146=CARTESIAN_POINT('Ctrl Pts',(8.1317880767571,129.106249999494,-5.90808986649102));
#296147=CARTESIAN_POINT('Ctrl Pts',(6.21213331202013,129.256249999493,-8.55026797822134));
#296148=CARTESIAN_POINT('Ctrl Pts',(3.10606665601002,129.406249999493,-9.5594902125713));
#296149=CARTESIAN_POINT('Ctrl Pts',(-8.77366151879469E-14,129.556249999492,
-10.5687124469213));
#296150=CARTESIAN_POINT('Ctrl Pts',(-3.1060666560102,129.706249999492,-9.5594902125713));
#296151=CARTESIAN_POINT('Ctrl Pts',(-6.2121333120203,129.856249999491,-8.55026797822134));
#296152=CARTESIAN_POINT('Ctrl Pts',(-8.13178807675728,130.00624999949,-5.90808986649102));
#296153=CARTESIAN_POINT('Ctrl Pts',(-10.0514428414943,130.15624999949,-3.2659117547607));
#296154=CARTESIAN_POINT('Ctrl Pts',(-10.0514428414943,130.306249999489,
2.46189346052968E-15));
#296155=CARTESIAN_POINT('Ctrl Pts',(-10.0514428414943,130.456249999489,
3.26591175476071));
#296156=CARTESIAN_POINT('Ctrl Pts',(-8.13178807675728,130.606249999488,
5.90808986649102));
#296157=CARTESIAN_POINT('Ctrl Pts',(-6.80976210866172,130.709551852955,
7.72770250737114));
#296158=CARTESIAN_POINT('Ctrl Pts',(-4.83831102398129,130.817307158506,
8.81034900733485));
#296159=CARTESIAN_POINT('Ctrl Pts',(-12.1623797632103,-3.28749999997638,
2.97892388940601E-15));
#296160=CARTESIAN_POINT('Ctrl Pts',(-12.1623797632103,-3.13749999997698,
3.95179673813154));
#296161=CARTESIAN_POINT('Ctrl Pts',(-9.83957192047908,-2.98749999997758,
7.14886745759543));
#296162=CARTESIAN_POINT('Ctrl Pts',(-7.51676407774787,-2.83749999997817,
10.3459381770593));
#296163=CARTESIAN_POINT('Ctrl Pts',(-3.75838203887394,-2.68749999997877,
11.5671105274575));
#296164=CARTESIAN_POINT('Ctrl Pts',(-8.66709987268145E-15,-2.53749999997937,
12.7882828778556));
#296165=CARTESIAN_POINT('Ctrl Pts',(3.75838203887392,-2.38749999997997,
11.5671105274575));
#296166=CARTESIAN_POINT('Ctrl Pts',(7.51676407774785,-2.23749999998057,
10.3459381770593));
#296167=CARTESIAN_POINT('Ctrl Pts',(9.83957192047906,-2.08749999998117,
7.14886745759543));
#296168=CARTESIAN_POINT('Ctrl Pts',(12.1623797632103,-1.93749999998176,
3.95179673813153));
#296169=CARTESIAN_POINT('Ctrl Pts',(12.1623797632103,-1.78749999998236,
-1.489461944703E-15));
#296170=CARTESIAN_POINT('Ctrl Pts',(12.1623797632103,-1.63749999998296,
-3.95179673813154));
#296171=CARTESIAN_POINT('Ctrl Pts',(9.83957192047906,-1.48749999998357,
-7.14886745759543));
#296172=CARTESIAN_POINT('Ctrl Pts',(7.51676407774784,-1.33749999998417,
-10.3459381770593));
#296173=CARTESIAN_POINT('Ctrl Pts',(3.75838203887392,-1.18749999998477,
-11.5671105274575));
#296174=CARTESIAN_POINT('Ctrl Pts',(-1.26631804471037E-14,-1.03749999998537,
-12.7882828778556));
#296175=CARTESIAN_POINT('Ctrl Pts',(-3.75838203887394,-0.887499999985973,
-11.5671105274575));
#296176=CARTESIAN_POINT('Ctrl Pts',(-7.51676407774787,-0.737499999986575,
-10.3459381770593));
#296177=CARTESIAN_POINT('Ctrl Pts',(-9.83957192047909,-0.587499999987176,
-7.14886745759543));
#296178=CARTESIAN_POINT('Ctrl Pts',(-12.1623797632103,-0.437499999987778,
-3.95179673813153));
#296179=CARTESIAN_POINT('Ctrl Pts',(-12.1623797632103,-0.287499999988378,
2.97892388940601E-15));
#296180=CARTESIAN_POINT('Ctrl Pts',(-12.1623797632103,-0.137499999988978,
3.95179673813154));
#296181=CARTESIAN_POINT('Ctrl Pts',(-9.83957192047909,0.0125000000104236,
7.14886745759543));
#296182=CARTESIAN_POINT('Ctrl Pts',(-7.51676407774787,0.162500000009825,
10.3459381770593));
#296183=CARTESIAN_POINT('Ctrl Pts',(-3.75838203887394,0.312500000009227,
11.5671105274575));
#296184=CARTESIAN_POINT('Ctrl Pts',(-1.03948091443433E-14,0.462500000008629,
12.7882828778556));
#296185=CARTESIAN_POINT('Ctrl Pts',(3.75838203887392,0.612500000008031,
11.5671105274575));
#296186=CARTESIAN_POINT('Ctrl Pts',(7.51676407774785,0.762500000007433,
10.3459381770593));
#296187=CARTESIAN_POINT('Ctrl Pts',(9.83957192047906,0.912500000006835,
7.14886745759543));
#296188=CARTESIAN_POINT('Ctrl Pts',(12.1623797632103,1.06250000000624,3.95179673813153));
#296189=CARTESIAN_POINT('Ctrl Pts',(12.1623797632103,1.21250000000564,-1.489461944703E-15));
#296190=CARTESIAN_POINT('Ctrl Pts',(12.1623797632103,1.36250000000504,-3.95179673813154));
#296191=CARTESIAN_POINT('Ctrl Pts',(9.83957192047906,1.51250000000444,-7.14886745759543));
#296192=CARTESIAN_POINT('Ctrl Pts',(7.51676407774784,1.66250000000383,-10.3459381770593));
#296193=CARTESIAN_POINT('Ctrl Pts',(3.75838203887391,1.81250000000323,-11.5671105274575));
#296194=CARTESIAN_POINT('Ctrl Pts',(-1.43908897187656E-14,1.96250000000263,
-12.7882828778556));
#296195=CARTESIAN_POINT('Ctrl Pts',(-3.75838203887394,2.11250000000203,
-11.5671105274575));
#296196=CARTESIAN_POINT('Ctrl Pts',(-7.51676407774787,2.26250000000143,
-10.3459381770593));
#296197=CARTESIAN_POINT('Ctrl Pts',(-9.83957192047909,2.41250000000082,
-7.14886745759543));
#296198=CARTESIAN_POINT('Ctrl Pts',(-12.1623797632103,2.56250000000022,
-3.95179673813153));
#296199=CARTESIAN_POINT('Ctrl Pts',(-12.1623797632103,2.71249999999962,
2.97892388940601E-15));
#296200=CARTESIAN_POINT('Ctrl Pts',(-12.1623797632103,2.86249999999902,
3.95179673813154));
#296201=CARTESIAN_POINT('Ctrl Pts',(-9.83957192047909,3.01249999999842,
7.14886745759543));
#296202=CARTESIAN_POINT('Ctrl Pts',(-7.51676407774787,3.16249999999782,
10.3459381770593));
#296203=CARTESIAN_POINT('Ctrl Pts',(-3.75838203887394,3.31249999999723,
11.5671105274575));
#296204=CARTESIAN_POINT('Ctrl Pts',(-1.21225184160051E-14,3.46249999999663,
12.7882828778556));
#296205=CARTESIAN_POINT('Ctrl Pts',(3.75838203887392,3.61249999999603,11.5671105274575));
#296206=CARTESIAN_POINT('Ctrl Pts',(7.51676407774784,3.76249999999543,10.3459381770593));
#296207=CARTESIAN_POINT('Ctrl Pts',(9.83957192047906,3.91249999999483,7.14886745759543));
#296208=CARTESIAN_POINT('Ctrl Pts',(12.1623797632103,4.06249999999424,3.95179673813153));
#296209=CARTESIAN_POINT('Ctrl Pts',(12.1623797632103,4.21249999999364,-1.489461944703E-15));
#296210=CARTESIAN_POINT('Ctrl Pts',(12.1623797632103,4.36249999999303,-3.95179673813154));
#296211=CARTESIAN_POINT('Ctrl Pts',(9.83957192047906,4.51249999999243,-7.14886745759543));
#296212=CARTESIAN_POINT('Ctrl Pts',(7.51676407774784,4.66249999999183,-10.3459381770593));
#296213=CARTESIAN_POINT('Ctrl Pts',(3.75838203887391,4.81249999999123,-11.5671105274575));
#296214=CARTESIAN_POINT('Ctrl Pts',(-1.61185989904274E-14,4.96249999999063,
-12.7882828778556));
#296215=CARTESIAN_POINT('Ctrl Pts',(-3.75838203887394,5.11249999999003,
-11.5671105274575));
#296216=CARTESIAN_POINT('Ctrl Pts',(-7.51676407774788,5.26249999998942,
-10.3459381770593));
#296217=CARTESIAN_POINT('Ctrl Pts',(-9.83957192047909,5.41249999998882,
-7.14886745759543));
#296218=CARTESIAN_POINT('Ctrl Pts',(-12.1623797632103,5.56249999998822,
-3.95179673813153));
#296219=CARTESIAN_POINT('Ctrl Pts',(-12.1623797632103,5.71249999998762,
2.97892388940601E-15));
#296220=CARTESIAN_POINT('Ctrl Pts',(-12.1623797632103,5.86249999998702,
3.95179673813154));
#296221=CARTESIAN_POINT('Ctrl Pts',(-9.83957192047909,6.01249999998642,
7.14886745759543));
#296222=CARTESIAN_POINT('Ctrl Pts',(-7.51676407774787,6.16249999998582,
10.3459381770593));
#296223=CARTESIAN_POINT('Ctrl Pts',(-3.75838203887394,6.31249999998523,
11.5671105274575));
#296224=CARTESIAN_POINT('Ctrl Pts',(-1.3850227687667E-14,6.46249999998463,
12.7882828778556));
#296225=CARTESIAN_POINT('Ctrl Pts',(3.75838203887392,6.61249999998403,11.5671105274575));
#296226=CARTESIAN_POINT('Ctrl Pts',(7.51676407774784,6.76249999998343,10.3459381770593));
#296227=CARTESIAN_POINT('Ctrl Pts',(9.83957192047906,6.91249999998283,7.14886745759543));
#296228=CARTESIAN_POINT('Ctrl Pts',(12.1623797632103,7.06249999998224,3.95179673813153));
#296229=CARTESIAN_POINT('Ctrl Pts',(12.1623797632103,7.21249999998164,-1.489461944703E-15));
#296230=CARTESIAN_POINT('Ctrl Pts',(12.1623797632103,7.36249999998104,-3.95179673813154));
#296231=CARTESIAN_POINT('Ctrl Pts',(9.83957192047906,7.51249999998044,-7.14886745759543));
#296232=CARTESIAN_POINT('Ctrl Pts',(7.51676407774784,7.66249999997983,-10.3459381770593));
#296233=CARTESIAN_POINT('Ctrl Pts',(3.75838203887391,7.81249999997923,-11.5671105274575));
#296234=CARTESIAN_POINT('Ctrl Pts',(-1.78463082620892E-14,7.96249999997863,
-12.7882828778556));
#296235=CARTESIAN_POINT('Ctrl Pts',(-3.75838203887395,8.11249999997803,
-11.5671105274575));
#296236=CARTESIAN_POINT('Ctrl Pts',(-7.51676407774788,8.26249999997743,
-10.3459381770593));
#296237=CARTESIAN_POINT('Ctrl Pts',(-9.83957192047909,8.41249999997682,
-7.14886745759543));
#296238=CARTESIAN_POINT('Ctrl Pts',(-12.1623797632103,8.56249999997622,
-3.95179673813153));
#296239=CARTESIAN_POINT('Ctrl Pts',(-12.1623797632103,8.71249999997562,
2.97892388940601E-15));
#296240=CARTESIAN_POINT('Ctrl Pts',(-12.1623797632103,8.86249999997502,
3.95179673813154));
#296241=CARTESIAN_POINT('Ctrl Pts',(-9.83957192047909,9.01249999997442,
7.14886745759543));
#296242=CARTESIAN_POINT('Ctrl Pts',(-7.51676407774787,9.16249999997382,
10.3459381770593));
#296243=CARTESIAN_POINT('Ctrl Pts',(-3.75838203887394,9.31249999997323,
11.5671105274575));
#296244=CARTESIAN_POINT('Ctrl Pts',(-1.55779369593288E-14,9.46249999997263,
12.7882828778556));
#296245=CARTESIAN_POINT('Ctrl Pts',(3.75838203887391,9.61249999997203,11.5671105274575));
#296246=CARTESIAN_POINT('Ctrl Pts',(7.51676407774784,9.76249999997144,10.3459381770593));
#296247=CARTESIAN_POINT('Ctrl Pts',(9.83957192047906,9.91249999997084,7.14886745759543));
#296248=CARTESIAN_POINT('Ctrl Pts',(12.1623797632103,10.0624999999702,3.95179673813153));
#296249=CARTESIAN_POINT('Ctrl Pts',(12.1623797632103,10.2124999999696,-1.489461944703E-15));
#296250=CARTESIAN_POINT('Ctrl Pts',(12.1623797632103,10.362499999969,-3.95179673813154));
#296251=CARTESIAN_POINT('Ctrl Pts',(9.83957192047905,10.5124999999684,-7.14886745759543));
#296252=CARTESIAN_POINT('Ctrl Pts',(7.51676407774784,10.6624999999678,-10.3459381770593));
#296253=CARTESIAN_POINT('Ctrl Pts',(3.75838203887391,10.8124999999672,-11.5671105274575));
#296254=CARTESIAN_POINT('Ctrl Pts',(-1.95740175337511E-14,10.9624999999666,
-12.7882828778556));
#296255=CARTESIAN_POINT('Ctrl Pts',(-3.75838203887395,11.112499999966,-11.5671105274575));
#296256=CARTESIAN_POINT('Ctrl Pts',(-7.51676407774788,11.2624999999654,
-10.3459381770593));
#296257=CARTESIAN_POINT('Ctrl Pts',(-9.83957192047909,11.4124999999648,
-7.14886745759543));
#296258=CARTESIAN_POINT('Ctrl Pts',(-12.1623797632103,11.5624999999642,
-3.95179673813153));
#296259=CARTESIAN_POINT('Ctrl Pts',(-12.1623797632103,11.7124999999636,
2.97892388940601E-15));
#296260=CARTESIAN_POINT('Ctrl Pts',(-12.1623797632103,11.862499999963,3.95179673813154));
#296261=CARTESIAN_POINT('Ctrl Pts',(-9.83957192047909,12.0124999999624,
7.14886745759543));
#296262=CARTESIAN_POINT('Ctrl Pts',(-7.51676407774788,12.1624999999618,
10.3459381770593));
#296263=CARTESIAN_POINT('Ctrl Pts',(-3.75838203887395,12.3124999999612,
11.5671105274575));
#296264=CARTESIAN_POINT('Ctrl Pts',(-1.73056462309906E-14,12.4624999999606,
12.7882828778556));
#296265=CARTESIAN_POINT('Ctrl Pts',(3.75838203887391,12.61249999996,11.5671105274575));
#296266=CARTESIAN_POINT('Ctrl Pts',(7.51676407774784,12.7624999999594,10.3459381770593));
#296267=CARTESIAN_POINT('Ctrl Pts',(9.83957192047906,12.9124999999588,7.14886745759543));
#296268=CARTESIAN_POINT('Ctrl Pts',(12.1623797632103,13.0624999999582,3.95179673813153));
#296269=CARTESIAN_POINT('Ctrl Pts',(12.1623797632103,13.2124999999576,-1.489461944703E-15));
#296270=CARTESIAN_POINT('Ctrl Pts',(12.1623797632103,13.362499999957,-3.95179673813154));
#296271=CARTESIAN_POINT('Ctrl Pts',(9.83957192047905,13.5124999999564,-7.14886745759543));
#296272=CARTESIAN_POINT('Ctrl Pts',(7.51676407774784,13.6624999999558,-10.3459381770593));
#296273=CARTESIAN_POINT('Ctrl Pts',(3.75838203887391,13.8124999999552,-11.5671105274575));
#296274=CARTESIAN_POINT('Ctrl Pts',(-2.13017268054129E-14,13.9624999999546,
-12.7882828778556));
#296275=CARTESIAN_POINT('Ctrl Pts',(-3.75838203887395,14.112499999954,-11.5671105274575));
#296276=CARTESIAN_POINT('Ctrl Pts',(-7.51676407774788,14.2624999999534,
-10.3459381770593));
#296277=CARTESIAN_POINT('Ctrl Pts',(-9.8395719204791,14.4124999999528,-7.14886745759543));
#296278=CARTESIAN_POINT('Ctrl Pts',(-12.1623797632103,14.5624999999522,
-3.95179673813153));
#296279=CARTESIAN_POINT('Ctrl Pts',(-12.1623797632103,14.7124999999516,
2.97892388940601E-15));
#296280=CARTESIAN_POINT('Ctrl Pts',(-12.1623797632103,14.862499999951,3.95179673813154));
#296281=CARTESIAN_POINT('Ctrl Pts',(-9.83957192047909,15.0124999999504,
7.14886745759543));
#296282=CARTESIAN_POINT('Ctrl Pts',(-7.51676407774788,15.1624999999498,
10.3459381770593));
#296283=CARTESIAN_POINT('Ctrl Pts',(-3.75838203887395,15.3124999999492,
11.5671105274575));
#296284=CARTESIAN_POINT('Ctrl Pts',(-1.90333555026525E-14,15.4624999999486,
12.7882828778556));
#296285=CARTESIAN_POINT('Ctrl Pts',(3.75838203887391,15.612499999948,11.5671105274575));
#296286=CARTESIAN_POINT('Ctrl Pts',(7.51676407774784,15.7624999999474,10.3459381770593));
#296287=CARTESIAN_POINT('Ctrl Pts',(9.83957192047905,15.9124999999468,7.14886745759543));
#296288=CARTESIAN_POINT('Ctrl Pts',(12.1623797632103,16.0624999999462,3.95179673813153));
#296289=CARTESIAN_POINT('Ctrl Pts',(12.1623797632103,16.2124999999456,-1.489461944703E-15));
#296290=CARTESIAN_POINT('Ctrl Pts',(12.1623797632103,16.362499999945,-3.95179673813154));
#296291=CARTESIAN_POINT('Ctrl Pts',(9.83957192047905,16.5124999999444,-7.14886745759543));
#296292=CARTESIAN_POINT('Ctrl Pts',(7.51676407774784,16.6624999999438,-10.3459381770593));
#296293=CARTESIAN_POINT('Ctrl Pts',(3.75838203887391,16.8124999999432,-11.5671105274575));
#296294=CARTESIAN_POINT('Ctrl Pts',(-2.30294360770748E-14,16.9624999999426,
-12.7882828778556));
#296295=CARTESIAN_POINT('Ctrl Pts',(-3.75838203887395,17.112499999942,-11.5671105274575));
#296296=CARTESIAN_POINT('Ctrl Pts',(-7.51676407774788,17.2624999999414,
-10.3459381770593));
#296297=CARTESIAN_POINT('Ctrl Pts',(-9.8395719204791,17.4124999999408,-7.14886745759543));
#296298=CARTESIAN_POINT('Ctrl Pts',(-12.1623797632103,17.5624999999402,
-3.95179673813153));
#296299=CARTESIAN_POINT('Ctrl Pts',(-12.1623797632103,17.7124999999396,
2.97892388940601E-15));
#296300=CARTESIAN_POINT('Ctrl Pts',(-12.1623797632103,17.862499999939,3.95179673813154));
#296301=CARTESIAN_POINT('Ctrl Pts',(-9.8395719204791,18.0124999999384,7.14886745759543));
#296302=CARTESIAN_POINT('Ctrl Pts',(-7.51676407774788,18.1624999999378,
10.3459381770593));
#296303=CARTESIAN_POINT('Ctrl Pts',(-3.75838203887395,18.3124999999372,
11.5671105274575));
#296304=CARTESIAN_POINT('Ctrl Pts',(-2.07610647743143E-14,18.4624999999366,
12.7882828778556));
#296305=CARTESIAN_POINT('Ctrl Pts',(3.75838203887391,18.612499999936,11.5671105274575));
#296306=CARTESIAN_POINT('Ctrl Pts',(7.51676407774784,18.7624999999354,10.3459381770593));
#296307=CARTESIAN_POINT('Ctrl Pts',(9.83957192047905,18.9124999999348,7.14886745759543));
#296308=CARTESIAN_POINT('Ctrl Pts',(12.1623797632103,19.0624999999342,3.95179673813153));
#296309=CARTESIAN_POINT('Ctrl Pts',(12.1623797632103,19.2124999999336,-1.489461944703E-15));
#296310=CARTESIAN_POINT('Ctrl Pts',(12.1623797632103,19.362499999933,-3.95179673813154));
#296311=CARTESIAN_POINT('Ctrl Pts',(9.83957192047905,19.5124999999324,-7.14886745759543));
#296312=CARTESIAN_POINT('Ctrl Pts',(7.51676407774784,19.6624999999318,-10.3459381770593));
#296313=CARTESIAN_POINT('Ctrl Pts',(3.7583820388739,19.8124999999312,-11.5671105274575));
#296314=CARTESIAN_POINT('Ctrl Pts',(-2.47571453487366E-14,19.9624999999306,
-12.7882828778556));
#296315=CARTESIAN_POINT('Ctrl Pts',(-3.75838203887395,20.11249999993,-11.5671105274575));
#296316=CARTESIAN_POINT('Ctrl Pts',(-7.51676407774788,20.2624999999294,
-10.3459381770593));
#296317=CARTESIAN_POINT('Ctrl Pts',(-9.8395719204791,20.4124999999288,-7.14886745759543));
#296318=CARTESIAN_POINT('Ctrl Pts',(-12.1623797632103,20.5624999999282,
-3.95179673813153));
#296319=CARTESIAN_POINT('Ctrl Pts',(-12.1623797632103,20.7124999999276,
2.97892388940601E-15));
#296320=CARTESIAN_POINT('Ctrl Pts',(-12.1623797632103,20.862499999927,3.95179673813154));
#296321=CARTESIAN_POINT('Ctrl Pts',(-9.8395719204791,21.0124999999264,7.14886745759543));
#296322=CARTESIAN_POINT('Ctrl Pts',(-7.51676407774788,21.1624999999258,
10.3459381770593));
#296323=CARTESIAN_POINT('Ctrl Pts',(-3.75838203887395,21.3124999999252,
11.5671105274575));
#296324=CARTESIAN_POINT('Ctrl Pts',(-2.24887740459762E-14,21.4624999999246,
12.7882828778556));
#296325=CARTESIAN_POINT('Ctrl Pts',(3.75838203887391,21.612499999924,11.5671105274575));
#296326=CARTESIAN_POINT('Ctrl Pts',(7.51676407774784,21.7624999999234,10.3459381770593));
#296327=CARTESIAN_POINT('Ctrl Pts',(9.83957192047905,21.9124999999228,7.14886745759543));
#296328=CARTESIAN_POINT('Ctrl Pts',(12.1623797632103,22.0624999999222,3.95179673813153));
#296329=CARTESIAN_POINT('Ctrl Pts',(12.1623797632103,22.2124999999216,-1.489461944703E-15));
#296330=CARTESIAN_POINT('Ctrl Pts',(12.1623797632103,22.362499999921,-3.95179673813154));
#296331=CARTESIAN_POINT('Ctrl Pts',(9.83957192047905,22.5124999999204,-7.14886745759543));
#296332=CARTESIAN_POINT('Ctrl Pts',(7.51676407774783,22.6624999999198,-10.3459381770593));
#296333=CARTESIAN_POINT('Ctrl Pts',(3.7583820388739,22.8124999999192,-11.5671105274575));
#296334=CARTESIAN_POINT('Ctrl Pts',(-2.64848546203984E-14,22.9624999999186,
-12.7882828778556));
#296335=CARTESIAN_POINT('Ctrl Pts',(-3.75838203887396,23.112499999918,-11.5671105274575));
#296336=CARTESIAN_POINT('Ctrl Pts',(-7.51676407774788,23.2624999999174,
-10.3459381770593));
#296337=CARTESIAN_POINT('Ctrl Pts',(-9.8395719204791,23.4124999999168,-7.14886745759543));
#296338=CARTESIAN_POINT('Ctrl Pts',(-12.1623797632103,23.5624999999162,
-3.95179673813153));
#296339=CARTESIAN_POINT('Ctrl Pts',(-12.1623797632103,23.7124999999156,
2.97892388940601E-15));
#296340=CARTESIAN_POINT('Ctrl Pts',(-12.1623797632103,23.862499999915,3.95179673813154));
#296341=CARTESIAN_POINT('Ctrl Pts',(-9.8395719204791,24.0124999999144,7.14886745759543));
#296342=CARTESIAN_POINT('Ctrl Pts',(-7.51676407774788,24.1624999999138,
10.3459381770593));
#296343=CARTESIAN_POINT('Ctrl Pts',(-3.75838203887395,24.3124999999132,
11.5671105274575));
#296344=CARTESIAN_POINT('Ctrl Pts',(-2.4216483317638E-14,24.4624999999126,
12.7882828778556));
#296345=CARTESIAN_POINT('Ctrl Pts',(3.7583820388739,24.612499999912,11.5671105274575));
#296346=CARTESIAN_POINT('Ctrl Pts',(7.51676407774783,24.7624999999114,10.3459381770593));
#296347=CARTESIAN_POINT('Ctrl Pts',(9.83957192047905,24.9124999999108,7.14886745759543));
#296348=CARTESIAN_POINT('Ctrl Pts',(12.1623797632103,25.0624999999102,3.95179673813153));
#296349=CARTESIAN_POINT('Ctrl Pts',(12.1623797632103,25.2124999999096,-1.489461944703E-15));
#296350=CARTESIAN_POINT('Ctrl Pts',(12.1623797632103,25.362499999909,-3.95179673813154));
#296351=CARTESIAN_POINT('Ctrl Pts',(9.83957192047905,25.5124999999084,-7.14886745759543));
#296352=CARTESIAN_POINT('Ctrl Pts',(7.51676407774783,25.6624999999078,-10.3459381770593));
#296353=CARTESIAN_POINT('Ctrl Pts',(3.7583820388739,25.8124999999072,-11.5671105274575));
#296354=CARTESIAN_POINT('Ctrl Pts',(-2.82125638920603E-14,25.9624999999066,
-12.7882828778556));
#296355=CARTESIAN_POINT('Ctrl Pts',(-3.75838203887396,26.112499999906,-11.5671105274575));
#296356=CARTESIAN_POINT('Ctrl Pts',(-7.51676407774788,26.2624999999054,
-10.3459381770593));
#296357=CARTESIAN_POINT('Ctrl Pts',(-9.8395719204791,26.4124999999048,-7.14886745759543));
#296358=CARTESIAN_POINT('Ctrl Pts',(-12.1623797632103,26.5624999999042,
-3.95179673813153));
#296359=CARTESIAN_POINT('Ctrl Pts',(-12.1623797632103,26.7124999999036,
2.97892388940601E-15));
#296360=CARTESIAN_POINT('Ctrl Pts',(-12.1623797632103,26.862499999903,3.95179673813154));
#296361=CARTESIAN_POINT('Ctrl Pts',(-9.8395719204791,27.0124999999024,7.14886745759543));
#296362=CARTESIAN_POINT('Ctrl Pts',(-7.51676407774788,27.1624999999018,
10.3459381770593));
#296363=CARTESIAN_POINT('Ctrl Pts',(-3.75838203887396,27.3124999999012,
11.5671105274575));
#296364=CARTESIAN_POINT('Ctrl Pts',(-2.59441925892998E-14,27.4624999999006,
12.7882828778556));
#296365=CARTESIAN_POINT('Ctrl Pts',(3.7583820388739,27.6124999999,11.5671105274575));
#296366=CARTESIAN_POINT('Ctrl Pts',(7.51676407774783,27.7624999998994,10.3459381770593));
#296367=CARTESIAN_POINT('Ctrl Pts',(9.83957192047905,27.9124999998988,7.14886745759543));
#296368=CARTESIAN_POINT('Ctrl Pts',(12.1623797632103,28.0624999998982,3.95179673813153));
#296369=CARTESIAN_POINT('Ctrl Pts',(12.1623797632103,28.2124999998976,-1.489461944703E-15));
#296370=CARTESIAN_POINT('Ctrl Pts',(12.1623797632103,28.362499999897,-3.95179673813154));
#296371=CARTESIAN_POINT('Ctrl Pts',(9.83957192047905,28.5124999998964,-7.14886745759543));
#296372=CARTESIAN_POINT('Ctrl Pts',(7.51676407774783,28.6624999998958,-10.3459381770593));
#296373=CARTESIAN_POINT('Ctrl Pts',(3.7583820388739,28.8124999998952,-11.5671105274575));
#296374=CARTESIAN_POINT('Ctrl Pts',(-2.99402731637221E-14,28.9624999998946,
-12.7882828778556));
#296375=CARTESIAN_POINT('Ctrl Pts',(-3.75838203887396,29.112499999894,-11.5671105274575));
#296376=CARTESIAN_POINT('Ctrl Pts',(-7.51676407774789,29.2624999998934,
-10.3459381770593));
#296377=CARTESIAN_POINT('Ctrl Pts',(-9.8395719204791,29.4124999998928,-7.14886745759543));
#296378=CARTESIAN_POINT('Ctrl Pts',(-12.1623797632103,29.5624999998922,
-3.95179673813153));
#296379=CARTESIAN_POINT('Ctrl Pts',(-12.1623797632103,29.7124999998916,
2.97892388940601E-15));
#296380=CARTESIAN_POINT('Ctrl Pts',(-12.1623797632103,29.862499999891,3.95179673813154));
#296381=CARTESIAN_POINT('Ctrl Pts',(-9.8395719204791,30.0124999998904,7.14886745759543));
#296382=CARTESIAN_POINT('Ctrl Pts',(-7.51676407774788,30.1624999998898,
10.3459381770593));
#296383=CARTESIAN_POINT('Ctrl Pts',(-3.75838203887396,30.3124999998892,
11.5671105274575));
#296384=CARTESIAN_POINT('Ctrl Pts',(-2.76719018609617E-14,30.4624999998886,
12.7882828778556));
#296385=CARTESIAN_POINT('Ctrl Pts',(3.7583820388739,30.612499999888,11.5671105274575));
#296386=CARTESIAN_POINT('Ctrl Pts',(7.51676407774783,30.7624999998874,10.3459381770593));
#296387=CARTESIAN_POINT('Ctrl Pts',(9.83957192047905,30.9124999998868,7.14886745759543));
#296388=CARTESIAN_POINT('Ctrl Pts',(12.1623797632103,31.0624999998862,3.95179673813153));
#296389=CARTESIAN_POINT('Ctrl Pts',(12.1623797632103,31.2124999998856,-1.489461944703E-15));
#296390=CARTESIAN_POINT('Ctrl Pts',(12.1623797632103,31.362499999885,-3.95179673813154));
#296391=CARTESIAN_POINT('Ctrl Pts',(9.83957192047904,31.5124999998844,-7.14886745759543));
#296392=CARTESIAN_POINT('Ctrl Pts',(7.51676407774783,31.6624999998838,-10.3459381770593));
#296393=CARTESIAN_POINT('Ctrl Pts',(3.7583820388739,31.8124999998832,-11.5671105274575));
#296394=CARTESIAN_POINT('Ctrl Pts',(-3.16679824353839E-14,31.9624999998826,
-12.7882828778556));
#296395=CARTESIAN_POINT('Ctrl Pts',(-3.75838203887396,32.112499999882,-11.5671105274575));
#296396=CARTESIAN_POINT('Ctrl Pts',(-7.51676407774789,32.2624999998814,
-10.3459381770593));
#296397=CARTESIAN_POINT('Ctrl Pts',(-9.83957192047911,32.4124999998808,
-7.14886745759543));
#296398=CARTESIAN_POINT('Ctrl Pts',(-12.1623797632103,32.5624999998802,
-3.95179673813153));
#296399=CARTESIAN_POINT('Ctrl Pts',(-12.1623797632103,32.7124999998796,
2.97892388940601E-15));
#296400=CARTESIAN_POINT('Ctrl Pts',(-12.1623797632103,32.862499999879,3.95179673813154));
#296401=CARTESIAN_POINT('Ctrl Pts',(-9.8395719204791,33.0124999998784,7.14886745759543));
#296402=CARTESIAN_POINT('Ctrl Pts',(-7.51676407774789,33.1624999998778,
10.3459381770593));
#296403=CARTESIAN_POINT('Ctrl Pts',(-3.75838203887396,33.3124999998772,
11.5671105274575));
#296404=CARTESIAN_POINT('Ctrl Pts',(-2.93996111326235E-14,33.4624999998766,
12.7882828778556));
#296405=CARTESIAN_POINT('Ctrl Pts',(3.7583820388739,33.612499999876,11.5671105274575));
#296406=CARTESIAN_POINT('Ctrl Pts',(7.51676407774783,33.7624999998754,10.3459381770593));
#296407=CARTESIAN_POINT('Ctrl Pts',(9.83957192047905,33.9124999998748,7.14886745759543));
#296408=CARTESIAN_POINT('Ctrl Pts',(12.1623797632103,34.0624999998742,3.95179673813153));
#296409=CARTESIAN_POINT('Ctrl Pts',(12.1623797632103,34.2124999998736,-1.489461944703E-15));
#296410=CARTESIAN_POINT('Ctrl Pts',(12.1623797632103,34.362499999873,-3.95179673813154));
#296411=CARTESIAN_POINT('Ctrl Pts',(9.83957192047904,34.5124999998724,-7.14886745759543));
#296412=CARTESIAN_POINT('Ctrl Pts',(7.51676407774783,34.6624999998718,-10.3459381770593));
#296413=CARTESIAN_POINT('Ctrl Pts',(3.7583820388739,34.8124999998712,-11.5671105274575));
#296414=CARTESIAN_POINT('Ctrl Pts',(-3.33956917070458E-14,34.9624999998706,
-12.7882828778556));
#296415=CARTESIAN_POINT('Ctrl Pts',(-3.75838203887396,35.11249999987,-11.5671105274575));
#296416=CARTESIAN_POINT('Ctrl Pts',(-7.51676407774789,35.2624999998694,
-10.3459381770593));
#296417=CARTESIAN_POINT('Ctrl Pts',(-9.83957192047911,35.4124999998688,
-7.14886745759543));
#296418=CARTESIAN_POINT('Ctrl Pts',(-12.1623797632103,35.5624999998682,
-3.95179673813153));
#296419=CARTESIAN_POINT('Ctrl Pts',(-12.1623797632103,35.7124999998676,
2.97892388940601E-15));
#296420=CARTESIAN_POINT('Ctrl Pts',(-12.1623797632103,35.862499999867,3.95179673813154));
#296421=CARTESIAN_POINT('Ctrl Pts',(-9.83957192047911,36.0124999998664,
7.14886745759543));
#296422=CARTESIAN_POINT('Ctrl Pts',(-7.51676407774789,36.1624999998658,
10.3459381770593));
#296423=CARTESIAN_POINT('Ctrl Pts',(-3.75838203887396,36.3124999998652,
11.5671105274575));
#296424=CARTESIAN_POINT('Ctrl Pts',(-3.11273204042854E-14,36.4624999998646,
12.7882828778556));
#296425=CARTESIAN_POINT('Ctrl Pts',(3.7583820388739,36.612499999864,11.5671105274575));
#296426=CARTESIAN_POINT('Ctrl Pts',(7.51676407774783,36.7624999998634,10.3459381770593));
#296427=CARTESIAN_POINT('Ctrl Pts',(9.83957192047904,36.9124999998628,7.14886745759543));
#296428=CARTESIAN_POINT('Ctrl Pts',(12.1623797632103,37.0624999998622,3.95179673813153));
#296429=CARTESIAN_POINT('Ctrl Pts',(12.1623797632103,37.2124999998616,-1.489461944703E-15));
#296430=CARTESIAN_POINT('Ctrl Pts',(12.1623797632103,37.362499999861,-3.95179673813154));
#296431=CARTESIAN_POINT('Ctrl Pts',(9.83957192047904,37.5124999998604,-7.14886745759543));
#296432=CARTESIAN_POINT('Ctrl Pts',(7.51676407774782,37.6624999998598,-10.3459381770593));
#296433=CARTESIAN_POINT('Ctrl Pts',(3.75838203887389,37.8124999998592,-11.5671105274575));
#296434=CARTESIAN_POINT('Ctrl Pts',(-3.51234009787076E-14,37.9624999998586,
-12.7882828778556));
#296435=CARTESIAN_POINT('Ctrl Pts',(-3.75838203887396,38.112499999858,-11.5671105274575));
#296436=CARTESIAN_POINT('Ctrl Pts',(-7.51676407774789,38.2624999998574,
-10.3459381770593));
#296437=CARTESIAN_POINT('Ctrl Pts',(-9.83957192047911,38.4124999998568,
-7.14886745759543));
#296438=CARTESIAN_POINT('Ctrl Pts',(-12.1623797632103,38.5624999998562,
-3.95179673813153));
#296439=CARTESIAN_POINT('Ctrl Pts',(-12.1623797632103,38.7124999998556,
2.97892388940601E-15));
#296440=CARTESIAN_POINT('Ctrl Pts',(-12.1623797632103,38.862499999855,3.95179673813154));
#296441=CARTESIAN_POINT('Ctrl Pts',(-9.83957192047911,39.0124999998544,
7.14886745759543));
#296442=CARTESIAN_POINT('Ctrl Pts',(-7.51676407774789,39.1624999998538,
10.3459381770593));
#296443=CARTESIAN_POINT('Ctrl Pts',(-3.75838203887396,39.3124999998532,
11.5671105274575));
#296444=CARTESIAN_POINT('Ctrl Pts',(-3.28550296759472E-14,39.4624999998526,
12.7882828778556));
#296445=CARTESIAN_POINT('Ctrl Pts',(3.7583820388739,39.612499999852,11.5671105274575));
#296446=CARTESIAN_POINT('Ctrl Pts',(7.51676407774782,39.7624999998514,10.3459381770593));
#296447=CARTESIAN_POINT('Ctrl Pts',(9.83957192047904,39.9124999998508,7.14886745759543));
#296448=CARTESIAN_POINT('Ctrl Pts',(12.1623797632103,40.0624999998502,3.95179673813153));
#296449=CARTESIAN_POINT('Ctrl Pts',(12.1623797632103,40.2124999998496,-1.489461944703E-15));
#296450=CARTESIAN_POINT('Ctrl Pts',(12.1623797632103,40.362499999849,-3.95179673813154));
#296451=CARTESIAN_POINT('Ctrl Pts',(9.83957192047904,40.5124999998484,-7.14886745759543));
#296452=CARTESIAN_POINT('Ctrl Pts',(7.51676407774782,40.6624999998478,-10.3459381770593));
#296453=CARTESIAN_POINT('Ctrl Pts',(3.75838203887389,40.8124999998472,-11.5671105274575));
#296454=CARTESIAN_POINT('Ctrl Pts',(-3.68511102503695E-14,40.9624999998466,
-12.7882828778556));
#296455=CARTESIAN_POINT('Ctrl Pts',(-3.75838203887397,41.112499999846,-11.5671105274575));
#296456=CARTESIAN_POINT('Ctrl Pts',(-7.51676407774789,41.2624999998454,
-10.3459381770593));
#296457=CARTESIAN_POINT('Ctrl Pts',(-9.83957192047911,41.4124999998448,
-7.14886745759543));
#296458=CARTESIAN_POINT('Ctrl Pts',(-12.1623797632103,41.5624999998442,
-3.95179673813153));
#296459=CARTESIAN_POINT('Ctrl Pts',(-12.1623797632103,41.7124999998436,
2.97892388940601E-15));
#296460=CARTESIAN_POINT('Ctrl Pts',(-12.1623797632103,41.862499999843,3.95179673813154));
#296461=CARTESIAN_POINT('Ctrl Pts',(-9.83957192047911,42.0124999998424,
7.14886745759543));
#296462=CARTESIAN_POINT('Ctrl Pts',(-7.51676407774789,42.1624999998418,
10.3459381770593));
#296463=CARTESIAN_POINT('Ctrl Pts',(-3.75838203887396,42.3124999998412,
11.5671105274575));
#296464=CARTESIAN_POINT('Ctrl Pts',(-3.4582738947609E-14,42.4624999998406,
12.7882828778556));
#296465=CARTESIAN_POINT('Ctrl Pts',(3.75838203887389,42.61249999984,11.5671105274575));
#296466=CARTESIAN_POINT('Ctrl Pts',(7.51676407774782,42.7624999998394,10.3459381770593));
#296467=CARTESIAN_POINT('Ctrl Pts',(9.83957192047904,42.9124999998388,7.14886745759543));
#296468=CARTESIAN_POINT('Ctrl Pts',(12.1623797632103,43.0624999998382,3.95179673813153));
#296469=CARTESIAN_POINT('Ctrl Pts',(12.1623797632103,43.2124999998376,-1.489461944703E-15));
#296470=CARTESIAN_POINT('Ctrl Pts',(12.1623797632103,43.362499999837,-3.95179673813154));
#296471=CARTESIAN_POINT('Ctrl Pts',(9.83957192047903,43.5124999998364,-7.14886745759543));
#296472=CARTESIAN_POINT('Ctrl Pts',(7.51676407774782,43.6624999998358,-10.3459381770593));
#296473=CARTESIAN_POINT('Ctrl Pts',(3.75838203887389,43.8124999998352,-11.5671105274575));
#296474=CARTESIAN_POINT('Ctrl Pts',(-3.85788195220313E-14,43.9624999998346,
-12.7882828778556));
#296475=CARTESIAN_POINT('Ctrl Pts',(-3.75838203887397,44.112499999834,-11.5671105274575));
#296476=CARTESIAN_POINT('Ctrl Pts',(-7.5167640777479,44.2624999998334,-10.3459381770593));
#296477=CARTESIAN_POINT('Ctrl Pts',(-9.83957192047911,44.4124999998328,
-7.14886745759543));
#296478=CARTESIAN_POINT('Ctrl Pts',(-12.1623797632103,44.5624999998322,
-3.95179673813153));
#296479=CARTESIAN_POINT('Ctrl Pts',(-12.1623797632103,44.7124999998316,
2.97892388940601E-15));
#296480=CARTESIAN_POINT('Ctrl Pts',(-12.1623797632103,44.862499999831,3.95179673813154));
#296481=CARTESIAN_POINT('Ctrl Pts',(-9.83957192047911,45.0124999998304,
7.14886745759543));
#296482=CARTESIAN_POINT('Ctrl Pts',(-7.51676407774789,45.1624999998298,
10.3459381770593));
#296483=CARTESIAN_POINT('Ctrl Pts',(-3.75838203887397,45.3124999998292,
11.5671105274575));
#296484=CARTESIAN_POINT('Ctrl Pts',(-3.63104482192709E-14,45.4624999998286,
12.7882828778556));
#296485=CARTESIAN_POINT('Ctrl Pts',(3.75838203887389,45.612499999828,11.5671105274575));
#296486=CARTESIAN_POINT('Ctrl Pts',(7.51676407774782,45.7624999998274,10.3459381770593));
#296487=CARTESIAN_POINT('Ctrl Pts',(9.83957192047904,45.9124999998268,7.14886745759543));
#296488=CARTESIAN_POINT('Ctrl Pts',(12.1623797632103,46.0624999998262,3.95179673813153));
#296489=CARTESIAN_POINT('Ctrl Pts',(12.1623797632103,46.2124999998256,-1.489461944703E-15));
#296490=CARTESIAN_POINT('Ctrl Pts',(12.1623797632103,46.362499999825,-3.95179673813154));
#296491=CARTESIAN_POINT('Ctrl Pts',(9.83957192047903,46.5124999998244,-7.14886745759543));
#296492=CARTESIAN_POINT('Ctrl Pts',(7.51676407774782,46.6624999998238,-10.3459381770593));
#296493=CARTESIAN_POINT('Ctrl Pts',(3.75838203887389,46.8124999998232,-11.5671105274575));
#296494=CARTESIAN_POINT('Ctrl Pts',(-4.03065287936931E-14,46.9624999998226,
-12.7882828778556));
#296495=CARTESIAN_POINT('Ctrl Pts',(-3.75838203887397,47.112499999822,-11.5671105274575));
#296496=CARTESIAN_POINT('Ctrl Pts',(-7.5167640777479,47.2624999998214,-10.3459381770593));
#296497=CARTESIAN_POINT('Ctrl Pts',(-9.83957192047912,47.4124999998208,
-7.14886745759543));
#296498=CARTESIAN_POINT('Ctrl Pts',(-12.1623797632103,47.5624999998202,
-3.95179673813153));
#296499=CARTESIAN_POINT('Ctrl Pts',(-12.1623797632103,47.7124999998196,
2.97892388940601E-15));
#296500=CARTESIAN_POINT('Ctrl Pts',(-12.1623797632103,47.862499999819,3.95179673813154));
#296501=CARTESIAN_POINT('Ctrl Pts',(-9.83957192047911,48.0124999998184,
7.14886745759543));
#296502=CARTESIAN_POINT('Ctrl Pts',(-7.51676407774789,48.1624999998178,
10.3459381770593));
#296503=CARTESIAN_POINT('Ctrl Pts',(-3.75838203887397,48.3124999998172,
11.5671105274575));
#296504=CARTESIAN_POINT('Ctrl Pts',(-3.80381574909327E-14,48.4624999998166,
12.7882828778556));
#296505=CARTESIAN_POINT('Ctrl Pts',(3.75838203887389,48.612499999816,11.5671105274575));
#296506=CARTESIAN_POINT('Ctrl Pts',(7.51676407774782,48.7624999998154,10.3459381770593));
#296507=CARTESIAN_POINT('Ctrl Pts',(9.83957192047903,48.9124999998148,7.14886745759543));
#296508=CARTESIAN_POINT('Ctrl Pts',(12.1623797632103,49.0624999998142,3.95179673813153));
#296509=CARTESIAN_POINT('Ctrl Pts',(12.1623797632103,49.2124999998136,-1.489461944703E-15));
#296510=CARTESIAN_POINT('Ctrl Pts',(12.1623797632103,49.362499999813,-3.95179673813154));
#296511=CARTESIAN_POINT('Ctrl Pts',(9.83957192047903,49.5124999998124,-7.14886745759543));
#296512=CARTESIAN_POINT('Ctrl Pts',(7.51676407774782,49.6624999998118,-10.3459381770593));
#296513=CARTESIAN_POINT('Ctrl Pts',(3.75838203887389,49.8124999998112,-11.5671105274575));
#296514=CARTESIAN_POINT('Ctrl Pts',(-4.2034238065355E-14,49.9624999998106,
-12.7882828778556));
#296515=CARTESIAN_POINT('Ctrl Pts',(-3.75838203887397,50.11249999981,-11.5671105274575));
#296516=CARTESIAN_POINT('Ctrl Pts',(-7.5167640777479,50.2624999998094,-10.3459381770593));
#296517=CARTESIAN_POINT('Ctrl Pts',(-9.83957192047912,50.4124999998088,
-7.14886745759543));
#296518=CARTESIAN_POINT('Ctrl Pts',(-12.1623797632103,50.5624999998082,
-3.95179673813153));
#296519=CARTESIAN_POINT('Ctrl Pts',(-12.1623797632103,50.7124999998076,
2.97892388940601E-15));
#296520=CARTESIAN_POINT('Ctrl Pts',(-12.1623797632103,50.862499999807,3.95179673813154));
#296521=CARTESIAN_POINT('Ctrl Pts',(-9.83957192047912,51.0124999998064,
7.14886745759543));
#296522=CARTESIAN_POINT('Ctrl Pts',(-7.5167640777479,51.1624999998058,10.3459381770593));
#296523=CARTESIAN_POINT('Ctrl Pts',(-3.75838203887397,51.3124999998052,
11.5671105274575));
#296524=CARTESIAN_POINT('Ctrl Pts',(-3.97658667625946E-14,51.4624999998046,
12.7882828778556));
#296525=CARTESIAN_POINT('Ctrl Pts',(3.75838203887389,51.612499999804,11.5671105274575));
#296526=CARTESIAN_POINT('Ctrl Pts',(7.51676407774782,51.7624999998034,10.3459381770593));
#296527=CARTESIAN_POINT('Ctrl Pts',(9.83957192047903,51.9124999998028,7.14886745759543));
#296528=CARTESIAN_POINT('Ctrl Pts',(12.1623797632103,52.0624999998022,3.95179673813153));
#296529=CARTESIAN_POINT('Ctrl Pts',(12.1623797632103,52.2124999998016,-1.489461944703E-15));
#296530=CARTESIAN_POINT('Ctrl Pts',(12.1623797632103,52.362499999801,-3.95179673813154));
#296531=CARTESIAN_POINT('Ctrl Pts',(9.83957192047903,52.5124999998004,-7.14886745759543));
#296532=CARTESIAN_POINT('Ctrl Pts',(7.51676407774781,52.6624999997998,-10.3459381770593));
#296533=CARTESIAN_POINT('Ctrl Pts',(3.75838203887388,52.8124999997992,-11.5671105274575));
#296534=CARTESIAN_POINT('Ctrl Pts',(-4.37619473370168E-14,52.9624999997986,
-12.7882828778556));
#296535=CARTESIAN_POINT('Ctrl Pts',(-3.75838203887397,53.112499999798,-11.5671105274575));
#296536=CARTESIAN_POINT('Ctrl Pts',(-7.5167640777479,53.2624999997974,-10.3459381770593));
#296537=CARTESIAN_POINT('Ctrl Pts',(-9.83957192047912,53.4124999997968,
-7.14886745759543));
#296538=CARTESIAN_POINT('Ctrl Pts',(-12.1623797632103,53.5624999997962,
-3.95179673813153));
#296539=CARTESIAN_POINT('Ctrl Pts',(-12.1623797632103,53.7124999997956,
2.97892388940601E-15));
#296540=CARTESIAN_POINT('Ctrl Pts',(-12.1623797632103,53.862499999795,3.95179673813154));
#296541=CARTESIAN_POINT('Ctrl Pts',(-9.83957192047912,54.0124999997944,
7.14886745759543));
#296542=CARTESIAN_POINT('Ctrl Pts',(-7.5167640777479,54.1624999997938,10.3459381770593));
#296543=CARTESIAN_POINT('Ctrl Pts',(-3.75838203887397,54.3124999997932,
11.5671105274575));
#296544=CARTESIAN_POINT('Ctrl Pts',(-4.14935760342564E-14,54.4624999997926,
12.7882828778556));
#296545=CARTESIAN_POINT('Ctrl Pts',(3.75838203887389,54.612499999792,11.5671105274575));
#296546=CARTESIAN_POINT('Ctrl Pts',(7.51676407774782,54.7624999997914,10.3459381770593));
#296547=CARTESIAN_POINT('Ctrl Pts',(9.83957192047903,54.9124999997908,7.14886745759543));
#296548=CARTESIAN_POINT('Ctrl Pts',(12.1623797632103,55.0624999997902,3.95179673813153));
#296549=CARTESIAN_POINT('Ctrl Pts',(12.1623797632103,55.2124999997896,-1.489461944703E-15));
#296550=CARTESIAN_POINT('Ctrl Pts',(12.1623797632103,55.362499999789,-3.95179673813154));
#296551=CARTESIAN_POINT('Ctrl Pts',(9.83957192047903,55.5124999997884,-7.14886745759543));
#296552=CARTESIAN_POINT('Ctrl Pts',(7.51676407774781,55.6624999997878,-10.3459381770593));
#296553=CARTESIAN_POINT('Ctrl Pts',(3.75838203887388,55.8124999997872,-11.5671105274575));
#296554=CARTESIAN_POINT('Ctrl Pts',(-4.54896566086787E-14,55.9624999997866,
-12.7882828778556));
#296555=CARTESIAN_POINT('Ctrl Pts',(-3.75838203887397,56.112499999786,-11.5671105274575));
#296556=CARTESIAN_POINT('Ctrl Pts',(-7.5167640777479,56.2624999997854,-10.3459381770593));
#296557=CARTESIAN_POINT('Ctrl Pts',(-9.83957192047912,56.4124999997848,
-7.14886745759543));
#296558=CARTESIAN_POINT('Ctrl Pts',(-12.1623797632103,56.5624999997842,
-3.95179673813153));
#296559=CARTESIAN_POINT('Ctrl Pts',(-12.1623797632103,56.7124999997836,
2.97892388940601E-15));
#296560=CARTESIAN_POINT('Ctrl Pts',(-12.1623797632103,56.862499999783,3.95179673813154));
#296561=CARTESIAN_POINT('Ctrl Pts',(-9.83957192047912,57.0124999997824,
7.14886745759543));
#296562=CARTESIAN_POINT('Ctrl Pts',(-7.5167640777479,57.1624999997818,10.3459381770593));
#296563=CARTESIAN_POINT('Ctrl Pts',(-3.75838203887397,57.3124999997812,
11.5671105274575));
#296564=CARTESIAN_POINT('Ctrl Pts',(-4.32212853059182E-14,57.4624999997806,
12.7882828778556));
#296565=CARTESIAN_POINT('Ctrl Pts',(3.75838203887389,57.61249999978,11.5671105274575));
#296566=CARTESIAN_POINT('Ctrl Pts',(7.51676407774781,57.7624999997794,10.3459381770593));
#296567=CARTESIAN_POINT('Ctrl Pts',(9.83957192047903,57.9124999997788,7.14886745759543));
#296568=CARTESIAN_POINT('Ctrl Pts',(12.1623797632103,58.0624999997782,3.95179673813153));
#296569=CARTESIAN_POINT('Ctrl Pts',(12.1623797632102,58.2124999997776,-1.489461944703E-15));
#296570=CARTESIAN_POINT('Ctrl Pts',(12.1623797632102,58.362499999777,-3.95179673813154));
#296571=CARTESIAN_POINT('Ctrl Pts',(9.83957192047903,58.5124999997764,-7.14886745759543));
#296572=CARTESIAN_POINT('Ctrl Pts',(7.51676407774781,58.6624999997758,-10.3459381770593));
#296573=CARTESIAN_POINT('Ctrl Pts',(3.75838203887388,58.8124999997752,-11.5671105274575));
#296574=CARTESIAN_POINT('Ctrl Pts',(-4.72173658803405E-14,58.9624999997746,
-12.7882828778556));
#296575=CARTESIAN_POINT('Ctrl Pts',(-3.75838203887398,59.112499999774,-11.5671105274575));
#296576=CARTESIAN_POINT('Ctrl Pts',(-7.51676407774791,59.2624999997734,
-10.3459381770593));
#296577=CARTESIAN_POINT('Ctrl Pts',(-9.83957192047912,59.4124999997728,
-7.14886745759543));
#296578=CARTESIAN_POINT('Ctrl Pts',(-12.1623797632103,59.5624999997722,
-3.95179673813153));
#296579=CARTESIAN_POINT('Ctrl Pts',(-12.1623797632103,59.7124999997716,
2.97892388940601E-15));
#296580=CARTESIAN_POINT('Ctrl Pts',(-12.1623797632103,59.862499999771,3.95179673813154));
#296581=CARTESIAN_POINT('Ctrl Pts',(-9.83957192047912,60.0124999997704,
7.14886745759543));
#296582=CARTESIAN_POINT('Ctrl Pts',(-7.5167640777479,60.1624999997698,10.3459381770593));
#296583=CARTESIAN_POINT('Ctrl Pts',(-3.75838203887397,60.3124999997692,
11.5671105274575));
#296584=CARTESIAN_POINT('Ctrl Pts',(-4.49489945775801E-14,60.4624999997686,
12.7882828778556));
#296585=CARTESIAN_POINT('Ctrl Pts',(3.75838203887388,60.612499999768,11.5671105274575));
#296586=CARTESIAN_POINT('Ctrl Pts',(7.51676407774781,60.7624999997674,10.3459381770593));
#296587=CARTESIAN_POINT('Ctrl Pts',(9.83957192047903,60.9124999997668,7.14886745759543));
#296588=CARTESIAN_POINT('Ctrl Pts',(12.1623797632103,61.0624999997662,3.95179673813153));
#296589=CARTESIAN_POINT('Ctrl Pts',(12.1623797632102,61.2124999997656,-1.489461944703E-15));
#296590=CARTESIAN_POINT('Ctrl Pts',(12.1623797632102,61.362499999765,-3.95179673813154));
#296591=CARTESIAN_POINT('Ctrl Pts',(9.83957192047902,61.5124999997644,-7.14886745759543));
#296592=CARTESIAN_POINT('Ctrl Pts',(7.51676407774781,61.6624999997638,-10.3459381770593));
#296593=CARTESIAN_POINT('Ctrl Pts',(3.75838203887388,61.8124999997632,-11.5671105274575));
#296594=CARTESIAN_POINT('Ctrl Pts',(-4.89450751520023E-14,61.9624999997626,
-12.7882828778556));
#296595=CARTESIAN_POINT('Ctrl Pts',(-3.75838203887398,62.112499999762,-11.5671105274575));
#296596=CARTESIAN_POINT('Ctrl Pts',(-7.51676407774791,62.2624999997614,
-10.3459381770593));
#296597=CARTESIAN_POINT('Ctrl Pts',(-9.83957192047912,62.4124999997608,
-7.14886745759543));
#296598=CARTESIAN_POINT('Ctrl Pts',(-12.1623797632103,62.5624999997602,
-3.95179673813153));
#296599=CARTESIAN_POINT('Ctrl Pts',(-12.1623797632103,62.7124999997596,
2.97892388940601E-15));
#296600=CARTESIAN_POINT('Ctrl Pts',(-12.1623797632103,62.862499999759,3.95179673813154));
#296601=CARTESIAN_POINT('Ctrl Pts',(-9.83957192047912,63.0124999997584,
7.14886745759543));
#296602=CARTESIAN_POINT('Ctrl Pts',(-7.5167640777479,63.1624999997578,10.3459381770593));
#296603=CARTESIAN_POINT('Ctrl Pts',(-3.75838203887398,63.3124999997572,
11.5671105274575));
#296604=CARTESIAN_POINT('Ctrl Pts',(-4.66767038492419E-14,63.4624999997566,
12.7882828778556));
#296605=CARTESIAN_POINT('Ctrl Pts',(3.75838203887388,63.612499999756,11.5671105274575));
#296606=CARTESIAN_POINT('Ctrl Pts',(7.51676407774781,63.7624999997554,10.3459381770593));
#296607=CARTESIAN_POINT('Ctrl Pts',(9.83957192047903,63.9124999997548,7.14886745759543));
#296608=CARTESIAN_POINT('Ctrl Pts',(12.1623797632102,64.0624999997542,3.95179673813153));
#296609=CARTESIAN_POINT('Ctrl Pts',(12.1623797632102,64.2124999997536,-1.489461944703E-15));
#296610=CARTESIAN_POINT('Ctrl Pts',(12.1623797632102,64.362499999753,-3.95179673813154));
#296611=CARTESIAN_POINT('Ctrl Pts',(9.83957192047902,64.5124999997524,-7.14886745759543));
#296612=CARTESIAN_POINT('Ctrl Pts',(7.51676407774781,64.6624999997518,-10.3459381770593));
#296613=CARTESIAN_POINT('Ctrl Pts',(3.75838203887388,64.8124999997512,-11.5671105274575));
#296614=CARTESIAN_POINT('Ctrl Pts',(-5.06727844236642E-14,64.9624999997506,
-12.7882828778556));
#296615=CARTESIAN_POINT('Ctrl Pts',(-3.75838203887398,65.11249999975,-11.5671105274575));
#296616=CARTESIAN_POINT('Ctrl Pts',(-7.51676407774791,65.2624999997494,
-10.3459381770593));
#296617=CARTESIAN_POINT('Ctrl Pts',(-9.83957192047913,65.4124999997488,
-7.14886745759543));
#296618=CARTESIAN_POINT('Ctrl Pts',(-12.1623797632103,65.5624999997482,
-3.95179673813153));
#296619=CARTESIAN_POINT('Ctrl Pts',(-12.1623797632103,65.7124999997476,
2.97892388940601E-15));
#296620=CARTESIAN_POINT('Ctrl Pts',(-12.1623797632103,65.862499999747,3.95179673813154));
#296621=CARTESIAN_POINT('Ctrl Pts',(-9.83957192047912,66.0124999997464,
7.14886745759543));
#296622=CARTESIAN_POINT('Ctrl Pts',(-7.51676407774791,66.1624999997458,
10.3459381770593));
#296623=CARTESIAN_POINT('Ctrl Pts',(-3.75838203887398,66.3124999997452,
11.5671105274575));
#296624=CARTESIAN_POINT('Ctrl Pts',(-4.84044131209037E-14,66.4624999997446,
12.7882828778556));
#296625=CARTESIAN_POINT('Ctrl Pts',(3.75838203887388,66.612499999744,11.5671105274575));
#296626=CARTESIAN_POINT('Ctrl Pts',(7.51676407774781,66.7624999997434,10.3459381770593));
#296627=CARTESIAN_POINT('Ctrl Pts',(9.83957192047902,66.9124999997428,7.14886745759543));
#296628=CARTESIAN_POINT('Ctrl Pts',(12.1623797632102,67.0624999997422,3.95179673813153));
#296629=CARTESIAN_POINT('Ctrl Pts',(12.1623797632102,67.2124999997416,-1.489461944703E-15));
#296630=CARTESIAN_POINT('Ctrl Pts',(12.1623797632102,67.362499999741,-3.95179673813154));
#296631=CARTESIAN_POINT('Ctrl Pts',(9.83957192047902,67.5124999997404,-7.14886745759543));
#296632=CARTESIAN_POINT('Ctrl Pts',(7.51676407774781,67.6624999997398,-10.3459381770593));
#296633=CARTESIAN_POINT('Ctrl Pts',(3.75838203887388,67.8124999997392,-11.5671105274575));
#296634=CARTESIAN_POINT('Ctrl Pts',(-5.2400493695326E-14,67.9624999997386,
-12.7882828778556));
#296635=CARTESIAN_POINT('Ctrl Pts',(-3.75838203887398,68.112499999738,-11.5671105274575));
#296636=CARTESIAN_POINT('Ctrl Pts',(-7.51676407774791,68.2624999997374,
-10.3459381770593));
#296637=CARTESIAN_POINT('Ctrl Pts',(-9.83957192047913,68.4124999997368,
-7.14886745759543));
#296638=CARTESIAN_POINT('Ctrl Pts',(-12.1623797632103,68.5624999997362,
-3.95179673813153));
#296639=CARTESIAN_POINT('Ctrl Pts',(-12.1623797632103,68.7124999997356,
2.97892388940601E-15));
#296640=CARTESIAN_POINT('Ctrl Pts',(-12.1623797632103,68.862499999735,3.95179673813154));
#296641=CARTESIAN_POINT('Ctrl Pts',(-9.83957192047913,69.0124999997344,
7.14886745759543));
#296642=CARTESIAN_POINT('Ctrl Pts',(-7.51676407774791,69.1624999997338,
10.3459381770593));
#296643=CARTESIAN_POINT('Ctrl Pts',(-3.75838203887398,69.3124999997332,
11.5671105274575));
#296644=CARTESIAN_POINT('Ctrl Pts',(-5.01321223925656E-14,69.4624999997326,
12.7882828778556));
#296645=CARTESIAN_POINT('Ctrl Pts',(3.75838203887388,69.612499999732,11.5671105274575));
#296646=CARTESIAN_POINT('Ctrl Pts',(7.51676407774781,69.7624999997314,10.3459381770593));
#296647=CARTESIAN_POINT('Ctrl Pts',(9.83957192047902,69.9124999997308,7.14886745759543));
#296648=CARTESIAN_POINT('Ctrl Pts',(12.1623797632102,70.0624999997302,3.95179673813153));
#296649=CARTESIAN_POINT('Ctrl Pts',(12.1623797632102,70.2124999997296,-1.489461944703E-15));
#296650=CARTESIAN_POINT('Ctrl Pts',(12.1623797632102,70.362499999729,-3.95179673813154));
#296651=CARTESIAN_POINT('Ctrl Pts',(9.83957192047902,70.5124999997284,-7.14886745759543));
#296652=CARTESIAN_POINT('Ctrl Pts',(7.5167640777478,70.6624999997278,-10.3459381770593));
#296653=CARTESIAN_POINT('Ctrl Pts',(3.75838203887388,70.8124999997272,-11.5671105274575));
#296654=CARTESIAN_POINT('Ctrl Pts',(-5.41282029669879E-14,70.9624999997266,
-12.7882828778556));
#296655=CARTESIAN_POINT('Ctrl Pts',(-3.75838203887398,71.112499999726,-11.5671105274575));
#296656=CARTESIAN_POINT('Ctrl Pts',(-7.51676407774791,71.2624999997254,
-10.3459381770593));
#296657=CARTESIAN_POINT('Ctrl Pts',(-9.83957192047913,71.4124999997248,
-7.14886745759543));
#296658=CARTESIAN_POINT('Ctrl Pts',(-12.1623797632103,71.5624999997242,
-3.95179673813153));
#296659=CARTESIAN_POINT('Ctrl Pts',(-12.1623797632103,71.7124999997236,
2.97892388940601E-15));
#296660=CARTESIAN_POINT('Ctrl Pts',(-12.1623797632103,71.862499999723,3.95179673813154));
#296661=CARTESIAN_POINT('Ctrl Pts',(-9.83957192047913,72.0124999997224,
7.14886745759543));
#296662=CARTESIAN_POINT('Ctrl Pts',(-7.51676407774791,72.1624999997218,
10.3459381770593));
#296663=CARTESIAN_POINT('Ctrl Pts',(-3.75838203887398,72.3124999997212,
11.5671105274575));
#296664=CARTESIAN_POINT('Ctrl Pts',(-5.18598316642274E-14,72.4624999997206,
12.7882828778556));
#296665=CARTESIAN_POINT('Ctrl Pts',(3.75838203887388,72.61249999972,11.5671105274575));
#296666=CARTESIAN_POINT('Ctrl Pts',(7.51676407774781,72.7624999997194,10.3459381770593));
#296667=CARTESIAN_POINT('Ctrl Pts',(9.83957192047902,72.9124999997188,7.14886745759543));
#296668=CARTESIAN_POINT('Ctrl Pts',(12.1623797632102,73.0624999997182,3.95179673813153));
#296669=CARTESIAN_POINT('Ctrl Pts',(12.1623797632102,73.2124999997176,-1.489461944703E-15));
#296670=CARTESIAN_POINT('Ctrl Pts',(12.1623797632102,73.362499999717,-3.95179673813154));
#296671=CARTESIAN_POINT('Ctrl Pts',(9.83957192047902,73.5124999997164,-7.14886745759543));
#296672=CARTESIAN_POINT('Ctrl Pts',(7.5167640777478,73.6624999997158,-10.3459381770593));
#296673=CARTESIAN_POINT('Ctrl Pts',(3.75838203887387,73.8124999997152,-11.5671105274575));
#296674=CARTESIAN_POINT('Ctrl Pts',(-5.58559122386497E-14,73.9624999997146,
-12.7882828778556));
#296675=CARTESIAN_POINT('Ctrl Pts',(-3.75838203887398,74.112499999714,-11.5671105274575));
#296676=CARTESIAN_POINT('Ctrl Pts',(-7.51676407774791,74.2624999997134,
-10.3459381770593));
#296677=CARTESIAN_POINT('Ctrl Pts',(-9.83957192047913,74.4124999997128,
-7.14886745759543));
#296678=CARTESIAN_POINT('Ctrl Pts',(-12.1623797632103,74.5624999997122,
-3.95179673813153));
#296679=CARTESIAN_POINT('Ctrl Pts',(-12.1623797632103,74.7124999997116,
2.97892388940601E-15));
#296680=CARTESIAN_POINT('Ctrl Pts',(-12.1623797632103,74.862499999711,3.95179673813154));
#296681=CARTESIAN_POINT('Ctrl Pts',(-9.83957192047913,75.0124999997104,
7.14886745759543));
#296682=CARTESIAN_POINT('Ctrl Pts',(-7.51676407774791,75.1624999997098,
10.3459381770593));
#296683=CARTESIAN_POINT('Ctrl Pts',(-3.75838203887398,75.3124999997092,
11.5671105274575));
#296684=CARTESIAN_POINT('Ctrl Pts',(-5.35875409358893E-14,75.4624999997086,
12.7882828778556));
#296685=CARTESIAN_POINT('Ctrl Pts',(3.75838203887388,75.612499999708,11.5671105274575));
#296686=CARTESIAN_POINT('Ctrl Pts',(7.5167640777478,75.7624999997074,10.3459381770593));
#296687=CARTESIAN_POINT('Ctrl Pts',(9.83957192047902,75.9124999997068,7.14886745759543));
#296688=CARTESIAN_POINT('Ctrl Pts',(12.1623797632102,76.0624999997062,3.95179673813153));
#296689=CARTESIAN_POINT('Ctrl Pts',(12.1623797632102,76.2124999997056,-1.489461944703E-15));
#296690=CARTESIAN_POINT('Ctrl Pts',(12.1623797632102,76.362499999705,-3.95179673813154));
#296691=CARTESIAN_POINT('Ctrl Pts',(9.83957192047902,76.5124999997044,-7.14886745759543));
#296692=CARTESIAN_POINT('Ctrl Pts',(7.5167640777478,76.6624999997038,-10.3459381770593));
#296693=CARTESIAN_POINT('Ctrl Pts',(3.75838203887387,76.8124999997032,-11.5671105274575));
#296694=CARTESIAN_POINT('Ctrl Pts',(-5.75836215103115E-14,76.9624999997026,
-12.7882828778556));
#296695=CARTESIAN_POINT('Ctrl Pts',(-3.75838203887399,77.112499999702,-11.5671105274575));
#296696=CARTESIAN_POINT('Ctrl Pts',(-7.51676407774791,77.2624999997014,
-10.3459381770593));
#296697=CARTESIAN_POINT('Ctrl Pts',(-9.83957192047913,77.4124999997008,
-7.14886745759543));
#296698=CARTESIAN_POINT('Ctrl Pts',(-12.1623797632103,77.5624999997002,
-3.95179673813153));
#296699=CARTESIAN_POINT('Ctrl Pts',(-12.1623797632103,77.7124999996996,
2.97892388940601E-15));
#296700=CARTESIAN_POINT('Ctrl Pts',(-12.1623797632103,77.862499999699,3.95179673813154));
#296701=CARTESIAN_POINT('Ctrl Pts',(-9.83957192047913,78.0124999996984,
7.14886745759543));
#296702=CARTESIAN_POINT('Ctrl Pts',(-7.51676407774791,78.1624999996978,
10.3459381770593));
#296703=CARTESIAN_POINT('Ctrl Pts',(-3.75838203887398,78.3124999996972,
11.5671105274575));
#296704=CARTESIAN_POINT('Ctrl Pts',(-5.53152502075511E-14,78.4624999996966,
12.7882828778556));
#296705=CARTESIAN_POINT('Ctrl Pts',(3.75838203887387,78.612499999696,11.5671105274575));
#296706=CARTESIAN_POINT('Ctrl Pts',(7.5167640777478,78.7624999996954,10.3459381770593));
#296707=CARTESIAN_POINT('Ctrl Pts',(9.83957192047902,78.9124999996948,7.14886745759543));
#296708=CARTESIAN_POINT('Ctrl Pts',(12.1623797632102,79.0624999996942,3.95179673813153));
#296709=CARTESIAN_POINT('Ctrl Pts',(12.1623797632102,79.2124999996936,-1.489461944703E-15));
#296710=CARTESIAN_POINT('Ctrl Pts',(12.1623797632102,79.362499999693,-3.95179673813154));
#296711=CARTESIAN_POINT('Ctrl Pts',(9.83957192047902,79.5124999996924,-7.14886745759543));
#296712=CARTESIAN_POINT('Ctrl Pts',(7.5167640777478,79.6624999996918,-10.3459381770593));
#296713=CARTESIAN_POINT('Ctrl Pts',(3.75838203887387,79.8124999996912,-11.5671105274575));
#296714=CARTESIAN_POINT('Ctrl Pts',(-5.93113307819734E-14,79.9624999996906,
-12.7882828778556));
#296715=CARTESIAN_POINT('Ctrl Pts',(-3.75838203887399,80.11249999969,-11.5671105274575));
#296716=CARTESIAN_POINT('Ctrl Pts',(-7.51676407774791,80.2624999996894,
-10.3459381770593));
#296717=CARTESIAN_POINT('Ctrl Pts',(-9.83957192047913,80.4124999996888,
-7.14886745759543));
#296718=CARTESIAN_POINT('Ctrl Pts',(-12.1623797632104,80.5624999996882,
-3.95179673813153));
#296719=CARTESIAN_POINT('Ctrl Pts',(-12.1623797632104,80.7124999996876,
2.97892388940601E-15));
#296720=CARTESIAN_POINT('Ctrl Pts',(-12.1623797632104,80.862499999687,3.95179673813154));
#296721=CARTESIAN_POINT('Ctrl Pts',(-9.83957192047913,81.0124999996864,
7.14886745759543));
#296722=CARTESIAN_POINT('Ctrl Pts',(-7.51676407774791,81.1624999996858,
10.3459381770593));
#296723=CARTESIAN_POINT('Ctrl Pts',(-3.75838203887399,81.3124999996852,
11.5671105274575));
#296724=CARTESIAN_POINT('Ctrl Pts',(-5.70429594792129E-14,81.4624999996846,
12.7882828778556));
#296725=CARTESIAN_POINT('Ctrl Pts',(3.75838203887387,81.612499999684,11.5671105274575));
#296726=CARTESIAN_POINT('Ctrl Pts',(7.5167640777478,81.7624999996834,10.3459381770593));
#296727=CARTESIAN_POINT('Ctrl Pts',(9.83957192047902,81.9124999996828,7.14886745759543));
#296728=CARTESIAN_POINT('Ctrl Pts',(12.1623797632102,82.0624999996822,3.95179673813153));
#296729=CARTESIAN_POINT('Ctrl Pts',(12.1623797632102,82.2124999996816,-1.489461944703E-15));
#296730=CARTESIAN_POINT('Ctrl Pts',(12.1623797632102,82.362499999681,-3.95179673813154));
#296731=CARTESIAN_POINT('Ctrl Pts',(9.83957192047902,82.5124999996804,-7.14886745759543));
#296732=CARTESIAN_POINT('Ctrl Pts',(7.5167640777478,82.6624999996798,-10.3459381770593));
#296733=CARTESIAN_POINT('Ctrl Pts',(3.75838203887387,82.8124999996792,-11.5671105274575));
#296734=CARTESIAN_POINT('Ctrl Pts',(-6.10390400536352E-14,82.9624999996786,
-12.7882828778556));
#296735=CARTESIAN_POINT('Ctrl Pts',(-3.75838203887399,83.112499999678,-11.5671105274575));
#296736=CARTESIAN_POINT('Ctrl Pts',(-7.51676407774792,83.2624999996774,
-10.3459381770593));
#296737=CARTESIAN_POINT('Ctrl Pts',(-9.83957192047914,83.4124999996768,
-7.14886745759543));
#296738=CARTESIAN_POINT('Ctrl Pts',(-12.1623797632104,83.5624999996762,
-3.95179673813153));
#296739=CARTESIAN_POINT('Ctrl Pts',(-12.1623797632104,83.7124999996756,
2.97892388940601E-15));
#296740=CARTESIAN_POINT('Ctrl Pts',(-12.1623797632104,83.862499999675,3.95179673813154));
#296741=CARTESIAN_POINT('Ctrl Pts',(-9.83957192047913,84.0124999996744,
7.14886745759543));
#296742=CARTESIAN_POINT('Ctrl Pts',(-7.51676407774791,84.1624999996738,
10.3459381770593));
#296743=CARTESIAN_POINT('Ctrl Pts',(-3.75838203887399,84.3124999996732,
11.5671105274575));
#296744=CARTESIAN_POINT('Ctrl Pts',(-5.87706687508748E-14,84.4624999996726,
12.7882828778556));
#296745=CARTESIAN_POINT('Ctrl Pts',(3.75838203887387,84.6124999996721,11.5671105274575));
#296746=CARTESIAN_POINT('Ctrl Pts',(7.5167640777478,84.7624999996714,10.3459381770593));
#296747=CARTESIAN_POINT('Ctrl Pts',(9.83957192047902,84.9124999996708,7.14886745759543));
#296748=CARTESIAN_POINT('Ctrl Pts',(12.1623797632102,85.0624999996702,3.95179673813153));
#296749=CARTESIAN_POINT('Ctrl Pts',(12.1623797632102,85.2124999996696,-1.489461944703E-15));
#296750=CARTESIAN_POINT('Ctrl Pts',(12.1623797632102,85.362499999669,-3.95179673813154));
#296751=CARTESIAN_POINT('Ctrl Pts',(9.83957192047901,85.5124999996684,-7.14886745759543));
#296752=CARTESIAN_POINT('Ctrl Pts',(7.5167640777478,85.6624999996678,-10.3459381770593));
#296753=CARTESIAN_POINT('Ctrl Pts',(3.75838203887387,85.8124999996672,-11.5671105274575));
#296754=CARTESIAN_POINT('Ctrl Pts',(-6.27667493252971E-14,85.9624999996666,
-12.7882828778556));
#296755=CARTESIAN_POINT('Ctrl Pts',(-3.75838203887399,86.112499999666,-11.5671105274575));
#296756=CARTESIAN_POINT('Ctrl Pts',(-7.51676407774792,86.2624999996654,
-10.3459381770593));
#296757=CARTESIAN_POINT('Ctrl Pts',(-9.83957192047914,86.4124999996648,
-7.14886745759543));
#296758=CARTESIAN_POINT('Ctrl Pts',(-12.1623797632104,86.5624999996642,
-3.95179673813153));
#296759=CARTESIAN_POINT('Ctrl Pts',(-12.1623797632104,86.7124999996636,
2.97892388940601E-15));
#296760=CARTESIAN_POINT('Ctrl Pts',(-12.1623797632104,86.862499999663,3.95179673813154));
#296761=CARTESIAN_POINT('Ctrl Pts',(-9.83957192047914,87.0124999996624,
7.14886745759543));
#296762=CARTESIAN_POINT('Ctrl Pts',(-7.51676407774792,87.1624999996618,
10.3459381770593));
#296763=CARTESIAN_POINT('Ctrl Pts',(-3.75838203887399,87.3124999996612,
11.5671105274575));
#296764=CARTESIAN_POINT('Ctrl Pts',(-6.04983780225366E-14,87.4624999996606,
12.7882828778556));
#296765=CARTESIAN_POINT('Ctrl Pts',(3.75838203887387,87.61249999966,11.5671105274575));
#296766=CARTESIAN_POINT('Ctrl Pts',(7.5167640777478,87.7624999996594,10.3459381770593));
#296767=CARTESIAN_POINT('Ctrl Pts',(9.83957192047901,87.9124999996588,7.14886745759543));
#296768=CARTESIAN_POINT('Ctrl Pts',(12.1623797632102,88.0624999996582,3.95179673813153));
#296769=CARTESIAN_POINT('Ctrl Pts',(12.1623797632102,88.2124999996576,-1.489461944703E-15));
#296770=CARTESIAN_POINT('Ctrl Pts',(12.1623797632102,88.362499999657,-3.95179673813154));
#296771=CARTESIAN_POINT('Ctrl Pts',(9.83957192047901,88.5124999996564,-7.14886745759543));
#296772=CARTESIAN_POINT('Ctrl Pts',(7.51676407774779,88.6624999996558,-10.3459381770593));
#296773=CARTESIAN_POINT('Ctrl Pts',(3.75838203887386,88.8124999996552,-11.5671105274575));
#296774=CARTESIAN_POINT('Ctrl Pts',(-6.44944585969589E-14,88.9624999996546,
-12.7882828778556));
#296775=CARTESIAN_POINT('Ctrl Pts',(-3.75838203887399,89.112499999654,-11.5671105274575));
#296776=CARTESIAN_POINT('Ctrl Pts',(-7.51676407774792,89.2624999996534,
-10.3459381770593));
#296777=CARTESIAN_POINT('Ctrl Pts',(-9.83957192047914,89.4124999996528,
-7.14886745759543));
#296778=CARTESIAN_POINT('Ctrl Pts',(-12.1623797632104,89.5624999996522,
-3.95179673813153));
#296779=CARTESIAN_POINT('Ctrl Pts',(-12.1623797632104,89.7124999996516,
2.97892388940601E-15));
#296780=CARTESIAN_POINT('Ctrl Pts',(-12.1623797632104,89.862499999651,3.95179673813154));
#296781=CARTESIAN_POINT('Ctrl Pts',(-9.83957192047914,90.0124999996504,
7.14886745759543));
#296782=CARTESIAN_POINT('Ctrl Pts',(-7.51676407774792,90.1624999996498,
10.3459381770593));
#296783=CARTESIAN_POINT('Ctrl Pts',(-3.75838203887399,90.3124999996492,
11.5671105274575));
#296784=CARTESIAN_POINT('Ctrl Pts',(-6.22260872941985E-14,90.4624999996486,
12.7882828778556));
#296785=CARTESIAN_POINT('Ctrl Pts',(3.75838203887387,90.612499999648,11.5671105274575));
#296786=CARTESIAN_POINT('Ctrl Pts',(7.5167640777478,90.7624999996474,10.3459381770593));
#296787=CARTESIAN_POINT('Ctrl Pts',(9.83957192047901,90.9124999996468,7.14886745759543));
#296788=CARTESIAN_POINT('Ctrl Pts',(12.1623797632102,91.0624999996462,3.95179673813153));
#296789=CARTESIAN_POINT('Ctrl Pts',(12.1623797632102,91.2124999996456,-1.489461944703E-15));
#296790=CARTESIAN_POINT('Ctrl Pts',(12.1623797632102,91.362499999645,-3.95179673813154));
#296791=CARTESIAN_POINT('Ctrl Pts',(9.83957192047901,91.5124999996444,-7.14886745759543));
#296792=CARTESIAN_POINT('Ctrl Pts',(7.51676407774779,91.6624999996438,-10.3459381770593));
#296793=CARTESIAN_POINT('Ctrl Pts',(3.75838203887386,91.8124999996432,-11.5671105274575));
#296794=CARTESIAN_POINT('Ctrl Pts',(-6.62221678686207E-14,91.9624999996426,
-12.7882828778556));
#296795=CARTESIAN_POINT('Ctrl Pts',(-3.75838203887399,92.112499999642,-11.5671105274575));
#296796=CARTESIAN_POINT('Ctrl Pts',(-7.51676407774792,92.2624999996414,
-10.3459381770593));
#296797=CARTESIAN_POINT('Ctrl Pts',(-9.83957192047914,92.4124999996408,
-7.14886745759543));
#296798=CARTESIAN_POINT('Ctrl Pts',(-12.1623797632104,92.5624999996402,
-3.95179673813153));
#296799=CARTESIAN_POINT('Ctrl Pts',(-12.1623797632104,92.7124999996396,
2.97892388940601E-15));
#296800=CARTESIAN_POINT('Ctrl Pts',(-12.1623797632104,92.862499999639,3.95179673813154));
#296801=CARTESIAN_POINT('Ctrl Pts',(-9.83957192047914,93.0124999996384,
7.14886745759543));
#296802=CARTESIAN_POINT('Ctrl Pts',(-7.51676407774792,93.1624999996378,
10.3459381770593));
#296803=CARTESIAN_POINT('Ctrl Pts',(-3.75838203887399,93.3124999996372,
11.5671105274575));
#296804=CARTESIAN_POINT('Ctrl Pts',(-6.39537965658603E-14,93.4624999996366,
12.7882828778556));
#296805=CARTESIAN_POINT('Ctrl Pts',(3.75838203887386,93.612499999636,11.5671105274575));
#296806=CARTESIAN_POINT('Ctrl Pts',(7.51676407774779,93.7624999996354,10.3459381770593));
#296807=CARTESIAN_POINT('Ctrl Pts',(9.83957192047901,93.9124999996348,7.14886745759543));
#296808=CARTESIAN_POINT('Ctrl Pts',(12.1623797632102,94.0624999996342,3.95179673813153));
#296809=CARTESIAN_POINT('Ctrl Pts',(12.1623797632102,94.2124999996336,-1.489461944703E-15));
#296810=CARTESIAN_POINT('Ctrl Pts',(12.1623797632102,94.362499999633,-3.95179673813154));
#296811=CARTESIAN_POINT('Ctrl Pts',(9.83957192047901,94.5124999996324,-7.14886745759543));
#296812=CARTESIAN_POINT('Ctrl Pts',(7.51676407774779,94.6624999996318,-10.3459381770593));
#296813=CARTESIAN_POINT('Ctrl Pts',(3.75838203887386,94.8124999996312,-11.5671105274575));
#296814=CARTESIAN_POINT('Ctrl Pts',(-6.79498771402825E-14,94.9624999996306,
-12.7882828778556));
#296815=CARTESIAN_POINT('Ctrl Pts',(-3.758382038874,95.11249999963,-11.5671105274575));
#296816=CARTESIAN_POINT('Ctrl Pts',(-7.51676407774792,95.2624999996294,
-10.3459381770593));
#296817=CARTESIAN_POINT('Ctrl Pts',(-9.83957192047914,95.4124999996288,
-7.14886745759543));
#296818=CARTESIAN_POINT('Ctrl Pts',(-12.1623797632104,95.5624999996282,
-3.95179673813153));
#296819=CARTESIAN_POINT('Ctrl Pts',(-12.1623797632104,95.7124999996276,
2.97892388940601E-15));
#296820=CARTESIAN_POINT('Ctrl Pts',(-12.1623797632104,95.862499999627,3.95179673813154));
#296821=CARTESIAN_POINT('Ctrl Pts',(-9.83957192047914,96.0124999996264,
7.14886745759543));
#296822=CARTESIAN_POINT('Ctrl Pts',(-7.51676407774792,96.1624999996258,
10.3459381770593));
#296823=CARTESIAN_POINT('Ctrl Pts',(-3.75838203887399,96.3124999996252,
11.5671105274575));
#296824=CARTESIAN_POINT('Ctrl Pts',(-6.56815058375222E-14,96.4624999996246,
12.7882828778556));
#296825=CARTESIAN_POINT('Ctrl Pts',(3.75838203887386,96.612499999624,11.5671105274575));
#296826=CARTESIAN_POINT('Ctrl Pts',(7.51676407774779,96.7624999996234,10.3459381770593));
#296827=CARTESIAN_POINT('Ctrl Pts',(9.83957192047901,96.9124999996228,7.14886745759543));
#296828=CARTESIAN_POINT('Ctrl Pts',(12.1623797632102,97.0624999996222,3.95179673813153));
#296829=CARTESIAN_POINT('Ctrl Pts',(12.1623797632102,97.2124999996216,-1.489461944703E-15));
#296830=CARTESIAN_POINT('Ctrl Pts',(12.1623797632102,97.3624999996211,-3.95179673813154));
#296831=CARTESIAN_POINT('Ctrl Pts',(9.83957192047901,97.5124999996204,-7.14886745759543));
#296832=CARTESIAN_POINT('Ctrl Pts',(7.51676407774779,97.6624999996198,-10.3459381770593));
#296833=CARTESIAN_POINT('Ctrl Pts',(3.75838203887386,97.8124999996192,-11.5671105274575));
#296834=CARTESIAN_POINT('Ctrl Pts',(-6.96775864119444E-14,97.9624999996187,
-12.7882828778556));
#296835=CARTESIAN_POINT('Ctrl Pts',(-3.758382038874,98.112499999618,-11.5671105274575));
#296836=CARTESIAN_POINT('Ctrl Pts',(-7.51676407774793,98.2624999996174,
-10.3459381770593));
#296837=CARTESIAN_POINT('Ctrl Pts',(-9.83957192047914,98.4124999996168,
-7.14886745759543));
#296838=CARTESIAN_POINT('Ctrl Pts',(-12.1623797632104,98.5624999996162,
-3.95179673813153));
#296839=CARTESIAN_POINT('Ctrl Pts',(-12.1623797632104,98.7124999996156,
2.97892388940601E-15));
#296840=CARTESIAN_POINT('Ctrl Pts',(-12.1623797632104,98.862499999615,3.95179673813154));
#296841=CARTESIAN_POINT('Ctrl Pts',(-9.83957192047914,99.0124999996144,
7.14886745759543));
#296842=CARTESIAN_POINT('Ctrl Pts',(-7.51676407774792,99.1624999996138,
10.3459381770593));
#296843=CARTESIAN_POINT('Ctrl Pts',(-3.758382038874,99.3124999996132,11.5671105274575));
#296844=CARTESIAN_POINT('Ctrl Pts',(-6.7409215109184E-14,99.4624999996126,
12.7882828778556));
#296845=CARTESIAN_POINT('Ctrl Pts',(3.75838203887386,99.612499999612,11.5671105274575));
#296846=CARTESIAN_POINT('Ctrl Pts',(7.51676407774779,99.7624999996114,10.3459381770593));
#296847=CARTESIAN_POINT('Ctrl Pts',(9.83957192047901,99.9124999996108,7.14886745759543));
#296848=CARTESIAN_POINT('Ctrl Pts',(12.1623797632102,100.06249999961,3.95179673813153));
#296849=CARTESIAN_POINT('Ctrl Pts',(12.1623797632102,100.21249999961,-1.489461944703E-15));
#296850=CARTESIAN_POINT('Ctrl Pts',(12.1623797632102,100.362499999609,-3.95179673813154));
#296851=CARTESIAN_POINT('Ctrl Pts',(9.839571920479,100.512499999608,-7.14886745759543));
#296852=CARTESIAN_POINT('Ctrl Pts',(7.51676407774779,100.662499999608,-10.3459381770593));
#296853=CARTESIAN_POINT('Ctrl Pts',(3.75838203887386,100.812499999607,-11.5671105274575));
#296854=CARTESIAN_POINT('Ctrl Pts',(-7.14052956836063E-14,100.962499999607,
-12.7882828778556));
#296855=CARTESIAN_POINT('Ctrl Pts',(-3.758382038874,101.112499999606,-11.5671105274575));
#296856=CARTESIAN_POINT('Ctrl Pts',(-7.51676407774793,101.262499999605,
-10.3459381770593));
#296857=CARTESIAN_POINT('Ctrl Pts',(-9.83957192047915,101.412499999605,
-7.14886745759543));
#296858=CARTESIAN_POINT('Ctrl Pts',(-12.1623797632104,101.562499999604,
-3.95179673813153));
#296859=CARTESIAN_POINT('Ctrl Pts',(-12.1623797632104,101.712499999604,
2.97892388940601E-15));
#296860=CARTESIAN_POINT('Ctrl Pts',(-12.1623797632104,101.862499999603,
3.95179673813154));
#296861=CARTESIAN_POINT('Ctrl Pts',(-9.83957192047914,102.012499999602,
7.14886745759543));
#296862=CARTESIAN_POINT('Ctrl Pts',(-7.51676407774793,102.162499999602,
10.3459381770593));
#296863=CARTESIAN_POINT('Ctrl Pts',(-3.758382038874,102.312499999601,11.5671105274575));
#296864=CARTESIAN_POINT('Ctrl Pts',(-6.91369243808458E-14,102.462499999601,
12.7882828778556));
#296865=CARTESIAN_POINT('Ctrl Pts',(3.75838203887386,102.6124999996,11.5671105274575));
#296866=CARTESIAN_POINT('Ctrl Pts',(7.51676407774779,102.762499999599,10.3459381770593));
#296867=CARTESIAN_POINT('Ctrl Pts',(9.839571920479,102.912499999599,7.14886745759543));
#296868=CARTESIAN_POINT('Ctrl Pts',(12.1623797632102,103.062499999598,3.95179673813153));
#296869=CARTESIAN_POINT('Ctrl Pts',(12.1623797632102,103.212499999598,-1.489461944703E-15));
#296870=CARTESIAN_POINT('Ctrl Pts',(12.1623797632102,103.362499999597,-3.95179673813154));
#296871=CARTESIAN_POINT('Ctrl Pts',(9.839571920479,103.512499999596,-7.14886745759543));
#296872=CARTESIAN_POINT('Ctrl Pts',(7.51676407774779,103.662499999596,-10.3459381770593));
#296873=CARTESIAN_POINT('Ctrl Pts',(3.75838203887386,103.812499999595,-11.5671105274575));
#296874=CARTESIAN_POINT('Ctrl Pts',(-7.31330049552681E-14,103.962499999595,
-12.7882828778556));
#296875=CARTESIAN_POINT('Ctrl Pts',(-3.758382038874,104.112499999594,-11.5671105274575));
#296876=CARTESIAN_POINT('Ctrl Pts',(-7.51676407774793,104.262499999593,
-10.3459381770593));
#296877=CARTESIAN_POINT('Ctrl Pts',(-9.83957192047915,104.412499999593,
-7.14886745759543));
#296878=CARTESIAN_POINT('Ctrl Pts',(-12.1623797632104,104.562499999592,
-3.95179673813153));
#296879=CARTESIAN_POINT('Ctrl Pts',(-12.1623797632104,104.712499999592,
2.97892388940601E-15));
#296880=CARTESIAN_POINT('Ctrl Pts',(-12.1623797632104,104.862499999591,
3.95179673813154));
#296881=CARTESIAN_POINT('Ctrl Pts',(-9.83957192047915,105.01249999959,7.14886745759543));
#296882=CARTESIAN_POINT('Ctrl Pts',(-7.51676407774793,105.16249999959,10.3459381770593));
#296883=CARTESIAN_POINT('Ctrl Pts',(-3.758382038874,105.312499999589,11.5671105274575));
#296884=CARTESIAN_POINT('Ctrl Pts',(-7.08646336525076E-14,105.462499999589,
12.7882828778556));
#296885=CARTESIAN_POINT('Ctrl Pts',(3.75838203887386,105.612499999588,11.5671105274575));
#296886=CARTESIAN_POINT('Ctrl Pts',(7.51676407774779,105.762499999587,10.3459381770593));
#296887=CARTESIAN_POINT('Ctrl Pts',(9.839571920479,105.912499999587,7.14886745759543));
#296888=CARTESIAN_POINT('Ctrl Pts',(12.1623797632102,106.062499999586,3.95179673813153));
#296889=CARTESIAN_POINT('Ctrl Pts',(12.1623797632102,106.212499999586,-1.489461944703E-15));
#296890=CARTESIAN_POINT('Ctrl Pts',(12.1623797632102,106.362499999585,-3.95179673813154));
#296891=CARTESIAN_POINT('Ctrl Pts',(9.839571920479,106.512499999584,-7.14886745759543));
#296892=CARTESIAN_POINT('Ctrl Pts',(7.51676407774778,106.662499999584,-10.3459381770593));
#296893=CARTESIAN_POINT('Ctrl Pts',(3.75838203887385,106.812499999583,-11.5671105274575));
#296894=CARTESIAN_POINT('Ctrl Pts',(-7.48607142269299E-14,106.962499999583,
-12.7882828778556));
#296895=CARTESIAN_POINT('Ctrl Pts',(-3.758382038874,107.112499999582,-11.5671105274575));
#296896=CARTESIAN_POINT('Ctrl Pts',(-7.51676407774793,107.262499999581,
-10.3459381770593));
#296897=CARTESIAN_POINT('Ctrl Pts',(-9.83957192047915,107.412499999581,
-7.14886745759543));
#296898=CARTESIAN_POINT('Ctrl Pts',(-12.1623797632104,107.56249999958,-3.95179673813153));
#296899=CARTESIAN_POINT('Ctrl Pts',(-12.1623797632104,107.71249999958,2.97892388940601E-15));
#296900=CARTESIAN_POINT('Ctrl Pts',(-12.1623797632104,107.862499999579,
3.95179673813154));
#296901=CARTESIAN_POINT('Ctrl Pts',(-9.83957192047915,108.012499999578,
7.14886745759543));
#296902=CARTESIAN_POINT('Ctrl Pts',(-7.51676407774793,108.162499999578,
10.3459381770593));
#296903=CARTESIAN_POINT('Ctrl Pts',(-3.758382038874,108.312499999577,11.5671105274575));
#296904=CARTESIAN_POINT('Ctrl Pts',(-7.25923429241695E-14,108.462499999577,
12.7882828778556));
#296905=CARTESIAN_POINT('Ctrl Pts',(3.75838203887386,108.612499999576,11.5671105274575));
#296906=CARTESIAN_POINT('Ctrl Pts',(7.51676407774779,108.762499999575,10.3459381770593));
#296907=CARTESIAN_POINT('Ctrl Pts',(9.839571920479,108.912499999575,7.14886745759543));
#296908=CARTESIAN_POINT('Ctrl Pts',(12.1623797632102,109.062499999574,3.95179673813153));
#296909=CARTESIAN_POINT('Ctrl Pts',(12.1623797632102,109.212499999574,-1.489461944703E-15));
#296910=CARTESIAN_POINT('Ctrl Pts',(12.1623797632102,109.362499999573,-3.95179673813154));
#296911=CARTESIAN_POINT('Ctrl Pts',(9.839571920479,109.512499999572,-7.14886745759543));
#296912=CARTESIAN_POINT('Ctrl Pts',(7.51676407774778,109.662499999572,-10.3459381770593));
#296913=CARTESIAN_POINT('Ctrl Pts',(3.75838203887385,109.812499999571,-11.5671105274575));
#296914=CARTESIAN_POINT('Ctrl Pts',(-7.65884234985918E-14,109.962499999571,
-12.7882828778556));
#296915=CARTESIAN_POINT('Ctrl Pts',(-3.75838203887401,110.11249999957,-11.5671105274575));
#296916=CARTESIAN_POINT('Ctrl Pts',(-7.51676407774793,110.262499999569,
-10.3459381770593));
#296917=CARTESIAN_POINT('Ctrl Pts',(-9.83957192047915,110.412499999569,
-7.14886745759543));
#296918=CARTESIAN_POINT('Ctrl Pts',(-12.1623797632104,110.562499999568,
-3.95179673813153));
#296919=CARTESIAN_POINT('Ctrl Pts',(-12.1623797632104,110.712499999568,
2.97892388940601E-15));
#296920=CARTESIAN_POINT('Ctrl Pts',(-12.1623797632104,110.862499999567,
3.95179673813154));
#296921=CARTESIAN_POINT('Ctrl Pts',(-9.83957192047915,111.012499999566,
7.14886745759543));
#296922=CARTESIAN_POINT('Ctrl Pts',(-7.51676407774793,111.162499999566,
10.3459381770593));
#296923=CARTESIAN_POINT('Ctrl Pts',(-3.758382038874,111.312499999565,11.5671105274575));
#296924=CARTESIAN_POINT('Ctrl Pts',(-7.43200521958313E-14,111.462499999565,
12.7882828778556));
#296925=CARTESIAN_POINT('Ctrl Pts',(3.75838203887385,111.612499999564,11.5671105274575));
#296926=CARTESIAN_POINT('Ctrl Pts',(7.51676407774778,111.762499999563,10.3459381770593));
#296927=CARTESIAN_POINT('Ctrl Pts',(9.839571920479,111.912499999563,7.14886745759543));
#296928=CARTESIAN_POINT('Ctrl Pts',(12.1623797632102,112.062499999562,3.95179673813153));
#296929=CARTESIAN_POINT('Ctrl Pts',(12.1623797632102,112.212499999562,-1.489461944703E-15));
#296930=CARTESIAN_POINT('Ctrl Pts',(12.1623797632102,112.362499999561,-3.95179673813154));
#296931=CARTESIAN_POINT('Ctrl Pts',(9.839571920479,112.51249999956,-7.14886745759543));
#296932=CARTESIAN_POINT('Ctrl Pts',(7.51676407774778,112.66249999956,-10.3459381770593));
#296933=CARTESIAN_POINT('Ctrl Pts',(3.75838203887385,112.812499999559,-11.5671105274575));
#296934=CARTESIAN_POINT('Ctrl Pts',(-7.83161327702536E-14,112.962499999559,
-12.7882828778556));
#296935=CARTESIAN_POINT('Ctrl Pts',(-3.75838203887401,113.112499999558,
-11.5671105274575));
#296936=CARTESIAN_POINT('Ctrl Pts',(-7.51676407774793,113.262499999557,
-10.3459381770593));
#296937=CARTESIAN_POINT('Ctrl Pts',(-9.83957192047915,113.412499999557,
-7.14886745759543));
#296938=CARTESIAN_POINT('Ctrl Pts',(-12.1623797632104,113.562499999556,
-3.95179673813153));
#296939=CARTESIAN_POINT('Ctrl Pts',(-12.1623797632104,113.712499999556,
2.97892388940601E-15));
#296940=CARTESIAN_POINT('Ctrl Pts',(-12.1623797632104,113.862499999555,
3.95179673813154));
#296941=CARTESIAN_POINT('Ctrl Pts',(-9.83957192047915,114.012499999554,
7.14886745759543));
#296942=CARTESIAN_POINT('Ctrl Pts',(-7.51676407774793,114.162499999554,
10.3459381770593));
#296943=CARTESIAN_POINT('Ctrl Pts',(-3.758382038874,114.312499999553,11.5671105274575));
#296944=CARTESIAN_POINT('Ctrl Pts',(-7.60477614674932E-14,114.462499999553,
12.7882828778556));
#296945=CARTESIAN_POINT('Ctrl Pts',(3.75838203887385,114.612499999552,11.5671105274575));
#296946=CARTESIAN_POINT('Ctrl Pts',(7.51676407774778,114.762499999551,10.3459381770593));
#296947=CARTESIAN_POINT('Ctrl Pts',(9.839571920479,114.912499999551,7.14886745759543));
#296948=CARTESIAN_POINT('Ctrl Pts',(12.1623797632102,115.06249999955,3.95179673813153));
#296949=CARTESIAN_POINT('Ctrl Pts',(12.1623797632102,115.21249999955,-1.489461944703E-15));
#296950=CARTESIAN_POINT('Ctrl Pts',(12.1623797632102,115.362499999549,-3.95179673813154));
#296951=CARTESIAN_POINT('Ctrl Pts',(9.839571920479,115.512499999548,-7.14886745759543));
#296952=CARTESIAN_POINT('Ctrl Pts',(7.51676407774778,115.662499999548,-10.3459381770593));
#296953=CARTESIAN_POINT('Ctrl Pts',(3.75838203887385,115.812499999547,-11.5671105274575));
#296954=CARTESIAN_POINT('Ctrl Pts',(-8.00438420419154E-14,115.962499999547,
-12.7882828778556));
#296955=CARTESIAN_POINT('Ctrl Pts',(-3.75838203887401,116.112499999546,
-11.5671105274575));
#296956=CARTESIAN_POINT('Ctrl Pts',(-7.51676407774794,116.262499999545,
-10.3459381770593));
#296957=CARTESIAN_POINT('Ctrl Pts',(-9.83957192047916,116.412499999545,
-7.14886745759543));
#296958=CARTESIAN_POINT('Ctrl Pts',(-12.1623797632104,116.562499999544,
-3.95179673813153));
#296959=CARTESIAN_POINT('Ctrl Pts',(-12.1623797632104,116.712499999544,
2.97892388940601E-15));
#296960=CARTESIAN_POINT('Ctrl Pts',(-12.1623797632104,116.862499999543,
3.95179673813154));
#296961=CARTESIAN_POINT('Ctrl Pts',(-9.83957192047915,117.012499999542,
7.14886745759543));
#296962=CARTESIAN_POINT('Ctrl Pts',(-7.51676407774793,117.162499999542,
10.3459381770593));
#296963=CARTESIAN_POINT('Ctrl Pts',(-3.75838203887401,117.312499999541,
11.5671105274575));
#296964=CARTESIAN_POINT('Ctrl Pts',(-7.7775470739155E-14,117.462499999541,
12.7882828778556));
#296965=CARTESIAN_POINT('Ctrl Pts',(3.75838203887385,117.61249999954,11.5671105274575));
#296966=CARTESIAN_POINT('Ctrl Pts',(7.51676407774778,117.762499999539,10.3459381770593));
#296967=CARTESIAN_POINT('Ctrl Pts',(9.839571920479,117.912499999539,7.14886745759543));
#296968=CARTESIAN_POINT('Ctrl Pts',(12.1623797632102,118.062499999538,3.95179673813153));
#296969=CARTESIAN_POINT('Ctrl Pts',(12.1623797632102,118.212499999538,-1.489461944703E-15));
#296970=CARTESIAN_POINT('Ctrl Pts',(12.1623797632102,118.362499999537,-3.95179673813154));
#296971=CARTESIAN_POINT('Ctrl Pts',(9.83957192047899,118.512499999536,-7.14886745759543));
#296972=CARTESIAN_POINT('Ctrl Pts',(7.51676407774778,118.662499999536,-10.3459381770593));
#296973=CARTESIAN_POINT('Ctrl Pts',(3.75838203887385,118.812499999535,-11.5671105274575));
#296974=CARTESIAN_POINT('Ctrl Pts',(-8.17715513135773E-14,118.962499999535,
-12.7882828778556));
#296975=CARTESIAN_POINT('Ctrl Pts',(-3.75838203887401,119.112499999534,
-11.5671105274575));
#296976=CARTESIAN_POINT('Ctrl Pts',(-7.51676407774794,119.262499999533,
-10.3459381770593));
#296977=CARTESIAN_POINT('Ctrl Pts',(-9.83957192047916,119.412499999533,
-7.14886745759543));
#296978=CARTESIAN_POINT('Ctrl Pts',(-12.1623797632104,119.562499999532,
-3.95179673813153));
#296979=CARTESIAN_POINT('Ctrl Pts',(-12.1623797632104,119.712499999532,
2.97892388940601E-15));
#296980=CARTESIAN_POINT('Ctrl Pts',(-12.1623797632104,119.862499999531,
3.95179673813154));
#296981=CARTESIAN_POINT('Ctrl Pts',(-9.83957192047916,120.01249999953,7.14886745759543));
#296982=CARTESIAN_POINT('Ctrl Pts',(-7.51676407774794,120.16249999953,10.3459381770593));
#296983=CARTESIAN_POINT('Ctrl Pts',(-3.75838203887401,120.312499999529,
11.5671105274575));
#296984=CARTESIAN_POINT('Ctrl Pts',(-7.95031800108169E-14,120.462499999529,
12.7882828778556));
#296985=CARTESIAN_POINT('Ctrl Pts',(3.75838203887385,120.612499999528,11.5671105274575));
#296986=CARTESIAN_POINT('Ctrl Pts',(7.51676407774778,120.762499999527,10.3459381770593));
#296987=CARTESIAN_POINT('Ctrl Pts',(9.83957192047899,120.912499999527,7.14886745759543));
#296988=CARTESIAN_POINT('Ctrl Pts',(12.1623797632102,121.062499999526,3.95179673813153));
#296989=CARTESIAN_POINT('Ctrl Pts',(12.1623797632102,121.212499999526,-1.489461944703E-15));
#296990=CARTESIAN_POINT('Ctrl Pts',(12.1623797632102,121.362499999525,-3.95179673813154));
#296991=CARTESIAN_POINT('Ctrl Pts',(9.83957192047899,121.512499999524,-7.14886745759543));
#296992=CARTESIAN_POINT('Ctrl Pts',(7.51676407774777,121.662499999524,-10.3459381770593));
#296993=CARTESIAN_POINT('Ctrl Pts',(3.75838203887385,121.812499999523,-11.5671105274575));
#296994=CARTESIAN_POINT('Ctrl Pts',(-8.34992605852391E-14,121.962499999523,
-12.7882828778556));
#296995=CARTESIAN_POINT('Ctrl Pts',(-3.75838203887401,122.112499999522,
-11.5671105274575));
#296996=CARTESIAN_POINT('Ctrl Pts',(-7.51676407774794,122.262499999521,
-10.3459381770593));
#296997=CARTESIAN_POINT('Ctrl Pts',(-9.83957192047916,122.412499999521,
-7.14886745759543));
#296998=CARTESIAN_POINT('Ctrl Pts',(-12.1623797632104,122.56249999952,-3.95179673813153));
#296999=CARTESIAN_POINT('Ctrl Pts',(-12.1623797632104,122.71249999952,2.97892388940601E-15));
#297000=CARTESIAN_POINT('Ctrl Pts',(-12.1623797632104,122.862499999519,
3.95179673813154));
#297001=CARTESIAN_POINT('Ctrl Pts',(-9.83957192047916,123.012499999518,
7.14886745759543));
#297002=CARTESIAN_POINT('Ctrl Pts',(-7.51676407774794,123.162499999518,
10.3459381770593));
#297003=CARTESIAN_POINT('Ctrl Pts',(-3.75838203887401,123.312499999517,
11.5671105274575));
#297004=CARTESIAN_POINT('Ctrl Pts',(-8.12308892824787E-14,123.462499999517,
12.7882828778556));
#297005=CARTESIAN_POINT('Ctrl Pts',(3.75838203887385,123.612499999516,11.5671105274575));
#297006=CARTESIAN_POINT('Ctrl Pts',(7.51676407774778,123.762499999515,10.3459381770593));
#297007=CARTESIAN_POINT('Ctrl Pts',(9.83957192047899,123.912499999515,7.14886745759543));
#297008=CARTESIAN_POINT('Ctrl Pts',(12.1623797632102,124.062499999514,3.95179673813153));
#297009=CARTESIAN_POINT('Ctrl Pts',(12.1623797632102,124.212499999514,-1.489461944703E-15));
#297010=CARTESIAN_POINT('Ctrl Pts',(12.1623797632102,124.362499999513,-3.95179673813154));
#297011=CARTESIAN_POINT('Ctrl Pts',(9.83957192047899,124.512499999512,-7.14886745759543));
#297012=CARTESIAN_POINT('Ctrl Pts',(7.51676407774777,124.662499999512,-10.3459381770593));
#297013=CARTESIAN_POINT('Ctrl Pts',(3.75838203887384,124.812499999511,-11.5671105274575));
#297014=CARTESIAN_POINT('Ctrl Pts',(-8.52269698569009E-14,124.962499999511,
-12.7882828778556));
#297015=CARTESIAN_POINT('Ctrl Pts',(-3.75838203887401,125.11249999951,-11.5671105274575));
#297016=CARTESIAN_POINT('Ctrl Pts',(-7.51676407774794,125.262499999509,
-10.3459381770593));
#297017=CARTESIAN_POINT('Ctrl Pts',(-9.83957192047916,125.412499999509,
-7.14886745759543));
#297018=CARTESIAN_POINT('Ctrl Pts',(-12.1623797632104,125.562499999508,
-3.95179673813153));
#297019=CARTESIAN_POINT('Ctrl Pts',(-12.1623797632104,125.712499999508,
2.97892388940601E-15));
#297020=CARTESIAN_POINT('Ctrl Pts',(-12.1623797632104,125.862499999507,
3.95179673813154));
#297021=CARTESIAN_POINT('Ctrl Pts',(-9.83957192047916,126.012499999506,
7.14886745759543));
#297022=CARTESIAN_POINT('Ctrl Pts',(-7.51676407774794,126.162499999506,
10.3459381770593));
#297023=CARTESIAN_POINT('Ctrl Pts',(-3.75838203887401,126.312499999505,
11.5671105274575));
#297024=CARTESIAN_POINT('Ctrl Pts',(-8.29585985541405E-14,126.462499999505,
12.7882828778556));
#297025=CARTESIAN_POINT('Ctrl Pts',(3.75838203887385,126.612499999504,11.5671105274575));
#297026=CARTESIAN_POINT('Ctrl Pts',(7.51676407774777,126.762499999503,10.3459381770593));
#297027=CARTESIAN_POINT('Ctrl Pts',(9.83957192047899,126.912499999503,7.14886745759543));
#297028=CARTESIAN_POINT('Ctrl Pts',(12.1623797632102,127.062499999502,3.95179673813153));
#297029=CARTESIAN_POINT('Ctrl Pts',(12.1623797632102,127.212499999502,-1.489461944703E-15));
#297030=CARTESIAN_POINT('Ctrl Pts',(12.1623797632102,127.362499999501,-3.95179673813154));
#297031=CARTESIAN_POINT('Ctrl Pts',(9.83957192047899,127.5124999995,-7.14886745759543));
#297032=CARTESIAN_POINT('Ctrl Pts',(7.51676407774777,127.6624999995,-10.3459381770593));
#297033=CARTESIAN_POINT('Ctrl Pts',(3.75838203887384,127.812499999499,-11.5671105274575));
#297034=CARTESIAN_POINT('Ctrl Pts',(-8.69546791285628E-14,127.962499999499,
-12.7882828778556));
#297035=CARTESIAN_POINT('Ctrl Pts',(-3.75838203887402,128.112499999498,
-11.5671105274575));
#297036=CARTESIAN_POINT('Ctrl Pts',(-7.51676407774795,128.262499999497,
-10.3459381770593));
#297037=CARTESIAN_POINT('Ctrl Pts',(-9.83957192047916,128.412499999497,
-7.14886745759543));
#297038=CARTESIAN_POINT('Ctrl Pts',(-12.1623797632104,128.562499999496,
-3.95179673813153));
#297039=CARTESIAN_POINT('Ctrl Pts',(-12.1623797632104,128.712499999496,
2.97892388940601E-15));
#297040=CARTESIAN_POINT('Ctrl Pts',(-12.1623797632104,128.862499999495,
3.95179673813154));
#297041=CARTESIAN_POINT('Ctrl Pts',(-9.83957192047916,129.012499999494,
7.14886745759543));
#297042=CARTESIAN_POINT('Ctrl Pts',(-7.51676407774794,129.162499999494,
10.3459381770593));
#297043=CARTESIAN_POINT('Ctrl Pts',(-3.75838203887401,129.312499999493,
11.5671105274575));
#297044=CARTESIAN_POINT('Ctrl Pts',(-8.46863078258024E-14,129.462499999493,
12.7882828778556));
#297045=CARTESIAN_POINT('Ctrl Pts',(3.75838203887384,129.612499999492,11.5671105274575));
#297046=CARTESIAN_POINT('Ctrl Pts',(7.51676407774777,129.762499999491,10.3459381770593));
#297047=CARTESIAN_POINT('Ctrl Pts',(9.83957192047899,129.912499999491,7.14886745759543));
#297048=CARTESIAN_POINT('Ctrl Pts',(12.1623797632102,130.06249999949,3.95179673813153));
#297049=CARTESIAN_POINT('Ctrl Pts',(12.1623797632102,130.21249999949,-1.489461944703E-15));
#297050=CARTESIAN_POINT('Ctrl Pts',(12.1623797632102,130.362499999489,-3.95179673813154));
#297051=CARTESIAN_POINT('Ctrl Pts',(9.83957192047899,130.512499999488,-7.14886745759543));
#297052=CARTESIAN_POINT('Ctrl Pts',(7.51676407774777,130.662499999488,-10.3459381770593));
#297053=CARTESIAN_POINT('Ctrl Pts',(3.75838203887384,130.812499999487,-11.5671105274575));
#297054=CARTESIAN_POINT('Ctrl Pts',(-8.86823884002247E-14,130.962499999487,
-12.7882828778556));
#297055=CARTESIAN_POINT('Ctrl Pts',(-3.75838203887402,131.112499999486,
-11.5671105274575));
#297056=CARTESIAN_POINT('Ctrl Pts',(-7.51676407774795,131.262499999485,
-10.3459381770593));
#297057=CARTESIAN_POINT('Ctrl Pts',(-9.83957192047916,131.412499999485,
-7.14886745759543));
#297058=CARTESIAN_POINT('Ctrl Pts',(-12.1623797632104,131.562499999484,
-3.95179673813153));
#297059=CARTESIAN_POINT('Ctrl Pts',(-12.1623797632104,131.712499999484,
2.97892388940601E-15));
#297060=CARTESIAN_POINT('Ctrl Pts',(-12.1623797632104,131.862499999483,
3.95179673813154));
#297061=CARTESIAN_POINT('Ctrl Pts',(-9.83957192047916,132.012499999482,
7.14886745759543));
#297062=CARTESIAN_POINT('Ctrl Pts',(-7.51676407774795,132.162499999482,
10.3459381770593));
#297063=CARTESIAN_POINT('Ctrl Pts',(-3.75838203887402,132.312499999481,
11.5671105274575));
#297064=CARTESIAN_POINT('Ctrl Pts',(-8.64140170974642E-14,132.462499999481,
12.7882828778556));
#297065=CARTESIAN_POINT('Ctrl Pts',(3.75838203887384,132.61249999948,11.5671105274575));
#297066=CARTESIAN_POINT('Ctrl Pts',(7.51676407774777,132.762499999479,10.3459381770593));
#297067=CARTESIAN_POINT('Ctrl Pts',(9.83957192047899,132.912499999479,7.14886745759543));
#297068=CARTESIAN_POINT('Ctrl Pts',(12.1623797632102,133.062499999478,3.95179673813153));
#297069=CARTESIAN_POINT('Ctrl Pts',(12.1623797632102,133.212499999478,-1.489461944703E-15));
#297070=CARTESIAN_POINT('Ctrl Pts',(12.1623797632102,133.362499999477,-3.95179673813154));
#297071=CARTESIAN_POINT('Ctrl Pts',(9.83957192047898,133.512499999476,-7.14886745759543));
#297072=CARTESIAN_POINT('Ctrl Pts',(7.51676407774777,133.662499999476,-10.3459381770593));
#297073=CARTESIAN_POINT('Ctrl Pts',(3.75838203887384,133.812499999475,-11.5671105274575));
#297074=CARTESIAN_POINT('Ctrl Pts',(-9.04100976718865E-14,133.962499999475,
-12.7882828778556));
#297075=CARTESIAN_POINT('Ctrl Pts',(-3.75838203887402,134.112499999474,
-11.5671105274575));
#297076=CARTESIAN_POINT('Ctrl Pts',(-7.51676407774795,134.262499999473,
-10.3459381770593));
#297077=CARTESIAN_POINT('Ctrl Pts',(-9.83957192047917,134.412499999473,
-7.14886745759543));
#297078=CARTESIAN_POINT('Ctrl Pts',(-12.1623797632104,134.562499999472,
-3.95179673813153));
#297079=CARTESIAN_POINT('Ctrl Pts',(-12.1623797632104,134.712499999472,
2.97892388940601E-15));
#297080=CARTESIAN_POINT('Ctrl Pts',(-12.1623797632104,134.862499999471,
3.95179673813154));
#297081=CARTESIAN_POINT('Ctrl Pts',(-9.83957192047916,135.01249999947,7.14886745759543));
#297082=CARTESIAN_POINT('Ctrl Pts',(-7.51676407774795,135.16249999947,10.3459381770593));
#297083=CARTESIAN_POINT('Ctrl Pts',(-3.75838203887402,135.312499999469,
11.5671105274575));
#297084=CARTESIAN_POINT('Ctrl Pts',(-8.8141726369126E-14,135.462499999469,
12.7882828778556));
#297085=CARTESIAN_POINT('Ctrl Pts',(3.75838203887384,135.612499999468,11.5671105274575));
#297086=CARTESIAN_POINT('Ctrl Pts',(7.51676407774777,135.762499999467,10.3459381770593));
#297087=CARTESIAN_POINT('Ctrl Pts',(9.83957192047898,135.912499999467,7.14886745759543));
#297088=CARTESIAN_POINT('Ctrl Pts',(12.1623797632102,136.062499999466,3.95179673813153));
#297089=CARTESIAN_POINT('Ctrl Pts',(12.1623797632102,136.212499999466,-1.489461944703E-15));
#297090=CARTESIAN_POINT('Ctrl Pts',(12.1623797632102,136.362499999465,-3.95179673813154));
#297091=CARTESIAN_POINT('Ctrl Pts',(9.83957192047898,136.512499999464,-7.14886745759543));
#297092=CARTESIAN_POINT('Ctrl Pts',(7.51676407774777,136.662499999464,-10.3459381770593));
#297093=CARTESIAN_POINT('Ctrl Pts',(3.75838203887384,136.812499999463,-11.5671105274575));
#297094=CARTESIAN_POINT('Ctrl Pts',(-9.21378069435483E-14,136.962499999463,
-12.7882828778556));
#297095=CARTESIAN_POINT('Ctrl Pts',(-3.75838203887402,137.112499999462,
-11.5671105274575));
#297096=CARTESIAN_POINT('Ctrl Pts',(-7.51676407774795,137.262499999461,
-10.3459381770593));
#297097=CARTESIAN_POINT('Ctrl Pts',(-9.83957192047917,137.412499999461,
-7.14886745759543));
#297098=CARTESIAN_POINT('Ctrl Pts',(-12.1623797632104,137.56249999946,-3.95179673813153));
#297099=CARTESIAN_POINT('Ctrl Pts',(-12.1623797632104,137.71249999946,2.97892388940601E-15));
#297100=CARTESIAN_POINT('Ctrl Pts',(-12.1623797632104,137.862499999459,
3.95179673813154));
#297101=CARTESIAN_POINT('Ctrl Pts',(-9.83957192047917,138.012499999458,
7.14886745759543));
#297102=CARTESIAN_POINT('Ctrl Pts',(-7.51676407774795,138.162499999458,
10.3459381770593));
#297103=CARTESIAN_POINT('Ctrl Pts',(-3.75838203887402,138.312499999457,
11.5671105274575));
#297104=CARTESIAN_POINT('Ctrl Pts',(-8.98694356407879E-14,138.462499999457,
12.7882828778556));
#297105=CARTESIAN_POINT('Ctrl Pts',(3.75838203887384,138.612499999456,11.5671105274575));
#297106=CARTESIAN_POINT('Ctrl Pts',(7.51676407774777,138.762499999455,10.3459381770593));
#297107=CARTESIAN_POINT('Ctrl Pts',(9.83957192047898,138.912499999455,7.14886745759543));
#297108=CARTESIAN_POINT('Ctrl Pts',(12.1623797632102,139.062499999454,3.95179673813153));
#297109=CARTESIAN_POINT('Ctrl Pts',(12.1623797632102,139.212499999454,-1.489461944703E-15));
#297110=CARTESIAN_POINT('Ctrl Pts',(12.1623797632102,139.362499999453,-3.95179673813154));
#297111=CARTESIAN_POINT('Ctrl Pts',(9.83957192047898,139.512499999452,-7.14886745759543));
#297112=CARTESIAN_POINT('Ctrl Pts',(7.51676407774776,139.662499999452,-10.3459381770593));
#297113=CARTESIAN_POINT('Ctrl Pts',(3.75838203887384,139.812499999451,-11.5671105274575));
#297114=CARTESIAN_POINT('Ctrl Pts',(-9.38655162152102E-14,139.962499999451,
-12.7882828778556));
#297115=CARTESIAN_POINT('Ctrl Pts',(-3.75838203887402,140.11249999945,-11.5671105274575));
#297116=CARTESIAN_POINT('Ctrl Pts',(-7.51676407774795,140.262499999449,
-10.3459381770593));
#297117=CARTESIAN_POINT('Ctrl Pts',(-9.83957192047917,140.412499999449,
-7.14886745759543));
#297118=CARTESIAN_POINT('Ctrl Pts',(-12.1623797632104,140.562499999448,
-3.95179673813153));
#297119=CARTESIAN_POINT('Ctrl Pts',(-12.1623797632104,140.712499999448,
2.97892388940601E-15));
#297120=CARTESIAN_POINT('Ctrl Pts',(-12.1623797632104,140.862499999447,
3.95179673813154));
#297121=CARTESIAN_POINT('Ctrl Pts',(-9.83957192047917,141.012499999446,
7.14886745759543));
#297122=CARTESIAN_POINT('Ctrl Pts',(-7.51676407774795,141.162499999446,
10.3459381770593));
#297123=CARTESIAN_POINT('Ctrl Pts',(-3.75838203887402,141.312499999445,
11.5671105274575));
#297124=CARTESIAN_POINT('Ctrl Pts',(-9.15971449124498E-14,141.462499999445,
12.7882828778556));
#297125=CARTESIAN_POINT('Ctrl Pts',(3.75838203887384,141.612499999444,11.5671105274575));
#297126=CARTESIAN_POINT('Ctrl Pts',(7.51676407774777,141.762499999443,10.3459381770593));
#297127=CARTESIAN_POINT('Ctrl Pts',(9.83957192047898,141.912499999443,7.14886745759543));
#297128=CARTESIAN_POINT('Ctrl Pts',(12.1623797632102,142.062499999442,3.95179673813153));
#297129=CARTESIAN_POINT('Ctrl Pts',(12.1623797632102,142.212499999442,-1.489461944703E-15));
#297130=CARTESIAN_POINT('Ctrl Pts',(12.1623797632102,142.362499999441,-3.95179673813154));
#297131=CARTESIAN_POINT('Ctrl Pts',(9.83957192047898,142.51249999944,-7.14886745759543));
#297132=CARTESIAN_POINT('Ctrl Pts',(7.51676407774776,142.66249999944,-10.3459381770593));
#297133=CARTESIAN_POINT('Ctrl Pts',(3.75838203887383,142.812499999439,-11.5671105274575));
#297134=CARTESIAN_POINT('Ctrl Pts',(-9.5593225486872E-14,142.962499999439,
-12.7882828778556));
#297135=CARTESIAN_POINT('Ctrl Pts',(-3.75838203887402,143.112499999438,
-11.5671105274575));
#297136=CARTESIAN_POINT('Ctrl Pts',(-7.51676407774795,143.262499999437,
-10.3459381770593));
#297137=CARTESIAN_POINT('Ctrl Pts',(-9.83957192047917,143.412499999437,
-7.14886745759543));
#297138=CARTESIAN_POINT('Ctrl Pts',(-12.1623797632104,143.562499999436,
-3.95179673813153));
#297139=CARTESIAN_POINT('Ctrl Pts',(-12.1623797632104,143.712499999436,
2.97892388940601E-15));
#297140=CARTESIAN_POINT('Ctrl Pts',(-12.1623797632104,143.862499999435,
3.95179673813154));
#297141=CARTESIAN_POINT('Ctrl Pts',(-9.83957192047917,144.012499999434,
7.14886745759543));
#297142=CARTESIAN_POINT('Ctrl Pts',(-7.51676407774795,144.162499999434,
10.3459381770593));
#297143=CARTESIAN_POINT('Ctrl Pts',(-3.75838203887402,144.312499999433,
11.5671105274575));
#297144=CARTESIAN_POINT('Ctrl Pts',(-9.33248541841116E-14,144.462499999433,
12.7882828778556));
#297145=CARTESIAN_POINT('Ctrl Pts',(3.75838203887384,144.612499999432,11.5671105274575));
#297146=CARTESIAN_POINT('Ctrl Pts',(7.51676407774776,144.762499999431,10.3459381770593));
#297147=CARTESIAN_POINT('Ctrl Pts',(9.83957192047898,144.912499999431,7.14886745759543));
#297148=CARTESIAN_POINT('Ctrl Pts',(12.1623797632102,145.06249999943,3.95179673813153));
#297149=CARTESIAN_POINT('Ctrl Pts',(12.1623797632102,145.21249999943,-1.489461944703E-15));
#297150=CARTESIAN_POINT('Ctrl Pts',(12.1623797632102,145.362499999429,-3.95179673813154));
#297151=CARTESIAN_POINT('Ctrl Pts',(9.83957192047898,145.512499999428,-7.14886745759543));
#297152=CARTESIAN_POINT('Ctrl Pts',(7.51676407774776,145.662499999428,-10.3459381770593));
#297153=CARTESIAN_POINT('Ctrl Pts',(3.75838203887383,145.812499999427,-11.5671105274575));
#297154=CARTESIAN_POINT('Ctrl Pts',(-9.73209347585338E-14,145.962499999427,
-12.7882828778556));
#297155=CARTESIAN_POINT('Ctrl Pts',(-3.75838203887403,146.112499999426,
-11.5671105274575));
#297156=CARTESIAN_POINT('Ctrl Pts',(-7.51676407774795,146.262499999425,
-10.3459381770593));
#297157=CARTESIAN_POINT('Ctrl Pts',(-9.83957192047917,146.412499999425,
-7.14886745759543));
#297158=CARTESIAN_POINT('Ctrl Pts',(-12.1623797632104,146.562499999424,
-3.95179673813153));
#297159=CARTESIAN_POINT('Ctrl Pts',(-12.1623797632104,146.712499999424,
2.97892388940601E-15));
#297160=CARTESIAN_POINT('Ctrl Pts',(-12.1623797632104,146.862499999423,
3.95179673813154));
#297161=CARTESIAN_POINT('Ctrl Pts',(-9.83957192047917,147.012499999422,
7.14886745759543));
#297162=CARTESIAN_POINT('Ctrl Pts',(-7.51676407774795,147.162499999422,
10.3459381770593));
#297163=CARTESIAN_POINT('Ctrl Pts',(-3.75838203887402,147.312499999421,
11.5671105274575));
#297164=CARTESIAN_POINT('Ctrl Pts',(-9.50525634557734E-14,147.462499999421,
12.7882828778556));
#297165=CARTESIAN_POINT('Ctrl Pts',(3.75838203887383,147.61249999942,11.5671105274575));
#297166=CARTESIAN_POINT('Ctrl Pts',(7.51676407774776,147.762499999419,10.3459381770593));
#297167=CARTESIAN_POINT('Ctrl Pts',(9.83957192047898,147.912499999419,7.14886745759543));
#297168=CARTESIAN_POINT('Ctrl Pts',(12.1623797632102,148.062499999418,3.95179673813153));
#297169=CARTESIAN_POINT('Ctrl Pts',(12.1623797632102,148.212499999418,-1.489461944703E-15));
#297170=CARTESIAN_POINT('Ctrl Pts',(12.1623797632102,148.362499999417,-3.95179673813154));
#297171=CARTESIAN_POINT('Ctrl Pts',(9.83957192047898,148.512499999416,-7.14886745759543));
#297172=CARTESIAN_POINT('Ctrl Pts',(7.51676407774776,148.662499999416,-10.3459381770593));
#297173=CARTESIAN_POINT('Ctrl Pts',(3.75838203887383,148.812499999415,-11.5671105274575));
#297174=CARTESIAN_POINT('Ctrl Pts',(-9.90486440301957E-14,148.962499999415,
-12.7882828778556));
#297175=CARTESIAN_POINT('Ctrl Pts',(-3.75838203887403,149.112499999414,
-11.5671105274575));
#297176=CARTESIAN_POINT('Ctrl Pts',(-7.51676407774795,149.262499999413,
-10.3459381770593));
#297177=CARTESIAN_POINT('Ctrl Pts',(-9.83957192047917,149.412499999413,
-7.14886745759543));
#297178=CARTESIAN_POINT('Ctrl Pts',(-12.1623797632104,149.562499999412,
-3.95179673813153));
#297179=CARTESIAN_POINT('Ctrl Pts',(-12.1623797632104,149.712499999412,
2.97892388940601E-15));
#297180=CARTESIAN_POINT('Ctrl Pts',(-12.1623797632104,149.862499999411,
3.95179673813154));
#297181=CARTESIAN_POINT('Ctrl Pts',(-9.83957192047917,150.01249999941,7.14886745759543));
#297182=CARTESIAN_POINT('Ctrl Pts',(-7.51676407774795,150.16249999941,10.3459381770593));
#297183=CARTESIAN_POINT('Ctrl Pts',(-3.75838203887403,150.312499999409,
11.5671105274575));
#297184=CARTESIAN_POINT('Ctrl Pts',(-9.67802727274353E-14,150.462499999409,
12.7882828778556));
#297185=CARTESIAN_POINT('Ctrl Pts',(3.75838203887383,150.612499999408,11.5671105274575));
#297186=CARTESIAN_POINT('Ctrl Pts',(7.51676407774776,150.762499999407,10.3459381770593));
#297187=CARTESIAN_POINT('Ctrl Pts',(9.83957192047898,150.912499999407,7.14886745759543));
#297188=CARTESIAN_POINT('Ctrl Pts',(12.1623797632102,151.062499999406,3.95179673813153));
#297189=CARTESIAN_POINT('Ctrl Pts',(12.1623797632102,151.212499999406,-1.489461944703E-15));
#297190=CARTESIAN_POINT('Ctrl Pts',(12.1623797632102,151.362499999405,-3.95179673813154));
#297191=CARTESIAN_POINT('Ctrl Pts',(9.83957192047897,151.512499999404,-7.14886745759543));
#297192=CARTESIAN_POINT('Ctrl Pts',(7.51676407774776,151.662499999404,-10.3459381770593));
#297193=CARTESIAN_POINT('Ctrl Pts',(3.75838203887383,151.812499999403,-11.5671105274575));
#297194=CARTESIAN_POINT('Ctrl Pts',(-1.00776353301858E-13,151.962499999403,
-12.7882828778556));
#297195=CARTESIAN_POINT('Ctrl Pts',(-3.75838203887403,152.112499999402,
-11.5671105274575));
#297196=CARTESIAN_POINT('Ctrl Pts',(-10.0514428414942,-2.06874999998125,
2.46189346052968E-15));
#297197=CARTESIAN_POINT('Ctrl Pts',(-10.0514428414942,-1.91874999998185,
3.26591175476071));
#297198=CARTESIAN_POINT('Ctrl Pts',(-8.1317880767572,-1.76874999998245,
5.90808986649102));
#297199=CARTESIAN_POINT('Ctrl Pts',(-6.21213331202023,-1.61874999998305,
8.55026797822134));
#297200=CARTESIAN_POINT('Ctrl Pts',(-3.10606665601012,-1.46874999998365,
9.5594902125713));
#297201=CARTESIAN_POINT('Ctrl Pts',(-9.77671023785295E-15,-1.31874999998425,
10.5687124469213));
#297202=CARTESIAN_POINT('Ctrl Pts',(3.1060666560101,-1.16874999998485,9.5594902125713));
#297203=CARTESIAN_POINT('Ctrl Pts',(6.21213331202021,-1.01874999998544,
8.55026797822134));
#297204=CARTESIAN_POINT('Ctrl Pts',(8.13178807675718,-0.868749999986043,
5.90808986649102));
#297205=CARTESIAN_POINT('Ctrl Pts',(10.0514428414942,-0.718749999986641,
3.2659117547607));
#297206=CARTESIAN_POINT('Ctrl Pts',(10.0514428414942,-0.568749999987242,
-1.23094673026484E-15));
#297207=CARTESIAN_POINT('Ctrl Pts',(10.0514428414942,-0.418749999987842,
-3.26591175476071));
#297208=CARTESIAN_POINT('Ctrl Pts',(8.13178807675718,-0.268749999988443,
-5.90808986649102));
#297209=CARTESIAN_POINT('Ctrl Pts',(6.2121333120202,-0.118749999989044,
-8.55026797822134));
#297210=CARTESIAN_POINT('Ctrl Pts',(3.10606665601009,0.0312500000103543,
-9.5594902125713));
#297211=CARTESIAN_POINT('Ctrl Pts',(-1.322915284753E-14,0.181250000009752,
-10.5687124469213));
#297212=CARTESIAN_POINT('Ctrl Pts',(-3.10606665601012,0.331250000009151,
-9.5594902125713));
#297213=CARTESIAN_POINT('Ctrl Pts',(-6.21213331202023,0.481250000008549,
-8.55026797822134));
#297214=CARTESIAN_POINT('Ctrl Pts',(-8.1317880767572,0.631250000007948,
-5.90808986649102));
#297215=CARTESIAN_POINT('Ctrl Pts',(-10.0514428414942,0.781250000007346,
-3.2659117547607));
#297216=CARTESIAN_POINT('Ctrl Pts',(-10.0514428414942,0.931250000006746,
2.46189346052968E-15));
#297217=CARTESIAN_POINT('Ctrl Pts',(-10.0514428414942,1.08125000000615,
3.26591175476071));
#297218=CARTESIAN_POINT('Ctrl Pts',(-8.1317880767572,1.23125000000555,5.90808986649102));
#297219=CARTESIAN_POINT('Ctrl Pts',(-6.21213331202023,1.38125000000495,
8.55026797822134));
#297220=CARTESIAN_POINT('Ctrl Pts',(-3.10606665601012,1.53125000000435,
9.5594902125713));
#297221=CARTESIAN_POINT('Ctrl Pts',(-1.15044195095148E-14,1.68125000000375,
10.5687124469213));
#297222=CARTESIAN_POINT('Ctrl Pts',(3.1060666560101,1.83125000000315,9.5594902125713));
#297223=CARTESIAN_POINT('Ctrl Pts',(6.2121333120202,1.98125000000256,8.55026797822134));
#297224=CARTESIAN_POINT('Ctrl Pts',(8.13178807675718,2.13125000000196,5.90808986649102));
#297225=CARTESIAN_POINT('Ctrl Pts',(10.0514428414942,2.28125000000136,3.2659117547607));
#297226=CARTESIAN_POINT('Ctrl Pts',(10.0514428414942,2.43125000000076,-1.23094673026484E-15));
#297227=CARTESIAN_POINT('Ctrl Pts',(10.0514428414942,2.58125000000016,-3.26591175476071));
#297228=CARTESIAN_POINT('Ctrl Pts',(8.13178807675718,2.73124999999956,-5.90808986649102));
#297229=CARTESIAN_POINT('Ctrl Pts',(6.2121333120202,2.88124999999896,-8.55026797822134));
#297230=CARTESIAN_POINT('Ctrl Pts',(3.10606665601009,3.03124999999835,-9.5594902125713));
#297231=CARTESIAN_POINT('Ctrl Pts',(-1.49568621191919E-14,3.18124999999775,
-10.5687124469213));
#297232=CARTESIAN_POINT('Ctrl Pts',(-3.10606665601012,3.33124999999715,
-9.5594902125713));
#297233=CARTESIAN_POINT('Ctrl Pts',(-6.21213331202023,3.48124999999655,
-8.55026797822134));
#297234=CARTESIAN_POINT('Ctrl Pts',(-8.13178807675721,3.63124999999595,
-5.90808986649102));
#297235=CARTESIAN_POINT('Ctrl Pts',(-10.0514428414942,3.78124999999535,
-3.2659117547607));
#297236=CARTESIAN_POINT('Ctrl Pts',(-10.0514428414942,3.93124999999475,
2.46189346052968E-15));
#297237=CARTESIAN_POINT('Ctrl Pts',(-10.0514428414942,4.08124999999415,
3.26591175476071));
#297238=CARTESIAN_POINT('Ctrl Pts',(-8.13178807675721,4.23124999999355,
5.90808986649102));
#297239=CARTESIAN_POINT('Ctrl Pts',(-6.21213331202023,4.38124999999295,
8.55026797822134));
#297240=CARTESIAN_POINT('Ctrl Pts',(-3.10606665601012,4.53124999999235,
9.5594902125713));
#297241=CARTESIAN_POINT('Ctrl Pts',(-1.32321287811766E-14,4.68124999999175,
10.5687124469213));
#297242=CARTESIAN_POINT('Ctrl Pts',(3.10606665601009,4.83124999999115,9.5594902125713));
#297243=CARTESIAN_POINT('Ctrl Pts',(6.2121333120202,4.98124999999055,8.55026797822134));
#297244=CARTESIAN_POINT('Ctrl Pts',(8.13178807675718,5.13124999998996,5.90808986649102));
#297245=CARTESIAN_POINT('Ctrl Pts',(10.0514428414942,5.28124999998936,3.2659117547607));
#297246=CARTESIAN_POINT('Ctrl Pts',(10.0514428414941,5.43124999998876,-1.23094673026484E-15));
#297247=CARTESIAN_POINT('Ctrl Pts',(10.0514428414941,5.58124999998816,-3.26591175476071));
#297248=CARTESIAN_POINT('Ctrl Pts',(8.13178807675717,5.73124999998756,-5.90808986649102));
#297249=CARTESIAN_POINT('Ctrl Pts',(6.2121333120202,5.88124999998695,-8.55026797822134));
#297250=CARTESIAN_POINT('Ctrl Pts',(3.10606665601009,6.03124999998635,-9.5594902125713));
#297251=CARTESIAN_POINT('Ctrl Pts',(-1.66845713908537E-14,6.18124999998575,
-10.5687124469213));
#297252=CARTESIAN_POINT('Ctrl Pts',(-3.10606665601012,6.33124999998515,
-9.5594902125713));
#297253=CARTESIAN_POINT('Ctrl Pts',(-6.21213331202023,6.48124999998455,
-8.55026797822134));
#297254=CARTESIAN_POINT('Ctrl Pts',(-8.13178807675721,6.63124999998395,
-5.90808986649102));
#297255=CARTESIAN_POINT('Ctrl Pts',(-10.0514428414942,6.78124999998335,
-3.2659117547607));
#297256=CARTESIAN_POINT('Ctrl Pts',(-10.0514428414942,6.93124999998275,
2.46189346052968E-15));
#297257=CARTESIAN_POINT('Ctrl Pts',(-10.0514428414942,7.08124999998215,
3.26591175476071));
#297258=CARTESIAN_POINT('Ctrl Pts',(-8.13178807675721,7.23124999998155,
5.90808986649102));
#297259=CARTESIAN_POINT('Ctrl Pts',(-6.21213331202023,7.38124999998095,
8.55026797822134));
#297260=CARTESIAN_POINT('Ctrl Pts',(-3.10606665601012,7.53124999998035,
9.5594902125713));
#297261=CARTESIAN_POINT('Ctrl Pts',(-1.49598380528385E-14,7.68124999997975,
10.5687124469213));
#297262=CARTESIAN_POINT('Ctrl Pts',(3.10606665601009,7.83124999997915,9.5594902125713));
#297263=CARTESIAN_POINT('Ctrl Pts',(6.2121333120202,7.98124999997856,8.55026797822134));
#297264=CARTESIAN_POINT('Ctrl Pts',(8.13178807675717,8.13124999997796,5.90808986649102));
#297265=CARTESIAN_POINT('Ctrl Pts',(10.0514428414942,8.28124999997736,3.2659117547607));
#297266=CARTESIAN_POINT('Ctrl Pts',(10.0514428414941,8.43124999997676,-1.23094673026484E-15));
#297267=CARTESIAN_POINT('Ctrl Pts',(10.0514428414941,8.58124999997616,-3.26591175476071));
#297268=CARTESIAN_POINT('Ctrl Pts',(8.13178807675717,8.73124999997556,-5.90808986649102));
#297269=CARTESIAN_POINT('Ctrl Pts',(6.2121333120202,8.88124999997496,-8.55026797822134));
#297270=CARTESIAN_POINT('Ctrl Pts',(3.10606665601009,9.03124999997436,-9.5594902125713));
#297271=CARTESIAN_POINT('Ctrl Pts',(-1.84122806625156E-14,9.18124999997375,
-10.5687124469213));
#297272=CARTESIAN_POINT('Ctrl Pts',(-3.10606665601013,9.33124999997315,
-9.5594902125713));
#297273=CARTESIAN_POINT('Ctrl Pts',(-6.21213331202023,9.48124999997255,
-8.55026797822134));
#297274=CARTESIAN_POINT('Ctrl Pts',(-8.13178807675721,9.63124999997195,
-5.90808986649102));
#297275=CARTESIAN_POINT('Ctrl Pts',(-10.0514428414942,9.78124999997135,
-3.2659117547607));
#297276=CARTESIAN_POINT('Ctrl Pts',(-10.0514428414942,9.93124999997075,
2.46189346052968E-15));
#297277=CARTESIAN_POINT('Ctrl Pts',(-10.0514428414942,10.0812499999701,
3.26591175476071));
#297278=CARTESIAN_POINT('Ctrl Pts',(-8.13178807675721,10.2312499999695,
5.90808986649102));
#297279=CARTESIAN_POINT('Ctrl Pts',(-6.21213331202023,10.3812499999689,
8.55026797822134));
#297280=CARTESIAN_POINT('Ctrl Pts',(-3.10606665601012,10.5312499999684,
9.5594902125713));
#297281=CARTESIAN_POINT('Ctrl Pts',(-1.66875473245003E-14,10.6812499999678,
10.5687124469213));
#297282=CARTESIAN_POINT('Ctrl Pts',(3.10606665601009,10.8312499999672,9.5594902125713));
#297283=CARTESIAN_POINT('Ctrl Pts',(6.2121333120202,10.9812499999666,8.55026797822134));
#297284=CARTESIAN_POINT('Ctrl Pts',(8.13178807675717,11.131249999966,5.90808986649102));
#297285=CARTESIAN_POINT('Ctrl Pts',(10.0514428414941,11.2812499999654,3.2659117547607));
#297286=CARTESIAN_POINT('Ctrl Pts',(10.0514428414941,11.4312499999648,-1.23094673026484E-15));
#297287=CARTESIAN_POINT('Ctrl Pts',(10.0514428414941,11.5812499999642,-3.26591175476071));
#297288=CARTESIAN_POINT('Ctrl Pts',(8.13178807675717,11.7312499999636,-5.90808986649102));
#297289=CARTESIAN_POINT('Ctrl Pts',(6.2121333120202,11.881249999963,-8.55026797822134));
#297290=CARTESIAN_POINT('Ctrl Pts',(3.10606665601009,12.0312499999624,-9.5594902125713));
#297291=CARTESIAN_POINT('Ctrl Pts',(-2.01399899341774E-14,12.1812499999618,
-10.5687124469213));
#297292=CARTESIAN_POINT('Ctrl Pts',(-3.10606665601013,12.3312499999612,
-9.5594902125713));
#297293=CARTESIAN_POINT('Ctrl Pts',(-6.21213331202024,12.4812499999605,
-8.55026797822134));
#297294=CARTESIAN_POINT('Ctrl Pts',(-8.13178807675721,12.6312499999599,
-5.90808986649102));
#297295=CARTESIAN_POINT('Ctrl Pts',(-10.0514428414942,12.7812499999593,
-3.2659117547607));
#297296=CARTESIAN_POINT('Ctrl Pts',(-10.0514428414942,12.9312499999587,
2.46189346052968E-15));
#297297=CARTESIAN_POINT('Ctrl Pts',(-10.0514428414942,13.0812499999581,
3.26591175476071));
#297298=CARTESIAN_POINT('Ctrl Pts',(-8.13178807675721,13.2312499999575,
5.90808986649102));
#297299=CARTESIAN_POINT('Ctrl Pts',(-6.21213331202023,13.3812499999569,
8.55026797822134));
#297300=CARTESIAN_POINT('Ctrl Pts',(-3.10606665601013,13.5312499999564,
9.5594902125713));
#297301=CARTESIAN_POINT('Ctrl Pts',(-1.84152565961621E-14,13.6812499999558,
10.5687124469213));
#297302=CARTESIAN_POINT('Ctrl Pts',(3.10606665601009,13.8312499999552,9.5594902125713));
#297303=CARTESIAN_POINT('Ctrl Pts',(6.2121333120202,13.9812499999546,8.55026797822134));
#297304=CARTESIAN_POINT('Ctrl Pts',(8.13178807675717,14.131249999954,5.90808986649102));
#297305=CARTESIAN_POINT('Ctrl Pts',(10.0514428414941,14.2812499999534,3.2659117547607));
#297306=CARTESIAN_POINT('Ctrl Pts',(10.0514428414941,14.4312499999528,-1.23094673026484E-15));
#297307=CARTESIAN_POINT('Ctrl Pts',(10.0514428414941,14.5812499999522,-3.26591175476071));
#297308=CARTESIAN_POINT('Ctrl Pts',(8.13178807675717,14.7312499999516,-5.90808986649102));
#297309=CARTESIAN_POINT('Ctrl Pts',(6.21213331202019,14.881249999951,-8.55026797822134));
#297310=CARTESIAN_POINT('Ctrl Pts',(3.10606665601009,15.0312499999504,-9.5594902125713));
#297311=CARTESIAN_POINT('Ctrl Pts',(-2.18676992058392E-14,15.1812499999498,
-10.5687124469213));
#297312=CARTESIAN_POINT('Ctrl Pts',(-3.10606665601013,15.3312499999492,
-9.5594902125713));
#297313=CARTESIAN_POINT('Ctrl Pts',(-6.21213331202024,15.4812499999485,
-8.55026797822134));
#297314=CARTESIAN_POINT('Ctrl Pts',(-8.13178807675721,15.6312499999479,
-5.90808986649102));
#297315=CARTESIAN_POINT('Ctrl Pts',(-10.0514428414942,15.7812499999473,
-3.2659117547607));
#297316=CARTESIAN_POINT('Ctrl Pts',(-10.0514428414942,15.9312499999467,
2.46189346052968E-15));
#297317=CARTESIAN_POINT('Ctrl Pts',(-10.0514428414942,16.0812499999461,
3.26591175476071));
#297318=CARTESIAN_POINT('Ctrl Pts',(-8.13178807675721,16.2312499999455,
5.90808986649102));
#297319=CARTESIAN_POINT('Ctrl Pts',(-6.21213331202024,16.3812499999449,
8.55026797822134));
#297320=CARTESIAN_POINT('Ctrl Pts',(-3.10606665601013,16.5312499999444,
9.5594902125713));
#297321=CARTESIAN_POINT('Ctrl Pts',(-2.0142965867824E-14,16.6812499999438,
10.5687124469213));
#297322=CARTESIAN_POINT('Ctrl Pts',(3.10606665601009,16.8312499999432,9.5594902125713));
#297323=CARTESIAN_POINT('Ctrl Pts',(6.21213331202019,16.9812499999426,8.55026797822134));
#297324=CARTESIAN_POINT('Ctrl Pts',(8.13178807675717,17.131249999942,5.90808986649102));
#297325=CARTESIAN_POINT('Ctrl Pts',(10.0514428414941,17.2812499999414,3.2659117547607));
#297326=CARTESIAN_POINT('Ctrl Pts',(10.0514428414941,17.4312499999408,-1.23094673026484E-15));
#297327=CARTESIAN_POINT('Ctrl Pts',(10.0514428414941,17.5812499999402,-3.26591175476071));
#297328=CARTESIAN_POINT('Ctrl Pts',(8.13178807675717,17.7312499999396,-5.90808986649102));
#297329=CARTESIAN_POINT('Ctrl Pts',(6.21213331202019,17.881249999939,-8.55026797822134));
#297330=CARTESIAN_POINT('Ctrl Pts',(3.10606665601008,18.0312499999384,-9.5594902125713));
#297331=CARTESIAN_POINT('Ctrl Pts',(-2.35954084775011E-14,18.1812499999378,
-10.5687124469213));
#297332=CARTESIAN_POINT('Ctrl Pts',(-3.10606665601013,18.3312499999371,
-9.5594902125713));
#297333=CARTESIAN_POINT('Ctrl Pts',(-6.21213331202024,18.4812499999365,
-8.55026797822134));
#297334=CARTESIAN_POINT('Ctrl Pts',(-8.13178807675721,18.6312499999359,
-5.90808986649102));
#297335=CARTESIAN_POINT('Ctrl Pts',(-10.0514428414942,18.7812499999353,
-3.2659117547607));
#297336=CARTESIAN_POINT('Ctrl Pts',(-10.0514428414942,18.9312499999347,
2.46189346052968E-15));
#297337=CARTESIAN_POINT('Ctrl Pts',(-10.0514428414942,19.0812499999341,
3.26591175476071));
#297338=CARTESIAN_POINT('Ctrl Pts',(-8.13178807675721,19.2312499999335,
5.90808986649102));
#297339=CARTESIAN_POINT('Ctrl Pts',(-6.21213331202024,19.381249999933,8.55026797822134));
#297340=CARTESIAN_POINT('Ctrl Pts',(-3.10606665601013,19.5312499999323,
9.5594902125713));
#297341=CARTESIAN_POINT('Ctrl Pts',(-2.18706751394858E-14,19.6812499999318,
10.5687124469213));
#297342=CARTESIAN_POINT('Ctrl Pts',(3.10606665601009,19.8312499999312,9.5594902125713));
#297343=CARTESIAN_POINT('Ctrl Pts',(6.21213331202019,19.9812499999306,8.55026797822134));
#297344=CARTESIAN_POINT('Ctrl Pts',(8.13178807675717,20.13124999993,5.90808986649102));
#297345=CARTESIAN_POINT('Ctrl Pts',(10.0514428414941,20.2812499999294,3.2659117547607));
#297346=CARTESIAN_POINT('Ctrl Pts',(10.0514428414941,20.4312499999288,-1.23094673026484E-15));
#297347=CARTESIAN_POINT('Ctrl Pts',(10.0514428414941,20.5812499999282,-3.26591175476071));
#297348=CARTESIAN_POINT('Ctrl Pts',(8.13178807675716,20.7312499999276,-5.90808986649102));
#297349=CARTESIAN_POINT('Ctrl Pts',(6.21213331202019,20.881249999927,-8.55026797822134));
#297350=CARTESIAN_POINT('Ctrl Pts',(3.10606665601008,21.0312499999264,-9.5594902125713));
#297351=CARTESIAN_POINT('Ctrl Pts',(-2.53231177491629E-14,21.1812499999258,
-10.5687124469213));
#297352=CARTESIAN_POINT('Ctrl Pts',(-3.10606665601013,21.3312499999251,
-9.5594902125713));
#297353=CARTESIAN_POINT('Ctrl Pts',(-6.21213331202024,21.4812499999245,
-8.55026797822134));
#297354=CARTESIAN_POINT('Ctrl Pts',(-8.13178807675722,21.6312499999239,
-5.90808986649102));
#297355=CARTESIAN_POINT('Ctrl Pts',(-10.0514428414942,21.7812499999233,
-3.2659117547607));
#297356=CARTESIAN_POINT('Ctrl Pts',(-10.0514428414942,21.9312499999227,
2.46189346052968E-15));
#297357=CARTESIAN_POINT('Ctrl Pts',(-10.0514428414942,22.0812499999221,
3.26591175476071));
#297358=CARTESIAN_POINT('Ctrl Pts',(-8.13178807675722,22.2312499999215,
5.90808986649102));
#297359=CARTESIAN_POINT('Ctrl Pts',(-6.21213331202024,22.3812499999209,
8.55026797822134));
#297360=CARTESIAN_POINT('Ctrl Pts',(-3.10606665601013,22.5312499999204,
9.5594902125713));
#297361=CARTESIAN_POINT('Ctrl Pts',(-2.35983844111477E-14,22.6812499999198,
10.5687124469213));
#297362=CARTESIAN_POINT('Ctrl Pts',(3.10606665601008,22.8312499999192,9.5594902125713));
#297363=CARTESIAN_POINT('Ctrl Pts',(6.21213331202019,22.9812499999186,8.55026797822134));
#297364=CARTESIAN_POINT('Ctrl Pts',(8.13178807675716,23.131249999918,5.90808986649102));
#297365=CARTESIAN_POINT('Ctrl Pts',(10.0514428414941,23.2812499999174,3.2659117547607));
#297366=CARTESIAN_POINT('Ctrl Pts',(10.0514428414941,23.4312499999168,-1.23094673026484E-15));
#297367=CARTESIAN_POINT('Ctrl Pts',(10.0514428414941,23.5812499999162,-3.26591175476071));
#297368=CARTESIAN_POINT('Ctrl Pts',(8.13178807675716,23.7312499999156,-5.90808986649102));
#297369=CARTESIAN_POINT('Ctrl Pts',(6.21213331202019,23.881249999915,-8.55026797822134));
#297370=CARTESIAN_POINT('Ctrl Pts',(3.10606665601008,24.0312499999144,-9.5594902125713));
#297371=CARTESIAN_POINT('Ctrl Pts',(-2.70508270208248E-14,24.1812499999138,
-10.5687124469213));
#297372=CARTESIAN_POINT('Ctrl Pts',(-3.10606665601014,24.3312499999131,
-9.5594902125713));
#297373=CARTESIAN_POINT('Ctrl Pts',(-6.21213331202024,24.4812499999125,
-8.55026797822134));
#297374=CARTESIAN_POINT('Ctrl Pts',(-8.13178807675722,24.6312499999119,
-5.90808986649102));
#297375=CARTESIAN_POINT('Ctrl Pts',(-10.0514428414942,24.7812499999113,
-3.2659117547607));
#297376=CARTESIAN_POINT('Ctrl Pts',(-10.0514428414942,24.9312499999107,
2.46189346052968E-15));
#297377=CARTESIAN_POINT('Ctrl Pts',(-10.0514428414942,25.0812499999101,
3.26591175476071));
#297378=CARTESIAN_POINT('Ctrl Pts',(-8.13178807675722,25.2312499999095,
5.90808986649102));
#297379=CARTESIAN_POINT('Ctrl Pts',(-6.21213331202024,25.381249999909,8.55026797822134));
#297380=CARTESIAN_POINT('Ctrl Pts',(-3.10606665601013,25.5312499999084,
9.5594902125713));
#297381=CARTESIAN_POINT('Ctrl Pts',(-2.53260936828095E-14,25.6812499999078,
10.5687124469213));
#297382=CARTESIAN_POINT('Ctrl Pts',(3.10606665601008,25.8312499999072,9.5594902125713));
#297383=CARTESIAN_POINT('Ctrl Pts',(6.21213331202019,25.9812499999066,8.55026797822134));
#297384=CARTESIAN_POINT('Ctrl Pts',(8.13178807675716,26.131249999906,5.90808986649102));
#297385=CARTESIAN_POINT('Ctrl Pts',(10.0514428414941,26.2812499999054,3.2659117547607));
#297386=CARTESIAN_POINT('Ctrl Pts',(10.0514428414941,26.4312499999048,-1.23094673026484E-15));
#297387=CARTESIAN_POINT('Ctrl Pts',(10.0514428414941,26.5812499999042,-3.26591175476071));
#297388=CARTESIAN_POINT('Ctrl Pts',(8.13178807675716,26.7312499999036,-5.90808986649102));
#297389=CARTESIAN_POINT('Ctrl Pts',(6.21213331202019,26.881249999903,-8.55026797822134));
#297390=CARTESIAN_POINT('Ctrl Pts',(3.10606665601008,27.0312499999024,-9.5594902125713));
#297391=CARTESIAN_POINT('Ctrl Pts',(-2.87785362924866E-14,27.1812499999018,
-10.5687124469213));
#297392=CARTESIAN_POINT('Ctrl Pts',(-3.10606665601014,27.3312499999011,
-9.5594902125713));
#297393=CARTESIAN_POINT('Ctrl Pts',(-6.21213331202024,27.4812499999005,
-8.55026797822134));
#297394=CARTESIAN_POINT('Ctrl Pts',(-8.13178807675722,27.6312499998999,
-5.90808986649102));
#297395=CARTESIAN_POINT('Ctrl Pts',(-10.0514428414942,27.7812499998993,
-3.2659117547607));
#297396=CARTESIAN_POINT('Ctrl Pts',(-10.0514428414942,27.9312499998987,
2.46189346052968E-15));
#297397=CARTESIAN_POINT('Ctrl Pts',(-10.0514428414942,28.0812499998981,
3.26591175476071));
#297398=CARTESIAN_POINT('Ctrl Pts',(-8.13178807675722,28.2312499998975,
5.90808986649102));
#297399=CARTESIAN_POINT('Ctrl Pts',(-6.21213331202024,28.3812499998969,
8.55026797822134));
#297400=CARTESIAN_POINT('Ctrl Pts',(-3.10606665601014,28.5312499998964,
9.5594902125713));
#297401=CARTESIAN_POINT('Ctrl Pts',(-2.70538029544713E-14,28.6812499998958,
10.5687124469213));
#297402=CARTESIAN_POINT('Ctrl Pts',(3.10606665601008,28.8312499998952,9.5594902125713));
#297403=CARTESIAN_POINT('Ctrl Pts',(6.21213331202019,28.9812499998946,8.55026797822134));
#297404=CARTESIAN_POINT('Ctrl Pts',(8.13178807675716,29.131249999894,5.90808986649102));
#297405=CARTESIAN_POINT('Ctrl Pts',(10.0514428414941,29.2812499998934,3.2659117547607));
#297406=CARTESIAN_POINT('Ctrl Pts',(10.0514428414941,29.4312499998928,-1.23094673026484E-15));
#297407=CARTESIAN_POINT('Ctrl Pts',(10.0514428414941,29.5812499998922,-3.26591175476071));
#297408=CARTESIAN_POINT('Ctrl Pts',(8.13178807675716,29.7312499998916,-5.90808986649102));
#297409=CARTESIAN_POINT('Ctrl Pts',(6.21213331202019,29.881249999891,-8.55026797822134));
#297410=CARTESIAN_POINT('Ctrl Pts',(3.10606665601008,30.0312499998904,-9.5594902125713));
#297411=CARTESIAN_POINT('Ctrl Pts',(-3.05062455641484E-14,30.1812499998898,
-10.5687124469213));
#297412=CARTESIAN_POINT('Ctrl Pts',(-3.10606665601014,30.3312499998892,
-9.5594902125713));
#297413=CARTESIAN_POINT('Ctrl Pts',(-6.21213331202025,30.4812499998885,
-8.55026797822134));
#297414=CARTESIAN_POINT('Ctrl Pts',(-8.13178807675722,30.6312499998879,
-5.90808986649102));
#297415=CARTESIAN_POINT('Ctrl Pts',(-10.0514428414942,30.7812499998873,
-3.2659117547607));
#297416=CARTESIAN_POINT('Ctrl Pts',(-10.0514428414942,30.9312499998867,
2.46189346052968E-15));
#297417=CARTESIAN_POINT('Ctrl Pts',(-10.0514428414942,31.0812499998861,
3.26591175476071));
#297418=CARTESIAN_POINT('Ctrl Pts',(-8.13178807675722,31.2312499998855,
5.90808986649102));
#297419=CARTESIAN_POINT('Ctrl Pts',(-6.21213331202024,31.381249999885,8.55026797822134));
#297420=CARTESIAN_POINT('Ctrl Pts',(-3.10606665601014,31.5312499998843,
9.5594902125713));
#297421=CARTESIAN_POINT('Ctrl Pts',(-2.87815122261332E-14,31.6812499998838,
10.5687124469213));
#297422=CARTESIAN_POINT('Ctrl Pts',(3.10606665601008,31.8312499998832,9.5594902125713));
#297423=CARTESIAN_POINT('Ctrl Pts',(6.21213331202019,31.9812499998826,8.55026797822134));
#297424=CARTESIAN_POINT('Ctrl Pts',(8.13178807675716,32.131249999882,5.90808986649102));
#297425=CARTESIAN_POINT('Ctrl Pts',(10.0514428414941,32.2812499998814,3.2659117547607));
#297426=CARTESIAN_POINT('Ctrl Pts',(10.0514428414941,32.4312499998808,-1.23094673026484E-15));
#297427=CARTESIAN_POINT('Ctrl Pts',(10.0514428414941,32.5812499998802,-3.26591175476071));
#297428=CARTESIAN_POINT('Ctrl Pts',(8.13178807675716,32.7312499998796,-5.90808986649102));
#297429=CARTESIAN_POINT('Ctrl Pts',(6.21213331202019,32.8812499998789,-8.55026797822134));
#297430=CARTESIAN_POINT('Ctrl Pts',(3.10606665601008,33.0312499998784,-9.5594902125713));
#297431=CARTESIAN_POINT('Ctrl Pts',(-3.22339548358103E-14,33.1812499998777,
-10.5687124469213));
#297432=CARTESIAN_POINT('Ctrl Pts',(-3.10606665601014,33.3312499998772,
-9.5594902125713));
#297433=CARTESIAN_POINT('Ctrl Pts',(-6.21213331202025,33.4812499998766,
-8.55026797822134));
#297434=CARTESIAN_POINT('Ctrl Pts',(-8.13178807675722,33.6312499998759,
-5.90808986649102));
#297435=CARTESIAN_POINT('Ctrl Pts',(-10.0514428414942,33.7812499998753,
-3.2659117547607));
#297436=CARTESIAN_POINT('Ctrl Pts',(-10.0514428414942,33.9312499998747,
2.46189346052968E-15));
#297437=CARTESIAN_POINT('Ctrl Pts',(-10.0514428414942,34.0812499998741,
3.26591175476071));
#297438=CARTESIAN_POINT('Ctrl Pts',(-8.13178807675722,34.2312499998735,
5.90808986649102));
#297439=CARTESIAN_POINT('Ctrl Pts',(-6.21213331202024,34.3812499998729,
8.55026797822134));
#297440=CARTESIAN_POINT('Ctrl Pts',(-3.10606665601014,34.5312499998724,
9.5594902125713));
#297441=CARTESIAN_POINT('Ctrl Pts',(-3.0509221497795E-14,34.6812499998718,
10.5687124469213));
#297442=CARTESIAN_POINT('Ctrl Pts',(3.10606665601008,34.8312499998712,9.5594902125713));
#297443=CARTESIAN_POINT('Ctrl Pts',(6.21213331202019,34.9812499998706,8.55026797822134));
#297444=CARTESIAN_POINT('Ctrl Pts',(8.13178807675716,35.13124999987,5.90808986649102));
#297445=CARTESIAN_POINT('Ctrl Pts',(10.0514428414941,35.2812499998694,3.2659117547607));
#297446=CARTESIAN_POINT('Ctrl Pts',(10.0514428414941,35.4312499998688,-1.23094673026484E-15));
#297447=CARTESIAN_POINT('Ctrl Pts',(10.0514428414941,35.5812499998682,-3.26591175476071));
#297448=CARTESIAN_POINT('Ctrl Pts',(8.13178807675716,35.7312499998676,-5.90808986649102));
#297449=CARTESIAN_POINT('Ctrl Pts',(6.21213331202018,35.881249999867,-8.55026797822134));
#297450=CARTESIAN_POINT('Ctrl Pts',(3.10606665601007,36.0312499998664,-9.5594902125713));
#297451=CARTESIAN_POINT('Ctrl Pts',(-3.39616641074721E-14,36.1812499998658,
-10.5687124469213));
#297452=CARTESIAN_POINT('Ctrl Pts',(-3.10606665601014,36.3312499998652,
-9.5594902125713));
#297453=CARTESIAN_POINT('Ctrl Pts',(-6.21213331202025,36.4812499998646,
-8.55026797822134));
#297454=CARTESIAN_POINT('Ctrl Pts',(-8.13178807675722,36.6312499998639,
-5.90808986649102));
#297455=CARTESIAN_POINT('Ctrl Pts',(-10.0514428414942,36.7812499998634,
-3.2659117547607));
#297456=CARTESIAN_POINT('Ctrl Pts',(-10.0514428414942,36.9312499998627,
2.46189346052968E-15));
#297457=CARTESIAN_POINT('Ctrl Pts',(-10.0514428414942,37.0812499998621,
3.26591175476071));
#297458=CARTESIAN_POINT('Ctrl Pts',(-8.13178807675722,37.2312499998615,
5.90808986649102));
#297459=CARTESIAN_POINT('Ctrl Pts',(-6.21213331202025,37.3812499998609,
8.55026797822134));
#297460=CARTESIAN_POINT('Ctrl Pts',(-3.10606665601014,37.5312499998603,
9.5594902125713));
#297461=CARTESIAN_POINT('Ctrl Pts',(-3.22369307694568E-14,37.6812499998598,
10.5687124469213));
#297462=CARTESIAN_POINT('Ctrl Pts',(3.10606665601008,37.8312499998592,9.5594902125713));
#297463=CARTESIAN_POINT('Ctrl Pts',(6.21213331202018,37.9812499998586,8.55026797822134));
#297464=CARTESIAN_POINT('Ctrl Pts',(8.13178807675716,38.131249999858,5.90808986649102));
#297465=CARTESIAN_POINT('Ctrl Pts',(10.0514428414941,38.2812499998574,3.2659117547607));
#297466=CARTESIAN_POINT('Ctrl Pts',(10.0514428414941,38.4312499998568,-1.23094673026484E-15));
#297467=CARTESIAN_POINT('Ctrl Pts',(10.0514428414941,38.5812499998562,-3.26591175476071));
#297468=CARTESIAN_POINT('Ctrl Pts',(8.13178807675715,38.7312499998556,-5.90808986649102));
#297469=CARTESIAN_POINT('Ctrl Pts',(6.21213331202018,38.881249999855,-8.55026797822134));
#297470=CARTESIAN_POINT('Ctrl Pts',(3.10606665601007,39.0312499998544,-9.5594902125713));
#297471=CARTESIAN_POINT('Ctrl Pts',(-3.5689373379134E-14,39.1812499998538,
-10.5687124469213));
#297472=CARTESIAN_POINT('Ctrl Pts',(-3.10606665601014,39.3312499998532,
-9.5594902125713));
#297473=CARTESIAN_POINT('Ctrl Pts',(-6.21213331202025,39.4812499998525,
-8.55026797822134));
#297474=CARTESIAN_POINT('Ctrl Pts',(-8.13178807675723,39.6312499998519,
-5.90808986649102));
#297475=CARTESIAN_POINT('Ctrl Pts',(-10.0514428414942,39.7812499998513,
-3.2659117547607));
#297476=CARTESIAN_POINT('Ctrl Pts',(-10.0514428414942,39.9312499998507,
2.46189346052968E-15));
#297477=CARTESIAN_POINT('Ctrl Pts',(-10.0514428414942,40.0812499998502,
3.26591175476071));
#297478=CARTESIAN_POINT('Ctrl Pts',(-8.13178807675723,40.2312499998495,
5.90808986649102));
#297479=CARTESIAN_POINT('Ctrl Pts',(-6.21213331202025,40.3812499998489,
8.55026797822134));
#297480=CARTESIAN_POINT('Ctrl Pts',(-3.10606665601014,40.5312499998483,
9.5594902125713));
#297481=CARTESIAN_POINT('Ctrl Pts',(-3.39646400411187E-14,40.6812499998478,
10.5687124469213));
#297482=CARTESIAN_POINT('Ctrl Pts',(3.10606665601007,40.8312499998472,9.5594902125713));
#297483=CARTESIAN_POINT('Ctrl Pts',(6.21213331202018,40.9812499998466,8.55026797822134));
#297484=CARTESIAN_POINT('Ctrl Pts',(8.13178807675715,41.131249999846,5.90808986649102));
#297485=CARTESIAN_POINT('Ctrl Pts',(10.0514428414941,41.2812499998454,3.2659117547607));
#297486=CARTESIAN_POINT('Ctrl Pts',(10.0514428414941,41.4312499998448,-1.23094673026484E-15));
#297487=CARTESIAN_POINT('Ctrl Pts',(10.0514428414941,41.5812499998442,-3.26591175476071));
#297488=CARTESIAN_POINT('Ctrl Pts',(8.13178807675715,41.7312499998436,-5.90808986649102));
#297489=CARTESIAN_POINT('Ctrl Pts',(6.21213331202018,41.881249999843,-8.55026797822134));
#297490=CARTESIAN_POINT('Ctrl Pts',(3.10606665601007,42.0312499998423,-9.5594902125713));
#297491=CARTESIAN_POINT('Ctrl Pts',(-3.74170826507958E-14,42.1812499998418,
-10.5687124469213));
#297492=CARTESIAN_POINT('Ctrl Pts',(-3.10606665601015,42.3312499998411,
-9.5594902125713));
#297493=CARTESIAN_POINT('Ctrl Pts',(-6.21213331202025,42.4812499998406,
-8.55026797822134));
#297494=CARTESIAN_POINT('Ctrl Pts',(-8.13178807675723,42.6312499998399,
-5.90808986649102));
#297495=CARTESIAN_POINT('Ctrl Pts',(-10.0514428414942,42.7812499998393,
-3.2659117547607));
#297496=CARTESIAN_POINT('Ctrl Pts',(-10.0514428414942,42.9312499998387,
2.46189346052968E-15));
#297497=CARTESIAN_POINT('Ctrl Pts',(-10.0514428414942,43.0812499998381,
3.26591175476071));
#297498=CARTESIAN_POINT('Ctrl Pts',(-8.13178807675723,43.2312499998375,
5.90808986649102));
#297499=CARTESIAN_POINT('Ctrl Pts',(-6.21213331202025,43.3812499998369,
8.55026797822134));
#297500=CARTESIAN_POINT('Ctrl Pts',(-3.10606665601014,43.5312499998363,
9.5594902125713));
#297501=CARTESIAN_POINT('Ctrl Pts',(-3.56923493127805E-14,43.6812499998357,
10.5687124469213));
#297502=CARTESIAN_POINT('Ctrl Pts',(3.10606665601007,43.8312499998352,9.5594902125713));
#297503=CARTESIAN_POINT('Ctrl Pts',(6.21213331202018,43.9812499998345,8.55026797822134));
#297504=CARTESIAN_POINT('Ctrl Pts',(8.13178807675715,44.131249999834,5.90808986649102));
#297505=CARTESIAN_POINT('Ctrl Pts',(10.0514428414941,44.2812499998334,3.2659117547607));
#297506=CARTESIAN_POINT('Ctrl Pts',(10.0514428414941,44.4312499998328,-1.23094673026484E-15));
#297507=CARTESIAN_POINT('Ctrl Pts',(10.0514428414941,44.5812499998322,-3.26591175476071));
#297508=CARTESIAN_POINT('Ctrl Pts',(8.13178807675715,44.7312499998316,-5.90808986649102));
#297509=CARTESIAN_POINT('Ctrl Pts',(6.21213331202018,44.881249999831,-8.55026797822134));
#297510=CARTESIAN_POINT('Ctrl Pts',(3.10606665601007,45.0312499998304,-9.5594902125713));
#297511=CARTESIAN_POINT('Ctrl Pts',(-3.91447919224576E-14,45.1812499998297,
-10.5687124469213));
#297512=CARTESIAN_POINT('Ctrl Pts',(-3.10606665601015,45.3312499998292,
-9.5594902125713));
#297513=CARTESIAN_POINT('Ctrl Pts',(-6.21213331202026,45.4812499998285,
-8.55026797822134));
#297514=CARTESIAN_POINT('Ctrl Pts',(-8.13178807675723,45.6312499998279,
-5.90808986649102));
#297515=CARTESIAN_POINT('Ctrl Pts',(-10.0514428414942,45.7812499998273,
-3.2659117547607));
#297516=CARTESIAN_POINT('Ctrl Pts',(-10.0514428414942,45.9312499998267,
2.46189346052968E-15));
#297517=CARTESIAN_POINT('Ctrl Pts',(-10.0514428414942,46.0812499998261,
3.26591175476071));
#297518=CARTESIAN_POINT('Ctrl Pts',(-8.13178807675723,46.2312499998255,
5.90808986649102));
#297519=CARTESIAN_POINT('Ctrl Pts',(-6.21213331202025,46.3812499998249,
8.55026797822134));
#297520=CARTESIAN_POINT('Ctrl Pts',(-3.10606665601015,46.5312499998244,
9.5594902125713));
#297521=CARTESIAN_POINT('Ctrl Pts',(-3.74200585844424E-14,46.6812499998238,
10.5687124469213));
#297522=CARTESIAN_POINT('Ctrl Pts',(3.10606665601007,46.8312499998232,9.5594902125713));
#297523=CARTESIAN_POINT('Ctrl Pts',(6.21213331202018,46.9812499998226,8.55026797822134));
#297524=CARTESIAN_POINT('Ctrl Pts',(8.13178807675715,47.131249999822,5.90808986649102));
#297525=CARTESIAN_POINT('Ctrl Pts',(10.0514428414941,47.2812499998214,3.2659117547607));
#297526=CARTESIAN_POINT('Ctrl Pts',(10.0514428414941,47.4312499998208,-1.23094673026484E-15));
#297527=CARTESIAN_POINT('Ctrl Pts',(10.0514428414941,47.5812499998202,-3.26591175476071));
#297528=CARTESIAN_POINT('Ctrl Pts',(8.13178807675715,47.7312499998196,-5.90808986649102));
#297529=CARTESIAN_POINT('Ctrl Pts',(6.21213331202017,47.881249999819,-8.55026797822134));
#297530=CARTESIAN_POINT('Ctrl Pts',(3.10606665601007,48.0312499998184,-9.5594902125713));
#297531=CARTESIAN_POINT('Ctrl Pts',(-4.08725011941195E-14,48.1812499998178,
-10.5687124469213));
#297532=CARTESIAN_POINT('Ctrl Pts',(-3.10606665601015,48.3312499998172,
-9.5594902125713));
#297533=CARTESIAN_POINT('Ctrl Pts',(-6.21213331202026,48.4812499998166,
-8.55026797822134));
#297534=CARTESIAN_POINT('Ctrl Pts',(-8.13178807675723,48.6312499998159,
-5.90808986649102));
#297535=CARTESIAN_POINT('Ctrl Pts',(-10.0514428414942,48.7812499998153,
-3.2659117547607));
#297536=CARTESIAN_POINT('Ctrl Pts',(-10.0514428414942,48.9312499998147,
2.46189346052968E-15));
#297537=CARTESIAN_POINT('Ctrl Pts',(-10.0514428414942,49.0812499998141,
3.26591175476071));
#297538=CARTESIAN_POINT('Ctrl Pts',(-8.13178807675723,49.2312499998135,
5.90808986649102));
#297539=CARTESIAN_POINT('Ctrl Pts',(-6.21213331202026,49.3812499998129,
8.55026797822134));
#297540=CARTESIAN_POINT('Ctrl Pts',(-3.10606665601015,49.5312499998124,
9.5594902125713));
#297541=CARTESIAN_POINT('Ctrl Pts',(-3.91477678561042E-14,49.6812499998117,
10.5687124469213));
#297542=CARTESIAN_POINT('Ctrl Pts',(3.10606665601007,49.8312499998111,9.5594902125713));
#297543=CARTESIAN_POINT('Ctrl Pts',(6.21213331202017,49.9812499998106,8.55026797822134));
#297544=CARTESIAN_POINT('Ctrl Pts',(8.13178807675715,50.13124999981,5.90808986649102));
#297545=CARTESIAN_POINT('Ctrl Pts',(10.0514428414941,50.2812499998094,3.2659117547607));
#297546=CARTESIAN_POINT('Ctrl Pts',(10.0514428414941,50.4312499998088,-1.23094673026484E-15));
#297547=CARTESIAN_POINT('Ctrl Pts',(10.0514428414941,50.5812499998082,-3.26591175476071));
#297548=CARTESIAN_POINT('Ctrl Pts',(8.13178807675715,50.7312499998076,-5.90808986649102));
#297549=CARTESIAN_POINT('Ctrl Pts',(6.21213331202017,50.881249999807,-8.55026797822134));
#297550=CARTESIAN_POINT('Ctrl Pts',(3.10606665601007,51.0312499998064,-9.5594902125713));
#297551=CARTESIAN_POINT('Ctrl Pts',(-4.26002104657813E-14,51.1812499998058,
-10.5687124469213));
#297552=CARTESIAN_POINT('Ctrl Pts',(-3.10606665601015,51.3312499998052,
-9.5594902125713));
#297553=CARTESIAN_POINT('Ctrl Pts',(-6.21213331202026,51.4812499998045,
-8.55026797822134));
#297554=CARTESIAN_POINT('Ctrl Pts',(-8.13178807675723,51.631249999804,-5.90808986649102));
#297555=CARTESIAN_POINT('Ctrl Pts',(-10.0514428414942,51.7812499998034,
-3.2659117547607));
#297556=CARTESIAN_POINT('Ctrl Pts',(-10.0514428414942,51.9312499998027,
2.46189346052968E-15));
#297557=CARTESIAN_POINT('Ctrl Pts',(-10.0514428414942,52.0812499998021,
3.26591175476071));
#297558=CARTESIAN_POINT('Ctrl Pts',(-8.13178807675723,52.2312499998015,
5.90808986649102));
#297559=CARTESIAN_POINT('Ctrl Pts',(-6.21213331202026,52.3812499998009,
8.55026797822134));
#297560=CARTESIAN_POINT('Ctrl Pts',(-3.10606665601015,52.5312499998004,
9.5594902125713));
#297561=CARTESIAN_POINT('Ctrl Pts',(-4.08754771277661E-14,52.6812499997998,
10.5687124469213));
#297562=CARTESIAN_POINT('Ctrl Pts',(3.10606665601007,52.8312499997991,9.5594902125713));
#297563=CARTESIAN_POINT('Ctrl Pts',(6.21213331202017,52.9812499997986,8.55026797822134));
#297564=CARTESIAN_POINT('Ctrl Pts',(8.13178807675715,53.131249999798,5.90808986649102));
#297565=CARTESIAN_POINT('Ctrl Pts',(10.0514428414941,53.2812499997974,3.2659117547607));
#297566=CARTESIAN_POINT('Ctrl Pts',(10.0514428414941,53.4312499997968,-1.23094673026484E-15));
#297567=CARTESIAN_POINT('Ctrl Pts',(10.0514428414941,53.5812499997962,-3.26591175476071));
#297568=CARTESIAN_POINT('Ctrl Pts',(8.13178807675714,53.7312499997956,-5.90808986649102));
#297569=CARTESIAN_POINT('Ctrl Pts',(6.21213331202017,53.881249999795,-8.55026797822134));
#297570=CARTESIAN_POINT('Ctrl Pts',(3.10606665601006,54.0312499997944,-9.5594902125713));
#297571=CARTESIAN_POINT('Ctrl Pts',(-4.43279197374432E-14,54.1812499997938,
-10.5687124469213));
#297572=CARTESIAN_POINT('Ctrl Pts',(-3.10606665601015,54.3312499997932,
-9.5594902125713));
#297573=CARTESIAN_POINT('Ctrl Pts',(-6.21213331202026,54.4812499997926,
-8.55026797822134));
#297574=CARTESIAN_POINT('Ctrl Pts',(-8.13178807675724,54.6312499997919,
-5.90808986649102));
#297575=CARTESIAN_POINT('Ctrl Pts',(-10.0514428414942,54.7812499997914,
-3.2659117547607));
#297576=CARTESIAN_POINT('Ctrl Pts',(-10.0514428414942,54.9312499997907,
2.46189346052968E-15));
#297577=CARTESIAN_POINT('Ctrl Pts',(-10.0514428414942,55.0812499997901,
3.26591175476071));
#297578=CARTESIAN_POINT('Ctrl Pts',(-8.13178807675724,55.2312499997895,
5.90808986649102));
#297579=CARTESIAN_POINT('Ctrl Pts',(-6.21213331202026,55.3812499997889,
8.55026797822134));
#297580=CARTESIAN_POINT('Ctrl Pts',(-3.10606665601015,55.5312499997884,
9.5594902125713));
#297581=CARTESIAN_POINT('Ctrl Pts',(-4.26031863994279E-14,55.6812499997877,
10.5687124469213));
#297582=CARTESIAN_POINT('Ctrl Pts',(3.10606665601006,55.8312499997871,9.5594902125713));
#297583=CARTESIAN_POINT('Ctrl Pts',(6.21213331202017,55.9812499997865,8.55026797822134));
#297584=CARTESIAN_POINT('Ctrl Pts',(8.13178807675714,56.131249999786,5.90808986649102));
#297585=CARTESIAN_POINT('Ctrl Pts',(10.0514428414941,56.2812499997854,3.2659117547607));
#297586=CARTESIAN_POINT('Ctrl Pts',(10.0514428414941,56.4312499997848,-1.23094673026484E-15));
#297587=CARTESIAN_POINT('Ctrl Pts',(10.0514428414941,56.5812499997842,-3.26591175476071));
#297588=CARTESIAN_POINT('Ctrl Pts',(8.13178807675714,56.7312499997836,-5.90808986649102));
#297589=CARTESIAN_POINT('Ctrl Pts',(6.21213331202017,56.881249999783,-8.55026797822134));
#297590=CARTESIAN_POINT('Ctrl Pts',(3.10606665601006,57.0312499997824,-9.5594902125713));
#297591=CARTESIAN_POINT('Ctrl Pts',(-4.6055629009105E-14,57.1812499997818,
-10.5687124469213));
#297592=CARTESIAN_POINT('Ctrl Pts',(-3.10606665601015,57.3312499997812,
-9.5594902125713));
#297593=CARTESIAN_POINT('Ctrl Pts',(-6.21213331202026,57.4812499997805,
-8.55026797822134));
#297594=CARTESIAN_POINT('Ctrl Pts',(-8.13178807675724,57.6312499997799,
-5.90808986649102));
#297595=CARTESIAN_POINT('Ctrl Pts',(-10.0514428414942,57.7812499997793,
-3.2659117547607));
#297596=CARTESIAN_POINT('Ctrl Pts',(-10.0514428414942,57.9312499997787,
2.46189346052968E-15));
#297597=CARTESIAN_POINT('Ctrl Pts',(-10.0514428414942,58.0812499997781,
3.26591175476071));
#297598=CARTESIAN_POINT('Ctrl Pts',(-8.13178807675724,58.2312499997775,
5.90808986649102));
#297599=CARTESIAN_POINT('Ctrl Pts',(-6.21213331202026,58.3812499997769,
8.55026797822134));
#297600=CARTESIAN_POINT('Ctrl Pts',(-3.10606665601015,58.5312499997763,
9.5594902125713));
#297601=CARTESIAN_POINT('Ctrl Pts',(-4.43308956710897E-14,58.6812499997758,
10.5687124469213));
#297602=CARTESIAN_POINT('Ctrl Pts',(3.10606665601006,58.8312499997751,9.5594902125713));
#297603=CARTESIAN_POINT('Ctrl Pts',(6.21213331202017,58.9812499997745,8.55026797822134));
#297604=CARTESIAN_POINT('Ctrl Pts',(8.13178807675714,59.131249999774,5.90808986649102));
#297605=CARTESIAN_POINT('Ctrl Pts',(10.0514428414941,59.2812499997734,3.2659117547607));
#297606=CARTESIAN_POINT('Ctrl Pts',(10.0514428414941,59.4312499997728,-1.23094673026484E-15));
#297607=CARTESIAN_POINT('Ctrl Pts',(10.0514428414941,59.5812499997722,-3.26591175476071));
#297608=CARTESIAN_POINT('Ctrl Pts',(8.13178807675714,59.7312499997716,-5.90808986649102));
#297609=CARTESIAN_POINT('Ctrl Pts',(6.21213331202017,59.881249999771,-8.55026797822134));
#297610=CARTESIAN_POINT('Ctrl Pts',(3.10606665601006,60.0312499997704,-9.5594902125713));
#297611=CARTESIAN_POINT('Ctrl Pts',(-4.77833382807668E-14,60.1812499997698,
-10.5687124469213));
#297612=CARTESIAN_POINT('Ctrl Pts',(-3.10606665601016,60.3312499997692,
-9.5594902125713));
#297613=CARTESIAN_POINT('Ctrl Pts',(-6.21213331202026,60.4812499997686,
-8.55026797822134));
#297614=CARTESIAN_POINT('Ctrl Pts',(-8.13178807675724,60.6312499997679,
-5.90808986649102));
#297615=CARTESIAN_POINT('Ctrl Pts',(-10.0514428414942,60.7812499997674,
-3.2659117547607));
#297616=CARTESIAN_POINT('Ctrl Pts',(-10.0514428414942,60.9312499997667,
2.46189346052968E-15));
#297617=CARTESIAN_POINT('Ctrl Pts',(-10.0514428414942,61.0812499997661,
3.26591175476071));
#297618=CARTESIAN_POINT('Ctrl Pts',(-8.13178807675724,61.2312499997655,
5.90808986649102));
#297619=CARTESIAN_POINT('Ctrl Pts',(-6.21213331202026,61.3812499997649,
8.55026797822134));
#297620=CARTESIAN_POINT('Ctrl Pts',(-3.10606665601015,61.5312499997643,
9.5594902125713));
#297621=CARTESIAN_POINT('Ctrl Pts',(-4.60586049427516E-14,61.6812499997638,
10.5687124469213));
#297622=CARTESIAN_POINT('Ctrl Pts',(3.10606665601006,61.8312499997632,9.5594902125713));
#297623=CARTESIAN_POINT('Ctrl Pts',(6.21213331202017,61.9812499997625,8.55026797822134));
#297624=CARTESIAN_POINT('Ctrl Pts',(8.13178807675714,62.131249999762,5.90808986649102));
#297625=CARTESIAN_POINT('Ctrl Pts',(10.0514428414941,62.2812499997614,3.2659117547607));
#297626=CARTESIAN_POINT('Ctrl Pts',(10.0514428414941,62.4312499997608,-1.23094673026484E-15));
#297627=CARTESIAN_POINT('Ctrl Pts',(10.0514428414941,62.5812499997602,-3.26591175476071));
#297628=CARTESIAN_POINT('Ctrl Pts',(8.13178807675714,62.7312499997596,-5.90808986649102));
#297629=CARTESIAN_POINT('Ctrl Pts',(6.21213331202017,62.881249999759,-8.55026797822134));
#297630=CARTESIAN_POINT('Ctrl Pts',(3.10606665601006,63.0312499997584,-9.5594902125713));
#297631=CARTESIAN_POINT('Ctrl Pts',(-4.95110475524287E-14,63.1812499997578,
-10.5687124469213));
#297632=CARTESIAN_POINT('Ctrl Pts',(-3.10606665601016,63.3312499997572,
-9.5594902125713));
#297633=CARTESIAN_POINT('Ctrl Pts',(-6.21213331202027,63.4812499997565,
-8.55026797822134));
#297634=CARTESIAN_POINT('Ctrl Pts',(-8.13178807675724,63.631249999756,-5.90808986649102));
#297635=CARTESIAN_POINT('Ctrl Pts',(-10.0514428414942,63.7812499997553,
-3.2659117547607));
#297636=CARTESIAN_POINT('Ctrl Pts',(-10.0514428414942,63.9312499997548,
2.46189346052968E-15));
#297637=CARTESIAN_POINT('Ctrl Pts',(-10.0514428414942,64.0812499997541,
3.26591175476071));
#297638=CARTESIAN_POINT('Ctrl Pts',(-8.13178807675724,64.2312499997535,
5.90808986649102));
#297639=CARTESIAN_POINT('Ctrl Pts',(-6.21213331202026,64.381249999753,8.55026797822134));
#297640=CARTESIAN_POINT('Ctrl Pts',(-3.10606665601016,64.5312499997523,
9.5594902125713));
#297641=CARTESIAN_POINT('Ctrl Pts',(-4.77863142144134E-14,64.6812499997518,
10.5687124469213));
#297642=CARTESIAN_POINT('Ctrl Pts',(3.10606665601006,64.8312499997512,9.5594902125713));
#297643=CARTESIAN_POINT('Ctrl Pts',(6.21213331202017,64.9812499997506,8.55026797822134));
#297644=CARTESIAN_POINT('Ctrl Pts',(8.13178807675714,65.13124999975,5.90808986649102));
#297645=CARTESIAN_POINT('Ctrl Pts',(10.0514428414941,65.2812499997493,3.2659117547607));
#297646=CARTESIAN_POINT('Ctrl Pts',(10.0514428414941,65.4312499997488,-1.23094673026484E-15));
#297647=CARTESIAN_POINT('Ctrl Pts',(10.0514428414941,65.5812499997482,-3.26591175476071));
#297648=CARTESIAN_POINT('Ctrl Pts',(8.13178807675714,65.7312499997475,-5.90808986649102));
#297649=CARTESIAN_POINT('Ctrl Pts',(6.21213331202016,65.881249999747,-8.55026797822134));
#297650=CARTESIAN_POINT('Ctrl Pts',(3.10606665601006,66.0312499997464,-9.5594902125713));
#297651=CARTESIAN_POINT('Ctrl Pts',(-5.12387568240905E-14,66.1812499997457,
-10.5687124469213));
#297652=CARTESIAN_POINT('Ctrl Pts',(-3.10606665601016,66.3312499997451,
-9.5594902125713));
#297653=CARTESIAN_POINT('Ctrl Pts',(-6.21213331202027,66.4812499997445,
-8.55026797822134));
#297654=CARTESIAN_POINT('Ctrl Pts',(-8.13178807675724,66.6312499997439,
-5.90808986649102));
#297655=CARTESIAN_POINT('Ctrl Pts',(-10.0514428414942,66.7812499997433,
-3.2659117547607));
#297656=CARTESIAN_POINT('Ctrl Pts',(-10.0514428414942,66.9312499997427,
2.46189346052968E-15));
#297657=CARTESIAN_POINT('Ctrl Pts',(-10.0514428414942,67.0812499997421,
3.26591175476071));
#297658=CARTESIAN_POINT('Ctrl Pts',(-8.13178807675724,67.2312499997416,
5.90808986649102));
#297659=CARTESIAN_POINT('Ctrl Pts',(-6.21213331202027,67.3812499997409,
8.55026797822134));
#297660=CARTESIAN_POINT('Ctrl Pts',(-3.10606665601016,67.5312499997404,
9.5594902125713));
#297661=CARTESIAN_POINT('Ctrl Pts',(-4.95140234860752E-14,67.6812499997397,
10.5687124469213));
#297662=CARTESIAN_POINT('Ctrl Pts',(3.10606665601006,67.8312499997391,9.5594902125713));
#297663=CARTESIAN_POINT('Ctrl Pts',(6.21213331202017,67.9812499997385,8.55026797822134));
#297664=CARTESIAN_POINT('Ctrl Pts',(8.13178807675714,68.1312499997379,5.90808986649102));
#297665=CARTESIAN_POINT('Ctrl Pts',(10.0514428414941,68.2812499997374,3.2659117547607));
#297666=CARTESIAN_POINT('Ctrl Pts',(10.0514428414941,68.4312499997367,-1.23094673026484E-15));
#297667=CARTESIAN_POINT('Ctrl Pts',(10.0514428414941,68.5812499997361,-3.26591175476071));
#297668=CARTESIAN_POINT('Ctrl Pts',(8.13178807675714,68.7312499997356,-5.90808986649102));
#297669=CARTESIAN_POINT('Ctrl Pts',(6.21213331202016,68.881249999735,-8.55026797822134));
#297670=CARTESIAN_POINT('Ctrl Pts',(3.10606665601006,69.0312499997344,-9.5594902125713));
#297671=CARTESIAN_POINT('Ctrl Pts',(-5.29664660957524E-14,69.1812499997337,
-10.5687124469213));
#297672=CARTESIAN_POINT('Ctrl Pts',(-3.10606665601016,69.3312499997332,
-9.5594902125713));
#297673=CARTESIAN_POINT('Ctrl Pts',(-6.21213331202027,69.4812499997326,
-8.55026797822134));
#297674=CARTESIAN_POINT('Ctrl Pts',(-8.13178807675724,69.6312499997319,
-5.90808986649102));
#297675=CARTESIAN_POINT('Ctrl Pts',(-10.0514428414942,69.7812499997313,
-3.2659117547607));
#297676=CARTESIAN_POINT('Ctrl Pts',(-10.0514428414942,69.9312499997307,
2.46189346052968E-15));
#297677=CARTESIAN_POINT('Ctrl Pts',(-10.0514428414942,70.0812499997301,
3.26591175476071));
#297678=CARTESIAN_POINT('Ctrl Pts',(-8.13178807675724,70.2312499997295,
5.90808986649102));
#297679=CARTESIAN_POINT('Ctrl Pts',(-6.21213331202027,70.3812499997289,
8.55026797822134));
#297680=CARTESIAN_POINT('Ctrl Pts',(-3.10606665601016,70.5312499997283,
9.5594902125713));
#297681=CARTESIAN_POINT('Ctrl Pts',(-5.12417327577371E-14,70.6812499997277,
10.5687124469213));
#297682=CARTESIAN_POINT('Ctrl Pts',(3.10606665601006,70.8312499997271,9.5594902125713));
#297683=CARTESIAN_POINT('Ctrl Pts',(6.21213331202016,70.9812499997265,8.55026797822134));
#297684=CARTESIAN_POINT('Ctrl Pts',(8.13178807675714,71.131249999726,5.90808986649102));
#297685=CARTESIAN_POINT('Ctrl Pts',(10.0514428414941,71.2812499997253,3.2659117547607));
#297686=CARTESIAN_POINT('Ctrl Pts',(10.0514428414941,71.4312499997248,-1.23094673026484E-15));
#297687=CARTESIAN_POINT('Ctrl Pts',(10.0514428414941,71.5812499997242,-3.26591175476071));
#297688=CARTESIAN_POINT('Ctrl Pts',(8.13178807675713,71.7312499997236,-5.90808986649102));
#297689=CARTESIAN_POINT('Ctrl Pts',(6.21213331202016,71.881249999723,-8.55026797822134));
#297690=CARTESIAN_POINT('Ctrl Pts',(3.10606665601005,72.0312499997223,-9.5594902125713));
#297691=CARTESIAN_POINT('Ctrl Pts',(-5.46941753674142E-14,72.1812499997217,
-10.5687124469213));
#297692=CARTESIAN_POINT('Ctrl Pts',(-3.10606665601016,72.3312499997212,
-9.5594902125713));
#297693=CARTESIAN_POINT('Ctrl Pts',(-6.21213331202027,72.4812499997205,
-8.55026797822134));
#297694=CARTESIAN_POINT('Ctrl Pts',(-8.13178807675725,72.63124999972,-5.90808986649102));
#297695=CARTESIAN_POINT('Ctrl Pts',(-10.0514428414942,72.7812499997193,
-3.2659117547607));
#297696=CARTESIAN_POINT('Ctrl Pts',(-10.0514428414942,72.9312499997187,
2.46189346052968E-15));
#297697=CARTESIAN_POINT('Ctrl Pts',(-10.0514428414942,73.0812499997181,
3.26591175476071));
#297698=CARTESIAN_POINT('Ctrl Pts',(-8.13178807675725,73.2312499997175,
5.90808986649102));
#297699=CARTESIAN_POINT('Ctrl Pts',(-6.21213331202027,73.381249999717,8.55026797822134));
#297700=CARTESIAN_POINT('Ctrl Pts',(-3.10606665601016,73.5312499997164,
9.5594902125713));
#297701=CARTESIAN_POINT('Ctrl Pts',(-5.29694420293989E-14,73.6812499997157,
10.5687124469213));
#297702=CARTESIAN_POINT('Ctrl Pts',(3.10606665601005,73.8312499997151,9.5594902125713));
#297703=CARTESIAN_POINT('Ctrl Pts',(6.21213331202016,73.9812499997146,8.55026797822134));
#297704=CARTESIAN_POINT('Ctrl Pts',(8.13178807675713,74.1312499997139,5.90808986649102));
#297705=CARTESIAN_POINT('Ctrl Pts',(10.0514428414941,74.2812499997134,3.2659117547607));
#297706=CARTESIAN_POINT('Ctrl Pts',(10.0514428414941,74.4312499997127,-1.23094673026484E-15));
#297707=CARTESIAN_POINT('Ctrl Pts',(10.0514428414941,74.5812499997122,-3.26591175476071));
#297708=CARTESIAN_POINT('Ctrl Pts',(8.13178807675713,74.7312499997116,-5.90808986649102));
#297709=CARTESIAN_POINT('Ctrl Pts',(6.21213331202016,74.8812499997109,-8.55026797822134));
#297710=CARTESIAN_POINT('Ctrl Pts',(3.10606665601005,75.0312499997104,-9.5594902125713));
#297711=CARTESIAN_POINT('Ctrl Pts',(-5.6421884639076E-14,75.1812499997098,
-10.5687124469213));
#297712=CARTESIAN_POINT('Ctrl Pts',(-3.10606665601016,75.3312499997092,
-9.5594902125713));
#297713=CARTESIAN_POINT('Ctrl Pts',(-6.21213331202027,75.4812499997086,
-8.55026797822134));
#297714=CARTESIAN_POINT('Ctrl Pts',(-8.13178807675725,75.6312499997079,
-5.90808986649102));
#297715=CARTESIAN_POINT('Ctrl Pts',(-10.0514428414942,75.7812499997073,
-3.2659117547607));
#297716=CARTESIAN_POINT('Ctrl Pts',(-10.0514428414942,75.9312499997068,
2.46189346052968E-15));
#297717=CARTESIAN_POINT('Ctrl Pts',(-10.0514428414942,76.0812499997061,
3.26591175476071));
#297718=CARTESIAN_POINT('Ctrl Pts',(-8.13178807675725,76.2312499997055,
5.90808986649102));
#297719=CARTESIAN_POINT('Ctrl Pts',(-6.21213331202027,76.3812499997049,
8.55026797822134));
#297720=CARTESIAN_POINT('Ctrl Pts',(-3.10606665601016,76.5312499997043,
9.5594902125713));
#297721=CARTESIAN_POINT('Ctrl Pts',(-5.46971513010608E-14,76.6812499997037,
10.5687124469213));
#297722=CARTESIAN_POINT('Ctrl Pts',(3.10606665601005,76.8312499997031,9.5594902125713));
#297723=CARTESIAN_POINT('Ctrl Pts',(6.21213331202016,76.9812499997025,8.55026797822134));
#297724=CARTESIAN_POINT('Ctrl Pts',(8.13178807675713,77.131249999702,5.90808986649102));
#297725=CARTESIAN_POINT('Ctrl Pts',(10.0514428414941,77.2812499997013,3.2659117547607));
#297726=CARTESIAN_POINT('Ctrl Pts',(10.0514428414941,77.4312499997008,-1.23094673026484E-15));
#297727=CARTESIAN_POINT('Ctrl Pts',(10.0514428414941,77.5812499997001,-3.26591175476071));
#297728=CARTESIAN_POINT('Ctrl Pts',(8.13178807675713,77.7312499996995,-5.90808986649102));
#297729=CARTESIAN_POINT('Ctrl Pts',(6.21213331202016,77.881249999699,-8.55026797822134));
#297730=CARTESIAN_POINT('Ctrl Pts',(3.10606665601005,78.0312499996984,-9.5594902125713));
#297731=CARTESIAN_POINT('Ctrl Pts',(-5.81495939107379E-14,78.1812499996978,
-10.5687124469213));
#297732=CARTESIAN_POINT('Ctrl Pts',(-3.10606665601017,78.3312499996971,
-9.5594902125713));
#297733=CARTESIAN_POINT('Ctrl Pts',(-6.21213331202028,78.4812499996966,
-8.55026797822134));
#297734=CARTESIAN_POINT('Ctrl Pts',(-8.13178807675725,78.631249999696,-5.90808986649102));
#297735=CARTESIAN_POINT('Ctrl Pts',(-10.0514428414942,78.7812499996954,
-3.2659117547607));
#297736=CARTESIAN_POINT('Ctrl Pts',(-10.0514428414942,78.9312499996948,
2.46189346052968E-15));
#297737=CARTESIAN_POINT('Ctrl Pts',(-10.0514428414942,79.0812499996942,
3.26591175476071));
#297738=CARTESIAN_POINT('Ctrl Pts',(-8.13178807675725,79.2312499996936,
5.90808986649102));
#297739=CARTESIAN_POINT('Ctrl Pts',(-6.21213331202027,79.381249999693,8.55026797822134));
#297740=CARTESIAN_POINT('Ctrl Pts',(-3.10606665601016,79.5312499996923,
9.5594902125713));
#297741=CARTESIAN_POINT('Ctrl Pts',(-5.64248605727226E-14,79.6812499996917,
10.5687124469213));
#297742=CARTESIAN_POINT('Ctrl Pts',(3.10606665601005,79.8312499996911,9.5594902125713));
#297743=CARTESIAN_POINT('Ctrl Pts',(6.21213331202016,79.9812499996905,8.55026797822134));
#297744=CARTESIAN_POINT('Ctrl Pts',(8.13178807675713,80.1312499996899,5.90808986649102));
#297745=CARTESIAN_POINT('Ctrl Pts',(10.0514428414941,80.2812499996894,3.2659117547607));
#297746=CARTESIAN_POINT('Ctrl Pts',(10.0514428414941,80.4312499996887,-1.23094673026484E-15));
#297747=CARTESIAN_POINT('Ctrl Pts',(10.0514428414941,80.5812499996882,-3.26591175476071));
#297748=CARTESIAN_POINT('Ctrl Pts',(8.13178807675713,80.7312499996875,-5.90808986649102));
#297749=CARTESIAN_POINT('Ctrl Pts',(6.21213331202016,80.881249999687,-8.55026797822134));
#297750=CARTESIAN_POINT('Ctrl Pts',(3.10606665601005,81.0312499996864,-9.5594902125713));
#297751=CARTESIAN_POINT('Ctrl Pts',(-5.98773031823997E-14,81.1812499996858,
-10.5687124469213));
#297752=CARTESIAN_POINT('Ctrl Pts',(-3.10606665601017,81.3312499996851,
-9.5594902125713));
#297753=CARTESIAN_POINT('Ctrl Pts',(-6.21213331202028,81.4812499996845,
-8.55026797822134));
#297754=CARTESIAN_POINT('Ctrl Pts',(-8.13178807675725,81.6312499996839,
-5.90808986649102));
#297755=CARTESIAN_POINT('Ctrl Pts',(-10.0514428414942,81.7812499996834,
-3.2659117547607));
#297756=CARTESIAN_POINT('Ctrl Pts',(-10.0514428414942,81.9312499996827,
2.46189346052968E-15));
#297757=CARTESIAN_POINT('Ctrl Pts',(-10.0514428414942,82.0812499996821,
3.26591175476071));
#297758=CARTESIAN_POINT('Ctrl Pts',(-8.13178807675725,82.2312499996816,
5.90808986649102));
#297759=CARTESIAN_POINT('Ctrl Pts',(-6.21213331202028,82.381249999681,8.55026797822134));
#297760=CARTESIAN_POINT('Ctrl Pts',(-3.10606665601017,82.5312499996804,
9.5594902125713));
#297761=CARTESIAN_POINT('Ctrl Pts',(-5.81525698443845E-14,82.6812499996797,
10.5687124469213));
#297762=CARTESIAN_POINT('Ctrl Pts',(3.10606665601005,82.8312499996792,9.5594902125713));
#297763=CARTESIAN_POINT('Ctrl Pts',(6.21213331202016,82.9812499996786,8.55026797822134));
#297764=CARTESIAN_POINT('Ctrl Pts',(8.13178807675713,83.131249999678,5.90808986649102));
#297765=CARTESIAN_POINT('Ctrl Pts',(10.0514428414941,83.2812499996773,3.2659117547607));
#297766=CARTESIAN_POINT('Ctrl Pts',(10.0514428414941,83.4312499996767,-1.23094673026484E-15));
#297767=CARTESIAN_POINT('Ctrl Pts',(10.0514428414941,83.5812499996761,-3.26591175476071));
#297768=CARTESIAN_POINT('Ctrl Pts',(8.13178807675713,83.7312499996756,-5.90808986649102));
#297769=CARTESIAN_POINT('Ctrl Pts',(6.21213331202016,83.8812499996749,-8.55026797822134));
#297770=CARTESIAN_POINT('Ctrl Pts',(3.10606665601005,84.0312499996743,-9.5594902125713));
#297771=CARTESIAN_POINT('Ctrl Pts',(-6.16050124540615E-14,84.1812499996738,
-10.5687124469213));
#297772=CARTESIAN_POINT('Ctrl Pts',(-3.10606665601017,84.3312499996732,
-9.5594902125713));
#297773=CARTESIAN_POINT('Ctrl Pts',(-6.21213331202028,84.4812499996725,
-8.55026797822134));
#297774=CARTESIAN_POINT('Ctrl Pts',(-8.13178807675725,84.631249999672,-5.90808986649102));
#297775=CARTESIAN_POINT('Ctrl Pts',(-10.0514428414942,84.7812499996714,
-3.2659117547607));
#297776=CARTESIAN_POINT('Ctrl Pts',(-10.0514428414942,84.9312499996708,
2.46189346052968E-15));
#297777=CARTESIAN_POINT('Ctrl Pts',(-10.0514428414942,85.0812499996701,
3.26591175476071));
#297778=CARTESIAN_POINT('Ctrl Pts',(-8.13178807675725,85.2312499996695,
5.90808986649102));
#297779=CARTESIAN_POINT('Ctrl Pts',(-6.21213331202028,85.381249999669,8.55026797822134));
#297780=CARTESIAN_POINT('Ctrl Pts',(-3.10606665601017,85.5312499996683,
9.5594902125713));
#297781=CARTESIAN_POINT('Ctrl Pts',(-5.98802791160463E-14,85.6812499996678,
10.5687124469213));
#297782=CARTESIAN_POINT('Ctrl Pts',(3.10606665601005,85.8312499996672,9.5594902125713));
#297783=CARTESIAN_POINT('Ctrl Pts',(6.21213331202016,85.9812499996666,8.55026797822134));
#297784=CARTESIAN_POINT('Ctrl Pts',(8.13178807675713,86.1312499996659,5.90808986649102));
#297785=CARTESIAN_POINT('Ctrl Pts',(10.0514428414941,86.2812499996653,3.2659117547607));
#297786=CARTESIAN_POINT('Ctrl Pts',(10.0514428414941,86.4312499996647,-1.23094673026484E-15));
#297787=CARTESIAN_POINT('Ctrl Pts',(10.0514428414941,86.5812499996642,-3.26591175476071));
#297788=CARTESIAN_POINT('Ctrl Pts',(8.13178807675713,86.7312499996635,-5.90808986649102));
#297789=CARTESIAN_POINT('Ctrl Pts',(6.21213331202015,86.8812499996629,-8.55026797822134));
#297790=CARTESIAN_POINT('Ctrl Pts',(3.10606665601004,87.0312499996624,-9.5594902125713));
#297791=CARTESIAN_POINT('Ctrl Pts',(-6.33327217257234E-14,87.1812499996618,
-10.5687124469213));
#297792=CARTESIAN_POINT('Ctrl Pts',(-3.10606665601017,87.3312499996611,
-9.5594902125713));
#297793=CARTESIAN_POINT('Ctrl Pts',(-6.21213331202028,87.4812499996605,
-8.55026797822134));
#297794=CARTESIAN_POINT('Ctrl Pts',(-8.13178807675726,87.6312499996599,
-5.90808986649102));
#297795=CARTESIAN_POINT('Ctrl Pts',(-10.0514428414942,87.7812499996594,
-3.2659117547607));
#297796=CARTESIAN_POINT('Ctrl Pts',(-10.0514428414942,87.9312499996587,
2.46189346052968E-15));
#297797=CARTESIAN_POINT('Ctrl Pts',(-10.0514428414942,88.0812499996581,
3.26591175476071));
#297798=CARTESIAN_POINT('Ctrl Pts',(-8.13178807675726,88.2312499996575,
5.90808986649102));
#297799=CARTESIAN_POINT('Ctrl Pts',(-6.21213331202028,88.3812499996569,
8.55026797822134));
#297800=CARTESIAN_POINT('Ctrl Pts',(-3.10606665601017,88.5312499996564,
9.5594902125713));
#297801=CARTESIAN_POINT('Ctrl Pts',(-6.16079883877081E-14,88.6812499996557,
10.5687124469213));
#297802=CARTESIAN_POINT('Ctrl Pts',(3.10606665601005,88.8312499996552,9.5594902125713));
#297803=CARTESIAN_POINT('Ctrl Pts',(6.21213331202016,88.9812499996546,8.55026797822134));
#297804=CARTESIAN_POINT('Ctrl Pts',(8.13178807675713,89.131249999654,5.90808986649102));
#297805=CARTESIAN_POINT('Ctrl Pts',(10.0514428414941,89.2812499996533,3.2659117547607));
#297806=CARTESIAN_POINT('Ctrl Pts',(10.0514428414941,89.4312499996527,-1.23094673026484E-15));
#297807=CARTESIAN_POINT('Ctrl Pts',(10.0514428414941,89.5812499996521,-3.26591175476071));
#297808=CARTESIAN_POINT('Ctrl Pts',(8.13178807675713,89.7312499996515,-5.90808986649102));
#297809=CARTESIAN_POINT('Ctrl Pts',(6.21213331202015,89.8812499996509,-8.55026797822134));
#297810=CARTESIAN_POINT('Ctrl Pts',(3.10606665601004,90.0312499996504,-9.5594902125713));
#297811=CARTESIAN_POINT('Ctrl Pts',(-6.50604309973852E-14,90.1812499996498,
-10.5687124469213));
#297812=CARTESIAN_POINT('Ctrl Pts',(-3.10606665601017,90.3312499996491,
-9.5594902125713));
#297813=CARTESIAN_POINT('Ctrl Pts',(-6.21213331202028,90.4812499996485,
-8.55026797822134));
#297814=CARTESIAN_POINT('Ctrl Pts',(-8.13178807675726,90.631249999648,-5.90808986649102));
#297815=CARTESIAN_POINT('Ctrl Pts',(-10.0514428414942,90.7812499996473,
-3.2659117547607));
#297816=CARTESIAN_POINT('Ctrl Pts',(-10.0514428414942,90.9312499996468,
2.46189346052968E-15));
#297817=CARTESIAN_POINT('Ctrl Pts',(-10.0514428414942,91.0812499996461,
3.26591175476071));
#297818=CARTESIAN_POINT('Ctrl Pts',(-8.13178807675726,91.2312499996455,
5.90808986649102));
#297819=CARTESIAN_POINT('Ctrl Pts',(-6.21213331202028,91.381249999645,8.55026797822134));
#297820=CARTESIAN_POINT('Ctrl Pts',(-3.10606665601017,91.5312499996443,
9.5594902125713));
#297821=CARTESIAN_POINT('Ctrl Pts',(-6.333569765937E-14,91.6812499996438,
10.5687124469213));
#297822=CARTESIAN_POINT('Ctrl Pts',(3.10606665601004,91.8312499996431,9.5594902125713));
#297823=CARTESIAN_POINT('Ctrl Pts',(6.21213331202015,91.9812499996426,8.55026797822134));
#297824=CARTESIAN_POINT('Ctrl Pts',(8.13178807675712,92.131249999642,5.90808986649102));
#297825=CARTESIAN_POINT('Ctrl Pts',(10.0514428414941,92.2812499996414,3.2659117547607));
#297826=CARTESIAN_POINT('Ctrl Pts',(10.0514428414941,92.4312499996408,-1.23094673026484E-15));
#297827=CARTESIAN_POINT('Ctrl Pts',(10.0514428414941,92.5812499996402,-3.26591175476071));
#297828=CARTESIAN_POINT('Ctrl Pts',(8.13178807675712,92.7312499996396,-5.90808986649102));
#297829=CARTESIAN_POINT('Ctrl Pts',(6.21213331202015,92.8812499996389,-8.55026797822134));
#297830=CARTESIAN_POINT('Ctrl Pts',(3.10606665601004,93.0312499996383,-9.5594902125713));
#297831=CARTESIAN_POINT('Ctrl Pts',(-6.67881402690471E-14,93.1812499996377,
-10.5687124469213));
#297832=CARTESIAN_POINT('Ctrl Pts',(-3.10606665601018,93.3312499996371,
-9.5594902125713));
#297833=CARTESIAN_POINT('Ctrl Pts',(-6.21213331202028,93.4812499996365,
-8.55026797822134));
#297834=CARTESIAN_POINT('Ctrl Pts',(-8.13178807675726,93.6312499996359,
-5.90808986649102));
#297835=CARTESIAN_POINT('Ctrl Pts',(-10.0514428414942,93.7812499996353,
-3.2659117547607));
#297836=CARTESIAN_POINT('Ctrl Pts',(-10.0514428414942,93.9312499996347,
2.46189346052968E-15));
#297837=CARTESIAN_POINT('Ctrl Pts',(-10.0514428414942,94.0812499996341,
3.26591175476071));
#297838=CARTESIAN_POINT('Ctrl Pts',(-8.13178807675726,94.2312499996335,
5.90808986649102));
#297839=CARTESIAN_POINT('Ctrl Pts',(-6.21213331202028,94.381249999633,8.55026797822134));
#297840=CARTESIAN_POINT('Ctrl Pts',(-3.10606665601017,94.5312499996324,
9.5594902125713));
#297841=CARTESIAN_POINT('Ctrl Pts',(-6.50634069310318E-14,94.6812499996317,
10.5687124469213));
#297842=CARTESIAN_POINT('Ctrl Pts',(3.10606665601004,94.8312499996312,9.5594902125713));
#297843=CARTESIAN_POINT('Ctrl Pts',(6.21213331202015,94.9812499996306,8.55026797822134));
#297844=CARTESIAN_POINT('Ctrl Pts',(8.13178807675712,95.13124999963,5.90808986649102));
#297845=CARTESIAN_POINT('Ctrl Pts',(10.0514428414941,95.2812499996293,3.2659117547607));
#297846=CARTESIAN_POINT('Ctrl Pts',(10.0514428414941,95.4312499996288,-1.23094673026484E-15));
#297847=CARTESIAN_POINT('Ctrl Pts',(10.0514428414941,95.5812499996282,-3.26591175476071));
#297848=CARTESIAN_POINT('Ctrl Pts',(8.13178807675712,95.7312499996276,-5.90808986649102));
#297849=CARTESIAN_POINT('Ctrl Pts',(6.21213331202015,95.8812499996269,-8.55026797822134));
#297850=CARTESIAN_POINT('Ctrl Pts',(3.10606665601004,96.0312499996264,-9.5594902125713));
#297851=CARTESIAN_POINT('Ctrl Pts',(-6.85158495407089E-14,96.1812499996257,
-10.5687124469213));
#297852=CARTESIAN_POINT('Ctrl Pts',(-3.10606665601018,96.3312499996252,
-9.5594902125713));
#297853=CARTESIAN_POINT('Ctrl Pts',(-6.21213331202028,96.4812499996245,
-8.55026797822134));
#297854=CARTESIAN_POINT('Ctrl Pts',(-8.13178807675726,96.6312499996239,
-5.90808986649102));
#297855=CARTESIAN_POINT('Ctrl Pts',(-10.0514428414942,96.7812499996234,
-3.2659117547607));
#297856=CARTESIAN_POINT('Ctrl Pts',(-10.0514428414942,96.9312499996227,
2.46189346052968E-15));
#297857=CARTESIAN_POINT('Ctrl Pts',(-10.0514428414942,97.0812499996221,
3.26591175476071));
#297858=CARTESIAN_POINT('Ctrl Pts',(-8.13178807675726,97.2312499996215,
5.90808986649102));
#297859=CARTESIAN_POINT('Ctrl Pts',(-6.21213331202028,97.381249999621,8.55026797822134));
#297860=CARTESIAN_POINT('Ctrl Pts',(-3.10606665601017,97.5312499996203,
9.5594902125713));
#297861=CARTESIAN_POINT('Ctrl Pts',(-6.67911162026936E-14,97.6812499996197,
10.5687124469213));
#297862=CARTESIAN_POINT('Ctrl Pts',(3.10606665601004,97.8312499996191,9.5594902125713));
#297863=CARTESIAN_POINT('Ctrl Pts',(6.21213331202015,97.9812499996186,8.55026797822134));
#297864=CARTESIAN_POINT('Ctrl Pts',(8.13178807675712,98.1312499996179,5.90808986649102));
#297865=CARTESIAN_POINT('Ctrl Pts',(10.0514428414941,98.2812499996173,3.2659117547607));
#297866=CARTESIAN_POINT('Ctrl Pts',(10.0514428414941,98.4312499996168,-1.23094673026484E-15));
#297867=CARTESIAN_POINT('Ctrl Pts',(10.0514428414941,98.5812499996162,-3.26591175476071));
#297868=CARTESIAN_POINT('Ctrl Pts',(8.13178807675712,98.7312499996156,-5.90808986649102));
#297869=CARTESIAN_POINT('Ctrl Pts',(6.21213331202015,98.8812499996149,-8.55026797822134));
#297870=CARTESIAN_POINT('Ctrl Pts',(3.10606665601004,99.0312499996143,-9.5594902125713));
#297871=CARTESIAN_POINT('Ctrl Pts',(-7.02435588123707E-14,99.1812499996138,
-10.5687124469213));
#297872=CARTESIAN_POINT('Ctrl Pts',(-3.10606665601018,99.3312499996131,
-9.5594902125713));
#297873=CARTESIAN_POINT('Ctrl Pts',(-6.21213331202028,99.4812499996125,
-8.55026797822134));
#297874=CARTESIAN_POINT('Ctrl Pts',(-8.13178807675726,99.631249999612,-5.90808986649102));
#297875=CARTESIAN_POINT('Ctrl Pts',(-10.0514428414942,99.7812499996113,
-3.2659117547607));
#297876=CARTESIAN_POINT('Ctrl Pts',(-10.0514428414942,99.9312499996108,
2.46189346052968E-15));
#297877=CARTESIAN_POINT('Ctrl Pts',(-10.0514428414942,100.08124999961,3.26591175476071));
#297878=CARTESIAN_POINT('Ctrl Pts',(-8.13178807675726,100.23124999961,5.90808986649102));
#297879=CARTESIAN_POINT('Ctrl Pts',(-6.21213331202028,100.381249999609,
8.55026797822134));
#297880=CARTESIAN_POINT('Ctrl Pts',(-3.10606665601018,100.531249999608,
9.5594902125713));
#297881=CARTESIAN_POINT('Ctrl Pts',(-6.85188254743555E-14,100.681249999608,
10.5687124469213));
#297882=CARTESIAN_POINT('Ctrl Pts',(3.10606665601004,100.831249999607,9.5594902125713));
#297883=CARTESIAN_POINT('Ctrl Pts',(6.21213331202015,100.981249999607,8.55026797822134));
#297884=CARTESIAN_POINT('Ctrl Pts',(8.13178807675712,101.131249999606,5.90808986649102));
#297885=CARTESIAN_POINT('Ctrl Pts',(10.0514428414941,101.281249999605,3.2659117547607));
#297886=CARTESIAN_POINT('Ctrl Pts',(10.0514428414941,101.431249999605,-1.23094673026484E-15));
#297887=CARTESIAN_POINT('Ctrl Pts',(10.0514428414941,101.581249999604,-3.26591175476071));
#297888=CARTESIAN_POINT('Ctrl Pts',(8.13178807675712,101.731249999604,-5.90808986649102));
#297889=CARTESIAN_POINT('Ctrl Pts',(6.21213331202014,101.881249999603,-8.55026797822134));
#297890=CARTESIAN_POINT('Ctrl Pts',(3.10606665601004,102.031249999602,-9.5594902125713));
#297891=CARTESIAN_POINT('Ctrl Pts',(-7.19712680840326E-14,102.181249999602,
-10.5687124469213));
#297892=CARTESIAN_POINT('Ctrl Pts',(-3.10606665601018,102.331249999601,
-9.5594902125713));
#297893=CARTESIAN_POINT('Ctrl Pts',(-6.21213331202029,102.481249999601,
-8.55026797822134));
#297894=CARTESIAN_POINT('Ctrl Pts',(-8.13178807675726,102.6312499996,-5.90808986649102));
#297895=CARTESIAN_POINT('Ctrl Pts',(-10.0514428414942,102.781249999599,
-3.2659117547607));
#297896=CARTESIAN_POINT('Ctrl Pts',(-10.0514428414942,102.931249999599,
2.46189346052968E-15));
#297897=CARTESIAN_POINT('Ctrl Pts',(-10.0514428414942,103.081249999598,
3.26591175476071));
#297898=CARTESIAN_POINT('Ctrl Pts',(-8.13178807675726,103.231249999598,
5.90808986649102));
#297899=CARTESIAN_POINT('Ctrl Pts',(-6.21213331202028,103.381249999597,
8.55026797822134));
#297900=CARTESIAN_POINT('Ctrl Pts',(-3.10606665601018,103.531249999596,
9.5594902125713));
#297901=CARTESIAN_POINT('Ctrl Pts',(-7.02465347460173E-14,103.681249999596,
10.5687124469213));
#297902=CARTESIAN_POINT('Ctrl Pts',(3.10606665601004,103.831249999595,9.5594902125713));
#297903=CARTESIAN_POINT('Ctrl Pts',(6.21213331202015,103.981249999595,8.55026797822134));
#297904=CARTESIAN_POINT('Ctrl Pts',(8.13178807675712,104.131249999594,5.90808986649102));
#297905=CARTESIAN_POINT('Ctrl Pts',(10.0514428414941,104.281249999593,3.2659117547607));
#297906=CARTESIAN_POINT('Ctrl Pts',(10.0514428414941,104.431249999593,-1.23094673026484E-15));
#297907=CARTESIAN_POINT('Ctrl Pts',(10.0514428414941,104.581249999592,-3.26591175476071));
#297908=CARTESIAN_POINT('Ctrl Pts',(8.13178807675712,104.731249999592,-5.90808986649102));
#297909=CARTESIAN_POINT('Ctrl Pts',(6.21213331202014,104.881249999591,-8.55026797822134));
#297910=CARTESIAN_POINT('Ctrl Pts',(3.10606665601003,105.03124999959,-9.5594902125713));
#297911=CARTESIAN_POINT('Ctrl Pts',(-7.36989773556944E-14,105.18124999959,
-10.5687124469213));
#297912=CARTESIAN_POINT('Ctrl Pts',(-3.10606665601018,105.331249999589,
-9.5594902125713));
#297913=CARTESIAN_POINT('Ctrl Pts',(-6.21213331202029,105.481249999589,
-8.55026797822134));
#297914=CARTESIAN_POINT('Ctrl Pts',(-8.13178807675726,105.631249999588,
-5.90808986649102));
#297915=CARTESIAN_POINT('Ctrl Pts',(-10.0514428414942,105.781249999587,
-3.2659117547607));
#297916=CARTESIAN_POINT('Ctrl Pts',(-10.0514428414942,105.931249999587,
2.46189346052968E-15));
#297917=CARTESIAN_POINT('Ctrl Pts',(-10.0514428414942,106.081249999586,
3.26591175476071));
#297918=CARTESIAN_POINT('Ctrl Pts',(-8.13178807675726,106.231249999586,
5.90808986649102));
#297919=CARTESIAN_POINT('Ctrl Pts',(-6.21213331202029,106.381249999585,
8.55026797822134));
#297920=CARTESIAN_POINT('Ctrl Pts',(-3.10606665601018,106.531249999584,
9.5594902125713));
#297921=CARTESIAN_POINT('Ctrl Pts',(-7.19742440176792E-14,106.681249999584,
10.5687124469213));
#297922=CARTESIAN_POINT('Ctrl Pts',(3.10606665601004,106.831249999583,9.5594902125713));
#297923=CARTESIAN_POINT('Ctrl Pts',(6.21213331202014,106.981249999583,8.55026797822134));
#297924=CARTESIAN_POINT('Ctrl Pts',(8.13178807675711,107.131249999582,5.90808986649102));
#297925=CARTESIAN_POINT('Ctrl Pts',(10.0514428414941,107.281249999581,3.2659117547607));
#297926=CARTESIAN_POINT('Ctrl Pts',(10.0514428414941,107.431249999581,-1.23094673026484E-15));
#297927=CARTESIAN_POINT('Ctrl Pts',(10.0514428414941,107.58124999958,-3.26591175476071));
#297928=CARTESIAN_POINT('Ctrl Pts',(8.13178807675711,107.73124999958,-5.90808986649102));
#297929=CARTESIAN_POINT('Ctrl Pts',(6.21213331202014,107.881249999579,-8.55026797822134));
#297930=CARTESIAN_POINT('Ctrl Pts',(3.10606665601003,108.031249999578,-9.5594902125713));
#297931=CARTESIAN_POINT('Ctrl Pts',(-7.54266866273562E-14,108.181249999578,
-10.5687124469213));
#297932=CARTESIAN_POINT('Ctrl Pts',(-3.10606665601018,108.331249999577,
-9.5594902125713));
#297933=CARTESIAN_POINT('Ctrl Pts',(-6.21213331202029,108.481249999577,
-8.55026797822134));
#297934=CARTESIAN_POINT('Ctrl Pts',(-8.13178807675727,108.631249999576,
-5.90808986649102));
#297935=CARTESIAN_POINT('Ctrl Pts',(-10.0514428414942,108.781249999575,
-3.2659117547607));
#297936=CARTESIAN_POINT('Ctrl Pts',(-10.0514428414942,108.931249999575,
2.46189346052968E-15));
#297937=CARTESIAN_POINT('Ctrl Pts',(-10.0514428414942,109.081249999574,
3.26591175476071));
#297938=CARTESIAN_POINT('Ctrl Pts',(-8.13178807675727,109.231249999574,
5.90808986649102));
#297939=CARTESIAN_POINT('Ctrl Pts',(-6.21213331202029,109.381249999573,
8.55026797822134));
#297940=CARTESIAN_POINT('Ctrl Pts',(-3.10606665601018,109.531249999572,
9.5594902125713));
#297941=CARTESIAN_POINT('Ctrl Pts',(-7.3701953289341E-14,109.681249999572,
10.5687124469213));
#297942=CARTESIAN_POINT('Ctrl Pts',(3.10606665601003,109.831249999571,9.5594902125713));
#297943=CARTESIAN_POINT('Ctrl Pts',(6.21213331202014,109.981249999571,8.55026797822134));
#297944=CARTESIAN_POINT('Ctrl Pts',(8.13178807675711,110.13124999957,5.90808986649102));
#297945=CARTESIAN_POINT('Ctrl Pts',(10.0514428414941,110.281249999569,3.2659117547607));
#297946=CARTESIAN_POINT('Ctrl Pts',(10.0514428414941,110.431249999569,-1.23094673026484E-15));
#297947=CARTESIAN_POINT('Ctrl Pts',(10.0514428414941,110.581249999568,-3.26591175476071));
#297948=CARTESIAN_POINT('Ctrl Pts',(8.13178807675711,110.731249999568,-5.90808986649102));
#297949=CARTESIAN_POINT('Ctrl Pts',(6.21213331202014,110.881249999567,-8.55026797822134));
#297950=CARTESIAN_POINT('Ctrl Pts',(3.10606665601003,111.031249999566,-9.5594902125713));
#297951=CARTESIAN_POINT('Ctrl Pts',(-7.71543958990181E-14,111.181249999566,
-10.5687124469213));
#297952=CARTESIAN_POINT('Ctrl Pts',(-3.10606665601019,111.331249999565,
-9.5594902125713));
#297953=CARTESIAN_POINT('Ctrl Pts',(-6.21213331202029,111.481249999565,
-8.55026797822134));
#297954=CARTESIAN_POINT('Ctrl Pts',(-8.13178807675727,111.631249999564,
-5.90808986649102));
#297955=CARTESIAN_POINT('Ctrl Pts',(-10.0514428414942,111.781249999563,
-3.2659117547607));
#297956=CARTESIAN_POINT('Ctrl Pts',(-10.0514428414942,111.931249999563,
2.46189346052968E-15));
#297957=CARTESIAN_POINT('Ctrl Pts',(-10.0514428414942,112.081249999562,
3.26591175476071));
#297958=CARTESIAN_POINT('Ctrl Pts',(-8.13178807675727,112.231249999562,
5.90808986649102));
#297959=CARTESIAN_POINT('Ctrl Pts',(-6.21213331202029,112.381249999561,
8.55026797822134));
#297960=CARTESIAN_POINT('Ctrl Pts',(-3.10606665601018,112.53124999956,9.5594902125713));
#297961=CARTESIAN_POINT('Ctrl Pts',(-7.54296625610028E-14,112.68124999956,
10.5687124469213));
#297962=CARTESIAN_POINT('Ctrl Pts',(3.10606665601003,112.831249999559,9.5594902125713));
#297963=CARTESIAN_POINT('Ctrl Pts',(6.21213331202014,112.981249999559,8.55026797822134));
#297964=CARTESIAN_POINT('Ctrl Pts',(8.13178807675711,113.131249999558,5.90808986649102));
#297965=CARTESIAN_POINT('Ctrl Pts',(10.0514428414941,113.281249999557,3.2659117547607));
#297966=CARTESIAN_POINT('Ctrl Pts',(10.0514428414941,113.431249999557,-1.23094673026484E-15));
#297967=CARTESIAN_POINT('Ctrl Pts',(10.0514428414941,113.581249999556,-3.26591175476071));
#297968=CARTESIAN_POINT('Ctrl Pts',(8.13178807675711,113.731249999556,-5.90808986649102));
#297969=CARTESIAN_POINT('Ctrl Pts',(6.21213331202014,113.881249999555,-8.55026797822134));
#297970=CARTESIAN_POINT('Ctrl Pts',(3.10606665601003,114.031249999554,-9.5594902125713));
#297971=CARTESIAN_POINT('Ctrl Pts',(-7.88821051706799E-14,114.181249999554,
-10.5687124469213));
#297972=CARTESIAN_POINT('Ctrl Pts',(-3.10606665601019,114.331249999553,
-9.5594902125713));
#297973=CARTESIAN_POINT('Ctrl Pts',(-6.2121333120203,114.481249999553,-8.55026797822134));
#297974=CARTESIAN_POINT('Ctrl Pts',(-8.13178807675727,114.631249999552,
-5.90808986649102));
#297975=CARTESIAN_POINT('Ctrl Pts',(-10.0514428414942,114.781249999551,
-3.2659117547607));
#297976=CARTESIAN_POINT('Ctrl Pts',(-10.0514428414942,114.931249999551,
2.46189346052968E-15));
#297977=CARTESIAN_POINT('Ctrl Pts',(-10.0514428414942,115.08124999955,3.26591175476071));
#297978=CARTESIAN_POINT('Ctrl Pts',(-8.13178807675727,115.23124999955,5.90808986649102));
#297979=CARTESIAN_POINT('Ctrl Pts',(-6.21213331202029,115.381249999549,
8.55026797822134));
#297980=CARTESIAN_POINT('Ctrl Pts',(-3.10606665601018,115.531249999548,
9.5594902125713));
#297981=CARTESIAN_POINT('Ctrl Pts',(-7.71573718326647E-14,115.681249999548,
10.5687124469213));
#297982=CARTESIAN_POINT('Ctrl Pts',(3.10606665601003,115.831249999547,9.5594902125713));
#297983=CARTESIAN_POINT('Ctrl Pts',(6.21213331202014,115.981249999547,8.55026797822134));
#297984=CARTESIAN_POINT('Ctrl Pts',(8.13178807675711,116.131249999546,5.90808986649102));
#297985=CARTESIAN_POINT('Ctrl Pts',(10.0514428414941,116.281249999545,3.2659117547607));
#297986=CARTESIAN_POINT('Ctrl Pts',(10.0514428414941,116.431249999545,-1.23094673026484E-15));
#297987=CARTESIAN_POINT('Ctrl Pts',(10.0514428414941,116.581249999544,-3.26591175476071));
#297988=CARTESIAN_POINT('Ctrl Pts',(8.13178807675711,116.731249999544,-5.90808986649102));
#297989=CARTESIAN_POINT('Ctrl Pts',(6.21213331202014,116.881249999543,-8.55026797822134));
#297990=CARTESIAN_POINT('Ctrl Pts',(3.10606665601003,117.031249999542,-9.5594902125713));
#297991=CARTESIAN_POINT('Ctrl Pts',(-8.06098144423418E-14,117.181249999542,
-10.5687124469213));
#297992=CARTESIAN_POINT('Ctrl Pts',(-3.10606665601019,117.331249999541,
-9.5594902125713));
#297993=CARTESIAN_POINT('Ctrl Pts',(-6.2121333120203,117.481249999541,-8.55026797822134));
#297994=CARTESIAN_POINT('Ctrl Pts',(-8.13178807675727,117.63124999954,-5.90808986649102));
#297995=CARTESIAN_POINT('Ctrl Pts',(-10.0514428414942,117.781249999539,
-3.2659117547607));
#297996=CARTESIAN_POINT('Ctrl Pts',(-10.0514428414942,117.931249999539,
2.46189346052968E-15));
#297997=CARTESIAN_POINT('Ctrl Pts',(-10.0514428414942,118.081249999538,
3.26591175476071));
#297998=CARTESIAN_POINT('Ctrl Pts',(-8.13178807675727,118.231249999538,
5.90808986649102));
#297999=CARTESIAN_POINT('Ctrl Pts',(-6.2121333120203,118.381249999537,8.55026797822134));
#298000=CARTESIAN_POINT('Ctrl Pts',(-3.10606665601019,118.531249999536,
9.5594902125713));
#298001=CARTESIAN_POINT('Ctrl Pts',(-7.88850811043265E-14,118.681249999536,
10.5687124469213));
#298002=CARTESIAN_POINT('Ctrl Pts',(3.10606665601003,118.831249999535,9.5594902125713));
#298003=CARTESIAN_POINT('Ctrl Pts',(6.21213331202014,118.981249999535,8.55026797822134));
#298004=CARTESIAN_POINT('Ctrl Pts',(8.13178807675711,119.131249999534,5.90808986649102));
#298005=CARTESIAN_POINT('Ctrl Pts',(10.0514428414941,119.281249999533,3.2659117547607));
#298006=CARTESIAN_POINT('Ctrl Pts',(10.0514428414941,119.431249999533,-1.23094673026484E-15));
#298007=CARTESIAN_POINT('Ctrl Pts',(10.0514428414941,119.581249999532,-3.26591175476071));
#298008=CARTESIAN_POINT('Ctrl Pts',(8.13178807675711,119.731249999532,-5.90808986649102));
#298009=CARTESIAN_POINT('Ctrl Pts',(6.21213331202013,119.881249999531,-8.55026797822134));
#298010=CARTESIAN_POINT('Ctrl Pts',(3.10606665601003,120.03124999953,-9.5594902125713));
#298011=CARTESIAN_POINT('Ctrl Pts',(-8.23375237140036E-14,120.18124999953,
-10.5687124469213));
#298012=CARTESIAN_POINT('Ctrl Pts',(-3.10606665601019,120.331249999529,
-9.5594902125713));
#298013=CARTESIAN_POINT('Ctrl Pts',(-6.2121333120203,120.481249999529,-8.55026797822134));
#298014=CARTESIAN_POINT('Ctrl Pts',(-8.13178807675727,120.631249999528,
-5.90808986649102));
#298015=CARTESIAN_POINT('Ctrl Pts',(-10.0514428414943,120.781249999527,
-3.2659117547607));
#298016=CARTESIAN_POINT('Ctrl Pts',(-10.0514428414943,120.931249999527,
2.46189346052968E-15));
#298017=CARTESIAN_POINT('Ctrl Pts',(-10.0514428414943,121.081249999526,
3.26591175476071));
#298018=CARTESIAN_POINT('Ctrl Pts',(-8.13178807675727,121.231249999526,
5.90808986649102));
#298019=CARTESIAN_POINT('Ctrl Pts',(-6.2121333120203,121.381249999525,8.55026797822134));
#298020=CARTESIAN_POINT('Ctrl Pts',(-3.10606665601019,121.531249999524,
9.5594902125713));
#298021=CARTESIAN_POINT('Ctrl Pts',(-8.06127903759884E-14,121.681249999524,
10.5687124469213));
#298022=CARTESIAN_POINT('Ctrl Pts',(3.10606665601003,121.831249999523,9.5594902125713));
#298023=CARTESIAN_POINT('Ctrl Pts',(6.21213331202014,121.981249999523,8.55026797822134));
#298024=CARTESIAN_POINT('Ctrl Pts',(8.13178807675711,122.131249999522,5.90808986649102));
#298025=CARTESIAN_POINT('Ctrl Pts',(10.0514428414941,122.281249999521,3.2659117547607));
#298026=CARTESIAN_POINT('Ctrl Pts',(10.0514428414941,122.431249999521,-1.23094673026484E-15));
#298027=CARTESIAN_POINT('Ctrl Pts',(10.0514428414941,122.58124999952,-3.26591175476071));
#298028=CARTESIAN_POINT('Ctrl Pts',(8.13178807675711,122.73124999952,-5.90808986649102));
#298029=CARTESIAN_POINT('Ctrl Pts',(6.21213331202013,122.881249999519,-8.55026797822134));
#298030=CARTESIAN_POINT('Ctrl Pts',(3.10606665601002,123.031249999518,-9.5594902125713));
#298031=CARTESIAN_POINT('Ctrl Pts',(-8.40652329856655E-14,123.181249999518,
-10.5687124469213));
#298032=CARTESIAN_POINT('Ctrl Pts',(-3.10606665601019,123.331249999517,
-9.5594902125713));
#298033=CARTESIAN_POINT('Ctrl Pts',(-6.2121333120203,123.481249999517,-8.55026797822134));
#298034=CARTESIAN_POINT('Ctrl Pts',(-8.13178807675727,123.631249999516,
-5.90808986649102));
#298035=CARTESIAN_POINT('Ctrl Pts',(-10.0514428414943,123.781249999515,
-3.2659117547607));
#298036=CARTESIAN_POINT('Ctrl Pts',(-10.0514428414943,123.931249999515,
2.46189346052968E-15));
#298037=CARTESIAN_POINT('Ctrl Pts',(-10.0514428414943,124.081249999514,
3.26591175476071));
#298038=CARTESIAN_POINT('Ctrl Pts',(-8.13178807675727,124.231249999514,
5.90808986649102));
#298039=CARTESIAN_POINT('Ctrl Pts',(-6.2121333120203,124.381249999513,8.55026797822134));
#298040=CARTESIAN_POINT('Ctrl Pts',(-3.10606665601019,124.531249999512,
9.5594902125713));
#298041=CARTESIAN_POINT('Ctrl Pts',(-8.23404996476502E-14,124.681249999512,
10.5687124469213));
#298042=CARTESIAN_POINT('Ctrl Pts',(3.10606665601002,124.831249999511,9.5594902125713));
#298043=CARTESIAN_POINT('Ctrl Pts',(6.21213331202013,124.981249999511,8.55026797822134));
#298044=CARTESIAN_POINT('Ctrl Pts',(8.13178807675711,125.13124999951,5.90808986649102));
#298045=CARTESIAN_POINT('Ctrl Pts',(10.0514428414941,125.281249999509,3.2659117547607));
#298046=CARTESIAN_POINT('Ctrl Pts',(10.0514428414941,125.431249999509,-1.23094673026484E-15));
#298047=CARTESIAN_POINT('Ctrl Pts',(10.0514428414941,125.581249999508,-3.26591175476071));
#298048=CARTESIAN_POINT('Ctrl Pts',(8.13178807675711,125.731249999508,-5.90808986649102));
#298049=CARTESIAN_POINT('Ctrl Pts',(6.21213331202013,125.881249999507,-8.55026797822134));
#298050=CARTESIAN_POINT('Ctrl Pts',(3.10606665601002,126.031249999506,-9.5594902125713));
#298051=CARTESIAN_POINT('Ctrl Pts',(-8.57929422573273E-14,126.181249999506,
-10.5687124469213));
#298052=CARTESIAN_POINT('Ctrl Pts',(-3.10606665601019,126.331249999505,
-9.5594902125713));
#298053=CARTESIAN_POINT('Ctrl Pts',(-6.2121333120203,126.481249999505,-8.55026797822134));
#298054=CARTESIAN_POINT('Ctrl Pts',(-8.13178807675728,126.631249999504,
-5.90808986649102));
#298055=CARTESIAN_POINT('Ctrl Pts',(-10.0514428414943,126.781249999503,
-3.2659117547607));
#298056=CARTESIAN_POINT('Ctrl Pts',(-10.0514428414943,126.931249999503,
2.46189346052968E-15));
#298057=CARTESIAN_POINT('Ctrl Pts',(-10.0514428414943,127.081249999502,
3.26591175476071));
#298058=CARTESIAN_POINT('Ctrl Pts',(-8.13178807675728,127.231249999502,
5.90808986649102));
#298059=CARTESIAN_POINT('Ctrl Pts',(-6.2121333120203,127.381249999501,8.55026797822134));
#298060=CARTESIAN_POINT('Ctrl Pts',(-3.10606665601019,127.5312499995,9.5594902125713));
#298061=CARTESIAN_POINT('Ctrl Pts',(-8.4068208919312E-14,127.6812499995,
10.5687124469213));
#298062=CARTESIAN_POINT('Ctrl Pts',(3.10606665601002,127.831249999499,9.5594902125713));
#298063=CARTESIAN_POINT('Ctrl Pts',(6.21213331202013,127.981249999499,8.55026797822134));
#298064=CARTESIAN_POINT('Ctrl Pts',(8.1317880767571,128.131249999498,5.90808986649102));
#298065=CARTESIAN_POINT('Ctrl Pts',(10.0514428414941,128.281249999497,3.2659117547607));
#298066=CARTESIAN_POINT('Ctrl Pts',(10.0514428414941,128.431249999497,-1.23094673026484E-15));
#298067=CARTESIAN_POINT('Ctrl Pts',(10.0514428414941,128.581249999496,-3.26591175476071));
#298068=CARTESIAN_POINT('Ctrl Pts',(8.1317880767571,128.731249999496,-5.90808986649102));
#298069=CARTESIAN_POINT('Ctrl Pts',(6.21213331202013,128.881249999495,-8.55026797822134));
#298070=CARTESIAN_POINT('Ctrl Pts',(3.10606665601002,129.031249999494,-9.5594902125713));
#298071=CARTESIAN_POINT('Ctrl Pts',(-8.75206515289892E-14,129.181249999494,
-10.5687124469213));
#298072=CARTESIAN_POINT('Ctrl Pts',(-3.1060666560102,129.331249999493,-9.5594902125713));
#298073=CARTESIAN_POINT('Ctrl Pts',(-6.2121333120203,129.481249999493,-8.55026797822134));
#298074=CARTESIAN_POINT('Ctrl Pts',(-8.13178807675728,129.631249999492,
-5.90808986649102));
#298075=CARTESIAN_POINT('Ctrl Pts',(-10.0514428414943,129.781249999491,
-3.2659117547607));
#298076=CARTESIAN_POINT('Ctrl Pts',(-10.0514428414943,129.931249999491,
2.46189346052968E-15));
#298077=CARTESIAN_POINT('Ctrl Pts',(-10.0514428414943,130.08124999949,3.26591175476071));
#298078=CARTESIAN_POINT('Ctrl Pts',(-8.13178807675728,130.23124999949,5.90808986649102));
#298079=CARTESIAN_POINT('Ctrl Pts',(-6.2121333120203,130.381249999489,8.55026797822134));
#298080=CARTESIAN_POINT('Ctrl Pts',(-3.10606665601019,130.531249999488,
9.5594902125713));
#298081=CARTESIAN_POINT('Ctrl Pts',(-8.57959181909739E-14,130.681249999488,
10.5687124469213));
#298082=CARTESIAN_POINT('Ctrl Pts',(3.10606665601002,130.831249999487,9.5594902125713));
#298083=CARTESIAN_POINT('Ctrl Pts',(6.21213331202013,130.981249999487,8.55026797822134));
#298084=CARTESIAN_POINT('Ctrl Pts',(8.1317880767571,131.131249999486,5.90808986649102));
#298085=CARTESIAN_POINT('Ctrl Pts',(10.0514428414941,131.281249999485,3.2659117547607));
#298086=CARTESIAN_POINT('Ctrl Pts',(10.0514428414941,131.431249999485,-1.23094673026484E-15));
#298087=CARTESIAN_POINT('Ctrl Pts',(10.0514428414941,131.581249999484,-3.26591175476071));
#298088=CARTESIAN_POINT('Ctrl Pts',(8.1317880767571,131.731249999484,-5.90808986649102));
#298089=CARTESIAN_POINT('Ctrl Pts',(6.21213331202012,131.881249999483,-8.55026797822134));
#298090=CARTESIAN_POINT('Ctrl Pts',(3.10606665601002,132.031249999482,-9.5594902125713));
#298091=CARTESIAN_POINT('Ctrl Pts',(-8.9248360800651E-14,132.181249999482,
-10.5687124469213));
#298092=CARTESIAN_POINT('Ctrl Pts',(-3.1060666560102,132.331249999481,-9.5594902125713));
#298093=CARTESIAN_POINT('Ctrl Pts',(-6.2121333120203,132.48124999948,-8.55026797822134));
#298094=CARTESIAN_POINT('Ctrl Pts',(-8.13178807675728,132.63124999948,-5.90808986649102));
#298095=CARTESIAN_POINT('Ctrl Pts',(-10.0514428414943,132.781249999479,
-3.2659117547607));
#298096=CARTESIAN_POINT('Ctrl Pts',(-10.0514428414943,132.931249999479,
2.46189346052968E-15));
#298097=CARTESIAN_POINT('Ctrl Pts',(-10.0514428414943,133.081249999478,
3.26591175476071));
#298098=CARTESIAN_POINT('Ctrl Pts',(-8.13178807675728,133.231249999478,
5.90808986649102));
#298099=CARTESIAN_POINT('Ctrl Pts',(-6.2121333120203,133.381249999477,8.55026797822134));
#298100=CARTESIAN_POINT('Ctrl Pts',(-3.1060666560102,133.531249999476,9.5594902125713));
#298101=CARTESIAN_POINT('Ctrl Pts',(-8.75236274626357E-14,133.681249999476,
10.5687124469213));
#298102=CARTESIAN_POINT('Ctrl Pts',(3.10606665601002,133.831249999475,9.5594902125713));
#298103=CARTESIAN_POINT('Ctrl Pts',(6.21213331202013,133.981249999475,8.55026797822134));
#298104=CARTESIAN_POINT('Ctrl Pts',(8.1317880767571,134.131249999474,5.90808986649102));
#298105=CARTESIAN_POINT('Ctrl Pts',(10.0514428414941,134.281249999473,3.2659117547607));
#298106=CARTESIAN_POINT('Ctrl Pts',(10.0514428414941,134.431249999473,-1.23094673026484E-15));
#298107=CARTESIAN_POINT('Ctrl Pts',(10.0514428414941,134.581249999472,-3.26591175476071));
#298108=CARTESIAN_POINT('Ctrl Pts',(8.1317880767571,134.731249999472,-5.90808986649102));
#298109=CARTESIAN_POINT('Ctrl Pts',(6.21213331202012,134.881249999471,-8.55026797822134));
#298110=CARTESIAN_POINT('Ctrl Pts',(3.10606665601002,135.03124999947,-9.5594902125713));
#298111=CARTESIAN_POINT('Ctrl Pts',(-9.09760700723128E-14,135.18124999947,
-10.5687124469213));
#298112=CARTESIAN_POINT('Ctrl Pts',(-3.1060666560102,135.331249999469,-9.5594902125713));
#298113=CARTESIAN_POINT('Ctrl Pts',(-6.21213331202031,135.481249999469,
-8.55026797822134));
#298114=CARTESIAN_POINT('Ctrl Pts',(-8.13178807675728,135.631249999468,
-5.90808986649102));
#298115=CARTESIAN_POINT('Ctrl Pts',(-10.0514428414943,135.781249999467,
-3.2659117547607));
#298116=CARTESIAN_POINT('Ctrl Pts',(-10.0514428414943,135.931249999467,
2.46189346052968E-15));
#298117=CARTESIAN_POINT('Ctrl Pts',(-10.0514428414943,136.081249999466,
3.26591175476071));
#298118=CARTESIAN_POINT('Ctrl Pts',(-8.13178807675728,136.231249999466,
5.90808986649102));
#298119=CARTESIAN_POINT('Ctrl Pts',(-6.2121333120203,136.381249999465,8.55026797822134));
#298120=CARTESIAN_POINT('Ctrl Pts',(-3.1060666560102,136.531249999464,9.5594902125713));
#298121=CARTESIAN_POINT('Ctrl Pts',(-8.92513367342975E-14,136.681249999464,
10.5687124469213));
#298122=CARTESIAN_POINT('Ctrl Pts',(3.10606665601002,136.831249999463,9.5594902125713));
#298123=CARTESIAN_POINT('Ctrl Pts',(6.21213331202012,136.981249999463,8.55026797822134));
#298124=CARTESIAN_POINT('Ctrl Pts',(8.1317880767571,137.131249999462,5.90808986649102));
#298125=CARTESIAN_POINT('Ctrl Pts',(10.0514428414941,137.281249999461,3.2659117547607));
#298126=CARTESIAN_POINT('Ctrl Pts',(10.0514428414941,137.431249999461,-1.23094673026484E-15));
#298127=CARTESIAN_POINT('Ctrl Pts',(10.0514428414941,137.58124999946,-3.26591175476071));
#298128=CARTESIAN_POINT('Ctrl Pts',(8.1317880767571,137.73124999946,-5.90808986649102));
#298129=CARTESIAN_POINT('Ctrl Pts',(6.21213331202012,137.881249999459,-8.55026797822134));
#298130=CARTESIAN_POINT('Ctrl Pts',(3.10606665601002,138.031249999458,-9.5594902125713));
#298131=CARTESIAN_POINT('Ctrl Pts',(-9.27037793439746E-14,138.181249999458,
-10.5687124469213));
#298132=CARTESIAN_POINT('Ctrl Pts',(-3.1060666560102,138.331249999457,-9.5594902125713));
#298133=CARTESIAN_POINT('Ctrl Pts',(-6.21213331202031,138.481249999456,
-8.55026797822134));
#298134=CARTESIAN_POINT('Ctrl Pts',(-8.13178807675728,138.631249999456,
-5.90808986649102));
#298135=CARTESIAN_POINT('Ctrl Pts',(-10.0514428414943,138.781249999455,
-3.2659117547607));
#298136=CARTESIAN_POINT('Ctrl Pts',(-10.0514428414943,138.931249999455,
2.46189346052968E-15));
#298137=CARTESIAN_POINT('Ctrl Pts',(-10.0514428414943,139.081249999454,
3.26591175476071));
#298138=CARTESIAN_POINT('Ctrl Pts',(-8.13178807675728,139.231249999454,
5.90808986649102));
#298139=CARTESIAN_POINT('Ctrl Pts',(-6.21213331202031,139.381249999453,
8.55026797822134));
#298140=CARTESIAN_POINT('Ctrl Pts',(-3.1060666560102,139.531249999452,9.5594902125713));
#298141=CARTESIAN_POINT('Ctrl Pts',(-9.09790460059594E-14,139.681249999452,
10.5687124469213));
#298142=CARTESIAN_POINT('Ctrl Pts',(3.10606665601002,139.831249999451,9.5594902125713));
#298143=CARTESIAN_POINT('Ctrl Pts',(6.21213331202012,139.981249999451,8.55026797822134));
#298144=CARTESIAN_POINT('Ctrl Pts',(8.1317880767571,140.13124999945,5.90808986649102));
#298145=CARTESIAN_POINT('Ctrl Pts',(10.0514428414941,140.281249999449,3.2659117547607));
#298146=CARTESIAN_POINT('Ctrl Pts',(10.0514428414941,140.431249999449,-1.23094673026484E-15));
#298147=CARTESIAN_POINT('Ctrl Pts',(10.0514428414941,140.581249999448,-3.26591175476071));
#298148=CARTESIAN_POINT('Ctrl Pts',(8.1317880767571,140.731249999448,-5.90808986649102));
#298149=CARTESIAN_POINT('Ctrl Pts',(6.21213331202012,140.881249999447,-8.55026797822134));
#298150=CARTESIAN_POINT('Ctrl Pts',(3.10606665601001,141.031249999446,-9.5594902125713));
#298151=CARTESIAN_POINT('Ctrl Pts',(-9.44314886156365E-14,141.181249999446,
-10.5687124469213));
#298152=CARTESIAN_POINT('Ctrl Pts',(-3.1060666560102,141.331249999445,-9.5594902125713));
#298153=CARTESIAN_POINT('Ctrl Pts',(-6.21213331202031,141.481249999445,
-8.55026797822134));
#298154=CARTESIAN_POINT('Ctrl Pts',(-8.13178807675729,141.631249999444,
-5.90808986649102));
#298155=CARTESIAN_POINT('Ctrl Pts',(-10.0514428414943,141.781249999443,
-3.2659117547607));
#298156=CARTESIAN_POINT('Ctrl Pts',(-10.0514428414943,141.931249999443,
2.46189346052968E-15));
#298157=CARTESIAN_POINT('Ctrl Pts',(-10.0514428414943,142.081249999442,
3.26591175476071));
#298158=CARTESIAN_POINT('Ctrl Pts',(-8.13178807675729,142.231249999442,
5.90808986649102));
#298159=CARTESIAN_POINT('Ctrl Pts',(-6.21213331202031,142.381249999441,
8.55026797822134));
#298160=CARTESIAN_POINT('Ctrl Pts',(-3.1060666560102,142.53124999944,9.5594902125713));
#298161=CARTESIAN_POINT('Ctrl Pts',(-9.27067552776212E-14,142.68124999944,
10.5687124469213));
#298162=CARTESIAN_POINT('Ctrl Pts',(3.10606665601001,142.831249999439,9.5594902125713));
#298163=CARTESIAN_POINT('Ctrl Pts',(6.21213331202012,142.981249999439,8.55026797822134));
#298164=CARTESIAN_POINT('Ctrl Pts',(8.1317880767571,143.131249999438,5.90808986649102));
#298165=CARTESIAN_POINT('Ctrl Pts',(10.0514428414941,143.281249999437,3.2659117547607));
#298166=CARTESIAN_POINT('Ctrl Pts',(10.0514428414941,143.431249999437,-1.23094673026484E-15));
#298167=CARTESIAN_POINT('Ctrl Pts',(10.0514428414941,143.581249999436,-3.26591175476071));
#298168=CARTESIAN_POINT('Ctrl Pts',(8.1317880767571,143.731249999436,-5.90808986649102));
#298169=CARTESIAN_POINT('Ctrl Pts',(6.21213331202012,143.881249999435,-8.55026797822134));
#298170=CARTESIAN_POINT('Ctrl Pts',(3.10606665601001,144.031249999434,-9.5594902125713));
#298171=CARTESIAN_POINT('Ctrl Pts',(-9.61591978872984E-14,144.181249999434,
-10.5687124469213));
#298172=CARTESIAN_POINT('Ctrl Pts',(-3.1060666560102,144.331249999433,-9.5594902125713));
#298173=CARTESIAN_POINT('Ctrl Pts',(-6.21213331202031,144.481249999432,
-8.55026797822134));
#298174=CARTESIAN_POINT('Ctrl Pts',(-8.13178807675729,144.631249999432,
-5.90808986649102));
#298175=CARTESIAN_POINT('Ctrl Pts',(-10.0514428414943,144.781249999431,
-3.2659117547607));
#298176=CARTESIAN_POINT('Ctrl Pts',(-10.0514428414943,144.931249999431,
2.46189346052968E-15));
#298177=CARTESIAN_POINT('Ctrl Pts',(-10.0514428414943,145.08124999943,3.26591175476071));
#298178=CARTESIAN_POINT('Ctrl Pts',(-8.13178807675729,145.23124999943,5.90808986649102));
#298179=CARTESIAN_POINT('Ctrl Pts',(-6.21213331202031,145.381249999429,
8.55026797822134));
#298180=CARTESIAN_POINT('Ctrl Pts',(-3.1060666560102,145.531249999428,9.5594902125713));
#298181=CARTESIAN_POINT('Ctrl Pts',(-9.44344645492831E-14,145.681249999428,
10.5687124469213));
#298182=CARTESIAN_POINT('Ctrl Pts',(3.10606665601001,145.831249999427,9.5594902125713));
#298183=CARTESIAN_POINT('Ctrl Pts',(6.21213331202012,145.981249999427,8.55026797822134));
#298184=CARTESIAN_POINT('Ctrl Pts',(8.13178807675709,146.131249999426,5.90808986649102));
#298185=CARTESIAN_POINT('Ctrl Pts',(10.0514428414941,146.281249999425,3.2659117547607));
#298186=CARTESIAN_POINT('Ctrl Pts',(10.0514428414941,146.431249999425,-1.23094673026484E-15));
#298187=CARTESIAN_POINT('Ctrl Pts',(10.0514428414941,146.581249999424,-3.26591175476071));
#298188=CARTESIAN_POINT('Ctrl Pts',(8.13178807675709,146.731249999424,-5.90808986649102));
#298189=CARTESIAN_POINT('Ctrl Pts',(6.21213331202012,146.881249999423,-8.55026797822134));
#298190=CARTESIAN_POINT('Ctrl Pts',(3.10606665601001,147.031249999422,-9.5594902125713));
#298191=CARTESIAN_POINT('Ctrl Pts',(-9.78869071589602E-14,147.181249999422,
-10.5687124469213));
#298192=CARTESIAN_POINT('Ctrl Pts',(-3.10606665601021,147.331249999421,
-9.5594902125713));
#298193=CARTESIAN_POINT('Ctrl Pts',(-6.21213331202032,147.481249999421,
-8.55026797822134));
#298194=CARTESIAN_POINT('Ctrl Pts',(-8.13178807675729,147.63124999942,-5.90808986649102));
#298195=CARTESIAN_POINT('Ctrl Pts',(-10.0514428414943,147.781249999419,
-3.2659117547607));
#298196=CARTESIAN_POINT('Ctrl Pts',(-10.0514428414943,147.931249999419,
2.46189346052968E-15));
#298197=CARTESIAN_POINT('Ctrl Pts',(-10.0514428414943,148.081249999418,
3.26591175476071));
#298198=CARTESIAN_POINT('Ctrl Pts',(-8.13178807675729,148.231249999418,
5.90808986649102));
#298199=CARTESIAN_POINT('Ctrl Pts',(-6.21213331202031,148.381249999417,
8.55026797822134));
#298200=CARTESIAN_POINT('Ctrl Pts',(-3.1060666560102,148.531249999416,9.5594902125713));
#298201=CARTESIAN_POINT('Ctrl Pts',(-9.61621738209449E-14,148.681249999416,
10.5687124469213));
#298202=CARTESIAN_POINT('Ctrl Pts',(3.10606665601001,148.831249999415,9.5594902125713));
#298203=CARTESIAN_POINT('Ctrl Pts',(6.21213331202012,148.981249999415,8.55026797822134));
#298204=CARTESIAN_POINT('Ctrl Pts',(8.13178807675709,149.131249999414,5.90808986649102));
#298205=CARTESIAN_POINT('Ctrl Pts',(10.0514428414941,149.281249999413,3.2659117547607));
#298206=CARTESIAN_POINT('Ctrl Pts',(10.0514428414941,149.431249999413,-1.23094673026484E-15));
#298207=CARTESIAN_POINT('Ctrl Pts',(10.0514428414941,149.581249999412,-3.26591175476071));
#298208=CARTESIAN_POINT('Ctrl Pts',(8.13178807675709,149.731249999412,-5.90808986649102));
#298209=CARTESIAN_POINT('Ctrl Pts',(6.21213331202012,149.881249999411,-8.55026797822134));
#298210=CARTESIAN_POINT('Ctrl Pts',(3.10606665601001,150.03124999941,-9.5594902125713));
#298211=CARTESIAN_POINT('Ctrl Pts',(-9.9614616430622E-14,150.18124999941,
-10.5687124469213));
#298212=CARTESIAN_POINT('Ctrl Pts',(-3.10606665601021,150.331249999409,
-9.5594902125713));
#298213=CARTESIAN_POINT('Ctrl Pts',(-6.21213331202032,150.481249999409,
-8.55026797822134));
#298214=CARTESIAN_POINT('Ctrl Pts',(-8.13178807675729,150.631249999408,
-5.90808986649102));
#298215=CARTESIAN_POINT('Ctrl Pts',(-10.0514428414943,150.781249999407,
-3.2659117547607));
#298216=CARTESIAN_POINT('Ctrl Pts',(-10.0514428414943,150.931249999407,
2.46189346052968E-15));
#298217=CARTESIAN_POINT('Ctrl Pts',(-10.0514428414943,151.081249999406,
3.26591175476071));
#298218=CARTESIAN_POINT('Ctrl Pts',(-8.13178807675729,151.231249999406,
5.90808986649102));
#298219=CARTESIAN_POINT('Ctrl Pts',(-6.21213331202032,151.381249999405,
8.55026797822134));
#298220=CARTESIAN_POINT('Ctrl Pts',(-3.10606665601021,151.531249999404,
9.5594902125713));
#298221=CARTESIAN_POINT('Ctrl Pts',(-9.78898830926068E-14,151.681249999404,
10.5687124469213));
#298222=CARTESIAN_POINT('Ctrl Pts',(3.10606665601001,151.831249999403,9.5594902125713));
#298223=CARTESIAN_POINT('Ctrl Pts',(6.21213331202012,151.981249999403,8.55026797822134));
#298224=CARTESIAN_POINT('Ctrl Pts',(8.13178807675709,152.131249999402,5.90808986649102));
#298225=CARTESIAN_POINT('Ctrl Pts',(10.0514428414941,152.281249999401,3.2659117547607));
#298226=CARTESIAN_POINT('Ctrl Pts',(10.0514428414941,152.431249999401,-1.23094673026484E-15));
#298227=CARTESIAN_POINT('Ctrl Pts',(10.0514428414941,152.5812499994,-3.26591175476071));
#298228=CARTESIAN_POINT('Ctrl Pts',(8.13178807675709,152.7312499994,-5.90808986649102));
#298229=CARTESIAN_POINT('Ctrl Pts',(6.21213331202012,152.881249999399,-8.55026797822134));
#298230=CARTESIAN_POINT('Ctrl Pts',(3.10606665601001,153.031249999398,-9.5594902125713));
#298231=CARTESIAN_POINT('Ctrl Pts',(-1.01342325702284E-13,153.181249999398,
-10.5687124469213));
#298232=CARTESIAN_POINT('Ctrl Pts',(-3.10606665601021,153.331249999397,
-9.5594902125713));
#298233=CARTESIAN_POINT('Ctrl Pts',(11.6184932898974,91.186,3.00176842421395));
#298234=CARTESIAN_POINT('Ctrl Pts',(11.2700427515582,91.186,4.04399430707808));
#298235=CARTESIAN_POINT('Ctrl Pts',(10.7791667820617,91.185999999732,5.03296359596024));
#298236=CARTESIAN_POINT('Ctrl Pts',(9.52052428043545,91.185999999732,6.8774807324221));
#298237=CARTESIAN_POINT('Ctrl Pts',(8.77953392736288,91.185999997219,7.68371450615621));
#298238=CARTESIAN_POINT('Ctrl Pts',(7.39526332234894,91.185999997219,8.81855324040878));
#298239=CARTESIAN_POINT('Ctrl Pts',(6.81132012907742,91.186,9.21313481182541));
#298240=CARTESIAN_POINT('Ctrl Pts',(5.05918236890942,91.186,10.1743250327452));
#298241=CARTESIAN_POINT('Ctrl Pts',(3.67332182531712,91.186,10.6827925701586));
#298242=CARTESIAN_POINT('Ctrl Pts',(0.735795623987487,91.186,11.0280650073144));
#298243=CARTESIAN_POINT('Ctrl Pts',(-0.652494305311852,91.186,10.9270735304368));
#298244=CARTESIAN_POINT('Ctrl Pts',(-2.97093150664768,91.186,10.3045254405431));
#298245=CARTESIAN_POINT('Ctrl Pts',(-4.34343559193747,91.1860000000001,
9.79240651982437));
#298246=CARTESIAN_POINT('Ctrl Pts',(-6.33964933794428,91.1860000000001,
8.2393064142999));
#298247=CARTESIAN_POINT('Ctrl Pts',(-6.89998590554459,91.186,7.69134457042996));
#298248=CARTESIAN_POINT('Ctrl Pts',(-7.82072333918513,91.186,6.5609072669913));
#298249=CARTESIAN_POINT('Ctrl Pts',(-8.27453946661952,91.186,5.90162129296699));
#298250=CARTESIAN_POINT('Ctrl Pts',(-8.66397270809382,91.186,5.09579043026947));
#298251=CARTESIAN_POINT('Ctrl Pts',(10.0514428414941,128.431249999497,-1.23094673026484E-15));
#298252=CARTESIAN_POINT('Ctrl Pts',(10.0514428414941,128.581249999496,-3.26591175476071));
#298253=CARTESIAN_POINT('Ctrl Pts',(8.1317880767571,128.731249999496,-5.90808986649102));
#298254=CARTESIAN_POINT('Ctrl Pts',(6.21213331202013,128.881249999495,-8.55026797822134));
#298255=CARTESIAN_POINT('Ctrl Pts',(3.10606665601002,129.031249999494,-9.5594902125713));
#298256=CARTESIAN_POINT('Ctrl Pts',(-8.75206515289892E-14,129.181249999494,
-10.5687124469213));
#298257=CARTESIAN_POINT('Ctrl Pts',(-3.1060666560102,129.331249999493,-9.5594902125713));
#298258=CARTESIAN_POINT('Ctrl Pts',(-6.2121333120203,129.481249999493,-8.55026797822134));
#298259=CARTESIAN_POINT('Ctrl Pts',(-8.13178807675728,129.631249999492,
-5.90808986649102));
#298260=CARTESIAN_POINT('Ctrl Pts',(-10.0514428414943,129.781249999491,
-3.2659117547607));
#298261=CARTESIAN_POINT('Ctrl Pts',(-10.0514428414943,129.931249999491,
2.46189346052968E-15));
#298262=CARTESIAN_POINT('Ctrl Pts',(-10.0514428414943,130.08124999949,3.26591175476071));
#298263=CARTESIAN_POINT('Ctrl Pts',(-8.13178807675728,130.23124999949,5.90808986649102));
#298264=CARTESIAN_POINT('Ctrl Pts',(-6.2121333120203,130.381249999489,8.55026797822134));
#298265=CARTESIAN_POINT('Ctrl Pts',(-3.10606665601019,130.531249999488,
9.5594902125713));
#298266=CARTESIAN_POINT('Ctrl Pts',(-0.158086395373697,130.673615598191,
10.5173470633579));
#298267=CARTESIAN_POINT('Ctrl Pts',(2.81735069959344,130.817307158506,9.64852518426128));
#298268=CARTESIAN_POINT('Origin',(-3.77475828372553E-14,-1.881249999982,
2.68644078414671E-15));
#298269=CARTESIAN_POINT('Origin',(-8.79029313101884E-14,130.96875,0.));
#298270=CARTESIAN_POINT('Origin',(0.,91.186,0.));
#298271=CARTESIAN_POINT('',(24.9999999999999,91.186,30.));
#298272=CARTESIAN_POINT('',(24.9999999999999,91.186,-30.));
#298273=CARTESIAN_POINT('',(24.9999999999999,91.186,30.));
#298274=CARTESIAN_POINT('',(-25.0000000000001,91.186,-30.));
#298275=CARTESIAN_POINT('',(-25.0000000000001,91.186,-30.));
#298276=CARTESIAN_POINT('',(-25.0000000000001,91.186,30.));
#298277=CARTESIAN_POINT('',(-25.0000000000001,91.186,30.));
#298278=CARTESIAN_POINT('',(-25.0000000000001,91.186,30.));
#298279=CARTESIAN_POINT('Origin',(0.,76.2,0.));
#298280=CARTESIAN_POINT('',(24.9999999999999,76.2,30.));
#298281=CARTESIAN_POINT('',(24.9999999999999,76.2,-30.));
#298282=CARTESIAN_POINT('',(24.9999999999999,76.2,30.));
#298283=CARTESIAN_POINT('',(-25.0000000000001,76.2,30.));
#298284=CARTESIAN_POINT('',(-25.0000000000001,76.2,30.));
#298285=CARTESIAN_POINT('',(-25.0000000000001,76.2,-30.));
#298286=CARTESIAN_POINT('',(-25.0000000000001,76.2,30.));
#298287=CARTESIAN_POINT('',(-25.0000000000001,76.2,-30.));
#298288=CARTESIAN_POINT('',(-15.58845726812,76.2,9.00000000000004));
#298289=CARTESIAN_POINT('',(-1.78703160926406E-13,76.2,18.));
#298290=CARTESIAN_POINT('Origin',(-1.78703160926406E-13,76.2,6.74376190435982E-14));
#298291=CARTESIAN_POINT('',(15.5884572681197,76.2,9.00000000000003));
#298292=CARTESIAN_POINT('Origin',(-1.78703160926406E-13,76.2,2.60289135494012E-29));
#298293=CARTESIAN_POINT('',(15.5884572681198,76.2,-9.00000000000011));
#298294=CARTESIAN_POINT('Origin',(-1.78703160926406E-13,76.2,6.74376190435982E-14));
#298295=CARTESIAN_POINT('',(-1.78703160926406E-13,76.2,-18.0000000000001));
#298296=CARTESIAN_POINT('Origin',(-1.78703160926406E-13,76.2,6.74376190435982E-14));
#298297=CARTESIAN_POINT('',(-15.5884572681201,76.2,-8.99999999999997));
#298298=CARTESIAN_POINT('Origin',(-1.78703160926406E-13,76.2,6.74376190435982E-14));
#298299=CARTESIAN_POINT('Origin',(-1.78703160926406E-13,76.2,6.74376190435982E-14));
#298300=CARTESIAN_POINT('Origin',(24.9999999999999,91.186,30.));
#298301=CARTESIAN_POINT('',(24.9999999999999,91.186,-30.));
#298302=CARTESIAN_POINT('',(24.9999999999999,91.186,30.));
#298303=CARTESIAN_POINT('Origin',(-25.0000000000001,91.186,-30.));
#298304=CARTESIAN_POINT('',(-25.0000000000001,91.186,-30.));
#298305=CARTESIAN_POINT('Origin',(-25.0000000000001,91.186,30.));
#298306=CARTESIAN_POINT('',(-25.0000000000001,91.186,30.));
#298307=CARTESIAN_POINT('Origin',(-25.0000000000001,91.186,30.));
#298308=CARTESIAN_POINT('Origin',(10.3923048454132,57.2,18.));
#298309=CARTESIAN_POINT('',(20.7846096908265,58.8076951545868,-8.45698818236971E-15));
#298310=CARTESIAN_POINT('',(20.7846096908265,74.5923048454133,-9.10794141489568E-15));
#298311=CARTESIAN_POINT('',(20.7846096908265,57.2,-9.10794141489568E-15));
#298312=CARTESIAN_POINT('Ctrl Pts',(20.7846096908597,74.5923048453941,-5.76297439360145E-11));
#298313=CARTESIAN_POINT('Ctrl Pts',(18.0000000000132,76.2,4.82308546373715));
#298314=CARTESIAN_POINT('Ctrl Pts',(15.5884572681197,76.2,9.00000000000019));
#298315=CARTESIAN_POINT('',(10.3923048454132,74.5923048454133,18.));
#298316=CARTESIAN_POINT('Ctrl Pts',(15.5884572681197,76.2,9.00000000000019));
#298317=CARTESIAN_POINT('Ctrl Pts',(13.1769145362263,76.2,13.1769145362631));
#298318=CARTESIAN_POINT('Ctrl Pts',(10.3923048453799,74.592304845394,18.0000000000577));
#298319=CARTESIAN_POINT('',(10.3923048454132,58.8076951545868,18.));
#298320=CARTESIAN_POINT('',(10.3923048454132,57.2,18.));
#298321=CARTESIAN_POINT('',(15.5884572681197,57.2,9.00000000000005));
#298322=CARTESIAN_POINT('Ctrl Pts',(15.5884572681198,57.2000000000001,9.00000000000012));
#298323=CARTESIAN_POINT('Ctrl Pts',(13.1769145362263,57.2000000000001,13.176914536263));
#298324=CARTESIAN_POINT('Ctrl Pts',(10.3923048453799,58.807695154606,18.0000000000576));
#298325=CARTESIAN_POINT('Ctrl Pts',(20.7846096908597,58.807695154606,-5.75819548439033E-11));
#298326=CARTESIAN_POINT('Ctrl Pts',(18.0000000000133,57.2000000000001,4.82308546373711));
#298327=CARTESIAN_POINT('Ctrl Pts',(15.5884572681198,57.2000000000001,9.0000000000001));
#298328=CARTESIAN_POINT('Origin',(-10.3923048454133,57.2,18.));
#298329=CARTESIAN_POINT('Ctrl Pts',(10.3923048454797,74.5923048453941,18.));
#298330=CARTESIAN_POINT('Ctrl Pts',(4.82308546378683,76.2,18.));
#298331=CARTESIAN_POINT('Ctrl Pts',(-1.71095103011815E-13,76.2,18.));
#298332=CARTESIAN_POINT('',(-10.3923048454133,74.5923048454133,18.));
#298333=CARTESIAN_POINT('Ctrl Pts',(-1.41221354866895E-13,76.2,18.));
#298334=CARTESIAN_POINT('Ctrl Pts',(-4.82308546378711,76.2,18.));
#298335=CARTESIAN_POINT('Ctrl Pts',(-10.39230484548,74.5923048453941,18.));
#298336=CARTESIAN_POINT('',(-10.3923048454133,58.8076951545867,18.));
#298337=CARTESIAN_POINT('',(-10.3923048454133,57.2,18.));
#298338=CARTESIAN_POINT('',(-1.37604970778725E-13,57.2,18.));
#298339=CARTESIAN_POINT('Ctrl Pts',(-1.34884499199791E-13,57.2,18.));
#298340=CARTESIAN_POINT('Ctrl Pts',(-4.82308546378705,57.2,18.));
#298341=CARTESIAN_POINT('Ctrl Pts',(-10.3923048454799,58.8076951546059,
18.));
#298342=CARTESIAN_POINT('Ctrl Pts',(10.3923048454797,58.807695154606,18.));
#298343=CARTESIAN_POINT('Ctrl Pts',(4.82308546378685,57.2,18.));
#298344=CARTESIAN_POINT('Ctrl Pts',(-1.27642378437386E-13,57.2,18.));
#298345=CARTESIAN_POINT('Origin',(-20.7846096908266,57.2,-3.51753081198983E-15));
#298346=CARTESIAN_POINT('Ctrl Pts',(-10.3923048453801,74.5923048453941,
18.0000000000576));
#298347=CARTESIAN_POINT('Ctrl Pts',(-13.1769145362265,76.2,13.1769145362629));
#298348=CARTESIAN_POINT('Ctrl Pts',(-15.58845726812,76.2,8.99999999999997));
#298349=CARTESIAN_POINT('',(-20.7846096908266,74.5923048454133,-3.06716835895631E-15));
#298350=CARTESIAN_POINT('Ctrl Pts',(-15.5884572681199,76.2000000000001,
9.00000000000014));
#298351=CARTESIAN_POINT('Ctrl Pts',(-18.0000000000134,76.2000000000001,
4.82308546373712));
#298352=CARTESIAN_POINT('Ctrl Pts',(-20.7846096908599,74.5923048453941,
-5.76355956615787E-11));
#298353=CARTESIAN_POINT('',(-20.7846096908266,58.8076951545866,-4.94143077032127E-15));
#298354=CARTESIAN_POINT('',(-20.7846096908266,57.2,-3.51753081198983E-15));
#298355=CARTESIAN_POINT('',(-15.58845726812,57.2,9.00000000000005));
#298356=CARTESIAN_POINT('Ctrl Pts',(-15.5884572681199,57.1999999999999,
9.00000000000004));
#298357=CARTESIAN_POINT('Ctrl Pts',(-18.0000000000134,57.1999999999999,
4.82308546373706));
#298358=CARTESIAN_POINT('Ctrl Pts',(-20.7846096908598,58.8076951546058,
-5.76404720995493E-11));
#298359=CARTESIAN_POINT('Ctrl Pts',(-10.39230484538,58.8076951546059,18.0000000000577));
#298360=CARTESIAN_POINT('Ctrl Pts',(-13.1769145362264,57.1999999999999,
13.176914536263));
#298361=CARTESIAN_POINT('Ctrl Pts',(-15.5884572681199,57.1999999999999,
9.00000000000004));
#298362=CARTESIAN_POINT('Origin',(-10.3923048454133,57.2,-18.));
#298363=CARTESIAN_POINT('Ctrl Pts',(-20.7846096908599,74.5923048453941,
5.76073123213497E-11));
#298364=CARTESIAN_POINT('Ctrl Pts',(-18.0000000000135,76.2,-4.823085463737));
#298365=CARTESIAN_POINT('Ctrl Pts',(-15.58845726812,76.2,-8.99999999999991));
#298366=CARTESIAN_POINT('',(-10.3923048454133,74.5923048454133,-18.));
#298367=CARTESIAN_POINT('Ctrl Pts',(-15.58845726812,76.2,-8.9999999999999));
#298368=CARTESIAN_POINT('Ctrl Pts',(-13.1769145362265,76.2000000000001,
-13.1769145362629));
#298369=CARTESIAN_POINT('Ctrl Pts',(-10.3923048453801,74.5923048453941,
-18.0000000000576));
#298370=CARTESIAN_POINT('',(-10.3923048454133,58.8076951545867,-18.));
#298371=CARTESIAN_POINT('',(-10.3923048454133,57.2,-18.));
#298372=CARTESIAN_POINT('',(-15.5884572681201,57.2,-8.99999999999995));
#298373=CARTESIAN_POINT('Ctrl Pts',(-15.58845726812,57.1999999999999,-8.99999999999989));
#298374=CARTESIAN_POINT('Ctrl Pts',(-13.1769145362265,57.1999999999999,
-13.1769145362629));
#298375=CARTESIAN_POINT('Ctrl Pts',(-10.39230484538,58.8076951546059,-18.0000000000576));
#298376=CARTESIAN_POINT('Ctrl Pts',(-20.7846096908598,58.8076951546058,
5.75917077198438E-11));
#298377=CARTESIAN_POINT('Ctrl Pts',(-18.0000000000135,57.1999999999999,
-4.82308546373701));
#298378=CARTESIAN_POINT('Ctrl Pts',(-15.58845726812,57.1999999999999,-8.99999999999989));
#298379=CARTESIAN_POINT('Origin',(10.3923048454132,57.2,-18.));
#298380=CARTESIAN_POINT('Ctrl Pts',(-10.3923048454799,74.5923048453941,
-18.));
#298381=CARTESIAN_POINT('Ctrl Pts',(-4.82308546378714,76.2,-18.));
#298382=CARTESIAN_POINT('Ctrl Pts',(-2.77011119161987E-13,76.2,-18.));
#298383=CARTESIAN_POINT('',(10.3923048454132,74.5923048454133,-18.));
#298384=CARTESIAN_POINT('Ctrl Pts',(-9.95791604830673E-14,76.2,-18.));
#298385=CARTESIAN_POINT('Ctrl Pts',(4.82308546378685,76.2,-18.));
#298386=CARTESIAN_POINT('Ctrl Pts',(10.3923048454797,74.5923048453941,-18.));
#298387=CARTESIAN_POINT('',(10.3923048454132,58.8076951545868,-18.));
#298388=CARTESIAN_POINT('',(10.3923048454132,57.2,-18.));
#298389=CARTESIAN_POINT('',(-1.406095999762E-13,57.2,-18.));
#298390=CARTESIAN_POINT('Ctrl Pts',(-1.37600294485693E-13,57.2,-18.));
#298391=CARTESIAN_POINT('Ctrl Pts',(4.82308546378685,57.2,-18.));
#298392=CARTESIAN_POINT('Ctrl Pts',(10.3923048454797,58.807695154606,-18.));
#298393=CARTESIAN_POINT('Ctrl Pts',(-10.3923048454799,58.8076951546059,
-18.));
#298394=CARTESIAN_POINT('Ctrl Pts',(-4.82308546378706,57.2,-18.));
#298395=CARTESIAN_POINT('Ctrl Pts',(-1.54800331296405E-13,57.2,-18.));
#298396=CARTESIAN_POINT('Origin',(20.7846096908265,57.2,-9.10794141489568E-15));
#298397=CARTESIAN_POINT('Ctrl Pts',(10.3923048453799,74.5923048453941,-18.0000000000576));
#298398=CARTESIAN_POINT('Ctrl Pts',(13.1769145362263,76.2,-13.176914536263));
#298399=CARTESIAN_POINT('Ctrl Pts',(15.5884572681198,76.2,-9.00000000000015));
#298400=CARTESIAN_POINT('Ctrl Pts',(15.5884572681198,76.2,-9.00000000000015));
#298401=CARTESIAN_POINT('Ctrl Pts',(18.0000000000133,76.2,-4.82308546373714));
#298402=CARTESIAN_POINT('Ctrl Pts',(20.7846096908597,74.592304845394,5.7606337033756E-11));
#298403=CARTESIAN_POINT('',(15.5884572681199,57.2,-8.99999999999999));
#298404=CARTESIAN_POINT('Ctrl Pts',(15.5884572681199,57.2000000000001,-8.99999999999997));
#298405=CARTESIAN_POINT('Ctrl Pts',(18.0000000000133,57.2000000000001,-4.82308546373704));
#298406=CARTESIAN_POINT('Ctrl Pts',(20.7846096908597,58.807695154606,5.76160899096971E-11));
#298407=CARTESIAN_POINT('Ctrl Pts',(10.3923048453799,58.807695154606,-18.0000000000576));
#298408=CARTESIAN_POINT('Ctrl Pts',(13.1769145362264,57.2000000000001,-13.176914536263));
#298409=CARTESIAN_POINT('Ctrl Pts',(15.5884572681199,57.2000000000001,-8.99999999999999));
#298410=CARTESIAN_POINT('Origin',(4.24836511114714E-14,57.2,0.));
#298411=CARTESIAN_POINT('Origin',(-1.37604970778725E-13,57.2,1.95387645016502E-29));
#298412=CARTESIAN_POINT('Origin',(-1.37604970778725E-13,57.2,6.74376190435982E-14));
#298413=CARTESIAN_POINT('Origin',(-1.37604970778725E-13,57.2,6.74376190435982E-14));
#298414=CARTESIAN_POINT('Origin',(-1.37604970778725E-13,57.2,6.74376190435982E-14));
#298415=CARTESIAN_POINT('Origin',(-1.37604970778725E-13,57.2,6.74376190435982E-14));
#298416=CARTESIAN_POINT('Origin',(-1.37604970778725E-13,57.2,6.74376190435982E-14));
#298417=CARTESIAN_POINT('Origin',(-1.37604970778725E-13,57.2,1.95387645016502E-29));
#298418=CARTESIAN_POINT('Origin',(-1.37604970778725E-13,57.2,1.95387645016502E-29));
#298419=CARTESIAN_POINT('Origin',(-1.37604970778725E-13,57.2,1.95387645016502E-29));
#298420=CARTESIAN_POINT('Origin',(-1.37604970778725E-13,57.2,1.95387645016502E-29));
#298421=CARTESIAN_POINT('Origin',(-1.37604970778725E-13,57.2,1.95387645016502E-29));
#298422=CARTESIAN_POINT('Origin',(-1.37604970778725E-13,57.2,1.95387645016502E-29));
#298423=CARTESIAN_POINT('Origin',(-1.78703160926406E-13,76.2,2.60289135494012E-29));
#298424=CARTESIAN_POINT('Origin',(-1.78703160926406E-13,76.2,2.60289135494012E-29));
#298425=CARTESIAN_POINT('Origin',(-1.78703160926406E-13,76.2,2.60289135494012E-29));
#298426=CARTESIAN_POINT('Origin',(-1.78703160926406E-13,76.2,2.60289135494012E-29));
#298427=CARTESIAN_POINT('Origin',(-1.78703160926406E-13,76.2,2.60289135494012E-29));
#298428=CARTESIAN_POINT('Origin',(-1.78703160926406E-13,76.2,2.60289135494012E-29));
#298429=CARTESIAN_POINT('Origin',(-1.38777878078145E-14,2.43125000000001,
0.));
#298430=CARTESIAN_POINT('Ctrl Pts',(-12.,2.43125000000001,1.10592091040473E-12));
#298431=CARTESIAN_POINT('Ctrl Pts',(-11.8804643241478,2.43125000000001,
1.79391945396996));
#298432=CARTESIAN_POINT('Ctrl Pts',(-11.3990610613138,2.43125000000001,
3.13396898737023));
#298433=CARTESIAN_POINT('Ctrl Pts',(-10.4104157884427,2.43125000000001,
5.318570795906));
#298434=CARTESIAN_POINT('Ctrl Pts',(-9.57359601299618,2.43125000000001,
6.56829747585552));
#298435=CARTESIAN_POINT('Ctrl Pts',(-7.38873844522587,2.43125000000001,
8.65742934749614));
#298436=CARTESIAN_POINT('Ctrl Pts',(-6.14298665404833,2.43125,9.45156675706131));
#298437=CARTESIAN_POINT('Ctrl Pts',(-3.8073824930157,2.43125,10.362657594245));
#298438=CARTESIAN_POINT('Ctrl Pts',(-2.35484140538957,2.43125000000001,
10.778449175978));
#298439=CARTESIAN_POINT('Ctrl Pts',(1.15015301169903,2.43125000000001,10.6841950237441));
#298440=CARTESIAN_POINT('Ctrl Pts',(2.53388342843634,2.43125000000001,10.2413561793839));
#298441=CARTESIAN_POINT('Ctrl Pts',(4.18319669729398,2.43125000000002,9.5097960999229));
#298442=CARTESIAN_POINT('Ctrl Pts',(4.85072362354194,2.43125000000002,9.11749903031561));
#298443=CARTESIAN_POINT('Ctrl Pts',(6.06416700972034,2.43125000000002,8.20405583130882));
#298444=CARTESIAN_POINT('Ctrl Pts',(6.60953367471901,2.43125000000002,7.69028293020246));
#298445=CARTESIAN_POINT('Ctrl Pts',(7.09357268597975,2.43125000000002,7.12128708482873));
#298446=CARTESIAN_POINT('Ctrl Pts',(10.0514428414954,2.43125000000002,1.00613961606655E-13));
#298447=CARTESIAN_POINT('Ctrl Pts',(10.1143780835885,2.43125000000002,-0.791127473640706));
#298448=CARTESIAN_POINT('Ctrl Pts',(10.0855072982437,2.43125000000002,-1.58682843497015));
#298449=CARTESIAN_POINT('Ctrl Pts',(9.84523379682252,2.43125000000002,-3.15557179232318));
#298450=CARTESIAN_POINT('Ctrl Pts',(9.63470068842676,2.43125000000002,-3.92325055631404));
#298451=CARTESIAN_POINT('Ctrl Pts',(8.67230516055593,2.43125000000002,-6.30994543448733));
#298452=CARTESIAN_POINT('Ctrl Pts',(7.71286120753459,2.43125000000002,-7.46066276667367));
#298453=CARTESIAN_POINT('Ctrl Pts',(6.06627958599162,2.43125000000002,-9.1152206243862));
#298454=CARTESIAN_POINT('Ctrl Pts',(4.9464571378071,2.43125000000001,-9.88345895797583));
#298455=CARTESIAN_POINT('Ctrl Pts',(2.75597210659317,2.43125000000001,-10.8484833593829));
#298456=CARTESIAN_POINT('Ctrl Pts',(1.37406648240357,2.43125000000002,-11.29221051564));
#298457=CARTESIAN_POINT('Ctrl Pts',(-1.98461349922251,2.43125000000001,
-11.4457083135333));
#298458=CARTESIAN_POINT('Ctrl Pts',(-3.50022085878334,2.43125000000001,
-11.1473855441023));
#298459=CARTESIAN_POINT('Ctrl Pts',(-6.14735486447011,2.43125000000001,
-10.1719281614562));
#298460=CARTESIAN_POINT('Ctrl Pts',(-7.38835529811323,2.43125000000001,
-9.4385927042382));
#298461=CARTESIAN_POINT('Ctrl Pts',(-8.46872171229246,2.43125000000001,
-8.50180878165033));
#298462=CARTESIAN_POINT('Ctrl Pts',(-10.0514428414942,-1.69374999998275,
2.46189346052968E-15));
#298463=CARTESIAN_POINT('Ctrl Pts',(-10.0514428414942,-1.54374999998335,
3.26591175476071));
#298464=CARTESIAN_POINT('Ctrl Pts',(-8.1317880767572,-1.39374999998395,
5.90808986649102));
#298465=CARTESIAN_POINT('Ctrl Pts',(-6.21213331202023,-1.24374999998455,
8.55026797822134));
#298466=CARTESIAN_POINT('Ctrl Pts',(-3.10606665601012,-1.09374999998515,
9.5594902125713));
#298467=CARTESIAN_POINT('Ctrl Pts',(-9.99267389681068E-15,-0.943749999985747,
10.5687124469213));
#298468=CARTESIAN_POINT('Ctrl Pts',(3.1060666560101,-0.793749999986346,
9.5594902125713));
#298469=CARTESIAN_POINT('Ctrl Pts',(6.21213331202021,-0.643749999986944,
8.55026797822134));
#298470=CARTESIAN_POINT('Ctrl Pts',(8.13178807675718,-0.493749999987543,
5.90808986649102));
#298471=CARTESIAN_POINT('Ctrl Pts',(10.0514428414942,-0.343749999988142,
3.2659117547607));
#298472=CARTESIAN_POINT('Ctrl Pts',(10.0514428414942,-0.193749999988742,
-1.23094673026484E-15));
#298473=CARTESIAN_POINT('Ctrl Pts',(10.0514428414942,-0.0437499999893418,
-3.26591175476071));
#298474=CARTESIAN_POINT('Ctrl Pts',(8.13178807675718,0.106250000010057,
-5.90808986649102));
#298475=CARTESIAN_POINT('Ctrl Pts',(6.2121333120202,0.256250000009456,-8.55026797822134));
#298476=CARTESIAN_POINT('Ctrl Pts',(3.10606665601009,0.406250000008854,
-9.5594902125713));
#298477=CARTESIAN_POINT('Ctrl Pts',(-1.34451165064878E-14,0.556250000008252,
-10.5687124469213));
#298478=CARTESIAN_POINT('Ctrl Pts',(-3.10606665601012,0.70625000000765,
-9.5594902125713));
#298479=CARTESIAN_POINT('Ctrl Pts',(-6.21213331202023,0.856250000007049,
-8.55026797822134));
#298480=CARTESIAN_POINT('Ctrl Pts',(-8.1317880767572,1.00625000000645,-5.90808986649102));
#298481=CARTESIAN_POINT('Ctrl Pts',(-10.0514428414942,1.15625000000585,
-3.2659117547607));
#298482=CARTESIAN_POINT('Ctrl Pts',(-10.0514428414942,1.30625000000525,
2.46189346052968E-15));
#298483=CARTESIAN_POINT('Ctrl Pts',(-10.0514428414942,1.45625000000465,
3.26591175476071));
#298484=CARTESIAN_POINT('Ctrl Pts',(-8.1317880767572,1.60625000000405,5.90808986649102));
#298485=CARTESIAN_POINT('Ctrl Pts',(-6.21213331202023,1.75625000000345,
8.55026797822134));
#298486=CARTESIAN_POINT('Ctrl Pts',(-3.10606665601012,1.90625000000285,
9.5594902125713));
#298487=CARTESIAN_POINT('Ctrl Pts',(-1.17203831684725E-14,2.05625000000225,
10.5687124469213));
#298488=CARTESIAN_POINT('Ctrl Pts',(3.1060666560101,2.20625000000165,9.5594902125713));
#298489=CARTESIAN_POINT('Ctrl Pts',(6.2121333120202,2.35625000000106,8.55026797822134));
#298490=CARTESIAN_POINT('Ctrl Pts',(8.13178807675718,2.50625000000046,5.90808986649102));
#298491=CARTESIAN_POINT('Ctrl Pts',(10.0514428414942,2.65624999999986,3.2659117547607));
#298492=CARTESIAN_POINT('Ctrl Pts',(10.0514428414942,2.80624999999926,-1.23094673026484E-15));
#298493=CARTESIAN_POINT('Ctrl Pts',(10.0514428414942,2.95624999999866,-3.26591175476071));
#298494=CARTESIAN_POINT('Ctrl Pts',(8.13178807675718,3.10624999999806,-5.90808986649102));
#298495=CARTESIAN_POINT('Ctrl Pts',(6.2121333120202,3.25624999999746,-8.55026797822134));
#298496=CARTESIAN_POINT('Ctrl Pts',(3.10606665601009,3.40624999999685,-9.5594902125713));
#298497=CARTESIAN_POINT('Ctrl Pts',(-1.51728257781496E-14,3.55624999999625,
-10.5687124469213));
#298498=CARTESIAN_POINT('Ctrl Pts',(-3.10606665601012,3.70624999999565,
-9.5594902125713));
#298499=CARTESIAN_POINT('Ctrl Pts',(-6.21213331202023,3.85624999999505,
-8.55026797822134));
#298500=CARTESIAN_POINT('Ctrl Pts',(-8.13178807675721,4.00624999999445,
-5.90808986649102));
#298501=CARTESIAN_POINT('Ctrl Pts',(-10.0514428414942,4.15624999999385,
-3.2659117547607));
#298502=CARTESIAN_POINT('Ctrl Pts',(-10.0514428414942,4.30624999999325,
2.46189346052968E-15));
#298503=CARTESIAN_POINT('Ctrl Pts',(-10.0514428414942,4.45624999999265,
3.26591175476071));
#298504=CARTESIAN_POINT('Ctrl Pts',(-8.13178807675721,4.60624999999205,
5.90808986649102));
#298505=CARTESIAN_POINT('Ctrl Pts',(-6.21213331202023,4.75624999999145,
8.55026797822134));
#298506=CARTESIAN_POINT('Ctrl Pts',(-3.10606665601012,4.90624999999085,
9.5594902125713));
#298507=CARTESIAN_POINT('Ctrl Pts',(-1.34480924401344E-14,5.05624999999025,
10.5687124469213));
#298508=CARTESIAN_POINT('Ctrl Pts',(3.10606665601009,5.20624999998966,9.5594902125713));
#298509=CARTESIAN_POINT('Ctrl Pts',(6.2121333120202,5.35624999998906,8.55026797822134));
#298510=CARTESIAN_POINT('Ctrl Pts',(8.13178807675718,5.50624999998846,5.90808986649102));
#298511=CARTESIAN_POINT('Ctrl Pts',(10.0514428414942,5.65624999998786,3.2659117547607));
#298512=CARTESIAN_POINT('Ctrl Pts',(10.0514428414941,5.80624999998726,-1.23094673026484E-15));
#298513=CARTESIAN_POINT('Ctrl Pts',(10.0514428414941,5.95624999998666,-3.26591175476071));
#298514=CARTESIAN_POINT('Ctrl Pts',(8.13178807675717,6.10624999998606,-5.90808986649102));
#298515=CARTESIAN_POINT('Ctrl Pts',(6.2121333120202,6.25624999998545,-8.55026797822134));
#298516=CARTESIAN_POINT('Ctrl Pts',(3.10606665601009,6.40624999998485,-9.5594902125713));
#298517=CARTESIAN_POINT('Ctrl Pts',(-1.69005350498115E-14,6.55624999998425,
-10.5687124469213));
#298518=CARTESIAN_POINT('Ctrl Pts',(-3.10606665601013,6.70624999998365,
-9.5594902125713));
#298519=CARTESIAN_POINT('Ctrl Pts',(-6.21213331202023,6.85624999998305,
-8.55026797822134));
#298520=CARTESIAN_POINT('Ctrl Pts',(-8.13178807675721,7.00624999998245,
-5.90808986649102));
#298521=CARTESIAN_POINT('Ctrl Pts',(-10.0514428414942,7.15624999998184,
-3.2659117547607));
#298522=CARTESIAN_POINT('Ctrl Pts',(-10.0514428414942,7.30624999998125,
2.46189346052968E-15));
#298523=CARTESIAN_POINT('Ctrl Pts',(-10.0514428414942,7.45624999998065,
3.26591175476071));
#298524=CARTESIAN_POINT('Ctrl Pts',(-8.13178807675721,7.60624999998005,
5.90808986649102));
#298525=CARTESIAN_POINT('Ctrl Pts',(-6.21213331202023,7.75624999997945,
8.55026797822134));
#298526=CARTESIAN_POINT('Ctrl Pts',(-3.10606665601012,7.90624999997885,
9.5594902125713));
#298527=CARTESIAN_POINT('Ctrl Pts',(-1.51758017117962E-14,8.05624999997825,
10.5687124469213));
#298528=CARTESIAN_POINT('Ctrl Pts',(3.10606665601009,8.20624999997765,9.5594902125713));
#298529=CARTESIAN_POINT('Ctrl Pts',(6.2121333120202,8.35624999997706,8.55026797822134));
#298530=CARTESIAN_POINT('Ctrl Pts',(8.13178807675717,8.50624999997646,5.90808986649102));
#298531=CARTESIAN_POINT('Ctrl Pts',(10.0514428414942,8.65624999997586,3.2659117547607));
#298532=CARTESIAN_POINT('Ctrl Pts',(10.0514428414941,8.80624999997526,-1.23094673026484E-15));
#298533=CARTESIAN_POINT('Ctrl Pts',(10.0514428414941,8.95624999997466,-3.26591175476071));
#298534=CARTESIAN_POINT('Ctrl Pts',(8.13178807675717,9.10624999997406,-5.90808986649102));
#298535=CARTESIAN_POINT('Ctrl Pts',(6.2121333120202,9.25624999997346,-8.55026797822134));
#298536=CARTESIAN_POINT('Ctrl Pts',(3.10606665601009,9.40624999997286,-9.5594902125713));
#298537=CARTESIAN_POINT('Ctrl Pts',(-1.86282443214733E-14,9.55624999997225,
-10.5687124469213));
#298538=CARTESIAN_POINT('Ctrl Pts',(-3.10606665601013,9.70624999997165,
-9.5594902125713));
#298539=CARTESIAN_POINT('Ctrl Pts',(-6.21213331202023,9.85624999997105,
-8.55026797822134));
#298540=CARTESIAN_POINT('Ctrl Pts',(-8.13178807675721,10.0062499999704,
-5.90808986649102));
#298541=CARTESIAN_POINT('Ctrl Pts',(-10.0514428414942,10.1562499999698,
-3.2659117547607));
#298542=CARTESIAN_POINT('Ctrl Pts',(-10.0514428414942,10.3062499999692,
2.46189346052968E-15));
#298543=CARTESIAN_POINT('Ctrl Pts',(-10.0514428414942,10.4562499999686,
3.26591175476071));
#298544=CARTESIAN_POINT('Ctrl Pts',(-8.13178807675721,10.606249999968,5.90808986649102));
#298545=CARTESIAN_POINT('Ctrl Pts',(-6.21213331202023,10.7562499999674,
8.55026797822134));
#298546=CARTESIAN_POINT('Ctrl Pts',(-3.10606665601013,10.9062499999668,
9.5594902125713));
#298547=CARTESIAN_POINT('Ctrl Pts',(-1.6903510983458E-14,11.0562499999663,
10.5687124469213));
#298548=CARTESIAN_POINT('Ctrl Pts',(3.10606665601009,11.2062499999657,9.5594902125713));
#298549=CARTESIAN_POINT('Ctrl Pts',(6.2121333120202,11.3562499999651,8.55026797822134));
#298550=CARTESIAN_POINT('Ctrl Pts',(8.13178807675717,11.5062499999645,5.90808986649102));
#298551=CARTESIAN_POINT('Ctrl Pts',(10.0514428414941,11.6562499999639,3.2659117547607));
#298552=CARTESIAN_POINT('Ctrl Pts',(10.0514428414941,11.8062499999633,-1.23094673026484E-15));
#298553=CARTESIAN_POINT('Ctrl Pts',(10.0514428414941,11.9562499999627,-3.26591175476071));
#298554=CARTESIAN_POINT('Ctrl Pts',(8.13178807675717,12.1062499999621,-5.90808986649102));
#298555=CARTESIAN_POINT('Ctrl Pts',(6.2121333120202,12.2562499999615,-8.55026797822134));
#298556=CARTESIAN_POINT('Ctrl Pts',(3.10606665601009,12.4062499999609,-9.5594902125713));
#298557=CARTESIAN_POINT('Ctrl Pts',(-2.03559535931351E-14,12.5562499999603,
-10.5687124469213));
#298558=CARTESIAN_POINT('Ctrl Pts',(-3.10606665601013,12.7062499999597,
-9.5594902125713));
#298559=CARTESIAN_POINT('Ctrl Pts',(-6.21213331202024,12.856249999959,-8.55026797822134));
#298560=CARTESIAN_POINT('Ctrl Pts',(-8.13178807675721,13.0062499999584,
-5.90808986649102));
#298561=CARTESIAN_POINT('Ctrl Pts',(-10.0514428414942,13.1562499999578,
-3.2659117547607));
#298562=CARTESIAN_POINT('Ctrl Pts',(-10.0514428414942,13.3062499999572,
2.46189346052968E-15));
#298563=CARTESIAN_POINT('Ctrl Pts',(-10.0514428414942,13.4562499999566,
3.26591175476071));
#298564=CARTESIAN_POINT('Ctrl Pts',(-8.13178807675721,13.606249999956,5.90808986649102));
#298565=CARTESIAN_POINT('Ctrl Pts',(-6.21213331202023,13.7562499999554,
8.55026797822134));
#298566=CARTESIAN_POINT('Ctrl Pts',(-3.10606665601013,13.9062499999549,
9.5594902125713));
#298567=CARTESIAN_POINT('Ctrl Pts',(-1.86312202551199E-14,14.0562499999543,
10.5687124469213));
#298568=CARTESIAN_POINT('Ctrl Pts',(3.10606665601009,14.2062499999537,9.5594902125713));
#298569=CARTESIAN_POINT('Ctrl Pts',(6.2121333120202,14.3562499999531,8.55026797822134));
#298570=CARTESIAN_POINT('Ctrl Pts',(8.13178807675717,14.5062499999525,5.90808986649102));
#298571=CARTESIAN_POINT('Ctrl Pts',(10.0514428414941,14.6562499999519,3.2659117547607));
#298572=CARTESIAN_POINT('Ctrl Pts',(10.0514428414941,14.8062499999513,-1.23094673026484E-15));
#298573=CARTESIAN_POINT('Ctrl Pts',(10.0514428414941,14.9562499999507,-3.26591175476071));
#298574=CARTESIAN_POINT('Ctrl Pts',(8.13178807675717,15.1062499999501,-5.90808986649102));
#298575=CARTESIAN_POINT('Ctrl Pts',(6.21213331202019,15.2562499999495,-8.55026797822134));
#298576=CARTESIAN_POINT('Ctrl Pts',(3.10606665601009,15.4062499999489,-9.5594902125713));
#298577=CARTESIAN_POINT('Ctrl Pts',(-2.2083662864797E-14,15.5562499999482,
-10.5687124469213));
#298578=CARTESIAN_POINT('Ctrl Pts',(-3.10606665601013,15.7062499999477,
-9.5594902125713));
#298579=CARTESIAN_POINT('Ctrl Pts',(-6.21213331202024,15.856249999947,-8.55026797822134));
#298580=CARTESIAN_POINT('Ctrl Pts',(-8.13178807675721,16.0062499999464,
-5.90808986649102));
#298581=CARTESIAN_POINT('Ctrl Pts',(-10.0514428414942,16.1562499999458,
-3.2659117547607));
#298582=CARTESIAN_POINT('Ctrl Pts',(-10.0514428414942,16.3062499999452,
2.46189346052968E-15));
#298583=CARTESIAN_POINT('Ctrl Pts',(-10.0514428414942,16.4562499999446,
3.26591175476071));
#298584=CARTESIAN_POINT('Ctrl Pts',(-8.13178807675721,16.606249999944,5.90808986649102));
#298585=CARTESIAN_POINT('Ctrl Pts',(-6.21213331202024,16.7562499999434,
8.55026797822134));
#298586=CARTESIAN_POINT('Ctrl Pts',(-3.10606665601013,16.9062499999428,
9.5594902125713));
#298587=CARTESIAN_POINT('Ctrl Pts',(-2.03589295267817E-14,17.0562499999422,
10.5687124469213));
#298588=CARTESIAN_POINT('Ctrl Pts',(3.10606665601009,17.2062499999417,9.5594902125713));
#298589=CARTESIAN_POINT('Ctrl Pts',(6.21213331202019,17.3562499999411,8.55026797822134));
#298590=CARTESIAN_POINT('Ctrl Pts',(8.13178807675717,17.5062499999405,5.90808986649102));
#298591=CARTESIAN_POINT('Ctrl Pts',(10.0514428414941,17.6562499999399,3.2659117547607));
#298592=CARTESIAN_POINT('Ctrl Pts',(10.0514428414941,17.8062499999393,-1.23094673026484E-15));
#298593=CARTESIAN_POINT('Ctrl Pts',(10.0514428414941,17.9562499999387,-3.26591175476071));
#298594=CARTESIAN_POINT('Ctrl Pts',(8.13178807675717,18.1062499999381,-5.90808986649102));
#298595=CARTESIAN_POINT('Ctrl Pts',(6.21213331202019,18.2562499999375,-8.55026797822134));
#298596=CARTESIAN_POINT('Ctrl Pts',(3.10606665601008,18.4062499999369,-9.5594902125713));
#298597=CARTESIAN_POINT('Ctrl Pts',(-2.38113721364588E-14,18.5562499999362,
-10.5687124469213));
#298598=CARTESIAN_POINT('Ctrl Pts',(-3.10606665601013,18.7062499999357,
-9.5594902125713));
#298599=CARTESIAN_POINT('Ctrl Pts',(-6.21213331202024,18.856249999935,-8.55026797822134));
#298600=CARTESIAN_POINT('Ctrl Pts',(-8.13178807675721,19.0062499999344,
-5.90808986649102));
#298601=CARTESIAN_POINT('Ctrl Pts',(-10.0514428414942,19.1562499999338,
-3.2659117547607));
#298602=CARTESIAN_POINT('Ctrl Pts',(-10.0514428414942,19.3062499999332,
2.46189346052968E-15));
#298603=CARTESIAN_POINT('Ctrl Pts',(-10.0514428414942,19.4562499999326,
3.26591175476071));
#298604=CARTESIAN_POINT('Ctrl Pts',(-8.13178807675721,19.606249999932,5.90808986649102));
#298605=CARTESIAN_POINT('Ctrl Pts',(-6.21213331202024,19.7562499999314,
8.55026797822134));
#298606=CARTESIAN_POINT('Ctrl Pts',(-3.10606665601013,19.9062499999308,
9.5594902125713));
#298607=CARTESIAN_POINT('Ctrl Pts',(-2.20866387984435E-14,20.0562499999302,
10.5687124469213));
#298608=CARTESIAN_POINT('Ctrl Pts',(3.10606665601009,20.2062499999297,9.5594902125713));
#298609=CARTESIAN_POINT('Ctrl Pts',(6.21213331202019,20.356249999929,8.55026797822134));
#298610=CARTESIAN_POINT('Ctrl Pts',(8.13178807675717,20.5062499999285,5.90808986649102));
#298611=CARTESIAN_POINT('Ctrl Pts',(10.0514428414941,20.6562499999279,3.2659117547607));
#298612=CARTESIAN_POINT('Ctrl Pts',(10.0514428414941,20.8062499999273,-1.23094673026484E-15));
#298613=CARTESIAN_POINT('Ctrl Pts',(10.0514428414941,20.9562499999267,-3.26591175476071));
#298614=CARTESIAN_POINT('Ctrl Pts',(8.13178807675716,21.1062499999261,-5.90808986649102));
#298615=CARTESIAN_POINT('Ctrl Pts',(6.21213331202019,21.2562499999255,-8.55026797822134));
#298616=CARTESIAN_POINT('Ctrl Pts',(3.10606665601008,21.4062499999249,-9.5594902125713));
#298617=CARTESIAN_POINT('Ctrl Pts',(-2.55390814081207E-14,21.5562499999242,
-10.5687124469213));
#298618=CARTESIAN_POINT('Ctrl Pts',(-3.10606665601013,21.7062499999237,
-9.5594902125713));
#298619=CARTESIAN_POINT('Ctrl Pts',(-6.21213331202024,21.856249999923,-8.55026797822134));
#298620=CARTESIAN_POINT('Ctrl Pts',(-8.13178807675722,22.0062499999224,
-5.90808986649102));
#298621=CARTESIAN_POINT('Ctrl Pts',(-10.0514428414942,22.1562499999218,
-3.2659117547607));
#298622=CARTESIAN_POINT('Ctrl Pts',(-10.0514428414942,22.3062499999212,
2.46189346052968E-15));
#298623=CARTESIAN_POINT('Ctrl Pts',(-10.0514428414942,22.4562499999206,
3.26591175476071));
#298624=CARTESIAN_POINT('Ctrl Pts',(-8.13178807675722,22.60624999992,5.90808986649102));
#298625=CARTESIAN_POINT('Ctrl Pts',(-6.21213331202024,22.7562499999194,
8.55026797822134));
#298626=CARTESIAN_POINT('Ctrl Pts',(-3.10606665601013,22.9062499999188,
9.5594902125713));
#298627=CARTESIAN_POINT('Ctrl Pts',(-2.38143480701054E-14,23.0562499999182,
10.5687124469213));
#298628=CARTESIAN_POINT('Ctrl Pts',(3.10606665601008,23.2062499999177,9.5594902125713));
#298629=CARTESIAN_POINT('Ctrl Pts',(6.21213331202019,23.3562499999171,8.55026797822134));
#298630=CARTESIAN_POINT('Ctrl Pts',(8.13178807675716,23.5062499999165,5.90808986649102));
#298631=CARTESIAN_POINT('Ctrl Pts',(10.0514428414941,23.6562499999159,3.2659117547607));
#298632=CARTESIAN_POINT('Ctrl Pts',(10.0514428414941,23.8062499999153,-1.23094673026484E-15));
#298633=CARTESIAN_POINT('Ctrl Pts',(10.0514428414941,23.9562499999147,-3.26591175476071));
#298634=CARTESIAN_POINT('Ctrl Pts',(8.13178807675716,24.1062499999141,-5.90808986649102));
#298635=CARTESIAN_POINT('Ctrl Pts',(6.21213331202019,24.2562499999135,-8.55026797822134));
#298636=CARTESIAN_POINT('Ctrl Pts',(3.10606665601008,24.4062499999129,-9.5594902125713));
#298637=CARTESIAN_POINT('Ctrl Pts',(-2.72667906797825E-14,24.5562499999122,
-10.5687124469213));
#298638=CARTESIAN_POINT('Ctrl Pts',(-3.10606665601014,24.7062499999116,
-9.5594902125713));
#298639=CARTESIAN_POINT('Ctrl Pts',(-6.21213331202024,24.856249999911,-8.55026797822134));
#298640=CARTESIAN_POINT('Ctrl Pts',(-8.13178807675722,25.0062499999104,
-5.90808986649102));
#298641=CARTESIAN_POINT('Ctrl Pts',(-10.0514428414942,25.1562499999098,
-3.2659117547607));
#298642=CARTESIAN_POINT('Ctrl Pts',(-10.0514428414942,25.3062499999092,
2.46189346052968E-15));
#298643=CARTESIAN_POINT('Ctrl Pts',(-10.0514428414942,25.4562499999086,
3.26591175476071));
#298644=CARTESIAN_POINT('Ctrl Pts',(-8.13178807675722,25.6062499999081,
5.90808986649102));
#298645=CARTESIAN_POINT('Ctrl Pts',(-6.21213331202024,25.7562499999074,
8.55026797822134));
#298646=CARTESIAN_POINT('Ctrl Pts',(-3.10606665601013,25.9062499999069,
9.5594902125713));
#298647=CARTESIAN_POINT('Ctrl Pts',(-2.55420573417672E-14,26.0562499999062,
10.5687124469213));
#298648=CARTESIAN_POINT('Ctrl Pts',(3.10606665601008,26.2062499999057,9.5594902125713));
#298649=CARTESIAN_POINT('Ctrl Pts',(6.21213331202019,26.356249999905,8.55026797822134));
#298650=CARTESIAN_POINT('Ctrl Pts',(8.13178807675716,26.5062499999045,5.90808986649102));
#298651=CARTESIAN_POINT('Ctrl Pts',(10.0514428414941,26.6562499999039,3.2659117547607));
#298652=CARTESIAN_POINT('Ctrl Pts',(10.0514428414941,26.8062499999033,-1.23094673026484E-15));
#298653=CARTESIAN_POINT('Ctrl Pts',(10.0514428414941,26.9562499999027,-3.26591175476071));
#298654=CARTESIAN_POINT('Ctrl Pts',(8.13178807675716,27.1062499999021,-5.90808986649102));
#298655=CARTESIAN_POINT('Ctrl Pts',(6.21213331202019,27.2562499999015,-8.55026797822134));
#298656=CARTESIAN_POINT('Ctrl Pts',(3.10606665601008,27.4062499999009,-9.5594902125713));
#298657=CARTESIAN_POINT('Ctrl Pts',(-2.89944999514443E-14,27.5562499999002,
-10.5687124469213));
#298658=CARTESIAN_POINT('Ctrl Pts',(-3.10606665601014,27.7062499998996,
-9.5594902125713));
#298659=CARTESIAN_POINT('Ctrl Pts',(-6.21213331202024,27.856249999899,-8.55026797822134));
#298660=CARTESIAN_POINT('Ctrl Pts',(-8.13178807675722,28.0062499998984,
-5.90808986649102));
#298661=CARTESIAN_POINT('Ctrl Pts',(-10.0514428414942,28.1562499998978,
-3.2659117547607));
#298662=CARTESIAN_POINT('Ctrl Pts',(-10.0514428414942,28.3062499998973,
2.46189346052968E-15));
#298663=CARTESIAN_POINT('Ctrl Pts',(-10.0514428414942,28.4562499998966,
3.26591175476071));
#298664=CARTESIAN_POINT('Ctrl Pts',(-8.13178807675722,28.606249999896,5.90808986649102));
#298665=CARTESIAN_POINT('Ctrl Pts',(-6.21213331202024,28.7562499998954,
8.55026797822134));
#298666=CARTESIAN_POINT('Ctrl Pts',(-3.10606665601014,28.9062499998949,
9.5594902125713));
#298667=CARTESIAN_POINT('Ctrl Pts',(-2.72697666134291E-14,29.0562499998942,
10.5687124469213));
#298668=CARTESIAN_POINT('Ctrl Pts',(3.10606665601008,29.2062499998937,9.5594902125713));
#298669=CARTESIAN_POINT('Ctrl Pts',(6.21213331202019,29.356249999893,8.55026797822134));
#298670=CARTESIAN_POINT('Ctrl Pts',(8.13178807675716,29.5062499998925,5.90808986649102));
#298671=CARTESIAN_POINT('Ctrl Pts',(10.0514428414941,29.6562499998919,3.2659117547607));
#298672=CARTESIAN_POINT('Ctrl Pts',(10.0514428414941,29.8062499998913,-1.23094673026484E-15));
#298673=CARTESIAN_POINT('Ctrl Pts',(10.0514428414941,29.9562499998907,-3.26591175476071));
#298674=CARTESIAN_POINT('Ctrl Pts',(8.13178807675716,30.1062499998901,-5.90808986649102));
#298675=CARTESIAN_POINT('Ctrl Pts',(6.21213331202019,30.2562499998895,-8.55026797822134));
#298676=CARTESIAN_POINT('Ctrl Pts',(3.10606665601008,30.4062499998889,-9.5594902125713));
#298677=CARTESIAN_POINT('Ctrl Pts',(-3.07222092231062E-14,30.5562499998883,
-10.5687124469213));
#298678=CARTESIAN_POINT('Ctrl Pts',(-3.10606665601014,30.7062499998877,
-9.5594902125713));
#298679=CARTESIAN_POINT('Ctrl Pts',(-6.21213331202025,30.8562499998871,
-8.55026797822134));
#298680=CARTESIAN_POINT('Ctrl Pts',(-8.13178807675722,31.0062499998864,
-5.90808986649102));
#298681=CARTESIAN_POINT('Ctrl Pts',(-10.0514428414942,31.1562499998858,
-3.2659117547607));
#298682=CARTESIAN_POINT('Ctrl Pts',(-10.0514428414942,31.3062499998852,
2.46189346052968E-15));
#298683=CARTESIAN_POINT('Ctrl Pts',(-10.0514428414942,31.4562499998847,
3.26591175476071));
#298684=CARTESIAN_POINT('Ctrl Pts',(-8.13178807675722,31.606249999884,5.90808986649102));
#298685=CARTESIAN_POINT('Ctrl Pts',(-6.21213331202024,31.7562499998835,
8.55026797822134));
#298686=CARTESIAN_POINT('Ctrl Pts',(-3.10606665601014,31.9062499998829,
9.5594902125713));
#298687=CARTESIAN_POINT('Ctrl Pts',(-2.89974758850909E-14,32.0562499998822,
10.5687124469213));
#298688=CARTESIAN_POINT('Ctrl Pts',(3.10606665601008,32.2062499998816,9.5594902125713));
#298689=CARTESIAN_POINT('Ctrl Pts',(6.21213331202019,32.3562499998811,8.55026797822134));
#298690=CARTESIAN_POINT('Ctrl Pts',(8.13178807675716,32.5062499998805,5.90808986649102));
#298691=CARTESIAN_POINT('Ctrl Pts',(10.0514428414941,32.6562499998798,3.2659117547607));
#298692=CARTESIAN_POINT('Ctrl Pts',(10.0514428414941,32.8062499998793,-1.23094673026484E-15));
#298693=CARTESIAN_POINT('Ctrl Pts',(10.0514428414941,32.9562499998787,-3.26591175476071));
#298694=CARTESIAN_POINT('Ctrl Pts',(8.13178807675716,33.1062499998781,-5.90808986649102));
#298695=CARTESIAN_POINT('Ctrl Pts',(6.21213331202019,33.2562499998775,-8.55026797822134));
#298696=CARTESIAN_POINT('Ctrl Pts',(3.10606665601008,33.4062499998769,-9.5594902125713));
#298697=CARTESIAN_POINT('Ctrl Pts',(-3.2449918494768E-14,33.5562499998763,
-10.5687124469213));
#298698=CARTESIAN_POINT('Ctrl Pts',(-3.10606665601014,33.7062499998756,
-9.5594902125713));
#298699=CARTESIAN_POINT('Ctrl Pts',(-6.21213331202025,33.8562499998751,
-8.55026797822134));
#298700=CARTESIAN_POINT('Ctrl Pts',(-8.13178807675722,34.0062499998744,
-5.90808986649102));
#298701=CARTESIAN_POINT('Ctrl Pts',(-10.0514428414942,34.1562499998739,
-3.2659117547607));
#298702=CARTESIAN_POINT('Ctrl Pts',(-10.0514428414942,34.3062499998732,
2.46189346052968E-15));
#298703=CARTESIAN_POINT('Ctrl Pts',(-10.0514428414942,34.4562499998727,
3.26591175476071));
#298704=CARTESIAN_POINT('Ctrl Pts',(-8.13178807675722,34.606249999872,5.90808986649102));
#298705=CARTESIAN_POINT('Ctrl Pts',(-6.21213331202024,34.7562499998715,
8.55026797822134));
#298706=CARTESIAN_POINT('Ctrl Pts',(-3.10606665601014,34.9062499998708,
9.5594902125713));
#298707=CARTESIAN_POINT('Ctrl Pts',(-3.07251851567527E-14,35.0562499998703,
10.5687124469213));
#298708=CARTESIAN_POINT('Ctrl Pts',(3.10606665601008,35.2062499998697,9.5594902125713));
#298709=CARTESIAN_POINT('Ctrl Pts',(6.21213331202019,35.3562499998691,8.55026797822134));
#298710=CARTESIAN_POINT('Ctrl Pts',(8.13178807675716,35.5062499998685,5.90808986649102));
#298711=CARTESIAN_POINT('Ctrl Pts',(10.0514428414941,35.6562499998679,3.2659117547607));
#298712=CARTESIAN_POINT('Ctrl Pts',(10.0514428414941,35.8062499998673,-1.23094673026484E-15));
#298713=CARTESIAN_POINT('Ctrl Pts',(10.0514428414941,35.9562499998667,-3.26591175476071));
#298714=CARTESIAN_POINT('Ctrl Pts',(8.13178807675716,36.1062499998661,-5.90808986649102));
#298715=CARTESIAN_POINT('Ctrl Pts',(6.21213331202018,36.2562499998655,-8.55026797822134));
#298716=CARTESIAN_POINT('Ctrl Pts',(3.10606665601007,36.4062499998649,-9.5594902125713));
#298717=CARTESIAN_POINT('Ctrl Pts',(-3.41776277664299E-14,36.5562499998642,
-10.5687124469213));
#298718=CARTESIAN_POINT('Ctrl Pts',(-3.10606665601014,36.7062499998636,
-9.5594902125713));
#298719=CARTESIAN_POINT('Ctrl Pts',(-6.21213331202025,36.856249999863,-8.55026797822134));
#298720=CARTESIAN_POINT('Ctrl Pts',(-8.13178807675722,37.0062499998624,
-5.90808986649102));
#298721=CARTESIAN_POINT('Ctrl Pts',(-10.0514428414942,37.1562499998618,
-3.2659117547607));
#298722=CARTESIAN_POINT('Ctrl Pts',(-10.0514428414942,37.3062499998613,
2.46189346052968E-15));
#298723=CARTESIAN_POINT('Ctrl Pts',(-10.0514428414942,37.4562499998606,
3.26591175476071));
#298724=CARTESIAN_POINT('Ctrl Pts',(-8.13178807675722,37.60624999986,5.90808986649102));
#298725=CARTESIAN_POINT('Ctrl Pts',(-6.21213331202025,37.7562499998594,
8.55026797822134));
#298726=CARTESIAN_POINT('Ctrl Pts',(-3.10606665601014,37.9062499998588,
9.5594902125713));
#298727=CARTESIAN_POINT('Ctrl Pts',(-3.24528944284146E-14,38.0562499998583,
10.5687124469213));
#298728=CARTESIAN_POINT('Ctrl Pts',(3.10606665601007,38.2062499998577,9.5594902125713));
#298729=CARTESIAN_POINT('Ctrl Pts',(6.21213331202018,38.3562499998571,8.55026797822134));
#298730=CARTESIAN_POINT('Ctrl Pts',(8.13178807675716,38.5062499998565,5.90808986649102));
#298731=CARTESIAN_POINT('Ctrl Pts',(10.0514428414941,38.6562499998559,3.2659117547607));
#298732=CARTESIAN_POINT('Ctrl Pts',(10.0514428414941,38.8062499998553,-1.23094673026484E-15));
#298733=CARTESIAN_POINT('Ctrl Pts',(10.0514428414941,38.9562499998547,-3.26591175476071));
#298734=CARTESIAN_POINT('Ctrl Pts',(8.13178807675715,39.1062499998541,-5.90808986649102));
#298735=CARTESIAN_POINT('Ctrl Pts',(6.21213331202018,39.2562499998535,-8.55026797822134));
#298736=CARTESIAN_POINT('Ctrl Pts',(3.10606665601007,39.4062499998529,-9.5594902125713));
#298737=CARTESIAN_POINT('Ctrl Pts',(-3.59053370380917E-14,39.5562499998523,
-10.5687124469213));
#298738=CARTESIAN_POINT('Ctrl Pts',(-3.10606665601014,39.7062499998516,
-9.5594902125713));
#298739=CARTESIAN_POINT('Ctrl Pts',(-6.21213331202025,39.856249999851,-8.55026797822134));
#298740=CARTESIAN_POINT('Ctrl Pts',(-8.13178807675723,40.0062499998505,
-5.90808986649102));
#298741=CARTESIAN_POINT('Ctrl Pts',(-10.0514428414942,40.1562499998499,
-3.2659117547607));
#298742=CARTESIAN_POINT('Ctrl Pts',(-10.0514428414942,40.3062499998493,
2.46189346052968E-15));
#298743=CARTESIAN_POINT('Ctrl Pts',(-10.0514428414942,40.4562499998487,
3.26591175476071));
#298744=CARTESIAN_POINT('Ctrl Pts',(-8.13178807675723,40.606249999848,5.90808986649102));
#298745=CARTESIAN_POINT('Ctrl Pts',(-6.21213331202025,40.7562499998475,
8.55026797822134));
#298746=CARTESIAN_POINT('Ctrl Pts',(-3.10606665601014,40.9062499998468,
9.5594902125713));
#298747=CARTESIAN_POINT('Ctrl Pts',(-3.41806037000764E-14,41.0562499998463,
10.5687124469213));
#298748=CARTESIAN_POINT('Ctrl Pts',(3.10606665601007,41.2062499998457,9.5594902125713));
#298749=CARTESIAN_POINT('Ctrl Pts',(6.21213331202018,41.3562499998451,8.55026797822134));
#298750=CARTESIAN_POINT('Ctrl Pts',(8.13178807675715,41.5062499998444,5.90808986649102));
#298751=CARTESIAN_POINT('Ctrl Pts',(10.0514428414941,41.6562499998439,3.2659117547607));
#298752=CARTESIAN_POINT('Ctrl Pts',(10.0514428414941,41.8062499998433,-1.23094673026484E-15));
#298753=CARTESIAN_POINT('Ctrl Pts',(10.0514428414941,41.9562499998427,-3.26591175476071));
#298754=CARTESIAN_POINT('Ctrl Pts',(8.13178807675715,42.1062499998421,-5.90808986649102));
#298755=CARTESIAN_POINT('Ctrl Pts',(6.21213331202018,42.2562499998414,-8.55026797822134));
#298756=CARTESIAN_POINT('Ctrl Pts',(3.10606665601007,42.4062499998408,-9.5594902125713));
#298757=CARTESIAN_POINT('Ctrl Pts',(-3.76330463097535E-14,42.5562499998402,
-10.5687124469213));
#298758=CARTESIAN_POINT('Ctrl Pts',(-3.10606665601015,42.7062499998396,
-9.5594902125713));
#298759=CARTESIAN_POINT('Ctrl Pts',(-6.21213331202025,42.8562499998391,
-8.55026797822134));
#298760=CARTESIAN_POINT('Ctrl Pts',(-8.13178807675723,43.0062499998385,
-5.90808986649102));
#298761=CARTESIAN_POINT('Ctrl Pts',(-10.0514428414942,43.1562499998379,
-3.2659117547607));
#298762=CARTESIAN_POINT('Ctrl Pts',(-10.0514428414942,43.3062499998373,
2.46189346052968E-15));
#298763=CARTESIAN_POINT('Ctrl Pts',(-10.0514428414942,43.4562499998366,
3.26591175476071));
#298764=CARTESIAN_POINT('Ctrl Pts',(-8.13178807675723,43.6062499998361,
5.90808986649102));
#298765=CARTESIAN_POINT('Ctrl Pts',(-6.21213331202025,43.7562499998354,
8.55026797822134));
#298766=CARTESIAN_POINT('Ctrl Pts',(-3.10606665601014,43.9062499998348,
9.5594902125713));
#298767=CARTESIAN_POINT('Ctrl Pts',(-3.59083129717383E-14,44.0562499998343,
10.5687124469213));
#298768=CARTESIAN_POINT('Ctrl Pts',(3.10606665601007,44.2062499998337,9.5594902125713));
#298769=CARTESIAN_POINT('Ctrl Pts',(6.21213331202018,44.3562499998331,8.55026797822134));
#298770=CARTESIAN_POINT('Ctrl Pts',(8.13178807675715,44.5062499998324,5.90808986649102));
#298771=CARTESIAN_POINT('Ctrl Pts',(10.0514428414941,44.6562499998319,3.2659117547607));
#298772=CARTESIAN_POINT('Ctrl Pts',(10.0514428414941,44.8062499998313,-1.23094673026484E-15));
#298773=CARTESIAN_POINT('Ctrl Pts',(10.0514428414941,44.9562499998307,-3.26591175476071));
#298774=CARTESIAN_POINT('Ctrl Pts',(8.13178807675715,45.1062499998301,-5.90808986649102));
#298775=CARTESIAN_POINT('Ctrl Pts',(6.21213331202018,45.2562499998295,-8.55026797822134));
#298776=CARTESIAN_POINT('Ctrl Pts',(3.10606665601007,45.4062499998289,-9.5594902125713));
#298777=CARTESIAN_POINT('Ctrl Pts',(-3.93607555814154E-14,45.5562499998283,
-10.5687124469213));
#298778=CARTESIAN_POINT('Ctrl Pts',(-3.10606665601015,45.7062499998276,
-9.5594902125713));
#298779=CARTESIAN_POINT('Ctrl Pts',(-6.21213331202026,45.856249999827,-8.55026797822134));
#298780=CARTESIAN_POINT('Ctrl Pts',(-8.13178807675723,46.0062499998265,
-5.90808986649102));
#298781=CARTESIAN_POINT('Ctrl Pts',(-10.0514428414942,46.1562499998259,
-3.2659117547607));
#298782=CARTESIAN_POINT('Ctrl Pts',(-10.0514428414942,46.3062499998252,
2.46189346052968E-15));
#298783=CARTESIAN_POINT('Ctrl Pts',(-10.0514428414942,46.4562499998247,
3.26591175476071));
#298784=CARTESIAN_POINT('Ctrl Pts',(-8.13178807675723,46.606249999824,5.90808986649102));
#298785=CARTESIAN_POINT('Ctrl Pts',(-6.21213331202025,46.7562499998235,
8.55026797822134));
#298786=CARTESIAN_POINT('Ctrl Pts',(-3.10606665601015,46.9062499998228,
9.5594902125713));
#298787=CARTESIAN_POINT('Ctrl Pts',(-3.76360222434001E-14,47.0562499998223,
10.5687124469213));
#298788=CARTESIAN_POINT('Ctrl Pts',(3.10606665601007,47.2062499998217,9.5594902125713));
#298789=CARTESIAN_POINT('Ctrl Pts',(6.21213331202018,47.3562499998211,8.55026797822134));
#298790=CARTESIAN_POINT('Ctrl Pts',(8.13178807675715,47.5062499998204,5.90808986649102));
#298791=CARTESIAN_POINT('Ctrl Pts',(10.0514428414941,47.6562499998198,3.2659117547607));
#298792=CARTESIAN_POINT('Ctrl Pts',(10.0514428414941,47.8062499998193,-1.23094673026484E-15));
#298793=CARTESIAN_POINT('Ctrl Pts',(10.0514428414941,47.9562499998186,-3.26591175476071));
#298794=CARTESIAN_POINT('Ctrl Pts',(8.13178807675715,48.1062499998181,-5.90808986649102));
#298795=CARTESIAN_POINT('Ctrl Pts',(6.21213331202017,48.2562499998174,-8.55026797822134));
#298796=CARTESIAN_POINT('Ctrl Pts',(3.10606665601007,48.4062499998169,-9.5594902125713));
#298797=CARTESIAN_POINT('Ctrl Pts',(-4.10884648530772E-14,48.5562499998163,
-10.5687124469213));
#298798=CARTESIAN_POINT('Ctrl Pts',(-3.10606665601015,48.7062499998157,
-9.5594902125713));
#298799=CARTESIAN_POINT('Ctrl Pts',(-6.21213331202026,48.8562499998151,
-8.55026797822134));
#298800=CARTESIAN_POINT('Ctrl Pts',(-8.13178807675723,49.0062499998145,
-5.90808986649102));
#298801=CARTESIAN_POINT('Ctrl Pts',(-10.0514428414942,49.1562499998138,
-3.2659117547607));
#298802=CARTESIAN_POINT('Ctrl Pts',(-10.0514428414942,49.3062499998132,
2.46189346052968E-15));
#298803=CARTESIAN_POINT('Ctrl Pts',(-10.0514428414942,49.4562499998126,
3.26591175476071));
#298804=CARTESIAN_POINT('Ctrl Pts',(-8.13178807675723,49.6062499998121,
5.90808986649102));
#298805=CARTESIAN_POINT('Ctrl Pts',(-6.21213331202026,49.7562499998114,
8.55026797822134));
#298806=CARTESIAN_POINT('Ctrl Pts',(-3.10606665601015,49.9062499998109,
9.5594902125713));
#298807=CARTESIAN_POINT('Ctrl Pts',(-3.9363731515062E-14,50.0562499998103,
10.5687124469213));
#298808=CARTESIAN_POINT('Ctrl Pts',(3.10606665601007,50.2062499998097,9.5594902125713));
#298809=CARTESIAN_POINT('Ctrl Pts',(6.21213331202017,50.3562499998091,8.55026797822134));
#298810=CARTESIAN_POINT('Ctrl Pts',(8.13178807675715,50.5062499998085,5.90808986649102));
#298811=CARTESIAN_POINT('Ctrl Pts',(10.0514428414941,50.6562499998078,3.2659117547607));
#298812=CARTESIAN_POINT('Ctrl Pts',(10.0514428414941,50.8062499998072,-1.23094673026484E-15));
#298813=CARTESIAN_POINT('Ctrl Pts',(10.0514428414941,50.9562499998067,-3.26591175476071));
#298814=CARTESIAN_POINT('Ctrl Pts',(8.13178807675715,51.1062499998061,-5.90808986649102));
#298815=CARTESIAN_POINT('Ctrl Pts',(6.21213331202017,51.2562499998055,-8.55026797822134));
#298816=CARTESIAN_POINT('Ctrl Pts',(3.10606665601006,51.4062499998048,-9.5594902125713));
#298817=CARTESIAN_POINT('Ctrl Pts',(-4.2816174124739E-14,51.5562499998043,
-10.5687124469213));
#298818=CARTESIAN_POINT('Ctrl Pts',(-3.10606665601015,51.7062499998037,
-9.5594902125713));
#298819=CARTESIAN_POINT('Ctrl Pts',(-6.21213331202026,51.856249999803,-8.55026797822134));
#298820=CARTESIAN_POINT('Ctrl Pts',(-8.13178807675723,52.0062499998025,
-5.90808986649102));
#298821=CARTESIAN_POINT('Ctrl Pts',(-10.0514428414942,52.1562499998019,
-3.2659117547607));
#298822=CARTESIAN_POINT('Ctrl Pts',(-10.0514428414942,52.3062499998012,
2.46189346052968E-15));
#298823=CARTESIAN_POINT('Ctrl Pts',(-10.0514428414942,52.4562499998006,
3.26591175476071));
#298824=CARTESIAN_POINT('Ctrl Pts',(-8.13178807675723,52.6062499998,5.90808986649102));
#298825=CARTESIAN_POINT('Ctrl Pts',(-6.21213331202026,52.7562499997994,
8.55026797822134));
#298826=CARTESIAN_POINT('Ctrl Pts',(-3.10606665601015,52.9062499997988,
9.5594902125713));
#298827=CARTESIAN_POINT('Ctrl Pts',(-4.10914407867238E-14,53.0562499997983,
10.5687124469213));
#298828=CARTESIAN_POINT('Ctrl Pts',(3.10606665601007,53.2062499997976,9.5594902125713));
#298829=CARTESIAN_POINT('Ctrl Pts',(6.21213331202017,53.3562499997971,8.55026797822134));
#298830=CARTESIAN_POINT('Ctrl Pts',(8.13178807675715,53.5062499997965,5.90808986649102));
#298831=CARTESIAN_POINT('Ctrl Pts',(10.0514428414941,53.6562499997959,3.2659117547607));
#298832=CARTESIAN_POINT('Ctrl Pts',(10.0514428414941,53.8062499997953,-1.23094673026484E-15));
#298833=CARTESIAN_POINT('Ctrl Pts',(10.0514428414941,53.9562499997946,-3.26591175476071));
#298834=CARTESIAN_POINT('Ctrl Pts',(8.13178807675714,54.106249999794,-5.90808986649102));
#298835=CARTESIAN_POINT('Ctrl Pts',(6.21213331202017,54.2562499997934,-8.55026797822134));
#298836=CARTESIAN_POINT('Ctrl Pts',(3.10606665601006,54.4062499997928,-9.5594902125713));
#298837=CARTESIAN_POINT('Ctrl Pts',(-4.45438833964009E-14,54.5562499997923,
-10.5687124469213));
#298838=CARTESIAN_POINT('Ctrl Pts',(-3.10606665601015,54.7062499997917,
-9.5594902125713));
#298839=CARTESIAN_POINT('Ctrl Pts',(-6.21213331202026,54.856249999791,-8.55026797822134));
#298840=CARTESIAN_POINT('Ctrl Pts',(-8.13178807675724,55.0062499997905,
-5.90808986649102));
#298841=CARTESIAN_POINT('Ctrl Pts',(-10.0514428414942,55.1562499997898,
-3.2659117547607));
#298842=CARTESIAN_POINT('Ctrl Pts',(-10.0514428414942,55.3062499997893,
2.46189346052968E-15));
#298843=CARTESIAN_POINT('Ctrl Pts',(-10.0514428414942,55.4562499997886,
3.26591175476071));
#298844=CARTESIAN_POINT('Ctrl Pts',(-8.13178807675724,55.606249999788,5.90808986649102));
#298845=CARTESIAN_POINT('Ctrl Pts',(-6.21213331202026,55.7562499997874,
8.55026797822134));
#298846=CARTESIAN_POINT('Ctrl Pts',(-3.10606665601015,55.9062499997869,
9.5594902125713));
#298847=CARTESIAN_POINT('Ctrl Pts',(-4.28191500583856E-14,56.0562499997862,
10.5687124469213));
#298848=CARTESIAN_POINT('Ctrl Pts',(3.10606665601006,56.2062499997857,9.5594902125713));
#298849=CARTESIAN_POINT('Ctrl Pts',(6.21213331202017,56.356249999785,8.55026797822134));
#298850=CARTESIAN_POINT('Ctrl Pts',(8.13178807675714,56.5062499997845,5.90808986649102));
#298851=CARTESIAN_POINT('Ctrl Pts',(10.0514428414941,56.6562499997839,3.2659117547607));
#298852=CARTESIAN_POINT('Ctrl Pts',(10.0514428414941,56.8062499997833,-1.23094673026484E-15));
#298853=CARTESIAN_POINT('Ctrl Pts',(10.0514428414941,56.9562499997827,-3.26591175476071));
#298854=CARTESIAN_POINT('Ctrl Pts',(8.13178807675714,57.1062499997821,-5.90808986649102));
#298855=CARTESIAN_POINT('Ctrl Pts',(6.21213331202017,57.2562499997814,-8.55026797822134));
#298856=CARTESIAN_POINT('Ctrl Pts',(3.10606665601006,57.4062499997808,-9.5594902125713));
#298857=CARTESIAN_POINT('Ctrl Pts',(-4.62715926680627E-14,57.5562499997802,
-10.5687124469213));
#298858=CARTESIAN_POINT('Ctrl Pts',(-3.10606665601015,57.7062499997797,
-9.5594902125713));
#298859=CARTESIAN_POINT('Ctrl Pts',(-6.21213331202026,57.856249999779,-8.55026797822134));
#298860=CARTESIAN_POINT('Ctrl Pts',(-8.13178807675724,58.0062499997784,
-5.90808986649102));
#298861=CARTESIAN_POINT('Ctrl Pts',(-10.0514428414942,58.1562499997778,
-3.2659117547607));
#298862=CARTESIAN_POINT('Ctrl Pts',(-10.0514428414942,58.3062499997773,
2.46189346052968E-15));
#298863=CARTESIAN_POINT('Ctrl Pts',(-10.0514428414942,58.4562499997766,
3.26591175476071));
#298864=CARTESIAN_POINT('Ctrl Pts',(-8.13178807675724,58.6062499997761,
5.90808986649102));
#298865=CARTESIAN_POINT('Ctrl Pts',(-6.21213331202026,58.7562499997754,
8.55026797822134));
#298866=CARTESIAN_POINT('Ctrl Pts',(-3.10606665601015,58.9062499997749,
9.5594902125713));
#298867=CARTESIAN_POINT('Ctrl Pts',(-4.45468593300475E-14,59.0562499997743,
10.5687124469213));
#298868=CARTESIAN_POINT('Ctrl Pts',(3.10606665601006,59.2062499997736,9.5594902125713));
#298869=CARTESIAN_POINT('Ctrl Pts',(6.21213331202017,59.356249999773,8.55026797822134));
#298870=CARTESIAN_POINT('Ctrl Pts',(8.13178807675714,59.5062499997725,5.90808986649102));
#298871=CARTESIAN_POINT('Ctrl Pts',(10.0514428414941,59.6562499997718,3.2659117547607));
#298872=CARTESIAN_POINT('Ctrl Pts',(10.0514428414941,59.8062499997713,-1.23094673026484E-15));
#298873=CARTESIAN_POINT('Ctrl Pts',(10.0514428414941,59.9562499997706,-3.26591175476071));
#298874=CARTESIAN_POINT('Ctrl Pts',(8.13178807675714,60.10624999977,-5.90808986649102));
#298875=CARTESIAN_POINT('Ctrl Pts',(6.21213331202017,60.2562499997694,-8.55026797822134));
#298876=CARTESIAN_POINT('Ctrl Pts',(3.10606665601006,60.4062499997689,-9.5594902125713));
#298877=CARTESIAN_POINT('Ctrl Pts',(-4.79993019397246E-14,60.5562499997682,
-10.5687124469213));
#298878=CARTESIAN_POINT('Ctrl Pts',(-3.10606665601016,60.7062499997676,
-9.5594902125713));
#298879=CARTESIAN_POINT('Ctrl Pts',(-6.21213331202026,60.856249999767,-8.55026797822134));
#298880=CARTESIAN_POINT('Ctrl Pts',(-8.13178807675724,61.0062499997664,
-5.90808986649102));
#298881=CARTESIAN_POINT('Ctrl Pts',(-10.0514428414942,61.1562499997658,
-3.2659117547607));
#298882=CARTESIAN_POINT('Ctrl Pts',(-10.0514428414942,61.3062499997652,
2.46189346052968E-15));
#298883=CARTESIAN_POINT('Ctrl Pts',(-10.0514428414942,61.4562499997646,
3.26591175476071));
#298884=CARTESIAN_POINT('Ctrl Pts',(-8.13178807675724,61.6062499997641,
5.90808986649102));
#298885=CARTESIAN_POINT('Ctrl Pts',(-6.21213331202026,61.7562499997634,
8.55026797822134));
#298886=CARTESIAN_POINT('Ctrl Pts',(-3.10606665601015,61.9062499997628,
9.5594902125713));
#298887=CARTESIAN_POINT('Ctrl Pts',(-4.62745686017093E-14,62.0562499997622,
10.5687124469213));
#298888=CARTESIAN_POINT('Ctrl Pts',(3.10606665601006,62.2062499997617,9.5594902125713));
#298889=CARTESIAN_POINT('Ctrl Pts',(6.21213331202017,62.356249999761,8.55026797822134));
#298890=CARTESIAN_POINT('Ctrl Pts',(8.13178807675714,62.5062499997605,5.90808986649102));
#298891=CARTESIAN_POINT('Ctrl Pts',(10.0514428414941,62.6562499997599,3.2659117547607));
#298892=CARTESIAN_POINT('Ctrl Pts',(10.0514428414941,62.8062499997593,-1.23094673026484E-15));
#298893=CARTESIAN_POINT('Ctrl Pts',(10.0514428414941,62.9562499997587,-3.26591175476071));
#298894=CARTESIAN_POINT('Ctrl Pts',(8.13178807675714,63.1062499997581,-5.90808986649102));
#298895=CARTESIAN_POINT('Ctrl Pts',(6.21213331202017,63.2562499997575,-8.55026797822134));
#298896=CARTESIAN_POINT('Ctrl Pts',(3.10606665601006,63.4062499997568,-9.5594902125713));
#298897=CARTESIAN_POINT('Ctrl Pts',(-4.97270112113864E-14,63.5562499997562,
-10.5687124469213));
#298898=CARTESIAN_POINT('Ctrl Pts',(-3.10606665601016,63.7062499997556,
-9.5594902125713));
#298899=CARTESIAN_POINT('Ctrl Pts',(-6.21213331202027,63.8562499997551,
-8.55026797822134));
#298900=CARTESIAN_POINT('Ctrl Pts',(-8.13178807675724,64.0062499997544,
-5.90808986649102));
#298901=CARTESIAN_POINT('Ctrl Pts',(-10.0514428414942,64.1562499997538,
-3.2659117547607));
#298902=CARTESIAN_POINT('Ctrl Pts',(-10.0514428414942,64.3062499997532,
2.46189346052968E-15));
#298903=CARTESIAN_POINT('Ctrl Pts',(-10.0514428414942,64.4562499997526,
3.26591175476071));
#298904=CARTESIAN_POINT('Ctrl Pts',(-8.13178807675724,64.606249999752,5.90808986649102));
#298905=CARTESIAN_POINT('Ctrl Pts',(-6.21213331202026,64.7562499997514,
8.55026797822134));
#298906=CARTESIAN_POINT('Ctrl Pts',(-3.10606665601016,64.9062499997509,
9.5594902125713));
#298907=CARTESIAN_POINT('Ctrl Pts',(-4.80022778733711E-14,65.0562499997502,
10.5687124469213));
#298908=CARTESIAN_POINT('Ctrl Pts',(3.10606665601006,65.2062499997497,9.5594902125713));
#298909=CARTESIAN_POINT('Ctrl Pts',(6.21213331202017,65.3562499997491,8.55026797822134));
#298910=CARTESIAN_POINT('Ctrl Pts',(8.13178807675714,65.5062499997484,5.90808986649102));
#298911=CARTESIAN_POINT('Ctrl Pts',(10.0514428414941,65.6562499997479,3.2659117547607));
#298912=CARTESIAN_POINT('Ctrl Pts',(10.0514428414941,65.8062499997473,-1.23094673026484E-15));
#298913=CARTESIAN_POINT('Ctrl Pts',(10.0514428414941,65.9562499997467,-3.26591175476071));
#298914=CARTESIAN_POINT('Ctrl Pts',(8.13178807675714,66.1062499997461,-5.90808986649102));
#298915=CARTESIAN_POINT('Ctrl Pts',(6.21213331202016,66.2562499997454,-8.55026797822134));
#298916=CARTESIAN_POINT('Ctrl Pts',(3.10606665601006,66.4062499997449,-9.5594902125713));
#298917=CARTESIAN_POINT('Ctrl Pts',(-5.14547204830482E-14,66.5562499997443,
-10.5687124469213));
#298918=CARTESIAN_POINT('Ctrl Pts',(-3.10606665601016,66.7062499997436,
-9.5594902125713));
#298919=CARTESIAN_POINT('Ctrl Pts',(-6.21213331202027,66.8562499997431,
-8.55026797822134));
#298920=CARTESIAN_POINT('Ctrl Pts',(-8.13178807675724,67.0062499997424,
-5.90808986649102));
#298921=CARTESIAN_POINT('Ctrl Pts',(-10.0514428414942,67.1562499997418,
-3.2659117547607));
#298922=CARTESIAN_POINT('Ctrl Pts',(-10.0514428414942,67.3062499997412,
2.46189346052968E-15));
#298923=CARTESIAN_POINT('Ctrl Pts',(-10.0514428414942,67.4562499997406,
3.26591175476071));
#298924=CARTESIAN_POINT('Ctrl Pts',(-8.13178807675724,67.60624999974,5.90808986649102));
#298925=CARTESIAN_POINT('Ctrl Pts',(-6.21213331202027,67.7562499997395,
8.55026797822134));
#298926=CARTESIAN_POINT('Ctrl Pts',(-3.10606665601016,67.9062499997388,
9.5594902125713));
#298927=CARTESIAN_POINT('Ctrl Pts',(-4.9729987145033E-14,68.0562499997382,
10.5687124469213));
#298928=CARTESIAN_POINT('Ctrl Pts',(3.10606665601006,68.2062499997377,9.5594902125713));
#298929=CARTESIAN_POINT('Ctrl Pts',(6.21213331202017,68.356249999737,8.55026797822134));
#298930=CARTESIAN_POINT('Ctrl Pts',(8.13178807675714,68.5062499997365,5.90808986649102));
#298931=CARTESIAN_POINT('Ctrl Pts',(10.0514428414941,68.6562499997358,3.2659117547607));
#298932=CARTESIAN_POINT('Ctrl Pts',(10.0514428414941,68.8062499997353,-1.23094673026484E-15));
#298933=CARTESIAN_POINT('Ctrl Pts',(10.0514428414941,68.9562499997347,-3.26591175476071));
#298934=CARTESIAN_POINT('Ctrl Pts',(8.13178807675714,69.1062499997341,-5.90808986649102));
#298935=CARTESIAN_POINT('Ctrl Pts',(6.21213331202016,69.2562499997335,-8.55026797822134));
#298936=CARTESIAN_POINT('Ctrl Pts',(3.10606665601005,69.4062499997329,-9.5594902125713));
#298937=CARTESIAN_POINT('Ctrl Pts',(-5.31824297547101E-14,69.5562499997323,
-10.5687124469213));
#298938=CARTESIAN_POINT('Ctrl Pts',(-3.10606665601016,69.7062499997317,
-9.5594902125713));
#298939=CARTESIAN_POINT('Ctrl Pts',(-6.21213331202027,69.856249999731,-8.55026797822134));
#298940=CARTESIAN_POINT('Ctrl Pts',(-8.13178807675724,70.0062499997304,
-5.90808986649102));
#298941=CARTESIAN_POINT('Ctrl Pts',(-10.0514428414942,70.1562499997298,
-3.2659117547607));
#298942=CARTESIAN_POINT('Ctrl Pts',(-10.0514428414942,70.3062499997292,
2.46189346052968E-15));
#298943=CARTESIAN_POINT('Ctrl Pts',(-10.0514428414942,70.4562499997286,
3.26591175476071));
#298944=CARTESIAN_POINT('Ctrl Pts',(-8.13178807675724,70.606249999728,5.90808986649102));
#298945=CARTESIAN_POINT('Ctrl Pts',(-6.21213331202027,70.7562499997274,
8.55026797822134));
#298946=CARTESIAN_POINT('Ctrl Pts',(-3.10606665601016,70.9062499997269,
9.5594902125713));
#298947=CARTESIAN_POINT('Ctrl Pts',(-5.14576964166948E-14,71.0562499997262,
10.5687124469213));
#298948=CARTESIAN_POINT('Ctrl Pts',(3.10606665601006,71.2062499997256,9.5594902125713));
#298949=CARTESIAN_POINT('Ctrl Pts',(6.21213331202016,71.3562499997251,8.55026797822134));
#298950=CARTESIAN_POINT('Ctrl Pts',(8.13178807675714,71.5062499997244,5.90808986649102));
#298951=CARTESIAN_POINT('Ctrl Pts',(10.0514428414941,71.6562499997239,3.2659117547607));
#298952=CARTESIAN_POINT('Ctrl Pts',(10.0514428414941,71.8062499997232,-1.23094673026484E-15));
#298953=CARTESIAN_POINT('Ctrl Pts',(10.0514428414941,71.9562499997227,-3.26591175476071));
#298954=CARTESIAN_POINT('Ctrl Pts',(8.13178807675713,72.1062499997221,-5.90808986649102));
#298955=CARTESIAN_POINT('Ctrl Pts',(6.21213331202016,72.2562499997215,-8.55026797822134));
#298956=CARTESIAN_POINT('Ctrl Pts',(3.10606665601005,72.4062499997209,-9.5594902125713));
#298957=CARTESIAN_POINT('Ctrl Pts',(-5.49101390263719E-14,72.5562499997203,
-10.5687124469213));
#298958=CARTESIAN_POINT('Ctrl Pts',(-3.10606665601016,72.7062499997197,
-9.5594902125713));
#298959=CARTESIAN_POINT('Ctrl Pts',(-6.21213331202027,72.8562499997191,
-8.55026797822134));
#298960=CARTESIAN_POINT('Ctrl Pts',(-8.13178807675725,73.0062499997184,
-5.90808986649102));
#298961=CARTESIAN_POINT('Ctrl Pts',(-10.0514428414942,73.1562499997178,
-3.2659117547607));
#298962=CARTESIAN_POINT('Ctrl Pts',(-10.0514428414942,73.3062499997172,
2.46189346052968E-15));
#298963=CARTESIAN_POINT('Ctrl Pts',(-10.0514428414942,73.4562499997166,
3.26591175476071));
#298964=CARTESIAN_POINT('Ctrl Pts',(-8.13178807675725,73.606249999716,5.90808986649102));
#298965=CARTESIAN_POINT('Ctrl Pts',(-6.21213331202027,73.7562499997155,
8.55026797822134));
#298966=CARTESIAN_POINT('Ctrl Pts',(-3.10606665601016,73.9062499997148,
9.5594902125713));
#298967=CARTESIAN_POINT('Ctrl Pts',(-5.31854056883567E-14,74.0562499997143,
10.5687124469213));
#298968=CARTESIAN_POINT('Ctrl Pts',(3.10606665601005,74.2062499997136,9.5594902125713));
#298969=CARTESIAN_POINT('Ctrl Pts',(6.21213331202016,74.3562499997131,8.55026797822134));
#298970=CARTESIAN_POINT('Ctrl Pts',(8.13178807675713,74.5062499997125,5.90808986649102));
#298971=CARTESIAN_POINT('Ctrl Pts',(10.0514428414941,74.6562499997118,3.2659117547607));
#298972=CARTESIAN_POINT('Ctrl Pts',(10.0514428414941,74.8062499997113,-1.23094673026484E-15));
#298973=CARTESIAN_POINT('Ctrl Pts',(10.0514428414941,74.9562499997106,-3.26591175476071));
#298974=CARTESIAN_POINT('Ctrl Pts',(8.13178807675713,75.10624999971,-5.90808986649102));
#298975=CARTESIAN_POINT('Ctrl Pts',(6.21213331202016,75.2562499997094,-8.55026797822134));
#298976=CARTESIAN_POINT('Ctrl Pts',(3.10606665601005,75.4062499997088,-9.5594902125713));
#298977=CARTESIAN_POINT('Ctrl Pts',(-5.66378482980338E-14,75.5562499997083,
-10.5687124469213));
#298978=CARTESIAN_POINT('Ctrl Pts',(-3.10606665601016,75.7062499997077,
-9.5594902125713));
#298979=CARTESIAN_POINT('Ctrl Pts',(-6.21213331202027,75.856249999707,-8.55026797822134));
#298980=CARTESIAN_POINT('Ctrl Pts',(-8.13178807675725,76.0062499997065,
-5.90808986649102));
#298981=CARTESIAN_POINT('Ctrl Pts',(-10.0514428414942,76.1562499997058,
-3.2659117547607));
#298982=CARTESIAN_POINT('Ctrl Pts',(-10.0514428414942,76.3062499997052,
2.46189346052968E-15));
#298983=CARTESIAN_POINT('Ctrl Pts',(-10.0514428414942,76.4562499997046,
3.26591175476071));
#298984=CARTESIAN_POINT('Ctrl Pts',(-8.13178807675725,76.606249999704,5.90808986649102));
#298985=CARTESIAN_POINT('Ctrl Pts',(-6.21213331202027,76.7562499997035,
8.55026797822134));
#298986=CARTESIAN_POINT('Ctrl Pts',(-3.10606665601016,76.9062499997029,
9.5594902125713));
#298987=CARTESIAN_POINT('Ctrl Pts',(-5.49131149600185E-14,77.0562499997022,
10.5687124469213));
#298988=CARTESIAN_POINT('Ctrl Pts',(3.10606665601005,77.2062499997016,9.5594902125713));
#298989=CARTESIAN_POINT('Ctrl Pts',(6.21213331202016,77.356249999701,8.55026797822134));
#298990=CARTESIAN_POINT('Ctrl Pts',(8.13178807675713,77.5062499997004,5.90808986649102));
#298991=CARTESIAN_POINT('Ctrl Pts',(10.0514428414941,77.6562499996998,3.2659117547607));
#298992=CARTESIAN_POINT('Ctrl Pts',(10.0514428414941,77.8062499996992,-1.23094673026484E-15));
#298993=CARTESIAN_POINT('Ctrl Pts',(10.0514428414941,77.9562499996987,-3.26591175476071));
#298994=CARTESIAN_POINT('Ctrl Pts',(8.13178807675713,78.1062499996981,-5.90808986649102));
#298995=CARTESIAN_POINT('Ctrl Pts',(6.21213331202016,78.2562499996974,-8.55026797822134));
#298996=CARTESIAN_POINT('Ctrl Pts',(3.10606665601005,78.4062499996969,-9.5594902125713));
#298997=CARTESIAN_POINT('Ctrl Pts',(-5.83655575696956E-14,78.5562499996963,
-10.5687124469213));
#298998=CARTESIAN_POINT('Ctrl Pts',(-3.10606665601017,78.7062499996957,
-9.5594902125713));
#298999=CARTESIAN_POINT('Ctrl Pts',(-6.21213331202028,78.8562499996951,
-8.55026797822134));
#299000=CARTESIAN_POINT('Ctrl Pts',(-8.13178807675725,79.0062499996944,
-5.90808986649102));
#299001=CARTESIAN_POINT('Ctrl Pts',(-10.0514428414942,79.1562499996939,
-3.2659117547607));
#299002=CARTESIAN_POINT('Ctrl Pts',(-10.0514428414942,79.3062499996932,
2.46189346052968E-15));
#299003=CARTESIAN_POINT('Ctrl Pts',(-10.0514428414942,79.4562499996926,
3.26591175476071));
#299004=CARTESIAN_POINT('Ctrl Pts',(-8.13178807675725,79.606249999692,5.90808986649102));
#299005=CARTESIAN_POINT('Ctrl Pts',(-6.21213331202027,79.7562499996915,
8.55026797822134));
#299006=CARTESIAN_POINT('Ctrl Pts',(-3.10606665601016,79.9062499996908,
9.5594902125713));
#299007=CARTESIAN_POINT('Ctrl Pts',(-5.66408242316803E-14,80.0562499996902,
10.5687124469213));
#299008=CARTESIAN_POINT('Ctrl Pts',(3.10606665601005,80.2062499996896,9.5594902125713));
#299009=CARTESIAN_POINT('Ctrl Pts',(6.21213331202016,80.356249999689,8.55026797822134));
#299010=CARTESIAN_POINT('Ctrl Pts',(8.13178807675713,80.5062499996884,5.90808986649102));
#299011=CARTESIAN_POINT('Ctrl Pts',(10.0514428414941,80.6562499996878,3.2659117547607));
#299012=CARTESIAN_POINT('Ctrl Pts',(10.0514428414941,80.8062499996873,-1.23094673026484E-15));
#299013=CARTESIAN_POINT('Ctrl Pts',(10.0514428414941,80.9562499996866,-3.26591175476071));
#299014=CARTESIAN_POINT('Ctrl Pts',(8.13178807675713,81.1062499996861,-5.90808986649102));
#299015=CARTESIAN_POINT('Ctrl Pts',(6.21213331202016,81.2562499996854,-8.55026797822134));
#299016=CARTESIAN_POINT('Ctrl Pts',(3.10606665601005,81.4062499996849,-9.5594902125713));
#299017=CARTESIAN_POINT('Ctrl Pts',(-6.00932668413574E-14,81.5562499996843,
-10.5687124469213));
#299018=CARTESIAN_POINT('Ctrl Pts',(-3.10606665601017,81.7062499996837,
-9.5594902125713));
#299019=CARTESIAN_POINT('Ctrl Pts',(-6.21213331202028,81.856249999683,-8.55026797822134));
#299020=CARTESIAN_POINT('Ctrl Pts',(-8.13178807675725,82.0062499996824,
-5.90808986649102));
#299021=CARTESIAN_POINT('Ctrl Pts',(-10.0514428414942,82.1562499996818,
-3.2659117547607));
#299022=CARTESIAN_POINT('Ctrl Pts',(-10.0514428414942,82.3062499996813,
2.46189346052968E-15));
#299023=CARTESIAN_POINT('Ctrl Pts',(-10.0514428414942,82.4562499996806,
3.26591175476071));
#299024=CARTESIAN_POINT('Ctrl Pts',(-8.13178807675725,82.60624999968,5.90808986649102));
#299025=CARTESIAN_POINT('Ctrl Pts',(-6.21213331202028,82.7562499996795,
8.55026797822134));
#299026=CARTESIAN_POINT('Ctrl Pts',(-3.10606665601017,82.9062499996789,
9.5594902125713));
#299027=CARTESIAN_POINT('Ctrl Pts',(-5.83685335033422E-14,83.0562499996782,
10.5687124469213));
#299028=CARTESIAN_POINT('Ctrl Pts',(3.10606665601005,83.2062499996776,9.5594902125713));
#299029=CARTESIAN_POINT('Ctrl Pts',(6.21213331202016,83.356249999677,8.55026797822134));
#299030=CARTESIAN_POINT('Ctrl Pts',(8.13178807675713,83.5062499996764,5.90808986649102));
#299031=CARTESIAN_POINT('Ctrl Pts',(10.0514428414941,83.6562499996759,3.2659117547607));
#299032=CARTESIAN_POINT('Ctrl Pts',(10.0514428414941,83.8062499996752,-1.23094673026484E-15));
#299033=CARTESIAN_POINT('Ctrl Pts',(10.0514428414941,83.9562499996747,-3.26591175476071));
#299034=CARTESIAN_POINT('Ctrl Pts',(8.13178807675713,84.106249999674,-5.90808986649102));
#299035=CARTESIAN_POINT('Ctrl Pts',(6.21213331202016,84.2562499996734,-8.55026797822134));
#299036=CARTESIAN_POINT('Ctrl Pts',(3.10606665601005,84.4062499996729,-9.5594902125713));
#299037=CARTESIAN_POINT('Ctrl Pts',(-6.18209761130193E-14,84.5562499996723,
-10.5687124469213));
#299038=CARTESIAN_POINT('Ctrl Pts',(-3.10606665601017,84.7062499996717,
-9.5594902125713));
#299039=CARTESIAN_POINT('Ctrl Pts',(-6.21213331202028,84.856249999671,-8.55026797822134));
#299040=CARTESIAN_POINT('Ctrl Pts',(-8.13178807675725,85.0062499996704,
-5.90808986649102));
#299041=CARTESIAN_POINT('Ctrl Pts',(-10.0514428414942,85.1562499996699,
-3.2659117547607));
#299042=CARTESIAN_POINT('Ctrl Pts',(-10.0514428414942,85.3062499996692,
2.46189346052968E-15));
#299043=CARTESIAN_POINT('Ctrl Pts',(-10.0514428414942,85.4562499996686,
3.26591175476071));
#299044=CARTESIAN_POINT('Ctrl Pts',(-8.13178807675725,85.606249999668,5.90808986649102));
#299045=CARTESIAN_POINT('Ctrl Pts',(-6.21213331202028,85.7562499996675,
8.55026797822134));
#299046=CARTESIAN_POINT('Ctrl Pts',(-3.10606665601017,85.9062499996669,
9.5594902125713));
#299047=CARTESIAN_POINT('Ctrl Pts',(-6.0096242775004E-14,86.0562499996662,
10.5687124469213));
#299048=CARTESIAN_POINT('Ctrl Pts',(3.10606665601005,86.2062499996657,9.5594902125713));
#299049=CARTESIAN_POINT('Ctrl Pts',(6.21213331202016,86.3562499996651,8.55026797822134));
#299050=CARTESIAN_POINT('Ctrl Pts',(8.13178807675713,86.5062499996644,5.90808986649102));
#299051=CARTESIAN_POINT('Ctrl Pts',(10.0514428414941,86.6562499996638,3.2659117547607));
#299052=CARTESIAN_POINT('Ctrl Pts',(10.0514428414941,86.8062499996633,-1.23094673026484E-15));
#299053=CARTESIAN_POINT('Ctrl Pts',(10.0514428414941,86.9562499996626,-3.26591175476071));
#299054=CARTESIAN_POINT('Ctrl Pts',(8.13178807675713,87.1062499996621,-5.90808986649102));
#299055=CARTESIAN_POINT('Ctrl Pts',(6.21213331202015,87.2562499996614,-8.55026797822134));
#299056=CARTESIAN_POINT('Ctrl Pts',(3.10606665601004,87.4062499996609,-9.5594902125713));
#299057=CARTESIAN_POINT('Ctrl Pts',(-6.35486853846811E-14,87.5562499996603,
-10.5687124469213));
#299058=CARTESIAN_POINT('Ctrl Pts',(-3.10606665601017,87.7062499996597,
-9.5594902125713));
#299059=CARTESIAN_POINT('Ctrl Pts',(-6.21213331202028,87.856249999659,-8.55026797822134));
#299060=CARTESIAN_POINT('Ctrl Pts',(-8.13178807675726,88.0062499996585,
-5.90808986649102));
#299061=CARTESIAN_POINT('Ctrl Pts',(-10.0514428414942,88.1562499996578,
-3.2659117547607));
#299062=CARTESIAN_POINT('Ctrl Pts',(-10.0514428414942,88.3062499996572,
2.46189346052968E-15));
#299063=CARTESIAN_POINT('Ctrl Pts',(-10.0514428414942,88.4562499996566,
3.26591175476071));
#299064=CARTESIAN_POINT('Ctrl Pts',(-8.13178807675726,88.6062499996561,
5.90808986649102));
#299065=CARTESIAN_POINT('Ctrl Pts',(-6.21213331202028,88.7562499996555,
8.55026797822134));
#299066=CARTESIAN_POINT('Ctrl Pts',(-3.10606665601017,88.9062499996548,
9.5594902125713));
#299067=CARTESIAN_POINT('Ctrl Pts',(-6.18239520466659E-14,89.0562499996542,
10.5687124469213));
#299068=CARTESIAN_POINT('Ctrl Pts',(3.10606665601005,89.2062499996537,9.5594902125713));
#299069=CARTESIAN_POINT('Ctrl Pts',(6.21213331202016,89.3562499996531,8.55026797822134));
#299070=CARTESIAN_POINT('Ctrl Pts',(8.13178807675713,89.5062499996525,5.90808986649102));
#299071=CARTESIAN_POINT('Ctrl Pts',(10.0514428414941,89.6562499996518,3.2659117547607));
#299072=CARTESIAN_POINT('Ctrl Pts',(10.0514428414941,89.8062499996512,-1.23094673026484E-15));
#299073=CARTESIAN_POINT('Ctrl Pts',(10.0514428414941,89.9562499996507,-3.26591175476071));
#299074=CARTESIAN_POINT('Ctrl Pts',(8.13178807675713,90.10624999965,-5.90808986649102));
#299075=CARTESIAN_POINT('Ctrl Pts',(6.21213331202015,90.2562499996494,-8.55026797822134));
#299076=CARTESIAN_POINT('Ctrl Pts',(3.10606665601004,90.4062499996488,-9.5594902125713));
#299077=CARTESIAN_POINT('Ctrl Pts',(-6.52763946563429E-14,90.5562499996483,
-10.5687124469213));
#299078=CARTESIAN_POINT('Ctrl Pts',(-3.10606665601017,90.7062499996476,
-9.5594902125713));
#299079=CARTESIAN_POINT('Ctrl Pts',(-6.21213331202028,90.856249999647,-8.55026797822134));
#299080=CARTESIAN_POINT('Ctrl Pts',(-8.13178807675726,91.0062499996464,
-5.90808986649102));
#299081=CARTESIAN_POINT('Ctrl Pts',(-10.0514428414942,91.1562499996458,
-3.2659117547607));
#299082=CARTESIAN_POINT('Ctrl Pts',(-10.0514428414942,91.3062499996452,
2.46189346052968E-15));
#299083=CARTESIAN_POINT('Ctrl Pts',(-10.0514428414942,91.4562499996446,
3.26591175476071));
#299084=CARTESIAN_POINT('Ctrl Pts',(-8.13178807675726,91.606249999644,5.90808986649102));
#299085=CARTESIAN_POINT('Ctrl Pts',(-6.21213331202028,91.7562499996434,
8.55026797822134));
#299086=CARTESIAN_POINT('Ctrl Pts',(-3.10606665601017,91.9062499996429,
9.5594902125713));
#299087=CARTESIAN_POINT('Ctrl Pts',(-6.35516613183277E-14,92.0562499996422,
10.5687124469213));
#299088=CARTESIAN_POINT('Ctrl Pts',(3.10606665601004,92.2062499996417,9.5594902125713));
#299089=CARTESIAN_POINT('Ctrl Pts',(6.21213331202015,92.3562499996411,8.55026797822134));
#299090=CARTESIAN_POINT('Ctrl Pts',(8.13178807675712,92.5062499996404,5.90808986649102));
#299091=CARTESIAN_POINT('Ctrl Pts',(10.0514428414941,92.6562499996398,3.2659117547607));
#299092=CARTESIAN_POINT('Ctrl Pts',(10.0514428414941,92.8062499996392,-1.23094673026484E-15));
#299093=CARTESIAN_POINT('Ctrl Pts',(10.0514428414941,92.9562499996387,-3.26591175476071));
#299094=CARTESIAN_POINT('Ctrl Pts',(8.13178807675712,93.1062499996381,-5.90808986649102));
#299095=CARTESIAN_POINT('Ctrl Pts',(6.21213331202015,93.2562499996374,-8.55026797822134));
#299096=CARTESIAN_POINT('Ctrl Pts',(3.10606665601004,93.4062499996369,-9.5594902125713));
#299097=CARTESIAN_POINT('Ctrl Pts',(-6.70041039280048E-14,93.5562499996362,
-10.5687124469213));
#299098=CARTESIAN_POINT('Ctrl Pts',(-3.10606665601018,93.7062499996357,
-9.5594902125713));
#299099=CARTESIAN_POINT('Ctrl Pts',(-6.21213331202028,93.856249999635,-8.55026797822134));
#299100=CARTESIAN_POINT('Ctrl Pts',(-8.13178807675726,94.0062499996344,
-5.90808986649102));
#299101=CARTESIAN_POINT('Ctrl Pts',(-10.0514428414942,94.1562499996338,
-3.2659117547607));
#299102=CARTESIAN_POINT('Ctrl Pts',(-10.0514428414942,94.3062499996333,
2.46189346052968E-15));
#299103=CARTESIAN_POINT('Ctrl Pts',(-10.0514428414942,94.4562499996326,
3.26591175476071));
#299104=CARTESIAN_POINT('Ctrl Pts',(-8.13178807675726,94.606249999632,5.90808986649102));
#299105=CARTESIAN_POINT('Ctrl Pts',(-6.21213331202028,94.7562499996315,
8.55026797822134));
#299106=CARTESIAN_POINT('Ctrl Pts',(-3.10606665601017,94.9062499996309,
9.5594902125713));
#299107=CARTESIAN_POINT('Ctrl Pts',(-6.52793705899895E-14,95.0562499996302,
10.5687124469213));
#299108=CARTESIAN_POINT('Ctrl Pts',(3.10606665601004,95.2062499996296,9.5594902125713));
#299109=CARTESIAN_POINT('Ctrl Pts',(6.21213331202015,95.3562499996291,8.55026797822134));
#299110=CARTESIAN_POINT('Ctrl Pts',(8.13178807675712,95.5062499996285,5.90808986649102));
#299111=CARTESIAN_POINT('Ctrl Pts',(10.0514428414941,95.6562499996278,3.2659117547607));
#299112=CARTESIAN_POINT('Ctrl Pts',(10.0514428414941,95.8062499996273,-1.23094673026484E-15));
#299113=CARTESIAN_POINT('Ctrl Pts',(10.0514428414941,95.9562499996266,-3.26591175476071));
#299114=CARTESIAN_POINT('Ctrl Pts',(8.13178807675712,96.1062499996261,-5.90808986649102));
#299115=CARTESIAN_POINT('Ctrl Pts',(6.21213331202015,96.2562499996255,-8.55026797822134));
#299116=CARTESIAN_POINT('Ctrl Pts',(3.10606665601004,96.4062499996248,-9.5594902125713));
#299117=CARTESIAN_POINT('Ctrl Pts',(-6.87318131996666E-14,96.5562499996243,
-10.5687124469213));
#299118=CARTESIAN_POINT('Ctrl Pts',(-3.10606665601018,96.7062499996236,
-9.5594902125713));
#299119=CARTESIAN_POINT('Ctrl Pts',(-6.21213331202028,96.856249999623,-8.55026797822134));
#299120=CARTESIAN_POINT('Ctrl Pts',(-8.13178807675726,97.0062499996224,
-5.90808986649102));
#299121=CARTESIAN_POINT('Ctrl Pts',(-10.0514428414942,97.1562499996218,
-3.2659117547607));
#299122=CARTESIAN_POINT('Ctrl Pts',(-10.0514428414942,97.3062499996212,
2.46189346052968E-15));
#299123=CARTESIAN_POINT('Ctrl Pts',(-10.0514428414942,97.4562499996206,
3.26591175476071));
#299124=CARTESIAN_POINT('Ctrl Pts',(-8.13178807675726,97.60624999962,5.90808986649102));
#299125=CARTESIAN_POINT('Ctrl Pts',(-6.21213331202028,97.7562499996195,
8.55026797822134));
#299126=CARTESIAN_POINT('Ctrl Pts',(-3.10606665601018,97.9062499996189,
9.5594902125713));
#299127=CARTESIAN_POINT('Ctrl Pts',(-6.70070798616514E-14,98.0562499996182,
10.5687124469213));
#299128=CARTESIAN_POINT('Ctrl Pts',(3.10606665601004,98.2062499996177,9.5594902125713));
#299129=CARTESIAN_POINT('Ctrl Pts',(6.21213331202015,98.3562499996171,8.55026797822134));
#299130=CARTESIAN_POINT('Ctrl Pts',(8.13178807675712,98.5062499996165,5.90808986649102));
#299131=CARTESIAN_POINT('Ctrl Pts',(10.0514428414941,98.6562499996158,3.2659117547607));
#299132=CARTESIAN_POINT('Ctrl Pts',(10.0514428414941,98.8062499996153,-1.23094673026484E-15));
#299133=CARTESIAN_POINT('Ctrl Pts',(10.0514428414941,98.9562499996147,-3.26591175476071));
#299134=CARTESIAN_POINT('Ctrl Pts',(8.13178807675712,99.1062499996141,-5.90808986649102));
#299135=CARTESIAN_POINT('Ctrl Pts',(6.21213331202015,99.2562499996134,-8.55026797822134));
#299136=CARTESIAN_POINT('Ctrl Pts',(3.10606665601004,99.4062499996129,-9.5594902125713));
#299137=CARTESIAN_POINT('Ctrl Pts',(-7.04595224713284E-14,99.5562499996123,
-10.5687124469213));
#299138=CARTESIAN_POINT('Ctrl Pts',(-3.10606665601018,99.7062499996117,
-9.5594902125713));
#299139=CARTESIAN_POINT('Ctrl Pts',(-6.21213331202028,99.856249999611,-8.55026797822134));
#299140=CARTESIAN_POINT('Ctrl Pts',(-8.13178807675726,100.00624999961,-5.90808986649102));
#299141=CARTESIAN_POINT('Ctrl Pts',(-10.0514428414942,100.15624999961,-3.2659117547607));
#299142=CARTESIAN_POINT('Ctrl Pts',(-10.0514428414942,100.306249999609,
2.46189346052968E-15));
#299143=CARTESIAN_POINT('Ctrl Pts',(-10.0514428414942,100.456249999609,
3.26591175476071));
#299144=CARTESIAN_POINT('Ctrl Pts',(-8.13178807675726,100.606249999608,
5.90808986649102));
#299145=CARTESIAN_POINT('Ctrl Pts',(-6.21213331202028,100.756249999607,
8.55026797822134));
#299146=CARTESIAN_POINT('Ctrl Pts',(-3.10606665601018,100.906249999607,
9.5594902125713));
#299147=CARTESIAN_POINT('Ctrl Pts',(-6.87347891333132E-14,101.056249999606,
10.5687124469213));
#299148=CARTESIAN_POINT('Ctrl Pts',(3.10606665601004,101.206249999606,9.5594902125713));
#299149=CARTESIAN_POINT('Ctrl Pts',(6.21213331202015,101.356249999605,8.55026797822134));
#299150=CARTESIAN_POINT('Ctrl Pts',(8.13178807675712,101.506249999604,5.90808986649102));
#299151=CARTESIAN_POINT('Ctrl Pts',(10.0514428414941,101.656249999604,3.2659117547607));
#299152=CARTESIAN_POINT('Ctrl Pts',(10.0514428414941,101.806249999603,-1.23094673026484E-15));
#299153=CARTESIAN_POINT('Ctrl Pts',(10.0514428414941,101.956249999603,-3.26591175476071));
#299154=CARTESIAN_POINT('Ctrl Pts',(8.13178807675712,102.106249999602,-5.90808986649102));
#299155=CARTESIAN_POINT('Ctrl Pts',(6.21213331202014,102.256249999601,-8.55026797822134));
#299156=CARTESIAN_POINT('Ctrl Pts',(3.10606665601004,102.406249999601,-9.5594902125713));
#299157=CARTESIAN_POINT('Ctrl Pts',(-7.21872317429903E-14,102.5562499996,
-10.5687124469213));
#299158=CARTESIAN_POINT('Ctrl Pts',(-3.10606665601018,102.7062499996,-9.5594902125713));
#299159=CARTESIAN_POINT('Ctrl Pts',(-6.21213331202029,102.856249999599,
-8.55026797822134));
#299160=CARTESIAN_POINT('Ctrl Pts',(-8.13178807675726,103.006249999598,
-5.90808986649102));
#299161=CARTESIAN_POINT('Ctrl Pts',(-10.0514428414942,103.156249999598,
-3.2659117547607));
#299162=CARTESIAN_POINT('Ctrl Pts',(-10.0514428414942,103.306249999597,
2.46189346052968E-15));
#299163=CARTESIAN_POINT('Ctrl Pts',(-10.0514428414942,103.456249999597,
3.26591175476071));
#299164=CARTESIAN_POINT('Ctrl Pts',(-8.13178807675726,103.606249999596,
5.90808986649102));
#299165=CARTESIAN_POINT('Ctrl Pts',(-6.21213331202028,103.756249999595,
8.55026797822134));
#299166=CARTESIAN_POINT('Ctrl Pts',(-3.10606665601018,103.906249999595,
9.5594902125713));
#299167=CARTESIAN_POINT('Ctrl Pts',(-7.04624984049751E-14,104.056249999594,
10.5687124469213));
#299168=CARTESIAN_POINT('Ctrl Pts',(3.10606665601004,104.206249999594,9.5594902125713));
#299169=CARTESIAN_POINT('Ctrl Pts',(6.21213331202015,104.356249999593,8.55026797822134));
#299170=CARTESIAN_POINT('Ctrl Pts',(8.13178807675712,104.506249999592,5.90808986649102));
#299171=CARTESIAN_POINT('Ctrl Pts',(10.0514428414941,104.656249999592,3.2659117547607));
#299172=CARTESIAN_POINT('Ctrl Pts',(10.0514428414941,104.806249999591,-1.23094673026484E-15));
#299173=CARTESIAN_POINT('Ctrl Pts',(10.0514428414941,104.956249999591,-3.26591175476071));
#299174=CARTESIAN_POINT('Ctrl Pts',(8.13178807675712,105.10624999959,-5.90808986649102));
#299175=CARTESIAN_POINT('Ctrl Pts',(6.21213331202014,105.256249999589,-8.55026797822134));
#299176=CARTESIAN_POINT('Ctrl Pts',(3.10606665601003,105.406249999589,-9.5594902125713));
#299177=CARTESIAN_POINT('Ctrl Pts',(-7.39149410146522E-14,105.556249999588,
-10.5687124469213));
#299178=CARTESIAN_POINT('Ctrl Pts',(-3.10606665601018,105.706249999588,
-9.5594902125713));
#299179=CARTESIAN_POINT('Ctrl Pts',(-6.21213331202029,105.856249999587,
-8.55026797822134));
#299180=CARTESIAN_POINT('Ctrl Pts',(-8.13178807675726,106.006249999586,
-5.90808986649102));
#299181=CARTESIAN_POINT('Ctrl Pts',(-10.0514428414942,106.156249999586,
-3.2659117547607));
#299182=CARTESIAN_POINT('Ctrl Pts',(-10.0514428414942,106.306249999585,
2.46189346052968E-15));
#299183=CARTESIAN_POINT('Ctrl Pts',(-10.0514428414942,106.456249999585,
3.26591175476071));
#299184=CARTESIAN_POINT('Ctrl Pts',(-8.13178807675726,106.606249999584,
5.90808986649102));
#299185=CARTESIAN_POINT('Ctrl Pts',(-6.21213331202029,106.756249999583,
8.55026797822134));
#299186=CARTESIAN_POINT('Ctrl Pts',(-3.10606665601018,106.906249999583,
9.5594902125713));
#299187=CARTESIAN_POINT('Ctrl Pts',(-7.21902076766369E-14,107.056249999582,
10.5687124469213));
#299188=CARTESIAN_POINT('Ctrl Pts',(3.10606665601003,107.206249999582,9.5594902125713));
#299189=CARTESIAN_POINT('Ctrl Pts',(6.21213331202014,107.356249999581,8.55026797822134));
#299190=CARTESIAN_POINT('Ctrl Pts',(8.13178807675711,107.50624999958,5.90808986649102));
#299191=CARTESIAN_POINT('Ctrl Pts',(10.0514428414941,107.65624999958,3.2659117547607));
#299192=CARTESIAN_POINT('Ctrl Pts',(10.0514428414941,107.806249999579,-1.23094673026484E-15));
#299193=CARTESIAN_POINT('Ctrl Pts',(10.0514428414941,107.956249999579,-3.26591175476071));
#299194=CARTESIAN_POINT('Ctrl Pts',(8.13178807675711,108.106249999578,-5.90808986649102));
#299195=CARTESIAN_POINT('Ctrl Pts',(6.21213331202014,108.256249999577,-8.55026797822134));
#299196=CARTESIAN_POINT('Ctrl Pts',(3.10606665601003,108.406249999577,-9.5594902125713));
#299197=CARTESIAN_POINT('Ctrl Pts',(-7.5642650286314E-14,108.556249999576,
-10.5687124469213));
#299198=CARTESIAN_POINT('Ctrl Pts',(-3.10606665601018,108.706249999576,
-9.5594902125713));
#299199=CARTESIAN_POINT('Ctrl Pts',(-6.21213331202029,108.856249999575,
-8.55026797822134));
#299200=CARTESIAN_POINT('Ctrl Pts',(-8.13178807675727,109.006249999574,
-5.90808986649102));
#299201=CARTESIAN_POINT('Ctrl Pts',(-10.0514428414942,109.156249999574,
-3.2659117547607));
#299202=CARTESIAN_POINT('Ctrl Pts',(-10.0514428414942,109.306249999573,
2.46189346052968E-15));
#299203=CARTESIAN_POINT('Ctrl Pts',(-10.0514428414942,109.456249999573,
3.26591175476071));
#299204=CARTESIAN_POINT('Ctrl Pts',(-8.13178807675727,109.606249999572,
5.90808986649102));
#299205=CARTESIAN_POINT('Ctrl Pts',(-6.21213331202029,109.756249999571,
8.55026797822134));
#299206=CARTESIAN_POINT('Ctrl Pts',(-3.10606665601018,109.906249999571,
9.5594902125713));
#299207=CARTESIAN_POINT('Ctrl Pts',(-7.39179169482987E-14,110.05624999957,
10.5687124469213));
#299208=CARTESIAN_POINT('Ctrl Pts',(3.10606665601003,110.20624999957,9.5594902125713));
#299209=CARTESIAN_POINT('Ctrl Pts',(6.21213331202014,110.356249999569,8.55026797822134));
#299210=CARTESIAN_POINT('Ctrl Pts',(8.13178807675711,110.506249999568,5.90808986649102));
#299211=CARTESIAN_POINT('Ctrl Pts',(10.0514428414941,110.656249999568,3.2659117547607));
#299212=CARTESIAN_POINT('Ctrl Pts',(10.0514428414941,110.806249999567,-1.23094673026484E-15));
#299213=CARTESIAN_POINT('Ctrl Pts',(10.0514428414941,110.956249999567,-3.26591175476071));
#299214=CARTESIAN_POINT('Ctrl Pts',(8.13178807675711,111.106249999566,-5.90808986649102));
#299215=CARTESIAN_POINT('Ctrl Pts',(6.21213331202014,111.256249999565,-8.55026797822134));
#299216=CARTESIAN_POINT('Ctrl Pts',(3.10606665601003,111.406249999565,-9.5594902125713));
#299217=CARTESIAN_POINT('Ctrl Pts',(-7.73703595579758E-14,111.556249999564,
-10.5687124469213));
#299218=CARTESIAN_POINT('Ctrl Pts',(-3.10606665601019,111.706249999564,
-9.5594902125713));
#299219=CARTESIAN_POINT('Ctrl Pts',(-6.21213331202029,111.856249999563,
-8.55026797822134));
#299220=CARTESIAN_POINT('Ctrl Pts',(-8.13178807675727,112.006249999562,
-5.90808986649102));
#299221=CARTESIAN_POINT('Ctrl Pts',(-10.0514428414942,112.156249999562,
-3.2659117547607));
#299222=CARTESIAN_POINT('Ctrl Pts',(-10.0514428414942,112.306249999561,
2.46189346052968E-15));
#299223=CARTESIAN_POINT('Ctrl Pts',(-10.0514428414942,112.456249999561,
3.26591175476071));
#299224=CARTESIAN_POINT('Ctrl Pts',(-8.13178807675727,112.60624999956,5.90808986649102));
#299225=CARTESIAN_POINT('Ctrl Pts',(-6.21213331202029,112.756249999559,
8.55026797822134));
#299226=CARTESIAN_POINT('Ctrl Pts',(-3.10606665601018,112.906249999559,
9.5594902125713));
#299227=CARTESIAN_POINT('Ctrl Pts',(-7.56456262199606E-14,113.056249999558,
10.5687124469213));
#299228=CARTESIAN_POINT('Ctrl Pts',(3.10606665601003,113.206249999558,9.5594902125713));
#299229=CARTESIAN_POINT('Ctrl Pts',(6.21213331202014,113.356249999557,8.55026797822134));
#299230=CARTESIAN_POINT('Ctrl Pts',(8.13178807675711,113.506249999556,5.90808986649102));
#299231=CARTESIAN_POINT('Ctrl Pts',(10.0514428414941,113.656249999556,3.2659117547607));
#299232=CARTESIAN_POINT('Ctrl Pts',(10.0514428414941,113.806249999555,-1.23094673026484E-15));
#299233=CARTESIAN_POINT('Ctrl Pts',(10.0514428414941,113.956249999555,-3.26591175476071));
#299234=CARTESIAN_POINT('Ctrl Pts',(8.13178807675711,114.106249999554,-5.90808986649102));
#299235=CARTESIAN_POINT('Ctrl Pts',(6.21213331202014,114.256249999553,-8.55026797822134));
#299236=CARTESIAN_POINT('Ctrl Pts',(3.10606665601003,114.406249999553,-9.5594902125713));
#299237=CARTESIAN_POINT('Ctrl Pts',(-7.90980688296377E-14,114.556249999552,
-10.5687124469213));
#299238=CARTESIAN_POINT('Ctrl Pts',(-3.10606665601019,114.706249999552,
-9.5594902125713));
#299239=CARTESIAN_POINT('Ctrl Pts',(-6.2121333120203,114.856249999551,-8.55026797822134));
#299240=CARTESIAN_POINT('Ctrl Pts',(-8.13178807675727,115.00624999955,-5.90808986649102));
#299241=CARTESIAN_POINT('Ctrl Pts',(-10.0514428414942,115.15624999955,-3.2659117547607));
#299242=CARTESIAN_POINT('Ctrl Pts',(-10.0514428414942,115.306249999549,
2.46189346052968E-15));
#299243=CARTESIAN_POINT('Ctrl Pts',(-10.0514428414942,115.456249999549,
3.26591175476071));
#299244=CARTESIAN_POINT('Ctrl Pts',(-8.13178807675727,115.606249999548,
5.90808986649102));
#299245=CARTESIAN_POINT('Ctrl Pts',(-6.21213331202029,115.756249999547,
8.55026797822134));
#299246=CARTESIAN_POINT('Ctrl Pts',(-3.10606665601019,115.906249999547,
9.5594902125713));
#299247=CARTESIAN_POINT('Ctrl Pts',(-7.73733354916224E-14,116.056249999546,
10.5687124469213));
#299248=CARTESIAN_POINT('Ctrl Pts',(3.10606665601003,116.206249999546,9.5594902125713));
#299249=CARTESIAN_POINT('Ctrl Pts',(6.21213331202014,116.356249999545,8.55026797822134));
#299250=CARTESIAN_POINT('Ctrl Pts',(8.13178807675711,116.506249999544,5.90808986649102));
#299251=CARTESIAN_POINT('Ctrl Pts',(10.0514428414941,116.656249999544,3.2659117547607));
#299252=CARTESIAN_POINT('Ctrl Pts',(10.0514428414941,116.806249999543,-1.23094673026484E-15));
#299253=CARTESIAN_POINT('Ctrl Pts',(10.0514428414941,116.956249999543,-3.26591175476071));
#299254=CARTESIAN_POINT('Ctrl Pts',(8.13178807675711,117.106249999542,-5.90808986649102));
#299255=CARTESIAN_POINT('Ctrl Pts',(6.21213331202014,117.256249999541,-8.55026797822134));
#299256=CARTESIAN_POINT('Ctrl Pts',(3.10606665601003,117.406249999541,-9.5594902125713));
#299257=CARTESIAN_POINT('Ctrl Pts',(-8.08257781012995E-14,117.55624999954,
-10.5687124469213));
#299258=CARTESIAN_POINT('Ctrl Pts',(-3.10606665601019,117.70624999954,-9.5594902125713));
#299259=CARTESIAN_POINT('Ctrl Pts',(-6.2121333120203,117.856249999539,-8.55026797822134));
#299260=CARTESIAN_POINT('Ctrl Pts',(-8.13178807675727,118.006249999538,
-5.90808986649102));
#299261=CARTESIAN_POINT('Ctrl Pts',(-10.0514428414942,118.156249999538,
-3.2659117547607));
#299262=CARTESIAN_POINT('Ctrl Pts',(-10.0514428414942,118.306249999537,
2.46189346052968E-15));
#299263=CARTESIAN_POINT('Ctrl Pts',(-10.0514428414942,118.456249999537,
3.26591175476071));
#299264=CARTESIAN_POINT('Ctrl Pts',(-8.13178807675727,118.606249999536,
5.90808986649102));
#299265=CARTESIAN_POINT('Ctrl Pts',(-6.2121333120203,118.756249999535,8.55026797822134));
#299266=CARTESIAN_POINT('Ctrl Pts',(-3.10606665601019,118.906249999535,
9.5594902125713));
#299267=CARTESIAN_POINT('Ctrl Pts',(-7.91010447632842E-14,119.056249999534,
10.5687124469213));
#299268=CARTESIAN_POINT('Ctrl Pts',(3.10606665601003,119.206249999534,9.5594902125713));
#299269=CARTESIAN_POINT('Ctrl Pts',(6.21213331202014,119.356249999533,8.55026797822134));
#299270=CARTESIAN_POINT('Ctrl Pts',(8.13178807675711,119.506249999532,5.90808986649102));
#299271=CARTESIAN_POINT('Ctrl Pts',(10.0514428414941,119.656249999532,3.2659117547607));
#299272=CARTESIAN_POINT('Ctrl Pts',(10.0514428414941,119.806249999531,-1.23094673026484E-15));
#299273=CARTESIAN_POINT('Ctrl Pts',(10.0514428414941,119.956249999531,-3.26591175476071));
#299274=CARTESIAN_POINT('Ctrl Pts',(8.13178807675711,120.10624999953,-5.90808986649102));
#299275=CARTESIAN_POINT('Ctrl Pts',(6.21213331202013,120.256249999529,-8.55026797822134));
#299276=CARTESIAN_POINT('Ctrl Pts',(3.10606665601003,120.406249999529,-9.5594902125713));
#299277=CARTESIAN_POINT('Ctrl Pts',(-8.25534873729613E-14,120.556249999528,
-10.5687124469213));
#299278=CARTESIAN_POINT('Ctrl Pts',(-3.10606665601019,120.706249999528,
-9.5594902125713));
#299279=CARTESIAN_POINT('Ctrl Pts',(-6.2121333120203,120.856249999527,-8.55026797822134));
#299280=CARTESIAN_POINT('Ctrl Pts',(-8.13178807675727,121.006249999526,
-5.90808986649102));
#299281=CARTESIAN_POINT('Ctrl Pts',(-10.0514428414943,121.156249999526,
-3.2659117547607));
#299282=CARTESIAN_POINT('Ctrl Pts',(-10.0514428414943,121.306249999525,
2.46189346052968E-15));
#299283=CARTESIAN_POINT('Ctrl Pts',(-10.0514428414943,121.456249999525,
3.26591175476071));
#299284=CARTESIAN_POINT('Ctrl Pts',(-8.13178807675727,121.606249999524,
5.90808986649102));
#299285=CARTESIAN_POINT('Ctrl Pts',(-6.2121333120203,121.756249999523,8.55026797822134));
#299286=CARTESIAN_POINT('Ctrl Pts',(-3.10606665601019,121.906249999523,
9.5594902125713));
#299287=CARTESIAN_POINT('Ctrl Pts',(-8.08287540349461E-14,122.056249999522,
10.5687124469213));
#299288=CARTESIAN_POINT('Ctrl Pts',(3.10606665601003,122.206249999522,9.5594902125713));
#299289=CARTESIAN_POINT('Ctrl Pts',(6.21213331202014,122.356249999521,8.55026797822134));
#299290=CARTESIAN_POINT('Ctrl Pts',(8.13178807675711,122.50624999952,5.90808986649102));
#299291=CARTESIAN_POINT('Ctrl Pts',(10.0514428414941,122.65624999952,3.2659117547607));
#299292=CARTESIAN_POINT('Ctrl Pts',(10.0514428414941,122.806249999519,-1.23094673026484E-15));
#299293=CARTESIAN_POINT('Ctrl Pts',(10.0514428414941,122.956249999519,-3.26591175476071));
#299294=CARTESIAN_POINT('Ctrl Pts',(8.13178807675711,123.106249999518,-5.90808986649102));
#299295=CARTESIAN_POINT('Ctrl Pts',(6.21213331202013,123.256249999517,-8.55026797822134));
#299296=CARTESIAN_POINT('Ctrl Pts',(3.10606665601002,123.406249999517,-9.5594902125713));
#299297=CARTESIAN_POINT('Ctrl Pts',(-8.42811966446232E-14,123.556249999516,
-10.5687124469213));
#299298=CARTESIAN_POINT('Ctrl Pts',(-3.10606665601019,123.706249999516,
-9.5594902125713));
#299299=CARTESIAN_POINT('Ctrl Pts',(-6.2121333120203,123.856249999515,-8.55026797822134));
#299300=CARTESIAN_POINT('Ctrl Pts',(-8.13178807675727,124.006249999514,
-5.90808986649102));
#299301=CARTESIAN_POINT('Ctrl Pts',(-10.0514428414943,124.156249999514,
-3.2659117547607));
#299302=CARTESIAN_POINT('Ctrl Pts',(-10.0514428414943,124.306249999513,
2.46189346052968E-15));
#299303=CARTESIAN_POINT('Ctrl Pts',(-10.0514428414943,124.456249999513,
3.26591175476071));
#299304=CARTESIAN_POINT('Ctrl Pts',(-8.13178807675727,124.606249999512,
5.90808986649102));
#299305=CARTESIAN_POINT('Ctrl Pts',(-6.2121333120203,124.756249999511,8.55026797822134));
#299306=CARTESIAN_POINT('Ctrl Pts',(-3.10606665601019,124.906249999511,
9.5594902125713));
#299307=CARTESIAN_POINT('Ctrl Pts',(-8.25564633066079E-14,125.05624999951,
10.5687124469213));
#299308=CARTESIAN_POINT('Ctrl Pts',(3.10606665601002,125.20624999951,9.5594902125713));
#299309=CARTESIAN_POINT('Ctrl Pts',(6.21213331202013,125.356249999509,8.55026797822134));
#299310=CARTESIAN_POINT('Ctrl Pts',(8.13178807675711,125.506249999508,5.90808986649102));
#299311=CARTESIAN_POINT('Ctrl Pts',(10.0514428414941,125.656249999508,3.2659117547607));
#299312=CARTESIAN_POINT('Ctrl Pts',(10.0514428414941,125.806249999507,-1.23094673026484E-15));
#299313=CARTESIAN_POINT('Ctrl Pts',(10.0514428414941,125.956249999507,-3.26591175476071));
#299314=CARTESIAN_POINT('Ctrl Pts',(8.13178807675711,126.106249999506,-5.90808986649102));
#299315=CARTESIAN_POINT('Ctrl Pts',(6.21213331202013,126.256249999505,-8.55026797822134));
#299316=CARTESIAN_POINT('Ctrl Pts',(3.10606665601002,126.406249999505,-9.5594902125713));
#299317=CARTESIAN_POINT('Ctrl Pts',(-8.6008905916285E-14,126.556249999504,
-10.5687124469213));
#299318=CARTESIAN_POINT('Ctrl Pts',(-3.10606665601019,126.706249999504,
-9.5594902125713));
#299319=CARTESIAN_POINT('Ctrl Pts',(-6.2121333120203,126.856249999503,-8.55026797822134));
#299320=CARTESIAN_POINT('Ctrl Pts',(-8.13178807675728,127.006249999502,
-5.90808986649102));
#299321=CARTESIAN_POINT('Ctrl Pts',(-10.0514428414943,127.156249999502,
-3.2659117547607));
#299322=CARTESIAN_POINT('Ctrl Pts',(-10.0514428414943,127.306249999501,
2.46189346052968E-15));
#299323=CARTESIAN_POINT('Ctrl Pts',(-10.0514428414943,127.456249999501,
3.26591175476071));
#299324=CARTESIAN_POINT('Ctrl Pts',(-8.13178807675728,127.6062499995,5.90808986649102));
#299325=CARTESIAN_POINT('Ctrl Pts',(-6.2121333120203,127.756249999499,8.55026797822134));
#299326=CARTESIAN_POINT('Ctrl Pts',(-3.10606665601019,127.906249999499,
9.5594902125713));
#299327=CARTESIAN_POINT('Ctrl Pts',(-8.42841725782698E-14,128.056249999498,
10.5687124469213));
#299328=CARTESIAN_POINT('Ctrl Pts',(3.10606665601002,128.206249999498,9.5594902125713));
#299329=CARTESIAN_POINT('Ctrl Pts',(6.21213331202013,128.356249999497,8.55026797822134));
#299330=CARTESIAN_POINT('Ctrl Pts',(8.1317880767571,128.506249999496,5.90808986649102));
#299331=CARTESIAN_POINT('Ctrl Pts',(10.0514428414941,128.656249999496,3.2659117547607));
#299332=CARTESIAN_POINT('Ctrl Pts',(10.0514428414941,128.806249999495,-1.23094673026484E-15));
#299333=CARTESIAN_POINT('Ctrl Pts',(10.0514428414941,128.956249999495,-3.26591175476071));
#299334=CARTESIAN_POINT('Ctrl Pts',(8.1317880767571,129.106249999494,-5.90808986649102));
#299335=CARTESIAN_POINT('Ctrl Pts',(6.21213331202013,129.256249999493,-8.55026797822134));
#299336=CARTESIAN_POINT('Ctrl Pts',(3.10606665601002,129.406249999493,-9.5594902125713));
#299337=CARTESIAN_POINT('Ctrl Pts',(-8.77366151879469E-14,129.556249999492,
-10.5687124469213));
#299338=CARTESIAN_POINT('Ctrl Pts',(-3.1060666560102,129.706249999492,-9.5594902125713));
#299339=CARTESIAN_POINT('Ctrl Pts',(-6.2121333120203,129.856249999491,-8.55026797822134));
#299340=CARTESIAN_POINT('Ctrl Pts',(-8.13178807675728,130.00624999949,-5.90808986649102));
#299341=CARTESIAN_POINT('Ctrl Pts',(-10.0514428414943,130.15624999949,-3.2659117547607));
#299342=CARTESIAN_POINT('Ctrl Pts',(-10.0514428414943,130.306249999489,
2.46189346052968E-15));
#299343=CARTESIAN_POINT('Ctrl Pts',(-10.0514428414943,130.456249999489,
3.26591175476071));
#299344=CARTESIAN_POINT('Ctrl Pts',(-8.13178807675728,130.606249999488,
5.90808986649102));
#299345=CARTESIAN_POINT('Ctrl Pts',(-6.2121333120203,130.756249999487,8.55026797822134));
#299346=CARTESIAN_POINT('Ctrl Pts',(-3.10606665601019,130.906249999487,
9.5594902125713));
#299347=CARTESIAN_POINT('Ctrl Pts',(-8.60118818499316E-14,131.056249999486,
10.5687124469213));
#299348=CARTESIAN_POINT('Ctrl Pts',(3.10606665601002,131.206249999486,9.5594902125713));
#299349=CARTESIAN_POINT('Ctrl Pts',(6.21213331202013,131.356249999485,8.55026797822134));
#299350=CARTESIAN_POINT('Ctrl Pts',(8.1317880767571,131.506249999484,5.90808986649102));
#299351=CARTESIAN_POINT('Ctrl Pts',(10.0514428414941,131.656249999484,3.2659117547607));
#299352=CARTESIAN_POINT('Ctrl Pts',(10.0514428414941,131.806249999483,-1.23094673026484E-15));
#299353=CARTESIAN_POINT('Ctrl Pts',(10.0514428414941,131.956249999483,-3.26591175476071));
#299354=CARTESIAN_POINT('Ctrl Pts',(8.1317880767571,132.106249999482,-5.90808986649102));
#299355=CARTESIAN_POINT('Ctrl Pts',(6.21213331202012,132.256249999481,-8.55026797822134));
#299356=CARTESIAN_POINT('Ctrl Pts',(3.10606665601002,132.406249999481,-9.5594902125713));
#299357=CARTESIAN_POINT('Ctrl Pts',(-8.94643244596087E-14,132.55624999948,
-10.5687124469213));
#299358=CARTESIAN_POINT('Ctrl Pts',(-3.1060666560102,132.70624999948,-9.5594902125713));
#299359=CARTESIAN_POINT('Ctrl Pts',(-6.2121333120203,132.856249999479,-8.55026797822134));
#299360=CARTESIAN_POINT('Ctrl Pts',(-8.13178807675728,133.006249999478,
-5.90808986649102));
#299361=CARTESIAN_POINT('Ctrl Pts',(-10.0514428414943,133.156249999478,
-3.2659117547607));
#299362=CARTESIAN_POINT('Ctrl Pts',(-10.0514428414943,133.306249999477,
2.46189346052968E-15));
#299363=CARTESIAN_POINT('Ctrl Pts',(-10.0514428414943,133.456249999477,
3.26591175476071));
#299364=CARTESIAN_POINT('Ctrl Pts',(-8.13178807675728,133.606249999476,
5.90808986649102));
#299365=CARTESIAN_POINT('Ctrl Pts',(-6.2121333120203,133.756249999475,8.55026797822134));
#299366=CARTESIAN_POINT('Ctrl Pts',(-3.1060666560102,133.906249999475,9.5594902125713));
#299367=CARTESIAN_POINT('Ctrl Pts',(-8.77395911215934E-14,134.056249999474,
10.5687124469213));
#299368=CARTESIAN_POINT('Ctrl Pts',(3.10606665601002,134.206249999474,9.5594902125713));
#299369=CARTESIAN_POINT('Ctrl Pts',(6.21213331202013,134.356249999473,8.55026797822134));
#299370=CARTESIAN_POINT('Ctrl Pts',(8.1317880767571,134.506249999472,5.90808986649102));
#299371=CARTESIAN_POINT('Ctrl Pts',(10.0514428414941,134.656249999472,3.2659117547607));
#299372=CARTESIAN_POINT('Ctrl Pts',(10.0514428414941,134.806249999471,-1.23094673026484E-15));
#299373=CARTESIAN_POINT('Ctrl Pts',(10.0514428414941,134.956249999471,-3.26591175476071));
#299374=CARTESIAN_POINT('Ctrl Pts',(8.1317880767571,135.10624999947,-5.90808986649102));
#299375=CARTESIAN_POINT('Ctrl Pts',(6.21213331202012,135.256249999469,-8.55026797822134));
#299376=CARTESIAN_POINT('Ctrl Pts',(3.10606665601002,135.406249999469,-9.5594902125713));
#299377=CARTESIAN_POINT('Ctrl Pts',(-9.11920337312706E-14,135.556249999468,
-10.5687124469213));
#299378=CARTESIAN_POINT('Ctrl Pts',(-3.1060666560102,135.706249999468,-9.5594902125713));
#299379=CARTESIAN_POINT('Ctrl Pts',(-6.21213331202031,135.856249999467,
-8.55026797822134));
#299380=CARTESIAN_POINT('Ctrl Pts',(-8.13178807675728,136.006249999466,
-5.90808986649102));
#299381=CARTESIAN_POINT('Ctrl Pts',(-10.0514428414943,136.156249999466,
-3.2659117547607));
#299382=CARTESIAN_POINT('Ctrl Pts',(-10.0514428414943,136.306249999465,
2.46189346052968E-15));
#299383=CARTESIAN_POINT('Ctrl Pts',(-10.0514428414943,136.456249999465,
3.26591175476071));
#299384=CARTESIAN_POINT('Ctrl Pts',(-8.13178807675728,136.606249999464,
5.90808986649102));
#299385=CARTESIAN_POINT('Ctrl Pts',(-6.2121333120203,136.756249999463,8.55026797822134));
#299386=CARTESIAN_POINT('Ctrl Pts',(-3.1060666560102,136.906249999463,9.5594902125713));
#299387=CARTESIAN_POINT('Ctrl Pts',(-8.94673003932553E-14,137.056249999462,
10.5687124469213));
#299388=CARTESIAN_POINT('Ctrl Pts',(3.10606665601002,137.206249999462,9.5594902125713));
#299389=CARTESIAN_POINT('Ctrl Pts',(6.21213331202012,137.356249999461,8.55026797822134));
#299390=CARTESIAN_POINT('Ctrl Pts',(8.1317880767571,137.50624999946,5.90808986649102));
#299391=CARTESIAN_POINT('Ctrl Pts',(10.0514428414941,137.65624999946,3.2659117547607));
#299392=CARTESIAN_POINT('Ctrl Pts',(10.0514428414941,137.806249999459,-1.23094673026484E-15));
#299393=CARTESIAN_POINT('Ctrl Pts',(10.0514428414941,137.956249999459,-3.26591175476071));
#299394=CARTESIAN_POINT('Ctrl Pts',(8.1317880767571,138.106249999458,-5.90808986649102));
#299395=CARTESIAN_POINT('Ctrl Pts',(6.21213331202012,138.256249999457,-8.55026797822134));
#299396=CARTESIAN_POINT('Ctrl Pts',(3.10606665601001,138.406249999457,-9.5594902125713));
#299397=CARTESIAN_POINT('Ctrl Pts',(-9.29197430029324E-14,138.556249999456,
-10.5687124469213));
#299398=CARTESIAN_POINT('Ctrl Pts',(-3.1060666560102,138.706249999456,-9.5594902125713));
#299399=CARTESIAN_POINT('Ctrl Pts',(-6.21213331202031,138.856249999455,
-8.55026797822134));
#299400=CARTESIAN_POINT('Ctrl Pts',(-8.13178807675728,139.006249999454,
-5.90808986649102));
#299401=CARTESIAN_POINT('Ctrl Pts',(-10.0514428414943,139.156249999454,
-3.2659117547607));
#299402=CARTESIAN_POINT('Ctrl Pts',(-10.0514428414943,139.306249999453,
2.46189346052968E-15));
#299403=CARTESIAN_POINT('Ctrl Pts',(-10.0514428414943,139.456249999453,
3.26591175476071));
#299404=CARTESIAN_POINT('Ctrl Pts',(-8.13178807675728,139.606249999452,
5.90808986649102));
#299405=CARTESIAN_POINT('Ctrl Pts',(-6.21213331202031,139.756249999451,
8.55026797822134));
#299406=CARTESIAN_POINT('Ctrl Pts',(-3.1060666560102,139.906249999451,9.5594902125713));
#299407=CARTESIAN_POINT('Ctrl Pts',(-9.11950096649171E-14,140.05624999945,
10.5687124469213));
#299408=CARTESIAN_POINT('Ctrl Pts',(3.10606665601002,140.20624999945,9.5594902125713));
#299409=CARTESIAN_POINT('Ctrl Pts',(6.21213331202012,140.356249999449,8.55026797822134));
#299410=CARTESIAN_POINT('Ctrl Pts',(8.1317880767571,140.506249999448,5.90808986649102));
#299411=CARTESIAN_POINT('Ctrl Pts',(10.0514428414941,140.656249999448,3.2659117547607));
#299412=CARTESIAN_POINT('Ctrl Pts',(10.0514428414941,140.806249999447,-1.23094673026484E-15));
#299413=CARTESIAN_POINT('Ctrl Pts',(10.0514428414941,140.956249999447,-3.26591175476071));
#299414=CARTESIAN_POINT('Ctrl Pts',(8.1317880767571,141.106249999446,-5.90808986649102));
#299415=CARTESIAN_POINT('Ctrl Pts',(6.21213331202012,141.256249999445,-8.55026797822134));
#299416=CARTESIAN_POINT('Ctrl Pts',(3.10606665601001,141.406249999445,-9.5594902125713));
#299417=CARTESIAN_POINT('Ctrl Pts',(-9.46474522745942E-14,141.556249999444,
-10.5687124469213));
#299418=CARTESIAN_POINT('Ctrl Pts',(-3.1060666560102,141.706249999444,-9.5594902125713));
#299419=CARTESIAN_POINT('Ctrl Pts',(-6.21213331202031,141.856249999443,
-8.55026797822134));
#299420=CARTESIAN_POINT('Ctrl Pts',(-8.13178807675729,142.006249999442,
-5.90808986649102));
#299421=CARTESIAN_POINT('Ctrl Pts',(-10.0514428414943,142.156249999442,
-3.2659117547607));
#299422=CARTESIAN_POINT('Ctrl Pts',(-10.0514428414943,142.306249999441,
2.46189346052968E-15));
#299423=CARTESIAN_POINT('Ctrl Pts',(-10.0514428414943,142.456249999441,
3.26591175476071));
#299424=CARTESIAN_POINT('Ctrl Pts',(-8.13178807675729,142.60624999944,5.90808986649102));
#299425=CARTESIAN_POINT('Ctrl Pts',(-6.21213331202031,142.756249999439,
8.55026797822134));
#299426=CARTESIAN_POINT('Ctrl Pts',(-3.1060666560102,142.906249999439,9.5594902125713));
#299427=CARTESIAN_POINT('Ctrl Pts',(-9.29227189365789E-14,143.056249999438,
10.5687124469213));
#299428=CARTESIAN_POINT('Ctrl Pts',(3.10606665601001,143.206249999438,9.5594902125713));
#299429=CARTESIAN_POINT('Ctrl Pts',(6.21213331202012,143.356249999437,8.55026797822134));
#299430=CARTESIAN_POINT('Ctrl Pts',(8.1317880767571,143.506249999436,5.90808986649102));
#299431=CARTESIAN_POINT('Ctrl Pts',(10.0514428414941,143.656249999436,3.2659117547607));
#299432=CARTESIAN_POINT('Ctrl Pts',(10.0514428414941,143.806249999435,-1.23094673026484E-15));
#299433=CARTESIAN_POINT('Ctrl Pts',(10.0514428414941,143.956249999435,-3.26591175476071));
#299434=CARTESIAN_POINT('Ctrl Pts',(8.1317880767571,144.106249999434,-5.90808986649102));
#299435=CARTESIAN_POINT('Ctrl Pts',(6.21213331202012,144.256249999433,-8.55026797822134));
#299436=CARTESIAN_POINT('Ctrl Pts',(3.10606665601001,144.406249999433,-9.5594902125713));
#299437=CARTESIAN_POINT('Ctrl Pts',(-9.63751615462561E-14,144.556249999432,
-10.5687124469213));
#299438=CARTESIAN_POINT('Ctrl Pts',(-3.1060666560102,144.706249999432,-9.5594902125713));
#299439=CARTESIAN_POINT('Ctrl Pts',(-6.21213331202031,144.856249999431,
-8.55026797822134));
#299440=CARTESIAN_POINT('Ctrl Pts',(-8.13178807675729,145.00624999943,-5.90808986649102));
#299441=CARTESIAN_POINT('Ctrl Pts',(-10.0514428414943,145.15624999943,-3.2659117547607));
#299442=CARTESIAN_POINT('Ctrl Pts',(-10.0514428414943,145.306249999429,
2.46189346052968E-15));
#299443=CARTESIAN_POINT('Ctrl Pts',(-10.0514428414943,145.456249999429,
3.26591175476071));
#299444=CARTESIAN_POINT('Ctrl Pts',(-8.13178807675729,145.606249999428,
5.90808986649102));
#299445=CARTESIAN_POINT('Ctrl Pts',(-6.21213331202031,145.756249999427,
8.55026797822134));
#299446=CARTESIAN_POINT('Ctrl Pts',(-3.1060666560102,145.906249999427,9.5594902125713));
#299447=CARTESIAN_POINT('Ctrl Pts',(-9.46504282082408E-14,146.056249999426,
10.5687124469213));
#299448=CARTESIAN_POINT('Ctrl Pts',(3.10606665601001,146.206249999426,9.5594902125713));
#299449=CARTESIAN_POINT('Ctrl Pts',(6.21213331202012,146.356249999425,8.55026797822134));
#299450=CARTESIAN_POINT('Ctrl Pts',(8.13178807675709,146.506249999424,5.90808986649102));
#299451=CARTESIAN_POINT('Ctrl Pts',(10.0514428414941,146.656249999424,3.2659117547607));
#299452=CARTESIAN_POINT('Ctrl Pts',(10.0514428414941,146.806249999423,-1.23094673026484E-15));
#299453=CARTESIAN_POINT('Ctrl Pts',(10.0514428414941,146.956249999423,-3.26591175476071));
#299454=CARTESIAN_POINT('Ctrl Pts',(8.13178807675709,147.106249999422,-5.90808986649102));
#299455=CARTESIAN_POINT('Ctrl Pts',(6.21213331202012,147.256249999421,-8.55026797822134));
#299456=CARTESIAN_POINT('Ctrl Pts',(3.10606665601001,147.406249999421,-9.5594902125713));
#299457=CARTESIAN_POINT('Ctrl Pts',(-9.81028708179179E-14,147.55624999942,
-10.5687124469213));
#299458=CARTESIAN_POINT('Ctrl Pts',(-3.10606665601021,147.70624999942,-9.5594902125713));
#299459=CARTESIAN_POINT('Ctrl Pts',(-6.21213331202032,147.856249999419,
-8.55026797822134));
#299460=CARTESIAN_POINT('Ctrl Pts',(-8.13178807675729,148.006249999418,
-5.90808986649102));
#299461=CARTESIAN_POINT('Ctrl Pts',(-10.0514428414943,148.156249999418,
-3.2659117547607));
#299462=CARTESIAN_POINT('Ctrl Pts',(-10.0514428414943,148.306249999417,
2.46189346052968E-15));
#299463=CARTESIAN_POINT('Ctrl Pts',(-10.0514428414943,148.456249999417,
3.26591175476071));
#299464=CARTESIAN_POINT('Ctrl Pts',(-8.13178807675729,148.606249999416,
5.90808986649102));
#299465=CARTESIAN_POINT('Ctrl Pts',(-6.21213331202031,148.756249999415,
8.55026797822134));
#299466=CARTESIAN_POINT('Ctrl Pts',(-3.1060666560102,148.906249999415,9.5594902125713));
#299467=CARTESIAN_POINT('Ctrl Pts',(-9.63781374799026E-14,149.056249999414,
10.5687124469213));
#299468=CARTESIAN_POINT('Ctrl Pts',(3.10606665601001,149.206249999414,9.5594902125713));
#299469=CARTESIAN_POINT('Ctrl Pts',(6.21213331202012,149.356249999413,8.55026797822134));
#299470=CARTESIAN_POINT('Ctrl Pts',(8.13178807675709,149.506249999412,5.90808986649102));
#299471=CARTESIAN_POINT('Ctrl Pts',(10.0514428414941,149.656249999412,3.2659117547607));
#299472=CARTESIAN_POINT('Ctrl Pts',(10.0514428414941,149.806249999411,-1.23094673026484E-15));
#299473=CARTESIAN_POINT('Ctrl Pts',(10.0514428414941,149.956249999411,-3.26591175476071));
#299474=CARTESIAN_POINT('Ctrl Pts',(8.13178807675709,150.10624999941,-5.90808986649102));
#299475=CARTESIAN_POINT('Ctrl Pts',(6.21213331202012,150.256249999409,-8.55026797822134));
#299476=CARTESIAN_POINT('Ctrl Pts',(3.10606665601001,150.406249999409,-9.5594902125713));
#299477=CARTESIAN_POINT('Ctrl Pts',(-9.98305800895797E-14,150.556249999408,
-10.5687124469213));
#299478=CARTESIAN_POINT('Ctrl Pts',(-3.10606665601021,150.706249999408,
-9.5594902125713));
#299479=CARTESIAN_POINT('Ctrl Pts',(-6.21213331202032,150.856249999407,
-8.55026797822134));
#299480=CARTESIAN_POINT('Ctrl Pts',(-8.13178807675729,151.006249999406,
-5.90808986649102));
#299481=CARTESIAN_POINT('Ctrl Pts',(-10.0514428414943,151.156249999406,
-3.2659117547607));
#299482=CARTESIAN_POINT('Ctrl Pts',(-10.0514428414943,151.306249999405,
2.46189346052968E-15));
#299483=CARTESIAN_POINT('Ctrl Pts',(-10.0514428414943,151.456249999405,
3.26591175476071));
#299484=CARTESIAN_POINT('Ctrl Pts',(-8.13178807675729,151.606249999404,
5.90808986649102));
#299485=CARTESIAN_POINT('Ctrl Pts',(-6.21213331202032,151.756249999403,
8.55026797822134));
#299486=CARTESIAN_POINT('Ctrl Pts',(-3.10606665601021,151.906249999403,
9.5594902125713));
#299487=CARTESIAN_POINT('Ctrl Pts',(-9.81058467515645E-14,152.056249999402,
10.5687124469213));
#299488=CARTESIAN_POINT('Ctrl Pts',(3.10606665601001,152.206249999402,9.5594902125713));
#299489=CARTESIAN_POINT('Ctrl Pts',(6.21213331202012,152.356249999401,8.55026797822134));
#299490=CARTESIAN_POINT('Ctrl Pts',(8.13178807675709,152.5062499994,5.90808986649102));
#299491=CARTESIAN_POINT('Ctrl Pts',(10.0514428414941,152.6562499994,3.2659117547607));
#299492=CARTESIAN_POINT('Ctrl Pts',(10.0514428414941,152.806249999399,-1.23094673026484E-15));
#299493=CARTESIAN_POINT('Ctrl Pts',(10.0514428414941,152.956249999399,-3.26591175476071));
#299494=CARTESIAN_POINT('Ctrl Pts',(8.13178807675709,153.106249999398,-5.90808986649102));
#299495=CARTESIAN_POINT('Ctrl Pts',(6.21213331202012,153.256249999397,-8.55026797822134));
#299496=CARTESIAN_POINT('Ctrl Pts',(3.10606665601001,153.406249999397,-9.5594902125713));
#299497=CARTESIAN_POINT('Ctrl Pts',(-1.01558289361242E-13,153.556249999396,
-10.5687124469213));
#299498=CARTESIAN_POINT('Ctrl Pts',(-3.10606665601021,153.706249999396,
-9.5594902125713));
#299499=CARTESIAN_POINT('Ctrl Pts',(-12.1623797632097,-0.474999999988005,
2.97892388940585E-15));
#299500=CARTESIAN_POINT('Ctrl Pts',(-12.1623797632096,-0.324999999988605,
3.95179673813133));
#299501=CARTESIAN_POINT('Ctrl Pts',(-9.83957192047856,-0.174999999989203,
7.14886745759505));
#299502=CARTESIAN_POINT('Ctrl Pts',(-7.51676407774747,-0.0249999999898023,
10.3459381770588));
#299503=CARTESIAN_POINT('Ctrl Pts',(-3.75838203887374,0.1250000000096,11.5671105274568));
#299504=CARTESIAN_POINT('Ctrl Pts',(-1.02868273148643E-14,0.275000000009002,
12.7882828778549));
#299505=CARTESIAN_POINT('Ctrl Pts',(3.75838203887372,0.425000000008404,
11.5671105274568));
#299506=CARTESIAN_POINT('Ctrl Pts',(7.51676407774745,0.575000000007806,
10.3459381770588));
#299507=CARTESIAN_POINT('Ctrl Pts',(9.83957192047854,0.725000000007208,
7.14886745759505));
#299508=CARTESIAN_POINT('Ctrl Pts',(12.1623797632096,0.875000000006609,
3.95179673813132));
#299509=CARTESIAN_POINT('Ctrl Pts',(12.1623797632096,1.02500000000601,-1.48946194470292E-15));
#299510=CARTESIAN_POINT('Ctrl Pts',(12.1623797632096,1.17500000000541,-3.95179673813132));
#299511=CARTESIAN_POINT('Ctrl Pts',(9.83957192047853,1.32500000000481,-7.14886745759505));
#299512=CARTESIAN_POINT('Ctrl Pts',(7.51676407774744,1.47500000000421,-10.3459381770588));
#299513=CARTESIAN_POINT('Ctrl Pts',(3.75838203887371,1.6250000000036,-11.5671105274568));
#299514=CARTESIAN_POINT('Ctrl Pts',(-1.42829078892864E-14,1.775000000003,
-12.7882828778549));
#299515=CARTESIAN_POINT('Ctrl Pts',(-3.75838203887374,1.9250000000024,-11.5671105274568));
#299516=CARTESIAN_POINT('Ctrl Pts',(-7.51676407774747,2.0750000000018,-10.3459381770588));
#299517=CARTESIAN_POINT('Ctrl Pts',(-9.83957192047856,2.2250000000012,-7.14886745759505));
#299518=CARTESIAN_POINT('Ctrl Pts',(-12.1623797632097,2.37500000000059,
-3.95179673813132));
#299519=CARTESIAN_POINT('Ctrl Pts',(-12.1623797632097,2.525,2.97892388940585E-15));
#299520=CARTESIAN_POINT('Ctrl Pts',(-12.1623797632097,2.6749999999994,3.95179673813133));
#299521=CARTESIAN_POINT('Ctrl Pts',(-9.83957192047856,2.8249999999988,7.14886745759505));
#299522=CARTESIAN_POINT('Ctrl Pts',(-7.51676407774747,2.9749999999982,10.3459381770588));
#299523=CARTESIAN_POINT('Ctrl Pts',(-3.75838203887374,3.1249999999976,11.5671105274568));
#299524=CARTESIAN_POINT('Ctrl Pts',(-1.20145365865262E-14,3.274999999997,
12.7882828778549));
#299525=CARTESIAN_POINT('Ctrl Pts',(3.75838203887372,3.4249999999964,11.5671105274568));
#299526=CARTESIAN_POINT('Ctrl Pts',(7.51676407774744,3.57499999999581,10.3459381770588));
#299527=CARTESIAN_POINT('Ctrl Pts',(9.83957192047853,3.72499999999521,7.14886745759505));
#299528=CARTESIAN_POINT('Ctrl Pts',(12.1623797632096,3.87499999999461,3.95179673813132));
#299529=CARTESIAN_POINT('Ctrl Pts',(12.1623797632096,4.02499999999401,-1.48946194470292E-15));
#299530=CARTESIAN_POINT('Ctrl Pts',(12.1623797632096,4.17499999999341,-3.95179673813132));
#299531=CARTESIAN_POINT('Ctrl Pts',(9.83957192047853,4.32499999999281,-7.14886745759505));
#299532=CARTESIAN_POINT('Ctrl Pts',(7.51676407774744,4.47499999999221,-10.3459381770588));
#299533=CARTESIAN_POINT('Ctrl Pts',(3.75838203887371,4.6249999999916,-11.5671105274568));
#299534=CARTESIAN_POINT('Ctrl Pts',(-1.60106171609483E-14,4.774999999991,
-12.7882828778549));
#299535=CARTESIAN_POINT('Ctrl Pts',(-3.75838203887374,4.9249999999904,-11.5671105274568));
#299536=CARTESIAN_POINT('Ctrl Pts',(-7.51676407774747,5.0749999999898,-10.3459381770588));
#299537=CARTESIAN_POINT('Ctrl Pts',(-9.83957192047857,5.2249999999892,-7.14886745759505));
#299538=CARTESIAN_POINT('Ctrl Pts',(-12.1623797632097,5.3749999999886,-3.95179673813132));
#299539=CARTESIAN_POINT('Ctrl Pts',(-12.1623797632097,5.52499999998799,
2.97892388940585E-15));
#299540=CARTESIAN_POINT('Ctrl Pts',(-12.1623797632097,5.6749999999874,3.95179673813133));
#299541=CARTESIAN_POINT('Ctrl Pts',(-9.83957192047857,5.8249999999868,7.14886745759505));
#299542=CARTESIAN_POINT('Ctrl Pts',(-7.51676407774747,5.9749999999862,10.3459381770588));
#299543=CARTESIAN_POINT('Ctrl Pts',(-3.75838203887374,6.1249999999856,11.5671105274568));
#299544=CARTESIAN_POINT('Ctrl Pts',(-1.3742245858188E-14,6.274999999985,
12.7882828778549));
#299545=CARTESIAN_POINT('Ctrl Pts',(3.75838203887371,6.4249999999844,11.5671105274568));
#299546=CARTESIAN_POINT('Ctrl Pts',(7.51676407774744,6.57499999998381,10.3459381770588));
#299547=CARTESIAN_POINT('Ctrl Pts',(9.83957192047853,6.72499999998321,7.14886745759505));
#299548=CARTESIAN_POINT('Ctrl Pts',(12.1623797632096,6.87499999998261,3.95179673813132));
#299549=CARTESIAN_POINT('Ctrl Pts',(12.1623797632096,7.02499999998201,-1.48946194470292E-15));
#299550=CARTESIAN_POINT('Ctrl Pts',(12.1623797632096,7.17499999998141,-3.95179673813132));
#299551=CARTESIAN_POINT('Ctrl Pts',(9.83957192047853,7.32499999998081,-7.14886745759505));
#299552=CARTESIAN_POINT('Ctrl Pts',(7.51676407774744,7.47499999998021,-10.3459381770588));
#299553=CARTESIAN_POINT('Ctrl Pts',(3.75838203887371,7.6249999999796,-11.5671105274568));
#299554=CARTESIAN_POINT('Ctrl Pts',(-1.77383264326101E-14,7.774999999979,
-12.7882828778549));
#299555=CARTESIAN_POINT('Ctrl Pts',(-3.75838203887375,7.9249999999784,-11.5671105274568));
#299556=CARTESIAN_POINT('Ctrl Pts',(-7.51676407774747,8.0749999999778,-10.3459381770588));
#299557=CARTESIAN_POINT('Ctrl Pts',(-9.83957192047857,8.2249999999772,-7.14886745759505));
#299558=CARTESIAN_POINT('Ctrl Pts',(-12.1623797632097,8.3749999999766,-3.95179673813132));
#299559=CARTESIAN_POINT('Ctrl Pts',(-12.1623797632097,8.52499999997599,
2.97892388940585E-15));
#299560=CARTESIAN_POINT('Ctrl Pts',(-12.1623797632097,8.6749999999754,3.95179673813133));
#299561=CARTESIAN_POINT('Ctrl Pts',(-9.83957192047857,8.8249999999748,7.14886745759505));
#299562=CARTESIAN_POINT('Ctrl Pts',(-7.51676407774747,8.9749999999742,10.3459381770588));
#299563=CARTESIAN_POINT('Ctrl Pts',(-3.75838203887374,9.1249999999736,11.5671105274568));
#299564=CARTESIAN_POINT('Ctrl Pts',(-1.54699551298498E-14,9.274999999973,
12.7882828778549));
#299565=CARTESIAN_POINT('Ctrl Pts',(3.75838203887371,9.4249999999724,11.5671105274568));
#299566=CARTESIAN_POINT('Ctrl Pts',(7.51676407774744,9.57499999997181,10.3459381770588));
#299567=CARTESIAN_POINT('Ctrl Pts',(9.83957192047853,9.72499999997121,7.14886745759505));
#299568=CARTESIAN_POINT('Ctrl Pts',(12.1623797632096,9.87499999997061,3.95179673813132));
#299569=CARTESIAN_POINT('Ctrl Pts',(12.1623797632096,10.02499999997,-1.48946194470292E-15));
#299570=CARTESIAN_POINT('Ctrl Pts',(12.1623797632096,10.1749999999694,-3.95179673813132));
#299571=CARTESIAN_POINT('Ctrl Pts',(9.83957192047853,10.3249999999688,-7.14886745759505));
#299572=CARTESIAN_POINT('Ctrl Pts',(7.51676407774744,10.4749999999682,-10.3459381770588));
#299573=CARTESIAN_POINT('Ctrl Pts',(3.75838203887371,10.6249999999676,-11.5671105274568));
#299574=CARTESIAN_POINT('Ctrl Pts',(-1.9466035704272E-14,10.774999999967,
-12.7882828778549));
#299575=CARTESIAN_POINT('Ctrl Pts',(-3.75838203887375,10.9249999999664,
-11.5671105274568));
#299576=CARTESIAN_POINT('Ctrl Pts',(-7.51676407774748,11.0749999999658,
-10.3459381770588));
#299577=CARTESIAN_POINT('Ctrl Pts',(-9.83957192047857,11.2249999999652,
-7.14886745759505));
#299578=CARTESIAN_POINT('Ctrl Pts',(-12.1623797632097,11.3749999999646,
-3.95179673813132));
#299579=CARTESIAN_POINT('Ctrl Pts',(-12.1623797632097,11.524999999964,2.97892388940585E-15));
#299580=CARTESIAN_POINT('Ctrl Pts',(-12.1623797632097,11.6749999999634,
3.95179673813133));
#299581=CARTESIAN_POINT('Ctrl Pts',(-9.83957192047857,11.8249999999628,
7.14886745759505));
#299582=CARTESIAN_POINT('Ctrl Pts',(-7.51676407774747,11.9749999999622,
10.3459381770588));
#299583=CARTESIAN_POINT('Ctrl Pts',(-3.75838203887375,12.1249999999616,
11.5671105274568));
#299584=CARTESIAN_POINT('Ctrl Pts',(-1.71976644015117E-14,12.274999999961,
12.7882828778549));
#299585=CARTESIAN_POINT('Ctrl Pts',(3.75838203887371,12.4249999999604,11.5671105274568));
#299586=CARTESIAN_POINT('Ctrl Pts',(7.51676407774744,12.5749999999598,10.3459381770588));
#299587=CARTESIAN_POINT('Ctrl Pts',(9.83957192047853,12.7249999999592,7.14886745759505));
#299588=CARTESIAN_POINT('Ctrl Pts',(12.1623797632096,12.8749999999586,3.95179673813132));
#299589=CARTESIAN_POINT('Ctrl Pts',(12.1623797632096,13.024999999958,-1.48946194470292E-15));
#299590=CARTESIAN_POINT('Ctrl Pts',(12.1623797632096,13.1749999999574,-3.95179673813132));
#299591=CARTESIAN_POINT('Ctrl Pts',(9.83957192047853,13.3249999999568,-7.14886745759505));
#299592=CARTESIAN_POINT('Ctrl Pts',(7.51676407774743,13.4749999999562,-10.3459381770588));
#299593=CARTESIAN_POINT('Ctrl Pts',(3.75838203887371,13.6249999999556,-11.5671105274568));
#299594=CARTESIAN_POINT('Ctrl Pts',(-2.11937449759338E-14,13.774999999955,
-12.7882828778549));
#299595=CARTESIAN_POINT('Ctrl Pts',(-3.75838203887375,13.9249999999544,
-11.5671105274568));
#299596=CARTESIAN_POINT('Ctrl Pts',(-7.51676407774748,14.0749999999538,
-10.3459381770588));
#299597=CARTESIAN_POINT('Ctrl Pts',(-9.83957192047857,14.2249999999532,
-7.14886745759505));
#299598=CARTESIAN_POINT('Ctrl Pts',(-12.1623797632097,14.3749999999526,
-3.95179673813132));
#299599=CARTESIAN_POINT('Ctrl Pts',(-12.1623797632097,14.524999999952,2.97892388940585E-15));
#299600=CARTESIAN_POINT('Ctrl Pts',(-12.1623797632097,14.6749999999514,
3.95179673813133));
#299601=CARTESIAN_POINT('Ctrl Pts',(-9.83957192047857,14.8249999999508,
7.14886745759505));
#299602=CARTESIAN_POINT('Ctrl Pts',(-7.51676407774747,14.9749999999502,
10.3459381770588));
#299603=CARTESIAN_POINT('Ctrl Pts',(-3.75838203887375,15.1249999999496,
11.5671105274568));
#299604=CARTESIAN_POINT('Ctrl Pts',(-1.89253736731735E-14,15.274999999949,
12.7882828778549));
#299605=CARTESIAN_POINT('Ctrl Pts',(3.75838203887371,15.4249999999484,11.5671105274568));
#299606=CARTESIAN_POINT('Ctrl Pts',(7.51676407774744,15.5749999999478,10.3459381770588));
#299607=CARTESIAN_POINT('Ctrl Pts',(9.83957192047853,15.7249999999472,7.14886745759505));
#299608=CARTESIAN_POINT('Ctrl Pts',(12.1623797632096,15.8749999999466,3.95179673813132));
#299609=CARTESIAN_POINT('Ctrl Pts',(12.1623797632096,16.024999999946,-1.48946194470292E-15));
#299610=CARTESIAN_POINT('Ctrl Pts',(12.1623797632096,16.1749999999454,-3.95179673813132));
#299611=CARTESIAN_POINT('Ctrl Pts',(9.83957192047852,16.3249999999448,-7.14886745759505));
#299612=CARTESIAN_POINT('Ctrl Pts',(7.51676407774743,16.4749999999442,-10.3459381770588));
#299613=CARTESIAN_POINT('Ctrl Pts',(3.7583820388737,16.6249999999436,-11.5671105274568));
#299614=CARTESIAN_POINT('Ctrl Pts',(-2.29214542475956E-14,16.774999999943,
-12.7882828778549));
#299615=CARTESIAN_POINT('Ctrl Pts',(-3.75838203887375,16.9249999999424,
-11.5671105274568));
#299616=CARTESIAN_POINT('Ctrl Pts',(-7.51676407774748,17.0749999999418,
-10.3459381770588));
#299617=CARTESIAN_POINT('Ctrl Pts',(-9.83957192047857,17.2249999999412,
-7.14886745759505));
#299618=CARTESIAN_POINT('Ctrl Pts',(-12.1623797632097,17.3749999999406,
-3.95179673813132));
#299619=CARTESIAN_POINT('Ctrl Pts',(-12.1623797632097,17.52499999994,2.97892388940585E-15));
#299620=CARTESIAN_POINT('Ctrl Pts',(-12.1623797632097,17.6749999999394,
3.95179673813133));
#299621=CARTESIAN_POINT('Ctrl Pts',(-9.83957192047857,17.8249999999388,
7.14886745759505));
#299622=CARTESIAN_POINT('Ctrl Pts',(-7.51676407774748,17.9749999999382,
10.3459381770588));
#299623=CARTESIAN_POINT('Ctrl Pts',(-3.75838203887375,18.1249999999376,
11.5671105274568));
#299624=CARTESIAN_POINT('Ctrl Pts',(-2.06530829448354E-14,18.274999999937,
12.7882828778549));
#299625=CARTESIAN_POINT('Ctrl Pts',(3.75838203887371,18.4249999999364,11.5671105274568));
#299626=CARTESIAN_POINT('Ctrl Pts',(7.51676407774743,18.5749999999358,10.3459381770588));
#299627=CARTESIAN_POINT('Ctrl Pts',(9.83957192047852,18.7249999999352,7.14886745759505));
#299628=CARTESIAN_POINT('Ctrl Pts',(12.1623797632096,18.8749999999346,3.95179673813132));
#299629=CARTESIAN_POINT('Ctrl Pts',(12.1623797632096,19.024999999934,-1.48946194470292E-15));
#299630=CARTESIAN_POINT('Ctrl Pts',(12.1623797632096,19.1749999999334,-3.95179673813132));
#299631=CARTESIAN_POINT('Ctrl Pts',(9.83957192047852,19.3249999999328,-7.14886745759505));
#299632=CARTESIAN_POINT('Ctrl Pts',(7.51676407774743,19.4749999999322,-10.3459381770588));
#299633=CARTESIAN_POINT('Ctrl Pts',(3.7583820388737,19.6249999999316,-11.5671105274568));
#299634=CARTESIAN_POINT('Ctrl Pts',(-2.46491635192575E-14,19.774999999931,
-12.7882828778549));
#299635=CARTESIAN_POINT('Ctrl Pts',(-3.75838203887375,19.9249999999304,
-11.5671105274568));
#299636=CARTESIAN_POINT('Ctrl Pts',(-7.51676407774748,20.0749999999298,
-10.3459381770588));
#299637=CARTESIAN_POINT('Ctrl Pts',(-9.83957192047857,20.2249999999292,
-7.14886745759505));
#299638=CARTESIAN_POINT('Ctrl Pts',(-12.1623797632097,20.3749999999286,
-3.95179673813132));
#299639=CARTESIAN_POINT('Ctrl Pts',(-12.1623797632097,20.524999999928,2.97892388940585E-15));
#299640=CARTESIAN_POINT('Ctrl Pts',(-12.1623797632097,20.6749999999274,
3.95179673813133));
#299641=CARTESIAN_POINT('Ctrl Pts',(-9.83957192047857,20.8249999999268,
7.14886745759505));
#299642=CARTESIAN_POINT('Ctrl Pts',(-7.51676407774748,20.9749999999262,
10.3459381770588));
#299643=CARTESIAN_POINT('Ctrl Pts',(-3.75838203887375,21.1249999999256,
11.5671105274568));
#299644=CARTESIAN_POINT('Ctrl Pts',(-2.23807922164972E-14,21.274999999925,
12.7882828778549));
#299645=CARTESIAN_POINT('Ctrl Pts',(3.7583820388737,21.4249999999244,11.5671105274568));
#299646=CARTESIAN_POINT('Ctrl Pts',(7.51676407774743,21.5749999999238,10.3459381770588));
#299647=CARTESIAN_POINT('Ctrl Pts',(9.83957192047852,21.7249999999232,7.14886745759505));
#299648=CARTESIAN_POINT('Ctrl Pts',(12.1623797632096,21.8749999999226,3.95179673813132));
#299649=CARTESIAN_POINT('Ctrl Pts',(12.1623797632096,22.024999999922,-1.48946194470292E-15));
#299650=CARTESIAN_POINT('Ctrl Pts',(12.1623797632096,22.1749999999214,-3.95179673813132));
#299651=CARTESIAN_POINT('Ctrl Pts',(9.83957192047852,22.3249999999208,-7.14886745759505));
#299652=CARTESIAN_POINT('Ctrl Pts',(7.51676407774743,22.4749999999202,-10.3459381770588));
#299653=CARTESIAN_POINT('Ctrl Pts',(3.7583820388737,22.6249999999196,-11.5671105274568));
#299654=CARTESIAN_POINT('Ctrl Pts',(-2.63768727909193E-14,22.774999999919,
-12.7882828778549));
#299655=CARTESIAN_POINT('Ctrl Pts',(-3.75838203887375,22.9249999999184,
-11.5671105274568));
#299656=CARTESIAN_POINT('Ctrl Pts',(-7.51676407774748,23.0749999999178,
-10.3459381770588));
#299657=CARTESIAN_POINT('Ctrl Pts',(-9.83957192047857,23.2249999999172,
-7.14886745759505));
#299658=CARTESIAN_POINT('Ctrl Pts',(-12.1623797632097,23.3749999999166,
-3.95179673813132));
#299659=CARTESIAN_POINT('Ctrl Pts',(-12.1623797632097,23.524999999916,2.97892388940585E-15));
#299660=CARTESIAN_POINT('Ctrl Pts',(-12.1623797632097,23.6749999999154,
3.95179673813133));
#299661=CARTESIAN_POINT('Ctrl Pts',(-9.83957192047857,23.8249999999148,
7.14886745759505));
#299662=CARTESIAN_POINT('Ctrl Pts',(-7.51676407774748,23.9749999999142,
10.3459381770588));
#299663=CARTESIAN_POINT('Ctrl Pts',(-3.75838203887375,24.1249999999136,
11.5671105274568));
#299664=CARTESIAN_POINT('Ctrl Pts',(-2.4108501488159E-14,24.274999999913,
12.7882828778549));
#299665=CARTESIAN_POINT('Ctrl Pts',(3.7583820388737,24.4249999999124,11.5671105274568));
#299666=CARTESIAN_POINT('Ctrl Pts',(7.51676407774743,24.5749999999118,10.3459381770588));
#299667=CARTESIAN_POINT('Ctrl Pts',(9.83957192047852,24.7249999999112,7.14886745759505));
#299668=CARTESIAN_POINT('Ctrl Pts',(12.1623797632096,24.8749999999106,3.95179673813132));
#299669=CARTESIAN_POINT('Ctrl Pts',(12.1623797632096,25.02499999991,-1.48946194470292E-15));
#299670=CARTESIAN_POINT('Ctrl Pts',(12.1623797632096,25.1749999999094,-3.95179673813132));
#299671=CARTESIAN_POINT('Ctrl Pts',(9.83957192047852,25.3249999999088,-7.14886745759505));
#299672=CARTESIAN_POINT('Ctrl Pts',(7.51676407774743,25.4749999999082,-10.3459381770588));
#299673=CARTESIAN_POINT('Ctrl Pts',(3.7583820388737,25.6249999999076,-11.5671105274568));
#299674=CARTESIAN_POINT('Ctrl Pts',(-2.81045820625811E-14,25.774999999907,
-12.7882828778549));
#299675=CARTESIAN_POINT('Ctrl Pts',(-3.75838203887376,25.9249999999064,
-11.5671105274568));
#299676=CARTESIAN_POINT('Ctrl Pts',(-7.51676407774749,26.0749999999058,
-10.3459381770588));
#299677=CARTESIAN_POINT('Ctrl Pts',(-9.83957192047857,26.2249999999052,
-7.14886745759505));
#299678=CARTESIAN_POINT('Ctrl Pts',(-12.1623797632097,26.3749999999046,
-3.95179673813132));
#299679=CARTESIAN_POINT('Ctrl Pts',(-12.1623797632097,26.524999999904,2.97892388940585E-15));
#299680=CARTESIAN_POINT('Ctrl Pts',(-12.1623797632097,26.6749999999034,
3.95179673813133));
#299681=CARTESIAN_POINT('Ctrl Pts',(-9.83957192047857,26.8249999999028,
7.14886745759505));
#299682=CARTESIAN_POINT('Ctrl Pts',(-7.51676407774748,26.9749999999022,
10.3459381770588));
#299683=CARTESIAN_POINT('Ctrl Pts',(-3.75838203887375,27.1249999999016,
11.5671105274568));
#299684=CARTESIAN_POINT('Ctrl Pts',(-2.58362107598209E-14,27.274999999901,
12.7882828778549));
#299685=CARTESIAN_POINT('Ctrl Pts',(3.7583820388737,27.4249999999004,11.5671105274568));
#299686=CARTESIAN_POINT('Ctrl Pts',(7.51676407774743,27.5749999998998,10.3459381770588));
#299687=CARTESIAN_POINT('Ctrl Pts',(9.83957192047852,27.7249999998992,7.14886745759505));
#299688=CARTESIAN_POINT('Ctrl Pts',(12.1623797632096,27.8749999998986,3.95179673813132));
#299689=CARTESIAN_POINT('Ctrl Pts',(12.1623797632096,28.024999999898,-1.48946194470292E-15));
#299690=CARTESIAN_POINT('Ctrl Pts',(12.1623797632096,28.1749999998974,-3.95179673813132));
#299691=CARTESIAN_POINT('Ctrl Pts',(9.83957192047852,28.3249999998968,-7.14886745759505));
#299692=CARTESIAN_POINT('Ctrl Pts',(7.51676407774743,28.4749999998962,-10.3459381770588));
#299693=CARTESIAN_POINT('Ctrl Pts',(3.7583820388737,28.6249999998956,-11.5671105274568));
#299694=CARTESIAN_POINT('Ctrl Pts',(-2.9832291334243E-14,28.774999999895,
-12.7882828778549));
#299695=CARTESIAN_POINT('Ctrl Pts',(-3.75838203887376,28.9249999998944,
-11.5671105274568));
#299696=CARTESIAN_POINT('Ctrl Pts',(-7.51676407774749,29.0749999998938,
-10.3459381770588));
#299697=CARTESIAN_POINT('Ctrl Pts',(-9.83957192047858,29.2249999998932,
-7.14886745759505));
#299698=CARTESIAN_POINT('Ctrl Pts',(-12.1623797632097,29.3749999998926,
-3.95179673813132));
#299699=CARTESIAN_POINT('Ctrl Pts',(-12.1623797632097,29.524999999892,2.97892388940585E-15));
#299700=CARTESIAN_POINT('Ctrl Pts',(-12.1623797632097,29.6749999998914,
3.95179673813133));
#299701=CARTESIAN_POINT('Ctrl Pts',(-9.83957192047858,29.8249999998908,
7.14886745759505));
#299702=CARTESIAN_POINT('Ctrl Pts',(-7.51676407774748,29.9749999998902,
10.3459381770588));
#299703=CARTESIAN_POINT('Ctrl Pts',(-3.75838203887376,30.1249999998896,
11.5671105274568));
#299704=CARTESIAN_POINT('Ctrl Pts',(-2.75639200314827E-14,30.274999999889,
12.7882828778549));
#299705=CARTESIAN_POINT('Ctrl Pts',(3.7583820388737,30.4249999998884,11.5671105274568));
#299706=CARTESIAN_POINT('Ctrl Pts',(7.51676407774743,30.5749999998878,10.3459381770588));
#299707=CARTESIAN_POINT('Ctrl Pts',(9.83957192047852,30.7249999998872,7.14886745759505));
#299708=CARTESIAN_POINT('Ctrl Pts',(12.1623797632096,30.8749999998866,3.95179673813132));
#299709=CARTESIAN_POINT('Ctrl Pts',(12.1623797632096,31.024999999886,-1.48946194470292E-15));
#299710=CARTESIAN_POINT('Ctrl Pts',(12.1623797632096,31.1749999998854,-3.95179673813132));
#299711=CARTESIAN_POINT('Ctrl Pts',(9.83957192047852,31.3249999998848,-7.14886745759505));
#299712=CARTESIAN_POINT('Ctrl Pts',(7.51676407774742,31.4749999998842,-10.3459381770588));
#299713=CARTESIAN_POINT('Ctrl Pts',(3.7583820388737,31.6249999998836,-11.5671105274568));
#299714=CARTESIAN_POINT('Ctrl Pts',(-3.15600006059048E-14,31.774999999883,
-12.7882828778549));
#299715=CARTESIAN_POINT('Ctrl Pts',(-3.75838203887376,31.9249999998824,
-11.5671105274568));
#299716=CARTESIAN_POINT('Ctrl Pts',(-7.51676407774749,32.0749999998818,
-10.3459381770588));
#299717=CARTESIAN_POINT('Ctrl Pts',(-9.83957192047858,32.2249999998812,
-7.14886745759505));
#299718=CARTESIAN_POINT('Ctrl Pts',(-12.1623797632097,32.3749999998806,
-3.95179673813132));
#299719=CARTESIAN_POINT('Ctrl Pts',(-12.1623797632097,32.52499999988,2.97892388940585E-15));
#299720=CARTESIAN_POINT('Ctrl Pts',(-12.1623797632097,32.6749999998794,
3.95179673813133));
#299721=CARTESIAN_POINT('Ctrl Pts',(-9.83957192047858,32.8249999998788,
7.14886745759505));
#299722=CARTESIAN_POINT('Ctrl Pts',(-7.51676407774749,32.9749999998782,
10.3459381770588));
#299723=CARTESIAN_POINT('Ctrl Pts',(-3.75838203887376,33.1249999998776,
11.5671105274568));
#299724=CARTESIAN_POINT('Ctrl Pts',(-2.92916293031446E-14,33.274999999877,
12.7882828778549));
#299725=CARTESIAN_POINT('Ctrl Pts',(3.7583820388737,33.4249999998764,11.5671105274568));
#299726=CARTESIAN_POINT('Ctrl Pts',(7.51676407774743,33.5749999998758,10.3459381770588));
#299727=CARTESIAN_POINT('Ctrl Pts',(9.83957192047852,33.7249999998752,7.14886745759505));
#299728=CARTESIAN_POINT('Ctrl Pts',(12.1623797632096,33.8749999998746,3.95179673813132));
#299729=CARTESIAN_POINT('Ctrl Pts',(12.1623797632096,34.024999999874,-1.48946194470292E-15));
#299730=CARTESIAN_POINT('Ctrl Pts',(12.1623797632096,34.1749999998734,-3.95179673813132));
#299731=CARTESIAN_POINT('Ctrl Pts',(9.83957192047851,34.3249999998728,-7.14886745759505));
#299732=CARTESIAN_POINT('Ctrl Pts',(7.51676407774742,34.4749999998722,-10.3459381770588));
#299733=CARTESIAN_POINT('Ctrl Pts',(3.7583820388737,34.6249999998716,-11.5671105274568));
#299734=CARTESIAN_POINT('Ctrl Pts',(-3.32877098775667E-14,34.774999999871,
-12.7882828778549));
#299735=CARTESIAN_POINT('Ctrl Pts',(-3.75838203887376,34.9249999998704,
-11.5671105274568));
#299736=CARTESIAN_POINT('Ctrl Pts',(-7.51676407774749,35.0749999998698,
-10.3459381770588));
#299737=CARTESIAN_POINT('Ctrl Pts',(-9.83957192047858,35.2249999998692,
-7.14886745759505));
#299738=CARTESIAN_POINT('Ctrl Pts',(-12.1623797632097,35.3749999998686,
-3.95179673813132));
#299739=CARTESIAN_POINT('Ctrl Pts',(-12.1623797632097,35.524999999868,2.97892388940585E-15));
#299740=CARTESIAN_POINT('Ctrl Pts',(-12.1623797632097,35.6749999998674,
3.95179673813133));
#299741=CARTESIAN_POINT('Ctrl Pts',(-9.83957192047858,35.8249999998668,
7.14886745759505));
#299742=CARTESIAN_POINT('Ctrl Pts',(-7.51676407774749,35.9749999998662,
10.3459381770588));
#299743=CARTESIAN_POINT('Ctrl Pts',(-3.75838203887376,36.1249999998656,
11.5671105274568));
#299744=CARTESIAN_POINT('Ctrl Pts',(-3.10193385748064E-14,36.274999999865,
12.7882828778549));
#299745=CARTESIAN_POINT('Ctrl Pts',(3.7583820388737,36.4249999998644,11.5671105274568));
#299746=CARTESIAN_POINT('Ctrl Pts',(7.51676407774742,36.5749999998638,10.3459381770588));
#299747=CARTESIAN_POINT('Ctrl Pts',(9.83957192047851,36.7249999998632,7.14886745759505));
#299748=CARTESIAN_POINT('Ctrl Pts',(12.1623797632096,36.8749999998626,3.95179673813132));
#299749=CARTESIAN_POINT('Ctrl Pts',(12.1623797632096,37.024999999862,-1.48946194470292E-15));
#299750=CARTESIAN_POINT('Ctrl Pts',(12.1623797632096,37.1749999998614,-3.95179673813132));
#299751=CARTESIAN_POINT('Ctrl Pts',(9.83957192047851,37.3249999998608,-7.14886745759505));
#299752=CARTESIAN_POINT('Ctrl Pts',(7.51676407774742,37.4749999998602,-10.3459381770588));
#299753=CARTESIAN_POINT('Ctrl Pts',(3.75838203887369,37.6249999998596,-11.5671105274568));
#299754=CARTESIAN_POINT('Ctrl Pts',(-3.50154191492285E-14,37.774999999859,
-12.7882828778549));
#299755=CARTESIAN_POINT('Ctrl Pts',(-3.75838203887376,37.9249999998584,
-11.5671105274568));
#299756=CARTESIAN_POINT('Ctrl Pts',(-7.51676407774749,38.0749999998578,
-10.3459381770588));
#299757=CARTESIAN_POINT('Ctrl Pts',(-9.83957192047858,38.2249999998572,
-7.14886745759505));
#299758=CARTESIAN_POINT('Ctrl Pts',(-12.1623797632097,38.3749999998566,
-3.95179673813132));
#299759=CARTESIAN_POINT('Ctrl Pts',(-12.1623797632097,38.524999999856,2.97892388940585E-15));
#299760=CARTESIAN_POINT('Ctrl Pts',(-12.1623797632097,38.6749999998554,
3.95179673813133));
#299761=CARTESIAN_POINT('Ctrl Pts',(-9.83957192047858,38.8249999998548,
7.14886745759505));
#299762=CARTESIAN_POINT('Ctrl Pts',(-7.51676407774749,38.9749999998542,
10.3459381770588));
#299763=CARTESIAN_POINT('Ctrl Pts',(-3.75838203887376,39.1249999998536,
11.5671105274568));
#299764=CARTESIAN_POINT('Ctrl Pts',(-3.27470478464682E-14,39.274999999853,
12.7882828778549));
#299765=CARTESIAN_POINT('Ctrl Pts',(3.7583820388737,39.4249999998524,11.5671105274568));
#299766=CARTESIAN_POINT('Ctrl Pts',(7.51676407774742,39.5749999998518,10.3459381770588));
#299767=CARTESIAN_POINT('Ctrl Pts',(9.83957192047851,39.7249999998512,7.14886745759505));
#299768=CARTESIAN_POINT('Ctrl Pts',(12.1623797632096,39.8749999998506,3.95179673813132));
#299769=CARTESIAN_POINT('Ctrl Pts',(12.1623797632096,40.02499999985,-1.48946194470292E-15));
#299770=CARTESIAN_POINT('Ctrl Pts',(12.1623797632096,40.1749999998494,-3.95179673813132));
#299771=CARTESIAN_POINT('Ctrl Pts',(9.83957192047851,40.3249999998488,-7.14886745759505));
#299772=CARTESIAN_POINT('Ctrl Pts',(7.51676407774742,40.4749999998482,-10.3459381770588));
#299773=CARTESIAN_POINT('Ctrl Pts',(3.75838203887369,40.6249999998476,-11.5671105274568));
#299774=CARTESIAN_POINT('Ctrl Pts',(-3.67431284208903E-14,40.774999999847,
-12.7882828778549));
#299775=CARTESIAN_POINT('Ctrl Pts',(-3.75838203887376,40.9249999998464,
-11.5671105274568));
#299776=CARTESIAN_POINT('Ctrl Pts',(-7.51676407774749,41.0749999998458,
-10.3459381770588));
#299777=CARTESIAN_POINT('Ctrl Pts',(-9.83957192047858,41.2249999998452,
-7.14886745759505));
#299778=CARTESIAN_POINT('Ctrl Pts',(-12.1623797632097,41.3749999998446,
-3.95179673813132));
#299779=CARTESIAN_POINT('Ctrl Pts',(-12.1623797632097,41.524999999844,2.97892388940585E-15));
#299780=CARTESIAN_POINT('Ctrl Pts',(-12.1623797632097,41.6749999998434,
3.95179673813133));
#299781=CARTESIAN_POINT('Ctrl Pts',(-9.83957192047858,41.8249999998428,
7.14886745759505));
#299782=CARTESIAN_POINT('Ctrl Pts',(-7.51676407774749,41.9749999998422,
10.3459381770588));
#299783=CARTESIAN_POINT('Ctrl Pts',(-3.75838203887376,42.1249999998416,
11.5671105274568));
#299784=CARTESIAN_POINT('Ctrl Pts',(-3.44747571181301E-14,42.274999999841,
12.7882828778549));
#299785=CARTESIAN_POINT('Ctrl Pts',(3.75838203887369,42.4249999998404,11.5671105274568));
#299786=CARTESIAN_POINT('Ctrl Pts',(7.51676407774742,42.5749999998398,10.3459381770588));
#299787=CARTESIAN_POINT('Ctrl Pts',(9.83957192047851,42.7249999998392,7.14886745759505));
#299788=CARTESIAN_POINT('Ctrl Pts',(12.1623797632096,42.8749999998386,3.95179673813132));
#299789=CARTESIAN_POINT('Ctrl Pts',(12.1623797632096,43.024999999838,-1.48946194470292E-15));
#299790=CARTESIAN_POINT('Ctrl Pts',(12.1623797632096,43.1749999998374,-3.95179673813132));
#299791=CARTESIAN_POINT('Ctrl Pts',(9.83957192047851,43.3249999998368,-7.14886745759505));
#299792=CARTESIAN_POINT('Ctrl Pts',(7.51676407774742,43.4749999998362,-10.3459381770588));
#299793=CARTESIAN_POINT('Ctrl Pts',(3.75838203887369,43.6249999998356,-11.5671105274568));
#299794=CARTESIAN_POINT('Ctrl Pts',(-3.84708376925522E-14,43.774999999835,
-12.7882828778549));
#299795=CARTESIAN_POINT('Ctrl Pts',(-3.75838203887377,43.9249999998344,
-11.5671105274568));
#299796=CARTESIAN_POINT('Ctrl Pts',(-7.51676407774749,44.0749999998338,
-10.3459381770588));
#299797=CARTESIAN_POINT('Ctrl Pts',(-9.83957192047859,44.2249999998332,
-7.14886745759505));
#299798=CARTESIAN_POINT('Ctrl Pts',(-12.1623797632097,44.3749999998326,
-3.95179673813132));
#299799=CARTESIAN_POINT('Ctrl Pts',(-12.1623797632097,44.524999999832,2.97892388940585E-15));
#299800=CARTESIAN_POINT('Ctrl Pts',(-12.1623797632097,44.6749999998314,
3.95179673813133));
#299801=CARTESIAN_POINT('Ctrl Pts',(-9.83957192047859,44.8249999998308,
7.14886745759505));
#299802=CARTESIAN_POINT('Ctrl Pts',(-7.51676407774749,44.9749999998302,
10.3459381770588));
#299803=CARTESIAN_POINT('Ctrl Pts',(-3.75838203887376,45.1249999998296,
11.5671105274568));
#299804=CARTESIAN_POINT('Ctrl Pts',(-3.62024663897919E-14,45.274999999829,
12.7882828778549));
#299805=CARTESIAN_POINT('Ctrl Pts',(3.75838203887369,45.4249999998284,11.5671105274568));
#299806=CARTESIAN_POINT('Ctrl Pts',(7.51676407774742,45.5749999998278,10.3459381770588));
#299807=CARTESIAN_POINT('Ctrl Pts',(9.83957192047851,45.7249999998272,7.14886745759505));
#299808=CARTESIAN_POINT('Ctrl Pts',(12.1623797632096,45.8749999998266,3.95179673813132));
#299809=CARTESIAN_POINT('Ctrl Pts',(12.1623797632096,46.024999999826,-1.48946194470292E-15));
#299810=CARTESIAN_POINT('Ctrl Pts',(12.1623797632096,46.1749999998254,-3.95179673813132));
#299811=CARTESIAN_POINT('Ctrl Pts',(9.83957192047851,46.3249999998248,-7.14886745759505));
#299812=CARTESIAN_POINT('Ctrl Pts',(7.51676407774742,46.4749999998242,-10.3459381770588));
#299813=CARTESIAN_POINT('Ctrl Pts',(3.75838203887369,46.6249999998236,-11.5671105274568));
#299814=CARTESIAN_POINT('Ctrl Pts',(-4.0198546964214E-14,46.774999999823,
-12.7882828778549));
#299815=CARTESIAN_POINT('Ctrl Pts',(-3.75838203887377,46.9249999998224,
-11.5671105274568));
#299816=CARTESIAN_POINT('Ctrl Pts',(-7.5167640777475,47.0749999998218,-10.3459381770588));
#299817=CARTESIAN_POINT('Ctrl Pts',(-9.83957192047859,47.2249999998212,
-7.14886745759505));
#299818=CARTESIAN_POINT('Ctrl Pts',(-12.1623797632097,47.3749999998206,
-3.95179673813132));
#299819=CARTESIAN_POINT('Ctrl Pts',(-12.1623797632097,47.52499999982,2.97892388940585E-15));
#299820=CARTESIAN_POINT('Ctrl Pts',(-12.1623797632097,47.6749999998194,
3.95179673813133));
#299821=CARTESIAN_POINT('Ctrl Pts',(-9.83957192047859,47.8249999998188,
7.14886745759505));
#299822=CARTESIAN_POINT('Ctrl Pts',(-7.51676407774749,47.9749999998182,
10.3459381770588));
#299823=CARTESIAN_POINT('Ctrl Pts',(-3.75838203887377,48.1249999998176,
11.5671105274568));
#299824=CARTESIAN_POINT('Ctrl Pts',(-3.79301756614538E-14,48.274999999817,
12.7882828778549));
#299825=CARTESIAN_POINT('Ctrl Pts',(3.75838203887369,48.4249999998164,11.5671105274568));
#299826=CARTESIAN_POINT('Ctrl Pts',(7.51676407774742,48.5749999998158,10.3459381770588));
#299827=CARTESIAN_POINT('Ctrl Pts',(9.83957192047851,48.7249999998152,7.14886745759505));
#299828=CARTESIAN_POINT('Ctrl Pts',(12.1623797632096,48.8749999998146,3.95179673813132));
#299829=CARTESIAN_POINT('Ctrl Pts',(12.1623797632096,49.024999999814,-1.48946194470292E-15));
#299830=CARTESIAN_POINT('Ctrl Pts',(12.1623797632096,49.1749999998134,-3.95179673813132));
#299831=CARTESIAN_POINT('Ctrl Pts',(9.83957192047851,49.3249999998128,-7.14886745759505));
#299832=CARTESIAN_POINT('Ctrl Pts',(7.51676407774741,49.4749999998122,-10.3459381770588));
#299833=CARTESIAN_POINT('Ctrl Pts',(3.75838203887369,49.6249999998116,-11.5671105274568));
#299834=CARTESIAN_POINT('Ctrl Pts',(-4.19262562358759E-14,49.774999999811,
-12.7882828778549));
#299835=CARTESIAN_POINT('Ctrl Pts',(-3.75838203887377,49.9249999998104,
-11.5671105274568));
#299836=CARTESIAN_POINT('Ctrl Pts',(-7.5167640777475,50.0749999998098,-10.3459381770588));
#299837=CARTESIAN_POINT('Ctrl Pts',(-9.83957192047859,50.2249999998092,
-7.14886745759505));
#299838=CARTESIAN_POINT('Ctrl Pts',(-12.1623797632097,50.3749999998086,
-3.95179673813132));
#299839=CARTESIAN_POINT('Ctrl Pts',(-12.1623797632097,50.524999999808,2.97892388940585E-15));
#299840=CARTESIAN_POINT('Ctrl Pts',(-12.1623797632097,50.6749999998074,
3.95179673813133));
#299841=CARTESIAN_POINT('Ctrl Pts',(-9.83957192047859,50.8249999998068,
7.14886745759505));
#299842=CARTESIAN_POINT('Ctrl Pts',(-7.51676407774749,50.9749999998062,
10.3459381770588));
#299843=CARTESIAN_POINT('Ctrl Pts',(-3.75838203887377,51.1249999998056,
11.5671105274568));
#299844=CARTESIAN_POINT('Ctrl Pts',(-3.96578849331156E-14,51.274999999805,
12.7882828778549));
#299845=CARTESIAN_POINT('Ctrl Pts',(3.75838203887369,51.4249999998044,11.5671105274568));
#299846=CARTESIAN_POINT('Ctrl Pts',(7.51676407774742,51.5749999998038,10.3459381770588));
#299847=CARTESIAN_POINT('Ctrl Pts',(9.83957192047851,51.7249999998032,7.14886745759505));
#299848=CARTESIAN_POINT('Ctrl Pts',(12.1623797632096,51.8749999998026,3.95179673813132));
#299849=CARTESIAN_POINT('Ctrl Pts',(12.1623797632096,52.024999999802,-1.48946194470292E-15));
#299850=CARTESIAN_POINT('Ctrl Pts',(12.1623797632096,52.1749999998014,-3.95179673813132));
#299851=CARTESIAN_POINT('Ctrl Pts',(9.8395719204785,52.3249999998008,-7.14886745759505));
#299852=CARTESIAN_POINT('Ctrl Pts',(7.51676407774741,52.4749999998002,-10.3459381770588));
#299853=CARTESIAN_POINT('Ctrl Pts',(3.75838203887368,52.6249999997996,-11.5671105274568));
#299854=CARTESIAN_POINT('Ctrl Pts',(-4.36539655075377E-14,52.774999999799,
-12.7882828778549));
#299855=CARTESIAN_POINT('Ctrl Pts',(-3.75838203887377,52.9249999997984,
-11.5671105274568));
#299856=CARTESIAN_POINT('Ctrl Pts',(-7.5167640777475,53.0749999997978,-10.3459381770588));
#299857=CARTESIAN_POINT('Ctrl Pts',(-9.83957192047859,53.2249999997972,
-7.14886745759505));
#299858=CARTESIAN_POINT('Ctrl Pts',(-12.1623797632097,53.3749999997966,
-3.95179673813132));
#299859=CARTESIAN_POINT('Ctrl Pts',(-12.1623797632097,53.524999999796,2.97892388940585E-15));
#299860=CARTESIAN_POINT('Ctrl Pts',(-12.1623797632097,53.6749999997954,
3.95179673813133));
#299861=CARTESIAN_POINT('Ctrl Pts',(-9.83957192047859,53.8249999997948,
7.14886745759505));
#299862=CARTESIAN_POINT('Ctrl Pts',(-7.5167640777475,53.9749999997942,10.3459381770588));
#299863=CARTESIAN_POINT('Ctrl Pts',(-3.75838203887377,54.1249999997936,
11.5671105274568));
#299864=CARTESIAN_POINT('Ctrl Pts',(-4.13855942047774E-14,54.274999999793,
12.7882828778549));
#299865=CARTESIAN_POINT('Ctrl Pts',(3.75838203887369,54.4249999997924,11.5671105274568));
#299866=CARTESIAN_POINT('Ctrl Pts',(7.51676407774741,54.5749999997918,10.3459381770588));
#299867=CARTESIAN_POINT('Ctrl Pts',(9.8395719204785,54.7249999997912,7.14886745759505));
#299868=CARTESIAN_POINT('Ctrl Pts',(12.1623797632096,54.8749999997906,3.95179673813132));
#299869=CARTESIAN_POINT('Ctrl Pts',(12.1623797632096,55.02499999979,-1.48946194470292E-15));
#299870=CARTESIAN_POINT('Ctrl Pts',(12.1623797632096,55.1749999997894,-3.95179673813132));
#299871=CARTESIAN_POINT('Ctrl Pts',(9.8395719204785,55.3249999997888,-7.14886745759505));
#299872=CARTESIAN_POINT('Ctrl Pts',(7.51676407774741,55.4749999997882,-10.3459381770588));
#299873=CARTESIAN_POINT('Ctrl Pts',(3.75838203887368,55.6249999997876,-11.5671105274568));
#299874=CARTESIAN_POINT('Ctrl Pts',(-4.53816747791995E-14,55.774999999787,
-12.7882828778549));
#299875=CARTESIAN_POINT('Ctrl Pts',(-3.75838203887377,55.9249999997864,
-11.5671105274568));
#299876=CARTESIAN_POINT('Ctrl Pts',(-7.5167640777475,56.0749999997858,-10.3459381770588));
#299877=CARTESIAN_POINT('Ctrl Pts',(-9.83957192047859,56.2249999997852,
-7.14886745759505));
#299878=CARTESIAN_POINT('Ctrl Pts',(-12.1623797632097,56.3749999997846,
-3.95179673813132));
#299879=CARTESIAN_POINT('Ctrl Pts',(-12.1623797632097,56.524999999784,2.97892388940585E-15));
#299880=CARTESIAN_POINT('Ctrl Pts',(-12.1623797632097,56.6749999997834,
3.95179673813133));
#299881=CARTESIAN_POINT('Ctrl Pts',(-9.83957192047859,56.8249999997828,
7.14886745759505));
#299882=CARTESIAN_POINT('Ctrl Pts',(-7.5167640777475,56.9749999997822,10.3459381770588));
#299883=CARTESIAN_POINT('Ctrl Pts',(-3.75838203887377,57.1249999997816,
11.5671105274568));
#299884=CARTESIAN_POINT('Ctrl Pts',(-4.31133034764393E-14,57.274999999781,
12.7882828778549));
#299885=CARTESIAN_POINT('Ctrl Pts',(3.75838203887368,57.4249999997804,11.5671105274568));
#299886=CARTESIAN_POINT('Ctrl Pts',(7.51676407774741,57.5749999997798,10.3459381770588));
#299887=CARTESIAN_POINT('Ctrl Pts',(9.8395719204785,57.7249999997792,7.14886745759505));
#299888=CARTESIAN_POINT('Ctrl Pts',(12.1623797632096,57.8749999997786,3.95179673813132));
#299889=CARTESIAN_POINT('Ctrl Pts',(12.1623797632096,58.024999999778,-1.48946194470292E-15));
#299890=CARTESIAN_POINT('Ctrl Pts',(12.1623797632096,58.1749999997774,-3.95179673813132));
#299891=CARTESIAN_POINT('Ctrl Pts',(9.8395719204785,58.3249999997768,-7.14886745759505));
#299892=CARTESIAN_POINT('Ctrl Pts',(7.51676407774741,58.4749999997762,-10.3459381770588));
#299893=CARTESIAN_POINT('Ctrl Pts',(3.75838203887368,58.6249999997756,-11.5671105274568));
#299894=CARTESIAN_POINT('Ctrl Pts',(-4.71093840508614E-14,58.774999999775,
-12.7882828778549));
#299895=CARTESIAN_POINT('Ctrl Pts',(-3.75838203887377,58.9249999997744,
-11.5671105274568));
#299896=CARTESIAN_POINT('Ctrl Pts',(-7.5167640777475,59.0749999997738,-10.3459381770588));
#299897=CARTESIAN_POINT('Ctrl Pts',(-9.83957192047859,59.2249999997732,
-7.14886745759505));
#299898=CARTESIAN_POINT('Ctrl Pts',(-12.1623797632097,59.3749999997726,
-3.95179673813132));
#299899=CARTESIAN_POINT('Ctrl Pts',(-12.1623797632097,59.524999999772,2.97892388940585E-15));
#299900=CARTESIAN_POINT('Ctrl Pts',(-12.1623797632097,59.6749999997714,
3.95179673813133));
#299901=CARTESIAN_POINT('Ctrl Pts',(-9.83957192047859,59.8249999997708,
7.14886745759505));
#299902=CARTESIAN_POINT('Ctrl Pts',(-7.5167640777475,59.9749999997702,10.3459381770588));
#299903=CARTESIAN_POINT('Ctrl Pts',(-3.75838203887377,60.1249999997696,
11.5671105274568));
#299904=CARTESIAN_POINT('Ctrl Pts',(-4.48410127481011E-14,60.274999999769,
12.7882828778549));
#299905=CARTESIAN_POINT('Ctrl Pts',(3.75838203887368,60.4249999997684,11.5671105274568));
#299906=CARTESIAN_POINT('Ctrl Pts',(7.51676407774741,60.5749999997678,10.3459381770588));
#299907=CARTESIAN_POINT('Ctrl Pts',(9.8395719204785,60.7249999997672,7.14886745759505));
#299908=CARTESIAN_POINT('Ctrl Pts',(12.1623797632096,60.8749999997666,3.95179673813132));
#299909=CARTESIAN_POINT('Ctrl Pts',(12.1623797632096,61.024999999766,-1.48946194470292E-15));
#299910=CARTESIAN_POINT('Ctrl Pts',(12.1623797632096,61.1749999997654,-3.95179673813132));
#299911=CARTESIAN_POINT('Ctrl Pts',(9.8395719204785,61.3249999997648,-7.14886745759505));
#299912=CARTESIAN_POINT('Ctrl Pts',(7.51676407774741,61.4749999997642,-10.3459381770588));
#299913=CARTESIAN_POINT('Ctrl Pts',(3.75838203887368,61.6249999997636,-11.5671105274568));
#299914=CARTESIAN_POINT('Ctrl Pts',(-4.88370933225232E-14,61.774999999763,
-12.7882828778549));
#299915=CARTESIAN_POINT('Ctrl Pts',(-3.75838203887378,61.9249999997624,
-11.5671105274568));
#299916=CARTESIAN_POINT('Ctrl Pts',(-7.5167640777475,62.0749999997618,-10.3459381770588));
#299917=CARTESIAN_POINT('Ctrl Pts',(-9.8395719204786,62.2249999997612,-7.14886745759505));
#299918=CARTESIAN_POINT('Ctrl Pts',(-12.1623797632097,62.3749999997606,
-3.95179673813132));
#299919=CARTESIAN_POINT('Ctrl Pts',(-12.1623797632097,62.52499999976,2.97892388940585E-15));
#299920=CARTESIAN_POINT('Ctrl Pts',(-12.1623797632097,62.6749999997594,
3.95179673813133));
#299921=CARTESIAN_POINT('Ctrl Pts',(-9.8395719204786,62.8249999997588,7.14886745759505));
#299922=CARTESIAN_POINT('Ctrl Pts',(-7.5167640777475,62.9749999997582,10.3459381770588));
#299923=CARTESIAN_POINT('Ctrl Pts',(-3.75838203887377,63.1249999997576,
11.5671105274568));
#299924=CARTESIAN_POINT('Ctrl Pts',(-4.6568722019763E-14,63.274999999757,
12.7882828778549));
#299925=CARTESIAN_POINT('Ctrl Pts',(3.75838203887368,63.4249999997564,11.5671105274568));
#299926=CARTESIAN_POINT('Ctrl Pts',(7.51676407774741,63.5749999997558,10.3459381770588));
#299927=CARTESIAN_POINT('Ctrl Pts',(9.8395719204785,63.7249999997552,7.14886745759505));
#299928=CARTESIAN_POINT('Ctrl Pts',(12.1623797632096,63.8749999997546,3.95179673813132));
#299929=CARTESIAN_POINT('Ctrl Pts',(12.1623797632096,64.024999999754,-1.48946194470292E-15));
#299930=CARTESIAN_POINT('Ctrl Pts',(12.1623797632096,64.1749999997534,-3.95179673813132));
#299931=CARTESIAN_POINT('Ctrl Pts',(9.8395719204785,64.3249999997528,-7.14886745759505));
#299932=CARTESIAN_POINT('Ctrl Pts',(7.5167640777474,64.4749999997522,-10.3459381770588));
#299933=CARTESIAN_POINT('Ctrl Pts',(3.75838203887368,64.6249999997516,-11.5671105274568));
#299934=CARTESIAN_POINT('Ctrl Pts',(-5.05648025941851E-14,64.774999999751,
-12.7882828778549));
#299935=CARTESIAN_POINT('Ctrl Pts',(-3.75838203887378,64.9249999997504,
-11.5671105274568));
#299936=CARTESIAN_POINT('Ctrl Pts',(-7.51676407774751,65.0749999997498,
-10.3459381770588));
#299937=CARTESIAN_POINT('Ctrl Pts',(-9.8395719204786,65.2249999997492,-7.14886745759505));
#299938=CARTESIAN_POINT('Ctrl Pts',(-12.1623797632097,65.3749999997486,
-3.95179673813132));
#299939=CARTESIAN_POINT('Ctrl Pts',(-12.1623797632097,65.524999999748,2.97892388940585E-15));
#299940=CARTESIAN_POINT('Ctrl Pts',(-12.1623797632097,65.6749999997474,
3.95179673813133));
#299941=CARTESIAN_POINT('Ctrl Pts',(-9.8395719204786,65.8249999997468,7.14886745759505));
#299942=CARTESIAN_POINT('Ctrl Pts',(-7.5167640777475,65.9749999997462,10.3459381770588));
#299943=CARTESIAN_POINT('Ctrl Pts',(-3.75838203887378,66.1249999997456,
11.5671105274568));
#299944=CARTESIAN_POINT('Ctrl Pts',(-4.82964312914248E-14,66.274999999745,
12.7882828778549));
#299945=CARTESIAN_POINT('Ctrl Pts',(3.75838203887368,66.4249999997444,11.5671105274568));
#299946=CARTESIAN_POINT('Ctrl Pts',(7.51676407774741,66.5749999997438,10.3459381770588));
#299947=CARTESIAN_POINT('Ctrl Pts',(9.8395719204785,66.7249999997432,7.14886745759505));
#299948=CARTESIAN_POINT('Ctrl Pts',(12.1623797632096,66.8749999997426,3.95179673813132));
#299949=CARTESIAN_POINT('Ctrl Pts',(12.1623797632096,67.024999999742,-1.48946194470292E-15));
#299950=CARTESIAN_POINT('Ctrl Pts',(12.1623797632096,67.1749999997414,-3.95179673813132));
#299951=CARTESIAN_POINT('Ctrl Pts',(9.8395719204785,67.3249999997408,-7.14886745759505));
#299952=CARTESIAN_POINT('Ctrl Pts',(7.5167640777474,67.4749999997402,-10.3459381770588));
#299953=CARTESIAN_POINT('Ctrl Pts',(3.75838203887368,67.6249999997396,-11.5671105274568));
#299954=CARTESIAN_POINT('Ctrl Pts',(-5.22925118658469E-14,67.774999999739,
-12.7882828778549));
#299955=CARTESIAN_POINT('Ctrl Pts',(-3.75838203887378,67.9249999997384,
-11.5671105274568));
#299956=CARTESIAN_POINT('Ctrl Pts',(-7.51676407774751,68.0749999997378,
-10.3459381770588));
#299957=CARTESIAN_POINT('Ctrl Pts',(-9.8395719204786,68.2249999997372,-7.14886745759505));
#299958=CARTESIAN_POINT('Ctrl Pts',(-12.1623797632097,68.3749999997366,
-3.95179673813132));
#299959=CARTESIAN_POINT('Ctrl Pts',(-12.1623797632097,68.524999999736,2.97892388940585E-15));
#299960=CARTESIAN_POINT('Ctrl Pts',(-12.1623797632097,68.6749999997354,
3.95179673813133));
#299961=CARTESIAN_POINT('Ctrl Pts',(-9.8395719204786,68.8249999997348,7.14886745759505));
#299962=CARTESIAN_POINT('Ctrl Pts',(-7.51676407774751,68.9749999997342,
10.3459381770588));
#299963=CARTESIAN_POINT('Ctrl Pts',(-3.75838203887378,69.1249999997336,
11.5671105274568));
#299964=CARTESIAN_POINT('Ctrl Pts',(-5.00241405630866E-14,69.274999999733,
12.7882828778549));
#299965=CARTESIAN_POINT('Ctrl Pts',(3.75838203887368,69.4249999997324,11.5671105274568));
#299966=CARTESIAN_POINT('Ctrl Pts',(7.5167640777474,69.5749999997318,10.3459381770588));
#299967=CARTESIAN_POINT('Ctrl Pts',(9.8395719204785,69.7249999997312,7.14886745759505));
#299968=CARTESIAN_POINT('Ctrl Pts',(12.1623797632096,69.8749999997306,3.95179673813132));
#299969=CARTESIAN_POINT('Ctrl Pts',(12.1623797632096,70.02499999973,-1.48946194470292E-15));
#299970=CARTESIAN_POINT('Ctrl Pts',(12.1623797632096,70.1749999997294,-3.95179673813132));
#299971=CARTESIAN_POINT('Ctrl Pts',(9.83957192047849,70.3249999997288,-7.14886745759505));
#299972=CARTESIAN_POINT('Ctrl Pts',(7.5167640777474,70.4749999997282,-10.3459381770588));
#299973=CARTESIAN_POINT('Ctrl Pts',(3.75838203887367,70.6249999997276,-11.5671105274568));
#299974=CARTESIAN_POINT('Ctrl Pts',(-5.40202211375087E-14,70.774999999727,
-12.7882828778549));
#299975=CARTESIAN_POINT('Ctrl Pts',(-3.75838203887378,70.9249999997264,
-11.5671105274568));
#299976=CARTESIAN_POINT('Ctrl Pts',(-7.51676407774751,71.0749999997258,
-10.3459381770588));
#299977=CARTESIAN_POINT('Ctrl Pts',(-9.8395719204786,71.2249999997252,-7.14886745759505));
#299978=CARTESIAN_POINT('Ctrl Pts',(-12.1623797632097,71.3749999997246,
-3.95179673813132));
#299979=CARTESIAN_POINT('Ctrl Pts',(-12.1623797632097,71.524999999724,2.97892388940585E-15));
#299980=CARTESIAN_POINT('Ctrl Pts',(-12.1623797632097,71.6749999997234,
3.95179673813133));
#299981=CARTESIAN_POINT('Ctrl Pts',(-9.8395719204786,71.8249999997228,7.14886745759505));
#299982=CARTESIAN_POINT('Ctrl Pts',(-7.51676407774751,71.9749999997222,
10.3459381770588));
#299983=CARTESIAN_POINT('Ctrl Pts',(-3.75838203887378,72.1249999997216,
11.5671105274568));
#299984=CARTESIAN_POINT('Ctrl Pts',(-5.17518498347485E-14,72.274999999721,
12.7882828778549));
#299985=CARTESIAN_POINT('Ctrl Pts',(3.75838203887368,72.4249999997204,11.5671105274568));
#299986=CARTESIAN_POINT('Ctrl Pts',(7.5167640777474,72.5749999997198,10.3459381770588));
#299987=CARTESIAN_POINT('Ctrl Pts',(9.83957192047849,72.7249999997192,7.14886745759505));
#299988=CARTESIAN_POINT('Ctrl Pts',(12.1623797632096,72.8749999997186,3.95179673813132));
#299989=CARTESIAN_POINT('Ctrl Pts',(12.1623797632096,73.024999999718,-1.48946194470292E-15));
#299990=CARTESIAN_POINT('Ctrl Pts',(12.1623797632096,73.1749999997174,-3.95179673813132));
#299991=CARTESIAN_POINT('Ctrl Pts',(9.83957192047849,73.3249999997168,-7.14886745759505));
#299992=CARTESIAN_POINT('Ctrl Pts',(7.5167640777474,73.4749999997162,-10.3459381770588));
#299993=CARTESIAN_POINT('Ctrl Pts',(3.75838203887367,73.6249999997156,-11.5671105274568));
#299994=CARTESIAN_POINT('Ctrl Pts',(-5.57479304091706E-14,73.774999999715,
-12.7882828778549));
#299995=CARTESIAN_POINT('Ctrl Pts',(-3.75838203887378,73.9249999997144,
-11.5671105274568));
#299996=CARTESIAN_POINT('Ctrl Pts',(-7.51676407774751,74.0749999997138,
-10.3459381770588));
#299997=CARTESIAN_POINT('Ctrl Pts',(-9.8395719204786,74.2249999997132,-7.14886745759505));
#299998=CARTESIAN_POINT('Ctrl Pts',(-12.1623797632097,74.3749999997126,
-3.95179673813132));
#299999=CARTESIAN_POINT('Ctrl Pts',(-12.1623797632097,74.524999999712,2.97892388940585E-15));
#300000=CARTESIAN_POINT('Ctrl Pts',(-12.1623797632097,74.6749999997114,
3.95179673813133));
#300001=CARTESIAN_POINT('Ctrl Pts',(-9.8395719204786,74.8249999997108,7.14886745759505));
#300002=CARTESIAN_POINT('Ctrl Pts',(-7.51676407774751,74.9749999997102,
10.3459381770588));
#300003=CARTESIAN_POINT('Ctrl Pts',(-3.75838203887378,75.1249999997096,
11.5671105274568));
#300004=CARTESIAN_POINT('Ctrl Pts',(-5.34795591064103E-14,75.274999999709,
12.7882828778549));
#300005=CARTESIAN_POINT('Ctrl Pts',(3.75838203887367,75.4249999997084,11.5671105274568));
#300006=CARTESIAN_POINT('Ctrl Pts',(7.5167640777474,75.5749999997078,10.3459381770588));
#300007=CARTESIAN_POINT('Ctrl Pts',(9.83957192047849,75.7249999997072,7.14886745759505));
#300008=CARTESIAN_POINT('Ctrl Pts',(12.1623797632096,75.8749999997066,3.95179673813132));
#300009=CARTESIAN_POINT('Ctrl Pts',(12.1623797632096,76.024999999706,-1.48946194470292E-15));
#300010=CARTESIAN_POINT('Ctrl Pts',(12.1623797632096,76.1749999997054,-3.95179673813132));
#300011=CARTESIAN_POINT('Ctrl Pts',(9.83957192047849,76.3249999997048,-7.14886745759505));
#300012=CARTESIAN_POINT('Ctrl Pts',(7.5167640777474,76.4749999997042,-10.3459381770588));
#300013=CARTESIAN_POINT('Ctrl Pts',(3.75838203887367,76.6249999997036,-11.5671105274568));
#300014=CARTESIAN_POINT('Ctrl Pts',(-5.74756396808324E-14,76.774999999703,
-12.7882828778549));
#300015=CARTESIAN_POINT('Ctrl Pts',(-3.75838203887379,76.9249999997024,
-11.5671105274568));
#300016=CARTESIAN_POINT('Ctrl Pts',(-7.51676407774751,77.0749999997018,
-10.3459381770588));
#300017=CARTESIAN_POINT('Ctrl Pts',(-9.8395719204786,77.2249999997012,-7.14886745759505));
#300018=CARTESIAN_POINT('Ctrl Pts',(-12.1623797632097,77.3749999997006,
-3.95179673813132));
#300019=CARTESIAN_POINT('Ctrl Pts',(-12.1623797632097,77.5249999997,2.97892388940585E-15));
#300020=CARTESIAN_POINT('Ctrl Pts',(-12.1623797632097,77.6749999996994,
3.95179673813133));
#300021=CARTESIAN_POINT('Ctrl Pts',(-9.8395719204786,77.8249999996988,7.14886745759505));
#300022=CARTESIAN_POINT('Ctrl Pts',(-7.51676407774751,77.9749999996982,
10.3459381770588));
#300023=CARTESIAN_POINT('Ctrl Pts',(-3.75838203887378,78.1249999996976,
11.5671105274568));
#300024=CARTESIAN_POINT('Ctrl Pts',(-5.52072683780721E-14,78.274999999697,
12.7882828778549));
#300025=CARTESIAN_POINT('Ctrl Pts',(3.75838203887367,78.4249999996964,11.5671105274568));
#300026=CARTESIAN_POINT('Ctrl Pts',(7.5167640777474,78.5749999996958,10.3459381770588));
#300027=CARTESIAN_POINT('Ctrl Pts',(9.83957192047849,78.7249999996952,7.14886745759505));
#300028=CARTESIAN_POINT('Ctrl Pts',(12.1623797632096,78.8749999996946,3.95179673813132));
#300029=CARTESIAN_POINT('Ctrl Pts',(12.1623797632096,79.024999999694,-1.48946194470292E-15));
#300030=CARTESIAN_POINT('Ctrl Pts',(12.1623797632096,79.1749999996934,-3.95179673813132));
#300031=CARTESIAN_POINT('Ctrl Pts',(9.83957192047849,79.3249999996928,-7.14886745759505));
#300032=CARTESIAN_POINT('Ctrl Pts',(7.5167640777474,79.4749999996922,-10.3459381770588));
#300033=CARTESIAN_POINT('Ctrl Pts',(3.75838203887367,79.6249999996916,-11.5671105274568));
#300034=CARTESIAN_POINT('Ctrl Pts',(-5.92033489524943E-14,79.774999999691,
-12.7882828778549));
#300035=CARTESIAN_POINT('Ctrl Pts',(-3.75838203887379,79.9249999996904,
-11.5671105274568));
#300036=CARTESIAN_POINT('Ctrl Pts',(-7.51676407774751,80.0749999996898,
-10.3459381770588));
#300037=CARTESIAN_POINT('Ctrl Pts',(-9.83957192047861,80.2249999996892,
-7.14886745759505));
#300038=CARTESIAN_POINT('Ctrl Pts',(-12.1623797632097,80.3749999996886,
-3.95179673813132));
#300039=CARTESIAN_POINT('Ctrl Pts',(-12.1623797632097,80.524999999688,2.97892388940585E-15));
#300040=CARTESIAN_POINT('Ctrl Pts',(-12.1623797632097,80.6749999996874,
3.95179673813133));
#300041=CARTESIAN_POINT('Ctrl Pts',(-9.83957192047861,80.8249999996868,
7.14886745759505));
#300042=CARTESIAN_POINT('Ctrl Pts',(-7.51676407774751,80.9749999996862,
10.3459381770588));
#300043=CARTESIAN_POINT('Ctrl Pts',(-3.75838203887378,81.1249999996856,
11.5671105274568));
#300044=CARTESIAN_POINT('Ctrl Pts',(-5.6934977649734E-14,81.274999999685,
12.7882828778549));
#300045=CARTESIAN_POINT('Ctrl Pts',(3.75838203887367,81.4249999996844,11.5671105274568));
#300046=CARTESIAN_POINT('Ctrl Pts',(7.5167640777474,81.5749999996838,10.3459381770588));
#300047=CARTESIAN_POINT('Ctrl Pts',(9.83957192047849,81.7249999996832,7.14886745759505));
#300048=CARTESIAN_POINT('Ctrl Pts',(12.1623797632096,81.8749999996826,3.95179673813132));
#300049=CARTESIAN_POINT('Ctrl Pts',(12.1623797632096,82.024999999682,-1.48946194470292E-15));
#300050=CARTESIAN_POINT('Ctrl Pts',(12.1623797632096,82.1749999996814,-3.95179673813132));
#300051=CARTESIAN_POINT('Ctrl Pts',(9.83957192047849,82.3249999996808,-7.14886745759505));
#300052=CARTESIAN_POINT('Ctrl Pts',(7.5167640777474,82.4749999996802,-10.3459381770588));
#300053=CARTESIAN_POINT('Ctrl Pts',(3.75838203887367,82.6249999996796,-11.5671105274568));
#300054=CARTESIAN_POINT('Ctrl Pts',(-6.09310582241561E-14,82.774999999679,
-12.7882828778549));
#300055=CARTESIAN_POINT('Ctrl Pts',(-3.75838203887379,82.9249999996784,
-11.5671105274568));
#300056=CARTESIAN_POINT('Ctrl Pts',(-7.51676407774752,83.0749999996778,
-10.3459381770588));
#300057=CARTESIAN_POINT('Ctrl Pts',(-9.83957192047861,83.2249999996772,
-7.14886745759505));
#300058=CARTESIAN_POINT('Ctrl Pts',(-12.1623797632097,83.3749999996766,
-3.95179673813132));
#300059=CARTESIAN_POINT('Ctrl Pts',(-12.1623797632097,83.524999999676,2.97892388940585E-15));
#300060=CARTESIAN_POINT('Ctrl Pts',(-12.1623797632097,83.6749999996754,
3.95179673813133));
#300061=CARTESIAN_POINT('Ctrl Pts',(-9.83957192047861,83.8249999996748,
7.14886745759505));
#300062=CARTESIAN_POINT('Ctrl Pts',(-7.51676407774751,83.9749999996742,
10.3459381770588));
#300063=CARTESIAN_POINT('Ctrl Pts',(-3.75838203887379,84.1249999996736,
11.5671105274568));
#300064=CARTESIAN_POINT('Ctrl Pts',(-5.86626869213958E-14,84.274999999673,
12.7882828778549));
#300065=CARTESIAN_POINT('Ctrl Pts',(3.75838203887367,84.4249999996724,11.5671105274568));
#300066=CARTESIAN_POINT('Ctrl Pts',(7.5167640777474,84.5749999996718,10.3459381770588));
#300067=CARTESIAN_POINT('Ctrl Pts',(9.83957192047849,84.7249999996712,7.14886745759505));
#300068=CARTESIAN_POINT('Ctrl Pts',(12.1623797632096,84.8749999996706,3.95179673813132));
#300069=CARTESIAN_POINT('Ctrl Pts',(12.1623797632096,85.02499999967,-1.48946194470292E-15));
#300070=CARTESIAN_POINT('Ctrl Pts',(12.1623797632096,85.1749999996694,-3.95179673813132));
#300071=CARTESIAN_POINT('Ctrl Pts',(9.83957192047849,85.3249999996688,-7.14886745759505));
#300072=CARTESIAN_POINT('Ctrl Pts',(7.51676407774739,85.4749999996682,-10.3459381770588));
#300073=CARTESIAN_POINT('Ctrl Pts',(3.75838203887367,85.6249999996676,-11.5671105274568));
#300074=CARTESIAN_POINT('Ctrl Pts',(-6.26587674958179E-14,85.774999999667,
-12.7882828778549));
#300075=CARTESIAN_POINT('Ctrl Pts',(-3.75838203887379,85.9249999996664,
-11.5671105274568));
#300076=CARTESIAN_POINT('Ctrl Pts',(-7.51676407774752,86.0749999996658,
-10.3459381770588));
#300077=CARTESIAN_POINT('Ctrl Pts',(-9.83957192047861,86.2249999996652,
-7.14886745759505));
#300078=CARTESIAN_POINT('Ctrl Pts',(-12.1623797632097,86.3749999996646,
-3.95179673813132));
#300079=CARTESIAN_POINT('Ctrl Pts',(-12.1623797632097,86.524999999664,2.97892388940585E-15));
#300080=CARTESIAN_POINT('Ctrl Pts',(-12.1623797632097,86.6749999996634,
3.95179673813133));
#300081=CARTESIAN_POINT('Ctrl Pts',(-9.83957192047861,86.8249999996628,
7.14886745759505));
#300082=CARTESIAN_POINT('Ctrl Pts',(-7.51676407774752,86.9749999996622,
10.3459381770588));
#300083=CARTESIAN_POINT('Ctrl Pts',(-3.75838203887379,87.1249999996616,
11.5671105274568));
#300084=CARTESIAN_POINT('Ctrl Pts',(-6.03903961930577E-14,87.274999999661,
12.7882828778549));
#300085=CARTESIAN_POINT('Ctrl Pts',(3.75838203887367,87.4249999996604,11.5671105274568));
#300086=CARTESIAN_POINT('Ctrl Pts',(7.5167640777474,87.5749999996598,10.3459381770588));
#300087=CARTESIAN_POINT('Ctrl Pts',(9.83957192047849,87.7249999996592,7.14886745759505));
#300088=CARTESIAN_POINT('Ctrl Pts',(12.1623797632096,87.8749999996586,3.95179673813132));
#300089=CARTESIAN_POINT('Ctrl Pts',(12.1623797632096,88.024999999658,-1.48946194470292E-15));
#300090=CARTESIAN_POINT('Ctrl Pts',(12.1623797632096,88.1749999996574,-3.95179673813132));
#300091=CARTESIAN_POINT('Ctrl Pts',(9.83957192047849,88.3249999996568,-7.14886745759505));
#300092=CARTESIAN_POINT('Ctrl Pts',(7.51676407774739,88.4749999996562,-10.3459381770588));
#300093=CARTESIAN_POINT('Ctrl Pts',(3.75838203887366,88.6249999996556,-11.5671105274568));
#300094=CARTESIAN_POINT('Ctrl Pts',(-6.43864767674798E-14,88.774999999655,
-12.7882828778549));
#300095=CARTESIAN_POINT('Ctrl Pts',(-3.75838203887379,88.9249999996544,
-11.5671105274568));
#300096=CARTESIAN_POINT('Ctrl Pts',(-7.51676407774752,89.0749999996538,
-10.3459381770588));
#300097=CARTESIAN_POINT('Ctrl Pts',(-9.83957192047861,89.2249999996532,
-7.14886745759505));
#300098=CARTESIAN_POINT('Ctrl Pts',(-12.1623797632097,89.3749999996526,
-3.95179673813132));
#300099=CARTESIAN_POINT('Ctrl Pts',(-12.1623797632097,89.524999999652,2.97892388940585E-15));
#300100=CARTESIAN_POINT('Ctrl Pts',(-12.1623797632097,89.6749999996514,
3.95179673813133));
#300101=CARTESIAN_POINT('Ctrl Pts',(-9.83957192047861,89.8249999996508,
7.14886745759505));
#300102=CARTESIAN_POINT('Ctrl Pts',(-7.51676407774752,89.9749999996502,
10.3459381770588));
#300103=CARTESIAN_POINT('Ctrl Pts',(-3.75838203887379,90.1249999996496,
11.5671105274568));
#300104=CARTESIAN_POINT('Ctrl Pts',(-6.21181054647195E-14,90.274999999649,
12.7882828778549));
#300105=CARTESIAN_POINT('Ctrl Pts',(3.75838203887366,90.4249999996484,11.5671105274568));
#300106=CARTESIAN_POINT('Ctrl Pts',(7.51676407774739,90.5749999996478,10.3459381770588));
#300107=CARTESIAN_POINT('Ctrl Pts',(9.83957192047848,90.7249999996472,7.14886745759505));
#300108=CARTESIAN_POINT('Ctrl Pts',(12.1623797632096,90.8749999996466,3.95179673813132));
#300109=CARTESIAN_POINT('Ctrl Pts',(12.1623797632096,91.024999999646,-1.48946194470292E-15));
#300110=CARTESIAN_POINT('Ctrl Pts',(12.1623797632096,91.1749999996454,-3.95179673813132));
#300111=CARTESIAN_POINT('Ctrl Pts',(9.83957192047848,91.3249999996448,-7.14886745759505));
#300112=CARTESIAN_POINT('Ctrl Pts',(7.51676407774739,91.4749999996442,-10.3459381770588));
#300113=CARTESIAN_POINT('Ctrl Pts',(3.75838203887366,91.6249999996436,-11.5671105274568));
#300114=CARTESIAN_POINT('Ctrl Pts',(-6.61141860391416E-14,91.774999999643,
-12.7882828778549));
#300115=CARTESIAN_POINT('Ctrl Pts',(-3.75838203887379,91.9249999996424,
-11.5671105274568));
#300116=CARTESIAN_POINT('Ctrl Pts',(-7.51676407774752,92.0749999996418,
-10.3459381770588));
#300117=CARTESIAN_POINT('Ctrl Pts',(-9.83957192047861,92.2249999996412,
-7.14886745759505));
#300118=CARTESIAN_POINT('Ctrl Pts',(-12.1623797632097,92.3749999996406,
-3.95179673813132));
#300119=CARTESIAN_POINT('Ctrl Pts',(-12.1623797632097,92.52499999964,2.97892388940585E-15));
#300120=CARTESIAN_POINT('Ctrl Pts',(-12.1623797632097,92.6749999996394,
3.95179673813133));
#300121=CARTESIAN_POINT('Ctrl Pts',(-9.83957192047861,92.8249999996388,
7.14886745759505));
#300122=CARTESIAN_POINT('Ctrl Pts',(-7.51676407774752,92.9749999996382,
10.3459381770588));
#300123=CARTESIAN_POINT('Ctrl Pts',(-3.75838203887379,93.1249999996376,
11.5671105274568));
#300124=CARTESIAN_POINT('Ctrl Pts',(-6.38458147363813E-14,93.274999999637,
12.7882828778549));
#300125=CARTESIAN_POINT('Ctrl Pts',(3.75838203887366,93.4249999996364,11.5671105274568));
#300126=CARTESIAN_POINT('Ctrl Pts',(7.51676407774739,93.5749999996358,10.3459381770588));
#300127=CARTESIAN_POINT('Ctrl Pts',(9.83957192047848,93.7249999996352,7.14886745759505));
#300128=CARTESIAN_POINT('Ctrl Pts',(12.1623797632096,93.8749999996346,3.95179673813132));
#300129=CARTESIAN_POINT('Ctrl Pts',(12.1623797632096,94.024999999634,-1.48946194470292E-15));
#300130=CARTESIAN_POINT('Ctrl Pts',(12.1623797632096,94.1749999996334,-3.95179673813132));
#300131=CARTESIAN_POINT('Ctrl Pts',(9.83957192047848,94.3249999996328,-7.14886745759505));
#300132=CARTESIAN_POINT('Ctrl Pts',(7.51676407774739,94.4749999996322,-10.3459381770588));
#300133=CARTESIAN_POINT('Ctrl Pts',(3.75838203887366,94.6249999996316,-11.5671105274568));
#300134=CARTESIAN_POINT('Ctrl Pts',(-6.78418953108034E-14,94.774999999631,
-12.7882828778549));
#300135=CARTESIAN_POINT('Ctrl Pts',(-3.7583820388738,94.9249999996304,-11.5671105274568));
#300136=CARTESIAN_POINT('Ctrl Pts',(-7.51676407774752,95.0749999996298,
-10.3459381770588));
#300137=CARTESIAN_POINT('Ctrl Pts',(-9.83957192047862,95.2249999996292,
-7.14886745759505));
#300138=CARTESIAN_POINT('Ctrl Pts',(-12.1623797632097,95.3749999996286,
-3.95179673813132));
#300139=CARTESIAN_POINT('Ctrl Pts',(-12.1623797632097,95.524999999628,2.97892388940585E-15));
#300140=CARTESIAN_POINT('Ctrl Pts',(-12.1623797632097,95.6749999996274,
3.95179673813133));
#300141=CARTESIAN_POINT('Ctrl Pts',(-9.83957192047862,95.8249999996268,
7.14886745759505));
#300142=CARTESIAN_POINT('Ctrl Pts',(-7.51676407774752,95.9749999996262,
10.3459381770588));
#300143=CARTESIAN_POINT('Ctrl Pts',(-3.75838203887379,96.1249999996256,
11.5671105274568));
#300144=CARTESIAN_POINT('Ctrl Pts',(-6.55735240080432E-14,96.274999999625,
12.7882828778549));
#300145=CARTESIAN_POINT('Ctrl Pts',(3.75838203887366,96.4249999996244,11.5671105274568));
#300146=CARTESIAN_POINT('Ctrl Pts',(7.51676407774739,96.5749999996238,10.3459381770588));
#300147=CARTESIAN_POINT('Ctrl Pts',(9.83957192047848,96.7249999996232,7.14886745759505));
#300148=CARTESIAN_POINT('Ctrl Pts',(12.1623797632096,96.8749999996226,3.95179673813132));
#300149=CARTESIAN_POINT('Ctrl Pts',(12.1623797632096,97.024999999622,-1.48946194470292E-15));
#300150=CARTESIAN_POINT('Ctrl Pts',(12.1623797632096,97.1749999996214,-3.95179673813132));
#300151=CARTESIAN_POINT('Ctrl Pts',(9.83957192047848,97.3249999996208,-7.14886745759505));
#300152=CARTESIAN_POINT('Ctrl Pts',(7.51676407774739,97.4749999996202,-10.3459381770588));
#300153=CARTESIAN_POINT('Ctrl Pts',(3.75838203887366,97.6249999996196,-11.5671105274568));
#300154=CARTESIAN_POINT('Ctrl Pts',(-6.95696045824653E-14,97.774999999619,
-12.7882828778549));
#300155=CARTESIAN_POINT('Ctrl Pts',(-3.7583820388738,97.9249999996184,-11.5671105274568));
#300156=CARTESIAN_POINT('Ctrl Pts',(-7.51676407774752,98.0749999996178,
-10.3459381770588));
#300157=CARTESIAN_POINT('Ctrl Pts',(-9.83957192047862,98.2249999996172,
-7.14886745759505));
#300158=CARTESIAN_POINT('Ctrl Pts',(-12.1623797632097,98.3749999996166,
-3.95179673813132));
#300159=CARTESIAN_POINT('Ctrl Pts',(-12.1623797632097,98.524999999616,2.97892388940585E-15));
#300160=CARTESIAN_POINT('Ctrl Pts',(-12.1623797632097,98.6749999996154,
3.95179673813133));
#300161=CARTESIAN_POINT('Ctrl Pts',(-9.83957192047862,98.8249999996148,
7.14886745759505));
#300162=CARTESIAN_POINT('Ctrl Pts',(-7.51676407774752,98.9749999996142,
10.3459381770588));
#300163=CARTESIAN_POINT('Ctrl Pts',(-3.7583820388738,99.1249999996136,11.5671105274568));
#300164=CARTESIAN_POINT('Ctrl Pts',(-6.7301233279705E-14,99.274999999613,
12.7882828778549));
#300165=CARTESIAN_POINT('Ctrl Pts',(3.75838203887366,99.4249999996124,11.5671105274568));
#300166=CARTESIAN_POINT('Ctrl Pts',(7.51676407774739,99.5749999996118,10.3459381770588));
#300167=CARTESIAN_POINT('Ctrl Pts',(9.83957192047848,99.7249999996112,7.14886745759505));
#300168=CARTESIAN_POINT('Ctrl Pts',(12.1623797632096,99.8749999996106,3.95179673813132));
#300169=CARTESIAN_POINT('Ctrl Pts',(12.1623797632096,100.02499999961,-1.48946194470292E-15));
#300170=CARTESIAN_POINT('Ctrl Pts',(12.1623797632096,100.174999999609,-3.95179673813132));
#300171=CARTESIAN_POINT('Ctrl Pts',(9.83957192047848,100.324999999609,-7.14886745759505));
#300172=CARTESIAN_POINT('Ctrl Pts',(7.51676407774738,100.474999999608,-10.3459381770588));
#300173=CARTESIAN_POINT('Ctrl Pts',(3.75838203887366,100.624999999608,-11.5671105274568));
#300174=CARTESIAN_POINT('Ctrl Pts',(-7.12973138541271E-14,100.774999999607,
-12.7882828778549));
#300175=CARTESIAN_POINT('Ctrl Pts',(-3.7583820388738,100.924999999606,-11.5671105274568));
#300176=CARTESIAN_POINT('Ctrl Pts',(-7.51676407774753,101.074999999606,
-10.3459381770588));
#300177=CARTESIAN_POINT('Ctrl Pts',(-9.83957192047862,101.224999999605,
-7.14886745759505));
#300178=CARTESIAN_POINT('Ctrl Pts',(-12.1623797632097,101.374999999605,
-3.95179673813132));
#300179=CARTESIAN_POINT('Ctrl Pts',(-12.1623797632097,101.524999999604,
2.97892388940585E-15));
#300180=CARTESIAN_POINT('Ctrl Pts',(-12.1623797632097,101.674999999603,
3.95179673813133));
#300181=CARTESIAN_POINT('Ctrl Pts',(-9.83957192047862,101.824999999603,
7.14886745759505));
#300182=CARTESIAN_POINT('Ctrl Pts',(-7.51676407774752,101.974999999602,
10.3459381770588));
#300183=CARTESIAN_POINT('Ctrl Pts',(-3.7583820388738,102.124999999602,11.5671105274568));
#300184=CARTESIAN_POINT('Ctrl Pts',(-6.90289425513669E-14,102.274999999601,
12.7882828778549));
#300185=CARTESIAN_POINT('Ctrl Pts',(3.75838203887366,102.4249999996,11.5671105274568));
#300186=CARTESIAN_POINT('Ctrl Pts',(7.51676407774739,102.5749999996,10.3459381770588));
#300187=CARTESIAN_POINT('Ctrl Pts',(9.83957192047848,102.724999999599,7.14886745759505));
#300188=CARTESIAN_POINT('Ctrl Pts',(12.1623797632096,102.874999999599,3.95179673813132));
#300189=CARTESIAN_POINT('Ctrl Pts',(12.1623797632096,103.024999999598,-1.48946194470292E-15));
#300190=CARTESIAN_POINT('Ctrl Pts',(12.1623797632096,103.174999999597,-3.95179673813132));
#300191=CARTESIAN_POINT('Ctrl Pts',(9.83957192047848,103.324999999597,-7.14886745759505));
#300192=CARTESIAN_POINT('Ctrl Pts',(7.51676407774738,103.474999999596,-10.3459381770588));
#300193=CARTESIAN_POINT('Ctrl Pts',(3.75838203887366,103.624999999596,-11.5671105274568));
#300194=CARTESIAN_POINT('Ctrl Pts',(-7.3025023125789E-14,103.774999999595,
-12.7882828778549));
#300195=CARTESIAN_POINT('Ctrl Pts',(-3.7583820388738,103.924999999594,-11.5671105274568));
#300196=CARTESIAN_POINT('Ctrl Pts',(-7.51676407774753,104.074999999594,
-10.3459381770588));
#300197=CARTESIAN_POINT('Ctrl Pts',(-9.83957192047862,104.224999999593,
-7.14886745759505));
#300198=CARTESIAN_POINT('Ctrl Pts',(-12.1623797632097,104.374999999593,
-3.95179673813132));
#300199=CARTESIAN_POINT('Ctrl Pts',(-12.1623797632097,104.524999999592,
2.97892388940585E-15));
#300200=CARTESIAN_POINT('Ctrl Pts',(-12.1623797632097,104.674999999591,
3.95179673813133));
#300201=CARTESIAN_POINT('Ctrl Pts',(-9.83957192047862,104.824999999591,
7.14886745759505));
#300202=CARTESIAN_POINT('Ctrl Pts',(-7.51676407774753,104.97499999959,10.3459381770588));
#300203=CARTESIAN_POINT('Ctrl Pts',(-3.7583820388738,105.12499999959,11.5671105274568));
#300204=CARTESIAN_POINT('Ctrl Pts',(-7.07566518230287E-14,105.274999999589,
12.7882828778549));
#300205=CARTESIAN_POINT('Ctrl Pts',(3.75838203887366,105.424999999588,11.5671105274568));
#300206=CARTESIAN_POINT('Ctrl Pts',(7.51676407774738,105.574999999588,10.3459381770588));
#300207=CARTESIAN_POINT('Ctrl Pts',(9.83957192047848,105.724999999587,7.14886745759505));
#300208=CARTESIAN_POINT('Ctrl Pts',(12.1623797632096,105.874999999587,3.95179673813132));
#300209=CARTESIAN_POINT('Ctrl Pts',(12.1623797632096,106.024999999586,-1.48946194470292E-15));
#300210=CARTESIAN_POINT('Ctrl Pts',(12.1623797632096,106.174999999585,-3.95179673813132));
#300211=CARTESIAN_POINT('Ctrl Pts',(9.83957192047848,106.324999999585,-7.14886745759505));
#300212=CARTESIAN_POINT('Ctrl Pts',(7.51676407774738,106.474999999584,-10.3459381770588));
#300213=CARTESIAN_POINT('Ctrl Pts',(3.75838203887365,106.624999999584,-11.5671105274568));
#300214=CARTESIAN_POINT('Ctrl Pts',(-7.47527323974508E-14,106.774999999583,
-12.7882828778549));
#300215=CARTESIAN_POINT('Ctrl Pts',(-3.7583820388738,106.924999999582,-11.5671105274568));
#300216=CARTESIAN_POINT('Ctrl Pts',(-7.51676407774753,107.074999999582,
-10.3459381770588));
#300217=CARTESIAN_POINT('Ctrl Pts',(-9.83957192047862,107.224999999581,
-7.14886745759505));
#300218=CARTESIAN_POINT('Ctrl Pts',(-12.1623797632097,107.374999999581,
-3.95179673813132));
#300219=CARTESIAN_POINT('Ctrl Pts',(-12.1623797632097,107.52499999958,2.97892388940585E-15));
#300220=CARTESIAN_POINT('Ctrl Pts',(-12.1623797632097,107.674999999579,
3.95179673813133));
#300221=CARTESIAN_POINT('Ctrl Pts',(-9.83957192047862,107.824999999579,
7.14886745759505));
#300222=CARTESIAN_POINT('Ctrl Pts',(-7.51676407774753,107.974999999578,
10.3459381770588));
#300223=CARTESIAN_POINT('Ctrl Pts',(-3.7583820388738,108.124999999578,11.5671105274568));
#300224=CARTESIAN_POINT('Ctrl Pts',(-7.24843610946905E-14,108.274999999577,
12.7882828778549));
#300225=CARTESIAN_POINT('Ctrl Pts',(3.75838203887366,108.424999999576,11.5671105274568));
#300226=CARTESIAN_POINT('Ctrl Pts',(7.51676407774738,108.574999999576,10.3459381770588));
#300227=CARTESIAN_POINT('Ctrl Pts',(9.83957192047847,108.724999999575,7.14886745759505));
#300228=CARTESIAN_POINT('Ctrl Pts',(12.1623797632096,108.874999999575,3.95179673813132));
#300229=CARTESIAN_POINT('Ctrl Pts',(12.1623797632096,109.024999999574,-1.48946194470292E-15));
#300230=CARTESIAN_POINT('Ctrl Pts',(12.1623797632096,109.174999999573,-3.95179673813132));
#300231=CARTESIAN_POINT('Ctrl Pts',(9.83957192047847,109.324999999573,-7.14886745759505));
#300232=CARTESIAN_POINT('Ctrl Pts',(7.51676407774738,109.474999999572,-10.3459381770588));
#300233=CARTESIAN_POINT('Ctrl Pts',(3.75838203887365,109.624999999572,-11.5671105274568));
#300234=CARTESIAN_POINT('Ctrl Pts',(-7.64804416691126E-14,109.774999999571,
-12.7882828778549));
#300235=CARTESIAN_POINT('Ctrl Pts',(-3.7583820388738,109.92499999957,-11.5671105274568));
#300236=CARTESIAN_POINT('Ctrl Pts',(-7.51676407774753,110.07499999957,-10.3459381770588));
#300237=CARTESIAN_POINT('Ctrl Pts',(-9.83957192047862,110.224999999569,
-7.14886745759505));
#300238=CARTESIAN_POINT('Ctrl Pts',(-12.1623797632097,110.374999999569,
-3.95179673813132));
#300239=CARTESIAN_POINT('Ctrl Pts',(-12.1623797632097,110.524999999568,
2.97892388940585E-15));
#300240=CARTESIAN_POINT('Ctrl Pts',(-12.1623797632097,110.674999999567,
3.95179673813133));
#300241=CARTESIAN_POINT('Ctrl Pts',(-9.83957192047862,110.824999999567,
7.14886745759505));
#300242=CARTESIAN_POINT('Ctrl Pts',(-7.51676407774753,110.974999999566,
10.3459381770588));
#300243=CARTESIAN_POINT('Ctrl Pts',(-3.7583820388738,111.124999999566,11.5671105274568));
#300244=CARTESIAN_POINT('Ctrl Pts',(-7.42120703663524E-14,111.274999999565,
12.7882828778549));
#300245=CARTESIAN_POINT('Ctrl Pts',(3.75838203887365,111.424999999564,11.5671105274568));
#300246=CARTESIAN_POINT('Ctrl Pts',(7.51676407774738,111.574999999564,10.3459381770588));
#300247=CARTESIAN_POINT('Ctrl Pts',(9.83957192047847,111.724999999563,7.14886745759505));
#300248=CARTESIAN_POINT('Ctrl Pts',(12.1623797632096,111.874999999563,3.95179673813132));
#300249=CARTESIAN_POINT('Ctrl Pts',(12.1623797632096,112.024999999562,-1.48946194470292E-15));
#300250=CARTESIAN_POINT('Ctrl Pts',(12.1623797632096,112.174999999561,-3.95179673813132));
#300251=CARTESIAN_POINT('Ctrl Pts',(9.83957192047847,112.324999999561,-7.14886745759505));
#300252=CARTESIAN_POINT('Ctrl Pts',(7.51676407774738,112.47499999956,-10.3459381770588));
#300253=CARTESIAN_POINT('Ctrl Pts',(3.75838203887365,112.62499999956,-11.5671105274568));
#300254=CARTESIAN_POINT('Ctrl Pts',(-7.82081509407745E-14,112.774999999559,
-12.7882828778549));
#300255=CARTESIAN_POINT('Ctrl Pts',(-3.75838203887381,112.924999999558,
-11.5671105274568));
#300256=CARTESIAN_POINT('Ctrl Pts',(-7.51676407774753,113.074999999558,
-10.3459381770588));
#300257=CARTESIAN_POINT('Ctrl Pts',(-9.83957192047863,113.224999999557,
-7.14886745759505));
#300258=CARTESIAN_POINT('Ctrl Pts',(-12.1623797632097,113.374999999557,
-3.95179673813132));
#300259=CARTESIAN_POINT('Ctrl Pts',(-12.1623797632097,113.524999999556,
2.97892388940585E-15));
#300260=CARTESIAN_POINT('Ctrl Pts',(-12.1623797632097,113.674999999555,
3.95179673813133));
#300261=CARTESIAN_POINT('Ctrl Pts',(-9.83957192047863,113.824999999555,
7.14886745759505));
#300262=CARTESIAN_POINT('Ctrl Pts',(-7.51676407774753,113.974999999554,
10.3459381770588));
#300263=CARTESIAN_POINT('Ctrl Pts',(-3.7583820388738,114.124999999554,11.5671105274568));
#300264=CARTESIAN_POINT('Ctrl Pts',(-7.59397796380142E-14,114.274999999553,
12.7882828778549));
#300265=CARTESIAN_POINT('Ctrl Pts',(3.75838203887365,114.424999999552,11.5671105274568));
#300266=CARTESIAN_POINT('Ctrl Pts',(7.51676407774738,114.574999999552,10.3459381770588));
#300267=CARTESIAN_POINT('Ctrl Pts',(9.83957192047847,114.724999999551,7.14886745759505));
#300268=CARTESIAN_POINT('Ctrl Pts',(12.1623797632096,114.874999999551,3.95179673813132));
#300269=CARTESIAN_POINT('Ctrl Pts',(12.1623797632096,115.02499999955,-1.48946194470292E-15));
#300270=CARTESIAN_POINT('Ctrl Pts',(12.1623797632096,115.174999999549,-3.95179673813132));
#300271=CARTESIAN_POINT('Ctrl Pts',(9.83957192047847,115.324999999549,-7.14886745759505));
#300272=CARTESIAN_POINT('Ctrl Pts',(7.51676407774738,115.474999999548,-10.3459381770588));
#300273=CARTESIAN_POINT('Ctrl Pts',(3.75838203887365,115.624999999548,-11.5671105274568));
#300274=CARTESIAN_POINT('Ctrl Pts',(-7.99358602124363E-14,115.774999999547,
-12.7882828778549));
#300275=CARTESIAN_POINT('Ctrl Pts',(-3.75838203887381,115.924999999546,
-11.5671105274568));
#300276=CARTESIAN_POINT('Ctrl Pts',(-7.51676407774754,116.074999999546,
-10.3459381770588));
#300277=CARTESIAN_POINT('Ctrl Pts',(-9.83957192047863,116.224999999545,
-7.14886745759505));
#300278=CARTESIAN_POINT('Ctrl Pts',(-12.1623797632097,116.374999999545,
-3.95179673813132));
#300279=CARTESIAN_POINT('Ctrl Pts',(-12.1623797632097,116.524999999544,
2.97892388940585E-15));
#300280=CARTESIAN_POINT('Ctrl Pts',(-12.1623797632097,116.674999999543,
3.95179673813133));
#300281=CARTESIAN_POINT('Ctrl Pts',(-9.83957192047863,116.824999999543,
7.14886745759505));
#300282=CARTESIAN_POINT('Ctrl Pts',(-7.51676407774753,116.974999999542,
10.3459381770588));
#300283=CARTESIAN_POINT('Ctrl Pts',(-3.75838203887381,117.124999999542,
11.5671105274568));
#300284=CARTESIAN_POINT('Ctrl Pts',(-7.76674889096761E-14,117.274999999541,
12.7882828778549));
#300285=CARTESIAN_POINT('Ctrl Pts',(3.75838203887365,117.42499999954,11.5671105274568));
#300286=CARTESIAN_POINT('Ctrl Pts',(7.51676407774738,117.57499999954,10.3459381770588));
#300287=CARTESIAN_POINT('Ctrl Pts',(9.83957192047847,117.724999999539,7.14886745759505));
#300288=CARTESIAN_POINT('Ctrl Pts',(12.1623797632096,117.874999999539,3.95179673813132));
#300289=CARTESIAN_POINT('Ctrl Pts',(12.1623797632096,118.024999999538,-1.48946194470292E-15));
#300290=CARTESIAN_POINT('Ctrl Pts',(12.1623797632096,118.174999999537,-3.95179673813132));
#300291=CARTESIAN_POINT('Ctrl Pts',(9.83957192047847,118.324999999537,-7.14886745759505));
#300292=CARTESIAN_POINT('Ctrl Pts',(7.51676407774737,118.474999999536,-10.3459381770588));
#300293=CARTESIAN_POINT('Ctrl Pts',(3.75838203887365,118.624999999536,-11.5671105274568));
#300294=CARTESIAN_POINT('Ctrl Pts',(-8.16635694840981E-14,118.774999999535,
-12.7882828778549));
#300295=CARTESIAN_POINT('Ctrl Pts',(-3.75838203887381,118.924999999534,
-11.5671105274568));
#300296=CARTESIAN_POINT('Ctrl Pts',(-7.51676407774754,119.074999999534,
-10.3459381770588));
#300297=CARTESIAN_POINT('Ctrl Pts',(-9.83957192047863,119.224999999533,
-7.14886745759505));
#300298=CARTESIAN_POINT('Ctrl Pts',(-12.1623797632097,119.374999999533,
-3.95179673813132));
#300299=CARTESIAN_POINT('Ctrl Pts',(-12.1623797632097,119.524999999532,
2.97892388940585E-15));
#300300=CARTESIAN_POINT('Ctrl Pts',(-12.1623797632097,119.674999999531,
3.95179673813133));
#300301=CARTESIAN_POINT('Ctrl Pts',(-9.83957192047863,119.824999999531,
7.14886745759505));
#300302=CARTESIAN_POINT('Ctrl Pts',(-7.51676407774754,119.97499999953,10.3459381770588));
#300303=CARTESIAN_POINT('Ctrl Pts',(-3.75838203887381,120.12499999953,11.5671105274568));
#300304=CARTESIAN_POINT('Ctrl Pts',(-7.93951981813379E-14,120.274999999529,
12.7882828778549));
#300305=CARTESIAN_POINT('Ctrl Pts',(3.75838203887365,120.424999999528,11.5671105274568));
#300306=CARTESIAN_POINT('Ctrl Pts',(7.51676407774738,120.574999999528,10.3459381770588));
#300307=CARTESIAN_POINT('Ctrl Pts',(9.83957192047847,120.724999999527,7.14886745759505));
#300308=CARTESIAN_POINT('Ctrl Pts',(12.1623797632096,120.874999999527,3.95179673813132));
#300309=CARTESIAN_POINT('Ctrl Pts',(12.1623797632096,121.024999999526,-1.48946194470292E-15));
#300310=CARTESIAN_POINT('Ctrl Pts',(12.1623797632096,121.174999999525,-3.95179673813132));
#300311=CARTESIAN_POINT('Ctrl Pts',(9.83957192047847,121.324999999525,-7.14886745759505));
#300312=CARTESIAN_POINT('Ctrl Pts',(7.51676407774737,121.474999999524,-10.3459381770588));
#300313=CARTESIAN_POINT('Ctrl Pts',(3.75838203887364,121.624999999524,-11.5671105274568));
#300314=CARTESIAN_POINT('Ctrl Pts',(-8.339127875576E-14,121.774999999523,
-12.7882828778549));
#300315=CARTESIAN_POINT('Ctrl Pts',(-3.75838203887381,121.924999999522,
-11.5671105274568));
#300316=CARTESIAN_POINT('Ctrl Pts',(-7.51676407774754,122.074999999522,
-10.3459381770588));
#300317=CARTESIAN_POINT('Ctrl Pts',(-9.83957192047863,122.224999999521,
-7.14886745759505));
#300318=CARTESIAN_POINT('Ctrl Pts',(-12.1623797632097,122.374999999521,
-3.95179673813132));
#300319=CARTESIAN_POINT('Ctrl Pts',(-12.1623797632097,122.52499999952,2.97892388940585E-15));
#300320=CARTESIAN_POINT('Ctrl Pts',(-12.1623797632097,122.674999999519,
3.95179673813133));
#300321=CARTESIAN_POINT('Ctrl Pts',(-9.83957192047863,122.824999999519,
7.14886745759505));
#300322=CARTESIAN_POINT('Ctrl Pts',(-7.51676407774754,122.974999999518,
10.3459381770588));
#300323=CARTESIAN_POINT('Ctrl Pts',(-3.75838203887381,123.124999999518,
11.5671105274568));
#300324=CARTESIAN_POINT('Ctrl Pts',(-8.11229074529997E-14,123.274999999517,
12.7882828778549));
#300325=CARTESIAN_POINT('Ctrl Pts',(3.75838203887365,123.424999999516,11.5671105274568));
#300326=CARTESIAN_POINT('Ctrl Pts',(7.51676407774737,123.574999999516,10.3459381770588));
#300327=CARTESIAN_POINT('Ctrl Pts',(9.83957192047846,123.724999999515,7.14886745759505));
#300328=CARTESIAN_POINT('Ctrl Pts',(12.1623797632096,123.874999999515,3.95179673813132));
#300329=CARTESIAN_POINT('Ctrl Pts',(12.1623797632096,124.024999999514,-1.48946194470292E-15));
#300330=CARTESIAN_POINT('Ctrl Pts',(12.1623797632096,124.174999999513,-3.95179673813132));
#300331=CARTESIAN_POINT('Ctrl Pts',(9.83957192047846,124.324999999513,-7.14886745759505));
#300332=CARTESIAN_POINT('Ctrl Pts',(7.51676407774737,124.474999999512,-10.3459381770588));
#300333=CARTESIAN_POINT('Ctrl Pts',(3.75838203887364,124.624999999512,-11.5671105274568));
#300334=CARTESIAN_POINT('Ctrl Pts',(-8.51189880274219E-14,124.774999999511,
-12.7882828778549));
#300335=CARTESIAN_POINT('Ctrl Pts',(-3.75838203887381,124.92499999951,-11.5671105274568));
#300336=CARTESIAN_POINT('Ctrl Pts',(-7.51676407774754,125.07499999951,-10.3459381770588));
#300337=CARTESIAN_POINT('Ctrl Pts',(-9.83957192047863,125.224999999509,
-7.14886745759505));
#300338=CARTESIAN_POINT('Ctrl Pts',(-12.1623797632097,125.374999999509,
-3.95179673813132));
#300339=CARTESIAN_POINT('Ctrl Pts',(-12.1623797632097,125.524999999508,
2.97892388940585E-15));
#300340=CARTESIAN_POINT('Ctrl Pts',(-12.1623797632097,125.674999999507,
3.95179673813133));
#300341=CARTESIAN_POINT('Ctrl Pts',(-9.83957192047863,125.824999999507,
7.14886745759505));
#300342=CARTESIAN_POINT('Ctrl Pts',(-7.51676407774754,125.974999999506,
10.3459381770588));
#300343=CARTESIAN_POINT('Ctrl Pts',(-3.75838203887381,126.124999999506,
11.5671105274568));
#300344=CARTESIAN_POINT('Ctrl Pts',(-8.28506167246616E-14,126.274999999505,
12.7882828778549));
#300345=CARTESIAN_POINT('Ctrl Pts',(3.75838203887364,126.424999999504,11.5671105274568));
#300346=CARTESIAN_POINT('Ctrl Pts',(7.51676407774737,126.574999999504,10.3459381770588));
#300347=CARTESIAN_POINT('Ctrl Pts',(9.83957192047846,126.724999999503,7.14886745759505));
#300348=CARTESIAN_POINT('Ctrl Pts',(12.1623797632096,126.874999999503,3.95179673813132));
#300349=CARTESIAN_POINT('Ctrl Pts',(12.1623797632096,127.024999999502,-1.48946194470292E-15));
#300350=CARTESIAN_POINT('Ctrl Pts',(12.1623797632096,127.174999999501,-3.95179673813132));
#300351=CARTESIAN_POINT('Ctrl Pts',(9.83957192047846,127.324999999501,-7.14886745759505));
#300352=CARTESIAN_POINT('Ctrl Pts',(7.51676407774737,127.4749999995,-10.3459381770588));
#300353=CARTESIAN_POINT('Ctrl Pts',(3.75838203887364,127.6249999995,-11.5671105274568));
#300354=CARTESIAN_POINT('Ctrl Pts',(-8.68466972990837E-14,127.774999999499,
-12.7882828778549));
#300355=CARTESIAN_POINT('Ctrl Pts',(-3.75838203887381,127.924999999498,
-11.5671105274568));
#300356=CARTESIAN_POINT('Ctrl Pts',(-7.51676407774754,128.074999999498,
-10.3459381770588));
#300357=CARTESIAN_POINT('Ctrl Pts',(-9.83957192047864,128.224999999497,
-7.14886745759505));
#300358=CARTESIAN_POINT('Ctrl Pts',(-12.1623797632097,128.374999999497,
-3.95179673813132));
#300359=CARTESIAN_POINT('Ctrl Pts',(-12.1623797632097,128.524999999496,
2.97892388940585E-15));
#300360=CARTESIAN_POINT('Ctrl Pts',(-12.1623797632097,128.674999999495,
3.95179673813133));
#300361=CARTESIAN_POINT('Ctrl Pts',(-9.83957192047864,128.824999999495,
7.14886745759505));
#300362=CARTESIAN_POINT('Ctrl Pts',(-7.51676407774754,128.974999999494,
10.3459381770588));
#300363=CARTESIAN_POINT('Ctrl Pts',(-3.75838203887381,129.124999999494,
11.5671105274568));
#300364=CARTESIAN_POINT('Ctrl Pts',(-8.45783259963234E-14,129.274999999493,
12.7882828778549));
#300365=CARTESIAN_POINT('Ctrl Pts',(3.75838203887364,129.424999999492,11.5671105274568));
#300366=CARTESIAN_POINT('Ctrl Pts',(7.51676407774737,129.574999999492,10.3459381770588));
#300367=CARTESIAN_POINT('Ctrl Pts',(9.83957192047846,129.724999999491,7.14886745759505));
#300368=CARTESIAN_POINT('Ctrl Pts',(12.1623797632096,129.874999999491,3.95179673813132));
#300369=CARTESIAN_POINT('Ctrl Pts',(12.1623797632096,130.02499999949,-1.48946194470292E-15));
#300370=CARTESIAN_POINT('Ctrl Pts',(12.1623797632096,130.174999999489,-3.95179673813132));
#300371=CARTESIAN_POINT('Ctrl Pts',(9.83957192047846,130.324999999489,-7.14886745759505));
#300372=CARTESIAN_POINT('Ctrl Pts',(7.51676407774737,130.474999999488,-10.3459381770588));
#300373=CARTESIAN_POINT('Ctrl Pts',(3.75838203887364,130.624999999488,-11.5671105274568));
#300374=CARTESIAN_POINT('Ctrl Pts',(-8.85744065707455E-14,130.774999999487,
-12.7882828778549));
#300375=CARTESIAN_POINT('Ctrl Pts',(-3.75838203887382,130.924999999486,
-11.5671105274568));
#300376=CARTESIAN_POINT('Ctrl Pts',(-7.51676407774754,131.074999999486,
-10.3459381770588));
#300377=CARTESIAN_POINT('Ctrl Pts',(-9.83957192047864,131.224999999485,
-7.14886745759505));
#300378=CARTESIAN_POINT('Ctrl Pts',(-12.1623797632097,131.374999999485,
-3.95179673813132));
#300379=CARTESIAN_POINT('Ctrl Pts',(-12.1623797632097,131.524999999484,
2.97892388940585E-15));
#300380=CARTESIAN_POINT('Ctrl Pts',(-12.1623797632097,131.674999999483,
3.95179673813133));
#300381=CARTESIAN_POINT('Ctrl Pts',(-9.83957192047864,131.824999999483,
7.14886745759505));
#300382=CARTESIAN_POINT('Ctrl Pts',(-7.51676407774754,131.974999999482,
10.3459381770588));
#300383=CARTESIAN_POINT('Ctrl Pts',(-3.75838203887381,132.124999999482,
11.5671105274568));
#300384=CARTESIAN_POINT('Ctrl Pts',(-8.63060352679853E-14,132.274999999481,
12.7882828778549));
#300385=CARTESIAN_POINT('Ctrl Pts',(3.75838203887364,132.42499999948,11.5671105274568));
#300386=CARTESIAN_POINT('Ctrl Pts',(7.51676407774737,132.57499999948,10.3459381770588));
#300387=CARTESIAN_POINT('Ctrl Pts',(9.83957192047846,132.724999999479,7.14886745759505));
#300388=CARTESIAN_POINT('Ctrl Pts',(12.1623797632096,132.874999999479,3.95179673813132));
#300389=CARTESIAN_POINT('Ctrl Pts',(12.1623797632096,133.024999999478,-1.48946194470292E-15));
#300390=CARTESIAN_POINT('Ctrl Pts',(12.1623797632096,133.174999999477,-3.95179673813132));
#300391=CARTESIAN_POINT('Ctrl Pts',(9.83957192047846,133.324999999477,-7.14886745759505));
#300392=CARTESIAN_POINT('Ctrl Pts',(7.51676407774736,133.474999999476,-10.3459381770588));
#300393=CARTESIAN_POINT('Ctrl Pts',(3.75838203887364,133.624999999476,-11.5671105274568));
#300394=CARTESIAN_POINT('Ctrl Pts',(-9.03021158424074E-14,133.774999999475,
-12.7882828778549));
#300395=CARTESIAN_POINT('Ctrl Pts',(-3.75838203887382,133.924999999474,
-11.5671105274568));
#300396=CARTESIAN_POINT('Ctrl Pts',(-7.51676407774755,134.074999999474,
-10.3459381770588));
#300397=CARTESIAN_POINT('Ctrl Pts',(-9.83957192047864,134.224999999473,
-7.14886745759505));
#300398=CARTESIAN_POINT('Ctrl Pts',(-12.1623797632097,134.374999999473,
-3.95179673813132));
#300399=CARTESIAN_POINT('Ctrl Pts',(-12.1623797632097,134.524999999472,
2.97892388940585E-15));
#300400=CARTESIAN_POINT('Ctrl Pts',(-12.1623797632097,134.674999999471,
3.95179673813133));
#300401=CARTESIAN_POINT('Ctrl Pts',(-9.83957192047864,134.824999999471,
7.14886745759505));
#300402=CARTESIAN_POINT('Ctrl Pts',(-7.51676407774754,134.97499999947,10.3459381770588));
#300403=CARTESIAN_POINT('Ctrl Pts',(-3.75838203887382,135.12499999947,11.5671105274568));
#300404=CARTESIAN_POINT('Ctrl Pts',(-8.80337445396471E-14,135.274999999469,
12.7882828778549));
#300405=CARTESIAN_POINT('Ctrl Pts',(3.75838203887364,135.424999999468,11.5671105274568));
#300406=CARTESIAN_POINT('Ctrl Pts',(7.51676407774737,135.574999999468,10.3459381770588));
#300407=CARTESIAN_POINT('Ctrl Pts',(9.83957192047846,135.724999999467,7.14886745759505));
#300408=CARTESIAN_POINT('Ctrl Pts',(12.1623797632096,135.874999999467,3.95179673813132));
#300409=CARTESIAN_POINT('Ctrl Pts',(12.1623797632096,136.024999999466,-1.48946194470292E-15));
#300410=CARTESIAN_POINT('Ctrl Pts',(12.1623797632095,136.174999999465,-3.95179673813132));
#300411=CARTESIAN_POINT('Ctrl Pts',(9.83957192047846,136.324999999465,-7.14886745759505));
#300412=CARTESIAN_POINT('Ctrl Pts',(7.51676407774736,136.474999999464,-10.3459381770588));
#300413=CARTESIAN_POINT('Ctrl Pts',(3.75838203887364,136.624999999464,-11.5671105274568));
#300414=CARTESIAN_POINT('Ctrl Pts',(-9.20298251140692E-14,136.774999999463,
-12.7882828778549));
#300415=CARTESIAN_POINT('Ctrl Pts',(-3.75838203887382,136.924999999462,
-11.5671105274568));
#300416=CARTESIAN_POINT('Ctrl Pts',(-7.51676407774755,137.074999999462,
-10.3459381770588));
#300417=CARTESIAN_POINT('Ctrl Pts',(-9.83957192047864,137.224999999461,
-7.14886745759505));
#300418=CARTESIAN_POINT('Ctrl Pts',(-12.1623797632097,137.374999999461,
-3.95179673813132));
#300419=CARTESIAN_POINT('Ctrl Pts',(-12.1623797632097,137.52499999946,2.97892388940585E-15));
#300420=CARTESIAN_POINT('Ctrl Pts',(-12.1623797632097,137.674999999459,
3.95179673813133));
#300421=CARTESIAN_POINT('Ctrl Pts',(-9.83957192047864,137.824999999459,
7.14886745759505));
#300422=CARTESIAN_POINT('Ctrl Pts',(-7.51676407774755,137.974999999458,
10.3459381770588));
#300423=CARTESIAN_POINT('Ctrl Pts',(-3.75838203887382,138.124999999458,
11.5671105274568));
#300424=CARTESIAN_POINT('Ctrl Pts',(-8.97614538113089E-14,138.274999999457,
12.7882828778549));
#300425=CARTESIAN_POINT('Ctrl Pts',(3.75838203887364,138.424999999456,11.5671105274568));
#300426=CARTESIAN_POINT('Ctrl Pts',(7.51676407774736,138.574999999456,10.3459381770588));
#300427=CARTESIAN_POINT('Ctrl Pts',(9.83957192047846,138.724999999455,7.14886745759505));
#300428=CARTESIAN_POINT('Ctrl Pts',(12.1623797632096,138.874999999455,3.95179673813132));
#300429=CARTESIAN_POINT('Ctrl Pts',(12.1623797632096,139.024999999454,-1.48946194470292E-15));
#300430=CARTESIAN_POINT('Ctrl Pts',(12.1623797632095,139.174999999453,-3.95179673813132));
#300431=CARTESIAN_POINT('Ctrl Pts',(9.83957192047846,139.324999999453,-7.14886745759505));
#300432=CARTESIAN_POINT('Ctrl Pts',(7.51676407774736,139.474999999452,-10.3459381770588));
#300433=CARTESIAN_POINT('Ctrl Pts',(3.75838203887363,139.624999999452,-11.5671105274568));
#300434=CARTESIAN_POINT('Ctrl Pts',(-9.3757534385731E-14,139.774999999451,
-12.7882828778549));
#300435=CARTESIAN_POINT('Ctrl Pts',(-3.75838203887382,139.92499999945,-11.5671105274568));
#300436=CARTESIAN_POINT('Ctrl Pts',(-7.51676407774755,140.07499999945,-10.3459381770588));
#300437=CARTESIAN_POINT('Ctrl Pts',(-9.83957192047864,140.224999999449,
-7.14886745759505));
#300438=CARTESIAN_POINT('Ctrl Pts',(-12.1623797632097,140.374999999449,
-3.95179673813132));
#300439=CARTESIAN_POINT('Ctrl Pts',(-12.1623797632097,140.524999999448,
2.97892388940585E-15));
#300440=CARTESIAN_POINT('Ctrl Pts',(-12.1623797632097,140.674999999447,
3.95179673813133));
#300441=CARTESIAN_POINT('Ctrl Pts',(-9.83957192047864,140.824999999447,
7.14886745759505));
#300442=CARTESIAN_POINT('Ctrl Pts',(-7.51676407774755,140.974999999446,
10.3459381770588));
#300443=CARTESIAN_POINT('Ctrl Pts',(-3.75838203887382,141.124999999446,
11.5671105274568));
#300444=CARTESIAN_POINT('Ctrl Pts',(-9.14891630829708E-14,141.274999999445,
12.7882828778549));
#300445=CARTESIAN_POINT('Ctrl Pts',(3.75838203887364,141.424999999444,11.5671105274568));
#300446=CARTESIAN_POINT('Ctrl Pts',(7.51676407774736,141.574999999444,10.3459381770588));
#300447=CARTESIAN_POINT('Ctrl Pts',(9.83957192047845,141.724999999443,7.14886745759505));
#300448=CARTESIAN_POINT('Ctrl Pts',(12.1623797632095,141.874999999443,3.95179673813132));
#300449=CARTESIAN_POINT('Ctrl Pts',(12.1623797632095,142.024999999442,-1.48946194470292E-15));
#300450=CARTESIAN_POINT('Ctrl Pts',(12.1623797632095,142.174999999441,-3.95179673813132));
#300451=CARTESIAN_POINT('Ctrl Pts',(9.83957192047845,142.324999999441,-7.14886745759505));
#300452=CARTESIAN_POINT('Ctrl Pts',(7.51676407774736,142.47499999944,-10.3459381770588));
#300453=CARTESIAN_POINT('Ctrl Pts',(3.75838203887363,142.62499999944,-11.5671105274568));
#300454=CARTESIAN_POINT('Ctrl Pts',(-9.54852436573929E-14,142.774999999439,
-12.7882828778549));
#300455=CARTESIAN_POINT('Ctrl Pts',(-3.75838203887382,142.924999999438,
-11.5671105274568));
#300456=CARTESIAN_POINT('Ctrl Pts',(-7.51676407774755,143.074999999438,
-10.3459381770588));
#300457=CARTESIAN_POINT('Ctrl Pts',(-9.83957192047864,143.224999999437,
-7.14886745759505));
#300458=CARTESIAN_POINT('Ctrl Pts',(-12.1623797632097,143.374999999437,
-3.95179673813132));
#300459=CARTESIAN_POINT('Ctrl Pts',(-12.1623797632097,143.524999999436,
2.97892388940585E-15));
#300460=CARTESIAN_POINT('Ctrl Pts',(-12.1623797632097,143.674999999435,
3.95179673813133));
#300461=CARTESIAN_POINT('Ctrl Pts',(-9.83957192047864,143.824999999435,
7.14886745759505));
#300462=CARTESIAN_POINT('Ctrl Pts',(-7.51676407774755,143.974999999434,
10.3459381770588));
#300463=CARTESIAN_POINT('Ctrl Pts',(-3.75838203887382,144.124999999434,
11.5671105274568));
#300464=CARTESIAN_POINT('Ctrl Pts',(-9.32168723546326E-14,144.274999999433,
12.7882828778549));
#300465=CARTESIAN_POINT('Ctrl Pts',(3.75838203887363,144.424999999432,11.5671105274568));
#300466=CARTESIAN_POINT('Ctrl Pts',(7.51676407774736,144.574999999432,10.3459381770588));
#300467=CARTESIAN_POINT('Ctrl Pts',(9.83957192047845,144.724999999431,7.14886745759505));
#300468=CARTESIAN_POINT('Ctrl Pts',(12.1623797632095,144.874999999431,3.95179673813132));
#300469=CARTESIAN_POINT('Ctrl Pts',(12.1623797632095,145.02499999943,-1.48946194470292E-15));
#300470=CARTESIAN_POINT('Ctrl Pts',(12.1623797632095,145.174999999429,-3.95179673813132));
#300471=CARTESIAN_POINT('Ctrl Pts',(9.83957192047845,145.324999999429,-7.14886745759505));
#300472=CARTESIAN_POINT('Ctrl Pts',(7.51676407774736,145.474999999428,-10.3459381770588));
#300473=CARTESIAN_POINT('Ctrl Pts',(3.75838203887363,145.624999999428,-11.5671105274568));
#300474=CARTESIAN_POINT('Ctrl Pts',(-9.72129529290547E-14,145.774999999427,
-12.7882828778549));
#300475=CARTESIAN_POINT('Ctrl Pts',(-3.75838203887382,145.924999999426,
-11.5671105274568));
#300476=CARTESIAN_POINT('Ctrl Pts',(-7.51676407774755,146.074999999426,
-10.3459381770588));
#300477=CARTESIAN_POINT('Ctrl Pts',(-9.83957192047865,146.224999999425,
-7.14886745759505));
#300478=CARTESIAN_POINT('Ctrl Pts',(-12.1623797632097,146.374999999425,
-3.95179673813132));
#300479=CARTESIAN_POINT('Ctrl Pts',(-12.1623797632097,146.524999999424,
2.97892388940585E-15));
#300480=CARTESIAN_POINT('Ctrl Pts',(-12.1623797632097,146.674999999423,
3.95179673813133));
#300481=CARTESIAN_POINT('Ctrl Pts',(-9.83957192047865,146.824999999423,
7.14886745759505));
#300482=CARTESIAN_POINT('Ctrl Pts',(-7.51676407774755,146.974999999422,
10.3459381770588));
#300483=CARTESIAN_POINT('Ctrl Pts',(-3.75838203887382,147.124999999422,
11.5671105274568));
#300484=CARTESIAN_POINT('Ctrl Pts',(-9.49445816262944E-14,147.274999999421,
12.7882828778549));
#300485=CARTESIAN_POINT('Ctrl Pts',(3.75838203887363,147.42499999942,11.5671105274568));
#300486=CARTESIAN_POINT('Ctrl Pts',(7.51676407774736,147.57499999942,10.3459381770588));
#300487=CARTESIAN_POINT('Ctrl Pts',(9.83957192047845,147.724999999419,7.14886745759505));
#300488=CARTESIAN_POINT('Ctrl Pts',(12.1623797632095,147.874999999419,3.95179673813132));
#300489=CARTESIAN_POINT('Ctrl Pts',(12.1623797632095,148.024999999418,-1.48946194470292E-15));
#300490=CARTESIAN_POINT('Ctrl Pts',(12.1623797632095,148.174999999417,-3.95179673813132));
#300491=CARTESIAN_POINT('Ctrl Pts',(9.83957192047845,148.324999999417,-7.14886745759505));
#300492=CARTESIAN_POINT('Ctrl Pts',(7.51676407774736,148.474999999416,-10.3459381770588));
#300493=CARTESIAN_POINT('Ctrl Pts',(3.75838203887363,148.624999999416,-11.5671105274568));
#300494=CARTESIAN_POINT('Ctrl Pts',(-9.89406622007166E-14,148.774999999415,
-12.7882828778549));
#300495=CARTESIAN_POINT('Ctrl Pts',(-3.75838203887383,148.924999999414,
-11.5671105274568));
#300496=CARTESIAN_POINT('Ctrl Pts',(-7.51676407774756,149.074999999414,
-10.3459381770588));
#300497=CARTESIAN_POINT('Ctrl Pts',(-9.83957192047865,149.224999999413,
-7.14886745759505));
#300498=CARTESIAN_POINT('Ctrl Pts',(-12.1623797632097,149.374999999413,
-3.95179673813132));
#300499=CARTESIAN_POINT('Ctrl Pts',(-12.1623797632097,149.524999999412,
2.97892388940585E-15));
#300500=CARTESIAN_POINT('Ctrl Pts',(-12.1623797632097,149.674999999411,
3.95179673813133));
#300501=CARTESIAN_POINT('Ctrl Pts',(-9.83957192047865,149.824999999411,
7.14886745759505));
#300502=CARTESIAN_POINT('Ctrl Pts',(-7.51676407774755,149.97499999941,10.3459381770588));
#300503=CARTESIAN_POINT('Ctrl Pts',(-3.75838203887382,150.12499999941,11.5671105274568));
#300504=CARTESIAN_POINT('Ctrl Pts',(-9.66722908979563E-14,150.274999999409,
12.7882828778549));
#300505=CARTESIAN_POINT('Ctrl Pts',(3.75838203887363,150.424999999408,11.5671105274568));
#300506=CARTESIAN_POINT('Ctrl Pts',(7.51676407774736,150.574999999408,10.3459381770588));
#300507=CARTESIAN_POINT('Ctrl Pts',(9.83957192047845,150.724999999407,7.14886745759505));
#300508=CARTESIAN_POINT('Ctrl Pts',(12.1623797632095,150.874999999407,3.95179673813132));
#300509=CARTESIAN_POINT('Ctrl Pts',(12.1623797632095,151.024999999406,-1.48946194470292E-15));
#300510=CARTESIAN_POINT('Ctrl Pts',(12.1623797632095,151.174999999405,-3.95179673813132));
#300511=CARTESIAN_POINT('Ctrl Pts',(9.83957192047845,151.324999999405,-7.14886745759505));
#300512=CARTESIAN_POINT('Ctrl Pts',(7.51676407774736,151.474999999404,-10.3459381770588));
#300513=CARTESIAN_POINT('Ctrl Pts',(3.75838203887363,151.624999999404,-11.5671105274568));
#300514=CARTESIAN_POINT('Ctrl Pts',(-1.00668371472378E-13,151.774999999403,
-12.7882828778549));
#300515=CARTESIAN_POINT('Ctrl Pts',(-3.75838203887383,151.924999999402,
-11.5671105274568));
#300516=CARTESIAN_POINT('Ctrl Pts',(-7.51676407774756,152.074999999402,
-10.3459381770588));
#300517=CARTESIAN_POINT('Ctrl Pts',(-9.83957192047865,152.224999999401,
-7.14886745759505));
#300518=CARTESIAN_POINT('Ctrl Pts',(-12.1623797632097,152.374999999401,
-3.95179673813132));
#300519=CARTESIAN_POINT('Ctrl Pts',(-12.1623797632097,152.5249999994,2.97892388940585E-15));
#300520=CARTESIAN_POINT('Ctrl Pts',(-12.1623797632097,152.674999999399,
3.95179673813133));
#300521=CARTESIAN_POINT('Ctrl Pts',(-9.83957192047865,152.824999999399,
7.14886745759505));
#300522=CARTESIAN_POINT('Ctrl Pts',(-7.51676407774756,152.974999999398,
10.3459381770588));
#300523=CARTESIAN_POINT('Ctrl Pts',(-3.75838203887383,153.124999999398,
11.5671105274568));
#300524=CARTESIAN_POINT('Ctrl Pts',(-9.84000001696181E-14,153.274999999397,
12.7882828778549));
#300525=CARTESIAN_POINT('Ctrl Pts',(3.75838203887363,153.424999999396,11.5671105274568));
#300526=CARTESIAN_POINT('Ctrl Pts',(7.51676407774736,153.574999999396,10.3459381770588));
#300527=CARTESIAN_POINT('Ctrl Pts',(9.83957192047845,153.724999999395,7.14886745759505));
#300528=CARTESIAN_POINT('Ctrl Pts',(12.1623797632095,153.874999999395,3.95179673813132));
#300529=CARTESIAN_POINT('Ctrl Pts',(12.1623797632095,154.024999999394,-1.48946194470292E-15));
#300530=CARTESIAN_POINT('Ctrl Pts',(12.1623797632095,154.174999999393,-3.95179673813132));
#300531=CARTESIAN_POINT('Ctrl Pts',(9.83957192047845,154.324999999393,-7.14886745759505));
#300532=CARTESIAN_POINT('Ctrl Pts',(7.51676407774735,154.474999999392,-10.3459381770588));
#300533=CARTESIAN_POINT('Ctrl Pts',(3.75838203887363,154.624999999392,-11.5671105274568));
#300534=CARTESIAN_POINT('Ctrl Pts',(-1.0239608074404E-13,154.774999999391,
-12.7882828778549));
#300535=CARTESIAN_POINT('Ctrl Pts',(-3.75838203887383,154.92499999939,-11.5671105274568));
#300536=CARTESIAN_POINT('Ctrl Pts',(10.0514428414941,59.8062499997713,-1.23094673026484E-15));
#300537=CARTESIAN_POINT('Ctrl Pts',(10.0514428414941,59.9562499997706,-3.26591175476071));
#300538=CARTESIAN_POINT('Ctrl Pts',(8.13178807675714,60.10624999977,-5.90808986649102));
#300539=CARTESIAN_POINT('Ctrl Pts',(7.55384587767069,60.1514098542684,-6.70355906039096));
#300540=CARTESIAN_POINT('Ctrl Pts',(6.83270577527258,60.1985571585059,-7.37194919844001));
#300541=CARTESIAN_POINT('Ctrl Pts',(-12.1623797632103,-3.28749999997638,
2.97892388940601E-15));
#300542=CARTESIAN_POINT('Ctrl Pts',(-12.1623797632103,-3.13749999997698,
3.95179673813154));
#300543=CARTESIAN_POINT('Ctrl Pts',(-9.83957192047908,-2.98749999997758,
7.14886745759543));
#300544=CARTESIAN_POINT('Ctrl Pts',(-7.51676407774787,-2.83749999997817,
10.3459381770593));
#300545=CARTESIAN_POINT('Ctrl Pts',(-3.75838203887394,-2.68749999997877,
11.5671105274575));
#300546=CARTESIAN_POINT('Ctrl Pts',(-8.66709987268145E-15,-2.53749999997937,
12.7882828778556));
#300547=CARTESIAN_POINT('Ctrl Pts',(3.75838203887392,-2.38749999997997,
11.5671105274575));
#300548=CARTESIAN_POINT('Ctrl Pts',(7.51676407774785,-2.23749999998057,
10.3459381770593));
#300549=CARTESIAN_POINT('Ctrl Pts',(9.83957192047906,-2.08749999998117,
7.14886745759543));
#300550=CARTESIAN_POINT('Ctrl Pts',(12.1623797632103,-1.93749999998176,
3.95179673813153));
#300551=CARTESIAN_POINT('Ctrl Pts',(12.1623797632103,-1.78749999998236,
-1.489461944703E-15));
#300552=CARTESIAN_POINT('Ctrl Pts',(12.1623797632103,-1.63749999998296,
-3.95179673813154));
#300553=CARTESIAN_POINT('Ctrl Pts',(9.83957192047906,-1.48749999998357,
-7.14886745759543));
#300554=CARTESIAN_POINT('Ctrl Pts',(7.51676407774784,-1.33749999998417,
-10.3459381770593));
#300555=CARTESIAN_POINT('Ctrl Pts',(3.75838203887392,-1.18749999998477,
-11.5671105274575));
#300556=CARTESIAN_POINT('Ctrl Pts',(-1.26631804471037E-14,-1.03749999998537,
-12.7882828778556));
#300557=CARTESIAN_POINT('Ctrl Pts',(-3.75838203887394,-0.887499999985973,
-11.5671105274575));
#300558=CARTESIAN_POINT('Ctrl Pts',(-7.51676407774787,-0.737499999986575,
-10.3459381770593));
#300559=CARTESIAN_POINT('Ctrl Pts',(-9.83957192047909,-0.587499999987176,
-7.14886745759543));
#300560=CARTESIAN_POINT('Ctrl Pts',(-12.1623797632103,-0.437499999987778,
-3.95179673813153));
#300561=CARTESIAN_POINT('Ctrl Pts',(-12.1623797632103,-0.287499999988378,
2.97892388940601E-15));
#300562=CARTESIAN_POINT('Ctrl Pts',(-12.1623797632103,-0.137499999988978,
3.95179673813154));
#300563=CARTESIAN_POINT('Ctrl Pts',(-9.83957192047909,0.0125000000104236,
7.14886745759543));
#300564=CARTESIAN_POINT('Ctrl Pts',(-7.51676407774787,0.162500000009825,
10.3459381770593));
#300565=CARTESIAN_POINT('Ctrl Pts',(-3.75838203887394,0.312500000009227,
11.5671105274575));
#300566=CARTESIAN_POINT('Ctrl Pts',(-1.03948091443433E-14,0.462500000008629,
12.7882828778556));
#300567=CARTESIAN_POINT('Ctrl Pts',(3.75838203887392,0.612500000008031,
11.5671105274575));
#300568=CARTESIAN_POINT('Ctrl Pts',(7.51676407774785,0.762500000007433,
10.3459381770593));
#300569=CARTESIAN_POINT('Ctrl Pts',(9.83957192047906,0.912500000006835,
7.14886745759543));
#300570=CARTESIAN_POINT('Ctrl Pts',(12.1623797632103,1.06250000000624,3.95179673813153));
#300571=CARTESIAN_POINT('Ctrl Pts',(12.1623797632103,1.21250000000564,-1.489461944703E-15));
#300572=CARTESIAN_POINT('Ctrl Pts',(12.1623797632103,1.36250000000504,-3.95179673813154));
#300573=CARTESIAN_POINT('Ctrl Pts',(9.83957192047906,1.51250000000444,-7.14886745759543));
#300574=CARTESIAN_POINT('Ctrl Pts',(7.51676407774784,1.66250000000383,-10.3459381770593));
#300575=CARTESIAN_POINT('Ctrl Pts',(3.75838203887391,1.81250000000323,-11.5671105274575));
#300576=CARTESIAN_POINT('Ctrl Pts',(-1.43908897187656E-14,1.96250000000263,
-12.7882828778556));
#300577=CARTESIAN_POINT('Ctrl Pts',(-3.75838203887394,2.11250000000203,
-11.5671105274575));
#300578=CARTESIAN_POINT('Ctrl Pts',(-7.51676407774787,2.26250000000143,
-10.3459381770593));
#300579=CARTESIAN_POINT('Ctrl Pts',(-9.83957192047909,2.41250000000082,
-7.14886745759543));
#300580=CARTESIAN_POINT('Ctrl Pts',(-12.1623797632103,2.56250000000022,
-3.95179673813153));
#300581=CARTESIAN_POINT('Ctrl Pts',(-12.1623797632103,2.71249999999962,
2.97892388940601E-15));
#300582=CARTESIAN_POINT('Ctrl Pts',(-12.1623797632103,2.86249999999902,
3.95179673813154));
#300583=CARTESIAN_POINT('Ctrl Pts',(-9.83957192047909,3.01249999999842,
7.14886745759543));
#300584=CARTESIAN_POINT('Ctrl Pts',(-7.51676407774787,3.16249999999782,
10.3459381770593));
#300585=CARTESIAN_POINT('Ctrl Pts',(-3.75838203887394,3.31249999999723,
11.5671105274575));
#300586=CARTESIAN_POINT('Ctrl Pts',(-1.21225184160051E-14,3.46249999999663,
12.7882828778556));
#300587=CARTESIAN_POINT('Ctrl Pts',(3.75838203887392,3.61249999999603,11.5671105274575));
#300588=CARTESIAN_POINT('Ctrl Pts',(7.51676407774784,3.76249999999543,10.3459381770593));
#300589=CARTESIAN_POINT('Ctrl Pts',(9.83957192047906,3.91249999999483,7.14886745759543));
#300590=CARTESIAN_POINT('Ctrl Pts',(12.1623797632103,4.06249999999424,3.95179673813153));
#300591=CARTESIAN_POINT('Ctrl Pts',(12.1623797632103,4.21249999999364,-1.489461944703E-15));
#300592=CARTESIAN_POINT('Ctrl Pts',(12.1623797632103,4.36249999999303,-3.95179673813154));
#300593=CARTESIAN_POINT('Ctrl Pts',(9.83957192047906,4.51249999999243,-7.14886745759543));
#300594=CARTESIAN_POINT('Ctrl Pts',(7.51676407774784,4.66249999999183,-10.3459381770593));
#300595=CARTESIAN_POINT('Ctrl Pts',(3.75838203887391,4.81249999999123,-11.5671105274575));
#300596=CARTESIAN_POINT('Ctrl Pts',(-1.61185989904274E-14,4.96249999999063,
-12.7882828778556));
#300597=CARTESIAN_POINT('Ctrl Pts',(-3.75838203887394,5.11249999999003,
-11.5671105274575));
#300598=CARTESIAN_POINT('Ctrl Pts',(-7.51676407774788,5.26249999998942,
-10.3459381770593));
#300599=CARTESIAN_POINT('Ctrl Pts',(-9.83957192047909,5.41249999998882,
-7.14886745759543));
#300600=CARTESIAN_POINT('Ctrl Pts',(-12.1623797632103,5.56249999998822,
-3.95179673813153));
#300601=CARTESIAN_POINT('Ctrl Pts',(-12.1623797632103,5.71249999998762,
2.97892388940601E-15));
#300602=CARTESIAN_POINT('Ctrl Pts',(-12.1623797632103,5.86249999998702,
3.95179673813154));
#300603=CARTESIAN_POINT('Ctrl Pts',(-9.83957192047909,6.01249999998642,
7.14886745759543));
#300604=CARTESIAN_POINT('Ctrl Pts',(-7.51676407774787,6.16249999998582,
10.3459381770593));
#300605=CARTESIAN_POINT('Ctrl Pts',(-3.75838203887394,6.31249999998523,
11.5671105274575));
#300606=CARTESIAN_POINT('Ctrl Pts',(-1.3850227687667E-14,6.46249999998463,
12.7882828778556));
#300607=CARTESIAN_POINT('Ctrl Pts',(3.75838203887392,6.61249999998403,11.5671105274575));
#300608=CARTESIAN_POINT('Ctrl Pts',(7.51676407774784,6.76249999998343,10.3459381770593));
#300609=CARTESIAN_POINT('Ctrl Pts',(9.83957192047906,6.91249999998283,7.14886745759543));
#300610=CARTESIAN_POINT('Ctrl Pts',(12.1623797632103,7.06249999998224,3.95179673813153));
#300611=CARTESIAN_POINT('Ctrl Pts',(12.1623797632103,7.21249999998164,-1.489461944703E-15));
#300612=CARTESIAN_POINT('Ctrl Pts',(12.1623797632103,7.36249999998104,-3.95179673813154));
#300613=CARTESIAN_POINT('Ctrl Pts',(9.83957192047906,7.51249999998044,-7.14886745759543));
#300614=CARTESIAN_POINT('Ctrl Pts',(7.51676407774784,7.66249999997983,-10.3459381770593));
#300615=CARTESIAN_POINT('Ctrl Pts',(3.75838203887391,7.81249999997923,-11.5671105274575));
#300616=CARTESIAN_POINT('Ctrl Pts',(-1.78463082620892E-14,7.96249999997863,
-12.7882828778556));
#300617=CARTESIAN_POINT('Ctrl Pts',(-3.75838203887395,8.11249999997803,
-11.5671105274575));
#300618=CARTESIAN_POINT('Ctrl Pts',(-7.51676407774788,8.26249999997743,
-10.3459381770593));
#300619=CARTESIAN_POINT('Ctrl Pts',(-9.83957192047909,8.41249999997682,
-7.14886745759543));
#300620=CARTESIAN_POINT('Ctrl Pts',(-12.1623797632103,8.56249999997622,
-3.95179673813153));
#300621=CARTESIAN_POINT('Ctrl Pts',(-12.1623797632103,8.71249999997562,
2.97892388940601E-15));
#300622=CARTESIAN_POINT('Ctrl Pts',(-12.1623797632103,8.86249999997502,
3.95179673813154));
#300623=CARTESIAN_POINT('Ctrl Pts',(-9.83957192047909,9.01249999997442,
7.14886745759543));
#300624=CARTESIAN_POINT('Ctrl Pts',(-7.51676407774787,9.16249999997382,
10.3459381770593));
#300625=CARTESIAN_POINT('Ctrl Pts',(-3.75838203887394,9.31249999997323,
11.5671105274575));
#300626=CARTESIAN_POINT('Ctrl Pts',(-1.55779369593288E-14,9.46249999997263,
12.7882828778556));
#300627=CARTESIAN_POINT('Ctrl Pts',(3.75838203887391,9.61249999997203,11.5671105274575));
#300628=CARTESIAN_POINT('Ctrl Pts',(7.51676407774784,9.76249999997144,10.3459381770593));
#300629=CARTESIAN_POINT('Ctrl Pts',(9.83957192047906,9.91249999997084,7.14886745759543));
#300630=CARTESIAN_POINT('Ctrl Pts',(12.1623797632103,10.0624999999702,3.95179673813153));
#300631=CARTESIAN_POINT('Ctrl Pts',(12.1623797632103,10.2124999999696,-1.489461944703E-15));
#300632=CARTESIAN_POINT('Ctrl Pts',(12.1623797632103,10.362499999969,-3.95179673813154));
#300633=CARTESIAN_POINT('Ctrl Pts',(9.83957192047905,10.5124999999684,-7.14886745759543));
#300634=CARTESIAN_POINT('Ctrl Pts',(7.51676407774784,10.6624999999678,-10.3459381770593));
#300635=CARTESIAN_POINT('Ctrl Pts',(3.75838203887391,10.8124999999672,-11.5671105274575));
#300636=CARTESIAN_POINT('Ctrl Pts',(-1.95740175337511E-14,10.9624999999666,
-12.7882828778556));
#300637=CARTESIAN_POINT('Ctrl Pts',(-3.75838203887395,11.112499999966,-11.5671105274575));
#300638=CARTESIAN_POINT('Ctrl Pts',(-7.51676407774788,11.2624999999654,
-10.3459381770593));
#300639=CARTESIAN_POINT('Ctrl Pts',(-9.83957192047909,11.4124999999648,
-7.14886745759543));
#300640=CARTESIAN_POINT('Ctrl Pts',(-12.1623797632103,11.5624999999642,
-3.95179673813153));
#300641=CARTESIAN_POINT('Ctrl Pts',(-12.1623797632103,11.7124999999636,
2.97892388940601E-15));
#300642=CARTESIAN_POINT('Ctrl Pts',(-12.1623797632103,11.862499999963,3.95179673813154));
#300643=CARTESIAN_POINT('Ctrl Pts',(-9.83957192047909,12.0124999999624,
7.14886745759543));
#300644=CARTESIAN_POINT('Ctrl Pts',(-7.51676407774788,12.1624999999618,
10.3459381770593));
#300645=CARTESIAN_POINT('Ctrl Pts',(-3.75838203887395,12.3124999999612,
11.5671105274575));
#300646=CARTESIAN_POINT('Ctrl Pts',(-1.73056462309906E-14,12.4624999999606,
12.7882828778556));
#300647=CARTESIAN_POINT('Ctrl Pts',(3.75838203887391,12.61249999996,11.5671105274575));
#300648=CARTESIAN_POINT('Ctrl Pts',(7.51676407774784,12.7624999999594,10.3459381770593));
#300649=CARTESIAN_POINT('Ctrl Pts',(9.83957192047906,12.9124999999588,7.14886745759543));
#300650=CARTESIAN_POINT('Ctrl Pts',(12.1623797632103,13.0624999999582,3.95179673813153));
#300651=CARTESIAN_POINT('Ctrl Pts',(12.1623797632103,13.2124999999576,-1.489461944703E-15));
#300652=CARTESIAN_POINT('Ctrl Pts',(12.1623797632103,13.362499999957,-3.95179673813154));
#300653=CARTESIAN_POINT('Ctrl Pts',(9.83957192047905,13.5124999999564,-7.14886745759543));
#300654=CARTESIAN_POINT('Ctrl Pts',(7.51676407774784,13.6624999999558,-10.3459381770593));
#300655=CARTESIAN_POINT('Ctrl Pts',(3.75838203887391,13.8124999999552,-11.5671105274575));
#300656=CARTESIAN_POINT('Ctrl Pts',(-2.13017268054129E-14,13.9624999999546,
-12.7882828778556));
#300657=CARTESIAN_POINT('Ctrl Pts',(-3.75838203887395,14.112499999954,-11.5671105274575));
#300658=CARTESIAN_POINT('Ctrl Pts',(-7.51676407774788,14.2624999999534,
-10.3459381770593));
#300659=CARTESIAN_POINT('Ctrl Pts',(-9.8395719204791,14.4124999999528,-7.14886745759543));
#300660=CARTESIAN_POINT('Ctrl Pts',(-12.1623797632103,14.5624999999522,
-3.95179673813153));
#300661=CARTESIAN_POINT('Ctrl Pts',(-12.1623797632103,14.7124999999516,
2.97892388940601E-15));
#300662=CARTESIAN_POINT('Ctrl Pts',(-12.1623797632103,14.862499999951,3.95179673813154));
#300663=CARTESIAN_POINT('Ctrl Pts',(-9.83957192047909,15.0124999999504,
7.14886745759543));
#300664=CARTESIAN_POINT('Ctrl Pts',(-7.51676407774788,15.1624999999498,
10.3459381770593));
#300665=CARTESIAN_POINT('Ctrl Pts',(-3.75838203887395,15.3124999999492,
11.5671105274575));
#300666=CARTESIAN_POINT('Ctrl Pts',(-1.90333555026525E-14,15.4624999999486,
12.7882828778556));
#300667=CARTESIAN_POINT('Ctrl Pts',(3.75838203887391,15.612499999948,11.5671105274575));
#300668=CARTESIAN_POINT('Ctrl Pts',(7.51676407774784,15.7624999999474,10.3459381770593));
#300669=CARTESIAN_POINT('Ctrl Pts',(9.83957192047905,15.9124999999468,7.14886745759543));
#300670=CARTESIAN_POINT('Ctrl Pts',(12.1623797632103,16.0624999999462,3.95179673813153));
#300671=CARTESIAN_POINT('Ctrl Pts',(12.1623797632103,16.2124999999456,-1.489461944703E-15));
#300672=CARTESIAN_POINT('Ctrl Pts',(12.1623797632103,16.362499999945,-3.95179673813154));
#300673=CARTESIAN_POINT('Ctrl Pts',(9.83957192047905,16.5124999999444,-7.14886745759543));
#300674=CARTESIAN_POINT('Ctrl Pts',(7.51676407774784,16.6624999999438,-10.3459381770593));
#300675=CARTESIAN_POINT('Ctrl Pts',(3.75838203887391,16.8124999999432,-11.5671105274575));
#300676=CARTESIAN_POINT('Ctrl Pts',(-2.30294360770748E-14,16.9624999999426,
-12.7882828778556));
#300677=CARTESIAN_POINT('Ctrl Pts',(-3.75838203887395,17.112499999942,-11.5671105274575));
#300678=CARTESIAN_POINT('Ctrl Pts',(-7.51676407774788,17.2624999999414,
-10.3459381770593));
#300679=CARTESIAN_POINT('Ctrl Pts',(-9.8395719204791,17.4124999999408,-7.14886745759543));
#300680=CARTESIAN_POINT('Ctrl Pts',(-12.1623797632103,17.5624999999402,
-3.95179673813153));
#300681=CARTESIAN_POINT('Ctrl Pts',(-12.1623797632103,17.7124999999396,
2.97892388940601E-15));
#300682=CARTESIAN_POINT('Ctrl Pts',(-12.1623797632103,17.862499999939,3.95179673813154));
#300683=CARTESIAN_POINT('Ctrl Pts',(-9.8395719204791,18.0124999999384,7.14886745759543));
#300684=CARTESIAN_POINT('Ctrl Pts',(-7.51676407774788,18.1624999999378,
10.3459381770593));
#300685=CARTESIAN_POINT('Ctrl Pts',(-3.75838203887395,18.3124999999372,
11.5671105274575));
#300686=CARTESIAN_POINT('Ctrl Pts',(-2.07610647743143E-14,18.4624999999366,
12.7882828778556));
#300687=CARTESIAN_POINT('Ctrl Pts',(3.75838203887391,18.612499999936,11.5671105274575));
#300688=CARTESIAN_POINT('Ctrl Pts',(7.51676407774784,18.7624999999354,10.3459381770593));
#300689=CARTESIAN_POINT('Ctrl Pts',(9.83957192047905,18.9124999999348,7.14886745759543));
#300690=CARTESIAN_POINT('Ctrl Pts',(12.1623797632103,19.0624999999342,3.95179673813153));
#300691=CARTESIAN_POINT('Ctrl Pts',(12.1623797632103,19.2124999999336,-1.489461944703E-15));
#300692=CARTESIAN_POINT('Ctrl Pts',(12.1623797632103,19.362499999933,-3.95179673813154));
#300693=CARTESIAN_POINT('Ctrl Pts',(9.83957192047905,19.5124999999324,-7.14886745759543));
#300694=CARTESIAN_POINT('Ctrl Pts',(7.51676407774784,19.6624999999318,-10.3459381770593));
#300695=CARTESIAN_POINT('Ctrl Pts',(3.7583820388739,19.8124999999312,-11.5671105274575));
#300696=CARTESIAN_POINT('Ctrl Pts',(-2.47571453487366E-14,19.9624999999306,
-12.7882828778556));
#300697=CARTESIAN_POINT('Ctrl Pts',(-3.75838203887395,20.11249999993,-11.5671105274575));
#300698=CARTESIAN_POINT('Ctrl Pts',(-7.51676407774788,20.2624999999294,
-10.3459381770593));
#300699=CARTESIAN_POINT('Ctrl Pts',(-9.8395719204791,20.4124999999288,-7.14886745759543));
#300700=CARTESIAN_POINT('Ctrl Pts',(-12.1623797632103,20.5624999999282,
-3.95179673813153));
#300701=CARTESIAN_POINT('Ctrl Pts',(-12.1623797632103,20.7124999999276,
2.97892388940601E-15));
#300702=CARTESIAN_POINT('Ctrl Pts',(-12.1623797632103,20.862499999927,3.95179673813154));
#300703=CARTESIAN_POINT('Ctrl Pts',(-9.8395719204791,21.0124999999264,7.14886745759543));
#300704=CARTESIAN_POINT('Ctrl Pts',(-7.51676407774788,21.1624999999258,
10.3459381770593));
#300705=CARTESIAN_POINT('Ctrl Pts',(-3.75838203887395,21.3124999999252,
11.5671105274575));
#300706=CARTESIAN_POINT('Ctrl Pts',(-2.24887740459762E-14,21.4624999999246,
12.7882828778556));
#300707=CARTESIAN_POINT('Ctrl Pts',(3.75838203887391,21.612499999924,11.5671105274575));
#300708=CARTESIAN_POINT('Ctrl Pts',(7.51676407774784,21.7624999999234,10.3459381770593));
#300709=CARTESIAN_POINT('Ctrl Pts',(9.83957192047905,21.9124999999228,7.14886745759543));
#300710=CARTESIAN_POINT('Ctrl Pts',(12.1623797632103,22.0624999999222,3.95179673813153));
#300711=CARTESIAN_POINT('Ctrl Pts',(12.1623797632103,22.2124999999216,-1.489461944703E-15));
#300712=CARTESIAN_POINT('Ctrl Pts',(12.1623797632103,22.362499999921,-3.95179673813154));
#300713=CARTESIAN_POINT('Ctrl Pts',(9.83957192047905,22.5124999999204,-7.14886745759543));
#300714=CARTESIAN_POINT('Ctrl Pts',(7.51676407774783,22.6624999999198,-10.3459381770593));
#300715=CARTESIAN_POINT('Ctrl Pts',(3.7583820388739,22.8124999999192,-11.5671105274575));
#300716=CARTESIAN_POINT('Ctrl Pts',(-2.64848546203984E-14,22.9624999999186,
-12.7882828778556));
#300717=CARTESIAN_POINT('Ctrl Pts',(-3.75838203887396,23.112499999918,-11.5671105274575));
#300718=CARTESIAN_POINT('Ctrl Pts',(-7.51676407774788,23.2624999999174,
-10.3459381770593));
#300719=CARTESIAN_POINT('Ctrl Pts',(-9.8395719204791,23.4124999999168,-7.14886745759543));
#300720=CARTESIAN_POINT('Ctrl Pts',(-12.1623797632103,23.5624999999162,
-3.95179673813153));
#300721=CARTESIAN_POINT('Ctrl Pts',(-12.1623797632103,23.7124999999156,
2.97892388940601E-15));
#300722=CARTESIAN_POINT('Ctrl Pts',(-12.1623797632103,23.862499999915,3.95179673813154));
#300723=CARTESIAN_POINT('Ctrl Pts',(-9.8395719204791,24.0124999999144,7.14886745759543));
#300724=CARTESIAN_POINT('Ctrl Pts',(-7.51676407774788,24.1624999999138,
10.3459381770593));
#300725=CARTESIAN_POINT('Ctrl Pts',(-3.75838203887395,24.3124999999132,
11.5671105274575));
#300726=CARTESIAN_POINT('Ctrl Pts',(-2.4216483317638E-14,24.4624999999126,
12.7882828778556));
#300727=CARTESIAN_POINT('Ctrl Pts',(3.7583820388739,24.612499999912,11.5671105274575));
#300728=CARTESIAN_POINT('Ctrl Pts',(7.51676407774783,24.7624999999114,10.3459381770593));
#300729=CARTESIAN_POINT('Ctrl Pts',(9.83957192047905,24.9124999999108,7.14886745759543));
#300730=CARTESIAN_POINT('Ctrl Pts',(12.1623797632103,25.0624999999102,3.95179673813153));
#300731=CARTESIAN_POINT('Ctrl Pts',(12.1623797632103,25.2124999999096,-1.489461944703E-15));
#300732=CARTESIAN_POINT('Ctrl Pts',(12.1623797632103,25.362499999909,-3.95179673813154));
#300733=CARTESIAN_POINT('Ctrl Pts',(9.83957192047905,25.5124999999084,-7.14886745759543));
#300734=CARTESIAN_POINT('Ctrl Pts',(7.51676407774783,25.6624999999078,-10.3459381770593));
#300735=CARTESIAN_POINT('Ctrl Pts',(3.7583820388739,25.8124999999072,-11.5671105274575));
#300736=CARTESIAN_POINT('Ctrl Pts',(-2.82125638920603E-14,25.9624999999066,
-12.7882828778556));
#300737=CARTESIAN_POINT('Ctrl Pts',(-3.75838203887396,26.112499999906,-11.5671105274575));
#300738=CARTESIAN_POINT('Ctrl Pts',(-7.51676407774788,26.2624999999054,
-10.3459381770593));
#300739=CARTESIAN_POINT('Ctrl Pts',(-9.8395719204791,26.4124999999048,-7.14886745759543));
#300740=CARTESIAN_POINT('Ctrl Pts',(-12.1623797632103,26.5624999999042,
-3.95179673813153));
#300741=CARTESIAN_POINT('Ctrl Pts',(-12.1623797632103,26.7124999999036,
2.97892388940601E-15));
#300742=CARTESIAN_POINT('Ctrl Pts',(-12.1623797632103,26.862499999903,3.95179673813154));
#300743=CARTESIAN_POINT('Ctrl Pts',(-9.8395719204791,27.0124999999024,7.14886745759543));
#300744=CARTESIAN_POINT('Ctrl Pts',(-7.51676407774788,27.1624999999018,
10.3459381770593));
#300745=CARTESIAN_POINT('Ctrl Pts',(-3.75838203887396,27.3124999999012,
11.5671105274575));
#300746=CARTESIAN_POINT('Ctrl Pts',(-2.59441925892998E-14,27.4624999999006,
12.7882828778556));
#300747=CARTESIAN_POINT('Ctrl Pts',(3.7583820388739,27.6124999999,11.5671105274575));
#300748=CARTESIAN_POINT('Ctrl Pts',(7.51676407774783,27.7624999998994,10.3459381770593));
#300749=CARTESIAN_POINT('Ctrl Pts',(9.83957192047905,27.9124999998988,7.14886745759543));
#300750=CARTESIAN_POINT('Ctrl Pts',(12.1623797632103,28.0624999998982,3.95179673813153));
#300751=CARTESIAN_POINT('Ctrl Pts',(12.1623797632103,28.2124999998976,-1.489461944703E-15));
#300752=CARTESIAN_POINT('Ctrl Pts',(12.1623797632103,28.362499999897,-3.95179673813154));
#300753=CARTESIAN_POINT('Ctrl Pts',(9.83957192047905,28.5124999998964,-7.14886745759543));
#300754=CARTESIAN_POINT('Ctrl Pts',(7.51676407774783,28.6624999998958,-10.3459381770593));
#300755=CARTESIAN_POINT('Ctrl Pts',(3.7583820388739,28.8124999998952,-11.5671105274575));
#300756=CARTESIAN_POINT('Ctrl Pts',(-2.99402731637221E-14,28.9624999998946,
-12.7882828778556));
#300757=CARTESIAN_POINT('Ctrl Pts',(-3.75838203887396,29.112499999894,-11.5671105274575));
#300758=CARTESIAN_POINT('Ctrl Pts',(-7.51676407774789,29.2624999998934,
-10.3459381770593));
#300759=CARTESIAN_POINT('Ctrl Pts',(-9.8395719204791,29.4124999998928,-7.14886745759543));
#300760=CARTESIAN_POINT('Ctrl Pts',(-12.1623797632103,29.5624999998922,
-3.95179673813153));
#300761=CARTESIAN_POINT('Ctrl Pts',(-12.1623797632103,29.7124999998916,
2.97892388940601E-15));
#300762=CARTESIAN_POINT('Ctrl Pts',(-12.1623797632103,29.862499999891,3.95179673813154));
#300763=CARTESIAN_POINT('Ctrl Pts',(-9.8395719204791,30.0124999998904,7.14886745759543));
#300764=CARTESIAN_POINT('Ctrl Pts',(-7.51676407774788,30.1624999998898,
10.3459381770593));
#300765=CARTESIAN_POINT('Ctrl Pts',(-3.75838203887396,30.3124999998892,
11.5671105274575));
#300766=CARTESIAN_POINT('Ctrl Pts',(-2.76719018609617E-14,30.4624999998886,
12.7882828778556));
#300767=CARTESIAN_POINT('Ctrl Pts',(3.7583820388739,30.612499999888,11.5671105274575));
#300768=CARTESIAN_POINT('Ctrl Pts',(7.51676407774783,30.7624999998874,10.3459381770593));
#300769=CARTESIAN_POINT('Ctrl Pts',(9.83957192047905,30.9124999998868,7.14886745759543));
#300770=CARTESIAN_POINT('Ctrl Pts',(12.1623797632103,31.0624999998862,3.95179673813153));
#300771=CARTESIAN_POINT('Ctrl Pts',(12.1623797632103,31.2124999998856,-1.489461944703E-15));
#300772=CARTESIAN_POINT('Ctrl Pts',(12.1623797632103,31.362499999885,-3.95179673813154));
#300773=CARTESIAN_POINT('Ctrl Pts',(9.83957192047904,31.5124999998844,-7.14886745759543));
#300774=CARTESIAN_POINT('Ctrl Pts',(7.51676407774783,31.6624999998838,-10.3459381770593));
#300775=CARTESIAN_POINT('Ctrl Pts',(3.7583820388739,31.8124999998832,-11.5671105274575));
#300776=CARTESIAN_POINT('Ctrl Pts',(-3.16679824353839E-14,31.9624999998826,
-12.7882828778556));
#300777=CARTESIAN_POINT('Ctrl Pts',(-3.75838203887396,32.112499999882,-11.5671105274575));
#300778=CARTESIAN_POINT('Ctrl Pts',(-7.51676407774789,32.2624999998814,
-10.3459381770593));
#300779=CARTESIAN_POINT('Ctrl Pts',(-9.83957192047911,32.4124999998808,
-7.14886745759543));
#300780=CARTESIAN_POINT('Ctrl Pts',(-12.1623797632103,32.5624999998802,
-3.95179673813153));
#300781=CARTESIAN_POINT('Ctrl Pts',(-12.1623797632103,32.7124999998796,
2.97892388940601E-15));
#300782=CARTESIAN_POINT('Ctrl Pts',(-12.1623797632103,32.862499999879,3.95179673813154));
#300783=CARTESIAN_POINT('Ctrl Pts',(-9.8395719204791,33.0124999998784,7.14886745759543));
#300784=CARTESIAN_POINT('Ctrl Pts',(-7.51676407774789,33.1624999998778,
10.3459381770593));
#300785=CARTESIAN_POINT('Ctrl Pts',(-3.75838203887396,33.3124999998772,
11.5671105274575));
#300786=CARTESIAN_POINT('Ctrl Pts',(-2.93996111326235E-14,33.4624999998766,
12.7882828778556));
#300787=CARTESIAN_POINT('Ctrl Pts',(3.7583820388739,33.612499999876,11.5671105274575));
#300788=CARTESIAN_POINT('Ctrl Pts',(7.51676407774783,33.7624999998754,10.3459381770593));
#300789=CARTESIAN_POINT('Ctrl Pts',(9.83957192047905,33.9124999998748,7.14886745759543));
#300790=CARTESIAN_POINT('Ctrl Pts',(12.1623797632103,34.0624999998742,3.95179673813153));
#300791=CARTESIAN_POINT('Ctrl Pts',(12.1623797632103,34.2124999998736,-1.489461944703E-15));
#300792=CARTESIAN_POINT('Ctrl Pts',(12.1623797632103,34.362499999873,-3.95179673813154));
#300793=CARTESIAN_POINT('Ctrl Pts',(9.83957192047904,34.5124999998724,-7.14886745759543));
#300794=CARTESIAN_POINT('Ctrl Pts',(7.51676407774783,34.6624999998718,-10.3459381770593));
#300795=CARTESIAN_POINT('Ctrl Pts',(3.7583820388739,34.8124999998712,-11.5671105274575));
#300796=CARTESIAN_POINT('Ctrl Pts',(-3.33956917070458E-14,34.9624999998706,
-12.7882828778556));
#300797=CARTESIAN_POINT('Ctrl Pts',(-3.75838203887396,35.11249999987,-11.5671105274575));
#300798=CARTESIAN_POINT('Ctrl Pts',(-7.51676407774789,35.2624999998694,
-10.3459381770593));
#300799=CARTESIAN_POINT('Ctrl Pts',(-9.83957192047911,35.4124999998688,
-7.14886745759543));
#300800=CARTESIAN_POINT('Ctrl Pts',(-12.1623797632103,35.5624999998682,
-3.95179673813153));
#300801=CARTESIAN_POINT('Ctrl Pts',(-12.1623797632103,35.7124999998676,
2.97892388940601E-15));
#300802=CARTESIAN_POINT('Ctrl Pts',(-12.1623797632103,35.862499999867,3.95179673813154));
#300803=CARTESIAN_POINT('Ctrl Pts',(-9.83957192047911,36.0124999998664,
7.14886745759543));
#300804=CARTESIAN_POINT('Ctrl Pts',(-7.51676407774789,36.1624999998658,
10.3459381770593));
#300805=CARTESIAN_POINT('Ctrl Pts',(-3.75838203887396,36.3124999998652,
11.5671105274575));
#300806=CARTESIAN_POINT('Ctrl Pts',(-3.11273204042854E-14,36.4624999998646,
12.7882828778556));
#300807=CARTESIAN_POINT('Ctrl Pts',(3.7583820388739,36.612499999864,11.5671105274575));
#300808=CARTESIAN_POINT('Ctrl Pts',(7.51676407774783,36.7624999998634,10.3459381770593));
#300809=CARTESIAN_POINT('Ctrl Pts',(9.83957192047904,36.9124999998628,7.14886745759543));
#300810=CARTESIAN_POINT('Ctrl Pts',(12.1623797632103,37.0624999998622,3.95179673813153));
#300811=CARTESIAN_POINT('Ctrl Pts',(12.1623797632103,37.2124999998616,-1.489461944703E-15));
#300812=CARTESIAN_POINT('Ctrl Pts',(12.1623797632103,37.362499999861,-3.95179673813154));
#300813=CARTESIAN_POINT('Ctrl Pts',(9.83957192047904,37.5124999998604,-7.14886745759543));
#300814=CARTESIAN_POINT('Ctrl Pts',(7.51676407774782,37.6624999998598,-10.3459381770593));
#300815=CARTESIAN_POINT('Ctrl Pts',(3.75838203887389,37.8124999998592,-11.5671105274575));
#300816=CARTESIAN_POINT('Ctrl Pts',(-3.51234009787076E-14,37.9624999998586,
-12.7882828778556));
#300817=CARTESIAN_POINT('Ctrl Pts',(-3.75838203887396,38.112499999858,-11.5671105274575));
#300818=CARTESIAN_POINT('Ctrl Pts',(-7.51676407774789,38.2624999998574,
-10.3459381770593));
#300819=CARTESIAN_POINT('Ctrl Pts',(-9.83957192047911,38.4124999998568,
-7.14886745759543));
#300820=CARTESIAN_POINT('Ctrl Pts',(-12.1623797632103,38.5624999998562,
-3.95179673813153));
#300821=CARTESIAN_POINT('Ctrl Pts',(-12.1623797632103,38.7124999998556,
2.97892388940601E-15));
#300822=CARTESIAN_POINT('Ctrl Pts',(-12.1623797632103,38.862499999855,3.95179673813154));
#300823=CARTESIAN_POINT('Ctrl Pts',(-9.83957192047911,39.0124999998544,
7.14886745759543));
#300824=CARTESIAN_POINT('Ctrl Pts',(-7.51676407774789,39.1624999998538,
10.3459381770593));
#300825=CARTESIAN_POINT('Ctrl Pts',(-3.75838203887396,39.3124999998532,
11.5671105274575));
#300826=CARTESIAN_POINT('Ctrl Pts',(-3.28550296759472E-14,39.4624999998526,
12.7882828778556));
#300827=CARTESIAN_POINT('Ctrl Pts',(3.7583820388739,39.612499999852,11.5671105274575));
#300828=CARTESIAN_POINT('Ctrl Pts',(7.51676407774782,39.7624999998514,10.3459381770593));
#300829=CARTESIAN_POINT('Ctrl Pts',(9.83957192047904,39.9124999998508,7.14886745759543));
#300830=CARTESIAN_POINT('Ctrl Pts',(12.1623797632103,40.0624999998502,3.95179673813153));
#300831=CARTESIAN_POINT('Ctrl Pts',(12.1623797632103,40.2124999998496,-1.489461944703E-15));
#300832=CARTESIAN_POINT('Ctrl Pts',(12.1623797632103,40.362499999849,-3.95179673813154));
#300833=CARTESIAN_POINT('Ctrl Pts',(9.83957192047904,40.5124999998484,-7.14886745759543));
#300834=CARTESIAN_POINT('Ctrl Pts',(7.51676407774782,40.6624999998478,-10.3459381770593));
#300835=CARTESIAN_POINT('Ctrl Pts',(3.75838203887389,40.8124999998472,-11.5671105274575));
#300836=CARTESIAN_POINT('Ctrl Pts',(-3.68511102503695E-14,40.9624999998466,
-12.7882828778556));
#300837=CARTESIAN_POINT('Ctrl Pts',(-3.75838203887397,41.112499999846,-11.5671105274575));
#300838=CARTESIAN_POINT('Ctrl Pts',(-7.51676407774789,41.2624999998454,
-10.3459381770593));
#300839=CARTESIAN_POINT('Ctrl Pts',(-9.83957192047911,41.4124999998448,
-7.14886745759543));
#300840=CARTESIAN_POINT('Ctrl Pts',(-12.1623797632103,41.5624999998442,
-3.95179673813153));
#300841=CARTESIAN_POINT('Ctrl Pts',(-12.1623797632103,41.7124999998436,
2.97892388940601E-15));
#300842=CARTESIAN_POINT('Ctrl Pts',(-12.1623797632103,41.862499999843,3.95179673813154));
#300843=CARTESIAN_POINT('Ctrl Pts',(-9.83957192047911,42.0124999998424,
7.14886745759543));
#300844=CARTESIAN_POINT('Ctrl Pts',(-7.51676407774789,42.1624999998418,
10.3459381770593));
#300845=CARTESIAN_POINT('Ctrl Pts',(-3.75838203887396,42.3124999998412,
11.5671105274575));
#300846=CARTESIAN_POINT('Ctrl Pts',(-3.4582738947609E-14,42.4624999998406,
12.7882828778556));
#300847=CARTESIAN_POINT('Ctrl Pts',(3.75838203887389,42.61249999984,11.5671105274575));
#300848=CARTESIAN_POINT('Ctrl Pts',(7.51676407774782,42.7624999998394,10.3459381770593));
#300849=CARTESIAN_POINT('Ctrl Pts',(9.83957192047904,42.9124999998388,7.14886745759543));
#300850=CARTESIAN_POINT('Ctrl Pts',(12.1623797632103,43.0624999998382,3.95179673813153));
#300851=CARTESIAN_POINT('Ctrl Pts',(12.1623797632103,43.2124999998376,-1.489461944703E-15));
#300852=CARTESIAN_POINT('Ctrl Pts',(12.1623797632103,43.362499999837,-3.95179673813154));
#300853=CARTESIAN_POINT('Ctrl Pts',(9.83957192047903,43.5124999998364,-7.14886745759543));
#300854=CARTESIAN_POINT('Ctrl Pts',(7.51676407774782,43.6624999998358,-10.3459381770593));
#300855=CARTESIAN_POINT('Ctrl Pts',(3.75838203887389,43.8124999998352,-11.5671105274575));
#300856=CARTESIAN_POINT('Ctrl Pts',(-3.85788195220313E-14,43.9624999998346,
-12.7882828778556));
#300857=CARTESIAN_POINT('Ctrl Pts',(-3.75838203887397,44.112499999834,-11.5671105274575));
#300858=CARTESIAN_POINT('Ctrl Pts',(-7.5167640777479,44.2624999998334,-10.3459381770593));
#300859=CARTESIAN_POINT('Ctrl Pts',(-9.83957192047911,44.4124999998328,
-7.14886745759543));
#300860=CARTESIAN_POINT('Ctrl Pts',(-12.1623797632103,44.5624999998322,
-3.95179673813153));
#300861=CARTESIAN_POINT('Ctrl Pts',(-12.1623797632103,44.7124999998316,
2.97892388940601E-15));
#300862=CARTESIAN_POINT('Ctrl Pts',(-12.1623797632103,44.862499999831,3.95179673813154));
#300863=CARTESIAN_POINT('Ctrl Pts',(-9.83957192047911,45.0124999998304,
7.14886745759543));
#300864=CARTESIAN_POINT('Ctrl Pts',(-7.51676407774789,45.1624999998298,
10.3459381770593));
#300865=CARTESIAN_POINT('Ctrl Pts',(-3.75838203887397,45.3124999998292,
11.5671105274575));
#300866=CARTESIAN_POINT('Ctrl Pts',(-3.63104482192709E-14,45.4624999998286,
12.7882828778556));
#300867=CARTESIAN_POINT('Ctrl Pts',(3.75838203887389,45.612499999828,11.5671105274575));
#300868=CARTESIAN_POINT('Ctrl Pts',(7.51676407774782,45.7624999998274,10.3459381770593));
#300869=CARTESIAN_POINT('Ctrl Pts',(9.83957192047904,45.9124999998268,7.14886745759543));
#300870=CARTESIAN_POINT('Ctrl Pts',(12.1623797632103,46.0624999998262,3.95179673813153));
#300871=CARTESIAN_POINT('Ctrl Pts',(12.1623797632103,46.2124999998256,-1.489461944703E-15));
#300872=CARTESIAN_POINT('Ctrl Pts',(12.1623797632103,46.362499999825,-3.95179673813154));
#300873=CARTESIAN_POINT('Ctrl Pts',(9.83957192047903,46.5124999998244,-7.14886745759543));
#300874=CARTESIAN_POINT('Ctrl Pts',(7.51676407774782,46.6624999998238,-10.3459381770593));
#300875=CARTESIAN_POINT('Ctrl Pts',(3.75838203887389,46.8124999998232,-11.5671105274575));
#300876=CARTESIAN_POINT('Ctrl Pts',(-4.03065287936931E-14,46.9624999998226,
-12.7882828778556));
#300877=CARTESIAN_POINT('Ctrl Pts',(-3.75838203887397,47.112499999822,-11.5671105274575));
#300878=CARTESIAN_POINT('Ctrl Pts',(-7.5167640777479,47.2624999998214,-10.3459381770593));
#300879=CARTESIAN_POINT('Ctrl Pts',(-9.83957192047912,47.4124999998208,
-7.14886745759543));
#300880=CARTESIAN_POINT('Ctrl Pts',(-12.1623797632103,47.5624999998202,
-3.95179673813153));
#300881=CARTESIAN_POINT('Ctrl Pts',(-12.1623797632103,47.7124999998196,
2.97892388940601E-15));
#300882=CARTESIAN_POINT('Ctrl Pts',(-12.1623797632103,47.862499999819,3.95179673813154));
#300883=CARTESIAN_POINT('Ctrl Pts',(-9.83957192047911,48.0124999998184,
7.14886745759543));
#300884=CARTESIAN_POINT('Ctrl Pts',(-7.51676407774789,48.1624999998178,
10.3459381770593));
#300885=CARTESIAN_POINT('Ctrl Pts',(-3.75838203887397,48.3124999998172,
11.5671105274575));
#300886=CARTESIAN_POINT('Ctrl Pts',(-3.80381574909327E-14,48.4624999998166,
12.7882828778556));
#300887=CARTESIAN_POINT('Ctrl Pts',(3.75838203887389,48.612499999816,11.5671105274575));
#300888=CARTESIAN_POINT('Ctrl Pts',(7.51676407774782,48.7624999998154,10.3459381770593));
#300889=CARTESIAN_POINT('Ctrl Pts',(9.83957192047903,48.9124999998148,7.14886745759543));
#300890=CARTESIAN_POINT('Ctrl Pts',(12.1623797632103,49.0624999998142,3.95179673813153));
#300891=CARTESIAN_POINT('Ctrl Pts',(12.1623797632103,49.2124999998136,-1.489461944703E-15));
#300892=CARTESIAN_POINT('Ctrl Pts',(12.1623797632103,49.362499999813,-3.95179673813154));
#300893=CARTESIAN_POINT('Ctrl Pts',(9.83957192047903,49.5124999998124,-7.14886745759543));
#300894=CARTESIAN_POINT('Ctrl Pts',(7.51676407774782,49.6624999998118,-10.3459381770593));
#300895=CARTESIAN_POINT('Ctrl Pts',(3.75838203887389,49.8124999998112,-11.5671105274575));
#300896=CARTESIAN_POINT('Ctrl Pts',(-4.2034238065355E-14,49.9624999998106,
-12.7882828778556));
#300897=CARTESIAN_POINT('Ctrl Pts',(-3.75838203887397,50.11249999981,-11.5671105274575));
#300898=CARTESIAN_POINT('Ctrl Pts',(-7.5167640777479,50.2624999998094,-10.3459381770593));
#300899=CARTESIAN_POINT('Ctrl Pts',(-9.83957192047912,50.4124999998088,
-7.14886745759543));
#300900=CARTESIAN_POINT('Ctrl Pts',(-12.1623797632103,50.5624999998082,
-3.95179673813153));
#300901=CARTESIAN_POINT('Ctrl Pts',(-12.1623797632103,50.7124999998076,
2.97892388940601E-15));
#300902=CARTESIAN_POINT('Ctrl Pts',(-12.1623797632103,50.862499999807,3.95179673813154));
#300903=CARTESIAN_POINT('Ctrl Pts',(-9.83957192047912,51.0124999998064,
7.14886745759543));
#300904=CARTESIAN_POINT('Ctrl Pts',(-7.5167640777479,51.1624999998058,10.3459381770593));
#300905=CARTESIAN_POINT('Ctrl Pts',(-3.75838203887397,51.3124999998052,
11.5671105274575));
#300906=CARTESIAN_POINT('Ctrl Pts',(-3.97658667625946E-14,51.4624999998046,
12.7882828778556));
#300907=CARTESIAN_POINT('Ctrl Pts',(3.75838203887389,51.612499999804,11.5671105274575));
#300908=CARTESIAN_POINT('Ctrl Pts',(7.51676407774782,51.7624999998034,10.3459381770593));
#300909=CARTESIAN_POINT('Ctrl Pts',(9.83957192047903,51.9124999998028,7.14886745759543));
#300910=CARTESIAN_POINT('Ctrl Pts',(12.1623797632103,52.0624999998022,3.95179673813153));
#300911=CARTESIAN_POINT('Ctrl Pts',(12.1623797632103,52.2124999998016,-1.489461944703E-15));
#300912=CARTESIAN_POINT('Ctrl Pts',(12.1623797632103,52.362499999801,-3.95179673813154));
#300913=CARTESIAN_POINT('Ctrl Pts',(9.83957192047903,52.5124999998004,-7.14886745759543));
#300914=CARTESIAN_POINT('Ctrl Pts',(7.51676407774781,52.6624999997998,-10.3459381770593));
#300915=CARTESIAN_POINT('Ctrl Pts',(3.75838203887388,52.8124999997992,-11.5671105274575));
#300916=CARTESIAN_POINT('Ctrl Pts',(-4.37619473370168E-14,52.9624999997986,
-12.7882828778556));
#300917=CARTESIAN_POINT('Ctrl Pts',(-3.75838203887397,53.112499999798,-11.5671105274575));
#300918=CARTESIAN_POINT('Ctrl Pts',(-7.5167640777479,53.2624999997974,-10.3459381770593));
#300919=CARTESIAN_POINT('Ctrl Pts',(-9.83957192047912,53.4124999997968,
-7.14886745759543));
#300920=CARTESIAN_POINT('Ctrl Pts',(-12.1623797632103,53.5624999997962,
-3.95179673813153));
#300921=CARTESIAN_POINT('Ctrl Pts',(-12.1623797632103,53.7124999997956,
2.97892388940601E-15));
#300922=CARTESIAN_POINT('Ctrl Pts',(-12.1623797632103,53.862499999795,3.95179673813154));
#300923=CARTESIAN_POINT('Ctrl Pts',(-9.83957192047912,54.0124999997944,
7.14886745759543));
#300924=CARTESIAN_POINT('Ctrl Pts',(-7.5167640777479,54.1624999997938,10.3459381770593));
#300925=CARTESIAN_POINT('Ctrl Pts',(-3.75838203887397,54.3124999997932,
11.5671105274575));
#300926=CARTESIAN_POINT('Ctrl Pts',(-4.14935760342564E-14,54.4624999997926,
12.7882828778556));
#300927=CARTESIAN_POINT('Ctrl Pts',(3.75838203887389,54.612499999792,11.5671105274575));
#300928=CARTESIAN_POINT('Ctrl Pts',(7.51676407774782,54.7624999997914,10.3459381770593));
#300929=CARTESIAN_POINT('Ctrl Pts',(9.83957192047903,54.9124999997908,7.14886745759543));
#300930=CARTESIAN_POINT('Ctrl Pts',(12.1623797632103,55.0624999997902,3.95179673813153));
#300931=CARTESIAN_POINT('Ctrl Pts',(12.1623797632103,55.2124999997896,-1.489461944703E-15));
#300932=CARTESIAN_POINT('Ctrl Pts',(12.1623797632103,55.362499999789,-3.95179673813154));
#300933=CARTESIAN_POINT('Ctrl Pts',(9.83957192047903,55.5124999997884,-7.14886745759543));
#300934=CARTESIAN_POINT('Ctrl Pts',(7.51676407774781,55.6624999997878,-10.3459381770593));
#300935=CARTESIAN_POINT('Ctrl Pts',(3.75838203887388,55.8124999997872,-11.5671105274575));
#300936=CARTESIAN_POINT('Ctrl Pts',(-4.54896566086787E-14,55.9624999997866,
-12.7882828778556));
#300937=CARTESIAN_POINT('Ctrl Pts',(-3.75838203887397,56.112499999786,-11.5671105274575));
#300938=CARTESIAN_POINT('Ctrl Pts',(-7.5167640777479,56.2624999997854,-10.3459381770593));
#300939=CARTESIAN_POINT('Ctrl Pts',(-9.83957192047912,56.4124999997848,
-7.14886745759543));
#300940=CARTESIAN_POINT('Ctrl Pts',(-12.1623797632103,56.5624999997842,
-3.95179673813153));
#300941=CARTESIAN_POINT('Ctrl Pts',(-12.1623797632103,56.7124999997836,
2.97892388940601E-15));
#300942=CARTESIAN_POINT('Ctrl Pts',(-12.1623797632103,56.862499999783,3.95179673813154));
#300943=CARTESIAN_POINT('Ctrl Pts',(-9.83957192047912,57.0124999997824,
7.14886745759543));
#300944=CARTESIAN_POINT('Ctrl Pts',(-7.5167640777479,57.1624999997818,10.3459381770593));
#300945=CARTESIAN_POINT('Ctrl Pts',(-3.75838203887397,57.3124999997812,
11.5671105274575));
#300946=CARTESIAN_POINT('Ctrl Pts',(-4.32212853059182E-14,57.4624999997806,
12.7882828778556));
#300947=CARTESIAN_POINT('Ctrl Pts',(3.75838203887389,57.61249999978,11.5671105274575));
#300948=CARTESIAN_POINT('Ctrl Pts',(7.51676407774781,57.7624999997794,10.3459381770593));
#300949=CARTESIAN_POINT('Ctrl Pts',(9.83957192047903,57.9124999997788,7.14886745759543));
#300950=CARTESIAN_POINT('Ctrl Pts',(12.1623797632103,58.0624999997782,3.95179673813153));
#300951=CARTESIAN_POINT('Ctrl Pts',(12.1623797632102,58.2124999997776,-1.489461944703E-15));
#300952=CARTESIAN_POINT('Ctrl Pts',(12.1623797632102,58.362499999777,-3.95179673813154));
#300953=CARTESIAN_POINT('Ctrl Pts',(9.83957192047903,58.5124999997764,-7.14886745759543));
#300954=CARTESIAN_POINT('Ctrl Pts',(7.51676407774781,58.6624999997758,-10.3459381770593));
#300955=CARTESIAN_POINT('Ctrl Pts',(3.75838203887388,58.8124999997752,-11.5671105274575));
#300956=CARTESIAN_POINT('Ctrl Pts',(-4.72173658803405E-14,58.9624999997746,
-12.7882828778556));
#300957=CARTESIAN_POINT('Ctrl Pts',(-3.75838203887398,59.112499999774,-11.5671105274575));
#300958=CARTESIAN_POINT('Ctrl Pts',(-7.51676407774791,59.2624999997734,
-10.3459381770593));
#300959=CARTESIAN_POINT('Ctrl Pts',(-9.83957192047912,59.4124999997728,
-7.14886745759543));
#300960=CARTESIAN_POINT('Ctrl Pts',(-12.1623797632103,59.5624999997722,
-3.95179673813153));
#300961=CARTESIAN_POINT('Ctrl Pts',(-12.1623797632103,59.7124999997716,
2.97892388940601E-15));
#300962=CARTESIAN_POINT('Ctrl Pts',(-12.1623797632103,59.862499999771,3.95179673813154));
#300963=CARTESIAN_POINT('Ctrl Pts',(-9.83957192047912,60.0124999997704,
7.14886745759543));
#300964=CARTESIAN_POINT('Ctrl Pts',(-7.5167640777479,60.1624999997698,10.3459381770593));
#300965=CARTESIAN_POINT('Ctrl Pts',(-3.75838203887397,60.3124999997692,
11.5671105274575));
#300966=CARTESIAN_POINT('Ctrl Pts',(-4.49489945775801E-14,60.4624999997686,
12.7882828778556));
#300967=CARTESIAN_POINT('Ctrl Pts',(3.75838203887388,60.612499999768,11.5671105274575));
#300968=CARTESIAN_POINT('Ctrl Pts',(7.51676407774781,60.7624999997674,10.3459381770593));
#300969=CARTESIAN_POINT('Ctrl Pts',(9.83957192047903,60.9124999997668,7.14886745759543));
#300970=CARTESIAN_POINT('Ctrl Pts',(12.1623797632103,61.0624999997662,3.95179673813153));
#300971=CARTESIAN_POINT('Ctrl Pts',(12.1623797632102,61.2124999997656,-1.489461944703E-15));
#300972=CARTESIAN_POINT('Ctrl Pts',(12.1623797632102,61.362499999765,-3.95179673813154));
#300973=CARTESIAN_POINT('Ctrl Pts',(9.83957192047902,61.5124999997644,-7.14886745759543));
#300974=CARTESIAN_POINT('Ctrl Pts',(7.51676407774781,61.6624999997638,-10.3459381770593));
#300975=CARTESIAN_POINT('Ctrl Pts',(3.75838203887388,61.8124999997632,-11.5671105274575));
#300976=CARTESIAN_POINT('Ctrl Pts',(-4.89450751520023E-14,61.9624999997626,
-12.7882828778556));
#300977=CARTESIAN_POINT('Ctrl Pts',(-3.75838203887398,62.112499999762,-11.5671105274575));
#300978=CARTESIAN_POINT('Ctrl Pts',(-7.51676407774791,62.2624999997614,
-10.3459381770593));
#300979=CARTESIAN_POINT('Ctrl Pts',(-9.83957192047912,62.4124999997608,
-7.14886745759543));
#300980=CARTESIAN_POINT('Ctrl Pts',(-12.1623797632103,62.5624999997602,
-3.95179673813153));
#300981=CARTESIAN_POINT('Ctrl Pts',(-12.1623797632103,62.7124999997596,
2.97892388940601E-15));
#300982=CARTESIAN_POINT('Ctrl Pts',(-12.1623797632103,62.862499999759,3.95179673813154));
#300983=CARTESIAN_POINT('Ctrl Pts',(-9.83957192047912,63.0124999997584,
7.14886745759543));
#300984=CARTESIAN_POINT('Ctrl Pts',(-7.5167640777479,63.1624999997578,10.3459381770593));
#300985=CARTESIAN_POINT('Ctrl Pts',(-3.75838203887398,63.3124999997572,
11.5671105274575));
#300986=CARTESIAN_POINT('Ctrl Pts',(-4.66767038492419E-14,63.4624999997566,
12.7882828778556));
#300987=CARTESIAN_POINT('Ctrl Pts',(3.75838203887388,63.612499999756,11.5671105274575));
#300988=CARTESIAN_POINT('Ctrl Pts',(7.51676407774781,63.7624999997554,10.3459381770593));
#300989=CARTESIAN_POINT('Ctrl Pts',(9.83957192047903,63.9124999997548,7.14886745759543));
#300990=CARTESIAN_POINT('Ctrl Pts',(12.1623797632102,64.0624999997542,3.95179673813153));
#300991=CARTESIAN_POINT('Ctrl Pts',(12.1623797632102,64.2124999997536,-1.489461944703E-15));
#300992=CARTESIAN_POINT('Ctrl Pts',(12.1623797632102,64.362499999753,-3.95179673813154));
#300993=CARTESIAN_POINT('Ctrl Pts',(9.83957192047902,64.5124999997524,-7.14886745759543));
#300994=CARTESIAN_POINT('Ctrl Pts',(7.51676407774781,64.6624999997518,-10.3459381770593));
#300995=CARTESIAN_POINT('Ctrl Pts',(3.75838203887388,64.8124999997512,-11.5671105274575));
#300996=CARTESIAN_POINT('Ctrl Pts',(-5.06727844236642E-14,64.9624999997506,
-12.7882828778556));
#300997=CARTESIAN_POINT('Ctrl Pts',(-3.75838203887398,65.11249999975,-11.5671105274575));
#300998=CARTESIAN_POINT('Ctrl Pts',(-7.51676407774791,65.2624999997494,
-10.3459381770593));
#300999=CARTESIAN_POINT('Ctrl Pts',(-9.83957192047913,65.4124999997488,
-7.14886745759543));
#301000=CARTESIAN_POINT('Ctrl Pts',(-12.1623797632103,65.5624999997482,
-3.95179673813153));
#301001=CARTESIAN_POINT('Ctrl Pts',(-12.1623797632103,65.7124999997476,
2.97892388940601E-15));
#301002=CARTESIAN_POINT('Ctrl Pts',(-12.1623797632103,65.862499999747,3.95179673813154));
#301003=CARTESIAN_POINT('Ctrl Pts',(-9.83957192047912,66.0124999997464,
7.14886745759543));
#301004=CARTESIAN_POINT('Ctrl Pts',(-7.51676407774791,66.1624999997458,
10.3459381770593));
#301005=CARTESIAN_POINT('Ctrl Pts',(-3.75838203887398,66.3124999997452,
11.5671105274575));
#301006=CARTESIAN_POINT('Ctrl Pts',(-4.84044131209037E-14,66.4624999997446,
12.7882828778556));
#301007=CARTESIAN_POINT('Ctrl Pts',(3.75838203887388,66.612499999744,11.5671105274575));
#301008=CARTESIAN_POINT('Ctrl Pts',(7.51676407774781,66.7624999997434,10.3459381770593));
#301009=CARTESIAN_POINT('Ctrl Pts',(9.83957192047902,66.9124999997428,7.14886745759543));
#301010=CARTESIAN_POINT('Ctrl Pts',(12.1623797632102,67.0624999997422,3.95179673813153));
#301011=CARTESIAN_POINT('Ctrl Pts',(12.1623797632102,67.2124999997416,-1.489461944703E-15));
#301012=CARTESIAN_POINT('Ctrl Pts',(12.1623797632102,67.362499999741,-3.95179673813154));
#301013=CARTESIAN_POINT('Ctrl Pts',(9.83957192047902,67.5124999997404,-7.14886745759543));
#301014=CARTESIAN_POINT('Ctrl Pts',(7.51676407774781,67.6624999997398,-10.3459381770593));
#301015=CARTESIAN_POINT('Ctrl Pts',(3.75838203887388,67.8124999997392,-11.5671105274575));
#301016=CARTESIAN_POINT('Ctrl Pts',(-5.2400493695326E-14,67.9624999997386,
-12.7882828778556));
#301017=CARTESIAN_POINT('Ctrl Pts',(-3.75838203887398,68.112499999738,-11.5671105274575));
#301018=CARTESIAN_POINT('Ctrl Pts',(-7.51676407774791,68.2624999997374,
-10.3459381770593));
#301019=CARTESIAN_POINT('Ctrl Pts',(-9.83957192047913,68.4124999997368,
-7.14886745759543));
#301020=CARTESIAN_POINT('Ctrl Pts',(-12.1623797632103,68.5624999997362,
-3.95179673813153));
#301021=CARTESIAN_POINT('Ctrl Pts',(-12.1623797632103,68.7124999997356,
2.97892388940601E-15));
#301022=CARTESIAN_POINT('Ctrl Pts',(-12.1623797632103,68.862499999735,3.95179673813154));
#301023=CARTESIAN_POINT('Ctrl Pts',(-9.83957192047913,69.0124999997344,
7.14886745759543));
#301024=CARTESIAN_POINT('Ctrl Pts',(-7.51676407774791,69.1624999997338,
10.3459381770593));
#301025=CARTESIAN_POINT('Ctrl Pts',(-3.75838203887398,69.3124999997332,
11.5671105274575));
#301026=CARTESIAN_POINT('Ctrl Pts',(-5.01321223925656E-14,69.4624999997326,
12.7882828778556));
#301027=CARTESIAN_POINT('Ctrl Pts',(3.75838203887388,69.612499999732,11.5671105274575));
#301028=CARTESIAN_POINT('Ctrl Pts',(7.51676407774781,69.7624999997314,10.3459381770593));
#301029=CARTESIAN_POINT('Ctrl Pts',(9.83957192047902,69.9124999997308,7.14886745759543));
#301030=CARTESIAN_POINT('Ctrl Pts',(12.1623797632102,70.0624999997302,3.95179673813153));
#301031=CARTESIAN_POINT('Ctrl Pts',(12.1623797632102,70.2124999997296,-1.489461944703E-15));
#301032=CARTESIAN_POINT('Ctrl Pts',(12.1623797632102,70.362499999729,-3.95179673813154));
#301033=CARTESIAN_POINT('Ctrl Pts',(9.83957192047902,70.5124999997284,-7.14886745759543));
#301034=CARTESIAN_POINT('Ctrl Pts',(7.5167640777478,70.6624999997278,-10.3459381770593));
#301035=CARTESIAN_POINT('Ctrl Pts',(3.75838203887388,70.8124999997272,-11.5671105274575));
#301036=CARTESIAN_POINT('Ctrl Pts',(-5.41282029669879E-14,70.9624999997266,
-12.7882828778556));
#301037=CARTESIAN_POINT('Ctrl Pts',(-3.75838203887398,71.112499999726,-11.5671105274575));
#301038=CARTESIAN_POINT('Ctrl Pts',(-7.51676407774791,71.2624999997254,
-10.3459381770593));
#301039=CARTESIAN_POINT('Ctrl Pts',(-9.83957192047913,71.4124999997248,
-7.14886745759543));
#301040=CARTESIAN_POINT('Ctrl Pts',(-12.1623797632103,71.5624999997242,
-3.95179673813153));
#301041=CARTESIAN_POINT('Ctrl Pts',(-12.1623797632103,71.7124999997236,
2.97892388940601E-15));
#301042=CARTESIAN_POINT('Ctrl Pts',(-12.1623797632103,71.862499999723,3.95179673813154));
#301043=CARTESIAN_POINT('Ctrl Pts',(-9.83957192047913,72.0124999997224,
7.14886745759543));
#301044=CARTESIAN_POINT('Ctrl Pts',(-7.51676407774791,72.1624999997218,
10.3459381770593));
#301045=CARTESIAN_POINT('Ctrl Pts',(-3.75838203887398,72.3124999997212,
11.5671105274575));
#301046=CARTESIAN_POINT('Ctrl Pts',(-5.18598316642274E-14,72.4624999997206,
12.7882828778556));
#301047=CARTESIAN_POINT('Ctrl Pts',(3.75838203887388,72.61249999972,11.5671105274575));
#301048=CARTESIAN_POINT('Ctrl Pts',(7.51676407774781,72.7624999997194,10.3459381770593));
#301049=CARTESIAN_POINT('Ctrl Pts',(9.83957192047902,72.9124999997188,7.14886745759543));
#301050=CARTESIAN_POINT('Ctrl Pts',(12.1623797632102,73.0624999997182,3.95179673813153));
#301051=CARTESIAN_POINT('Ctrl Pts',(12.1623797632102,73.2124999997176,-1.489461944703E-15));
#301052=CARTESIAN_POINT('Ctrl Pts',(12.1623797632102,73.362499999717,-3.95179673813154));
#301053=CARTESIAN_POINT('Ctrl Pts',(9.83957192047902,73.5124999997164,-7.14886745759543));
#301054=CARTESIAN_POINT('Ctrl Pts',(7.5167640777478,73.6624999997158,-10.3459381770593));
#301055=CARTESIAN_POINT('Ctrl Pts',(3.75838203887387,73.8124999997152,-11.5671105274575));
#301056=CARTESIAN_POINT('Ctrl Pts',(-5.58559122386497E-14,73.9624999997146,
-12.7882828778556));
#301057=CARTESIAN_POINT('Ctrl Pts',(-3.75838203887398,74.112499999714,-11.5671105274575));
#301058=CARTESIAN_POINT('Ctrl Pts',(-7.51676407774791,74.2624999997134,
-10.3459381770593));
#301059=CARTESIAN_POINT('Ctrl Pts',(-9.83957192047913,74.4124999997128,
-7.14886745759543));
#301060=CARTESIAN_POINT('Ctrl Pts',(-12.1623797632103,74.5624999997122,
-3.95179673813153));
#301061=CARTESIAN_POINT('Ctrl Pts',(-12.1623797632103,74.7124999997116,
2.97892388940601E-15));
#301062=CARTESIAN_POINT('Ctrl Pts',(-12.1623797632103,74.862499999711,3.95179673813154));
#301063=CARTESIAN_POINT('Ctrl Pts',(-9.83957192047913,75.0124999997104,
7.14886745759543));
#301064=CARTESIAN_POINT('Ctrl Pts',(-7.51676407774791,75.1624999997098,
10.3459381770593));
#301065=CARTESIAN_POINT('Ctrl Pts',(-3.75838203887398,75.3124999997092,
11.5671105274575));
#301066=CARTESIAN_POINT('Ctrl Pts',(-5.35875409358893E-14,75.4624999997086,
12.7882828778556));
#301067=CARTESIAN_POINT('Ctrl Pts',(3.75838203887388,75.612499999708,11.5671105274575));
#301068=CARTESIAN_POINT('Ctrl Pts',(7.5167640777478,75.7624999997074,10.3459381770593));
#301069=CARTESIAN_POINT('Ctrl Pts',(9.83957192047902,75.9124999997068,7.14886745759543));
#301070=CARTESIAN_POINT('Ctrl Pts',(12.1623797632102,76.0624999997062,3.95179673813153));
#301071=CARTESIAN_POINT('Ctrl Pts',(12.1623797632102,76.2124999997056,-1.489461944703E-15));
#301072=CARTESIAN_POINT('Ctrl Pts',(12.1623797632102,76.362499999705,-3.95179673813154));
#301073=CARTESIAN_POINT('Ctrl Pts',(9.83957192047902,76.5124999997044,-7.14886745759543));
#301074=CARTESIAN_POINT('Ctrl Pts',(7.5167640777478,76.6624999997038,-10.3459381770593));
#301075=CARTESIAN_POINT('Ctrl Pts',(3.75838203887387,76.8124999997032,-11.5671105274575));
#301076=CARTESIAN_POINT('Ctrl Pts',(-5.75836215103115E-14,76.9624999997026,
-12.7882828778556));
#301077=CARTESIAN_POINT('Ctrl Pts',(-3.75838203887399,77.112499999702,-11.5671105274575));
#301078=CARTESIAN_POINT('Ctrl Pts',(-7.51676407774791,77.2624999997014,
-10.3459381770593));
#301079=CARTESIAN_POINT('Ctrl Pts',(-9.83957192047913,77.4124999997008,
-7.14886745759543));
#301080=CARTESIAN_POINT('Ctrl Pts',(-12.1623797632103,77.5624999997002,
-3.95179673813153));
#301081=CARTESIAN_POINT('Ctrl Pts',(-12.1623797632103,77.7124999996996,
2.97892388940601E-15));
#301082=CARTESIAN_POINT('Ctrl Pts',(-12.1623797632103,77.862499999699,3.95179673813154));
#301083=CARTESIAN_POINT('Ctrl Pts',(-9.83957192047913,78.0124999996984,
7.14886745759543));
#301084=CARTESIAN_POINT('Ctrl Pts',(-7.51676407774791,78.1624999996978,
10.3459381770593));
#301085=CARTESIAN_POINT('Ctrl Pts',(-3.75838203887398,78.3124999996972,
11.5671105274575));
#301086=CARTESIAN_POINT('Ctrl Pts',(-5.53152502075511E-14,78.4624999996966,
12.7882828778556));
#301087=CARTESIAN_POINT('Ctrl Pts',(3.75838203887387,78.612499999696,11.5671105274575));
#301088=CARTESIAN_POINT('Ctrl Pts',(7.5167640777478,78.7624999996954,10.3459381770593));
#301089=CARTESIAN_POINT('Ctrl Pts',(9.83957192047902,78.9124999996948,7.14886745759543));
#301090=CARTESIAN_POINT('Ctrl Pts',(12.1623797632102,79.0624999996942,3.95179673813153));
#301091=CARTESIAN_POINT('Ctrl Pts',(12.1623797632102,79.2124999996936,-1.489461944703E-15));
#301092=CARTESIAN_POINT('Ctrl Pts',(12.1623797632102,79.362499999693,-3.95179673813154));
#301093=CARTESIAN_POINT('Ctrl Pts',(9.83957192047902,79.5124999996924,-7.14886745759543));
#301094=CARTESIAN_POINT('Ctrl Pts',(7.5167640777478,79.6624999996918,-10.3459381770593));
#301095=CARTESIAN_POINT('Ctrl Pts',(3.75838203887387,79.8124999996912,-11.5671105274575));
#301096=CARTESIAN_POINT('Ctrl Pts',(-5.93113307819734E-14,79.9624999996906,
-12.7882828778556));
#301097=CARTESIAN_POINT('Ctrl Pts',(-3.75838203887399,80.11249999969,-11.5671105274575));
#301098=CARTESIAN_POINT('Ctrl Pts',(-7.51676407774791,80.2624999996894,
-10.3459381770593));
#301099=CARTESIAN_POINT('Ctrl Pts',(-9.83957192047913,80.4124999996888,
-7.14886745759543));
#301100=CARTESIAN_POINT('Ctrl Pts',(-12.1623797632104,80.5624999996882,
-3.95179673813153));
#301101=CARTESIAN_POINT('Ctrl Pts',(-12.1623797632104,80.7124999996876,
2.97892388940601E-15));
#301102=CARTESIAN_POINT('Ctrl Pts',(-12.1623797632104,80.862499999687,3.95179673813154));
#301103=CARTESIAN_POINT('Ctrl Pts',(-9.83957192047913,81.0124999996864,
7.14886745759543));
#301104=CARTESIAN_POINT('Ctrl Pts',(-7.51676407774791,81.1624999996858,
10.3459381770593));
#301105=CARTESIAN_POINT('Ctrl Pts',(-3.75838203887399,81.3124999996852,
11.5671105274575));
#301106=CARTESIAN_POINT('Ctrl Pts',(-5.70429594792129E-14,81.4624999996846,
12.7882828778556));
#301107=CARTESIAN_POINT('Ctrl Pts',(3.75838203887387,81.612499999684,11.5671105274575));
#301108=CARTESIAN_POINT('Ctrl Pts',(7.5167640777478,81.7624999996834,10.3459381770593));
#301109=CARTESIAN_POINT('Ctrl Pts',(9.83957192047902,81.9124999996828,7.14886745759543));
#301110=CARTESIAN_POINT('Ctrl Pts',(12.1623797632102,82.0624999996822,3.95179673813153));
#301111=CARTESIAN_POINT('Ctrl Pts',(12.1623797632102,82.2124999996816,-1.489461944703E-15));
#301112=CARTESIAN_POINT('Ctrl Pts',(12.1623797632102,82.362499999681,-3.95179673813154));
#301113=CARTESIAN_POINT('Ctrl Pts',(9.83957192047902,82.5124999996804,-7.14886745759543));
#301114=CARTESIAN_POINT('Ctrl Pts',(7.5167640777478,82.6624999996798,-10.3459381770593));
#301115=CARTESIAN_POINT('Ctrl Pts',(3.75838203887387,82.8124999996792,-11.5671105274575));
#301116=CARTESIAN_POINT('Ctrl Pts',(-6.10390400536352E-14,82.9624999996786,
-12.7882828778556));
#301117=CARTESIAN_POINT('Ctrl Pts',(-3.75838203887399,83.112499999678,-11.5671105274575));
#301118=CARTESIAN_POINT('Ctrl Pts',(-7.51676407774792,83.2624999996774,
-10.3459381770593));
#301119=CARTESIAN_POINT('Ctrl Pts',(-9.83957192047914,83.4124999996768,
-7.14886745759543));
#301120=CARTESIAN_POINT('Ctrl Pts',(-12.1623797632104,83.5624999996762,
-3.95179673813153));
#301121=CARTESIAN_POINT('Ctrl Pts',(-12.1623797632104,83.7124999996756,
2.97892388940601E-15));
#301122=CARTESIAN_POINT('Ctrl Pts',(-12.1623797632104,83.862499999675,3.95179673813154));
#301123=CARTESIAN_POINT('Ctrl Pts',(-9.83957192047913,84.0124999996744,
7.14886745759543));
#301124=CARTESIAN_POINT('Ctrl Pts',(-7.51676407774791,84.1624999996738,
10.3459381770593));
#301125=CARTESIAN_POINT('Ctrl Pts',(-3.75838203887399,84.3124999996732,
11.5671105274575));
#301126=CARTESIAN_POINT('Ctrl Pts',(-5.87706687508748E-14,84.4624999996726,
12.7882828778556));
#301127=CARTESIAN_POINT('Ctrl Pts',(3.75838203887387,84.6124999996721,11.5671105274575));
#301128=CARTESIAN_POINT('Ctrl Pts',(7.5167640777478,84.7624999996714,10.3459381770593));
#301129=CARTESIAN_POINT('Ctrl Pts',(9.83957192047902,84.9124999996708,7.14886745759543));
#301130=CARTESIAN_POINT('Ctrl Pts',(12.1623797632102,85.0624999996702,3.95179673813153));
#301131=CARTESIAN_POINT('Ctrl Pts',(12.1623797632102,85.2124999996696,-1.489461944703E-15));
#301132=CARTESIAN_POINT('Ctrl Pts',(12.1623797632102,85.362499999669,-3.95179673813154));
#301133=CARTESIAN_POINT('Ctrl Pts',(9.83957192047901,85.5124999996684,-7.14886745759543));
#301134=CARTESIAN_POINT('Ctrl Pts',(7.5167640777478,85.6624999996678,-10.3459381770593));
#301135=CARTESIAN_POINT('Ctrl Pts',(3.75838203887387,85.8124999996672,-11.5671105274575));
#301136=CARTESIAN_POINT('Ctrl Pts',(-6.27667493252971E-14,85.9624999996666,
-12.7882828778556));
#301137=CARTESIAN_POINT('Ctrl Pts',(-3.75838203887399,86.112499999666,-11.5671105274575));
#301138=CARTESIAN_POINT('Ctrl Pts',(-7.51676407774792,86.2624999996654,
-10.3459381770593));
#301139=CARTESIAN_POINT('Ctrl Pts',(-9.83957192047914,86.4124999996648,
-7.14886745759543));
#301140=CARTESIAN_POINT('Ctrl Pts',(-12.1623797632104,86.5624999996642,
-3.95179673813153));
#301141=CARTESIAN_POINT('Ctrl Pts',(-12.1623797632104,86.7124999996636,
2.97892388940601E-15));
#301142=CARTESIAN_POINT('Ctrl Pts',(-12.1623797632104,86.862499999663,3.95179673813154));
#301143=CARTESIAN_POINT('Ctrl Pts',(-9.83957192047914,87.0124999996624,
7.14886745759543));
#301144=CARTESIAN_POINT('Ctrl Pts',(-7.51676407774792,87.1624999996618,
10.3459381770593));
#301145=CARTESIAN_POINT('Ctrl Pts',(-3.75838203887399,87.3124999996612,
11.5671105274575));
#301146=CARTESIAN_POINT('Ctrl Pts',(-6.04983780225366E-14,87.4624999996606,
12.7882828778556));
#301147=CARTESIAN_POINT('Ctrl Pts',(3.75838203887387,87.61249999966,11.5671105274575));
#301148=CARTESIAN_POINT('Ctrl Pts',(7.5167640777478,87.7624999996594,10.3459381770593));
#301149=CARTESIAN_POINT('Ctrl Pts',(9.83957192047901,87.9124999996588,7.14886745759543));
#301150=CARTESIAN_POINT('Ctrl Pts',(12.1623797632102,88.0624999996582,3.95179673813153));
#301151=CARTESIAN_POINT('Ctrl Pts',(12.1623797632102,88.2124999996576,-1.489461944703E-15));
#301152=CARTESIAN_POINT('Ctrl Pts',(12.1623797632102,88.362499999657,-3.95179673813154));
#301153=CARTESIAN_POINT('Ctrl Pts',(9.83957192047901,88.5124999996564,-7.14886745759543));
#301154=CARTESIAN_POINT('Ctrl Pts',(7.51676407774779,88.6624999996558,-10.3459381770593));
#301155=CARTESIAN_POINT('Ctrl Pts',(3.75838203887386,88.8124999996552,-11.5671105274575));
#301156=CARTESIAN_POINT('Ctrl Pts',(-6.44944585969589E-14,88.9624999996546,
-12.7882828778556));
#301157=CARTESIAN_POINT('Ctrl Pts',(-3.75838203887399,89.112499999654,-11.5671105274575));
#301158=CARTESIAN_POINT('Ctrl Pts',(-7.51676407774792,89.2624999996534,
-10.3459381770593));
#301159=CARTESIAN_POINT('Ctrl Pts',(-9.83957192047914,89.4124999996528,
-7.14886745759543));
#301160=CARTESIAN_POINT('Ctrl Pts',(-12.1623797632104,89.5624999996522,
-3.95179673813153));
#301161=CARTESIAN_POINT('Ctrl Pts',(-12.1623797632104,89.7124999996516,
2.97892388940601E-15));
#301162=CARTESIAN_POINT('Ctrl Pts',(-12.1623797632104,89.862499999651,3.95179673813154));
#301163=CARTESIAN_POINT('Ctrl Pts',(-9.83957192047914,90.0124999996504,
7.14886745759543));
#301164=CARTESIAN_POINT('Ctrl Pts',(-7.51676407774792,90.1624999996498,
10.3459381770593));
#301165=CARTESIAN_POINT('Ctrl Pts',(-3.75838203887399,90.3124999996492,
11.5671105274575));
#301166=CARTESIAN_POINT('Ctrl Pts',(-6.22260872941985E-14,90.4624999996486,
12.7882828778556));
#301167=CARTESIAN_POINT('Ctrl Pts',(3.75838203887387,90.612499999648,11.5671105274575));
#301168=CARTESIAN_POINT('Ctrl Pts',(7.5167640777478,90.7624999996474,10.3459381770593));
#301169=CARTESIAN_POINT('Ctrl Pts',(9.83957192047901,90.9124999996468,7.14886745759543));
#301170=CARTESIAN_POINT('Ctrl Pts',(12.1623797632102,91.0624999996462,3.95179673813153));
#301171=CARTESIAN_POINT('Ctrl Pts',(12.1623797632102,91.2124999996456,-1.489461944703E-15));
#301172=CARTESIAN_POINT('Ctrl Pts',(12.1623797632102,91.362499999645,-3.95179673813154));
#301173=CARTESIAN_POINT('Ctrl Pts',(9.83957192047901,91.5124999996444,-7.14886745759543));
#301174=CARTESIAN_POINT('Ctrl Pts',(7.51676407774779,91.6624999996438,-10.3459381770593));
#301175=CARTESIAN_POINT('Ctrl Pts',(3.75838203887386,91.8124999996432,-11.5671105274575));
#301176=CARTESIAN_POINT('Ctrl Pts',(-6.62221678686207E-14,91.9624999996426,
-12.7882828778556));
#301177=CARTESIAN_POINT('Ctrl Pts',(-3.75838203887399,92.112499999642,-11.5671105274575));
#301178=CARTESIAN_POINT('Ctrl Pts',(-7.51676407774792,92.2624999996414,
-10.3459381770593));
#301179=CARTESIAN_POINT('Ctrl Pts',(-9.83957192047914,92.4124999996408,
-7.14886745759543));
#301180=CARTESIAN_POINT('Ctrl Pts',(-12.1623797632104,92.5624999996402,
-3.95179673813153));
#301181=CARTESIAN_POINT('Ctrl Pts',(-12.1623797632104,92.7124999996396,
2.97892388940601E-15));
#301182=CARTESIAN_POINT('Ctrl Pts',(-12.1623797632104,92.862499999639,3.95179673813154));
#301183=CARTESIAN_POINT('Ctrl Pts',(-9.83957192047914,93.0124999996384,
7.14886745759543));
#301184=CARTESIAN_POINT('Ctrl Pts',(-7.51676407774792,93.1624999996378,
10.3459381770593));
#301185=CARTESIAN_POINT('Ctrl Pts',(-3.75838203887399,93.3124999996372,
11.5671105274575));
#301186=CARTESIAN_POINT('Ctrl Pts',(-6.39537965658603E-14,93.4624999996366,
12.7882828778556));
#301187=CARTESIAN_POINT('Ctrl Pts',(3.75838203887386,93.612499999636,11.5671105274575));
#301188=CARTESIAN_POINT('Ctrl Pts',(7.51676407774779,93.7624999996354,10.3459381770593));
#301189=CARTESIAN_POINT('Ctrl Pts',(9.83957192047901,93.9124999996348,7.14886745759543));
#301190=CARTESIAN_POINT('Ctrl Pts',(12.1623797632102,94.0624999996342,3.95179673813153));
#301191=CARTESIAN_POINT('Ctrl Pts',(12.1623797632102,94.2124999996336,-1.489461944703E-15));
#301192=CARTESIAN_POINT('Ctrl Pts',(12.1623797632102,94.362499999633,-3.95179673813154));
#301193=CARTESIAN_POINT('Ctrl Pts',(9.83957192047901,94.5124999996324,-7.14886745759543));
#301194=CARTESIAN_POINT('Ctrl Pts',(7.51676407774779,94.6624999996318,-10.3459381770593));
#301195=CARTESIAN_POINT('Ctrl Pts',(3.75838203887386,94.8124999996312,-11.5671105274575));
#301196=CARTESIAN_POINT('Ctrl Pts',(-6.79498771402825E-14,94.9624999996306,
-12.7882828778556));
#301197=CARTESIAN_POINT('Ctrl Pts',(-3.758382038874,95.11249999963,-11.5671105274575));
#301198=CARTESIAN_POINT('Ctrl Pts',(-7.51676407774792,95.2624999996294,
-10.3459381770593));
#301199=CARTESIAN_POINT('Ctrl Pts',(-9.83957192047914,95.4124999996288,
-7.14886745759543));
#301200=CARTESIAN_POINT('Ctrl Pts',(-12.1623797632104,95.5624999996282,
-3.95179673813153));
#301201=CARTESIAN_POINT('Ctrl Pts',(-12.1623797632104,95.7124999996276,
2.97892388940601E-15));
#301202=CARTESIAN_POINT('Ctrl Pts',(-12.1623797632104,95.862499999627,3.95179673813154));
#301203=CARTESIAN_POINT('Ctrl Pts',(-9.83957192047914,96.0124999996264,
7.14886745759543));
#301204=CARTESIAN_POINT('Ctrl Pts',(-7.51676407774792,96.1624999996258,
10.3459381770593));
#301205=CARTESIAN_POINT('Ctrl Pts',(-3.75838203887399,96.3124999996252,
11.5671105274575));
#301206=CARTESIAN_POINT('Ctrl Pts',(-6.56815058375222E-14,96.4624999996246,
12.7882828778556));
#301207=CARTESIAN_POINT('Ctrl Pts',(3.75838203887386,96.612499999624,11.5671105274575));
#301208=CARTESIAN_POINT('Ctrl Pts',(7.51676407774779,96.7624999996234,10.3459381770593));
#301209=CARTESIAN_POINT('Ctrl Pts',(9.83957192047901,96.9124999996228,7.14886745759543));
#301210=CARTESIAN_POINT('Ctrl Pts',(12.1623797632102,97.0624999996222,3.95179673813153));
#301211=CARTESIAN_POINT('Ctrl Pts',(12.1623797632102,97.2124999996216,-1.489461944703E-15));
#301212=CARTESIAN_POINT('Ctrl Pts',(12.1623797632102,97.3624999996211,-3.95179673813154));
#301213=CARTESIAN_POINT('Ctrl Pts',(9.83957192047901,97.5124999996204,-7.14886745759543));
#301214=CARTESIAN_POINT('Ctrl Pts',(7.51676407774779,97.6624999996198,-10.3459381770593));
#301215=CARTESIAN_POINT('Ctrl Pts',(3.75838203887386,97.8124999996192,-11.5671105274575));
#301216=CARTESIAN_POINT('Ctrl Pts',(-6.96775864119444E-14,97.9624999996187,
-12.7882828778556));
#301217=CARTESIAN_POINT('Ctrl Pts',(-3.758382038874,98.112499999618,-11.5671105274575));
#301218=CARTESIAN_POINT('Ctrl Pts',(-7.51676407774793,98.2624999996174,
-10.3459381770593));
#301219=CARTESIAN_POINT('Ctrl Pts',(-9.83957192047914,98.4124999996168,
-7.14886745759543));
#301220=CARTESIAN_POINT('Ctrl Pts',(-12.1623797632104,98.5624999996162,
-3.95179673813153));
#301221=CARTESIAN_POINT('Ctrl Pts',(-12.1623797632104,98.7124999996156,
2.97892388940601E-15));
#301222=CARTESIAN_POINT('Ctrl Pts',(-12.1623797632104,98.862499999615,3.95179673813154));
#301223=CARTESIAN_POINT('Ctrl Pts',(-9.83957192047914,99.0124999996144,
7.14886745759543));
#301224=CARTESIAN_POINT('Ctrl Pts',(-7.51676407774792,99.1624999996138,
10.3459381770593));
#301225=CARTESIAN_POINT('Ctrl Pts',(-3.758382038874,99.3124999996132,11.5671105274575));
#301226=CARTESIAN_POINT('Ctrl Pts',(-6.7409215109184E-14,99.4624999996126,
12.7882828778556));
#301227=CARTESIAN_POINT('Ctrl Pts',(3.75838203887386,99.612499999612,11.5671105274575));
#301228=CARTESIAN_POINT('Ctrl Pts',(7.51676407774779,99.7624999996114,10.3459381770593));
#301229=CARTESIAN_POINT('Ctrl Pts',(9.83957192047901,99.9124999996108,7.14886745759543));
#301230=CARTESIAN_POINT('Ctrl Pts',(12.1623797632102,100.06249999961,3.95179673813153));
#301231=CARTESIAN_POINT('Ctrl Pts',(12.1623797632102,100.21249999961,-1.489461944703E-15));
#301232=CARTESIAN_POINT('Ctrl Pts',(12.1623797632102,100.362499999609,-3.95179673813154));
#301233=CARTESIAN_POINT('Ctrl Pts',(9.839571920479,100.512499999608,-7.14886745759543));
#301234=CARTESIAN_POINT('Ctrl Pts',(7.51676407774779,100.662499999608,-10.3459381770593));
#301235=CARTESIAN_POINT('Ctrl Pts',(3.75838203887386,100.812499999607,-11.5671105274575));
#301236=CARTESIAN_POINT('Ctrl Pts',(-7.14052956836063E-14,100.962499999607,
-12.7882828778556));
#301237=CARTESIAN_POINT('Ctrl Pts',(-3.758382038874,101.112499999606,-11.5671105274575));
#301238=CARTESIAN_POINT('Ctrl Pts',(-7.51676407774793,101.262499999605,
-10.3459381770593));
#301239=CARTESIAN_POINT('Ctrl Pts',(-9.83957192047915,101.412499999605,
-7.14886745759543));
#301240=CARTESIAN_POINT('Ctrl Pts',(-12.1623797632104,101.562499999604,
-3.95179673813153));
#301241=CARTESIAN_POINT('Ctrl Pts',(-12.1623797632104,101.712499999604,
2.97892388940601E-15));
#301242=CARTESIAN_POINT('Ctrl Pts',(-12.1623797632104,101.862499999603,
3.95179673813154));
#301243=CARTESIAN_POINT('Ctrl Pts',(-9.83957192047914,102.012499999602,
7.14886745759543));
#301244=CARTESIAN_POINT('Ctrl Pts',(-7.51676407774793,102.162499999602,
10.3459381770593));
#301245=CARTESIAN_POINT('Ctrl Pts',(-3.758382038874,102.312499999601,11.5671105274575));
#301246=CARTESIAN_POINT('Ctrl Pts',(-6.91369243808458E-14,102.462499999601,
12.7882828778556));
#301247=CARTESIAN_POINT('Ctrl Pts',(3.75838203887386,102.6124999996,11.5671105274575));
#301248=CARTESIAN_POINT('Ctrl Pts',(7.51676407774779,102.762499999599,10.3459381770593));
#301249=CARTESIAN_POINT('Ctrl Pts',(9.839571920479,102.912499999599,7.14886745759543));
#301250=CARTESIAN_POINT('Ctrl Pts',(12.1623797632102,103.062499999598,3.95179673813153));
#301251=CARTESIAN_POINT('Ctrl Pts',(12.1623797632102,103.212499999598,-1.489461944703E-15));
#301252=CARTESIAN_POINT('Ctrl Pts',(12.1623797632102,103.362499999597,-3.95179673813154));
#301253=CARTESIAN_POINT('Ctrl Pts',(9.839571920479,103.512499999596,-7.14886745759543));
#301254=CARTESIAN_POINT('Ctrl Pts',(7.51676407774779,103.662499999596,-10.3459381770593));
#301255=CARTESIAN_POINT('Ctrl Pts',(3.75838203887386,103.812499999595,-11.5671105274575));
#301256=CARTESIAN_POINT('Ctrl Pts',(-7.31330049552681E-14,103.962499999595,
-12.7882828778556));
#301257=CARTESIAN_POINT('Ctrl Pts',(-3.758382038874,104.112499999594,-11.5671105274575));
#301258=CARTESIAN_POINT('Ctrl Pts',(-7.51676407774793,104.262499999593,
-10.3459381770593));
#301259=CARTESIAN_POINT('Ctrl Pts',(-9.83957192047915,104.412499999593,
-7.14886745759543));
#301260=CARTESIAN_POINT('Ctrl Pts',(-12.1623797632104,104.562499999592,
-3.95179673813153));
#301261=CARTESIAN_POINT('Ctrl Pts',(-12.1623797632104,104.712499999592,
2.97892388940601E-15));
#301262=CARTESIAN_POINT('Ctrl Pts',(-12.1623797632104,104.862499999591,
3.95179673813154));
#301263=CARTESIAN_POINT('Ctrl Pts',(-9.83957192047915,105.01249999959,7.14886745759543));
#301264=CARTESIAN_POINT('Ctrl Pts',(-7.51676407774793,105.16249999959,10.3459381770593));
#301265=CARTESIAN_POINT('Ctrl Pts',(-3.758382038874,105.312499999589,11.5671105274575));
#301266=CARTESIAN_POINT('Ctrl Pts',(-7.08646336525076E-14,105.462499999589,
12.7882828778556));
#301267=CARTESIAN_POINT('Ctrl Pts',(3.75838203887386,105.612499999588,11.5671105274575));
#301268=CARTESIAN_POINT('Ctrl Pts',(7.51676407774779,105.762499999587,10.3459381770593));
#301269=CARTESIAN_POINT('Ctrl Pts',(9.839571920479,105.912499999587,7.14886745759543));
#301270=CARTESIAN_POINT('Ctrl Pts',(12.1623797632102,106.062499999586,3.95179673813153));
#301271=CARTESIAN_POINT('Ctrl Pts',(12.1623797632102,106.212499999586,-1.489461944703E-15));
#301272=CARTESIAN_POINT('Ctrl Pts',(12.1623797632102,106.362499999585,-3.95179673813154));
#301273=CARTESIAN_POINT('Ctrl Pts',(9.839571920479,106.512499999584,-7.14886745759543));
#301274=CARTESIAN_POINT('Ctrl Pts',(7.51676407774778,106.662499999584,-10.3459381770593));
#301275=CARTESIAN_POINT('Ctrl Pts',(3.75838203887385,106.812499999583,-11.5671105274575));
#301276=CARTESIAN_POINT('Ctrl Pts',(-7.48607142269299E-14,106.962499999583,
-12.7882828778556));
#301277=CARTESIAN_POINT('Ctrl Pts',(-3.758382038874,107.112499999582,-11.5671105274575));
#301278=CARTESIAN_POINT('Ctrl Pts',(-7.51676407774793,107.262499999581,
-10.3459381770593));
#301279=CARTESIAN_POINT('Ctrl Pts',(-9.83957192047915,107.412499999581,
-7.14886745759543));
#301280=CARTESIAN_POINT('Ctrl Pts',(-12.1623797632104,107.56249999958,-3.95179673813153));
#301281=CARTESIAN_POINT('Ctrl Pts',(-12.1623797632104,107.71249999958,2.97892388940601E-15));
#301282=CARTESIAN_POINT('Ctrl Pts',(-12.1623797632104,107.862499999579,
3.95179673813154));
#301283=CARTESIAN_POINT('Ctrl Pts',(-9.83957192047915,108.012499999578,
7.14886745759543));
#301284=CARTESIAN_POINT('Ctrl Pts',(-7.51676407774793,108.162499999578,
10.3459381770593));
#301285=CARTESIAN_POINT('Ctrl Pts',(-3.758382038874,108.312499999577,11.5671105274575));
#301286=CARTESIAN_POINT('Ctrl Pts',(-7.25923429241695E-14,108.462499999577,
12.7882828778556));
#301287=CARTESIAN_POINT('Ctrl Pts',(3.75838203887386,108.612499999576,11.5671105274575));
#301288=CARTESIAN_POINT('Ctrl Pts',(7.51676407774779,108.762499999575,10.3459381770593));
#301289=CARTESIAN_POINT('Ctrl Pts',(9.839571920479,108.912499999575,7.14886745759543));
#301290=CARTESIAN_POINT('Ctrl Pts',(12.1623797632102,109.062499999574,3.95179673813153));
#301291=CARTESIAN_POINT('Ctrl Pts',(12.1623797632102,109.212499999574,-1.489461944703E-15));
#301292=CARTESIAN_POINT('Ctrl Pts',(12.1623797632102,109.362499999573,-3.95179673813154));
#301293=CARTESIAN_POINT('Ctrl Pts',(9.839571920479,109.512499999572,-7.14886745759543));
#301294=CARTESIAN_POINT('Ctrl Pts',(7.51676407774778,109.662499999572,-10.3459381770593));
#301295=CARTESIAN_POINT('Ctrl Pts',(3.75838203887385,109.812499999571,-11.5671105274575));
#301296=CARTESIAN_POINT('Ctrl Pts',(-7.65884234985918E-14,109.962499999571,
-12.7882828778556));
#301297=CARTESIAN_POINT('Ctrl Pts',(-3.75838203887401,110.11249999957,-11.5671105274575));
#301298=CARTESIAN_POINT('Ctrl Pts',(-7.51676407774793,110.262499999569,
-10.3459381770593));
#301299=CARTESIAN_POINT('Ctrl Pts',(-9.83957192047915,110.412499999569,
-7.14886745759543));
#301300=CARTESIAN_POINT('Ctrl Pts',(-12.1623797632104,110.562499999568,
-3.95179673813153));
#301301=CARTESIAN_POINT('Ctrl Pts',(-12.1623797632104,110.712499999568,
2.97892388940601E-15));
#301302=CARTESIAN_POINT('Ctrl Pts',(-12.1623797632104,110.862499999567,
3.95179673813154));
#301303=CARTESIAN_POINT('Ctrl Pts',(-9.83957192047915,111.012499999566,
7.14886745759543));
#301304=CARTESIAN_POINT('Ctrl Pts',(-7.51676407774793,111.162499999566,
10.3459381770593));
#301305=CARTESIAN_POINT('Ctrl Pts',(-3.758382038874,111.312499999565,11.5671105274575));
#301306=CARTESIAN_POINT('Ctrl Pts',(-7.43200521958313E-14,111.462499999565,
12.7882828778556));
#301307=CARTESIAN_POINT('Ctrl Pts',(3.75838203887385,111.612499999564,11.5671105274575));
#301308=CARTESIAN_POINT('Ctrl Pts',(7.51676407774778,111.762499999563,10.3459381770593));
#301309=CARTESIAN_POINT('Ctrl Pts',(9.839571920479,111.912499999563,7.14886745759543));
#301310=CARTESIAN_POINT('Ctrl Pts',(12.1623797632102,112.062499999562,3.95179673813153));
#301311=CARTESIAN_POINT('Ctrl Pts',(12.1623797632102,112.212499999562,-1.489461944703E-15));
#301312=CARTESIAN_POINT('Ctrl Pts',(12.1623797632102,112.362499999561,-3.95179673813154));
#301313=CARTESIAN_POINT('Ctrl Pts',(9.839571920479,112.51249999956,-7.14886745759543));
#301314=CARTESIAN_POINT('Ctrl Pts',(7.51676407774778,112.66249999956,-10.3459381770593));
#301315=CARTESIAN_POINT('Ctrl Pts',(3.75838203887385,112.812499999559,-11.5671105274575));
#301316=CARTESIAN_POINT('Ctrl Pts',(-7.83161327702536E-14,112.962499999559,
-12.7882828778556));
#301317=CARTESIAN_POINT('Ctrl Pts',(-3.75838203887401,113.112499999558,
-11.5671105274575));
#301318=CARTESIAN_POINT('Ctrl Pts',(-7.51676407774793,113.262499999557,
-10.3459381770593));
#301319=CARTESIAN_POINT('Ctrl Pts',(-9.83957192047915,113.412499999557,
-7.14886745759543));
#301320=CARTESIAN_POINT('Ctrl Pts',(-12.1623797632104,113.562499999556,
-3.95179673813153));
#301321=CARTESIAN_POINT('Ctrl Pts',(-12.1623797632104,113.712499999556,
2.97892388940601E-15));
#301322=CARTESIAN_POINT('Ctrl Pts',(-12.1623797632104,113.862499999555,
3.95179673813154));
#301323=CARTESIAN_POINT('Ctrl Pts',(-9.83957192047915,114.012499999554,
7.14886745759543));
#301324=CARTESIAN_POINT('Ctrl Pts',(-7.51676407774793,114.162499999554,
10.3459381770593));
#301325=CARTESIAN_POINT('Ctrl Pts',(-3.758382038874,114.312499999553,11.5671105274575));
#301326=CARTESIAN_POINT('Ctrl Pts',(-7.60477614674932E-14,114.462499999553,
12.7882828778556));
#301327=CARTESIAN_POINT('Ctrl Pts',(3.75838203887385,114.612499999552,11.5671105274575));
#301328=CARTESIAN_POINT('Ctrl Pts',(7.51676407774778,114.762499999551,10.3459381770593));
#301329=CARTESIAN_POINT('Ctrl Pts',(9.839571920479,114.912499999551,7.14886745759543));
#301330=CARTESIAN_POINT('Ctrl Pts',(12.1623797632102,115.06249999955,3.95179673813153));
#301331=CARTESIAN_POINT('Ctrl Pts',(12.1623797632102,115.21249999955,-1.489461944703E-15));
#301332=CARTESIAN_POINT('Ctrl Pts',(12.1623797632102,115.362499999549,-3.95179673813154));
#301333=CARTESIAN_POINT('Ctrl Pts',(9.839571920479,115.512499999548,-7.14886745759543));
#301334=CARTESIAN_POINT('Ctrl Pts',(7.51676407774778,115.662499999548,-10.3459381770593));
#301335=CARTESIAN_POINT('Ctrl Pts',(3.75838203887385,115.812499999547,-11.5671105274575));
#301336=CARTESIAN_POINT('Ctrl Pts',(-8.00438420419154E-14,115.962499999547,
-12.7882828778556));
#301337=CARTESIAN_POINT('Ctrl Pts',(-3.75838203887401,116.112499999546,
-11.5671105274575));
#301338=CARTESIAN_POINT('Ctrl Pts',(-7.51676407774794,116.262499999545,
-10.3459381770593));
#301339=CARTESIAN_POINT('Ctrl Pts',(-9.83957192047916,116.412499999545,
-7.14886745759543));
#301340=CARTESIAN_POINT('Ctrl Pts',(-12.1623797632104,116.562499999544,
-3.95179673813153));
#301341=CARTESIAN_POINT('Ctrl Pts',(-12.1623797632104,116.712499999544,
2.97892388940601E-15));
#301342=CARTESIAN_POINT('Ctrl Pts',(-12.1623797632104,116.862499999543,
3.95179673813154));
#301343=CARTESIAN_POINT('Ctrl Pts',(-9.83957192047915,117.012499999542,
7.14886745759543));
#301344=CARTESIAN_POINT('Ctrl Pts',(-7.51676407774793,117.162499999542,
10.3459381770593));
#301345=CARTESIAN_POINT('Ctrl Pts',(-3.75838203887401,117.312499999541,
11.5671105274575));
#301346=CARTESIAN_POINT('Ctrl Pts',(-7.7775470739155E-14,117.462499999541,
12.7882828778556));
#301347=CARTESIAN_POINT('Ctrl Pts',(3.75838203887385,117.61249999954,11.5671105274575));
#301348=CARTESIAN_POINT('Ctrl Pts',(7.51676407774778,117.762499999539,10.3459381770593));
#301349=CARTESIAN_POINT('Ctrl Pts',(9.839571920479,117.912499999539,7.14886745759543));
#301350=CARTESIAN_POINT('Ctrl Pts',(12.1623797632102,118.062499999538,3.95179673813153));
#301351=CARTESIAN_POINT('Ctrl Pts',(12.1623797632102,118.212499999538,-1.489461944703E-15));
#301352=CARTESIAN_POINT('Ctrl Pts',(12.1623797632102,118.362499999537,-3.95179673813154));
#301353=CARTESIAN_POINT('Ctrl Pts',(9.83957192047899,118.512499999536,-7.14886745759543));
#301354=CARTESIAN_POINT('Ctrl Pts',(7.51676407774778,118.662499999536,-10.3459381770593));
#301355=CARTESIAN_POINT('Ctrl Pts',(3.75838203887385,118.812499999535,-11.5671105274575));
#301356=CARTESIAN_POINT('Ctrl Pts',(-8.17715513135773E-14,118.962499999535,
-12.7882828778556));
#301357=CARTESIAN_POINT('Ctrl Pts',(-3.75838203887401,119.112499999534,
-11.5671105274575));
#301358=CARTESIAN_POINT('Ctrl Pts',(-7.51676407774794,119.262499999533,
-10.3459381770593));
#301359=CARTESIAN_POINT('Ctrl Pts',(-9.83957192047916,119.412499999533,
-7.14886745759543));
#301360=CARTESIAN_POINT('Ctrl Pts',(-12.1623797632104,119.562499999532,
-3.95179673813153));
#301361=CARTESIAN_POINT('Ctrl Pts',(-12.1623797632104,119.712499999532,
2.97892388940601E-15));
#301362=CARTESIAN_POINT('Ctrl Pts',(-12.1623797632104,119.862499999531,
3.95179673813154));
#301363=CARTESIAN_POINT('Ctrl Pts',(-9.83957192047916,120.01249999953,7.14886745759543));
#301364=CARTESIAN_POINT('Ctrl Pts',(-7.51676407774794,120.16249999953,10.3459381770593));
#301365=CARTESIAN_POINT('Ctrl Pts',(-3.75838203887401,120.312499999529,
11.5671105274575));
#301366=CARTESIAN_POINT('Ctrl Pts',(-7.95031800108169E-14,120.462499999529,
12.7882828778556));
#301367=CARTESIAN_POINT('Ctrl Pts',(3.75838203887385,120.612499999528,11.5671105274575));
#301368=CARTESIAN_POINT('Ctrl Pts',(7.51676407774778,120.762499999527,10.3459381770593));
#301369=CARTESIAN_POINT('Ctrl Pts',(9.83957192047899,120.912499999527,7.14886745759543));
#301370=CARTESIAN_POINT('Ctrl Pts',(12.1623797632102,121.062499999526,3.95179673813153));
#301371=CARTESIAN_POINT('Ctrl Pts',(12.1623797632102,121.212499999526,-1.489461944703E-15));
#301372=CARTESIAN_POINT('Ctrl Pts',(12.1623797632102,121.362499999525,-3.95179673813154));
#301373=CARTESIAN_POINT('Ctrl Pts',(9.83957192047899,121.512499999524,-7.14886745759543));
#301374=CARTESIAN_POINT('Ctrl Pts',(7.51676407774777,121.662499999524,-10.3459381770593));
#301375=CARTESIAN_POINT('Ctrl Pts',(3.75838203887385,121.812499999523,-11.5671105274575));
#301376=CARTESIAN_POINT('Ctrl Pts',(-8.34992605852391E-14,121.962499999523,
-12.7882828778556));
#301377=CARTESIAN_POINT('Ctrl Pts',(-3.75838203887401,122.112499999522,
-11.5671105274575));
#301378=CARTESIAN_POINT('Ctrl Pts',(-7.51676407774794,122.262499999521,
-10.3459381770593));
#301379=CARTESIAN_POINT('Ctrl Pts',(-9.83957192047916,122.412499999521,
-7.14886745759543));
#301380=CARTESIAN_POINT('Ctrl Pts',(-12.1623797632104,122.56249999952,-3.95179673813153));
#301381=CARTESIAN_POINT('Ctrl Pts',(-12.1623797632104,122.71249999952,2.97892388940601E-15));
#301382=CARTESIAN_POINT('Ctrl Pts',(-12.1623797632104,122.862499999519,
3.95179673813154));
#301383=CARTESIAN_POINT('Ctrl Pts',(-9.83957192047916,123.012499999518,
7.14886745759543));
#301384=CARTESIAN_POINT('Ctrl Pts',(-7.51676407774794,123.162499999518,
10.3459381770593));
#301385=CARTESIAN_POINT('Ctrl Pts',(-3.75838203887401,123.312499999517,
11.5671105274575));
#301386=CARTESIAN_POINT('Ctrl Pts',(-8.12308892824787E-14,123.462499999517,
12.7882828778556));
#301387=CARTESIAN_POINT('Ctrl Pts',(3.75838203887385,123.612499999516,11.5671105274575));
#301388=CARTESIAN_POINT('Ctrl Pts',(7.51676407774778,123.762499999515,10.3459381770593));
#301389=CARTESIAN_POINT('Ctrl Pts',(9.83957192047899,123.912499999515,7.14886745759543));
#301390=CARTESIAN_POINT('Ctrl Pts',(12.1623797632102,124.062499999514,3.95179673813153));
#301391=CARTESIAN_POINT('Ctrl Pts',(12.1623797632102,124.212499999514,-1.489461944703E-15));
#301392=CARTESIAN_POINT('Ctrl Pts',(12.1623797632102,124.362499999513,-3.95179673813154));
#301393=CARTESIAN_POINT('Ctrl Pts',(9.83957192047899,124.512499999512,-7.14886745759543));
#301394=CARTESIAN_POINT('Ctrl Pts',(7.51676407774777,124.662499999512,-10.3459381770593));
#301395=CARTESIAN_POINT('Ctrl Pts',(3.75838203887384,124.812499999511,-11.5671105274575));
#301396=CARTESIAN_POINT('Ctrl Pts',(-8.52269698569009E-14,124.962499999511,
-12.7882828778556));
#301397=CARTESIAN_POINT('Ctrl Pts',(-3.75838203887401,125.11249999951,-11.5671105274575));
#301398=CARTESIAN_POINT('Ctrl Pts',(-7.51676407774794,125.262499999509,
-10.3459381770593));
#301399=CARTESIAN_POINT('Ctrl Pts',(-9.83957192047916,125.412499999509,
-7.14886745759543));
#301400=CARTESIAN_POINT('Ctrl Pts',(-12.1623797632104,125.562499999508,
-3.95179673813153));
#301401=CARTESIAN_POINT('Ctrl Pts',(-12.1623797632104,125.712499999508,
2.97892388940601E-15));
#301402=CARTESIAN_POINT('Ctrl Pts',(-12.1623797632104,125.862499999507,
3.95179673813154));
#301403=CARTESIAN_POINT('Ctrl Pts',(-9.83957192047916,126.012499999506,
7.14886745759543));
#301404=CARTESIAN_POINT('Ctrl Pts',(-7.51676407774794,126.162499999506,
10.3459381770593));
#301405=CARTESIAN_POINT('Ctrl Pts',(-3.75838203887401,126.312499999505,
11.5671105274575));
#301406=CARTESIAN_POINT('Ctrl Pts',(-8.29585985541405E-14,126.462499999505,
12.7882828778556));
#301407=CARTESIAN_POINT('Ctrl Pts',(3.75838203887385,126.612499999504,11.5671105274575));
#301408=CARTESIAN_POINT('Ctrl Pts',(7.51676407774777,126.762499999503,10.3459381770593));
#301409=CARTESIAN_POINT('Ctrl Pts',(9.83957192047899,126.912499999503,7.14886745759543));
#301410=CARTESIAN_POINT('Ctrl Pts',(12.1623797632102,127.062499999502,3.95179673813153));
#301411=CARTESIAN_POINT('Ctrl Pts',(12.1623797632102,127.212499999502,-1.489461944703E-15));
#301412=CARTESIAN_POINT('Ctrl Pts',(12.1623797632102,127.362499999501,-3.95179673813154));
#301413=CARTESIAN_POINT('Ctrl Pts',(9.83957192047899,127.5124999995,-7.14886745759543));
#301414=CARTESIAN_POINT('Ctrl Pts',(7.51676407774777,127.6624999995,-10.3459381770593));
#301415=CARTESIAN_POINT('Ctrl Pts',(3.75838203887384,127.812499999499,-11.5671105274575));
#301416=CARTESIAN_POINT('Ctrl Pts',(-8.69546791285628E-14,127.962499999499,
-12.7882828778556));
#301417=CARTESIAN_POINT('Ctrl Pts',(-3.75838203887402,128.112499999498,
-11.5671105274575));
#301418=CARTESIAN_POINT('Ctrl Pts',(-7.51676407774795,128.262499999497,
-10.3459381770593));
#301419=CARTESIAN_POINT('Ctrl Pts',(-9.83957192047916,128.412499999497,
-7.14886745759543));
#301420=CARTESIAN_POINT('Ctrl Pts',(-12.1623797632104,128.562499999496,
-3.95179673813153));
#301421=CARTESIAN_POINT('Ctrl Pts',(-12.1623797632104,128.712499999496,
2.97892388940601E-15));
#301422=CARTESIAN_POINT('Ctrl Pts',(-12.1623797632104,128.862499999495,
3.95179673813154));
#301423=CARTESIAN_POINT('Ctrl Pts',(-9.83957192047916,129.012499999494,
7.14886745759543));
#301424=CARTESIAN_POINT('Ctrl Pts',(-7.51676407774794,129.162499999494,
10.3459381770593));
#301425=CARTESIAN_POINT('Ctrl Pts',(-3.75838203887401,129.312499999493,
11.5671105274575));
#301426=CARTESIAN_POINT('Ctrl Pts',(-8.46863078258024E-14,129.462499999493,
12.7882828778556));
#301427=CARTESIAN_POINT('Ctrl Pts',(3.75838203887384,129.612499999492,11.5671105274575));
#301428=CARTESIAN_POINT('Ctrl Pts',(7.51676407774777,129.762499999491,10.3459381770593));
#301429=CARTESIAN_POINT('Ctrl Pts',(9.83957192047899,129.912499999491,7.14886745759543));
#301430=CARTESIAN_POINT('Ctrl Pts',(12.1623797632102,130.06249999949,3.95179673813153));
#301431=CARTESIAN_POINT('Ctrl Pts',(12.1623797632102,130.21249999949,-1.489461944703E-15));
#301432=CARTESIAN_POINT('Ctrl Pts',(12.1623797632102,130.362499999489,-3.95179673813154));
#301433=CARTESIAN_POINT('Ctrl Pts',(9.83957192047899,130.512499999488,-7.14886745759543));
#301434=CARTESIAN_POINT('Ctrl Pts',(7.51676407774777,130.662499999488,-10.3459381770593));
#301435=CARTESIAN_POINT('Ctrl Pts',(3.75838203887384,130.812499999487,-11.5671105274575));
#301436=CARTESIAN_POINT('Ctrl Pts',(-8.86823884002247E-14,130.962499999487,
-12.7882828778556));
#301437=CARTESIAN_POINT('Ctrl Pts',(-3.75838203887402,131.112499999486,
-11.5671105274575));
#301438=CARTESIAN_POINT('Ctrl Pts',(-7.51676407774795,131.262499999485,
-10.3459381770593));
#301439=CARTESIAN_POINT('Ctrl Pts',(-9.83957192047916,131.412499999485,
-7.14886745759543));
#301440=CARTESIAN_POINT('Ctrl Pts',(-12.1623797632104,131.562499999484,
-3.95179673813153));
#301441=CARTESIAN_POINT('Ctrl Pts',(-12.1623797632104,131.712499999484,
2.97892388940601E-15));
#301442=CARTESIAN_POINT('Ctrl Pts',(-12.1623797632104,131.862499999483,
3.95179673813154));
#301443=CARTESIAN_POINT('Ctrl Pts',(-9.83957192047916,132.012499999482,
7.14886745759543));
#301444=CARTESIAN_POINT('Ctrl Pts',(-7.51676407774795,132.162499999482,
10.3459381770593));
#301445=CARTESIAN_POINT('Ctrl Pts',(-3.75838203887402,132.312499999481,
11.5671105274575));
#301446=CARTESIAN_POINT('Ctrl Pts',(-8.64140170974642E-14,132.462499999481,
12.7882828778556));
#301447=CARTESIAN_POINT('Ctrl Pts',(3.75838203887384,132.61249999948,11.5671105274575));
#301448=CARTESIAN_POINT('Ctrl Pts',(7.51676407774777,132.762499999479,10.3459381770593));
#301449=CARTESIAN_POINT('Ctrl Pts',(9.83957192047899,132.912499999479,7.14886745759543));
#301450=CARTESIAN_POINT('Ctrl Pts',(12.1623797632102,133.062499999478,3.95179673813153));
#301451=CARTESIAN_POINT('Ctrl Pts',(12.1623797632102,133.212499999478,-1.489461944703E-15));
#301452=CARTESIAN_POINT('Ctrl Pts',(12.1623797632102,133.362499999477,-3.95179673813154));
#301453=CARTESIAN_POINT('Ctrl Pts',(9.83957192047898,133.512499999476,-7.14886745759543));
#301454=CARTESIAN_POINT('Ctrl Pts',(7.51676407774777,133.662499999476,-10.3459381770593));
#301455=CARTESIAN_POINT('Ctrl Pts',(3.75838203887384,133.812499999475,-11.5671105274575));
#301456=CARTESIAN_POINT('Ctrl Pts',(-9.04100976718865E-14,133.962499999475,
-12.7882828778556));
#301457=CARTESIAN_POINT('Ctrl Pts',(-3.75838203887402,134.112499999474,
-11.5671105274575));
#301458=CARTESIAN_POINT('Ctrl Pts',(-7.51676407774795,134.262499999473,
-10.3459381770593));
#301459=CARTESIAN_POINT('Ctrl Pts',(-9.83957192047917,134.412499999473,
-7.14886745759543));
#301460=CARTESIAN_POINT('Ctrl Pts',(-12.1623797632104,134.562499999472,
-3.95179673813153));
#301461=CARTESIAN_POINT('Ctrl Pts',(-12.1623797632104,134.712499999472,
2.97892388940601E-15));
#301462=CARTESIAN_POINT('Ctrl Pts',(-12.1623797632104,134.862499999471,
3.95179673813154));
#301463=CARTESIAN_POINT('Ctrl Pts',(-9.83957192047916,135.01249999947,7.14886745759543));
#301464=CARTESIAN_POINT('Ctrl Pts',(-7.51676407774795,135.16249999947,10.3459381770593));
#301465=CARTESIAN_POINT('Ctrl Pts',(-3.75838203887402,135.312499999469,
11.5671105274575));
#301466=CARTESIAN_POINT('Ctrl Pts',(-8.8141726369126E-14,135.462499999469,
12.7882828778556));
#301467=CARTESIAN_POINT('Ctrl Pts',(3.75838203887384,135.612499999468,11.5671105274575));
#301468=CARTESIAN_POINT('Ctrl Pts',(7.51676407774777,135.762499999467,10.3459381770593));
#301469=CARTESIAN_POINT('Ctrl Pts',(9.83957192047898,135.912499999467,7.14886745759543));
#301470=CARTESIAN_POINT('Ctrl Pts',(12.1623797632102,136.062499999466,3.95179673813153));
#301471=CARTESIAN_POINT('Ctrl Pts',(12.1623797632102,136.212499999466,-1.489461944703E-15));
#301472=CARTESIAN_POINT('Ctrl Pts',(12.1623797632102,136.362499999465,-3.95179673813154));
#301473=CARTESIAN_POINT('Ctrl Pts',(9.83957192047898,136.512499999464,-7.14886745759543));
#301474=CARTESIAN_POINT('Ctrl Pts',(7.51676407774777,136.662499999464,-10.3459381770593));
#301475=CARTESIAN_POINT('Ctrl Pts',(3.75838203887384,136.812499999463,-11.5671105274575));
#301476=CARTESIAN_POINT('Ctrl Pts',(-9.21378069435483E-14,136.962499999463,
-12.7882828778556));
#301477=CARTESIAN_POINT('Ctrl Pts',(-3.75838203887402,137.112499999462,
-11.5671105274575));
#301478=CARTESIAN_POINT('Ctrl Pts',(-7.51676407774795,137.262499999461,
-10.3459381770593));
#301479=CARTESIAN_POINT('Ctrl Pts',(-9.83957192047917,137.412499999461,
-7.14886745759543));
#301480=CARTESIAN_POINT('Ctrl Pts',(-12.1623797632104,137.56249999946,-3.95179673813153));
#301481=CARTESIAN_POINT('Ctrl Pts',(-12.1623797632104,137.71249999946,2.97892388940601E-15));
#301482=CARTESIAN_POINT('Ctrl Pts',(-12.1623797632104,137.862499999459,
3.95179673813154));
#301483=CARTESIAN_POINT('Ctrl Pts',(-9.83957192047917,138.012499999458,
7.14886745759543));
#301484=CARTESIAN_POINT('Ctrl Pts',(-7.51676407774795,138.162499999458,
10.3459381770593));
#301485=CARTESIAN_POINT('Ctrl Pts',(-3.75838203887402,138.312499999457,
11.5671105274575));
#301486=CARTESIAN_POINT('Ctrl Pts',(-8.98694356407879E-14,138.462499999457,
12.7882828778556));
#301487=CARTESIAN_POINT('Ctrl Pts',(3.75838203887384,138.612499999456,11.5671105274575));
#301488=CARTESIAN_POINT('Ctrl Pts',(7.51676407774777,138.762499999455,10.3459381770593));
#301489=CARTESIAN_POINT('Ctrl Pts',(9.83957192047898,138.912499999455,7.14886745759543));
#301490=CARTESIAN_POINT('Ctrl Pts',(12.1623797632102,139.062499999454,3.95179673813153));
#301491=CARTESIAN_POINT('Ctrl Pts',(12.1623797632102,139.212499999454,-1.489461944703E-15));
#301492=CARTESIAN_POINT('Ctrl Pts',(12.1623797632102,139.362499999453,-3.95179673813154));
#301493=CARTESIAN_POINT('Ctrl Pts',(9.83957192047898,139.512499999452,-7.14886745759543));
#301494=CARTESIAN_POINT('Ctrl Pts',(7.51676407774776,139.662499999452,-10.3459381770593));
#301495=CARTESIAN_POINT('Ctrl Pts',(3.75838203887384,139.812499999451,-11.5671105274575));
#301496=CARTESIAN_POINT('Ctrl Pts',(-9.38655162152102E-14,139.962499999451,
-12.7882828778556));
#301497=CARTESIAN_POINT('Ctrl Pts',(-3.75838203887402,140.11249999945,-11.5671105274575));
#301498=CARTESIAN_POINT('Ctrl Pts',(-7.51676407774795,140.262499999449,
-10.3459381770593));
#301499=CARTESIAN_POINT('Ctrl Pts',(-9.83957192047917,140.412499999449,
-7.14886745759543));
#301500=CARTESIAN_POINT('Ctrl Pts',(-12.1623797632104,140.562499999448,
-3.95179673813153));
#301501=CARTESIAN_POINT('Ctrl Pts',(-12.1623797632104,140.712499999448,
2.97892388940601E-15));
#301502=CARTESIAN_POINT('Ctrl Pts',(-12.1623797632104,140.862499999447,
3.95179673813154));
#301503=CARTESIAN_POINT('Ctrl Pts',(-9.83957192047917,141.012499999446,
7.14886745759543));
#301504=CARTESIAN_POINT('Ctrl Pts',(-7.51676407774795,141.162499999446,
10.3459381770593));
#301505=CARTESIAN_POINT('Ctrl Pts',(-3.75838203887402,141.312499999445,
11.5671105274575));
#301506=CARTESIAN_POINT('Ctrl Pts',(-9.15971449124498E-14,141.462499999445,
12.7882828778556));
#301507=CARTESIAN_POINT('Ctrl Pts',(3.75838203887384,141.612499999444,11.5671105274575));
#301508=CARTESIAN_POINT('Ctrl Pts',(7.51676407774777,141.762499999443,10.3459381770593));
#301509=CARTESIAN_POINT('Ctrl Pts',(9.83957192047898,141.912499999443,7.14886745759543));
#301510=CARTESIAN_POINT('Ctrl Pts',(12.1623797632102,142.062499999442,3.95179673813153));
#301511=CARTESIAN_POINT('Ctrl Pts',(12.1623797632102,142.212499999442,-1.489461944703E-15));
#301512=CARTESIAN_POINT('Ctrl Pts',(12.1623797632102,142.362499999441,-3.95179673813154));
#301513=CARTESIAN_POINT('Ctrl Pts',(9.83957192047898,142.51249999944,-7.14886745759543));
#301514=CARTESIAN_POINT('Ctrl Pts',(7.51676407774776,142.66249999944,-10.3459381770593));
#301515=CARTESIAN_POINT('Ctrl Pts',(3.75838203887383,142.812499999439,-11.5671105274575));
#301516=CARTESIAN_POINT('Ctrl Pts',(-9.5593225486872E-14,142.962499999439,
-12.7882828778556));
#301517=CARTESIAN_POINT('Ctrl Pts',(-3.75838203887402,143.112499999438,
-11.5671105274575));
#301518=CARTESIAN_POINT('Ctrl Pts',(-7.51676407774795,143.262499999437,
-10.3459381770593));
#301519=CARTESIAN_POINT('Ctrl Pts',(-9.83957192047917,143.412499999437,
-7.14886745759543));
#301520=CARTESIAN_POINT('Ctrl Pts',(-12.1623797632104,143.562499999436,
-3.95179673813153));
#301521=CARTESIAN_POINT('Ctrl Pts',(-12.1623797632104,143.712499999436,
2.97892388940601E-15));
#301522=CARTESIAN_POINT('Ctrl Pts',(-12.1623797632104,143.862499999435,
3.95179673813154));
#301523=CARTESIAN_POINT('Ctrl Pts',(-9.83957192047917,144.012499999434,
7.14886745759543));
#301524=CARTESIAN_POINT('Ctrl Pts',(-7.51676407774795,144.162499999434,
10.3459381770593));
#301525=CARTESIAN_POINT('Ctrl Pts',(-3.75838203887402,144.312499999433,
11.5671105274575));
#301526=CARTESIAN_POINT('Ctrl Pts',(-9.33248541841116E-14,144.462499999433,
12.7882828778556));
#301527=CARTESIAN_POINT('Ctrl Pts',(3.75838203887384,144.612499999432,11.5671105274575));
#301528=CARTESIAN_POINT('Ctrl Pts',(7.51676407774776,144.762499999431,10.3459381770593));
#301529=CARTESIAN_POINT('Ctrl Pts',(9.83957192047898,144.912499999431,7.14886745759543));
#301530=CARTESIAN_POINT('Ctrl Pts',(12.1623797632102,145.06249999943,3.95179673813153));
#301531=CARTESIAN_POINT('Ctrl Pts',(12.1623797632102,145.21249999943,-1.489461944703E-15));
#301532=CARTESIAN_POINT('Ctrl Pts',(12.1623797632102,145.362499999429,-3.95179673813154));
#301533=CARTESIAN_POINT('Ctrl Pts',(9.83957192047898,145.512499999428,-7.14886745759543));
#301534=CARTESIAN_POINT('Ctrl Pts',(7.51676407774776,145.662499999428,-10.3459381770593));
#301535=CARTESIAN_POINT('Ctrl Pts',(3.75838203887383,145.812499999427,-11.5671105274575));
#301536=CARTESIAN_POINT('Ctrl Pts',(-9.73209347585338E-14,145.962499999427,
-12.7882828778556));
#301537=CARTESIAN_POINT('Ctrl Pts',(-3.75838203887403,146.112499999426,
-11.5671105274575));
#301538=CARTESIAN_POINT('Ctrl Pts',(-7.51676407774795,146.262499999425,
-10.3459381770593));
#301539=CARTESIAN_POINT('Ctrl Pts',(-9.83957192047917,146.412499999425,
-7.14886745759543));
#301540=CARTESIAN_POINT('Ctrl Pts',(-12.1623797632104,146.562499999424,
-3.95179673813153));
#301541=CARTESIAN_POINT('Ctrl Pts',(-12.1623797632104,146.712499999424,
2.97892388940601E-15));
#301542=CARTESIAN_POINT('Ctrl Pts',(-12.1623797632104,146.862499999423,
3.95179673813154));
#301543=CARTESIAN_POINT('Ctrl Pts',(-9.83957192047917,147.012499999422,
7.14886745759543));
#301544=CARTESIAN_POINT('Ctrl Pts',(-7.51676407774795,147.162499999422,
10.3459381770593));
#301545=CARTESIAN_POINT('Ctrl Pts',(-3.75838203887402,147.312499999421,
11.5671105274575));
#301546=CARTESIAN_POINT('Ctrl Pts',(-9.50525634557734E-14,147.462499999421,
12.7882828778556));
#301547=CARTESIAN_POINT('Ctrl Pts',(3.75838203887383,147.61249999942,11.5671105274575));
#301548=CARTESIAN_POINT('Ctrl Pts',(7.51676407774776,147.762499999419,10.3459381770593));
#301549=CARTESIAN_POINT('Ctrl Pts',(9.83957192047898,147.912499999419,7.14886745759543));
#301550=CARTESIAN_POINT('Ctrl Pts',(12.1623797632102,148.062499999418,3.95179673813153));
#301551=CARTESIAN_POINT('Ctrl Pts',(12.1623797632102,148.212499999418,-1.489461944703E-15));
#301552=CARTESIAN_POINT('Ctrl Pts',(12.1623797632102,148.362499999417,-3.95179673813154));
#301553=CARTESIAN_POINT('Ctrl Pts',(9.83957192047898,148.512499999416,-7.14886745759543));
#301554=CARTESIAN_POINT('Ctrl Pts',(7.51676407774776,148.662499999416,-10.3459381770593));
#301555=CARTESIAN_POINT('Ctrl Pts',(3.75838203887383,148.812499999415,-11.5671105274575));
#301556=CARTESIAN_POINT('Ctrl Pts',(-9.90486440301957E-14,148.962499999415,
-12.7882828778556));
#301557=CARTESIAN_POINT('Ctrl Pts',(-3.75838203887403,149.112499999414,
-11.5671105274575));
#301558=CARTESIAN_POINT('Ctrl Pts',(-7.51676407774795,149.262499999413,
-10.3459381770593));
#301559=CARTESIAN_POINT('Ctrl Pts',(-9.83957192047917,149.412499999413,
-7.14886745759543));
#301560=CARTESIAN_POINT('Ctrl Pts',(-12.1623797632104,149.562499999412,
-3.95179673813153));
#301561=CARTESIAN_POINT('Ctrl Pts',(-12.1623797632104,149.712499999412,
2.97892388940601E-15));
#301562=CARTESIAN_POINT('Ctrl Pts',(-12.1623797632104,149.862499999411,
3.95179673813154));
#301563=CARTESIAN_POINT('Ctrl Pts',(-9.83957192047917,150.01249999941,7.14886745759543));
#301564=CARTESIAN_POINT('Ctrl Pts',(-7.51676407774795,150.16249999941,10.3459381770593));
#301565=CARTESIAN_POINT('Ctrl Pts',(-3.75838203887403,150.312499999409,
11.5671105274575));
#301566=CARTESIAN_POINT('Ctrl Pts',(-9.67802727274353E-14,150.462499999409,
12.7882828778556));
#301567=CARTESIAN_POINT('Ctrl Pts',(3.75838203887383,150.612499999408,11.5671105274575));
#301568=CARTESIAN_POINT('Ctrl Pts',(7.51676407774776,150.762499999407,10.3459381770593));
#301569=CARTESIAN_POINT('Ctrl Pts',(9.83957192047898,150.912499999407,7.14886745759543));
#301570=CARTESIAN_POINT('Ctrl Pts',(12.1623797632102,151.062499999406,3.95179673813153));
#301571=CARTESIAN_POINT('Ctrl Pts',(12.1623797632102,151.212499999406,-1.489461944703E-15));
#301572=CARTESIAN_POINT('Ctrl Pts',(12.1623797632102,151.362499999405,-3.95179673813154));
#301573=CARTESIAN_POINT('Ctrl Pts',(9.83957192047897,151.512499999404,-7.14886745759543));
#301574=CARTESIAN_POINT('Ctrl Pts',(7.51676407774776,151.662499999404,-10.3459381770593));
#301575=CARTESIAN_POINT('Ctrl Pts',(3.75838203887383,151.812499999403,-11.5671105274575));
#301576=CARTESIAN_POINT('Ctrl Pts',(-1.00776353301858E-13,151.962499999403,
-12.7882828778556));
#301577=CARTESIAN_POINT('Ctrl Pts',(-3.75838203887403,152.112499999402,
-11.5671105274575));
#301578=CARTESIAN_POINT('Ctrl Pts',(-10.0514428414942,-2.06874999998125,
2.46189346052968E-15));
#301579=CARTESIAN_POINT('Ctrl Pts',(-10.0514428414942,-1.91874999998185,
3.26591175476071));
#301580=CARTESIAN_POINT('Ctrl Pts',(-8.1317880767572,-1.76874999998245,
5.90808986649102));
#301581=CARTESIAN_POINT('Ctrl Pts',(-6.21213331202023,-1.61874999998305,
8.55026797822134));
#301582=CARTESIAN_POINT('Ctrl Pts',(-3.10606665601012,-1.46874999998365,
9.5594902125713));
#301583=CARTESIAN_POINT('Ctrl Pts',(-9.77671023785295E-15,-1.31874999998425,
10.5687124469213));
#301584=CARTESIAN_POINT('Ctrl Pts',(3.1060666560101,-1.16874999998485,9.5594902125713));
#301585=CARTESIAN_POINT('Ctrl Pts',(6.21213331202021,-1.01874999998544,
8.55026797822134));
#301586=CARTESIAN_POINT('Ctrl Pts',(8.13178807675718,-0.868749999986043,
5.90808986649102));
#301587=CARTESIAN_POINT('Ctrl Pts',(10.0514428414942,-0.718749999986641,
3.2659117547607));
#301588=CARTESIAN_POINT('Ctrl Pts',(10.0514428414942,-0.568749999987242,
-1.23094673026484E-15));
#301589=CARTESIAN_POINT('Ctrl Pts',(10.0514428414942,-0.418749999987842,
-3.26591175476071));
#301590=CARTESIAN_POINT('Ctrl Pts',(8.13178807675718,-0.268749999988443,
-5.90808986649102));
#301591=CARTESIAN_POINT('Ctrl Pts',(6.2121333120202,-0.118749999989044,
-8.55026797822134));
#301592=CARTESIAN_POINT('Ctrl Pts',(3.10606665601009,0.0312500000103543,
-9.5594902125713));
#301593=CARTESIAN_POINT('Ctrl Pts',(-1.322915284753E-14,0.181250000009752,
-10.5687124469213));
#301594=CARTESIAN_POINT('Ctrl Pts',(-3.10606665601012,0.331250000009151,
-9.5594902125713));
#301595=CARTESIAN_POINT('Ctrl Pts',(-6.21213331202023,0.481250000008549,
-8.55026797822134));
#301596=CARTESIAN_POINT('Ctrl Pts',(-8.1317880767572,0.631250000007948,
-5.90808986649102));
#301597=CARTESIAN_POINT('Ctrl Pts',(-10.0514428414942,0.781250000007346,
-3.2659117547607));
#301598=CARTESIAN_POINT('Ctrl Pts',(-10.0514428414942,0.931250000006746,
2.46189346052968E-15));
#301599=CARTESIAN_POINT('Ctrl Pts',(-10.0514428414942,1.08125000000615,
3.26591175476071));
#301600=CARTESIAN_POINT('Ctrl Pts',(-8.1317880767572,1.23125000000555,5.90808986649102));
#301601=CARTESIAN_POINT('Ctrl Pts',(-6.21213331202023,1.38125000000495,
8.55026797822134));
#301602=CARTESIAN_POINT('Ctrl Pts',(-3.10606665601012,1.53125000000435,
9.5594902125713));
#301603=CARTESIAN_POINT('Ctrl Pts',(-1.15044195095148E-14,1.68125000000375,
10.5687124469213));
#301604=CARTESIAN_POINT('Ctrl Pts',(3.1060666560101,1.83125000000315,9.5594902125713));
#301605=CARTESIAN_POINT('Ctrl Pts',(6.2121333120202,1.98125000000256,8.55026797822134));
#301606=CARTESIAN_POINT('Ctrl Pts',(8.13178807675718,2.13125000000196,5.90808986649102));
#301607=CARTESIAN_POINT('Ctrl Pts',(10.0514428414942,2.28125000000136,3.2659117547607));
#301608=CARTESIAN_POINT('Ctrl Pts',(10.0514428414942,2.43125000000076,-1.23094673026484E-15));
#301609=CARTESIAN_POINT('Ctrl Pts',(10.0514428414942,2.58125000000016,-3.26591175476071));
#301610=CARTESIAN_POINT('Ctrl Pts',(8.13178807675718,2.73124999999956,-5.90808986649102));
#301611=CARTESIAN_POINT('Ctrl Pts',(6.2121333120202,2.88124999999896,-8.55026797822134));
#301612=CARTESIAN_POINT('Ctrl Pts',(3.10606665601009,3.03124999999835,-9.5594902125713));
#301613=CARTESIAN_POINT('Ctrl Pts',(-1.49568621191919E-14,3.18124999999775,
-10.5687124469213));
#301614=CARTESIAN_POINT('Ctrl Pts',(-3.10606665601012,3.33124999999715,
-9.5594902125713));
#301615=CARTESIAN_POINT('Ctrl Pts',(-6.21213331202023,3.48124999999655,
-8.55026797822134));
#301616=CARTESIAN_POINT('Ctrl Pts',(-8.13178807675721,3.63124999999595,
-5.90808986649102));
#301617=CARTESIAN_POINT('Ctrl Pts',(-10.0514428414942,3.78124999999535,
-3.2659117547607));
#301618=CARTESIAN_POINT('Ctrl Pts',(-10.0514428414942,3.93124999999475,
2.46189346052968E-15));
#301619=CARTESIAN_POINT('Ctrl Pts',(-10.0514428414942,4.08124999999415,
3.26591175476071));
#301620=CARTESIAN_POINT('Ctrl Pts',(-8.13178807675721,4.23124999999355,
5.90808986649102));
#301621=CARTESIAN_POINT('Ctrl Pts',(-6.21213331202023,4.38124999999295,
8.55026797822134));
#301622=CARTESIAN_POINT('Ctrl Pts',(-3.10606665601012,4.53124999999235,
9.5594902125713));
#301623=CARTESIAN_POINT('Ctrl Pts',(-1.32321287811766E-14,4.68124999999175,
10.5687124469213));
#301624=CARTESIAN_POINT('Ctrl Pts',(3.10606665601009,4.83124999999115,9.5594902125713));
#301625=CARTESIAN_POINT('Ctrl Pts',(6.2121333120202,4.98124999999055,8.55026797822134));
#301626=CARTESIAN_POINT('Ctrl Pts',(8.13178807675718,5.13124999998996,5.90808986649102));
#301627=CARTESIAN_POINT('Ctrl Pts',(10.0514428414942,5.28124999998936,3.2659117547607));
#301628=CARTESIAN_POINT('Ctrl Pts',(10.0514428414941,5.43124999998876,-1.23094673026484E-15));
#301629=CARTESIAN_POINT('Ctrl Pts',(10.0514428414941,5.58124999998816,-3.26591175476071));
#301630=CARTESIAN_POINT('Ctrl Pts',(8.13178807675717,5.73124999998756,-5.90808986649102));
#301631=CARTESIAN_POINT('Ctrl Pts',(6.2121333120202,5.88124999998695,-8.55026797822134));
#301632=CARTESIAN_POINT('Ctrl Pts',(3.10606665601009,6.03124999998635,-9.5594902125713));
#301633=CARTESIAN_POINT('Ctrl Pts',(-1.66845713908537E-14,6.18124999998575,
-10.5687124469213));
#301634=CARTESIAN_POINT('Ctrl Pts',(-3.10606665601012,6.33124999998515,
-9.5594902125713));
#301635=CARTESIAN_POINT('Ctrl Pts',(-6.21213331202023,6.48124999998455,
-8.55026797822134));
#301636=CARTESIAN_POINT('Ctrl Pts',(-8.13178807675721,6.63124999998395,
-5.90808986649102));
#301637=CARTESIAN_POINT('Ctrl Pts',(-10.0514428414942,6.78124999998335,
-3.2659117547607));
#301638=CARTESIAN_POINT('Ctrl Pts',(-10.0514428414942,6.93124999998275,
2.46189346052968E-15));
#301639=CARTESIAN_POINT('Ctrl Pts',(-10.0514428414942,7.08124999998215,
3.26591175476071));
#301640=CARTESIAN_POINT('Ctrl Pts',(-8.13178807675721,7.23124999998155,
5.90808986649102));
#301641=CARTESIAN_POINT('Ctrl Pts',(-6.21213331202023,7.38124999998095,
8.55026797822134));
#301642=CARTESIAN_POINT('Ctrl Pts',(-3.10606665601012,7.53124999998035,
9.5594902125713));
#301643=CARTESIAN_POINT('Ctrl Pts',(-1.49598380528385E-14,7.68124999997975,
10.5687124469213));
#301644=CARTESIAN_POINT('Ctrl Pts',(3.10606665601009,7.83124999997915,9.5594902125713));
#301645=CARTESIAN_POINT('Ctrl Pts',(6.2121333120202,7.98124999997856,8.55026797822134));
#301646=CARTESIAN_POINT('Ctrl Pts',(8.13178807675717,8.13124999997796,5.90808986649102));
#301647=CARTESIAN_POINT('Ctrl Pts',(10.0514428414942,8.28124999997736,3.2659117547607));
#301648=CARTESIAN_POINT('Ctrl Pts',(10.0514428414941,8.43124999997676,-1.23094673026484E-15));
#301649=CARTESIAN_POINT('Ctrl Pts',(10.0514428414941,8.58124999997616,-3.26591175476071));
#301650=CARTESIAN_POINT('Ctrl Pts',(8.13178807675717,8.73124999997556,-5.90808986649102));
#301651=CARTESIAN_POINT('Ctrl Pts',(6.2121333120202,8.88124999997496,-8.55026797822134));
#301652=CARTESIAN_POINT('Ctrl Pts',(3.10606665601009,9.03124999997436,-9.5594902125713));
#301653=CARTESIAN_POINT('Ctrl Pts',(-1.84122806625156E-14,9.18124999997375,
-10.5687124469213));
#301654=CARTESIAN_POINT('Ctrl Pts',(-3.10606665601013,9.33124999997315,
-9.5594902125713));
#301655=CARTESIAN_POINT('Ctrl Pts',(-6.21213331202023,9.48124999997255,
-8.55026797822134));
#301656=CARTESIAN_POINT('Ctrl Pts',(-8.13178807675721,9.63124999997195,
-5.90808986649102));
#301657=CARTESIAN_POINT('Ctrl Pts',(-10.0514428414942,9.78124999997135,
-3.2659117547607));
#301658=CARTESIAN_POINT('Ctrl Pts',(-10.0514428414942,9.93124999997075,
2.46189346052968E-15));
#301659=CARTESIAN_POINT('Ctrl Pts',(-10.0514428414942,10.0812499999701,
3.26591175476071));
#301660=CARTESIAN_POINT('Ctrl Pts',(-8.13178807675721,10.2312499999695,
5.90808986649102));
#301661=CARTESIAN_POINT('Ctrl Pts',(-6.21213331202023,10.3812499999689,
8.55026797822134));
#301662=CARTESIAN_POINT('Ctrl Pts',(-3.10606665601012,10.5312499999684,
9.5594902125713));
#301663=CARTESIAN_POINT('Ctrl Pts',(-1.66875473245003E-14,10.6812499999678,
10.5687124469213));
#301664=CARTESIAN_POINT('Ctrl Pts',(3.10606665601009,10.8312499999672,9.5594902125713));
#301665=CARTESIAN_POINT('Ctrl Pts',(6.2121333120202,10.9812499999666,8.55026797822134));
#301666=CARTESIAN_POINT('Ctrl Pts',(8.13178807675717,11.131249999966,5.90808986649102));
#301667=CARTESIAN_POINT('Ctrl Pts',(10.0514428414941,11.2812499999654,3.2659117547607));
#301668=CARTESIAN_POINT('Ctrl Pts',(10.0514428414941,11.4312499999648,-1.23094673026484E-15));
#301669=CARTESIAN_POINT('Ctrl Pts',(10.0514428414941,11.5812499999642,-3.26591175476071));
#301670=CARTESIAN_POINT('Ctrl Pts',(8.13178807675717,11.7312499999636,-5.90808986649102));
#301671=CARTESIAN_POINT('Ctrl Pts',(6.2121333120202,11.881249999963,-8.55026797822134));
#301672=CARTESIAN_POINT('Ctrl Pts',(3.10606665601009,12.0312499999624,-9.5594902125713));
#301673=CARTESIAN_POINT('Ctrl Pts',(-2.01399899341774E-14,12.1812499999618,
-10.5687124469213));
#301674=CARTESIAN_POINT('Ctrl Pts',(-3.10606665601013,12.3312499999612,
-9.5594902125713));
#301675=CARTESIAN_POINT('Ctrl Pts',(-6.21213331202024,12.4812499999605,
-8.55026797822134));
#301676=CARTESIAN_POINT('Ctrl Pts',(-8.13178807675721,12.6312499999599,
-5.90808986649102));
#301677=CARTESIAN_POINT('Ctrl Pts',(-10.0514428414942,12.7812499999593,
-3.2659117547607));
#301678=CARTESIAN_POINT('Ctrl Pts',(-10.0514428414942,12.9312499999587,
2.46189346052968E-15));
#301679=CARTESIAN_POINT('Ctrl Pts',(-10.0514428414942,13.0812499999581,
3.26591175476071));
#301680=CARTESIAN_POINT('Ctrl Pts',(-8.13178807675721,13.2312499999575,
5.90808986649102));
#301681=CARTESIAN_POINT('Ctrl Pts',(-6.21213331202023,13.3812499999569,
8.55026797822134));
#301682=CARTESIAN_POINT('Ctrl Pts',(-3.10606665601013,13.5312499999564,
9.5594902125713));
#301683=CARTESIAN_POINT('Ctrl Pts',(-1.84152565961621E-14,13.6812499999558,
10.5687124469213));
#301684=CARTESIAN_POINT('Ctrl Pts',(3.10606665601009,13.8312499999552,9.5594902125713));
#301685=CARTESIAN_POINT('Ctrl Pts',(6.2121333120202,13.9812499999546,8.55026797822134));
#301686=CARTESIAN_POINT('Ctrl Pts',(8.13178807675717,14.131249999954,5.90808986649102));
#301687=CARTESIAN_POINT('Ctrl Pts',(10.0514428414941,14.2812499999534,3.2659117547607));
#301688=CARTESIAN_POINT('Ctrl Pts',(10.0514428414941,14.4312499999528,-1.23094673026484E-15));
#301689=CARTESIAN_POINT('Ctrl Pts',(10.0514428414941,14.5812499999522,-3.26591175476071));
#301690=CARTESIAN_POINT('Ctrl Pts',(8.13178807675717,14.7312499999516,-5.90808986649102));
#301691=CARTESIAN_POINT('Ctrl Pts',(6.21213331202019,14.881249999951,-8.55026797822134));
#301692=CARTESIAN_POINT('Ctrl Pts',(3.10606665601009,15.0312499999504,-9.5594902125713));
#301693=CARTESIAN_POINT('Ctrl Pts',(-2.18676992058392E-14,15.1812499999498,
-10.5687124469213));
#301694=CARTESIAN_POINT('Ctrl Pts',(-3.10606665601013,15.3312499999492,
-9.5594902125713));
#301695=CARTESIAN_POINT('Ctrl Pts',(-6.21213331202024,15.4812499999485,
-8.55026797822134));
#301696=CARTESIAN_POINT('Ctrl Pts',(-8.13178807675721,15.6312499999479,
-5.90808986649102));
#301697=CARTESIAN_POINT('Ctrl Pts',(-10.0514428414942,15.7812499999473,
-3.2659117547607));
#301698=CARTESIAN_POINT('Ctrl Pts',(-10.0514428414942,15.9312499999467,
2.46189346052968E-15));
#301699=CARTESIAN_POINT('Ctrl Pts',(-10.0514428414942,16.0812499999461,
3.26591175476071));
#301700=CARTESIAN_POINT('Ctrl Pts',(-8.13178807675721,16.2312499999455,
5.90808986649102));
#301701=CARTESIAN_POINT('Ctrl Pts',(-6.21213331202024,16.3812499999449,
8.55026797822134));
#301702=CARTESIAN_POINT('Ctrl Pts',(-3.10606665601013,16.5312499999444,
9.5594902125713));
#301703=CARTESIAN_POINT('Ctrl Pts',(-2.0142965867824E-14,16.6812499999438,
10.5687124469213));
#301704=CARTESIAN_POINT('Ctrl Pts',(3.10606665601009,16.8312499999432,9.5594902125713));
#301705=CARTESIAN_POINT('Ctrl Pts',(6.21213331202019,16.9812499999426,8.55026797822134));
#301706=CARTESIAN_POINT('Ctrl Pts',(8.13178807675717,17.131249999942,5.90808986649102));
#301707=CARTESIAN_POINT('Ctrl Pts',(10.0514428414941,17.2812499999414,3.2659117547607));
#301708=CARTESIAN_POINT('Ctrl Pts',(10.0514428414941,17.4312499999408,-1.23094673026484E-15));
#301709=CARTESIAN_POINT('Ctrl Pts',(10.0514428414941,17.5812499999402,-3.26591175476071));
#301710=CARTESIAN_POINT('Ctrl Pts',(8.13178807675717,17.7312499999396,-5.90808986649102));
#301711=CARTESIAN_POINT('Ctrl Pts',(6.21213331202019,17.881249999939,-8.55026797822134));
#301712=CARTESIAN_POINT('Ctrl Pts',(3.10606665601008,18.0312499999384,-9.5594902125713));
#301713=CARTESIAN_POINT('Ctrl Pts',(-2.35954084775011E-14,18.1812499999378,
-10.5687124469213));
#301714=CARTESIAN_POINT('Ctrl Pts',(-3.10606665601013,18.3312499999371,
-9.5594902125713));
#301715=CARTESIAN_POINT('Ctrl Pts',(-6.21213331202024,18.4812499999365,
-8.55026797822134));
#301716=CARTESIAN_POINT('Ctrl Pts',(-8.13178807675721,18.6312499999359,
-5.90808986649102));
#301717=CARTESIAN_POINT('Ctrl Pts',(-10.0514428414942,18.7812499999353,
-3.2659117547607));
#301718=CARTESIAN_POINT('Ctrl Pts',(-10.0514428414942,18.9312499999347,
2.46189346052968E-15));
#301719=CARTESIAN_POINT('Ctrl Pts',(-10.0514428414942,19.0812499999341,
3.26591175476071));
#301720=CARTESIAN_POINT('Ctrl Pts',(-8.13178807675721,19.2312499999335,
5.90808986649102));
#301721=CARTESIAN_POINT('Ctrl Pts',(-6.21213331202024,19.381249999933,8.55026797822134));
#301722=CARTESIAN_POINT('Ctrl Pts',(-3.10606665601013,19.5312499999323,
9.5594902125713));
#301723=CARTESIAN_POINT('Ctrl Pts',(-2.18706751394858E-14,19.6812499999318,
10.5687124469213));
#301724=CARTESIAN_POINT('Ctrl Pts',(3.10606665601009,19.8312499999312,9.5594902125713));
#301725=CARTESIAN_POINT('Ctrl Pts',(6.21213331202019,19.9812499999306,8.55026797822134));
#301726=CARTESIAN_POINT('Ctrl Pts',(8.13178807675717,20.13124999993,5.90808986649102));
#301727=CARTESIAN_POINT('Ctrl Pts',(10.0514428414941,20.2812499999294,3.2659117547607));
#301728=CARTESIAN_POINT('Ctrl Pts',(10.0514428414941,20.4312499999288,-1.23094673026484E-15));
#301729=CARTESIAN_POINT('Ctrl Pts',(10.0514428414941,20.5812499999282,-3.26591175476071));
#301730=CARTESIAN_POINT('Ctrl Pts',(8.13178807675716,20.7312499999276,-5.90808986649102));
#301731=CARTESIAN_POINT('Ctrl Pts',(6.21213331202019,20.881249999927,-8.55026797822134));
#301732=CARTESIAN_POINT('Ctrl Pts',(3.10606665601008,21.0312499999264,-9.5594902125713));
#301733=CARTESIAN_POINT('Ctrl Pts',(-2.53231177491629E-14,21.1812499999258,
-10.5687124469213));
#301734=CARTESIAN_POINT('Ctrl Pts',(-3.10606665601013,21.3312499999251,
-9.5594902125713));
#301735=CARTESIAN_POINT('Ctrl Pts',(-6.21213331202024,21.4812499999245,
-8.55026797822134));
#301736=CARTESIAN_POINT('Ctrl Pts',(-8.13178807675722,21.6312499999239,
-5.90808986649102));
#301737=CARTESIAN_POINT('Ctrl Pts',(-10.0514428414942,21.7812499999233,
-3.2659117547607));
#301738=CARTESIAN_POINT('Ctrl Pts',(-10.0514428414942,21.9312499999227,
2.46189346052968E-15));
#301739=CARTESIAN_POINT('Ctrl Pts',(-10.0514428414942,22.0812499999221,
3.26591175476071));
#301740=CARTESIAN_POINT('Ctrl Pts',(-8.13178807675722,22.2312499999215,
5.90808986649102));
#301741=CARTESIAN_POINT('Ctrl Pts',(-6.21213331202024,22.3812499999209,
8.55026797822134));
#301742=CARTESIAN_POINT('Ctrl Pts',(-3.10606665601013,22.5312499999204,
9.5594902125713));
#301743=CARTESIAN_POINT('Ctrl Pts',(-2.35983844111477E-14,22.6812499999198,
10.5687124469213));
#301744=CARTESIAN_POINT('Ctrl Pts',(3.10606665601008,22.8312499999192,9.5594902125713));
#301745=CARTESIAN_POINT('Ctrl Pts',(6.21213331202019,22.9812499999186,8.55026797822134));
#301746=CARTESIAN_POINT('Ctrl Pts',(8.13178807675716,23.131249999918,5.90808986649102));
#301747=CARTESIAN_POINT('Ctrl Pts',(10.0514428414941,23.2812499999174,3.2659117547607));
#301748=CARTESIAN_POINT('Ctrl Pts',(10.0514428414941,23.4312499999168,-1.23094673026484E-15));
#301749=CARTESIAN_POINT('Ctrl Pts',(10.0514428414941,23.5812499999162,-3.26591175476071));
#301750=CARTESIAN_POINT('Ctrl Pts',(8.13178807675716,23.7312499999156,-5.90808986649102));
#301751=CARTESIAN_POINT('Ctrl Pts',(6.21213331202019,23.881249999915,-8.55026797822134));
#301752=CARTESIAN_POINT('Ctrl Pts',(3.10606665601008,24.0312499999144,-9.5594902125713));
#301753=CARTESIAN_POINT('Ctrl Pts',(-2.70508270208248E-14,24.1812499999138,
-10.5687124469213));
#301754=CARTESIAN_POINT('Ctrl Pts',(-3.10606665601014,24.3312499999131,
-9.5594902125713));
#301755=CARTESIAN_POINT('Ctrl Pts',(-6.21213331202024,24.4812499999125,
-8.55026797822134));
#301756=CARTESIAN_POINT('Ctrl Pts',(-8.13178807675722,24.6312499999119,
-5.90808986649102));
#301757=CARTESIAN_POINT('Ctrl Pts',(-10.0514428414942,24.7812499999113,
-3.2659117547607));
#301758=CARTESIAN_POINT('Ctrl Pts',(-10.0514428414942,24.9312499999107,
2.46189346052968E-15));
#301759=CARTESIAN_POINT('Ctrl Pts',(-10.0514428414942,25.0812499999101,
3.26591175476071));
#301760=CARTESIAN_POINT('Ctrl Pts',(-8.13178807675722,25.2312499999095,
5.90808986649102));
#301761=CARTESIAN_POINT('Ctrl Pts',(-6.21213331202024,25.381249999909,8.55026797822134));
#301762=CARTESIAN_POINT('Ctrl Pts',(-3.10606665601013,25.5312499999084,
9.5594902125713));
#301763=CARTESIAN_POINT('Ctrl Pts',(-2.53260936828095E-14,25.6812499999078,
10.5687124469213));
#301764=CARTESIAN_POINT('Ctrl Pts',(3.10606665601008,25.8312499999072,9.5594902125713));
#301765=CARTESIAN_POINT('Ctrl Pts',(6.21213331202019,25.9812499999066,8.55026797822134));
#301766=CARTESIAN_POINT('Ctrl Pts',(8.13178807675716,26.131249999906,5.90808986649102));
#301767=CARTESIAN_POINT('Ctrl Pts',(10.0514428414941,26.2812499999054,3.2659117547607));
#301768=CARTESIAN_POINT('Ctrl Pts',(10.0514428414941,26.4312499999048,-1.23094673026484E-15));
#301769=CARTESIAN_POINT('Ctrl Pts',(10.0514428414941,26.5812499999042,-3.26591175476071));
#301770=CARTESIAN_POINT('Ctrl Pts',(8.13178807675716,26.7312499999036,-5.90808986649102));
#301771=CARTESIAN_POINT('Ctrl Pts',(6.21213331202019,26.881249999903,-8.55026797822134));
#301772=CARTESIAN_POINT('Ctrl Pts',(3.10606665601008,27.0312499999024,-9.5594902125713));
#301773=CARTESIAN_POINT('Ctrl Pts',(-2.87785362924866E-14,27.1812499999018,
-10.5687124469213));
#301774=CARTESIAN_POINT('Ctrl Pts',(-3.10606665601014,27.3312499999011,
-9.5594902125713));
#301775=CARTESIAN_POINT('Ctrl Pts',(-6.21213331202024,27.4812499999005,
-8.55026797822134));
#301776=CARTESIAN_POINT('Ctrl Pts',(-8.13178807675722,27.6312499998999,
-5.90808986649102));
#301777=CARTESIAN_POINT('Ctrl Pts',(-10.0514428414942,27.7812499998993,
-3.2659117547607));
#301778=CARTESIAN_POINT('Ctrl Pts',(-10.0514428414942,27.9312499998987,
2.46189346052968E-15));
#301779=CARTESIAN_POINT('Ctrl Pts',(-10.0514428414942,28.0812499998981,
3.26591175476071));
#301780=CARTESIAN_POINT('Ctrl Pts',(-8.13178807675722,28.2312499998975,
5.90808986649102));
#301781=CARTESIAN_POINT('Ctrl Pts',(-6.21213331202024,28.3812499998969,
8.55026797822134));
#301782=CARTESIAN_POINT('Ctrl Pts',(-3.10606665601014,28.5312499998964,
9.5594902125713));
#301783=CARTESIAN_POINT('Ctrl Pts',(-2.70538029544713E-14,28.6812499998958,
10.5687124469213));
#301784=CARTESIAN_POINT('Ctrl Pts',(3.10606665601008,28.8312499998952,9.5594902125713));
#301785=CARTESIAN_POINT('Ctrl Pts',(6.21213331202019,28.9812499998946,8.55026797822134));
#301786=CARTESIAN_POINT('Ctrl Pts',(8.13178807675716,29.131249999894,5.90808986649102));
#301787=CARTESIAN_POINT('Ctrl Pts',(10.0514428414941,29.2812499998934,3.2659117547607));
#301788=CARTESIAN_POINT('Ctrl Pts',(10.0514428414941,29.4312499998928,-1.23094673026484E-15));
#301789=CARTESIAN_POINT('Ctrl Pts',(10.0514428414941,29.5812499998922,-3.26591175476071));
#301790=CARTESIAN_POINT('Ctrl Pts',(8.13178807675716,29.7312499998916,-5.90808986649102));
#301791=CARTESIAN_POINT('Ctrl Pts',(6.21213331202019,29.881249999891,-8.55026797822134));
#301792=CARTESIAN_POINT('Ctrl Pts',(3.10606665601008,30.0312499998904,-9.5594902125713));
#301793=CARTESIAN_POINT('Ctrl Pts',(-3.05062455641484E-14,30.1812499998898,
-10.5687124469213));
#301794=CARTESIAN_POINT('Ctrl Pts',(-3.10606665601014,30.3312499998892,
-9.5594902125713));
#301795=CARTESIAN_POINT('Ctrl Pts',(-6.21213331202025,30.4812499998885,
-8.55026797822134));
#301796=CARTESIAN_POINT('Ctrl Pts',(-8.13178807675722,30.6312499998879,
-5.90808986649102));
#301797=CARTESIAN_POINT('Ctrl Pts',(-10.0514428414942,30.7812499998873,
-3.2659117547607));
#301798=CARTESIAN_POINT('Ctrl Pts',(-10.0514428414942,30.9312499998867,
2.46189346052968E-15));
#301799=CARTESIAN_POINT('Ctrl Pts',(-10.0514428414942,31.0812499998861,
3.26591175476071));
#301800=CARTESIAN_POINT('Ctrl Pts',(-8.13178807675722,31.2312499998855,
5.90808986649102));
#301801=CARTESIAN_POINT('Ctrl Pts',(-6.21213331202024,31.381249999885,8.55026797822134));
#301802=CARTESIAN_POINT('Ctrl Pts',(-3.10606665601014,31.5312499998843,
9.5594902125713));
#301803=CARTESIAN_POINT('Ctrl Pts',(-2.87815122261332E-14,31.6812499998838,
10.5687124469213));
#301804=CARTESIAN_POINT('Ctrl Pts',(3.10606665601008,31.8312499998832,9.5594902125713));
#301805=CARTESIAN_POINT('Ctrl Pts',(6.21213331202019,31.9812499998826,8.55026797822134));
#301806=CARTESIAN_POINT('Ctrl Pts',(8.13178807675716,32.131249999882,5.90808986649102));
#301807=CARTESIAN_POINT('Ctrl Pts',(10.0514428414941,32.2812499998814,3.2659117547607));
#301808=CARTESIAN_POINT('Ctrl Pts',(10.0514428414941,32.4312499998808,-1.23094673026484E-15));
#301809=CARTESIAN_POINT('Ctrl Pts',(10.0514428414941,32.5812499998802,-3.26591175476071));
#301810=CARTESIAN_POINT('Ctrl Pts',(8.13178807675716,32.7312499998796,-5.90808986649102));
#301811=CARTESIAN_POINT('Ctrl Pts',(6.21213331202019,32.8812499998789,-8.55026797822134));
#301812=CARTESIAN_POINT('Ctrl Pts',(3.10606665601008,33.0312499998784,-9.5594902125713));
#301813=CARTESIAN_POINT('Ctrl Pts',(-3.22339548358103E-14,33.1812499998777,
-10.5687124469213));
#301814=CARTESIAN_POINT('Ctrl Pts',(-3.10606665601014,33.3312499998772,
-9.5594902125713));
#301815=CARTESIAN_POINT('Ctrl Pts',(-6.21213331202025,33.4812499998766,
-8.55026797822134));
#301816=CARTESIAN_POINT('Ctrl Pts',(-8.13178807675722,33.6312499998759,
-5.90808986649102));
#301817=CARTESIAN_POINT('Ctrl Pts',(-10.0514428414942,33.7812499998753,
-3.2659117547607));
#301818=CARTESIAN_POINT('Ctrl Pts',(-10.0514428414942,33.9312499998747,
2.46189346052968E-15));
#301819=CARTESIAN_POINT('Ctrl Pts',(-10.0514428414942,34.0812499998741,
3.26591175476071));
#301820=CARTESIAN_POINT('Ctrl Pts',(-8.13178807675722,34.2312499998735,
5.90808986649102));
#301821=CARTESIAN_POINT('Ctrl Pts',(-6.21213331202024,34.3812499998729,
8.55026797822134));
#301822=CARTESIAN_POINT('Ctrl Pts',(-3.10606665601014,34.5312499998724,
9.5594902125713));
#301823=CARTESIAN_POINT('Ctrl Pts',(-3.0509221497795E-14,34.6812499998718,
10.5687124469213));
#301824=CARTESIAN_POINT('Ctrl Pts',(3.10606665601008,34.8312499998712,9.5594902125713));
#301825=CARTESIAN_POINT('Ctrl Pts',(6.21213331202019,34.9812499998706,8.55026797822134));
#301826=CARTESIAN_POINT('Ctrl Pts',(8.13178807675716,35.13124999987,5.90808986649102));
#301827=CARTESIAN_POINT('Ctrl Pts',(10.0514428414941,35.2812499998694,3.2659117547607));
#301828=CARTESIAN_POINT('Ctrl Pts',(10.0514428414941,35.4312499998688,-1.23094673026484E-15));
#301829=CARTESIAN_POINT('Ctrl Pts',(10.0514428414941,35.5812499998682,-3.26591175476071));
#301830=CARTESIAN_POINT('Ctrl Pts',(8.13178807675716,35.7312499998676,-5.90808986649102));
#301831=CARTESIAN_POINT('Ctrl Pts',(6.21213331202018,35.881249999867,-8.55026797822134));
#301832=CARTESIAN_POINT('Ctrl Pts',(3.10606665601007,36.0312499998664,-9.5594902125713));
#301833=CARTESIAN_POINT('Ctrl Pts',(-3.39616641074721E-14,36.1812499998658,
-10.5687124469213));
#301834=CARTESIAN_POINT('Ctrl Pts',(-3.10606665601014,36.3312499998652,
-9.5594902125713));
#301835=CARTESIAN_POINT('Ctrl Pts',(-6.21213331202025,36.4812499998646,
-8.55026797822134));
#301836=CARTESIAN_POINT('Ctrl Pts',(-8.13178807675722,36.6312499998639,
-5.90808986649102));
#301837=CARTESIAN_POINT('Ctrl Pts',(-10.0514428414942,36.7812499998634,
-3.2659117547607));
#301838=CARTESIAN_POINT('Ctrl Pts',(-10.0514428414942,36.9312499998627,
2.46189346052968E-15));
#301839=CARTESIAN_POINT('Ctrl Pts',(-10.0514428414942,37.0812499998621,
3.26591175476071));
#301840=CARTESIAN_POINT('Ctrl Pts',(-8.13178807675722,37.2312499998615,
5.90808986649102));
#301841=CARTESIAN_POINT('Ctrl Pts',(-6.21213331202025,37.3812499998609,
8.55026797822134));
#301842=CARTESIAN_POINT('Ctrl Pts',(-3.10606665601014,37.5312499998603,
9.5594902125713));
#301843=CARTESIAN_POINT('Ctrl Pts',(-3.22369307694568E-14,37.6812499998598,
10.5687124469213));
#301844=CARTESIAN_POINT('Ctrl Pts',(3.10606665601008,37.8312499998592,9.5594902125713));
#301845=CARTESIAN_POINT('Ctrl Pts',(6.21213331202018,37.9812499998586,8.55026797822134));
#301846=CARTESIAN_POINT('Ctrl Pts',(8.13178807675716,38.131249999858,5.90808986649102));
#301847=CARTESIAN_POINT('Ctrl Pts',(10.0514428414941,38.2812499998574,3.2659117547607));
#301848=CARTESIAN_POINT('Ctrl Pts',(10.0514428414941,38.4312499998568,-1.23094673026484E-15));
#301849=CARTESIAN_POINT('Ctrl Pts',(10.0514428414941,38.5812499998562,-3.26591175476071));
#301850=CARTESIAN_POINT('Ctrl Pts',(8.13178807675715,38.7312499998556,-5.90808986649102));
#301851=CARTESIAN_POINT('Ctrl Pts',(6.21213331202018,38.881249999855,-8.55026797822134));
#301852=CARTESIAN_POINT('Ctrl Pts',(3.10606665601007,39.0312499998544,-9.5594902125713));
#301853=CARTESIAN_POINT('Ctrl Pts',(-3.5689373379134E-14,39.1812499998538,
-10.5687124469213));
#301854=CARTESIAN_POINT('Ctrl Pts',(-3.10606665601014,39.3312499998532,
-9.5594902125713));
#301855=CARTESIAN_POINT('Ctrl Pts',(-6.21213331202025,39.4812499998525,
-8.55026797822134));
#301856=CARTESIAN_POINT('Ctrl Pts',(-8.13178807675723,39.6312499998519,
-5.90808986649102));
#301857=CARTESIAN_POINT('Ctrl Pts',(-10.0514428414942,39.7812499998513,
-3.2659117547607));
#301858=CARTESIAN_POINT('Ctrl Pts',(-10.0514428414942,39.9312499998507,
2.46189346052968E-15));
#301859=CARTESIAN_POINT('Ctrl Pts',(-10.0514428414942,40.0812499998502,
3.26591175476071));
#301860=CARTESIAN_POINT('Ctrl Pts',(-8.13178807675723,40.2312499998495,
5.90808986649102));
#301861=CARTESIAN_POINT('Ctrl Pts',(-6.21213331202025,40.3812499998489,
8.55026797822134));
#301862=CARTESIAN_POINT('Ctrl Pts',(-3.10606665601014,40.5312499998483,
9.5594902125713));
#301863=CARTESIAN_POINT('Ctrl Pts',(-3.39646400411187E-14,40.6812499998478,
10.5687124469213));
#301864=CARTESIAN_POINT('Ctrl Pts',(3.10606665601007,40.8312499998472,9.5594902125713));
#301865=CARTESIAN_POINT('Ctrl Pts',(6.21213331202018,40.9812499998466,8.55026797822134));
#301866=CARTESIAN_POINT('Ctrl Pts',(8.13178807675715,41.131249999846,5.90808986649102));
#301867=CARTESIAN_POINT('Ctrl Pts',(10.0514428414941,41.2812499998454,3.2659117547607));
#301868=CARTESIAN_POINT('Ctrl Pts',(10.0514428414941,41.4312499998448,-1.23094673026484E-15));
#301869=CARTESIAN_POINT('Ctrl Pts',(10.0514428414941,41.5812499998442,-3.26591175476071));
#301870=CARTESIAN_POINT('Ctrl Pts',(8.13178807675715,41.7312499998436,-5.90808986649102));
#301871=CARTESIAN_POINT('Ctrl Pts',(6.21213331202018,41.881249999843,-8.55026797822134));
#301872=CARTESIAN_POINT('Ctrl Pts',(3.10606665601007,42.0312499998423,-9.5594902125713));
#301873=CARTESIAN_POINT('Ctrl Pts',(-3.74170826507958E-14,42.1812499998418,
-10.5687124469213));
#301874=CARTESIAN_POINT('Ctrl Pts',(-3.10606665601015,42.3312499998411,
-9.5594902125713));
#301875=CARTESIAN_POINT('Ctrl Pts',(-6.21213331202025,42.4812499998406,
-8.55026797822134));
#301876=CARTESIAN_POINT('Ctrl Pts',(-8.13178807675723,42.6312499998399,
-5.90808986649102));
#301877=CARTESIAN_POINT('Ctrl Pts',(-10.0514428414942,42.7812499998393,
-3.2659117547607));
#301878=CARTESIAN_POINT('Ctrl Pts',(-10.0514428414942,42.9312499998387,
2.46189346052968E-15));
#301879=CARTESIAN_POINT('Ctrl Pts',(-10.0514428414942,43.0812499998381,
3.26591175476071));
#301880=CARTESIAN_POINT('Ctrl Pts',(-8.13178807675723,43.2312499998375,
5.90808986649102));
#301881=CARTESIAN_POINT('Ctrl Pts',(-6.21213331202025,43.3812499998369,
8.55026797822134));
#301882=CARTESIAN_POINT('Ctrl Pts',(-3.10606665601014,43.5312499998363,
9.5594902125713));
#301883=CARTESIAN_POINT('Ctrl Pts',(-3.56923493127805E-14,43.6812499998357,
10.5687124469213));
#301884=CARTESIAN_POINT('Ctrl Pts',(3.10606665601007,43.8312499998352,9.5594902125713));
#301885=CARTESIAN_POINT('Ctrl Pts',(6.21213331202018,43.9812499998345,8.55026797822134));
#301886=CARTESIAN_POINT('Ctrl Pts',(8.13178807675715,44.131249999834,5.90808986649102));
#301887=CARTESIAN_POINT('Ctrl Pts',(10.0514428414941,44.2812499998334,3.2659117547607));
#301888=CARTESIAN_POINT('Ctrl Pts',(10.0514428414941,44.4312499998328,-1.23094673026484E-15));
#301889=CARTESIAN_POINT('Ctrl Pts',(10.0514428414941,44.5812499998322,-3.26591175476071));
#301890=CARTESIAN_POINT('Ctrl Pts',(8.13178807675715,44.7312499998316,-5.90808986649102));
#301891=CARTESIAN_POINT('Ctrl Pts',(6.21213331202018,44.881249999831,-8.55026797822134));
#301892=CARTESIAN_POINT('Ctrl Pts',(3.10606665601007,45.0312499998304,-9.5594902125713));
#301893=CARTESIAN_POINT('Ctrl Pts',(-3.91447919224576E-14,45.1812499998297,
-10.5687124469213));
#301894=CARTESIAN_POINT('Ctrl Pts',(-3.10606665601015,45.3312499998292,
-9.5594902125713));
#301895=CARTESIAN_POINT('Ctrl Pts',(-6.21213331202026,45.4812499998285,
-8.55026797822134));
#301896=CARTESIAN_POINT('Ctrl Pts',(-8.13178807675723,45.6312499998279,
-5.90808986649102));
#301897=CARTESIAN_POINT('Ctrl Pts',(-10.0514428414942,45.7812499998273,
-3.2659117547607));
#301898=CARTESIAN_POINT('Ctrl Pts',(-10.0514428414942,45.9312499998267,
2.46189346052968E-15));
#301899=CARTESIAN_POINT('Ctrl Pts',(-10.0514428414942,46.0812499998261,
3.26591175476071));
#301900=CARTESIAN_POINT('Ctrl Pts',(-8.13178807675723,46.2312499998255,
5.90808986649102));
#301901=CARTESIAN_POINT('Ctrl Pts',(-6.21213331202025,46.3812499998249,
8.55026797822134));
#301902=CARTESIAN_POINT('Ctrl Pts',(-3.10606665601015,46.5312499998244,
9.5594902125713));
#301903=CARTESIAN_POINT('Ctrl Pts',(-3.74200585844424E-14,46.6812499998238,
10.5687124469213));
#301904=CARTESIAN_POINT('Ctrl Pts',(3.10606665601007,46.8312499998232,9.5594902125713));
#301905=CARTESIAN_POINT('Ctrl Pts',(6.21213331202018,46.9812499998226,8.55026797822134));
#301906=CARTESIAN_POINT('Ctrl Pts',(8.13178807675715,47.131249999822,5.90808986649102));
#301907=CARTESIAN_POINT('Ctrl Pts',(10.0514428414941,47.2812499998214,3.2659117547607));
#301908=CARTESIAN_POINT('Ctrl Pts',(10.0514428414941,47.4312499998208,-1.23094673026484E-15));
#301909=CARTESIAN_POINT('Ctrl Pts',(10.0514428414941,47.5812499998202,-3.26591175476071));
#301910=CARTESIAN_POINT('Ctrl Pts',(8.13178807675715,47.7312499998196,-5.90808986649102));
#301911=CARTESIAN_POINT('Ctrl Pts',(6.21213331202017,47.881249999819,-8.55026797822134));
#301912=CARTESIAN_POINT('Ctrl Pts',(3.10606665601007,48.0312499998184,-9.5594902125713));
#301913=CARTESIAN_POINT('Ctrl Pts',(-4.08725011941195E-14,48.1812499998178,
-10.5687124469213));
#301914=CARTESIAN_POINT('Ctrl Pts',(-3.10606665601015,48.3312499998172,
-9.5594902125713));
#301915=CARTESIAN_POINT('Ctrl Pts',(-6.21213331202026,48.4812499998166,
-8.55026797822134));
#301916=CARTESIAN_POINT('Ctrl Pts',(-8.13178807675723,48.6312499998159,
-5.90808986649102));
#301917=CARTESIAN_POINT('Ctrl Pts',(-10.0514428414942,48.7812499998153,
-3.2659117547607));
#301918=CARTESIAN_POINT('Ctrl Pts',(-10.0514428414942,48.9312499998147,
2.46189346052968E-15));
#301919=CARTESIAN_POINT('Ctrl Pts',(-10.0514428414942,49.0812499998141,
3.26591175476071));
#301920=CARTESIAN_POINT('Ctrl Pts',(-8.13178807675723,49.2312499998135,
5.90808986649102));
#301921=CARTESIAN_POINT('Ctrl Pts',(-6.21213331202026,49.3812499998129,
8.55026797822134));
#301922=CARTESIAN_POINT('Ctrl Pts',(-3.10606665601015,49.5312499998124,
9.5594902125713));
#301923=CARTESIAN_POINT('Ctrl Pts',(-3.91477678561042E-14,49.6812499998117,
10.5687124469213));
#301924=CARTESIAN_POINT('Ctrl Pts',(3.10606665601007,49.8312499998111,9.5594902125713));
#301925=CARTESIAN_POINT('Ctrl Pts',(6.21213331202017,49.9812499998106,8.55026797822134));
#301926=CARTESIAN_POINT('Ctrl Pts',(8.13178807675715,50.13124999981,5.90808986649102));
#301927=CARTESIAN_POINT('Ctrl Pts',(10.0514428414941,50.2812499998094,3.2659117547607));
#301928=CARTESIAN_POINT('Ctrl Pts',(10.0514428414941,50.4312499998088,-1.23094673026484E-15));
#301929=CARTESIAN_POINT('Ctrl Pts',(10.0514428414941,50.5812499998082,-3.26591175476071));
#301930=CARTESIAN_POINT('Ctrl Pts',(8.13178807675715,50.7312499998076,-5.90808986649102));
#301931=CARTESIAN_POINT('Ctrl Pts',(6.21213331202017,50.881249999807,-8.55026797822134));
#301932=CARTESIAN_POINT('Ctrl Pts',(3.10606665601007,51.0312499998064,-9.5594902125713));
#301933=CARTESIAN_POINT('Ctrl Pts',(-4.26002104657813E-14,51.1812499998058,
-10.5687124469213));
#301934=CARTESIAN_POINT('Ctrl Pts',(-3.10606665601015,51.3312499998052,
-9.5594902125713));
#301935=CARTESIAN_POINT('Ctrl Pts',(-6.21213331202026,51.4812499998045,
-8.55026797822134));
#301936=CARTESIAN_POINT('Ctrl Pts',(-8.13178807675723,51.631249999804,-5.90808986649102));
#301937=CARTESIAN_POINT('Ctrl Pts',(-10.0514428414942,51.7812499998034,
-3.2659117547607));
#301938=CARTESIAN_POINT('Ctrl Pts',(-10.0514428414942,51.9312499998027,
2.46189346052968E-15));
#301939=CARTESIAN_POINT('Ctrl Pts',(-10.0514428414942,52.0812499998021,
3.26591175476071));
#301940=CARTESIAN_POINT('Ctrl Pts',(-8.13178807675723,52.2312499998015,
5.90808986649102));
#301941=CARTESIAN_POINT('Ctrl Pts',(-6.21213331202026,52.3812499998009,
8.55026797822134));
#301942=CARTESIAN_POINT('Ctrl Pts',(-3.10606665601015,52.5312499998004,
9.5594902125713));
#301943=CARTESIAN_POINT('Ctrl Pts',(-4.08754771277661E-14,52.6812499997998,
10.5687124469213));
#301944=CARTESIAN_POINT('Ctrl Pts',(3.10606665601007,52.8312499997991,9.5594902125713));
#301945=CARTESIAN_POINT('Ctrl Pts',(6.21213331202017,52.9812499997986,8.55026797822134));
#301946=CARTESIAN_POINT('Ctrl Pts',(8.13178807675715,53.131249999798,5.90808986649102));
#301947=CARTESIAN_POINT('Ctrl Pts',(10.0514428414941,53.2812499997974,3.2659117547607));
#301948=CARTESIAN_POINT('Ctrl Pts',(10.0514428414941,53.4312499997968,-1.23094673026484E-15));
#301949=CARTESIAN_POINT('Ctrl Pts',(10.0514428414941,53.5812499997962,-3.26591175476071));
#301950=CARTESIAN_POINT('Ctrl Pts',(8.13178807675714,53.7312499997956,-5.90808986649102));
#301951=CARTESIAN_POINT('Ctrl Pts',(6.21213331202017,53.881249999795,-8.55026797822134));
#301952=CARTESIAN_POINT('Ctrl Pts',(3.10606665601006,54.0312499997944,-9.5594902125713));
#301953=CARTESIAN_POINT('Ctrl Pts',(-4.43279197374432E-14,54.1812499997938,
-10.5687124469213));
#301954=CARTESIAN_POINT('Ctrl Pts',(-3.10606665601015,54.3312499997932,
-9.5594902125713));
#301955=CARTESIAN_POINT('Ctrl Pts',(-6.21213331202026,54.4812499997926,
-8.55026797822134));
#301956=CARTESIAN_POINT('Ctrl Pts',(-8.13178807675724,54.6312499997919,
-5.90808986649102));
#301957=CARTESIAN_POINT('Ctrl Pts',(-10.0514428414942,54.7812499997914,
-3.2659117547607));
#301958=CARTESIAN_POINT('Ctrl Pts',(-10.0514428414942,54.9312499997907,
2.46189346052968E-15));
#301959=CARTESIAN_POINT('Ctrl Pts',(-10.0514428414942,55.0812499997901,
3.26591175476071));
#301960=CARTESIAN_POINT('Ctrl Pts',(-8.13178807675724,55.2312499997895,
5.90808986649102));
#301961=CARTESIAN_POINT('Ctrl Pts',(-6.21213331202026,55.3812499997889,
8.55026797822134));
#301962=CARTESIAN_POINT('Ctrl Pts',(-3.10606665601015,55.5312499997884,
9.5594902125713));
#301963=CARTESIAN_POINT('Ctrl Pts',(-4.26031863994279E-14,55.6812499997877,
10.5687124469213));
#301964=CARTESIAN_POINT('Ctrl Pts',(3.10606665601006,55.8312499997871,9.5594902125713));
#301965=CARTESIAN_POINT('Ctrl Pts',(6.21213331202017,55.9812499997865,8.55026797822134));
#301966=CARTESIAN_POINT('Ctrl Pts',(8.13178807675714,56.131249999786,5.90808986649102));
#301967=CARTESIAN_POINT('Ctrl Pts',(10.0514428414941,56.2812499997854,3.2659117547607));
#301968=CARTESIAN_POINT('Ctrl Pts',(10.0514428414941,56.4312499997848,-1.23094673026484E-15));
#301969=CARTESIAN_POINT('Ctrl Pts',(10.0514428414941,56.5812499997842,-3.26591175476071));
#301970=CARTESIAN_POINT('Ctrl Pts',(8.13178807675714,56.7312499997836,-5.90808986649102));
#301971=CARTESIAN_POINT('Ctrl Pts',(6.21213331202017,56.881249999783,-8.55026797822134));
#301972=CARTESIAN_POINT('Ctrl Pts',(3.10606665601006,57.0312499997824,-9.5594902125713));
#301973=CARTESIAN_POINT('Ctrl Pts',(-4.6055629009105E-14,57.1812499997818,
-10.5687124469213));
#301974=CARTESIAN_POINT('Ctrl Pts',(-3.10606665601015,57.3312499997812,
-9.5594902125713));
#301975=CARTESIAN_POINT('Ctrl Pts',(-6.21213331202026,57.4812499997805,
-8.55026797822134));
#301976=CARTESIAN_POINT('Ctrl Pts',(-8.13178807675724,57.6312499997799,
-5.90808986649102));
#301977=CARTESIAN_POINT('Ctrl Pts',(-10.0514428414942,57.7812499997793,
-3.2659117547607));
#301978=CARTESIAN_POINT('Ctrl Pts',(-10.0514428414942,57.9312499997787,
2.46189346052968E-15));
#301979=CARTESIAN_POINT('Ctrl Pts',(-10.0514428414942,58.0812499997781,
3.26591175476071));
#301980=CARTESIAN_POINT('Ctrl Pts',(-8.13178807675724,58.2312499997775,
5.90808986649102));
#301981=CARTESIAN_POINT('Ctrl Pts',(-6.21213331202026,58.3812499997769,
8.55026797822134));
#301982=CARTESIAN_POINT('Ctrl Pts',(-3.10606665601015,58.5312499997763,
9.5594902125713));
#301983=CARTESIAN_POINT('Ctrl Pts',(-4.43308956710897E-14,58.6812499997758,
10.5687124469213));
#301984=CARTESIAN_POINT('Ctrl Pts',(3.10606665601006,58.8312499997751,9.5594902125713));
#301985=CARTESIAN_POINT('Ctrl Pts',(6.21213331202017,58.9812499997745,8.55026797822134));
#301986=CARTESIAN_POINT('Ctrl Pts',(8.13178807675714,59.131249999774,5.90808986649102));
#301987=CARTESIAN_POINT('Ctrl Pts',(10.0514428414941,59.2812499997734,3.2659117547607));
#301988=CARTESIAN_POINT('Ctrl Pts',(10.0514428414941,59.4312499997728,-1.23094673026484E-15));
#301989=CARTESIAN_POINT('Ctrl Pts',(10.0514428414941,59.5812499997722,-3.26591175476071));
#301990=CARTESIAN_POINT('Ctrl Pts',(8.13178807675714,59.7312499997716,-5.90808986649102));
#301991=CARTESIAN_POINT('Ctrl Pts',(6.21213331202017,59.881249999771,-8.55026797822134));
#301992=CARTESIAN_POINT('Ctrl Pts',(3.10606665601006,60.0312499997704,-9.5594902125713));
#301993=CARTESIAN_POINT('Ctrl Pts',(-4.77833382807668E-14,60.1812499997698,
-10.5687124469213));
#301994=CARTESIAN_POINT('Ctrl Pts',(-3.10606665601016,60.3312499997692,
-9.5594902125713));
#301995=CARTESIAN_POINT('Ctrl Pts',(-6.21213331202026,60.4812499997686,
-8.55026797822134));
#301996=CARTESIAN_POINT('Ctrl Pts',(-8.13178807675724,60.6312499997679,
-5.90808986649102));
#301997=CARTESIAN_POINT('Ctrl Pts',(-10.0514428414942,60.7812499997674,
-3.2659117547607));
#301998=CARTESIAN_POINT('Ctrl Pts',(-10.0514428414942,60.9312499997667,
2.46189346052968E-15));
#301999=CARTESIAN_POINT('Ctrl Pts',(-10.0514428414942,61.0812499997661,
3.26591175476071));
#302000=CARTESIAN_POINT('Ctrl Pts',(-8.13178807675724,61.2312499997655,
5.90808986649102));
#302001=CARTESIAN_POINT('Ctrl Pts',(-6.21213331202026,61.3812499997649,
8.55026797822134));
#302002=CARTESIAN_POINT('Ctrl Pts',(-3.10606665601015,61.5312499997643,
9.5594902125713));
#302003=CARTESIAN_POINT('Ctrl Pts',(-4.60586049427516E-14,61.6812499997638,
10.5687124469213));
#302004=CARTESIAN_POINT('Ctrl Pts',(3.10606665601006,61.8312499997632,9.5594902125713));
#302005=CARTESIAN_POINT('Ctrl Pts',(6.21213331202017,61.9812499997625,8.55026797822134));
#302006=CARTESIAN_POINT('Ctrl Pts',(8.13178807675714,62.131249999762,5.90808986649102));
#302007=CARTESIAN_POINT('Ctrl Pts',(10.0514428414941,62.2812499997614,3.2659117547607));
#302008=CARTESIAN_POINT('Ctrl Pts',(10.0514428414941,62.4312499997608,-1.23094673026484E-15));
#302009=CARTESIAN_POINT('Ctrl Pts',(10.0514428414941,62.5812499997602,-3.26591175476071));
#302010=CARTESIAN_POINT('Ctrl Pts',(8.13178807675714,62.7312499997596,-5.90808986649102));
#302011=CARTESIAN_POINT('Ctrl Pts',(6.21213331202017,62.881249999759,-8.55026797822134));
#302012=CARTESIAN_POINT('Ctrl Pts',(3.10606665601006,63.0312499997584,-9.5594902125713));
#302013=CARTESIAN_POINT('Ctrl Pts',(-4.95110475524287E-14,63.1812499997578,
-10.5687124469213));
#302014=CARTESIAN_POINT('Ctrl Pts',(-3.10606665601016,63.3312499997572,
-9.5594902125713));
#302015=CARTESIAN_POINT('Ctrl Pts',(-6.21213331202027,63.4812499997565,
-8.55026797822134));
#302016=CARTESIAN_POINT('Ctrl Pts',(-8.13178807675724,63.631249999756,-5.90808986649102));
#302017=CARTESIAN_POINT('Ctrl Pts',(-10.0514428414942,63.7812499997553,
-3.2659117547607));
#302018=CARTESIAN_POINT('Ctrl Pts',(-10.0514428414942,63.9312499997548,
2.46189346052968E-15));
#302019=CARTESIAN_POINT('Ctrl Pts',(-10.0514428414942,64.0812499997541,
3.26591175476071));
#302020=CARTESIAN_POINT('Ctrl Pts',(-8.13178807675724,64.2312499997535,
5.90808986649102));
#302021=CARTESIAN_POINT('Ctrl Pts',(-6.21213331202026,64.381249999753,8.55026797822134));
#302022=CARTESIAN_POINT('Ctrl Pts',(-3.10606665601016,64.5312499997523,
9.5594902125713));
#302023=CARTESIAN_POINT('Ctrl Pts',(-4.77863142144134E-14,64.6812499997518,
10.5687124469213));
#302024=CARTESIAN_POINT('Ctrl Pts',(3.10606665601006,64.8312499997512,9.5594902125713));
#302025=CARTESIAN_POINT('Ctrl Pts',(6.21213331202017,64.9812499997506,8.55026797822134));
#302026=CARTESIAN_POINT('Ctrl Pts',(8.13178807675714,65.13124999975,5.90808986649102));
#302027=CARTESIAN_POINT('Ctrl Pts',(10.0514428414941,65.2812499997493,3.2659117547607));
#302028=CARTESIAN_POINT('Ctrl Pts',(10.0514428414941,65.4312499997488,-1.23094673026484E-15));
#302029=CARTESIAN_POINT('Ctrl Pts',(10.0514428414941,65.5812499997482,-3.26591175476071));
#302030=CARTESIAN_POINT('Ctrl Pts',(8.13178807675714,65.7312499997475,-5.90808986649102));
#302031=CARTESIAN_POINT('Ctrl Pts',(6.21213331202016,65.881249999747,-8.55026797822134));
#302032=CARTESIAN_POINT('Ctrl Pts',(3.10606665601006,66.0312499997464,-9.5594902125713));
#302033=CARTESIAN_POINT('Ctrl Pts',(-5.12387568240905E-14,66.1812499997457,
-10.5687124469213));
#302034=CARTESIAN_POINT('Ctrl Pts',(-3.10606665601016,66.3312499997451,
-9.5594902125713));
#302035=CARTESIAN_POINT('Ctrl Pts',(-6.21213331202027,66.4812499997445,
-8.55026797822134));
#302036=CARTESIAN_POINT('Ctrl Pts',(-8.13178807675724,66.6312499997439,
-5.90808986649102));
#302037=CARTESIAN_POINT('Ctrl Pts',(-10.0514428414942,66.7812499997433,
-3.2659117547607));
#302038=CARTESIAN_POINT('Ctrl Pts',(-10.0514428414942,66.9312499997427,
2.46189346052968E-15));
#302039=CARTESIAN_POINT('Ctrl Pts',(-10.0514428414942,67.0812499997421,
3.26591175476071));
#302040=CARTESIAN_POINT('Ctrl Pts',(-8.13178807675724,67.2312499997416,
5.90808986649102));
#302041=CARTESIAN_POINT('Ctrl Pts',(-6.21213331202027,67.3812499997409,
8.55026797822134));
#302042=CARTESIAN_POINT('Ctrl Pts',(-3.10606665601016,67.5312499997404,
9.5594902125713));
#302043=CARTESIAN_POINT('Ctrl Pts',(-4.95140234860752E-14,67.6812499997397,
10.5687124469213));
#302044=CARTESIAN_POINT('Ctrl Pts',(3.10606665601006,67.8312499997391,9.5594902125713));
#302045=CARTESIAN_POINT('Ctrl Pts',(6.21213331202017,67.9812499997385,8.55026797822134));
#302046=CARTESIAN_POINT('Ctrl Pts',(8.13178807675714,68.1312499997379,5.90808986649102));
#302047=CARTESIAN_POINT('Ctrl Pts',(10.0514428414941,68.2812499997374,3.2659117547607));
#302048=CARTESIAN_POINT('Ctrl Pts',(10.0514428414941,68.4312499997367,-1.23094673026484E-15));
#302049=CARTESIAN_POINT('Ctrl Pts',(10.0514428414941,68.5812499997361,-3.26591175476071));
#302050=CARTESIAN_POINT('Ctrl Pts',(8.13178807675714,68.7312499997356,-5.90808986649102));
#302051=CARTESIAN_POINT('Ctrl Pts',(6.21213331202016,68.881249999735,-8.55026797822134));
#302052=CARTESIAN_POINT('Ctrl Pts',(3.10606665601006,69.0312499997344,-9.5594902125713));
#302053=CARTESIAN_POINT('Ctrl Pts',(-5.29664660957524E-14,69.1812499997337,
-10.5687124469213));
#302054=CARTESIAN_POINT('Ctrl Pts',(-3.10606665601016,69.3312499997332,
-9.5594902125713));
#302055=CARTESIAN_POINT('Ctrl Pts',(-6.21213331202027,69.4812499997326,
-8.55026797822134));
#302056=CARTESIAN_POINT('Ctrl Pts',(-8.13178807675724,69.6312499997319,
-5.90808986649102));
#302057=CARTESIAN_POINT('Ctrl Pts',(-10.0514428414942,69.7812499997313,
-3.2659117547607));
#302058=CARTESIAN_POINT('Ctrl Pts',(-10.0514428414942,69.9312499997307,
2.46189346052968E-15));
#302059=CARTESIAN_POINT('Ctrl Pts',(-10.0514428414942,70.0812499997301,
3.26591175476071));
#302060=CARTESIAN_POINT('Ctrl Pts',(-8.13178807675724,70.2312499997295,
5.90808986649102));
#302061=CARTESIAN_POINT('Ctrl Pts',(-6.21213331202027,70.3812499997289,
8.55026797822134));
#302062=CARTESIAN_POINT('Ctrl Pts',(-3.10606665601016,70.5312499997283,
9.5594902125713));
#302063=CARTESIAN_POINT('Ctrl Pts',(-5.12417327577371E-14,70.6812499997277,
10.5687124469213));
#302064=CARTESIAN_POINT('Ctrl Pts',(3.10606665601006,70.8312499997271,9.5594902125713));
#302065=CARTESIAN_POINT('Ctrl Pts',(6.21213331202016,70.9812499997265,8.55026797822134));
#302066=CARTESIAN_POINT('Ctrl Pts',(8.13178807675714,71.131249999726,5.90808986649102));
#302067=CARTESIAN_POINT('Ctrl Pts',(10.0514428414941,71.2812499997253,3.2659117547607));
#302068=CARTESIAN_POINT('Ctrl Pts',(10.0514428414941,71.4312499997248,-1.23094673026484E-15));
#302069=CARTESIAN_POINT('Ctrl Pts',(10.0514428414941,71.5812499997242,-3.26591175476071));
#302070=CARTESIAN_POINT('Ctrl Pts',(8.13178807675713,71.7312499997236,-5.90808986649102));
#302071=CARTESIAN_POINT('Ctrl Pts',(6.21213331202016,71.881249999723,-8.55026797822134));
#302072=CARTESIAN_POINT('Ctrl Pts',(3.10606665601005,72.0312499997223,-9.5594902125713));
#302073=CARTESIAN_POINT('Ctrl Pts',(-5.46941753674142E-14,72.1812499997217,
-10.5687124469213));
#302074=CARTESIAN_POINT('Ctrl Pts',(-3.10606665601016,72.3312499997212,
-9.5594902125713));
#302075=CARTESIAN_POINT('Ctrl Pts',(-6.21213331202027,72.4812499997205,
-8.55026797822134));
#302076=CARTESIAN_POINT('Ctrl Pts',(-8.13178807675725,72.63124999972,-5.90808986649102));
#302077=CARTESIAN_POINT('Ctrl Pts',(-10.0514428414942,72.7812499997193,
-3.2659117547607));
#302078=CARTESIAN_POINT('Ctrl Pts',(-10.0514428414942,72.9312499997187,
2.46189346052968E-15));
#302079=CARTESIAN_POINT('Ctrl Pts',(-10.0514428414942,73.0812499997181,
3.26591175476071));
#302080=CARTESIAN_POINT('Ctrl Pts',(-8.13178807675725,73.2312499997175,
5.90808986649102));
#302081=CARTESIAN_POINT('Ctrl Pts',(-6.21213331202027,73.381249999717,8.55026797822134));
#302082=CARTESIAN_POINT('Ctrl Pts',(-3.10606665601016,73.5312499997164,
9.5594902125713));
#302083=CARTESIAN_POINT('Ctrl Pts',(-5.29694420293989E-14,73.6812499997157,
10.5687124469213));
#302084=CARTESIAN_POINT('Ctrl Pts',(3.10606665601005,73.8312499997151,9.5594902125713));
#302085=CARTESIAN_POINT('Ctrl Pts',(6.21213331202016,73.9812499997146,8.55026797822134));
#302086=CARTESIAN_POINT('Ctrl Pts',(8.13178807675713,74.1312499997139,5.90808986649102));
#302087=CARTESIAN_POINT('Ctrl Pts',(10.0514428414941,74.2812499997134,3.2659117547607));
#302088=CARTESIAN_POINT('Ctrl Pts',(10.0514428414941,74.4312499997127,-1.23094673026484E-15));
#302089=CARTESIAN_POINT('Ctrl Pts',(10.0514428414941,74.5812499997122,-3.26591175476071));
#302090=CARTESIAN_POINT('Ctrl Pts',(8.13178807675713,74.7312499997116,-5.90808986649102));
#302091=CARTESIAN_POINT('Ctrl Pts',(6.21213331202016,74.8812499997109,-8.55026797822134));
#302092=CARTESIAN_POINT('Ctrl Pts',(3.10606665601005,75.0312499997104,-9.5594902125713));
#302093=CARTESIAN_POINT('Ctrl Pts',(-5.6421884639076E-14,75.1812499997098,
-10.5687124469213));
#302094=CARTESIAN_POINT('Ctrl Pts',(-3.10606665601016,75.3312499997092,
-9.5594902125713));
#302095=CARTESIAN_POINT('Ctrl Pts',(-6.21213331202027,75.4812499997086,
-8.55026797822134));
#302096=CARTESIAN_POINT('Ctrl Pts',(-8.13178807675725,75.6312499997079,
-5.90808986649102));
#302097=CARTESIAN_POINT('Ctrl Pts',(-10.0514428414942,75.7812499997073,
-3.2659117547607));
#302098=CARTESIAN_POINT('Ctrl Pts',(-10.0514428414942,75.9312499997068,
2.46189346052968E-15));
#302099=CARTESIAN_POINT('Ctrl Pts',(-10.0514428414942,76.0812499997061,
3.26591175476071));
#302100=CARTESIAN_POINT('Ctrl Pts',(-8.13178807675725,76.2312499997055,
5.90808986649102));
#302101=CARTESIAN_POINT('Ctrl Pts',(-6.21213331202027,76.3812499997049,
8.55026797822134));
#302102=CARTESIAN_POINT('Ctrl Pts',(-3.10606665601016,76.5312499997043,
9.5594902125713));
#302103=CARTESIAN_POINT('Ctrl Pts',(-5.46971513010608E-14,76.6812499997037,
10.5687124469213));
#302104=CARTESIAN_POINT('Ctrl Pts',(3.10606665601005,76.8312499997031,9.5594902125713));
#302105=CARTESIAN_POINT('Ctrl Pts',(6.21213331202016,76.9812499997025,8.55026797822134));
#302106=CARTESIAN_POINT('Ctrl Pts',(8.13178807675713,77.131249999702,5.90808986649102));
#302107=CARTESIAN_POINT('Ctrl Pts',(10.0514428414941,77.2812499997013,3.2659117547607));
#302108=CARTESIAN_POINT('Ctrl Pts',(10.0514428414941,77.4312499997008,-1.23094673026484E-15));
#302109=CARTESIAN_POINT('Ctrl Pts',(10.0514428414941,77.5812499997001,-3.26591175476071));
#302110=CARTESIAN_POINT('Ctrl Pts',(8.13178807675713,77.7312499996995,-5.90808986649102));
#302111=CARTESIAN_POINT('Ctrl Pts',(6.21213331202016,77.881249999699,-8.55026797822134));
#302112=CARTESIAN_POINT('Ctrl Pts',(3.10606665601005,78.0312499996984,-9.5594902125713));
#302113=CARTESIAN_POINT('Ctrl Pts',(-5.81495939107379E-14,78.1812499996978,
-10.5687124469213));
#302114=CARTESIAN_POINT('Ctrl Pts',(-3.10606665601017,78.3312499996971,
-9.5594902125713));
#302115=CARTESIAN_POINT('Ctrl Pts',(-6.21213331202028,78.4812499996966,
-8.55026797822134));
#302116=CARTESIAN_POINT('Ctrl Pts',(-8.13178807675725,78.631249999696,-5.90808986649102));
#302117=CARTESIAN_POINT('Ctrl Pts',(-10.0514428414942,78.7812499996954,
-3.2659117547607));
#302118=CARTESIAN_POINT('Ctrl Pts',(-10.0514428414942,78.9312499996948,
2.46189346052968E-15));
#302119=CARTESIAN_POINT('Ctrl Pts',(-10.0514428414942,79.0812499996942,
3.26591175476071));
#302120=CARTESIAN_POINT('Ctrl Pts',(-8.13178807675725,79.2312499996936,
5.90808986649102));
#302121=CARTESIAN_POINT('Ctrl Pts',(-6.21213331202027,79.381249999693,8.55026797822134));
#302122=CARTESIAN_POINT('Ctrl Pts',(-3.10606665601016,79.5312499996923,
9.5594902125713));
#302123=CARTESIAN_POINT('Ctrl Pts',(-5.64248605727226E-14,79.6812499996917,
10.5687124469213));
#302124=CARTESIAN_POINT('Ctrl Pts',(3.10606665601005,79.8312499996911,9.5594902125713));
#302125=CARTESIAN_POINT('Ctrl Pts',(6.21213331202016,79.9812499996905,8.55026797822134));
#302126=CARTESIAN_POINT('Ctrl Pts',(8.13178807675713,80.1312499996899,5.90808986649102));
#302127=CARTESIAN_POINT('Ctrl Pts',(10.0514428414941,80.2812499996894,3.2659117547607));
#302128=CARTESIAN_POINT('Ctrl Pts',(10.0514428414941,80.4312499996887,-1.23094673026484E-15));
#302129=CARTESIAN_POINT('Ctrl Pts',(10.0514428414941,80.5812499996882,-3.26591175476071));
#302130=CARTESIAN_POINT('Ctrl Pts',(8.13178807675713,80.7312499996875,-5.90808986649102));
#302131=CARTESIAN_POINT('Ctrl Pts',(6.21213331202016,80.881249999687,-8.55026797822134));
#302132=CARTESIAN_POINT('Ctrl Pts',(3.10606665601005,81.0312499996864,-9.5594902125713));
#302133=CARTESIAN_POINT('Ctrl Pts',(-5.98773031823997E-14,81.1812499996858,
-10.5687124469213));
#302134=CARTESIAN_POINT('Ctrl Pts',(-3.10606665601017,81.3312499996851,
-9.5594902125713));
#302135=CARTESIAN_POINT('Ctrl Pts',(-6.21213331202028,81.4812499996845,
-8.55026797822134));
#302136=CARTESIAN_POINT('Ctrl Pts',(-8.13178807675725,81.6312499996839,
-5.90808986649102));
#302137=CARTESIAN_POINT('Ctrl Pts',(-10.0514428414942,81.7812499996834,
-3.2659117547607));
#302138=CARTESIAN_POINT('Ctrl Pts',(-10.0514428414942,81.9312499996827,
2.46189346052968E-15));
#302139=CARTESIAN_POINT('Ctrl Pts',(-10.0514428414942,82.0812499996821,
3.26591175476071));
#302140=CARTESIAN_POINT('Ctrl Pts',(-8.13178807675725,82.2312499996816,
5.90808986649102));
#302141=CARTESIAN_POINT('Ctrl Pts',(-6.21213331202028,82.381249999681,8.55026797822134));
#302142=CARTESIAN_POINT('Ctrl Pts',(-3.10606665601017,82.5312499996804,
9.5594902125713));
#302143=CARTESIAN_POINT('Ctrl Pts',(-5.81525698443845E-14,82.6812499996797,
10.5687124469213));
#302144=CARTESIAN_POINT('Ctrl Pts',(3.10606665601005,82.8312499996792,9.5594902125713));
#302145=CARTESIAN_POINT('Ctrl Pts',(6.21213331202016,82.9812499996786,8.55026797822134));
#302146=CARTESIAN_POINT('Ctrl Pts',(8.13178807675713,83.131249999678,5.90808986649102));
#302147=CARTESIAN_POINT('Ctrl Pts',(10.0514428414941,83.2812499996773,3.2659117547607));
#302148=CARTESIAN_POINT('Ctrl Pts',(10.0514428414941,83.4312499996767,-1.23094673026484E-15));
#302149=CARTESIAN_POINT('Ctrl Pts',(10.0514428414941,83.5812499996761,-3.26591175476071));
#302150=CARTESIAN_POINT('Ctrl Pts',(8.13178807675713,83.7312499996756,-5.90808986649102));
#302151=CARTESIAN_POINT('Ctrl Pts',(6.21213331202016,83.8812499996749,-8.55026797822134));
#302152=CARTESIAN_POINT('Ctrl Pts',(3.10606665601005,84.0312499996743,-9.5594902125713));
#302153=CARTESIAN_POINT('Ctrl Pts',(-6.16050124540615E-14,84.1812499996738,
-10.5687124469213));
#302154=CARTESIAN_POINT('Ctrl Pts',(-3.10606665601017,84.3312499996732,
-9.5594902125713));
#302155=CARTESIAN_POINT('Ctrl Pts',(-6.21213331202028,84.4812499996725,
-8.55026797822134));
#302156=CARTESIAN_POINT('Ctrl Pts',(-8.13178807675725,84.631249999672,-5.90808986649102));
#302157=CARTESIAN_POINT('Ctrl Pts',(-10.0514428414942,84.7812499996714,
-3.2659117547607));
#302158=CARTESIAN_POINT('Ctrl Pts',(-10.0514428414942,84.9312499996708,
2.46189346052968E-15));
#302159=CARTESIAN_POINT('Ctrl Pts',(-10.0514428414942,85.0812499996701,
3.26591175476071));
#302160=CARTESIAN_POINT('Ctrl Pts',(-8.13178807675725,85.2312499996695,
5.90808986649102));
#302161=CARTESIAN_POINT('Ctrl Pts',(-6.21213331202028,85.381249999669,8.55026797822134));
#302162=CARTESIAN_POINT('Ctrl Pts',(-3.10606665601017,85.5312499996683,
9.5594902125713));
#302163=CARTESIAN_POINT('Ctrl Pts',(-5.98802791160463E-14,85.6812499996678,
10.5687124469213));
#302164=CARTESIAN_POINT('Ctrl Pts',(3.10606665601005,85.8312499996672,9.5594902125713));
#302165=CARTESIAN_POINT('Ctrl Pts',(6.21213331202016,85.9812499996666,8.55026797822134));
#302166=CARTESIAN_POINT('Ctrl Pts',(8.13178807675713,86.1312499996659,5.90808986649102));
#302167=CARTESIAN_POINT('Ctrl Pts',(10.0514428414941,86.2812499996653,3.2659117547607));
#302168=CARTESIAN_POINT('Ctrl Pts',(10.0514428414941,86.4312499996647,-1.23094673026484E-15));
#302169=CARTESIAN_POINT('Ctrl Pts',(10.0514428414941,86.5812499996642,-3.26591175476071));
#302170=CARTESIAN_POINT('Ctrl Pts',(8.13178807675713,86.7312499996635,-5.90808986649102));
#302171=CARTESIAN_POINT('Ctrl Pts',(6.21213331202015,86.8812499996629,-8.55026797822134));
#302172=CARTESIAN_POINT('Ctrl Pts',(3.10606665601004,87.0312499996624,-9.5594902125713));
#302173=CARTESIAN_POINT('Ctrl Pts',(-6.33327217257234E-14,87.1812499996618,
-10.5687124469213));
#302174=CARTESIAN_POINT('Ctrl Pts',(-3.10606665601017,87.3312499996611,
-9.5594902125713));
#302175=CARTESIAN_POINT('Ctrl Pts',(-6.21213331202028,87.4812499996605,
-8.55026797822134));
#302176=CARTESIAN_POINT('Ctrl Pts',(-8.13178807675726,87.6312499996599,
-5.90808986649102));
#302177=CARTESIAN_POINT('Ctrl Pts',(-10.0514428414942,87.7812499996594,
-3.2659117547607));
#302178=CARTESIAN_POINT('Ctrl Pts',(-10.0514428414942,87.9312499996587,
2.46189346052968E-15));
#302179=CARTESIAN_POINT('Ctrl Pts',(-10.0514428414942,88.0812499996581,
3.26591175476071));
#302180=CARTESIAN_POINT('Ctrl Pts',(-8.13178807675726,88.2312499996575,
5.90808986649102));
#302181=CARTESIAN_POINT('Ctrl Pts',(-6.21213331202028,88.3812499996569,
8.55026797822134));
#302182=CARTESIAN_POINT('Ctrl Pts',(-3.10606665601017,88.5312499996564,
9.5594902125713));
#302183=CARTESIAN_POINT('Ctrl Pts',(-6.16079883877081E-14,88.6812499996557,
10.5687124469213));
#302184=CARTESIAN_POINT('Ctrl Pts',(3.10606665601005,88.8312499996552,9.5594902125713));
#302185=CARTESIAN_POINT('Ctrl Pts',(6.21213331202016,88.9812499996546,8.55026797822134));
#302186=CARTESIAN_POINT('Ctrl Pts',(8.13178807675713,89.131249999654,5.90808986649102));
#302187=CARTESIAN_POINT('Ctrl Pts',(10.0514428414941,89.2812499996533,3.2659117547607));
#302188=CARTESIAN_POINT('Ctrl Pts',(10.0514428414941,89.4312499996527,-1.23094673026484E-15));
#302189=CARTESIAN_POINT('Ctrl Pts',(10.0514428414941,89.5812499996521,-3.26591175476071));
#302190=CARTESIAN_POINT('Ctrl Pts',(8.13178807675713,89.7312499996515,-5.90808986649102));
#302191=CARTESIAN_POINT('Ctrl Pts',(6.21213331202015,89.8812499996509,-8.55026797822134));
#302192=CARTESIAN_POINT('Ctrl Pts',(3.10606665601004,90.0312499996504,-9.5594902125713));
#302193=CARTESIAN_POINT('Ctrl Pts',(-6.50604309973852E-14,90.1812499996498,
-10.5687124469213));
#302194=CARTESIAN_POINT('Ctrl Pts',(-3.10606665601017,90.3312499996491,
-9.5594902125713));
#302195=CARTESIAN_POINT('Ctrl Pts',(-6.21213331202028,90.4812499996485,
-8.55026797822134));
#302196=CARTESIAN_POINT('Ctrl Pts',(-8.13178807675726,90.631249999648,-5.90808986649102));
#302197=CARTESIAN_POINT('Ctrl Pts',(-10.0514428414942,90.7812499996473,
-3.2659117547607));
#302198=CARTESIAN_POINT('Ctrl Pts',(-10.0514428414942,90.9312499996468,
2.46189346052968E-15));
#302199=CARTESIAN_POINT('Ctrl Pts',(-10.0514428414942,91.0812499996461,
3.26591175476071));
#302200=CARTESIAN_POINT('Ctrl Pts',(-8.13178807675726,91.2312499996455,
5.90808986649102));
#302201=CARTESIAN_POINT('Ctrl Pts',(-6.21213331202028,91.381249999645,8.55026797822134));
#302202=CARTESIAN_POINT('Ctrl Pts',(-3.10606665601017,91.5312499996443,
9.5594902125713));
#302203=CARTESIAN_POINT('Ctrl Pts',(-6.333569765937E-14,91.6812499996438,
10.5687124469213));
#302204=CARTESIAN_POINT('Ctrl Pts',(3.10606665601004,91.8312499996431,9.5594902125713));
#302205=CARTESIAN_POINT('Ctrl Pts',(6.21213331202015,91.9812499996426,8.55026797822134));
#302206=CARTESIAN_POINT('Ctrl Pts',(8.13178807675712,92.131249999642,5.90808986649102));
#302207=CARTESIAN_POINT('Ctrl Pts',(10.0514428414941,92.2812499996414,3.2659117547607));
#302208=CARTESIAN_POINT('Ctrl Pts',(10.0514428414941,92.4312499996408,-1.23094673026484E-15));
#302209=CARTESIAN_POINT('Ctrl Pts',(10.0514428414941,92.5812499996402,-3.26591175476071));
#302210=CARTESIAN_POINT('Ctrl Pts',(8.13178807675712,92.7312499996396,-5.90808986649102));
#302211=CARTESIAN_POINT('Ctrl Pts',(6.21213331202015,92.8812499996389,-8.55026797822134));
#302212=CARTESIAN_POINT('Ctrl Pts',(3.10606665601004,93.0312499996383,-9.5594902125713));
#302213=CARTESIAN_POINT('Ctrl Pts',(-6.67881402690471E-14,93.1812499996377,
-10.5687124469213));
#302214=CARTESIAN_POINT('Ctrl Pts',(-3.10606665601018,93.3312499996371,
-9.5594902125713));
#302215=CARTESIAN_POINT('Ctrl Pts',(-6.21213331202028,93.4812499996365,
-8.55026797822134));
#302216=CARTESIAN_POINT('Ctrl Pts',(-8.13178807675726,93.6312499996359,
-5.90808986649102));
#302217=CARTESIAN_POINT('Ctrl Pts',(-10.0514428414942,93.7812499996353,
-3.2659117547607));
#302218=CARTESIAN_POINT('Ctrl Pts',(-10.0514428414942,93.9312499996347,
2.46189346052968E-15));
#302219=CARTESIAN_POINT('Ctrl Pts',(-10.0514428414942,94.0812499996341,
3.26591175476071));
#302220=CARTESIAN_POINT('Ctrl Pts',(-8.13178807675726,94.2312499996335,
5.90808986649102));
#302221=CARTESIAN_POINT('Ctrl Pts',(-6.21213331202028,94.381249999633,8.55026797822134));
#302222=CARTESIAN_POINT('Ctrl Pts',(-3.10606665601017,94.5312499996324,
9.5594902125713));
#302223=CARTESIAN_POINT('Ctrl Pts',(-6.50634069310318E-14,94.6812499996317,
10.5687124469213));
#302224=CARTESIAN_POINT('Ctrl Pts',(3.10606665601004,94.8312499996312,9.5594902125713));
#302225=CARTESIAN_POINT('Ctrl Pts',(6.21213331202015,94.9812499996306,8.55026797822134));
#302226=CARTESIAN_POINT('Ctrl Pts',(8.13178807675712,95.13124999963,5.90808986649102));
#302227=CARTESIAN_POINT('Ctrl Pts',(10.0514428414941,95.2812499996293,3.2659117547607));
#302228=CARTESIAN_POINT('Ctrl Pts',(10.0514428414941,95.4312499996288,-1.23094673026484E-15));
#302229=CARTESIAN_POINT('Ctrl Pts',(10.0514428414941,95.5812499996282,-3.26591175476071));
#302230=CARTESIAN_POINT('Ctrl Pts',(8.13178807675712,95.7312499996276,-5.90808986649102));
#302231=CARTESIAN_POINT('Ctrl Pts',(6.21213331202015,95.8812499996269,-8.55026797822134));
#302232=CARTESIAN_POINT('Ctrl Pts',(3.10606665601004,96.0312499996264,-9.5594902125713));
#302233=CARTESIAN_POINT('Ctrl Pts',(-6.85158495407089E-14,96.1812499996257,
-10.5687124469213));
#302234=CARTESIAN_POINT('Ctrl Pts',(-3.10606665601018,96.3312499996252,
-9.5594902125713));
#302235=CARTESIAN_POINT('Ctrl Pts',(-6.21213331202028,96.4812499996245,
-8.55026797822134));
#302236=CARTESIAN_POINT('Ctrl Pts',(-8.13178807675726,96.6312499996239,
-5.90808986649102));
#302237=CARTESIAN_POINT('Ctrl Pts',(-10.0514428414942,96.7812499996234,
-3.2659117547607));
#302238=CARTESIAN_POINT('Ctrl Pts',(-10.0514428414942,96.9312499996227,
2.46189346052968E-15));
#302239=CARTESIAN_POINT('Ctrl Pts',(-10.0514428414942,97.0812499996221,
3.26591175476071));
#302240=CARTESIAN_POINT('Ctrl Pts',(-8.13178807675726,97.2312499996215,
5.90808986649102));
#302241=CARTESIAN_POINT('Ctrl Pts',(-6.21213331202028,97.381249999621,8.55026797822134));
#302242=CARTESIAN_POINT('Ctrl Pts',(-3.10606665601017,97.5312499996203,
9.5594902125713));
#302243=CARTESIAN_POINT('Ctrl Pts',(-6.67911162026936E-14,97.6812499996197,
10.5687124469213));
#302244=CARTESIAN_POINT('Ctrl Pts',(3.10606665601004,97.8312499996191,9.5594902125713));
#302245=CARTESIAN_POINT('Ctrl Pts',(6.21213331202015,97.9812499996186,8.55026797822134));
#302246=CARTESIAN_POINT('Ctrl Pts',(8.13178807675712,98.1312499996179,5.90808986649102));
#302247=CARTESIAN_POINT('Ctrl Pts',(10.0514428414941,98.2812499996173,3.2659117547607));
#302248=CARTESIAN_POINT('Ctrl Pts',(10.0514428414941,98.4312499996168,-1.23094673026484E-15));
#302249=CARTESIAN_POINT('Ctrl Pts',(10.0514428414941,98.5812499996162,-3.26591175476071));
#302250=CARTESIAN_POINT('Ctrl Pts',(8.13178807675712,98.7312499996156,-5.90808986649102));
#302251=CARTESIAN_POINT('Ctrl Pts',(6.21213331202015,98.8812499996149,-8.55026797822134));
#302252=CARTESIAN_POINT('Ctrl Pts',(3.10606665601004,99.0312499996143,-9.5594902125713));
#302253=CARTESIAN_POINT('Ctrl Pts',(-7.02435588123707E-14,99.1812499996138,
-10.5687124469213));
#302254=CARTESIAN_POINT('Ctrl Pts',(-3.10606665601018,99.3312499996131,
-9.5594902125713));
#302255=CARTESIAN_POINT('Ctrl Pts',(-6.21213331202028,99.4812499996125,
-8.55026797822134));
#302256=CARTESIAN_POINT('Ctrl Pts',(-8.13178807675726,99.631249999612,-5.90808986649102));
#302257=CARTESIAN_POINT('Ctrl Pts',(-10.0514428414942,99.7812499996113,
-3.2659117547607));
#302258=CARTESIAN_POINT('Ctrl Pts',(-10.0514428414942,99.9312499996108,
2.46189346052968E-15));
#302259=CARTESIAN_POINT('Ctrl Pts',(-10.0514428414942,100.08124999961,3.26591175476071));
#302260=CARTESIAN_POINT('Ctrl Pts',(-8.13178807675726,100.23124999961,5.90808986649102));
#302261=CARTESIAN_POINT('Ctrl Pts',(-6.21213331202028,100.381249999609,
8.55026797822134));
#302262=CARTESIAN_POINT('Ctrl Pts',(-3.10606665601018,100.531249999608,
9.5594902125713));
#302263=CARTESIAN_POINT('Ctrl Pts',(-6.85188254743555E-14,100.681249999608,
10.5687124469213));
#302264=CARTESIAN_POINT('Ctrl Pts',(3.10606665601004,100.831249999607,9.5594902125713));
#302265=CARTESIAN_POINT('Ctrl Pts',(6.21213331202015,100.981249999607,8.55026797822134));
#302266=CARTESIAN_POINT('Ctrl Pts',(8.13178807675712,101.131249999606,5.90808986649102));
#302267=CARTESIAN_POINT('Ctrl Pts',(10.0514428414941,101.281249999605,3.2659117547607));
#302268=CARTESIAN_POINT('Ctrl Pts',(10.0514428414941,101.431249999605,-1.23094673026484E-15));
#302269=CARTESIAN_POINT('Ctrl Pts',(10.0514428414941,101.581249999604,-3.26591175476071));
#302270=CARTESIAN_POINT('Ctrl Pts',(8.13178807675712,101.731249999604,-5.90808986649102));
#302271=CARTESIAN_POINT('Ctrl Pts',(6.21213331202014,101.881249999603,-8.55026797822134));
#302272=CARTESIAN_POINT('Ctrl Pts',(3.10606665601004,102.031249999602,-9.5594902125713));
#302273=CARTESIAN_POINT('Ctrl Pts',(-7.19712680840326E-14,102.181249999602,
-10.5687124469213));
#302274=CARTESIAN_POINT('Ctrl Pts',(-3.10606665601018,102.331249999601,
-9.5594902125713));
#302275=CARTESIAN_POINT('Ctrl Pts',(-6.21213331202029,102.481249999601,
-8.55026797822134));
#302276=CARTESIAN_POINT('Ctrl Pts',(-8.13178807675726,102.6312499996,-5.90808986649102));
#302277=CARTESIAN_POINT('Ctrl Pts',(-10.0514428414942,102.781249999599,
-3.2659117547607));
#302278=CARTESIAN_POINT('Ctrl Pts',(-10.0514428414942,102.931249999599,
2.46189346052968E-15));
#302279=CARTESIAN_POINT('Ctrl Pts',(-10.0514428414942,103.081249999598,
3.26591175476071));
#302280=CARTESIAN_POINT('Ctrl Pts',(-8.13178807675726,103.231249999598,
5.90808986649102));
#302281=CARTESIAN_POINT('Ctrl Pts',(-6.21213331202028,103.381249999597,
8.55026797822134));
#302282=CARTESIAN_POINT('Ctrl Pts',(-3.10606665601018,103.531249999596,
9.5594902125713));
#302283=CARTESIAN_POINT('Ctrl Pts',(-7.02465347460173E-14,103.681249999596,
10.5687124469213));
#302284=CARTESIAN_POINT('Ctrl Pts',(3.10606665601004,103.831249999595,9.5594902125713));
#302285=CARTESIAN_POINT('Ctrl Pts',(6.21213331202015,103.981249999595,8.55026797822134));
#302286=CARTESIAN_POINT('Ctrl Pts',(8.13178807675712,104.131249999594,5.90808986649102));
#302287=CARTESIAN_POINT('Ctrl Pts',(10.0514428414941,104.281249999593,3.2659117547607));
#302288=CARTESIAN_POINT('Ctrl Pts',(10.0514428414941,104.431249999593,-1.23094673026484E-15));
#302289=CARTESIAN_POINT('Ctrl Pts',(10.0514428414941,104.581249999592,-3.26591175476071));
#302290=CARTESIAN_POINT('Ctrl Pts',(8.13178807675712,104.731249999592,-5.90808986649102));
#302291=CARTESIAN_POINT('Ctrl Pts',(6.21213331202014,104.881249999591,-8.55026797822134));
#302292=CARTESIAN_POINT('Ctrl Pts',(3.10606665601003,105.03124999959,-9.5594902125713));
#302293=CARTESIAN_POINT('Ctrl Pts',(-7.36989773556944E-14,105.18124999959,
-10.5687124469213));
#302294=CARTESIAN_POINT('Ctrl Pts',(-3.10606665601018,105.331249999589,
-9.5594902125713));
#302295=CARTESIAN_POINT('Ctrl Pts',(-6.21213331202029,105.481249999589,
-8.55026797822134));
#302296=CARTESIAN_POINT('Ctrl Pts',(-8.13178807675726,105.631249999588,
-5.90808986649102));
#302297=CARTESIAN_POINT('Ctrl Pts',(-10.0514428414942,105.781249999587,
-3.2659117547607));
#302298=CARTESIAN_POINT('Ctrl Pts',(-10.0514428414942,105.931249999587,
2.46189346052968E-15));
#302299=CARTESIAN_POINT('Ctrl Pts',(-10.0514428414942,106.081249999586,
3.26591175476071));
#302300=CARTESIAN_POINT('Ctrl Pts',(-8.13178807675726,106.231249999586,
5.90808986649102));
#302301=CARTESIAN_POINT('Ctrl Pts',(-6.21213331202029,106.381249999585,
8.55026797822134));
#302302=CARTESIAN_POINT('Ctrl Pts',(-3.10606665601018,106.531249999584,
9.5594902125713));
#302303=CARTESIAN_POINT('Ctrl Pts',(-7.19742440176792E-14,106.681249999584,
10.5687124469213));
#302304=CARTESIAN_POINT('Ctrl Pts',(3.10606665601004,106.831249999583,9.5594902125713));
#302305=CARTESIAN_POINT('Ctrl Pts',(6.21213331202014,106.981249999583,8.55026797822134));
#302306=CARTESIAN_POINT('Ctrl Pts',(8.13178807675711,107.131249999582,5.90808986649102));
#302307=CARTESIAN_POINT('Ctrl Pts',(10.0514428414941,107.281249999581,3.2659117547607));
#302308=CARTESIAN_POINT('Ctrl Pts',(10.0514428414941,107.431249999581,-1.23094673026484E-15));
#302309=CARTESIAN_POINT('Ctrl Pts',(10.0514428414941,107.58124999958,-3.26591175476071));
#302310=CARTESIAN_POINT('Ctrl Pts',(8.13178807675711,107.73124999958,-5.90808986649102));
#302311=CARTESIAN_POINT('Ctrl Pts',(6.21213331202014,107.881249999579,-8.55026797822134));
#302312=CARTESIAN_POINT('Ctrl Pts',(3.10606665601003,108.031249999578,-9.5594902125713));
#302313=CARTESIAN_POINT('Ctrl Pts',(-7.54266866273562E-14,108.181249999578,
-10.5687124469213));
#302314=CARTESIAN_POINT('Ctrl Pts',(-3.10606665601018,108.331249999577,
-9.5594902125713));
#302315=CARTESIAN_POINT('Ctrl Pts',(-6.21213331202029,108.481249999577,
-8.55026797822134));
#302316=CARTESIAN_POINT('Ctrl Pts',(-8.13178807675727,108.631249999576,
-5.90808986649102));
#302317=CARTESIAN_POINT('Ctrl Pts',(-10.0514428414942,108.781249999575,
-3.2659117547607));
#302318=CARTESIAN_POINT('Ctrl Pts',(-10.0514428414942,108.931249999575,
2.46189346052968E-15));
#302319=CARTESIAN_POINT('Ctrl Pts',(-10.0514428414942,109.081249999574,
3.26591175476071));
#302320=CARTESIAN_POINT('Ctrl Pts',(-8.13178807675727,109.231249999574,
5.90808986649102));
#302321=CARTESIAN_POINT('Ctrl Pts',(-6.21213331202029,109.381249999573,
8.55026797822134));
#302322=CARTESIAN_POINT('Ctrl Pts',(-3.10606665601018,109.531249999572,
9.5594902125713));
#302323=CARTESIAN_POINT('Ctrl Pts',(-7.3701953289341E-14,109.681249999572,
10.5687124469213));
#302324=CARTESIAN_POINT('Ctrl Pts',(3.10606665601003,109.831249999571,9.5594902125713));
#302325=CARTESIAN_POINT('Ctrl Pts',(6.21213331202014,109.981249999571,8.55026797822134));
#302326=CARTESIAN_POINT('Ctrl Pts',(8.13178807675711,110.13124999957,5.90808986649102));
#302327=CARTESIAN_POINT('Ctrl Pts',(10.0514428414941,110.281249999569,3.2659117547607));
#302328=CARTESIAN_POINT('Ctrl Pts',(10.0514428414941,110.431249999569,-1.23094673026484E-15));
#302329=CARTESIAN_POINT('Ctrl Pts',(10.0514428414941,110.581249999568,-3.26591175476071));
#302330=CARTESIAN_POINT('Ctrl Pts',(8.13178807675711,110.731249999568,-5.90808986649102));
#302331=CARTESIAN_POINT('Ctrl Pts',(6.21213331202014,110.881249999567,-8.55026797822134));
#302332=CARTESIAN_POINT('Ctrl Pts',(3.10606665601003,111.031249999566,-9.5594902125713));
#302333=CARTESIAN_POINT('Ctrl Pts',(-7.71543958990181E-14,111.181249999566,
-10.5687124469213));
#302334=CARTESIAN_POINT('Ctrl Pts',(-3.10606665601019,111.331249999565,
-9.5594902125713));
#302335=CARTESIAN_POINT('Ctrl Pts',(-6.21213331202029,111.481249999565,
-8.55026797822134));
#302336=CARTESIAN_POINT('Ctrl Pts',(-8.13178807675727,111.631249999564,
-5.90808986649102));
#302337=CARTESIAN_POINT('Ctrl Pts',(-10.0514428414942,111.781249999563,
-3.2659117547607));
#302338=CARTESIAN_POINT('Ctrl Pts',(-10.0514428414942,111.931249999563,
2.46189346052968E-15));
#302339=CARTESIAN_POINT('Ctrl Pts',(-10.0514428414942,112.081249999562,
3.26591175476071));
#302340=CARTESIAN_POINT('Ctrl Pts',(-8.13178807675727,112.231249999562,
5.90808986649102));
#302341=CARTESIAN_POINT('Ctrl Pts',(-6.21213331202029,112.381249999561,
8.55026797822134));
#302342=CARTESIAN_POINT('Ctrl Pts',(-3.10606665601018,112.53124999956,9.5594902125713));
#302343=CARTESIAN_POINT('Ctrl Pts',(-7.54296625610028E-14,112.68124999956,
10.5687124469213));
#302344=CARTESIAN_POINT('Ctrl Pts',(3.10606665601003,112.831249999559,9.5594902125713));
#302345=CARTESIAN_POINT('Ctrl Pts',(6.21213331202014,112.981249999559,8.55026797822134));
#302346=CARTESIAN_POINT('Ctrl Pts',(8.13178807675711,113.131249999558,5.90808986649102));
#302347=CARTESIAN_POINT('Ctrl Pts',(10.0514428414941,113.281249999557,3.2659117547607));
#302348=CARTESIAN_POINT('Ctrl Pts',(10.0514428414941,113.431249999557,-1.23094673026484E-15));
#302349=CARTESIAN_POINT('Ctrl Pts',(10.0514428414941,113.581249999556,-3.26591175476071));
#302350=CARTESIAN_POINT('Ctrl Pts',(8.13178807675711,113.731249999556,-5.90808986649102));
#302351=CARTESIAN_POINT('Ctrl Pts',(6.21213331202014,113.881249999555,-8.55026797822134));
#302352=CARTESIAN_POINT('Ctrl Pts',(3.10606665601003,114.031249999554,-9.5594902125713));
#302353=CARTESIAN_POINT('Ctrl Pts',(-7.88821051706799E-14,114.181249999554,
-10.5687124469213));
#302354=CARTESIAN_POINT('Ctrl Pts',(-3.10606665601019,114.331249999553,
-9.5594902125713));
#302355=CARTESIAN_POINT('Ctrl Pts',(-6.2121333120203,114.481249999553,-8.55026797822134));
#302356=CARTESIAN_POINT('Ctrl Pts',(-8.13178807675727,114.631249999552,
-5.90808986649102));
#302357=CARTESIAN_POINT('Ctrl Pts',(-10.0514428414942,114.781249999551,
-3.2659117547607));
#302358=CARTESIAN_POINT('Ctrl Pts',(-10.0514428414942,114.931249999551,
2.46189346052968E-15));
#302359=CARTESIAN_POINT('Ctrl Pts',(-10.0514428414942,115.08124999955,3.26591175476071));
#302360=CARTESIAN_POINT('Ctrl Pts',(-8.13178807675727,115.23124999955,5.90808986649102));
#302361=CARTESIAN_POINT('Ctrl Pts',(-6.21213331202029,115.381249999549,
8.55026797822134));
#302362=CARTESIAN_POINT('Ctrl Pts',(-3.10606665601018,115.531249999548,
9.5594902125713));
#302363=CARTESIAN_POINT('Ctrl Pts',(-7.71573718326647E-14,115.681249999548,
10.5687124469213));
#302364=CARTESIAN_POINT('Ctrl Pts',(3.10606665601003,115.831249999547,9.5594902125713));
#302365=CARTESIAN_POINT('Ctrl Pts',(6.21213331202014,115.981249999547,8.55026797822134));
#302366=CARTESIAN_POINT('Ctrl Pts',(8.13178807675711,116.131249999546,5.90808986649102));
#302367=CARTESIAN_POINT('Ctrl Pts',(10.0514428414941,116.281249999545,3.2659117547607));
#302368=CARTESIAN_POINT('Ctrl Pts',(10.0514428414941,116.431249999545,-1.23094673026484E-15));
#302369=CARTESIAN_POINT('Ctrl Pts',(10.0514428414941,116.581249999544,-3.26591175476071));
#302370=CARTESIAN_POINT('Ctrl Pts',(8.13178807675711,116.731249999544,-5.90808986649102));
#302371=CARTESIAN_POINT('Ctrl Pts',(6.21213331202014,116.881249999543,-8.55026797822134));
#302372=CARTESIAN_POINT('Ctrl Pts',(3.10606665601003,117.031249999542,-9.5594902125713));
#302373=CARTESIAN_POINT('Ctrl Pts',(-8.06098144423418E-14,117.181249999542,
-10.5687124469213));
#302374=CARTESIAN_POINT('Ctrl Pts',(-3.10606665601019,117.331249999541,
-9.5594902125713));
#302375=CARTESIAN_POINT('Ctrl Pts',(-6.2121333120203,117.481249999541,-8.55026797822134));
#302376=CARTESIAN_POINT('Ctrl Pts',(-8.13178807675727,117.63124999954,-5.90808986649102));
#302377=CARTESIAN_POINT('Ctrl Pts',(-10.0514428414942,117.781249999539,
-3.2659117547607));
#302378=CARTESIAN_POINT('Ctrl Pts',(-10.0514428414942,117.931249999539,
2.46189346052968E-15));
#302379=CARTESIAN_POINT('Ctrl Pts',(-10.0514428414942,118.081249999538,
3.26591175476071));
#302380=CARTESIAN_POINT('Ctrl Pts',(-8.13178807675727,118.231249999538,
5.90808986649102));
#302381=CARTESIAN_POINT('Ctrl Pts',(-6.2121333120203,118.381249999537,8.55026797822134));
#302382=CARTESIAN_POINT('Ctrl Pts',(-3.10606665601019,118.531249999536,
9.5594902125713));
#302383=CARTESIAN_POINT('Ctrl Pts',(-7.88850811043265E-14,118.681249999536,
10.5687124469213));
#302384=CARTESIAN_POINT('Ctrl Pts',(3.10606665601003,118.831249999535,9.5594902125713));
#302385=CARTESIAN_POINT('Ctrl Pts',(6.21213331202014,118.981249999535,8.55026797822134));
#302386=CARTESIAN_POINT('Ctrl Pts',(8.13178807675711,119.131249999534,5.90808986649102));
#302387=CARTESIAN_POINT('Ctrl Pts',(10.0514428414941,119.281249999533,3.2659117547607));
#302388=CARTESIAN_POINT('Ctrl Pts',(10.0514428414941,119.431249999533,-1.23094673026484E-15));
#302389=CARTESIAN_POINT('Ctrl Pts',(10.0514428414941,119.581249999532,-3.26591175476071));
#302390=CARTESIAN_POINT('Ctrl Pts',(8.13178807675711,119.731249999532,-5.90808986649102));
#302391=CARTESIAN_POINT('Ctrl Pts',(6.21213331202013,119.881249999531,-8.55026797822134));
#302392=CARTESIAN_POINT('Ctrl Pts',(3.10606665601003,120.03124999953,-9.5594902125713));
#302393=CARTESIAN_POINT('Ctrl Pts',(-8.23375237140036E-14,120.18124999953,
-10.5687124469213));
#302394=CARTESIAN_POINT('Ctrl Pts',(-3.10606665601019,120.331249999529,
-9.5594902125713));
#302395=CARTESIAN_POINT('Ctrl Pts',(-6.2121333120203,120.481249999529,-8.55026797822134));
#302396=CARTESIAN_POINT('Ctrl Pts',(-8.13178807675727,120.631249999528,
-5.90808986649102));
#302397=CARTESIAN_POINT('Ctrl Pts',(-10.0514428414943,120.781249999527,
-3.2659117547607));
#302398=CARTESIAN_POINT('Ctrl Pts',(-10.0514428414943,120.931249999527,
2.46189346052968E-15));
#302399=CARTESIAN_POINT('Ctrl Pts',(-10.0514428414943,121.081249999526,
3.26591175476071));
#302400=CARTESIAN_POINT('Ctrl Pts',(-8.13178807675727,121.231249999526,
5.90808986649102));
#302401=CARTESIAN_POINT('Ctrl Pts',(-6.2121333120203,121.381249999525,8.55026797822134));
#302402=CARTESIAN_POINT('Ctrl Pts',(-3.10606665601019,121.531249999524,
9.5594902125713));
#302403=CARTESIAN_POINT('Ctrl Pts',(-8.06127903759884E-14,121.681249999524,
10.5687124469213));
#302404=CARTESIAN_POINT('Ctrl Pts',(3.10606665601003,121.831249999523,9.5594902125713));
#302405=CARTESIAN_POINT('Ctrl Pts',(6.21213331202014,121.981249999523,8.55026797822134));
#302406=CARTESIAN_POINT('Ctrl Pts',(8.13178807675711,122.131249999522,5.90808986649102));
#302407=CARTESIAN_POINT('Ctrl Pts',(10.0514428414941,122.281249999521,3.2659117547607));
#302408=CARTESIAN_POINT('Ctrl Pts',(10.0514428414941,122.431249999521,-1.23094673026484E-15));
#302409=CARTESIAN_POINT('Ctrl Pts',(10.0514428414941,122.58124999952,-3.26591175476071));
#302410=CARTESIAN_POINT('Ctrl Pts',(8.13178807675711,122.73124999952,-5.90808986649102));
#302411=CARTESIAN_POINT('Ctrl Pts',(6.21213331202013,122.881249999519,-8.55026797822134));
#302412=CARTESIAN_POINT('Ctrl Pts',(3.10606665601002,123.031249999518,-9.5594902125713));
#302413=CARTESIAN_POINT('Ctrl Pts',(-8.40652329856655E-14,123.181249999518,
-10.5687124469213));
#302414=CARTESIAN_POINT('Ctrl Pts',(-3.10606665601019,123.331249999517,
-9.5594902125713));
#302415=CARTESIAN_POINT('Ctrl Pts',(-6.2121333120203,123.481249999517,-8.55026797822134));
#302416=CARTESIAN_POINT('Ctrl Pts',(-8.13178807675727,123.631249999516,
-5.90808986649102));
#302417=CARTESIAN_POINT('Ctrl Pts',(-10.0514428414943,123.781249999515,
-3.2659117547607));
#302418=CARTESIAN_POINT('Ctrl Pts',(-10.0514428414943,123.931249999515,
2.46189346052968E-15));
#302419=CARTESIAN_POINT('Ctrl Pts',(-10.0514428414943,124.081249999514,
3.26591175476071));
#302420=CARTESIAN_POINT('Ctrl Pts',(-8.13178807675727,124.231249999514,
5.90808986649102));
#302421=CARTESIAN_POINT('Ctrl Pts',(-6.2121333120203,124.381249999513,8.55026797822134));
#302422=CARTESIAN_POINT('Ctrl Pts',(-3.10606665601019,124.531249999512,
9.5594902125713));
#302423=CARTESIAN_POINT('Ctrl Pts',(-8.23404996476502E-14,124.681249999512,
10.5687124469213));
#302424=CARTESIAN_POINT('Ctrl Pts',(3.10606665601002,124.831249999511,9.5594902125713));
#302425=CARTESIAN_POINT('Ctrl Pts',(6.21213331202013,124.981249999511,8.55026797822134));
#302426=CARTESIAN_POINT('Ctrl Pts',(8.13178807675711,125.13124999951,5.90808986649102));
#302427=CARTESIAN_POINT('Ctrl Pts',(10.0514428414941,125.281249999509,3.2659117547607));
#302428=CARTESIAN_POINT('Ctrl Pts',(10.0514428414941,125.431249999509,-1.23094673026484E-15));
#302429=CARTESIAN_POINT('Ctrl Pts',(10.0514428414941,125.581249999508,-3.26591175476071));
#302430=CARTESIAN_POINT('Ctrl Pts',(8.13178807675711,125.731249999508,-5.90808986649102));
#302431=CARTESIAN_POINT('Ctrl Pts',(6.21213331202013,125.881249999507,-8.55026797822134));
#302432=CARTESIAN_POINT('Ctrl Pts',(3.10606665601002,126.031249999506,-9.5594902125713));
#302433=CARTESIAN_POINT('Ctrl Pts',(-8.57929422573273E-14,126.181249999506,
-10.5687124469213));
#302434=CARTESIAN_POINT('Ctrl Pts',(-3.10606665601019,126.331249999505,
-9.5594902125713));
#302435=CARTESIAN_POINT('Ctrl Pts',(-6.2121333120203,126.481249999505,-8.55026797822134));
#302436=CARTESIAN_POINT('Ctrl Pts',(-8.13178807675728,126.631249999504,
-5.90808986649102));
#302437=CARTESIAN_POINT('Ctrl Pts',(-10.0514428414943,126.781249999503,
-3.2659117547607));
#302438=CARTESIAN_POINT('Ctrl Pts',(-10.0514428414943,126.931249999503,
2.46189346052968E-15));
#302439=CARTESIAN_POINT('Ctrl Pts',(-10.0514428414943,127.081249999502,
3.26591175476071));
#302440=CARTESIAN_POINT('Ctrl Pts',(-8.13178807675728,127.231249999502,
5.90808986649102));
#302441=CARTESIAN_POINT('Ctrl Pts',(-6.2121333120203,127.381249999501,8.55026797822134));
#302442=CARTESIAN_POINT('Ctrl Pts',(-3.10606665601019,127.5312499995,9.5594902125713));
#302443=CARTESIAN_POINT('Ctrl Pts',(-8.4068208919312E-14,127.6812499995,
10.5687124469213));
#302444=CARTESIAN_POINT('Ctrl Pts',(3.10606665601002,127.831249999499,9.5594902125713));
#302445=CARTESIAN_POINT('Ctrl Pts',(6.21213331202013,127.981249999499,8.55026797822134));
#302446=CARTESIAN_POINT('Ctrl Pts',(8.1317880767571,128.131249999498,5.90808986649102));
#302447=CARTESIAN_POINT('Ctrl Pts',(10.0514428414941,128.281249999497,3.2659117547607));
#302448=CARTESIAN_POINT('Ctrl Pts',(10.0514428414941,128.431249999497,-1.23094673026484E-15));
#302449=CARTESIAN_POINT('Ctrl Pts',(10.0514428414941,128.581249999496,-3.26591175476071));
#302450=CARTESIAN_POINT('Ctrl Pts',(8.1317880767571,128.731249999496,-5.90808986649102));
#302451=CARTESIAN_POINT('Ctrl Pts',(6.21213331202013,128.881249999495,-8.55026797822134));
#302452=CARTESIAN_POINT('Ctrl Pts',(3.10606665601002,129.031249999494,-9.5594902125713));
#302453=CARTESIAN_POINT('Ctrl Pts',(-8.75206515289892E-14,129.181249999494,
-10.5687124469213));
#302454=CARTESIAN_POINT('Ctrl Pts',(-3.1060666560102,129.331249999493,-9.5594902125713));
#302455=CARTESIAN_POINT('Ctrl Pts',(-6.2121333120203,129.481249999493,-8.55026797822134));
#302456=CARTESIAN_POINT('Ctrl Pts',(-8.13178807675728,129.631249999492,
-5.90808986649102));
#302457=CARTESIAN_POINT('Ctrl Pts',(-10.0514428414943,129.781249999491,
-3.2659117547607));
#302458=CARTESIAN_POINT('Ctrl Pts',(-10.0514428414943,129.931249999491,
2.46189346052968E-15));
#302459=CARTESIAN_POINT('Ctrl Pts',(-10.0514428414943,130.08124999949,3.26591175476071));
#302460=CARTESIAN_POINT('Ctrl Pts',(-8.13178807675728,130.23124999949,5.90808986649102));
#302461=CARTESIAN_POINT('Ctrl Pts',(-6.2121333120203,130.381249999489,8.55026797822134));
#302462=CARTESIAN_POINT('Ctrl Pts',(-3.10606665601019,130.531249999488,
9.5594902125713));
#302463=CARTESIAN_POINT('Ctrl Pts',(-8.57959181909739E-14,130.681249999488,
10.5687124469213));
#302464=CARTESIAN_POINT('Ctrl Pts',(3.10606665601002,130.831249999487,9.5594902125713));
#302465=CARTESIAN_POINT('Ctrl Pts',(6.21213331202013,130.981249999487,8.55026797822134));
#302466=CARTESIAN_POINT('Ctrl Pts',(8.1317880767571,131.131249999486,5.90808986649102));
#302467=CARTESIAN_POINT('Ctrl Pts',(10.0514428414941,131.281249999485,3.2659117547607));
#302468=CARTESIAN_POINT('Ctrl Pts',(10.0514428414941,131.431249999485,-1.23094673026484E-15));
#302469=CARTESIAN_POINT('Ctrl Pts',(10.0514428414941,131.581249999484,-3.26591175476071));
#302470=CARTESIAN_POINT('Ctrl Pts',(8.1317880767571,131.731249999484,-5.90808986649102));
#302471=CARTESIAN_POINT('Ctrl Pts',(6.21213331202012,131.881249999483,-8.55026797822134));
#302472=CARTESIAN_POINT('Ctrl Pts',(3.10606665601002,132.031249999482,-9.5594902125713));
#302473=CARTESIAN_POINT('Ctrl Pts',(-8.9248360800651E-14,132.181249999482,
-10.5687124469213));
#302474=CARTESIAN_POINT('Ctrl Pts',(-3.1060666560102,132.331249999481,-9.5594902125713));
#302475=CARTESIAN_POINT('Ctrl Pts',(-6.2121333120203,132.48124999948,-8.55026797822134));
#302476=CARTESIAN_POINT('Ctrl Pts',(-8.13178807675728,132.63124999948,-5.90808986649102));
#302477=CARTESIAN_POINT('Ctrl Pts',(-10.0514428414943,132.781249999479,
-3.2659117547607));
#302478=CARTESIAN_POINT('Ctrl Pts',(-10.0514428414943,132.931249999479,
2.46189346052968E-15));
#302479=CARTESIAN_POINT('Ctrl Pts',(-10.0514428414943,133.081249999478,
3.26591175476071));
#302480=CARTESIAN_POINT('Ctrl Pts',(-8.13178807675728,133.231249999478,
5.90808986649102));
#302481=CARTESIAN_POINT('Ctrl Pts',(-6.2121333120203,133.381249999477,8.55026797822134));
#302482=CARTESIAN_POINT('Ctrl Pts',(-3.1060666560102,133.531249999476,9.5594902125713));
#302483=CARTESIAN_POINT('Ctrl Pts',(-8.75236274626357E-14,133.681249999476,
10.5687124469213));
#302484=CARTESIAN_POINT('Ctrl Pts',(3.10606665601002,133.831249999475,9.5594902125713));
#302485=CARTESIAN_POINT('Ctrl Pts',(6.21213331202013,133.981249999475,8.55026797822134));
#302486=CARTESIAN_POINT('Ctrl Pts',(8.1317880767571,134.131249999474,5.90808986649102));
#302487=CARTESIAN_POINT('Ctrl Pts',(10.0514428414941,134.281249999473,3.2659117547607));
#302488=CARTESIAN_POINT('Ctrl Pts',(10.0514428414941,134.431249999473,-1.23094673026484E-15));
#302489=CARTESIAN_POINT('Ctrl Pts',(10.0514428414941,134.581249999472,-3.26591175476071));
#302490=CARTESIAN_POINT('Ctrl Pts',(8.1317880767571,134.731249999472,-5.90808986649102));
#302491=CARTESIAN_POINT('Ctrl Pts',(6.21213331202012,134.881249999471,-8.55026797822134));
#302492=CARTESIAN_POINT('Ctrl Pts',(3.10606665601002,135.03124999947,-9.5594902125713));
#302493=CARTESIAN_POINT('Ctrl Pts',(-9.09760700723128E-14,135.18124999947,
-10.5687124469213));
#302494=CARTESIAN_POINT('Ctrl Pts',(-3.1060666560102,135.331249999469,-9.5594902125713));
#302495=CARTESIAN_POINT('Ctrl Pts',(-6.21213331202031,135.481249999469,
-8.55026797822134));
#302496=CARTESIAN_POINT('Ctrl Pts',(-8.13178807675728,135.631249999468,
-5.90808986649102));
#302497=CARTESIAN_POINT('Ctrl Pts',(-10.0514428414943,135.781249999467,
-3.2659117547607));
#302498=CARTESIAN_POINT('Ctrl Pts',(-10.0514428414943,135.931249999467,
2.46189346052968E-15));
#302499=CARTESIAN_POINT('Ctrl Pts',(-10.0514428414943,136.081249999466,
3.26591175476071));
#302500=CARTESIAN_POINT('Ctrl Pts',(-8.13178807675728,136.231249999466,
5.90808986649102));
#302501=CARTESIAN_POINT('Ctrl Pts',(-6.2121333120203,136.381249999465,8.55026797822134));
#302502=CARTESIAN_POINT('Ctrl Pts',(-3.1060666560102,136.531249999464,9.5594902125713));
#302503=CARTESIAN_POINT('Ctrl Pts',(-8.92513367342975E-14,136.681249999464,
10.5687124469213));
#302504=CARTESIAN_POINT('Ctrl Pts',(3.10606665601002,136.831249999463,9.5594902125713));
#302505=CARTESIAN_POINT('Ctrl Pts',(6.21213331202012,136.981249999463,8.55026797822134));
#302506=CARTESIAN_POINT('Ctrl Pts',(8.1317880767571,137.131249999462,5.90808986649102));
#302507=CARTESIAN_POINT('Ctrl Pts',(10.0514428414941,137.281249999461,3.2659117547607));
#302508=CARTESIAN_POINT('Ctrl Pts',(10.0514428414941,137.431249999461,-1.23094673026484E-15));
#302509=CARTESIAN_POINT('Ctrl Pts',(10.0514428414941,137.58124999946,-3.26591175476071));
#302510=CARTESIAN_POINT('Ctrl Pts',(8.1317880767571,137.73124999946,-5.90808986649102));
#302511=CARTESIAN_POINT('Ctrl Pts',(6.21213331202012,137.881249999459,-8.55026797822134));
#302512=CARTESIAN_POINT('Ctrl Pts',(3.10606665601002,138.031249999458,-9.5594902125713));
#302513=CARTESIAN_POINT('Ctrl Pts',(-9.27037793439746E-14,138.181249999458,
-10.5687124469213));
#302514=CARTESIAN_POINT('Ctrl Pts',(-3.1060666560102,138.331249999457,-9.5594902125713));
#302515=CARTESIAN_POINT('Ctrl Pts',(-6.21213331202031,138.481249999456,
-8.55026797822134));
#302516=CARTESIAN_POINT('Ctrl Pts',(-8.13178807675728,138.631249999456,
-5.90808986649102));
#302517=CARTESIAN_POINT('Ctrl Pts',(-10.0514428414943,138.781249999455,
-3.2659117547607));
#302518=CARTESIAN_POINT('Ctrl Pts',(-10.0514428414943,138.931249999455,
2.46189346052968E-15));
#302519=CARTESIAN_POINT('Ctrl Pts',(-10.0514428414943,139.081249999454,
3.26591175476071));
#302520=CARTESIAN_POINT('Ctrl Pts',(-8.13178807675728,139.231249999454,
5.90808986649102));
#302521=CARTESIAN_POINT('Ctrl Pts',(-6.21213331202031,139.381249999453,
8.55026797822134));
#302522=CARTESIAN_POINT('Ctrl Pts',(-3.1060666560102,139.531249999452,9.5594902125713));
#302523=CARTESIAN_POINT('Ctrl Pts',(-9.09790460059594E-14,139.681249999452,
10.5687124469213));
#302524=CARTESIAN_POINT('Ctrl Pts',(3.10606665601002,139.831249999451,9.5594902125713));
#302525=CARTESIAN_POINT('Ctrl Pts',(6.21213331202012,139.981249999451,8.55026797822134));
#302526=CARTESIAN_POINT('Ctrl Pts',(8.1317880767571,140.13124999945,5.90808986649102));
#302527=CARTESIAN_POINT('Ctrl Pts',(10.0514428414941,140.281249999449,3.2659117547607));
#302528=CARTESIAN_POINT('Ctrl Pts',(10.0514428414941,140.431249999449,-1.23094673026484E-15));
#302529=CARTESIAN_POINT('Ctrl Pts',(10.0514428414941,140.581249999448,-3.26591175476071));
#302530=CARTESIAN_POINT('Ctrl Pts',(8.1317880767571,140.731249999448,-5.90808986649102));
#302531=CARTESIAN_POINT('Ctrl Pts',(6.21213331202012,140.881249999447,-8.55026797822134));
#302532=CARTESIAN_POINT('Ctrl Pts',(3.10606665601001,141.031249999446,-9.5594902125713));
#302533=CARTESIAN_POINT('Ctrl Pts',(-9.44314886156365E-14,141.181249999446,
-10.5687124469213));
#302534=CARTESIAN_POINT('Ctrl Pts',(-3.1060666560102,141.331249999445,-9.5594902125713));
#302535=CARTESIAN_POINT('Ctrl Pts',(-6.21213331202031,141.481249999445,
-8.55026797822134));
#302536=CARTESIAN_POINT('Ctrl Pts',(-8.13178807675729,141.631249999444,
-5.90808986649102));
#302537=CARTESIAN_POINT('Ctrl Pts',(-10.0514428414943,141.781249999443,
-3.2659117547607));
#302538=CARTESIAN_POINT('Ctrl Pts',(-10.0514428414943,141.931249999443,
2.46189346052968E-15));
#302539=CARTESIAN_POINT('Ctrl Pts',(-10.0514428414943,142.081249999442,
3.26591175476071));
#302540=CARTESIAN_POINT('Ctrl Pts',(-8.13178807675729,142.231249999442,
5.90808986649102));
#302541=CARTESIAN_POINT('Ctrl Pts',(-6.21213331202031,142.381249999441,
8.55026797822134));
#302542=CARTESIAN_POINT('Ctrl Pts',(-3.1060666560102,142.53124999944,9.5594902125713));
#302543=CARTESIAN_POINT('Ctrl Pts',(-9.27067552776212E-14,142.68124999944,
10.5687124469213));
#302544=CARTESIAN_POINT('Ctrl Pts',(3.10606665601001,142.831249999439,9.5594902125713));
#302545=CARTESIAN_POINT('Ctrl Pts',(6.21213331202012,142.981249999439,8.55026797822134));
#302546=CARTESIAN_POINT('Ctrl Pts',(8.1317880767571,143.131249999438,5.90808986649102));
#302547=CARTESIAN_POINT('Ctrl Pts',(10.0514428414941,143.281249999437,3.2659117547607));
#302548=CARTESIAN_POINT('Ctrl Pts',(10.0514428414941,143.431249999437,-1.23094673026484E-15));
#302549=CARTESIAN_POINT('Ctrl Pts',(10.0514428414941,143.581249999436,-3.26591175476071));
#302550=CARTESIAN_POINT('Ctrl Pts',(8.1317880767571,143.731249999436,-5.90808986649102));
#302551=CARTESIAN_POINT('Ctrl Pts',(6.21213331202012,143.881249999435,-8.55026797822134));
#302552=CARTESIAN_POINT('Ctrl Pts',(3.10606665601001,144.031249999434,-9.5594902125713));
#302553=CARTESIAN_POINT('Ctrl Pts',(-9.61591978872984E-14,144.181249999434,
-10.5687124469213));
#302554=CARTESIAN_POINT('Ctrl Pts',(-3.1060666560102,144.331249999433,-9.5594902125713));
#302555=CARTESIAN_POINT('Ctrl Pts',(-6.21213331202031,144.481249999432,
-8.55026797822134));
#302556=CARTESIAN_POINT('Ctrl Pts',(-8.13178807675729,144.631249999432,
-5.90808986649102));
#302557=CARTESIAN_POINT('Ctrl Pts',(-10.0514428414943,144.781249999431,
-3.2659117547607));
#302558=CARTESIAN_POINT('Ctrl Pts',(-10.0514428414943,144.931249999431,
2.46189346052968E-15));
#302559=CARTESIAN_POINT('Ctrl Pts',(-10.0514428414943,145.08124999943,3.26591175476071));
#302560=CARTESIAN_POINT('Ctrl Pts',(-8.13178807675729,145.23124999943,5.90808986649102));
#302561=CARTESIAN_POINT('Ctrl Pts',(-6.21213331202031,145.381249999429,
8.55026797822134));
#302562=CARTESIAN_POINT('Ctrl Pts',(-3.1060666560102,145.531249999428,9.5594902125713));
#302563=CARTESIAN_POINT('Ctrl Pts',(-9.44344645492831E-14,145.681249999428,
10.5687124469213));
#302564=CARTESIAN_POINT('Ctrl Pts',(3.10606665601001,145.831249999427,9.5594902125713));
#302565=CARTESIAN_POINT('Ctrl Pts',(6.21213331202012,145.981249999427,8.55026797822134));
#302566=CARTESIAN_POINT('Ctrl Pts',(8.13178807675709,146.131249999426,5.90808986649102));
#302567=CARTESIAN_POINT('Ctrl Pts',(10.0514428414941,146.281249999425,3.2659117547607));
#302568=CARTESIAN_POINT('Ctrl Pts',(10.0514428414941,146.431249999425,-1.23094673026484E-15));
#302569=CARTESIAN_POINT('Ctrl Pts',(10.0514428414941,146.581249999424,-3.26591175476071));
#302570=CARTESIAN_POINT('Ctrl Pts',(8.13178807675709,146.731249999424,-5.90808986649102));
#302571=CARTESIAN_POINT('Ctrl Pts',(6.21213331202012,146.881249999423,-8.55026797822134));
#302572=CARTESIAN_POINT('Ctrl Pts',(3.10606665601001,147.031249999422,-9.5594902125713));
#302573=CARTESIAN_POINT('Ctrl Pts',(-9.78869071589602E-14,147.181249999422,
-10.5687124469213));
#302574=CARTESIAN_POINT('Ctrl Pts',(-3.10606665601021,147.331249999421,
-9.5594902125713));
#302575=CARTESIAN_POINT('Ctrl Pts',(-6.21213331202032,147.481249999421,
-8.55026797822134));
#302576=CARTESIAN_POINT('Ctrl Pts',(-8.13178807675729,147.63124999942,-5.90808986649102));
#302577=CARTESIAN_POINT('Ctrl Pts',(-10.0514428414943,147.781249999419,
-3.2659117547607));
#302578=CARTESIAN_POINT('Ctrl Pts',(-10.0514428414943,147.931249999419,
2.46189346052968E-15));
#302579=CARTESIAN_POINT('Ctrl Pts',(-10.0514428414943,148.081249999418,
3.26591175476071));
#302580=CARTESIAN_POINT('Ctrl Pts',(-8.13178807675729,148.231249999418,
5.90808986649102));
#302581=CARTESIAN_POINT('Ctrl Pts',(-6.21213331202031,148.381249999417,
8.55026797822134));
#302582=CARTESIAN_POINT('Ctrl Pts',(-3.1060666560102,148.531249999416,9.5594902125713));
#302583=CARTESIAN_POINT('Ctrl Pts',(-9.61621738209449E-14,148.681249999416,
10.5687124469213));
#302584=CARTESIAN_POINT('Ctrl Pts',(3.10606665601001,148.831249999415,9.5594902125713));
#302585=CARTESIAN_POINT('Ctrl Pts',(6.21213331202012,148.981249999415,8.55026797822134));
#302586=CARTESIAN_POINT('Ctrl Pts',(8.13178807675709,149.131249999414,5.90808986649102));
#302587=CARTESIAN_POINT('Ctrl Pts',(10.0514428414941,149.281249999413,3.2659117547607));
#302588=CARTESIAN_POINT('Ctrl Pts',(10.0514428414941,149.431249999413,-1.23094673026484E-15));
#302589=CARTESIAN_POINT('Ctrl Pts',(10.0514428414941,149.581249999412,-3.26591175476071));
#302590=CARTESIAN_POINT('Ctrl Pts',(8.13178807675709,149.731249999412,-5.90808986649102));
#302591=CARTESIAN_POINT('Ctrl Pts',(6.21213331202012,149.881249999411,-8.55026797822134));
#302592=CARTESIAN_POINT('Ctrl Pts',(3.10606665601001,150.03124999941,-9.5594902125713));
#302593=CARTESIAN_POINT('Ctrl Pts',(-9.9614616430622E-14,150.18124999941,
-10.5687124469213));
#302594=CARTESIAN_POINT('Ctrl Pts',(-3.10606665601021,150.331249999409,
-9.5594902125713));
#302595=CARTESIAN_POINT('Ctrl Pts',(-6.21213331202032,150.481249999409,
-8.55026797822134));
#302596=CARTESIAN_POINT('Ctrl Pts',(-8.13178807675729,150.631249999408,
-5.90808986649102));
#302597=CARTESIAN_POINT('Ctrl Pts',(-10.0514428414943,150.781249999407,
-3.2659117547607));
#302598=CARTESIAN_POINT('Ctrl Pts',(-10.0514428414943,150.931249999407,
2.46189346052968E-15));
#302599=CARTESIAN_POINT('Ctrl Pts',(-10.0514428414943,151.081249999406,
3.26591175476071));
#302600=CARTESIAN_POINT('Ctrl Pts',(-8.13178807675729,151.231249999406,
5.90808986649102));
#302601=CARTESIAN_POINT('Ctrl Pts',(-6.21213331202032,151.381249999405,
8.55026797822134));
#302602=CARTESIAN_POINT('Ctrl Pts',(-3.10606665601021,151.531249999404,
9.5594902125713));
#302603=CARTESIAN_POINT('Ctrl Pts',(-9.78898830926068E-14,151.681249999404,
10.5687124469213));
#302604=CARTESIAN_POINT('Ctrl Pts',(3.10606665601001,151.831249999403,9.5594902125713));
#302605=CARTESIAN_POINT('Ctrl Pts',(6.21213331202012,151.981249999403,8.55026797822134));
#302606=CARTESIAN_POINT('Ctrl Pts',(8.13178807675709,152.131249999402,5.90808986649102));
#302607=CARTESIAN_POINT('Ctrl Pts',(10.0514428414941,152.281249999401,3.2659117547607));
#302608=CARTESIAN_POINT('Ctrl Pts',(10.0514428414941,152.431249999401,-1.23094673026484E-15));
#302609=CARTESIAN_POINT('Ctrl Pts',(10.0514428414941,152.5812499994,-3.26591175476071));
#302610=CARTESIAN_POINT('Ctrl Pts',(8.13178807675709,152.7312499994,-5.90808986649102));
#302611=CARTESIAN_POINT('Ctrl Pts',(6.21213331202012,152.881249999399,-8.55026797822134));
#302612=CARTESIAN_POINT('Ctrl Pts',(3.10606665601001,153.031249999398,-9.5594902125713));
#302613=CARTESIAN_POINT('Ctrl Pts',(-1.01342325702284E-13,153.181249999398,
-10.5687124469213));
#302614=CARTESIAN_POINT('Ctrl Pts',(-3.10606665601021,153.331249999397,
-9.5594902125713));
#302615=CARTESIAN_POINT('Ctrl Pts',(10.0514428414941,59.4312499997728,-1.23094673026484E-15));
#302616=CARTESIAN_POINT('Ctrl Pts',(10.0514428414941,59.5812499997722,-3.26591175476071));
#302617=CARTESIAN_POINT('Ctrl Pts',(8.13178807675714,59.7312499997716,-5.90808986649102));
#302618=CARTESIAN_POINT('Ctrl Pts',(6.21213331202017,59.881249999771,-8.55026797822134));
#302619=CARTESIAN_POINT('Ctrl Pts',(3.10606665601006,60.0312499997704,-9.5594902125713));
#302620=CARTESIAN_POINT('Ctrl Pts',(1.41674609610483,60.1128316630275,-10.1083837357357));
#302621=CARTESIAN_POINT('Ctrl Pts',(-0.358381257737887,60.1985571585059,
-10.0450518201713));
#302622=CARTESIAN_POINT('Origin',(-3.77475828372553E-14,-1.881249999982,
2.68644078414671E-15));
#302623=CARTESIAN_POINT('Origin',(0.,-21.2328125,0.));
#302624=CARTESIAN_POINT('',(-1.45809509523482E-16,-21.2328125,1.190625));
#302625=CARTESIAN_POINT('Origin',(0.,-21.2328125,0.));
#302626=CARTESIAN_POINT('',(-1.45809509523482E-16,-21.43125,1.190625));
#302627=CARTESIAN_POINT('',(-1.45809509523482E-16,-21.2328125,1.190625));
#302628=CARTESIAN_POINT('Origin',(0.,-21.43125,0.));
#302629=CARTESIAN_POINT('Origin',(-22.4506403026729,-21.2328125,22.4506403026729));
#302630=CARTESIAN_POINT('',(-22.4506403026729,-21.2328125,23.6412653026729));
#302631=CARTESIAN_POINT('Origin',(-22.4506403026729,-21.2328125,22.4506403026729));
#302632=CARTESIAN_POINT('',(-22.4506403026729,-21.43125,23.6412653026729));
#302633=CARTESIAN_POINT('',(-22.4506403026729,-21.2328125,23.6412653026729));
#302634=CARTESIAN_POINT('Origin',(-22.4506403026729,-21.43125,22.4506403026729));
#302635=CARTESIAN_POINT('Origin',(-31.75,-21.2328125,-6.93889390390723E-15));
#302636=CARTESIAN_POINT('',(-31.75,-21.2328125,1.19062499999999));
#302637=CARTESIAN_POINT('Origin',(-31.75,-21.2328125,-6.93889390390723E-15));
#302638=CARTESIAN_POINT('',(-31.75,-21.43125,1.19062499999999));
#302639=CARTESIAN_POINT('',(-31.75,-21.2328125,1.19062499999999));
#302640=CARTESIAN_POINT('Origin',(-31.75,-21.43125,-6.93889390390723E-15));
#302641=CARTESIAN_POINT('Origin',(-22.4506403026729,-21.2328125,-22.4506403026729));
#302642=CARTESIAN_POINT('',(-22.4506403026729,-21.2328125,-21.2600153026729));
#302643=CARTESIAN_POINT('Origin',(-22.4506403026729,-21.2328125,-22.4506403026729));
#302644=CARTESIAN_POINT('',(-22.4506403026729,-21.43125,-21.2600153026729));
#302645=CARTESIAN_POINT('',(-22.4506403026729,-21.2328125,-21.2600153026729));
#302646=CARTESIAN_POINT('Origin',(-22.4506403026729,-21.43125,-22.4506403026729));
#302647=CARTESIAN_POINT('Origin',(3.46944695195361E-15,-21.2328125,-31.75));
#302648=CARTESIAN_POINT('',(3.32363744243013E-15,-21.2328125,-30.559375));
#302649=CARTESIAN_POINT('Origin',(3.46944695195361E-15,-21.2328125,-31.75));
#302650=CARTESIAN_POINT('',(3.32363744243013E-15,-21.43125,-30.559375));
#302651=CARTESIAN_POINT('',(3.32363744243013E-15,-21.2328125,-30.559375));
#302652=CARTESIAN_POINT('Origin',(3.46944695195361E-15,-21.43125,-31.75));
#302653=CARTESIAN_POINT('Origin',(22.4506403026729,-21.2328125,-22.4506403026729));
#302654=CARTESIAN_POINT('',(22.4506403026729,-21.2328125,-21.2600153026729));
#302655=CARTESIAN_POINT('Origin',(22.4506403026729,-21.2328125,-22.4506403026729));
#302656=CARTESIAN_POINT('',(22.4506403026729,-21.43125,-21.2600153026729));
#302657=CARTESIAN_POINT('',(22.4506403026729,-21.2328125,-21.2600153026729));
#302658=CARTESIAN_POINT('Origin',(22.4506403026729,-21.43125,-22.4506403026729));
#302659=CARTESIAN_POINT('Origin',(31.75,-21.2328125,1.73472347597681E-15));
#302660=CARTESIAN_POINT('',(31.75,-21.2328125,1.190625));
#302661=CARTESIAN_POINT('Origin',(31.75,-21.2328125,1.73472347597681E-15));
#302662=CARTESIAN_POINT('',(31.75,-21.43125,1.190625));
#302663=CARTESIAN_POINT('',(31.75,-21.2328125,1.190625));
#302664=CARTESIAN_POINT('Origin',(31.75,-21.43125,1.73472347597681E-15));
#302665=CARTESIAN_POINT('Origin',(22.4506403026729,-21.2328125,22.4506403026729));
#302666=CARTESIAN_POINT('',(22.4506403026729,-21.2328125,23.6412653026729));
#302667=CARTESIAN_POINT('Origin',(22.4506403026729,-21.2328125,22.4506403026729));
#302668=CARTESIAN_POINT('',(22.4506403026729,-21.43125,23.6412653026729));
#302669=CARTESIAN_POINT('',(22.4506403026729,-21.2328125,23.6412653026729));
#302670=CARTESIAN_POINT('Origin',(22.4506403026729,-21.43125,22.4506403026729));
#302671=CARTESIAN_POINT('Origin',(0.,-21.2328125,31.75));
#302672=CARTESIAN_POINT('',(-1.45809509523482E-16,-21.2328125,32.940625));
#302673=CARTESIAN_POINT('Origin',(0.,-21.2328125,31.75));
#302674=CARTESIAN_POINT('',(-1.45809509523482E-16,-21.43125,32.940625));
#302675=CARTESIAN_POINT('',(-1.45809509523482E-16,-21.2328125,32.940625));
#302676=CARTESIAN_POINT('Origin',(0.,-21.43125,31.75));
#302677=CARTESIAN_POINT('Origin',(0.,132.185697587277,0.));
#302678=CARTESIAN_POINT('',(-6.76664131233047E-15,-21.43125,55.2538194444444));
#302679=CARTESIAN_POINT('Origin',(0.,-21.43125,0.));
#302680=CARTESIAN_POINT('',(-6.76664131233047E-15,16.66875,55.2538194444444));
#302681=CARTESIAN_POINT('',(-6.76664131233047E-15,132.185697587277,55.2538194444444));
#302682=CARTESIAN_POINT('Origin',(0.,16.66875,0.));
#302683=CARTESIAN_POINT('Origin',(1.50669826507598E-15,16.66875,0.));
#302684=CARTESIAN_POINT('',(-3.9516490262161E-15,-15.478125,-44.5707880434783));
#302685=CARTESIAN_POINT('Origin',(1.50669826507598E-15,-15.478125,0.));
#302686=CARTESIAN_POINT('',(-3.9516490262161E-15,2.03437500000001,-44.5707880434783));
#302687=CARTESIAN_POINT('',(-3.9516490262161E-15,16.66875,-44.5707880434783));
#302688=CARTESIAN_POINT('Origin',(1.50669826507598E-15,2.03437500000001,
0.));
#302689=CARTESIAN_POINT('Origin',(0.,-9.56874999999999,0.));
#302690=CARTESIAN_POINT('',(-22.4667164334275,2.03437500000001,0.));
#302691=CARTESIAN_POINT('Origin',(2.48195539786777E-18,2.03437500000001,
0.));
#302692=CARTESIAN_POINT('',(-5.54781797994763E-16,9.29993150981749,-16.8332621659243));
#302693=CARTESIAN_POINT('Origin',(1.13459982601988E-17,9.29993150981749,
0.));
#302694=CARTESIAN_POINT('Origin',(1.50669826507598E-15,16.271875,0.));
#302695=CARTESIAN_POINT('',(-3.9516490262161E-15,16.271875,-44.5707880434783));
#302696=CARTESIAN_POINT('Origin',(1.50669826507598E-15,16.271875,0.));
#302697=CARTESIAN_POINT('',(-4.00025219605726E-15,16.66875,-44.9676630434783));
#302698=CARTESIAN_POINT('Origin',(-4.00025219605726E-15,16.271875,-44.9676630434783));
#302699=CARTESIAN_POINT('Origin',(1.50669826507598E-15,16.66875,0.));
#302700=CARTESIAN_POINT('Origin',(1.50669826507598E-15,14.684375,0.));
#302701=CARTESIAN_POINT('',(-6.03384967835924E-16,15.08125,17.2301371659243));
#302702=CARTESIAN_POINT('Origin',(1.50669826507598E-15,15.08125,0.));
#302703=CARTESIAN_POINT('',(-5.54781797994763E-16,14.684375,16.8332621659243));
#302704=CARTESIAN_POINT('Origin',(-6.03384967835924E-16,14.684375,17.2301371659243));
#302705=CARTESIAN_POINT('',(3.56817832814672E-15,14.684375,-16.8332621659243));
#302706=CARTESIAN_POINT('Origin',(1.50669826507598E-15,14.684375,0.));
#302707=CARTESIAN_POINT('Origin',(1.50669826507598E-15,14.684375,0.));
#302708=CARTESIAN_POINT('Origin',(1.50669826507598E-15,16.66875,0.));
#302709=CARTESIAN_POINT('',(-5.54781797994763E-16,16.66875,-16.8332621659243));
#302710=CARTESIAN_POINT('Origin',(0.,15.71625,0.));
#302711=CARTESIAN_POINT('',(-5.38058221954622E-15,15.08125,-43.9357880434783));
#302712=CARTESIAN_POINT('Origin',(1.50669826507598E-15,15.08125,0.));
#302713=CARTESIAN_POINT('',(-5.45834729129208E-15,15.71625,-44.5707880434783));
#302714=CARTESIAN_POINT('Origin',(-5.38058221954622E-15,15.71625,-43.9357880434783));
#302715=CARTESIAN_POINT('Origin',(1.50669826507598E-15,15.71625,0.));
#302716=CARTESIAN_POINT('Origin',(1.50669826507598E-15,16.66875,0.));
#302717=CARTESIAN_POINT('',(-3.9516490262161E-15,16.66875,-44.5707880434783));
#302718=CARTESIAN_POINT('Origin',(0.,16.66875,0.));
#302719=CARTESIAN_POINT('Origin',(-43.9357880434783,15.08125,0.));
#302720=CARTESIAN_POINT('Origin',(-44.5707880434783,-15.478125,0.));
#302721=CARTESIAN_POINT('Origin',(-16.8332621659243,2.03437500000001,0.));
#302722=CARTESIAN_POINT('Origin',(0.,-21.2328125,31.75));
#302723=CARTESIAN_POINT('Origin',(22.4506403026729,-21.2328125,22.4506403026729));
#302724=CARTESIAN_POINT('Origin',(31.75,-21.2328125,1.73472347597681E-15));
#302725=CARTESIAN_POINT('Origin',(22.4506403026729,-21.2328125,-22.4506403026729));
#302726=CARTESIAN_POINT('Origin',(3.46944695195361E-15,-21.2328125,-31.75));
#302727=CARTESIAN_POINT('Origin',(-22.4506403026729,-21.2328125,-22.4506403026729));
#302728=CARTESIAN_POINT('Origin',(-31.75,-21.2328125,-6.93889390390723E-15));
#302729=CARTESIAN_POINT('Origin',(-22.4506403026729,-21.2328125,22.4506403026729));
#302730=CARTESIAN_POINT('Origin',(0.,-21.2328125,0.));
#302731=CARTESIAN_POINT('Origin',(0.,-21.43125,0.));
#302732=CARTESIAN_POINT('',(0.,0.,0.));
#302733=CARTESIAN_POINT('Origin',(0.,0.,678.));
#302734=CARTESIAN_POINT('',(24.,-24.,678.));
#302735=CARTESIAN_POINT('',(24.,24.,678.));
#302736=CARTESIAN_POINT('',(24.,-24.,678.));
#302737=CARTESIAN_POINT('',(-24.,24.,678.));
#302738=CARTESIAN_POINT('',(-24.,24.,678.));
#302739=CARTESIAN_POINT('',(-24.,-24.,678.));
#302740=CARTESIAN_POINT('',(-24.,-24.,678.));
#302741=CARTESIAN_POINT('',(-24.,-24.,678.));
#302742=CARTESIAN_POINT('',(19.55,-19.55,678.));
#302743=CARTESIAN_POINT('',(19.55,19.55,678.));
#302744=CARTESIAN_POINT('',(19.55,-19.55,678.));
#302745=CARTESIAN_POINT('',(-19.55,-19.55,678.));
#302746=CARTESIAN_POINT('',(-19.55,-19.55,678.));
#302747=CARTESIAN_POINT('',(-19.55,19.55,678.));
#302748=CARTESIAN_POINT('',(-19.55,-19.55,678.));
#302749=CARTESIAN_POINT('',(-19.55,19.55,678.));
#302750=CARTESIAN_POINT('Origin',(0.,0.,0.));
#302751=CARTESIAN_POINT('',(24.,-24.,0.));
#302752=CARTESIAN_POINT('',(24.,24.,0.));
#302753=CARTESIAN_POINT('',(24.,-24.,0.));
#302754=CARTESIAN_POINT('',(-24.,-24.,0.));
#302755=CARTESIAN_POINT('',(-24.,-24.,0.));
#302756=CARTESIAN_POINT('',(-24.,24.,0.));
#302757=CARTESIAN_POINT('',(-24.,-24.,0.));
#302758=CARTESIAN_POINT('',(-24.,24.,0.));
#302759=CARTESIAN_POINT('',(-19.55,-19.55,0.));
#302760=CARTESIAN_POINT('',(19.55,-19.55,0.));
#302761=CARTESIAN_POINT('',(-19.55,-19.55,0.));
#302762=CARTESIAN_POINT('',(19.55,19.55,0.));
#302763=CARTESIAN_POINT('',(19.55,-19.55,0.));
#302764=CARTESIAN_POINT('',(-19.55,19.55,0.));
#302765=CARTESIAN_POINT('',(-19.55,19.55,0.));
#302766=CARTESIAN_POINT('',(-19.55,-19.55,0.));
#302767=CARTESIAN_POINT('Origin',(24.,-24.,678.));
#302768=CARTESIAN_POINT('',(24.,24.,678.));
#302769=CARTESIAN_POINT('',(24.,-24.,678.));
#302770=CARTESIAN_POINT('Origin',(-24.,24.,678.));
#302771=CARTESIAN_POINT('',(-24.,24.,678.));
#302772=CARTESIAN_POINT('Origin',(-24.,-24.,678.));
#302773=CARTESIAN_POINT('',(-24.,-24.,678.));
#302774=CARTESIAN_POINT('Origin',(-24.,-24.,678.));
#302775=CARTESIAN_POINT('Origin',(19.55,-19.55,678.));
#302776=CARTESIAN_POINT('',(19.55,-19.55,678.));
#302777=CARTESIAN_POINT('',(19.55,19.55,678.));
#302778=CARTESIAN_POINT('Origin',(-19.55,19.55,678.));
#302779=CARTESIAN_POINT('',(-19.55,19.55,678.));
#302780=CARTESIAN_POINT('Origin',(-19.55,-19.55,678.));
#302781=CARTESIAN_POINT('',(-19.55,-19.55,678.));
#302782=CARTESIAN_POINT('Origin',(-19.55,-19.55,678.));
#302783=CARTESIAN_POINT('',(0.,0.,0.));
#302784=CARTESIAN_POINT('Origin',(346.089749425718,367.316749888869,10.));
#302785=CARTESIAN_POINT('',(346.089749425718,237.316749888869,0.));
#302786=CARTESIAN_POINT('',(346.089749425718,367.316749888869,0.));
#302787=CARTESIAN_POINT('',(346.089749425718,367.316749888869,0.));
#302788=CARTESIAN_POINT('',(346.089749425718,367.316749888869,10.));
#302789=CARTESIAN_POINT('',(346.089749425718,367.316749888869,10.));
#302790=CARTESIAN_POINT('',(346.089749425718,237.316749888869,10.));
#302791=CARTESIAN_POINT('',(346.089749425718,367.316749888869,10.));
#302792=CARTESIAN_POINT('',(346.089749425718,237.316749888869,10.));
#302793=CARTESIAN_POINT('Origin',(346.089749425718,367.316749888869,10.));
#302794=CARTESIAN_POINT('',(296.089749425718,367.316749888869,0.));
#302795=CARTESIAN_POINT('',(346.089749425718,367.316749888869,0.));
#302796=CARTESIAN_POINT('',(296.089749425718,367.316749888869,10.));
#302797=CARTESIAN_POINT('',(296.089749425718,367.316749888869,10.));
#302798=CARTESIAN_POINT('',(346.089749425718,367.316749888869,10.));
#302799=CARTESIAN_POINT('Origin',(296.089749425718,367.316749888869,10.));
#302800=CARTESIAN_POINT('',(296.089749425718,237.316749888869,0.));
#302801=CARTESIAN_POINT('',(296.089749425718,367.316749888869,0.));
#302802=CARTESIAN_POINT('',(296.089749425718,237.316749888869,10.));
#302803=CARTESIAN_POINT('',(296.089749425718,237.316749888869,10.));
#302804=CARTESIAN_POINT('',(296.089749425718,367.316749888869,10.));
#302805=CARTESIAN_POINT('Origin',(346.089749425718,237.316749888869,10.));
#302806=CARTESIAN_POINT('',(346.089749425718,237.316749888869,0.));
#302807=CARTESIAN_POINT('',(346.089749425718,237.316749888869,10.));
#302808=CARTESIAN_POINT('Origin',(0.,0.,10.));
#302809=CARTESIAN_POINT('Origin',(0.,0.,0.));
#302810=CARTESIAN_POINT('',(0.,0.,0.));
#302811=CARTESIAN_POINT('',(0.,0.,0.));
#302812=CARTESIAN_POINT('Origin',(-25.,1.73472347597681E-14,703.603184599603));
#302813=CARTESIAN_POINT('',(-25.,1.73472347597681E-14,709.603184599603));
#302814=CARTESIAN_POINT('Origin',(-25.,1.73472347597681E-14,703.603184599603));
#302815=CARTESIAN_POINT('',(-25.,-5.,709.603184599603));
#302816=CARTESIAN_POINT('',(-25.,1.73472347597681E-14,709.603184599603));
#302817=CARTESIAN_POINT('Origin',(-25.,-5.,703.603184599603));
#302818=CARTESIAN_POINT('Origin',(-25.,1.73472347597681E-14,779.104914303734));
#302819=CARTESIAN_POINT('',(-25.,1.73472347597681E-14,785.104914303734));
#302820=CARTESIAN_POINT('Origin',(-25.,1.73472347597681E-14,779.104914303734));
#302821=CARTESIAN_POINT('',(-25.,-5.,785.104914303734));
#302822=CARTESIAN_POINT('',(-25.,1.73472347597681E-14,785.104914303734));
#302823=CARTESIAN_POINT('Origin',(-25.,-5.,779.104914303734));
#302824=CARTESIAN_POINT('Origin',(-50.,-14.7745526128092,765.354049451668));
#302825=CARTESIAN_POINT('',(-5.00000000000001,-14.7745526128092,771.354049451668));
#302826=CARTESIAN_POINT('Origin',(-5.,-14.7745526128092,765.354049451668));
#302827=CARTESIAN_POINT('',(8.88178419700125E-15,-14.7745526128092,771.354049451668));
#302828=CARTESIAN_POINT('',(-50.,-14.7745526128092,771.354049451668));
#302829=CARTESIAN_POINT('Origin',(0.,-14.7745526128092,765.354049451668));
#302830=CARTESIAN_POINT('Origin',(-50.,-14.7745526128092,717.354049451669));
#302831=CARTESIAN_POINT('',(-5.00000000000001,-14.7745526128092,723.354049451668));
#302832=CARTESIAN_POINT('Origin',(-5.,-14.7745526128092,717.354049451669));
#302833=CARTESIAN_POINT('',(8.88178419700125E-15,-14.7745526128092,723.354049451668));
#302834=CARTESIAN_POINT('',(-50.,-14.7745526128092,723.354049451668));
#302835=CARTESIAN_POINT('Origin',(0.,-14.7745526128092,717.354049451669));
#302836=CARTESIAN_POINT('Origin',(-50.,-59.7745526128092,741.354049451668));
#302837=CARTESIAN_POINT('',(-5.,-59.7745526128092,747.354049451668));
#302838=CARTESIAN_POINT('Origin',(-5.,-59.7745526128092,741.354049451668));
#302839=CARTESIAN_POINT('',(8.88178419700125E-15,-59.7745526128092,747.354049451668));
#302840=CARTESIAN_POINT('',(-50.,-59.7745526128092,747.354049451668));
#302841=CARTESIAN_POINT('Origin',(0.,-59.7745526128092,741.354049451668));
#302842=CARTESIAN_POINT('Origin',(-50.,-14.7745526128092,765.354049451668));
#302843=CARTESIAN_POINT('',(-50.,-14.7745526128092,771.354049451668));
#302844=CARTESIAN_POINT('Origin',(-50.,-14.7745526128092,765.354049451668));
#302845=CARTESIAN_POINT('',(-45.,-14.7745526128092,771.354049451668));
#302846=CARTESIAN_POINT('',(-50.,-14.7745526128092,771.354049451668));
#302847=CARTESIAN_POINT('Origin',(-45.,-14.7745526128092,765.354049451668));
#302848=CARTESIAN_POINT('Origin',(-50.,-14.7745526128092,717.354049451669));
#302849=CARTESIAN_POINT('',(-50.,-14.7745526128092,723.354049451668));
#302850=CARTESIAN_POINT('Origin',(-50.,-14.7745526128092,717.354049451669));
#302851=CARTESIAN_POINT('',(-45.,-14.7745526128092,723.354049451668));
#302852=CARTESIAN_POINT('',(-50.,-14.7745526128092,723.354049451668));
#302853=CARTESIAN_POINT('Origin',(-45.,-14.7745526128092,717.354049451669));
#302854=CARTESIAN_POINT('Origin',(-50.,-59.7745526128092,741.354049451668));
#302855=CARTESIAN_POINT('',(-50.,-59.7745526128092,747.354049451668));
#302856=CARTESIAN_POINT('Origin',(-50.,-59.7745526128092,741.354049451668));
#302857=CARTESIAN_POINT('',(-45.,-59.7745526128092,747.354049451668));
#302858=CARTESIAN_POINT('',(-50.,-59.7745526128092,747.354049451668));
#302859=CARTESIAN_POINT('Origin',(-45.,-59.7745526128092,741.354049451668));
#302860=CARTESIAN_POINT('Origin',(-50.,-79.2745526128092,771.354049451668));
#302861=CARTESIAN_POINT('',(-45.,-5.00000000000001,808.831171763833));
#302862=CARTESIAN_POINT('',(-5.,-5.,808.831171763833));
#302863=CARTESIAN_POINT('',(-50.,-5.,808.831171763833));
#302864=CARTESIAN_POINT('',(-4.99999999999999,-79.2745526128092,771.354049451668));
#302865=CARTESIAN_POINT('',(-4.99999999999999,-79.2745526128092,771.354049451668));
#302866=CARTESIAN_POINT('',(0.,-79.2745526128092,771.354049451668));
#302867=CARTESIAN_POINT('',(-50.,-79.2745526128092,771.354049451668));
#302868=CARTESIAN_POINT('',(0.,0.,811.354049451668));
#302869=CARTESIAN_POINT('',(0.,-79.2745526128092,771.354049451668));
#302870=CARTESIAN_POINT('',(-50.,0.,811.354049451668));
#302871=CARTESIAN_POINT('',(-50.,0.,811.354049451668));
#302872=CARTESIAN_POINT('',(-50.,-79.2745526128092,771.354049451668));
#302873=CARTESIAN_POINT('',(-50.,-79.2745526128092,771.354049451668));
#302874=CARTESIAN_POINT('',(-45.,-79.2745526128092,771.354049451668));
#302875=CARTESIAN_POINT('',(-50.,-79.2745526128092,771.354049451668));
#302876=CARTESIAN_POINT('',(-45.,-79.2745526128092,771.354049451668));
#302877=CARTESIAN_POINT('Origin',(-50.,1.71450551880629E-14,671.354049451668));
#302878=CARTESIAN_POINT('',(-4.99999999999999,-79.2745526128092,711.354049451668));
#302879=CARTESIAN_POINT('',(0.,-79.2745526128092,711.354049451668));
#302880=CARTESIAN_POINT('',(-50.,-79.2745526128092,711.354049451668));
#302881=CARTESIAN_POINT('',(-5.,-5.,673.876927139504));
#302882=CARTESIAN_POINT('',(-5.,2.21713726265793E-14,671.354049451668));
#302883=CARTESIAN_POINT('',(-45.,-5.,673.876927139504));
#302884=CARTESIAN_POINT('',(-50.,-5.,673.876927139504));
#302885=CARTESIAN_POINT('',(-45.,-79.2745526128092,711.354049451668));
#302886=CARTESIAN_POINT('',(-45.,1.71450551880629E-14,671.354049451668));
#302887=CARTESIAN_POINT('',(-50.,-79.2745526128092,711.354049451668));
#302888=CARTESIAN_POINT('',(-50.,-79.2745526128092,711.354049451668));
#302889=CARTESIAN_POINT('',(-50.,1.71450551880629E-14,671.354049451668));
#302890=CARTESIAN_POINT('',(-50.,1.71450551880629E-14,671.354049451668));
#302891=CARTESIAN_POINT('',(0.,1.71450551880629E-14,671.354049451668));
#302892=CARTESIAN_POINT('',(-50.,1.71450551880629E-14,671.354049451668));
#302893=CARTESIAN_POINT('',(0.,1.71450551880629E-14,671.354049451668));
#302894=CARTESIAN_POINT('Origin',(-50.,-79.2745526128092,711.354049451668));
#302895=CARTESIAN_POINT('',(-4.99999999999999,-79.2745526128092,711.354049451668));
#302896=CARTESIAN_POINT('',(0.,-79.2745526128092,711.354049451668));
#302897=CARTESIAN_POINT('Origin',(-50.,-79.2745526128092,711.354049451668));
#302898=CARTESIAN_POINT('',(-45.,-79.2745526128092,711.354049451668));
#302899=CARTESIAN_POINT('',(-50.,-79.2745526128092,711.354049451668));
#302900=CARTESIAN_POINT('Origin',(-50.,0.,811.354049451668));
#302901=CARTESIAN_POINT('',(0.,0.,811.354049451668));
#302902=CARTESIAN_POINT('',(-50.,0.,811.354049451668));
#302903=CARTESIAN_POINT('Origin',(-50.,0.,0.));
#302904=CARTESIAN_POINT('Origin',(0.,0.,0.));
#302905=CARTESIAN_POINT('Origin',(-5.,-5.,671.354049451668));
#302906=CARTESIAN_POINT('',(-5.,-5.,671.354049451668));
#302907=CARTESIAN_POINT('Origin',(-45.,-5.,671.354049451668));
#302908=CARTESIAN_POINT('',(-45.,-5.,671.354049451668));
#302909=CARTESIAN_POINT('Origin',(-45.,-79.2745526128092,671.354049451668));
#302910=CARTESIAN_POINT('',(0.,0.,0.));
#302911=CARTESIAN_POINT('Origin',(0.,94.6262929075966,-30.));
#302912=CARTESIAN_POINT('',(-44.2634,94.6262929075966,-37.));
#302913=CARTESIAN_POINT('Origin',(-44.2634,94.6262929075966,-30.));
#302914=CARTESIAN_POINT('',(-50.,94.6262929075966,-37.));
#302915=CARTESIAN_POINT('',(-6.51208132172169E-80,94.6262929075966,-37.));
#302916=CARTESIAN_POINT('Origin',(-50.,94.6262929075966,-30.));
#302917=CARTESIAN_POINT('Origin',(0.,50.6262929075966,-30.));
#302918=CARTESIAN_POINT('',(-44.2634,50.6262929075966,-37.));
#302919=CARTESIAN_POINT('Origin',(-44.2634,50.6262929075966,-30.));
#302920=CARTESIAN_POINT('',(-50.,50.6262929075966,-37.));
#302921=CARTESIAN_POINT('',(-6.51208132172169E-80,50.6262929075966,-37.));
#302922=CARTESIAN_POINT('Origin',(-50.,50.6262929075966,-30.));
#302923=CARTESIAN_POINT('Origin',(-44.2634,0.,-6.47319999999996));
#302924=CARTESIAN_POINT('',(-10.,0.,-5.73659999999998));
#302925=CARTESIAN_POINT('',(-43.5268,0.,-5.73659999999998));
#302926=CARTESIAN_POINT('',(0.,0.,-5.73659999999998));
#302927=CARTESIAN_POINT('',(-10.,0.,0.));
#302928=CARTESIAN_POINT('',(-10.,0.,-6.47319999999996));
#302929=CARTESIAN_POINT('',(-43.5268,0.,0.));
#302930=CARTESIAN_POINT('',(0.,0.,0.));
#302931=CARTESIAN_POINT('',(-43.5268,0.,0.));
#302932=CARTESIAN_POINT('Origin',(-44.2634,500.,-53.5268));
#302933=CARTESIAN_POINT('',(-43.5268,500.,-54.2634));
#302934=CARTESIAN_POINT('',(-10.,500.,-54.2634));
#302935=CARTESIAN_POINT('',(-50.,500.,-54.2634));
#302936=CARTESIAN_POINT('',(-10.,500.,-59.9999999999999));
#302937=CARTESIAN_POINT('',(-10.,500.,-53.5268));
#302938=CARTESIAN_POINT('',(-43.5268,500.,-59.9999999999999));
#302939=CARTESIAN_POINT('',(-50.,500.,-59.9999999999999));
#302940=CARTESIAN_POINT('',(-43.5268,500.,-59.9999999999999));
#302941=CARTESIAN_POINT('Origin',(-50.,500.,-54.2634));
#302942=CARTESIAN_POINT('',(-10.,0.,-54.2634));
#302943=CARTESIAN_POINT('',(-10.,500.,-54.2634));
#302944=CARTESIAN_POINT('',(-43.5268,0.,-54.2634));
#302945=CARTESIAN_POINT('',(-43.5268,500.,-54.2634));
#302946=CARTESIAN_POINT('',(-50.,0.,-54.2634));
#302947=CARTESIAN_POINT('Origin',(-50.,500.,-59.9999999999999));
#302948=CARTESIAN_POINT('',(-10.,0.,-59.9999999999999));
#302949=CARTESIAN_POINT('',(-10.,500.,-59.9999999999999));
#302950=CARTESIAN_POINT('',(-43.5268,0.,-59.9999999999999));
#302951=CARTESIAN_POINT('',(-50.,0.,-59.9999999999999));
#302952=CARTESIAN_POINT('',(-43.5268,500.,-59.9999999999999));
#302953=CARTESIAN_POINT('Origin',(0.,500.,0.));
#302954=CARTESIAN_POINT('',(-10.,500.,0.));
#302955=CARTESIAN_POINT('',(-10.,500.,0.));
#302956=CARTESIAN_POINT('',(-43.5268,500.,0.));
#302957=CARTESIAN_POINT('',(0.,500.,0.));
#302958=CARTESIAN_POINT('',(-43.5268,500.,0.));
#302959=CARTESIAN_POINT('Origin',(0.,500.,-5.73659999999998));
#302960=CARTESIAN_POINT('',(-10.,500.,-5.73659999999998));
#302961=CARTESIAN_POINT('',(-10.,500.,-5.73659999999998));
#302962=CARTESIAN_POINT('',(-43.5268,500.,-5.73659999999998));
#302963=CARTESIAN_POINT('',(-43.5268,500.,-5.73659999999998));
#302964=CARTESIAN_POINT('',(0.,500.,-5.73659999999998));
#302965=CARTESIAN_POINT('Origin',(-43.5268,500.,-53.5268));
#302966=CARTESIAN_POINT('',(-10.,500.,-53.5268));
#302967=CARTESIAN_POINT('',(-43.5268,500.,-5.73659999999998));
#302968=CARTESIAN_POINT('Origin',(-43.5268,0.,-53.5268));
#302969=CARTESIAN_POINT('',(-10.,0.,-53.5268));
#302970=CARTESIAN_POINT('',(-43.5268,0.,-54.2634));
#302971=CARTESIAN_POINT('Origin',(-50.,500.,-6.47319999999996));
#302972=CARTESIAN_POINT('',(-50.,500.,-6.47319999999996));
#302973=CARTESIAN_POINT('',(-44.2634,500.,-6.47319999999996));
#302974=CARTESIAN_POINT('',(-50.,500.,-6.47319999999996));
#302975=CARTESIAN_POINT('Origin',(-43.5268,500.,-6.47319999999996));
#302976=CARTESIAN_POINT('Origin',(-43.5268,500.,-6.47319999999996));
#302977=CARTESIAN_POINT('Origin',(-43.5268,500.,-5.73659999999998));
#302978=CARTESIAN_POINT('',(-50.,500.,-53.5268));
#302979=CARTESIAN_POINT('',(-50.,500.,0.));
#302980=CARTESIAN_POINT('',(-44.2634,500.,-53.5268));
#302981=CARTESIAN_POINT('',(-44.2634,500.,0.));
#302982=CARTESIAN_POINT('',(-44.2634,500.,-53.5268));
#302983=CARTESIAN_POINT('Origin',(-43.5268,0.,0.));
#302984=CARTESIAN_POINT('',(-50.,0.,-6.47319999999996));
#302985=CARTESIAN_POINT('Origin',(-43.5268,0.,-6.47319999999996));
#302986=CARTESIAN_POINT('',(-44.2634,0.,-6.47319999999996));
#302987=CARTESIAN_POINT('',(-44.2634,0.,-6.47319999999996));
#302988=CARTESIAN_POINT('Origin',(-43.5268,0.,-6.47319999999996));
#302989=CARTESIAN_POINT('Origin',(-43.5268,500.,-59.9999999999999));
#302990=CARTESIAN_POINT('Origin',(-43.5268,500.,-53.5268));
#302991=CARTESIAN_POINT('Origin',(-43.5268,500.,-53.5268));
#302992=CARTESIAN_POINT('Origin',(-50.,0.,-53.5268));
#302993=CARTESIAN_POINT('',(-50.,0.,-53.5268));
#302994=CARTESIAN_POINT('',(-44.2634,0.,-53.5268));
#302995=CARTESIAN_POINT('',(-50.,0.,-53.5268));
#302996=CARTESIAN_POINT('Origin',(-43.5268,0.,-53.5268));
#302997=CARTESIAN_POINT('Origin',(-43.5268,0.,-53.5268));
#302998=CARTESIAN_POINT('Origin',(-43.5268,0.,-54.2634));
#302999=CARTESIAN_POINT('',(-50.,0.,0.));
#303000=CARTESIAN_POINT('',(-44.2634,0.,0.));
#303001=CARTESIAN_POINT('Origin',(-43.5268,500.,-53.5268));
#303002=CARTESIAN_POINT('',(-50.,500.,-53.5268));
#303003=CARTESIAN_POINT('Origin',(-50.,500.,0.));
#303004=CARTESIAN_POINT('',(-50.,500.,-6.47319999999996));
#303005=CARTESIAN_POINT('Origin',(-43.5268,500.,-6.47319999999996));
#303006=CARTESIAN_POINT('Origin',(-43.5268,500.,-6.47319999999996));
#303007=CARTESIAN_POINT('',(-44.2634,500.,-6.47319999999996));
#303008=CARTESIAN_POINT('Origin',(-44.2634,500.,0.));
#303009=CARTESIAN_POINT('',(-44.2634,500.,-53.5268));
#303010=CARTESIAN_POINT('Origin',(-43.5268,500.,-53.5268));
#303011=CARTESIAN_POINT('Origin',(-10.,0.,0.));
#303012=CARTESIAN_POINT('Origin',(-10.,0.,0.));
#303013=CARTESIAN_POINT('',(-1.9813213246787E-15,6.58918503465636E-15,-129.303419070752));
#303014=CARTESIAN_POINT('',(-55.,-504.999999999996,582.050630380917));
#303015=CARTESIAN_POINT('',(0.,0.,0.));
#303016=CARTESIAN_POINT('',(0.,0.,0.));
#303017=CARTESIAN_POINT('Origin',(0.,0.,-6.25));
#303018=CARTESIAN_POINT('',(5.37130094929936,6.75842020936191E-16,-7.30047956616129));
#303019=CARTESIAN_POINT('',(5.01311188422819,-1.51535511969235E-8,-7.89896988241093));
#303020=CARTESIAN_POINT('',(6.,7.34788079488412E-16,-6.25));
#303021=CARTESIAN_POINT('',(-1.99181552565186,-4.4367514004807,-8.14921769587173));
#303022=CARTESIAN_POINT('Ctrl Pts',(5.37130094929936,-3.33760796777938E-14,
-7.30047956616129));
#303023=CARTESIAN_POINT('Ctrl Pts',(5.35949613657535,-0.24487406843198,
-7.32020397092237));
#303024=CARTESIAN_POINT('Ctrl Pts',(5.33089609710725,-0.489174973669408,
-7.3400128720385));
#303025=CARTESIAN_POINT('Ctrl Pts',(5.17387350532135,-1.32594283703992,
-7.40831624823914));
#303026=CARTESIAN_POINT('Ctrl Pts',(4.94337733797269,-2.00208110275183,
-7.46191832542485));
#303027=CARTESIAN_POINT('Ctrl Pts',(4.135529692896,-3.22829554366765,-7.5825649977898));
#303028=CARTESIAN_POINT('Ctrl Pts',(3.65537383524051,-3.71624330385309,
-7.63934640218176));
#303029=CARTESIAN_POINT('Ctrl Pts',(2.81761097171447,-4.2876964714026,-7.72097514658463));
#303030=CARTESIAN_POINT('Ctrl Pts',(2.52798755635282,-4.44587552657713,
-7.7478249552209));
#303031=CARTESIAN_POINT('Ctrl Pts',(1.62248349050186,-4.83055343071447,
-7.83060295463442));
#303032=CARTESIAN_POINT('Ctrl Pts',(0.979093877184556,-4.96673405732115,
-7.88693356223904));
#303033=CARTESIAN_POINT('Ctrl Pts',(-0.0815626816840825,-4.98311764351839,
-7.97601494030423));
#303034=CARTESIAN_POINT('Ctrl Pts',(-0.489396493730051,-4.93962656003035,
-8.00971505568742));
#303035=CARTESIAN_POINT('Ctrl Pts',(-1.27171916279866,-4.75351932140029,
-8.07963665620959));
#303036=CARTESIAN_POINT('Ctrl Pts',(-1.64199121952478,-4.61659114940763,
-8.11447673563966));
#303037=CARTESIAN_POINT('Ctrl Pts',(-1.99181552565213,-4.43675140048056,
-8.14921769587174));
#303038=CARTESIAN_POINT('',(-8.23019658238468E-15,-4.86334165753294,-8.14921769586694));
#303039=CARTESIAN_POINT('Origin',(2.7761126730752E-12,-8.43769498715119E-14,
-8.14921769586996));
#303040=CARTESIAN_POINT('',(1.71816547201427,-4.54972521023778,-8.14921769586694));
#303041=CARTESIAN_POINT('Origin',(2.7761126730752E-12,-8.43769498715119E-14,
-8.14921769586996));
#303042=CARTESIAN_POINT('Ctrl Pts',(5.01311188460799,-1.51897319028427E-8,
-7.89896988177634));
#303043=CARTESIAN_POINT('Ctrl Pts',(5.01031248911982,-0.111425970447792,
-7.90364733023118));
#303044=CARTESIAN_POINT('Ctrl Pts',(5.00379305356662,-0.222868907769304,
-7.90833333607711));
#303045=CARTESIAN_POINT('Ctrl Pts',(4.93276471993697,-0.993412490924391,
-7.94078816013389));
#303046=CARTESIAN_POINT('Ctrl Pts',(4.74158396418353,-1.63814017417777,
-7.9670716620526));
#303047=CARTESIAN_POINT('Ctrl Pts',(4.12882368574125,-2.78526381827432,
-8.02155068727517));
#303048=CARTESIAN_POINT('Ctrl Pts',(3.72380763625359,-3.28278277037162,
-8.04890588172946));
#303049=CARTESIAN_POINT('Ctrl Pts',(3.0083686262991,-3.8791542331357,-8.08784865603926));
#303050=CARTESIAN_POINT('Ctrl Pts',(2.76324026463121,-4.04886263939069,
-8.09985312775988));
#303051=CARTESIAN_POINT('Ctrl Pts',(2.25310822001618,-4.33623890495757,
-8.12443626150599));
#303052=CARTESIAN_POINT('Ctrl Pts',(1.99012163569433,-4.45498389569414,
-8.1367741716118));
#303053=CARTESIAN_POINT('Ctrl Pts',(1.7181654720148,-4.54972521023984,-8.14921769586818));
#303054=CARTESIAN_POINT('Origin',(0.,0.,-6.25));
#303055=CARTESIAN_POINT('',(6.00000000000001,7.34788079488412E-16,-6.24999999999999));
#303056=CARTESIAN_POINT('',(5.79150250913883,-4.07985132406587E-8,-6.59837392151535));
#303057=CARTESIAN_POINT('',(6.,7.34788079488412E-16,-6.25));
#303058=CARTESIAN_POINT('',(-4.69368212308316,3.73755911357259,-6.25));
#303059=CARTESIAN_POINT('Origin',(0.,0.,-6.25));
#303060=CARTESIAN_POINT('Ctrl Pts',(-4.69368212308327,3.73755911357246,
-6.24999999999999));
#303061=CARTESIAN_POINT('Ctrl Pts',(-4.47931229413755,3.98417297990529,
-6.2735175918551));
#303062=CARTESIAN_POINT('Ctrl Pts',(-4.24517515415671,4.21288061384112,
-6.29699494886437));
#303063=CARTESIAN_POINT('Ctrl Pts',(-3.73824535882191,4.63306114584445,
-6.34373678665324));
#303064=CARTESIAN_POINT('Ctrl Pts',(-3.46311344043465,4.8254397731834,-6.36673295318495));
#303065=CARTESIAN_POINT('Ctrl Pts',(-2.61709904150763,5.31420645490152,
-6.43586741835045));
#303066=CARTESIAN_POINT('Ctrl Pts',(-2.01132344467331,5.54175028025111,
-6.4832708210197));
#303067=CARTESIAN_POINT('Ctrl Pts',(-0.709373907000955,5.79860843459997,
-6.58134608458575));
#303068=CARTESIAN_POINT('Ctrl Pts',(0.0607328538516277,5.82805956485233,
-6.63458381103649));
#303069=CARTESIAN_POINT('Ctrl Pts',(1.59056128122726,5.5230058836078,-6.75065224080422));
#303070=CARTESIAN_POINT('Ctrl Pts',(2.27675244419754,5.24082004643196,-6.80704464760716));
#303071=CARTESIAN_POINT('Ctrl Pts',(3.19418049150465,4.63517684059687,-6.8892666820807));
#303072=CARTESIAN_POINT('Ctrl Pts',(3.48108835199279,4.40384543340971,-6.91585698981735));
#303073=CARTESIAN_POINT('Ctrl Pts',(4.25543222161972,3.63818404351202,-6.99831471866209));
#303074=CARTESIAN_POINT('Ctrl Pts',(4.6639348739115,3.03582746123758,-7.05511965050512));
#303075=CARTESIAN_POINT('Ctrl Pts',(5.08174624992373,2.04992573335704,-7.13811636816271));
#303076=CARTESIAN_POINT('Ctrl Pts',(5.18876418155107,1.71225479149455,-7.16453632905808));
#303077=CARTESIAN_POINT('Ctrl Pts',(5.35674037236568,0.91751942246152,-7.22703534262863));
#303078=CARTESIAN_POINT('Ctrl Pts',(5.39336840224904,0.457757959406786,
-7.26360753911587));
#303079=CARTESIAN_POINT('Ctrl Pts',(5.37130094929936,-3.12250225675825E-14,
-7.30047956616129));
#303080=CARTESIAN_POINT('Ctrl Pts',(5.79150251002447,-4.08715098570989E-8,
-6.59837392003555));
#303081=CARTESIAN_POINT('Ctrl Pts',(5.78622620886167,-0.242624984188651,
-6.60718997399902));
#303082=CARTESIAN_POINT('Ctrl Pts',(5.76569093304197,-0.48517843769391,
-6.61602762172233));
#303083=CARTESIAN_POINT('Ctrl Pts',(5.61802685922734,-1.47764885751981,
-6.65228846746928));
#303084=CARTESIAN_POINT('Ctrl Pts',(5.35891175563966,-2.20323592534325,
-6.67825170395312));
#303085=CARTESIAN_POINT('Ctrl Pts',(4.58795209849609,-3.4778117678666,-6.73266638985813));
#303086=CARTESIAN_POINT('Ctrl Pts',(4.09682911910025,-4.02200629394887,
-6.75961746925105));
#303087=CARTESIAN_POINT('Ctrl Pts',(2.91579372493104,-4.91318919925457,
-6.81237098041607));
#303088=CARTESIAN_POINT('Ctrl Pts',(2.23615222767148,-5.23945205078007,
-6.83949358047068));
#303089=CARTESIAN_POINT('Ctrl Pts',(0.803951054870913,-5.60382767875596,
-6.89466397257435));
#303090=CARTESIAN_POINT('Ctrl Pts',(0.066616853526438,-5.64568700227111,
-6.92051793742075));
#303091=CARTESIAN_POINT('Ctrl Pts',(-1.36792175401848,-5.44358556920285,
-6.9740664250011));
#303092=CARTESIAN_POINT('Ctrl Pts',(-2.05335593367427,-5.20623554562473,
-7.0015197208454));
#303093=CARTESIAN_POINT('Ctrl Pts',(-2.98371962683623,-4.66518039986776,
-7.04169659153851));
#303094=CARTESIAN_POINT('Ctrl Pts',(-3.27649310242692,-4.45498049694096,
-7.05459359477552));
#303095=CARTESIAN_POINT('Ctrl Pts',(-4.08296464203206,-3.74583790814793,
-7.09438665629067));
#303096=CARTESIAN_POINT('Ctrl Pts',(-4.52224764583201,-3.17326931077197,
-7.1220224387253));
#303097=CARTESIAN_POINT('Ctrl Pts',(-5.15782661187924,-1.88828578285408,
-7.17665427481457));
#303098=CARTESIAN_POINT('Ctrl Pts',(-5.3478870036423,-1.18502548968262,
-7.20265852585526));
#303099=CARTESIAN_POINT('Ctrl Pts',(-5.43745663373269,0.240850696861676,
-7.25798060499546));
#303100=CARTESIAN_POINT('Ctrl Pts',(-5.3428952326372,0.948072453679164,
-7.28567732776423));
#303101=CARTESIAN_POINT('Ctrl Pts',(-5.00327031004583,1.9442091185813,-7.32503387950306));
#303102=CARTESIAN_POINT('Ctrl Pts',(-4.86200640131429,2.25567825662979,
-7.33807215464932));
#303103=CARTESIAN_POINT('Ctrl Pts',(-4.34701152607719,3.15146660065799,
-7.3784316289358));
#303104=CARTESIAN_POINT('Ctrl Pts',(-3.88973731817415,3.677372363608,-7.40595644717349));
#303105=CARTESIAN_POINT('Ctrl Pts',(-3.07248932416454,4.31314430551931,
-7.44575193906138));
#303106=CARTESIAN_POINT('Ctrl Pts',(-2.78019273290024,4.49803618553494,
-7.45875196950415));
#303107=CARTESIAN_POINT('Ctrl Pts',(-1.86812467545593,4.95520711875464,
-7.49887716589848));
#303108=CARTESIAN_POINT('Ctrl Pts',(-1.21257768598591,5.13831190723762,
-7.52617650525911));
#303109=CARTESIAN_POINT('Ctrl Pts',(-0.197987061024375,5.21976008243166,
-7.56629157595421));
#303110=CARTESIAN_POINT('Ctrl Pts',(0.14823260987749,5.21371159144093,-7.57938335761268));
#303111=CARTESIAN_POINT('Ctrl Pts',(1.14507170889072,5.09521848164692,-7.61905190624652));
#303112=CARTESIAN_POINT('Ctrl Pts',(1.77812890210808,4.8932013671744,-7.64606356122794));
#303113=CARTESIAN_POINT('Ctrl Pts',(2.94977305341439,4.25392304181889,-7.69989480814926));
#303114=CARTESIAN_POINT('Ctrl Pts',(3.47603239672043,3.81558390378902,-7.72589291549634));
#303115=CARTESIAN_POINT('Ctrl Pts',(4.36266523902092,2.70877261234113,-7.78424215387609));
#303116=CARTESIAN_POINT('Ctrl Pts',(4.65063554164098,2.09183110209941,-7.8119962939325));
#303117=CARTESIAN_POINT('Ctrl Pts',(4.95957080834306,1.02920291987346,-7.85593681680382));
#303118=CARTESIAN_POINT('Ctrl Pts',(5.02604495679351,0.514782525821281,
-7.87736029543306));
#303119=CARTESIAN_POINT('Ctrl Pts',(5.01311188460799,-1.51897246170041E-8,
-7.89896988177633));
#303120=CARTESIAN_POINT('Origin',(0.,5.28128932132296E-15,28.75));
#303121=CARTESIAN_POINT('',(-5.85847138935259E-14,6.00000000000001,-34.28125));
#303122=CARTESIAN_POINT('',(-3.80863551318268E-8,6.,-34.4999999965812));
#303123=CARTESIAN_POINT('',(-7.34788079488412E-16,6.00000000000001,28.75));
#303124=CARTESIAN_POINT('',(4.25090439081149,-4.23436085615996,-34.9375));
#303125=CARTESIAN_POINT('Ctrl Pts',(4.25090439081131,-4.23436085616012,
-34.9375));
#303126=CARTESIAN_POINT('Ctrl Pts',(4.57842694135838,-3.90555868376502,
-34.9158612474513));
#303127=CARTESIAN_POINT('Ctrl Pts',(4.8666884707777,-3.53987524186764,-34.8939034477777));
#303128=CARTESIAN_POINT('Ctrl Pts',(5.35099960474064,-2.75288783728409,
-34.8504221559952));
#303129=CARTESIAN_POINT('Ctrl Pts',(5.54624537763172,-2.33469267044124,
-34.8290396542675));
#303130=CARTESIAN_POINT('Ctrl Pts',(5.93769197870665,-1.16099003000688,
-34.7733696884182));
#303131=CARTESIAN_POINT('Ctrl Pts',(6.03802727504269,-0.38280372816298,
-34.7368155254264));
#303132=CARTESIAN_POINT('Ctrl Pts',(5.93613876085929,1.16979111500093,-34.6635444479723));
#303133=CARTESIAN_POINT('Ctrl Pts',(5.73443158550596,1.92936928850432,-34.6291555807375));
#303134=CARTESIAN_POINT('Ctrl Pts',(5.04757392259691,3.33831174457208,-34.5563097868784));
#303135=CARTESIAN_POINT('Ctrl Pts',(4.56540424651573,3.97233357802226,-34.5187280711688));
#303136=CARTESIAN_POINT('Ctrl Pts',(3.39493264467983,5.00726959792219,-34.4467466779379));
#303137=CARTESIAN_POINT('Ctrl Pts',(2.72181234083079,5.40278223269688,-34.4121222158328));
#303138=CARTESIAN_POINT('Ctrl Pts',(1.35141069093833,5.885163881108,-34.3435799039178));
#303139=CARTESIAN_POINT('Ctrl Pts',(0.677750244888653,6.00000000000002,
-34.3116693862439));
#303140=CARTESIAN_POINT('Ctrl Pts',(-1.17128529097954E-13,6.00000000000001,
-34.28125));
#303141=CARTESIAN_POINT('',(6.,-4.85064251358796E-14,-34.9375));
#303142=CARTESIAN_POINT('Origin',(0.,1.06641418988252E-16,-34.9375));
#303143=CARTESIAN_POINT('Ctrl Pts',(-3.81631717626602E-8,6.00000000000001,
-34.4999999982871));
#303144=CARTESIAN_POINT('Ctrl Pts',(0.00902402059876882,6.0000000000574,
-34.5004050240772));
#303145=CARTESIAN_POINT('Ctrl Pts',(0.0180490097901645,5.99997964170809,
-34.500810388521));
#303146=CARTESIAN_POINT('Ctrl Pts',(0.823120666418123,5.99634673739877,
-34.53699730689));
#303147=CARTESIAN_POINT('Ctrl Pts',(1.61051049598886,5.83436739183676,-34.574699832785));
#303148=CARTESIAN_POINT('Ctrl Pts',(3.05567733514661,5.22127282706155,-34.648504052116));
#303149=CARTESIAN_POINT('Ctrl Pts',(3.70291154165463,4.78406868782487,-34.6825614856431));
#303150=CARTESIAN_POINT('Ctrl Pts',(4.80280196089368,3.68073736688949,-34.7551963264752));
#303151=CARTESIAN_POINT('Ctrl Pts',(5.24218143742912,3.02230172778511,-34.7925231893462));
#303152=CARTESIAN_POINT('Ctrl Pts',(5.84452203149045,1.56954177113762,-34.8646974890673));
#303153=CARTESIAN_POINT('Ctrl Pts',(6.00000000000006,0.788620520688176,
-34.9002829014713));
#303154=CARTESIAN_POINT('Ctrl Pts',(6.,-4.91551244152788E-13,-34.9375));
#303155=CARTESIAN_POINT('Origin',(0.,5.28128932132296E-15,28.75));
#303156=CARTESIAN_POINT('',(-3.67394039744206E-16,6.00000000000001,-32.53125));
#303157=CARTESIAN_POINT('',(5.89081071343833E-14,6.00000000000001,-32.75));
#303158=CARTESIAN_POINT('',(-7.34788079488412E-16,6.00000000000001,28.75));
#303159=CARTESIAN_POINT('Ctrl Pts',(-1.17128529097954E-13,6.00000000000001,
-34.28125));
#303160=CARTESIAN_POINT('Ctrl Pts',(-0.108384071515868,6.,-34.2763854101913));
#303161=CARTESIAN_POINT('Ctrl Pts',(-0.216868918889474,5.99706326538351,
-34.2714734698916));
#303162=CARTESIAN_POINT('Ctrl Pts',(-1.10632833147993,5.94876325515211,
-34.2308475902887));
#303163=CARTESIAN_POINT('Ctrl Pts',(-1.8715220700096,5.75404967145616,-34.1936639146874));
#303164=CARTESIAN_POINT('Ctrl Pts',(-3.27732969254155,5.08520215713945,
-34.1208131866992));
#303165=CARTESIAN_POINT('Ctrl Pts',(-3.90583688862295,4.6200222074111,-34.0867962988153));
#303166=CARTESIAN_POINT('Ctrl Pts',(-4.96419389426119,3.46223757396747,
-34.0132345504217));
#303167=CARTESIAN_POINT('Ctrl Pts',(-5.37827905946631,2.77570034754371,
-33.9755364210912));
#303168=CARTESIAN_POINT('Ctrl Pts',(-5.90897846093929,1.29838225353826,
-33.9044117656504));
#303169=CARTESIAN_POINT('Ctrl Pts',(-6.02719803969626,0.524254806297659,
-33.8684909777813));
#303170=CARTESIAN_POINT('Ctrl Pts',(-5.96210557152171,-1.0308328138026,
-33.7951022595577));
#303171=CARTESIAN_POINT('Ctrl Pts',(-5.77757864786675,-1.79691869170657,
-33.7604093625649));
#303172=CARTESIAN_POINT('Ctrl Pts',(-5.12277511184992,-3.22128116433398,
-33.6878639918628));
#303173=CARTESIAN_POINT('Ctrl Pts',(-4.65649941089954,-3.86477543194963,
-33.6503615071499));
#303174=CARTESIAN_POINT('Ctrl Pts',(-3.51221800515534,-4.92568780168271,
-33.5781148393894));
#303175=CARTESIAN_POINT('Ctrl Pts',(-2.84877639424579,-5.33690318824915,
-33.5437814648957));
#303176=CARTESIAN_POINT('Ctrl Pts',(-1.38572560561628,-5.89115588770843,
-33.4700326728546));
#303177=CARTESIAN_POINT('Ctrl Pts',(-0.597716088973461,-6.02233759768107,
-33.4334029790675));
#303178=CARTESIAN_POINT('Ctrl Pts',(0.972974403763956,-5.97179825915299,
-33.3621688264213));
#303179=CARTESIAN_POINT('Ctrl Pts',(1.74062231116078,-5.79475641957087,
-33.3251327135761));
#303180=CARTESIAN_POINT('Ctrl Pts',(3.16081248404929,-5.15859730436504,
-33.2521131610558));
#303181=CARTESIAN_POINT('Ctrl Pts',(3.80062254498545,-4.70713671292783,
-33.2180408575116));
#303182=CARTESIAN_POINT('Ctrl Pts',(4.88414625852493,-3.57386905460812,
-33.1447170559047));
#303183=CARTESIAN_POINT('Ctrl Pts',(5.31280041392579,-2.89855838340594,
-33.1070434212808));
#303184=CARTESIAN_POINT('Ctrl Pts',(5.87671476476011,-1.43676814578373,
-33.0355902597443));
#303185=CARTESIAN_POINT('Ctrl Pts',(6.0129458883674,-0.666805810236944,
-33.0002183385585));
#303186=CARTESIAN_POINT('Ctrl Pts',(5.98497004399974,0.890595063639399,
-32.9267204517406));
#303187=CARTESIAN_POINT('Ctrl Pts',(5.81781237721756,1.66315413256212,-32.8916324976544));
#303188=CARTESIAN_POINT('Ctrl Pts',(5.19528344649061,3.10252795163422,-32.8194092688793));
#303189=CARTESIAN_POINT('Ctrl Pts',(4.74507858515327,3.75511045874178,-32.7820055896562));
#303190=CARTESIAN_POINT('Ctrl Pts',(3.62730635389745,4.84159283638975,-32.7095180095524));
#303191=CARTESIAN_POINT('Ctrl Pts',(2.97357104700137,5.26841834326881,-32.6753813462562));
#303192=CARTESIAN_POINT('Ctrl Pts',(1.5397809252432,5.85046892585287,-32.6025404715633));
#303193=CARTESIAN_POINT('Ctrl Pts',(0.773378841668639,6.00000000000001,
-32.565961473548));
#303194=CARTESIAN_POINT('Ctrl Pts',(0.,6.00000000000001,-32.53125));
#303195=CARTESIAN_POINT('Ctrl Pts',(1.20892879040824E-13,6.00000000000001,
-32.75));
#303196=CARTESIAN_POINT('Ctrl Pts',(0.101226978026802,6.00000000000001,
-32.7545433588053));
#303197=CARTESIAN_POINT('Ctrl Pts',(0.202542059223401,5.99743830632742,
-32.7591280299677));
#303198=CARTESIAN_POINT('Ctrl Pts',(1.0952378532439,5.95217274272906,-32.7998549153593));
#303199=CARTESIAN_POINT('Ctrl Pts',(1.87087028470847,5.75566529874471,-32.8375332700768));
#303200=CARTESIAN_POINT('Ctrl Pts',(3.28576200148526,5.07989761547696,-32.9108926375521));
#303201=CARTESIAN_POINT('Ctrl Pts',(3.91422276511424,4.61307350891332,-32.9449516172195));
#303202=CARTESIAN_POINT('Ctrl Pts',(4.96197798508461,3.46238840871191,-33.0179482233254));
#303203=CARTESIAN_POINT('Ctrl Pts',(5.36989820990069,2.7881238855527,-33.0550067747929));
#303204=CARTESIAN_POINT('Ctrl Pts',(5.9079690533841,1.31185279064064,-33.1262959336857));
#303205=CARTESIAN_POINT('Ctrl Pts',(6.02925391706431,0.522762592374781,
-33.1628294437601));
#303206=CARTESIAN_POINT('Ctrl Pts',(5.95961829588552,-1.03971876991942,
-33.2365670923304));
#303207=CARTESIAN_POINT('Ctrl Pts',(5.77614425526705,-1.79839779288808,
-33.2709368978481));
#303208=CARTESIAN_POINT('Ctrl Pts',(5.12550864735129,-3.2169944522379,-33.34314651697));
#303209=CARTESIAN_POINT('Ctrl Pts',(4.65960067010865,-3.86108944277504,
-33.3806617367387));
#303210=CARTESIAN_POINT('Ctrl Pts',(3.51084852237016,-4.92775631107311,
-33.4532521238869));
#303211=CARTESIAN_POINT('Ctrl Pts',(2.84095246385544,-5.3420796293192,-33.4878951854373));
#303212=CARTESIAN_POINT('Ctrl Pts',(1.38408388046699,-5.8895313701482,-33.5612673216253));
#303213=CARTESIAN_POINT('Ctrl Pts',(0.611551412160819,-6.01898036856992,
-33.5972750113054));
#303214=CARTESIAN_POINT('Ctrl Pts',(-0.958066353514807,-5.97602948847404,
-33.6683503518475));
#303215=CARTESIAN_POINT('Ctrl Pts',(-1.73982057618241,-5.7968743721596,
-33.7060504154366));
#303216=CARTESIAN_POINT('Ctrl Pts',(-3.170196499209,-5.15265150375837,-33.7796447302089));
#303217=CARTESIAN_POINT('Ctrl Pts',(-3.80819541469486,-4.70081017847485,
-33.8136607523942));
#303218=CARTESIAN_POINT('Ctrl Pts',(-4.88252428158932,-3.57393764912711,
-33.8864853329209));
#303219=CARTESIAN_POINT('Ctrl Pts',(-5.30645780204214,-2.90751445746667,
-33.9236887001835));
#303220=CARTESIAN_POINT('Ctrl Pts',(-5.87645223250051,-1.44478940952579,
-33.9953462086932));
#303221=CARTESIAN_POINT('Ctrl Pts',(-6.01515533592036,-0.661874546528561,
-34.0312643808833));
#303222=CARTESIAN_POINT('Ctrl Pts',(-5.98251251181234,0.898857082688321,
-34.1049194548989));
#303223=CARTESIAN_POINT('Ctrl Pts',(-5.81692267237066,1.66186808788108,
-34.1395930812488));
#303224=CARTESIAN_POINT('Ctrl Pts',(-5.19902883015015,3.09723430781878,
-34.2115347278343));
#303225=CARTESIAN_POINT('Ctrl Pts',(-4.74704361554874,3.75344008909624,
-34.2491261279251));
#303226=CARTESIAN_POINT('Ctrl Pts',(-3.62283478247836,4.84570247476016,
-34.3220129326361));
#303227=CARTESIAN_POINT('Ctrl Pts',(-2.96439897541636,5.27428539262215,
-34.3563658839136));
#303228=CARTESIAN_POINT('Ctrl Pts',(-1.52961471346436,5.85243628070298,
-34.4291945079416));
#303229=CARTESIAN_POINT('Ctrl Pts',(-0.768275485445276,5.99999999511337,
-34.4655175797308));
#303230=CARTESIAN_POINT('Ctrl Pts',(-3.81631719281739E-8,6.00000000000001,
-34.4999999982871));
#303231=CARTESIAN_POINT('Origin',(0.,5.28128932132296E-15,28.75));
#303232=CARTESIAN_POINT('',(9.41032275168811E-15,6.00000000000001,-30.78125));
#303233=CARTESIAN_POINT('',(9.97088032893578E-14,6.00000000000001,-31.));
#303234=CARTESIAN_POINT('',(-7.34788079488412E-16,6.00000000000001,28.75));
#303235=CARTESIAN_POINT('Ctrl Pts',(0.,6.00000000000001,-32.53125));
#303236=CARTESIAN_POINT('Ctrl Pts',(-0.0207690573584315,6.00000000000001,
-32.5303178247888));
#303237=CARTESIAN_POINT('Ctrl Pts',(-0.0415430061147588,5.99989216163293,
-32.5293838573947));
#303238=CARTESIAN_POINT('Ctrl Pts',(-0.841006245186672,5.99158781913607,
-32.4933805358452));
#303239=CARTESIAN_POINT('Ctrl Pts',(-1.61068386481173,5.83198141208384,
-32.4565075903841));
#303240=CARTESIAN_POINT('Ctrl Pts',(-3.044601448773,5.22823200529503,-32.3833445536335));
#303241=CARTESIAN_POINT('Ctrl Pts',(-3.69549266007054,4.79033984663976,
-32.3491337385401));
#303242=CARTESIAN_POINT('Ctrl Pts',(-4.80334021408749,3.68137854692293,
-32.2760632228768));
#303243=CARTESIAN_POINT('Ctrl Pts',(-5.24597846606345,3.01734590148864,
-32.2384322725386));
#303244=CARTESIAN_POINT('Ctrl Pts',(-5.84212141658066,1.57115192461308,
-32.166680577062));
#303245=CARTESIAN_POINT('Ctrl Pts',(-5.99586509941762,0.805312094376112,
-32.1317548182574));
#303246=CARTESIAN_POINT('Ctrl Pts',(-6.00403147863122,-0.754142683708398,
-32.0581600022407));
#303247=CARTESIAN_POINT('Ctrl Pts',(-5.85382593447647,-1.53291003267978,
-32.022604158818));
#303248=CARTESIAN_POINT('Ctrl Pts',(-5.26264945206019,-2.9863796247127,
-31.9507124484071));
#303249=CARTESIAN_POINT('Ctrl Pts',(-4.82810908500552,-3.64736325627361,
-31.9134225368205));
#303250=CARTESIAN_POINT('Ctrl Pts',(-3.73622037314246,-4.75813199432988,
-31.8407256984623));
#303251=CARTESIAN_POINT('Ctrl Pts',(-3.09188414984736,-5.19994269877488,
-31.8066901827843));
#303252=CARTESIAN_POINT('Ctrl Pts',(-1.65133577154749,-5.82286643701931,
-31.7329499111875));
#303253=CARTESIAN_POINT('Ctrl Pts',(-0.865682176198026,-5.9902742219109,
-31.695246147753));
#303254=CARTESIAN_POINT('Ctrl Pts',(0.706644344028913,-6.00868616151848,
-31.6244070900408));
#303255=CARTESIAN_POINT('Ctrl Pts',(1.47804211685083,-5.86679277977569,
-31.5879686004718));
#303256=CARTESIAN_POINT('Ctrl Pts',(2.92554908503179,-5.29601993753442,
-31.5146765411862));
#303257=CARTESIAN_POINT('Ctrl Pts',(3.58761091395686,-4.87193281549254,
-31.4802414783041));
#303258=CARTESIAN_POINT('Ctrl Pts',(4.71962558921563,-3.78773895117872,
-31.4074461995991));
#303259=CARTESIAN_POINT('Ctrl Pts',(5.17605210346062,-3.1353364702396,-31.369876810361));
#303260=CARTESIAN_POINT('Ctrl Pts',(5.80434426291947,-1.70523417590895,
-31.2978476982129));
#303261=CARTESIAN_POINT('Ctrl Pts',(5.97560654373616,-0.943589180749387,
-31.2632804815045));
#303262=CARTESIAN_POINT('Ctrl Pts',(6.01997746580024,0.617720913462348,
-31.1895981081883));
#303263=CARTESIAN_POINT('Ctrl Pts',(5.88679218178514,1.40260600427601,-31.1534935782495));
#303264=CARTESIAN_POINT('Ctrl Pts',(5.32693106100196,2.86968313364672,-31.081950998121));
#303265=CARTESIAN_POINT('Ctrl Pts',(4.90807734750157,3.53864163612625,-31.0447917430663));
#303266=CARTESIAN_POINT('Ctrl Pts',(3.84216949904923,4.67313211014774,-30.9719099038645));
#303267=CARTESIAN_POINT('Ctrl Pts',(3.20719947099793,5.12974654011133,-30.9378895610532));
#303268=CARTESIAN_POINT('Ctrl Pts',(1.78171913024569,5.78405398749862,-30.8643679073598));
#303269=CARTESIAN_POINT('Ctrl Pts',(1.00187685407056,5.96876287124623,-30.8266726650034));
#303270=CARTESIAN_POINT('Ctrl Pts',(0.139109519067466,5.99879134583971,
-30.7875112627417));
#303271=CARTESIAN_POINT('Ctrl Pts',(0.0695316236776035,6.00000000000001,
-30.7843707798636));
#303272=CARTESIAN_POINT('Ctrl Pts',(1.95554335828646E-14,6.00000000000001,
-30.78125));
#303273=CARTESIAN_POINT('Ctrl Pts',(1.95468641273067E-13,6.00000000000001,
-31.));
#303274=CARTESIAN_POINT('Ctrl Pts',(0.192480391743009,6.00000000000001,
-31.0086390752714));
#303275=CARTESIAN_POINT('Ctrl Pts',(0.385175336776876,5.99073815588791,
-31.0174228488735));
#303276=CARTESIAN_POINT('Ctrl Pts',(1.36259758706729,5.89623557832433,-31.0626705418382));
#303277=CARTESIAN_POINT('Ctrl Pts',(2.12514322937052,5.66621663354107,-31.1002502330905));
#303278=CARTESIAN_POINT('Ctrl Pts',(3.50849430626312,4.92917067266951,-31.1730876072041));
#303279=CARTESIAN_POINT('Ctrl Pts',(4.11785741159083,4.43277444959469,-31.2074840261001));
#303280=CARTESIAN_POINT('Ctrl Pts',(5.11206217936272,3.23590118583016,-31.2807586367548));
#303281=CARTESIAN_POINT('Ctrl Pts',(5.48780835773937,2.54714948329529,-31.3172932455467));
#303282=CARTESIAN_POINT('Ctrl Pts',(5.96126157266137,1.04717135230941,-31.3880812004976));
#303283=CARTESIAN_POINT('Ctrl Pts',(6.04743504137724,0.248245656005264,
-31.4257846276549));
#303284=CARTESIAN_POINT('Ctrl Pts',(5.90508288133881,-1.31491660614123,
-31.499554409699));
#303285=CARTESIAN_POINT('Ctrl Pts',(5.6864221554242,-2.06485464078017,-31.5335989449693));
#303286=CARTESIAN_POINT('Ctrl Pts',(4.97179813757506,-3.44898577482212,
-31.6062676659712));
#303287=CARTESIAN_POINT('Ctrl Pts',(4.47923637511587,-4.06826307747327,
-31.6435747080998));
#303288=CARTESIAN_POINT('Ctrl Pts',(3.28282590619554,-5.08326089637558,
-31.7155143896323));
#303289=CARTESIAN_POINT('Ctrl Pts',(2.59016248889123,-5.46878178255341,
-31.7509991027567));
#303290=CARTESIAN_POINT('Ctrl Pts',(1.10635514205171,-5.94769239519725,
-31.8245807702451));
#303291=CARTESIAN_POINT('Ctrl Pts',(0.330695573118393,-6.04066858929894,
-31.8595643450552));
#303292=CARTESIAN_POINT('Ctrl Pts',(-1.22965422233335,-5.9256236563421,
-31.9312750839606));
#303293=CARTESIAN_POINT('Ctrl Pts',(-1.99889947408283,-5.71221688244377,
-31.9689132121872));
#303294=CARTESIAN_POINT('Ctrl Pts',(-3.39816416024533,-5.00561355812641,
-32.0420208798779));
#303295=CARTESIAN_POINT('Ctrl Pts',(-4.01711344159292,-4.52398864671584,
-32.0762069469204));
#303296=CARTESIAN_POINT('Ctrl Pts',(-5.03821886158916,-3.3500802270945,
-32.149350968764));
#303297=CARTESIAN_POINT('Ctrl Pts',(-5.43013455809175,-2.66841319466599,
-32.18624819355));
#303298=CARTESIAN_POINT('Ctrl Pts',(-5.93634537132962,-1.17910038073495,
-32.2571515107645));
#303299=CARTESIAN_POINT('Ctrl Pts',(-6.04013871036333,-0.383942995801495,
-32.2943807095057));
#303300=CARTESIAN_POINT('Ctrl Pts',(-5.93344113536867,1.18006674061518,
-32.3681904861132));
#303301=CARTESIAN_POINT('Ctrl Pts',(-5.73207110480485,1.93433663116224,
-32.4023495484525));
#303302=CARTESIAN_POINT('Ctrl Pts',(-5.04881105659906,3.33564669229781,
-32.474804145282));
#303303=CARTESIAN_POINT('Ctrl Pts',(-4.56921775066433,3.9672789462146,-32.5122231613382));
#303304=CARTESIAN_POINT('Ctrl Pts',(-3.39611509864136,5.00788017065549,
-32.5844938332572));
#303305=CARTESIAN_POINT('Ctrl Pts',(-2.7146732507898,5.40768074024111,-32.6195196436924));
#303306=CARTESIAN_POINT('Ctrl Pts',(-1.33988046218305,5.88711983323846,
-32.6882161303145));
#303307=CARTESIAN_POINT('Ctrl Pts',(-0.671954625988052,6.00000000000001,
-32.7198407378522));
#303308=CARTESIAN_POINT('Ctrl Pts',(1.17267306976032E-13,6.00000000000001,
-32.75));
#303309=CARTESIAN_POINT('Origin',(0.,5.28128932132296E-15,28.75));
#303310=CARTESIAN_POINT('',(1.04704806900171E-13,6.00000000000001,-29.03125));
#303311=CARTESIAN_POINT('',(4.71640292020203E-14,6.00000000000001,-29.25));
#303312=CARTESIAN_POINT('',(-7.34788079488412E-16,6.00000000000001,28.75));
#303313=CARTESIAN_POINT('Ctrl Pts',(1.94289029309402E-14,6.00000000000001,
-30.78125));
#303314=CARTESIAN_POINT('Ctrl Pts',(-0.704864443656357,6.00000000000001,
-30.7496136502932));
#303315=CARTESIAN_POINT('Ctrl Pts',(-1.40481278019294,5.8757909125551,-30.7163865671313));
#303316=CARTESIAN_POINT('Ctrl Pts',(-2.8007074185605,5.36339161903709,-30.6462622990238));
#303317=CARTESIAN_POINT('Ctrl Pts',(-3.47430190621078,4.95370253286064,
-30.6115065138825));
#303318=CARTESIAN_POINT('Ctrl Pts',(-4.63089515695248,3.89535469290408,
-30.5390162389076));
#303319=CARTESIAN_POINT('Ctrl Pts',(-5.10122445799473,3.25522376900886,
-30.5015297221078));
#303320=CARTESIAN_POINT('Ctrl Pts',(-5.76234994545687,1.84212165447154,
-30.4292389025261));
#303321=CARTESIAN_POINT('Ctrl Pts',(-5.95156915004192,1.0848499521348,-30.3949469527781));
#303322=CARTESIAN_POINT('Ctrl Pts',(-6.03309815537622,-0.478146796057514,
-30.3211849817774));
#303323=CARTESIAN_POINT('Ctrl Pts',(-5.91742199390294,-1.26919744498096,
-30.2844367168996));
#303324=CARTESIAN_POINT('Ctrl Pts',(-5.38958939797156,-2.74971122093979,
-30.2132695741452));
#303325=CARTESIAN_POINT('Ctrl Pts',(-4.98681025949129,-3.42640040904264,
-30.1762610591455));
#303326=CARTESIAN_POINT('Ctrl Pts',(-3.94760498399162,-4.58460705526198,
-30.1032144511309));
#303327=CARTESIAN_POINT('Ctrl Pts',(-3.32220122185289,-5.05620348553668,
-30.0691236742813));
#303328=CARTESIAN_POINT('Ctrl Pts',(-1.9123128295532,-5.74194964722611,
-29.9958433509657));
#303329=CARTESIAN_POINT('Ctrl Pts',(-1.13870354070256,-5.94393308235964,
-29.958175942521));
#303330=CARTESIAN_POINT('Ctrl Pts',(0.42496937034516,-6.03483497128459,
-29.8866681386596));
#303331=CARTESIAN_POINT('Ctrl Pts',(1.19961504217379,-5.92965560982826,
-29.8513819604272));
#303332=CARTESIAN_POINT('Ctrl Pts',(2.67449347367522,-5.42778080813352,
-29.7778661539947));
#303333=CARTESIAN_POINT('Ctrl Pts',(3.35957359596598,-5.03259151514035,
-29.7427009342106));
#303334=CARTESIAN_POINT('Ctrl Pts',(4.54027172258665,-4.00026220830159,
-29.6705353893156));
#303335=CARTESIAN_POINT('Ctrl Pts',(5.02410576631555,-3.37260995383446,
-29.6331506938396));
#303336=CARTESIAN_POINT('Ctrl Pts',(5.71757164042095,-1.97682878946513,
-29.5606240875025));
#303337=CARTESIAN_POINT('Ctrl Pts',(5.92455807718776,-1.22395815615349,
-29.526511838676));
#303338=CARTESIAN_POINT('Ctrl Pts',(6.0428954553716,0.340483743180655,-29.4526816671517));
#303339=CARTESIAN_POINT('Ctrl Pts',(5.94460390403452,1.13752054552757,-29.4152180994969));
#303340=CARTESIAN_POINT('Ctrl Pts',(5.44837127419153,2.63082072784357,-29.3444393322137));
#303341=CARTESIAN_POINT('Ctrl Pts',(5.061471000005,3.31471999799366,-29.3075960048891));
#303342=CARTESIAN_POINT('Ctrl Pts',(4.04873821818579,4.49579143546424,-29.2344107512955));
#303343=CARTESIAN_POINT('Ctrl Pts',(3.43276754758097,4.98202204428083,-29.2001680226396));
#303344=CARTESIAN_POINT('Ctrl Pts',(2.03843111779232,5.69815320480461,-29.1271426017013));
#303345=CARTESIAN_POINT('Ctrl Pts',(1.27124048780868,5.9167673788676,-29.0895207495745));
#303346=CARTESIAN_POINT('Ctrl Pts',(0.322588527977472,5.99350329256427,
-29.0458234474269));
#303347=CARTESIAN_POINT('Ctrl Pts',(0.161206502432719,6.00000000000001,
-29.0384854128966));
#303348=CARTESIAN_POINT('Ctrl Pts',(1.93907390144687E-13,6.00000000000001,
-29.03125));
#303349=CARTESIAN_POINT('Ctrl Pts',(9.68669588985449E-14,6.00000000000001,
-29.25));
#303350=CARTESIAN_POINT('Ctrl Pts',(0.286651477677494,6.00000000000001,
-29.2628657452839));
#303351=CARTESIAN_POINT('Ctrl Pts',(0.573540169208329,5.97945896409856,
-29.2760416941836));
#303352=CARTESIAN_POINT('Ctrl Pts',(1.63558733452117,5.82592456515333,-29.3259484781988));
#303353=CARTESIAN_POINT('Ctrl Pts',(2.38316140859931,5.56211378691976,-29.3633489998486));
#303354=CARTESIAN_POINT('Ctrl Pts',(3.73233274900629,4.76264945459428,-29.4355625567));
#303355=CARTESIAN_POINT('Ctrl Pts',(4.32136492355195,4.2354394021771,-29.4706633366508));
#303356=CARTESIAN_POINT('Ctrl Pts',(5.25857762796228,2.99123139186498,-29.5441642606426));
#303357=CARTESIAN_POINT('Ctrl Pts',(5.60044042765665,2.28803483898915,-29.5795215543397));
#303358=CARTESIAN_POINT('Ctrl Pts',(6.0023904933203,0.773765246573121,-29.6509839613422));
#303359=CARTESIAN_POINT('Ctrl Pts',(6.05200298287115,-0.0245078164848521,
-29.6886565890019));
#303360=CARTESIAN_POINT('Ctrl Pts',(5.84051654196882,-1.57806577620796,
-29.7619731184864));
#303361=CARTESIAN_POINT('Ctrl Pts',(5.58775672103756,-2.31924417928738,
-29.7960483467769));
#303362=CARTESIAN_POINT('Ctrl Pts',(4.81182247083947,-3.66814028245793,
-29.8690724998309));
#303363=CARTESIAN_POINT('Ctrl Pts',(4.29448652728783,-4.2622013513743,-29.9061040093557));
#303364=CARTESIAN_POINT('Ctrl Pts',(3.05281519195233,-5.22554202599166,
-29.9773269364519));
#303365=CARTESIAN_POINT('Ctrl Pts',(2.33786443112479,-5.58215914785155,
-30.0139763873589));
#303366=CARTESIAN_POINT('Ctrl Pts',(0.828066686841113,-5.99269296781362,
-30.0877274173048));
#303367=CARTESIAN_POINT('Ctrl Pts',(0.0495846113847159,-6.04943122111391,
-30.122053627619));
#303368=CARTESIAN_POINT('Ctrl Pts',(-1.49956460832676,-5.86265275286791,
-30.1943077664288));
#303369=CARTESIAN_POINT('Ctrl Pts',(-2.25480486348769,-5.61562537169326,
-30.2318076105281));
#303370=CARTESIAN_POINT('Ctrl Pts',(-3.62126633277269,-4.8472531835407,
-30.3043437711416));
#303371=CARTESIAN_POINT('Ctrl Pts',(-4.22054539170578,-4.33548353481681,
-30.3390470374932));
#303372=CARTESIAN_POINT('Ctrl Pts',(-5.18642183250232,-3.11495209027315,
-30.4124391058358));
#303373=CARTESIAN_POINT('Ctrl Pts',(-5.54530022786586,-2.41896863887779,
-30.4483424403002));
#303374=CARTESIAN_POINT('Ctrl Pts',(-5.98324466608953,-0.911644430772845,
-30.5194770761562));
#303375=CARTESIAN_POINT('Ctrl Pts',(-6.05123888368179,-0.11284038478345,
-30.5571747623118));
#303376=CARTESIAN_POINT('Ctrl Pts',(-5.87451724783255,1.44577205681473,
-30.6307298262308));
#303377=CARTESIAN_POINT('Ctrl Pts',(-5.63896641315693,2.19140848180257,
-30.6647471097636));
#303378=CARTESIAN_POINT('Ctrl Pts',(-4.89387689377796,3.55831024139031,
-30.7376031061344));
#303379=CARTESIAN_POINT('Ctrl Pts',(-4.38890566872202,4.16523404545883,
-30.7747827237829));
#303380=CARTESIAN_POINT('Ctrl Pts',(-3.16995377471245,5.15483455341167,
-30.8463780244946));
#303381=CARTESIAN_POINT('Ctrl Pts',(-2.46627405518811,5.52616432810409,
-30.8823964018584));
#303382=CARTESIAN_POINT('Ctrl Pts',(-1.15469560180341,5.91637509284195,
-30.9469544002939));
#303383=CARTESIAN_POINT('Ctrl Pts',(-0.578371165749778,6.00000000000001,
-30.9740410335283));
#303384=CARTESIAN_POINT('Ctrl Pts',(1.95815585968262E-13,6.00000000000001,
-31.));
#303385=CARTESIAN_POINT('Origin',(0.,5.28128932132296E-15,28.75));
#303386=CARTESIAN_POINT('',(7.15195468047347E-14,6.00000000000001,-27.28125));
#303387=CARTESIAN_POINT('',(-6.78587090085839E-15,6.,-27.5));
#303388=CARTESIAN_POINT('',(-7.34788079488412E-16,6.00000000000001,28.75));
#303389=CARTESIAN_POINT('Ctrl Pts',(1.95815585968262E-13,6.00000000000001,
-29.03125));
#303390=CARTESIAN_POINT('Ctrl Pts',(-0.610249439421955,6.00000000000001,
-29.0038602446397));
#303391=CARTESIAN_POINT('Ctrl Pts',(-1.21786201252579,5.90690156183558,
-28.9752311538903));
#303392=CARTESIAN_POINT('Ctrl Pts',(-2.55148792189418,5.48705543591433,
-28.9092514196746));
#303393=CARTESIAN_POINT('Ctrl Pts',(-3.24760583894352,5.10596548303448,
-28.8736082177562));
#303394=CARTESIAN_POINT('Ctrl Pts',(-4.45112089716229,4.09890357032682,
-28.8017744511858));
#303395=CARTESIAN_POINT('Ctrl Pts',(-4.94760843976345,3.48347646890437,
-28.7645055106421));
#303396=CARTESIAN_POINT('Ctrl Pts',(-5.67182017599792,2.10470908298376,
-28.6917756205893));
#303397=CARTESIAN_POINT('Ctrl Pts',(-5.89578562602353,1.35611449396653,
-28.6577486475297));
#303398=CARTESIAN_POINT('Ctrl Pts',(-6.04895800130868,-0.205663265311409,
-28.5840442038559));
#303399=CARTESIAN_POINT('Ctrl Pts',(-5.96850777040572,-1.00459381990524,
-28.5463405474231));
#303400=CARTESIAN_POINT('Ctrl Pts',(-5.50622535136872,-2.50693594684814,
-28.4754410292194));
#303401=CARTESIAN_POINT('Ctrl Pts',(-5.13579504561634,-3.1979756493988,
-28.4391149504284));
#303402=CARTESIAN_POINT('Ctrl Pts',(-4.15050879706537,-4.40232478825339,
-28.3658023055152));
#303403=CARTESIAN_POINT('Ctrl Pts',(-3.54431604105256,-4.90357289469593,
-28.3313186909329));
#303404=CARTESIAN_POINT('Ctrl Pts',(-2.16625974246611,-5.65054504877781,
-28.2585742047604));
#303405=CARTESIAN_POINT('Ctrl Pts',(-1.40598363649959,-5.88596336037959,
-28.2210176360802));
#303406=CARTESIAN_POINT('Ctrl Pts',(0.147279405670193,-6.04784927531251,
-28.148941873453));
#303407=CARTESIAN_POINT('Ctrl Pts',(0.924813814001573,-5.97853548635556,
-28.1144286638591));
#303408=CARTESIAN_POINT('Ctrl Pts',(2.42568354534179,-5.54424244603929,
-28.0407318602604));
#303409=CARTESIAN_POINT('Ctrl Pts',(3.13294184602698,-5.17756195704528,
-28.0045224284731));
#303410=CARTESIAN_POINT('Ctrl Pts',(4.35914453457563,-4.19626846643179,
-27.9330431560128));
#303411=CARTESIAN_POINT('Ctrl Pts',(4.86807798850928,-3.59340439537263,
-27.895908628745));
#303412=CARTESIAN_POINT('Ctrl Pts',(5.62299595244372,-2.23217790543008,
-27.8229966795709));
#303413=CARTESIAN_POINT('Ctrl Pts',(5.86401787523608,-1.48795013782962,
-27.7889703219834));
#303414=CARTESIAN_POINT('Ctrl Pts',(6.05182027084722,0.0691006475390994,
-27.7154889567727));
#303415=CARTESIAN_POINT('Ctrl Pts',(5.98968621790758,0.867780062776776,
-27.6777971522736));
#303416=CARTESIAN_POINT('Ctrl Pts',(5.56320596227397,2.37737110688484,-27.6065555384013));
#303417=CARTESIAN_POINT('Ctrl Pts',(5.20975555576252,3.07566435592076,-27.5708363558793));
#303418=CARTESIAN_POINT('Ctrl Pts',(4.25301324905677,4.30376937191957,-27.4974085042368));
#303419=CARTESIAN_POINT('Ctrl Pts',(3.65699459682159,4.82047213605789,-27.4625879156476));
#303420=CARTESIAN_POINT('Ctrl Pts',(2.29602198104218,5.59881858726608,-27.3901526526114));
#303421=CARTESIAN_POINT('Ctrl Pts',(1.54319585172335,5.85124120675132,-27.3526824808857));
#303422=CARTESIAN_POINT('Ctrl Pts',(0.50954384865693,5.98378966357065,-27.3043561986591));
#303423=CARTESIAN_POINT('Ctrl Pts',(0.254646309755558,6.00000000000001,
-27.2926792610153));
#303424=CARTESIAN_POINT('Ctrl Pts',(1.60010893424101E-13,6.00000000000001,
-27.28125));
#303425=CARTESIAN_POINT('Ctrl Pts',(-1.17961196366423E-15,6.,-27.5));
#303426=CARTESIAN_POINT('Ctrl Pts',(0.377235656919635,6.,-27.5169314245762));
#303427=CARTESIAN_POINT('Ctrl Pts',(0.754485140073713,5.96442592083391,
-27.5343822583682));
#303428=CARTESIAN_POINT('Ctrl Pts',(1.89456069066491,5.74645700806578,-27.5887308514134));
#303429=CARTESIAN_POINT('Ctrl Pts',(2.62638182574243,5.45099215112501,-27.6258859576961));
#303430=CARTESIAN_POINT('Ctrl Pts',(3.94112457471264,4.59230934778127,-27.6974178627425));
#303431=CARTESIAN_POINT('Ctrl Pts',(4.5099125490794,4.03516302190933,-27.7335399717867));
#303432=CARTESIAN_POINT('Ctrl Pts',(5.39088733266033,2.74527874512438,-27.8072248081781));
#303433=CARTESIAN_POINT('Ctrl Pts',(5.69952008114898,2.02822455227368,-27.8417826923468));
#303434=CARTESIAN_POINT('Ctrl Pts',(6.03075325171242,0.501778354246832,
-27.9138197457337));
#303435=CARTESIAN_POINT('Ctrl Pts',(6.04443204519531,-0.294262028749672,
-27.9513870072867));
#303436=CARTESIAN_POINT('Ctrl Pts',(5.76486704792437,-1.83659373028309,
-28.0241737398078));
#303437=CARTESIAN_POINT('Ctrl Pts',(5.47800526874849,-2.56869813601061,
-28.0586168264342));
#303438=CARTESIAN_POINT('Ctrl Pts',(4.64153171368649,-3.8807184948118,-28.1319123847809));
#303439=CARTESIAN_POINT('Ctrl Pts',(4.10050931867602,-4.44852880355724,
-28.1683316905335));
#303440=CARTESIAN_POINT('Ctrl Pts',(2.81712374957459,-5.35691334710362,
-28.2391810119292));
#303441=CARTESIAN_POINT('Ctrl Pts',(2.08295367998982,-5.68277256001296,
-28.2768847961935));
#303442=CARTESIAN_POINT('Ctrl Pts',(0.551193702838028,-6.02456364307832,
-28.3506190562634));
#303443=CARTESIAN_POINT('Ctrl Pts',(-0.229808331612538,-6.04536025298797,
-28.3846529572114));
#303444=CARTESIAN_POINT('Ctrl Pts',(-1.7658615910938,-5.7875341411008,-28.457355423015));
#303445=CARTESIAN_POINT('Ctrl Pts',(-2.50570328065487,-5.5077506064569,
-28.4946418289714));
#303446=CARTESIAN_POINT('Ctrl Pts',(-3.837810688472,-4.67850656084197,-28.5665237947856));
#303447=CARTESIAN_POINT('Ctrl Pts',(-4.4167879978859,-4.13633090591235,
-28.6020942203917));
#303448=CARTESIAN_POINT('Ctrl Pts',(-5.32600147259978,-2.86925199581966,
-28.6756916728271));
#303449=CARTESIAN_POINT('Ctrl Pts',(-5.65129429890576,-2.15910805588953,
-28.7106059519222));
#303450=CARTESIAN_POINT('Ctrl Pts',(-6.0180445264865,-0.638534087601508,
-28.7823658791792));
#303451=CARTESIAN_POINT('Ctrl Pts',(-6.0497371949765,0.158824111054979,
-28.8199953319561));
#303452=CARTESIAN_POINT('Ctrl Pts',(-5.80432700148254,1.7070087594602,-28.8930582805972));
#303453=CARTESIAN_POINT('Ctrl Pts',(-5.53464382422108,2.44372552721769,
-28.9272743091343));
#303454=CARTESIAN_POINT('Ctrl Pts',(-4.72859032973606,3.77447570968008,
-29.0004411392496));
#303455=CARTESIAN_POINT('Ctrl Pts',(-4.19938443770355,4.35562977310738,
-29.0373091259254));
#303456=CARTESIAN_POINT('Ctrl Pts',(-2.93563108841771,5.29277984299625,
-29.1081446408385));
#303457=CARTESIAN_POINT('Ctrl Pts',(-2.20955995394194,5.63467162059852,
-29.1455008693368));
#303458=CARTESIAN_POINT('Ctrl Pts',(-0.966427806999832,5.94153914542989,
-29.2057713778286));
#303459=CARTESIAN_POINT('Ctrl Pts',(-0.483589923497758,6.00000000000001,
-29.2282950891166));
#303460=CARTESIAN_POINT('Ctrl Pts',(9.95037385820297E-14,6.00000000000001,
-29.25));
#303461=CARTESIAN_POINT('Origin',(0.,5.28128932132296E-15,28.75));
#303462=CARTESIAN_POINT('',(9.83277999899942E-15,6.00000000000001,-25.53125));
#303463=CARTESIAN_POINT('',(-2.77760249601778E-14,6.00000000000001,-25.75));
#303464=CARTESIAN_POINT('',(-7.34788079488412E-16,6.00000000000001,28.75));
#303465=CARTESIAN_POINT('Ctrl Pts',(1.56402668594069E-13,6.00000000000001,
-27.28125));
#303466=CARTESIAN_POINT('Ctrl Pts',(-0.515599972979865,6.00000000000001,
-27.2581083857495));
#303467=CARTESIAN_POINT('Ctrl Pts',(-1.0300826338281,5.93354318425289,-27.2340477577944));
#303468=CARTESIAN_POINT('Ctrl Pts',(-2.29679405472947,5.59933751463919,
-27.172320262185));
#303469=CARTESIAN_POINT('Ctrl Pts',(-3.01531948397537,5.24743031318486,
-27.1354527228736));
#303470=CARTESIAN_POINT('Ctrl Pts',(-4.26412494016267,4.29247762847823,
-27.0643521519629));
#303471=CARTESIAN_POINT('Ctrl Pts',(-4.78531220279368,3.70254234769101,
-27.0273713313243));
#303472=CARTESIAN_POINT('Ctrl Pts',(-5.57096178642922,2.35943764443092,
-26.9542987968875));
#303473=CARTESIAN_POINT('Ctrl Pts',(-5.82916690872251,1.61968626176987,
-26.9201872998274));
#303474=CARTESIAN_POINT('Ctrl Pts',(-6.05159797685185,0.0678141053886751,
-26.8469503278835));
#303475=CARTESIAN_POINT('Ctrl Pts',(-6.00776923179659,-0.730206667473291,
-26.8092896064688));
#303476=CARTESIAN_POINT('Ctrl Pts',(-5.61716718813836,-2.24656139245816,
-26.737728796518));
#303477=CARTESIAN_POINT('Ctrl Pts',(-5.28065340098111,-2.95200885115185,
-26.7025241271465));
#303478=CARTESIAN_POINT('Ctrl Pts',(-4.35246985184518,-4.20362012985325,
-26.6289910099454));
#303479=CARTESIAN_POINT('Ctrl Pts',(-3.76667509345661,-4.73566915601005,
-26.5937474028814));
#303480=CARTESIAN_POINT('Ctrl Pts',(-2.42298861909404,-5.54480086236121,
-26.5216390401035));
#303481=CARTESIAN_POINT('Ctrl Pts',(-1.67788280009698,-5.8138083469795,
-26.484273515561));
#303482=CARTESIAN_POINT('Ctrl Pts',(-0.1372705771751,-6.04811974682917,
-26.4117093532099));
#303483=CARTESIAN_POINT('Ctrl Pts',(0.642927897219295,-6.01541556988549,
-26.3776183515732));
#303484=CARTESIAN_POINT('Ctrl Pts',(2.16950435979991,-5.65037716134794,
-26.3037777190948));
#303485=CARTESIAN_POINT('Ctrl Pts',(2.89901934420476,-5.31309077866264,
-26.2661856841095));
#303486=CARTESIAN_POINT('Ctrl Pts',(4.16954515512449,-4.38411016073118,
-26.1954742137953));
#303487=CARTESIAN_POINT('Ctrl Pts',(4.70236067534888,-3.80699612262179,
-26.1586603459099));
#303488=CARTESIAN_POINT('Ctrl Pts',(5.51768033346227,-2.48194352687644,
-26.0854540122438));
#303489=CARTESIAN_POINT('Ctrl Pts',(5.79259576457618,-1.7466224230031,-26.051177754673));
#303490=CARTESIAN_POINT('Ctrl Pts',(6.04843928027968,-0.20017839722435,
-25.9781969506402));
#303491=CARTESIAN_POINT('Ctrl Pts',(6.02225281868307,0.596819500941055,
-25.9405845014012));
#303492=CARTESIAN_POINT('Ctrl Pts',(5.66634373735787,2.11923799365917,-25.8687375261336));
#303493=CARTESIAN_POINT('Ctrl Pts',(5.34614199354874,2.83150153213201,-25.8339416536829));
#303494=CARTESIAN_POINT('Ctrl Pts',(4.44554852974558,4.10556993485991,-25.7603164565406));
#303495=CARTESIAN_POINT('Ctrl Pts',(3.86967628599886,4.65232884939375,-25.7245857730241));
#303496=CARTESIAN_POINT('Ctrl Pts',(2.5428539596324,5.49062280133483,-25.6528090391118));
#303497=CARTESIAN_POINT('Ctrl Pts',(1.8054379564654,5.77523896294413,-25.6155610291488));
#303498=CARTESIAN_POINT('Ctrl Pts',(0.691935818399132,5.97008963046896,
-25.5627422685962));
#303499=CARTESIAN_POINT('Ctrl Pts',(0.345904466615894,6.00000000000001,
-25.5467751903674));
#303500=CARTESIAN_POINT('Ctrl Pts',(4.42701431069281E-14,6.00000000000001,
-25.53125));
#303501=CARTESIAN_POINT('Ctrl Pts',(-7.72992780895265E-14,6.00000000000001,
-25.75));
#303502=CARTESIAN_POINT('Ctrl Pts',(0.468122861239281,6.00000000000001,
-25.7710107045081));
#303503=CARTESIAN_POINT('Ctrl Pts',(0.935658867261643,5.94521908422345,
-25.7927939576161));
#303504=CARTESIAN_POINT('Ctrl Pts',(2.15006328245386,5.65535233061078,-25.8515271547163));
#303505=CARTESIAN_POINT('Ctrl Pts',(2.8648072218771,5.32904983641039,-25.888365502735));
#303506=CARTESIAN_POINT('Ctrl Pts',(4.14348544173313,4.41179809432033,-25.9591328580284));
#303507=CARTESIAN_POINT('Ctrl Pts',(4.69118642268346,3.82432388055873,-25.9966181218902));
#303508=CARTESIAN_POINT('Ctrl Pts',(5.51417090692893,2.48845339563324,-26.0704500946619));
#303509=CARTESIAN_POINT('Ctrl Pts',(5.78875318796602,1.75750763251673,-26.1045585433572));
#303510=CARTESIAN_POINT('Ctrl Pts',(6.04709949106524,0.220551590446189,
-26.1770915842196));
#303511=CARTESIAN_POINT('Ctrl Pts',(6.02406943819719,-0.571552026603184,
-26.2144730593237));
#303512=CARTESIAN_POINT('Ctrl Pts',(5.6746508052643,-2.10051584936312,-26.2866289261136));
#303513=CARTESIAN_POINT('Ctrl Pts',(5.35218037901748,-2.82276500625205,
-26.3218072890385));
#303514=CARTESIAN_POINT('Ctrl Pts',(4.45306886958014,-4.09512251548566,
-26.3953260566928));
#303515=CARTESIAN_POINT('Ctrl Pts',(3.88784123991802,-4.63513569953974,
-26.4305981980043));
#303516=CARTESIAN_POINT('Ctrl Pts',(2.56886747369248,-5.47976480362057,
-26.5021150535304));
#303517=CARTESIAN_POINT('Ctrl Pts',(1.82413919618432,-5.7705596910345,-26.5397813658791));
#303518=CARTESIAN_POINT('Ctrl Pts',(0.280280424224938,-6.04348549428708,
-26.6130543694334));
#303519=CARTESIAN_POINT('Ctrl Pts',(-0.502909218070725,-6.02904208015853,
-26.6471484862228));
#303520=CARTESIAN_POINT('Ctrl Pts',(-2.02419019540456,-5.70184808991998,
-26.7201995442795));
#303521=CARTESIAN_POINT('Ctrl Pts',(-2.74754178218265,-5.39068842638131,
-26.7572033953967));
#303522=CARTESIAN_POINT('Ctrl Pts',(-4.04426038676789,-4.50231719623974,
-26.8283592810692));
#303523=CARTESIAN_POINT('Ctrl Pts',(-4.60250180003155,-3.92988985996744,
-26.8651276125343));
#303524=CARTESIAN_POINT('Ctrl Pts',(-5.45439599366001,-2.61680010808329,
-26.9388917553293));
#303525=CARTESIAN_POINT('Ctrl Pts',(-5.74592617895212,-1.89272959036154,
-26.9731770597458));
#303526=CARTESIAN_POINT('Ctrl Pts',(-6.04059162878921,-0.360751196876833,
-27.0454751921409));
#303527=CARTESIAN_POINT('Ctrl Pts',(-6.03580606113762,0.433520368449108,
-27.0829589784866));
#303528=CARTESIAN_POINT('Ctrl Pts',(-5.72115497813815,1.96937350683204,
-27.1554399703925));
#303529=CARTESIAN_POINT('Ctrl Pts',(-5.41649047631603,2.6966028159408,-27.1902065518807));
#303530=CARTESIAN_POINT('Ctrl Pts',(-4.54866121558117,3.98888755690702,
-27.2636183915751));
#303531=CARTESIAN_POINT('Ctrl Pts',(-3.99551283052029,4.54282944451347,
-27.2994194535087));
#303532=CARTESIAN_POINT('Ctrl Pts',(-2.69416048978434,5.41952961295404,
-27.3706131116443));
#303533=CARTESIAN_POINT('Ctrl Pts',(-1.9545299925419,5.72796048538167,-27.4083078123562));
#303534=CARTESIAN_POINT('Ctrl Pts',(-0.78814350312714,5.96117321500919,
-27.4640596219032));
#303535=CARTESIAN_POINT('Ctrl Pts',(-0.394104857598537,6.00000000000001,
-27.4823114370311));
#303536=CARTESIAN_POINT('Ctrl Pts',(-3.33066907387547E-15,6.00000000000001,
-27.5));
#303537=CARTESIAN_POINT('Origin',(0.,5.28128932132296E-15,28.75));
#303538=CARTESIAN_POINT('',(-8.03487180356169E-15,6.00000000000001,-23.78125));
#303539=CARTESIAN_POINT('',(-1.19751063656468E-13,6.00000000000001,-24.));
#303540=CARTESIAN_POINT('',(-7.34788079488412E-16,6.00000000000001,28.75));
#303541=CARTESIAN_POINT('Ctrl Pts',(3.31679128606766E-14,6.00000000000001,
-25.53125));
#303542=CARTESIAN_POINT('Ctrl Pts',(-0.424871467655015,6.00000000000001,
-25.5121805428127));
#303543=CARTESIAN_POINT('Ctrl Pts',(-0.849492094009211,5.95487440164865,
-25.4924642624639));
#303544=CARTESIAN_POINT('Ctrl Pts',(-2.04357041809809,5.69697560214102,
-25.4351095583023));
#303545=CARTESIAN_POINT('Ctrl Pts',(-2.77946209252457,5.37646734180537,
-25.397406538171));
#303546=CARTESIAN_POINT('Ctrl Pts',(-4.06842357584219,4.47781098282506,
-25.3264488230175));
#303547=CARTESIAN_POINT('Ctrl Pts',(-4.61319027180827,3.91427068836823,
-25.2902295636634));
#303548=CARTESIAN_POINT('Ctrl Pts',(-5.45934039323248,2.60831583895651,
-25.2168971647068));
#303549=CARTESIAN_POINT('Ctrl Pts',(-5.75169131396413,1.87770392850516,
-25.1823638393329));
#303550=CARTESIAN_POINT('Ctrl Pts',(-6.04210854266238,0.337325462177737,
-25.109669285173));
#303551=CARTESIAN_POINT('Ctrl Pts',(-6.03414577828957,-0.458212785890218,
-25.0721257207018));
#303552=CARTESIAN_POINT('Ctrl Pts',(-5.71421415547629,-1.98642443711181,
-25.0000053508862));
#303553=CARTESIAN_POINT('Ctrl Pts',(-5.41087198181499,-2.70565746338242,
-24.9655418924847));
#303554=CARTESIAN_POINT('Ctrl Pts',(-4.53888313243973,-4.00274287099822,
-24.8918313815121));
#303555=CARTESIAN_POINT('Ctrl Pts',(-3.9733481599669,-4.56462612152847,
-24.8555178639272));
#303556=CARTESIAN_POINT('Ctrl Pts',(-2.66416049607204,-5.43255081936865,
-24.7841005094968));
#303557=CARTESIAN_POINT('Ctrl Pts',(-1.93493481390922,-5.73291475230064,
-24.7469904497704));
#303558=CARTESIAN_POINT('Ctrl Pts',(-0.408310660204593,-6.03607995383764,
-24.6740499943789));
#303559=CARTESIAN_POINT('Ctrl Pts',(0.374153358504102,-6.03829357754675,
-24.6400153658748));
#303560=CARTESIAN_POINT('Ctrl Pts',(1.9140313804275,-5.74154198020781,-24.5665735703691));
#303561=CARTESIAN_POINT('Ctrl Pts',(2.65529281663034,-5.4385950621266,-24.5288856427459));
#303562=CARTESIAN_POINT('Ctrl Pts',(3.96218395129926,-4.57186551408942,
-24.4575887924404));
#303563=CARTESIAN_POINT('Ctrl Pts',(4.51910798429228,-4.0222652428609,-24.4219625218225));
#303564=CARTESIAN_POINT('Ctrl Pts',(5.39671051287872,-2.7361803294309,-24.3485162873228));
#303565=CARTESIAN_POINT('Ctrl Pts',(5.70693322891675,-2.01049405427323,
-24.3136305583248));
#303566=CARTESIAN_POINT('Ctrl Pts',(6.03247247102471,-0.476747960636583,
-24.241249003461));
#303567=CARTESIAN_POINT('Ctrl Pts',(6.04297780476799,0.316889074752779,
-24.2037951622696));
#303568=CARTESIAN_POINT('Ctrl Pts',(5.75967743453439,1.85048055115758,-24.1314209042039));
#303569=CARTESIAN_POINT('Ctrl Pts',(5.47345416616638,2.57671226734841,-24.0972009530275));
#303570=CARTESIAN_POINT('Ctrl Pts',(4.63060265135997,3.89695887401926,-24.0234144001431));
#303571=CARTESIAN_POINT('Ctrl Pts',(4.07565211473755,4.47410856406866,-23.9864296082687));
#303572=CARTESIAN_POINT('Ctrl Pts',(2.78456422924563,5.37158127780049,-23.9153937155443));
#303573=CARTESIAN_POINT('Ctrl Pts',(2.06388598663886,5.6875268386056,-23.8784400574907));
#303574=CARTESIAN_POINT('Ctrl Pts',(0.874224439928393,5.95220036785164,
-23.8211847928979));
#303575=CARTESIAN_POINT('Ctrl Pts',(0.437278592210077,6.00000000000001,
-23.8008763247309));
#303576=CARTESIAN_POINT('Ctrl Pts',(-4.16333634234434E-15,6.00000000000001,
-23.78125));
#303577=CARTESIAN_POINT('Ctrl Pts',(-2.38281616660174E-13,6.,-24.));
#303578=CARTESIAN_POINT('Ctrl Pts',(0.562550298860549,6.00000000000002,
-24.0252488803239));
#303579=CARTESIAN_POINT('Ctrl Pts',(1.1233551042289,5.92088791056928,-24.0515731358351));
#303580=CARTESIAN_POINT('Ctrl Pts',(2.41071026870567,5.54884547697468,-24.1147789683531));
#303581=CARTESIAN_POINT('Ctrl Pts',(3.10683165180809,5.19121363532752,-24.1504820805078));
#303582=CARTESIAN_POINT('Ctrl Pts',(4.33846198761852,4.2198397478983,-24.2217331841809));
#303583=CARTESIAN_POINT('Ctrl Pts',(4.85774809512149,3.60991749279142,-24.259424364326));
#303584=CARTESIAN_POINT('Ctrl Pts',(5.62013568794327,2.23937998964814,-24.3328990059842));
#303585=CARTESIAN_POINT('Ctrl Pts',(5.86211841709987,1.49543160766457,-24.3669266075694));
#303586=CARTESIAN_POINT('Ctrl Pts',(6.05047063792894,-0.0496575713316277,
-24.4398434727813));
#303587=CARTESIAN_POINT('Ctrl Pts',(5.99258710491169,-0.836440604727685,
-24.4769738554007));
#303588=CARTESIAN_POINT('Ctrl Pts',(5.57639177404937,-2.35084427814086,
-24.5484425900419));
#303589=CARTESIAN_POINT('Ctrl Pts',(5.21923032242104,-3.06306108589369,
-24.5846696335685));
#303590=CARTESIAN_POINT('Ctrl Pts',(4.25938687942677,-4.29601921088136,
-24.6583687981531));
#303591=CARTESIAN_POINT('Ctrl Pts',(3.67074897074401,-4.80871760926913,
-24.6928733281883));
#303592=CARTESIAN_POINT('Ctrl Pts',(2.31850296533907,-5.58979575758995,
-24.7649567530249));
#303593=CARTESIAN_POINT('Ctrl Pts',(1.56493274222149,-5.84570310131582,
-24.8025111407221));
#303594=CARTESIAN_POINT('Ctrl Pts',(0.0108649931927007,-6.05038621000914,
-24.875247146657));
#303595=CARTESIAN_POINT('Ctrl Pts',(-0.774206948697535,-6.00065650544021,
-24.9097390673429));
#303596=CARTESIAN_POINT('Ctrl Pts',(-2.27896334720533,-5.60443537022234,
-24.983055100494));
#303597=CARTESIAN_POINT('Ctrl Pts',(-2.98456358044658,-5.26265704441739,
-25.0193627830976));
#303598=CARTESIAN_POINT('Ctrl Pts',(-4.24091987830039,-4.31819521272542,
-25.0902722707001));
#303599=CARTESIAN_POINT('Ctrl Pts',(-4.77518588066601,-3.71883157954491,
-25.1279758557517));
#303600=CARTESIAN_POINT('Ctrl Pts',(-5.56839113636215,-2.36482273658844,
-25.2016742944687));
#303601=CARTESIAN_POINT('Ctrl Pts',(-5.82675235100875,-1.62736996328308,
-25.2357000858749));
#303602=CARTESIAN_POINT('Ctrl Pts',(-6.05028457959359,-0.0861277442399659,
-25.3084354028214));
#303603=CARTESIAN_POINT('Ctrl Pts',(-6.00986496171919,0.703516433178524,
-25.3457008104321));
#303604=CARTESIAN_POINT('Ctrl Pts',(-5.62719500215083,2.22544989670628,
-25.417524895883));
#303605=CARTESIAN_POINT('Ctrl Pts',(-5.28753359193716,2.94278461795138,
-25.4531828441067));
#303606=CARTESIAN_POINT('Ctrl Pts',(-4.35829222660762,4.19571637994054,
-25.5267957198342));
#303607=CARTESIAN_POINT('Ctrl Pts',(-3.78144475897279,4.72222451038447,
-25.5616436241724));
#303608=CARTESIAN_POINT('Ctrl Pts',(-2.44580348839665,5.53553560979869,
-25.6334518444767));
#303609=CARTESIAN_POINT('Ctrl Pts',(-1.69651006241038,5.8091243938572,-25.6710721315185));
#303610=CARTESIAN_POINT('Ctrl Pts',(-0.612088581728065,5.97660254263791,
-25.7221864857074));
#303611=CARTESIAN_POINT('Ctrl Pts',(-0.305934362215538,6.,-25.7362687832285));
#303612=CARTESIAN_POINT('Ctrl Pts',(-8.5417783957098E-14,6.,-25.75));
#303613=CARTESIAN_POINT('Origin',(0.,5.28128932132296E-15,28.75));
#303614=CARTESIAN_POINT('',(-7.12481952681565E-14,6.00000000000001,-22.03125));
#303615=CARTESIAN_POINT('',(-9.35567391692183E-14,6.00000000000001,-22.25));
#303616=CARTESIAN_POINT('',(-7.34788079488412E-16,6.00000000000001,28.75));
#303617=CARTESIAN_POINT('Ctrl Pts',(-2.4980018054066E-15,6.00000000000001,
-23.78125));
#303618=CARTESIAN_POINT('Ctrl Pts',(-0.335678938243623,6.00000000000001,
-23.7661837608457));
#303619=CARTESIAN_POINT('Ctrl Pts',(-0.671516877978854,5.97183185980311,
-23.7506995998679));
#303620=CARTESIAN_POINT('Ctrl Pts',(-1.78399880945041,5.78301956731754,
-23.6980146887665));
#303621=CARTESIAN_POINT('Ctrl Pts',(-2.53020766877619,5.49764207970405,
-23.6603609273815));
#303622=CARTESIAN_POINT('Ctrl Pts',(-3.8544843350439,4.66286957682803,-23.588749804504));
#303623=CARTESIAN_POINT('Ctrl Pts',(-4.42338717316591,4.12711664154783,
-23.5536209266038));
#303624=CARTESIAN_POINT('Ctrl Pts',(-5.33202476696476,2.86087582747025,
-23.4800714468375));
#303625=CARTESIAN_POINT('Ctrl Pts',(-5.65992614642843,2.14016759121118,
-23.4447501972058));
#303626=CARTESIAN_POINT('Ctrl Pts',(-6.0198832742675,0.613385006056967,
-23.3726972688164));
#303627=CARTESIAN_POINT('Ctrl Pts',(-6.04843144717586,-0.17797995869111,
-23.3353506526777));
#303628=CARTESIAN_POINT('Ctrl Pts',(-5.80111053815611,-1.71634487147645,
-23.2627511234614));
#303629=CARTESIAN_POINT('Ctrl Pts',(-5.53166742647866,-2.44936002522379,
-23.2286780048958));
#303630=CARTESIAN_POINT('Ctrl Pts',(-4.71759406830737,-3.79188557378601,
-23.1548391310901));
#303631=CARTESIAN_POINT('Ctrl Pts',(-4.17324741617074,-4.38385846244696,
-23.1171380935287));
#303632=CARTESIAN_POINT('Ctrl Pts',(-2.90022435542836,-5.3097653973734,
-23.0464747038104));
#303633=CARTESIAN_POINT('Ctrl Pts',(-2.18817042753906,-5.6406633513231,
-23.0097017276048));
#303634=CARTESIAN_POINT('Ctrl Pts',(-0.677268637078028,-6.01220148828043,
-22.9364698319252));
#303635=CARTESIAN_POINT('Ctrl Pts',(0.107166082282369,-6.04928022076788,
-22.9021587469481));
#303636=CARTESIAN_POINT('Ctrl Pts',(1.65778944458732,-5.82022117327913,
-22.8292218525854));
#303637=CARTESIAN_POINT('Ctrl Pts',(2.40838629926702,-5.55184163046472,
-22.7916190320049));
#303638=CARTESIAN_POINT('Ctrl Pts',(3.74897402294149,-4.74802073922283,
-22.7197271994846));
#303639=CARTESIAN_POINT('Ctrl Pts',(4.32931016190671,-4.22558757161908,
-22.6849901296395));
#303640=CARTESIAN_POINT('Ctrl Pts',(5.26760358278042,-2.97853795055449,
-22.6113507357543));
#303641=CARTESIAN_POINT('Ctrl Pts',(5.61243739670297,-2.26270345189369,
-22.5755329901724));
#303642=CARTESIAN_POINT('Ctrl Pts',(6.00505048721559,-0.742956757380043,
-22.5038121041637));
#303643=CARTESIAN_POINT('Ctrl Pts',(6.05065732510423,0.0458787591654085,
-22.466584859409));
#303644=CARTESIAN_POINT('Ctrl Pts',(5.83755064987419,1.58831186705197,-22.3937933412526));
#303645=CARTESIAN_POINT('Ctrl Pts',(5.58404404604623,2.32769785635364,-22.3597759082447));
#303646=CARTESIAN_POINT('Ctrl Pts',(4.79997695723648,3.68666091872496,-22.2861418040706));
#303647=CARTESIAN_POINT('Ctrl Pts',(4.27014167758665,4.28919961095268,-22.2484399008116));
#303648=CARTESIAN_POINT('Ctrl Pts',(3.02110325597171,5.24170194126841,-22.1774264213415));
#303649=CARTESIAN_POINT('Ctrl Pts',(2.31832001262212,5.58820722058684,-22.141308201694));
#303650=CARTESIAN_POINT('Ctrl Pts',(1.05648178820591,5.9300776639719,-22.0796876512508));
#303651=CARTESIAN_POINT('Ctrl Pts',(0.528871597020288,6.00000000000002,
-22.054987283025));
#303652=CARTESIAN_POINT('Ctrl Pts',(-1.62925228863742E-13,6.00000000000001,
-22.03125));
#303653=CARTESIAN_POINT('Ctrl Pts',(-1.95399252334028E-13,6.00000000000001,
-22.25));
#303654=CARTESIAN_POINT('Ctrl Pts',(0.656191862353245,6.00000000000003,
-22.2794517838416));
#303655=CARTESIAN_POINT('Ctrl Pts',(1.3088204429588,5.89235411864679,-22.3103134730883));
#303656=CARTESIAN_POINT('Ctrl Pts',(2.66420982212309,5.43144549898009,-22.3778688426481));
#303657=CARTESIAN_POINT('Ctrl Pts',(3.34166154948581,5.04300495159892,-22.4126546193864));
#303658=CARTESIAN_POINT('Ctrl Pts',(4.52376996083162,4.0198446987934,-22.4845092129917));
#303659=CARTESIAN_POINT('Ctrl Pts',(5.01300408269997,3.39019222799627,-22.5221200696207));
#303660=CARTESIAN_POINT('Ctrl Pts',(5.71415884595264,1.98829432878365,-22.5950934940657));
#303661=CARTESIAN_POINT('Ctrl Pts',(5.92350949341426,1.2316432847712,-22.6293754796774));
#303662=CARTESIAN_POINT('Ctrl Pts',(6.04178496665432,-0.319651749022043,
-22.7025852156724));
#303663=CARTESIAN_POINT('Ctrl Pts',(5.94947753572463,-1.09962436224066,
-22.7393941964615));
#303664=CARTESIAN_POINT('Ctrl Pts',(5.46672872976866,-2.5977463093425,-22.8100945531612));
#303665=CARTESIAN_POINT('Ctrl Pts',(5.07430203729619,-3.29926283752869,
-22.8477079238963));
#303666=CARTESIAN_POINT('Ctrl Pts',(4.05298994766479,-4.49131097267786,
-22.9215502467933));
#303667=CARTESIAN_POINT('Ctrl Pts',(3.44069211491054,-4.97596767892926,
-22.9556380070889));
#303668=CARTESIAN_POINT('Ctrl Pts',(2.05614934249828,-5.69103060964564,
-23.0282082820789));
#303669=CARTESIAN_POINT('Ctrl Pts',(1.29513526144091,-5.91085755822875,
-23.0655705991662));
#303670=CARTESIAN_POINT('Ctrl Pts',(-0.267634289993002,-6.04507160849594,
-23.1376694933283));
#303671=CARTESIAN_POINT('Ctrl Pts',(-1.05430233439035,-5.9584376020307,
-23.1729262486461));
#303672=CARTESIAN_POINT('Ctrl Pts',(-2.54063295535784,-5.49042836134954,
-23.2464621896157));
#303673=CARTESIAN_POINT('Ctrl Pts',(-3.22726175325772,-5.11706468944888,
-23.281653690679));
#303674=CARTESIAN_POINT('Ctrl Pts',(-4.43384493330011,-4.11915413759816,
-23.3532231684686));
#303675=CARTESIAN_POINT('Ctrl Pts',(-4.93793618465934,-3.49902022137446,
-23.3908827340176));
#303676=CARTESIAN_POINT('Ctrl Pts',(-5.66927354555103,-2.11233708108698,
-23.464112503659));
#303677=CARTESIAN_POINT('Ctrl Pts',(-5.89472741732509,-1.36191398326544,
-23.4982276591553));
#303678=CARTESIAN_POINT('Ctrl Pts',(-6.04757394140331,0.186562965779997,
-23.5713044022405));
#303679=CARTESIAN_POINT('Ctrl Pts',(-5.97218525221358,0.970078970704557,
-23.6082806051026));
#303680=CARTESIAN_POINT('Ctrl Pts',(-5.52223138513339,2.47644746769361,
-23.6793701384108));
#303681=CARTESIAN_POINT('Ctrl Pts',(-5.1472713583218,3.18333137095973,-23.7162575928246));
#303682=CARTESIAN_POINT('Ctrl Pts',(-4.15637220130421,4.39575702607239,
-23.7900342937022));
#303683=CARTESIAN_POINT('Ctrl Pts',(-3.55577783328524,4.89434051268096,
-23.8242822318611));
#303684=CARTESIAN_POINT('Ctrl Pts',(-2.18703255785244,5.64227648233448,
-23.8966228680967));
#303685=CARTESIAN_POINT('Ctrl Pts',(-1.42950610207241,5.88004402157154,
-23.9340902841137));
#303686=CARTESIAN_POINT('Ctrl Pts',(-0.432193866804079,5.98833909651615,
-23.9804318375719));
#303687=CARTESIAN_POINT('Ctrl Pts',(-0.215975941419464,6.,-23.9903063766764));
#303688=CARTESIAN_POINT('Ctrl Pts',(-2.333550019884E-13,6.00000000000001,
-24.));
#303689=CARTESIAN_POINT('Origin',(0.,5.28128932132296E-15,28.75));
#303690=CARTESIAN_POINT('',(-9.03475007386612E-14,6.00000000000001,-20.28125));
#303691=CARTESIAN_POINT('',(-1.94920572052551E-14,6.00000000000001,-20.5));
#303692=CARTESIAN_POINT('',(-7.34788079488412E-16,6.00000000000001,28.75));
#303693=CARTESIAN_POINT('Ctrl Pts',(-1.57304724801577E-13,6.00000000000001,
-22.03125));
#303694=CARTESIAN_POINT('Ctrl Pts',(-0.247873021895561,6.,-22.0201247436842));
#303695=CARTESIAN_POINT('Ctrl Pts',(-0.496002946576206,5.98464052621168,
-22.0087639645042));
#303696=CARTESIAN_POINT('Ctrl Pts',(-1.52456266669614,5.85628831960672,
-21.9607274339426));
#303697=CARTESIAN_POINT('Ctrl Pts',(-2.27935912362775,5.6057945493989,-21.9231969572814));
#303698=CARTESIAN_POINT('Ctrl Pts',(-3.63658527559146,4.83459846183184,
-21.851034122486));
#303699=CARTESIAN_POINT('Ctrl Pts',(-4.22880540848471,4.32611718065054,
-21.8166162324363));
#303700=CARTESIAN_POINT('Ctrl Pts',(-5.19795128892809,3.09928099276133,
-21.7428927596501));
#303701=CARTESIAN_POINT('Ctrl Pts',(-5.56044007690697,2.38864648574926,
-21.7064765766973));
#303702=CARTESIAN_POINT('Ctrl Pts',(-5.9867757063381,0.8766083832202,-21.6351194796338));
#303703=CARTESIAN_POINT('Ctrl Pts',(-6.0499263152208,0.0907660482333399,
-21.5980334910728));
#303704=CARTESIAN_POINT('Ctrl Pts',(-5.87223060423317,-1.455392310674,-21.525066168419));
#303705=CARTESIAN_POINT('Ctrl Pts',(-5.63520842710562,-2.20129232723029,
-21.4910212850226));
#303706=CARTESIAN_POINT('Ctrl Pts',(-4.8821456275804,-3.57673174904142,
-21.4176181515899));
#303707=CARTESIAN_POINT('Ctrl Pts',(-4.36741253731134,-4.18976557690947,
-21.3799344694682));
#303708=CARTESIAN_POINT('Ctrl Pts',(-3.14329011578986,-5.16916925119684,
-21.3085850543928));
#303709=CARTESIAN_POINT('Ctrl Pts',(-2.45002533896817,-5.53155019941288,
-21.2730457649249));
#303710=CARTESIAN_POINT('Ctrl Pts',(-0.957187551194655,-5.97457647883464,
-21.199582098388));
#303711=CARTESIAN_POINT('Ctrl Pts',(-0.171029298425594,-6.04834889542311,
-21.1646313763769));
#303712=CARTESIAN_POINT('Ctrl Pts',(1.38893230643956,-5.88968803969353,
-21.0923019950446));
#303713=CARTESIAN_POINT('Ctrl Pts',(2.14755740121632,-5.65734375361809,
-21.0548643580485));
#303714=CARTESIAN_POINT('Ctrl Pts',(3.52113213764988,-4.91933400793448,
-20.9824517191035));
#303715=CARTESIAN_POINT('Ctrl Pts',(4.12527633807941,-4.42496301159265,
-20.9482619411319));
#303716=CARTESIAN_POINT('Ctrl Pts',(5.12539903961644,-3.21868849573097,
-20.8744642354037));
#303717=CARTESIAN_POINT('Ctrl Pts',(5.50565256972684,-2.51341682920263,
-20.8373648208451));
#303718=CARTESIAN_POINT('Ctrl Pts',(5.96558036928433,-1.00951013376385,
-20.7663914664955));
#303719=CARTESIAN_POINT('Ctrl Pts',(6.04612404274221,-0.227033301870451,
-20.729464304971));
#303720=CARTESIAN_POINT('Ctrl Pts',(5.90378336153341,1.32235028147315,-20.6563447754034));
#303721=CARTESIAN_POINT('Ctrl Pts',(5.68322161727553,2.07467398036568,-20.6221873757411));
#303722=CARTESIAN_POINT('Ctrl Pts',(4.96442531708872,3.45955244748875,-20.5493743862554));
#303723=CARTESIAN_POINT('Ctrl Pts',(4.47065980115618,4.07765474955389,-20.5120788141737));
#303724=CARTESIAN_POINT('Ctrl Pts',(3.27207338608969,5.09022865022444,-20.4401713181278));
#303725=CARTESIAN_POINT('Ctrl Pts',(2.57835365451257,5.47439645533847,-20.4046390020441));
#303726=CARTESIAN_POINT('Ctrl Pts',(1.23785258780516,5.90379474609851,-20.3382113885289));
#303727=CARTESIAN_POINT('Ctrl Pts',(0.62034706770823,6.00000000000002,-20.3090929660486));
#303728=CARTESIAN_POINT('Ctrl Pts',(-1.47798440153224E-13,6.00000000000001,
-20.28125));
#303729=CARTESIAN_POINT('Ctrl Pts',(-3.76088049591772E-14,6.00000000000001,
-20.5));
#303730=CARTESIAN_POINT('Ctrl Pts',(0.751667244622775,6.00000000000001,
-20.5337369944364));
#303731=CARTESIAN_POINT('Ctrl Pts',(1.49709646348268,5.85874691471607,-20.5692539491075));
#303732=CARTESIAN_POINT('Ctrl Pts',(2.91697016964531,5.29994718308846,-20.6411311400109));
#303733=CARTESIAN_POINT('Ctrl Pts',(3.57513286629982,4.88022499191249,-20.6753457987847));
#303734=CARTESIAN_POINT('Ctrl Pts',(4.7050259366176,3.80534525963323,-20.7477266155594));
#303735=CARTESIAN_POINT('Ctrl Pts',(5.16257605915517,3.15685666003015,-20.7851777420668));
#303736=CARTESIAN_POINT('Ctrl Pts',(5.79984105333037,1.72427323992447,-20.8575504815529));
#303737=CARTESIAN_POINT('Ctrl Pts',(5.97493881429629,0.954659623675638,
-20.8924470748686));
#303738=CARTESIAN_POINT('Ctrl Pts',(6.01987134289518,-0.601709779497567,
-20.9658962838423));
#303739=CARTESIAN_POINT('Ctrl Pts',(5.89186530074486,-1.37358364193026,
-21.0015076337564));
#303740=CARTESIAN_POINT('Ctrl Pts',(5.34311178807529,-2.84252935860833,
-21.0728134403276));
#303741=CARTESIAN_POINT('Ctrl Pts',(4.92108859791892,-3.5230141412278,-21.1105006834493));
#303742=CARTESIAN_POINT('Ctrl Pts',(3.84903999758734,-4.66753875550232,
-21.1839359619654));
#303743=CARTESIAN_POINT('Ctrl Pts',(3.21440337745087,-5.12529377974754,
-21.217972170754));
#303744=CARTESIAN_POINT('Ctrl Pts',(1.8007497746658,-5.77646175250193,-21.2909172223232));
#303745=CARTESIAN_POINT('Ctrl Pts',(1.0341775543896,-5.96160739771503,-21.3280232357259));
#303746=CARTESIAN_POINT('Ctrl Pts',(-0.535211348682595,-6.02801740479988,
-21.3994304165227));
#303747=CARTESIAN_POINT('Ctrl Pts',(-1.32301831633981,-5.9053511948978,
-21.43576117391));
#303748=CARTESIAN_POINT('Ctrl Pts',(-2.79061117887403,-5.36755070584623,
-21.509473899263));
#303749=CARTESIAN_POINT('Ctrl Pts',(-3.45851012257618,-4.96354983867725,
-21.5439294686769));
#303750=CARTESIAN_POINT('Ctrl Pts',(-4.61488432690181,-3.91454190531348,
-21.6160570730109));
#303751=CARTESIAN_POINT('Ctrl Pts',(-5.08849735367067,-3.27535965659795,
-21.6535984574679));
#303752=CARTESIAN_POINT('Ctrl Pts',(-5.75808020596784,-1.85804308932178,
-21.7262847835302));
#303753=CARTESIAN_POINT('Ctrl Pts',(-5.95053647815811,-1.09494819472666,
-21.7608264843129));
#303754=CARTESIAN_POINT('Ctrl Pts',(-6.03260156551894,0.459014061554021,
-21.8341620936266));
#303755=CARTESIAN_POINT('Ctrl Pts',(-5.9226277498516,1.23502253689428,-21.8703640934126));
#303756=CARTESIAN_POINT('Ctrl Pts',(-5.40715008322945,2.71927554296194,
-21.9413312834925));
#303757=CARTESIAN_POINT('Ctrl Pts',(-4.99979132457304,3.41082384765497,
-21.9790341493098));
#303758=CARTESIAN_POINT('Ctrl Pts',(-3.95300016548896,4.57966689906188,
-22.0526972776334));
#303759=CARTESIAN_POINT('Ctrl Pts',(-3.3296347280991,5.05104938957677,-22.086717524614));
#303760=CARTESIAN_POINT('Ctrl Pts',(-1.93049251833636,5.73464181947698,
-22.1594841196669));
#303761=CARTESIAN_POINT('Ctrl Pts',(-1.16654129184404,5.93735242962764,
-22.1967286510459));
#303762=CARTESIAN_POINT('Ctrl Pts',(-0.256820521077725,5.99588198305167,
-22.2384130996943));
#303763=CARTESIAN_POINT('Ctrl Pts',(-0.128344782741232,6.,-22.2442395158865));
#303764=CARTESIAN_POINT('Ctrl Pts',(-1.91166527052644E-13,6.00000000000001,
-22.25));
#303765=CARTESIAN_POINT('Origin',(0.,5.28128932132296E-15,28.75));
#303766=CARTESIAN_POINT('',(-3.9716265690857E-14,6.00000000000001,-18.53125));
#303767=CARTESIAN_POINT('',(-3.67394039744206E-16,6.00000000000001,-18.75));
#303768=CARTESIAN_POINT('',(-7.34788079488412E-16,6.00000000000001,28.75));
#303769=CARTESIAN_POINT('Ctrl Pts',(-1.47763745683704E-13,6.00000000000001,
-20.28125));
#303770=CARTESIAN_POINT('Ctrl Pts',(-0.151341421450277,6.,-20.2744573603978));
#303771=CARTESIAN_POINT('Ctrl Pts',(-0.302844493584432,5.99427408416176,
-20.2675739625073));
#303772=CARTESIAN_POINT('Ctrl Pts',(-1.24236034038075,5.92295011427716,
-20.2243656396503));
#303773=CARTESIAN_POINT('Ctrl Pts',(-2.01098178465626,5.70795123698633,
-20.1867322915282));
#303774=CARTESIAN_POINT('Ctrl Pts',(-3.40874545772043,4.99843626968568,
-20.1136495321756));
#303775=CARTESIAN_POINT('Ctrl Pts',(-4.02678653947944,4.5154055432828,-20.079447029591));
#303776=CARTESIAN_POINT('Ctrl Pts',(-5.04534034063016,3.33930747050941,
-20.0062901872633));
#303777=CARTESIAN_POINT('Ctrl Pts',(-5.43572687334624,2.65695546252764,
-19.9694092280431));
#303778=CARTESIAN_POINT('Ctrl Pts',(-5.93889519613326,1.16642195364104,
-19.8985437012015));
#303779=CARTESIAN_POINT('Ctrl Pts',(-6.04101219096814,0.370690431713295,
-19.8612438667696));
#303780=CARTESIAN_POINT('Ctrl Pts',(-5.93076718624805,-1.19345347347955,
-19.7874277583809));
#303781=CARTESIAN_POINT('Ctrl Pts',(-5.7276852635711,-1.94729765908645,
-19.7532839443771));
#303782=CARTESIAN_POINT('Ctrl Pts',(-5.04131269253674,-3.34692773546802,
-19.6808071500655));
#303783=CARTESIAN_POINT('Ctrl Pts',(-4.56042397818458,-3.97735030277139,
-19.6433983859095));
#303784=CARTESIAN_POINT('Ctrl Pts',(-3.38500376937153,-5.01543481853053,
-19.5711595140265));
#303785=CARTESIAN_POINT('Ctrl Pts',(-2.70245368343677,-5.4138325992579,
-19.5360921922617));
#303786=CARTESIAN_POINT('Ctrl Pts',(-1.23056392229115,-5.92333804168213,
-19.4625992457995));
#303787=CARTESIAN_POINT('Ctrl Pts',(-0.456262618514595,-6.03257604821388,
-19.4272034499686));
#303788=CARTESIAN_POINT('Ctrl Pts',(1.10846582193937,-5.94969996581479,
-19.3557653139141));
#303789=CARTESIAN_POINT('Ctrl Pts',(1.88348680883554,-5.75152486160218,
-19.3180900825478));
#303790=CARTESIAN_POINT('Ctrl Pts',(3.29686085754974,-5.07271961556052,
-19.244754534603));
#303791=CARTESIAN_POINT('Ctrl Pts',(3.92439310707554,-4.60444447817209,
-19.2106868126757));
#303792=CARTESIAN_POINT('Ctrl Pts',(4.96955304918596,-3.45146912203818,
-19.1376747561693));
#303793=CARTESIAN_POINT('Ctrl Pts',(5.37591212001511,-2.77646359988469,
-19.1006312186925));
#303794=CARTESIAN_POINT('Ctrl Pts',(5.91087352636686,-1.298898771716,-19.0293789186388));
#303795=CARTESIAN_POINT('Ctrl Pts',(6.03045617527048,-0.509212114109225,
-18.9927810731533));
#303796=CARTESIAN_POINT('Ctrl Pts',(5.95721002747372,1.05342816605473,-18.9190359248263));
#303797=CARTESIAN_POINT('Ctrl Pts',(5.7719916699652,1.81168071604723,-18.884690775451));
#303798=CARTESIAN_POINT('Ctrl Pts',(5.11816962927493,3.22861464934185,-18.8124562497169));
#303799=CARTESIAN_POINT('Ctrl Pts',(4.6509165381178,3.87150983857004,-18.7749495256425));
#303800=CARTESIAN_POINT('Ctrl Pts',(3.49978141236025,4.93565584114126,-18.7023892825157));
#303801=CARTESIAN_POINT('Ctrl Pts',(2.82876329496631,5.34857491435388,-18.6677130065915));
#303802=CARTESIAN_POINT('Ctrl Pts',(1.42608294779958,5.87195791157714,-18.5971239972846));
#303803=CARTESIAN_POINT('Ctrl Pts',(0.715656660019808,6.00000000000002,
-18.5633707355119));
#303804=CARTESIAN_POINT('Ctrl Pts',(-7.63278329429795E-14,6.00000000000001,
-18.53125));
#303805=CARTESIAN_POINT('Ctrl Pts',(0.,6.00000000000001,-18.75));
#303806=CARTESIAN_POINT('Ctrl Pts',(0.0625576798651179,6.00000000000001,
-18.7528077691461));
#303807=CARTESIAN_POINT('Ctrl Pts',(0.125154581959141,5.99902163936348,
-18.7556315664582));
#303808=CARTESIAN_POINT('Ctrl Pts',(0.967737410896536,5.97264035166073,
-18.7938338417149));
#303809=CARTESIAN_POINT('Ctrl Pts',(1.73547339036332,5.7962914090571,-18.830863802741));
#303810=CARTESIAN_POINT('Ctrl Pts',(3.15621783845425,5.1614171433603,-18.9038894953428));
#303811=CARTESIAN_POINT('Ctrl Pts',(3.7964695325015,4.71049503639122,-18.9379657218031));
#303812=CARTESIAN_POINT('Ctrl Pts',(4.88096931989516,3.57819103271377,-19.0112798068587));
#303813=CARTESIAN_POINT('Ctrl Pts',(5.31018654380289,2.90332477675006,-19.0489520928996));
#303814=CARTESIAN_POINT('Ctrl Pts',(5.8753917453225,1.44214909582631,-19.1204175979676));
#303815=CARTESIAN_POINT('Ctrl Pts',(6.01232352562349,0.672350327266813,
-19.1557700009456));
#303816=CARTESIAN_POINT('Ctrl Pts',(5.98579268880053,-0.885136459007744,
-19.2292719421979));
#303817=CARTESIAN_POINT('Ctrl Pts',(5.81931204714878,-1.65794558834559,
-19.2643770423195));
#303818=CARTESIAN_POINT('Ctrl Pts',(5.19803815918352,-3.09789282705286,
-19.3365873502453));
#303819=CARTESIAN_POINT('Ctrl Pts',(4.74845942672044,-3.75081969854014,
-19.3739868089024));
#303820=CARTESIAN_POINT('Ctrl Pts',(3.63172083244038,-4.83828467655621,
-19.4464832321469));
#303821=CARTESIAN_POINT('Ctrl Pts',(2.9783622869238,-5.26571334302712,-19.4806141611536));
#303822=CARTESIAN_POINT('Ctrl Pts',(1.54139711553658,-5.8505717235476,-19.5536384882869));
#303823=CARTESIAN_POINT('Ctrl Pts',(0.770788081296015,-6.00089330918489,
-19.5903917798261));
#303824=CARTESIAN_POINT('Ctrl Pts',(-0.80324358287202,-5.99907723165657,
-19.6610653463289));
#303825=CARTESIAN_POINT('Ctrl Pts',(-1.59143129627999,-5.83963662859492,
-19.6987666602242));
#303826=CARTESIAN_POINT('Ctrl Pts',(-3.03874051749023,-5.23113632868795,
-19.7726000361462));
#303827=CARTESIAN_POINT('Ctrl Pts',(-3.68732366708566,-4.79608062870309,
-19.8066704794307));
#303828=CARTESIAN_POINT('Ctrl Pts',(-4.79093238880868,-3.69622675941705,
-19.8792756948774));
#303829=CARTESIAN_POINT('Ctrl Pts',(-5.23256165534556,-3.03899004588078,
-19.9166191904337));
#303830=CARTESIAN_POINT('Ctrl Pts',(-5.83791511633105,-1.59183537170407,
-19.9886630567254));
#303831=CARTESIAN_POINT('Ctrl Pts',(-5.99579642745818,-0.815865254731442,
-20.0239971500552));
#303832=CARTESIAN_POINT('Ctrl Pts',(-6.00398471018805,0.742684723690697,
-20.0975492661709));
#303833=CARTESIAN_POINT('Ctrl Pts',(-5.85816251601702,1.51039810786933,
-20.1326660504154));
#303834=CARTESIAN_POINT('Ctrl Pts',(-5.27658788872336,2.96370756497431,
-20.2042852996448));
#303835=CARTESIAN_POINT('Ctrl Pts',(-4.84025153538123,3.63288532261787,
-20.2419378793285));
#303836=CARTESIAN_POINT('Ctrl Pts',(-3.74338724710428,4.75289780919206,
-20.3151256591363));
#303837=CARTESIAN_POINT('Ctrl Pts',(-3.097519322501,5.19695573390423,-20.3492633345057));
#303838=CARTESIAN_POINT('Ctrl Pts',(-1.66977786964651,5.81544118927583,
-20.4223640693831));
#303839=CARTESIAN_POINT('Ctrl Pts',(-0.900973720731938,5.98296395990984,
-20.4593132579278));
#303840=CARTESIAN_POINT('Ctrl Pts',(-0.0810795530095108,5.99958931099151,
-20.4963549265385));
#303841=CARTESIAN_POINT('Ctrl Pts',(-0.0405309741502277,6.00000000000001,
-20.4981808529516));
#303842=CARTESIAN_POINT('Ctrl Pts',(-3.82493263310218E-14,6.00000000000001,
-20.5));
#303843=CARTESIAN_POINT('Origin',(0.,5.28128932132296E-15,28.75));
#303844=CARTESIAN_POINT('',(-1.02900123223315E-14,6.,-16.78125));
#303845=CARTESIAN_POINT('',(9.87720526123303E-14,6.00000000000001,-17.));
#303846=CARTESIAN_POINT('',(-7.34788079488412E-16,6.00000000000001,28.75));
#303847=CARTESIAN_POINT('Ctrl Pts',(-7.86977433022255E-14,6.00000000000001,
-18.53125));
#303848=CARTESIAN_POINT('Ctrl Pts',(-0.0591815161736599,6.,-18.5285937628204));
#303849=CARTESIAN_POINT('Ctrl Pts',(-0.118397665734984,5.99912439105894,
-18.5259232018973));
#303850=CARTESIAN_POINT('Ctrl Pts',(-0.971344796056654,5.97386191467371,
-18.4872720628927));
#303851=CARTESIAN_POINT('Ctrl Pts',(-1.75252380605554,5.79302235819084,
-18.4495732517552));
#303852=CARTESIAN_POINT('Ctrl Pts',(-3.18142084004477,5.14574194746944,
-18.3760007246305));
#303853=CARTESIAN_POINT('Ctrl Pts',(-3.81850338647645,4.69245511397807,
-18.3419843197056));
#303854=CARTESIAN_POINT('Ctrl Pts',(-4.89028640478282,3.56327240875473,
-18.2691421571158));
#303855=CARTESIAN_POINT('Ctrl Pts',(-5.31268370124598,2.8960777624856,-18.231951949522));
#303856=CARTESIAN_POINT('Ctrl Pts',(-5.87961294008907,1.43203112109182,
-18.1603290088255));
#303857=CARTESIAN_POINT('Ctrl Pts',(-6.01664803826308,0.648519325586922,
-18.1243553507422));
#303858=CARTESIAN_POINT('Ctrl Pts',(-5.98045895803983,-0.912389514358998,
-18.0506919136813));
#303859=CARTESIAN_POINT('Ctrl Pts',(-5.81315367720038,-1.67498819720559,
-18.016051448691));
#303860=CARTESIAN_POINT('Ctrl Pts',(-5.19211398101436,-3.10876791568235,
-17.9440831108857));
#303861=CARTESIAN_POINT('Ctrl Pts',(-4.73878323141223,-3.7638272730509,
-17.9064981568775));
#303862=CARTESIAN_POINT('Ctrl Pts',(-3.61221176537734,-4.85365451609604,
-17.8336387876631));
#303863=CARTESIAN_POINT('Ctrl Pts',(-2.95268028276217,-5.2808804537495,
-17.7992619693778));
#303864=CARTESIAN_POINT('Ctrl Pts',(-1.50820722228345,-5.85915920969641,
-17.7259966193809));
#303865=CARTESIAN_POINT('Ctrl Pts',(-0.737182559925239,-6.00506156514386,
-17.6894106944917));
#303866=CARTESIAN_POINT('Ctrl Pts',(0.835968013690152,-5.99454619998606,
-17.6186498092636));
#303867=CARTESIAN_POINT('Ctrl Pts',(1.62283774721748,-5.83092716781848,
-17.5809467146831));
#303868=CARTESIAN_POINT('Ctrl Pts',(3.06661496728735,-5.21486446529017,
-17.5071615801235));
#303869=CARTESIAN_POINT('Ctrl Pts',(3.71297579564821,-4.77627073019087,
-17.4731116171325));
#303870=CARTESIAN_POINT('Ctrl Pts',(4.8104566336335,-3.67069316263874,-17.400457855095));
#303871=CARTESIAN_POINT('Ctrl Pts',(5.24837854165107,-3.01148563919624,
-17.3631419536501));
#303872=CARTESIAN_POINT('Ctrl Pts',(5.84631551067217,-1.56101531678997,
-17.2911772241996));
#303873=CARTESIAN_POINT('Ctrl Pts',(6.00018354690918,-0.783579769628771,
-17.2557292120879));
#303874=CARTESIAN_POINT('Ctrl Pts',(5.99981868468909,0.775448512298382,
-17.1821545235585));
#303875=CARTESIAN_POINT('Ctrl Pts',(5.84985309194878,1.54218372945034,-17.1471398889382));
#303876=CARTESIAN_POINT('Ctrl Pts',(5.26065622016204,2.99178389100055,-17.0754508247896));
#303877=CARTESIAN_POINT('Ctrl Pts',(4.82101861067321,3.65827939799473,-17.0378090784958));
#303878=CARTESIAN_POINT('Ctrl Pts',(3.71840534420017,4.7725230781345,-16.9646820780105));
#303879=CARTESIAN_POINT('Ctrl Pts',(3.0699121665964,5.2133618283659,-16.9305083211487));
#303880=CARTESIAN_POINT('Ctrl Pts',(1.63893320564537,5.82415510192505,-16.8573744552194));
#303881=CARTESIAN_POINT('Ctrl Pts',(0.869662874250451,5.9875431625253,-16.8204646409149));
#303882=CARTESIAN_POINT('Ctrl Pts',(0.0604305076310009,5.99977183602817,
-16.7839656229107));
#303883=CARTESIAN_POINT('Ctrl Pts',(0.0302102150732426,6.00000000000001,
-16.7826059216065));
#303884=CARTESIAN_POINT('Ctrl Pts',(0.,6.00000000000001,-16.78125));
#303885=CARTESIAN_POINT('Ctrl Pts',(2.40155118014229E-13,6.00000000000001,
-17.));
#303886=CARTESIAN_POINT('Ctrl Pts',(0.149839070834264,6.00000000000001,
-17.0067252097723));
#303887=CARTESIAN_POINT('Ctrl Pts',(0.29984142897883,5.99438720189135,-17.013539601656));
#303888=CARTESIAN_POINT('Ctrl Pts',(1.23126125053171,5.92438123344339,-17.0563653306895));
#303889=CARTESIAN_POINT('Ctrl Pts',(1.99378277856738,5.71306256869026,-17.0936712272069));
#303890=CARTESIAN_POINT('Ctrl Pts',(3.3856398038237,5.01362882161217,-17.1663418613708));
#303891=CARTESIAN_POINT('Ctrl Pts',(4.00345032815514,4.53557099792926,-17.2003857335309));
#303892=CARTESIAN_POINT('Ctrl Pts',(5.03766420273522,3.35484842220266,-17.2741535349205));
#303893=CARTESIAN_POINT('Ctrl Pts',(5.43768812582968,2.65795542972892,-17.3118569970205));
#303894=CARTESIAN_POINT('Ctrl Pts',(5.93664279052796,1.16630144852512,-17.3826484198299));
#303895=CARTESIAN_POINT('Ctrl Pts',(6.0376698073148,0.388270682262536,-17.4191764744786));
#303896=CARTESIAN_POINT('Ctrl Pts',(5.93720336712971,-1.16442414842643,
-17.4924522706097));
#303897=CARTESIAN_POINT('Ctrl Pts',(5.73615945908819,-1.92425541901812,
-17.5268512437108));
#303898=CARTESIAN_POINT('Ctrl Pts',(5.05054144881868,-3.33380380872942,
-17.5996857850032));
#303899=CARTESIAN_POINT('Ctrl Pts',(4.56898506298219,-3.96820028743554,
-17.6372647923931));
#303900=CARTESIAN_POINT('Ctrl Pts',(3.39952375656374,-5.00415180210665,
-17.709256932137));
#303901=CARTESIAN_POINT('Ctrl Pts',(2.72677857386028,-5.40027560207936,
-17.7438683302719));
#303902=CARTESIAN_POINT('Ctrl Pts',(1.25428390249301,-5.920119876792,-17.8175392014876));
#303903=CARTESIAN_POINT('Ctrl Pts',(0.466727693143441,-6.03350134537977,
-17.8535633533743));
#303904=CARTESIAN_POINT('Ctrl Pts',(-1.10112874673013,-5.94971903273988,
-17.9251550989244));
#303905=CARTESIAN_POINT('Ctrl Pts',(-1.86642583924248,-5.75569549769191,
-17.9623333501411));
#303906=CARTESIAN_POINT('Ctrl Pts',(-3.27280399884356,-5.08812162592839,
-18.035191111525));
#303907=CARTESIAN_POINT('Ctrl Pts',(-3.9017540577933,-4.62347698782573,
-18.0692085445849));
#303908=CARTESIAN_POINT('Ctrl Pts',(-4.96110379436915,-3.46664759703071,
-18.1427613596476));
#303909=CARTESIAN_POINT('Ctrl Pts',(-5.37576543940734,-2.7805448114744,
-18.180458893232));
#303910=CARTESIAN_POINT('Ctrl Pts',(-5.90777261316549,-1.30382779769193,
-18.2515968761224));
#303911=CARTESIAN_POINT('Ctrl Pts',(-6.02670083067333,-0.529862767402638,
-18.2874943676283));
#303912=CARTESIAN_POINT('Ctrl Pts',(-5.96306756539131,1.02531963810942,
-18.3608875590274));
#303913=CARTESIAN_POINT('Ctrl Pts',(-5.77922274327131,1.79166177857745,
-18.3955943244606));
#303914=CARTESIAN_POINT('Ctrl Pts',(-5.12568929132447,3.21662469276153,
-18.4681273887681));
#303915=CARTESIAN_POINT('Ctrl Pts',(-4.66004482307642,3.86048509497539,
-18.5056263425187));
#303916=CARTESIAN_POINT('Ctrl Pts',(-3.51680399465396,4.922414739695,-18.577882984766));
#303917=CARTESIAN_POINT('Ctrl Pts',(-2.85374503878448,5.33424812827792,
-18.6122068083788));
#303918=CARTESIAN_POINT('Ctrl Pts',(-1.44965307897512,5.86766072759046,
-18.683005439964));
#303919=CARTESIAN_POINT('Ctrl Pts',(-0.727564949466366,6.00000000000001,
-18.7173447861033));
#303920=CARTESIAN_POINT('Ctrl Pts',(-3.60822483003176E-15,6.00000000000001,
-18.75));
#303921=CARTESIAN_POINT('Origin',(0.,5.28128932132296E-15,28.75));
#303922=CARTESIAN_POINT('',(7.74869955620949E-14,6.00000000000001,-15.03125));
#303923=CARTESIAN_POINT('',(8.5709584838225E-14,6.00000000000001,-15.25));
#303924=CARTESIAN_POINT('',(-7.34788079488412E-16,6.00000000000001,28.75));
#303925=CARTESIAN_POINT('Ctrl Pts',(-2.77555756156289E-15,6.,-16.78125));
#303926=CARTESIAN_POINT('Ctrl Pts',(-0.762995914369974,6.,-16.7470045421831));
#303927=CARTESIAN_POINT('Ctrl Pts',(-1.51937474040237,5.85445698505616,
-16.7109335760792));
#303928=CARTESIAN_POINT('Ctrl Pts',(-2.94654565841153,5.28357027467349,
-16.6385525968161));
#303929=CARTESIAN_POINT('Ctrl Pts',(-3.60240026688677,4.86014142112396,
-16.6043810427931));
#303930=CARTESIAN_POINT('Ctrl Pts',(-4.72598043643502,3.77920016817781,
-16.5319439136972));
#303931=CARTESIAN_POINT('Ctrl Pts',(-5.17970425282934,3.1285664882428,-16.494517027221));
#303932=CARTESIAN_POINT('Ctrl Pts',(-5.8092898938032,1.69243114615325,-16.4222216952709));
#303933=CARTESIAN_POINT('Ctrl Pts',(-5.98025194768284,0.921280430733282,
-16.3872276722945));
#303934=CARTESIAN_POINT('Ctrl Pts',(-6.01635011330383,-0.635631715023033,
-16.3137528498556));
#303935=CARTESIAN_POINT('Ctrl Pts',(-5.88405811920462,-1.4065114945738,
-16.278268627381));
#303936=CARTESIAN_POINT('Ctrl Pts',(-5.32740290463626,-2.87174215114001,
-16.2068854740689));
#303937=CARTESIAN_POINT('Ctrl Pts',(-4.90191964302404,-3.54954068251286,
-16.1692048116772));
#303938=CARTESIAN_POINT('Ctrl Pts',(-3.82388772255212,-4.68821226796535,
-16.0958270276199));
#303939=CARTESIAN_POINT('Ctrl Pts',(-3.18655783477906,-5.14269353849257,
-16.0617742944772));
#303940=CARTESIAN_POINT('Ctrl Pts',(-1.76949133222635,-5.78605770987929,
-15.9887898675571));
#303941=CARTESIAN_POINT('Ctrl Pts',(-1.002349018499,-5.96698758165948,-15.9517197467449));
#303942=CARTESIAN_POINT('Ctrl Pts',(0.567728586615961,-6.02514302424957,
-15.8804020340791));
#303943=CARTESIAN_POINT('Ctrl Pts',(1.35564413377838,-5.89805180320577,
-15.8439180358184));
#303944=CARTESIAN_POINT('Ctrl Pts',(2.82088234409026,-5.35170012385111,
-15.7701862891916));
#303945=CARTESIAN_POINT('Ctrl Pts',(3.486466596131,-4.94394913206419,-15.7357966941946));
#303946=CARTESIAN_POINT('Ctrl Pts',(4.63656757456683,-3.88874666387088,
-15.6636065985564));
#303947=CARTESIAN_POINT('Ctrl Pts',(5.10637394239805,-3.2473143931632,-15.6260849024967));
#303948=CARTESIAN_POINT('Ctrl Pts',(5.76828544948956,-1.8263270111654,-15.5534712225508));
#303949=CARTESIAN_POINT('Ctrl Pts',(5.9566277070017,-1.0616775585047,-15.5188533859303));
#303950=CARTESIAN_POINT('Ctrl Pts',(6.02988463147326,0.492873969955938,
-15.4454899672962));
#303951=CARTESIAN_POINT('Ctrl Pts',(5.91563081234682,1.26790813161792,-15.4094362565975));
#303952=CARTESIAN_POINT('Ctrl Pts',(5.39225127407362,2.74857516884805,-15.3383867864066));
#303953=CARTESIAN_POINT('Ctrl Pts',(4.98139695353482,3.43753260359899,-15.3006858752191));
#303954=CARTESIAN_POINT('Ctrl Pts',(3.92859923421987,4.60064881530623,-15.2270747788359));
#303955=CARTESIAN_POINT('Ctrl Pts',(3.30256757325392,5.06881789833565,-15.193058499304));
#303956=CARTESIAN_POINT('Ctrl Pts',(1.89995959949218,5.74477422197141,-15.1202477106475));
#303957=CARTESIAN_POINT('Ctrl Pts',(1.13535431743488,5.94334142844029,-15.0830342480049));
#303958=CARTESIAN_POINT('Ctrl Pts',(0.236119305774866,5.99651893777345,
-15.0418984811186));
#303959=CARTESIAN_POINT('Ctrl Pts',(0.118002034649196,6.00000000000001,
-15.0365462717411));
#303960=CARTESIAN_POINT('Ctrl Pts',(1.47416800988509E-13,6.00000000000001,
-15.03125));
#303961=CARTESIAN_POINT('Ctrl Pts',(1.46965772884755E-13,6.00000000000001,
-15.25));
#303962=CARTESIAN_POINT('Ctrl Pts',(0.239244323353593,6.00000000000001,
-15.2607379754322));
#303963=CARTESIAN_POINT('Ctrl Pts',(0.478743560224347,5.98569123812276,
-15.2716960615625));
#303964=CARTESIAN_POINT('Ctrl Pts',(1.49888728445648,5.86286612757501,-15.3192742544649));
#303965=CARTESIAN_POINT('Ctrl Pts',(2.25444285070019,5.61581264251811,-15.3567886313169));
#303966=CARTESIAN_POINT('Ctrl Pts',(3.61480890219032,4.85090024903875,-15.429000756656));
#303967=CARTESIAN_POINT('Ctrl Pts',(4.20929919129207,4.34509667563156,-15.4633680510008));
#303968=CARTESIAN_POINT('Ctrl Pts',(5.18434125342705,3.12215321735148,-15.5371064557438));
#303969=CARTESIAN_POINT('Ctrl Pts',(5.55020848663417,2.41252824406093,-15.5736463796502));
#303970=CARTESIAN_POINT('Ctrl Pts',(5.98295890856739,0.902007856180706,
-15.6449318517253));
#303971=CARTESIAN_POINT('Ctrl Pts',(6.04943761408849,0.116778643172001,
-15.6819889054305));
#303972=CARTESIAN_POINT('Ctrl Pts',(5.87848705715856,-1.43003326182809,
-15.7549870706616));
#303973=CARTESIAN_POINT('Ctrl Pts',(5.64460477390343,-2.1771648796185,-15.7890468905164));
#303974=CARTESIAN_POINT('Ctrl Pts',(4.89744175132958,-3.55568208160752,
-15.8624038777688));
#303975=CARTESIAN_POINT('Ctrl Pts',(4.38559395946307,-4.17066467448128,
-15.9000819273598));
#303976=CARTESIAN_POINT('Ctrl Pts',(3.1662280353415,-5.15512186862005,-15.9714923429295));
#303977=CARTESIAN_POINT('Ctrl Pts',(2.47476798475488,-5.52049650357891,
-16.0069325140209));
#303978=CARTESIAN_POINT('Ctrl Pts',(0.983693207862198,-5.97033057503644,
-16.0804163318438));
#303979=CARTESIAN_POINT('Ctrl Pts',(0.197391021470089,-6.04760579088883,
-16.1154462703826));
#303980=CARTESIAN_POINT('Ctrl Pts',(-1.3633589140374,-5.89561518199393,
-16.1877137598355));
#303981=CARTESIAN_POINT('Ctrl Pts',(-2.12265616753833,-5.66668645028802,
-16.2251317550863));
#303982=CARTESIAN_POINT('Ctrl Pts',(-3.49924836607179,-4.93493292272614,
-16.2975885899212));
#303983=CARTESIAN_POINT('Ctrl Pts',(-4.10562278276477,-4.4432136474317,
-16.3317460828671));
#303984=CARTESIAN_POINT('Ctrl Pts',(-5.11154083410974,-3.24081677352315,
-16.4055564996032));
#303985=CARTESIAN_POINT('Ctrl Pts',(-5.49512206213318,-2.53656496888065,
-16.4427927569157));
#303986=CARTESIAN_POINT('Ctrl Pts',(-5.96130427935292,-1.03422257730741,
-16.5136922876079));
#303987=CARTESIAN_POINT('Ctrl Pts',(-6.04507636618779,-0.252414557192574,
-16.5505878861269));
#303988=CARTESIAN_POINT('Ctrl Pts',(-5.9093273272881,1.29751549309194,-16.623733204922));
#303989=CARTESIAN_POINT('Ctrl Pts',(-5.69183561586978,2.05102812652172,
-16.657920888541));
#303990=CARTESIAN_POINT('Ctrl Pts',(-4.97543154461942,3.44529752823625,
-16.7310260623448));
#303991=CARTESIAN_POINT('Ctrl Pts',(-4.4786810474085,4.07019095030031,-16.7686637179511));
#303992=CARTESIAN_POINT('Ctrl Pts',(-3.28419150975437,5.08066070730256,
-16.8403772346117));
#303993=CARTESIAN_POINT('Ctrl Pts',(-2.60210904155631,5.46150942826808,
-16.8753568518416));
#303994=CARTESIAN_POINT('Ctrl Pts',(-1.26309840810919,5.89980686100247,
-16.9418473495661));
#303995=CARTESIAN_POINT('Ctrl Pts',(-0.633071948168211,6.00000000000001,
-16.9715859046061));
#303996=CARTESIAN_POINT('Ctrl Pts',(2.37448949391705E-13,6.00000000000001,
-17.));
#303997=CARTESIAN_POINT('Origin',(0.,5.28128932132296E-15,28.75));
#303998=CARTESIAN_POINT('',(9.14341723089484E-14,6.00000000000001,-13.28125));
#303999=CARTESIAN_POINT('',(6.50211092512395E-15,6.00000000000001,-13.5));
#304000=CARTESIAN_POINT('',(-7.34788079488412E-16,6.00000000000001,28.75));
#304001=CARTESIAN_POINT('Ctrl Pts',(1.46549439250521E-13,6.,-15.03125));
#304002=CARTESIAN_POINT('Ctrl Pts',(-0.66735187386771,6.,-15.0012973226459));
#304003=CARTESIAN_POINT('Ctrl Pts',(-1.33087327795904,5.88866100281656,
-14.9698928741171));
#304004=CARTESIAN_POINT('Ctrl Pts',(-2.69406578468223,5.41668316456592,
-14.9018258515768));
#304005=CARTESIAN_POINT('Ctrl Pts',(-3.36927694279044,5.02458086822543,
-14.8671259278388));
#304006=CARTESIAN_POINT('Ctrl Pts',(-4.545372492241,3.99531773232578,-14.795205119886));
#304007=CARTESIAN_POINT('Ctrl Pts',(-5.03095626552528,3.36339510574058,
-14.7576088470367));
#304008=CARTESIAN_POINT('Ctrl Pts',(-5.7247193048184,1.95784216770291,-14.6847009145714));
#304009=CARTESIAN_POINT('Ctrl Pts',(-5.93011958458863,1.19967591081642,
-14.6503658949762));
#304010=CARTESIAN_POINT('Ctrl Pts',(-6.03992846624795,-0.352356705974768,
-14.5771213504791));
#304011=CARTESIAN_POINT('Ctrl Pts',(-5.94344657136843,-1.1314072910134,
-14.5404193980675));
#304012=CARTESIAN_POINT('Ctrl Pts',(-5.45288773164758,-2.62677185445911,
-14.469719199516));
#304013=CARTESIAN_POINT('Ctrl Pts',(-5.05660369673818,-3.32634294818924,
-14.4320172297277));
#304014=CARTESIAN_POINT('Ctrl Pts',(-4.0287896424963,-4.5130527616718,-14.3581983631882));
#304015=CARTESIAN_POINT('Ctrl Pts',(-3.41379145975777,-4.9944802221304,
-14.3241346393133));
#304016=CARTESIAN_POINT('Ctrl Pts',(-2.02565547621593,-5.70189879844987,
-14.25151457081));
#304017=CARTESIAN_POINT('Ctrl Pts',(-1.26389202499577,-5.91756242934041,
-14.2141793348777));
#304018=CARTESIAN_POINT('Ctrl Pts',(0.299762092627998,-6.04364376330619,
-14.1421593409458));
#304019=CARTESIAN_POINT('Ctrl Pts',(1.08658867426295,-5.95271641631752,
-14.1067912133187));
#304020=CARTESIAN_POINT('Ctrl Pts',(2.57072633147742,-5.47637605377605,
-14.0332322033617));
#304021=CARTESIAN_POINT('Ctrl Pts',(3.25513422151646,-5.09935195025191,
-13.9981468843864));
#304022=CARTESIAN_POINT('Ctrl Pts',(4.45581733815711,-4.09529386357075,
-13.926506358527));
#304023=CARTESIAN_POINT('Ctrl Pts',(4.95632750342893,-3.47282417207507,
-13.8888569501452));
#304024=CARTESIAN_POINT('Ctrl Pts',(5.68037470491989,-2.0824231669912,-13.8156874564946));
#304025=CARTESIAN_POINT('Ctrl Pts',(5.90194277265011,-1.33048982502385,
-13.7815393512917));
#304026=CARTESIAN_POINT('Ctrl Pts',(6.04644434796632,0.218710856532157,
-13.7084284533456));
#304027=CARTESIAN_POINT('Ctrl Pts',(5.96696002944824,1.00140412246603,-13.6714910777235));
#304028=CARTESIAN_POINT('Ctrl Pts',(5.5090831597919,2.50582032466959,-13.6004936783954));
#304029=CARTESIAN_POINT('Ctrl Pts',(5.12991944744186,3.21142492404718,-13.563438477574));
#304030=CARTESIAN_POINT('Ctrl Pts',(4.13169520542801,4.41896754161158,-13.4896450178015));
#304031=CARTESIAN_POINT('Ctrl Pts',(3.52828162141067,4.91420636676231,-13.4554439484537));
#304032=CARTESIAN_POINT('Ctrl Pts',(2.15569821673854,5.65426229804528,-13.3830459631315));
#304033=CARTESIAN_POINT('Ctrl Pts',(1.39729636086131,5.88772412806485,-13.3456020482254));
#304034=CARTESIAN_POINT('Ctrl Pts',(0.41062612721705,5.98947399864505,-13.2998335893983));
#304035=CARTESIAN_POINT('Ctrl Pts',(0.205196689547594,6.00000000000001,
-13.2904598194023));
#304036=CARTESIAN_POINT('Ctrl Pts',(1.60357838119296E-13,6.00000000000001,
-13.28125));
#304037=CARTESIAN_POINT('Ctrl Pts',(-1.38777878078145E-16,6.00000000000001,
-13.5));
#304038=CARTESIAN_POINT('Ctrl Pts',(0.327777791193107,6.00000000000001,
-13.5147116128805));
#304039=CARTESIAN_POINT('Ctrl Pts',(0.655733943217833,5.97314225488786,
-13.5298229065593));
#304040=CARTESIAN_POINT('Ctrl Pts',(1.76080102696931,5.79008139572056,-13.5820911428346));
#304041=CARTESIAN_POINT('Ctrl Pts',(2.50784671930172,5.50783221520244,-13.6197368425539));
#304042=CARTESIAN_POINT('Ctrl Pts',(3.83516240013118,4.67875298122624,-13.6914013383341));
#304043=CARTESIAN_POINT('Ctrl Pts',(4.40618039353526,4.14545661396193,-13.7264515580286));
#304044=CARTESIAN_POINT('Ctrl Pts',(5.32030200711686,2.88274754157419,-13.8000183191284));
#304045=CARTESIAN_POINT('Ctrl Pts',(5.65133170850177,2.16293172541357,-13.835425502794));
#304046=CARTESIAN_POINT('Ctrl Pts',(6.0173450674626,0.637422317825967,-13.90741834655));
#304047=CARTESIAN_POINT('Ctrl Pts',(6.04906161240216,-0.153501012269999,
-13.9447441207756));
#304048=CARTESIAN_POINT('Ctrl Pts',(5.80808025958564,-1.69265443149444,
-14.0173808617066));
#304049=CARTESIAN_POINT('Ctrl Pts',(5.54159120090127,-2.4268558179121,-14.0514375150167));
#304050=CARTESIAN_POINT('Ctrl Pts',(4.73308137588808,-3.77246607804078,
-14.1252398343965));
#304051=CARTESIAN_POINT('Ctrl Pts',(4.19141704377373,-4.36642845683353,
-14.1629424247462));
#304052=CARTESIAN_POINT('Ctrl Pts',(2.92283134564345,-5.29730868071715,
-14.2336726042976));
#304053=CARTESIAN_POINT('Ctrl Pts',(2.21250088012577,-5.63111929827263,
-14.2703170673848));
#304054=CARTESIAN_POINT('Ctrl Pts',(0.703234222332097,-6.00926253915792,
-14.3435718980254));
#304055=CARTESIAN_POINT('Ctrl Pts',(-0.0813751723367943,-6.04972473594463,
-14.377927200096));
#304056=CARTESIAN_POINT('Ctrl Pts',(-1.6329431622039,-5.82719528272542,
-14.4508112688191));
#304057=CARTESIAN_POINT('Ctrl Pts',(-2.38435662489997,-5.5621557904809,
-14.4884020320523));
#304058=CARTESIAN_POINT('Ctrl Pts',(-3.72809186809351,-4.7644223507681,
-14.5603463589942));
#304059=CARTESIAN_POINT('Ctrl Pts',(-4.31065812373274,-4.24459900497216,
-14.5950166285999));
#304060=CARTESIAN_POINT('Ctrl Pts',(-5.25473931733798,-3.00132172450994,
-14.6686725436814));
#304061=CARTESIAN_POINT('Ctrl Pts',(-5.60288211475291,-2.28645239165933,
-14.7045962342353));
#304062=CARTESIAN_POINT('Ctrl Pts',(-6.00184118239683,-0.768121793220075,
-14.7762502909063));
#304063=CARTESIAN_POINT('Ctrl Pts',(-6.05075533966853,0.0201800109101076,
-14.8134523483535));
#304064=CARTESIAN_POINT('Ctrl Pts',(-5.84430619638249,1.56335120441045,
-14.8862786987318));
#304065=CARTESIAN_POINT('Ctrl Pts',(-5.59389917079461,2.30396805033726,
-14.9202947230065));
#304066=CARTESIAN_POINT('Ctrl Pts',(-4.81566514298174,3.66607000268275,
-14.9938868647953));
#304067=CARTESIAN_POINT('Ctrl Pts',(-4.28866309072003,4.27061589916235,
-15.03158681112));
#304068=CARTESIAN_POINT('Ctrl Pts',(-3.04430197290824,5.22822388667977,
-15.1026654784338));
#304069=CARTESIAN_POINT('Ctrl Pts',(-2.34331405581276,5.57773485223415,
-15.1386672715034));
#304070=CARTESIAN_POINT('Ctrl Pts',(-1.07453784633482,5.92765342078551,
-15.2007165872237));
#304071=CARTESIAN_POINT('Ctrl Pts',(-0.537960873596693,6.00000000000001,
-15.2258547640204));
#304072=CARTESIAN_POINT('Ctrl Pts',(1.61121116448726E-13,6.00000000000001,
-15.25));
#304073=CARTESIAN_POINT('Origin',(0.,5.28128932132296E-15,28.75));
#304074=CARTESIAN_POINT('',(2.04492876719775E-14,6.00000000000001,-11.53125));
#304075=CARTESIAN_POINT('',(-6.44949795900495E-16,6.00000000000001,-11.75));
#304076=CARTESIAN_POINT('',(-7.34788079488412E-16,6.00000000000001,28.75));
#304077=CARTESIAN_POINT('Ctrl Pts',(1.57512891618694E-13,6.00000000000001,
-13.28125));
#304078=CARTESIAN_POINT('Ctrl Pts',(-0.573980629105695,6.00000000000001,
-13.2554880934792));
#304079=CARTESIAN_POINT('Ctrl Pts',(-1.14603217573204,5.91763999221552,
-13.2286116862984));
#304080=CARTESIAN_POINT('Ctrl Pts',(-2.4419267062499,5.53513980010466,-13.1648700734188));
#304081=CARTESIAN_POINT('Ctrl Pts',(-3.13578102190386,5.17373789630424,
-13.1292976708043));
#304082=CARTESIAN_POINT('Ctrl Pts',(-4.36145501139311,4.19598829988954,
-13.0579683686895));
#304083=CARTESIAN_POINT('Ctrl Pts',(-4.87712915420713,3.58359392864256,
-13.0202829968094));
#304084=CARTESIAN_POINT('Ctrl Pts',(-5.63211775910767,2.20916311949069,
-12.9468649516664));
#304085=CARTESIAN_POINT('Ctrl Pts',(-5.87016462544125,1.46366565576377,
-12.9128242727264));
#304086=CARTESIAN_POINT('Ctrl Pts',(-6.0500616200403,-0.0822755225612855,
-12.8398671994015));
#304087=CARTESIAN_POINT('Ctrl Pts',(-5.98799810878256,-0.868314983456971,
-12.8027719079449));
#304088=CARTESIAN_POINT('Ctrl Pts',(-5.56375655704784,-2.38084496844363,
-12.7313915976408));
#304089=CARTESIAN_POINT('Ctrl Pts',(-5.20236924062146,-3.0918075866398,
-12.6950151226897));
#304090=CARTESIAN_POINT('Ctrl Pts',(-4.23514621504392,-4.31991116899216,
-12.6212965995673));
#304091=CARTESIAN_POINT('Ctrl Pts',(-3.64366648286652,-4.82926489771456,
-12.5868614836686));
#304092=CARTESIAN_POINT('Ctrl Pts',(-2.28746711962188,-5.60250684109875,
-12.5147148987157));
#304093=CARTESIAN_POINT('Ctrl Pts',(-1.53292126968421,-5.8541210542095,
-12.477179330227));
#304094=CARTESIAN_POINT('Ctrl Pts',(0.0222798434847502,-6.05041700754087,
-12.4045147683223));
#304095=CARTESIAN_POINT('Ctrl Pts',(0.807561443282626,-5.99632148589134,
-12.3699506676802));
#304096=CARTESIAN_POINT('Ctrl Pts',(2.31017703688754,-5.59159109628828,
-12.296606626736));
#304097=CARTESIAN_POINT('Ctrl Pts',(3.01354411696049,-5.2460644128885,-12.2604498204306));
#304098=CARTESIAN_POINT('Ctrl Pts',(4.26410133507651,-4.29522557818065,
-12.1894577225396));
#304099=CARTESIAN_POINT('Ctrl Pts',(4.79485640139218,-3.69334236966529,
-12.1517553313286));
#304100=CARTESIAN_POINT('Ctrl Pts',(5.58081886858524,-2.33540318145575,
-12.078107742142));
#304101=CARTESIAN_POINT('Ctrl Pts',(5.83533250109748,-1.59641767050439,
-12.0440891931576));
#304102=CARTESIAN_POINT('Ctrl Pts',(6.05060200132583,-0.0542281005932625,
-11.9713091682056));
#304103=CARTESIAN_POINT('Ctrl Pts',(6.00607047451364,0.734777899607572,
-11.934073877874));
#304104=CARTESIAN_POINT('Ctrl Pts',(5.61551958022899,2.25498133873888,-11.8623314368728));
#304105=CARTESIAN_POINT('Ctrl Pts',(5.27175974242709,2.97112818183415,-11.8265474550426));
#304106=CARTESIAN_POINT('Ctrl Pts',(4.3353453527759,4.21940059916099,-11.752913497935));
#304107=CARTESIAN_POINT('Ctrl Pts',(3.75573331455707,4.74268032871428,-11.7181540580097));
#304108=CARTESIAN_POINT('Ctrl Pts',(2.41617000682841,5.54847427122919,-11.646279430568));
#304109=CARTESIAN_POINT('Ctrl Pts',(1.66584109193327,5.81793662423257,-11.6086728449161));
#304110=CARTESIAN_POINT('Ctrl Pts',(0.591316333642613,5.97816519706421,
-11.558108407162));
#304111=CARTESIAN_POINT('Ctrl Pts',(0.295541259485836,6.00000000000001,
-11.5445147443378));
#304112=CARTESIAN_POINT('Ctrl Pts',(8.16707812489881E-14,6.00000000000001,
-11.53125));
#304113=CARTESIAN_POINT('Ctrl Pts',(-1.45716771982052E-15,6.00000000000001,
-11.75));
#304114=CARTESIAN_POINT('Ctrl Pts',(0.416845576792399,6.00000000000001,
-11.7687092320514));
#304115=CARTESIAN_POINT('Ctrl Pts',(0.833493300982548,5.95656316824371,
-11.7880430377037));
#304116=CARTESIAN_POINT('Ctrl Pts',(2.02039612084546,5.70518972109559,-11.8449805231463));
#304117=CARTESIAN_POINT('Ctrl Pts',(2.75728128825485,5.38782752092871,-11.8826822540648));
#304118=CARTESIAN_POINT('Ctrl Pts',(4.04949626850756,4.49489052928717,-11.9537025881064));
#304119=CARTESIAN_POINT('Ctrl Pts',(4.59645541967849,3.93385564503483,-11.9898084787577));
#304120=CARTESIAN_POINT('Ctrl Pts',(5.44827395812056,2.63146422558047,-12.0631620642225));
#304121=CARTESIAN_POINT('Ctrl Pts',(5.74384238938711,1.90173151395159,-12.0977522350444));
#304122=CARTESIAN_POINT('Ctrl Pts',(6.04060669966887,0.36251640842141,-12.1703918871161));
#304123=CARTESIAN_POINT('Ctrl Pts',(6.03598507272798,-0.432709508607057,
-12.2079207118553));
#304124=CARTESIAN_POINT('Ctrl Pts',(5.7226670320772,-1.96193118601187,-12.2800887474913));
#304125=CARTESIAN_POINT('Ctrl Pts',(5.42241874027092,-2.68243489957792,
-12.3145011806245));
#304126=CARTESIAN_POINT('Ctrl Pts',(4.55568892318795,-3.98372213282641,
-12.3882262348037));
#304127=CARTESIAN_POINT('Ctrl Pts',(3.99206020552507,-4.54837147961571,
-12.4246552386242));
#304128=CARTESIAN_POINT('Ctrl Pts',(2.68612979394882,-5.42167675647812,
-12.4960048649511));
#304129=CARTESIAN_POINT('Ctrl Pts',(1.95843226440761,-5.72488742607485,
-12.5330878516889));
#304130=CARTESIAN_POINT('Ctrl Pts',(0.433189775767892,-6.03437164221625,
-12.6060584462626));
#304131=CARTESIAN_POINT('Ctrl Pts',(-0.349468372851078,-6.0397987907425,
-12.6401047497293));
#304132=CARTESIAN_POINT('Ctrl Pts',(-1.8904147258544,-5.74931568846158,
-12.7135030794629));
#304133=CARTESIAN_POINT('Ctrl Pts',(-2.63260735637681,-5.44956408199337,
-12.7511862034793));
#304134=CARTESIAN_POINT('Ctrl Pts',(-3.94270090736319,-4.58864472992702,
-12.8225420554432));
#304135=CARTESIAN_POINT('Ctrl Pts',(-4.50181657165394,-4.0415696806281,
-12.8580707922009));
#304136=CARTESIAN_POINT('Ctrl Pts',(-5.38509416954836,-2.75909556727989,
-12.9315365891624));
#304137=CARTESIAN_POINT('Ctrl Pts',(-5.69854638141101,-2.03431059711724,
-12.9664954757139));
#304138=CARTESIAN_POINT('Ctrl Pts',(-6.03039733330066,-0.501806972866215,
-13.038818395145));
#304139=CARTESIAN_POINT('Ctrl Pts',(-6.04421585770172,0.291443690587449,
-13.0762540024177));
#304140=CARTESIAN_POINT('Ctrl Pts',(-5.76750740744192,1.8259476416692,-13.1486713225888));
#304141=CARTESIAN_POINT('Ctrl Pts',(-5.4843606631894,2.55342877114943,-13.1828575540103));
#304142=CARTESIAN_POINT('Ctrl Pts',(-4.64675548347716,3.87781462041123,
-13.2566566129115));
#304143=CARTESIAN_POINT('Ctrl Pts',(-4.09371675122386,4.45769755329096,
-13.2937702714903));
#304144=CARTESIAN_POINT('Ctrl Pts',(-2.80590088304983,5.36042237566801,
-13.3647358998891));
#304145=CARTESIAN_POINT('Ctrl Pts',(-2.08678176698081,5.67912400530407,
-13.4016597725162));
#304146=CARTESIAN_POINT('Ctrl Pts',(-0.890512478632302,5.95039638288354,
-13.4593078448214));
#304147=CARTESIAN_POINT('Ctrl Pts',(-0.445453596806061,6.00000000000001,
-13.4800067574786));
#304148=CARTESIAN_POINT('Ctrl Pts',(-7.21644966006352E-15,6.00000000000001,
-13.5));
#304149=CARTESIAN_POINT('Origin',(0.,5.28128932132296E-15,28.75));
#304150=CARTESIAN_POINT('',(-2.93478478418988E-15,6.00000000000001,-9.78125));
#304151=CARTESIAN_POINT('',(-6.83338598285155E-14,6.00000000000001,-10.));
#304152=CARTESIAN_POINT('',(-7.34788079488412E-16,6.00000000000001,28.75));
#304153=CARTESIAN_POINT('Ctrl Pts',(7.74380559676047E-14,6.00000000000001,
-11.53125));
#304154=CARTESIAN_POINT('Ctrl Pts',(-0.478944394585049,6.00000000000001,
-11.5097535938561));
#304155=CARTESIAN_POINT('Ctrl Pts',(-0.957199281274125,5.94265698294226,
-11.4874518824837));
#304156=CARTESIAN_POINT('Ctrl Pts',(-2.18016139292464,5.64376182111039,
-11.4282029269918));
#304157=CARTESIAN_POINT('Ctrl Pts',(-2.8927901865173,5.31385278926475,-11.3914069174792));
#304158=CARTESIAN_POINT('Ctrl Pts',(-4.16707304774843,4.38968577054325,
-11.320735990777));
#304159=CARTESIAN_POINT('Ctrl Pts',(-4.7122067867575,3.79858157252758,-11.2830659584832));
#304160=CARTESIAN_POINT('Ctrl Pts',(-5.52817353808929,2.4572253914444,-11.2092192096192));
#304161=CARTESIAN_POINT('Ctrl Pts',(-5.79864984016499,1.72462569233648,
-11.1751396704854));
#304162=CARTESIAN_POINT('Ctrl Pts',(-6.04818769601602,0.186540241838315,
-11.1025533298373));
#304163=CARTESIAN_POINT('Ctrl Pts',(-6.02074829091575,-0.604976250624933,
-11.065199562703));
#304164=CARTESIAN_POINT('Ctrl Pts',(-5.66290961022047,-2.1322007963153,
-10.9931257770211));
#304165=CARTESIAN_POINT('Ctrl Pts',(-5.33610124725688,-2.85322000262038,
-10.9578339280619));
#304166=CARTESIAN_POINT('Ctrl Pts',(-4.4293802801778,-4.1206933283928,-10.8842905570082));
#304167=CARTESIAN_POINT('Ctrl Pts',(-3.8612167765651,-4.65730412455171,
-10.8491335297397));
#304168=CARTESIAN_POINT('Ctrl Pts',(-2.5380046111267,-5.49406311947361,
-10.7775412150547));
#304169=CARTESIAN_POINT('Ctrl Pts',(-1.79209090127394,-5.78053228501042,
-10.7398847805265));
#304170=CARTESIAN_POINT('Ctrl Pts',(-0.246868659707394,-6.04498528485984,
-10.6666741422391));
#304171=CARTESIAN_POINT('Ctrl Pts',(0.536570867436116,-6.02618227783149,
-10.632548976392));
#304172=CARTESIAN_POINT('Ctrl Pts',(2.05589147767883,-5.69043622770825,
-10.559461187726));
#304173=CARTESIAN_POINT('Ctrl Pts',(2.77711115164746,-5.37545375198148,
-10.5224972736616));
#304174=CARTESIAN_POINT('Ctrl Pts',(4.06933731651797,-4.47981446503917,
-10.4514370291489));
#304175=CARTESIAN_POINT('Ctrl Pts',(4.6249530196992,-3.90361749743191,-10.4144965398214));
#304176=CARTESIAN_POINT('Ctrl Pts',(5.46963106611957,-2.58481422655512,
-10.3407144265787));
#304177=CARTESIAN_POINT('Ctrl Pts',(5.75692585399269,-1.85901826685715,
-10.3064820132932));
#304178=CARTESIAN_POINT('Ctrl Pts',(6.04252155509357,-0.325748505886516,
-10.234122937834));
#304179=CARTESIAN_POINT('Ctrl Pts',(6.0331706455049,0.468019907972567,-10.1966628965434));
#304180=CARTESIAN_POINT('Ctrl Pts',(5.70982978291748,2.00219512628821,-10.1242610901454));
#304181=CARTESIAN_POINT('Ctrl Pts',(5.40073061139426,2.72819414196556,-10.0894001367273));
#304182=CARTESIAN_POINT('Ctrl Pts',(4.52510304641024,4.01553378463539,-10.0159607808973));
#304183=CARTESIAN_POINT('Ctrl Pts',(3.96894184952754,4.56601213198919,-9.98029988335034));
#304184=CARTESIAN_POINT('Ctrl Pts',(2.66316757061658,5.43476013554676,-9.90902372494367));
#304185=CARTESIAN_POINT('Ctrl Pts',(1.92223293760542,5.73881717093973,-9.87133427597963));
#304186=CARTESIAN_POINT('Ctrl Pts',(0.765970530564992,5.96333217942141,
-9.8161637062234));
#304187=CARTESIAN_POINT('Ctrl Pts',(0.382990950460819,6.00000000000001,
-9.79843973875384));
#304188=CARTESIAN_POINT('Ctrl Pts',(2.08166817117217E-16,6.00000000000001,
-9.78125));
#304189=CARTESIAN_POINT('Ctrl Pts',(-1.61953783717195E-13,6.00000000000001,
-10.));
#304190=CARTESIAN_POINT('Ctrl Pts',(0.506806976524611,6.00000000000002,
-10.0227469592026));
#304191=CARTESIAN_POINT('Ctrl Pts',(1.01260390412922,5.93579069372547,-10.0463849702122));
#304192=CARTESIAN_POINT('Ctrl Pts',(2.27288361303783,5.60917766018831,-10.1077130660897));
#304193=CARTESIAN_POINT('Ctrl Pts',(2.99348358036239,5.26001392829972,-10.1447111295798));
#304194=CARTESIAN_POINT('Ctrl Pts',(4.24641366615186,4.30994255992357,-10.2157397471939));
#304195=CARTESIAN_POINT('Ctrl Pts',(4.76982050763015,3.72241176721537,-10.2526903345165));
#304196=CARTESIAN_POINT('Ctrl Pts',(5.56109371518005,2.38268610160769,-10.325789852975));
#304197=CARTESIAN_POINT('Ctrl Pts',(5.82245658329901,1.64376593499296,-10.3599263163893));
#304198=CARTESIAN_POINT('Ctrl Pts',(6.0512218582964,0.0928902020369393,
-10.4331162644633));
#304199=CARTESIAN_POINT('Ctrl Pts',(6.01073950667083,-0.704965909147716,
-10.4707692150558));
#304200=CARTESIAN_POINT('Ctrl Pts',(5.62670873719465,-2.22250515293938,
-10.5423859255975));
#304201=CARTESIAN_POINT('Ctrl Pts',(5.29328924334698,-2.9292511354159,-10.5775064834447));
#304202=CARTESIAN_POINT('Ctrl Pts',(4.37033294396524,-4.18513628552011,
-10.6510577761562));
#304203=CARTESIAN_POINT('Ctrl Pts',(3.78641460417051,-4.7199811781779,-10.6863878479209));
#304204=CARTESIAN_POINT('Ctrl Pts',(2.44591141916343,-5.53468177772513,
-10.7584345485147));
#304205=CARTESIAN_POINT('Ctrl Pts',(1.7022457118447,-5.80667789793638,-10.7957790209596));
#304206=CARTESIAN_POINT('Ctrl Pts',(0.162872612909248,-6.04749624303929,
-10.868382460803));
#304207=CARTESIAN_POINT('Ctrl Pts',(-0.617551262279904,-6.01808563333494,
-10.9024537334159));
#304208=CARTESIAN_POINT('Ctrl Pts',(-2.1460587063946,-5.65936981510677,
-10.9762888294743));
#304209=CARTESIAN_POINT('Ctrl Pts',(-2.8773821779996,-5.32492488610066,
-11.0139900585689));
#304210=CARTESIAN_POINT('Ctrl Pts',(-4.15170856301579,-4.40092878990582,
-11.0846604461239));
#304211=CARTESIAN_POINT('Ctrl Pts',(-4.68668143124714,-3.82624308537361,
-11.1214198826724));
#304212=CARTESIAN_POINT('Ctrl Pts',(-5.50753211944379,-2.50447647075609,
-11.1946541847529));
#304213=CARTESIAN_POINT('Ctrl Pts',(-5.78554098360329,-1.76998424880603,
-11.2289697386716));
#304214=CARTESIAN_POINT('Ctrl Pts',(-6.04754045729825,-0.224586729143651,
-11.3019011552991));
#304215=CARTESIAN_POINT('Ctrl Pts',(-6.02460146093533,0.572181149457134,
-11.3395027493034));
#304216=CARTESIAN_POINT('Ctrl Pts',(-5.67509238313919,2.09566706085101,
-11.4114000988956));
#304217=CARTESIAN_POINT('Ctrl Pts',(-5.35789365274268,2.80917758532298,
-11.4461300445477));
#304218=CARTESIAN_POINT('Ctrl Pts',(-4.46238861113384,4.08736038724291,
-11.5197711795635));
#304219=CARTESIAN_POINT('Ctrl Pts',(-3.88835145901532,4.6368193454047,-11.5555998510682));
#304220=CARTESIAN_POINT('Ctrl Pts',(-2.56465550571106,5.4804292886302,-11.627313789211));
#304221=CARTESIAN_POINT('Ctrl Pts',(-1.8286808935447,5.76787930195984,-11.6645384323918));
#304222=CARTESIAN_POINT('Ctrl Pts',(-0.708218790008448,5.96866285305186,
-11.7177560974923));
#304223=CARTESIAN_POINT('Ctrl Pts',(-0.354058654631202,6.00000000000001,
-11.7341088261503));
#304224=CARTESIAN_POINT('Ctrl Pts',(-2.28983498828939E-15,6.00000000000001,
-11.75));
#304225=CARTESIAN_POINT('Origin',(0.,5.28128932132296E-15,28.75));
#304226=CARTESIAN_POINT('',(-1.90330186412546E-14,6.00000000000001,-8.03125));
#304227=CARTESIAN_POINT('',(-1.09203944922529E-13,6.00000000000001,-8.25));
#304228=CARTESIAN_POINT('',(-7.34788079488412E-16,6.00000000000001,28.75));
#304229=CARTESIAN_POINT('Ctrl Pts',(6.80011602582908E-15,6.00000000000001,
-9.78125));
#304230=CARTESIAN_POINT('Ctrl Pts',(-0.388602026377374,6.00000000000001,
-9.76380841997154));
#304231=CARTESIAN_POINT('Ctrl Pts',(-0.777166054444378,5.9622499020027,
-9.74581802315442));
#304232=CARTESIAN_POINT('Ctrl Pts',(-1.92676662500396,5.73568003297688,
-9.69091648912202));
#304233=CARTESIAN_POINT('Ctrl Pts',(-2.65652048244608,5.43630645796336,
-9.65379716608499));
#304234=CARTESIAN_POINT('Ctrl Pts',(-3.96683623993474,4.57025182575815,
-9.5823564513502));
#304235=CARTESIAN_POINT('Ctrl Pts',(-4.53303160142738,4.00932852398643,
-9.54608237298229));
#304236=CARTESIAN_POINT('Ctrl Pts',(-5.40684351104387,2.71370187661587,
-9.47237698684475));
#304237=CARTESIAN_POINT('Ctrl Pts',(-5.71125860824631,1.99491010941579,
-9.43789511054481));
#304238=CARTESIAN_POINT('Ctrl Pts',(-6.03348298153471,0.467052589512942,
-9.36579145312735));
#304239=CARTESIAN_POINT('Ctrl Pts',(-6.04260469747069,-0.328590751166323,
-9.32824292905656));
#304240=CARTESIAN_POINT('Ctrl Pts',(-5.75438844535648,-1.86936901721857,
-9.2555295072849));
#304241=CARTESIAN_POINT('Ctrl Pts',(-5.46315202926576,-2.60028471515326,
-9.22101519242572));
#304242=CARTESIAN_POINT('Ctrl Pts',(-4.61896599239245,-3.9074724955742,
-9.14769020261236));
#304243=CARTESIAN_POINT('Ctrl Pts',(-4.07495912894505,-4.471880200415,-9.11143100203713));
#304244=CARTESIAN_POINT('Ctrl Pts',(-2.78712718969374,-5.37251473323832,
-9.04049513571143));
#304245=CARTESIAN_POINT('Ctrl Pts',(-2.05158235279043,-5.69411111262987,
-9.00279181424585));
#304246=CARTESIAN_POINT('Ctrl Pts',(-0.518250505640008,-6.02750935739265,
-8.92910939967429));
#304247=CARTESIAN_POINT('Ctrl Pts',(0.263032496357224,-6.04402808210129,
-8.89508641893388));
#304248=CARTESIAN_POINT('Ctrl Pts',(1.79739454407277,-5.77776187457389,
-8.82233677486526));
#304249=CARTESIAN_POINT('Ctrl Pts',(2.53530645242296,-5.49412713587424,
-8.78508081966443));
#304250=CARTESIAN_POINT('Ctrl Pts',(3.86320679732842,-4.65767263690705,
-8.71328252652601));
#304251=CARTESIAN_POINT('Ctrl Pts',(4.4397120908807,-4.11184665082716,-8.67758508419934));
#304252=CARTESIAN_POINT('Ctrl Pts',(5.34206193972246,-2.83920041590143,
-8.60396546431831));
#304253=CARTESIAN_POINT('Ctrl Pts',(5.66330063348323,-2.1273680295604,-8.5691461518703));
#304254=CARTESIAN_POINT('Ctrl Pts',(6.02141876131934,-0.605321673871035,
-8.49731673873819));
#304255=CARTESIAN_POINT('Ctrl Pts',(6.04872666814296,0.191752635061683,
-8.45970068347199));
#304256=CARTESIAN_POINT('Ctrl Pts',(5.7950085307118,1.73855461207809,-8.38670298676888));
#304257=CARTESIAN_POINT('Ctrl Pts',(5.52116004088795,2.47416095481492,-8.35243964785031));
#304258=CARTESIAN_POINT('Ctrl Pts',(4.70772808498026,3.80037871309697,-8.27924119192351));
#304259=CARTESIAN_POINT('Ctrl Pts',(4.17564627581371,4.37831843098813,-8.24241615238277));
#304260=CARTESIAN_POINT('Ctrl Pts',(2.90649933401595,5.30896766302181,-8.17167922360083));
#304261=CARTESIAN_POINT('Ctrl Pts',(2.17768679266873,5.64719520584165,-8.13413593561579));
#304262=CARTESIAN_POINT('Ctrl Pts',(0.943246395536786,5.94432176111744,
-8.07439759373647));
#304263=CARTESIAN_POINT('Ctrl Pts',(0.471941141175927,6.00000000000001,
-8.05243207992706));
#304264=CARTESIAN_POINT('Ctrl Pts',(7.63278329429795E-15,6.00000000000001,
-8.03125));
#304265=CARTESIAN_POINT('Ctrl Pts',(-2.34257058195908E-13,6.00000000000001,
-8.25));
#304266=CARTESIAN_POINT('Ctrl Pts',(0.601647630917533,6.00000000000003,
-8.27700368137915));
#304267=CARTESIAN_POINT('Ctrl Pts',(1.20082592209495,5.9095079146255,-8.30521620791198));
#304268=CARTESIAN_POINT('Ctrl Pts',(2.52855355862817,5.49773655197143,-8.37081345366251));
#304269=CARTESIAN_POINT('Ctrl Pts',(3.22671330303811,5.11927365697742,-8.40655413950261));
#304270=CARTESIAN_POINT('Ctrl Pts',(4.4344121015205,4.11691443543296,-8.47832441230436));
#304271=CARTESIAN_POINT('Ctrl Pts',(4.93320525707645,3.50377324199252,-8.51557003339302));
#304272=CARTESIAN_POINT('Ctrl Pts',(5.66306913910022,2.12819291474537,-8.58833502833265));
#304273=CARTESIAN_POINT('Ctrl Pts',(5.8901663336146,1.3803946904201,-8.62235550546283));
#304274=CARTESIAN_POINT('Ctrl Pts',(6.04971570472001,-0.180546511890212,
-8.6960204697897));
#304275=CARTESIAN_POINT('Ctrl Pts',(5.97263858541093,-0.979461368579639,
-8.73372338539672));
#304276=CARTESIAN_POINT('Ctrl Pts',(5.51694325189492,-2.48317467545613,
-8.80468761322603));
#304277=CARTESIAN_POINT('Ctrl Pts',(5.14964343591734,-3.17555790368862,
-8.84089500505658));
#304278=CARTESIAN_POINT('Ctrl Pts',(4.16961317154647,-4.38430093711925,
-8.91422961085586));
#304279=CARTESIAN_POINT('Ctrl Pts',(3.56529066470427,-4.88840332562846,
-8.94876868456539));
#304280=CARTESIAN_POINT('Ctrl Pts',(2.19036461375986,-5.6411978714834,-9.02145758607322));
#304281=CARTESIAN_POINT('Ctrl Pts',(1.43143927045969,-5.87977906581147,
-9.05899965400121));
#304282=CARTESIAN_POINT('Ctrl Pts',(-0.12072927485402,-6.04843331813573,
-9.13112499737227));
#304283=CARTESIAN_POINT('Ctrl Pts',(-0.898524678529774,-5.98253848692881,
-9.16558302680733));
#304284=CARTESIAN_POINT('Ctrl Pts',(-2.40183152527019,-5.55470177551167,
-9.23929506037957));
#304285=CARTESIAN_POINT('Ctrl Pts',(-3.11118581935181,-5.19075376816449,
-9.27562041898045));
#304286=CARTESIAN_POINT('Ctrl Pts',(-4.34161915907198,-4.21433886457743,
-9.34703078329607));
#304287=CARTESIAN_POINT('Ctrl Pts',(-4.85285758834909,-3.61386310603759,
-9.38413806365142));
#304288=CARTESIAN_POINT('Ctrl Pts',(-5.61351687637761,-2.25597851663534,
-9.4570816796323));
#304289=CARTESIAN_POINT('Ctrl Pts',(-5.85773998176046,-1.51257877292681,
-9.49111738726339));
#304290=CARTESIAN_POINT('Ctrl Pts',(-6.05201376863221,0.0435386693816897,
-9.56455470553419));
#304291=CARTESIAN_POINT('Ctrl Pts',(-5.99330170963915,0.842125999098481,
-9.60224216427281));
#304292=CARTESIAN_POINT('Ctrl Pts',(-5.57352042624842,2.35301795961981,
-9.67354517184851));
#304293=CARTESIAN_POINT('Ctrl Pts',(-5.22323802825824,3.05265547123128,
-9.70916118036732));
#304294=CARTESIAN_POINT('Ctrl Pts',(-4.27183094512667,4.28517180180405,
-9.78260945995225));
#304295=CARTESIAN_POINT('Ctrl Pts',(-3.67771878891341,4.80475048924421,
-9.8175026488078));
#304296=CARTESIAN_POINT('Ctrl Pts',(-2.3199614111963,5.58889423094391,-9.88987814650373));
#304297=CARTESIAN_POINT('Ctrl Pts',(-1.56855801761912,5.84444793696307,
-9.92733012342345));
#304298=CARTESIAN_POINT('Ctrl Pts',(-0.527084730838563,5.98265377315508,
-9.9760899508761));
#304299=CARTESIAN_POINT('Ctrl Pts',(-0.263417336813236,6.,-9.98817706998664));
#304300=CARTESIAN_POINT('Ctrl Pts',(-1.62023172656234E-13,6.00000000000001,
-10.));
#304301=CARTESIAN_POINT('Origin',(0.,5.28128932132296E-15,28.75));
#304302=CARTESIAN_POINT('',(7.34788079488411E-16,6.,28.75));
#304303=CARTESIAN_POINT('Origin',(0.,5.28128932132296E-15,28.75));
#304304=CARTESIAN_POINT('',(-7.34788079488411E-16,6.,-6.25));
#304305=CARTESIAN_POINT('',(-7.34788079488412E-16,6.00000000000001,28.75));
#304306=CARTESIAN_POINT('',(-0.683563368987403,5.96093458449081,-6.25));
#304307=CARTESIAN_POINT('Origin',(0.,0.,-6.25));
#304308=CARTESIAN_POINT('',(-1.00356855195047E-13,6.00000000000001,-6.28124999999999));
#304309=CARTESIAN_POINT('Ctrl Pts',(-2.33216224110322E-13,6.00000000000001,
-6.28124999999999));
#304310=CARTESIAN_POINT('Ctrl Pts',(-0.227963499279154,6.,-6.27101834049654));
#304311=CARTESIAN_POINT('Ctrl Pts',(-0.456179827689892,5.98700953252767,
-6.26058588897497));
#304312=CARTESIAN_POINT('Ctrl Pts',(-0.683563368987794,5.96093458449077,
-6.24999999999997));
#304313=CARTESIAN_POINT('',(-3.94387125597461E-14,6.00000000000001,-6.50000000000001));
#304314=CARTESIAN_POINT('',(-7.34788079488412E-16,6.00000000000001,28.75));
#304315=CARTESIAN_POINT('Ctrl Pts',(-4.69368212308332,3.7375591135724,-6.24999999999999));
#304316=CARTESIAN_POINT('Ctrl Pts',(-4.40357806234582,4.10187609220501,
-6.27195673881733));
#304317=CARTESIAN_POINT('Ctrl Pts',(-4.07203711875145,4.43118894332342,
-6.29372645570828));
#304318=CARTESIAN_POINT('Ctrl Pts',(-3.34186406804379,5.0045981835736,-6.33587340548671));
#304319=CARTESIAN_POINT('Ctrl Pts',(-2.94615269925129,5.24731162971662,
-6.35679146205122));
#304320=CARTESIAN_POINT('Ctrl Pts',(-1.80697107584555,5.77616674464259,
-6.41563369018026));
#304321=CARTESIAN_POINT('Ctrl Pts',(-1.02830160855357,5.96422013354298,
-6.45332506752402));
#304322=CARTESIAN_POINT('Ctrl Pts',(-0.157047722683405,5.9984596369681,
-6.49292878150876));
#304323=CARTESIAN_POINT('Ctrl Pts',(-0.078495223191784,6.,-6.49647690793095));
#304324=CARTESIAN_POINT('Ctrl Pts',(-7.81426370400037E-14,6.00000000000001,
-6.50000000000001));
#304325=CARTESIAN_POINT('Origin',(0.,0.,-6.25));
#304326=CARTESIAN_POINT('Origin',(-3.81730450148946E-15,-2.22044604925031E-15,
-37.015625));
#304327=CARTESIAN_POINT('',(-4.41289208089522E-15,-4.86334165753294,-8.25));
#304328=CARTESIAN_POINT('',(-8.23019658238468E-15,-4.86334165753294,-37.015625));
#304329=CARTESIAN_POINT('Ctrl Pts',(-5.9558757940577E-16,-4.86334165753294,
-8.25));
#304330=CARTESIAN_POINT('Ctrl Pts',(0.887704914026675,-4.86334165753294,
-8.20084520853896));
#304331=CARTESIAN_POINT('Ctrl Pts',(1.71816547201427,-4.54972521023778,
-8.14921769586694));
#304332=CARTESIAN_POINT('Origin',(-3.81730450148946E-15,-2.22044604925031E-15,
-37.015625));
#304333=CARTESIAN_POINT('',(-4.41289208089522E-15,-4.86334165753294,-10.));
#304334=CARTESIAN_POINT('',(-4.41289208089522E-15,-4.86334165753294,-9.78125));
#304335=CARTESIAN_POINT('',(-8.23019658238468E-15,-4.86334165753294,-37.015625));
#304336=CARTESIAN_POINT('Ctrl Pts',(-5.9558757940577E-16,-4.86334165753294,
-10.));
#304337=CARTESIAN_POINT('Ctrl Pts',(1.58019549404244,-4.86334165753293,
-9.9125));
#304338=CARTESIAN_POINT('Ctrl Pts',(2.85860050315749,-3.93452605039577,
-9.825));
#304339=CARTESIAN_POINT('Ctrl Pts',(4.13700551227254,-3.0057104432586,-9.7375));
#304340=CARTESIAN_POINT('Ctrl Pts',(4.62531277436637,-1.5028552216293,-9.65));
#304341=CARTESIAN_POINT('Ctrl Pts',(5.1136200364602,2.01466554122251E-15,
-9.56249999999999));
#304342=CARTESIAN_POINT('Ctrl Pts',(4.62531277436638,1.5028552216293,-9.475));
#304343=CARTESIAN_POINT('Ctrl Pts',(4.13700551227254,3.00571044325861,-9.38749999999999));
#304344=CARTESIAN_POINT('Ctrl Pts',(2.8586005031575,3.93452605039578,-9.3));
#304345=CARTESIAN_POINT('Ctrl Pts',(1.58019549404244,4.86334165753294,-9.21249999999999));
#304346=CARTESIAN_POINT('Ctrl Pts',(0.,4.86334165753294,-9.125));
#304347=CARTESIAN_POINT('Ctrl Pts',(-1.58019549404244,4.86334165753294,
-9.03749999999999));
#304348=CARTESIAN_POINT('Ctrl Pts',(-2.8586005031575,3.93452605039578,-8.95));
#304349=CARTESIAN_POINT('Ctrl Pts',(-4.13700551227254,3.00571044325861,
-8.8625));
#304350=CARTESIAN_POINT('Ctrl Pts',(-4.62531277436637,1.5028552216293,-8.775));
#304351=CARTESIAN_POINT('Ctrl Pts',(-5.1136200364602,3.29446615486983E-15,
-8.6875));
#304352=CARTESIAN_POINT('Ctrl Pts',(-4.62531277436638,-1.5028552216293,
-8.6));
#304353=CARTESIAN_POINT('Ctrl Pts',(-4.13700551227254,-3.0057104432586,
-8.51249999999999));
#304354=CARTESIAN_POINT('Ctrl Pts',(-2.8586005031575,-3.93452605039577,
-8.425));
#304355=CARTESIAN_POINT('Ctrl Pts',(-1.58019549404244,-4.86334165753293,
-8.33749999999999));
#304356=CARTESIAN_POINT('Ctrl Pts',(-5.9558757940577E-16,-4.86334165753294,
-8.25));
#304357=CARTESIAN_POINT('Ctrl Pts',(-5.9558757940577E-16,-4.86334165753294,
-9.78125));
#304358=CARTESIAN_POINT('Ctrl Pts',(1.58019549404244,-4.86334165753293,
-9.69375));
#304359=CARTESIAN_POINT('Ctrl Pts',(2.85860050315749,-3.93452605039577,
-9.60625));
#304360=CARTESIAN_POINT('Ctrl Pts',(4.13700551227254,-3.0057104432586,-9.51875));
#304361=CARTESIAN_POINT('Ctrl Pts',(4.62531277436637,-1.5028552216293,-9.43125));
#304362=CARTESIAN_POINT('Ctrl Pts',(5.1136200364602,2.021496774149E-15,
-9.34375000000001));
#304363=CARTESIAN_POINT('Ctrl Pts',(4.62531277436638,1.5028552216293,-9.25625));
#304364=CARTESIAN_POINT('Ctrl Pts',(4.13700551227254,3.00571044325861,-9.16875000000001));
#304365=CARTESIAN_POINT('Ctrl Pts',(2.8586005031575,3.93452605039578,-9.08125));
#304366=CARTESIAN_POINT('Ctrl Pts',(1.58019549404244,4.86334165753294,-8.99375000000001));
#304367=CARTESIAN_POINT('Ctrl Pts',(0.,4.86334165753294,-8.90625));
#304368=CARTESIAN_POINT('Ctrl Pts',(-1.58019549404244,4.86334165753294,
-8.81875));
#304369=CARTESIAN_POINT('Ctrl Pts',(-2.8586005031575,3.93452605039578,-8.73125));
#304370=CARTESIAN_POINT('Ctrl Pts',(-4.13700551227254,3.00571044325861,
-8.64375));
#304371=CARTESIAN_POINT('Ctrl Pts',(-4.62531277436637,1.5028552216293,-8.55625));
#304372=CARTESIAN_POINT('Ctrl Pts',(-5.1136200364602,3.30129738779633E-15,
-8.46875000000001));
#304373=CARTESIAN_POINT('Ctrl Pts',(-4.62531277436638,-1.5028552216293,
-8.38125));
#304374=CARTESIAN_POINT('Ctrl Pts',(-4.13700551227254,-3.0057104432586,
-8.29375000000001));
#304375=CARTESIAN_POINT('Ctrl Pts',(-2.8586005031575,-3.93452605039577,
-8.20625));
#304376=CARTESIAN_POINT('Ctrl Pts',(-2.45120890801561,-4.23051336981829,
-8.1783662195699));
#304377=CARTESIAN_POINT('Ctrl Pts',(-1.99181552565186,-4.4367514004807,
-8.14921769587173));
#304378=CARTESIAN_POINT('Origin',(-3.81730450148946E-15,-2.22044604925031E-15,
-37.015625));
#304379=CARTESIAN_POINT('',(-4.41289208089522E-15,-4.86334165753294,-11.75));
#304380=CARTESIAN_POINT('',(-4.41289208089522E-15,-4.86334165753294,-11.53125));
#304381=CARTESIAN_POINT('',(-8.23019658238468E-15,-4.86334165753294,-37.015625));
#304382=CARTESIAN_POINT('Ctrl Pts',(-5.9558757940577E-16,-4.86334165753294,
-11.75));
#304383=CARTESIAN_POINT('Ctrl Pts',(1.58019549404244,-4.86334165753293,
-11.6625));
#304384=CARTESIAN_POINT('Ctrl Pts',(2.85860050315749,-3.93452605039577,
-11.575));
#304385=CARTESIAN_POINT('Ctrl Pts',(4.13700551227254,-3.0057104432586,-11.4875));
#304386=CARTESIAN_POINT('Ctrl Pts',(4.62531277436637,-1.5028552216293,-11.4));
#304387=CARTESIAN_POINT('Ctrl Pts',(5.1136200364602,1.96001567781056E-15,
-11.3125));
#304388=CARTESIAN_POINT('Ctrl Pts',(4.62531277436638,1.5028552216293,-11.225));
#304389=CARTESIAN_POINT('Ctrl Pts',(4.13700551227254,3.00571044325861,-11.1375));
#304390=CARTESIAN_POINT('Ctrl Pts',(2.8586005031575,3.93452605039578,-11.05));
#304391=CARTESIAN_POINT('Ctrl Pts',(1.58019549404244,4.86334165753294,-10.9625));
#304392=CARTESIAN_POINT('Ctrl Pts',(0.,4.86334165753294,-10.875));
#304393=CARTESIAN_POINT('Ctrl Pts',(-1.58019549404244,4.86334165753294,
-10.7875));
#304394=CARTESIAN_POINT('Ctrl Pts',(-2.8586005031575,3.93452605039578,-10.7));
#304395=CARTESIAN_POINT('Ctrl Pts',(-4.13700551227254,3.00571044325861,
-10.6125));
#304396=CARTESIAN_POINT('Ctrl Pts',(-4.62531277436637,1.5028552216293,-10.525));
#304397=CARTESIAN_POINT('Ctrl Pts',(-5.1136200364602,3.23981629145788E-15,
-10.4375));
#304398=CARTESIAN_POINT('Ctrl Pts',(-4.62531277436638,-1.5028552216293,
-10.35));
#304399=CARTESIAN_POINT('Ctrl Pts',(-4.13700551227254,-3.0057104432586,
-10.2625));
#304400=CARTESIAN_POINT('Ctrl Pts',(-2.8586005031575,-3.93452605039577,
-10.175));
#304401=CARTESIAN_POINT('Ctrl Pts',(-1.58019549404244,-4.86334165753293,
-10.0875));
#304402=CARTESIAN_POINT('Ctrl Pts',(-5.9558757940577E-16,-4.86334165753294,
-10.));
#304403=CARTESIAN_POINT('Ctrl Pts',(-5.9558757940577E-16,-4.86334165753294,
-11.53125));
#304404=CARTESIAN_POINT('Ctrl Pts',(1.58019549404244,-4.86334165753293,
-11.44375));
#304405=CARTESIAN_POINT('Ctrl Pts',(2.85860050315749,-3.93452605039577,
-11.35625));
#304406=CARTESIAN_POINT('Ctrl Pts',(4.13700551227254,-3.0057104432586,-11.26875));
#304407=CARTESIAN_POINT('Ctrl Pts',(4.62531277436637,-1.5028552216293,-11.18125));
#304408=CARTESIAN_POINT('Ctrl Pts',(5.1136200364602,1.96684691073705E-15,
-11.09375));
#304409=CARTESIAN_POINT('Ctrl Pts',(4.62531277436638,1.5028552216293,-11.00625));
#304410=CARTESIAN_POINT('Ctrl Pts',(4.13700551227254,3.00571044325861,-10.91875));
#304411=CARTESIAN_POINT('Ctrl Pts',(2.8586005031575,3.93452605039578,-10.83125));
#304412=CARTESIAN_POINT('Ctrl Pts',(1.58019549404244,4.86334165753294,-10.74375));
#304413=CARTESIAN_POINT('Ctrl Pts',(0.,4.86334165753294,-10.65625));
#304414=CARTESIAN_POINT('Ctrl Pts',(-1.58019549404244,4.86334165753294,
-10.56875));
#304415=CARTESIAN_POINT('Ctrl Pts',(-2.8586005031575,3.93452605039578,-10.48125));
#304416=CARTESIAN_POINT('Ctrl Pts',(-4.13700551227254,3.00571044325861,
-10.39375));
#304417=CARTESIAN_POINT('Ctrl Pts',(-4.62531277436637,1.5028552216293,-10.30625));
#304418=CARTESIAN_POINT('Ctrl Pts',(-5.1136200364602,3.24664752438437E-15,
-10.21875));
#304419=CARTESIAN_POINT('Ctrl Pts',(-4.62531277436638,-1.5028552216293,
-10.13125));
#304420=CARTESIAN_POINT('Ctrl Pts',(-4.13700551227254,-3.0057104432586,
-10.04375));
#304421=CARTESIAN_POINT('Ctrl Pts',(-2.8586005031575,-3.93452605039577,
-9.95625));
#304422=CARTESIAN_POINT('Ctrl Pts',(-1.58019549404244,-4.86334165753293,
-9.86875));
#304423=CARTESIAN_POINT('Ctrl Pts',(-5.9558757940577E-16,-4.86334165753294,
-9.78125));
#304424=CARTESIAN_POINT('Origin',(-3.81730450148946E-15,-2.22044604925031E-15,
-37.015625));
#304425=CARTESIAN_POINT('',(-4.41289208089522E-15,-4.86334165753294,-13.5));
#304426=CARTESIAN_POINT('',(-4.41289208089522E-15,-4.86334165753294,-13.28125));
#304427=CARTESIAN_POINT('',(-8.23019658238468E-15,-4.86334165753294,-37.015625));
#304428=CARTESIAN_POINT('Ctrl Pts',(-5.9558757940577E-16,-4.86334165753294,
-13.5));
#304429=CARTESIAN_POINT('Ctrl Pts',(1.58019549404244,-4.86334165753293,
-13.4125));
#304430=CARTESIAN_POINT('Ctrl Pts',(2.85860050315749,-3.93452605039577,
-13.325));
#304431=CARTESIAN_POINT('Ctrl Pts',(4.13700551227254,-3.0057104432586,-13.2375));
#304432=CARTESIAN_POINT('Ctrl Pts',(4.62531277436637,-1.5028552216293,-13.15));
#304433=CARTESIAN_POINT('Ctrl Pts',(5.1136200364602,1.90536581439861E-15,
-13.0625));
#304434=CARTESIAN_POINT('Ctrl Pts',(4.62531277436638,1.5028552216293,-12.975));
#304435=CARTESIAN_POINT('Ctrl Pts',(4.13700551227254,3.00571044325861,-12.8875));
#304436=CARTESIAN_POINT('Ctrl Pts',(2.8586005031575,3.93452605039578,-12.8));
#304437=CARTESIAN_POINT('Ctrl Pts',(1.58019549404244,4.86334165753294,-12.7125));
#304438=CARTESIAN_POINT('Ctrl Pts',(0.,4.86334165753294,-12.625));
#304439=CARTESIAN_POINT('Ctrl Pts',(-1.58019549404244,4.86334165753294,
-12.5375));
#304440=CARTESIAN_POINT('Ctrl Pts',(-2.8586005031575,3.93452605039578,-12.45));
#304441=CARTESIAN_POINT('Ctrl Pts',(-4.13700551227254,3.00571044325861,
-12.3625));
#304442=CARTESIAN_POINT('Ctrl Pts',(-4.62531277436637,1.5028552216293,-12.275));
#304443=CARTESIAN_POINT('Ctrl Pts',(-5.1136200364602,3.18516642804593E-15,
-12.1875));
#304444=CARTESIAN_POINT('Ctrl Pts',(-4.62531277436638,-1.5028552216293,
-12.1));
#304445=CARTESIAN_POINT('Ctrl Pts',(-4.13700551227254,-3.0057104432586,
-12.0125));
#304446=CARTESIAN_POINT('Ctrl Pts',(-2.8586005031575,-3.93452605039577,
-11.925));
#304447=CARTESIAN_POINT('Ctrl Pts',(-1.58019549404244,-4.86334165753293,
-11.8375));
#304448=CARTESIAN_POINT('Ctrl Pts',(-5.9558757940577E-16,-4.86334165753294,
-11.75));
#304449=CARTESIAN_POINT('Ctrl Pts',(-5.9558757940577E-16,-4.86334165753294,
-13.28125));
#304450=CARTESIAN_POINT('Ctrl Pts',(1.58019549404244,-4.86334165753293,
-13.19375));
#304451=CARTESIAN_POINT('Ctrl Pts',(2.85860050315749,-3.93452605039577,
-13.10625));
#304452=CARTESIAN_POINT('Ctrl Pts',(4.13700551227254,-3.0057104432586,-13.01875));
#304453=CARTESIAN_POINT('Ctrl Pts',(4.62531277436637,-1.5028552216293,-12.93125));
#304454=CARTESIAN_POINT('Ctrl Pts',(5.1136200364602,1.9121970473251E-15,
-12.84375));
#304455=CARTESIAN_POINT('Ctrl Pts',(4.62531277436638,1.5028552216293,-12.75625));
#304456=CARTESIAN_POINT('Ctrl Pts',(4.13700551227254,3.00571044325861,-12.66875));
#304457=CARTESIAN_POINT('Ctrl Pts',(2.8586005031575,3.93452605039578,-12.58125));
#304458=CARTESIAN_POINT('Ctrl Pts',(1.58019549404244,4.86334165753294,-12.49375));
#304459=CARTESIAN_POINT('Ctrl Pts',(0.,4.86334165753294,-12.40625));
#304460=CARTESIAN_POINT('Ctrl Pts',(-1.58019549404244,4.86334165753294,
-12.31875));
#304461=CARTESIAN_POINT('Ctrl Pts',(-2.8586005031575,3.93452605039578,-12.23125));
#304462=CARTESIAN_POINT('Ctrl Pts',(-4.13700551227254,3.00571044325861,
-12.14375));
#304463=CARTESIAN_POINT('Ctrl Pts',(-4.62531277436637,1.5028552216293,-12.05625));
#304464=CARTESIAN_POINT('Ctrl Pts',(-5.1136200364602,3.19199766097243E-15,
-11.96875));
#304465=CARTESIAN_POINT('Ctrl Pts',(-4.62531277436638,-1.5028552216293,
-11.88125));
#304466=CARTESIAN_POINT('Ctrl Pts',(-4.13700551227254,-3.0057104432586,
-11.79375));
#304467=CARTESIAN_POINT('Ctrl Pts',(-2.8586005031575,-3.93452605039577,
-11.70625));
#304468=CARTESIAN_POINT('Ctrl Pts',(-1.58019549404244,-4.86334165753293,
-11.61875));
#304469=CARTESIAN_POINT('Ctrl Pts',(-5.9558757940577E-16,-4.86334165753294,
-11.53125));
#304470=CARTESIAN_POINT('Origin',(-3.81730450148946E-15,-2.22044604925031E-15,
-37.015625));
#304471=CARTESIAN_POINT('',(-4.41289208089522E-15,-4.86334165753294,-15.25));
#304472=CARTESIAN_POINT('',(-4.41289208089522E-15,-4.86334165753294,-15.03125));
#304473=CARTESIAN_POINT('',(-8.23019658238468E-15,-4.86334165753294,-37.015625));
#304474=CARTESIAN_POINT('Ctrl Pts',(-5.9558757940577E-16,-4.86334165753294,
-15.25));
#304475=CARTESIAN_POINT('Ctrl Pts',(1.58019549404244,-4.86334165753293,
-15.1625));
#304476=CARTESIAN_POINT('Ctrl Pts',(2.85860050315749,-3.93452605039577,
-15.075));
#304477=CARTESIAN_POINT('Ctrl Pts',(4.13700551227254,-3.0057104432586,-14.9875));
#304478=CARTESIAN_POINT('Ctrl Pts',(4.62531277436637,-1.5028552216293,-14.9));
#304479=CARTESIAN_POINT('Ctrl Pts',(5.1136200364602,1.85071595098665E-15,
-14.8125));
#304480=CARTESIAN_POINT('Ctrl Pts',(4.62531277436638,1.5028552216293,-14.725));
#304481=CARTESIAN_POINT('Ctrl Pts',(4.13700551227254,3.00571044325861,-14.6375));
#304482=CARTESIAN_POINT('Ctrl Pts',(2.8586005031575,3.93452605039578,-14.55));
#304483=CARTESIAN_POINT('Ctrl Pts',(1.58019549404244,4.86334165753294,-14.4625));
#304484=CARTESIAN_POINT('Ctrl Pts',(0.,4.86334165753294,-14.375));
#304485=CARTESIAN_POINT('Ctrl Pts',(-1.58019549404244,4.86334165753294,
-14.2875));
#304486=CARTESIAN_POINT('Ctrl Pts',(-2.8586005031575,3.93452605039578,-14.2));
#304487=CARTESIAN_POINT('Ctrl Pts',(-4.13700551227254,3.00571044325861,
-14.1125));
#304488=CARTESIAN_POINT('Ctrl Pts',(-4.62531277436637,1.5028552216293,-14.025));
#304489=CARTESIAN_POINT('Ctrl Pts',(-5.1136200364602,3.13051656463398E-15,
-13.9375));
#304490=CARTESIAN_POINT('Ctrl Pts',(-4.62531277436638,-1.5028552216293,
-13.85));
#304491=CARTESIAN_POINT('Ctrl Pts',(-4.13700551227254,-3.0057104432586,
-13.7625));
#304492=CARTESIAN_POINT('Ctrl Pts',(-2.8586005031575,-3.93452605039577,
-13.675));
#304493=CARTESIAN_POINT('Ctrl Pts',(-1.58019549404244,-4.86334165753293,
-13.5875));
#304494=CARTESIAN_POINT('Ctrl Pts',(-5.9558757940577E-16,-4.86334165753294,
-13.5));
#304495=CARTESIAN_POINT('Ctrl Pts',(-5.9558757940577E-16,-4.86334165753294,
-15.03125));
#304496=CARTESIAN_POINT('Ctrl Pts',(1.58019549404244,-4.86334165753293,
-14.94375));
#304497=CARTESIAN_POINT('Ctrl Pts',(2.85860050315749,-3.93452605039577,
-14.85625));
#304498=CARTESIAN_POINT('Ctrl Pts',(4.13700551227254,-3.0057104432586,-14.76875));
#304499=CARTESIAN_POINT('Ctrl Pts',(4.62531277436637,-1.5028552216293,-14.68125));
#304500=CARTESIAN_POINT('Ctrl Pts',(5.1136200364602,1.85754718391315E-15,
-14.59375));
#304501=CARTESIAN_POINT('Ctrl Pts',(4.62531277436638,1.5028552216293,-14.50625));
#304502=CARTESIAN_POINT('Ctrl Pts',(4.13700551227254,3.00571044325861,-14.41875));
#304503=CARTESIAN_POINT('Ctrl Pts',(2.8586005031575,3.93452605039578,-14.33125));
#304504=CARTESIAN_POINT('Ctrl Pts',(1.58019549404244,4.86334165753294,-14.24375));
#304505=CARTESIAN_POINT('Ctrl Pts',(0.,4.86334165753294,-14.15625));
#304506=CARTESIAN_POINT('Ctrl Pts',(-1.58019549404244,4.86334165753294,
-14.06875));
#304507=CARTESIAN_POINT('Ctrl Pts',(-2.8586005031575,3.93452605039578,-13.98125));
#304508=CARTESIAN_POINT('Ctrl Pts',(-4.13700551227254,3.00571044325861,
-13.89375));
#304509=CARTESIAN_POINT('Ctrl Pts',(-4.62531277436637,1.5028552216293,-13.80625));
#304510=CARTESIAN_POINT('Ctrl Pts',(-5.1136200364602,3.13734779756048E-15,
-13.71875));
#304511=CARTESIAN_POINT('Ctrl Pts',(-4.62531277436638,-1.5028552216293,
-13.63125));
#304512=CARTESIAN_POINT('Ctrl Pts',(-4.13700551227254,-3.0057104432586,
-13.54375));
#304513=CARTESIAN_POINT('Ctrl Pts',(-2.8586005031575,-3.93452605039577,
-13.45625));
#304514=CARTESIAN_POINT('Ctrl Pts',(-1.58019549404244,-4.86334165753293,
-13.36875));
#304515=CARTESIAN_POINT('Ctrl Pts',(-5.9558757940577E-16,-4.86334165753294,
-13.28125));
#304516=CARTESIAN_POINT('Origin',(-3.81730450148946E-15,-2.22044604925031E-15,
-37.015625));
#304517=CARTESIAN_POINT('',(-4.41289208089522E-15,-4.86334165753294,-17.));
#304518=CARTESIAN_POINT('',(-4.41289208089522E-15,-4.86334165753294,-16.78125));
#304519=CARTESIAN_POINT('',(-8.23019658238468E-15,-4.86334165753294,-37.015625));
#304520=CARTESIAN_POINT('Ctrl Pts',(-5.9558757940577E-16,-4.86334165753294,
-17.));
#304521=CARTESIAN_POINT('Ctrl Pts',(1.58019549404244,-4.86334165753293,
-16.9125));
#304522=CARTESIAN_POINT('Ctrl Pts',(2.85860050315749,-3.93452605039577,
-16.825));
#304523=CARTESIAN_POINT('Ctrl Pts',(4.13700551227254,-3.0057104432586,-16.7375));
#304524=CARTESIAN_POINT('Ctrl Pts',(4.62531277436637,-1.5028552216293,-16.65));
#304525=CARTESIAN_POINT('Ctrl Pts',(5.1136200364602,1.7960660875747E-15,
-16.5625));
#304526=CARTESIAN_POINT('Ctrl Pts',(4.62531277436638,1.5028552216293,-16.475));
#304527=CARTESIAN_POINT('Ctrl Pts',(4.13700551227254,3.00571044325861,-16.3875));
#304528=CARTESIAN_POINT('Ctrl Pts',(2.8586005031575,3.93452605039578,-16.3));
#304529=CARTESIAN_POINT('Ctrl Pts',(1.58019549404244,4.86334165753294,-16.2125));
#304530=CARTESIAN_POINT('Ctrl Pts',(0.,4.86334165753294,-16.125));
#304531=CARTESIAN_POINT('Ctrl Pts',(-1.58019549404244,4.86334165753294,
-16.0375));
#304532=CARTESIAN_POINT('Ctrl Pts',(-2.8586005031575,3.93452605039578,-15.95));
#304533=CARTESIAN_POINT('Ctrl Pts',(-4.13700551227254,3.00571044325861,
-15.8625));
#304534=CARTESIAN_POINT('Ctrl Pts',(-4.62531277436637,1.5028552216293,-15.775));
#304535=CARTESIAN_POINT('Ctrl Pts',(-5.1136200364602,3.07586670122203E-15,
-15.6875));
#304536=CARTESIAN_POINT('Ctrl Pts',(-4.62531277436638,-1.5028552216293,
-15.6));
#304537=CARTESIAN_POINT('Ctrl Pts',(-4.13700551227254,-3.0057104432586,
-15.5125));
#304538=CARTESIAN_POINT('Ctrl Pts',(-2.8586005031575,-3.93452605039577,
-15.425));
#304539=CARTESIAN_POINT('Ctrl Pts',(-1.58019549404244,-4.86334165753293,
-15.3375));
#304540=CARTESIAN_POINT('Ctrl Pts',(-5.9558757940577E-16,-4.86334165753294,
-15.25));
#304541=CARTESIAN_POINT('Ctrl Pts',(-5.9558757940577E-16,-4.86334165753294,
-16.78125));
#304542=CARTESIAN_POINT('Ctrl Pts',(1.58019549404244,-4.86334165753293,
-16.69375));
#304543=CARTESIAN_POINT('Ctrl Pts',(2.85860050315749,-3.93452605039577,
-16.60625));
#304544=CARTESIAN_POINT('Ctrl Pts',(4.13700551227254,-3.0057104432586,-16.51875));
#304545=CARTESIAN_POINT('Ctrl Pts',(4.62531277436637,-1.5028552216293,-16.43125));
#304546=CARTESIAN_POINT('Ctrl Pts',(5.1136200364602,1.8028973205012E-15,
-16.34375));
#304547=CARTESIAN_POINT('Ctrl Pts',(4.62531277436638,1.5028552216293,-16.25625));
#304548=CARTESIAN_POINT('Ctrl Pts',(4.13700551227254,3.00571044325861,-16.16875));
#304549=CARTESIAN_POINT('Ctrl Pts',(2.8586005031575,3.93452605039578,-16.08125));
#304550=CARTESIAN_POINT('Ctrl Pts',(1.58019549404244,4.86334165753294,-15.99375));
#304551=CARTESIAN_POINT('Ctrl Pts',(0.,4.86334165753294,-15.90625));
#304552=CARTESIAN_POINT('Ctrl Pts',(-1.58019549404244,4.86334165753294,
-15.81875));
#304553=CARTESIAN_POINT('Ctrl Pts',(-2.8586005031575,3.93452605039578,-15.73125));
#304554=CARTESIAN_POINT('Ctrl Pts',(-4.13700551227254,3.00571044325861,
-15.64375));
#304555=CARTESIAN_POINT('Ctrl Pts',(-4.62531277436637,1.5028552216293,-15.55625));
#304556=CARTESIAN_POINT('Ctrl Pts',(-5.1136200364602,3.08269793414853E-15,
-15.46875));
#304557=CARTESIAN_POINT('Ctrl Pts',(-4.62531277436638,-1.5028552216293,
-15.38125));
#304558=CARTESIAN_POINT('Ctrl Pts',(-4.13700551227254,-3.0057104432586,
-15.29375));
#304559=CARTESIAN_POINT('Ctrl Pts',(-2.8586005031575,-3.93452605039577,
-15.20625));
#304560=CARTESIAN_POINT('Ctrl Pts',(-1.58019549404244,-4.86334165753293,
-15.11875));
#304561=CARTESIAN_POINT('Ctrl Pts',(-5.9558757940577E-16,-4.86334165753294,
-15.03125));
#304562=CARTESIAN_POINT('Origin',(-3.81730450148946E-15,-2.22044604925031E-15,
-37.015625));
#304563=CARTESIAN_POINT('',(-4.41289208089522E-15,-4.86334165753294,-18.75));
#304564=CARTESIAN_POINT('',(-4.41289208089522E-15,-4.86334165753294,-18.53125));
#304565=CARTESIAN_POINT('',(-8.23019658238468E-15,-4.86334165753294,-37.015625));
#304566=CARTESIAN_POINT('Ctrl Pts',(-5.9558757940577E-16,-4.86334165753294,
-18.75));
#304567=CARTESIAN_POINT('Ctrl Pts',(1.58019549404244,-4.86334165753293,
-18.6625));
#304568=CARTESIAN_POINT('Ctrl Pts',(2.85860050315749,-3.93452605039577,
-18.575));
#304569=CARTESIAN_POINT('Ctrl Pts',(4.13700551227254,-3.0057104432586,-18.4875));
#304570=CARTESIAN_POINT('Ctrl Pts',(4.62531277436637,-1.5028552216293,-18.4));
#304571=CARTESIAN_POINT('Ctrl Pts',(5.1136200364602,1.74141622416275E-15,
-18.3125));
#304572=CARTESIAN_POINT('Ctrl Pts',(4.62531277436638,1.5028552216293,-18.225));
#304573=CARTESIAN_POINT('Ctrl Pts',(4.13700551227254,3.00571044325861,-18.1375));
#304574=CARTESIAN_POINT('Ctrl Pts',(2.8586005031575,3.93452605039578,-18.05));
#304575=CARTESIAN_POINT('Ctrl Pts',(1.58019549404244,4.86334165753294,-17.9625));
#304576=CARTESIAN_POINT('Ctrl Pts',(0.,4.86334165753294,-17.875));
#304577=CARTESIAN_POINT('Ctrl Pts',(-1.58019549404244,4.86334165753294,
-17.7875));
#304578=CARTESIAN_POINT('Ctrl Pts',(-2.8586005031575,3.93452605039578,-17.7));
#304579=CARTESIAN_POINT('Ctrl Pts',(-4.13700551227254,3.00571044325861,
-17.6125));
#304580=CARTESIAN_POINT('Ctrl Pts',(-4.62531277436637,1.5028552216293,-17.525));
#304581=CARTESIAN_POINT('Ctrl Pts',(-5.1136200364602,3.02121683781008E-15,
-17.4375));
#304582=CARTESIAN_POINT('Ctrl Pts',(-4.62531277436638,-1.5028552216293,
-17.35));
#304583=CARTESIAN_POINT('Ctrl Pts',(-4.13700551227254,-3.0057104432586,
-17.2625));
#304584=CARTESIAN_POINT('Ctrl Pts',(-2.8586005031575,-3.93452605039577,
-17.175));
#304585=CARTESIAN_POINT('Ctrl Pts',(-1.58019549404244,-4.86334165753293,
-17.0875));
#304586=CARTESIAN_POINT('Ctrl Pts',(-5.9558757940577E-16,-4.86334165753294,
-17.));
#304587=CARTESIAN_POINT('Ctrl Pts',(-5.9558757940577E-16,-4.86334165753294,
-18.53125));
#304588=CARTESIAN_POINT('Ctrl Pts',(1.58019549404244,-4.86334165753293,
-18.44375));
#304589=CARTESIAN_POINT('Ctrl Pts',(2.85860050315749,-3.93452605039577,
-18.35625));
#304590=CARTESIAN_POINT('Ctrl Pts',(4.13700551227254,-3.0057104432586,-18.26875));
#304591=CARTESIAN_POINT('Ctrl Pts',(4.62531277436637,-1.5028552216293,-18.18125));
#304592=CARTESIAN_POINT('Ctrl Pts',(5.1136200364602,1.74824745708925E-15,
-18.09375));
#304593=CARTESIAN_POINT('Ctrl Pts',(4.62531277436638,1.5028552216293,-18.00625));
#304594=CARTESIAN_POINT('Ctrl Pts',(4.13700551227254,3.00571044325861,-17.91875));
#304595=CARTESIAN_POINT('Ctrl Pts',(2.8586005031575,3.93452605039578,-17.83125));
#304596=CARTESIAN_POINT('Ctrl Pts',(1.58019549404244,4.86334165753294,-17.74375));
#304597=CARTESIAN_POINT('Ctrl Pts',(0.,4.86334165753294,-17.65625));
#304598=CARTESIAN_POINT('Ctrl Pts',(-1.58019549404244,4.86334165753294,
-17.56875));
#304599=CARTESIAN_POINT('Ctrl Pts',(-2.8586005031575,3.93452605039578,-17.48125));
#304600=CARTESIAN_POINT('Ctrl Pts',(-4.13700551227254,3.00571044325861,
-17.39375));
#304601=CARTESIAN_POINT('Ctrl Pts',(-4.62531277436637,1.5028552216293,-17.30625));
#304602=CARTESIAN_POINT('Ctrl Pts',(-5.1136200364602,3.02804807073658E-15,
-17.21875));
#304603=CARTESIAN_POINT('Ctrl Pts',(-4.62531277436638,-1.5028552216293,
-17.13125));
#304604=CARTESIAN_POINT('Ctrl Pts',(-4.13700551227254,-3.0057104432586,
-17.04375));
#304605=CARTESIAN_POINT('Ctrl Pts',(-2.8586005031575,-3.93452605039577,
-16.95625));
#304606=CARTESIAN_POINT('Ctrl Pts',(-1.58019549404244,-4.86334165753293,
-16.86875));
#304607=CARTESIAN_POINT('Ctrl Pts',(-5.9558757940577E-16,-4.86334165753294,
-16.78125));
#304608=CARTESIAN_POINT('Origin',(-3.81730450148946E-15,-2.22044604925031E-15,
-37.015625));
#304609=CARTESIAN_POINT('',(-4.41289208089522E-15,-4.86334165753294,-20.5));
#304610=CARTESIAN_POINT('',(-4.41289208089522E-15,-4.86334165753294,-20.28125));
#304611=CARTESIAN_POINT('',(-8.23019658238468E-15,-4.86334165753294,-37.015625));
#304612=CARTESIAN_POINT('Ctrl Pts',(-5.9558757940577E-16,-4.86334165753294,
-20.5));
#304613=CARTESIAN_POINT('Ctrl Pts',(1.58019549404244,-4.86334165753293,
-20.4125));
#304614=CARTESIAN_POINT('Ctrl Pts',(2.85860050315749,-3.93452605039577,
-20.325));
#304615=CARTESIAN_POINT('Ctrl Pts',(4.13700551227254,-3.0057104432586,-20.2375));
#304616=CARTESIAN_POINT('Ctrl Pts',(4.62531277436637,-1.5028552216293,-20.15));
#304617=CARTESIAN_POINT('Ctrl Pts',(5.1136200364602,1.6867663607508E-15,
-20.0625));
#304618=CARTESIAN_POINT('Ctrl Pts',(4.62531277436638,1.5028552216293,-19.975));
#304619=CARTESIAN_POINT('Ctrl Pts',(4.13700551227254,3.00571044325861,-19.8875));
#304620=CARTESIAN_POINT('Ctrl Pts',(2.8586005031575,3.93452605039578,-19.8));
#304621=CARTESIAN_POINT('Ctrl Pts',(1.58019549404244,4.86334165753294,-19.7125));
#304622=CARTESIAN_POINT('Ctrl Pts',(0.,4.86334165753294,-19.625));
#304623=CARTESIAN_POINT('Ctrl Pts',(-1.58019549404244,4.86334165753294,
-19.5375));
#304624=CARTESIAN_POINT('Ctrl Pts',(-2.8586005031575,3.93452605039578,-19.45));
#304625=CARTESIAN_POINT('Ctrl Pts',(-4.13700551227254,3.00571044325861,
-19.3625));
#304626=CARTESIAN_POINT('Ctrl Pts',(-4.62531277436637,1.5028552216293,-19.275));
#304627=CARTESIAN_POINT('Ctrl Pts',(-5.1136200364602,2.96656697439813E-15,
-19.1875));
#304628=CARTESIAN_POINT('Ctrl Pts',(-4.62531277436638,-1.5028552216293,
-19.1));
#304629=CARTESIAN_POINT('Ctrl Pts',(-4.13700551227254,-3.0057104432586,
-19.0125));
#304630=CARTESIAN_POINT('Ctrl Pts',(-2.8586005031575,-3.93452605039577,
-18.925));
#304631=CARTESIAN_POINT('Ctrl Pts',(-1.58019549404244,-4.86334165753293,
-18.8375));
#304632=CARTESIAN_POINT('Ctrl Pts',(-5.9558757940577E-16,-4.86334165753294,
-18.75));
#304633=CARTESIAN_POINT('Ctrl Pts',(-5.9558757940577E-16,-4.86334165753294,
-20.28125));
#304634=CARTESIAN_POINT('Ctrl Pts',(1.58019549404244,-4.86334165753293,
-20.19375));
#304635=CARTESIAN_POINT('Ctrl Pts',(2.85860050315749,-3.93452605039577,
-20.10625));
#304636=CARTESIAN_POINT('Ctrl Pts',(4.13700551227254,-3.0057104432586,-20.01875));
#304637=CARTESIAN_POINT('Ctrl Pts',(4.62531277436637,-1.5028552216293,-19.93125));
#304638=CARTESIAN_POINT('Ctrl Pts',(5.1136200364602,1.6935975936773E-15,
-19.84375));
#304639=CARTESIAN_POINT('Ctrl Pts',(4.62531277436638,1.5028552216293,-19.75625));
#304640=CARTESIAN_POINT('Ctrl Pts',(4.13700551227254,3.00571044325861,-19.66875));
#304641=CARTESIAN_POINT('Ctrl Pts',(2.8586005031575,3.93452605039578,-19.58125));
#304642=CARTESIAN_POINT('Ctrl Pts',(1.58019549404244,4.86334165753294,-19.49375));
#304643=CARTESIAN_POINT('Ctrl Pts',(0.,4.86334165753294,-19.40625));
#304644=CARTESIAN_POINT('Ctrl Pts',(-1.58019549404244,4.86334165753294,
-19.31875));
#304645=CARTESIAN_POINT('Ctrl Pts',(-2.8586005031575,3.93452605039578,-19.23125));
#304646=CARTESIAN_POINT('Ctrl Pts',(-4.13700551227254,3.00571044325861,
-19.14375));
#304647=CARTESIAN_POINT('Ctrl Pts',(-4.62531277436637,1.5028552216293,-19.05625));
#304648=CARTESIAN_POINT('Ctrl Pts',(-5.1136200364602,2.97339820732463E-15,
-18.96875));
#304649=CARTESIAN_POINT('Ctrl Pts',(-4.62531277436638,-1.5028552216293,
-18.88125));
#304650=CARTESIAN_POINT('Ctrl Pts',(-4.13700551227254,-3.0057104432586,
-18.79375));
#304651=CARTESIAN_POINT('Ctrl Pts',(-2.8586005031575,-3.93452605039577,
-18.70625));
#304652=CARTESIAN_POINT('Ctrl Pts',(-1.58019549404244,-4.86334165753293,
-18.61875));
#304653=CARTESIAN_POINT('Ctrl Pts',(-5.9558757940577E-16,-4.86334165753294,
-18.53125));
#304654=CARTESIAN_POINT('Origin',(-3.81730450148946E-15,-2.22044604925031E-15,
-37.015625));
#304655=CARTESIAN_POINT('',(-4.41289208089522E-15,-4.86334165753294,-22.25));
#304656=CARTESIAN_POINT('',(-4.41289208089522E-15,-4.86334165753294,-22.03125));
#304657=CARTESIAN_POINT('',(-8.23019658238468E-15,-4.86334165753294,-37.015625));
#304658=CARTESIAN_POINT('Ctrl Pts',(-5.9558757940577E-16,-4.86334165753294,
-22.25));
#304659=CARTESIAN_POINT('Ctrl Pts',(1.58019549404244,-4.86334165753293,
-22.1625));
#304660=CARTESIAN_POINT('Ctrl Pts',(2.85860050315749,-3.93452605039577,
-22.075));
#304661=CARTESIAN_POINT('Ctrl Pts',(4.13700551227254,-3.0057104432586,-21.9875));
#304662=CARTESIAN_POINT('Ctrl Pts',(4.62531277436637,-1.5028552216293,-21.9));
#304663=CARTESIAN_POINT('Ctrl Pts',(5.1136200364602,1.63211649733885E-15,
-21.8125));
#304664=CARTESIAN_POINT('Ctrl Pts',(4.62531277436638,1.5028552216293,-21.725));
#304665=CARTESIAN_POINT('Ctrl Pts',(4.13700551227254,3.00571044325861,-21.6375));
#304666=CARTESIAN_POINT('Ctrl Pts',(2.8586005031575,3.93452605039578,-21.55));
#304667=CARTESIAN_POINT('Ctrl Pts',(1.58019549404244,4.86334165753294,-21.4625));
#304668=CARTESIAN_POINT('Ctrl Pts',(0.,4.86334165753294,-21.375));
#304669=CARTESIAN_POINT('Ctrl Pts',(-1.58019549404244,4.86334165753294,
-21.2875));
#304670=CARTESIAN_POINT('Ctrl Pts',(-2.8586005031575,3.93452605039578,-21.2));
#304671=CARTESIAN_POINT('Ctrl Pts',(-4.13700551227254,3.00571044325861,
-21.1125));
#304672=CARTESIAN_POINT('Ctrl Pts',(-4.62531277436637,1.5028552216293,-21.025));
#304673=CARTESIAN_POINT('Ctrl Pts',(-5.1136200364602,2.91191711098618E-15,
-20.9375));
#304674=CARTESIAN_POINT('Ctrl Pts',(-4.62531277436638,-1.5028552216293,
-20.85));
#304675=CARTESIAN_POINT('Ctrl Pts',(-4.13700551227254,-3.0057104432586,
-20.7625));
#304676=CARTESIAN_POINT('Ctrl Pts',(-2.8586005031575,-3.93452605039577,
-20.675));
#304677=CARTESIAN_POINT('Ctrl Pts',(-1.58019549404244,-4.86334165753293,
-20.5875));
#304678=CARTESIAN_POINT('Ctrl Pts',(-5.9558757940577E-16,-4.86334165753294,
-20.5));
#304679=CARTESIAN_POINT('Ctrl Pts',(-5.9558757940577E-16,-4.86334165753294,
-22.03125));
#304680=CARTESIAN_POINT('Ctrl Pts',(1.58019549404244,-4.86334165753293,
-21.94375));
#304681=CARTESIAN_POINT('Ctrl Pts',(2.85860050315749,-3.93452605039577,
-21.85625));
#304682=CARTESIAN_POINT('Ctrl Pts',(4.13700551227254,-3.0057104432586,-21.76875));
#304683=CARTESIAN_POINT('Ctrl Pts',(4.62531277436637,-1.5028552216293,-21.68125));
#304684=CARTESIAN_POINT('Ctrl Pts',(5.1136200364602,1.63894773026535E-15,
-21.59375));
#304685=CARTESIAN_POINT('Ctrl Pts',(4.62531277436638,1.5028552216293,-21.50625));
#304686=CARTESIAN_POINT('Ctrl Pts',(4.13700551227254,3.00571044325861,-21.41875));
#304687=CARTESIAN_POINT('Ctrl Pts',(2.8586005031575,3.93452605039578,-21.33125));
#304688=CARTESIAN_POINT('Ctrl Pts',(1.58019549404244,4.86334165753294,-21.24375));
#304689=CARTESIAN_POINT('Ctrl Pts',(0.,4.86334165753294,-21.15625));
#304690=CARTESIAN_POINT('Ctrl Pts',(-1.58019549404244,4.86334165753294,
-21.06875));
#304691=CARTESIAN_POINT('Ctrl Pts',(-2.8586005031575,3.93452605039578,-20.98125));
#304692=CARTESIAN_POINT('Ctrl Pts',(-4.13700551227254,3.00571044325861,
-20.89375));
#304693=CARTESIAN_POINT('Ctrl Pts',(-4.62531277436637,1.5028552216293,-20.80625));
#304694=CARTESIAN_POINT('Ctrl Pts',(-5.1136200364602,2.91874834391268E-15,
-20.71875));
#304695=CARTESIAN_POINT('Ctrl Pts',(-4.62531277436638,-1.5028552216293,
-20.63125));
#304696=CARTESIAN_POINT('Ctrl Pts',(-4.13700551227254,-3.0057104432586,
-20.54375));
#304697=CARTESIAN_POINT('Ctrl Pts',(-2.8586005031575,-3.93452605039577,
-20.45625));
#304698=CARTESIAN_POINT('Ctrl Pts',(-1.58019549404244,-4.86334165753293,
-20.36875));
#304699=CARTESIAN_POINT('Ctrl Pts',(-5.9558757940577E-16,-4.86334165753294,
-20.28125));
#304700=CARTESIAN_POINT('Origin',(-3.81730450148946E-15,-2.22044604925031E-15,
-37.015625));
#304701=CARTESIAN_POINT('',(-4.41289208089522E-15,-4.86334165753294,-24.));
#304702=CARTESIAN_POINT('',(-4.41289208089522E-15,-4.86334165753294,-23.78125));
#304703=CARTESIAN_POINT('',(-8.23019658238468E-15,-4.86334165753294,-37.015625));
#304704=CARTESIAN_POINT('Ctrl Pts',(-5.9558757940577E-16,-4.86334165753294,
-24.));
#304705=CARTESIAN_POINT('Ctrl Pts',(1.58019549404244,-4.86334165753293,
-23.9125));
#304706=CARTESIAN_POINT('Ctrl Pts',(2.85860050315749,-3.93452605039577,
-23.825));
#304707=CARTESIAN_POINT('Ctrl Pts',(4.13700551227254,-3.0057104432586,-23.7375));
#304708=CARTESIAN_POINT('Ctrl Pts',(4.62531277436637,-1.5028552216293,-23.65));
#304709=CARTESIAN_POINT('Ctrl Pts',(5.1136200364602,1.5774666339269E-15,
-23.5625));
#304710=CARTESIAN_POINT('Ctrl Pts',(4.62531277436638,1.5028552216293,-23.475));
#304711=CARTESIAN_POINT('Ctrl Pts',(4.13700551227254,3.00571044325861,-23.3875));
#304712=CARTESIAN_POINT('Ctrl Pts',(2.8586005031575,3.93452605039578,-23.3));
#304713=CARTESIAN_POINT('Ctrl Pts',(1.58019549404244,4.86334165753294,-23.2125));
#304714=CARTESIAN_POINT('Ctrl Pts',(0.,4.86334165753294,-23.125));
#304715=CARTESIAN_POINT('Ctrl Pts',(-1.58019549404244,4.86334165753294,
-23.0375));
#304716=CARTESIAN_POINT('Ctrl Pts',(-2.8586005031575,3.93452605039578,-22.95));
#304717=CARTESIAN_POINT('Ctrl Pts',(-4.13700551227254,3.00571044325861,
-22.8625));
#304718=CARTESIAN_POINT('Ctrl Pts',(-4.62531277436637,1.5028552216293,-22.775));
#304719=CARTESIAN_POINT('Ctrl Pts',(-5.1136200364602,2.85726724757423E-15,
-22.6875));
#304720=CARTESIAN_POINT('Ctrl Pts',(-4.62531277436638,-1.5028552216293,
-22.6));
#304721=CARTESIAN_POINT('Ctrl Pts',(-4.13700551227254,-3.0057104432586,
-22.5125));
#304722=CARTESIAN_POINT('Ctrl Pts',(-2.8586005031575,-3.93452605039577,
-22.425));
#304723=CARTESIAN_POINT('Ctrl Pts',(-1.58019549404244,-4.86334165753293,
-22.3375));
#304724=CARTESIAN_POINT('Ctrl Pts',(-5.9558757940577E-16,-4.86334165753294,
-22.25));
#304725=CARTESIAN_POINT('Ctrl Pts',(-5.9558757940577E-16,-4.86334165753294,
-23.78125));
#304726=CARTESIAN_POINT('Ctrl Pts',(1.58019549404244,-4.86334165753293,
-23.69375));
#304727=CARTESIAN_POINT('Ctrl Pts',(2.85860050315749,-3.93452605039577,
-23.60625));
#304728=CARTESIAN_POINT('Ctrl Pts',(4.13700551227254,-3.0057104432586,-23.51875));
#304729=CARTESIAN_POINT('Ctrl Pts',(4.62531277436637,-1.5028552216293,-23.43125));
#304730=CARTESIAN_POINT('Ctrl Pts',(5.1136200364602,1.5842978668534E-15,
-23.34375));
#304731=CARTESIAN_POINT('Ctrl Pts',(4.62531277436638,1.5028552216293,-23.25625));
#304732=CARTESIAN_POINT('Ctrl Pts',(4.13700551227254,3.00571044325861,-23.16875));
#304733=CARTESIAN_POINT('Ctrl Pts',(2.8586005031575,3.93452605039578,-23.08125));
#304734=CARTESIAN_POINT('Ctrl Pts',(1.58019549404244,4.86334165753294,-22.99375));
#304735=CARTESIAN_POINT('Ctrl Pts',(0.,4.86334165753294,-22.90625));
#304736=CARTESIAN_POINT('Ctrl Pts',(-1.58019549404244,4.86334165753294,
-22.81875));
#304737=CARTESIAN_POINT('Ctrl Pts',(-2.8586005031575,3.93452605039578,-22.73125));
#304738=CARTESIAN_POINT('Ctrl Pts',(-4.13700551227254,3.00571044325861,
-22.64375));
#304739=CARTESIAN_POINT('Ctrl Pts',(-4.62531277436637,1.5028552216293,-22.55625));
#304740=CARTESIAN_POINT('Ctrl Pts',(-5.1136200364602,2.86409848050072E-15,
-22.46875));
#304741=CARTESIAN_POINT('Ctrl Pts',(-4.62531277436638,-1.5028552216293,
-22.38125));
#304742=CARTESIAN_POINT('Ctrl Pts',(-4.13700551227254,-3.0057104432586,
-22.29375));
#304743=CARTESIAN_POINT('Ctrl Pts',(-2.8586005031575,-3.93452605039577,
-22.20625));
#304744=CARTESIAN_POINT('Ctrl Pts',(-1.58019549404244,-4.86334165753293,
-22.11875));
#304745=CARTESIAN_POINT('Ctrl Pts',(-5.9558757940577E-16,-4.86334165753294,
-22.03125));
#304746=CARTESIAN_POINT('Origin',(-3.81730450148946E-15,-2.22044604925031E-15,
-37.015625));
#304747=CARTESIAN_POINT('',(-4.41289208089522E-15,-4.86334165753294,-25.75));
#304748=CARTESIAN_POINT('',(-4.41289208089522E-15,-4.86334165753294,-25.53125));
#304749=CARTESIAN_POINT('',(-8.23019658238468E-15,-4.86334165753294,-37.015625));
#304750=CARTESIAN_POINT('Ctrl Pts',(-5.9558757940577E-16,-4.86334165753294,
-25.75));
#304751=CARTESIAN_POINT('Ctrl Pts',(1.58019549404244,-4.86334165753293,
-25.6625));
#304752=CARTESIAN_POINT('Ctrl Pts',(2.85860050315749,-3.93452605039577,
-25.575));
#304753=CARTESIAN_POINT('Ctrl Pts',(4.13700551227254,-3.0057104432586,-25.4875));
#304754=CARTESIAN_POINT('Ctrl Pts',(4.62531277436637,-1.5028552216293,-25.4));
#304755=CARTESIAN_POINT('Ctrl Pts',(5.1136200364602,1.52281677051495E-15,
-25.3125));
#304756=CARTESIAN_POINT('Ctrl Pts',(4.62531277436638,1.5028552216293,-25.225));
#304757=CARTESIAN_POINT('Ctrl Pts',(4.13700551227254,3.00571044325861,-25.1375));
#304758=CARTESIAN_POINT('Ctrl Pts',(2.8586005031575,3.93452605039578,-25.05));
#304759=CARTESIAN_POINT('Ctrl Pts',(1.58019549404244,4.86334165753293,-24.9625));
#304760=CARTESIAN_POINT('Ctrl Pts',(0.,4.86334165753294,-24.875));
#304761=CARTESIAN_POINT('Ctrl Pts',(-1.58019549404244,4.86334165753293,
-24.7875));
#304762=CARTESIAN_POINT('Ctrl Pts',(-2.8586005031575,3.93452605039578,-24.7));
#304763=CARTESIAN_POINT('Ctrl Pts',(-4.13700551227254,3.00571044325861,
-24.6125));
#304764=CARTESIAN_POINT('Ctrl Pts',(-4.62531277436637,1.5028552216293,-24.525));
#304765=CARTESIAN_POINT('Ctrl Pts',(-5.1136200364602,2.80261738416228E-15,
-24.4375));
#304766=CARTESIAN_POINT('Ctrl Pts',(-4.62531277436638,-1.5028552216293,
-24.35));
#304767=CARTESIAN_POINT('Ctrl Pts',(-4.13700551227254,-3.0057104432586,
-24.2625));
#304768=CARTESIAN_POINT('Ctrl Pts',(-2.8586005031575,-3.93452605039577,
-24.175));
#304769=CARTESIAN_POINT('Ctrl Pts',(-1.58019549404244,-4.86334165753293,
-24.0875));
#304770=CARTESIAN_POINT('Ctrl Pts',(-5.9558757940577E-16,-4.86334165753294,
-24.));
#304771=CARTESIAN_POINT('Ctrl Pts',(-5.9558757940577E-16,-4.86334165753294,
-25.53125));
#304772=CARTESIAN_POINT('Ctrl Pts',(1.58019549404244,-4.86334165753293,
-25.44375));
#304773=CARTESIAN_POINT('Ctrl Pts',(2.85860050315749,-3.93452605039577,
-25.35625));
#304774=CARTESIAN_POINT('Ctrl Pts',(4.13700551227254,-3.0057104432586,-25.26875));
#304775=CARTESIAN_POINT('Ctrl Pts',(4.62531277436637,-1.5028552216293,-25.18125));
#304776=CARTESIAN_POINT('Ctrl Pts',(5.1136200364602,1.52964800344145E-15,
-25.09375));
#304777=CARTESIAN_POINT('Ctrl Pts',(4.62531277436638,1.5028552216293,-25.00625));
#304778=CARTESIAN_POINT('Ctrl Pts',(4.13700551227254,3.00571044325861,-24.91875));
#304779=CARTESIAN_POINT('Ctrl Pts',(2.8586005031575,3.93452605039578,-24.83125));
#304780=CARTESIAN_POINT('Ctrl Pts',(1.58019549404244,4.86334165753293,-24.74375));
#304781=CARTESIAN_POINT('Ctrl Pts',(0.,4.86334165753294,-24.65625));
#304782=CARTESIAN_POINT('Ctrl Pts',(-1.58019549404244,4.86334165753293,
-24.56875));
#304783=CARTESIAN_POINT('Ctrl Pts',(-2.8586005031575,3.93452605039578,-24.48125));
#304784=CARTESIAN_POINT('Ctrl Pts',(-4.13700551227254,3.00571044325861,
-24.39375));
#304785=CARTESIAN_POINT('Ctrl Pts',(-4.62531277436637,1.5028552216293,-24.30625));
#304786=CARTESIAN_POINT('Ctrl Pts',(-5.1136200364602,2.80944861708877E-15,
-24.21875));
#304787=CARTESIAN_POINT('Ctrl Pts',(-4.62531277436638,-1.5028552216293,
-24.13125));
#304788=CARTESIAN_POINT('Ctrl Pts',(-4.13700551227254,-3.0057104432586,
-24.04375));
#304789=CARTESIAN_POINT('Ctrl Pts',(-2.8586005031575,-3.93452605039577,
-23.95625));
#304790=CARTESIAN_POINT('Ctrl Pts',(-1.58019549404244,-4.86334165753293,
-23.86875));
#304791=CARTESIAN_POINT('Ctrl Pts',(-5.9558757940577E-16,-4.86334165753294,
-23.78125));
#304792=CARTESIAN_POINT('Origin',(-3.81730450148946E-15,-2.22044604925031E-15,
-37.015625));
#304793=CARTESIAN_POINT('',(-4.41289208089522E-15,-4.86334165753294,-27.5));
#304794=CARTESIAN_POINT('',(-4.41289208089522E-15,-4.86334165753294,-27.28125));
#304795=CARTESIAN_POINT('',(-8.23019658238468E-15,-4.86334165753294,-37.015625));
#304796=CARTESIAN_POINT('Ctrl Pts',(-5.9558757940577E-16,-4.86334165753294,
-27.5));
#304797=CARTESIAN_POINT('Ctrl Pts',(1.58019549404244,-4.86334165753293,
-27.4125));
#304798=CARTESIAN_POINT('Ctrl Pts',(2.85860050315749,-3.93452605039577,
-27.325));
#304799=CARTESIAN_POINT('Ctrl Pts',(4.13700551227254,-3.0057104432586,-27.2375));
#304800=CARTESIAN_POINT('Ctrl Pts',(4.62531277436637,-1.5028552216293,-27.15));
#304801=CARTESIAN_POINT('Ctrl Pts',(5.1136200364602,1.468166907103E-15,
-27.0625));
#304802=CARTESIAN_POINT('Ctrl Pts',(4.62531277436638,1.5028552216293,-26.975));
#304803=CARTESIAN_POINT('Ctrl Pts',(4.13700551227254,3.00571044325861,-26.8875));
#304804=CARTESIAN_POINT('Ctrl Pts',(2.8586005031575,3.93452605039578,-26.8));
#304805=CARTESIAN_POINT('Ctrl Pts',(1.58019549404244,4.86334165753293,-26.7125));
#304806=CARTESIAN_POINT('Ctrl Pts',(0.,4.86334165753294,-26.625));
#304807=CARTESIAN_POINT('Ctrl Pts',(-1.58019549404244,4.86334165753293,
-26.5375));
#304808=CARTESIAN_POINT('Ctrl Pts',(-2.8586005031575,3.93452605039578,-26.45));
#304809=CARTESIAN_POINT('Ctrl Pts',(-4.13700551227254,3.00571044325861,
-26.3625));
#304810=CARTESIAN_POINT('Ctrl Pts',(-4.62531277436637,1.5028552216293,-26.275));
#304811=CARTESIAN_POINT('Ctrl Pts',(-5.1136200364602,2.74796752075033E-15,
-26.1875));
#304812=CARTESIAN_POINT('Ctrl Pts',(-4.62531277436638,-1.5028552216293,
-26.1));
#304813=CARTESIAN_POINT('Ctrl Pts',(-4.13700551227254,-3.0057104432586,
-26.0125));
#304814=CARTESIAN_POINT('Ctrl Pts',(-2.8586005031575,-3.93452605039577,
-25.925));
#304815=CARTESIAN_POINT('Ctrl Pts',(-1.58019549404244,-4.86334165753293,
-25.8375));
#304816=CARTESIAN_POINT('Ctrl Pts',(-5.9558757940577E-16,-4.86334165753294,
-25.75));
#304817=CARTESIAN_POINT('Ctrl Pts',(-5.9558757940577E-16,-4.86334165753294,
-27.28125));
#304818=CARTESIAN_POINT('Ctrl Pts',(1.58019549404244,-4.86334165753293,
-27.19375));
#304819=CARTESIAN_POINT('Ctrl Pts',(2.85860050315749,-3.93452605039577,
-27.10625));
#304820=CARTESIAN_POINT('Ctrl Pts',(4.13700551227254,-3.0057104432586,-27.01875));
#304821=CARTESIAN_POINT('Ctrl Pts',(4.62531277436637,-1.5028552216293,-26.93125));
#304822=CARTESIAN_POINT('Ctrl Pts',(5.1136200364602,1.47499814002949E-15,
-26.84375));
#304823=CARTESIAN_POINT('Ctrl Pts',(4.62531277436638,1.5028552216293,-26.75625));
#304824=CARTESIAN_POINT('Ctrl Pts',(4.13700551227254,3.00571044325861,-26.66875));
#304825=CARTESIAN_POINT('Ctrl Pts',(2.8586005031575,3.93452605039578,-26.58125));
#304826=CARTESIAN_POINT('Ctrl Pts',(1.58019549404244,4.86334165753293,-26.49375));
#304827=CARTESIAN_POINT('Ctrl Pts',(0.,4.86334165753294,-26.40625));
#304828=CARTESIAN_POINT('Ctrl Pts',(-1.58019549404244,4.86334165753293,
-26.31875));
#304829=CARTESIAN_POINT('Ctrl Pts',(-2.8586005031575,3.93452605039578,-26.23125));
#304830=CARTESIAN_POINT('Ctrl Pts',(-4.13700551227254,3.00571044325861,
-26.14375));
#304831=CARTESIAN_POINT('Ctrl Pts',(-4.62531277436637,1.5028552216293,-26.05625));
#304832=CARTESIAN_POINT('Ctrl Pts',(-5.1136200364602,2.75479875367682E-15,
-25.96875));
#304833=CARTESIAN_POINT('Ctrl Pts',(-4.62531277436638,-1.5028552216293,
-25.88125));
#304834=CARTESIAN_POINT('Ctrl Pts',(-4.13700551227254,-3.0057104432586,
-25.79375));
#304835=CARTESIAN_POINT('Ctrl Pts',(-2.8586005031575,-3.93452605039577,
-25.70625));
#304836=CARTESIAN_POINT('Ctrl Pts',(-1.58019549404244,-4.86334165753293,
-25.61875));
#304837=CARTESIAN_POINT('Ctrl Pts',(-5.9558757940577E-16,-4.86334165753294,
-25.53125));
#304838=CARTESIAN_POINT('Origin',(-3.81730450148946E-15,-2.22044604925031E-15,
-37.015625));
#304839=CARTESIAN_POINT('',(-4.41289208089522E-15,-4.86334165753294,-29.25));
#304840=CARTESIAN_POINT('',(-4.41289208089522E-15,-4.86334165753294,-29.03125));
#304841=CARTESIAN_POINT('',(-8.23019658238468E-15,-4.86334165753294,-37.015625));
#304842=CARTESIAN_POINT('Ctrl Pts',(-5.9558757940577E-16,-4.86334165753294,
-29.25));
#304843=CARTESIAN_POINT('Ctrl Pts',(1.58019549404244,-4.86334165753293,
-29.1625));
#304844=CARTESIAN_POINT('Ctrl Pts',(2.85860050315749,-3.93452605039577,
-29.075));
#304845=CARTESIAN_POINT('Ctrl Pts',(4.13700551227254,-3.0057104432586,-28.9875));
#304846=CARTESIAN_POINT('Ctrl Pts',(4.62531277436637,-1.5028552216293,-28.9));
#304847=CARTESIAN_POINT('Ctrl Pts',(5.1136200364602,1.41351704369105E-15,
-28.8125));
#304848=CARTESIAN_POINT('Ctrl Pts',(4.62531277436638,1.5028552216293,-28.725));
#304849=CARTESIAN_POINT('Ctrl Pts',(4.13700551227254,3.00571044325861,-28.6375));
#304850=CARTESIAN_POINT('Ctrl Pts',(2.8586005031575,3.93452605039578,-28.55));
#304851=CARTESIAN_POINT('Ctrl Pts',(1.58019549404244,4.86334165753293,-28.4625));
#304852=CARTESIAN_POINT('Ctrl Pts',(0.,4.86334165753294,-28.375));
#304853=CARTESIAN_POINT('Ctrl Pts',(-1.58019549404244,4.86334165753293,
-28.2875));
#304854=CARTESIAN_POINT('Ctrl Pts',(-2.8586005031575,3.93452605039578,-28.2));
#304855=CARTESIAN_POINT('Ctrl Pts',(-4.13700551227254,3.00571044325861,
-28.1125));
#304856=CARTESIAN_POINT('Ctrl Pts',(-4.62531277436637,1.5028552216293,-28.025));
#304857=CARTESIAN_POINT('Ctrl Pts',(-5.1136200364602,2.69331765733838E-15,
-27.9375));
#304858=CARTESIAN_POINT('Ctrl Pts',(-4.62531277436638,-1.5028552216293,
-27.85));
#304859=CARTESIAN_POINT('Ctrl Pts',(-4.13700551227254,-3.0057104432586,
-27.7625));
#304860=CARTESIAN_POINT('Ctrl Pts',(-2.8586005031575,-3.93452605039577,
-27.675));
#304861=CARTESIAN_POINT('Ctrl Pts',(-1.58019549404244,-4.86334165753293,
-27.5875));
#304862=CARTESIAN_POINT('Ctrl Pts',(-5.9558757940577E-16,-4.86334165753294,
-27.5));
#304863=CARTESIAN_POINT('Ctrl Pts',(-5.9558757940577E-16,-4.86334165753294,
-29.03125));
#304864=CARTESIAN_POINT('Ctrl Pts',(1.58019549404244,-4.86334165753293,
-28.94375));
#304865=CARTESIAN_POINT('Ctrl Pts',(2.85860050315749,-3.93452605039577,
-28.85625));
#304866=CARTESIAN_POINT('Ctrl Pts',(4.13700551227254,-3.0057104432586,-28.76875));
#304867=CARTESIAN_POINT('Ctrl Pts',(4.62531277436637,-1.5028552216293,-28.68125));
#304868=CARTESIAN_POINT('Ctrl Pts',(5.1136200364602,1.42034827661754E-15,
-28.59375));
#304869=CARTESIAN_POINT('Ctrl Pts',(4.62531277436638,1.5028552216293,-28.50625));
#304870=CARTESIAN_POINT('Ctrl Pts',(4.13700551227254,3.00571044325861,-28.41875));
#304871=CARTESIAN_POINT('Ctrl Pts',(2.8586005031575,3.93452605039578,-28.33125));
#304872=CARTESIAN_POINT('Ctrl Pts',(1.58019549404244,4.86334165753293,-28.24375));
#304873=CARTESIAN_POINT('Ctrl Pts',(0.,4.86334165753294,-28.15625));
#304874=CARTESIAN_POINT('Ctrl Pts',(-1.58019549404244,4.86334165753293,
-28.06875));
#304875=CARTESIAN_POINT('Ctrl Pts',(-2.8586005031575,3.93452605039578,-27.98125));
#304876=CARTESIAN_POINT('Ctrl Pts',(-4.13700551227254,3.00571044325861,
-27.89375));
#304877=CARTESIAN_POINT('Ctrl Pts',(-4.62531277436637,1.5028552216293,-27.80625));
#304878=CARTESIAN_POINT('Ctrl Pts',(-5.1136200364602,2.70014889026487E-15,
-27.71875));
#304879=CARTESIAN_POINT('Ctrl Pts',(-4.62531277436638,-1.5028552216293,
-27.63125));
#304880=CARTESIAN_POINT('Ctrl Pts',(-4.13700551227254,-3.0057104432586,
-27.54375));
#304881=CARTESIAN_POINT('Ctrl Pts',(-2.8586005031575,-3.93452605039577,
-27.45625));
#304882=CARTESIAN_POINT('Ctrl Pts',(-1.58019549404244,-4.86334165753293,
-27.36875));
#304883=CARTESIAN_POINT('Ctrl Pts',(-5.9558757940577E-16,-4.86334165753294,
-27.28125));
#304884=CARTESIAN_POINT('Origin',(-3.81730450148946E-15,-2.22044604925031E-15,
-37.015625));
#304885=CARTESIAN_POINT('',(-4.41289208089522E-15,-4.86334165753294,-31.));
#304886=CARTESIAN_POINT('',(-4.41289208089522E-15,-4.86334165753294,-30.78125));
#304887=CARTESIAN_POINT('',(-8.23019658238468E-15,-4.86334165753294,-37.015625));
#304888=CARTESIAN_POINT('Ctrl Pts',(-5.9558757940577E-16,-4.86334165753294,
-31.));
#304889=CARTESIAN_POINT('Ctrl Pts',(1.58019549404244,-4.86334165753293,
-30.9125));
#304890=CARTESIAN_POINT('Ctrl Pts',(2.85860050315749,-3.93452605039577,
-30.825));
#304891=CARTESIAN_POINT('Ctrl Pts',(4.13700551227254,-3.0057104432586,-30.7375));
#304892=CARTESIAN_POINT('Ctrl Pts',(4.62531277436637,-1.5028552216293,-30.65));
#304893=CARTESIAN_POINT('Ctrl Pts',(5.1136200364602,1.3588671802791E-15,
-30.5625));
#304894=CARTESIAN_POINT('Ctrl Pts',(4.62531277436638,1.5028552216293,-30.475));
#304895=CARTESIAN_POINT('Ctrl Pts',(4.13700551227254,3.00571044325861,-30.3875));
#304896=CARTESIAN_POINT('Ctrl Pts',(2.8586005031575,3.93452605039578,-30.3));
#304897=CARTESIAN_POINT('Ctrl Pts',(1.58019549404244,4.86334165753293,-30.2125));
#304898=CARTESIAN_POINT('Ctrl Pts',(0.,4.86334165753294,-30.125));
#304899=CARTESIAN_POINT('Ctrl Pts',(-1.58019549404244,4.86334165753293,
-30.0375));
#304900=CARTESIAN_POINT('Ctrl Pts',(-2.8586005031575,3.93452605039578,-29.95));
#304901=CARTESIAN_POINT('Ctrl Pts',(-4.13700551227254,3.00571044325861,
-29.8625));
#304902=CARTESIAN_POINT('Ctrl Pts',(-4.62531277436637,1.5028552216293,-29.775));
#304903=CARTESIAN_POINT('Ctrl Pts',(-5.1136200364602,2.63866779392642E-15,
-29.6875));
#304904=CARTESIAN_POINT('Ctrl Pts',(-4.62531277436638,-1.5028552216293,
-29.6));
#304905=CARTESIAN_POINT('Ctrl Pts',(-4.13700551227254,-3.0057104432586,
-29.5125));
#304906=CARTESIAN_POINT('Ctrl Pts',(-2.8586005031575,-3.93452605039577,
-29.425));
#304907=CARTESIAN_POINT('Ctrl Pts',(-1.58019549404244,-4.86334165753293,
-29.3375));
#304908=CARTESIAN_POINT('Ctrl Pts',(-5.9558757940577E-16,-4.86334165753294,
-29.25));
#304909=CARTESIAN_POINT('Ctrl Pts',(-5.9558757940577E-16,-4.86334165753294,
-30.78125));
#304910=CARTESIAN_POINT('Ctrl Pts',(1.58019549404244,-4.86334165753293,
-30.69375));
#304911=CARTESIAN_POINT('Ctrl Pts',(2.85860050315749,-3.93452605039577,
-30.60625));
#304912=CARTESIAN_POINT('Ctrl Pts',(4.13700551227254,-3.0057104432586,-30.51875));
#304913=CARTESIAN_POINT('Ctrl Pts',(4.62531277436637,-1.5028552216293,-30.43125));
#304914=CARTESIAN_POINT('Ctrl Pts',(5.1136200364602,1.36569841320559E-15,
-30.34375));
#304915=CARTESIAN_POINT('Ctrl Pts',(4.62531277436638,1.5028552216293,-30.25625));
#304916=CARTESIAN_POINT('Ctrl Pts',(4.13700551227254,3.00571044325861,-30.16875));
#304917=CARTESIAN_POINT('Ctrl Pts',(2.8586005031575,3.93452605039578,-30.08125));
#304918=CARTESIAN_POINT('Ctrl Pts',(1.58019549404244,4.86334165753293,-29.99375));
#304919=CARTESIAN_POINT('Ctrl Pts',(0.,4.86334165753294,-29.90625));
#304920=CARTESIAN_POINT('Ctrl Pts',(-1.58019549404244,4.86334165753293,
-29.81875));
#304921=CARTESIAN_POINT('Ctrl Pts',(-2.8586005031575,3.93452605039578,-29.73125));
#304922=CARTESIAN_POINT('Ctrl Pts',(-4.13700551227254,3.00571044325861,
-29.64375));
#304923=CARTESIAN_POINT('Ctrl Pts',(-4.62531277436637,1.5028552216293,-29.55625));
#304924=CARTESIAN_POINT('Ctrl Pts',(-5.1136200364602,2.64549902685292E-15,
-29.46875));
#304925=CARTESIAN_POINT('Ctrl Pts',(-4.62531277436638,-1.5028552216293,
-29.38125));
#304926=CARTESIAN_POINT('Ctrl Pts',(-4.13700551227254,-3.0057104432586,
-29.29375));
#304927=CARTESIAN_POINT('Ctrl Pts',(-2.8586005031575,-3.93452605039577,
-29.20625));
#304928=CARTESIAN_POINT('Ctrl Pts',(-1.58019549404244,-4.86334165753293,
-29.11875));
#304929=CARTESIAN_POINT('Ctrl Pts',(-5.9558757940577E-16,-4.86334165753294,
-29.03125));
#304930=CARTESIAN_POINT('Origin',(-3.81730450148946E-15,-2.22044604925031E-15,
-37.015625));
#304931=CARTESIAN_POINT('',(-4.41289208089522E-15,-4.86334165753294,-32.75));
#304932=CARTESIAN_POINT('',(-4.41289208089522E-15,-4.86334165753294,-32.53125));
#304933=CARTESIAN_POINT('',(-8.23019658238468E-15,-4.86334165753294,-37.015625));
#304934=CARTESIAN_POINT('Ctrl Pts',(-5.9558757940577E-16,-4.86334165753294,
-32.75));
#304935=CARTESIAN_POINT('Ctrl Pts',(1.58019549404244,-4.86334165753293,
-32.6625));
#304936=CARTESIAN_POINT('Ctrl Pts',(2.85860050315749,-3.93452605039577,
-32.575));
#304937=CARTESIAN_POINT('Ctrl Pts',(4.13700551227254,-3.0057104432586,-32.4875));
#304938=CARTESIAN_POINT('Ctrl Pts',(4.62531277436637,-1.5028552216293,-32.4));
#304939=CARTESIAN_POINT('Ctrl Pts',(5.1136200364602,1.30421731686715E-15,
-32.3125));
#304940=CARTESIAN_POINT('Ctrl Pts',(4.62531277436638,1.5028552216293,-32.225));
#304941=CARTESIAN_POINT('Ctrl Pts',(4.13700551227254,3.00571044325861,-32.1375));
#304942=CARTESIAN_POINT('Ctrl Pts',(2.8586005031575,3.93452605039578,-32.05));
#304943=CARTESIAN_POINT('Ctrl Pts',(1.58019549404244,4.86334165753293,-31.9625));
#304944=CARTESIAN_POINT('Ctrl Pts',(0.,4.86334165753294,-31.875));
#304945=CARTESIAN_POINT('Ctrl Pts',(-1.58019549404244,4.86334165753293,
-31.7875));
#304946=CARTESIAN_POINT('Ctrl Pts',(-2.8586005031575,3.93452605039578,-31.7));
#304947=CARTESIAN_POINT('Ctrl Pts',(-4.13700551227254,3.00571044325861,
-31.6125));
#304948=CARTESIAN_POINT('Ctrl Pts',(-4.62531277436637,1.5028552216293,-31.525));
#304949=CARTESIAN_POINT('Ctrl Pts',(-5.1136200364602,2.58401793051447E-15,
-31.4375));
#304950=CARTESIAN_POINT('Ctrl Pts',(-4.62531277436638,-1.5028552216293,
-31.35));
#304951=CARTESIAN_POINT('Ctrl Pts',(-4.13700551227254,-3.0057104432586,
-31.2625));
#304952=CARTESIAN_POINT('Ctrl Pts',(-2.8586005031575,-3.93452605039577,
-31.175));
#304953=CARTESIAN_POINT('Ctrl Pts',(-1.58019549404244,-4.86334165753293,
-31.0875));
#304954=CARTESIAN_POINT('Ctrl Pts',(-5.9558757940577E-16,-4.86334165753294,
-31.));
#304955=CARTESIAN_POINT('Ctrl Pts',(-5.9558757940577E-16,-4.86334165753294,
-32.53125));
#304956=CARTESIAN_POINT('Ctrl Pts',(1.58019549404244,-4.86334165753293,
-32.44375));
#304957=CARTESIAN_POINT('Ctrl Pts',(2.85860050315749,-3.93452605039577,
-32.35625));
#304958=CARTESIAN_POINT('Ctrl Pts',(4.13700551227254,-3.0057104432586,-32.26875));
#304959=CARTESIAN_POINT('Ctrl Pts',(4.62531277436637,-1.5028552216293,-32.18125));
#304960=CARTESIAN_POINT('Ctrl Pts',(5.1136200364602,1.31104854979364E-15,
-32.09375));
#304961=CARTESIAN_POINT('Ctrl Pts',(4.62531277436638,1.5028552216293,-32.00625));
#304962=CARTESIAN_POINT('Ctrl Pts',(4.13700551227254,3.00571044325861,-31.91875));
#304963=CARTESIAN_POINT('Ctrl Pts',(2.8586005031575,3.93452605039578,-31.83125));
#304964=CARTESIAN_POINT('Ctrl Pts',(1.58019549404244,4.86334165753293,-31.74375));
#304965=CARTESIAN_POINT('Ctrl Pts',(0.,4.86334165753294,-31.65625));
#304966=CARTESIAN_POINT('Ctrl Pts',(-1.58019549404244,4.86334165753293,
-31.56875));
#304967=CARTESIAN_POINT('Ctrl Pts',(-2.8586005031575,3.93452605039578,-31.48125));
#304968=CARTESIAN_POINT('Ctrl Pts',(-4.13700551227254,3.00571044325861,
-31.39375));
#304969=CARTESIAN_POINT('Ctrl Pts',(-4.62531277436637,1.5028552216293,-31.30625));
#304970=CARTESIAN_POINT('Ctrl Pts',(-5.1136200364602,2.59084916344097E-15,
-31.21875));
#304971=CARTESIAN_POINT('Ctrl Pts',(-4.62531277436638,-1.5028552216293,
-31.13125));
#304972=CARTESIAN_POINT('Ctrl Pts',(-4.13700551227254,-3.0057104432586,
-31.04375));
#304973=CARTESIAN_POINT('Ctrl Pts',(-2.8586005031575,-3.93452605039577,
-30.95625));
#304974=CARTESIAN_POINT('Ctrl Pts',(-1.58019549404244,-4.86334165753293,
-30.86875));
#304975=CARTESIAN_POINT('Ctrl Pts',(-5.9558757940577E-16,-4.86334165753294,
-30.78125));
#304976=CARTESIAN_POINT('Origin',(-3.81730450148946E-15,-2.22044604925031E-15,
-37.015625));
#304977=CARTESIAN_POINT('',(-4.41289208089522E-15,-4.86334165753294,-34.5));
#304978=CARTESIAN_POINT('',(-4.41289208089522E-15,-4.86334165753294,-34.28125));
#304979=CARTESIAN_POINT('',(-8.23019658238468E-15,-4.86334165753294,-37.015625));
#304980=CARTESIAN_POINT('Ctrl Pts',(-5.9558757940577E-16,-4.86334165753294,
-34.5));
#304981=CARTESIAN_POINT('Ctrl Pts',(1.58019549404244,-4.86334165753293,
-34.4125));
#304982=CARTESIAN_POINT('Ctrl Pts',(2.85860050315749,-3.93452605039577,
-34.325));
#304983=CARTESIAN_POINT('Ctrl Pts',(4.13700551227254,-3.0057104432586,-34.2375));
#304984=CARTESIAN_POINT('Ctrl Pts',(4.62531277436637,-1.5028552216293,-34.15));
#304985=CARTESIAN_POINT('Ctrl Pts',(5.1136200364602,1.2495674534552E-15,
-34.0625));
#304986=CARTESIAN_POINT('Ctrl Pts',(4.62531277436638,1.5028552216293,-33.975));
#304987=CARTESIAN_POINT('Ctrl Pts',(4.13700551227254,3.00571044325861,-33.8875));
#304988=CARTESIAN_POINT('Ctrl Pts',(2.8586005031575,3.93452605039578,-33.8));
#304989=CARTESIAN_POINT('Ctrl Pts',(1.58019549404244,4.86334165753293,-33.7125));
#304990=CARTESIAN_POINT('Ctrl Pts',(0.,4.86334165753294,-33.625));
#304991=CARTESIAN_POINT('Ctrl Pts',(-1.58019549404244,4.86334165753293,
-33.5375));
#304992=CARTESIAN_POINT('Ctrl Pts',(-2.8586005031575,3.93452605039578,-33.45));
#304993=CARTESIAN_POINT('Ctrl Pts',(-4.13700551227254,3.00571044325861,
-33.3625));
#304994=CARTESIAN_POINT('Ctrl Pts',(-4.62531277436637,1.5028552216293,-33.275));
#304995=CARTESIAN_POINT('Ctrl Pts',(-5.1136200364602,2.52936806710252E-15,
-33.1875));
#304996=CARTESIAN_POINT('Ctrl Pts',(-4.62531277436638,-1.5028552216293,
-33.1));
#304997=CARTESIAN_POINT('Ctrl Pts',(-4.13700551227254,-3.0057104432586,
-33.0125));
#304998=CARTESIAN_POINT('Ctrl Pts',(-2.8586005031575,-3.93452605039577,
-32.925));
#304999=CARTESIAN_POINT('Ctrl Pts',(-1.58019549404244,-4.86334165753293,
-32.8375));
#305000=CARTESIAN_POINT('Ctrl Pts',(-5.9558757940577E-16,-4.86334165753294,
-32.75));
#305001=CARTESIAN_POINT('Ctrl Pts',(-5.9558757940577E-16,-4.86334165753294,
-34.28125));
#305002=CARTESIAN_POINT('Ctrl Pts',(1.58019549404244,-4.86334165753293,
-34.19375));
#305003=CARTESIAN_POINT('Ctrl Pts',(2.85860050315749,-3.93452605039577,
-34.10625));
#305004=CARTESIAN_POINT('Ctrl Pts',(4.13700551227254,-3.0057104432586,-34.01875));
#305005=CARTESIAN_POINT('Ctrl Pts',(4.62531277436637,-1.5028552216293,-33.93125));
#305006=CARTESIAN_POINT('Ctrl Pts',(5.1136200364602,1.25639868638169E-15,
-33.84375));
#305007=CARTESIAN_POINT('Ctrl Pts',(4.62531277436638,1.5028552216293,-33.75625));
#305008=CARTESIAN_POINT('Ctrl Pts',(4.13700551227254,3.00571044325861,-33.66875));
#305009=CARTESIAN_POINT('Ctrl Pts',(2.8586005031575,3.93452605039578,-33.58125));
#305010=CARTESIAN_POINT('Ctrl Pts',(1.58019549404244,4.86334165753293,-33.49375));
#305011=CARTESIAN_POINT('Ctrl Pts',(0.,4.86334165753294,-33.40625));
#305012=CARTESIAN_POINT('Ctrl Pts',(-1.58019549404244,4.86334165753293,
-33.31875));
#305013=CARTESIAN_POINT('Ctrl Pts',(-2.8586005031575,3.93452605039578,-33.23125));
#305014=CARTESIAN_POINT('Ctrl Pts',(-4.13700551227254,3.00571044325861,
-33.14375));
#305015=CARTESIAN_POINT('Ctrl Pts',(-4.62531277436637,1.5028552216293,-33.05625));
#305016=CARTESIAN_POINT('Ctrl Pts',(-5.1136200364602,2.53619930002902E-15,
-32.96875));
#305017=CARTESIAN_POINT('Ctrl Pts',(-4.62531277436638,-1.5028552216293,
-32.88125));
#305018=CARTESIAN_POINT('Ctrl Pts',(-4.13700551227254,-3.0057104432586,
-32.79375));
#305019=CARTESIAN_POINT('Ctrl Pts',(-2.8586005031575,-3.93452605039577,
-32.70625));
#305020=CARTESIAN_POINT('Ctrl Pts',(-1.58019549404244,-4.86334165753293,
-32.61875));
#305021=CARTESIAN_POINT('Ctrl Pts',(-5.9558757940577E-16,-4.86334165753294,
-32.53125));
#305022=CARTESIAN_POINT('Origin',(-3.81730450148946E-15,-2.22044604925031E-15,
-37.015625));
#305023=CARTESIAN_POINT('',(-8.23019658238468E-15,-4.86334165753294,-36.0741583424671));
#305024=CARTESIAN_POINT('',(-4.41289208089522E-15,-4.86334165753294,-36.03125));
#305025=CARTESIAN_POINT('',(-8.23019658238468E-15,-4.86334165753294,-37.015625));
#305026=CARTESIAN_POINT('',(2.87087722362434,-3.92557716072047,-36.0741583424671));
#305027=CARTESIAN_POINT('Origin',(-3.81730450148946E-15,-2.22044604925031E-15,
-36.0741583424671));
#305028=CARTESIAN_POINT('Ctrl Pts',(2.87087722362434,-3.92557716072047,
-36.074158342467));
#305029=CARTESIAN_POINT('Ctrl Pts',(4.13959932290703,-2.99772751497028,
-35.9870352138948));
#305030=CARTESIAN_POINT('Ctrl Pts',(4.62531277436637,-1.5028552216293,-35.9));
#305031=CARTESIAN_POINT('Ctrl Pts',(5.1136200364602,1.19491759004325E-15,
-35.8125));
#305032=CARTESIAN_POINT('Ctrl Pts',(4.62531277436638,1.5028552216293,-35.725));
#305033=CARTESIAN_POINT('Ctrl Pts',(4.13700551227254,3.00571044325861,-35.6375));
#305034=CARTESIAN_POINT('Ctrl Pts',(2.8586005031575,3.93452605039578,-35.55));
#305035=CARTESIAN_POINT('Ctrl Pts',(1.58019549404244,4.86334165753293,-35.4625));
#305036=CARTESIAN_POINT('Ctrl Pts',(0.,4.86334165753294,-35.375));
#305037=CARTESIAN_POINT('Ctrl Pts',(-1.58019549404244,4.86334165753293,
-35.2875));
#305038=CARTESIAN_POINT('Ctrl Pts',(-2.8586005031575,3.93452605039578,-35.2));
#305039=CARTESIAN_POINT('Ctrl Pts',(-4.13700551227254,3.00571044325861,
-35.1125));
#305040=CARTESIAN_POINT('Ctrl Pts',(-4.62531277436637,1.5028552216293,-35.025));
#305041=CARTESIAN_POINT('Ctrl Pts',(-5.1136200364602,2.47471820369058E-15,
-34.9375));
#305042=CARTESIAN_POINT('Ctrl Pts',(-4.62531277436638,-1.5028552216293,
-34.85));
#305043=CARTESIAN_POINT('Ctrl Pts',(-4.13700551227254,-3.0057104432586,
-34.7625));
#305044=CARTESIAN_POINT('Ctrl Pts',(-2.8586005031575,-3.93452605039577,
-34.675));
#305045=CARTESIAN_POINT('Ctrl Pts',(-1.58019549404244,-4.86334165753293,
-34.5875));
#305046=CARTESIAN_POINT('Ctrl Pts',(-5.9558757940577E-16,-4.86334165753294,
-34.5));
#305047=CARTESIAN_POINT('Ctrl Pts',(-5.9558757940577E-16,-4.86334165753294,
-36.03125));
#305048=CARTESIAN_POINT('Ctrl Pts',(1.58019549404244,-4.86334165753293,
-35.94375));
#305049=CARTESIAN_POINT('Ctrl Pts',(2.85860050315749,-3.93452605039577,
-35.85625));
#305050=CARTESIAN_POINT('Ctrl Pts',(4.13700551227254,-3.0057104432586,-35.76875));
#305051=CARTESIAN_POINT('Ctrl Pts',(4.62531277436637,-1.5028552216293,-35.68125));
#305052=CARTESIAN_POINT('Ctrl Pts',(5.1136200364602,1.20174882296974E-15,
-35.59375));
#305053=CARTESIAN_POINT('Ctrl Pts',(4.62531277436638,1.5028552216293,-35.50625));
#305054=CARTESIAN_POINT('Ctrl Pts',(4.13700551227254,3.00571044325861,-35.41875));
#305055=CARTESIAN_POINT('Ctrl Pts',(2.8586005031575,3.93452605039578,-35.33125));
#305056=CARTESIAN_POINT('Ctrl Pts',(1.58019549404244,4.86334165753293,-35.24375));
#305057=CARTESIAN_POINT('Ctrl Pts',(0.,4.86334165753294,-35.15625));
#305058=CARTESIAN_POINT('Ctrl Pts',(-1.58019549404244,4.86334165753293,
-35.06875));
#305059=CARTESIAN_POINT('Ctrl Pts',(-2.8586005031575,3.93452605039578,-34.98125));
#305060=CARTESIAN_POINT('Ctrl Pts',(-4.13700551227254,3.00571044325861,
-34.89375));
#305061=CARTESIAN_POINT('Ctrl Pts',(-4.62531277436637,1.5028552216293,-34.80625));
#305062=CARTESIAN_POINT('Ctrl Pts',(-5.1136200364602,2.48154943661707E-15,
-34.71875));
#305063=CARTESIAN_POINT('Ctrl Pts',(-4.62531277436638,-1.5028552216293,
-34.63125));
#305064=CARTESIAN_POINT('Ctrl Pts',(-4.13700551227254,-3.0057104432586,
-34.54375));
#305065=CARTESIAN_POINT('Ctrl Pts',(-2.8586005031575,-3.93452605039577,
-34.45625));
#305066=CARTESIAN_POINT('Ctrl Pts',(-1.58019549404244,-4.86334165753293,
-34.36875));
#305067=CARTESIAN_POINT('Ctrl Pts',(-5.9558757940577E-16,-4.86334165753294,
-34.28125));
#305068=CARTESIAN_POINT('Origin',(0.,1.54726425086094E-32,-36.25));
#305069=CARTESIAN_POINT('',(-5.74053187100322E-16,4.6875,-36.25));
#305070=CARTESIAN_POINT('Origin',(0.,0.,-36.25));
#305071=CARTESIAN_POINT('Origin',(0.,0.,-36.25));
#305072=CARTESIAN_POINT('',(-0.75570415697393,-4.80426927898796,-36.0741583424671));
#305073=CARTESIAN_POINT('Origin',(-3.81730450148946E-15,-2.22044604925031E-15,
-36.0741583424671));
#305074=CARTESIAN_POINT('Ctrl Pts',(-0.755704156980561,-4.80426927898596,
-36.074158342468));
#305075=CARTESIAN_POINT('Ctrl Pts',(-0.20401214347208,-4.96963876412555,
-35.9965237414583));
#305076=CARTESIAN_POINT('Ctrl Pts',(0.311551649488213,-5.01323384168292,
-35.9327029210741));
#305077=CARTESIAN_POINT('Ctrl Pts',(1.25407404975781,-4.99702713055866,
-35.8106779496758));
#305078=CARTESIAN_POINT('Ctrl Pts',(1.76270719049683,-4.91132116278564,
-35.7443314791183));
#305079=CARTESIAN_POINT('Ctrl Pts',(3.0561085366865,-4.48758075325132,-35.5736761112956));
#305080=CARTESIAN_POINT('Ctrl Pts',(3.66622286879486,-4.06718946684808,
-35.4903729948851));
#305081=CARTESIAN_POINT('Ctrl Pts',(4.61382316280902,-3.24347284732762,
-35.3397991561213));
#305082=CARTESIAN_POINT('Ctrl Pts',(5.04706534954943,-2.69479623139893,
-35.2577302368079));
#305083=CARTESIAN_POINT('Ctrl Pts',(5.53804224961896,-1.75560587935618,
-35.1392571522409));
#305084=CARTESIAN_POINT('Ctrl Pts',(5.67664426551943,-1.41114454880524,
-35.0991515136516));
#305085=CARTESIAN_POINT('Ctrl Pts',(5.88654445210013,-0.717259107080557,
-35.0184068473996));
#305086=CARTESIAN_POINT('Ctrl Pts',(5.95970573886025,-0.360868816120939,
-34.9777942611398));
#305087=CARTESIAN_POINT('Ctrl Pts',(6.00000000000006,1.3086753902769E-13,
-34.9375));
#305088=CARTESIAN_POINT('',(5.66027585496539E-13,5.3065902853892,-35.6309097146108));
#305089=CARTESIAN_POINT('Ctrl Pts',(4.25090439081148,-4.23436085615996,
-34.9375));
#305090=CARTESIAN_POINT('Ctrl Pts',(3.94586432209468,-4.52301011578173,
-34.9499085068966));
#305091=CARTESIAN_POINT('Ctrl Pts',(3.60994414662963,-4.78043202406146,
-34.9619227444854));
#305092=CARTESIAN_POINT('Ctrl Pts',(2.89993674271926,-5.21329695011778,
-34.986087803612));
#305093=CARTESIAN_POINT('Ctrl Pts',(2.52765946231677,-5.39008399969571,
-34.9983670497719));
#305094=CARTESIAN_POINT('Ctrl Pts',(1.33396338181343,-5.81126867800779,
-35.0366314074234));
#305095=CARTESIAN_POINT('Ctrl Pts',(0.582212176146963,-5.88009959498879,
-35.0592032216902));
#305096=CARTESIAN_POINT('Ctrl Pts',(-0.78543039238956,-5.83604565467705,
-35.0990862861668));
#305097=CARTESIAN_POINT('Ctrl Pts',(-1.54046399409007,-5.65922745007568,
-35.1227986339086));
#305098=CARTESIAN_POINT('Ctrl Pts',(-2.87943510559081,-5.04856276714971,
-35.1682398652137));
#305099=CARTESIAN_POINT('Ctrl Pts',(-3.5125870879507,-4.61978096154844,
-35.1902411990604));
#305100=CARTESIAN_POINT('Ctrl Pts',(-4.31607850491965,-3.7579555268088,
-35.2267553883466));
#305101=CARTESIAN_POINT('Ctrl Pts',(-4.54240102332553,-3.46176213771459,
-35.2384602619037));
#305102=CARTESIAN_POINT('Ctrl Pts',(-5.12359255224559,-2.52341861708909,
-35.2732506014562));
#305103=CARTESIAN_POINT('Ctrl Pts',(-5.38789728595103,-1.82861905627414,
-35.2952726496514));
#305104=CARTESIAN_POINT('Ctrl Pts',(-5.62948928770176,-0.391419802924234,
-35.340899264706));
#305105=CARTESIAN_POINT('Ctrl Pts',(-5.60963733778489,0.338237306065926,
-35.3643460096725));
#305106=CARTESIAN_POINT('Ctrl Pts',(-5.29068241366305,1.7582581177162,-35.4105557797717));
#305107=CARTESIAN_POINT('Ctrl Pts',(-4.99092361989608,2.43522600496335,
-35.4329662937982));
#305108=CARTESIAN_POINT('Ctrl Pts',(-4.12356683987079,3.65185184338728,
-35.4818385718741));
#305109=CARTESIAN_POINT('Ctrl Pts',(-3.60214275753461,4.11179926418803,
-35.5041628936101));
#305110=CARTESIAN_POINT('Ctrl Pts',(-2.50569072638291,4.82632890339624,
-35.5456578831318));
#305111=CARTESIAN_POINT('Ctrl Pts',(-1.84237918164405,5.09141668561591,
-35.569351301463));
#305112=CARTESIAN_POINT('Ctrl Pts',(-0.787765501183242,5.286414527606,-35.6051819697655));
#305113=CARTESIAN_POINT('Ctrl Pts',(-0.402304728178604,5.31953353865749,
-35.6179664613425));
#305114=CARTESIAN_POINT('Ctrl Pts',(1.1326703464043E-12,5.3065902853892,
-35.6309097146108));
#305115=CARTESIAN_POINT('',(-5.74053187100322E-16,4.6875,-36.25));
#305116=CARTESIAN_POINT('Ctrl Pts',(1.13305198556901E-12,5.3065902853892,
-35.6309097146108));
#305117=CARTESIAN_POINT('Ctrl Pts',(0.301858928469087,5.29687865067854,
-35.6406213493215));
#305118=CARTESIAN_POINT('Ctrl Pts',(0.613170200032512,5.26082782642507,
-35.6509592015469));
#305119=CARTESIAN_POINT('Ctrl Pts',(1.59305535335563,5.05107298329413,-35.6847185175551));
#305120=CARTESIAN_POINT('Ctrl Pts',(2.22246370547848,4.78190033023382,-35.7081169756363));
#305121=CARTESIAN_POINT('Ctrl Pts',(3.06451237669578,4.20907822167898,-35.7421202323282));
#305122=CARTESIAN_POINT('Ctrl Pts',(3.32719700442894,3.99037699520634,-35.7532357491875));
#305123=CARTESIAN_POINT('Ctrl Pts',(4.02745140797445,3.27661400272233,-35.7873464474319));
#305124=CARTESIAN_POINT('Ctrl Pts',(4.39375114628118,2.72273009067369,-35.8105276921273));
#305125=CARTESIAN_POINT('Ctrl Pts',(4.90047483751086,1.49956602513327,-35.8561248424504));
#305126=CARTESIAN_POINT('Ctrl Pts',(5.0333291364154,0.84052286403436,-35.878337573202));
#305127=CARTESIAN_POINT('Ctrl Pts',(5.03197635517925,-0.154058292819836,
-35.9137516628987));
#305128=CARTESIAN_POINT('Ctrl Pts',(4.99971688172876,-0.479745816608457,
-35.9254296301762));
#305129=CARTESIAN_POINT('Ctrl Pts',(4.81851961074914,-1.3918952367453,-35.9583641196365));
#305130=CARTESIAN_POINT('Ctrl Pts',(4.5840718021508,-2.01546334153228,-35.9805560596166));
#305131=CARTESIAN_POINT('Ctrl Pts',(3.83654650082638,-3.12507114135312,
-36.0291042366888));
#305132=CARTESIAN_POINT('Ctrl Pts',(3.38981590912108,-3.57335138044469,
-36.0521323813635));
#305133=CARTESIAN_POINT('Ctrl Pts',(2.87087722362394,-3.92557716072074,
-36.0741583424671));
#305134=CARTESIAN_POINT('Ctrl Pts',(0.,6.09472152853892,-36.1953125));
#305135=CARTESIAN_POINT('Ctrl Pts',(-1.98029506767702,6.09472152853892,
-36.1078125));
#305136=CARTESIAN_POINT('Ctrl Pts',(-3.58238743130462,4.93073329257085,
-36.0203125));
#305137=CARTESIAN_POINT('Ctrl Pts',(-5.18447979493222,3.76674505660277,
-35.9328125));
#305138=CARTESIAN_POINT('Ctrl Pts',(-5.7964246247213,1.88337252830138,-35.8453125));
#305139=CARTESIAN_POINT('Ctrl Pts',(-6.40836945451038,2.52838161674187E-15,
-35.7578125));
#305140=CARTESIAN_POINT('Ctrl Pts',(-5.7964246247213,-1.88337252830138,
-35.6703125));
#305141=CARTESIAN_POINT('Ctrl Pts',(-5.18447979493222,-3.76674505660276,
-35.5828125));
#305142=CARTESIAN_POINT('Ctrl Pts',(-3.58238743130462,-4.93073329257084,
-35.4953125));
#305143=CARTESIAN_POINT('Ctrl Pts',(-1.98029506767702,-6.09472152853892,
-35.4078125));
#305144=CARTESIAN_POINT('Ctrl Pts',(-7.46388121161966E-16,-6.09472152853892,
-35.3203125));
#305145=CARTESIAN_POINT('Ctrl Pts',(1.98029506767702,-6.09472152853892,
-35.2328125));
#305146=CARTESIAN_POINT('Ctrl Pts',(3.58238743130462,-4.93073329257084,
-35.1453125));
#305147=CARTESIAN_POINT('Ctrl Pts',(5.18447979493222,-3.76674505660277,
-35.0578125));
#305148=CARTESIAN_POINT('Ctrl Pts',(5.7964246247213,-1.88337252830138,-34.9703125));
#305149=CARTESIAN_POINT('Ctrl Pts',(6.40836945451038,9.86108720403888E-16,
-34.8828125));
#305150=CARTESIAN_POINT('Ctrl Pts',(5.7964246247213,1.88337252830138,-34.7953125));
#305151=CARTESIAN_POINT('Ctrl Pts',(5.18447979493222,3.76674505660277,-34.7078125));
#305152=CARTESIAN_POINT('Ctrl Pts',(3.58238743130462,4.93073329257085,-34.6203125));
#305153=CARTESIAN_POINT('Ctrl Pts',(1.98029506767702,6.09472152853892,-34.5328125));
#305154=CARTESIAN_POINT('Ctrl Pts',(0.,6.09472152853892,-34.4453125));
#305155=CARTESIAN_POINT('Ctrl Pts',(-1.98029506767702,6.09472152853892,
-34.3578125));
#305156=CARTESIAN_POINT('Ctrl Pts',(-3.58238743130462,4.93073329257085,
-34.2703125));
#305157=CARTESIAN_POINT('Ctrl Pts',(-5.18447979493222,3.76674505660277,
-34.1828125));
#305158=CARTESIAN_POINT('Ctrl Pts',(-5.7964246247213,1.88337252830138,-34.0953125));
#305159=CARTESIAN_POINT('Ctrl Pts',(-6.40836945451038,2.58303148015383E-15,
-34.0078125));
#305160=CARTESIAN_POINT('Ctrl Pts',(-5.7964246247213,-1.88337252830138,
-33.9203125));
#305161=CARTESIAN_POINT('Ctrl Pts',(-5.18447979493222,-3.76674505660276,
-33.8328125));
#305162=CARTESIAN_POINT('Ctrl Pts',(-3.58238743130462,-4.93073329257084,
-33.7453125));
#305163=CARTESIAN_POINT('Ctrl Pts',(-1.98029506767702,-6.09472152853892,
-33.6578125));
#305164=CARTESIAN_POINT('Ctrl Pts',(-7.46388121161966E-16,-6.09472152853892,
-33.5703125));
#305165=CARTESIAN_POINT('Ctrl Pts',(1.98029506767702,-6.09472152853892,
-33.4828125));
#305166=CARTESIAN_POINT('Ctrl Pts',(3.58238743130462,-4.93073329257084,
-33.3953125));
#305167=CARTESIAN_POINT('Ctrl Pts',(5.18447979493222,-3.76674505660277,
-33.3078125));
#305168=CARTESIAN_POINT('Ctrl Pts',(5.7964246247213,-1.88337252830138,-33.2203125));
#305169=CARTESIAN_POINT('Ctrl Pts',(6.40836945451038,1.04075858381584E-15,
-33.1328125));
#305170=CARTESIAN_POINT('Ctrl Pts',(5.7964246247213,1.88337252830138,-33.0453125));
#305171=CARTESIAN_POINT('Ctrl Pts',(5.18447979493222,3.76674505660277,-32.9578125));
#305172=CARTESIAN_POINT('Ctrl Pts',(3.58238743130462,4.93073329257085,-32.8703125));
#305173=CARTESIAN_POINT('Ctrl Pts',(1.98029506767702,6.09472152853892,-32.7828125));
#305174=CARTESIAN_POINT('Ctrl Pts',(0.,6.09472152853892,-32.6953125));
#305175=CARTESIAN_POINT('Ctrl Pts',(-1.98029506767702,6.09472152853892,
-32.6078125));
#305176=CARTESIAN_POINT('Ctrl Pts',(-3.58238743130462,4.93073329257085,
-32.5203125));
#305177=CARTESIAN_POINT('Ctrl Pts',(-5.18447979493222,3.76674505660277,
-32.4328125));
#305178=CARTESIAN_POINT('Ctrl Pts',(-5.7964246247213,1.88337252830138,-32.3453125));
#305179=CARTESIAN_POINT('Ctrl Pts',(-6.40836945451038,2.63768134356578E-15,
-32.2578125));
#305180=CARTESIAN_POINT('Ctrl Pts',(-5.7964246247213,-1.88337252830138,
-32.1703125));
#305181=CARTESIAN_POINT('Ctrl Pts',(-5.18447979493222,-3.76674505660276,
-32.0828125));
#305182=CARTESIAN_POINT('Ctrl Pts',(-3.58238743130462,-4.93073329257084,
-31.9953125));
#305183=CARTESIAN_POINT('Ctrl Pts',(-1.98029506767702,-6.09472152853892,
-31.9078125));
#305184=CARTESIAN_POINT('Ctrl Pts',(-7.46388121161966E-16,-6.09472152853892,
-31.8203125));
#305185=CARTESIAN_POINT('Ctrl Pts',(1.98029506767702,-6.09472152853892,
-31.7328125));
#305186=CARTESIAN_POINT('Ctrl Pts',(3.58238743130462,-4.93073329257084,
-31.6453125));
#305187=CARTESIAN_POINT('Ctrl Pts',(5.18447979493222,-3.76674505660277,
-31.5578125));
#305188=CARTESIAN_POINT('Ctrl Pts',(5.7964246247213,-1.88337252830138,-31.4703125));
#305189=CARTESIAN_POINT('Ctrl Pts',(6.40836945451038,1.09540844722779E-15,
-31.3828125));
#305190=CARTESIAN_POINT('Ctrl Pts',(5.7964246247213,1.88337252830138,-31.2953125));
#305191=CARTESIAN_POINT('Ctrl Pts',(5.18447979493222,3.76674505660277,-31.2078125));
#305192=CARTESIAN_POINT('Ctrl Pts',(3.58238743130462,4.93073329257085,-31.1203125));
#305193=CARTESIAN_POINT('Ctrl Pts',(1.98029506767702,6.09472152853892,-31.0328125));
#305194=CARTESIAN_POINT('Ctrl Pts',(0.,6.09472152853892,-30.9453125));
#305195=CARTESIAN_POINT('Ctrl Pts',(-1.98029506767702,6.09472152853892,
-30.8578125));
#305196=CARTESIAN_POINT('Ctrl Pts',(-3.58238743130462,4.93073329257085,
-30.7703125));
#305197=CARTESIAN_POINT('Ctrl Pts',(-5.18447979493222,3.76674505660277,
-30.6828125));
#305198=CARTESIAN_POINT('Ctrl Pts',(-5.7964246247213,1.88337252830138,-30.5953125));
#305199=CARTESIAN_POINT('Ctrl Pts',(-6.40836945451038,2.69233120697773E-15,
-30.5078125));
#305200=CARTESIAN_POINT('Ctrl Pts',(-5.7964246247213,-1.88337252830138,
-30.4203125));
#305201=CARTESIAN_POINT('Ctrl Pts',(-5.18447979493222,-3.76674505660276,
-30.3328125));
#305202=CARTESIAN_POINT('Ctrl Pts',(-3.58238743130462,-4.93073329257084,
-30.2453125));
#305203=CARTESIAN_POINT('Ctrl Pts',(-1.98029506767702,-6.09472152853892,
-30.1578125));
#305204=CARTESIAN_POINT('Ctrl Pts',(-7.46388121161966E-16,-6.09472152853892,
-30.0703125));
#305205=CARTESIAN_POINT('Ctrl Pts',(1.98029506767702,-6.09472152853892,
-29.9828125));
#305206=CARTESIAN_POINT('Ctrl Pts',(3.58238743130462,-4.93073329257084,
-29.8953125));
#305207=CARTESIAN_POINT('Ctrl Pts',(5.18447979493222,-3.76674505660277,
-29.8078125));
#305208=CARTESIAN_POINT('Ctrl Pts',(5.7964246247213,-1.88337252830138,-29.7203125));
#305209=CARTESIAN_POINT('Ctrl Pts',(6.40836945451038,1.15005831063974E-15,
-29.6328125));
#305210=CARTESIAN_POINT('Ctrl Pts',(5.7964246247213,1.88337252830138,-29.5453125));
#305211=CARTESIAN_POINT('Ctrl Pts',(5.18447979493222,3.76674505660277,-29.4578125));
#305212=CARTESIAN_POINT('Ctrl Pts',(3.58238743130462,4.93073329257085,-29.3703125));
#305213=CARTESIAN_POINT('Ctrl Pts',(1.98029506767702,6.09472152853892,-29.2828125));
#305214=CARTESIAN_POINT('Ctrl Pts',(0.,6.09472152853892,-29.1953125));
#305215=CARTESIAN_POINT('Ctrl Pts',(-1.98029506767702,6.09472152853892,
-29.1078125));
#305216=CARTESIAN_POINT('Ctrl Pts',(-3.58238743130462,4.93073329257085,
-29.0203125));
#305217=CARTESIAN_POINT('Ctrl Pts',(-5.18447979493222,3.76674505660277,
-28.9328125));
#305218=CARTESIAN_POINT('Ctrl Pts',(-5.7964246247213,1.88337252830138,-28.8453125));
#305219=CARTESIAN_POINT('Ctrl Pts',(-6.40836945451038,2.74698107038968E-15,
-28.7578125));
#305220=CARTESIAN_POINT('Ctrl Pts',(-5.7964246247213,-1.88337252830138,
-28.6703125));
#305221=CARTESIAN_POINT('Ctrl Pts',(-5.18447979493222,-3.76674505660276,
-28.5828125));
#305222=CARTESIAN_POINT('Ctrl Pts',(-3.58238743130462,-4.93073329257084,
-28.4953125));
#305223=CARTESIAN_POINT('Ctrl Pts',(-1.98029506767702,-6.09472152853892,
-28.4078125));
#305224=CARTESIAN_POINT('Ctrl Pts',(-7.46388121161966E-16,-6.09472152853892,
-28.3203125));
#305225=CARTESIAN_POINT('Ctrl Pts',(1.98029506767702,-6.09472152853892,
-28.2328125));
#305226=CARTESIAN_POINT('Ctrl Pts',(3.58238743130462,-4.93073329257084,
-28.1453125));
#305227=CARTESIAN_POINT('Ctrl Pts',(5.18447979493222,-3.76674505660277,
-28.0578125));
#305228=CARTESIAN_POINT('Ctrl Pts',(5.7964246247213,-1.88337252830138,-27.9703125));
#305229=CARTESIAN_POINT('Ctrl Pts',(6.40836945451038,1.20470817405169E-15,
-27.8828125));
#305230=CARTESIAN_POINT('Ctrl Pts',(5.7964246247213,1.88337252830138,-27.7953125));
#305231=CARTESIAN_POINT('Ctrl Pts',(5.18447979493222,3.76674505660277,-27.7078125));
#305232=CARTESIAN_POINT('Ctrl Pts',(3.58238743130462,4.93073329257085,-27.6203125));
#305233=CARTESIAN_POINT('Ctrl Pts',(1.98029506767702,6.09472152853892,-27.5328125));
#305234=CARTESIAN_POINT('Ctrl Pts',(0.,6.09472152853892,-27.4453125));
#305235=CARTESIAN_POINT('Ctrl Pts',(-1.98029506767702,6.09472152853892,
-27.3578125));
#305236=CARTESIAN_POINT('Ctrl Pts',(-3.58238743130462,4.93073329257085,
-27.2703125));
#305237=CARTESIAN_POINT('Ctrl Pts',(-5.18447979493222,3.76674505660277,
-27.1828125));
#305238=CARTESIAN_POINT('Ctrl Pts',(-5.7964246247213,1.88337252830138,-27.0953125));
#305239=CARTESIAN_POINT('Ctrl Pts',(-6.40836945451038,2.80163093380163E-15,
-27.0078125));
#305240=CARTESIAN_POINT('Ctrl Pts',(-5.7964246247213,-1.88337252830138,
-26.9203125));
#305241=CARTESIAN_POINT('Ctrl Pts',(-5.18447979493222,-3.76674505660276,
-26.8328125));
#305242=CARTESIAN_POINT('Ctrl Pts',(-3.58238743130462,-4.93073329257084,
-26.7453125));
#305243=CARTESIAN_POINT('Ctrl Pts',(-1.98029506767702,-6.09472152853892,
-26.6578125));
#305244=CARTESIAN_POINT('Ctrl Pts',(-7.46388121161966E-16,-6.09472152853892,
-26.5703125));
#305245=CARTESIAN_POINT('Ctrl Pts',(1.98029506767702,-6.09472152853892,
-26.4828125));
#305246=CARTESIAN_POINT('Ctrl Pts',(3.58238743130462,-4.93073329257084,
-26.3953125));
#305247=CARTESIAN_POINT('Ctrl Pts',(5.18447979493222,-3.76674505660277,
-26.3078125));
#305248=CARTESIAN_POINT('Ctrl Pts',(5.7964246247213,-1.88337252830138,-26.2203125));
#305249=CARTESIAN_POINT('Ctrl Pts',(6.40836945451038,1.25935803746364E-15,
-26.1328125));
#305250=CARTESIAN_POINT('Ctrl Pts',(5.7964246247213,1.88337252830138,-26.0453125));
#305251=CARTESIAN_POINT('Ctrl Pts',(5.18447979493222,3.76674505660277,-25.9578125));
#305252=CARTESIAN_POINT('Ctrl Pts',(3.58238743130462,4.93073329257085,-25.8703125));
#305253=CARTESIAN_POINT('Ctrl Pts',(1.98029506767702,6.09472152853892,-25.7828125));
#305254=CARTESIAN_POINT('Ctrl Pts',(0.,6.09472152853892,-25.6953125));
#305255=CARTESIAN_POINT('Ctrl Pts',(-1.98029506767702,6.09472152853892,
-25.6078125));
#305256=CARTESIAN_POINT('Ctrl Pts',(-3.58238743130462,4.93073329257085,
-25.5203125));
#305257=CARTESIAN_POINT('Ctrl Pts',(-5.18447979493222,3.76674505660277,
-25.4328125));
#305258=CARTESIAN_POINT('Ctrl Pts',(-5.7964246247213,1.88337252830138,-25.3453125));
#305259=CARTESIAN_POINT('Ctrl Pts',(-6.40836945451038,2.85628079721358E-15,
-25.2578125));
#305260=CARTESIAN_POINT('Ctrl Pts',(-5.7964246247213,-1.88337252830138,
-25.1703125));
#305261=CARTESIAN_POINT('Ctrl Pts',(-5.18447979493222,-3.76674505660276,
-25.0828125));
#305262=CARTESIAN_POINT('Ctrl Pts',(-3.58238743130462,-4.93073329257084,
-24.9953125));
#305263=CARTESIAN_POINT('Ctrl Pts',(-1.98029506767702,-6.09472152853892,
-24.9078125));
#305264=CARTESIAN_POINT('Ctrl Pts',(-7.46388121161966E-16,-6.09472152853892,
-24.8203125));
#305265=CARTESIAN_POINT('Ctrl Pts',(1.98029506767702,-6.09472152853892,
-24.7328125));
#305266=CARTESIAN_POINT('Ctrl Pts',(3.58238743130462,-4.93073329257084,
-24.6453125));
#305267=CARTESIAN_POINT('Ctrl Pts',(5.18447979493222,-3.76674505660277,
-24.5578125));
#305268=CARTESIAN_POINT('Ctrl Pts',(5.7964246247213,-1.88337252830138,-24.4703125));
#305269=CARTESIAN_POINT('Ctrl Pts',(6.40836945451038,1.31400790087559E-15,
-24.3828125));
#305270=CARTESIAN_POINT('Ctrl Pts',(5.7964246247213,1.88337252830138,-24.2953125));
#305271=CARTESIAN_POINT('Ctrl Pts',(5.18447979493222,3.76674505660277,-24.2078125));
#305272=CARTESIAN_POINT('Ctrl Pts',(3.58238743130462,4.93073329257085,-24.1203125));
#305273=CARTESIAN_POINT('Ctrl Pts',(1.98029506767702,6.09472152853892,-24.0328125));
#305274=CARTESIAN_POINT('Ctrl Pts',(0.,6.09472152853892,-23.9453125));
#305275=CARTESIAN_POINT('Ctrl Pts',(-1.98029506767702,6.09472152853892,
-23.8578125));
#305276=CARTESIAN_POINT('Ctrl Pts',(-3.58238743130462,4.93073329257085,
-23.7703125));
#305277=CARTESIAN_POINT('Ctrl Pts',(-5.18447979493222,3.76674505660277,
-23.6828125));
#305278=CARTESIAN_POINT('Ctrl Pts',(-5.7964246247213,1.88337252830138,-23.5953125));
#305279=CARTESIAN_POINT('Ctrl Pts',(-6.40836945451038,2.91093066062553E-15,
-23.5078125));
#305280=CARTESIAN_POINT('Ctrl Pts',(-5.7964246247213,-1.88337252830138,
-23.4203125));
#305281=CARTESIAN_POINT('Ctrl Pts',(-5.18447979493222,-3.76674505660276,
-23.3328125));
#305282=CARTESIAN_POINT('Ctrl Pts',(-3.58238743130462,-4.93073329257084,
-23.2453125));
#305283=CARTESIAN_POINT('Ctrl Pts',(-1.98029506767702,-6.09472152853892,
-23.1578125));
#305284=CARTESIAN_POINT('Ctrl Pts',(-7.46388121161966E-16,-6.09472152853892,
-23.0703125));
#305285=CARTESIAN_POINT('Ctrl Pts',(1.98029506767702,-6.09472152853892,
-22.9828125));
#305286=CARTESIAN_POINT('Ctrl Pts',(3.58238743130462,-4.93073329257084,
-22.8953125));
#305287=CARTESIAN_POINT('Ctrl Pts',(5.18447979493222,-3.76674505660277,
-22.8078125));
#305288=CARTESIAN_POINT('Ctrl Pts',(5.7964246247213,-1.88337252830138,-22.7203125));
#305289=CARTESIAN_POINT('Ctrl Pts',(6.40836945451038,1.36865776428754E-15,
-22.6328125));
#305290=CARTESIAN_POINT('Ctrl Pts',(5.7964246247213,1.88337252830138,-22.5453125));
#305291=CARTESIAN_POINT('Ctrl Pts',(5.18447979493222,3.76674505660277,-22.4578125));
#305292=CARTESIAN_POINT('Ctrl Pts',(3.58238743130462,4.93073329257085,-22.3703125));
#305293=CARTESIAN_POINT('Ctrl Pts',(1.98029506767702,6.09472152853892,-22.2828125));
#305294=CARTESIAN_POINT('Ctrl Pts',(0.,6.09472152853893,-22.1953125));
#305295=CARTESIAN_POINT('Ctrl Pts',(-1.98029506767702,6.09472152853892,
-22.1078125));
#305296=CARTESIAN_POINT('Ctrl Pts',(-3.58238743130462,4.93073329257085,
-22.0203125));
#305297=CARTESIAN_POINT('Ctrl Pts',(-5.18447979493222,3.76674505660277,
-21.9328125));
#305298=CARTESIAN_POINT('Ctrl Pts',(-5.7964246247213,1.88337252830138,-21.8453125));
#305299=CARTESIAN_POINT('Ctrl Pts',(-6.40836945451038,2.96558052403748E-15,
-21.7578125));
#305300=CARTESIAN_POINT('Ctrl Pts',(-5.7964246247213,-1.88337252830138,
-21.6703125));
#305301=CARTESIAN_POINT('Ctrl Pts',(-5.18447979493222,-3.76674505660276,
-21.5828125));
#305302=CARTESIAN_POINT('Ctrl Pts',(-3.58238743130462,-4.93073329257084,
-21.4953125));
#305303=CARTESIAN_POINT('Ctrl Pts',(-1.98029506767702,-6.09472152853892,
-21.4078125));
#305304=CARTESIAN_POINT('Ctrl Pts',(-7.46388121161966E-16,-6.09472152853892,
-21.3203125));
#305305=CARTESIAN_POINT('Ctrl Pts',(1.98029506767702,-6.09472152853892,
-21.2328125));
#305306=CARTESIAN_POINT('Ctrl Pts',(3.58238743130462,-4.93073329257084,
-21.1453125));
#305307=CARTESIAN_POINT('Ctrl Pts',(5.18447979493222,-3.76674505660277,
-21.0578125));
#305308=CARTESIAN_POINT('Ctrl Pts',(5.7964246247213,-1.88337252830138,-20.9703125));
#305309=CARTESIAN_POINT('Ctrl Pts',(6.40836945451038,1.42330762769949E-15,
-20.8828125));
#305310=CARTESIAN_POINT('Ctrl Pts',(5.7964246247213,1.88337252830138,-20.7953125));
#305311=CARTESIAN_POINT('Ctrl Pts',(5.18447979493222,3.76674505660277,-20.7078125));
#305312=CARTESIAN_POINT('Ctrl Pts',(3.58238743130462,4.93073329257085,-20.6203125));
#305313=CARTESIAN_POINT('Ctrl Pts',(1.98029506767702,6.09472152853892,-20.5328125));
#305314=CARTESIAN_POINT('Ctrl Pts',(0.,6.09472152853893,-20.4453125));
#305315=CARTESIAN_POINT('Ctrl Pts',(-1.98029506767702,6.09472152853892,
-20.3578125));
#305316=CARTESIAN_POINT('Ctrl Pts',(-3.58238743130462,4.93073329257085,
-20.2703125));
#305317=CARTESIAN_POINT('Ctrl Pts',(-5.18447979493222,3.76674505660277,
-20.1828125));
#305318=CARTESIAN_POINT('Ctrl Pts',(-5.7964246247213,1.88337252830138,-20.0953125));
#305319=CARTESIAN_POINT('Ctrl Pts',(-6.40836945451038,3.02023038744943E-15,
-20.0078125));
#305320=CARTESIAN_POINT('Ctrl Pts',(-5.7964246247213,-1.88337252830138,
-19.9203125));
#305321=CARTESIAN_POINT('Ctrl Pts',(-5.18447979493222,-3.76674505660276,
-19.8328125));
#305322=CARTESIAN_POINT('Ctrl Pts',(-3.58238743130462,-4.93073329257084,
-19.7453125));
#305323=CARTESIAN_POINT('Ctrl Pts',(-1.98029506767702,-6.09472152853892,
-19.6578125));
#305324=CARTESIAN_POINT('Ctrl Pts',(-7.46388121161966E-16,-6.09472152853892,
-19.5703125));
#305325=CARTESIAN_POINT('Ctrl Pts',(1.98029506767702,-6.09472152853892,
-19.4828125));
#305326=CARTESIAN_POINT('Ctrl Pts',(3.58238743130462,-4.93073329257084,
-19.3953125));
#305327=CARTESIAN_POINT('Ctrl Pts',(5.18447979493222,-3.76674505660277,
-19.3078125));
#305328=CARTESIAN_POINT('Ctrl Pts',(5.7964246247213,-1.88337252830138,-19.2203125));
#305329=CARTESIAN_POINT('Ctrl Pts',(6.40836945451038,1.47795749111144E-15,
-19.1328125));
#305330=CARTESIAN_POINT('Ctrl Pts',(5.7964246247213,1.88337252830138,-19.0453125));
#305331=CARTESIAN_POINT('Ctrl Pts',(5.18447979493222,3.76674505660277,-18.9578125));
#305332=CARTESIAN_POINT('Ctrl Pts',(3.58238743130462,4.93073329257085,-18.8703125));
#305333=CARTESIAN_POINT('Ctrl Pts',(1.98029506767702,6.09472152853892,-18.7828125));
#305334=CARTESIAN_POINT('Ctrl Pts',(0.,6.09472152853893,-18.6953125));
#305335=CARTESIAN_POINT('Ctrl Pts',(-1.98029506767702,6.09472152853892,
-18.6078125));
#305336=CARTESIAN_POINT('Ctrl Pts',(-3.58238743130462,4.93073329257085,
-18.5203125));
#305337=CARTESIAN_POINT('Ctrl Pts',(-5.18447979493222,3.76674505660277,
-18.4328125));
#305338=CARTESIAN_POINT('Ctrl Pts',(-5.7964246247213,1.88337252830138,-18.3453125));
#305339=CARTESIAN_POINT('Ctrl Pts',(-6.40836945451038,3.07488025086138E-15,
-18.2578125));
#305340=CARTESIAN_POINT('Ctrl Pts',(-5.7964246247213,-1.88337252830138,
-18.1703125));
#305341=CARTESIAN_POINT('Ctrl Pts',(-5.18447979493222,-3.76674505660276,
-18.0828125));
#305342=CARTESIAN_POINT('Ctrl Pts',(-3.58238743130462,-4.93073329257084,
-17.9953125));
#305343=CARTESIAN_POINT('Ctrl Pts',(-1.98029506767702,-6.09472152853892,
-17.9078125));
#305344=CARTESIAN_POINT('Ctrl Pts',(-7.46388121161966E-16,-6.09472152853892,
-17.8203125));
#305345=CARTESIAN_POINT('Ctrl Pts',(1.98029506767702,-6.09472152853892,
-17.7328125));
#305346=CARTESIAN_POINT('Ctrl Pts',(3.58238743130462,-4.93073329257084,
-17.6453125));
#305347=CARTESIAN_POINT('Ctrl Pts',(5.18447979493222,-3.76674505660277,
-17.5578125));
#305348=CARTESIAN_POINT('Ctrl Pts',(5.7964246247213,-1.88337252830138,-17.4703125));
#305349=CARTESIAN_POINT('Ctrl Pts',(6.40836945451038,1.5326073545234E-15,
-17.3828125));
#305350=CARTESIAN_POINT('Ctrl Pts',(5.7964246247213,1.88337252830138,-17.2953125));
#305351=CARTESIAN_POINT('Ctrl Pts',(5.18447979493222,3.76674505660277,-17.2078125));
#305352=CARTESIAN_POINT('Ctrl Pts',(3.58238743130462,4.93073329257085,-17.1203125));
#305353=CARTESIAN_POINT('Ctrl Pts',(1.98029506767702,6.09472152853892,-17.0328125));
#305354=CARTESIAN_POINT('Ctrl Pts',(0.,6.09472152853893,-16.9453125));
#305355=CARTESIAN_POINT('Ctrl Pts',(-1.98029506767702,6.09472152853892,
-16.8578125));
#305356=CARTESIAN_POINT('Ctrl Pts',(-3.58238743130462,4.93073329257085,
-16.7703125));
#305357=CARTESIAN_POINT('Ctrl Pts',(-5.18447979493222,3.76674505660277,
-16.6828125));
#305358=CARTESIAN_POINT('Ctrl Pts',(-5.7964246247213,1.88337252830138,-16.5953125));
#305359=CARTESIAN_POINT('Ctrl Pts',(-6.40836945451038,3.12953011427333E-15,
-16.5078125));
#305360=CARTESIAN_POINT('Ctrl Pts',(-5.7964246247213,-1.88337252830138,
-16.4203125));
#305361=CARTESIAN_POINT('Ctrl Pts',(-5.18447979493222,-3.76674505660276,
-16.3328125));
#305362=CARTESIAN_POINT('Ctrl Pts',(-3.58238743130462,-4.93073329257084,
-16.2453125));
#305363=CARTESIAN_POINT('Ctrl Pts',(-1.98029506767702,-6.09472152853892,
-16.1578125));
#305364=CARTESIAN_POINT('Ctrl Pts',(-7.46388121161966E-16,-6.09472152853892,
-16.0703125));
#305365=CARTESIAN_POINT('Ctrl Pts',(1.98029506767702,-6.09472152853892,
-15.9828125));
#305366=CARTESIAN_POINT('Ctrl Pts',(3.58238743130462,-4.93073329257084,
-15.8953125));
#305367=CARTESIAN_POINT('Ctrl Pts',(5.18447979493222,-3.76674505660277,
-15.8078125));
#305368=CARTESIAN_POINT('Ctrl Pts',(5.7964246247213,-1.88337252830138,-15.7203125));
#305369=CARTESIAN_POINT('Ctrl Pts',(6.40836945451038,1.58725721793535E-15,
-15.6328125));
#305370=CARTESIAN_POINT('Ctrl Pts',(5.7964246247213,1.88337252830138,-15.5453125));
#305371=CARTESIAN_POINT('Ctrl Pts',(5.18447979493222,3.76674505660277,-15.4578125));
#305372=CARTESIAN_POINT('Ctrl Pts',(3.58238743130462,4.93073329257085,-15.3703125));
#305373=CARTESIAN_POINT('Ctrl Pts',(1.98029506767702,6.09472152853892,-15.2828125));
#305374=CARTESIAN_POINT('Ctrl Pts',(0.,6.09472152853893,-15.1953125));
#305375=CARTESIAN_POINT('Ctrl Pts',(-1.98029506767702,6.09472152853892,
-15.1078125));
#305376=CARTESIAN_POINT('Ctrl Pts',(-3.58238743130462,4.93073329257085,
-15.0203125));
#305377=CARTESIAN_POINT('Ctrl Pts',(-5.18447979493222,3.76674505660277,
-14.9328125));
#305378=CARTESIAN_POINT('Ctrl Pts',(-5.7964246247213,1.88337252830138,-14.8453125));
#305379=CARTESIAN_POINT('Ctrl Pts',(-6.40836945451038,3.18417997768528E-15,
-14.7578125));
#305380=CARTESIAN_POINT('Ctrl Pts',(-5.7964246247213,-1.88337252830138,
-14.6703125));
#305381=CARTESIAN_POINT('Ctrl Pts',(-5.18447979493222,-3.76674505660276,
-14.5828125));
#305382=CARTESIAN_POINT('Ctrl Pts',(-3.58238743130462,-4.93073329257084,
-14.4953125));
#305383=CARTESIAN_POINT('Ctrl Pts',(-1.98029506767702,-6.09472152853892,
-14.4078125));
#305384=CARTESIAN_POINT('Ctrl Pts',(-7.46388121161966E-16,-6.09472152853892,
-14.3203125));
#305385=CARTESIAN_POINT('Ctrl Pts',(1.98029506767702,-6.09472152853892,
-14.2328125));
#305386=CARTESIAN_POINT('Ctrl Pts',(3.58238743130462,-4.93073329257084,
-14.1453125));
#305387=CARTESIAN_POINT('Ctrl Pts',(5.18447979493222,-3.76674505660277,
-14.0578125));
#305388=CARTESIAN_POINT('Ctrl Pts',(5.7964246247213,-1.88337252830138,-13.9703125));
#305389=CARTESIAN_POINT('Ctrl Pts',(6.40836945451038,1.6419070813473E-15,
-13.8828125));
#305390=CARTESIAN_POINT('Ctrl Pts',(5.7964246247213,1.88337252830138,-13.7953125));
#305391=CARTESIAN_POINT('Ctrl Pts',(5.18447979493222,3.76674505660277,-13.7078125));
#305392=CARTESIAN_POINT('Ctrl Pts',(3.58238743130462,4.93073329257085,-13.6203125));
#305393=CARTESIAN_POINT('Ctrl Pts',(1.98029506767702,6.09472152853892,-13.5328125));
#305394=CARTESIAN_POINT('Ctrl Pts',(0.,6.09472152853893,-13.4453125));
#305395=CARTESIAN_POINT('Ctrl Pts',(-1.98029506767702,6.09472152853892,
-13.3578125));
#305396=CARTESIAN_POINT('Ctrl Pts',(-3.58238743130462,4.93073329257085,
-13.2703125));
#305397=CARTESIAN_POINT('Ctrl Pts',(-5.18447979493222,3.76674505660277,
-13.1828125));
#305398=CARTESIAN_POINT('Ctrl Pts',(-5.7964246247213,1.88337252830138,-13.0953125));
#305399=CARTESIAN_POINT('Ctrl Pts',(-6.40836945451038,3.23882984109724E-15,
-13.0078125));
#305400=CARTESIAN_POINT('Ctrl Pts',(-5.7964246247213,-1.88337252830138,
-12.9203125));
#305401=CARTESIAN_POINT('Ctrl Pts',(-5.18447979493222,-3.76674505660276,
-12.8328125));
#305402=CARTESIAN_POINT('Ctrl Pts',(-3.58238743130462,-4.93073329257084,
-12.7453125));
#305403=CARTESIAN_POINT('Ctrl Pts',(-1.98029506767702,-6.09472152853892,
-12.6578125));
#305404=CARTESIAN_POINT('Ctrl Pts',(-7.46388121161966E-16,-6.09472152853892,
-12.5703125));
#305405=CARTESIAN_POINT('Ctrl Pts',(1.98029506767702,-6.09472152853892,
-12.4828125));
#305406=CARTESIAN_POINT('Ctrl Pts',(3.58238743130462,-4.93073329257084,
-12.3953125));
#305407=CARTESIAN_POINT('Ctrl Pts',(5.18447979493222,-3.76674505660277,
-12.3078125));
#305408=CARTESIAN_POINT('Ctrl Pts',(5.7964246247213,-1.88337252830138,-12.2203125));
#305409=CARTESIAN_POINT('Ctrl Pts',(6.40836945451038,1.69655694475925E-15,
-12.1328125));
#305410=CARTESIAN_POINT('Ctrl Pts',(5.7964246247213,1.88337252830138,-12.0453125));
#305411=CARTESIAN_POINT('Ctrl Pts',(5.18447979493222,3.76674505660277,-11.9578125));
#305412=CARTESIAN_POINT('Ctrl Pts',(3.58238743130462,4.93073329257085,-11.8703125));
#305413=CARTESIAN_POINT('Ctrl Pts',(1.98029506767702,6.09472152853892,-11.7828125));
#305414=CARTESIAN_POINT('Ctrl Pts',(0.,6.09472152853893,-11.6953125));
#305415=CARTESIAN_POINT('Ctrl Pts',(-1.98029506767702,6.09472152853892,
-11.6078125));
#305416=CARTESIAN_POINT('Ctrl Pts',(-3.58238743130462,4.93073329257085,
-11.5203125));
#305417=CARTESIAN_POINT('Ctrl Pts',(-5.18447979493222,3.76674505660277,
-11.4328125));
#305418=CARTESIAN_POINT('Ctrl Pts',(-5.7964246247213,1.88337252830138,-11.3453125));
#305419=CARTESIAN_POINT('Ctrl Pts',(-6.40836945451038,3.29347970450919E-15,
-11.2578125));
#305420=CARTESIAN_POINT('Ctrl Pts',(-5.7964246247213,-1.88337252830138,
-11.1703125));
#305421=CARTESIAN_POINT('Ctrl Pts',(-5.18447979493222,-3.76674505660276,
-11.0828125));
#305422=CARTESIAN_POINT('Ctrl Pts',(-3.58238743130462,-4.93073329257084,
-10.9953125));
#305423=CARTESIAN_POINT('Ctrl Pts',(-1.98029506767702,-6.09472152853892,
-10.9078125));
#305424=CARTESIAN_POINT('Ctrl Pts',(-7.46388121161966E-16,-6.09472152853892,
-10.8203125));
#305425=CARTESIAN_POINT('Ctrl Pts',(1.98029506767702,-6.09472152853892,
-10.7328125));
#305426=CARTESIAN_POINT('Ctrl Pts',(3.58238743130462,-4.93073329257084,
-10.6453125));
#305427=CARTESIAN_POINT('Ctrl Pts',(5.18447979493222,-3.76674505660277,
-10.5578125));
#305428=CARTESIAN_POINT('Ctrl Pts',(5.7964246247213,-1.88337252830138,-10.4703125));
#305429=CARTESIAN_POINT('Ctrl Pts',(6.40836945451038,1.7512068081712E-15,
-10.3828125));
#305430=CARTESIAN_POINT('Ctrl Pts',(5.7964246247213,1.88337252830138,-10.2953125));
#305431=CARTESIAN_POINT('Ctrl Pts',(5.18447979493222,3.76674505660277,-10.2078125));
#305432=CARTESIAN_POINT('Ctrl Pts',(3.58238743130462,4.93073329257085,-10.1203125));
#305433=CARTESIAN_POINT('Ctrl Pts',(1.98029506767702,6.09472152853892,-10.0328125));
#305434=CARTESIAN_POINT('Ctrl Pts',(0.,6.09472152853893,-9.94531250000001));
#305435=CARTESIAN_POINT('Ctrl Pts',(-1.98029506767702,6.09472152853892,
-9.85781250000001));
#305436=CARTESIAN_POINT('Ctrl Pts',(-3.58238743130462,4.93073329257085,
-9.77031250000001));
#305437=CARTESIAN_POINT('Ctrl Pts',(-5.18447979493222,3.76674505660277,
-9.6828125));
#305438=CARTESIAN_POINT('Ctrl Pts',(-5.7964246247213,1.88337252830138,-9.59531250000001));
#305439=CARTESIAN_POINT('Ctrl Pts',(-6.40836945451038,3.34812956792114E-15,
-9.50781250000001));
#305440=CARTESIAN_POINT('Ctrl Pts',(-5.7964246247213,-1.88337252830138,
-9.42031250000001));
#305441=CARTESIAN_POINT('Ctrl Pts',(-5.18447979493222,-3.76674505660276,
-9.3328125));
#305442=CARTESIAN_POINT('Ctrl Pts',(-3.58238743130462,-4.93073329257084,
-9.24531250000001));
#305443=CARTESIAN_POINT('Ctrl Pts',(-1.98029506767702,-6.09472152853892,
-9.15781250000001));
#305444=CARTESIAN_POINT('Ctrl Pts',(-7.46388121161966E-16,-6.09472152853892,
-9.07031250000001));
#305445=CARTESIAN_POINT('Ctrl Pts',(1.98029506767702,-6.09472152853892,
-8.9828125));
#305446=CARTESIAN_POINT('Ctrl Pts',(3.58238743130462,-4.93073329257084,
-8.89531250000001));
#305447=CARTESIAN_POINT('Ctrl Pts',(5.18447979493222,-3.76674505660277,
-8.8078125));
#305448=CARTESIAN_POINT('Ctrl Pts',(5.7964246247213,-1.88337252830138,-8.72031250000001));
#305449=CARTESIAN_POINT('Ctrl Pts',(6.40836945451038,1.80585667158315E-15,
-8.6328125));
#305450=CARTESIAN_POINT('Ctrl Pts',(5.7964246247213,1.88337252830138,-8.54531250000001));
#305451=CARTESIAN_POINT('Ctrl Pts',(5.18447979493222,3.76674505660277,-8.4578125));
#305452=CARTESIAN_POINT('Ctrl Pts',(3.58238743130462,4.93073329257085,-8.37031250000001));
#305453=CARTESIAN_POINT('Ctrl Pts',(1.98029506767702,6.09472152853892,-8.28281250000001));
#305454=CARTESIAN_POINT('Ctrl Pts',(0.,6.09472152853893,-8.19531250000001));
#305455=CARTESIAN_POINT('Ctrl Pts',(-1.98029506767702,6.09472152853892,
-8.10781249999999));
#305456=CARTESIAN_POINT('Ctrl Pts',(-3.58238743130462,4.93073329257085,
-8.02031250000001));
#305457=CARTESIAN_POINT('Ctrl Pts',(-5.18447979493222,3.76674505660277,
-7.9328125));
#305458=CARTESIAN_POINT('Ctrl Pts',(-5.7964246247213,1.88337252830138,-7.84531250000001));
#305459=CARTESIAN_POINT('Ctrl Pts',(-6.40836945451038,3.40277943133309E-15,
-7.7578125));
#305460=CARTESIAN_POINT('Ctrl Pts',(-5.7964246247213,-1.88337252830138,
-7.67031250000001));
#305461=CARTESIAN_POINT('Ctrl Pts',(-5.18447979493222,-3.76674505660276,
-7.5828125));
#305462=CARTESIAN_POINT('Ctrl Pts',(-3.58238743130462,-4.93073329257084,
-7.49531250000001));
#305463=CARTESIAN_POINT('Ctrl Pts',(-1.98029506767702,-6.09472152853892,
-7.4078125));
#305464=CARTESIAN_POINT('Ctrl Pts',(-7.46388121161966E-16,-6.09472152853892,
-7.32031250000001));
#305465=CARTESIAN_POINT('Ctrl Pts',(1.98029506767702,-6.09472152853892,
-7.23281250000001));
#305466=CARTESIAN_POINT('Ctrl Pts',(3.58238743130462,-4.93073329257084,
-7.14531250000001));
#305467=CARTESIAN_POINT('Ctrl Pts',(5.18447979493222,-3.76674505660277,
-7.05781250000001));
#305468=CARTESIAN_POINT('Ctrl Pts',(5.7964246247213,-1.88337252830138,-6.97031250000001));
#305469=CARTESIAN_POINT('Ctrl Pts',(6.40836945451038,1.8605065349951E-15,
-6.8828125));
#305470=CARTESIAN_POINT('Ctrl Pts',(5.7964246247213,1.88337252830138,-6.79531250000001));
#305471=CARTESIAN_POINT('Ctrl Pts',(5.18447979493222,3.76674505660277,-6.7078125));
#305472=CARTESIAN_POINT('Ctrl Pts',(3.58238743130462,4.93073329257085,-6.62031250000001));
#305473=CARTESIAN_POINT('Ctrl Pts',(1.98029506767702,6.09472152853892,-6.5328125));
#305474=CARTESIAN_POINT('Ctrl Pts',(0.,6.09472152853893,-6.44531250000001));
#305475=CARTESIAN_POINT('Ctrl Pts',(-1.98029506767702,6.09472152853892,
-6.35781250000001));
#305476=CARTESIAN_POINT('Ctrl Pts',(-3.58238743130462,4.93073329257085,
-6.27031250000001));
#305477=CARTESIAN_POINT('Ctrl Pts',(-5.18447979493222,3.76674505660277,
-6.18281250000001));
#305478=CARTESIAN_POINT('Ctrl Pts',(-5.7964246247213,1.88337252830138,-6.09531250000001));
#305479=CARTESIAN_POINT('Ctrl Pts',(-6.40836945451038,3.45742929474504E-15,
-6.00781250000001));
#305480=CARTESIAN_POINT('Ctrl Pts',(-5.7964246247213,-1.88337252830138,
-5.92031250000001));
#305481=CARTESIAN_POINT('Ctrl Pts',(-5.18447979493222,-3.76674505660276,
-5.8328125));
#305482=CARTESIAN_POINT('Ctrl Pts',(-3.58238743130462,-4.93073329257084,
-5.74531250000001));
#305483=CARTESIAN_POINT('Ctrl Pts',(-1.98029506767702,-6.09472152853892,
-5.6578125));
#305484=CARTESIAN_POINT('Ctrl Pts',(-7.46388121161966E-16,-6.09472152853892,
-5.57031250000001));
#305485=CARTESIAN_POINT('Ctrl Pts',(1.98029506767702,-6.09472152853892,
-5.48281250000001));
#305486=CARTESIAN_POINT('Ctrl Pts',(3.58238743130462,-4.93073329257084,
-5.39531250000001));
#305487=CARTESIAN_POINT('Ctrl Pts',(5.18447979493222,-3.76674505660277,
-5.30781250000001));
#305488=CARTESIAN_POINT('Ctrl Pts',(5.7964246247213,-1.88337252830138,-5.22031250000001));
#305489=CARTESIAN_POINT('Ctrl Pts',(6.40836945451038,1.91515639840705E-15,
-5.13281250000001));
#305490=CARTESIAN_POINT('Ctrl Pts',(5.7964246247213,1.88337252830138,-5.04531250000001));
#305491=CARTESIAN_POINT('Ctrl Pts',(5.18447979493222,3.76674505660277,-4.9578125));
#305492=CARTESIAN_POINT('Ctrl Pts',(3.58238743130462,4.93073329257085,-4.87031250000001));
#305493=CARTESIAN_POINT('Ctrl Pts',(1.98029506767702,6.09472152853892,-4.7828125));
#305494=CARTESIAN_POINT('Ctrl Pts',(0.,6.09472152853893,-4.69531250000001));
#305495=CARTESIAN_POINT('Ctrl Pts',(-1.98029506767702,6.09472152853892,
-4.60781250000001));
#305496=CARTESIAN_POINT('Ctrl Pts',(-3.58238743130462,4.93073329257085,
-4.52031250000001));
#305497=CARTESIAN_POINT('Ctrl Pts',(-4.25030452462165,4.44546311909431,
-4.48383348855718));
#305498=CARTESIAN_POINT('Ctrl Pts',(-4.76505105107542,3.79998934091675,
-4.44551580562765));
#305499=CARTESIAN_POINT('Ctrl Pts',(0.,4.86332528902566,-36.9062594503621));
#305500=CARTESIAN_POINT('Ctrl Pts',(-1.58019017559203,4.86332528902566,
-36.8187594503621));
#305501=CARTESIAN_POINT('Ctrl Pts',(-2.85859088199032,3.93451280799522,
-36.7312594503621));
#305502=CARTESIAN_POINT('Ctrl Pts',(-4.1369915883886,3.00570032696477,-36.6437594503621));
#305503=CARTESIAN_POINT('Ctrl Pts',(-4.62529720699086,1.50285016348238,
-36.5562594503621));
#305504=CARTESIAN_POINT('Ctrl Pts',(-5.11360282559314,2.42689822422288E-15,
-36.4687594503621));
#305505=CARTESIAN_POINT('Ctrl Pts',(-4.62529720699087,-1.50285016348238,
-36.3812594503621));
#305506=CARTESIAN_POINT('Ctrl Pts',(-4.1369915883886,-3.00570032696476,
-36.2937594503621));
#305507=CARTESIAN_POINT('Ctrl Pts',(-2.85859088199032,-3.93451280799521,
-36.2062594503621));
#305508=CARTESIAN_POINT('Ctrl Pts',(-1.58019017559203,-4.86332528902566,
-36.118759450362));
#305509=CARTESIAN_POINT('Ctrl Pts',(-5.95585574841766E-16,-4.86332528902566,
-36.0312594503621));
#305510=CARTESIAN_POINT('Ctrl Pts',(1.58019017559203,-4.86332528902566,
-35.9437594503621));
#305511=CARTESIAN_POINT('Ctrl Pts',(2.85859088199031,-3.93451280799521,
-35.8562594503621));
#305512=CARTESIAN_POINT('Ctrl Pts',(4.13699158838859,-3.00570032696476,
-35.768759450362));
#305513=CARTESIAN_POINT('Ctrl Pts',(4.62529720699086,-1.50285016348238,
-35.6812594503621));
#305514=CARTESIAN_POINT('Ctrl Pts',(5.11360282559314,1.20175168943416E-15,
-35.5937594503621));
#305515=CARTESIAN_POINT('Ctrl Pts',(4.62529720699087,1.50285016348238,-35.5062594503621));
#305516=CARTESIAN_POINT('Ctrl Pts',(4.1369915883886,3.00570032696477,-35.418759450362));
#305517=CARTESIAN_POINT('Ctrl Pts',(2.85859088199032,3.93451280799522,-35.3312594503621));
#305518=CARTESIAN_POINT('Ctrl Pts',(1.58019017559203,4.86332528902566,-35.2437594503621));
#305519=CARTESIAN_POINT('Ctrl Pts',(0.,4.86332528902566,-35.1562594503621));
#305520=CARTESIAN_POINT('Ctrl Pts',(-1.58019017559203,4.86332528902566,
-35.0687594503621));
#305521=CARTESIAN_POINT('Ctrl Pts',(-2.85859088199032,3.93451280799522,
-34.9812594503621));
#305522=CARTESIAN_POINT('Ctrl Pts',(-4.1369915883886,3.00570032696477,-34.893759450362));
#305523=CARTESIAN_POINT('Ctrl Pts',(-4.62529720699086,1.50285016348238,
-34.8062594503621));
#305524=CARTESIAN_POINT('Ctrl Pts',(-5.11360282559314,2.48154808763483E-15,
-34.7187594503621));
#305525=CARTESIAN_POINT('Ctrl Pts',(-4.62529720699087,-1.50285016348238,
-34.6312594503621));
#305526=CARTESIAN_POINT('Ctrl Pts',(-4.1369915883886,-3.00570032696476,
-34.5437594503621));
#305527=CARTESIAN_POINT('Ctrl Pts',(-2.85859088199032,-3.93451280799521,
-34.4562594503621));
#305528=CARTESIAN_POINT('Ctrl Pts',(-1.58019017559203,-4.86332528902566,
-34.3687594503621));
#305529=CARTESIAN_POINT('Ctrl Pts',(-5.95585574841766E-16,-4.86332528902566,
-34.2812594503621));
#305530=CARTESIAN_POINT('Ctrl Pts',(1.58019017559203,-4.86332528902566,
-34.1937594503621));
#305531=CARTESIAN_POINT('Ctrl Pts',(2.85859088199031,-3.93451280799521,
-34.1062594503621));
#305532=CARTESIAN_POINT('Ctrl Pts',(4.13699158838859,-3.00570032696476,
-34.0187594503621));
#305533=CARTESIAN_POINT('Ctrl Pts',(4.62529720699086,-1.50285016348238,
-33.9312594503621));
#305534=CARTESIAN_POINT('Ctrl Pts',(5.11360282559314,1.25640155284611E-15,
-33.8437594503621));
#305535=CARTESIAN_POINT('Ctrl Pts',(4.62529720699087,1.50285016348238,-33.7562594503621));
#305536=CARTESIAN_POINT('Ctrl Pts',(4.1369915883886,3.00570032696477,-33.6687594503621));
#305537=CARTESIAN_POINT('Ctrl Pts',(2.85859088199032,3.93451280799522,-33.5812594503621));
#305538=CARTESIAN_POINT('Ctrl Pts',(1.58019017559203,4.86332528902566,-33.4937594503621));
#305539=CARTESIAN_POINT('Ctrl Pts',(0.,4.86332528902566,-33.4062594503621));
#305540=CARTESIAN_POINT('Ctrl Pts',(-1.58019017559203,4.86332528902566,
-33.3187594503621));
#305541=CARTESIAN_POINT('Ctrl Pts',(-2.85859088199032,3.93451280799522,
-33.2312594503621));
#305542=CARTESIAN_POINT('Ctrl Pts',(-4.1369915883886,3.00570032696477,-33.1437594503621));
#305543=CARTESIAN_POINT('Ctrl Pts',(-4.62529720699086,1.50285016348238,
-33.0562594503621));
#305544=CARTESIAN_POINT('Ctrl Pts',(-5.11360282559314,2.53619795104679E-15,
-32.9687594503621));
#305545=CARTESIAN_POINT('Ctrl Pts',(-4.62529720699087,-1.50285016348238,
-32.8812594503621));
#305546=CARTESIAN_POINT('Ctrl Pts',(-4.1369915883886,-3.00570032696476,
-32.7937594503621));
#305547=CARTESIAN_POINT('Ctrl Pts',(-2.85859088199032,-3.93451280799521,
-32.7062594503621));
#305548=CARTESIAN_POINT('Ctrl Pts',(-1.58019017559203,-4.86332528902566,
-32.6187594503621));
#305549=CARTESIAN_POINT('Ctrl Pts',(-5.95585574841766E-16,-4.86332528902566,
-32.5312594503621));
#305550=CARTESIAN_POINT('Ctrl Pts',(1.58019017559203,-4.86332528902566,
-32.4437594503621));
#305551=CARTESIAN_POINT('Ctrl Pts',(2.85859088199031,-3.93451280799521,
-32.3562594503621));
#305552=CARTESIAN_POINT('Ctrl Pts',(4.13699158838859,-3.00570032696476,
-32.2687594503621));
#305553=CARTESIAN_POINT('Ctrl Pts',(4.62529720699086,-1.50285016348238,
-32.1812594503621));
#305554=CARTESIAN_POINT('Ctrl Pts',(5.11360282559314,1.31105141625806E-15,
-32.0937594503621));
#305555=CARTESIAN_POINT('Ctrl Pts',(4.62529720699087,1.50285016348238,-32.0062594503621));
#305556=CARTESIAN_POINT('Ctrl Pts',(4.1369915883886,3.00570032696477,-31.9187594503621));
#305557=CARTESIAN_POINT('Ctrl Pts',(2.85859088199032,3.93451280799522,-31.8312594503621));
#305558=CARTESIAN_POINT('Ctrl Pts',(1.58019017559203,4.86332528902566,-31.7437594503621));
#305559=CARTESIAN_POINT('Ctrl Pts',(0.,4.86332528902566,-31.6562594503621));
#305560=CARTESIAN_POINT('Ctrl Pts',(-1.58019017559203,4.86332528902566,
-31.5687594503621));
#305561=CARTESIAN_POINT('Ctrl Pts',(-2.85859088199032,3.93451280799522,
-31.4812594503621));
#305562=CARTESIAN_POINT('Ctrl Pts',(-4.1369915883886,3.00570032696477,-31.3937594503621));
#305563=CARTESIAN_POINT('Ctrl Pts',(-4.62529720699086,1.50285016348238,
-31.3062594503621));
#305564=CARTESIAN_POINT('Ctrl Pts',(-5.11360282559314,2.59084781445874E-15,
-31.2187594503621));
#305565=CARTESIAN_POINT('Ctrl Pts',(-4.62529720699087,-1.50285016348238,
-31.1312594503621));
#305566=CARTESIAN_POINT('Ctrl Pts',(-4.1369915883886,-3.00570032696476,
-31.0437594503621));
#305567=CARTESIAN_POINT('Ctrl Pts',(-2.85859088199032,-3.93451280799521,
-30.9562594503621));
#305568=CARTESIAN_POINT('Ctrl Pts',(-1.58019017559203,-4.86332528902566,
-30.8687594503621));
#305569=CARTESIAN_POINT('Ctrl Pts',(-5.95585574841766E-16,-4.86332528902566,
-30.7812594503621));
#305570=CARTESIAN_POINT('Ctrl Pts',(1.58019017559203,-4.86332528902566,
-30.6937594503621));
#305571=CARTESIAN_POINT('Ctrl Pts',(2.85859088199031,-3.93451280799521,
-30.6062594503621));
#305572=CARTESIAN_POINT('Ctrl Pts',(4.13699158838859,-3.00570032696476,
-30.5187594503621));
#305573=CARTESIAN_POINT('Ctrl Pts',(4.62529720699086,-1.50285016348238,
-30.4312594503621));
#305574=CARTESIAN_POINT('Ctrl Pts',(5.11360282559314,1.36570127967001E-15,
-30.3437594503621));
#305575=CARTESIAN_POINT('Ctrl Pts',(4.62529720699087,1.50285016348238,-30.2562594503621));
#305576=CARTESIAN_POINT('Ctrl Pts',(4.1369915883886,3.00570032696477,-30.1687594503621));
#305577=CARTESIAN_POINT('Ctrl Pts',(2.85859088199032,3.93451280799522,-30.0812594503621));
#305578=CARTESIAN_POINT('Ctrl Pts',(1.58019017559203,4.86332528902566,-29.9937594503621));
#305579=CARTESIAN_POINT('Ctrl Pts',(0.,4.86332528902566,-29.9062594503621));
#305580=CARTESIAN_POINT('Ctrl Pts',(-1.58019017559203,4.86332528902566,
-29.8187594503621));
#305581=CARTESIAN_POINT('Ctrl Pts',(-2.85859088199032,3.93451280799522,
-29.7312594503621));
#305582=CARTESIAN_POINT('Ctrl Pts',(-4.1369915883886,3.00570032696477,-29.6437594503621));
#305583=CARTESIAN_POINT('Ctrl Pts',(-4.62529720699086,1.50285016348238,
-29.5562594503621));
#305584=CARTESIAN_POINT('Ctrl Pts',(-5.11360282559314,2.64549767787069E-15,
-29.4687594503621));
#305585=CARTESIAN_POINT('Ctrl Pts',(-4.62529720699087,-1.50285016348238,
-29.3812594503621));
#305586=CARTESIAN_POINT('Ctrl Pts',(-4.1369915883886,-3.00570032696476,
-29.2937594503621));
#305587=CARTESIAN_POINT('Ctrl Pts',(-2.85859088199032,-3.93451280799521,
-29.2062594503621));
#305588=CARTESIAN_POINT('Ctrl Pts',(-1.58019017559203,-4.86332528902566,
-29.1187594503621));
#305589=CARTESIAN_POINT('Ctrl Pts',(-5.95585574841766E-16,-4.86332528902566,
-29.0312594503621));
#305590=CARTESIAN_POINT('Ctrl Pts',(1.58019017559203,-4.86332528902566,
-28.9437594503621));
#305591=CARTESIAN_POINT('Ctrl Pts',(2.85859088199031,-3.93451280799521,
-28.8562594503621));
#305592=CARTESIAN_POINT('Ctrl Pts',(4.13699158838859,-3.00570032696476,
-28.7687594503621));
#305593=CARTESIAN_POINT('Ctrl Pts',(4.62529720699086,-1.50285016348238,
-28.6812594503621));
#305594=CARTESIAN_POINT('Ctrl Pts',(5.11360282559314,1.42035114308196E-15,
-28.5937594503621));
#305595=CARTESIAN_POINT('Ctrl Pts',(4.62529720699087,1.50285016348238,-28.5062594503621));
#305596=CARTESIAN_POINT('Ctrl Pts',(4.1369915883886,3.00570032696477,-28.4187594503621));
#305597=CARTESIAN_POINT('Ctrl Pts',(2.85859088199032,3.93451280799522,-28.3312594503621));
#305598=CARTESIAN_POINT('Ctrl Pts',(1.58019017559203,4.86332528902566,-28.2437594503621));
#305599=CARTESIAN_POINT('Ctrl Pts',(0.,4.86332528902566,-28.1562594503621));
#305600=CARTESIAN_POINT('Ctrl Pts',(-1.58019017559203,4.86332528902566,
-28.0687594503621));
#305601=CARTESIAN_POINT('Ctrl Pts',(-2.85859088199032,3.93451280799522,
-27.9812594503621));
#305602=CARTESIAN_POINT('Ctrl Pts',(-4.1369915883886,3.00570032696477,-27.8937594503621));
#305603=CARTESIAN_POINT('Ctrl Pts',(-4.62529720699086,1.50285016348238,
-27.8062594503621));
#305604=CARTESIAN_POINT('Ctrl Pts',(-5.11360282559314,2.70014754128264E-15,
-27.7187594503621));
#305605=CARTESIAN_POINT('Ctrl Pts',(-4.62529720699087,-1.50285016348238,
-27.6312594503621));
#305606=CARTESIAN_POINT('Ctrl Pts',(-4.1369915883886,-3.00570032696476,
-27.5437594503621));
#305607=CARTESIAN_POINT('Ctrl Pts',(-2.85859088199032,-3.93451280799521,
-27.4562594503621));
#305608=CARTESIAN_POINT('Ctrl Pts',(-1.58019017559203,-4.86332528902566,
-27.3687594503621));
#305609=CARTESIAN_POINT('Ctrl Pts',(-5.95585574841766E-16,-4.86332528902566,
-27.2812594503621));
#305610=CARTESIAN_POINT('Ctrl Pts',(1.58019017559203,-4.86332528902566,
-27.1937594503621));
#305611=CARTESIAN_POINT('Ctrl Pts',(2.85859088199031,-3.93451280799521,
-27.1062594503621));
#305612=CARTESIAN_POINT('Ctrl Pts',(4.13699158838859,-3.00570032696476,
-27.0187594503621));
#305613=CARTESIAN_POINT('Ctrl Pts',(4.62529720699086,-1.50285016348238,
-26.9312594503621));
#305614=CARTESIAN_POINT('Ctrl Pts',(5.11360282559314,1.47500100649391E-15,
-26.8437594503621));
#305615=CARTESIAN_POINT('Ctrl Pts',(4.62529720699087,1.50285016348238,-26.7562594503621));
#305616=CARTESIAN_POINT('Ctrl Pts',(4.1369915883886,3.00570032696477,-26.6687594503621));
#305617=CARTESIAN_POINT('Ctrl Pts',(2.85859088199032,3.93451280799522,-26.5812594503621));
#305618=CARTESIAN_POINT('Ctrl Pts',(1.58019017559203,4.86332528902566,-26.4937594503621));
#305619=CARTESIAN_POINT('Ctrl Pts',(0.,4.86332528902566,-26.4062594503621));
#305620=CARTESIAN_POINT('Ctrl Pts',(-1.58019017559203,4.86332528902566,
-26.3187594503621));
#305621=CARTESIAN_POINT('Ctrl Pts',(-2.85859088199032,3.93451280799522,
-26.2312594503621));
#305622=CARTESIAN_POINT('Ctrl Pts',(-4.1369915883886,3.00570032696477,-26.1437594503621));
#305623=CARTESIAN_POINT('Ctrl Pts',(-4.62529720699086,1.50285016348238,
-26.0562594503621));
#305624=CARTESIAN_POINT('Ctrl Pts',(-5.11360282559314,2.75479740469459E-15,
-25.9687594503621));
#305625=CARTESIAN_POINT('Ctrl Pts',(-4.62529720699087,-1.50285016348238,
-25.8812594503621));
#305626=CARTESIAN_POINT('Ctrl Pts',(-4.1369915883886,-3.00570032696476,
-25.7937594503621));
#305627=CARTESIAN_POINT('Ctrl Pts',(-2.85859088199032,-3.93451280799521,
-25.7062594503621));
#305628=CARTESIAN_POINT('Ctrl Pts',(-1.58019017559203,-4.86332528902566,
-25.6187594503621));
#305629=CARTESIAN_POINT('Ctrl Pts',(-5.95585574841766E-16,-4.86332528902566,
-25.5312594503621));
#305630=CARTESIAN_POINT('Ctrl Pts',(1.58019017559203,-4.86332528902566,
-25.4437594503621));
#305631=CARTESIAN_POINT('Ctrl Pts',(2.85859088199031,-3.93451280799521,
-25.3562594503621));
#305632=CARTESIAN_POINT('Ctrl Pts',(4.13699158838859,-3.00570032696476,
-25.2687594503621));
#305633=CARTESIAN_POINT('Ctrl Pts',(4.62529720699086,-1.50285016348238,
-25.1812594503621));
#305634=CARTESIAN_POINT('Ctrl Pts',(5.11360282559314,1.52965086990587E-15,
-25.0937594503621));
#305635=CARTESIAN_POINT('Ctrl Pts',(4.62529720699087,1.50285016348238,-25.0062594503621));
#305636=CARTESIAN_POINT('Ctrl Pts',(4.1369915883886,3.00570032696477,-24.9187594503621));
#305637=CARTESIAN_POINT('Ctrl Pts',(2.85859088199032,3.93451280799522,-24.8312594503621));
#305638=CARTESIAN_POINT('Ctrl Pts',(1.58019017559203,4.86332528902566,-24.7437594503621));
#305639=CARTESIAN_POINT('Ctrl Pts',(0.,4.86332528902566,-24.6562594503621));
#305640=CARTESIAN_POINT('Ctrl Pts',(-1.58019017559203,4.86332528902566,
-24.5687594503621));
#305641=CARTESIAN_POINT('Ctrl Pts',(-2.85859088199032,3.93451280799522,
-24.4812594503621));
#305642=CARTESIAN_POINT('Ctrl Pts',(-4.1369915883886,3.00570032696477,-24.3937594503621));
#305643=CARTESIAN_POINT('Ctrl Pts',(-4.62529720699086,1.50285016348238,
-24.3062594503621));
#305644=CARTESIAN_POINT('Ctrl Pts',(-5.11360282559314,2.80944726810654E-15,
-24.2187594503621));
#305645=CARTESIAN_POINT('Ctrl Pts',(-4.62529720699087,-1.50285016348238,
-24.1312594503621));
#305646=CARTESIAN_POINT('Ctrl Pts',(-4.1369915883886,-3.00570032696476,
-24.0437594503621));
#305647=CARTESIAN_POINT('Ctrl Pts',(-2.85859088199032,-3.93451280799521,
-23.9562594503621));
#305648=CARTESIAN_POINT('Ctrl Pts',(-1.58019017559203,-4.86332528902566,
-23.8687594503621));
#305649=CARTESIAN_POINT('Ctrl Pts',(-5.95585574841766E-16,-4.86332528902566,
-23.7812594503621));
#305650=CARTESIAN_POINT('Ctrl Pts',(1.58019017559203,-4.86332528902566,
-23.6937594503621));
#305651=CARTESIAN_POINT('Ctrl Pts',(2.85859088199031,-3.93451280799521,
-23.6062594503621));
#305652=CARTESIAN_POINT('Ctrl Pts',(4.13699158838859,-3.00570032696476,
-23.5187594503621));
#305653=CARTESIAN_POINT('Ctrl Pts',(4.62529720699086,-1.50285016348238,
-23.4312594503621));
#305654=CARTESIAN_POINT('Ctrl Pts',(5.11360282559314,1.58430073331782E-15,
-23.3437594503621));
#305655=CARTESIAN_POINT('Ctrl Pts',(4.62529720699087,1.50285016348238,-23.2562594503621));
#305656=CARTESIAN_POINT('Ctrl Pts',(4.1369915883886,3.00570032696477,-23.1687594503621));
#305657=CARTESIAN_POINT('Ctrl Pts',(2.85859088199032,3.93451280799522,-23.0812594503621));
#305658=CARTESIAN_POINT('Ctrl Pts',(1.58019017559203,4.86332528902566,-22.9937594503621));
#305659=CARTESIAN_POINT('Ctrl Pts',(0.,4.86332528902566,-22.9062594503621));
#305660=CARTESIAN_POINT('Ctrl Pts',(-1.58019017559203,4.86332528902566,
-22.8187594503621));
#305661=CARTESIAN_POINT('Ctrl Pts',(-2.85859088199032,3.93451280799522,
-22.7312594503621));
#305662=CARTESIAN_POINT('Ctrl Pts',(-4.1369915883886,3.00570032696477,-22.6437594503621));
#305663=CARTESIAN_POINT('Ctrl Pts',(-4.62529720699086,1.50285016348238,
-22.5562594503621));
#305664=CARTESIAN_POINT('Ctrl Pts',(-5.11360282559314,2.86409713151849E-15,
-22.4687594503621));
#305665=CARTESIAN_POINT('Ctrl Pts',(-4.62529720699087,-1.50285016348238,
-22.3812594503621));
#305666=CARTESIAN_POINT('Ctrl Pts',(-4.1369915883886,-3.00570032696476,
-22.2937594503621));
#305667=CARTESIAN_POINT('Ctrl Pts',(-2.85859088199032,-3.93451280799521,
-22.2062594503621));
#305668=CARTESIAN_POINT('Ctrl Pts',(-1.58019017559203,-4.86332528902566,
-22.1187594503621));
#305669=CARTESIAN_POINT('Ctrl Pts',(-5.95585574841766E-16,-4.86332528902566,
-22.0312594503621));
#305670=CARTESIAN_POINT('Ctrl Pts',(1.58019017559203,-4.86332528902566,
-21.9437594503621));
#305671=CARTESIAN_POINT('Ctrl Pts',(2.85859088199031,-3.93451280799521,
-21.8562594503621));
#305672=CARTESIAN_POINT('Ctrl Pts',(4.13699158838859,-3.00570032696476,
-21.7687594503621));
#305673=CARTESIAN_POINT('Ctrl Pts',(4.62529720699086,-1.50285016348238,
-21.6812594503621));
#305674=CARTESIAN_POINT('Ctrl Pts',(5.11360282559314,1.63895059672977E-15,
-21.5937594503621));
#305675=CARTESIAN_POINT('Ctrl Pts',(4.62529720699087,1.50285016348238,-21.5062594503621));
#305676=CARTESIAN_POINT('Ctrl Pts',(4.1369915883886,3.00570032696477,-21.4187594503621));
#305677=CARTESIAN_POINT('Ctrl Pts',(2.85859088199032,3.93451280799522,-21.3312594503621));
#305678=CARTESIAN_POINT('Ctrl Pts',(1.58019017559203,4.86332528902566,-21.2437594503621));
#305679=CARTESIAN_POINT('Ctrl Pts',(0.,4.86332528902566,-21.1562594503621));
#305680=CARTESIAN_POINT('Ctrl Pts',(-1.58019017559203,4.86332528902566,
-21.0687594503621));
#305681=CARTESIAN_POINT('Ctrl Pts',(-2.85859088199032,3.93451280799522,
-20.9812594503621));
#305682=CARTESIAN_POINT('Ctrl Pts',(-4.1369915883886,3.00570032696477,-20.8937594503621));
#305683=CARTESIAN_POINT('Ctrl Pts',(-4.62529720699086,1.50285016348238,
-20.8062594503621));
#305684=CARTESIAN_POINT('Ctrl Pts',(-5.11360282559314,2.91874699493044E-15,
-20.7187594503621));
#305685=CARTESIAN_POINT('Ctrl Pts',(-4.62529720699087,-1.50285016348238,
-20.6312594503621));
#305686=CARTESIAN_POINT('Ctrl Pts',(-4.1369915883886,-3.00570032696476,
-20.5437594503621));
#305687=CARTESIAN_POINT('Ctrl Pts',(-2.85859088199032,-3.93451280799521,
-20.4562594503621));
#305688=CARTESIAN_POINT('Ctrl Pts',(-1.58019017559203,-4.86332528902566,
-20.3687594503621));
#305689=CARTESIAN_POINT('Ctrl Pts',(-5.95585574841766E-16,-4.86332528902566,
-20.2812594503621));
#305690=CARTESIAN_POINT('Ctrl Pts',(1.58019017559203,-4.86332528902566,
-20.1937594503621));
#305691=CARTESIAN_POINT('Ctrl Pts',(2.85859088199031,-3.93451280799521,
-20.1062594503621));
#305692=CARTESIAN_POINT('Ctrl Pts',(4.13699158838859,-3.00570032696476,
-20.0187594503621));
#305693=CARTESIAN_POINT('Ctrl Pts',(4.62529720699086,-1.50285016348238,
-19.9312594503621));
#305694=CARTESIAN_POINT('Ctrl Pts',(5.11360282559314,1.69360046014172E-15,
-19.8437594503621));
#305695=CARTESIAN_POINT('Ctrl Pts',(4.62529720699087,1.50285016348238,-19.7562594503621));
#305696=CARTESIAN_POINT('Ctrl Pts',(4.1369915883886,3.00570032696477,-19.6687594503621));
#305697=CARTESIAN_POINT('Ctrl Pts',(2.85859088199032,3.93451280799522,-19.5812594503621));
#305698=CARTESIAN_POINT('Ctrl Pts',(1.58019017559203,4.86332528902566,-19.4937594503621));
#305699=CARTESIAN_POINT('Ctrl Pts',(0.,4.86332528902566,-19.4062594503621));
#305700=CARTESIAN_POINT('Ctrl Pts',(-1.58019017559203,4.86332528902566,
-19.3187594503621));
#305701=CARTESIAN_POINT('Ctrl Pts',(-2.85859088199032,3.93451280799522,
-19.2312594503621));
#305702=CARTESIAN_POINT('Ctrl Pts',(-4.1369915883886,3.00570032696477,-19.1437594503621));
#305703=CARTESIAN_POINT('Ctrl Pts',(-4.62529720699086,1.50285016348238,
-19.0562594503621));
#305704=CARTESIAN_POINT('Ctrl Pts',(-5.11360282559314,2.97339685834239E-15,
-18.9687594503621));
#305705=CARTESIAN_POINT('Ctrl Pts',(-4.62529720699087,-1.50285016348238,
-18.8812594503621));
#305706=CARTESIAN_POINT('Ctrl Pts',(-4.1369915883886,-3.00570032696476,
-18.7937594503621));
#305707=CARTESIAN_POINT('Ctrl Pts',(-2.85859088199032,-3.93451280799521,
-18.7062594503621));
#305708=CARTESIAN_POINT('Ctrl Pts',(-1.58019017559203,-4.86332528902566,
-18.6187594503621));
#305709=CARTESIAN_POINT('Ctrl Pts',(-5.95585574841766E-16,-4.86332528902566,
-18.5312594503621));
#305710=CARTESIAN_POINT('Ctrl Pts',(1.58019017559203,-4.86332528902566,
-18.4437594503621));
#305711=CARTESIAN_POINT('Ctrl Pts',(2.85859088199031,-3.93451280799521,
-18.3562594503621));
#305712=CARTESIAN_POINT('Ctrl Pts',(4.13699158838859,-3.00570032696476,
-18.2687594503621));
#305713=CARTESIAN_POINT('Ctrl Pts',(4.62529720699086,-1.50285016348238,
-18.1812594503621));
#305714=CARTESIAN_POINT('Ctrl Pts',(5.11360282559314,1.74825032355367E-15,
-18.0937594503621));
#305715=CARTESIAN_POINT('Ctrl Pts',(4.62529720699087,1.50285016348238,-18.0062594503621));
#305716=CARTESIAN_POINT('Ctrl Pts',(4.1369915883886,3.00570032696477,-17.9187594503621));
#305717=CARTESIAN_POINT('Ctrl Pts',(2.85859088199032,3.93451280799522,-17.8312594503621));
#305718=CARTESIAN_POINT('Ctrl Pts',(1.58019017559203,4.86332528902566,-17.7437594503621));
#305719=CARTESIAN_POINT('Ctrl Pts',(0.,4.86332528902566,-17.6562594503621));
#305720=CARTESIAN_POINT('Ctrl Pts',(-1.58019017559203,4.86332528902566,
-17.5687594503621));
#305721=CARTESIAN_POINT('Ctrl Pts',(-2.85859088199032,3.93451280799522,
-17.4812594503621));
#305722=CARTESIAN_POINT('Ctrl Pts',(-4.1369915883886,3.00570032696477,-17.3937594503621));
#305723=CARTESIAN_POINT('Ctrl Pts',(-4.62529720699086,1.50285016348238,
-17.3062594503621));
#305724=CARTESIAN_POINT('Ctrl Pts',(-5.11360282559314,3.02804672175434E-15,
-17.2187594503621));
#305725=CARTESIAN_POINT('Ctrl Pts',(-4.62529720699087,-1.50285016348238,
-17.1312594503621));
#305726=CARTESIAN_POINT('Ctrl Pts',(-4.1369915883886,-3.00570032696476,
-17.0437594503621));
#305727=CARTESIAN_POINT('Ctrl Pts',(-2.85859088199032,-3.93451280799521,
-16.9562594503621));
#305728=CARTESIAN_POINT('Ctrl Pts',(-1.58019017559203,-4.86332528902566,
-16.8687594503621));
#305729=CARTESIAN_POINT('Ctrl Pts',(-5.95585574841766E-16,-4.86332528902566,
-16.7812594503621));
#305730=CARTESIAN_POINT('Ctrl Pts',(1.58019017559203,-4.86332528902566,
-16.6937594503621));
#305731=CARTESIAN_POINT('Ctrl Pts',(2.85859088199031,-3.93451280799521,
-16.6062594503621));
#305732=CARTESIAN_POINT('Ctrl Pts',(4.13699158838859,-3.00570032696476,
-16.5187594503621));
#305733=CARTESIAN_POINT('Ctrl Pts',(4.62529720699086,-1.50285016348238,
-16.4312594503621));
#305734=CARTESIAN_POINT('Ctrl Pts',(5.11360282559314,1.80290018696562E-15,
-16.3437594503621));
#305735=CARTESIAN_POINT('Ctrl Pts',(4.62529720699087,1.50285016348238,-16.2562594503621));
#305736=CARTESIAN_POINT('Ctrl Pts',(4.1369915883886,3.00570032696477,-16.1687594503621));
#305737=CARTESIAN_POINT('Ctrl Pts',(2.85859088199032,3.93451280799522,-16.0812594503621));
#305738=CARTESIAN_POINT('Ctrl Pts',(1.58019017559203,4.86332528902566,-15.9937594503621));
#305739=CARTESIAN_POINT('Ctrl Pts',(0.,4.86332528902566,-15.9062594503621));
#305740=CARTESIAN_POINT('Ctrl Pts',(-1.58019017559203,4.86332528902566,
-15.8187594503621));
#305741=CARTESIAN_POINT('Ctrl Pts',(-2.85859088199032,3.93451280799522,
-15.7312594503621));
#305742=CARTESIAN_POINT('Ctrl Pts',(-4.1369915883886,3.00570032696477,-15.6437594503621));
#305743=CARTESIAN_POINT('Ctrl Pts',(-4.62529720699086,1.50285016348238,
-15.5562594503621));
#305744=CARTESIAN_POINT('Ctrl Pts',(-5.11360282559314,3.08269658516629E-15,
-15.4687594503621));
#305745=CARTESIAN_POINT('Ctrl Pts',(-4.62529720699087,-1.50285016348238,
-15.3812594503621));
#305746=CARTESIAN_POINT('Ctrl Pts',(-4.1369915883886,-3.00570032696476,
-15.2937594503621));
#305747=CARTESIAN_POINT('Ctrl Pts',(-2.85859088199032,-3.93451280799521,
-15.2062594503621));
#305748=CARTESIAN_POINT('Ctrl Pts',(-1.58019017559203,-4.86332528902566,
-15.1187594503621));
#305749=CARTESIAN_POINT('Ctrl Pts',(-5.95585574841766E-16,-4.86332528902566,
-15.0312594503621));
#305750=CARTESIAN_POINT('Ctrl Pts',(1.58019017559203,-4.86332528902566,
-14.9437594503621));
#305751=CARTESIAN_POINT('Ctrl Pts',(2.85859088199031,-3.93451280799521,
-14.8562594503621));
#305752=CARTESIAN_POINT('Ctrl Pts',(4.13699158838859,-3.00570032696476,
-14.7687594503621));
#305753=CARTESIAN_POINT('Ctrl Pts',(4.62529720699086,-1.50285016348238,
-14.6812594503621));
#305754=CARTESIAN_POINT('Ctrl Pts',(5.11360282559314,1.85755005037757E-15,
-14.5937594503621));
#305755=CARTESIAN_POINT('Ctrl Pts',(4.62529720699087,1.50285016348238,-14.5062594503621));
#305756=CARTESIAN_POINT('Ctrl Pts',(4.1369915883886,3.00570032696477,-14.4187594503621));
#305757=CARTESIAN_POINT('Ctrl Pts',(2.85859088199032,3.93451280799522,-14.3312594503621));
#305758=CARTESIAN_POINT('Ctrl Pts',(1.58019017559203,4.86332528902566,-14.2437594503621));
#305759=CARTESIAN_POINT('Ctrl Pts',(0.,4.86332528902566,-14.1562594503621));
#305760=CARTESIAN_POINT('Ctrl Pts',(-1.58019017559203,4.86332528902566,
-14.0687594503621));
#305761=CARTESIAN_POINT('Ctrl Pts',(-2.85859088199032,3.93451280799522,
-13.9812594503621));
#305762=CARTESIAN_POINT('Ctrl Pts',(-4.1369915883886,3.00570032696477,-13.8937594503621));
#305763=CARTESIAN_POINT('Ctrl Pts',(-4.62529720699086,1.50285016348238,
-13.8062594503621));
#305764=CARTESIAN_POINT('Ctrl Pts',(-5.11360282559314,3.13734644857824E-15,
-13.7187594503621));
#305765=CARTESIAN_POINT('Ctrl Pts',(-4.62529720699087,-1.50285016348238,
-13.6312594503621));
#305766=CARTESIAN_POINT('Ctrl Pts',(-4.1369915883886,-3.00570032696476,
-13.5437594503621));
#305767=CARTESIAN_POINT('Ctrl Pts',(-2.85859088199032,-3.93451280799521,
-13.4562594503621));
#305768=CARTESIAN_POINT('Ctrl Pts',(-1.58019017559203,-4.86332528902566,
-13.3687594503621));
#305769=CARTESIAN_POINT('Ctrl Pts',(-5.95585574841766E-16,-4.86332528902566,
-13.2812594503621));
#305770=CARTESIAN_POINT('Ctrl Pts',(1.58019017559203,-4.86332528902566,
-13.1937594503621));
#305771=CARTESIAN_POINT('Ctrl Pts',(2.85859088199031,-3.93451280799521,
-13.1062594503621));
#305772=CARTESIAN_POINT('Ctrl Pts',(4.13699158838859,-3.00570032696476,
-13.0187594503621));
#305773=CARTESIAN_POINT('Ctrl Pts',(4.62529720699086,-1.50285016348238,
-12.9312594503621));
#305774=CARTESIAN_POINT('Ctrl Pts',(5.11360282559314,1.91219991378952E-15,
-12.8437594503621));
#305775=CARTESIAN_POINT('Ctrl Pts',(4.62529720699087,1.50285016348238,-12.7562594503621));
#305776=CARTESIAN_POINT('Ctrl Pts',(4.1369915883886,3.00570032696477,-12.6687594503621));
#305777=CARTESIAN_POINT('Ctrl Pts',(2.85859088199032,3.93451280799522,-12.5812594503621));
#305778=CARTESIAN_POINT('Ctrl Pts',(1.58019017559203,4.86332528902566,-12.4937594503621));
#305779=CARTESIAN_POINT('Ctrl Pts',(0.,4.86332528902566,-12.4062594503621));
#305780=CARTESIAN_POINT('Ctrl Pts',(-1.58019017559203,4.86332528902566,
-12.3187594503621));
#305781=CARTESIAN_POINT('Ctrl Pts',(-2.85859088199032,3.93451280799522,
-12.2312594503621));
#305782=CARTESIAN_POINT('Ctrl Pts',(-4.1369915883886,3.00570032696477,-12.1437594503621));
#305783=CARTESIAN_POINT('Ctrl Pts',(-4.62529720699086,1.50285016348238,
-12.0562594503621));
#305784=CARTESIAN_POINT('Ctrl Pts',(-5.11360282559314,3.1919963119902E-15,
-11.9687594503621));
#305785=CARTESIAN_POINT('Ctrl Pts',(-4.62529720699087,-1.50285016348238,
-11.8812594503621));
#305786=CARTESIAN_POINT('Ctrl Pts',(-4.1369915883886,-3.00570032696476,
-11.7937594503621));
#305787=CARTESIAN_POINT('Ctrl Pts',(-2.85859088199032,-3.93451280799521,
-11.7062594503621));
#305788=CARTESIAN_POINT('Ctrl Pts',(-1.58019017559203,-4.86332528902566,
-11.6187594503621));
#305789=CARTESIAN_POINT('Ctrl Pts',(-5.95585574841766E-16,-4.86332528902566,
-11.5312594503621));
#305790=CARTESIAN_POINT('Ctrl Pts',(1.58019017559203,-4.86332528902566,
-11.4437594503621));
#305791=CARTESIAN_POINT('Ctrl Pts',(2.85859088199031,-3.93451280799521,
-11.3562594503621));
#305792=CARTESIAN_POINT('Ctrl Pts',(4.13699158838859,-3.00570032696476,
-11.2687594503621));
#305793=CARTESIAN_POINT('Ctrl Pts',(4.62529720699086,-1.50285016348238,
-11.1812594503621));
#305794=CARTESIAN_POINT('Ctrl Pts',(5.11360282559314,1.96684977720147E-15,
-11.0937594503621));
#305795=CARTESIAN_POINT('Ctrl Pts',(4.62529720699087,1.50285016348238,-11.0062594503621));
#305796=CARTESIAN_POINT('Ctrl Pts',(4.1369915883886,3.00570032696477,-10.9187594503621));
#305797=CARTESIAN_POINT('Ctrl Pts',(2.85859088199032,3.93451280799522,-10.8312594503621));
#305798=CARTESIAN_POINT('Ctrl Pts',(1.58019017559203,4.86332528902566,-10.7437594503621));
#305799=CARTESIAN_POINT('Ctrl Pts',(0.,4.86332528902566,-10.6562594503621));
#305800=CARTESIAN_POINT('Ctrl Pts',(-1.58019017559203,4.86332528902566,
-10.5687594503621));
#305801=CARTESIAN_POINT('Ctrl Pts',(-2.85859088199032,3.93451280799522,
-10.4812594503621));
#305802=CARTESIAN_POINT('Ctrl Pts',(-4.1369915883886,3.00570032696477,-10.3937594503621));
#305803=CARTESIAN_POINT('Ctrl Pts',(-4.62529720699086,1.50285016348238,
-10.3062594503621));
#305804=CARTESIAN_POINT('Ctrl Pts',(-5.11360282559314,3.24664617540214E-15,
-10.2187594503621));
#305805=CARTESIAN_POINT('Ctrl Pts',(-4.62529720699087,-1.50285016348238,
-10.1312594503621));
#305806=CARTESIAN_POINT('Ctrl Pts',(-4.1369915883886,-3.00570032696476,
-10.0437594503621));
#305807=CARTESIAN_POINT('Ctrl Pts',(-2.85859088199032,-3.93451280799521,
-9.95625945036208));
#305808=CARTESIAN_POINT('Ctrl Pts',(-1.58019017559203,-4.86332528902566,
-9.86875945036208));
#305809=CARTESIAN_POINT('Ctrl Pts',(-5.95585574841766E-16,-4.86332528902566,
-9.78125945036208));
#305810=CARTESIAN_POINT('Ctrl Pts',(1.58019017559203,-4.86332528902566,
-9.69375945036209));
#305811=CARTESIAN_POINT('Ctrl Pts',(2.85859088199031,-3.93451280799521,
-9.60625945036209));
#305812=CARTESIAN_POINT('Ctrl Pts',(4.13699158838859,-3.00570032696476,
-9.51875945036208));
#305813=CARTESIAN_POINT('Ctrl Pts',(4.62529720699086,-1.50285016348238,
-9.43125945036208));
#305814=CARTESIAN_POINT('Ctrl Pts',(5.11360282559314,2.02149964061342E-15,
-9.34375945036209));
#305815=CARTESIAN_POINT('Ctrl Pts',(4.62529720699087,1.50285016348238,-9.25625945036208));
#305816=CARTESIAN_POINT('Ctrl Pts',(4.1369915883886,3.00570032696477,-9.16875945036209));
#305817=CARTESIAN_POINT('Ctrl Pts',(2.85859088199032,3.93451280799522,-9.08125945036208));
#305818=CARTESIAN_POINT('Ctrl Pts',(1.58019017559203,4.86332528902566,-8.99375945036209));
#305819=CARTESIAN_POINT('Ctrl Pts',(0.,4.86332528902566,-8.90625945036208));
#305820=CARTESIAN_POINT('Ctrl Pts',(-1.58019017559203,4.86332528902566,
-8.81875945036208));
#305821=CARTESIAN_POINT('Ctrl Pts',(-2.85859088199032,3.93451280799522,
-8.73125945036208));
#305822=CARTESIAN_POINT('Ctrl Pts',(-4.1369915883886,3.00570032696477,-8.64375945036208));
#305823=CARTESIAN_POINT('Ctrl Pts',(-4.62529720699086,1.50285016348238,
-8.55625945036208));
#305824=CARTESIAN_POINT('Ctrl Pts',(-5.11360282559314,3.3012960388141E-15,
-8.46875945036209));
#305825=CARTESIAN_POINT('Ctrl Pts',(-4.62529720699087,-1.50285016348238,
-8.38125945036208));
#305826=CARTESIAN_POINT('Ctrl Pts',(-4.1369915883886,-3.00570032696476,
-8.29375945036209));
#305827=CARTESIAN_POINT('Ctrl Pts',(-2.85859088199032,-3.93451280799521,
-8.20625945036208));
#305828=CARTESIAN_POINT('Ctrl Pts',(-1.58019017559203,-4.86332528902566,
-8.11875945036208));
#305829=CARTESIAN_POINT('Ctrl Pts',(-5.95585574841766E-16,-4.86332528902566,
-8.03125945036208));
#305830=CARTESIAN_POINT('Ctrl Pts',(1.58019017559203,-4.86332528902566,
-7.94375945036208));
#305831=CARTESIAN_POINT('Ctrl Pts',(2.85859088199031,-3.93451280799521,
-7.85625945036208));
#305832=CARTESIAN_POINT('Ctrl Pts',(4.13699158838859,-3.00570032696476,
-7.76875945036209));
#305833=CARTESIAN_POINT('Ctrl Pts',(4.62529720699086,-1.50285016348238,
-7.68125945036208));
#305834=CARTESIAN_POINT('Ctrl Pts',(5.11360282559314,2.07614950402537E-15,
-7.59375945036209));
#305835=CARTESIAN_POINT('Ctrl Pts',(4.62529720699087,1.50285016348238,-7.50625945036208));
#305836=CARTESIAN_POINT('Ctrl Pts',(4.1369915883886,3.00570032696477,-7.41875945036209));
#305837=CARTESIAN_POINT('Ctrl Pts',(2.85859088199032,3.93451280799522,-7.33125945036208));
#305838=CARTESIAN_POINT('Ctrl Pts',(1.58019017559203,4.86332528902566,-7.24375945036208));
#305839=CARTESIAN_POINT('Ctrl Pts',(0.,4.86332528902566,-7.15625945036208));
#305840=CARTESIAN_POINT('Ctrl Pts',(-1.58019017559203,4.86332528902566,
-7.06875945036209));
#305841=CARTESIAN_POINT('Ctrl Pts',(-2.85859088199032,3.93451280799522,
-6.98125945036208));
#305842=CARTESIAN_POINT('Ctrl Pts',(-4.1369915883886,3.00570032696477,-6.89375945036209));
#305843=CARTESIAN_POINT('Ctrl Pts',(-4.62529720699086,1.50285016348238,
-6.80625945036208));
#305844=CARTESIAN_POINT('Ctrl Pts',(-5.11360282559314,3.35594590222605E-15,
-6.71875945036209));
#305845=CARTESIAN_POINT('Ctrl Pts',(-4.62529720699087,-1.50285016348238,
-6.63125945036208));
#305846=CARTESIAN_POINT('Ctrl Pts',(-4.1369915883886,-3.00570032696476,
-6.54375945036209));
#305847=CARTESIAN_POINT('Ctrl Pts',(-2.85859088199032,-3.93451280799521,
-6.45625945036208));
#305848=CARTESIAN_POINT('Ctrl Pts',(-1.58019017559203,-4.86332528902566,
-6.36875945036209));
#305849=CARTESIAN_POINT('Ctrl Pts',(-5.95585574841766E-16,-4.86332528902566,
-6.28125945036208));
#305850=CARTESIAN_POINT('Ctrl Pts',(1.58019017559203,-4.86332528902566,
-6.19375945036209));
#305851=CARTESIAN_POINT('Ctrl Pts',(2.85859088199031,-3.93451280799521,
-6.10625945036208));
#305852=CARTESIAN_POINT('Ctrl Pts',(4.13699158838859,-3.00570032696476,
-6.0187594503621));
#305853=CARTESIAN_POINT('Ctrl Pts',(4.62529720699086,-1.50285016348238,
-5.93125945036208));
#305854=CARTESIAN_POINT('Ctrl Pts',(5.11360282559314,2.13079936743733E-15,
-5.84375945036209));
#305855=CARTESIAN_POINT('Ctrl Pts',(4.62529720699087,1.50285016348238,-5.75625945036208));
#305856=CARTESIAN_POINT('Ctrl Pts',(4.1369915883886,3.00570032696477,-5.66875945036209));
#305857=CARTESIAN_POINT('Ctrl Pts',(2.85859088199032,3.93451280799522,-5.58125945036208));
#305858=CARTESIAN_POINT('Ctrl Pts',(1.58019017559203,4.86332528902566,-5.49375945036209));
#305859=CARTESIAN_POINT('Ctrl Pts',(0.,4.86332528902566,-5.40625945036208));
#305860=CARTESIAN_POINT('Ctrl Pts',(-1.58019017559203,4.86332528902566,
-5.31875945036209));
#305861=CARTESIAN_POINT('Ctrl Pts',(-2.85859088199032,3.93451280799522,
-5.23125945036208));
#305862=CARTESIAN_POINT('Ctrl Pts',(-3.3915599562443,3.54728810943805,-5.19478043891927));
#305863=CARTESIAN_POINT('Ctrl Pts',(-3.80230551497385,3.03222783406459,
-5.15646275598973));
#305864=CARTESIAN_POINT('Ctrl Pts',(-7.36910532594948E-14,6.00000000000001,
-6.50000000000001));
#305865=CARTESIAN_POINT('Ctrl Pts',(0.695536090209394,6.00000000000002,
-6.53121766629259));
#305866=CARTESIAN_POINT('Ctrl Pts',(1.38641832502867,5.87905710063626,-6.563990204745));
#305867=CARTESIAN_POINT('Ctrl Pts',(2.77639380398129,5.37608234738622,-6.63371136268937));
#305868=CARTESIAN_POINT('Ctrl Pts',(3.45221402618498,4.96919013454356,-6.66853947573316));
#305869=CARTESIAN_POINT('Ctrl Pts',(4.61350745859033,3.91586257612663,-6.74096845709073));
#305870=CARTESIAN_POINT('Ctrl Pts',(5.08648051138953,3.27813009530638,-6.77843673756609));
#305871=CARTESIAN_POINT('Ctrl Pts',(5.75390094257317,1.86835407146478,-6.85077518450608));
#305872=CARTESIAN_POINT('Ctrl Pts',(5.94657177527691,1.11193156507019,-6.88502499392445));
#305873=CARTESIAN_POINT('Ctrl Pts',(6.03524834172125,-0.45136365758525,
-6.95880105072841));
#305874=CARTESIAN_POINT('Ctrl Pts',(5.9229448545129,-1.24358642710857,-6.99568226363595));
#305875=CARTESIAN_POINT('Ctrl Pts',(5.40125880336164,-2.72662372932836,
-7.06677525385319));
#305876=CARTESIAN_POINT('Ctrl Pts',(5.00156711282546,-3.40474766259226,
-7.10375290376194));
#305877=CARTESIAN_POINT('Ctrl Pts',(3.96750118999664,-4.56744311065716,
-7.17682833144899));
#305878=CARTESIAN_POINT('Ctrl Pts',(3.34393241019509,-5.04189722999588,
-7.21094233439999));
#305879=CARTESIAN_POINT('Ctrl Pts',(1.93705624242696,-5.73360223580846,
-7.28417436019869));
#305880=CARTESIAN_POINT('Ctrl Pts',(1.16467505775192,-5.93885250963874,
-7.32183428918265));
#305881=CARTESIAN_POINT('Ctrl Pts',(-0.398071677820406,-6.03664804127998,
-7.39340105590642));
#305882=CARTESIAN_POINT('Ctrl Pts',(-1.17301020650276,-5.93495392183099,
-7.42859667074508));
#305883=CARTESIAN_POINT('Ctrl Pts',(-2.65044753997004,-5.43963450410889,
-7.50213172873049));
#305884=CARTESIAN_POINT('Ctrl Pts',(-3.33769715417903,-5.04720323133648,
-7.53738436153389));
#305885=CARTESIAN_POINT('Ctrl Pts',(-4.5229067872758,-4.01981977607675,
-7.60948622083326));
#305886=CARTESIAN_POINT('Ctrl Pts',(-5.00925311469169,-3.39455260229493,
-7.64684954334406));
#305887=CARTESIAN_POINT('Ctrl Pts',(-5.708787772007,-2.00208695227552,-7.71941790734077));
#305888=CARTESIAN_POINT('Ctrl Pts',(-5.91911839235579,-1.25005304156578,
-7.75350667432105));
#305889=CARTESIAN_POINT('Ctrl Pts',(-6.0443882583849,0.31463515188788,-7.82734846911949));
#305890=CARTESIAN_POINT('Ctrl Pts',(-5.94937536630207,1.11278518743067,
-7.86495515658336));
#305891=CARTESIAN_POINT('Ctrl Pts',(-5.45907891653994,2.6084356620542,-7.93565899265305));
#305892=CARTESIAN_POINT('Ctrl Pts',(-5.07516282202342,3.29364355428696,
-7.97246950412426));
#305893=CARTESIAN_POINT('Ctrl Pts',(-4.06741694281494,4.47895159391096,
-8.04567817732591));
#305894=CARTESIAN_POINT('Ctrl Pts',(-3.45321844823359,4.96791566333691,
-8.07995836388455));
#305895=CARTESIAN_POINT('Ctrl Pts',(-2.06182138758084,5.68968624537131,
-8.15293409901987));
#305896=CARTESIAN_POINT('Ctrl Pts',(-1.29586495890513,5.91137919559933,
-8.19054545545049));
#305897=CARTESIAN_POINT('Ctrl Pts',(-0.339438395925482,5.99280698755147,
-8.23466012744105));
#305898=CARTESIAN_POINT('Ctrl Pts',(-0.169625758311113,6.,-8.24238670661075));
#305899=CARTESIAN_POINT('Ctrl Pts',(-2.33459085396959E-13,6.00000000000001,
-8.25));
#305900=CARTESIAN_POINT('Ctrl Pts',(-0.75570415697393,-4.80426927898796,
-36.0741583424671));
#305901=CARTESIAN_POINT('Ctrl Pts',(-0.380160882715947,-4.86334165753294,
-36.0523006088412));
#305902=CARTESIAN_POINT('Ctrl Pts',(-5.9558757940577E-16,-4.86334165753294,
-36.03125));
#305903=CARTESIAN_POINT('Ctrl Pts',(0.,4.86333050978515,-37.1249935638448));
#305904=CARTESIAN_POINT('Ctrl Pts',(-1.58019187191962,4.86333050978515,
-37.0374935638448));
#305905=CARTESIAN_POINT('Ctrl Pts',(-2.85859395067575,3.93451703167837,
-36.9499935638448));
#305906=CARTESIAN_POINT('Ctrl Pts',(-4.13699602943188,3.00570355357158,
-36.8624935638448));
#305907=CARTESIAN_POINT('Ctrl Pts',(-4.6253021722282,1.50285177678579,-36.7749935638448));
#305908=CARTESIAN_POINT('Ctrl Pts',(-5.11360831502452,2.42006782353912E-15,
-36.6874935638448));
#305909=CARTESIAN_POINT('Ctrl Pts',(-4.6253021722282,-1.50285177678579,
-36.5999935638448));
#305910=CARTESIAN_POINT('Ctrl Pts',(-4.13699602943188,-3.00570355357157,
-36.5124935638448));
#305911=CARTESIAN_POINT('Ctrl Pts',(-2.85859395067575,-3.93451703167836,
-36.4249935638448));
#305912=CARTESIAN_POINT('Ctrl Pts',(-1.58019187191962,-4.86333050978515,
-36.3374935638448));
#305913=CARTESIAN_POINT('Ctrl Pts',(-5.95586214200406E-16,-4.86333050978515,
-36.2499935638448));
#305914=CARTESIAN_POINT('Ctrl Pts',(1.58019187191962,-4.86333050978515,
-36.1624935638448));
#305915=CARTESIAN_POINT('Ctrl Pts',(2.85859395067575,-3.93451703167836,
-36.0749935638448));
#305916=CARTESIAN_POINT('Ctrl Pts',(4.13699602943187,-3.00570355357157,
-35.9874935638448));
#305917=CARTESIAN_POINT('Ctrl Pts',(4.6253021722282,-1.50285177678579,-35.8999935638448));
#305918=CARTESIAN_POINT('Ctrl Pts',(5.11360831502452,1.19491994422748E-15,
-35.8124935638448));
#305919=CARTESIAN_POINT('Ctrl Pts',(4.6253021722282,1.50285177678579,-35.7249935638448));
#305920=CARTESIAN_POINT('Ctrl Pts',(4.13699602943188,3.00570355357158,-35.6374935638448));
#305921=CARTESIAN_POINT('Ctrl Pts',(2.85859395067575,3.93451703167837,-35.5499935638448));
#305922=CARTESIAN_POINT('Ctrl Pts',(1.58019187191962,4.86333050978515,-35.4624935638448));
#305923=CARTESIAN_POINT('Ctrl Pts',(0.,4.86333050978515,-35.3749935638448));
#305924=CARTESIAN_POINT('Ctrl Pts',(-1.58019187191962,4.86333050978515,
-35.2874935638448));
#305925=CARTESIAN_POINT('Ctrl Pts',(-2.85859395067575,3.93451703167837,
-35.1999935638448));
#305926=CARTESIAN_POINT('Ctrl Pts',(-4.13699602943188,3.00570355357158,
-35.1124935638448));
#305927=CARTESIAN_POINT('Ctrl Pts',(-4.6253021722282,1.50285177678579,-35.0249935638448));
#305928=CARTESIAN_POINT('Ctrl Pts',(-5.11360831502452,2.47471768695107E-15,
-34.9374935638448));
#305929=CARTESIAN_POINT('Ctrl Pts',(-4.6253021722282,-1.50285177678579,
-34.8499935638448));
#305930=CARTESIAN_POINT('Ctrl Pts',(-4.13699602943188,-3.00570355357157,
-34.7624935638448));
#305931=CARTESIAN_POINT('Ctrl Pts',(-2.85859395067575,-3.93451703167836,
-34.6749935638448));
#305932=CARTESIAN_POINT('Ctrl Pts',(-1.58019187191962,-4.86333050978515,
-34.5874935638448));
#305933=CARTESIAN_POINT('Ctrl Pts',(-5.95586214200406E-16,-4.86333050978515,
-34.4999935638448));
#305934=CARTESIAN_POINT('Ctrl Pts',(1.58019187191962,-4.86333050978515,
-34.4124935638448));
#305935=CARTESIAN_POINT('Ctrl Pts',(2.85859395067575,-3.93451703167836,
-34.3249935638448));
#305936=CARTESIAN_POINT('Ctrl Pts',(4.13699602943187,-3.00570355357157,
-34.2374935638448));
#305937=CARTESIAN_POINT('Ctrl Pts',(4.6253021722282,-1.50285177678579,-34.1499935638448));
#305938=CARTESIAN_POINT('Ctrl Pts',(5.11360831502452,1.24956980763943E-15,
-34.0624935638448));
#305939=CARTESIAN_POINT('Ctrl Pts',(4.6253021722282,1.50285177678579,-33.9749935638448));
#305940=CARTESIAN_POINT('Ctrl Pts',(4.13699602943188,3.00570355357158,-33.8874935638448));
#305941=CARTESIAN_POINT('Ctrl Pts',(2.85859395067575,3.93451703167837,-33.7999935638448));
#305942=CARTESIAN_POINT('Ctrl Pts',(1.58019187191962,4.86333050978515,-33.7124935638448));
#305943=CARTESIAN_POINT('Ctrl Pts',(0.,4.86333050978515,-33.6249935638448));
#305944=CARTESIAN_POINT('Ctrl Pts',(-1.58019187191962,4.86333050978515,
-33.5374935638448));
#305945=CARTESIAN_POINT('Ctrl Pts',(-2.85859395067575,3.93451703167837,
-33.4499935638448));
#305946=CARTESIAN_POINT('Ctrl Pts',(-4.13699602943188,3.00570355357158,
-33.3624935638448));
#305947=CARTESIAN_POINT('Ctrl Pts',(-4.6253021722282,1.50285177678579,-33.2749935638448));
#305948=CARTESIAN_POINT('Ctrl Pts',(-5.11360831502452,2.52936755036302E-15,
-33.1874935638448));
#305949=CARTESIAN_POINT('Ctrl Pts',(-4.6253021722282,-1.50285177678579,
-33.0999935638448));
#305950=CARTESIAN_POINT('Ctrl Pts',(-4.13699602943188,-3.00570355357157,
-33.0124935638448));
#305951=CARTESIAN_POINT('Ctrl Pts',(-2.85859395067575,-3.93451703167836,
-32.9249935638448));
#305952=CARTESIAN_POINT('Ctrl Pts',(-1.58019187191962,-4.86333050978515,
-32.8374935638448));
#305953=CARTESIAN_POINT('Ctrl Pts',(-5.95586214200406E-16,-4.86333050978515,
-32.7499935638448));
#305954=CARTESIAN_POINT('Ctrl Pts',(1.58019187191962,-4.86333050978515,
-32.6624935638448));
#305955=CARTESIAN_POINT('Ctrl Pts',(2.85859395067575,-3.93451703167836,
-32.5749935638448));
#305956=CARTESIAN_POINT('Ctrl Pts',(4.13699602943187,-3.00570355357157,
-32.4874935638448));
#305957=CARTESIAN_POINT('Ctrl Pts',(4.6253021722282,-1.50285177678579,-32.3999935638448));
#305958=CARTESIAN_POINT('Ctrl Pts',(5.11360831502452,1.30421967105138E-15,
-32.3124935638448));
#305959=CARTESIAN_POINT('Ctrl Pts',(4.6253021722282,1.50285177678579,-32.2249935638448));
#305960=CARTESIAN_POINT('Ctrl Pts',(4.13699602943188,3.00570355357158,-32.1374935638448));
#305961=CARTESIAN_POINT('Ctrl Pts',(2.85859395067575,3.93451703167837,-32.0499935638448));
#305962=CARTESIAN_POINT('Ctrl Pts',(1.58019187191962,4.86333050978515,-31.9624935638448));
#305963=CARTESIAN_POINT('Ctrl Pts',(0.,4.86333050978515,-31.8749935638448));
#305964=CARTESIAN_POINT('Ctrl Pts',(-1.58019187191962,4.86333050978515,
-31.7874935638448));
#305965=CARTESIAN_POINT('Ctrl Pts',(-2.85859395067575,3.93451703167837,
-31.6999935638448));
#305966=CARTESIAN_POINT('Ctrl Pts',(-4.13699602943188,3.00570355357158,
-31.6124935638448));
#305967=CARTESIAN_POINT('Ctrl Pts',(-4.6253021722282,1.50285177678579,-31.5249935638448));
#305968=CARTESIAN_POINT('Ctrl Pts',(-5.11360831502452,2.58401741377497E-15,
-31.4374935638448));
#305969=CARTESIAN_POINT('Ctrl Pts',(-4.6253021722282,-1.50285177678579,
-31.3499935638448));
#305970=CARTESIAN_POINT('Ctrl Pts',(-4.13699602943188,-3.00570355357157,
-31.2624935638448));
#305971=CARTESIAN_POINT('Ctrl Pts',(-2.85859395067575,-3.93451703167836,
-31.1749935638448));
#305972=CARTESIAN_POINT('Ctrl Pts',(-1.58019187191962,-4.86333050978515,
-31.0874935638448));
#305973=CARTESIAN_POINT('Ctrl Pts',(-5.95586214200406E-16,-4.86333050978515,
-30.9999935638448));
#305974=CARTESIAN_POINT('Ctrl Pts',(1.58019187191962,-4.86333050978515,
-30.9124935638448));
#305975=CARTESIAN_POINT('Ctrl Pts',(2.85859395067575,-3.93451703167836,
-30.8249935638448));
#305976=CARTESIAN_POINT('Ctrl Pts',(4.13699602943187,-3.00570355357157,
-30.7374935638448));
#305977=CARTESIAN_POINT('Ctrl Pts',(4.6253021722282,-1.50285177678579,-30.6499935638448));
#305978=CARTESIAN_POINT('Ctrl Pts',(5.11360831502452,1.35886953446333E-15,
-30.5624935638448));
#305979=CARTESIAN_POINT('Ctrl Pts',(4.6253021722282,1.50285177678579,-30.4749935638448));
#305980=CARTESIAN_POINT('Ctrl Pts',(4.13699602943188,3.00570355357158,-30.3874935638448));
#305981=CARTESIAN_POINT('Ctrl Pts',(2.85859395067575,3.93451703167837,-30.2999935638448));
#305982=CARTESIAN_POINT('Ctrl Pts',(1.58019187191962,4.86333050978515,-30.2124935638448));
#305983=CARTESIAN_POINT('Ctrl Pts',(0.,4.86333050978515,-30.1249935638448));
#305984=CARTESIAN_POINT('Ctrl Pts',(-1.58019187191962,4.86333050978515,
-30.0374935638448));
#305985=CARTESIAN_POINT('Ctrl Pts',(-2.85859395067575,3.93451703167837,
-29.9499935638448));
#305986=CARTESIAN_POINT('Ctrl Pts',(-4.13699602943188,3.00570355357158,
-29.8624935638448));
#305987=CARTESIAN_POINT('Ctrl Pts',(-4.6253021722282,1.50285177678579,-29.7749935638448));
#305988=CARTESIAN_POINT('Ctrl Pts',(-5.11360831502452,2.63866727718692E-15,
-29.6874935638448));
#305989=CARTESIAN_POINT('Ctrl Pts',(-4.6253021722282,-1.50285177678579,
-29.5999935638448));
#305990=CARTESIAN_POINT('Ctrl Pts',(-4.13699602943188,-3.00570355357157,
-29.5124935638448));
#305991=CARTESIAN_POINT('Ctrl Pts',(-2.85859395067575,-3.93451703167836,
-29.4249935638448));
#305992=CARTESIAN_POINT('Ctrl Pts',(-1.58019187191962,-4.86333050978515,
-29.3374935638448));
#305993=CARTESIAN_POINT('Ctrl Pts',(-5.95586214200406E-16,-4.86333050978515,
-29.2499935638448));
#305994=CARTESIAN_POINT('Ctrl Pts',(1.58019187191962,-4.86333050978515,
-29.1624935638448));
#305995=CARTESIAN_POINT('Ctrl Pts',(2.85859395067575,-3.93451703167836,
-29.0749935638448));
#305996=CARTESIAN_POINT('Ctrl Pts',(4.13699602943187,-3.00570355357157,
-28.9874935638448));
#305997=CARTESIAN_POINT('Ctrl Pts',(4.6253021722282,-1.50285177678579,-28.8999935638448));
#305998=CARTESIAN_POINT('Ctrl Pts',(5.11360831502452,1.41351939787528E-15,
-28.8124935638448));
#305999=CARTESIAN_POINT('Ctrl Pts',(4.6253021722282,1.50285177678579,-28.7249935638448));
#306000=CARTESIAN_POINT('Ctrl Pts',(4.13699602943188,3.00570355357158,-28.6374935638448));
#306001=CARTESIAN_POINT('Ctrl Pts',(2.85859395067575,3.93451703167837,-28.5499935638448));
#306002=CARTESIAN_POINT('Ctrl Pts',(1.58019187191962,4.86333050978515,-28.4624935638448));
#306003=CARTESIAN_POINT('Ctrl Pts',(0.,4.86333050978515,-28.3749935638448));
#306004=CARTESIAN_POINT('Ctrl Pts',(-1.58019187191962,4.86333050978515,
-28.2874935638448));
#306005=CARTESIAN_POINT('Ctrl Pts',(-2.85859395067575,3.93451703167837,
-28.1999935638448));
#306006=CARTESIAN_POINT('Ctrl Pts',(-4.13699602943188,3.00570355357158,
-28.1124935638448));
#306007=CARTESIAN_POINT('Ctrl Pts',(-4.6253021722282,1.50285177678579,-28.0249935638448));
#306008=CARTESIAN_POINT('Ctrl Pts',(-5.11360831502452,2.69331714059887E-15,
-27.9374935638448));
#306009=CARTESIAN_POINT('Ctrl Pts',(-4.6253021722282,-1.50285177678579,
-27.8499935638448));
#306010=CARTESIAN_POINT('Ctrl Pts',(-4.13699602943188,-3.00570355357157,
-27.7624935638448));
#306011=CARTESIAN_POINT('Ctrl Pts',(-2.85859395067575,-3.93451703167836,
-27.6749935638448));
#306012=CARTESIAN_POINT('Ctrl Pts',(-1.58019187191962,-4.86333050978515,
-27.5874935638448));
#306013=CARTESIAN_POINT('Ctrl Pts',(-5.95586214200406E-16,-4.86333050978515,
-27.4999935638448));
#306014=CARTESIAN_POINT('Ctrl Pts',(1.58019187191962,-4.86333050978515,
-27.4124935638448));
#306015=CARTESIAN_POINT('Ctrl Pts',(2.85859395067575,-3.93451703167836,
-27.3249935638448));
#306016=CARTESIAN_POINT('Ctrl Pts',(4.13699602943187,-3.00570355357157,
-27.2374935638448));
#306017=CARTESIAN_POINT('Ctrl Pts',(4.6253021722282,-1.50285177678579,-27.1499935638448));
#306018=CARTESIAN_POINT('Ctrl Pts',(5.11360831502452,1.46816926128723E-15,
-27.0624935638448));
#306019=CARTESIAN_POINT('Ctrl Pts',(4.6253021722282,1.50285177678579,-26.9749935638448));
#306020=CARTESIAN_POINT('Ctrl Pts',(4.13699602943188,3.00570355357158,-26.8874935638448));
#306021=CARTESIAN_POINT('Ctrl Pts',(2.85859395067575,3.93451703167837,-26.7999935638448));
#306022=CARTESIAN_POINT('Ctrl Pts',(1.58019187191962,4.86333050978515,-26.7124935638448));
#306023=CARTESIAN_POINT('Ctrl Pts',(0.,4.86333050978515,-26.6249935638448));
#306024=CARTESIAN_POINT('Ctrl Pts',(-1.58019187191962,4.86333050978515,
-26.5374935638448));
#306025=CARTESIAN_POINT('Ctrl Pts',(-2.85859395067575,3.93451703167837,
-26.4499935638448));
#306026=CARTESIAN_POINT('Ctrl Pts',(-4.13699602943188,3.00570355357158,
-26.3624935638448));
#306027=CARTESIAN_POINT('Ctrl Pts',(-4.6253021722282,1.50285177678579,-26.2749935638448));
#306028=CARTESIAN_POINT('Ctrl Pts',(-5.11360831502452,2.74796700401082E-15,
-26.1874935638448));
#306029=CARTESIAN_POINT('Ctrl Pts',(-4.6253021722282,-1.50285177678579,
-26.0999935638448));
#306030=CARTESIAN_POINT('Ctrl Pts',(-4.13699602943188,-3.00570355357157,
-26.0124935638448));
#306031=CARTESIAN_POINT('Ctrl Pts',(-2.85859395067575,-3.93451703167836,
-25.9249935638448));
#306032=CARTESIAN_POINT('Ctrl Pts',(-1.58019187191962,-4.86333050978515,
-25.8374935638448));
#306033=CARTESIAN_POINT('Ctrl Pts',(-5.95586214200406E-16,-4.86333050978515,
-25.7499935638448));
#306034=CARTESIAN_POINT('Ctrl Pts',(1.58019187191962,-4.86333050978515,
-25.6624935638448));
#306035=CARTESIAN_POINT('Ctrl Pts',(2.85859395067575,-3.93451703167836,
-25.5749935638448));
#306036=CARTESIAN_POINT('Ctrl Pts',(4.13699602943187,-3.00570355357157,
-25.4874935638448));
#306037=CARTESIAN_POINT('Ctrl Pts',(4.6253021722282,-1.50285177678579,-25.3999935638448));
#306038=CARTESIAN_POINT('Ctrl Pts',(5.11360831502452,1.52281912469918E-15,
-25.3124935638448));
#306039=CARTESIAN_POINT('Ctrl Pts',(4.6253021722282,1.50285177678579,-25.2249935638448));
#306040=CARTESIAN_POINT('Ctrl Pts',(4.13699602943188,3.00570355357158,-25.1374935638448));
#306041=CARTESIAN_POINT('Ctrl Pts',(2.85859395067575,3.93451703167837,-25.0499935638448));
#306042=CARTESIAN_POINT('Ctrl Pts',(1.58019187191962,4.86333050978515,-24.9624935638448));
#306043=CARTESIAN_POINT('Ctrl Pts',(0.,4.86333050978515,-24.8749935638448));
#306044=CARTESIAN_POINT('Ctrl Pts',(-1.58019187191962,4.86333050978515,
-24.7874935638448));
#306045=CARTESIAN_POINT('Ctrl Pts',(-2.85859395067575,3.93451703167837,
-24.6999935638448));
#306046=CARTESIAN_POINT('Ctrl Pts',(-4.13699602943188,3.00570355357158,
-24.6124935638448));
#306047=CARTESIAN_POINT('Ctrl Pts',(-4.6253021722282,1.50285177678579,-24.5249935638448));
#306048=CARTESIAN_POINT('Ctrl Pts',(-5.11360831502452,2.80261686742278E-15,
-24.4374935638448));
#306049=CARTESIAN_POINT('Ctrl Pts',(-4.6253021722282,-1.50285177678579,
-24.3499935638448));
#306050=CARTESIAN_POINT('Ctrl Pts',(-4.13699602943188,-3.00570355357157,
-24.2624935638448));
#306051=CARTESIAN_POINT('Ctrl Pts',(-2.85859395067575,-3.93451703167836,
-24.1749935638448));
#306052=CARTESIAN_POINT('Ctrl Pts',(-1.58019187191962,-4.86333050978515,
-24.0874935638448));
#306053=CARTESIAN_POINT('Ctrl Pts',(-5.95586214200406E-16,-4.86333050978515,
-23.9999935638448));
#306054=CARTESIAN_POINT('Ctrl Pts',(1.58019187191962,-4.86333050978515,
-23.9124935638448));
#306055=CARTESIAN_POINT('Ctrl Pts',(2.85859395067575,-3.93451703167836,
-23.8249935638448));
#306056=CARTESIAN_POINT('Ctrl Pts',(4.13699602943187,-3.00570355357157,
-23.7374935638448));
#306057=CARTESIAN_POINT('Ctrl Pts',(4.6253021722282,-1.50285177678579,-23.6499935638448));
#306058=CARTESIAN_POINT('Ctrl Pts',(5.11360831502452,1.57746898811114E-15,
-23.5624935638448));
#306059=CARTESIAN_POINT('Ctrl Pts',(4.6253021722282,1.50285177678579,-23.4749935638448));
#306060=CARTESIAN_POINT('Ctrl Pts',(4.13699602943188,3.00570355357158,-23.3874935638448));
#306061=CARTESIAN_POINT('Ctrl Pts',(2.85859395067575,3.93451703167837,-23.2999935638448));
#306062=CARTESIAN_POINT('Ctrl Pts',(1.58019187191962,4.86333050978515,-23.2124935638448));
#306063=CARTESIAN_POINT('Ctrl Pts',(0.,4.86333050978515,-23.1249935638448));
#306064=CARTESIAN_POINT('Ctrl Pts',(-1.58019187191962,4.86333050978515,
-23.0374935638448));
#306065=CARTESIAN_POINT('Ctrl Pts',(-2.85859395067575,3.93451703167837,
-22.9499935638448));
#306066=CARTESIAN_POINT('Ctrl Pts',(-4.13699602943188,3.00570355357158,
-22.8624935638448));
#306067=CARTESIAN_POINT('Ctrl Pts',(-4.6253021722282,1.50285177678579,-22.7749935638448));
#306068=CARTESIAN_POINT('Ctrl Pts',(-5.11360831502452,2.85726673083472E-15,
-22.6874935638448));
#306069=CARTESIAN_POINT('Ctrl Pts',(-4.6253021722282,-1.50285177678579,
-22.5999935638448));
#306070=CARTESIAN_POINT('Ctrl Pts',(-4.13699602943188,-3.00570355357157,
-22.5124935638448));
#306071=CARTESIAN_POINT('Ctrl Pts',(-2.85859395067575,-3.93451703167836,
-22.4249935638448));
#306072=CARTESIAN_POINT('Ctrl Pts',(-1.58019187191962,-4.86333050978515,
-22.3374935638448));
#306073=CARTESIAN_POINT('Ctrl Pts',(-5.95586214200406E-16,-4.86333050978515,
-22.2499935638448));
#306074=CARTESIAN_POINT('Ctrl Pts',(1.58019187191962,-4.86333050978515,
-22.1624935638448));
#306075=CARTESIAN_POINT('Ctrl Pts',(2.85859395067575,-3.93451703167836,
-22.0749935638448));
#306076=CARTESIAN_POINT('Ctrl Pts',(4.13699602943187,-3.00570355357157,
-21.9874935638448));
#306077=CARTESIAN_POINT('Ctrl Pts',(4.6253021722282,-1.50285177678579,-21.8999935638448));
#306078=CARTESIAN_POINT('Ctrl Pts',(5.11360831502452,1.63211885152309E-15,
-21.8124935638448));
#306079=CARTESIAN_POINT('Ctrl Pts',(4.6253021722282,1.50285177678579,-21.7249935638448));
#306080=CARTESIAN_POINT('Ctrl Pts',(4.13699602943188,3.00570355357158,-21.6374935638448));
#306081=CARTESIAN_POINT('Ctrl Pts',(2.85859395067575,3.93451703167837,-21.5499935638448));
#306082=CARTESIAN_POINT('Ctrl Pts',(1.58019187191962,4.86333050978515,-21.4624935638448));
#306083=CARTESIAN_POINT('Ctrl Pts',(0.,4.86333050978515,-21.3749935638448));
#306084=CARTESIAN_POINT('Ctrl Pts',(-1.58019187191962,4.86333050978515,
-21.2874935638448));
#306085=CARTESIAN_POINT('Ctrl Pts',(-2.85859395067575,3.93451703167837,
-21.1999935638448));
#306086=CARTESIAN_POINT('Ctrl Pts',(-4.13699602943188,3.00570355357158,
-21.1124935638448));
#306087=CARTESIAN_POINT('Ctrl Pts',(-4.6253021722282,1.50285177678579,-21.0249935638448));
#306088=CARTESIAN_POINT('Ctrl Pts',(-5.11360831502452,2.91191659424667E-15,
-20.9374935638448));
#306089=CARTESIAN_POINT('Ctrl Pts',(-4.6253021722282,-1.50285177678579,
-20.8499935638448));
#306090=CARTESIAN_POINT('Ctrl Pts',(-4.13699602943188,-3.00570355357157,
-20.7624935638448));
#306091=CARTESIAN_POINT('Ctrl Pts',(-2.85859395067575,-3.93451703167836,
-20.6749935638448));
#306092=CARTESIAN_POINT('Ctrl Pts',(-1.58019187191962,-4.86333050978515,
-20.5874935638448));
#306093=CARTESIAN_POINT('Ctrl Pts',(-5.95586214200406E-16,-4.86333050978515,
-20.4999935638448));
#306094=CARTESIAN_POINT('Ctrl Pts',(1.58019187191962,-4.86333050978515,
-20.4124935638448));
#306095=CARTESIAN_POINT('Ctrl Pts',(2.85859395067575,-3.93451703167836,
-20.3249935638448));
#306096=CARTESIAN_POINT('Ctrl Pts',(4.13699602943187,-3.00570355357157,
-20.2374935638448));
#306097=CARTESIAN_POINT('Ctrl Pts',(4.6253021722282,-1.50285177678579,-20.1499935638448));
#306098=CARTESIAN_POINT('Ctrl Pts',(5.11360831502452,1.68676871493504E-15,
-20.0624935638448));
#306099=CARTESIAN_POINT('Ctrl Pts',(4.6253021722282,1.50285177678579,-19.9749935638448));
#306100=CARTESIAN_POINT('Ctrl Pts',(4.13699602943188,3.00570355357158,-19.8874935638448));
#306101=CARTESIAN_POINT('Ctrl Pts',(2.85859395067575,3.93451703167837,-19.7999935638448));
#306102=CARTESIAN_POINT('Ctrl Pts',(1.58019187191962,4.86333050978515,-19.7124935638448));
#306103=CARTESIAN_POINT('Ctrl Pts',(0.,4.86333050978515,-19.6249935638448));
#306104=CARTESIAN_POINT('Ctrl Pts',(-1.58019187191962,4.86333050978515,
-19.5374935638448));
#306105=CARTESIAN_POINT('Ctrl Pts',(-2.85859395067575,3.93451703167837,
-19.4499935638448));
#306106=CARTESIAN_POINT('Ctrl Pts',(-4.13699602943188,3.00570355357158,
-19.3624935638448));
#306107=CARTESIAN_POINT('Ctrl Pts',(-4.6253021722282,1.50285177678579,-19.2749935638448));
#306108=CARTESIAN_POINT('Ctrl Pts',(-5.11360831502452,2.96656645765862E-15,
-19.1874935638448));
#306109=CARTESIAN_POINT('Ctrl Pts',(-4.6253021722282,-1.50285177678579,
-19.0999935638448));
#306110=CARTESIAN_POINT('Ctrl Pts',(-4.13699602943188,-3.00570355357157,
-19.0124935638448));
#306111=CARTESIAN_POINT('Ctrl Pts',(-2.85859395067575,-3.93451703167836,
-18.9249935638448));
#306112=CARTESIAN_POINT('Ctrl Pts',(-1.58019187191962,-4.86333050978515,
-18.8374935638448));
#306113=CARTESIAN_POINT('Ctrl Pts',(-5.95586214200406E-16,-4.86333050978515,
-18.7499935638448));
#306114=CARTESIAN_POINT('Ctrl Pts',(1.58019187191962,-4.86333050978515,
-18.6624935638448));
#306115=CARTESIAN_POINT('Ctrl Pts',(2.85859395067575,-3.93451703167836,
-18.5749935638448));
#306116=CARTESIAN_POINT('Ctrl Pts',(4.13699602943187,-3.00570355357157,
-18.4874935638448));
#306117=CARTESIAN_POINT('Ctrl Pts',(4.6253021722282,-1.50285177678579,-18.3999935638448));
#306118=CARTESIAN_POINT('Ctrl Pts',(5.11360831502452,1.74141857834699E-15,
-18.3124935638448));
#306119=CARTESIAN_POINT('Ctrl Pts',(4.6253021722282,1.50285177678579,-18.2249935638448));
#306120=CARTESIAN_POINT('Ctrl Pts',(4.13699602943188,3.00570355357158,-18.1374935638448));
#306121=CARTESIAN_POINT('Ctrl Pts',(2.85859395067575,3.93451703167837,-18.0499935638448));
#306122=CARTESIAN_POINT('Ctrl Pts',(1.58019187191962,4.86333050978515,-17.9624935638448));
#306123=CARTESIAN_POINT('Ctrl Pts',(0.,4.86333050978515,-17.8749935638448));
#306124=CARTESIAN_POINT('Ctrl Pts',(-1.58019187191962,4.86333050978515,
-17.7874935638448));
#306125=CARTESIAN_POINT('Ctrl Pts',(-2.85859395067575,3.93451703167837,
-17.6999935638448));
#306126=CARTESIAN_POINT('Ctrl Pts',(-4.13699602943188,3.00570355357158,
-17.6124935638448));
#306127=CARTESIAN_POINT('Ctrl Pts',(-4.6253021722282,1.50285177678579,-17.5249935638448));
#306128=CARTESIAN_POINT('Ctrl Pts',(-5.11360831502452,3.02121632107057E-15,
-17.4374935638448));
#306129=CARTESIAN_POINT('Ctrl Pts',(-4.6253021722282,-1.50285177678579,
-17.3499935638448));
#306130=CARTESIAN_POINT('Ctrl Pts',(-4.13699602943188,-3.00570355357157,
-17.2624935638448));
#306131=CARTESIAN_POINT('Ctrl Pts',(-2.85859395067575,-3.93451703167836,
-17.1749935638448));
#306132=CARTESIAN_POINT('Ctrl Pts',(-1.58019187191962,-4.86333050978515,
-17.0874935638448));
#306133=CARTESIAN_POINT('Ctrl Pts',(-5.95586214200406E-16,-4.86333050978515,
-16.9999935638448));
#306134=CARTESIAN_POINT('Ctrl Pts',(1.58019187191962,-4.86333050978515,
-16.9124935638448));
#306135=CARTESIAN_POINT('Ctrl Pts',(2.85859395067575,-3.93451703167836,
-16.8249935638448));
#306136=CARTESIAN_POINT('Ctrl Pts',(4.13699602943187,-3.00570355357157,
-16.7374935638448));
#306137=CARTESIAN_POINT('Ctrl Pts',(4.6253021722282,-1.50285177678579,-16.6499935638448));
#306138=CARTESIAN_POINT('Ctrl Pts',(5.11360831502452,1.79606844175894E-15,
-16.5624935638448));
#306139=CARTESIAN_POINT('Ctrl Pts',(4.6253021722282,1.50285177678579,-16.4749935638448));
#306140=CARTESIAN_POINT('Ctrl Pts',(4.13699602943188,3.00570355357158,-16.3874935638448));
#306141=CARTESIAN_POINT('Ctrl Pts',(2.85859395067575,3.93451703167837,-16.2999935638448));
#306142=CARTESIAN_POINT('Ctrl Pts',(1.58019187191962,4.86333050978515,-16.2124935638448));
#306143=CARTESIAN_POINT('Ctrl Pts',(0.,4.86333050978515,-16.1249935638448));
#306144=CARTESIAN_POINT('Ctrl Pts',(-1.58019187191962,4.86333050978515,
-16.0374935638448));
#306145=CARTESIAN_POINT('Ctrl Pts',(-2.85859395067575,3.93451703167837,
-15.9499935638448));
#306146=CARTESIAN_POINT('Ctrl Pts',(-4.13699602943188,3.00570355357158,
-15.8624935638448));
#306147=CARTESIAN_POINT('Ctrl Pts',(-4.6253021722282,1.50285177678579,-15.7749935638448));
#306148=CARTESIAN_POINT('Ctrl Pts',(-5.11360831502452,3.07586618448253E-15,
-15.6874935638448));
#306149=CARTESIAN_POINT('Ctrl Pts',(-4.6253021722282,-1.50285177678579,
-15.5999935638448));
#306150=CARTESIAN_POINT('Ctrl Pts',(-4.13699602943188,-3.00570355357157,
-15.5124935638448));
#306151=CARTESIAN_POINT('Ctrl Pts',(-2.85859395067575,-3.93451703167836,
-15.4249935638448));
#306152=CARTESIAN_POINT('Ctrl Pts',(-1.58019187191962,-4.86333050978515,
-15.3374935638448));
#306153=CARTESIAN_POINT('Ctrl Pts',(-5.95586214200406E-16,-4.86333050978515,
-15.2499935638448));
#306154=CARTESIAN_POINT('Ctrl Pts',(1.58019187191962,-4.86333050978515,
-15.1624935638448));
#306155=CARTESIAN_POINT('Ctrl Pts',(2.85859395067575,-3.93451703167836,
-15.0749935638448));
#306156=CARTESIAN_POINT('Ctrl Pts',(4.13699602943187,-3.00570355357157,
-14.9874935638448));
#306157=CARTESIAN_POINT('Ctrl Pts',(4.6253021722282,-1.50285177678579,-14.8999935638448));
#306158=CARTESIAN_POINT('Ctrl Pts',(5.11360831502452,1.85071830517089E-15,
-14.8124935638448));
#306159=CARTESIAN_POINT('Ctrl Pts',(4.6253021722282,1.50285177678579,-14.7249935638448));
#306160=CARTESIAN_POINT('Ctrl Pts',(4.13699602943188,3.00570355357158,-14.6374935638448));
#306161=CARTESIAN_POINT('Ctrl Pts',(2.85859395067575,3.93451703167837,-14.5499935638448));
#306162=CARTESIAN_POINT('Ctrl Pts',(1.58019187191962,4.86333050978515,-14.4624935638448));
#306163=CARTESIAN_POINT('Ctrl Pts',(0.,4.86333050978515,-14.3749935638448));
#306164=CARTESIAN_POINT('Ctrl Pts',(-1.58019187191962,4.86333050978515,
-14.2874935638448));
#306165=CARTESIAN_POINT('Ctrl Pts',(-2.85859395067575,3.93451703167837,
-14.1999935638448));
#306166=CARTESIAN_POINT('Ctrl Pts',(-4.13699602943188,3.00570355357158,
-14.1124935638448));
#306167=CARTESIAN_POINT('Ctrl Pts',(-4.6253021722282,1.50285177678579,-14.0249935638448));
#306168=CARTESIAN_POINT('Ctrl Pts',(-5.11360831502452,3.13051604789448E-15,
-13.9374935638448));
#306169=CARTESIAN_POINT('Ctrl Pts',(-4.6253021722282,-1.50285177678579,
-13.8499935638448));
#306170=CARTESIAN_POINT('Ctrl Pts',(-4.13699602943188,-3.00570355357157,
-13.7624935638448));
#306171=CARTESIAN_POINT('Ctrl Pts',(-2.85859395067575,-3.93451703167836,
-13.6749935638448));
#306172=CARTESIAN_POINT('Ctrl Pts',(-1.58019187191962,-4.86333050978515,
-13.5874935638448));
#306173=CARTESIAN_POINT('Ctrl Pts',(-5.95586214200406E-16,-4.86333050978515,
-13.4999935638448));
#306174=CARTESIAN_POINT('Ctrl Pts',(1.58019187191962,-4.86333050978515,
-13.4124935638448));
#306175=CARTESIAN_POINT('Ctrl Pts',(2.85859395067575,-3.93451703167836,
-13.3249935638448));
#306176=CARTESIAN_POINT('Ctrl Pts',(4.13699602943187,-3.00570355357157,
-13.2374935638448));
#306177=CARTESIAN_POINT('Ctrl Pts',(4.6253021722282,-1.50285177678579,-13.1499935638448));
#306178=CARTESIAN_POINT('Ctrl Pts',(5.11360831502452,1.90536816858284E-15,
-13.0624935638448));
#306179=CARTESIAN_POINT('Ctrl Pts',(4.6253021722282,1.50285177678579,-12.9749935638448));
#306180=CARTESIAN_POINT('Ctrl Pts',(4.13699602943188,3.00570355357158,-12.8874935638448));
#306181=CARTESIAN_POINT('Ctrl Pts',(2.85859395067575,3.93451703167837,-12.7999935638448));
#306182=CARTESIAN_POINT('Ctrl Pts',(1.58019187191962,4.86333050978515,-12.7124935638448));
#306183=CARTESIAN_POINT('Ctrl Pts',(0.,4.86333050978515,-12.6249935638448));
#306184=CARTESIAN_POINT('Ctrl Pts',(-1.58019187191962,4.86333050978515,
-12.5374935638448));
#306185=CARTESIAN_POINT('Ctrl Pts',(-2.85859395067575,3.93451703167837,
-12.4499935638448));
#306186=CARTESIAN_POINT('Ctrl Pts',(-4.13699602943188,3.00570355357158,
-12.3624935638448));
#306187=CARTESIAN_POINT('Ctrl Pts',(-4.6253021722282,1.50285177678579,-12.2749935638448));
#306188=CARTESIAN_POINT('Ctrl Pts',(-5.11360831502452,3.18516591130643E-15,
-12.1874935638448));
#306189=CARTESIAN_POINT('Ctrl Pts',(-4.6253021722282,-1.50285177678579,
-12.0999935638448));
#306190=CARTESIAN_POINT('Ctrl Pts',(-4.13699602943188,-3.00570355357157,
-12.0124935638448));
#306191=CARTESIAN_POINT('Ctrl Pts',(-2.85859395067575,-3.93451703167836,
-11.9249935638448));
#306192=CARTESIAN_POINT('Ctrl Pts',(-1.58019187191962,-4.86333050978515,
-11.8374935638448));
#306193=CARTESIAN_POINT('Ctrl Pts',(-5.95586214200406E-16,-4.86333050978515,
-11.7499935638448));
#306194=CARTESIAN_POINT('Ctrl Pts',(1.58019187191962,-4.86333050978515,
-11.6624935638448));
#306195=CARTESIAN_POINT('Ctrl Pts',(2.85859395067575,-3.93451703167836,
-11.5749935638448));
#306196=CARTESIAN_POINT('Ctrl Pts',(4.13699602943187,-3.00570355357157,
-11.4874935638448));
#306197=CARTESIAN_POINT('Ctrl Pts',(4.6253021722282,-1.50285177678579,-11.3999935638448));
#306198=CARTESIAN_POINT('Ctrl Pts',(5.11360831502452,1.96001803199479E-15,
-11.3124935638448));
#306199=CARTESIAN_POINT('Ctrl Pts',(4.6253021722282,1.50285177678579,-11.2249935638448));
#306200=CARTESIAN_POINT('Ctrl Pts',(4.13699602943188,3.00570355357158,-11.1374935638448));
#306201=CARTESIAN_POINT('Ctrl Pts',(2.85859395067575,3.93451703167837,-11.0499935638448));
#306202=CARTESIAN_POINT('Ctrl Pts',(1.58019187191962,4.86333050978515,-10.9624935638448));
#306203=CARTESIAN_POINT('Ctrl Pts',(0.,4.86333050978515,-10.8749935638448));
#306204=CARTESIAN_POINT('Ctrl Pts',(-1.58019187191962,4.86333050978515,
-10.7874935638448));
#306205=CARTESIAN_POINT('Ctrl Pts',(-2.85859395067575,3.93451703167837,
-10.6999935638448));
#306206=CARTESIAN_POINT('Ctrl Pts',(-4.13699602943188,3.00570355357158,
-10.6124935638448));
#306207=CARTESIAN_POINT('Ctrl Pts',(-4.6253021722282,1.50285177678579,-10.5249935638448));
#306208=CARTESIAN_POINT('Ctrl Pts',(-5.11360831502452,3.23981577471838E-15,
-10.4374935638448));
#306209=CARTESIAN_POINT('Ctrl Pts',(-4.6253021722282,-1.50285177678579,
-10.3499935638448));
#306210=CARTESIAN_POINT('Ctrl Pts',(-4.13699602943188,-3.00570355357157,
-10.2624935638448));
#306211=CARTESIAN_POINT('Ctrl Pts',(-2.85859395067575,-3.93451703167836,
-10.1749935638448));
#306212=CARTESIAN_POINT('Ctrl Pts',(-1.58019187191962,-4.86333050978515,
-10.0874935638448));
#306213=CARTESIAN_POINT('Ctrl Pts',(-5.95586214200406E-16,-4.86333050978515,
-9.99999356384482));
#306214=CARTESIAN_POINT('Ctrl Pts',(1.58019187191962,-4.86333050978515,
-9.91249356384481));
#306215=CARTESIAN_POINT('Ctrl Pts',(2.85859395067575,-3.93451703167836,
-9.82499356384482));
#306216=CARTESIAN_POINT('Ctrl Pts',(4.13699602943187,-3.00570355357157,
-9.73749356384481));
#306217=CARTESIAN_POINT('Ctrl Pts',(4.6253021722282,-1.50285177678579,-9.64999356384482));
#306218=CARTESIAN_POINT('Ctrl Pts',(5.11360831502452,2.01466789540674E-15,
-9.56249356384481));
#306219=CARTESIAN_POINT('Ctrl Pts',(4.6253021722282,1.50285177678579,-9.47499356384482));
#306220=CARTESIAN_POINT('Ctrl Pts',(4.13699602943188,3.00570355357158,-9.3874935638448));
#306221=CARTESIAN_POINT('Ctrl Pts',(2.85859395067575,3.93451703167837,-9.29999356384481));
#306222=CARTESIAN_POINT('Ctrl Pts',(1.58019187191962,4.86333050978515,-9.21249356384481));
#306223=CARTESIAN_POINT('Ctrl Pts',(0.,4.86333050978515,-9.12499356384482));
#306224=CARTESIAN_POINT('Ctrl Pts',(-1.58019187191962,4.86333050978515,
-9.03749356384481));
#306225=CARTESIAN_POINT('Ctrl Pts',(-2.85859395067575,3.93451703167837,
-8.94999356384482));
#306226=CARTESIAN_POINT('Ctrl Pts',(-4.13699602943188,3.00570355357158,
-8.86249356384481));
#306227=CARTESIAN_POINT('Ctrl Pts',(-4.6253021722282,1.50285177678579,-8.77499356384481));
#306228=CARTESIAN_POINT('Ctrl Pts',(-5.11360831502452,3.29446563813033E-15,
-8.68749356384481));
#306229=CARTESIAN_POINT('Ctrl Pts',(-4.6253021722282,-1.50285177678579,
-8.59999356384482));
#306230=CARTESIAN_POINT('Ctrl Pts',(-4.13699602943188,-3.00570355357157,
-8.5124935638448));
#306231=CARTESIAN_POINT('Ctrl Pts',(-2.85859395067575,-3.93451703167836,
-8.42499356384482));
#306232=CARTESIAN_POINT('Ctrl Pts',(-1.58019187191962,-4.86333050978515,
-8.33749356384481));
#306233=CARTESIAN_POINT('Ctrl Pts',(-5.95586214200406E-16,-4.86333050978515,
-8.24999356384481));
#306234=CARTESIAN_POINT('Ctrl Pts',(1.58019187191962,-4.86333050978515,
-8.16249356384481));
#306235=CARTESIAN_POINT('Ctrl Pts',(2.85859395067575,-3.93451703167836,
-8.07499356384482));
#306236=CARTESIAN_POINT('Ctrl Pts',(4.13699602943187,-3.00570355357157,
-7.98749356384481));
#306237=CARTESIAN_POINT('Ctrl Pts',(4.6253021722282,-1.50285177678579,-7.89999356384481));
#306238=CARTESIAN_POINT('Ctrl Pts',(5.11360831502452,2.06931775881869E-15,
-7.81249356384481));
#306239=CARTESIAN_POINT('Ctrl Pts',(4.6253021722282,1.50285177678579,-7.72499356384482));
#306240=CARTESIAN_POINT('Ctrl Pts',(4.13699602943188,3.00570355357158,-7.6374935638448));
#306241=CARTESIAN_POINT('Ctrl Pts',(2.85859395067575,3.93451703167837,-7.54999356384482));
#306242=CARTESIAN_POINT('Ctrl Pts',(1.58019187191962,4.86333050978515,-7.46249356384481));
#306243=CARTESIAN_POINT('Ctrl Pts',(0.,4.86333050978515,-7.37499356384482));
#306244=CARTESIAN_POINT('Ctrl Pts',(-1.58019187191962,4.86333050978515,
-7.28749356384481));
#306245=CARTESIAN_POINT('Ctrl Pts',(-2.85859395067575,3.93451703167837,
-7.19999356384482));
#306246=CARTESIAN_POINT('Ctrl Pts',(-4.13699602943188,3.00570355357158,
-7.11249356384481));
#306247=CARTESIAN_POINT('Ctrl Pts',(-4.6253021722282,1.50285177678579,-7.02499356384482));
#306248=CARTESIAN_POINT('Ctrl Pts',(-5.11360831502452,3.34911550154228E-15,
-6.93749356384481));
#306249=CARTESIAN_POINT('Ctrl Pts',(-4.6253021722282,-1.50285177678579,
-6.84999356384481));
#306250=CARTESIAN_POINT('Ctrl Pts',(-4.13699602943188,-3.00570355357157,
-6.76249356384481));
#306251=CARTESIAN_POINT('Ctrl Pts',(-2.85859395067575,-3.93451703167836,
-6.67499356384482));
#306252=CARTESIAN_POINT('Ctrl Pts',(-1.58019187191962,-4.86333050978515,
-6.58749356384481));
#306253=CARTESIAN_POINT('Ctrl Pts',(-5.95586214200406E-16,-4.86333050978515,
-6.49999356384482));
#306254=CARTESIAN_POINT('Ctrl Pts',(1.58019187191962,-4.86333050978515,
-6.41249356384481));
#306255=CARTESIAN_POINT('Ctrl Pts',(2.85859395067575,-3.93451703167836,
-6.32499356384482));
#306256=CARTESIAN_POINT('Ctrl Pts',(4.13699602943187,-3.00570355357157,
-6.23749356384481));
#306257=CARTESIAN_POINT('Ctrl Pts',(4.6253021722282,-1.50285177678579,-6.14999356384482));
#306258=CARTESIAN_POINT('Ctrl Pts',(5.11360831502452,2.12396762223064E-15,
-6.06249356384482));
#306259=CARTESIAN_POINT('Ctrl Pts',(4.6253021722282,1.50285177678579,-5.97499356384481));
#306260=CARTESIAN_POINT('Ctrl Pts',(4.13699602943188,3.00570355357158,-5.88749356384482));
#306261=CARTESIAN_POINT('Ctrl Pts',(2.85859395067575,3.93451703167837,-5.79999356384481));
#306262=CARTESIAN_POINT('Ctrl Pts',(1.58019187191962,4.86333050978515,-5.71249356384481));
#306263=CARTESIAN_POINT('Ctrl Pts',(0.,4.86333050978515,-5.62499356384482));
#306264=CARTESIAN_POINT('Ctrl Pts',(-1.58019187191962,4.86333050978515,
-5.53749356384482));
#306265=CARTESIAN_POINT('Ctrl Pts',(-2.85859395067575,3.93451703167837,
-5.44999356384482));
#306266=CARTESIAN_POINT('Ctrl Pts',(-3.39156536058037,3.54729063617168,
-5.41351443169882));
#306267=CARTESIAN_POINT('Ctrl Pts',(-3.80231226593749,3.03222774205837,
-5.3751966204675));
#306268=CARTESIAN_POINT('Ctrl Pts',(0.,6.09472152853892,-37.8359375));
#306269=CARTESIAN_POINT('Ctrl Pts',(-1.98029506767702,6.09472152853892,
-37.7484375));
#306270=CARTESIAN_POINT('Ctrl Pts',(-3.58238743130462,4.93073329257085,
-37.6609375));
#306271=CARTESIAN_POINT('Ctrl Pts',(-5.18447979493222,3.76674505660277,
-37.5734375));
#306272=CARTESIAN_POINT('Ctrl Pts',(-5.7964246247213,1.88337252830138,-37.4859375));
#306273=CARTESIAN_POINT('Ctrl Pts',(-6.40836945451038,2.47714736979317E-15,
-37.3984375));
#306274=CARTESIAN_POINT('Ctrl Pts',(-5.7964246247213,-1.88337252830138,
-37.3109375));
#306275=CARTESIAN_POINT('Ctrl Pts',(-5.18447979493222,-3.76674505660276,
-37.2234375));
#306276=CARTESIAN_POINT('Ctrl Pts',(-3.58238743130462,-4.93073329257084,
-37.1359375));
#306277=CARTESIAN_POINT('Ctrl Pts',(-1.98029506767702,-6.09472152853892,
-37.0484374999999));
#306278=CARTESIAN_POINT('Ctrl Pts',(-7.46388121161966E-16,-6.09472152853892,
-36.9609375));
#306279=CARTESIAN_POINT('Ctrl Pts',(1.98029506767702,-6.09472152853892,
-36.8734375));
#306280=CARTESIAN_POINT('Ctrl Pts',(3.58238743130462,-4.93073329257084,
-36.7859375));
#306281=CARTESIAN_POINT('Ctrl Pts',(5.18447979493222,-3.76674505660277,
-36.6984375));
#306282=CARTESIAN_POINT('Ctrl Pts',(5.7964246247213,-1.88337252830138,-36.6109375));
#306283=CARTESIAN_POINT('Ctrl Pts',(6.40836945451038,9.34874473455184E-16,
-36.5234375));
#306284=CARTESIAN_POINT('Ctrl Pts',(5.7964246247213,1.88337252830138,-36.4359375));
#306285=CARTESIAN_POINT('Ctrl Pts',(5.18447979493222,3.76674505660277,-36.3484375));
#306286=CARTESIAN_POINT('Ctrl Pts',(3.58238743130462,4.93073329257085,-36.2609375));
#306287=CARTESIAN_POINT('Ctrl Pts',(1.98029506767702,6.09472152853892,-36.1734375));
#306288=CARTESIAN_POINT('Ctrl Pts',(0.,6.09472152853892,-36.0859375));
#306289=CARTESIAN_POINT('Ctrl Pts',(-1.98029506767702,6.09472152853892,
-35.9984375));
#306290=CARTESIAN_POINT('Ctrl Pts',(-3.58238743130462,4.93073329257085,
-35.9109375));
#306291=CARTESIAN_POINT('Ctrl Pts',(-5.18447979493222,3.76674505660277,
-35.8234375));
#306292=CARTESIAN_POINT('Ctrl Pts',(-5.7964246247213,1.88337252830138,-35.7359375));
#306293=CARTESIAN_POINT('Ctrl Pts',(-6.40836945451038,2.53179723320512E-15,
-35.6484375));
#306294=CARTESIAN_POINT('Ctrl Pts',(-5.7964246247213,-1.88337252830138,
-35.5609375));
#306295=CARTESIAN_POINT('Ctrl Pts',(-5.18447979493222,-3.76674505660276,
-35.4734375));
#306296=CARTESIAN_POINT('Ctrl Pts',(-3.58238743130462,-4.93073329257084,
-35.3859375));
#306297=CARTESIAN_POINT('Ctrl Pts',(-1.98029506767702,-6.09472152853892,
-35.2984375));
#306298=CARTESIAN_POINT('Ctrl Pts',(-7.46388121161966E-16,-6.09472152853892,
-35.2109375));
#306299=CARTESIAN_POINT('Ctrl Pts',(1.98029506767702,-6.09472152853892,
-35.1234375));
#306300=CARTESIAN_POINT('Ctrl Pts',(3.58238743130462,-4.93073329257084,
-35.0359375));
#306301=CARTESIAN_POINT('Ctrl Pts',(5.18447979493222,-3.76674505660277,
-34.9484375));
#306302=CARTESIAN_POINT('Ctrl Pts',(5.7964246247213,-1.88337252830138,-34.8609375));
#306303=CARTESIAN_POINT('Ctrl Pts',(6.40836945451038,9.89524336867135E-16,
-34.7734375));
#306304=CARTESIAN_POINT('Ctrl Pts',(5.7964246247213,1.88337252830138,-34.6859375));
#306305=CARTESIAN_POINT('Ctrl Pts',(5.18447979493222,3.76674505660277,-34.5984375));
#306306=CARTESIAN_POINT('Ctrl Pts',(3.58238743130462,4.93073329257085,-34.5109375));
#306307=CARTESIAN_POINT('Ctrl Pts',(1.98029506767702,6.09472152853892,-34.4234375));
#306308=CARTESIAN_POINT('Ctrl Pts',(0.,6.09472152853892,-34.3359375));
#306309=CARTESIAN_POINT('Ctrl Pts',(-1.98029506767702,6.09472152853892,
-34.2484375));
#306310=CARTESIAN_POINT('Ctrl Pts',(-3.58238743130462,4.93073329257085,
-34.1609375));
#306311=CARTESIAN_POINT('Ctrl Pts',(-5.18447979493222,3.76674505660277,
-34.0734375));
#306312=CARTESIAN_POINT('Ctrl Pts',(-5.7964246247213,1.88337252830138,-33.9859375));
#306313=CARTESIAN_POINT('Ctrl Pts',(-6.40836945451038,2.58644709661707E-15,
-33.8984375));
#306314=CARTESIAN_POINT('Ctrl Pts',(-5.7964246247213,-1.88337252830138,
-33.8109375));
#306315=CARTESIAN_POINT('Ctrl Pts',(-5.18447979493222,-3.76674505660276,
-33.7234375));
#306316=CARTESIAN_POINT('Ctrl Pts',(-3.58238743130462,-4.93073329257084,
-33.6359375));
#306317=CARTESIAN_POINT('Ctrl Pts',(-1.98029506767702,-6.09472152853892,
-33.5484375));
#306318=CARTESIAN_POINT('Ctrl Pts',(-7.46388121161966E-16,-6.09472152853892,
-33.4609375));
#306319=CARTESIAN_POINT('Ctrl Pts',(1.98029506767702,-6.09472152853892,
-33.3734375));
#306320=CARTESIAN_POINT('Ctrl Pts',(3.58238743130462,-4.93073329257084,
-33.2859375));
#306321=CARTESIAN_POINT('Ctrl Pts',(5.18447979493222,-3.76674505660277,
-33.1984375));
#306322=CARTESIAN_POINT('Ctrl Pts',(5.7964246247213,-1.88337252830138,-33.1109375));
#306323=CARTESIAN_POINT('Ctrl Pts',(6.40836945451038,1.04417420027908E-15,
-33.0234375));
#306324=CARTESIAN_POINT('Ctrl Pts',(5.7964246247213,1.88337252830138,-32.9359375));
#306325=CARTESIAN_POINT('Ctrl Pts',(5.18447979493222,3.76674505660277,-32.8484375));
#306326=CARTESIAN_POINT('Ctrl Pts',(3.58238743130462,4.93073329257085,-32.7609375));
#306327=CARTESIAN_POINT('Ctrl Pts',(1.98029506767702,6.09472152853892,-32.6734375));
#306328=CARTESIAN_POINT('Ctrl Pts',(0.,6.09472152853892,-32.5859375));
#306329=CARTESIAN_POINT('Ctrl Pts',(-1.98029506767702,6.09472152853892,
-32.4984375));
#306330=CARTESIAN_POINT('Ctrl Pts',(-3.58238743130462,4.93073329257085,
-32.4109375));
#306331=CARTESIAN_POINT('Ctrl Pts',(-5.18447979493222,3.76674505660277,
-32.3234375));
#306332=CARTESIAN_POINT('Ctrl Pts',(-5.7964246247213,1.88337252830138,-32.2359375));
#306333=CARTESIAN_POINT('Ctrl Pts',(-6.40836945451038,2.64109696002902E-15,
-32.1484375));
#306334=CARTESIAN_POINT('Ctrl Pts',(-5.7964246247213,-1.88337252830138,
-32.0609375));
#306335=CARTESIAN_POINT('Ctrl Pts',(-5.18447979493222,-3.76674505660276,
-31.9734375));
#306336=CARTESIAN_POINT('Ctrl Pts',(-3.58238743130462,-4.93073329257084,
-31.8859375));
#306337=CARTESIAN_POINT('Ctrl Pts',(-1.98029506767702,-6.09472152853892,
-31.7984375));
#306338=CARTESIAN_POINT('Ctrl Pts',(-7.46388121161966E-16,-6.09472152853892,
-31.7109375));
#306339=CARTESIAN_POINT('Ctrl Pts',(1.98029506767702,-6.09472152853892,
-31.6234375));
#306340=CARTESIAN_POINT('Ctrl Pts',(3.58238743130462,-4.93073329257084,
-31.5359375));
#306341=CARTESIAN_POINT('Ctrl Pts',(5.18447979493222,-3.76674505660277,
-31.4484375));
#306342=CARTESIAN_POINT('Ctrl Pts',(5.7964246247213,-1.88337252830138,-31.3609375));
#306343=CARTESIAN_POINT('Ctrl Pts',(6.40836945451038,1.09882406369103E-15,
-31.2734375));
#306344=CARTESIAN_POINT('Ctrl Pts',(5.7964246247213,1.88337252830138,-31.1859375));
#306345=CARTESIAN_POINT('Ctrl Pts',(5.18447979493222,3.76674505660277,-31.0984375));
#306346=CARTESIAN_POINT('Ctrl Pts',(3.58238743130462,4.93073329257085,-31.0109375));
#306347=CARTESIAN_POINT('Ctrl Pts',(1.98029506767702,6.09472152853892,-30.9234375));
#306348=CARTESIAN_POINT('Ctrl Pts',(0.,6.09472152853892,-30.8359375));
#306349=CARTESIAN_POINT('Ctrl Pts',(-1.98029506767702,6.09472152853892,
-30.7484375));
#306350=CARTESIAN_POINT('Ctrl Pts',(-3.58238743130462,4.93073329257085,
-30.6609375));
#306351=CARTESIAN_POINT('Ctrl Pts',(-5.18447979493222,3.76674505660277,
-30.5734375));
#306352=CARTESIAN_POINT('Ctrl Pts',(-5.7964246247213,1.88337252830138,-30.4859375));
#306353=CARTESIAN_POINT('Ctrl Pts',(-6.40836945451038,2.69574682344097E-15,
-30.3984375));
#306354=CARTESIAN_POINT('Ctrl Pts',(-5.7964246247213,-1.88337252830138,
-30.3109375));
#306355=CARTESIAN_POINT('Ctrl Pts',(-5.18447979493222,-3.76674505660276,
-30.2234375));
#306356=CARTESIAN_POINT('Ctrl Pts',(-3.58238743130462,-4.93073329257084,
-30.1359375));
#306357=CARTESIAN_POINT('Ctrl Pts',(-1.98029506767702,-6.09472152853892,
-30.0484375));
#306358=CARTESIAN_POINT('Ctrl Pts',(-7.46388121161966E-16,-6.09472152853892,
-29.9609375));
#306359=CARTESIAN_POINT('Ctrl Pts',(1.98029506767702,-6.09472152853892,
-29.8734375));
#306360=CARTESIAN_POINT('Ctrl Pts',(3.58238743130462,-4.93073329257084,
-29.7859375));
#306361=CARTESIAN_POINT('Ctrl Pts',(5.18447979493222,-3.76674505660277,
-29.6984375));
#306362=CARTESIAN_POINT('Ctrl Pts',(5.7964246247213,-1.88337252830138,-29.6109375));
#306363=CARTESIAN_POINT('Ctrl Pts',(6.40836945451038,1.15347392710299E-15,
-29.5234375));
#306364=CARTESIAN_POINT('Ctrl Pts',(5.7964246247213,1.88337252830138,-29.4359375));
#306365=CARTESIAN_POINT('Ctrl Pts',(5.18447979493222,3.76674505660277,-29.3484375));
#306366=CARTESIAN_POINT('Ctrl Pts',(3.58238743130462,4.93073329257085,-29.2609375));
#306367=CARTESIAN_POINT('Ctrl Pts',(1.98029506767702,6.09472152853892,-29.1734375));
#306368=CARTESIAN_POINT('Ctrl Pts',(0.,6.09472152853892,-29.0859375));
#306369=CARTESIAN_POINT('Ctrl Pts',(-1.98029506767702,6.09472152853892,
-28.9984375));
#306370=CARTESIAN_POINT('Ctrl Pts',(-3.58238743130462,4.93073329257085,
-28.9109375));
#306371=CARTESIAN_POINT('Ctrl Pts',(-5.18447979493222,3.76674505660277,
-28.8234375));
#306372=CARTESIAN_POINT('Ctrl Pts',(-5.7964246247213,1.88337252830138,-28.7359375));
#306373=CARTESIAN_POINT('Ctrl Pts',(-6.40836945451038,2.75039668685292E-15,
-28.6484375));
#306374=CARTESIAN_POINT('Ctrl Pts',(-5.7964246247213,-1.88337252830138,
-28.5609375));
#306375=CARTESIAN_POINT('Ctrl Pts',(-5.18447979493222,-3.76674505660276,
-28.4734375));
#306376=CARTESIAN_POINT('Ctrl Pts',(-3.58238743130462,-4.93073329257084,
-28.3859375));
#306377=CARTESIAN_POINT('Ctrl Pts',(-1.98029506767702,-6.09472152853892,
-28.2984375));
#306378=CARTESIAN_POINT('Ctrl Pts',(-7.46388121161966E-16,-6.09472152853892,
-28.2109375));
#306379=CARTESIAN_POINT('Ctrl Pts',(1.98029506767702,-6.09472152853892,
-28.1234375));
#306380=CARTESIAN_POINT('Ctrl Pts',(3.58238743130462,-4.93073329257084,
-28.0359375));
#306381=CARTESIAN_POINT('Ctrl Pts',(5.18447979493222,-3.76674505660277,
-27.9484375));
#306382=CARTESIAN_POINT('Ctrl Pts',(5.7964246247213,-1.88337252830138,-27.8609375));
#306383=CARTESIAN_POINT('Ctrl Pts',(6.40836945451038,1.20812379051494E-15,
-27.7734375));
#306384=CARTESIAN_POINT('Ctrl Pts',(5.7964246247213,1.88337252830138,-27.6859375));
#306385=CARTESIAN_POINT('Ctrl Pts',(5.18447979493222,3.76674505660277,-27.5984375));
#306386=CARTESIAN_POINT('Ctrl Pts',(3.58238743130462,4.93073329257085,-27.5109375));
#306387=CARTESIAN_POINT('Ctrl Pts',(1.98029506767702,6.09472152853892,-27.4234375));
#306388=CARTESIAN_POINT('Ctrl Pts',(0.,6.09472152853892,-27.3359375));
#306389=CARTESIAN_POINT('Ctrl Pts',(-1.98029506767702,6.09472152853892,
-27.2484375));
#306390=CARTESIAN_POINT('Ctrl Pts',(-3.58238743130462,4.93073329257085,
-27.1609375));
#306391=CARTESIAN_POINT('Ctrl Pts',(-5.18447979493222,3.76674505660277,
-27.0734375));
#306392=CARTESIAN_POINT('Ctrl Pts',(-5.7964246247213,1.88337252830138,-26.9859375));
#306393=CARTESIAN_POINT('Ctrl Pts',(-6.40836945451038,2.80504655026487E-15,
-26.8984375));
#306394=CARTESIAN_POINT('Ctrl Pts',(-5.7964246247213,-1.88337252830138,
-26.8109375));
#306395=CARTESIAN_POINT('Ctrl Pts',(-5.18447979493222,-3.76674505660276,
-26.7234375));
#306396=CARTESIAN_POINT('Ctrl Pts',(-3.58238743130462,-4.93073329257084,
-26.6359375));
#306397=CARTESIAN_POINT('Ctrl Pts',(-1.98029506767702,-6.09472152853892,
-26.5484375));
#306398=CARTESIAN_POINT('Ctrl Pts',(-7.46388121161966E-16,-6.09472152853892,
-26.4609375));
#306399=CARTESIAN_POINT('Ctrl Pts',(1.98029506767702,-6.09472152853892,
-26.3734375));
#306400=CARTESIAN_POINT('Ctrl Pts',(3.58238743130462,-4.93073329257084,
-26.2859375));
#306401=CARTESIAN_POINT('Ctrl Pts',(5.18447979493222,-3.76674505660277,
-26.1984375));
#306402=CARTESIAN_POINT('Ctrl Pts',(5.7964246247213,-1.88337252830138,-26.1109375));
#306403=CARTESIAN_POINT('Ctrl Pts',(6.40836945451038,1.26277365392689E-15,
-26.0234375));
#306404=CARTESIAN_POINT('Ctrl Pts',(5.7964246247213,1.88337252830138,-25.9359375));
#306405=CARTESIAN_POINT('Ctrl Pts',(5.18447979493222,3.76674505660277,-25.8484375));
#306406=CARTESIAN_POINT('Ctrl Pts',(3.58238743130462,4.93073329257085,-25.7609375));
#306407=CARTESIAN_POINT('Ctrl Pts',(1.98029506767702,6.09472152853892,-25.6734375));
#306408=CARTESIAN_POINT('Ctrl Pts',(0.,6.09472152853892,-25.5859375));
#306409=CARTESIAN_POINT('Ctrl Pts',(-1.98029506767702,6.09472152853892,
-25.4984375));
#306410=CARTESIAN_POINT('Ctrl Pts',(-3.58238743130462,4.93073329257085,
-25.4109375));
#306411=CARTESIAN_POINT('Ctrl Pts',(-5.18447979493222,3.76674505660277,
-25.3234375));
#306412=CARTESIAN_POINT('Ctrl Pts',(-5.7964246247213,1.88337252830138,-25.2359375));
#306413=CARTESIAN_POINT('Ctrl Pts',(-6.40836945451038,2.85969641367683E-15,
-25.1484375));
#306414=CARTESIAN_POINT('Ctrl Pts',(-5.7964246247213,-1.88337252830138,
-25.0609375));
#306415=CARTESIAN_POINT('Ctrl Pts',(-5.18447979493222,-3.76674505660276,
-24.9734375));
#306416=CARTESIAN_POINT('Ctrl Pts',(-3.58238743130462,-4.93073329257084,
-24.8859375));
#306417=CARTESIAN_POINT('Ctrl Pts',(-1.98029506767702,-6.09472152853892,
-24.7984375));
#306418=CARTESIAN_POINT('Ctrl Pts',(-7.46388121161966E-16,-6.09472152853892,
-24.7109375));
#306419=CARTESIAN_POINT('Ctrl Pts',(1.98029506767702,-6.09472152853892,
-24.6234375));
#306420=CARTESIAN_POINT('Ctrl Pts',(3.58238743130462,-4.93073329257084,
-24.5359375));
#306421=CARTESIAN_POINT('Ctrl Pts',(5.18447979493222,-3.76674505660277,
-24.4484375));
#306422=CARTESIAN_POINT('Ctrl Pts',(5.7964246247213,-1.88337252830138,-24.3609375));
#306423=CARTESIAN_POINT('Ctrl Pts',(6.40836945451038,1.31742351733884E-15,
-24.2734375));
#306424=CARTESIAN_POINT('Ctrl Pts',(5.7964246247213,1.88337252830138,-24.1859375));
#306425=CARTESIAN_POINT('Ctrl Pts',(5.18447979493222,3.76674505660277,-24.0984375));
#306426=CARTESIAN_POINT('Ctrl Pts',(3.58238743130462,4.93073329257085,-24.0109375));
#306427=CARTESIAN_POINT('Ctrl Pts',(1.98029506767702,6.09472152853892,-23.9234375));
#306428=CARTESIAN_POINT('Ctrl Pts',(0.,6.09472152853893,-23.8359375));
#306429=CARTESIAN_POINT('Ctrl Pts',(-1.98029506767702,6.09472152853892,
-23.7484375));
#306430=CARTESIAN_POINT('Ctrl Pts',(-3.58238743130462,4.93073329257085,
-23.6609375));
#306431=CARTESIAN_POINT('Ctrl Pts',(-5.18447979493222,3.76674505660277,
-23.5734375));
#306432=CARTESIAN_POINT('Ctrl Pts',(-5.7964246247213,1.88337252830138,-23.4859375));
#306433=CARTESIAN_POINT('Ctrl Pts',(-6.40836945451038,2.91434627708878E-15,
-23.3984375));
#306434=CARTESIAN_POINT('Ctrl Pts',(-5.7964246247213,-1.88337252830138,
-23.3109375));
#306435=CARTESIAN_POINT('Ctrl Pts',(-5.18447979493222,-3.76674505660276,
-23.2234375));
#306436=CARTESIAN_POINT('Ctrl Pts',(-3.58238743130462,-4.93073329257084,
-23.1359375));
#306437=CARTESIAN_POINT('Ctrl Pts',(-1.98029506767702,-6.09472152853892,
-23.0484375));
#306438=CARTESIAN_POINT('Ctrl Pts',(-7.46388121161966E-16,-6.09472152853892,
-22.9609375));
#306439=CARTESIAN_POINT('Ctrl Pts',(1.98029506767702,-6.09472152853892,
-22.8734375));
#306440=CARTESIAN_POINT('Ctrl Pts',(3.58238743130462,-4.93073329257084,
-22.7859375));
#306441=CARTESIAN_POINT('Ctrl Pts',(5.18447979493222,-3.76674505660277,
-22.6984375));
#306442=CARTESIAN_POINT('Ctrl Pts',(5.7964246247213,-1.88337252830138,-22.6109375));
#306443=CARTESIAN_POINT('Ctrl Pts',(6.40836945451038,1.37207338075079E-15,
-22.5234375));
#306444=CARTESIAN_POINT('Ctrl Pts',(5.7964246247213,1.88337252830138,-22.4359375));
#306445=CARTESIAN_POINT('Ctrl Pts',(5.18447979493222,3.76674505660277,-22.3484375));
#306446=CARTESIAN_POINT('Ctrl Pts',(3.58238743130462,4.93073329257085,-22.2609375));
#306447=CARTESIAN_POINT('Ctrl Pts',(1.98029506767702,6.09472152853892,-22.1734375));
#306448=CARTESIAN_POINT('Ctrl Pts',(0.,6.09472152853893,-22.0859375));
#306449=CARTESIAN_POINT('Ctrl Pts',(-1.98029506767702,6.09472152853892,
-21.9984375));
#306450=CARTESIAN_POINT('Ctrl Pts',(-3.58238743130462,4.93073329257085,
-21.9109375));
#306451=CARTESIAN_POINT('Ctrl Pts',(-5.18447979493222,3.76674505660277,
-21.8234375));
#306452=CARTESIAN_POINT('Ctrl Pts',(-5.7964246247213,1.88337252830138,-21.7359375));
#306453=CARTESIAN_POINT('Ctrl Pts',(-6.40836945451038,2.96899614050073E-15,
-21.6484375));
#306454=CARTESIAN_POINT('Ctrl Pts',(-5.7964246247213,-1.88337252830138,
-21.5609375));
#306455=CARTESIAN_POINT('Ctrl Pts',(-5.18447979493222,-3.76674505660276,
-21.4734375));
#306456=CARTESIAN_POINT('Ctrl Pts',(-3.58238743130462,-4.93073329257084,
-21.3859375));
#306457=CARTESIAN_POINT('Ctrl Pts',(-1.98029506767702,-6.09472152853892,
-21.2984375));
#306458=CARTESIAN_POINT('Ctrl Pts',(-7.46388121161966E-16,-6.09472152853892,
-21.2109375));
#306459=CARTESIAN_POINT('Ctrl Pts',(1.98029506767702,-6.09472152853892,
-21.1234375));
#306460=CARTESIAN_POINT('Ctrl Pts',(3.58238743130462,-4.93073329257084,
-21.0359375));
#306461=CARTESIAN_POINT('Ctrl Pts',(5.18447979493222,-3.76674505660277,
-20.9484375));
#306462=CARTESIAN_POINT('Ctrl Pts',(5.7964246247213,-1.88337252830138,-20.8609375));
#306463=CARTESIAN_POINT('Ctrl Pts',(6.40836945451038,1.42672324416274E-15,
-20.7734375));
#306464=CARTESIAN_POINT('Ctrl Pts',(5.7964246247213,1.88337252830138,-20.6859375));
#306465=CARTESIAN_POINT('Ctrl Pts',(5.18447979493222,3.76674505660277,-20.5984375));
#306466=CARTESIAN_POINT('Ctrl Pts',(3.58238743130462,4.93073329257085,-20.5109375));
#306467=CARTESIAN_POINT('Ctrl Pts',(1.98029506767702,6.09472152853892,-20.4234375));
#306468=CARTESIAN_POINT('Ctrl Pts',(0.,6.09472152853893,-20.3359375));
#306469=CARTESIAN_POINT('Ctrl Pts',(-1.98029506767702,6.09472152853892,
-20.2484375));
#306470=CARTESIAN_POINT('Ctrl Pts',(-3.58238743130462,4.93073329257085,
-20.1609375));
#306471=CARTESIAN_POINT('Ctrl Pts',(-5.18447979493222,3.76674505660277,
-20.0734375));
#306472=CARTESIAN_POINT('Ctrl Pts',(-5.7964246247213,1.88337252830138,-19.9859375));
#306473=CARTESIAN_POINT('Ctrl Pts',(-6.40836945451038,3.02364600391268E-15,
-19.8984375));
#306474=CARTESIAN_POINT('Ctrl Pts',(-5.7964246247213,-1.88337252830138,
-19.8109375));
#306475=CARTESIAN_POINT('Ctrl Pts',(-5.18447979493222,-3.76674505660276,
-19.7234375));
#306476=CARTESIAN_POINT('Ctrl Pts',(-3.58238743130462,-4.93073329257084,
-19.6359375));
#306477=CARTESIAN_POINT('Ctrl Pts',(-1.98029506767702,-6.09472152853892,
-19.5484375));
#306478=CARTESIAN_POINT('Ctrl Pts',(-7.46388121161966E-16,-6.09472152853892,
-19.4609375));
#306479=CARTESIAN_POINT('Ctrl Pts',(1.98029506767702,-6.09472152853892,
-19.3734375));
#306480=CARTESIAN_POINT('Ctrl Pts',(3.58238743130462,-4.93073329257084,
-19.2859375));
#306481=CARTESIAN_POINT('Ctrl Pts',(5.18447979493222,-3.76674505660277,
-19.1984375));
#306482=CARTESIAN_POINT('Ctrl Pts',(5.7964246247213,-1.88337252830138,-19.1109375));
#306483=CARTESIAN_POINT('Ctrl Pts',(6.40836945451038,1.48137310757469E-15,
-19.0234375));
#306484=CARTESIAN_POINT('Ctrl Pts',(5.7964246247213,1.88337252830138,-18.9359375));
#306485=CARTESIAN_POINT('Ctrl Pts',(5.18447979493222,3.76674505660277,-18.8484375));
#306486=CARTESIAN_POINT('Ctrl Pts',(3.58238743130462,4.93073329257085,-18.7609375));
#306487=CARTESIAN_POINT('Ctrl Pts',(1.98029506767702,6.09472152853892,-18.6734375));
#306488=CARTESIAN_POINT('Ctrl Pts',(0.,6.09472152853893,-18.5859375));
#306489=CARTESIAN_POINT('Ctrl Pts',(-1.98029506767702,6.09472152853892,
-18.4984375));
#306490=CARTESIAN_POINT('Ctrl Pts',(-3.58238743130462,4.93073329257085,
-18.4109375));
#306491=CARTESIAN_POINT('Ctrl Pts',(-5.18447979493222,3.76674505660277,
-18.3234375));
#306492=CARTESIAN_POINT('Ctrl Pts',(-5.7964246247213,1.88337252830138,-18.2359375));
#306493=CARTESIAN_POINT('Ctrl Pts',(-6.40836945451038,3.07829586732463E-15,
-18.1484375));
#306494=CARTESIAN_POINT('Ctrl Pts',(-5.7964246247213,-1.88337252830138,
-18.0609375));
#306495=CARTESIAN_POINT('Ctrl Pts',(-5.18447979493222,-3.76674505660276,
-17.9734375));
#306496=CARTESIAN_POINT('Ctrl Pts',(-3.58238743130462,-4.93073329257084,
-17.8859375));
#306497=CARTESIAN_POINT('Ctrl Pts',(-1.98029506767702,-6.09472152853892,
-17.7984375));
#306498=CARTESIAN_POINT('Ctrl Pts',(-7.46388121161966E-16,-6.09472152853892,
-17.7109375));
#306499=CARTESIAN_POINT('Ctrl Pts',(1.98029506767702,-6.09472152853892,
-17.6234375));
#306500=CARTESIAN_POINT('Ctrl Pts',(3.58238743130462,-4.93073329257084,
-17.5359375));
#306501=CARTESIAN_POINT('Ctrl Pts',(5.18447979493222,-3.76674505660277,
-17.4484375));
#306502=CARTESIAN_POINT('Ctrl Pts',(5.7964246247213,-1.88337252830138,-17.3609375));
#306503=CARTESIAN_POINT('Ctrl Pts',(6.40836945451038,1.53602297098664E-15,
-17.2734375));
#306504=CARTESIAN_POINT('Ctrl Pts',(5.7964246247213,1.88337252830138,-17.1859375));
#306505=CARTESIAN_POINT('Ctrl Pts',(5.18447979493222,3.76674505660277,-17.0984375));
#306506=CARTESIAN_POINT('Ctrl Pts',(3.58238743130462,4.93073329257085,-17.0109375));
#306507=CARTESIAN_POINT('Ctrl Pts',(1.98029506767702,6.09472152853892,-16.9234375));
#306508=CARTESIAN_POINT('Ctrl Pts',(0.,6.09472152853893,-16.8359375));
#306509=CARTESIAN_POINT('Ctrl Pts',(-1.98029506767702,6.09472152853892,
-16.7484375));
#306510=CARTESIAN_POINT('Ctrl Pts',(-3.58238743130462,4.93073329257085,
-16.6609375));
#306511=CARTESIAN_POINT('Ctrl Pts',(-5.18447979493222,3.76674505660277,
-16.5734375));
#306512=CARTESIAN_POINT('Ctrl Pts',(-5.7964246247213,1.88337252830138,-16.4859375));
#306513=CARTESIAN_POINT('Ctrl Pts',(-6.40836945451038,3.13294573073658E-15,
-16.3984375));
#306514=CARTESIAN_POINT('Ctrl Pts',(-5.7964246247213,-1.88337252830138,
-16.3109375));
#306515=CARTESIAN_POINT('Ctrl Pts',(-5.18447979493222,-3.76674505660276,
-16.2234375));
#306516=CARTESIAN_POINT('Ctrl Pts',(-3.58238743130462,-4.93073329257084,
-16.1359375));
#306517=CARTESIAN_POINT('Ctrl Pts',(-1.98029506767702,-6.09472152853892,
-16.0484375));
#306518=CARTESIAN_POINT('Ctrl Pts',(-7.46388121161966E-16,-6.09472152853892,
-15.9609375));
#306519=CARTESIAN_POINT('Ctrl Pts',(1.98029506767702,-6.09472152853892,
-15.8734375));
#306520=CARTESIAN_POINT('Ctrl Pts',(3.58238743130462,-4.93073329257084,
-15.7859375));
#306521=CARTESIAN_POINT('Ctrl Pts',(5.18447979493222,-3.76674505660277,
-15.6984375));
#306522=CARTESIAN_POINT('Ctrl Pts',(5.7964246247213,-1.88337252830138,-15.6109375));
#306523=CARTESIAN_POINT('Ctrl Pts',(6.40836945451038,1.59067283439859E-15,
-15.5234375));
#306524=CARTESIAN_POINT('Ctrl Pts',(5.7964246247213,1.88337252830138,-15.4359375));
#306525=CARTESIAN_POINT('Ctrl Pts',(5.18447979493222,3.76674505660277,-15.3484375));
#306526=CARTESIAN_POINT('Ctrl Pts',(3.58238743130462,4.93073329257085,-15.2609375));
#306527=CARTESIAN_POINT('Ctrl Pts',(1.98029506767702,6.09472152853892,-15.1734375));
#306528=CARTESIAN_POINT('Ctrl Pts',(0.,6.09472152853893,-15.0859375));
#306529=CARTESIAN_POINT('Ctrl Pts',(-1.98029506767702,6.09472152853892,
-14.9984375));
#306530=CARTESIAN_POINT('Ctrl Pts',(-3.58238743130462,4.93073329257085,
-14.9109375));
#306531=CARTESIAN_POINT('Ctrl Pts',(-5.18447979493222,3.76674505660277,
-14.8234375));
#306532=CARTESIAN_POINT('Ctrl Pts',(-5.7964246247213,1.88337252830138,-14.7359375));
#306533=CARTESIAN_POINT('Ctrl Pts',(-6.40836945451038,3.18759559414853E-15,
-14.6484375));
#306534=CARTESIAN_POINT('Ctrl Pts',(-5.7964246247213,-1.88337252830138,
-14.5609375));
#306535=CARTESIAN_POINT('Ctrl Pts',(-5.18447979493222,-3.76674505660276,
-14.4734375));
#306536=CARTESIAN_POINT('Ctrl Pts',(-3.58238743130462,-4.93073329257084,
-14.3859375));
#306537=CARTESIAN_POINT('Ctrl Pts',(-1.98029506767702,-6.09472152853892,
-14.2984375));
#306538=CARTESIAN_POINT('Ctrl Pts',(-7.46388121161966E-16,-6.09472152853892,
-14.2109375));
#306539=CARTESIAN_POINT('Ctrl Pts',(1.98029506767702,-6.09472152853892,
-14.1234375));
#306540=CARTESIAN_POINT('Ctrl Pts',(3.58238743130462,-4.93073329257084,
-14.0359375));
#306541=CARTESIAN_POINT('Ctrl Pts',(5.18447979493222,-3.76674505660277,
-13.9484375));
#306542=CARTESIAN_POINT('Ctrl Pts',(5.7964246247213,-1.88337252830138,-13.8609375));
#306543=CARTESIAN_POINT('Ctrl Pts',(6.40836945451038,1.64532269781054E-15,
-13.7734375));
#306544=CARTESIAN_POINT('Ctrl Pts',(5.7964246247213,1.88337252830138,-13.6859375));
#306545=CARTESIAN_POINT('Ctrl Pts',(5.18447979493222,3.76674505660277,-13.5984375));
#306546=CARTESIAN_POINT('Ctrl Pts',(3.58238743130462,4.93073329257085,-13.5109375));
#306547=CARTESIAN_POINT('Ctrl Pts',(1.98029506767702,6.09472152853892,-13.4234375));
#306548=CARTESIAN_POINT('Ctrl Pts',(0.,6.09472152853893,-13.3359375));
#306549=CARTESIAN_POINT('Ctrl Pts',(-1.98029506767702,6.09472152853892,
-13.2484375));
#306550=CARTESIAN_POINT('Ctrl Pts',(-3.58238743130462,4.93073329257085,
-13.1609375));
#306551=CARTESIAN_POINT('Ctrl Pts',(-5.18447979493222,3.76674505660277,
-13.0734375));
#306552=CARTESIAN_POINT('Ctrl Pts',(-5.7964246247213,1.88337252830138,-12.9859375));
#306553=CARTESIAN_POINT('Ctrl Pts',(-6.40836945451038,3.24224545756048E-15,
-12.8984375));
#306554=CARTESIAN_POINT('Ctrl Pts',(-5.7964246247213,-1.88337252830138,
-12.8109375));
#306555=CARTESIAN_POINT('Ctrl Pts',(-5.18447979493222,-3.76674505660276,
-12.7234375));
#306556=CARTESIAN_POINT('Ctrl Pts',(-3.58238743130462,-4.93073329257084,
-12.6359375));
#306557=CARTESIAN_POINT('Ctrl Pts',(-1.98029506767702,-6.09472152853892,
-12.5484375));
#306558=CARTESIAN_POINT('Ctrl Pts',(-7.46388121161966E-16,-6.09472152853892,
-12.4609375));
#306559=CARTESIAN_POINT('Ctrl Pts',(1.98029506767702,-6.09472152853892,
-12.3734375));
#306560=CARTESIAN_POINT('Ctrl Pts',(3.58238743130462,-4.93073329257084,
-12.2859375));
#306561=CARTESIAN_POINT('Ctrl Pts',(5.18447979493222,-3.76674505660277,
-12.1984375));
#306562=CARTESIAN_POINT('Ctrl Pts',(5.7964246247213,-1.88337252830138,-12.1109375));
#306563=CARTESIAN_POINT('Ctrl Pts',(6.40836945451038,1.69997256122249E-15,
-12.0234375));
#306564=CARTESIAN_POINT('Ctrl Pts',(5.7964246247213,1.88337252830138,-11.9359375));
#306565=CARTESIAN_POINT('Ctrl Pts',(5.18447979493222,3.76674505660277,-11.8484375));
#306566=CARTESIAN_POINT('Ctrl Pts',(3.58238743130462,4.93073329257085,-11.7609375));
#306567=CARTESIAN_POINT('Ctrl Pts',(1.98029506767702,6.09472152853892,-11.6734375));
#306568=CARTESIAN_POINT('Ctrl Pts',(0.,6.09472152853893,-11.5859375));
#306569=CARTESIAN_POINT('Ctrl Pts',(-1.98029506767702,6.09472152853892,
-11.4984375));
#306570=CARTESIAN_POINT('Ctrl Pts',(-3.58238743130462,4.93073329257085,
-11.4109375));
#306571=CARTESIAN_POINT('Ctrl Pts',(-5.18447979493222,3.76674505660277,
-11.3234375));
#306572=CARTESIAN_POINT('Ctrl Pts',(-5.7964246247213,1.88337252830138,-11.2359375));
#306573=CARTESIAN_POINT('Ctrl Pts',(-6.40836945451038,3.29689532097243E-15,
-11.1484375));
#306574=CARTESIAN_POINT('Ctrl Pts',(-5.7964246247213,-1.88337252830138,
-11.0609375));
#306575=CARTESIAN_POINT('Ctrl Pts',(-5.18447979493222,-3.76674505660276,
-10.9734375));
#306576=CARTESIAN_POINT('Ctrl Pts',(-3.58238743130462,-4.93073329257084,
-10.8859375));
#306577=CARTESIAN_POINT('Ctrl Pts',(-1.98029506767702,-6.09472152853892,
-10.7984375));
#306578=CARTESIAN_POINT('Ctrl Pts',(-7.46388121161966E-16,-6.09472152853892,
-10.7109375));
#306579=CARTESIAN_POINT('Ctrl Pts',(1.98029506767702,-6.09472152853892,
-10.6234375));
#306580=CARTESIAN_POINT('Ctrl Pts',(3.58238743130462,-4.93073329257084,
-10.5359375));
#306581=CARTESIAN_POINT('Ctrl Pts',(5.18447979493222,-3.76674505660277,
-10.4484375));
#306582=CARTESIAN_POINT('Ctrl Pts',(5.7964246247213,-1.88337252830138,-10.3609375));
#306583=CARTESIAN_POINT('Ctrl Pts',(6.40836945451038,1.75462242463444E-15,
-10.2734375));
#306584=CARTESIAN_POINT('Ctrl Pts',(5.7964246247213,1.88337252830138,-10.1859375));
#306585=CARTESIAN_POINT('Ctrl Pts',(5.18447979493222,3.76674505660277,-10.0984375));
#306586=CARTESIAN_POINT('Ctrl Pts',(3.58238743130462,4.93073329257085,-10.0109375));
#306587=CARTESIAN_POINT('Ctrl Pts',(1.98029506767702,6.09472152853892,-9.9234375));
#306588=CARTESIAN_POINT('Ctrl Pts',(0.,6.09472152853893,-9.8359375));
#306589=CARTESIAN_POINT('Ctrl Pts',(-1.98029506767702,6.09472152853892,
-9.74843749999999));
#306590=CARTESIAN_POINT('Ctrl Pts',(-3.58238743130462,4.93073329257085,
-9.6609375));
#306591=CARTESIAN_POINT('Ctrl Pts',(-5.18447979493222,3.76674505660277,
-9.57343749999999));
#306592=CARTESIAN_POINT('Ctrl Pts',(-5.7964246247213,1.88337252830138,-9.4859375));
#306593=CARTESIAN_POINT('Ctrl Pts',(-6.40836945451038,3.35154518438438E-15,
-9.39843749999999));
#306594=CARTESIAN_POINT('Ctrl Pts',(-5.7964246247213,-1.88337252830138,
-9.3109375));
#306595=CARTESIAN_POINT('Ctrl Pts',(-5.18447979493222,-3.76674505660276,
-9.2234375));
#306596=CARTESIAN_POINT('Ctrl Pts',(-3.58238743130462,-4.93073329257084,
-9.1359375));
#306597=CARTESIAN_POINT('Ctrl Pts',(-1.98029506767702,-6.09472152853892,
-9.0484375));
#306598=CARTESIAN_POINT('Ctrl Pts',(-7.46388121161966E-16,-6.09472152853892,
-8.9609375));
#306599=CARTESIAN_POINT('Ctrl Pts',(1.98029506767702,-6.09472152853892,
-8.8734375));
#306600=CARTESIAN_POINT('Ctrl Pts',(3.58238743130462,-4.93073329257084,
-8.7859375));
#306601=CARTESIAN_POINT('Ctrl Pts',(5.18447979493222,-3.76674505660277,
-8.6984375));
#306602=CARTESIAN_POINT('Ctrl Pts',(5.7964246247213,-1.88337252830138,-8.6109375));
#306603=CARTESIAN_POINT('Ctrl Pts',(6.40836945451038,1.80927228804639E-15,
-8.5234375));
#306604=CARTESIAN_POINT('Ctrl Pts',(5.7964246247213,1.88337252830138,-8.4359375));
#306605=CARTESIAN_POINT('Ctrl Pts',(5.18447979493222,3.76674505660277,-8.34843749999999));
#306606=CARTESIAN_POINT('Ctrl Pts',(3.58238743130462,4.93073329257085,-8.2609375));
#306607=CARTESIAN_POINT('Ctrl Pts',(1.98029506767702,6.09472152853892,-8.1734375));
#306608=CARTESIAN_POINT('Ctrl Pts',(0.,6.09472152853893,-8.0859375));
#306609=CARTESIAN_POINT('Ctrl Pts',(-1.98029506767702,6.09472152853892,
-7.9984375));
#306610=CARTESIAN_POINT('Ctrl Pts',(-3.58238743130462,4.93073329257085,
-7.9109375));
#306611=CARTESIAN_POINT('Ctrl Pts',(-5.18447979493222,3.76674505660277,
-7.8234375));
#306612=CARTESIAN_POINT('Ctrl Pts',(-5.7964246247213,1.88337252830138,-7.7359375));
#306613=CARTESIAN_POINT('Ctrl Pts',(-6.40836945451038,3.40619504779633E-15,
-7.64843749999999));
#306614=CARTESIAN_POINT('Ctrl Pts',(-5.7964246247213,-1.88337252830138,
-7.5609375));
#306615=CARTESIAN_POINT('Ctrl Pts',(-5.18447979493222,-3.76674505660276,
-7.47343749999999));
#306616=CARTESIAN_POINT('Ctrl Pts',(-3.58238743130462,-4.93073329257084,
-7.3859375));
#306617=CARTESIAN_POINT('Ctrl Pts',(-1.98029506767702,-6.09472152853892,
-7.2984375));
#306618=CARTESIAN_POINT('Ctrl Pts',(-7.46388121161966E-16,-6.09472152853892,
-7.2109375));
#306619=CARTESIAN_POINT('Ctrl Pts',(1.98029506767702,-6.09472152853892,
-7.1234375));
#306620=CARTESIAN_POINT('Ctrl Pts',(3.58238743130462,-4.93073329257084,
-7.0359375));
#306621=CARTESIAN_POINT('Ctrl Pts',(5.18447979493222,-3.76674505660277,
-6.9484375));
#306622=CARTESIAN_POINT('Ctrl Pts',(5.7964246247213,-1.88337252830138,-6.8609375));
#306623=CARTESIAN_POINT('Ctrl Pts',(6.40836945451038,1.86392215145835E-15,
-6.7734375));
#306624=CARTESIAN_POINT('Ctrl Pts',(5.7964246247213,1.88337252830138,-6.6859375));
#306625=CARTESIAN_POINT('Ctrl Pts',(5.18447979493222,3.76674505660277,-6.59843749999999));
#306626=CARTESIAN_POINT('Ctrl Pts',(3.58238743130462,4.93073329257085,-6.5109375));
#306627=CARTESIAN_POINT('Ctrl Pts',(1.98029506767702,6.09472152853892,-6.4234375));
#306628=CARTESIAN_POINT('Ctrl Pts',(0.,6.09472152853893,-6.3359375));
#306629=CARTESIAN_POINT('Ctrl Pts',(-1.98029506767702,6.09472152853892,
-6.2484375));
#306630=CARTESIAN_POINT('Ctrl Pts',(-3.58238743130462,4.93073329257085,
-6.1609375));
#306631=CARTESIAN_POINT('Ctrl Pts',(-4.25030673465153,4.4454615134136,-6.12445836785401));
#306632=CARTESIAN_POINT('Ctrl Pts',(-4.76505439612012,3.79998514634624,
-6.08614055662269));
#306633=CARTESIAN_POINT('Ctrl Pts',(6.66133814775094E-15,6.00000000000001,
-8.03125));
#306634=CARTESIAN_POINT('Ctrl Pts',(-0.298350089586693,6.00000000000001,
-8.01785918726406));
#306635=CARTESIAN_POINT('Ctrl Pts',(-0.596925028388715,5.97774819526054,
-8.00413377716093));
#306636=CARTESIAN_POINT('Ctrl Pts',(-1.66924937211483,5.81630856274366,
-7.95365043907342));
#306637=CARTESIAN_POINT('Ctrl Pts',(-2.41486229564473,5.54836098887262,
-7.91627761124828));
#306638=CARTESIAN_POINT('Ctrl Pts',(-3.75967261426721,4.74120264916727,
-7.84414758536147));
#306639=CARTESIAN_POINT('Ctrl Pts',(-4.34613026038862,4.21014287943788,
-7.8089338812994));
#306640=CARTESIAN_POINT('Ctrl Pts',(-5.27616152650459,2.96004444542891,
-7.73540726990233));
#306641=CARTESIAN_POINT('Ctrl Pts',(-5.61376950107607,2.2550567903524,-7.70017212388947));
#306642=CARTESIAN_POINT('Ctrl Pts',(-6.00669408698858,0.739124739792806,
-7.62863126106828));
#306643=CARTESIAN_POINT('Ctrl Pts',(-6.05170607345556,-0.0589509747342593,
-7.59096794681035));
#306644=CARTESIAN_POINT('Ctrl Pts',(-5.83151436888551,-1.61117175748842,
-7.51771452226127));
#306645=CARTESIAN_POINT('Ctrl Pts',(-5.57442451266052,-2.35121606288477,
-7.48361115339666));
#306646=CARTESIAN_POINT('Ctrl Pts',(-4.79076292912546,-3.69551058096904,
-7.4105483376614));
#306647=CARTESIAN_POINT('Ctrl Pts',(-4.27036201929517,-4.28629300582258,
-7.37355698610541));
#306648=CARTESIAN_POINT('Ctrl Pts',(-3.02301551530211,-5.24296670219167,
-7.30243117764194));
#306649=CARTESIAN_POINT('Ctrl Pts',(-2.30522251047422,-5.59584071305071,
-7.26560902624741));
#306650=CARTESIAN_POINT('Ctrl Pts',(-0.792137449271004,-5.99755024079105,
-7.19183913962938));
#306651=CARTESIAN_POINT('Ctrl Pts',(-0.0133123538000254,-6.04962216438536,
-7.1575711534076));
#306652=CARTESIAN_POINT('Ctrl Pts',(1.53424879406655,-5.85360958345414,
-7.08525362770043));
#306653=CARTESIAN_POINT('Ctrl Pts',(2.28757340913091,-5.60229241516888,
-7.04777720365975));
#306654=CARTESIAN_POINT('Ctrl Pts',(3.64967592975576,-4.82599117489345,
-6.97532105322719));
#306655=CARTESIAN_POINT('Ctrl Pts',(4.24636514478383,-4.31030147320438,
-6.94052530193557));
#306656=CARTESIAN_POINT('Ctrl Pts',(5.20498502284638,-3.08375106151128,
-6.86710472233009));
#306657=CARTESIAN_POINT('Ctrl Pts',(5.55955074770865,-2.38593173989502,
-6.8313484606247));
#306658=CARTESIAN_POINT('Ctrl Pts',(5.98838803540964,-0.876802577728364,
-6.7601286441889));
#306659=CARTESIAN_POINT('Ctrl Pts',(6.05172653326255,-0.0780941398890815,
-6.72243547003608));
#306660=CARTESIAN_POINT('Ctrl Pts',(5.86620171282064,1.47928141572156,-6.64893877805449));
#306661=CARTESIAN_POINT('Ctrl Pts',(5.62630539476616,2.22379961680138,-6.61491500177162));
#306662=CARTESIAN_POINT('Ctrl Pts',(4.87340782866889,3.58619747205795,-6.54201437438082));
#306663=CARTESIAN_POINT('Ctrl Pts',(4.36528719811434,4.18989905677479,-6.50487041815271));
#306664=CARTESIAN_POINT('Ctrl Pts',(3.1405741703139,5.17290477810806,-6.43336709522222));
#306665=CARTESIAN_POINT('Ctrl Pts',(2.43405248916498,5.54054391885069,-6.39719769893698));
#306666=CARTESIAN_POINT('Ctrl Pts',(1.13079062593595,5.91984127184233,-6.33317212698165));
#306667=CARTESIAN_POINT('Ctrl Pts',(0.566258670473045,6.00000000000003,
-6.30666532274017));
#306668=CARTESIAN_POINT('Ctrl Pts',(-2.35089725464377E-13,6.00000000000001,
-6.28124999999999));
#306669=CARTESIAN_POINT('Ctrl Pts',(-0.683563368987388,5.96093458449081,
-6.24999999999999));
#306670=CARTESIAN_POINT('Ctrl Pts',(-0.0383159840272598,6.02151021407911,
-6.2722728378837));
#306671=CARTESIAN_POINT('Ctrl Pts',(0.613802036334531,5.97768570738805,
-6.29369507965025));
#306672=CARTESIAN_POINT('Ctrl Pts',(1.86095346059866,5.68339189538494,-6.33868681212296));
#306673=CARTESIAN_POINT('Ctrl Pts',(2.44827655643883,5.44153698589087,-6.36115046126864));
#306674=CARTESIAN_POINT('Ctrl Pts',(3.31527595182957,4.91053707074575,-6.3964523351205));
#306675=CARTESIAN_POINT('Ctrl Pts',(3.62530031161791,4.67669984037455,-6.40939585433822));
#306676=CARTESIAN_POINT('Ctrl Pts',(4.46934833248225,3.89702715050554,-6.44942871893781));
#306677=CARTESIAN_POINT('Ctrl Pts',(4.92290194524358,3.27617829245186,-6.47696465561948));
#306678=CARTESIAN_POINT('Ctrl Pts',(5.40410302848904,2.24559647875469,-6.517292807541));
#306679=CARTESIAN_POINT('Ctrl Pts',(5.53060158549463,1.88938934315057,-6.53018354451336));
#306680=CARTESIAN_POINT('Ctrl Pts',(5.74574294589262,1.02496405516718,-6.56123991687386));
#306681=CARTESIAN_POINT('Ctrl Pts',(5.80264385515304,0.512322540210554,
-6.57975809488675));
#306682=CARTESIAN_POINT('Ctrl Pts',(5.79150251002447,-4.08715104815993E-8,
-6.59837392003554));
#306683=CARTESIAN_POINT('Origin',(-3.81730450148946E-15,-2.22044604925031E-15,
-37.015625));
#306684=CARTESIAN_POINT('Origin',(0.,0.,36.25));
#306685=CARTESIAN_POINT('',(-1.53209212662338,6.06688311688312,36.25));
#306686=CARTESIAN_POINT('',(-2.04107142857143,5.43420251623377,36.25));
#306687=CARTESIAN_POINT('Ctrl Pts',(-1.53209212662338,6.06688311688312,
36.25));
#306688=CARTESIAN_POINT('Ctrl Pts',(-1.54951650473831,6.066434027441,36.25));
#306689=CARTESIAN_POINT('Ctrl Pts',(-1.58393065600793,6.06554704990339,
36.25));
#306690=CARTESIAN_POINT('Ctrl Pts',(-1.63443083923324,6.05712286492333,
36.25));
#306691=CARTESIAN_POINT('Ctrl Pts',(-1.68245238910184,6.04224031339717,
36.25));
#306692=CARTESIAN_POINT('Ctrl Pts',(-1.72937966613072,6.02430730620351,
36.25));
#306693=CARTESIAN_POINT('Ctrl Pts',(-1.77322121904902,5.9981366813217,36.25));
#306694=CARTESIAN_POINT('Ctrl Pts',(-1.81610239307926,5.96827285277195,
36.25));
#306695=CARTESIAN_POINT('Ctrl Pts',(-1.85592360031061,5.93155196527191,
36.25));
#306696=CARTESIAN_POINT('Ctrl Pts',(-1.89389884878363,5.89060348709459,
36.25));
#306697=CARTESIAN_POINT('Ctrl Pts',(-1.92842298904565,5.84507968533497,
36.25));
#306698=CARTESIAN_POINT('Ctrl Pts',(-1.95895617838667,5.79605922055842,
36.25));
#306699=CARTESIAN_POINT('Ctrl Pts',(-1.98409150523322,5.74343345049149,
36.25));
#306700=CARTESIAN_POINT('Ctrl Pts',(-2.00454652849223,5.68767671276928,
36.25));
#306701=CARTESIAN_POINT('Ctrl Pts',(-2.02161548775311,5.6290296721576,36.25));
#306702=CARTESIAN_POINT('Ctrl Pts',(-2.03309476195626,5.56687880407454,
36.25));
#306703=CARTESIAN_POINT('Ctrl Pts',(-2.03932413346711,5.50155035955671,
36.25));
#306704=CARTESIAN_POINT('Ctrl Pts',(-2.04048048892973,5.45697972788144,
36.25));
#306705=CARTESIAN_POINT('Ctrl Pts',(-2.04107142857143,5.43420251623377,
36.25));
#306706=CARTESIAN_POINT('',(-1.52371651785714,4.78863636363636,36.25));
#306707=CARTESIAN_POINT('Ctrl Pts',(-2.04107142857143,5.43420251623377,
36.25));
#306708=CARTESIAN_POINT('Ctrl Pts',(-2.0405543266768,5.41055942108448,36.25));
#306709=CARTESIAN_POINT('Ctrl Pts',(-2.03954125408768,5.36423939815085,
36.25));
#306710=CARTESIAN_POINT('Ctrl Pts',(-2.03228105709878,5.2966367303295,36.25));
#306711=CARTESIAN_POINT('Ctrl Pts',(-2.02107341871046,5.23250639408275,
36.25));
#306712=CARTESIAN_POINT('Ctrl Pts',(-2.00398348773993,5.17226185872411,
36.25));
#306713=CARTESIAN_POINT('Ctrl Pts',(-1.98289443792092,5.11515155101266,
36.25));
#306714=CARTESIAN_POINT('Ctrl Pts',(-1.95643257885054,5.06166487648077,
36.25));
#306715=CARTESIAN_POINT('Ctrl Pts',(-1.92516888970118,5.0117585395718,36.25));
#306716=CARTESIAN_POINT('Ctrl Pts',(-1.89024117171633,4.96538056994282,
36.25));
#306717=CARTESIAN_POINT('Ctrl Pts',(-1.85077488100797,4.9247537203412,36.25));
#306718=CARTESIAN_POINT('Ctrl Pts',(-1.81007783686995,4.8879898300525,36.25));
#306719=CARTESIAN_POINT('Ctrl Pts',(-1.76718752939314,4.85710381362087,
36.25));
#306720=CARTESIAN_POINT('Ctrl Pts',(-1.72190013812572,4.83218747720399,
36.25));
#306721=CARTESIAN_POINT('Ctrl Pts',(-1.67490398148407,4.81303741070313,
36.25));
#306722=CARTESIAN_POINT('Ctrl Pts',(-1.62621370039499,4.79855444913016,
36.25));
#306723=CARTESIAN_POINT('Ctrl Pts',(-1.57556683534013,4.78994040169141,
36.25));
#306724=CARTESIAN_POINT('Ctrl Pts',(-1.54114485828132,4.789074687262,36.25));
#306725=CARTESIAN_POINT('Ctrl Pts',(-1.52371651785714,4.78863636363636,
36.25));
#306726=CARTESIAN_POINT('',(-1.01022727272727,5.42131696428571,36.25));
#306727=CARTESIAN_POINT('Ctrl Pts',(-1.52371651785714,4.78863636363636,
36.25));
#306728=CARTESIAN_POINT('Ctrl Pts',(-1.50606613811182,4.78904075129562,
36.25));
#306729=CARTESIAN_POINT('Ctrl Pts',(-1.4714149990235,4.78983464316812,36.25));
#306730=CARTESIAN_POINT('Ctrl Pts',(-1.42050302431008,4.79884546139153,
36.25));
#306731=CARTESIAN_POINT('Ctrl Pts',(-1.37159611734391,4.81206099883602,
36.25));
#306732=CARTESIAN_POINT('Ctrl Pts',(-1.32477571753144,4.83107657862712,
36.25));
#306733=CARTESIAN_POINT('Ctrl Pts',(-1.27989304559387,4.85499849822356,
36.25));
#306734=CARTESIAN_POINT('Ctrl Pts',(-1.23739271777899,4.88475706229418,
36.25));
#306735=CARTESIAN_POINT('Ctrl Pts',(-1.19710037531277,4.92023184841449,
36.25));
#306736=CARTESIAN_POINT('Ctrl Pts',(-1.15864753037992,4.96016808484432,
36.25));
#306737=CARTESIAN_POINT('Ctrl Pts',(-1.12433596830973,5.00550562421531,
36.25));
#306738=CARTESIAN_POINT('Ctrl Pts',(-1.09262300577192,5.05353436556821,
36.25));
#306739=CARTESIAN_POINT('Ctrl Pts',(-1.0681718193395,5.10649857927001,36.25));
#306740=CARTESIAN_POINT('Ctrl Pts',(-1.04618243948374,5.16193679017606,
36.25));
#306741=CARTESIAN_POINT('Ctrl Pts',(-1.03075200559165,5.22177284922642,
36.25));
#306742=CARTESIAN_POINT('Ctrl Pts',(-1.0178443165815,5.28488392294487,36.25));
#306743=CARTESIAN_POINT('Ctrl Pts',(-1.01206974131962,5.35205975094169,
36.25));
#306744=CARTESIAN_POINT('Ctrl Pts',(-1.01085017356999,5.39790252089427,
36.25));
#306745=CARTESIAN_POINT('Ctrl Pts',(-1.01022727272727,5.42131696428571,
36.25));
#306746=CARTESIAN_POINT('Ctrl Pts',(-1.01022727272727,5.42131696428571,
36.25));
#306747=CARTESIAN_POINT('Ctrl Pts',(-1.01076599462072,5.44495600403826,
36.25));
#306748=CARTESIAN_POINT('Ctrl Pts',(-1.0118214237133,5.49126808190085,36.25));
#306749=CARTESIAN_POINT('Ctrl Pts',(-1.01878267475616,5.55896687878814,
36.25));
#306750=CARTESIAN_POINT('Ctrl Pts',(-1.03107800379365,5.62293356367208,
36.25));
#306751=CARTESIAN_POINT('Ctrl Pts',(-1.04789745408079,5.68327106051297,
36.25));
#306752=CARTESIAN_POINT('Ctrl Pts',(-1.06908652243424,5.74035420483588,
36.25));
#306753=CARTESIAN_POINT('Ctrl Pts',(-1.09547159489994,5.79399835274014,
36.25));
#306754=CARTESIAN_POINT('Ctrl Pts',(-1.12719592427129,5.8437725973715,36.25));
#306755=CARTESIAN_POINT('Ctrl Pts',(-1.1634661665603,5.88934000071629,36.25));
#306756=CARTESIAN_POINT('Ctrl Pts',(-1.20222138279797,5.93098943621083,
36.25));
#306757=CARTESIAN_POINT('Ctrl Pts',(-1.24358478999076,5.96739207884556,
36.25));
#306758=CARTESIAN_POINT('Ctrl Pts',(-1.28715520747738,5.99780008387924,
36.25));
#306759=CARTESIAN_POINT('Ctrl Pts',(-1.33229168731682,6.02332207855003,
36.25));
#306760=CARTESIAN_POINT('Ctrl Pts',(-1.37963229428386,6.04244867323907,
36.25));
#306761=CARTESIAN_POINT('Ctrl Pts',(-1.42850133450328,6.05706063884487,
36.25));
#306762=CARTESIAN_POINT('Ctrl Pts',(-1.47960608156579,6.0655628055813,36.25));
#306763=CARTESIAN_POINT('Ctrl Pts',(-1.51445101604866,6.06643934639816,
36.25));
#306764=CARTESIAN_POINT('Ctrl Pts',(-1.53209212662338,6.06688311688312,
36.25));
#306765=CARTESIAN_POINT('Origin',(0.,0.,36.25));
#306766=CARTESIAN_POINT('',(-1.52758218344156,7.38636363636364,36.25));
#306767=CARTESIAN_POINT('',(-1.91737012987013,6.90444399350649,36.25));
#306768=CARTESIAN_POINT('Ctrl Pts',(-1.52758218344156,7.38636363636364,
36.25));
#306769=CARTESIAN_POINT('Ctrl Pts',(-1.55358237022155,7.38486930154146,
36.25));
#306770=CARTESIAN_POINT('Ctrl Pts',(-1.60499794902611,7.38191424239284,
36.25));
#306771=CARTESIAN_POINT('Ctrl Pts',(-1.67863965341545,7.354443366284,36.25));
#306772=CARTESIAN_POINT('Ctrl Pts',(-1.74575926016136,7.30974046602882,
36.25));
#306773=CARTESIAN_POINT('Ctrl Pts',(-1.80513211335571,7.24931351323173,
36.25));
#306774=CARTESIAN_POINT('Ctrl Pts',(-1.85584586752056,7.17700242184242,
36.25));
#306775=CARTESIAN_POINT('Ctrl Pts',(-1.8909492802511,7.09344714231162,36.25));
#306776=CARTESIAN_POINT('Ctrl Pts',(-1.91396932214169,7.00188822714751,
36.25));
#306777=CARTESIAN_POINT('Ctrl Pts',(-1.91621068652427,6.93766582705582,
36.25));
#306778=CARTESIAN_POINT('Ctrl Pts',(-1.91737012987013,6.90444399350649,
36.25));
#306779=CARTESIAN_POINT('',(-1.52371651785714,6.39675324675325,36.25));
#306780=CARTESIAN_POINT('Ctrl Pts',(-1.91737012987013,6.90444399350649,
36.25));
#306781=CARTESIAN_POINT('Ctrl Pts',(-1.91613148952843,6.8676136615146,36.25));
#306782=CARTESIAN_POINT('Ctrl Pts',(-1.91376144516393,6.79714161418861,
36.25));
#306783=CARTESIAN_POINT('Ctrl Pts',(-1.89249074922576,6.69694686802566,
36.25));
#306784=CARTESIAN_POINT('Ctrl Pts',(-1.85626188657584,6.60868448959127,
36.25));
#306785=CARTESIAN_POINT('Ctrl Pts',(-1.80667059916436,6.53319043392833,
36.25));
#306786=CARTESIAN_POINT('Ctrl Pts',(-1.74600279585425,6.47327605218271,
36.25));
#306787=CARTESIAN_POINT('Ctrl Pts',(-1.67833795046176,6.42829274914181,
36.25));
#306788=CARTESIAN_POINT('Ctrl Pts',(-1.60297996097691,6.4012532984509,36.25));
#306789=CARTESIAN_POINT('Ctrl Pts',(-1.5503437032771,6.39826496143831,36.25));
#306790=CARTESIAN_POINT('Ctrl Pts',(-1.52371651785714,6.39675324675325,
36.25));
#306791=CARTESIAN_POINT('',(-1.13392857142857,6.88318283279221,36.25));
#306792=CARTESIAN_POINT('Ctrl Pts',(-1.52371651785714,6.39675324675325,
36.25));
#306793=CARTESIAN_POINT('Ctrl Pts',(-1.49749406178753,6.39823178023093,
36.25));
#306794=CARTESIAN_POINT('Ctrl Pts',(-1.44564553849367,6.40115522024948,
36.25));
#306795=CARTESIAN_POINT('Ctrl Pts',(-1.37190501458764,6.42869442089,36.25));
#306796=CARTESIAN_POINT('Ctrl Pts',(-1.30436731865975,6.47176243493413,
36.25));
#306797=CARTESIAN_POINT('Ctrl Pts',(-1.24507578007146,6.5313545752525,36.25));
#306798=CARTESIAN_POINT('Ctrl Pts',(-1.19545427309708,6.60421240376617,
36.25));
#306799=CARTESIAN_POINT('Ctrl Pts',(-1.15909489053248,6.68851996626879,
36.25));
#306800=CARTESIAN_POINT('Ctrl Pts',(-1.13760625764887,6.78290098418177,
36.25));
#306801=CARTESIAN_POINT('Ctrl Pts',(-1.13518507442834,6.84892095288905,
36.25));
#306802=CARTESIAN_POINT('Ctrl Pts',(-1.13392857142857,6.88318283279221,
36.25));
#306803=CARTESIAN_POINT('Ctrl Pts',(-1.13392857142857,6.88318283279221,
36.25));
#306804=CARTESIAN_POINT('Ctrl Pts',(-1.13513622427257,6.91852455417192,
36.25));
#306805=CARTESIAN_POINT('Ctrl Pts',(-1.13746675383528,6.98672704040914,
36.25));
#306806=CARTESIAN_POINT('Ctrl Pts',(-1.15960212713315,7.08387655284218,
36.25));
#306807=CARTESIAN_POINT('Ctrl Pts',(-1.1967070851926,7.17101343023865,36.25));
#306808=CARTESIAN_POINT('Ctrl Pts',(-1.248366652071,7.24570928090529,36.25));
#306809=CARTESIAN_POINT('Ctrl Pts',(-1.30855629123278,7.30781082924543,
36.25));
#306810=CARTESIAN_POINT('Ctrl Pts',(-1.3763696724576,7.35293658272662,36.25));
#306811=CARTESIAN_POINT('Ctrl Pts',(-1.45006627196568,7.38129222806274,
36.25));
#306812=CARTESIAN_POINT('Ctrl Pts',(-1.50156524889417,7.38466150198483,
36.25));
#306813=CARTESIAN_POINT('Ctrl Pts',(-1.52758218344156,7.38636363636364,
36.25));
#306814=CARTESIAN_POINT('Origin',(0.,0.,36.25));
#306815=CARTESIAN_POINT('',(1.51920657467533,6.06688311688312,36.25));
#306816=CARTESIAN_POINT('',(1.01022727272727,5.43420251623377,36.25));
#306817=CARTESIAN_POINT('Ctrl Pts',(1.51920657467533,6.06688311688312,36.25));
#306818=CARTESIAN_POINT('Ctrl Pts',(1.5017821965604,6.066434027441,36.25));
#306819=CARTESIAN_POINT('Ctrl Pts',(1.46736804529077,6.06554704990339,36.25));
#306820=CARTESIAN_POINT('Ctrl Pts',(1.41686786206546,6.05712286492333,36.25));
#306821=CARTESIAN_POINT('Ctrl Pts',(1.36884631219687,6.04224031339717,36.25));
#306822=CARTESIAN_POINT('Ctrl Pts',(1.32191903516798,6.02430730620351,36.25));
#306823=CARTESIAN_POINT('Ctrl Pts',(1.27807748224968,5.99813668132169,36.25));
#306824=CARTESIAN_POINT('Ctrl Pts',(1.23519630821944,5.96827285277196,36.25));
#306825=CARTESIAN_POINT('Ctrl Pts',(1.19537510098809,5.93155196527191,36.25));
#306826=CARTESIAN_POINT('Ctrl Pts',(1.15739985251507,5.89060348709459,36.25));
#306827=CARTESIAN_POINT('Ctrl Pts',(1.12287571225305,5.84507968533496,36.25));
#306828=CARTESIAN_POINT('Ctrl Pts',(1.09234252291203,5.79605922055842,36.25));
#306829=CARTESIAN_POINT('Ctrl Pts',(1.06720719606548,5.74343345049149,36.25));
#306830=CARTESIAN_POINT('Ctrl Pts',(1.04675217280647,5.68767671276929,36.25));
#306831=CARTESIAN_POINT('Ctrl Pts',(1.02968321354559,5.6290296721576,36.25));
#306832=CARTESIAN_POINT('Ctrl Pts',(1.01820393934243,5.56687880407454,36.25));
#306833=CARTESIAN_POINT('Ctrl Pts',(1.01197456783159,5.50155035955671,36.25));
#306834=CARTESIAN_POINT('Ctrl Pts',(1.01081821236896,5.45697972788144,36.25));
#306835=CARTESIAN_POINT('Ctrl Pts',(1.01022727272727,5.43420251623377,36.25));
#306836=CARTESIAN_POINT('',(1.52758218344156,4.78863636363636,36.25));
#306837=CARTESIAN_POINT('Ctrl Pts',(1.01022727272727,5.43420251623377,36.25));
#306838=CARTESIAN_POINT('Ctrl Pts',(1.01074437462189,5.41055942108448,36.25));
#306839=CARTESIAN_POINT('Ctrl Pts',(1.01175744721102,5.36423939815086,36.25));
#306840=CARTESIAN_POINT('Ctrl Pts',(1.01901764419993,5.2966367303295,36.25));
#306841=CARTESIAN_POINT('Ctrl Pts',(1.03022528258824,5.23250639408275,36.25));
#306842=CARTESIAN_POINT('Ctrl Pts',(1.04731521355877,5.17226185872411,36.25));
#306843=CARTESIAN_POINT('Ctrl Pts',(1.06840426337778,5.11515155101266,36.25));
#306844=CARTESIAN_POINT('Ctrl Pts',(1.09486612244816,5.06166487648077,36.25));
#306845=CARTESIAN_POINT('Ctrl Pts',(1.12612981159753,5.0117585395718,36.25));
#306846=CARTESIAN_POINT('Ctrl Pts',(1.16105752958236,4.96538056994282,36.25));
#306847=CARTESIAN_POINT('Ctrl Pts',(1.20052382029073,4.9247537203412,36.25));
#306848=CARTESIAN_POINT('Ctrl Pts',(1.24122086442875,4.88798983005251,36.25));
#306849=CARTESIAN_POINT('Ctrl Pts',(1.28411117190556,4.85710381362087,36.25));
#306850=CARTESIAN_POINT('Ctrl Pts',(1.32939856317298,4.83218747720399,36.25));
#306851=CARTESIAN_POINT('Ctrl Pts',(1.37639471981463,4.81303741070312,36.25));
#306852=CARTESIAN_POINT('Ctrl Pts',(1.42508500090371,4.79855444913016,36.25));
#306853=CARTESIAN_POINT('Ctrl Pts',(1.47573186595857,4.78994040169141,36.25));
#306854=CARTESIAN_POINT('Ctrl Pts',(1.51015384301738,4.789074687262,36.25));
#306855=CARTESIAN_POINT('Ctrl Pts',(1.52758218344156,4.78863636363636,36.25));
#306856=CARTESIAN_POINT('',(2.04107142857143,5.42131696428571,36.25));
#306857=CARTESIAN_POINT('Ctrl Pts',(1.52758218344156,4.78863636363636,36.25));
#306858=CARTESIAN_POINT('Ctrl Pts',(1.54523256318688,4.78904075129562,36.25));
#306859=CARTESIAN_POINT('Ctrl Pts',(1.5798837022752,4.78983464316812,36.25));
#306860=CARTESIAN_POINT('Ctrl Pts',(1.63079567698862,4.79884546139153,36.25));
#306861=CARTESIAN_POINT('Ctrl Pts',(1.67970258395479,4.81206099883602,36.25));
#306862=CARTESIAN_POINT('Ctrl Pts',(1.72652298376726,4.83107657862712,36.25));
#306863=CARTESIAN_POINT('Ctrl Pts',(1.77140565570483,4.85499849822356,36.25));
#306864=CARTESIAN_POINT('Ctrl Pts',(1.81390598351971,4.88475706229418,36.25));
#306865=CARTESIAN_POINT('Ctrl Pts',(1.85419832598593,4.92023184841449,36.25));
#306866=CARTESIAN_POINT('Ctrl Pts',(1.89265117091878,4.96016808484432,36.25));
#306867=CARTESIAN_POINT('Ctrl Pts',(1.92696273298897,5.00550562421531,36.25));
#306868=CARTESIAN_POINT('Ctrl Pts',(1.95867569552678,5.05353436556821,36.25));
#306869=CARTESIAN_POINT('Ctrl Pts',(1.9831268819592,5.10649857927001,36.25));
#306870=CARTESIAN_POINT('Ctrl Pts',(2.00511626181496,5.16193679017606,36.25));
#306871=CARTESIAN_POINT('Ctrl Pts',(2.02054669570705,5.22177284922642,36.25));
#306872=CARTESIAN_POINT('Ctrl Pts',(2.0334543847172,5.28488392294487,36.25));
#306873=CARTESIAN_POINT('Ctrl Pts',(2.03922895997908,5.35205975094169,36.25));
#306874=CARTESIAN_POINT('Ctrl Pts',(2.04044852772871,5.39790252089427,36.25));
#306875=CARTESIAN_POINT('Ctrl Pts',(2.04107142857143,5.42131696428571,36.25));
#306876=CARTESIAN_POINT('Ctrl Pts',(2.04107142857143,5.42131696428571,36.25));
#306877=CARTESIAN_POINT('Ctrl Pts',(2.04053270667799,5.44495600403826,36.25));
#306878=CARTESIAN_POINT('Ctrl Pts',(2.0394772775854,5.49126808190085,36.25));
#306879=CARTESIAN_POINT('Ctrl Pts',(2.03251602654254,5.55896687878814,36.25));
#306880=CARTESIAN_POINT('Ctrl Pts',(2.02022069750506,5.62293356367208,36.25));
#306881=CARTESIAN_POINT('Ctrl Pts',(2.00340124721791,5.68327106051297,36.25));
#306882=CARTESIAN_POINT('Ctrl Pts',(1.98221217886446,5.74035420483588,36.25));
#306883=CARTESIAN_POINT('Ctrl Pts',(1.95582710639876,5.79399835274014,36.25));
#306884=CARTESIAN_POINT('Ctrl Pts',(1.92410277702741,5.84377259737151,36.25));
#306885=CARTESIAN_POINT('Ctrl Pts',(1.88783253473841,5.88934000071629,36.25));
#306886=CARTESIAN_POINT('Ctrl Pts',(1.84907731850073,5.93098943621083,36.25));
#306887=CARTESIAN_POINT('Ctrl Pts',(1.80771391130794,5.96739207884556,36.25));
#306888=CARTESIAN_POINT('Ctrl Pts',(1.76414349382133,5.99780008387924,36.25));
#306889=CARTESIAN_POINT('Ctrl Pts',(1.71900701398188,6.02332207855003,36.25));
#306890=CARTESIAN_POINT('Ctrl Pts',(1.67166640701484,6.04244867323907,36.25));
#306891=CARTESIAN_POINT('Ctrl Pts',(1.62279736679542,6.05706063884487,36.25));
#306892=CARTESIAN_POINT('Ctrl Pts',(1.57169261973291,6.0655628055813,36.25));
#306893=CARTESIAN_POINT('Ctrl Pts',(1.53684768525004,6.06643934639816,36.25));
#306894=CARTESIAN_POINT('Ctrl Pts',(1.51920657467533,6.06688311688312,36.25));
#306895=CARTESIAN_POINT('Origin',(0.,0.,36.25));
#306896=CARTESIAN_POINT('',(1.52371651785715,7.38636363636364,36.25));
#306897=CARTESIAN_POINT('',(1.13392857142857,6.90444399350649,36.25));
#306898=CARTESIAN_POINT('Ctrl Pts',(1.52371651785715,7.38636363636364,36.25));
#306899=CARTESIAN_POINT('Ctrl Pts',(1.49771633107715,7.38486930154146,36.25));
#306900=CARTESIAN_POINT('Ctrl Pts',(1.4463007522726,7.38191424239284,36.25));
#306901=CARTESIAN_POINT('Ctrl Pts',(1.37265904788325,7.354443366284,36.25));
#306902=CARTESIAN_POINT('Ctrl Pts',(1.30553944113734,7.30974046602882,36.25));
#306903=CARTESIAN_POINT('Ctrl Pts',(1.246166587943,7.24931351323173,36.25));
#306904=CARTESIAN_POINT('Ctrl Pts',(1.19545283377814,7.17700242184241,36.25));
#306905=CARTESIAN_POINT('Ctrl Pts',(1.16034942104761,7.09344714231162,36.25));
#306906=CARTESIAN_POINT('Ctrl Pts',(1.13732937915702,7.0018882271475,36.25));
#306907=CARTESIAN_POINT('Ctrl Pts',(1.13508801477443,6.93766582705582,36.25));
#306908=CARTESIAN_POINT('Ctrl Pts',(1.13392857142857,6.90444399350649,36.25));
#306909=CARTESIAN_POINT('',(1.52758218344156,6.39675324675325,36.25));
#306910=CARTESIAN_POINT('Ctrl Pts',(1.13392857142857,6.90444399350649,36.25));
#306911=CARTESIAN_POINT('Ctrl Pts',(1.13516721177027,6.8676136615146,36.25));
#306912=CARTESIAN_POINT('Ctrl Pts',(1.13753725613477,6.79714161418862,36.25));
#306913=CARTESIAN_POINT('Ctrl Pts',(1.15880795207294,6.69694686802566,36.25));
#306914=CARTESIAN_POINT('Ctrl Pts',(1.19503681472287,6.60868448959127,36.25));
#306915=CARTESIAN_POINT('Ctrl Pts',(1.24462810213434,6.53319043392833,36.25));
#306916=CARTESIAN_POINT('Ctrl Pts',(1.30529590544445,6.47327605218271,36.25));
#306917=CARTESIAN_POINT('Ctrl Pts',(1.37296075083694,6.42829274914181,36.25));
#306918=CARTESIAN_POINT('Ctrl Pts',(1.44831874032179,6.4012532984509,36.25));
#306919=CARTESIAN_POINT('Ctrl Pts',(1.50095499802161,6.39826496143831,36.25));
#306920=CARTESIAN_POINT('Ctrl Pts',(1.52758218344156,6.39675324675325,36.25));
#306921=CARTESIAN_POINT('',(1.91737012987013,6.88318283279221,36.25));
#306922=CARTESIAN_POINT('Ctrl Pts',(1.52758218344156,6.39675324675325,36.25));
#306923=CARTESIAN_POINT('Ctrl Pts',(1.55380463951118,6.39823178023093,36.25));
#306924=CARTESIAN_POINT('Ctrl Pts',(1.60565316280503,6.40115522024948,36.25));
#306925=CARTESIAN_POINT('Ctrl Pts',(1.67939368671106,6.42869442089,36.25));
#306926=CARTESIAN_POINT('Ctrl Pts',(1.74693138263896,6.47176243493413,36.25));
#306927=CARTESIAN_POINT('Ctrl Pts',(1.80622292122723,6.5313545752525,36.25));
#306928=CARTESIAN_POINT('Ctrl Pts',(1.85584442820162,6.60421240376617,36.25));
#306929=CARTESIAN_POINT('Ctrl Pts',(1.89220381076623,6.68851996626879,36.25));
#306930=CARTESIAN_POINT('Ctrl Pts',(1.91369244364984,6.78290098418177,36.25));
#306931=CARTESIAN_POINT('Ctrl Pts',(1.91611362687036,6.84892095288905,36.25));
#306932=CARTESIAN_POINT('Ctrl Pts',(1.91737012987013,6.88318283279221,36.25));
#306933=CARTESIAN_POINT('Ctrl Pts',(1.91737012987013,6.88318283279221,36.25));
#306934=CARTESIAN_POINT('Ctrl Pts',(1.91616247702613,6.91852455417192,36.25));
#306935=CARTESIAN_POINT('Ctrl Pts',(1.91383194746342,6.98672704040914,36.25));
#306936=CARTESIAN_POINT('Ctrl Pts',(1.89169657416555,7.08387655284218,36.25));
#306937=CARTESIAN_POINT('Ctrl Pts',(1.8545916161061,7.17101343023865,36.25));
#306938=CARTESIAN_POINT('Ctrl Pts',(1.80293204922771,7.24570928090529,36.25));
#306939=CARTESIAN_POINT('Ctrl Pts',(1.74274241006592,7.30781082924543,36.25));
#306940=CARTESIAN_POINT('Ctrl Pts',(1.6749290288411,7.35293658272662,36.25));
#306941=CARTESIAN_POINT('Ctrl Pts',(1.60123242933302,7.38129222806274,36.25));
#306942=CARTESIAN_POINT('Ctrl Pts',(1.54973345240453,7.38466150198483,36.25));
#306943=CARTESIAN_POINT('Ctrl Pts',(1.52371651785715,7.38636363636364,36.25));
#306944=CARTESIAN_POINT('Ctrl Pts',(-1.52371651785714,4.78863636363636,
36.05));
#306945=CARTESIAN_POINT('Ctrl Pts',(-1.52371651785714,4.78863636363636,
36.29));
#306946=CARTESIAN_POINT('Ctrl Pts',(-1.50606613811182,4.78904075129562,
36.05));
#306947=CARTESIAN_POINT('Ctrl Pts',(-1.50606613811182,4.78904075129562,
36.29));
#306948=CARTESIAN_POINT('Ctrl Pts',(-1.4714149990235,4.78983464316812,36.05));
#306949=CARTESIAN_POINT('Ctrl Pts',(-1.4714149990235,4.78983464316812,36.29));
#306950=CARTESIAN_POINT('Ctrl Pts',(-1.42050302431008,4.79884546139153,
36.05));
#306951=CARTESIAN_POINT('Ctrl Pts',(-1.42050302431008,4.79884546139153,
36.29));
#306952=CARTESIAN_POINT('Ctrl Pts',(-1.37159611734391,4.81206099883602,
36.05));
#306953=CARTESIAN_POINT('Ctrl Pts',(-1.37159611734391,4.81206099883602,
36.29));
#306954=CARTESIAN_POINT('Ctrl Pts',(-1.32477571753144,4.83107657862712,
36.05));
#306955=CARTESIAN_POINT('Ctrl Pts',(-1.32477571753144,4.83107657862712,
36.29));
#306956=CARTESIAN_POINT('Ctrl Pts',(-1.27989304559387,4.85499849822356,
36.05));
#306957=CARTESIAN_POINT('Ctrl Pts',(-1.27989304559387,4.85499849822356,
36.29));
#306958=CARTESIAN_POINT('Ctrl Pts',(-1.23739271777899,4.88475706229418,
36.05));
#306959=CARTESIAN_POINT('Ctrl Pts',(-1.23739271777899,4.88475706229418,
36.29));
#306960=CARTESIAN_POINT('Ctrl Pts',(-1.19710037531277,4.92023184841449,
36.05));
#306961=CARTESIAN_POINT('Ctrl Pts',(-1.19710037531277,4.92023184841449,
36.29));
#306962=CARTESIAN_POINT('Ctrl Pts',(-1.15864753037992,4.96016808484432,
36.05));
#306963=CARTESIAN_POINT('Ctrl Pts',(-1.15864753037992,4.96016808484432,
36.29));
#306964=CARTESIAN_POINT('Ctrl Pts',(-1.12433596830973,5.00550562421531,
36.05));
#306965=CARTESIAN_POINT('Ctrl Pts',(-1.12433596830973,5.00550562421531,
36.29));
#306966=CARTESIAN_POINT('Ctrl Pts',(-1.09262300577192,5.05353436556821,
36.05));
#306967=CARTESIAN_POINT('Ctrl Pts',(-1.09262300577192,5.05353436556821,
36.29));
#306968=CARTESIAN_POINT('Ctrl Pts',(-1.0681718193395,5.10649857927001,36.05));
#306969=CARTESIAN_POINT('Ctrl Pts',(-1.0681718193395,5.10649857927001,36.29));
#306970=CARTESIAN_POINT('Ctrl Pts',(-1.04618243948374,5.16193679017606,
36.05));
#306971=CARTESIAN_POINT('Ctrl Pts',(-1.04618243948374,5.16193679017606,
36.29));
#306972=CARTESIAN_POINT('Ctrl Pts',(-1.03075200559165,5.22177284922642,
36.05));
#306973=CARTESIAN_POINT('Ctrl Pts',(-1.03075200559165,5.22177284922642,
36.29));
#306974=CARTESIAN_POINT('Ctrl Pts',(-1.0178443165815,5.28488392294487,36.05));
#306975=CARTESIAN_POINT('Ctrl Pts',(-1.0178443165815,5.28488392294487,36.29));
#306976=CARTESIAN_POINT('Ctrl Pts',(-1.01206974131962,5.35205975094169,
36.05));
#306977=CARTESIAN_POINT('Ctrl Pts',(-1.01206974131962,5.35205975094169,
36.29));
#306978=CARTESIAN_POINT('Ctrl Pts',(-1.01085017356999,5.39790252089427,
36.05));
#306979=CARTESIAN_POINT('Ctrl Pts',(-1.01085017356999,5.39790252089427,
36.29));
#306980=CARTESIAN_POINT('Ctrl Pts',(-1.01022727272727,5.42131696428571,
36.05));
#306981=CARTESIAN_POINT('Ctrl Pts',(-1.01022727272727,5.42131696428571,
36.29));
#306982=CARTESIAN_POINT('',(-1.52371651785714,4.78863636363636,36.05));
#306983=CARTESIAN_POINT('',(-1.52371651785714,4.78863636363636,32.1799631621335));
#306984=CARTESIAN_POINT('',(-1.01022727272727,5.42131696428571,36.05));
#306985=CARTESIAN_POINT('Ctrl Pts',(-1.01022727272727,5.42131696428571,
36.05));
#306986=CARTESIAN_POINT('Ctrl Pts',(-1.01085017356999,5.39790252089427,
36.05));
#306987=CARTESIAN_POINT('Ctrl Pts',(-1.01206974131962,5.35205975094169,
36.05));
#306988=CARTESIAN_POINT('Ctrl Pts',(-1.0178443165815,5.28488392294487,36.05));
#306989=CARTESIAN_POINT('Ctrl Pts',(-1.03075200559165,5.22177284922642,
36.05));
#306990=CARTESIAN_POINT('Ctrl Pts',(-1.04618243948374,5.16193679017606,
36.05));
#306991=CARTESIAN_POINT('Ctrl Pts',(-1.0681718193395,5.10649857927001,36.05));
#306992=CARTESIAN_POINT('Ctrl Pts',(-1.09262300577192,5.05353436556821,
36.05));
#306993=CARTESIAN_POINT('Ctrl Pts',(-1.12433596830973,5.00550562421531,
36.05));
#306994=CARTESIAN_POINT('Ctrl Pts',(-1.15864753037992,4.96016808484432,
36.05));
#306995=CARTESIAN_POINT('Ctrl Pts',(-1.19710037531277,4.92023184841449,
36.05));
#306996=CARTESIAN_POINT('Ctrl Pts',(-1.23739271777899,4.88475706229418,
36.05));
#306997=CARTESIAN_POINT('Ctrl Pts',(-1.27989304559387,4.85499849822356,
36.05));
#306998=CARTESIAN_POINT('Ctrl Pts',(-1.32477571753144,4.83107657862712,
36.05));
#306999=CARTESIAN_POINT('Ctrl Pts',(-1.37159611734391,4.81206099883602,
36.05));
#307000=CARTESIAN_POINT('Ctrl Pts',(-1.42050302431008,4.79884546139153,
36.05));
#307001=CARTESIAN_POINT('Ctrl Pts',(-1.4714149990235,4.78983464316812,36.05));
#307002=CARTESIAN_POINT('Ctrl Pts',(-1.50606613811182,4.78904075129562,
36.05));
#307003=CARTESIAN_POINT('Ctrl Pts',(-1.52371651785714,4.78863636363636,
36.05));
#307004=CARTESIAN_POINT('',(-1.01022727272727,5.42131696428571,32.1799631621335));
#307005=CARTESIAN_POINT('Ctrl Pts',(-1.01022727272727,5.42131696428571,
36.05));
#307006=CARTESIAN_POINT('Ctrl Pts',(-1.01022727272727,5.42131696428571,
36.29));
#307007=CARTESIAN_POINT('Ctrl Pts',(-1.01076599462072,5.44495600403826,
36.05));
#307008=CARTESIAN_POINT('Ctrl Pts',(-1.01076599462072,5.44495600403826,
36.29));
#307009=CARTESIAN_POINT('Ctrl Pts',(-1.0118214237133,5.49126808190085,36.05));
#307010=CARTESIAN_POINT('Ctrl Pts',(-1.0118214237133,5.49126808190085,36.29));
#307011=CARTESIAN_POINT('Ctrl Pts',(-1.01878267475616,5.55896687878814,
36.05));
#307012=CARTESIAN_POINT('Ctrl Pts',(-1.01878267475616,5.55896687878814,
36.29));
#307013=CARTESIAN_POINT('Ctrl Pts',(-1.03107800379365,5.62293356367208,
36.05));
#307014=CARTESIAN_POINT('Ctrl Pts',(-1.03107800379365,5.62293356367208,
36.29));
#307015=CARTESIAN_POINT('Ctrl Pts',(-1.04789745408079,5.68327106051297,
36.05));
#307016=CARTESIAN_POINT('Ctrl Pts',(-1.04789745408079,5.68327106051297,
36.29));
#307017=CARTESIAN_POINT('Ctrl Pts',(-1.06908652243424,5.74035420483588,
36.05));
#307018=CARTESIAN_POINT('Ctrl Pts',(-1.06908652243424,5.74035420483588,
36.29));
#307019=CARTESIAN_POINT('Ctrl Pts',(-1.09547159489994,5.79399835274014,
36.05));
#307020=CARTESIAN_POINT('Ctrl Pts',(-1.09547159489994,5.79399835274014,
36.29));
#307021=CARTESIAN_POINT('Ctrl Pts',(-1.12719592427129,5.8437725973715,36.05));
#307022=CARTESIAN_POINT('Ctrl Pts',(-1.12719592427129,5.8437725973715,36.29));
#307023=CARTESIAN_POINT('Ctrl Pts',(-1.1634661665603,5.88934000071629,36.05));
#307024=CARTESIAN_POINT('Ctrl Pts',(-1.1634661665603,5.88934000071629,36.29));
#307025=CARTESIAN_POINT('Ctrl Pts',(-1.20222138279797,5.93098943621083,
36.05));
#307026=CARTESIAN_POINT('Ctrl Pts',(-1.20222138279797,5.93098943621083,
36.29));
#307027=CARTESIAN_POINT('Ctrl Pts',(-1.24358478999076,5.96739207884556,
36.05));
#307028=CARTESIAN_POINT('Ctrl Pts',(-1.24358478999076,5.96739207884556,
36.29));
#307029=CARTESIAN_POINT('Ctrl Pts',(-1.28715520747738,5.99780008387924,
36.05));
#307030=CARTESIAN_POINT('Ctrl Pts',(-1.28715520747738,5.99780008387924,
36.29));
#307031=CARTESIAN_POINT('Ctrl Pts',(-1.33229168731682,6.02332207855003,
36.05));
#307032=CARTESIAN_POINT('Ctrl Pts',(-1.33229168731682,6.02332207855003,
36.29));
#307033=CARTESIAN_POINT('Ctrl Pts',(-1.37963229428386,6.04244867323907,
36.05));
#307034=CARTESIAN_POINT('Ctrl Pts',(-1.37963229428386,6.04244867323907,
36.29));
#307035=CARTESIAN_POINT('Ctrl Pts',(-1.42850133450328,6.05706063884487,
36.05));
#307036=CARTESIAN_POINT('Ctrl Pts',(-1.42850133450328,6.05706063884487,
36.29));
#307037=CARTESIAN_POINT('Ctrl Pts',(-1.47960608156579,6.0655628055813,36.05));
#307038=CARTESIAN_POINT('Ctrl Pts',(-1.47960608156579,6.0655628055813,36.29));
#307039=CARTESIAN_POINT('Ctrl Pts',(-1.51445101604866,6.06643934639816,
36.05));
#307040=CARTESIAN_POINT('Ctrl Pts',(-1.51445101604866,6.06643934639816,
36.29));
#307041=CARTESIAN_POINT('Ctrl Pts',(-1.53209212662338,6.06688311688312,
36.05));
#307042=CARTESIAN_POINT('Ctrl Pts',(-1.53209212662338,6.06688311688312,
36.29));
#307043=CARTESIAN_POINT('',(-1.53209212662338,6.06688311688312,36.05));
#307044=CARTESIAN_POINT('Ctrl Pts',(-1.53209212662338,6.06688311688312,
36.05));
#307045=CARTESIAN_POINT('Ctrl Pts',(-1.51445101604866,6.06643934639816,
36.05));
#307046=CARTESIAN_POINT('Ctrl Pts',(-1.47960608156579,6.0655628055813,36.05));
#307047=CARTESIAN_POINT('Ctrl Pts',(-1.42850133450328,6.05706063884487,
36.05));
#307048=CARTESIAN_POINT('Ctrl Pts',(-1.37963229428386,6.04244867323907,
36.05));
#307049=CARTESIAN_POINT('Ctrl Pts',(-1.33229168731682,6.02332207855003,
36.05));
#307050=CARTESIAN_POINT('Ctrl Pts',(-1.28715520747738,5.99780008387924,
36.05));
#307051=CARTESIAN_POINT('Ctrl Pts',(-1.24358478999076,5.96739207884556,
36.05));
#307052=CARTESIAN_POINT('Ctrl Pts',(-1.20222138279797,5.93098943621083,
36.05));
#307053=CARTESIAN_POINT('Ctrl Pts',(-1.1634661665603,5.88934000071629,36.05));
#307054=CARTESIAN_POINT('Ctrl Pts',(-1.12719592427129,5.8437725973715,36.05));
#307055=CARTESIAN_POINT('Ctrl Pts',(-1.09547159489994,5.79399835274014,
36.05));
#307056=CARTESIAN_POINT('Ctrl Pts',(-1.06908652243424,5.74035420483588,
36.05));
#307057=CARTESIAN_POINT('Ctrl Pts',(-1.04789745408079,5.68327106051297,
36.05));
#307058=CARTESIAN_POINT('Ctrl Pts',(-1.03107800379365,5.62293356367208,
36.05));
#307059=CARTESIAN_POINT('Ctrl Pts',(-1.01878267475616,5.55896687878814,
36.05));
#307060=CARTESIAN_POINT('Ctrl Pts',(-1.0118214237133,5.49126808190085,36.05));
#307061=CARTESIAN_POINT('Ctrl Pts',(-1.01076599462072,5.44495600403826,
36.05));
#307062=CARTESIAN_POINT('Ctrl Pts',(-1.01022727272727,5.42131696428571,
36.05));
#307063=CARTESIAN_POINT('',(-1.53209212662338,6.06688311688312,32.1799631621335));
#307064=CARTESIAN_POINT('Ctrl Pts',(-1.53209212662338,6.06688311688312,
36.05));
#307065=CARTESIAN_POINT('Ctrl Pts',(-1.53209212662338,6.06688311688312,
36.29));
#307066=CARTESIAN_POINT('Ctrl Pts',(-1.54951650473831,6.066434027441,36.05));
#307067=CARTESIAN_POINT('Ctrl Pts',(-1.54951650473831,6.066434027441,36.29));
#307068=CARTESIAN_POINT('Ctrl Pts',(-1.58393065600793,6.06554704990339,
36.05));
#307069=CARTESIAN_POINT('Ctrl Pts',(-1.58393065600793,6.06554704990339,
36.29));
#307070=CARTESIAN_POINT('Ctrl Pts',(-1.63443083923324,6.05712286492333,
36.05));
#307071=CARTESIAN_POINT('Ctrl Pts',(-1.63443083923324,6.05712286492333,
36.29));
#307072=CARTESIAN_POINT('Ctrl Pts',(-1.68245238910184,6.04224031339717,
36.05));
#307073=CARTESIAN_POINT('Ctrl Pts',(-1.68245238910184,6.04224031339717,
36.29));
#307074=CARTESIAN_POINT('Ctrl Pts',(-1.72937966613072,6.02430730620351,
36.05));
#307075=CARTESIAN_POINT('Ctrl Pts',(-1.72937966613072,6.02430730620351,
36.29));
#307076=CARTESIAN_POINT('Ctrl Pts',(-1.77322121904902,5.9981366813217,36.05));
#307077=CARTESIAN_POINT('Ctrl Pts',(-1.77322121904902,5.9981366813217,36.29));
#307078=CARTESIAN_POINT('Ctrl Pts',(-1.81610239307926,5.96827285277195,
36.05));
#307079=CARTESIAN_POINT('Ctrl Pts',(-1.81610239307926,5.96827285277195,
36.29));
#307080=CARTESIAN_POINT('Ctrl Pts',(-1.85592360031061,5.93155196527191,
36.05));
#307081=CARTESIAN_POINT('Ctrl Pts',(-1.85592360031061,5.93155196527191,
36.29));
#307082=CARTESIAN_POINT('Ctrl Pts',(-1.89389884878363,5.89060348709459,
36.05));
#307083=CARTESIAN_POINT('Ctrl Pts',(-1.89389884878363,5.89060348709459,
36.29));
#307084=CARTESIAN_POINT('Ctrl Pts',(-1.92842298904565,5.84507968533497,
36.05));
#307085=CARTESIAN_POINT('Ctrl Pts',(-1.92842298904565,5.84507968533497,
36.29));
#307086=CARTESIAN_POINT('Ctrl Pts',(-1.95895617838667,5.79605922055842,
36.05));
#307087=CARTESIAN_POINT('Ctrl Pts',(-1.95895617838667,5.79605922055842,
36.29));
#307088=CARTESIAN_POINT('Ctrl Pts',(-1.98409150523322,5.74343345049149,
36.05));
#307089=CARTESIAN_POINT('Ctrl Pts',(-1.98409150523322,5.74343345049149,
36.29));
#307090=CARTESIAN_POINT('Ctrl Pts',(-2.00454652849223,5.68767671276928,
36.05));
#307091=CARTESIAN_POINT('Ctrl Pts',(-2.00454652849223,5.68767671276928,
36.29));
#307092=CARTESIAN_POINT('Ctrl Pts',(-2.02161548775311,5.6290296721576,36.05));
#307093=CARTESIAN_POINT('Ctrl Pts',(-2.02161548775311,5.6290296721576,36.29));
#307094=CARTESIAN_POINT('Ctrl Pts',(-2.03309476195626,5.56687880407454,
36.05));
#307095=CARTESIAN_POINT('Ctrl Pts',(-2.03309476195626,5.56687880407454,
36.29));
#307096=CARTESIAN_POINT('Ctrl Pts',(-2.03932413346711,5.50155035955671,
36.05));
#307097=CARTESIAN_POINT('Ctrl Pts',(-2.03932413346711,5.50155035955671,
36.29));
#307098=CARTESIAN_POINT('Ctrl Pts',(-2.04048048892973,5.45697972788144,
36.05));
#307099=CARTESIAN_POINT('Ctrl Pts',(-2.04048048892973,5.45697972788144,
36.29));
#307100=CARTESIAN_POINT('Ctrl Pts',(-2.04107142857143,5.43420251623377,
36.05));
#307101=CARTESIAN_POINT('Ctrl Pts',(-2.04107142857143,5.43420251623377,
36.29));
#307102=CARTESIAN_POINT('',(-2.04107142857143,5.43420251623377,36.05));
#307103=CARTESIAN_POINT('Ctrl Pts',(-2.04107142857143,5.43420251623377,
36.05));
#307104=CARTESIAN_POINT('Ctrl Pts',(-2.04048048892973,5.45697972788144,
36.05));
#307105=CARTESIAN_POINT('Ctrl Pts',(-2.03932413346711,5.50155035955671,
36.05));
#307106=CARTESIAN_POINT('Ctrl Pts',(-2.03309476195626,5.56687880407454,
36.05));
#307107=CARTESIAN_POINT('Ctrl Pts',(-2.02161548775311,5.6290296721576,36.05));
#307108=CARTESIAN_POINT('Ctrl Pts',(-2.00454652849223,5.68767671276928,
36.05));
#307109=CARTESIAN_POINT('Ctrl Pts',(-1.98409150523322,5.74343345049149,
36.05));
#307110=CARTESIAN_POINT('Ctrl Pts',(-1.95895617838667,5.79605922055842,
36.05));
#307111=CARTESIAN_POINT('Ctrl Pts',(-1.92842298904565,5.84507968533497,
36.05));
#307112=CARTESIAN_POINT('Ctrl Pts',(-1.89389884878363,5.89060348709459,
36.05));
#307113=CARTESIAN_POINT('Ctrl Pts',(-1.85592360031061,5.93155196527191,
36.05));
#307114=CARTESIAN_POINT('Ctrl Pts',(-1.81610239307926,5.96827285277195,
36.05));
#307115=CARTESIAN_POINT('Ctrl Pts',(-1.77322121904902,5.9981366813217,36.05));
#307116=CARTESIAN_POINT('Ctrl Pts',(-1.72937966613072,6.02430730620351,
36.05));
#307117=CARTESIAN_POINT('Ctrl Pts',(-1.68245238910184,6.04224031339717,
36.05));
#307118=CARTESIAN_POINT('Ctrl Pts',(-1.63443083923324,6.05712286492333,
36.05));
#307119=CARTESIAN_POINT('Ctrl Pts',(-1.58393065600793,6.06554704990339,
36.05));
#307120=CARTESIAN_POINT('Ctrl Pts',(-1.54951650473831,6.066434027441,36.05));
#307121=CARTESIAN_POINT('Ctrl Pts',(-1.53209212662338,6.06688311688312,
36.05));
#307122=CARTESIAN_POINT('',(-2.04107142857143,5.43420251623377,32.1799631621335));
#307123=CARTESIAN_POINT('Ctrl Pts',(-2.04107142857143,5.43420251623377,
36.05));
#307124=CARTESIAN_POINT('Ctrl Pts',(-2.04107142857143,5.43420251623377,
36.29));
#307125=CARTESIAN_POINT('Ctrl Pts',(-2.0405543266768,5.41055942108448,36.05));
#307126=CARTESIAN_POINT('Ctrl Pts',(-2.0405543266768,5.41055942108448,36.29));
#307127=CARTESIAN_POINT('Ctrl Pts',(-2.03954125408768,5.36423939815085,
36.05));
#307128=CARTESIAN_POINT('Ctrl Pts',(-2.03954125408768,5.36423939815085,
36.29));
#307129=CARTESIAN_POINT('Ctrl Pts',(-2.03228105709878,5.2966367303295,36.05));
#307130=CARTESIAN_POINT('Ctrl Pts',(-2.03228105709878,5.2966367303295,36.29));
#307131=CARTESIAN_POINT('Ctrl Pts',(-2.02107341871046,5.23250639408275,
36.05));
#307132=CARTESIAN_POINT('Ctrl Pts',(-2.02107341871046,5.23250639408275,
36.29));
#307133=CARTESIAN_POINT('Ctrl Pts',(-2.00398348773993,5.17226185872411,
36.05));
#307134=CARTESIAN_POINT('Ctrl Pts',(-2.00398348773993,5.17226185872411,
36.29));
#307135=CARTESIAN_POINT('Ctrl Pts',(-1.98289443792092,5.11515155101266,
36.05));
#307136=CARTESIAN_POINT('Ctrl Pts',(-1.98289443792092,5.11515155101266,
36.29));
#307137=CARTESIAN_POINT('Ctrl Pts',(-1.95643257885054,5.06166487648077,
36.05));
#307138=CARTESIAN_POINT('Ctrl Pts',(-1.95643257885054,5.06166487648077,
36.29));
#307139=CARTESIAN_POINT('Ctrl Pts',(-1.92516888970118,5.0117585395718,36.05));
#307140=CARTESIAN_POINT('Ctrl Pts',(-1.92516888970118,5.0117585395718,36.29));
#307141=CARTESIAN_POINT('Ctrl Pts',(-1.89024117171633,4.96538056994282,
36.05));
#307142=CARTESIAN_POINT('Ctrl Pts',(-1.89024117171633,4.96538056994282,
36.29));
#307143=CARTESIAN_POINT('Ctrl Pts',(-1.85077488100797,4.9247537203412,36.05));
#307144=CARTESIAN_POINT('Ctrl Pts',(-1.85077488100797,4.9247537203412,36.29));
#307145=CARTESIAN_POINT('Ctrl Pts',(-1.81007783686995,4.8879898300525,36.05));
#307146=CARTESIAN_POINT('Ctrl Pts',(-1.81007783686995,4.8879898300525,36.29));
#307147=CARTESIAN_POINT('Ctrl Pts',(-1.76718752939314,4.85710381362087,
36.05));
#307148=CARTESIAN_POINT('Ctrl Pts',(-1.76718752939314,4.85710381362087,
36.29));
#307149=CARTESIAN_POINT('Ctrl Pts',(-1.72190013812572,4.83218747720399,
36.05));
#307150=CARTESIAN_POINT('Ctrl Pts',(-1.72190013812572,4.83218747720399,
36.29));
#307151=CARTESIAN_POINT('Ctrl Pts',(-1.67490398148407,4.81303741070313,
36.05));
#307152=CARTESIAN_POINT('Ctrl Pts',(-1.67490398148407,4.81303741070313,
36.29));
#307153=CARTESIAN_POINT('Ctrl Pts',(-1.62621370039499,4.79855444913016,
36.05));
#307154=CARTESIAN_POINT('Ctrl Pts',(-1.62621370039499,4.79855444913016,
36.29));
#307155=CARTESIAN_POINT('Ctrl Pts',(-1.57556683534013,4.78994040169141,
36.05));
#307156=CARTESIAN_POINT('Ctrl Pts',(-1.57556683534013,4.78994040169141,
36.29));
#307157=CARTESIAN_POINT('Ctrl Pts',(-1.54114485828132,4.789074687262,36.05));
#307158=CARTESIAN_POINT('Ctrl Pts',(-1.54114485828132,4.789074687262,36.29));
#307159=CARTESIAN_POINT('Ctrl Pts',(-1.52371651785714,4.78863636363636,
36.05));
#307160=CARTESIAN_POINT('Ctrl Pts',(-1.52371651785714,4.78863636363636,
36.29));
#307161=CARTESIAN_POINT('Ctrl Pts',(-1.52371651785714,4.78863636363636,
36.05));
#307162=CARTESIAN_POINT('Ctrl Pts',(-1.54114485828132,4.789074687262,36.05));
#307163=CARTESIAN_POINT('Ctrl Pts',(-1.57556683534013,4.78994040169141,
36.05));
#307164=CARTESIAN_POINT('Ctrl Pts',(-1.62621370039499,4.79855444913016,
36.05));
#307165=CARTESIAN_POINT('Ctrl Pts',(-1.67490398148407,4.81303741070313,
36.05));
#307166=CARTESIAN_POINT('Ctrl Pts',(-1.72190013812572,4.83218747720399,
36.05));
#307167=CARTESIAN_POINT('Ctrl Pts',(-1.76718752939314,4.85710381362087,
36.05));
#307168=CARTESIAN_POINT('Ctrl Pts',(-1.81007783686995,4.8879898300525,36.05));
#307169=CARTESIAN_POINT('Ctrl Pts',(-1.85077488100797,4.9247537203412,36.05));
#307170=CARTESIAN_POINT('Ctrl Pts',(-1.89024117171633,4.96538056994282,
36.05));
#307171=CARTESIAN_POINT('Ctrl Pts',(-1.92516888970118,5.0117585395718,36.05));
#307172=CARTESIAN_POINT('Ctrl Pts',(-1.95643257885054,5.06166487648077,
36.05));
#307173=CARTESIAN_POINT('Ctrl Pts',(-1.98289443792092,5.11515155101266,
36.05));
#307174=CARTESIAN_POINT('Ctrl Pts',(-2.00398348773993,5.17226185872411,
36.05));
#307175=CARTESIAN_POINT('Ctrl Pts',(-2.02107341871046,5.23250639408275,
36.05));
#307176=CARTESIAN_POINT('Ctrl Pts',(-2.03228105709878,5.2966367303295,36.05));
#307177=CARTESIAN_POINT('Ctrl Pts',(-2.03954125408768,5.36423939815085,
36.05));
#307178=CARTESIAN_POINT('Ctrl Pts',(-2.0405543266768,5.41055942108448,36.05));
#307179=CARTESIAN_POINT('Ctrl Pts',(-2.04107142857143,5.43420251623377,
36.05));
#307180=CARTESIAN_POINT('Ctrl Pts',(-1.52371651785714,6.39675324675325,
36.05));
#307181=CARTESIAN_POINT('Ctrl Pts',(-1.52371651785714,6.39675324675325,
36.29));
#307182=CARTESIAN_POINT('Ctrl Pts',(-1.49749406178753,6.39823178023093,
36.05));
#307183=CARTESIAN_POINT('Ctrl Pts',(-1.49749406178753,6.39823178023093,
36.29));
#307184=CARTESIAN_POINT('Ctrl Pts',(-1.44564553849367,6.40115522024948,
36.05));
#307185=CARTESIAN_POINT('Ctrl Pts',(-1.44564553849367,6.40115522024948,
36.29));
#307186=CARTESIAN_POINT('Ctrl Pts',(-1.37190501458764,6.42869442089,36.05));
#307187=CARTESIAN_POINT('Ctrl Pts',(-1.37190501458764,6.42869442089,36.29));
#307188=CARTESIAN_POINT('Ctrl Pts',(-1.30436731865975,6.47176243493413,
36.05));
#307189=CARTESIAN_POINT('Ctrl Pts',(-1.30436731865975,6.47176243493413,
36.29));
#307190=CARTESIAN_POINT('Ctrl Pts',(-1.24507578007146,6.5313545752525,36.05));
#307191=CARTESIAN_POINT('Ctrl Pts',(-1.24507578007146,6.5313545752525,36.29));
#307192=CARTESIAN_POINT('Ctrl Pts',(-1.19545427309708,6.60421240376617,
36.05));
#307193=CARTESIAN_POINT('Ctrl Pts',(-1.19545427309708,6.60421240376617,
36.29));
#307194=CARTESIAN_POINT('Ctrl Pts',(-1.15909489053248,6.68851996626879,
36.05));
#307195=CARTESIAN_POINT('Ctrl Pts',(-1.15909489053248,6.68851996626879,
36.29));
#307196=CARTESIAN_POINT('Ctrl Pts',(-1.13760625764887,6.78290098418177,
36.05));
#307197=CARTESIAN_POINT('Ctrl Pts',(-1.13760625764887,6.78290098418177,
36.29));
#307198=CARTESIAN_POINT('Ctrl Pts',(-1.13518507442834,6.84892095288905,
36.05));
#307199=CARTESIAN_POINT('Ctrl Pts',(-1.13518507442834,6.84892095288905,
36.29));
#307200=CARTESIAN_POINT('Ctrl Pts',(-1.13392857142857,6.88318283279221,
36.05));
#307201=CARTESIAN_POINT('Ctrl Pts',(-1.13392857142857,6.88318283279221,
36.29));
#307202=CARTESIAN_POINT('',(-1.52371651785714,6.39675324675325,36.05));
#307203=CARTESIAN_POINT('',(-1.52371651785714,6.39675324675325,32.1799631621335));
#307204=CARTESIAN_POINT('',(-1.13392857142857,6.88318283279221,36.05));
#307205=CARTESIAN_POINT('Ctrl Pts',(-1.13392857142857,6.88318283279221,
36.05));
#307206=CARTESIAN_POINT('Ctrl Pts',(-1.13518507442834,6.84892095288905,
36.05));
#307207=CARTESIAN_POINT('Ctrl Pts',(-1.13760625764887,6.78290098418177,
36.05));
#307208=CARTESIAN_POINT('Ctrl Pts',(-1.15909489053248,6.68851996626879,
36.05));
#307209=CARTESIAN_POINT('Ctrl Pts',(-1.19545427309708,6.60421240376617,
36.05));
#307210=CARTESIAN_POINT('Ctrl Pts',(-1.24507578007146,6.5313545752525,36.05));
#307211=CARTESIAN_POINT('Ctrl Pts',(-1.30436731865975,6.47176243493413,
36.05));
#307212=CARTESIAN_POINT('Ctrl Pts',(-1.37190501458764,6.42869442089,36.05));
#307213=CARTESIAN_POINT('Ctrl Pts',(-1.44564553849367,6.40115522024948,
36.05));
#307214=CARTESIAN_POINT('Ctrl Pts',(-1.49749406178753,6.39823178023093,
36.05));
#307215=CARTESIAN_POINT('Ctrl Pts',(-1.52371651785714,6.39675324675325,
36.05));
#307216=CARTESIAN_POINT('',(-1.13392857142857,6.88318283279221,32.1799631621335));
#307217=CARTESIAN_POINT('Ctrl Pts',(-1.13392857142857,6.88318283279221,
36.05));
#307218=CARTESIAN_POINT('Ctrl Pts',(-1.13392857142857,6.88318283279221,
36.29));
#307219=CARTESIAN_POINT('Ctrl Pts',(-1.13513622427257,6.91852455417192,
36.05));
#307220=CARTESIAN_POINT('Ctrl Pts',(-1.13513622427257,6.91852455417192,
36.29));
#307221=CARTESIAN_POINT('Ctrl Pts',(-1.13746675383528,6.98672704040914,
36.05));
#307222=CARTESIAN_POINT('Ctrl Pts',(-1.13746675383528,6.98672704040914,
36.29));
#307223=CARTESIAN_POINT('Ctrl Pts',(-1.15960212713315,7.08387655284218,
36.05));
#307224=CARTESIAN_POINT('Ctrl Pts',(-1.15960212713315,7.08387655284218,
36.29));
#307225=CARTESIAN_POINT('Ctrl Pts',(-1.1967070851926,7.17101343023865,36.05));
#307226=CARTESIAN_POINT('Ctrl Pts',(-1.1967070851926,7.17101343023865,36.29));
#307227=CARTESIAN_POINT('Ctrl Pts',(-1.248366652071,7.24570928090529,36.05));
#307228=CARTESIAN_POINT('Ctrl Pts',(-1.248366652071,7.24570928090529,36.29));
#307229=CARTESIAN_POINT('Ctrl Pts',(-1.30855629123278,7.30781082924543,
36.05));
#307230=CARTESIAN_POINT('Ctrl Pts',(-1.30855629123278,7.30781082924543,
36.29));
#307231=CARTESIAN_POINT('Ctrl Pts',(-1.3763696724576,7.35293658272662,36.05));
#307232=CARTESIAN_POINT('Ctrl Pts',(-1.3763696724576,7.35293658272662,36.29));
#307233=CARTESIAN_POINT('Ctrl Pts',(-1.45006627196568,7.38129222806274,
36.05));
#307234=CARTESIAN_POINT('Ctrl Pts',(-1.45006627196568,7.38129222806274,
36.29));
#307235=CARTESIAN_POINT('Ctrl Pts',(-1.50156524889417,7.38466150198483,
36.05));
#307236=CARTESIAN_POINT('Ctrl Pts',(-1.50156524889417,7.38466150198483,
36.29));
#307237=CARTESIAN_POINT('Ctrl Pts',(-1.52758218344156,7.38636363636364,
36.05));
#307238=CARTESIAN_POINT('Ctrl Pts',(-1.52758218344156,7.38636363636364,
36.29));
#307239=CARTESIAN_POINT('',(-1.52758218344156,7.38636363636364,36.05));
#307240=CARTESIAN_POINT('Ctrl Pts',(-1.52758218344156,7.38636363636364,
36.05));
#307241=CARTESIAN_POINT('Ctrl Pts',(-1.50156524889417,7.38466150198483,
36.05));
#307242=CARTESIAN_POINT('Ctrl Pts',(-1.45006627196568,7.38129222806274,
36.05));
#307243=CARTESIAN_POINT('Ctrl Pts',(-1.3763696724576,7.35293658272662,36.05));
#307244=CARTESIAN_POINT('Ctrl Pts',(-1.30855629123278,7.30781082924543,
36.05));
#307245=CARTESIAN_POINT('Ctrl Pts',(-1.248366652071,7.24570928090529,36.05));
#307246=CARTESIAN_POINT('Ctrl Pts',(-1.1967070851926,7.17101343023865,36.05));
#307247=CARTESIAN_POINT('Ctrl Pts',(-1.15960212713315,7.08387655284218,
36.05));
#307248=CARTESIAN_POINT('Ctrl Pts',(-1.13746675383528,6.98672704040914,
36.05));
#307249=CARTESIAN_POINT('Ctrl Pts',(-1.13513622427257,6.91852455417192,
36.05));
#307250=CARTESIAN_POINT('Ctrl Pts',(-1.13392857142857,6.88318283279221,
36.05));
#307251=CARTESIAN_POINT('',(-1.52758218344156,7.38636363636364,32.1799631621335));
#307252=CARTESIAN_POINT('Ctrl Pts',(-1.52758218344156,7.38636363636364,
36.05));
#307253=CARTESIAN_POINT('Ctrl Pts',(-1.52758218344156,7.38636363636364,
36.29));
#307254=CARTESIAN_POINT('Ctrl Pts',(-1.55358237022155,7.38486930154146,
36.05));
#307255=CARTESIAN_POINT('Ctrl Pts',(-1.55358237022155,7.38486930154146,
36.29));
#307256=CARTESIAN_POINT('Ctrl Pts',(-1.60499794902611,7.38191424239284,
36.05));
#307257=CARTESIAN_POINT('Ctrl Pts',(-1.60499794902611,7.38191424239284,
36.29));
#307258=CARTESIAN_POINT('Ctrl Pts',(-1.67863965341545,7.354443366284,36.05));
#307259=CARTESIAN_POINT('Ctrl Pts',(-1.67863965341545,7.354443366284,36.29));
#307260=CARTESIAN_POINT('Ctrl Pts',(-1.74575926016136,7.30974046602882,
36.05));
#307261=CARTESIAN_POINT('Ctrl Pts',(-1.74575926016136,7.30974046602882,
36.29));
#307262=CARTESIAN_POINT('Ctrl Pts',(-1.80513211335571,7.24931351323173,
36.05));
#307263=CARTESIAN_POINT('Ctrl Pts',(-1.80513211335571,7.24931351323173,
36.29));
#307264=CARTESIAN_POINT('Ctrl Pts',(-1.85584586752056,7.17700242184242,
36.05));
#307265=CARTESIAN_POINT('Ctrl Pts',(-1.85584586752056,7.17700242184242,
36.29));
#307266=CARTESIAN_POINT('Ctrl Pts',(-1.8909492802511,7.09344714231162,36.05));
#307267=CARTESIAN_POINT('Ctrl Pts',(-1.8909492802511,7.09344714231162,36.29));
#307268=CARTESIAN_POINT('Ctrl Pts',(-1.91396932214169,7.00188822714751,
36.05));
#307269=CARTESIAN_POINT('Ctrl Pts',(-1.91396932214169,7.00188822714751,
36.29));
#307270=CARTESIAN_POINT('Ctrl Pts',(-1.91621068652427,6.93766582705582,
36.05));
#307271=CARTESIAN_POINT('Ctrl Pts',(-1.91621068652427,6.93766582705582,
36.29));
#307272=CARTESIAN_POINT('Ctrl Pts',(-1.91737012987013,6.90444399350649,
36.05));
#307273=CARTESIAN_POINT('Ctrl Pts',(-1.91737012987013,6.90444399350649,
36.29));
#307274=CARTESIAN_POINT('',(-1.91737012987013,6.90444399350649,36.05));
#307275=CARTESIAN_POINT('Ctrl Pts',(-1.91737012987013,6.90444399350649,
36.05));
#307276=CARTESIAN_POINT('Ctrl Pts',(-1.91621068652427,6.93766582705582,
36.05));
#307277=CARTESIAN_POINT('Ctrl Pts',(-1.91396932214169,7.00188822714751,
36.05));
#307278=CARTESIAN_POINT('Ctrl Pts',(-1.8909492802511,7.09344714231162,36.05));
#307279=CARTESIAN_POINT('Ctrl Pts',(-1.85584586752056,7.17700242184242,
36.05));
#307280=CARTESIAN_POINT('Ctrl Pts',(-1.80513211335571,7.24931351323173,
36.05));
#307281=CARTESIAN_POINT('Ctrl Pts',(-1.74575926016136,7.30974046602882,
36.05));
#307282=CARTESIAN_POINT('Ctrl Pts',(-1.67863965341545,7.354443366284,36.05));
#307283=CARTESIAN_POINT('Ctrl Pts',(-1.60499794902611,7.38191424239284,
36.05));
#307284=CARTESIAN_POINT('Ctrl Pts',(-1.55358237022155,7.38486930154146,
36.05));
#307285=CARTESIAN_POINT('Ctrl Pts',(-1.52758218344156,7.38636363636364,
36.05));
#307286=CARTESIAN_POINT('',(-1.91737012987013,6.90444399350649,32.1799631621335));
#307287=CARTESIAN_POINT('Ctrl Pts',(-1.91737012987013,6.90444399350649,
36.05));
#307288=CARTESIAN_POINT('Ctrl Pts',(-1.91737012987013,6.90444399350649,
36.29));
#307289=CARTESIAN_POINT('Ctrl Pts',(-1.91613148952843,6.8676136615146,36.05));
#307290=CARTESIAN_POINT('Ctrl Pts',(-1.91613148952843,6.8676136615146,36.29));
#307291=CARTESIAN_POINT('Ctrl Pts',(-1.91376144516393,6.79714161418861,
36.05));
#307292=CARTESIAN_POINT('Ctrl Pts',(-1.91376144516393,6.79714161418861,
36.29));
#307293=CARTESIAN_POINT('Ctrl Pts',(-1.89249074922576,6.69694686802566,
36.05));
#307294=CARTESIAN_POINT('Ctrl Pts',(-1.89249074922576,6.69694686802566,
36.29));
#307295=CARTESIAN_POINT('Ctrl Pts',(-1.85626188657584,6.60868448959127,
36.05));
#307296=CARTESIAN_POINT('Ctrl Pts',(-1.85626188657584,6.60868448959127,
36.29));
#307297=CARTESIAN_POINT('Ctrl Pts',(-1.80667059916436,6.53319043392833,
36.05));
#307298=CARTESIAN_POINT('Ctrl Pts',(-1.80667059916436,6.53319043392833,
36.29));
#307299=CARTESIAN_POINT('Ctrl Pts',(-1.74600279585425,6.47327605218271,
36.05));
#307300=CARTESIAN_POINT('Ctrl Pts',(-1.74600279585425,6.47327605218271,
36.29));
#307301=CARTESIAN_POINT('Ctrl Pts',(-1.67833795046176,6.42829274914181,
36.05));
#307302=CARTESIAN_POINT('Ctrl Pts',(-1.67833795046176,6.42829274914181,
36.29));
#307303=CARTESIAN_POINT('Ctrl Pts',(-1.60297996097691,6.4012532984509,36.05));
#307304=CARTESIAN_POINT('Ctrl Pts',(-1.60297996097691,6.4012532984509,36.29));
#307305=CARTESIAN_POINT('Ctrl Pts',(-1.5503437032771,6.39826496143831,36.05));
#307306=CARTESIAN_POINT('Ctrl Pts',(-1.5503437032771,6.39826496143831,36.29));
#307307=CARTESIAN_POINT('Ctrl Pts',(-1.52371651785714,6.39675324675325,
36.05));
#307308=CARTESIAN_POINT('Ctrl Pts',(-1.52371651785714,6.39675324675325,
36.29));
#307309=CARTESIAN_POINT('Ctrl Pts',(-1.52371651785714,6.39675324675325,
36.05));
#307310=CARTESIAN_POINT('Ctrl Pts',(-1.5503437032771,6.39826496143831,36.05));
#307311=CARTESIAN_POINT('Ctrl Pts',(-1.60297996097691,6.4012532984509,36.05));
#307312=CARTESIAN_POINT('Ctrl Pts',(-1.67833795046176,6.42829274914181,
36.05));
#307313=CARTESIAN_POINT('Ctrl Pts',(-1.74600279585425,6.47327605218271,
36.05));
#307314=CARTESIAN_POINT('Ctrl Pts',(-1.80667059916436,6.53319043392833,
36.05));
#307315=CARTESIAN_POINT('Ctrl Pts',(-1.85626188657584,6.60868448959127,
36.05));
#307316=CARTESIAN_POINT('Ctrl Pts',(-1.89249074922576,6.69694686802566,
36.05));
#307317=CARTESIAN_POINT('Ctrl Pts',(-1.91376144516393,6.79714161418861,
36.05));
#307318=CARTESIAN_POINT('Ctrl Pts',(-1.91613148952843,6.8676136615146,36.05));
#307319=CARTESIAN_POINT('Ctrl Pts',(-1.91737012987013,6.90444399350649,
36.05));
#307320=CARTESIAN_POINT('Ctrl Pts',(1.52758218344156,4.78863636363636,36.05));
#307321=CARTESIAN_POINT('Ctrl Pts',(1.52758218344156,4.78863636363636,36.29));
#307322=CARTESIAN_POINT('Ctrl Pts',(1.54523256318688,4.78904075129562,36.05));
#307323=CARTESIAN_POINT('Ctrl Pts',(1.54523256318688,4.78904075129562,36.29));
#307324=CARTESIAN_POINT('Ctrl Pts',(1.5798837022752,4.78983464316812,36.05));
#307325=CARTESIAN_POINT('Ctrl Pts',(1.5798837022752,4.78983464316812,36.29));
#307326=CARTESIAN_POINT('Ctrl Pts',(1.63079567698862,4.79884546139153,36.05));
#307327=CARTESIAN_POINT('Ctrl Pts',(1.63079567698862,4.79884546139153,36.29));
#307328=CARTESIAN_POINT('Ctrl Pts',(1.67970258395479,4.81206099883602,36.05));
#307329=CARTESIAN_POINT('Ctrl Pts',(1.67970258395479,4.81206099883602,36.29));
#307330=CARTESIAN_POINT('Ctrl Pts',(1.72652298376726,4.83107657862712,36.05));
#307331=CARTESIAN_POINT('Ctrl Pts',(1.72652298376726,4.83107657862712,36.29));
#307332=CARTESIAN_POINT('Ctrl Pts',(1.77140565570483,4.85499849822356,36.05));
#307333=CARTESIAN_POINT('Ctrl Pts',(1.77140565570483,4.85499849822356,36.29));
#307334=CARTESIAN_POINT('Ctrl Pts',(1.81390598351971,4.88475706229418,36.05));
#307335=CARTESIAN_POINT('Ctrl Pts',(1.81390598351971,4.88475706229418,36.29));
#307336=CARTESIAN_POINT('Ctrl Pts',(1.85419832598593,4.92023184841449,36.05));
#307337=CARTESIAN_POINT('Ctrl Pts',(1.85419832598593,4.92023184841449,36.29));
#307338=CARTESIAN_POINT('Ctrl Pts',(1.89265117091878,4.96016808484432,36.05));
#307339=CARTESIAN_POINT('Ctrl Pts',(1.89265117091878,4.96016808484432,36.29));
#307340=CARTESIAN_POINT('Ctrl Pts',(1.92696273298897,5.00550562421531,36.05));
#307341=CARTESIAN_POINT('Ctrl Pts',(1.92696273298897,5.00550562421531,36.29));
#307342=CARTESIAN_POINT('Ctrl Pts',(1.95867569552678,5.05353436556821,36.05));
#307343=CARTESIAN_POINT('Ctrl Pts',(1.95867569552678,5.05353436556821,36.29));
#307344=CARTESIAN_POINT('Ctrl Pts',(1.9831268819592,5.10649857927001,36.05));
#307345=CARTESIAN_POINT('Ctrl Pts',(1.9831268819592,5.10649857927001,36.29));
#307346=CARTESIAN_POINT('Ctrl Pts',(2.00511626181496,5.16193679017606,36.05));
#307347=CARTESIAN_POINT('Ctrl Pts',(2.00511626181496,5.16193679017606,36.29));
#307348=CARTESIAN_POINT('Ctrl Pts',(2.02054669570705,5.22177284922642,36.05));
#307349=CARTESIAN_POINT('Ctrl Pts',(2.02054669570705,5.22177284922642,36.29));
#307350=CARTESIAN_POINT('Ctrl Pts',(2.0334543847172,5.28488392294487,36.05));
#307351=CARTESIAN_POINT('Ctrl Pts',(2.0334543847172,5.28488392294487,36.29));
#307352=CARTESIAN_POINT('Ctrl Pts',(2.03922895997908,5.35205975094169,36.05));
#307353=CARTESIAN_POINT('Ctrl Pts',(2.03922895997908,5.35205975094169,36.29));
#307354=CARTESIAN_POINT('Ctrl Pts',(2.04044852772871,5.39790252089427,36.05));
#307355=CARTESIAN_POINT('Ctrl Pts',(2.04044852772871,5.39790252089427,36.29));
#307356=CARTESIAN_POINT('Ctrl Pts',(2.04107142857143,5.42131696428571,36.05));
#307357=CARTESIAN_POINT('Ctrl Pts',(2.04107142857143,5.42131696428571,36.29));
#307358=CARTESIAN_POINT('',(1.52758218344156,4.78863636363636,36.05));
#307359=CARTESIAN_POINT('',(1.52758218344156,4.78863636363636,32.1799631621335));
#307360=CARTESIAN_POINT('',(2.04107142857143,5.42131696428571,36.05));
#307361=CARTESIAN_POINT('Ctrl Pts',(2.04107142857143,5.42131696428571,36.05));
#307362=CARTESIAN_POINT('Ctrl Pts',(2.04044852772871,5.39790252089427,36.05));
#307363=CARTESIAN_POINT('Ctrl Pts',(2.03922895997908,5.35205975094169,36.05));
#307364=CARTESIAN_POINT('Ctrl Pts',(2.0334543847172,5.28488392294487,36.05));
#307365=CARTESIAN_POINT('Ctrl Pts',(2.02054669570705,5.22177284922642,36.05));
#307366=CARTESIAN_POINT('Ctrl Pts',(2.00511626181496,5.16193679017606,36.05));
#307367=CARTESIAN_POINT('Ctrl Pts',(1.9831268819592,5.10649857927001,36.05));
#307368=CARTESIAN_POINT('Ctrl Pts',(1.95867569552678,5.05353436556821,36.05));
#307369=CARTESIAN_POINT('Ctrl Pts',(1.92696273298897,5.00550562421531,36.05));
#307370=CARTESIAN_POINT('Ctrl Pts',(1.89265117091878,4.96016808484432,36.05));
#307371=CARTESIAN_POINT('Ctrl Pts',(1.85419832598593,4.92023184841449,36.05));
#307372=CARTESIAN_POINT('Ctrl Pts',(1.81390598351971,4.88475706229418,36.05));
#307373=CARTESIAN_POINT('Ctrl Pts',(1.77140565570483,4.85499849822356,36.05));
#307374=CARTESIAN_POINT('Ctrl Pts',(1.72652298376726,4.83107657862712,36.05));
#307375=CARTESIAN_POINT('Ctrl Pts',(1.67970258395479,4.81206099883602,36.05));
#307376=CARTESIAN_POINT('Ctrl Pts',(1.63079567698862,4.79884546139153,36.05));
#307377=CARTESIAN_POINT('Ctrl Pts',(1.5798837022752,4.78983464316812,36.05));
#307378=CARTESIAN_POINT('Ctrl Pts',(1.54523256318688,4.78904075129562,36.05));
#307379=CARTESIAN_POINT('Ctrl Pts',(1.52758218344156,4.78863636363636,36.05));
#307380=CARTESIAN_POINT('',(2.04107142857143,5.42131696428571,32.1799631621335));
#307381=CARTESIAN_POINT('Ctrl Pts',(2.04107142857143,5.42131696428571,36.05));
#307382=CARTESIAN_POINT('Ctrl Pts',(2.04107142857143,5.42131696428571,36.29));
#307383=CARTESIAN_POINT('Ctrl Pts',(2.04053270667799,5.44495600403826,36.05));
#307384=CARTESIAN_POINT('Ctrl Pts',(2.04053270667799,5.44495600403826,36.29));
#307385=CARTESIAN_POINT('Ctrl Pts',(2.0394772775854,5.49126808190085,36.05));
#307386=CARTESIAN_POINT('Ctrl Pts',(2.0394772775854,5.49126808190085,36.29));
#307387=CARTESIAN_POINT('Ctrl Pts',(2.03251602654254,5.55896687878814,36.05));
#307388=CARTESIAN_POINT('Ctrl Pts',(2.03251602654254,5.55896687878814,36.29));
#307389=CARTESIAN_POINT('Ctrl Pts',(2.02022069750506,5.62293356367208,36.05));
#307390=CARTESIAN_POINT('Ctrl Pts',(2.02022069750506,5.62293356367208,36.29));
#307391=CARTESIAN_POINT('Ctrl Pts',(2.00340124721791,5.68327106051297,36.05));
#307392=CARTESIAN_POINT('Ctrl Pts',(2.00340124721791,5.68327106051297,36.29));
#307393=CARTESIAN_POINT('Ctrl Pts',(1.98221217886446,5.74035420483588,36.05));
#307394=CARTESIAN_POINT('Ctrl Pts',(1.98221217886446,5.74035420483588,36.29));
#307395=CARTESIAN_POINT('Ctrl Pts',(1.95582710639876,5.79399835274014,36.05));
#307396=CARTESIAN_POINT('Ctrl Pts',(1.95582710639876,5.79399835274014,36.29));
#307397=CARTESIAN_POINT('Ctrl Pts',(1.92410277702741,5.84377259737151,36.05));
#307398=CARTESIAN_POINT('Ctrl Pts',(1.92410277702741,5.84377259737151,36.29));
#307399=CARTESIAN_POINT('Ctrl Pts',(1.88783253473841,5.88934000071629,36.05));
#307400=CARTESIAN_POINT('Ctrl Pts',(1.88783253473841,5.88934000071629,36.29));
#307401=CARTESIAN_POINT('Ctrl Pts',(1.84907731850073,5.93098943621083,36.05));
#307402=CARTESIAN_POINT('Ctrl Pts',(1.84907731850073,5.93098943621083,36.29));
#307403=CARTESIAN_POINT('Ctrl Pts',(1.80771391130794,5.96739207884556,36.05));
#307404=CARTESIAN_POINT('Ctrl Pts',(1.80771391130794,5.96739207884556,36.29));
#307405=CARTESIAN_POINT('Ctrl Pts',(1.76414349382133,5.99780008387924,36.05));
#307406=CARTESIAN_POINT('Ctrl Pts',(1.76414349382133,5.99780008387924,36.29));
#307407=CARTESIAN_POINT('Ctrl Pts',(1.71900701398188,6.02332207855003,36.05));
#307408=CARTESIAN_POINT('Ctrl Pts',(1.71900701398188,6.02332207855003,36.29));
#307409=CARTESIAN_POINT('Ctrl Pts',(1.67166640701484,6.04244867323907,36.05));
#307410=CARTESIAN_POINT('Ctrl Pts',(1.67166640701484,6.04244867323907,36.29));
#307411=CARTESIAN_POINT('Ctrl Pts',(1.62279736679542,6.05706063884487,36.05));
#307412=CARTESIAN_POINT('Ctrl Pts',(1.62279736679542,6.05706063884487,36.29));
#307413=CARTESIAN_POINT('Ctrl Pts',(1.57169261973291,6.0655628055813,36.05));
#307414=CARTESIAN_POINT('Ctrl Pts',(1.57169261973291,6.0655628055813,36.29));
#307415=CARTESIAN_POINT('Ctrl Pts',(1.53684768525004,6.06643934639816,36.05));
#307416=CARTESIAN_POINT('Ctrl Pts',(1.53684768525004,6.06643934639816,36.29));
#307417=CARTESIAN_POINT('Ctrl Pts',(1.51920657467533,6.06688311688312,36.05));
#307418=CARTESIAN_POINT('Ctrl Pts',(1.51920657467533,6.06688311688312,36.29));
#307419=CARTESIAN_POINT('',(1.51920657467533,6.06688311688312,36.05));
#307420=CARTESIAN_POINT('Ctrl Pts',(1.51920657467533,6.06688311688312,36.05));
#307421=CARTESIAN_POINT('Ctrl Pts',(1.53684768525004,6.06643934639816,36.05));
#307422=CARTESIAN_POINT('Ctrl Pts',(1.57169261973291,6.0655628055813,36.05));
#307423=CARTESIAN_POINT('Ctrl Pts',(1.62279736679542,6.05706063884487,36.05));
#307424=CARTESIAN_POINT('Ctrl Pts',(1.67166640701484,6.04244867323907,36.05));
#307425=CARTESIAN_POINT('Ctrl Pts',(1.71900701398188,6.02332207855003,36.05));
#307426=CARTESIAN_POINT('Ctrl Pts',(1.76414349382133,5.99780008387924,36.05));
#307427=CARTESIAN_POINT('Ctrl Pts',(1.80771391130794,5.96739207884556,36.05));
#307428=CARTESIAN_POINT('Ctrl Pts',(1.84907731850073,5.93098943621083,36.05));
#307429=CARTESIAN_POINT('Ctrl Pts',(1.88783253473841,5.88934000071629,36.05));
#307430=CARTESIAN_POINT('Ctrl Pts',(1.92410277702741,5.84377259737151,36.05));
#307431=CARTESIAN_POINT('Ctrl Pts',(1.95582710639876,5.79399835274014,36.05));
#307432=CARTESIAN_POINT('Ctrl Pts',(1.98221217886446,5.74035420483588,36.05));
#307433=CARTESIAN_POINT('Ctrl Pts',(2.00340124721791,5.68327106051297,36.05));
#307434=CARTESIAN_POINT('Ctrl Pts',(2.02022069750506,5.62293356367208,36.05));
#307435=CARTESIAN_POINT('Ctrl Pts',(2.03251602654254,5.55896687878814,36.05));
#307436=CARTESIAN_POINT('Ctrl Pts',(2.0394772775854,5.49126808190085,36.05));
#307437=CARTESIAN_POINT('Ctrl Pts',(2.04053270667799,5.44495600403826,36.05));
#307438=CARTESIAN_POINT('Ctrl Pts',(2.04107142857143,5.42131696428571,36.05));
#307439=CARTESIAN_POINT('',(1.51920657467533,6.06688311688312,32.1799631621335));
#307440=CARTESIAN_POINT('Ctrl Pts',(1.51920657467533,6.06688311688312,36.05));
#307441=CARTESIAN_POINT('Ctrl Pts',(1.51920657467533,6.06688311688312,36.29));
#307442=CARTESIAN_POINT('Ctrl Pts',(1.5017821965604,6.066434027441,36.05));
#307443=CARTESIAN_POINT('Ctrl Pts',(1.5017821965604,6.066434027441,36.29));
#307444=CARTESIAN_POINT('Ctrl Pts',(1.46736804529077,6.06554704990339,36.05));
#307445=CARTESIAN_POINT('Ctrl Pts',(1.46736804529077,6.06554704990339,36.29));
#307446=CARTESIAN_POINT('Ctrl Pts',(1.41686786206546,6.05712286492333,36.05));
#307447=CARTESIAN_POINT('Ctrl Pts',(1.41686786206546,6.05712286492333,36.29));
#307448=CARTESIAN_POINT('Ctrl Pts',(1.36884631219687,6.04224031339717,36.05));
#307449=CARTESIAN_POINT('Ctrl Pts',(1.36884631219687,6.04224031339717,36.29));
#307450=CARTESIAN_POINT('Ctrl Pts',(1.32191903516798,6.02430730620351,36.05));
#307451=CARTESIAN_POINT('Ctrl Pts',(1.32191903516798,6.02430730620351,36.29));
#307452=CARTESIAN_POINT('Ctrl Pts',(1.27807748224968,5.99813668132169,36.05));
#307453=CARTESIAN_POINT('Ctrl Pts',(1.27807748224968,5.99813668132169,36.29));
#307454=CARTESIAN_POINT('Ctrl Pts',(1.23519630821944,5.96827285277196,36.05));
#307455=CARTESIAN_POINT('Ctrl Pts',(1.23519630821944,5.96827285277196,36.29));
#307456=CARTESIAN_POINT('Ctrl Pts',(1.19537510098809,5.93155196527191,36.05));
#307457=CARTESIAN_POINT('Ctrl Pts',(1.19537510098809,5.93155196527191,36.29));
#307458=CARTESIAN_POINT('Ctrl Pts',(1.15739985251507,5.89060348709459,36.05));
#307459=CARTESIAN_POINT('Ctrl Pts',(1.15739985251507,5.89060348709459,36.29));
#307460=CARTESIAN_POINT('Ctrl Pts',(1.12287571225305,5.84507968533496,36.05));
#307461=CARTESIAN_POINT('Ctrl Pts',(1.12287571225305,5.84507968533496,36.29));
#307462=CARTESIAN_POINT('Ctrl Pts',(1.09234252291203,5.79605922055842,36.05));
#307463=CARTESIAN_POINT('Ctrl Pts',(1.09234252291203,5.79605922055842,36.29));
#307464=CARTESIAN_POINT('Ctrl Pts',(1.06720719606548,5.74343345049149,36.05));
#307465=CARTESIAN_POINT('Ctrl Pts',(1.06720719606548,5.74343345049149,36.29));
#307466=CARTESIAN_POINT('Ctrl Pts',(1.04675217280647,5.68767671276929,36.05));
#307467=CARTESIAN_POINT('Ctrl Pts',(1.04675217280647,5.68767671276929,36.29));
#307468=CARTESIAN_POINT('Ctrl Pts',(1.02968321354559,5.6290296721576,36.05));
#307469=CARTESIAN_POINT('Ctrl Pts',(1.02968321354559,5.6290296721576,36.29));
#307470=CARTESIAN_POINT('Ctrl Pts',(1.01820393934243,5.56687880407454,36.05));
#307471=CARTESIAN_POINT('Ctrl Pts',(1.01820393934243,5.56687880407454,36.29));
#307472=CARTESIAN_POINT('Ctrl Pts',(1.01197456783159,5.50155035955671,36.05));
#307473=CARTESIAN_POINT('Ctrl Pts',(1.01197456783159,5.50155035955671,36.29));
#307474=CARTESIAN_POINT('Ctrl Pts',(1.01081821236896,5.45697972788144,36.05));
#307475=CARTESIAN_POINT('Ctrl Pts',(1.01081821236896,5.45697972788144,36.29));
#307476=CARTESIAN_POINT('Ctrl Pts',(1.01022727272727,5.43420251623377,36.05));
#307477=CARTESIAN_POINT('Ctrl Pts',(1.01022727272727,5.43420251623377,36.29));
#307478=CARTESIAN_POINT('',(1.01022727272727,5.43420251623377,36.05));
#307479=CARTESIAN_POINT('Ctrl Pts',(1.01022727272727,5.43420251623377,36.05));
#307480=CARTESIAN_POINT('Ctrl Pts',(1.01081821236896,5.45697972788144,36.05));
#307481=CARTESIAN_POINT('Ctrl Pts',(1.01197456783159,5.50155035955671,36.05));
#307482=CARTESIAN_POINT('Ctrl Pts',(1.01820393934243,5.56687880407454,36.05));
#307483=CARTESIAN_POINT('Ctrl Pts',(1.02968321354559,5.6290296721576,36.05));
#307484=CARTESIAN_POINT('Ctrl Pts',(1.04675217280647,5.68767671276929,36.05));
#307485=CARTESIAN_POINT('Ctrl Pts',(1.06720719606548,5.74343345049149,36.05));
#307486=CARTESIAN_POINT('Ctrl Pts',(1.09234252291203,5.79605922055842,36.05));
#307487=CARTESIAN_POINT('Ctrl Pts',(1.12287571225305,5.84507968533496,36.05));
#307488=CARTESIAN_POINT('Ctrl Pts',(1.15739985251507,5.89060348709459,36.05));
#307489=CARTESIAN_POINT('Ctrl Pts',(1.19537510098809,5.93155196527191,36.05));
#307490=CARTESIAN_POINT('Ctrl Pts',(1.23519630821944,5.96827285277196,36.05));
#307491=CARTESIAN_POINT('Ctrl Pts',(1.27807748224968,5.99813668132169,36.05));
#307492=CARTESIAN_POINT('Ctrl Pts',(1.32191903516798,6.02430730620351,36.05));
#307493=CARTESIAN_POINT('Ctrl Pts',(1.36884631219687,6.04224031339717,36.05));
#307494=CARTESIAN_POINT('Ctrl Pts',(1.41686786206546,6.05712286492333,36.05));
#307495=CARTESIAN_POINT('Ctrl Pts',(1.46736804529077,6.06554704990339,36.05));
#307496=CARTESIAN_POINT('Ctrl Pts',(1.5017821965604,6.066434027441,36.05));
#307497=CARTESIAN_POINT('Ctrl Pts',(1.51920657467533,6.06688311688312,36.05));
#307498=CARTESIAN_POINT('',(1.01022727272727,5.43420251623377,32.1799631621335));
#307499=CARTESIAN_POINT('Ctrl Pts',(1.01022727272727,5.43420251623377,36.05));
#307500=CARTESIAN_POINT('Ctrl Pts',(1.01022727272727,5.43420251623377,36.29));
#307501=CARTESIAN_POINT('Ctrl Pts',(1.01074437462189,5.41055942108448,36.05));
#307502=CARTESIAN_POINT('Ctrl Pts',(1.01074437462189,5.41055942108448,36.29));
#307503=CARTESIAN_POINT('Ctrl Pts',(1.01175744721102,5.36423939815086,36.05));
#307504=CARTESIAN_POINT('Ctrl Pts',(1.01175744721102,5.36423939815086,36.29));
#307505=CARTESIAN_POINT('Ctrl Pts',(1.01901764419993,5.2966367303295,36.05));
#307506=CARTESIAN_POINT('Ctrl Pts',(1.01901764419993,5.2966367303295,36.29));
#307507=CARTESIAN_POINT('Ctrl Pts',(1.03022528258824,5.23250639408275,36.05));
#307508=CARTESIAN_POINT('Ctrl Pts',(1.03022528258824,5.23250639408275,36.29));
#307509=CARTESIAN_POINT('Ctrl Pts',(1.04731521355877,5.17226185872411,36.05));
#307510=CARTESIAN_POINT('Ctrl Pts',(1.04731521355877,5.17226185872411,36.29));
#307511=CARTESIAN_POINT('Ctrl Pts',(1.06840426337778,5.11515155101266,36.05));
#307512=CARTESIAN_POINT('Ctrl Pts',(1.06840426337778,5.11515155101266,36.29));
#307513=CARTESIAN_POINT('Ctrl Pts',(1.09486612244816,5.06166487648077,36.05));
#307514=CARTESIAN_POINT('Ctrl Pts',(1.09486612244816,5.06166487648077,36.29));
#307515=CARTESIAN_POINT('Ctrl Pts',(1.12612981159753,5.0117585395718,36.05));
#307516=CARTESIAN_POINT('Ctrl Pts',(1.12612981159753,5.0117585395718,36.29));
#307517=CARTESIAN_POINT('Ctrl Pts',(1.16105752958236,4.96538056994282,36.05));
#307518=CARTESIAN_POINT('Ctrl Pts',(1.16105752958236,4.96538056994282,36.29));
#307519=CARTESIAN_POINT('Ctrl Pts',(1.20052382029073,4.9247537203412,36.05));
#307520=CARTESIAN_POINT('Ctrl Pts',(1.20052382029073,4.9247537203412,36.29));
#307521=CARTESIAN_POINT('Ctrl Pts',(1.24122086442875,4.88798983005251,36.05));
#307522=CARTESIAN_POINT('Ctrl Pts',(1.24122086442875,4.88798983005251,36.29));
#307523=CARTESIAN_POINT('Ctrl Pts',(1.28411117190556,4.85710381362087,36.05));
#307524=CARTESIAN_POINT('Ctrl Pts',(1.28411117190556,4.85710381362087,36.29));
#307525=CARTESIAN_POINT('Ctrl Pts',(1.32939856317298,4.83218747720399,36.05));
#307526=CARTESIAN_POINT('Ctrl Pts',(1.32939856317298,4.83218747720399,36.29));
#307527=CARTESIAN_POINT('Ctrl Pts',(1.37639471981463,4.81303741070312,36.05));
#307528=CARTESIAN_POINT('Ctrl Pts',(1.37639471981463,4.81303741070312,36.29));
#307529=CARTESIAN_POINT('Ctrl Pts',(1.42508500090371,4.79855444913016,36.05));
#307530=CARTESIAN_POINT('Ctrl Pts',(1.42508500090371,4.79855444913016,36.29));
#307531=CARTESIAN_POINT('Ctrl Pts',(1.47573186595857,4.78994040169141,36.05));
#307532=CARTESIAN_POINT('Ctrl Pts',(1.47573186595857,4.78994040169141,36.29));
#307533=CARTESIAN_POINT('Ctrl Pts',(1.51015384301738,4.789074687262,36.05));
#307534=CARTESIAN_POINT('Ctrl Pts',(1.51015384301738,4.789074687262,36.29));
#307535=CARTESIAN_POINT('Ctrl Pts',(1.52758218344156,4.78863636363636,36.05));
#307536=CARTESIAN_POINT('Ctrl Pts',(1.52758218344156,4.78863636363636,36.29));
#307537=CARTESIAN_POINT('Ctrl Pts',(1.52758218344156,4.78863636363636,36.05));
#307538=CARTESIAN_POINT('Ctrl Pts',(1.51015384301738,4.789074687262,36.05));
#307539=CARTESIAN_POINT('Ctrl Pts',(1.47573186595857,4.78994040169141,36.05));
#307540=CARTESIAN_POINT('Ctrl Pts',(1.42508500090371,4.79855444913016,36.05));
#307541=CARTESIAN_POINT('Ctrl Pts',(1.37639471981463,4.81303741070312,36.05));
#307542=CARTESIAN_POINT('Ctrl Pts',(1.32939856317298,4.83218747720399,36.05));
#307543=CARTESIAN_POINT('Ctrl Pts',(1.28411117190556,4.85710381362087,36.05));
#307544=CARTESIAN_POINT('Ctrl Pts',(1.24122086442875,4.88798983005251,36.05));
#307545=CARTESIAN_POINT('Ctrl Pts',(1.20052382029073,4.9247537203412,36.05));
#307546=CARTESIAN_POINT('Ctrl Pts',(1.16105752958236,4.96538056994282,36.05));
#307547=CARTESIAN_POINT('Ctrl Pts',(1.12612981159753,5.0117585395718,36.05));
#307548=CARTESIAN_POINT('Ctrl Pts',(1.09486612244816,5.06166487648077,36.05));
#307549=CARTESIAN_POINT('Ctrl Pts',(1.06840426337778,5.11515155101266,36.05));
#307550=CARTESIAN_POINT('Ctrl Pts',(1.04731521355877,5.17226185872411,36.05));
#307551=CARTESIAN_POINT('Ctrl Pts',(1.03022528258824,5.23250639408275,36.05));
#307552=CARTESIAN_POINT('Ctrl Pts',(1.01901764419993,5.2966367303295,36.05));
#307553=CARTESIAN_POINT('Ctrl Pts',(1.01175744721102,5.36423939815086,36.05));
#307554=CARTESIAN_POINT('Ctrl Pts',(1.01074437462189,5.41055942108448,36.05));
#307555=CARTESIAN_POINT('Ctrl Pts',(1.01022727272727,5.43420251623377,36.05));
#307556=CARTESIAN_POINT('Ctrl Pts',(1.52758218344156,6.39675324675325,36.05));
#307557=CARTESIAN_POINT('Ctrl Pts',(1.52758218344156,6.39675324675325,36.29));
#307558=CARTESIAN_POINT('Ctrl Pts',(1.55380463951118,6.39823178023093,36.05));
#307559=CARTESIAN_POINT('Ctrl Pts',(1.55380463951118,6.39823178023093,36.29));
#307560=CARTESIAN_POINT('Ctrl Pts',(1.60565316280503,6.40115522024948,36.05));
#307561=CARTESIAN_POINT('Ctrl Pts',(1.60565316280503,6.40115522024948,36.29));
#307562=CARTESIAN_POINT('Ctrl Pts',(1.67939368671106,6.42869442089,36.05));
#307563=CARTESIAN_POINT('Ctrl Pts',(1.67939368671106,6.42869442089,36.29));
#307564=CARTESIAN_POINT('Ctrl Pts',(1.74693138263896,6.47176243493413,36.05));
#307565=CARTESIAN_POINT('Ctrl Pts',(1.74693138263896,6.47176243493413,36.29));
#307566=CARTESIAN_POINT('Ctrl Pts',(1.80622292122723,6.5313545752525,36.05));
#307567=CARTESIAN_POINT('Ctrl Pts',(1.80622292122723,6.5313545752525,36.29));
#307568=CARTESIAN_POINT('Ctrl Pts',(1.85584442820162,6.60421240376617,36.05));
#307569=CARTESIAN_POINT('Ctrl Pts',(1.85584442820162,6.60421240376617,36.29));
#307570=CARTESIAN_POINT('Ctrl Pts',(1.89220381076623,6.68851996626879,36.05));
#307571=CARTESIAN_POINT('Ctrl Pts',(1.89220381076623,6.68851996626879,36.29));
#307572=CARTESIAN_POINT('Ctrl Pts',(1.91369244364984,6.78290098418177,36.05));
#307573=CARTESIAN_POINT('Ctrl Pts',(1.91369244364984,6.78290098418177,36.29));
#307574=CARTESIAN_POINT('Ctrl Pts',(1.91611362687036,6.84892095288905,36.05));
#307575=CARTESIAN_POINT('Ctrl Pts',(1.91611362687036,6.84892095288905,36.29));
#307576=CARTESIAN_POINT('Ctrl Pts',(1.91737012987013,6.88318283279221,36.05));
#307577=CARTESIAN_POINT('Ctrl Pts',(1.91737012987013,6.88318283279221,36.29));
#307578=CARTESIAN_POINT('',(1.52758218344156,6.39675324675325,36.05));
#307579=CARTESIAN_POINT('',(1.52758218344156,6.39675324675325,32.1799631621335));
#307580=CARTESIAN_POINT('',(1.91737012987013,6.88318283279221,36.05));
#307581=CARTESIAN_POINT('Ctrl Pts',(1.91737012987013,6.88318283279221,36.05));
#307582=CARTESIAN_POINT('Ctrl Pts',(1.91611362687036,6.84892095288905,36.05));
#307583=CARTESIAN_POINT('Ctrl Pts',(1.91369244364984,6.78290098418177,36.05));
#307584=CARTESIAN_POINT('Ctrl Pts',(1.89220381076623,6.68851996626879,36.05));
#307585=CARTESIAN_POINT('Ctrl Pts',(1.85584442820162,6.60421240376617,36.05));
#307586=CARTESIAN_POINT('Ctrl Pts',(1.80622292122723,6.5313545752525,36.05));
#307587=CARTESIAN_POINT('Ctrl Pts',(1.74693138263896,6.47176243493413,36.05));
#307588=CARTESIAN_POINT('Ctrl Pts',(1.67939368671106,6.42869442089,36.05));
#307589=CARTESIAN_POINT('Ctrl Pts',(1.60565316280503,6.40115522024948,36.05));
#307590=CARTESIAN_POINT('Ctrl Pts',(1.55380463951118,6.39823178023093,36.05));
#307591=CARTESIAN_POINT('Ctrl Pts',(1.52758218344156,6.39675324675325,36.05));
#307592=CARTESIAN_POINT('',(1.91737012987013,6.88318283279221,32.1799631621335));
#307593=CARTESIAN_POINT('Ctrl Pts',(1.91737012987013,6.88318283279221,36.05));
#307594=CARTESIAN_POINT('Ctrl Pts',(1.91737012987013,6.88318283279221,36.29));
#307595=CARTESIAN_POINT('Ctrl Pts',(1.91616247702613,6.91852455417192,36.05));
#307596=CARTESIAN_POINT('Ctrl Pts',(1.91616247702613,6.91852455417192,36.29));
#307597=CARTESIAN_POINT('Ctrl Pts',(1.91383194746342,6.98672704040914,36.05));
#307598=CARTESIAN_POINT('Ctrl Pts',(1.91383194746342,6.98672704040914,36.29));
#307599=CARTESIAN_POINT('Ctrl Pts',(1.89169657416555,7.08387655284218,36.05));
#307600=CARTESIAN_POINT('Ctrl Pts',(1.89169657416555,7.08387655284218,36.29));
#307601=CARTESIAN_POINT('Ctrl Pts',(1.8545916161061,7.17101343023865,36.05));
#307602=CARTESIAN_POINT('Ctrl Pts',(1.8545916161061,7.17101343023865,36.29));
#307603=CARTESIAN_POINT('Ctrl Pts',(1.80293204922771,7.24570928090529,36.05));
#307604=CARTESIAN_POINT('Ctrl Pts',(1.80293204922771,7.24570928090529,36.29));
#307605=CARTESIAN_POINT('Ctrl Pts',(1.74274241006592,7.30781082924543,36.05));
#307606=CARTESIAN_POINT('Ctrl Pts',(1.74274241006592,7.30781082924543,36.29));
#307607=CARTESIAN_POINT('Ctrl Pts',(1.6749290288411,7.35293658272662,36.05));
#307608=CARTESIAN_POINT('Ctrl Pts',(1.6749290288411,7.35293658272662,36.29));
#307609=CARTESIAN_POINT('Ctrl Pts',(1.60123242933302,7.38129222806274,36.05));
#307610=CARTESIAN_POINT('Ctrl Pts',(1.60123242933302,7.38129222806274,36.29));
#307611=CARTESIAN_POINT('Ctrl Pts',(1.54973345240453,7.38466150198483,36.05));
#307612=CARTESIAN_POINT('Ctrl Pts',(1.54973345240453,7.38466150198483,36.29));
#307613=CARTESIAN_POINT('Ctrl Pts',(1.52371651785715,7.38636363636364,36.05));
#307614=CARTESIAN_POINT('Ctrl Pts',(1.52371651785715,7.38636363636364,36.29));
#307615=CARTESIAN_POINT('',(1.52371651785715,7.38636363636364,36.05));
#307616=CARTESIAN_POINT('Ctrl Pts',(1.52371651785715,7.38636363636364,36.05));
#307617=CARTESIAN_POINT('Ctrl Pts',(1.54973345240453,7.38466150198483,36.05));
#307618=CARTESIAN_POINT('Ctrl Pts',(1.60123242933302,7.38129222806274,36.05));
#307619=CARTESIAN_POINT('Ctrl Pts',(1.6749290288411,7.35293658272662,36.05));
#307620=CARTESIAN_POINT('Ctrl Pts',(1.74274241006592,7.30781082924543,36.05));
#307621=CARTESIAN_POINT('Ctrl Pts',(1.80293204922771,7.24570928090529,36.05));
#307622=CARTESIAN_POINT('Ctrl Pts',(1.8545916161061,7.17101343023865,36.05));
#307623=CARTESIAN_POINT('Ctrl Pts',(1.89169657416555,7.08387655284218,36.05));
#307624=CARTESIAN_POINT('Ctrl Pts',(1.91383194746342,6.98672704040914,36.05));
#307625=CARTESIAN_POINT('Ctrl Pts',(1.91616247702613,6.91852455417192,36.05));
#307626=CARTESIAN_POINT('Ctrl Pts',(1.91737012987013,6.88318283279221,36.05));
#307627=CARTESIAN_POINT('',(1.52371651785715,7.38636363636364,32.1799631621335));
#307628=CARTESIAN_POINT('Ctrl Pts',(1.52371651785715,7.38636363636364,36.05));
#307629=CARTESIAN_POINT('Ctrl Pts',(1.52371651785715,7.38636363636364,36.29));
#307630=CARTESIAN_POINT('Ctrl Pts',(1.49771633107715,7.38486930154146,36.05));
#307631=CARTESIAN_POINT('Ctrl Pts',(1.49771633107715,7.38486930154146,36.29));
#307632=CARTESIAN_POINT('Ctrl Pts',(1.4463007522726,7.38191424239284,36.05));
#307633=CARTESIAN_POINT('Ctrl Pts',(1.4463007522726,7.38191424239284,36.29));
#307634=CARTESIAN_POINT('Ctrl Pts',(1.37265904788325,7.354443366284,36.05));
#307635=CARTESIAN_POINT('Ctrl Pts',(1.37265904788325,7.354443366284,36.29));
#307636=CARTESIAN_POINT('Ctrl Pts',(1.30553944113734,7.30974046602882,36.05));
#307637=CARTESIAN_POINT('Ctrl Pts',(1.30553944113734,7.30974046602882,36.29));
#307638=CARTESIAN_POINT('Ctrl Pts',(1.246166587943,7.24931351323173,36.05));
#307639=CARTESIAN_POINT('Ctrl Pts',(1.246166587943,7.24931351323173,36.29));
#307640=CARTESIAN_POINT('Ctrl Pts',(1.19545283377814,7.17700242184241,36.05));
#307641=CARTESIAN_POINT('Ctrl Pts',(1.19545283377814,7.17700242184241,36.29));
#307642=CARTESIAN_POINT('Ctrl Pts',(1.16034942104761,7.09344714231162,36.05));
#307643=CARTESIAN_POINT('Ctrl Pts',(1.16034942104761,7.09344714231162,36.29));
#307644=CARTESIAN_POINT('Ctrl Pts',(1.13732937915702,7.0018882271475,36.05));
#307645=CARTESIAN_POINT('Ctrl Pts',(1.13732937915702,7.0018882271475,36.29));
#307646=CARTESIAN_POINT('Ctrl Pts',(1.13508801477443,6.93766582705582,36.05));
#307647=CARTESIAN_POINT('Ctrl Pts',(1.13508801477443,6.93766582705582,36.29));
#307648=CARTESIAN_POINT('Ctrl Pts',(1.13392857142857,6.90444399350649,36.05));
#307649=CARTESIAN_POINT('Ctrl Pts',(1.13392857142857,6.90444399350649,36.29));
#307650=CARTESIAN_POINT('',(1.13392857142857,6.9044439935065,36.05));
#307651=CARTESIAN_POINT('Ctrl Pts',(1.13392857142857,6.9044439935065,36.05));
#307652=CARTESIAN_POINT('Ctrl Pts',(1.13508801477443,6.93766582705582,36.05));
#307653=CARTESIAN_POINT('Ctrl Pts',(1.13732937915702,7.0018882271475,36.05));
#307654=CARTESIAN_POINT('Ctrl Pts',(1.16034942104761,7.09344714231162,36.05));
#307655=CARTESIAN_POINT('Ctrl Pts',(1.19545283377814,7.17700242184241,36.05));
#307656=CARTESIAN_POINT('Ctrl Pts',(1.246166587943,7.24931351323173,36.05));
#307657=CARTESIAN_POINT('Ctrl Pts',(1.30553944113734,7.30974046602882,36.05));
#307658=CARTESIAN_POINT('Ctrl Pts',(1.37265904788325,7.354443366284,36.05));
#307659=CARTESIAN_POINT('Ctrl Pts',(1.4463007522726,7.38191424239284,36.05));
#307660=CARTESIAN_POINT('Ctrl Pts',(1.49771633107715,7.38486930154146,36.05));
#307661=CARTESIAN_POINT('Ctrl Pts',(1.52371651785715,7.38636363636364,36.05));
#307662=CARTESIAN_POINT('',(1.13392857142857,6.9044439935065,32.1799631621335));
#307663=CARTESIAN_POINT('Ctrl Pts',(1.13392857142857,6.9044439935065,36.05));
#307664=CARTESIAN_POINT('Ctrl Pts',(1.13392857142857,6.9044439935065,36.29));
#307665=CARTESIAN_POINT('Ctrl Pts',(1.13516721177027,6.8676136615146,36.05));
#307666=CARTESIAN_POINT('Ctrl Pts',(1.13516721177027,6.8676136615146,36.29));
#307667=CARTESIAN_POINT('Ctrl Pts',(1.13753725613477,6.79714161418862,36.05));
#307668=CARTESIAN_POINT('Ctrl Pts',(1.13753725613477,6.79714161418862,36.29));
#307669=CARTESIAN_POINT('Ctrl Pts',(1.15880795207294,6.69694686802566,36.05));
#307670=CARTESIAN_POINT('Ctrl Pts',(1.15880795207294,6.69694686802566,36.29));
#307671=CARTESIAN_POINT('Ctrl Pts',(1.19503681472287,6.60868448959127,36.05));
#307672=CARTESIAN_POINT('Ctrl Pts',(1.19503681472287,6.60868448959127,36.29));
#307673=CARTESIAN_POINT('Ctrl Pts',(1.24462810213434,6.53319043392833,36.05));
#307674=CARTESIAN_POINT('Ctrl Pts',(1.24462810213434,6.53319043392833,36.29));
#307675=CARTESIAN_POINT('Ctrl Pts',(1.30529590544445,6.47327605218271,36.05));
#307676=CARTESIAN_POINT('Ctrl Pts',(1.30529590544445,6.47327605218271,36.29));
#307677=CARTESIAN_POINT('Ctrl Pts',(1.37296075083694,6.42829274914181,36.05));
#307678=CARTESIAN_POINT('Ctrl Pts',(1.37296075083694,6.42829274914181,36.29));
#307679=CARTESIAN_POINT('Ctrl Pts',(1.44831874032179,6.4012532984509,36.05));
#307680=CARTESIAN_POINT('Ctrl Pts',(1.44831874032179,6.4012532984509,36.29));
#307681=CARTESIAN_POINT('Ctrl Pts',(1.50095499802161,6.39826496143831,36.05));
#307682=CARTESIAN_POINT('Ctrl Pts',(1.50095499802161,6.39826496143831,36.29));
#307683=CARTESIAN_POINT('Ctrl Pts',(1.52758218344156,6.39675324675325,36.05));
#307684=CARTESIAN_POINT('Ctrl Pts',(1.52758218344156,6.39675324675325,36.29));
#307685=CARTESIAN_POINT('Ctrl Pts',(1.52758218344156,6.39675324675325,36.05));
#307686=CARTESIAN_POINT('Ctrl Pts',(1.50095499802161,6.39826496143831,36.05));
#307687=CARTESIAN_POINT('Ctrl Pts',(1.44831874032179,6.4012532984509,36.05));
#307688=CARTESIAN_POINT('Ctrl Pts',(1.37296075083694,6.42829274914181,36.05));
#307689=CARTESIAN_POINT('Ctrl Pts',(1.30529590544445,6.47327605218271,36.05));
#307690=CARTESIAN_POINT('Ctrl Pts',(1.24462810213434,6.53319043392833,36.05));
#307691=CARTESIAN_POINT('Ctrl Pts',(1.19503681472287,6.60868448959127,36.05));
#307692=CARTESIAN_POINT('Ctrl Pts',(1.15880795207294,6.69694686802566,36.05));
#307693=CARTESIAN_POINT('Ctrl Pts',(1.13753725613477,6.79714161418862,36.05));
#307694=CARTESIAN_POINT('Ctrl Pts',(1.13516721177027,6.8676136615146,36.05));
#307695=CARTESIAN_POINT('Ctrl Pts',(1.13392857142857,6.9044439935065,36.05));
#307696=CARTESIAN_POINT('Origin',(0.,0.,36.05));
#307697=CARTESIAN_POINT('',(-2.24724025974026,6.89542410714286,36.05));
#307698=CARTESIAN_POINT('',(-1.86131797889611,6.24212662337662,36.05));
#307699=CARTESIAN_POINT('Ctrl Pts',(-2.24724025974026,6.89542410714286,
36.05));
#307700=CARTESIAN_POINT('Ctrl Pts',(-2.24635828463311,6.85667628421743,
36.05));
#307701=CARTESIAN_POINT('Ctrl Pts',(-2.24466128369114,6.78212192154818,
36.05));
#307702=CARTESIAN_POINT('Ctrl Pts',(-2.22526998846174,6.67544579213543,
36.05));
#307703=CARTESIAN_POINT('Ctrl Pts',(-2.19544755091121,6.57824013430206,
36.05));
#307704=CARTESIAN_POINT('Ctrl Pts',(-2.15255407155767,6.49069341485485,
36.05));
#307705=CARTESIAN_POINT('Ctrl Pts',(-2.09711468722833,6.41311300974787,
36.05));
#307706=CARTESIAN_POINT('Ctrl Pts',(-2.02981249733957,6.34542328474194,
36.05));
#307707=CARTESIAN_POINT('Ctrl Pts',(-1.95088478291998,6.28713666449684,
36.05));
#307708=CARTESIAN_POINT('Ctrl Pts',(-1.89166914263337,6.25737900558171,
36.05));
#307709=CARTESIAN_POINT('Ctrl Pts',(-1.86131797889611,6.24212662337662,
36.05));
#307710=CARTESIAN_POINT('',(-2.37094155844156,5.43291396103896,36.05));
#307711=CARTESIAN_POINT('Ctrl Pts',(-1.86131797889611,6.24212662337662,
36.05));
#307712=CARTESIAN_POINT('Ctrl Pts',(-1.88076808190029,6.23557324032603,
36.05));
#307713=CARTESIAN_POINT('Ctrl Pts',(-1.91917711253447,6.22263196745495,
36.05));
#307714=CARTESIAN_POINT('Ctrl Pts',(-1.97432962905344,6.19776979492405,
36.05));
#307715=CARTESIAN_POINT('Ctrl Pts',(-2.02656583006182,6.16910978501208,
36.05));
#307716=CARTESIAN_POINT('Ctrl Pts',(-2.07499444571376,6.1351992195304,36.05));
#307717=CARTESIAN_POINT('Ctrl Pts',(-2.1202782797022,6.09774166415627,36.05));
#307718=CARTESIAN_POINT('Ctrl Pts',(-2.16248925313098,6.05629105732706,
36.05));
#307719=CARTESIAN_POINT('Ctrl Pts',(-2.20124132093025,6.01030469320115,
36.05));
#307720=CARTESIAN_POINT('Ctrl Pts',(-2.23643083441821,5.96019951630268,
36.05));
#307721=CARTESIAN_POINT('Ctrl Pts',(-2.26824051996169,5.90641132135784,
36.05));
#307722=CARTESIAN_POINT('Ctrl Pts',(-2.29590420953425,5.84911895337204,
36.05));
#307723=CARTESIAN_POINT('Ctrl Pts',(-2.31914738800462,5.78833295550162,
36.05));
#307724=CARTESIAN_POINT('Ctrl Pts',(-2.33776644819188,5.72405509656198,
36.05));
#307725=CARTESIAN_POINT('Ctrl Pts',(-2.35252585809151,5.65624108672131,
36.05));
#307726=CARTESIAN_POINT('Ctrl Pts',(-2.36345937406549,5.58482539360676,
36.05));
#307727=CARTESIAN_POINT('Ctrl Pts',(-2.37001876348768,5.50992190470655,
36.05));
#307728=CARTESIAN_POINT('Ctrl Pts',(-2.37063000734488,5.45891313799848,
36.05));
#307729=CARTESIAN_POINT('Ctrl Pts',(-2.37094155844156,5.43291396103896,
36.05));
#307730=CARTESIAN_POINT('',(-1.52371651785714,4.45876623376623,36.05));
#307731=CARTESIAN_POINT('Ctrl Pts',(-2.37094155844156,5.43291396103896,
36.05));
#307732=CARTESIAN_POINT('Ctrl Pts',(-2.37024051692734,5.39744356397404,
36.05));
#307733=CARTESIAN_POINT('Ctrl Pts',(-2.36886427906175,5.32781045016027,
36.05));
#307734=CARTESIAN_POINT('Ctrl Pts',(-2.35686977721559,5.22616336292247,
36.05));
#307735=CARTESIAN_POINT('Ctrl Pts',(-2.33853623055972,5.12949961741785,
36.05));
#307736=CARTESIAN_POINT('Ctrl Pts',(-2.31200320040195,5.03825698338498,
36.05));
#307737=CARTESIAN_POINT('Ctrl Pts',(-2.27806144254569,4.95218254596678,
36.05));
#307738=CARTESIAN_POINT('Ctrl Pts',(-2.2354792856985,4.87186228483585,36.05));
#307739=CARTESIAN_POINT('Ctrl Pts',(-2.18686174567011,4.79599402074389,
36.05));
#307740=CARTESIAN_POINT('Ctrl Pts',(-2.1298438000822,4.72680658155488,36.05));
#307741=CARTESIAN_POINT('Ctrl Pts',(-2.06813219984915,4.66375358613811,
36.05));
#307742=CARTESIAN_POINT('Ctrl Pts',(-2.00109150543013,4.60959489382438,
36.05));
#307743=CARTESIAN_POINT('Ctrl Pts',(-1.93122097549665,4.56241550483758,
36.05));
#307744=CARTESIAN_POINT('Ctrl Pts',(-1.85703181398638,4.52434515927101,
36.05));
#307745=CARTESIAN_POINT('Ctrl Pts',(-1.77882069442911,4.49538915943629,
36.05));
#307746=CARTESIAN_POINT('Ctrl Pts',(-1.69736543838644,4.47372823681752,
36.05));
#307747=CARTESIAN_POINT('Ctrl Pts',(-1.61170021909538,4.46161006986558,
36.05));
#307748=CARTESIAN_POINT('Ctrl Pts',(-1.55338922539081,4.4597253240939,36.05));
#307749=CARTESIAN_POINT('Ctrl Pts',(-1.52371651785714,4.45876623376623,
36.05));
#307750=CARTESIAN_POINT('',(-0.680357142857142,5.42196124188312,36.05));
#307751=CARTESIAN_POINT('Ctrl Pts',(-1.52371651785714,4.45876623376623,
36.05));
#307752=CARTESIAN_POINT('Ctrl Pts',(-1.49447449269809,4.45973608112409,
36.05));
#307753=CARTESIAN_POINT('Ctrl Pts',(-1.43680842361535,4.46164864649648,
36.05));
#307754=CARTESIAN_POINT('Ctrl Pts',(-1.35198241500324,4.47370190759594,
36.05));
#307755=CARTESIAN_POINT('Ctrl Pts',(-1.27102264425494,4.49553589484458,
36.05));
#307756=CARTESIAN_POINT('Ctrl Pts',(-1.19309519794087,4.5241565808727,36.05));
#307757=CARTESIAN_POINT('Ctrl Pts',(-1.11934856150417,4.56264762609262,
36.05));
#307758=CARTESIAN_POINT('Ctrl Pts',(-1.04958738921064,4.60935645208091,
36.05));
#307759=CARTESIAN_POINT('Ctrl Pts',(-0.983169721460654,4.66400945675856,
36.05));
#307760=CARTESIAN_POINT('Ctrl Pts',(-0.921346136582458,4.72672058470318,
36.05));
#307761=CARTESIAN_POINT('Ctrl Pts',(-0.864790653609182,4.79615096254107,
36.05));
#307762=CARTESIAN_POINT('Ctrl Pts',(-0.814894945031659,4.87078209602146,
36.05));
#307763=CARTESIAN_POINT('Ctrl Pts',(-0.773615124031434,4.95095791492866,
36.05));
#307764=CARTESIAN_POINT('Ctrl Pts',(-0.739130657263025,5.03559649057185,
36.05));
#307765=CARTESIAN_POINT('Ctrl Pts',(-0.713135864328774,5.12552781537341,
36.05));
#307766=CARTESIAN_POINT('Ctrl Pts',(-0.693373801633478,5.21999888881734,
36.05));
#307767=CARTESIAN_POINT('Ctrl Pts',(-0.682716393984036,5.31949010994648,
36.05));
#307768=CARTESIAN_POINT('Ctrl Pts',(-0.681153739192598,5.3873620729942,
36.05));
#307769=CARTESIAN_POINT('Ctrl Pts',(-0.680357142857142,5.42196124188312,
36.05));
#307770=CARTESIAN_POINT('',(-1.18611505681818,6.24212662337662,36.05));
#307771=CARTESIAN_POINT('Ctrl Pts',(-0.680357142857142,5.42196124188312,
36.05));
#307772=CARTESIAN_POINT('Ctrl Pts',(-0.680643402753075,5.44731949788714,
36.05));
#307773=CARTESIAN_POINT('Ctrl Pts',(-0.681202359695404,5.4968345485113,
36.05));
#307774=CARTESIAN_POINT('Ctrl Pts',(-0.688060973290405,5.56952358146944,
36.05));
#307775=CARTESIAN_POINT('Ctrl Pts',(-0.698134608146914,5.63904690448481,
36.05));
#307776=CARTESIAN_POINT('Ctrl Pts',(-0.712369756219759,5.70553707456913,
36.05));
#307777=CARTESIAN_POINT('Ctrl Pts',(-0.730130420178432,5.76902496530641,
36.05));
#307778=CARTESIAN_POINT('Ctrl Pts',(-0.753130561450395,5.82909896870107,
36.05));
#307779=CARTESIAN_POINT('Ctrl Pts',(-0.778997347786388,5.88660676946342,
36.05));
#307780=CARTESIAN_POINT('Ctrl Pts',(-0.810449385509135,5.94000771696759,
36.05));
#307781=CARTESIAN_POINT('Ctrl Pts',(-0.844529687053187,5.99064810748104,
36.05));
#307782=CARTESIAN_POINT('Ctrl Pts',(-0.882532948756259,6.03778353402304,
36.05));
#307783=CARTESIAN_POINT('Ctrl Pts',(-0.924520209270103,6.08096773911451,
36.05));
#307784=CARTESIAN_POINT('Ctrl Pts',(-0.969980971511446,6.12033427680283,
36.05));
#307785=CARTESIAN_POINT('Ctrl Pts',(-1.01831785359978,6.15682435284569,
36.05));
#307786=CARTESIAN_POINT('Ctrl Pts',(-1.07097627880842,6.18887731351974,
36.05));
#307787=CARTESIAN_POINT('Ctrl Pts',(-1.12679451037092,6.21812962575334,
36.05));
#307788=CARTESIAN_POINT('Ctrl Pts',(-1.16621033677113,6.23407454786033,
36.05));
#307789=CARTESIAN_POINT('Ctrl Pts',(-1.18611505681818,6.24212662337662,
36.05));
#307790=CARTESIAN_POINT('',(-0.804058441558441,6.88253855519481,36.05));
#307791=CARTESIAN_POINT('Ctrl Pts',(-1.18611505681818,6.24212662337662,
36.05));
#307792=CARTESIAN_POINT('Ctrl Pts',(-1.15549574155667,6.25752314612396,
36.05));
#307793=CARTESIAN_POINT('Ctrl Pts',(-1.09604440098142,6.28741747621295,
36.05));
#307794=CARTESIAN_POINT('Ctrl Pts',(-1.0177935092216,6.34678274879809,36.05));
#307795=CARTESIAN_POINT('Ctrl Pts',(-0.951235352872532,6.41405772296989,
36.05));
#307796=CARTESIAN_POINT('Ctrl Pts',(-0.897038222357849,6.4907436496301,
36.05));
#307797=CARTESIAN_POINT('Ctrl Pts',(-0.854639610807379,6.57608978278239,
36.05));
#307798=CARTESIAN_POINT('Ctrl Pts',(-0.825519260309656,6.6705401244345,
36.05));
#307799=CARTESIAN_POINT('Ctrl Pts',(-0.806813602327297,6.77356208818653,
36.05));
#307800=CARTESIAN_POINT('Ctrl Pts',(-0.804999967272473,6.8452978442089,
36.05));
#307801=CARTESIAN_POINT('Ctrl Pts',(-0.804058441558441,6.88253855519481,
36.05));
#307802=CARTESIAN_POINT('',(-1.52887073863637,7.71623376623377,36.05));
#307803=CARTESIAN_POINT('Ctrl Pts',(-0.804058441558441,6.88253855519481,
36.05));
#307804=CARTESIAN_POINT('Ctrl Pts',(-0.804650124600102,6.91241766550898,
36.05));
#307805=CARTESIAN_POINT('Ctrl Pts',(-0.805811171394462,6.97104879536392,
36.05));
#307806=CARTESIAN_POINT('Ctrl Pts',(-0.815733176885725,7.05701575208482,
36.05));
#307807=CARTESIAN_POINT('Ctrl Pts',(-0.831597303625935,7.13897358699381,
36.05));
#307808=CARTESIAN_POINT('Ctrl Pts',(-0.854229034877609,7.21661236790923,
36.05));
#307809=CARTESIAN_POINT('Ctrl Pts',(-0.883047786444258,7.29002627559583,
36.05));
#307810=CARTESIAN_POINT('Ctrl Pts',(-0.919708538459593,7.35843862911193,
36.05));
#307811=CARTESIAN_POINT('Ctrl Pts',(-0.961621998889034,7.42336185115535,
36.05));
#307812=CARTESIAN_POINT('Ctrl Pts',(-1.00970620194357,7.48362087256877,
36.05));
#307813=CARTESIAN_POINT('Ctrl Pts',(-1.06268331120451,7.53791001729144,
36.05));
#307814=CARTESIAN_POINT('Ctrl Pts',(-1.119447579553,7.58560597597768,36.05));
#307815=CARTESIAN_POINT('Ctrl Pts',(-1.17924186808025,7.62639783586101,
36.05));
#307816=CARTESIAN_POINT('Ctrl Pts',(-1.24280687342643,7.65953041457979,
36.05));
#307817=CARTESIAN_POINT('Ctrl Pts',(-1.30973339831807,7.68468886160549,
36.05));
#307818=CARTESIAN_POINT('Ctrl Pts',(-1.37991458997475,7.7027904588233,36.05));
#307819=CARTESIAN_POINT('Ctrl Pts',(-1.45335117903047,7.71392449956901,
36.05));
#307820=CARTESIAN_POINT('Ctrl Pts',(-1.50349048519761,7.71545767890599,
36.05));
#307821=CARTESIAN_POINT('Ctrl Pts',(-1.52887073863637,7.71623376623377,
36.05));
#307822=CARTESIAN_POINT('Ctrl Pts',(-1.52887073863637,7.71623376623377,
36.05));
#307823=CARTESIAN_POINT('Ctrl Pts',(-1.55402639381368,7.71538504428939,
36.05));
#307824=CARTESIAN_POINT('Ctrl Pts',(-1.60368781725867,7.71370952681349,
36.05));
#307825=CARTESIAN_POINT('Ctrl Pts',(-1.67660001580121,7.7036309678914,36.05));
#307826=CARTESIAN_POINT('Ctrl Pts',(-1.746104953362,7.68533220871074,36.05));
#307827=CARTESIAN_POINT('Ctrl Pts',(-1.81235851864406,7.65993643724945,
36.05));
#307828=CARTESIAN_POINT('Ctrl Pts',(-1.87562432631225,7.62785439831755,
36.05));
#307829=CARTESIAN_POINT('Ctrl Pts',(-1.93532052837525,7.58805917500155,
36.05));
#307830=CARTESIAN_POINT('Ctrl Pts',(-1.99157504243468,7.54133429965825,
36.05));
#307831=CARTESIAN_POINT('Ctrl Pts',(-2.04420697733625,7.48817807892744,
36.05));
#307832=CARTESIAN_POINT('Ctrl Pts',(-2.09163145310384,7.42884662646377,
36.05));
#307833=CARTESIAN_POINT('Ctrl Pts',(-2.13381867185592,7.36527391878087,
36.05));
#307834=CARTESIAN_POINT('Ctrl Pts',(-2.1683837201686,7.29688183752562,36.05));
#307835=CARTESIAN_POINT('Ctrl Pts',(-2.19802765306379,7.22519194306317,
36.05));
#307836=CARTESIAN_POINT('Ctrl Pts',(-2.2194554245458,7.1485092997012,36.05));
#307837=CARTESIAN_POINT('Ctrl Pts',(-2.23564047821614,7.06800054423278,
36.05));
#307838=CARTESIAN_POINT('Ctrl Pts',(-2.24549498801578,6.98307391394772,
36.05));
#307839=CARTESIAN_POINT('Ctrl Pts',(-2.24664961358837,6.92508712200564,
36.05));
#307840=CARTESIAN_POINT('Ctrl Pts',(-2.24724025974026,6.89542410714286,
36.05));
#307841=CARTESIAN_POINT('Origin',(0.,0.,36.05));
#307842=CARTESIAN_POINT('',(0.804058441558442,6.89542410714286,36.05));
#307843=CARTESIAN_POINT('',(1.1899807224026,6.24212662337662,36.05));
#307844=CARTESIAN_POINT('Ctrl Pts',(0.804058441558442,6.89542410714286,
36.05));
#307845=CARTESIAN_POINT('Ctrl Pts',(0.804940416665592,6.85667628421743,
36.05));
#307846=CARTESIAN_POINT('Ctrl Pts',(0.806637417607563,6.78212192154818,
36.05));
#307847=CARTESIAN_POINT('Ctrl Pts',(0.82602871283696,6.67544579213543,36.05));
#307848=CARTESIAN_POINT('Ctrl Pts',(0.855851150387493,6.57824013430206,
36.05));
#307849=CARTESIAN_POINT('Ctrl Pts',(0.898744629741027,6.49069341485485,
36.05));
#307850=CARTESIAN_POINT('Ctrl Pts',(0.954184014070375,6.41311300974787,
36.05));
#307851=CARTESIAN_POINT('Ctrl Pts',(1.02148620395913,6.34542328474194,36.05));
#307852=CARTESIAN_POINT('Ctrl Pts',(1.10041391837872,6.28713666449684,36.05));
#307853=CARTESIAN_POINT('Ctrl Pts',(1.15962955866533,6.25737900558172,36.05));
#307854=CARTESIAN_POINT('Ctrl Pts',(1.1899807224026,6.24212662337662,36.05));
#307855=CARTESIAN_POINT('',(0.680357142857143,5.43291396103896,36.05));
#307856=CARTESIAN_POINT('Ctrl Pts',(1.1899807224026,6.24212662337662,36.05));
#307857=CARTESIAN_POINT('Ctrl Pts',(1.17053061939841,6.23557324032603,36.05));
#307858=CARTESIAN_POINT('Ctrl Pts',(1.13212158876422,6.22263196745495,36.05));
#307859=CARTESIAN_POINT('Ctrl Pts',(1.07696907224526,6.19776979492405,36.05));
#307860=CARTESIAN_POINT('Ctrl Pts',(1.02473287123688,6.16910978501208,36.05));
#307861=CARTESIAN_POINT('Ctrl Pts',(0.976304255584941,6.1351992195304,36.05));
#307862=CARTESIAN_POINT('Ctrl Pts',(0.931020421596495,6.09774166415628,
36.05));
#307863=CARTESIAN_POINT('Ctrl Pts',(0.888809448167726,6.05629105732706,
36.05));
#307864=CARTESIAN_POINT('Ctrl Pts',(0.850057380368458,6.01030469320115,
36.05));
#307865=CARTESIAN_POINT('Ctrl Pts',(0.814867866880491,5.96019951630268,
36.05));
#307866=CARTESIAN_POINT('Ctrl Pts',(0.783058181337012,5.90641132135784,
36.05));
#307867=CARTESIAN_POINT('Ctrl Pts',(0.755394491764458,5.84911895337204,
36.05));
#307868=CARTESIAN_POINT('Ctrl Pts',(0.732151313294084,5.78833295550162,
36.05));
#307869=CARTESIAN_POINT('Ctrl Pts',(0.713532253106825,5.72405509656199,
36.05));
#307870=CARTESIAN_POINT('Ctrl Pts',(0.698772843207189,5.65624108672131,
36.05));
#307871=CARTESIAN_POINT('Ctrl Pts',(0.687839327233214,5.58482539360676,
36.05));
#307872=CARTESIAN_POINT('Ctrl Pts',(0.681279937811019,5.50992190470655,
36.05));
#307873=CARTESIAN_POINT('Ctrl Pts',(0.680668693953829,5.45891313799848,
36.05));
#307874=CARTESIAN_POINT('Ctrl Pts',(0.680357142857143,5.43291396103896,
36.05));
#307875=CARTESIAN_POINT('',(1.52758218344156,4.45876623376623,36.05));
#307876=CARTESIAN_POINT('Ctrl Pts',(0.680357142857143,5.43291396103896,
36.05));
#307877=CARTESIAN_POINT('Ctrl Pts',(0.681058184371366,5.39744356397404,
36.05));
#307878=CARTESIAN_POINT('Ctrl Pts',(0.682434422236949,5.32781045016027,
36.05));
#307879=CARTESIAN_POINT('Ctrl Pts',(0.694428924083107,5.22616336292247,
36.05));
#307880=CARTESIAN_POINT('Ctrl Pts',(0.712762470738981,5.12949961741785,
36.05));
#307881=CARTESIAN_POINT('Ctrl Pts',(0.739295500896744,5.03825698338498,
36.05));
#307882=CARTESIAN_POINT('Ctrl Pts',(0.773237258753005,4.95218254596678,
36.05));
#307883=CARTESIAN_POINT('Ctrl Pts',(0.815819415600203,4.87186228483585,
36.05));
#307884=CARTESIAN_POINT('Ctrl Pts',(0.864436955628593,4.79599402074389,
36.05));
#307885=CARTESIAN_POINT('Ctrl Pts',(0.921454901216499,4.72680658155488,
36.05));
#307886=CARTESIAN_POINT('Ctrl Pts',(0.983166501449546,4.66375358613811,
36.05));
#307887=CARTESIAN_POINT('Ctrl Pts',(1.05020719586857,4.60959489382439,36.05));
#307888=CARTESIAN_POINT('Ctrl Pts',(1.12007772580205,4.56241550483758,36.05));
#307889=CARTESIAN_POINT('Ctrl Pts',(1.19426688731232,4.52434515927101,36.05));
#307890=CARTESIAN_POINT('Ctrl Pts',(1.27247800686959,4.49538915943629,36.05));
#307891=CARTESIAN_POINT('Ctrl Pts',(1.35393326291226,4.47372823681752,36.05));
#307892=CARTESIAN_POINT('Ctrl Pts',(1.43959848220332,4.46161006986558,36.05));
#307893=CARTESIAN_POINT('Ctrl Pts',(1.49790947590789,4.4597253240939,36.05));
#307894=CARTESIAN_POINT('Ctrl Pts',(1.52758218344156,4.45876623376623,36.05));
#307895=CARTESIAN_POINT('',(2.37094155844156,5.42196124188312,36.05));
#307896=CARTESIAN_POINT('Ctrl Pts',(1.52758218344156,4.45876623376623,36.05));
#307897=CARTESIAN_POINT('Ctrl Pts',(1.55682420860062,4.45973608112409,36.05));
#307898=CARTESIAN_POINT('Ctrl Pts',(1.61449027768335,4.46164864649648,36.05));
#307899=CARTESIAN_POINT('Ctrl Pts',(1.69931628629545,4.47370190759594,36.05));
#307900=CARTESIAN_POINT('Ctrl Pts',(1.78027605704376,4.49553589484458,36.05));
#307901=CARTESIAN_POINT('Ctrl Pts',(1.85820350335783,4.5241565808727,36.05));
#307902=CARTESIAN_POINT('Ctrl Pts',(1.93195013979453,4.56264762609262,36.05));
#307903=CARTESIAN_POINT('Ctrl Pts',(2.00171131208806,4.60935645208091,36.05));
#307904=CARTESIAN_POINT('Ctrl Pts',(2.06812897983805,4.66400945675856,36.05));
#307905=CARTESIAN_POINT('Ctrl Pts',(2.12995256471625,4.72672058470318,36.05));
#307906=CARTESIAN_POINT('Ctrl Pts',(2.18650804768952,4.79615096254107,36.05));
#307907=CARTESIAN_POINT('Ctrl Pts',(2.23640375626704,4.87078209602146,36.05));
#307908=CARTESIAN_POINT('Ctrl Pts',(2.27768357726726,4.95095791492866,36.05));
#307909=CARTESIAN_POINT('Ctrl Pts',(2.31216804403568,5.03559649057185,36.05));
#307910=CARTESIAN_POINT('Ctrl Pts',(2.33816283696992,5.12552781537341,36.05));
#307911=CARTESIAN_POINT('Ctrl Pts',(2.35792489966522,5.21999888881734,36.05));
#307912=CARTESIAN_POINT('Ctrl Pts',(2.36858230731467,5.31949010994648,36.05));
#307913=CARTESIAN_POINT('Ctrl Pts',(2.3701449621061,5.3873620729942,36.05));
#307914=CARTESIAN_POINT('Ctrl Pts',(2.37094155844156,5.42196124188312,36.05));
#307915=CARTESIAN_POINT('',(1.86518364448052,6.24212662337662,36.05));
#307916=CARTESIAN_POINT('Ctrl Pts',(2.37094155844156,5.42196124188312,36.05));
#307917=CARTESIAN_POINT('Ctrl Pts',(2.37065529854562,5.44731949788714,36.05));
#307918=CARTESIAN_POINT('Ctrl Pts',(2.3700963416033,5.4968345485113,36.05));
#307919=CARTESIAN_POINT('Ctrl Pts',(2.3632377280083,5.56952358146944,36.05));
#307920=CARTESIAN_POINT('Ctrl Pts',(2.35316409315178,5.63904690448481,36.05));
#307921=CARTESIAN_POINT('Ctrl Pts',(2.33892894507894,5.70553707456913,36.05));
#307922=CARTESIAN_POINT('Ctrl Pts',(2.32116828112027,5.76902496530642,36.05));
#307923=CARTESIAN_POINT('Ctrl Pts',(2.2981681398483,5.82909896870107,36.05));
#307924=CARTESIAN_POINT('Ctrl Pts',(2.27230135351232,5.88660676946342,36.05));
#307925=CARTESIAN_POINT('Ctrl Pts',(2.24084931578957,5.94000771696759,36.05));
#307926=CARTESIAN_POINT('Ctrl Pts',(2.20676901424551,5.99064810748104,36.05));
#307927=CARTESIAN_POINT('Ctrl Pts',(2.16876575254244,6.03778353402304,36.05));
#307928=CARTESIAN_POINT('Ctrl Pts',(2.1267784920286,6.08096773911451,36.05));
#307929=CARTESIAN_POINT('Ctrl Pts',(2.08131772978725,6.12033427680283,36.05));
#307930=CARTESIAN_POINT('Ctrl Pts',(2.03298084769892,6.1568243528457,36.05));
#307931=CARTESIAN_POINT('Ctrl Pts',(1.98032242249028,6.18887731351974,36.05));
#307932=CARTESIAN_POINT('Ctrl Pts',(1.92450419092778,6.21812962575333,36.05));
#307933=CARTESIAN_POINT('Ctrl Pts',(1.88508836452757,6.23407454786033,36.05));
#307934=CARTESIAN_POINT('Ctrl Pts',(1.86518364448052,6.24212662337662,36.05));
#307935=CARTESIAN_POINT('',(2.24724025974026,6.88253855519481,36.05));
#307936=CARTESIAN_POINT('Ctrl Pts',(1.86518364448052,6.24212662337662,36.05));
#307937=CARTESIAN_POINT('Ctrl Pts',(1.89580295974203,6.25752314612396,36.05));
#307938=CARTESIAN_POINT('Ctrl Pts',(1.95525430031729,6.28741747621295,36.05));
#307939=CARTESIAN_POINT('Ctrl Pts',(2.0335051920771,6.34678274879809,36.05));
#307940=CARTESIAN_POINT('Ctrl Pts',(2.10006334842617,6.41405772296989,36.05));
#307941=CARTESIAN_POINT('Ctrl Pts',(2.15426047894085,6.4907436496301,36.05));
#307942=CARTESIAN_POINT('Ctrl Pts',(2.19665909049132,6.57608978278239,36.05));
#307943=CARTESIAN_POINT('Ctrl Pts',(2.22577944098905,6.6705401244345,36.05));
#307944=CARTESIAN_POINT('Ctrl Pts',(2.24448509897141,6.77356208818653,36.05));
#307945=CARTESIAN_POINT('Ctrl Pts',(2.24629873402623,6.8452978442089,36.05));
#307946=CARTESIAN_POINT('Ctrl Pts',(2.24724025974026,6.88253855519481,36.05));
#307947=CARTESIAN_POINT('',(1.52242796266234,7.71623376623377,36.05));
#307948=CARTESIAN_POINT('Ctrl Pts',(2.24724025974026,6.88253855519481,36.05));
#307949=CARTESIAN_POINT('Ctrl Pts',(2.2466485766986,6.91241766550898,36.05));
#307950=CARTESIAN_POINT('Ctrl Pts',(2.24548752990423,6.97104879536392,36.05));
#307951=CARTESIAN_POINT('Ctrl Pts',(2.23556552441298,7.05701575208482,36.05));
#307952=CARTESIAN_POINT('Ctrl Pts',(2.21970139767277,7.13897358699381,36.05));
#307953=CARTESIAN_POINT('Ctrl Pts',(2.19706966642109,7.21661236790923,36.05));
#307954=CARTESIAN_POINT('Ctrl Pts',(2.16825091485445,7.29002627559583,36.05));
#307955=CARTESIAN_POINT('Ctrl Pts',(2.1315901628391,7.35843862911193,36.05));
#307956=CARTESIAN_POINT('Ctrl Pts',(2.08967670240967,7.42336185115535,36.05));
#307957=CARTESIAN_POINT('Ctrl Pts',(2.04159249935513,7.48362087256877,36.05));
#307958=CARTESIAN_POINT('Ctrl Pts',(1.98861539009419,7.53791001729144,36.05));
#307959=CARTESIAN_POINT('Ctrl Pts',(1.9318511217457,7.58560597597768,36.05));
#307960=CARTESIAN_POINT('Ctrl Pts',(1.87205683321845,7.62639783586101,36.05));
#307961=CARTESIAN_POINT('Ctrl Pts',(1.80849182787228,7.65953041457979,36.05));
#307962=CARTESIAN_POINT('Ctrl Pts',(1.74156530298064,7.68468886160549,36.05));
#307963=CARTESIAN_POINT('Ctrl Pts',(1.67138411132394,7.7027904588233,36.05));
#307964=CARTESIAN_POINT('Ctrl Pts',(1.59794752226823,7.71392449956901,36.05));
#307965=CARTESIAN_POINT('Ctrl Pts',(1.54780821610109,7.71545767890599,36.05));
#307966=CARTESIAN_POINT('Ctrl Pts',(1.52242796266234,7.71623376623377,36.05));
#307967=CARTESIAN_POINT('Ctrl Pts',(1.52242796266234,7.71623376623377,36.05));
#307968=CARTESIAN_POINT('Ctrl Pts',(1.49727230748502,7.71538504428939,36.05));
#307969=CARTESIAN_POINT('Ctrl Pts',(1.44761088404003,7.71370952681349,36.05));
#307970=CARTESIAN_POINT('Ctrl Pts',(1.37469868549749,7.7036309678914,36.05));
#307971=CARTESIAN_POINT('Ctrl Pts',(1.3051937479367,7.68533220871074,36.05));
#307972=CARTESIAN_POINT('Ctrl Pts',(1.23894018265463,7.65993643724945,36.05));
#307973=CARTESIAN_POINT('Ctrl Pts',(1.17567437498645,7.62785439831755,36.05));
#307974=CARTESIAN_POINT('Ctrl Pts',(1.11597817292345,7.58805917500155,36.05));
#307975=CARTESIAN_POINT('Ctrl Pts',(1.05972365886402,7.54133429965824,36.05));
#307976=CARTESIAN_POINT('Ctrl Pts',(1.00709172396245,7.48817807892744,36.05));
#307977=CARTESIAN_POINT('Ctrl Pts',(0.959667248194858,7.42884662646377,
36.05));
#307978=CARTESIAN_POINT('Ctrl Pts',(0.917480029442785,7.36527391878087,
36.05));
#307979=CARTESIAN_POINT('Ctrl Pts',(0.882914981130102,7.29688183752562,
36.05));
#307980=CARTESIAN_POINT('Ctrl Pts',(0.853271048234912,7.22519194306317,
36.05));
#307981=CARTESIAN_POINT('Ctrl Pts',(0.831843276752908,7.1485092997012,36.05));
#307982=CARTESIAN_POINT('Ctrl Pts',(0.815658223082562,7.06800054423278,
36.05));
#307983=CARTESIAN_POINT('Ctrl Pts',(0.805803713282925,6.98307391394772,
36.05));
#307984=CARTESIAN_POINT('Ctrl Pts',(0.804649087710329,6.92508712200564,
36.05));
#307985=CARTESIAN_POINT('Ctrl Pts',(0.804058441558442,6.89542410714286,
36.05));
#307986=CARTESIAN_POINT('Origin',(0.,0.,36.05));
#307987=CARTESIAN_POINT('',(-0.185551948051949,4.95357142857143,36.05));
#307988=CARTESIAN_POINT('',(-0.185551948051949,4.5,36.05));
#307989=CARTESIAN_POINT('',(-0.185551948051949,4.5,36.05));
#307990=CARTESIAN_POINT('',(0.144318181818181,4.5,36.05));
#307991=CARTESIAN_POINT('',(0.144318181818181,4.5,36.05));
#307992=CARTESIAN_POINT('',(0.144318181818181,4.95357142857143,36.05));
#307993=CARTESIAN_POINT('',(0.144318181818181,4.95357142857143,36.05));
#307994=CARTESIAN_POINT('',(-0.185551948051949,4.95357142857143,36.05));
#307995=CARTESIAN_POINT('Ctrl Pts',(-1.18611505681818,6.24212662337662,
36.05));
#307996=CARTESIAN_POINT('Ctrl Pts',(-1.18611505681818,6.24212662337662,
36.29));
#307997=CARTESIAN_POINT('Ctrl Pts',(-1.16621033677113,6.23407454786033,
36.05));
#307998=CARTESIAN_POINT('Ctrl Pts',(-1.16621033677113,6.23407454786033,
36.29));
#307999=CARTESIAN_POINT('Ctrl Pts',(-1.12679451037092,6.21812962575334,
36.05));
#308000=CARTESIAN_POINT('Ctrl Pts',(-1.12679451037092,6.21812962575334,
36.29));
#308001=CARTESIAN_POINT('Ctrl Pts',(-1.07097627880842,6.18887731351974,
36.05));
#308002=CARTESIAN_POINT('Ctrl Pts',(-1.07097627880842,6.18887731351974,
36.29));
#308003=CARTESIAN_POINT('Ctrl Pts',(-1.01831785359978,6.15682435284569,
36.05));
#308004=CARTESIAN_POINT('Ctrl Pts',(-1.01831785359978,6.15682435284569,
36.29));
#308005=CARTESIAN_POINT('Ctrl Pts',(-0.969980971511446,6.12033427680283,
36.05));
#308006=CARTESIAN_POINT('Ctrl Pts',(-0.969980971511446,6.12033427680283,
36.29));
#308007=CARTESIAN_POINT('Ctrl Pts',(-0.924520209270103,6.08096773911451,
36.05));
#308008=CARTESIAN_POINT('Ctrl Pts',(-0.924520209270103,6.08096773911451,
36.29));
#308009=CARTESIAN_POINT('Ctrl Pts',(-0.882532948756259,6.03778353402304,
36.05));
#308010=CARTESIAN_POINT('Ctrl Pts',(-0.882532948756259,6.03778353402304,
36.29));
#308011=CARTESIAN_POINT('Ctrl Pts',(-0.844529687053187,5.99064810748104,
36.05));
#308012=CARTESIAN_POINT('Ctrl Pts',(-0.844529687053187,5.99064810748104,
36.29));
#308013=CARTESIAN_POINT('Ctrl Pts',(-0.810449385509135,5.94000771696759,
36.05));
#308014=CARTESIAN_POINT('Ctrl Pts',(-0.810449385509135,5.94000771696759,
36.29));
#308015=CARTESIAN_POINT('Ctrl Pts',(-0.778997347786388,5.88660676946342,
36.05));
#308016=CARTESIAN_POINT('Ctrl Pts',(-0.778997347786388,5.88660676946342,
36.29));
#308017=CARTESIAN_POINT('Ctrl Pts',(-0.753130561450395,5.82909896870107,
36.05));
#308018=CARTESIAN_POINT('Ctrl Pts',(-0.753130561450395,5.82909896870107,
36.29));
#308019=CARTESIAN_POINT('Ctrl Pts',(-0.730130420178432,5.76902496530641,
36.05));
#308020=CARTESIAN_POINT('Ctrl Pts',(-0.730130420178432,5.76902496530641,
36.29));
#308021=CARTESIAN_POINT('Ctrl Pts',(-0.712369756219759,5.70553707456913,
36.05));
#308022=CARTESIAN_POINT('Ctrl Pts',(-0.712369756219759,5.70553707456913,
36.29));
#308023=CARTESIAN_POINT('Ctrl Pts',(-0.698134608146914,5.63904690448481,
36.05));
#308024=CARTESIAN_POINT('Ctrl Pts',(-0.698134608146914,5.63904690448481,
36.29));
#308025=CARTESIAN_POINT('Ctrl Pts',(-0.688060973290405,5.56952358146944,
36.05));
#308026=CARTESIAN_POINT('Ctrl Pts',(-0.688060973290405,5.56952358146944,
36.29));
#308027=CARTESIAN_POINT('Ctrl Pts',(-0.681202359695404,5.4968345485113,
36.05));
#308028=CARTESIAN_POINT('Ctrl Pts',(-0.681202359695404,5.4968345485113,
36.29));
#308029=CARTESIAN_POINT('Ctrl Pts',(-0.680643402753075,5.44731949788714,
36.05));
#308030=CARTESIAN_POINT('Ctrl Pts',(-0.680643402753075,5.44731949788714,
36.29));
#308031=CARTESIAN_POINT('Ctrl Pts',(-0.680357142857142,5.42196124188312,
36.05));
#308032=CARTESIAN_POINT('Ctrl Pts',(-0.680357142857142,5.42196124188312,
36.29));
#308033=CARTESIAN_POINT('',(-1.18611505681818,6.24212662337662,36.25));
#308034=CARTESIAN_POINT('',(-1.18611505681818,6.24212662337662,32.1799631621335));
#308035=CARTESIAN_POINT('',(-0.680357142857142,5.42196124188312,36.25));
#308036=CARTESIAN_POINT('',(-0.680357142857142,5.42196124188312,32.1799631621335));
#308037=CARTESIAN_POINT('Ctrl Pts',(-1.18611505681818,6.24212662337662,
36.25));
#308038=CARTESIAN_POINT('Ctrl Pts',(-1.16621033677113,6.23407454786033,
36.25));
#308039=CARTESIAN_POINT('Ctrl Pts',(-1.12679451037092,6.21812962575334,
36.25));
#308040=CARTESIAN_POINT('Ctrl Pts',(-1.07097627880842,6.18887731351974,
36.25));
#308041=CARTESIAN_POINT('Ctrl Pts',(-1.01831785359978,6.15682435284569,
36.25));
#308042=CARTESIAN_POINT('Ctrl Pts',(-0.969980971511446,6.12033427680283,
36.25));
#308043=CARTESIAN_POINT('Ctrl Pts',(-0.924520209270103,6.08096773911451,
36.25));
#308044=CARTESIAN_POINT('Ctrl Pts',(-0.882532948756259,6.03778353402304,
36.25));
#308045=CARTESIAN_POINT('Ctrl Pts',(-0.844529687053187,5.99064810748104,
36.25));
#308046=CARTESIAN_POINT('Ctrl Pts',(-0.810449385509135,5.94000771696759,
36.25));
#308047=CARTESIAN_POINT('Ctrl Pts',(-0.778997347786388,5.88660676946342,
36.25));
#308048=CARTESIAN_POINT('Ctrl Pts',(-0.753130561450395,5.82909896870107,
36.25));
#308049=CARTESIAN_POINT('Ctrl Pts',(-0.730130420178432,5.76902496530641,
36.25));
#308050=CARTESIAN_POINT('Ctrl Pts',(-0.712369756219759,5.70553707456913,
36.25));
#308051=CARTESIAN_POINT('Ctrl Pts',(-0.698134608146914,5.63904690448481,
36.25));
#308052=CARTESIAN_POINT('Ctrl Pts',(-0.688060973290405,5.56952358146944,
36.25));
#308053=CARTESIAN_POINT('Ctrl Pts',(-0.681202359695404,5.4968345485113,
36.25));
#308054=CARTESIAN_POINT('Ctrl Pts',(-0.680643402753075,5.44731949788714,
36.25));
#308055=CARTESIAN_POINT('Ctrl Pts',(-0.680357142857142,5.42196124188312,
36.25));
#308056=CARTESIAN_POINT('Ctrl Pts',(-0.804058441558441,6.88253855519481,
36.05));
#308057=CARTESIAN_POINT('Ctrl Pts',(-0.804058441558441,6.88253855519481,
36.29));
#308058=CARTESIAN_POINT('Ctrl Pts',(-0.804999967272473,6.8452978442089,
36.05));
#308059=CARTESIAN_POINT('Ctrl Pts',(-0.804999967272473,6.8452978442089,
36.29));
#308060=CARTESIAN_POINT('Ctrl Pts',(-0.806813602327297,6.77356208818653,
36.05));
#308061=CARTESIAN_POINT('Ctrl Pts',(-0.806813602327297,6.77356208818653,
36.29));
#308062=CARTESIAN_POINT('Ctrl Pts',(-0.825519260309656,6.6705401244345,
36.05));
#308063=CARTESIAN_POINT('Ctrl Pts',(-0.825519260309656,6.6705401244345,
36.29));
#308064=CARTESIAN_POINT('Ctrl Pts',(-0.854639610807379,6.57608978278239,
36.05));
#308065=CARTESIAN_POINT('Ctrl Pts',(-0.854639610807379,6.57608978278239,
36.29));
#308066=CARTESIAN_POINT('Ctrl Pts',(-0.897038222357849,6.4907436496301,
36.05));
#308067=CARTESIAN_POINT('Ctrl Pts',(-0.897038222357849,6.4907436496301,
36.29));
#308068=CARTESIAN_POINT('Ctrl Pts',(-0.951235352872532,6.41405772296989,
36.05));
#308069=CARTESIAN_POINT('Ctrl Pts',(-0.951235352872532,6.41405772296989,
36.29));
#308070=CARTESIAN_POINT('Ctrl Pts',(-1.0177935092216,6.34678274879809,36.05));
#308071=CARTESIAN_POINT('Ctrl Pts',(-1.0177935092216,6.34678274879809,36.29));
#308072=CARTESIAN_POINT('Ctrl Pts',(-1.09604440098142,6.28741747621295,
36.05));
#308073=CARTESIAN_POINT('Ctrl Pts',(-1.09604440098142,6.28741747621295,
36.29));
#308074=CARTESIAN_POINT('Ctrl Pts',(-1.15549574155667,6.25752314612396,
36.05));
#308075=CARTESIAN_POINT('Ctrl Pts',(-1.15549574155667,6.25752314612396,
36.29));
#308076=CARTESIAN_POINT('Ctrl Pts',(-1.18611505681818,6.24212662337662,
36.05));
#308077=CARTESIAN_POINT('Ctrl Pts',(-1.18611505681818,6.24212662337662,
36.29));
#308078=CARTESIAN_POINT('',(-0.804058441558441,6.88253855519481,36.25));
#308079=CARTESIAN_POINT('',(-0.804058441558441,6.88253855519481,32.1799631621335));
#308080=CARTESIAN_POINT('Ctrl Pts',(-0.804058441558441,6.88253855519481,
36.25));
#308081=CARTESIAN_POINT('Ctrl Pts',(-0.804999967272473,6.8452978442089,
36.25));
#308082=CARTESIAN_POINT('Ctrl Pts',(-0.806813602327297,6.77356208818653,
36.25));
#308083=CARTESIAN_POINT('Ctrl Pts',(-0.825519260309656,6.6705401244345,
36.25));
#308084=CARTESIAN_POINT('Ctrl Pts',(-0.854639610807379,6.57608978278239,
36.25));
#308085=CARTESIAN_POINT('Ctrl Pts',(-0.897038222357849,6.4907436496301,
36.25));
#308086=CARTESIAN_POINT('Ctrl Pts',(-0.951235352872532,6.41405772296989,
36.25));
#308087=CARTESIAN_POINT('Ctrl Pts',(-1.0177935092216,6.34678274879809,36.25));
#308088=CARTESIAN_POINT('Ctrl Pts',(-1.09604440098142,6.28741747621295,
36.25));
#308089=CARTESIAN_POINT('Ctrl Pts',(-1.15549574155667,6.25752314612396,
36.25));
#308090=CARTESIAN_POINT('Ctrl Pts',(-1.18611505681818,6.24212662337662,
36.25));
#308091=CARTESIAN_POINT('Ctrl Pts',(-1.52887073863637,7.71623376623377,
36.05));
#308092=CARTESIAN_POINT('Ctrl Pts',(-1.52887073863637,7.71623376623377,
36.29));
#308093=CARTESIAN_POINT('Ctrl Pts',(-1.50349048519761,7.71545767890599,
36.05));
#308094=CARTESIAN_POINT('Ctrl Pts',(-1.50349048519761,7.71545767890599,
36.29));
#308095=CARTESIAN_POINT('Ctrl Pts',(-1.45335117903047,7.71392449956901,
36.05));
#308096=CARTESIAN_POINT('Ctrl Pts',(-1.45335117903047,7.71392449956901,
36.29));
#308097=CARTESIAN_POINT('Ctrl Pts',(-1.37991458997475,7.7027904588233,36.05));
#308098=CARTESIAN_POINT('Ctrl Pts',(-1.37991458997475,7.7027904588233,36.29));
#308099=CARTESIAN_POINT('Ctrl Pts',(-1.30973339831807,7.68468886160549,
36.05));
#308100=CARTESIAN_POINT('Ctrl Pts',(-1.30973339831807,7.68468886160549,
36.29));
#308101=CARTESIAN_POINT('Ctrl Pts',(-1.24280687342643,7.65953041457979,
36.05));
#308102=CARTESIAN_POINT('Ctrl Pts',(-1.24280687342643,7.65953041457979,
36.29));
#308103=CARTESIAN_POINT('Ctrl Pts',(-1.17924186808025,7.62639783586101,
36.05));
#308104=CARTESIAN_POINT('Ctrl Pts',(-1.17924186808025,7.62639783586101,
36.29));
#308105=CARTESIAN_POINT('Ctrl Pts',(-1.119447579553,7.58560597597768,36.05));
#308106=CARTESIAN_POINT('Ctrl Pts',(-1.119447579553,7.58560597597768,36.29));
#308107=CARTESIAN_POINT('Ctrl Pts',(-1.06268331120451,7.53791001729144,
36.05));
#308108=CARTESIAN_POINT('Ctrl Pts',(-1.06268331120451,7.53791001729144,
36.29));
#308109=CARTESIAN_POINT('Ctrl Pts',(-1.00970620194357,7.48362087256877,
36.05));
#308110=CARTESIAN_POINT('Ctrl Pts',(-1.00970620194357,7.48362087256877,
36.29));
#308111=CARTESIAN_POINT('Ctrl Pts',(-0.961621998889034,7.42336185115535,
36.05));
#308112=CARTESIAN_POINT('Ctrl Pts',(-0.961621998889034,7.42336185115535,
36.29));
#308113=CARTESIAN_POINT('Ctrl Pts',(-0.919708538459593,7.35843862911193,
36.05));
#308114=CARTESIAN_POINT('Ctrl Pts',(-0.919708538459593,7.35843862911193,
36.29));
#308115=CARTESIAN_POINT('Ctrl Pts',(-0.883047786444258,7.29002627559583,
36.05));
#308116=CARTESIAN_POINT('Ctrl Pts',(-0.883047786444258,7.29002627559583,
36.29));
#308117=CARTESIAN_POINT('Ctrl Pts',(-0.854229034877609,7.21661236790923,
36.05));
#308118=CARTESIAN_POINT('Ctrl Pts',(-0.854229034877609,7.21661236790923,
36.29));
#308119=CARTESIAN_POINT('Ctrl Pts',(-0.831597303625935,7.13897358699381,
36.05));
#308120=CARTESIAN_POINT('Ctrl Pts',(-0.831597303625935,7.13897358699381,
36.29));
#308121=CARTESIAN_POINT('Ctrl Pts',(-0.815733176885725,7.05701575208482,
36.05));
#308122=CARTESIAN_POINT('Ctrl Pts',(-0.815733176885725,7.05701575208482,
36.29));
#308123=CARTESIAN_POINT('Ctrl Pts',(-0.805811171394462,6.97104879536392,
36.05));
#308124=CARTESIAN_POINT('Ctrl Pts',(-0.805811171394462,6.97104879536392,
36.29));
#308125=CARTESIAN_POINT('Ctrl Pts',(-0.804650124600102,6.91241766550898,
36.05));
#308126=CARTESIAN_POINT('Ctrl Pts',(-0.804650124600102,6.91241766550898,
36.29));
#308127=CARTESIAN_POINT('Ctrl Pts',(-0.804058441558441,6.88253855519481,
36.05));
#308128=CARTESIAN_POINT('Ctrl Pts',(-0.804058441558441,6.88253855519481,
36.29));
#308129=CARTESIAN_POINT('',(-1.52887073863637,7.71623376623377,36.25));
#308130=CARTESIAN_POINT('',(-1.52887073863637,7.71623376623377,32.1799631621335));
#308131=CARTESIAN_POINT('Ctrl Pts',(-1.52887073863637,7.71623376623377,
36.25));
#308132=CARTESIAN_POINT('Ctrl Pts',(-1.50349048519761,7.71545767890599,
36.25));
#308133=CARTESIAN_POINT('Ctrl Pts',(-1.45335117903047,7.71392449956901,
36.25));
#308134=CARTESIAN_POINT('Ctrl Pts',(-1.37991458997475,7.7027904588233,36.25));
#308135=CARTESIAN_POINT('Ctrl Pts',(-1.30973339831807,7.68468886160549,
36.25));
#308136=CARTESIAN_POINT('Ctrl Pts',(-1.24280687342643,7.65953041457979,
36.25));
#308137=CARTESIAN_POINT('Ctrl Pts',(-1.17924186808025,7.62639783586101,
36.25));
#308138=CARTESIAN_POINT('Ctrl Pts',(-1.119447579553,7.58560597597768,36.25));
#308139=CARTESIAN_POINT('Ctrl Pts',(-1.06268331120451,7.53791001729144,
36.25));
#308140=CARTESIAN_POINT('Ctrl Pts',(-1.00970620194357,7.48362087256877,
36.25));
#308141=CARTESIAN_POINT('Ctrl Pts',(-0.961621998889034,7.42336185115535,
36.25));
#308142=CARTESIAN_POINT('Ctrl Pts',(-0.919708538459593,7.35843862911193,
36.25));
#308143=CARTESIAN_POINT('Ctrl Pts',(-0.883047786444258,7.29002627559583,
36.25));
#308144=CARTESIAN_POINT('Ctrl Pts',(-0.854229034877609,7.21661236790923,
36.25));
#308145=CARTESIAN_POINT('Ctrl Pts',(-0.831597303625935,7.13897358699381,
36.25));
#308146=CARTESIAN_POINT('Ctrl Pts',(-0.815733176885725,7.05701575208482,
36.25));
#308147=CARTESIAN_POINT('Ctrl Pts',(-0.805811171394462,6.97104879536392,
36.25));
#308148=CARTESIAN_POINT('Ctrl Pts',(-0.804650124600102,6.91241766550898,
36.25));
#308149=CARTESIAN_POINT('Ctrl Pts',(-0.804058441558441,6.88253855519481,
36.25));
#308150=CARTESIAN_POINT('Ctrl Pts',(-2.24724025974026,6.89542410714286,
36.05));
#308151=CARTESIAN_POINT('Ctrl Pts',(-2.24724025974026,6.89542410714286,
36.29));
#308152=CARTESIAN_POINT('Ctrl Pts',(-2.24664961358837,6.92508712200564,
36.05));
#308153=CARTESIAN_POINT('Ctrl Pts',(-2.24664961358837,6.92508712200564,
36.29));
#308154=CARTESIAN_POINT('Ctrl Pts',(-2.24549498801578,6.98307391394772,
36.05));
#308155=CARTESIAN_POINT('Ctrl Pts',(-2.24549498801578,6.98307391394772,
36.29));
#308156=CARTESIAN_POINT('Ctrl Pts',(-2.23564047821614,7.06800054423278,
36.05));
#308157=CARTESIAN_POINT('Ctrl Pts',(-2.23564047821614,7.06800054423278,
36.29));
#308158=CARTESIAN_POINT('Ctrl Pts',(-2.2194554245458,7.1485092997012,36.05));
#308159=CARTESIAN_POINT('Ctrl Pts',(-2.2194554245458,7.1485092997012,36.29));
#308160=CARTESIAN_POINT('Ctrl Pts',(-2.19802765306379,7.22519194306317,
36.05));
#308161=CARTESIAN_POINT('Ctrl Pts',(-2.19802765306379,7.22519194306317,
36.29));
#308162=CARTESIAN_POINT('Ctrl Pts',(-2.1683837201686,7.29688183752562,36.05));
#308163=CARTESIAN_POINT('Ctrl Pts',(-2.1683837201686,7.29688183752562,36.29));
#308164=CARTESIAN_POINT('Ctrl Pts',(-2.13381867185592,7.36527391878087,
36.05));
#308165=CARTESIAN_POINT('Ctrl Pts',(-2.13381867185592,7.36527391878087,
36.29));
#308166=CARTESIAN_POINT('Ctrl Pts',(-2.09163145310384,7.42884662646377,
36.05));
#308167=CARTESIAN_POINT('Ctrl Pts',(-2.09163145310384,7.42884662646377,
36.29));
#308168=CARTESIAN_POINT('Ctrl Pts',(-2.04420697733625,7.48817807892744,
36.05));
#308169=CARTESIAN_POINT('Ctrl Pts',(-2.04420697733625,7.48817807892744,
36.29));
#308170=CARTESIAN_POINT('Ctrl Pts',(-1.99157504243468,7.54133429965825,
36.05));
#308171=CARTESIAN_POINT('Ctrl Pts',(-1.99157504243468,7.54133429965825,
36.29));
#308172=CARTESIAN_POINT('Ctrl Pts',(-1.93532052837525,7.58805917500155,
36.05));
#308173=CARTESIAN_POINT('Ctrl Pts',(-1.93532052837525,7.58805917500155,
36.29));
#308174=CARTESIAN_POINT('Ctrl Pts',(-1.87562432631225,7.62785439831755,
36.05));
#308175=CARTESIAN_POINT('Ctrl Pts',(-1.87562432631225,7.62785439831755,
36.29));
#308176=CARTESIAN_POINT('Ctrl Pts',(-1.81235851864406,7.65993643724945,
36.05));
#308177=CARTESIAN_POINT('Ctrl Pts',(-1.81235851864406,7.65993643724945,
36.29));
#308178=CARTESIAN_POINT('Ctrl Pts',(-1.746104953362,7.68533220871074,36.05));
#308179=CARTESIAN_POINT('Ctrl Pts',(-1.746104953362,7.68533220871074,36.29));
#308180=CARTESIAN_POINT('Ctrl Pts',(-1.67660001580121,7.7036309678914,36.05));
#308181=CARTESIAN_POINT('Ctrl Pts',(-1.67660001580121,7.7036309678914,36.29));
#308182=CARTESIAN_POINT('Ctrl Pts',(-1.60368781725867,7.71370952681349,
36.05));
#308183=CARTESIAN_POINT('Ctrl Pts',(-1.60368781725867,7.71370952681349,
36.29));
#308184=CARTESIAN_POINT('Ctrl Pts',(-1.55402639381368,7.71538504428939,
36.05));
#308185=CARTESIAN_POINT('Ctrl Pts',(-1.55402639381368,7.71538504428939,
36.29));
#308186=CARTESIAN_POINT('Ctrl Pts',(-1.52887073863637,7.71623376623377,
36.05));
#308187=CARTESIAN_POINT('Ctrl Pts',(-1.52887073863637,7.71623376623377,
36.29));
#308188=CARTESIAN_POINT('',(-2.24724025974026,6.89542410714286,36.25));
#308189=CARTESIAN_POINT('',(-2.24724025974026,6.89542410714286,32.1799631621335));
#308190=CARTESIAN_POINT('Ctrl Pts',(-2.24724025974026,6.89542410714286,
36.25));
#308191=CARTESIAN_POINT('Ctrl Pts',(-2.24664961358837,6.92508712200564,
36.25));
#308192=CARTESIAN_POINT('Ctrl Pts',(-2.24549498801578,6.98307391394772,
36.25));
#308193=CARTESIAN_POINT('Ctrl Pts',(-2.23564047821614,7.06800054423278,
36.25));
#308194=CARTESIAN_POINT('Ctrl Pts',(-2.2194554245458,7.1485092997012,36.25));
#308195=CARTESIAN_POINT('Ctrl Pts',(-2.19802765306379,7.22519194306317,
36.25));
#308196=CARTESIAN_POINT('Ctrl Pts',(-2.1683837201686,7.29688183752562,36.25));
#308197=CARTESIAN_POINT('Ctrl Pts',(-2.13381867185592,7.36527391878087,
36.25));
#308198=CARTESIAN_POINT('Ctrl Pts',(-2.09163145310384,7.42884662646377,
36.25));
#308199=CARTESIAN_POINT('Ctrl Pts',(-2.04420697733625,7.48817807892744,
36.25));
#308200=CARTESIAN_POINT('Ctrl Pts',(-1.99157504243468,7.54133429965825,
36.25));
#308201=CARTESIAN_POINT('Ctrl Pts',(-1.93532052837525,7.58805917500155,
36.25));
#308202=CARTESIAN_POINT('Ctrl Pts',(-1.87562432631225,7.62785439831755,
36.25));
#308203=CARTESIAN_POINT('Ctrl Pts',(-1.81235851864406,7.65993643724945,
36.25));
#308204=CARTESIAN_POINT('Ctrl Pts',(-1.746104953362,7.68533220871074,36.25));
#308205=CARTESIAN_POINT('Ctrl Pts',(-1.67660001580121,7.7036309678914,36.25));
#308206=CARTESIAN_POINT('Ctrl Pts',(-1.60368781725867,7.71370952681349,
36.25));
#308207=CARTESIAN_POINT('Ctrl Pts',(-1.55402639381368,7.71538504428939,
36.25));
#308208=CARTESIAN_POINT('Ctrl Pts',(-1.52887073863637,7.71623376623377,
36.25));
#308209=CARTESIAN_POINT('Ctrl Pts',(-1.86131797889611,6.24212662337662,
36.05));
#308210=CARTESIAN_POINT('Ctrl Pts',(-1.86131797889611,6.24212662337662,
36.29));
#308211=CARTESIAN_POINT('Ctrl Pts',(-1.89166914263337,6.25737900558171,
36.05));
#308212=CARTESIAN_POINT('Ctrl Pts',(-1.89166914263337,6.25737900558171,
36.29));
#308213=CARTESIAN_POINT('Ctrl Pts',(-1.95088478291998,6.28713666449684,
36.05));
#308214=CARTESIAN_POINT('Ctrl Pts',(-1.95088478291998,6.28713666449684,
36.29));
#308215=CARTESIAN_POINT('Ctrl Pts',(-2.02981249733957,6.34542328474194,
36.05));
#308216=CARTESIAN_POINT('Ctrl Pts',(-2.02981249733957,6.34542328474194,
36.29));
#308217=CARTESIAN_POINT('Ctrl Pts',(-2.09711468722833,6.41311300974787,
36.05));
#308218=CARTESIAN_POINT('Ctrl Pts',(-2.09711468722833,6.41311300974787,
36.29));
#308219=CARTESIAN_POINT('Ctrl Pts',(-2.15255407155767,6.49069341485485,
36.05));
#308220=CARTESIAN_POINT('Ctrl Pts',(-2.15255407155767,6.49069341485485,
36.29));
#308221=CARTESIAN_POINT('Ctrl Pts',(-2.19544755091121,6.57824013430206,
36.05));
#308222=CARTESIAN_POINT('Ctrl Pts',(-2.19544755091121,6.57824013430206,
36.29));
#308223=CARTESIAN_POINT('Ctrl Pts',(-2.22526998846174,6.67544579213543,
36.05));
#308224=CARTESIAN_POINT('Ctrl Pts',(-2.22526998846174,6.67544579213543,
36.29));
#308225=CARTESIAN_POINT('Ctrl Pts',(-2.24466128369114,6.78212192154818,
36.05));
#308226=CARTESIAN_POINT('Ctrl Pts',(-2.24466128369114,6.78212192154818,
36.29));
#308227=CARTESIAN_POINT('Ctrl Pts',(-2.24635828463311,6.85667628421743,
36.05));
#308228=CARTESIAN_POINT('Ctrl Pts',(-2.24635828463311,6.85667628421743,
36.29));
#308229=CARTESIAN_POINT('Ctrl Pts',(-2.24724025974026,6.89542410714286,
36.05));
#308230=CARTESIAN_POINT('Ctrl Pts',(-2.24724025974026,6.89542410714286,
36.29));
#308231=CARTESIAN_POINT('',(-1.86131797889611,6.24212662337662,36.25));
#308232=CARTESIAN_POINT('',(-1.86131797889611,6.24212662337662,32.1799631621335));
#308233=CARTESIAN_POINT('Ctrl Pts',(-1.86131797889611,6.24212662337662,
36.25));
#308234=CARTESIAN_POINT('Ctrl Pts',(-1.89166914263337,6.25737900558171,
36.25));
#308235=CARTESIAN_POINT('Ctrl Pts',(-1.95088478291998,6.28713666449684,
36.25));
#308236=CARTESIAN_POINT('Ctrl Pts',(-2.02981249733957,6.34542328474194,
36.25));
#308237=CARTESIAN_POINT('Ctrl Pts',(-2.09711468722833,6.41311300974787,
36.25));
#308238=CARTESIAN_POINT('Ctrl Pts',(-2.15255407155767,6.49069341485485,
36.25));
#308239=CARTESIAN_POINT('Ctrl Pts',(-2.19544755091121,6.57824013430206,
36.25));
#308240=CARTESIAN_POINT('Ctrl Pts',(-2.22526998846174,6.67544579213543,
36.25));
#308241=CARTESIAN_POINT('Ctrl Pts',(-2.24466128369114,6.78212192154818,
36.25));
#308242=CARTESIAN_POINT('Ctrl Pts',(-2.24635828463311,6.85667628421743,
36.25));
#308243=CARTESIAN_POINT('Ctrl Pts',(-2.24724025974026,6.89542410714286,
36.25));
#308244=CARTESIAN_POINT('Ctrl Pts',(-2.37094155844156,5.43291396103896,
36.05));
#308245=CARTESIAN_POINT('Ctrl Pts',(-2.37094155844156,5.43291396103896,
36.29));
#308246=CARTESIAN_POINT('Ctrl Pts',(-2.37063000734488,5.45891313799848,
36.05));
#308247=CARTESIAN_POINT('Ctrl Pts',(-2.37063000734488,5.45891313799848,
36.29));
#308248=CARTESIAN_POINT('Ctrl Pts',(-2.37001876348768,5.50992190470655,
36.05));
#308249=CARTESIAN_POINT('Ctrl Pts',(-2.37001876348768,5.50992190470655,
36.29));
#308250=CARTESIAN_POINT('Ctrl Pts',(-2.36345937406549,5.58482539360676,
36.05));
#308251=CARTESIAN_POINT('Ctrl Pts',(-2.36345937406549,5.58482539360676,
36.29));
#308252=CARTESIAN_POINT('Ctrl Pts',(-2.35252585809151,5.65624108672131,
36.05));
#308253=CARTESIAN_POINT('Ctrl Pts',(-2.35252585809151,5.65624108672131,
36.29));
#308254=CARTESIAN_POINT('Ctrl Pts',(-2.33776644819188,5.72405509656198,
36.05));
#308255=CARTESIAN_POINT('Ctrl Pts',(-2.33776644819188,5.72405509656198,
36.29));
#308256=CARTESIAN_POINT('Ctrl Pts',(-2.31914738800462,5.78833295550162,
36.05));
#308257=CARTESIAN_POINT('Ctrl Pts',(-2.31914738800462,5.78833295550162,
36.29));
#308258=CARTESIAN_POINT('Ctrl Pts',(-2.29590420953425,5.84911895337204,
36.05));
#308259=CARTESIAN_POINT('Ctrl Pts',(-2.29590420953425,5.84911895337204,
36.29));
#308260=CARTESIAN_POINT('Ctrl Pts',(-2.26824051996169,5.90641132135784,
36.05));
#308261=CARTESIAN_POINT('Ctrl Pts',(-2.26824051996169,5.90641132135784,
36.29));
#308262=CARTESIAN_POINT('Ctrl Pts',(-2.23643083441821,5.96019951630268,
36.05));
#308263=CARTESIAN_POINT('Ctrl Pts',(-2.23643083441821,5.96019951630268,
36.29));
#308264=CARTESIAN_POINT('Ctrl Pts',(-2.20124132093025,6.01030469320115,
36.05));
#308265=CARTESIAN_POINT('Ctrl Pts',(-2.20124132093025,6.01030469320115,
36.29));
#308266=CARTESIAN_POINT('Ctrl Pts',(-2.16248925313098,6.05629105732706,
36.05));
#308267=CARTESIAN_POINT('Ctrl Pts',(-2.16248925313098,6.05629105732706,
36.29));
#308268=CARTESIAN_POINT('Ctrl Pts',(-2.1202782797022,6.09774166415627,36.05));
#308269=CARTESIAN_POINT('Ctrl Pts',(-2.1202782797022,6.09774166415627,36.29));
#308270=CARTESIAN_POINT('Ctrl Pts',(-2.07499444571376,6.1351992195304,36.05));
#308271=CARTESIAN_POINT('Ctrl Pts',(-2.07499444571376,6.1351992195304,36.29));
#308272=CARTESIAN_POINT('Ctrl Pts',(-2.02656583006182,6.16910978501208,
36.05));
#308273=CARTESIAN_POINT('Ctrl Pts',(-2.02656583006182,6.16910978501208,
36.29));
#308274=CARTESIAN_POINT('Ctrl Pts',(-1.97432962905344,6.19776979492405,
36.05));
#308275=CARTESIAN_POINT('Ctrl Pts',(-1.97432962905344,6.19776979492405,
36.29));
#308276=CARTESIAN_POINT('Ctrl Pts',(-1.91917711253447,6.22263196745495,
36.05));
#308277=CARTESIAN_POINT('Ctrl Pts',(-1.91917711253447,6.22263196745495,
36.29));
#308278=CARTESIAN_POINT('Ctrl Pts',(-1.88076808190029,6.23557324032603,
36.05));
#308279=CARTESIAN_POINT('Ctrl Pts',(-1.88076808190029,6.23557324032603,
36.29));
#308280=CARTESIAN_POINT('Ctrl Pts',(-1.86131797889611,6.24212662337662,
36.05));
#308281=CARTESIAN_POINT('Ctrl Pts',(-1.86131797889611,6.24212662337662,
36.29));
#308282=CARTESIAN_POINT('',(-2.37094155844156,5.43291396103896,36.25));
#308283=CARTESIAN_POINT('',(-2.37094155844156,5.43291396103896,32.1799631621335));
#308284=CARTESIAN_POINT('Ctrl Pts',(-2.37094155844156,5.43291396103896,
36.25));
#308285=CARTESIAN_POINT('Ctrl Pts',(-2.37063000734488,5.45891313799848,
36.25));
#308286=CARTESIAN_POINT('Ctrl Pts',(-2.37001876348768,5.50992190470655,
36.25));
#308287=CARTESIAN_POINT('Ctrl Pts',(-2.36345937406549,5.58482539360676,
36.25));
#308288=CARTESIAN_POINT('Ctrl Pts',(-2.35252585809151,5.65624108672131,
36.25));
#308289=CARTESIAN_POINT('Ctrl Pts',(-2.33776644819188,5.72405509656198,
36.25));
#308290=CARTESIAN_POINT('Ctrl Pts',(-2.31914738800462,5.78833295550162,
36.25));
#308291=CARTESIAN_POINT('Ctrl Pts',(-2.29590420953425,5.84911895337204,
36.25));
#308292=CARTESIAN_POINT('Ctrl Pts',(-2.26824051996169,5.90641132135784,
36.25));
#308293=CARTESIAN_POINT('Ctrl Pts',(-2.23643083441821,5.96019951630268,
36.25));
#308294=CARTESIAN_POINT('Ctrl Pts',(-2.20124132093025,6.01030469320115,
36.25));
#308295=CARTESIAN_POINT('Ctrl Pts',(-2.16248925313098,6.05629105732706,
36.25));
#308296=CARTESIAN_POINT('Ctrl Pts',(-2.1202782797022,6.09774166415627,36.25));
#308297=CARTESIAN_POINT('Ctrl Pts',(-2.07499444571376,6.1351992195304,36.25));
#308298=CARTESIAN_POINT('Ctrl Pts',(-2.02656583006182,6.16910978501208,
36.25));
#308299=CARTESIAN_POINT('Ctrl Pts',(-1.97432962905344,6.19776979492405,
36.25));
#308300=CARTESIAN_POINT('Ctrl Pts',(-1.91917711253447,6.22263196745495,
36.25));
#308301=CARTESIAN_POINT('Ctrl Pts',(-1.88076808190029,6.23557324032603,
36.25));
#308302=CARTESIAN_POINT('Ctrl Pts',(-1.86131797889611,6.24212662337662,
36.25));
#308303=CARTESIAN_POINT('Ctrl Pts',(-1.52371651785714,4.45876623376623,
36.05));
#308304=CARTESIAN_POINT('Ctrl Pts',(-1.52371651785714,4.45876623376623,
36.29));
#308305=CARTESIAN_POINT('Ctrl Pts',(-1.55338922539081,4.4597253240939,36.05));
#308306=CARTESIAN_POINT('Ctrl Pts',(-1.55338922539081,4.4597253240939,36.29));
#308307=CARTESIAN_POINT('Ctrl Pts',(-1.61170021909538,4.46161006986558,
36.05));
#308308=CARTESIAN_POINT('Ctrl Pts',(-1.61170021909538,4.46161006986558,
36.29));
#308309=CARTESIAN_POINT('Ctrl Pts',(-1.69736543838644,4.47372823681752,
36.05));
#308310=CARTESIAN_POINT('Ctrl Pts',(-1.69736543838644,4.47372823681752,
36.29));
#308311=CARTESIAN_POINT('Ctrl Pts',(-1.77882069442911,4.49538915943629,
36.05));
#308312=CARTESIAN_POINT('Ctrl Pts',(-1.77882069442911,4.49538915943629,
36.29));
#308313=CARTESIAN_POINT('Ctrl Pts',(-1.85703181398638,4.52434515927101,
36.05));
#308314=CARTESIAN_POINT('Ctrl Pts',(-1.85703181398638,4.52434515927101,
36.29));
#308315=CARTESIAN_POINT('Ctrl Pts',(-1.93122097549665,4.56241550483758,
36.05));
#308316=CARTESIAN_POINT('Ctrl Pts',(-1.93122097549665,4.56241550483758,
36.29));
#308317=CARTESIAN_POINT('Ctrl Pts',(-2.00109150543013,4.60959489382438,
36.05));
#308318=CARTESIAN_POINT('Ctrl Pts',(-2.00109150543013,4.60959489382438,
36.29));
#308319=CARTESIAN_POINT('Ctrl Pts',(-2.06813219984915,4.66375358613811,
36.05));
#308320=CARTESIAN_POINT('Ctrl Pts',(-2.06813219984915,4.66375358613811,
36.29));
#308321=CARTESIAN_POINT('Ctrl Pts',(-2.1298438000822,4.72680658155488,36.05));
#308322=CARTESIAN_POINT('Ctrl Pts',(-2.1298438000822,4.72680658155488,36.29));
#308323=CARTESIAN_POINT('Ctrl Pts',(-2.18686174567011,4.79599402074389,
36.05));
#308324=CARTESIAN_POINT('Ctrl Pts',(-2.18686174567011,4.79599402074389,
36.29));
#308325=CARTESIAN_POINT('Ctrl Pts',(-2.2354792856985,4.87186228483585,36.05));
#308326=CARTESIAN_POINT('Ctrl Pts',(-2.2354792856985,4.87186228483585,36.29));
#308327=CARTESIAN_POINT('Ctrl Pts',(-2.27806144254569,4.95218254596678,
36.05));
#308328=CARTESIAN_POINT('Ctrl Pts',(-2.27806144254569,4.95218254596678,
36.29));
#308329=CARTESIAN_POINT('Ctrl Pts',(-2.31200320040195,5.03825698338498,
36.05));
#308330=CARTESIAN_POINT('Ctrl Pts',(-2.31200320040195,5.03825698338498,
36.29));
#308331=CARTESIAN_POINT('Ctrl Pts',(-2.33853623055972,5.12949961741785,
36.05));
#308332=CARTESIAN_POINT('Ctrl Pts',(-2.33853623055972,5.12949961741785,
36.29));
#308333=CARTESIAN_POINT('Ctrl Pts',(-2.35686977721559,5.22616336292247,
36.05));
#308334=CARTESIAN_POINT('Ctrl Pts',(-2.35686977721559,5.22616336292247,
36.29));
#308335=CARTESIAN_POINT('Ctrl Pts',(-2.36886427906175,5.32781045016027,
36.05));
#308336=CARTESIAN_POINT('Ctrl Pts',(-2.36886427906175,5.32781045016027,
36.29));
#308337=CARTESIAN_POINT('Ctrl Pts',(-2.37024051692734,5.39744356397404,
36.05));
#308338=CARTESIAN_POINT('Ctrl Pts',(-2.37024051692734,5.39744356397404,
36.29));
#308339=CARTESIAN_POINT('Ctrl Pts',(-2.37094155844156,5.43291396103896,
36.05));
#308340=CARTESIAN_POINT('Ctrl Pts',(-2.37094155844156,5.43291396103896,
36.29));
#308341=CARTESIAN_POINT('',(-1.52371651785714,4.45876623376623,36.25));
#308342=CARTESIAN_POINT('',(-1.52371651785714,4.45876623376623,32.1799631621335));
#308343=CARTESIAN_POINT('Ctrl Pts',(-1.52371651785714,4.45876623376623,
36.25));
#308344=CARTESIAN_POINT('Ctrl Pts',(-1.55338922539081,4.4597253240939,36.25));
#308345=CARTESIAN_POINT('Ctrl Pts',(-1.61170021909538,4.46161006986558,
36.25));
#308346=CARTESIAN_POINT('Ctrl Pts',(-1.69736543838644,4.47372823681752,
36.25));
#308347=CARTESIAN_POINT('Ctrl Pts',(-1.77882069442911,4.49538915943629,
36.25));
#308348=CARTESIAN_POINT('Ctrl Pts',(-1.85703181398638,4.52434515927101,
36.25));
#308349=CARTESIAN_POINT('Ctrl Pts',(-1.93122097549665,4.56241550483758,
36.25));
#308350=CARTESIAN_POINT('Ctrl Pts',(-2.00109150543013,4.60959489382438,
36.25));
#308351=CARTESIAN_POINT('Ctrl Pts',(-2.06813219984915,4.66375358613811,
36.25));
#308352=CARTESIAN_POINT('Ctrl Pts',(-2.1298438000822,4.72680658155488,36.25));
#308353=CARTESIAN_POINT('Ctrl Pts',(-2.18686174567011,4.79599402074389,
36.25));
#308354=CARTESIAN_POINT('Ctrl Pts',(-2.2354792856985,4.87186228483585,36.25));
#308355=CARTESIAN_POINT('Ctrl Pts',(-2.27806144254569,4.95218254596678,
36.25));
#308356=CARTESIAN_POINT('Ctrl Pts',(-2.31200320040195,5.03825698338498,
36.25));
#308357=CARTESIAN_POINT('Ctrl Pts',(-2.33853623055972,5.12949961741785,
36.25));
#308358=CARTESIAN_POINT('Ctrl Pts',(-2.35686977721559,5.22616336292247,
36.25));
#308359=CARTESIAN_POINT('Ctrl Pts',(-2.36886427906175,5.32781045016027,
36.25));
#308360=CARTESIAN_POINT('Ctrl Pts',(-2.37024051692734,5.39744356397404,
36.25));
#308361=CARTESIAN_POINT('Ctrl Pts',(-2.37094155844156,5.43291396103896,
36.25));
#308362=CARTESIAN_POINT('Ctrl Pts',(-0.680357142857142,5.42196124188312,
36.05));
#308363=CARTESIAN_POINT('Ctrl Pts',(-0.680357142857142,5.42196124188312,
36.29));
#308364=CARTESIAN_POINT('Ctrl Pts',(-0.681153739192598,5.3873620729942,
36.05));
#308365=CARTESIAN_POINT('Ctrl Pts',(-0.681153739192598,5.3873620729942,
36.29));
#308366=CARTESIAN_POINT('Ctrl Pts',(-0.682716393984036,5.31949010994648,
36.05));
#308367=CARTESIAN_POINT('Ctrl Pts',(-0.682716393984036,5.31949010994648,
36.29));
#308368=CARTESIAN_POINT('Ctrl Pts',(-0.693373801633478,5.21999888881734,
36.05));
#308369=CARTESIAN_POINT('Ctrl Pts',(-0.693373801633478,5.21999888881734,
36.29));
#308370=CARTESIAN_POINT('Ctrl Pts',(-0.713135864328774,5.12552781537341,
36.05));
#308371=CARTESIAN_POINT('Ctrl Pts',(-0.713135864328774,5.12552781537341,
36.29));
#308372=CARTESIAN_POINT('Ctrl Pts',(-0.739130657263025,5.03559649057185,
36.05));
#308373=CARTESIAN_POINT('Ctrl Pts',(-0.739130657263025,5.03559649057185,
36.29));
#308374=CARTESIAN_POINT('Ctrl Pts',(-0.773615124031434,4.95095791492866,
36.05));
#308375=CARTESIAN_POINT('Ctrl Pts',(-0.773615124031434,4.95095791492866,
36.29));
#308376=CARTESIAN_POINT('Ctrl Pts',(-0.814894945031659,4.87078209602146,
36.05));
#308377=CARTESIAN_POINT('Ctrl Pts',(-0.814894945031659,4.87078209602146,
36.29));
#308378=CARTESIAN_POINT('Ctrl Pts',(-0.864790653609182,4.79615096254107,
36.05));
#308379=CARTESIAN_POINT('Ctrl Pts',(-0.864790653609182,4.79615096254107,
36.29));
#308380=CARTESIAN_POINT('Ctrl Pts',(-0.921346136582458,4.72672058470318,
36.05));
#308381=CARTESIAN_POINT('Ctrl Pts',(-0.921346136582458,4.72672058470318,
36.29));
#308382=CARTESIAN_POINT('Ctrl Pts',(-0.983169721460654,4.66400945675856,
36.05));
#308383=CARTESIAN_POINT('Ctrl Pts',(-0.983169721460654,4.66400945675856,
36.29));
#308384=CARTESIAN_POINT('Ctrl Pts',(-1.04958738921064,4.60935645208091,
36.05));
#308385=CARTESIAN_POINT('Ctrl Pts',(-1.04958738921064,4.60935645208091,
36.29));
#308386=CARTESIAN_POINT('Ctrl Pts',(-1.11934856150417,4.56264762609262,
36.05));
#308387=CARTESIAN_POINT('Ctrl Pts',(-1.11934856150417,4.56264762609262,
36.29));
#308388=CARTESIAN_POINT('Ctrl Pts',(-1.19309519794087,4.5241565808727,36.05));
#308389=CARTESIAN_POINT('Ctrl Pts',(-1.19309519794087,4.5241565808727,36.29));
#308390=CARTESIAN_POINT('Ctrl Pts',(-1.27102264425494,4.49553589484458,
36.05));
#308391=CARTESIAN_POINT('Ctrl Pts',(-1.27102264425494,4.49553589484458,
36.29));
#308392=CARTESIAN_POINT('Ctrl Pts',(-1.35198241500324,4.47370190759594,
36.05));
#308393=CARTESIAN_POINT('Ctrl Pts',(-1.35198241500324,4.47370190759594,
36.29));
#308394=CARTESIAN_POINT('Ctrl Pts',(-1.43680842361535,4.46164864649648,
36.05));
#308395=CARTESIAN_POINT('Ctrl Pts',(-1.43680842361535,4.46164864649648,
36.29));
#308396=CARTESIAN_POINT('Ctrl Pts',(-1.49447449269809,4.45973608112409,
36.05));
#308397=CARTESIAN_POINT('Ctrl Pts',(-1.49447449269809,4.45973608112409,
36.29));
#308398=CARTESIAN_POINT('Ctrl Pts',(-1.52371651785714,4.45876623376623,
36.05));
#308399=CARTESIAN_POINT('Ctrl Pts',(-1.52371651785714,4.45876623376623,
36.29));
#308400=CARTESIAN_POINT('Ctrl Pts',(-0.680357142857142,5.42196124188312,
36.25));
#308401=CARTESIAN_POINT('Ctrl Pts',(-0.681153739192598,5.3873620729942,
36.25));
#308402=CARTESIAN_POINT('Ctrl Pts',(-0.682716393984036,5.31949010994648,
36.25));
#308403=CARTESIAN_POINT('Ctrl Pts',(-0.693373801633478,5.21999888881734,
36.25));
#308404=CARTESIAN_POINT('Ctrl Pts',(-0.713135864328774,5.12552781537341,
36.25));
#308405=CARTESIAN_POINT('Ctrl Pts',(-0.739130657263025,5.03559649057185,
36.25));
#308406=CARTESIAN_POINT('Ctrl Pts',(-0.773615124031434,4.95095791492866,
36.25));
#308407=CARTESIAN_POINT('Ctrl Pts',(-0.814894945031659,4.87078209602146,
36.25));
#308408=CARTESIAN_POINT('Ctrl Pts',(-0.864790653609182,4.79615096254107,
36.25));
#308409=CARTESIAN_POINT('Ctrl Pts',(-0.921346136582458,4.72672058470318,
36.25));
#308410=CARTESIAN_POINT('Ctrl Pts',(-0.983169721460654,4.66400945675856,
36.25));
#308411=CARTESIAN_POINT('Ctrl Pts',(-1.04958738921064,4.60935645208091,
36.25));
#308412=CARTESIAN_POINT('Ctrl Pts',(-1.11934856150417,4.56264762609262,
36.25));
#308413=CARTESIAN_POINT('Ctrl Pts',(-1.19309519794087,4.5241565808727,36.25));
#308414=CARTESIAN_POINT('Ctrl Pts',(-1.27102264425494,4.49553589484458,
36.25));
#308415=CARTESIAN_POINT('Ctrl Pts',(-1.35198241500324,4.47370190759594,
36.25));
#308416=CARTESIAN_POINT('Ctrl Pts',(-1.43680842361535,4.46164864649648,
36.25));
#308417=CARTESIAN_POINT('Ctrl Pts',(-1.49447449269809,4.45973608112409,
36.25));
#308418=CARTESIAN_POINT('Ctrl Pts',(-1.52371651785714,4.45876623376623,
36.25));
#308419=CARTESIAN_POINT('Ctrl Pts',(1.86518364448052,6.24212662337662,36.05));
#308420=CARTESIAN_POINT('Ctrl Pts',(1.86518364448052,6.24212662337662,36.29));
#308421=CARTESIAN_POINT('Ctrl Pts',(1.88508836452757,6.23407454786033,36.05));
#308422=CARTESIAN_POINT('Ctrl Pts',(1.88508836452757,6.23407454786033,36.29));
#308423=CARTESIAN_POINT('Ctrl Pts',(1.92450419092778,6.21812962575333,36.05));
#308424=CARTESIAN_POINT('Ctrl Pts',(1.92450419092778,6.21812962575333,36.29));
#308425=CARTESIAN_POINT('Ctrl Pts',(1.98032242249028,6.18887731351974,36.05));
#308426=CARTESIAN_POINT('Ctrl Pts',(1.98032242249028,6.18887731351974,36.29));
#308427=CARTESIAN_POINT('Ctrl Pts',(2.03298084769892,6.1568243528457,36.05));
#308428=CARTESIAN_POINT('Ctrl Pts',(2.03298084769892,6.1568243528457,36.29));
#308429=CARTESIAN_POINT('Ctrl Pts',(2.08131772978725,6.12033427680283,36.05));
#308430=CARTESIAN_POINT('Ctrl Pts',(2.08131772978725,6.12033427680283,36.29));
#308431=CARTESIAN_POINT('Ctrl Pts',(2.1267784920286,6.08096773911451,36.05));
#308432=CARTESIAN_POINT('Ctrl Pts',(2.1267784920286,6.08096773911451,36.29));
#308433=CARTESIAN_POINT('Ctrl Pts',(2.16876575254244,6.03778353402304,36.05));
#308434=CARTESIAN_POINT('Ctrl Pts',(2.16876575254244,6.03778353402304,36.29));
#308435=CARTESIAN_POINT('Ctrl Pts',(2.20676901424551,5.99064810748104,36.05));
#308436=CARTESIAN_POINT('Ctrl Pts',(2.20676901424551,5.99064810748104,36.29));
#308437=CARTESIAN_POINT('Ctrl Pts',(2.24084931578957,5.94000771696759,36.05));
#308438=CARTESIAN_POINT('Ctrl Pts',(2.24084931578957,5.94000771696759,36.29));
#308439=CARTESIAN_POINT('Ctrl Pts',(2.27230135351232,5.88660676946342,36.05));
#308440=CARTESIAN_POINT('Ctrl Pts',(2.27230135351232,5.88660676946342,36.29));
#308441=CARTESIAN_POINT('Ctrl Pts',(2.2981681398483,5.82909896870107,36.05));
#308442=CARTESIAN_POINT('Ctrl Pts',(2.2981681398483,5.82909896870107,36.29));
#308443=CARTESIAN_POINT('Ctrl Pts',(2.32116828112027,5.76902496530642,36.05));
#308444=CARTESIAN_POINT('Ctrl Pts',(2.32116828112027,5.76902496530642,36.29));
#308445=CARTESIAN_POINT('Ctrl Pts',(2.33892894507894,5.70553707456913,36.05));
#308446=CARTESIAN_POINT('Ctrl Pts',(2.33892894507894,5.70553707456913,36.29));
#308447=CARTESIAN_POINT('Ctrl Pts',(2.35316409315178,5.63904690448481,36.05));
#308448=CARTESIAN_POINT('Ctrl Pts',(2.35316409315178,5.63904690448481,36.29));
#308449=CARTESIAN_POINT('Ctrl Pts',(2.3632377280083,5.56952358146944,36.05));
#308450=CARTESIAN_POINT('Ctrl Pts',(2.3632377280083,5.56952358146944,36.29));
#308451=CARTESIAN_POINT('Ctrl Pts',(2.3700963416033,5.4968345485113,36.05));
#308452=CARTESIAN_POINT('Ctrl Pts',(2.3700963416033,5.4968345485113,36.29));
#308453=CARTESIAN_POINT('Ctrl Pts',(2.37065529854562,5.44731949788714,36.05));
#308454=CARTESIAN_POINT('Ctrl Pts',(2.37065529854562,5.44731949788714,36.29));
#308455=CARTESIAN_POINT('Ctrl Pts',(2.37094155844156,5.42196124188312,36.05));
#308456=CARTESIAN_POINT('Ctrl Pts',(2.37094155844156,5.42196124188312,36.29));
#308457=CARTESIAN_POINT('',(1.86518364448052,6.24212662337662,36.25));
#308458=CARTESIAN_POINT('',(1.86518364448052,6.24212662337662,32.1799631621335));
#308459=CARTESIAN_POINT('',(2.37094155844156,5.42196124188312,36.25));
#308460=CARTESIAN_POINT('',(2.37094155844156,5.42196124188312,32.1799631621335));
#308461=CARTESIAN_POINT('Ctrl Pts',(1.86518364448052,6.24212662337662,36.25));
#308462=CARTESIAN_POINT('Ctrl Pts',(1.88508836452757,6.23407454786033,36.25));
#308463=CARTESIAN_POINT('Ctrl Pts',(1.92450419092778,6.21812962575333,36.25));
#308464=CARTESIAN_POINT('Ctrl Pts',(1.98032242249028,6.18887731351974,36.25));
#308465=CARTESIAN_POINT('Ctrl Pts',(2.03298084769892,6.1568243528457,36.25));
#308466=CARTESIAN_POINT('Ctrl Pts',(2.08131772978725,6.12033427680283,36.25));
#308467=CARTESIAN_POINT('Ctrl Pts',(2.1267784920286,6.08096773911451,36.25));
#308468=CARTESIAN_POINT('Ctrl Pts',(2.16876575254244,6.03778353402304,36.25));
#308469=CARTESIAN_POINT('Ctrl Pts',(2.20676901424551,5.99064810748104,36.25));
#308470=CARTESIAN_POINT('Ctrl Pts',(2.24084931578957,5.94000771696759,36.25));
#308471=CARTESIAN_POINT('Ctrl Pts',(2.27230135351232,5.88660676946342,36.25));
#308472=CARTESIAN_POINT('Ctrl Pts',(2.2981681398483,5.82909896870107,36.25));
#308473=CARTESIAN_POINT('Ctrl Pts',(2.32116828112027,5.76902496530642,36.25));
#308474=CARTESIAN_POINT('Ctrl Pts',(2.33892894507894,5.70553707456913,36.25));
#308475=CARTESIAN_POINT('Ctrl Pts',(2.35316409315178,5.63904690448481,36.25));
#308476=CARTESIAN_POINT('Ctrl Pts',(2.3632377280083,5.56952358146944,36.25));
#308477=CARTESIAN_POINT('Ctrl Pts',(2.3700963416033,5.4968345485113,36.25));
#308478=CARTESIAN_POINT('Ctrl Pts',(2.37065529854562,5.44731949788714,36.25));
#308479=CARTESIAN_POINT('Ctrl Pts',(2.37094155844156,5.42196124188312,36.25));
#308480=CARTESIAN_POINT('Ctrl Pts',(2.24724025974026,6.88253855519481,36.05));
#308481=CARTESIAN_POINT('Ctrl Pts',(2.24724025974026,6.88253855519481,36.29));
#308482=CARTESIAN_POINT('Ctrl Pts',(2.24629873402623,6.8452978442089,36.05));
#308483=CARTESIAN_POINT('Ctrl Pts',(2.24629873402623,6.8452978442089,36.29));
#308484=CARTESIAN_POINT('Ctrl Pts',(2.24448509897141,6.77356208818653,36.05));
#308485=CARTESIAN_POINT('Ctrl Pts',(2.24448509897141,6.77356208818653,36.29));
#308486=CARTESIAN_POINT('Ctrl Pts',(2.22577944098905,6.6705401244345,36.05));
#308487=CARTESIAN_POINT('Ctrl Pts',(2.22577944098905,6.6705401244345,36.29));
#308488=CARTESIAN_POINT('Ctrl Pts',(2.19665909049132,6.57608978278239,36.05));
#308489=CARTESIAN_POINT('Ctrl Pts',(2.19665909049132,6.57608978278239,36.29));
#308490=CARTESIAN_POINT('Ctrl Pts',(2.15426047894085,6.4907436496301,36.05));
#308491=CARTESIAN_POINT('Ctrl Pts',(2.15426047894085,6.4907436496301,36.29));
#308492=CARTESIAN_POINT('Ctrl Pts',(2.10006334842617,6.41405772296989,36.05));
#308493=CARTESIAN_POINT('Ctrl Pts',(2.10006334842617,6.41405772296989,36.29));
#308494=CARTESIAN_POINT('Ctrl Pts',(2.0335051920771,6.34678274879809,36.05));
#308495=CARTESIAN_POINT('Ctrl Pts',(2.0335051920771,6.34678274879809,36.29));
#308496=CARTESIAN_POINT('Ctrl Pts',(1.95525430031729,6.28741747621295,36.05));
#308497=CARTESIAN_POINT('Ctrl Pts',(1.95525430031729,6.28741747621295,36.29));
#308498=CARTESIAN_POINT('Ctrl Pts',(1.89580295974203,6.25752314612396,36.05));
#308499=CARTESIAN_POINT('Ctrl Pts',(1.89580295974203,6.25752314612396,36.29));
#308500=CARTESIAN_POINT('Ctrl Pts',(1.86518364448052,6.24212662337662,36.05));
#308501=CARTESIAN_POINT('Ctrl Pts',(1.86518364448052,6.24212662337662,36.29));
#308502=CARTESIAN_POINT('',(2.24724025974026,6.88253855519481,36.25));
#308503=CARTESIAN_POINT('',(2.24724025974026,6.88253855519481,32.1799631621335));
#308504=CARTESIAN_POINT('Ctrl Pts',(2.24724025974026,6.88253855519481,36.25));
#308505=CARTESIAN_POINT('Ctrl Pts',(2.24629873402623,6.8452978442089,36.25));
#308506=CARTESIAN_POINT('Ctrl Pts',(2.24448509897141,6.77356208818653,36.25));
#308507=CARTESIAN_POINT('Ctrl Pts',(2.22577944098905,6.6705401244345,36.25));
#308508=CARTESIAN_POINT('Ctrl Pts',(2.19665909049132,6.57608978278239,36.25));
#308509=CARTESIAN_POINT('Ctrl Pts',(2.15426047894085,6.4907436496301,36.25));
#308510=CARTESIAN_POINT('Ctrl Pts',(2.10006334842617,6.41405772296989,36.25));
#308511=CARTESIAN_POINT('Ctrl Pts',(2.0335051920771,6.34678274879809,36.25));
#308512=CARTESIAN_POINT('Ctrl Pts',(1.95525430031729,6.28741747621295,36.25));
#308513=CARTESIAN_POINT('Ctrl Pts',(1.89580295974203,6.25752314612396,36.25));
#308514=CARTESIAN_POINT('Ctrl Pts',(1.86518364448052,6.24212662337662,36.25));
#308515=CARTESIAN_POINT('Ctrl Pts',(1.52242796266234,7.71623376623377,36.05));
#308516=CARTESIAN_POINT('Ctrl Pts',(1.52242796266234,7.71623376623377,36.29));
#308517=CARTESIAN_POINT('Ctrl Pts',(1.54780821610109,7.71545767890599,36.05));
#308518=CARTESIAN_POINT('Ctrl Pts',(1.54780821610109,7.71545767890599,36.29));
#308519=CARTESIAN_POINT('Ctrl Pts',(1.59794752226823,7.71392449956901,36.05));
#308520=CARTESIAN_POINT('Ctrl Pts',(1.59794752226823,7.71392449956901,36.29));
#308521=CARTESIAN_POINT('Ctrl Pts',(1.67138411132394,7.7027904588233,36.05));
#308522=CARTESIAN_POINT('Ctrl Pts',(1.67138411132394,7.7027904588233,36.29));
#308523=CARTESIAN_POINT('Ctrl Pts',(1.74156530298064,7.68468886160549,36.05));
#308524=CARTESIAN_POINT('Ctrl Pts',(1.74156530298064,7.68468886160549,36.29));
#308525=CARTESIAN_POINT('Ctrl Pts',(1.80849182787228,7.65953041457979,36.05));
#308526=CARTESIAN_POINT('Ctrl Pts',(1.80849182787228,7.65953041457979,36.29));
#308527=CARTESIAN_POINT('Ctrl Pts',(1.87205683321845,7.62639783586101,36.05));
#308528=CARTESIAN_POINT('Ctrl Pts',(1.87205683321845,7.62639783586101,36.29));
#308529=CARTESIAN_POINT('Ctrl Pts',(1.9318511217457,7.58560597597768,36.05));
#308530=CARTESIAN_POINT('Ctrl Pts',(1.9318511217457,7.58560597597768,36.29));
#308531=CARTESIAN_POINT('Ctrl Pts',(1.98861539009419,7.53791001729144,36.05));
#308532=CARTESIAN_POINT('Ctrl Pts',(1.98861539009419,7.53791001729144,36.29));
#308533=CARTESIAN_POINT('Ctrl Pts',(2.04159249935513,7.48362087256877,36.05));
#308534=CARTESIAN_POINT('Ctrl Pts',(2.04159249935513,7.48362087256877,36.29));
#308535=CARTESIAN_POINT('Ctrl Pts',(2.08967670240967,7.42336185115535,36.05));
#308536=CARTESIAN_POINT('Ctrl Pts',(2.08967670240967,7.42336185115535,36.29));
#308537=CARTESIAN_POINT('Ctrl Pts',(2.1315901628391,7.35843862911193,36.05));
#308538=CARTESIAN_POINT('Ctrl Pts',(2.1315901628391,7.35843862911193,36.29));
#308539=CARTESIAN_POINT('Ctrl Pts',(2.16825091485445,7.29002627559583,36.05));
#308540=CARTESIAN_POINT('Ctrl Pts',(2.16825091485445,7.29002627559583,36.29));
#308541=CARTESIAN_POINT('Ctrl Pts',(2.19706966642109,7.21661236790923,36.05));
#308542=CARTESIAN_POINT('Ctrl Pts',(2.19706966642109,7.21661236790923,36.29));
#308543=CARTESIAN_POINT('Ctrl Pts',(2.21970139767277,7.13897358699381,36.05));
#308544=CARTESIAN_POINT('Ctrl Pts',(2.21970139767277,7.13897358699381,36.29));
#308545=CARTESIAN_POINT('Ctrl Pts',(2.23556552441298,7.05701575208482,36.05));
#308546=CARTESIAN_POINT('Ctrl Pts',(2.23556552441298,7.05701575208482,36.29));
#308547=CARTESIAN_POINT('Ctrl Pts',(2.24548752990423,6.97104879536392,36.05));
#308548=CARTESIAN_POINT('Ctrl Pts',(2.24548752990423,6.97104879536392,36.29));
#308549=CARTESIAN_POINT('Ctrl Pts',(2.2466485766986,6.91241766550898,36.05));
#308550=CARTESIAN_POINT('Ctrl Pts',(2.2466485766986,6.91241766550898,36.29));
#308551=CARTESIAN_POINT('Ctrl Pts',(2.24724025974026,6.88253855519481,36.05));
#308552=CARTESIAN_POINT('Ctrl Pts',(2.24724025974026,6.88253855519481,36.29));
#308553=CARTESIAN_POINT('',(1.52242796266234,7.71623376623377,36.25));
#308554=CARTESIAN_POINT('',(1.52242796266234,7.71623376623377,32.1799631621335));
#308555=CARTESIAN_POINT('Ctrl Pts',(1.52242796266234,7.71623376623377,36.25));
#308556=CARTESIAN_POINT('Ctrl Pts',(1.54780821610109,7.71545767890599,36.25));
#308557=CARTESIAN_POINT('Ctrl Pts',(1.59794752226823,7.71392449956901,36.25));
#308558=CARTESIAN_POINT('Ctrl Pts',(1.67138411132394,7.7027904588233,36.25));
#308559=CARTESIAN_POINT('Ctrl Pts',(1.74156530298064,7.68468886160549,36.25));
#308560=CARTESIAN_POINT('Ctrl Pts',(1.80849182787228,7.65953041457979,36.25));
#308561=CARTESIAN_POINT('Ctrl Pts',(1.87205683321845,7.62639783586101,36.25));
#308562=CARTESIAN_POINT('Ctrl Pts',(1.9318511217457,7.58560597597768,36.25));
#308563=CARTESIAN_POINT('Ctrl Pts',(1.98861539009419,7.53791001729144,36.25));
#308564=CARTESIAN_POINT('Ctrl Pts',(2.04159249935513,7.48362087256877,36.25));
#308565=CARTESIAN_POINT('Ctrl Pts',(2.08967670240967,7.42336185115535,36.25));
#308566=CARTESIAN_POINT('Ctrl Pts',(2.1315901628391,7.35843862911193,36.25));
#308567=CARTESIAN_POINT('Ctrl Pts',(2.16825091485445,7.29002627559583,36.25));
#308568=CARTESIAN_POINT('Ctrl Pts',(2.19706966642109,7.21661236790923,36.25));
#308569=CARTESIAN_POINT('Ctrl Pts',(2.21970139767277,7.13897358699381,36.25));
#308570=CARTESIAN_POINT('Ctrl Pts',(2.23556552441298,7.05701575208482,36.25));
#308571=CARTESIAN_POINT('Ctrl Pts',(2.24548752990423,6.97104879536392,36.25));
#308572=CARTESIAN_POINT('Ctrl Pts',(2.2466485766986,6.91241766550898,36.25));
#308573=CARTESIAN_POINT('Ctrl Pts',(2.24724025974026,6.88253855519481,36.25));
#308574=CARTESIAN_POINT('Ctrl Pts',(0.804058441558442,6.89542410714286,
36.05));
#308575=CARTESIAN_POINT('Ctrl Pts',(0.804058441558442,6.89542410714286,
36.29));
#308576=CARTESIAN_POINT('Ctrl Pts',(0.804649087710329,6.92508712200564,
36.05));
#308577=CARTESIAN_POINT('Ctrl Pts',(0.804649087710329,6.92508712200564,
36.29));
#308578=CARTESIAN_POINT('Ctrl Pts',(0.805803713282925,6.98307391394772,
36.05));
#308579=CARTESIAN_POINT('Ctrl Pts',(0.805803713282925,6.98307391394772,
36.29));
#308580=CARTESIAN_POINT('Ctrl Pts',(0.815658223082562,7.06800054423278,
36.05));
#308581=CARTESIAN_POINT('Ctrl Pts',(0.815658223082562,7.06800054423278,
36.29));
#308582=CARTESIAN_POINT('Ctrl Pts',(0.831843276752908,7.1485092997012,36.05));
#308583=CARTESIAN_POINT('Ctrl Pts',(0.831843276752908,7.1485092997012,36.29));
#308584=CARTESIAN_POINT('Ctrl Pts',(0.853271048234912,7.22519194306317,
36.05));
#308585=CARTESIAN_POINT('Ctrl Pts',(0.853271048234912,7.22519194306317,
36.29));
#308586=CARTESIAN_POINT('Ctrl Pts',(0.882914981130102,7.29688183752562,
36.05));
#308587=CARTESIAN_POINT('Ctrl Pts',(0.882914981130102,7.29688183752562,
36.29));
#308588=CARTESIAN_POINT('Ctrl Pts',(0.917480029442785,7.36527391878087,
36.05));
#308589=CARTESIAN_POINT('Ctrl Pts',(0.917480029442785,7.36527391878087,
36.29));
#308590=CARTESIAN_POINT('Ctrl Pts',(0.959667248194858,7.42884662646377,
36.05));
#308591=CARTESIAN_POINT('Ctrl Pts',(0.959667248194858,7.42884662646377,
36.29));
#308592=CARTESIAN_POINT('Ctrl Pts',(1.00709172396245,7.48817807892744,36.05));
#308593=CARTESIAN_POINT('Ctrl Pts',(1.00709172396245,7.48817807892744,36.29));
#308594=CARTESIAN_POINT('Ctrl Pts',(1.05972365886402,7.54133429965824,36.05));
#308595=CARTESIAN_POINT('Ctrl Pts',(1.05972365886402,7.54133429965824,36.29));
#308596=CARTESIAN_POINT('Ctrl Pts',(1.11597817292345,7.58805917500155,36.05));
#308597=CARTESIAN_POINT('Ctrl Pts',(1.11597817292345,7.58805917500155,36.29));
#308598=CARTESIAN_POINT('Ctrl Pts',(1.17567437498645,7.62785439831755,36.05));
#308599=CARTESIAN_POINT('Ctrl Pts',(1.17567437498645,7.62785439831755,36.29));
#308600=CARTESIAN_POINT('Ctrl Pts',(1.23894018265463,7.65993643724945,36.05));
#308601=CARTESIAN_POINT('Ctrl Pts',(1.23894018265463,7.65993643724945,36.29));
#308602=CARTESIAN_POINT('Ctrl Pts',(1.3051937479367,7.68533220871074,36.05));
#308603=CARTESIAN_POINT('Ctrl Pts',(1.3051937479367,7.68533220871074,36.29));
#308604=CARTESIAN_POINT('Ctrl Pts',(1.37469868549749,7.7036309678914,36.05));
#308605=CARTESIAN_POINT('Ctrl Pts',(1.37469868549749,7.7036309678914,36.29));
#308606=CARTESIAN_POINT('Ctrl Pts',(1.44761088404003,7.71370952681349,36.05));
#308607=CARTESIAN_POINT('Ctrl Pts',(1.44761088404003,7.71370952681349,36.29));
#308608=CARTESIAN_POINT('Ctrl Pts',(1.49727230748502,7.71538504428939,36.05));
#308609=CARTESIAN_POINT('Ctrl Pts',(1.49727230748502,7.71538504428939,36.29));
#308610=CARTESIAN_POINT('Ctrl Pts',(1.52242796266234,7.71623376623377,36.05));
#308611=CARTESIAN_POINT('Ctrl Pts',(1.52242796266234,7.71623376623377,36.29));
#308612=CARTESIAN_POINT('',(0.804058441558442,6.89542410714286,36.25));
#308613=CARTESIAN_POINT('',(0.804058441558442,6.89542410714286,32.1799631621335));
#308614=CARTESIAN_POINT('Ctrl Pts',(0.804058441558442,6.89542410714286,
36.25));
#308615=CARTESIAN_POINT('Ctrl Pts',(0.804649087710329,6.92508712200564,
36.25));
#308616=CARTESIAN_POINT('Ctrl Pts',(0.805803713282925,6.98307391394772,
36.25));
#308617=CARTESIAN_POINT('Ctrl Pts',(0.815658223082562,7.06800054423278,
36.25));
#308618=CARTESIAN_POINT('Ctrl Pts',(0.831843276752908,7.1485092997012,36.25));
#308619=CARTESIAN_POINT('Ctrl Pts',(0.853271048234912,7.22519194306317,
36.25));
#308620=CARTESIAN_POINT('Ctrl Pts',(0.882914981130102,7.29688183752562,
36.25));
#308621=CARTESIAN_POINT('Ctrl Pts',(0.917480029442785,7.36527391878087,
36.25));
#308622=CARTESIAN_POINT('Ctrl Pts',(0.959667248194858,7.42884662646377,
36.25));
#308623=CARTESIAN_POINT('Ctrl Pts',(1.00709172396245,7.48817807892744,36.25));
#308624=CARTESIAN_POINT('Ctrl Pts',(1.05972365886402,7.54133429965824,36.25));
#308625=CARTESIAN_POINT('Ctrl Pts',(1.11597817292345,7.58805917500155,36.25));
#308626=CARTESIAN_POINT('Ctrl Pts',(1.17567437498645,7.62785439831755,36.25));
#308627=CARTESIAN_POINT('Ctrl Pts',(1.23894018265463,7.65993643724945,36.25));
#308628=CARTESIAN_POINT('Ctrl Pts',(1.3051937479367,7.68533220871074,36.25));
#308629=CARTESIAN_POINT('Ctrl Pts',(1.37469868549749,7.7036309678914,36.25));
#308630=CARTESIAN_POINT('Ctrl Pts',(1.44761088404003,7.71370952681349,36.25));
#308631=CARTESIAN_POINT('Ctrl Pts',(1.49727230748502,7.71538504428939,36.25));
#308632=CARTESIAN_POINT('Ctrl Pts',(1.52242796266234,7.71623376623377,36.25));
#308633=CARTESIAN_POINT('Ctrl Pts',(1.1899807224026,6.24212662337662,36.05));
#308634=CARTESIAN_POINT('Ctrl Pts',(1.1899807224026,6.24212662337662,36.29));
#308635=CARTESIAN_POINT('Ctrl Pts',(1.15962955866533,6.25737900558172,36.05));
#308636=CARTESIAN_POINT('Ctrl Pts',(1.15962955866533,6.25737900558172,36.29));
#308637=CARTESIAN_POINT('Ctrl Pts',(1.10041391837872,6.28713666449684,36.05));
#308638=CARTESIAN_POINT('Ctrl Pts',(1.10041391837872,6.28713666449684,36.29));
#308639=CARTESIAN_POINT('Ctrl Pts',(1.02148620395913,6.34542328474194,36.05));
#308640=CARTESIAN_POINT('Ctrl Pts',(1.02148620395913,6.34542328474194,36.29));
#308641=CARTESIAN_POINT('Ctrl Pts',(0.954184014070375,6.41311300974787,
36.05));
#308642=CARTESIAN_POINT('Ctrl Pts',(0.954184014070375,6.41311300974787,
36.29));
#308643=CARTESIAN_POINT('Ctrl Pts',(0.898744629741027,6.49069341485485,
36.05));
#308644=CARTESIAN_POINT('Ctrl Pts',(0.898744629741027,6.49069341485485,
36.29));
#308645=CARTESIAN_POINT('Ctrl Pts',(0.855851150387493,6.57824013430206,
36.05));
#308646=CARTESIAN_POINT('Ctrl Pts',(0.855851150387493,6.57824013430206,
36.29));
#308647=CARTESIAN_POINT('Ctrl Pts',(0.82602871283696,6.67544579213543,36.05));
#308648=CARTESIAN_POINT('Ctrl Pts',(0.82602871283696,6.67544579213543,36.29));
#308649=CARTESIAN_POINT('Ctrl Pts',(0.806637417607563,6.78212192154818,
36.05));
#308650=CARTESIAN_POINT('Ctrl Pts',(0.806637417607563,6.78212192154818,
36.29));
#308651=CARTESIAN_POINT('Ctrl Pts',(0.804940416665592,6.85667628421743,
36.05));
#308652=CARTESIAN_POINT('Ctrl Pts',(0.804940416665592,6.85667628421743,
36.29));
#308653=CARTESIAN_POINT('Ctrl Pts',(0.804058441558442,6.89542410714286,
36.05));
#308654=CARTESIAN_POINT('Ctrl Pts',(0.804058441558442,6.89542410714286,
36.29));
#308655=CARTESIAN_POINT('',(1.1899807224026,6.24212662337662,36.25));
#308656=CARTESIAN_POINT('',(1.1899807224026,6.24212662337662,32.1799631621335));
#308657=CARTESIAN_POINT('Ctrl Pts',(1.1899807224026,6.24212662337662,36.25));
#308658=CARTESIAN_POINT('Ctrl Pts',(1.15962955866533,6.25737900558172,36.25));
#308659=CARTESIAN_POINT('Ctrl Pts',(1.10041391837872,6.28713666449684,36.25));
#308660=CARTESIAN_POINT('Ctrl Pts',(1.02148620395913,6.34542328474194,36.25));
#308661=CARTESIAN_POINT('Ctrl Pts',(0.954184014070375,6.41311300974787,
36.25));
#308662=CARTESIAN_POINT('Ctrl Pts',(0.898744629741027,6.49069341485485,
36.25));
#308663=CARTESIAN_POINT('Ctrl Pts',(0.855851150387493,6.57824013430206,
36.25));
#308664=CARTESIAN_POINT('Ctrl Pts',(0.82602871283696,6.67544579213543,36.25));
#308665=CARTESIAN_POINT('Ctrl Pts',(0.806637417607563,6.78212192154818,
36.25));
#308666=CARTESIAN_POINT('Ctrl Pts',(0.804940416665592,6.85667628421743,
36.25));
#308667=CARTESIAN_POINT('Ctrl Pts',(0.804058441558442,6.89542410714286,
36.25));
#308668=CARTESIAN_POINT('Ctrl Pts',(0.680357142857143,5.43291396103896,
36.05));
#308669=CARTESIAN_POINT('Ctrl Pts',(0.680357142857143,5.43291396103896,
36.29));
#308670=CARTESIAN_POINT('Ctrl Pts',(0.680668693953829,5.45891313799848,
36.05));
#308671=CARTESIAN_POINT('Ctrl Pts',(0.680668693953829,5.45891313799848,
36.29));
#308672=CARTESIAN_POINT('Ctrl Pts',(0.681279937811019,5.50992190470655,
36.05));
#308673=CARTESIAN_POINT('Ctrl Pts',(0.681279937811019,5.50992190470655,
36.29));
#308674=CARTESIAN_POINT('Ctrl Pts',(0.687839327233214,5.58482539360676,
36.05));
#308675=CARTESIAN_POINT('Ctrl Pts',(0.687839327233214,5.58482539360676,
36.29));
#308676=CARTESIAN_POINT('Ctrl Pts',(0.698772843207189,5.65624108672131,
36.05));
#308677=CARTESIAN_POINT('Ctrl Pts',(0.698772843207189,5.65624108672131,
36.29));
#308678=CARTESIAN_POINT('Ctrl Pts',(0.713532253106825,5.72405509656199,
36.05));
#308679=CARTESIAN_POINT('Ctrl Pts',(0.713532253106825,5.72405509656199,
36.29));
#308680=CARTESIAN_POINT('Ctrl Pts',(0.732151313294084,5.78833295550162,
36.05));
#308681=CARTESIAN_POINT('Ctrl Pts',(0.732151313294084,5.78833295550162,
36.29));
#308682=CARTESIAN_POINT('Ctrl Pts',(0.755394491764458,5.84911895337204,
36.05));
#308683=CARTESIAN_POINT('Ctrl Pts',(0.755394491764458,5.84911895337204,
36.29));
#308684=CARTESIAN_POINT('Ctrl Pts',(0.783058181337012,5.90641132135784,
36.05));
#308685=CARTESIAN_POINT('Ctrl Pts',(0.783058181337012,5.90641132135784,
36.29));
#308686=CARTESIAN_POINT('Ctrl Pts',(0.814867866880491,5.96019951630268,
36.05));
#308687=CARTESIAN_POINT('Ctrl Pts',(0.814867866880491,5.96019951630268,
36.29));
#308688=CARTESIAN_POINT('Ctrl Pts',(0.850057380368458,6.01030469320115,
36.05));
#308689=CARTESIAN_POINT('Ctrl Pts',(0.850057380368458,6.01030469320115,
36.29));
#308690=CARTESIAN_POINT('Ctrl Pts',(0.888809448167726,6.05629105732706,
36.05));
#308691=CARTESIAN_POINT('Ctrl Pts',(0.888809448167726,6.05629105732706,
36.29));
#308692=CARTESIAN_POINT('Ctrl Pts',(0.931020421596495,6.09774166415628,
36.05));
#308693=CARTESIAN_POINT('Ctrl Pts',(0.931020421596495,6.09774166415628,
36.29));
#308694=CARTESIAN_POINT('Ctrl Pts',(0.976304255584941,6.1351992195304,36.05));
#308695=CARTESIAN_POINT('Ctrl Pts',(0.976304255584941,6.1351992195304,36.29));
#308696=CARTESIAN_POINT('Ctrl Pts',(1.02473287123688,6.16910978501208,36.05));
#308697=CARTESIAN_POINT('Ctrl Pts',(1.02473287123688,6.16910978501208,36.29));
#308698=CARTESIAN_POINT('Ctrl Pts',(1.07696907224526,6.19776979492405,36.05));
#308699=CARTESIAN_POINT('Ctrl Pts',(1.07696907224526,6.19776979492405,36.29));
#308700=CARTESIAN_POINT('Ctrl Pts',(1.13212158876422,6.22263196745495,36.05));
#308701=CARTESIAN_POINT('Ctrl Pts',(1.13212158876422,6.22263196745495,36.29));
#308702=CARTESIAN_POINT('Ctrl Pts',(1.17053061939841,6.23557324032603,36.05));
#308703=CARTESIAN_POINT('Ctrl Pts',(1.17053061939841,6.23557324032603,36.29));
#308704=CARTESIAN_POINT('Ctrl Pts',(1.1899807224026,6.24212662337662,36.05));
#308705=CARTESIAN_POINT('Ctrl Pts',(1.1899807224026,6.24212662337662,36.29));
#308706=CARTESIAN_POINT('',(0.680357142857143,5.43291396103896,36.25));
#308707=CARTESIAN_POINT('',(0.680357142857143,5.43291396103896,32.1799631621335));
#308708=CARTESIAN_POINT('Ctrl Pts',(0.680357142857143,5.43291396103896,
36.25));
#308709=CARTESIAN_POINT('Ctrl Pts',(0.680668693953829,5.45891313799848,
36.25));
#308710=CARTESIAN_POINT('Ctrl Pts',(0.681279937811019,5.50992190470655,
36.25));
#308711=CARTESIAN_POINT('Ctrl Pts',(0.687839327233214,5.58482539360676,
36.25));
#308712=CARTESIAN_POINT('Ctrl Pts',(0.698772843207189,5.65624108672131,
36.25));
#308713=CARTESIAN_POINT('Ctrl Pts',(0.713532253106825,5.72405509656199,
36.25));
#308714=CARTESIAN_POINT('Ctrl Pts',(0.732151313294084,5.78833295550162,
36.25));
#308715=CARTESIAN_POINT('Ctrl Pts',(0.755394491764458,5.84911895337204,
36.25));
#308716=CARTESIAN_POINT('Ctrl Pts',(0.783058181337012,5.90641132135784,
36.25));
#308717=CARTESIAN_POINT('Ctrl Pts',(0.814867866880491,5.96019951630268,
36.25));
#308718=CARTESIAN_POINT('Ctrl Pts',(0.850057380368458,6.01030469320115,
36.25));
#308719=CARTESIAN_POINT('Ctrl Pts',(0.888809448167726,6.05629105732706,
36.25));
#308720=CARTESIAN_POINT('Ctrl Pts',(0.931020421596495,6.09774166415628,
36.25));
#308721=CARTESIAN_POINT('Ctrl Pts',(0.976304255584941,6.1351992195304,36.25));
#308722=CARTESIAN_POINT('Ctrl Pts',(1.02473287123688,6.16910978501208,36.25));
#308723=CARTESIAN_POINT('Ctrl Pts',(1.07696907224526,6.19776979492405,36.25));
#308724=CARTESIAN_POINT('Ctrl Pts',(1.13212158876422,6.22263196745495,36.25));
#308725=CARTESIAN_POINT('Ctrl Pts',(1.17053061939841,6.23557324032603,36.25));
#308726=CARTESIAN_POINT('Ctrl Pts',(1.1899807224026,6.24212662337662,36.25));
#308727=CARTESIAN_POINT('Ctrl Pts',(1.52758218344156,4.45876623376623,36.05));
#308728=CARTESIAN_POINT('Ctrl Pts',(1.52758218344156,4.45876623376623,36.29));
#308729=CARTESIAN_POINT('Ctrl Pts',(1.49790947590789,4.4597253240939,36.05));
#308730=CARTESIAN_POINT('Ctrl Pts',(1.49790947590789,4.4597253240939,36.29));
#308731=CARTESIAN_POINT('Ctrl Pts',(1.43959848220332,4.46161006986558,36.05));
#308732=CARTESIAN_POINT('Ctrl Pts',(1.43959848220332,4.46161006986558,36.29));
#308733=CARTESIAN_POINT('Ctrl Pts',(1.35393326291226,4.47372823681752,36.05));
#308734=CARTESIAN_POINT('Ctrl Pts',(1.35393326291226,4.47372823681752,36.29));
#308735=CARTESIAN_POINT('Ctrl Pts',(1.27247800686959,4.49538915943629,36.05));
#308736=CARTESIAN_POINT('Ctrl Pts',(1.27247800686959,4.49538915943629,36.29));
#308737=CARTESIAN_POINT('Ctrl Pts',(1.19426688731232,4.52434515927101,36.05));
#308738=CARTESIAN_POINT('Ctrl Pts',(1.19426688731232,4.52434515927101,36.29));
#308739=CARTESIAN_POINT('Ctrl Pts',(1.12007772580205,4.56241550483758,36.05));
#308740=CARTESIAN_POINT('Ctrl Pts',(1.12007772580205,4.56241550483758,36.29));
#308741=CARTESIAN_POINT('Ctrl Pts',(1.05020719586857,4.60959489382439,36.05));
#308742=CARTESIAN_POINT('Ctrl Pts',(1.05020719586857,4.60959489382439,36.29));
#308743=CARTESIAN_POINT('Ctrl Pts',(0.983166501449546,4.66375358613811,
36.05));
#308744=CARTESIAN_POINT('Ctrl Pts',(0.983166501449546,4.66375358613811,
36.29));
#308745=CARTESIAN_POINT('Ctrl Pts',(0.921454901216499,4.72680658155488,
36.05));
#308746=CARTESIAN_POINT('Ctrl Pts',(0.921454901216499,4.72680658155488,
36.29));
#308747=CARTESIAN_POINT('Ctrl Pts',(0.864436955628593,4.79599402074389,
36.05));
#308748=CARTESIAN_POINT('Ctrl Pts',(0.864436955628593,4.79599402074389,
36.29));
#308749=CARTESIAN_POINT('Ctrl Pts',(0.815819415600203,4.87186228483585,
36.05));
#308750=CARTESIAN_POINT('Ctrl Pts',(0.815819415600203,4.87186228483585,
36.29));
#308751=CARTESIAN_POINT('Ctrl Pts',(0.773237258753005,4.95218254596678,
36.05));
#308752=CARTESIAN_POINT('Ctrl Pts',(0.773237258753005,4.95218254596678,
36.29));
#308753=CARTESIAN_POINT('Ctrl Pts',(0.739295500896744,5.03825698338498,
36.05));
#308754=CARTESIAN_POINT('Ctrl Pts',(0.739295500896744,5.03825698338498,
36.29));
#308755=CARTESIAN_POINT('Ctrl Pts',(0.712762470738981,5.12949961741785,
36.05));
#308756=CARTESIAN_POINT('Ctrl Pts',(0.712762470738981,5.12949961741785,
36.29));
#308757=CARTESIAN_POINT('Ctrl Pts',(0.694428924083107,5.22616336292247,
36.05));
#308758=CARTESIAN_POINT('Ctrl Pts',(0.694428924083107,5.22616336292247,
36.29));
#308759=CARTESIAN_POINT('Ctrl Pts',(0.682434422236949,5.32781045016027,
36.05));
#308760=CARTESIAN_POINT('Ctrl Pts',(0.682434422236949,5.32781045016027,
36.29));
#308761=CARTESIAN_POINT('Ctrl Pts',(0.681058184371366,5.39744356397404,
36.05));
#308762=CARTESIAN_POINT('Ctrl Pts',(0.681058184371366,5.39744356397404,
36.29));
#308763=CARTESIAN_POINT('Ctrl Pts',(0.680357142857143,5.43291396103896,
36.05));
#308764=CARTESIAN_POINT('Ctrl Pts',(0.680357142857143,5.43291396103896,
36.29));
#308765=CARTESIAN_POINT('',(1.52758218344156,4.45876623376623,36.25));
#308766=CARTESIAN_POINT('',(1.52758218344156,4.45876623376623,32.1799631621335));
#308767=CARTESIAN_POINT('Ctrl Pts',(1.52758218344156,4.45876623376623,36.25));
#308768=CARTESIAN_POINT('Ctrl Pts',(1.49790947590789,4.4597253240939,36.25));
#308769=CARTESIAN_POINT('Ctrl Pts',(1.43959848220332,4.46161006986558,36.25));
#308770=CARTESIAN_POINT('Ctrl Pts',(1.35393326291226,4.47372823681752,36.25));
#308771=CARTESIAN_POINT('Ctrl Pts',(1.27247800686959,4.49538915943629,36.25));
#308772=CARTESIAN_POINT('Ctrl Pts',(1.19426688731232,4.52434515927101,36.25));
#308773=CARTESIAN_POINT('Ctrl Pts',(1.12007772580205,4.56241550483758,36.25));
#308774=CARTESIAN_POINT('Ctrl Pts',(1.05020719586857,4.60959489382439,36.25));
#308775=CARTESIAN_POINT('Ctrl Pts',(0.983166501449546,4.66375358613811,
36.25));
#308776=CARTESIAN_POINT('Ctrl Pts',(0.921454901216499,4.72680658155488,
36.25));
#308777=CARTESIAN_POINT('Ctrl Pts',(0.864436955628593,4.79599402074389,
36.25));
#308778=CARTESIAN_POINT('Ctrl Pts',(0.815819415600203,4.87186228483585,
36.25));
#308779=CARTESIAN_POINT('Ctrl Pts',(0.773237258753005,4.95218254596678,
36.25));
#308780=CARTESIAN_POINT('Ctrl Pts',(0.739295500896744,5.03825698338498,
36.25));
#308781=CARTESIAN_POINT('Ctrl Pts',(0.712762470738981,5.12949961741785,
36.25));
#308782=CARTESIAN_POINT('Ctrl Pts',(0.694428924083107,5.22616336292247,
36.25));
#308783=CARTESIAN_POINT('Ctrl Pts',(0.682434422236949,5.32781045016027,
36.25));
#308784=CARTESIAN_POINT('Ctrl Pts',(0.681058184371366,5.39744356397404,
36.25));
#308785=CARTESIAN_POINT('Ctrl Pts',(0.680357142857143,5.43291396103896,
36.25));
#308786=CARTESIAN_POINT('Ctrl Pts',(2.37094155844156,5.42196124188312,36.05));
#308787=CARTESIAN_POINT('Ctrl Pts',(2.37094155844156,5.42196124188312,36.29));
#308788=CARTESIAN_POINT('Ctrl Pts',(2.3701449621061,5.3873620729942,36.05));
#308789=CARTESIAN_POINT('Ctrl Pts',(2.3701449621061,5.3873620729942,36.29));
#308790=CARTESIAN_POINT('Ctrl Pts',(2.36858230731467,5.31949010994648,36.05));
#308791=CARTESIAN_POINT('Ctrl Pts',(2.36858230731467,5.31949010994648,36.29));
#308792=CARTESIAN_POINT('Ctrl Pts',(2.35792489966522,5.21999888881734,36.05));
#308793=CARTESIAN_POINT('Ctrl Pts',(2.35792489966522,5.21999888881734,36.29));
#308794=CARTESIAN_POINT('Ctrl Pts',(2.33816283696992,5.12552781537341,36.05));
#308795=CARTESIAN_POINT('Ctrl Pts',(2.33816283696992,5.12552781537341,36.29));
#308796=CARTESIAN_POINT('Ctrl Pts',(2.31216804403568,5.03559649057185,36.05));
#308797=CARTESIAN_POINT('Ctrl Pts',(2.31216804403568,5.03559649057185,36.29));
#308798=CARTESIAN_POINT('Ctrl Pts',(2.27768357726726,4.95095791492866,36.05));
#308799=CARTESIAN_POINT('Ctrl Pts',(2.27768357726726,4.95095791492866,36.29));
#308800=CARTESIAN_POINT('Ctrl Pts',(2.23640375626704,4.87078209602146,36.05));
#308801=CARTESIAN_POINT('Ctrl Pts',(2.23640375626704,4.87078209602146,36.29));
#308802=CARTESIAN_POINT('Ctrl Pts',(2.18650804768952,4.79615096254107,36.05));
#308803=CARTESIAN_POINT('Ctrl Pts',(2.18650804768952,4.79615096254107,36.29));
#308804=CARTESIAN_POINT('Ctrl Pts',(2.12995256471625,4.72672058470318,36.05));
#308805=CARTESIAN_POINT('Ctrl Pts',(2.12995256471625,4.72672058470318,36.29));
#308806=CARTESIAN_POINT('Ctrl Pts',(2.06812897983805,4.66400945675856,36.05));
#308807=CARTESIAN_POINT('Ctrl Pts',(2.06812897983805,4.66400945675856,36.29));
#308808=CARTESIAN_POINT('Ctrl Pts',(2.00171131208806,4.60935645208091,36.05));
#308809=CARTESIAN_POINT('Ctrl Pts',(2.00171131208806,4.60935645208091,36.29));
#308810=CARTESIAN_POINT('Ctrl Pts',(1.93195013979453,4.56264762609262,36.05));
#308811=CARTESIAN_POINT('Ctrl Pts',(1.93195013979453,4.56264762609262,36.29));
#308812=CARTESIAN_POINT('Ctrl Pts',(1.85820350335783,4.5241565808727,36.05));
#308813=CARTESIAN_POINT('Ctrl Pts',(1.85820350335783,4.5241565808727,36.29));
#308814=CARTESIAN_POINT('Ctrl Pts',(1.78027605704376,4.49553589484458,36.05));
#308815=CARTESIAN_POINT('Ctrl Pts',(1.78027605704376,4.49553589484458,36.29));
#308816=CARTESIAN_POINT('Ctrl Pts',(1.69931628629545,4.47370190759594,36.05));
#308817=CARTESIAN_POINT('Ctrl Pts',(1.69931628629545,4.47370190759594,36.29));
#308818=CARTESIAN_POINT('Ctrl Pts',(1.61449027768335,4.46164864649648,36.05));
#308819=CARTESIAN_POINT('Ctrl Pts',(1.61449027768335,4.46164864649648,36.29));
#308820=CARTESIAN_POINT('Ctrl Pts',(1.55682420860062,4.45973608112409,36.05));
#308821=CARTESIAN_POINT('Ctrl Pts',(1.55682420860062,4.45973608112409,36.29));
#308822=CARTESIAN_POINT('Ctrl Pts',(1.52758218344156,4.45876623376623,36.05));
#308823=CARTESIAN_POINT('Ctrl Pts',(1.52758218344156,4.45876623376623,36.29));
#308824=CARTESIAN_POINT('Ctrl Pts',(2.37094155844156,5.42196124188312,36.25));
#308825=CARTESIAN_POINT('Ctrl Pts',(2.3701449621061,5.3873620729942,36.25));
#308826=CARTESIAN_POINT('Ctrl Pts',(2.36858230731467,5.31949010994648,36.25));
#308827=CARTESIAN_POINT('Ctrl Pts',(2.35792489966522,5.21999888881734,36.25));
#308828=CARTESIAN_POINT('Ctrl Pts',(2.33816283696992,5.12552781537341,36.25));
#308829=CARTESIAN_POINT('Ctrl Pts',(2.31216804403568,5.03559649057185,36.25));
#308830=CARTESIAN_POINT('Ctrl Pts',(2.27768357726726,4.95095791492866,36.25));
#308831=CARTESIAN_POINT('Ctrl Pts',(2.23640375626704,4.87078209602146,36.25));
#308832=CARTESIAN_POINT('Ctrl Pts',(2.18650804768952,4.79615096254107,36.25));
#308833=CARTESIAN_POINT('Ctrl Pts',(2.12995256471625,4.72672058470318,36.25));
#308834=CARTESIAN_POINT('Ctrl Pts',(2.06812897983805,4.66400945675856,36.25));
#308835=CARTESIAN_POINT('Ctrl Pts',(2.00171131208806,4.60935645208091,36.25));
#308836=CARTESIAN_POINT('Ctrl Pts',(1.93195013979453,4.56264762609262,36.25));
#308837=CARTESIAN_POINT('Ctrl Pts',(1.85820350335783,4.5241565808727,36.25));
#308838=CARTESIAN_POINT('Ctrl Pts',(1.78027605704376,4.49553589484458,36.25));
#308839=CARTESIAN_POINT('Ctrl Pts',(1.69931628629545,4.47370190759594,36.25));
#308840=CARTESIAN_POINT('Ctrl Pts',(1.61449027768335,4.46164864649648,36.25));
#308841=CARTESIAN_POINT('Ctrl Pts',(1.55682420860062,4.45973608112409,36.25));
#308842=CARTESIAN_POINT('Ctrl Pts',(1.52758218344156,4.45876623376623,36.25));
#308843=CARTESIAN_POINT('Origin',(-0.185551948051949,4.5,32.1799631621335));
#308844=CARTESIAN_POINT('',(-0.185551948051949,4.5,36.25));
#308845=CARTESIAN_POINT('',(-0.185551948051949,4.5,32.1799631621335));
#308846=CARTESIAN_POINT('',(-0.185551948051949,4.95357142857143,36.25));
#308847=CARTESIAN_POINT('',(-0.185551948051949,4.95357142857143,32.1799631621335));
#308848=CARTESIAN_POINT('',(-0.185551948051949,0.,36.25));
#308849=CARTESIAN_POINT('Origin',(0.144318181818181,4.5,32.1799631621335));
#308850=CARTESIAN_POINT('',(0.144318181818181,4.5,36.25));
#308851=CARTESIAN_POINT('',(0.144318181818181,4.5,32.1799631621335));
#308852=CARTESIAN_POINT('',(0.,4.5,36.25));
#308853=CARTESIAN_POINT('Origin',(0.144318181818181,4.95357142857143,32.1799631621335));
#308854=CARTESIAN_POINT('',(0.144318181818181,4.95357142857143,36.25));
#308855=CARTESIAN_POINT('',(0.144318181818181,4.95357142857143,32.1799631621335));
#308856=CARTESIAN_POINT('',(0.144318181818181,0.,36.25));
#308857=CARTESIAN_POINT('Origin',(-0.185551948051949,4.95357142857143,32.1799631621335));
#308858=CARTESIAN_POINT('',(0.,4.95357142857143,36.25));
#308859=CARTESIAN_POINT('Origin',(0.,0.,36.25));
#308860=CARTESIAN_POINT('',(4.75,-8.22724133595217,36.25));
#308861=CARTESIAN_POINT('',(9.5,0.,36.25));
#308862=CARTESIAN_POINT('Origin',(0.,0.,36.25));
#308863=CARTESIAN_POINT('',(4.75,8.22724133595217,36.25));
#308864=CARTESIAN_POINT('Origin',(0.,0.,36.25));
#308865=CARTESIAN_POINT('',(-4.75,8.22724133595217,36.25));
#308866=CARTESIAN_POINT('Origin',(0.,0.,36.25));
#308867=CARTESIAN_POINT('',(-9.5,-1.50231459873716E-15,36.25));
#308868=CARTESIAN_POINT('Origin',(0.,0.,36.25));
#308869=CARTESIAN_POINT('',(-4.75,-8.22724133595217,36.25));
#308870=CARTESIAN_POINT('Origin',(0.,0.,36.25));
#308871=CARTESIAN_POINT('Origin',(0.,0.,36.25));
#308872=CARTESIAN_POINT('Origin',(0.,0.,36.25));
#308873=CARTESIAN_POINT('',(-2.91010732950533E-15,-10.9696551146029,35.4014942239681));
#308874=CARTESIAN_POINT('Ctrl Pts',(-4.74999999999998,-8.22724133595217,
36.25));
#308875=CARTESIAN_POINT('Ctrl Pts',(-2.54551732809356,-9.50000000000121,
36.25));
#308876=CARTESIAN_POINT('Ctrl Pts',(5.22468907019947E-12,-10.9696551146059,
35.4014942239664));
#308877=CARTESIAN_POINT('Ctrl Pts',(-5.2327759896147E-12,-10.9696551146059,
35.4014942239664));
#308878=CARTESIAN_POINT('Ctrl Pts',(2.54551732809357,-9.50000000000122,
36.25));
#308879=CARTESIAN_POINT('Ctrl Pts',(4.75000000000001,-8.22724133595218,
36.25));
#308880=CARTESIAN_POINT('Origin',(0.,0.,36.25));
#308881=CARTESIAN_POINT('',(9.5,-5.48482755730145,35.4014942239681));
#308882=CARTESIAN_POINT('Ctrl Pts',(4.75000000000001,-8.22724133595218,
36.25));
#308883=CARTESIAN_POINT('Ctrl Pts',(6.95448267190644,-6.95448267190313,
36.25));
#308884=CARTESIAN_POINT('Ctrl Pts',(9.50000000000523,-5.48482755729844,
35.4014942239664));
#308885=CARTESIAN_POINT('Ctrl Pts',(9.5,-5.48482755730749,35.4014942239664));
#308886=CARTESIAN_POINT('Ctrl Pts',(9.5,-2.54551732809809,36.25));
#308887=CARTESIAN_POINT('Ctrl Pts',(9.5,1.60134500782782E-14,36.25));
#308888=CARTESIAN_POINT('Origin',(0.,0.,36.25));
#308889=CARTESIAN_POINT('',(9.5,5.48482755730145,35.4014942239681));
#308890=CARTESIAN_POINT('Ctrl Pts',(9.5,1.60134500782782E-14,36.25));
#308891=CARTESIAN_POINT('Ctrl Pts',(9.5,2.5455173280981,36.25));
#308892=CARTESIAN_POINT('Ctrl Pts',(9.5,5.48482755730748,35.4014942239664));
#308893=CARTESIAN_POINT('Ctrl Pts',(9.50000000000522,5.48482755729844,35.4014942239664));
#308894=CARTESIAN_POINT('Ctrl Pts',(6.95448267190642,6.95448267190313,36.25));
#308895=CARTESIAN_POINT('Ctrl Pts',(4.74999999999998,8.22724133595218,36.25));
#308896=CARTESIAN_POINT('Origin',(0.,0.,36.25));
#308897=CARTESIAN_POINT('',(-4.96520474180093E-16,10.9696551146029,35.4014942239681));
#308898=CARTESIAN_POINT('Ctrl Pts',(4.74999999999998,8.22724133595218,36.25));
#308899=CARTESIAN_POINT('Ctrl Pts',(2.54551732809355,9.50000000000122,36.25));
#308900=CARTESIAN_POINT('Ctrl Pts',(-5.2257673261215E-12,10.9696551146059,
35.4014942239664));
#308901=CARTESIAN_POINT('Ctrl Pts',(5.23169773369267E-12,10.9696551146059,
35.4014942239664));
#308902=CARTESIAN_POINT('Ctrl Pts',(-2.54551732809357,9.50000000000122,
36.25));
#308903=CARTESIAN_POINT('Ctrl Pts',(-4.75,8.22724133595218,36.25));
#308904=CARTESIAN_POINT('Origin',(0.,0.,36.25));
#308905=CARTESIAN_POINT('',(-9.5,-5.48482755730144,35.4014942239681));
#308906=CARTESIAN_POINT('Ctrl Pts',(-9.5,-1.40117688184935E-14,36.25));
#308907=CARTESIAN_POINT('Ctrl Pts',(-9.5,-2.54551732809809,36.25));
#308908=CARTESIAN_POINT('Ctrl Pts',(-9.5,-5.48482755730747,35.4014942239664));
#308909=CARTESIAN_POINT('Ctrl Pts',(-9.50000000000523,-5.48482755729841,
35.4014942239664));
#308910=CARTESIAN_POINT('Ctrl Pts',(-6.95448267190643,-6.95448267190312,
36.25));
#308911=CARTESIAN_POINT('Ctrl Pts',(-4.74999999999998,-8.22724133595217,
36.25));
#308912=CARTESIAN_POINT('Origin',(0.,0.,36.25));
#308913=CARTESIAN_POINT('',(-9.5,5.48482755730145,35.4014942239681));
#308914=CARTESIAN_POINT('Ctrl Pts',(-9.5,5.48482755730747,35.4014942239664));
#308915=CARTESIAN_POINT('Ctrl Pts',(-9.5,2.54551732809808,36.25));
#308916=CARTESIAN_POINT('Ctrl Pts',(-9.5,-1.40117688184935E-14,36.25));
#308917=CARTESIAN_POINT('Ctrl Pts',(-4.75,8.22724133595218,36.25));
#308918=CARTESIAN_POINT('Ctrl Pts',(-6.95448267190644,6.95448267190313,
36.25));
#308919=CARTESIAN_POINT('Ctrl Pts',(-9.50000000000522,5.48482755729844,
35.4014942239664));
#308920=CARTESIAN_POINT('Origin',(-9.5,-5.48482755730144,36.25));
#308921=CARTESIAN_POINT('',(-9.5,-5.48482755730144,28.75));
#308922=CARTESIAN_POINT('',(-9.5,-5.48482755730144,36.25));
#308923=CARTESIAN_POINT('',(-2.51906757195928E-15,-10.9696551146029,28.75));
#308924=CARTESIAN_POINT('',(-9.5,-5.48482755730144,28.75));
#308925=CARTESIAN_POINT('',(-2.51906757195928E-15,-10.9696551146029,36.25));
#308926=CARTESIAN_POINT('Origin',(-2.51906757195928E-15,-10.9696551146029,
36.25));
#308927=CARTESIAN_POINT('',(9.5,-5.48482755730145,28.75));
#308928=CARTESIAN_POINT('',(-2.51906757195928E-15,-10.9696551146029,28.75));
#308929=CARTESIAN_POINT('',(9.5,-5.48482755730145,36.25));
#308930=CARTESIAN_POINT('Origin',(9.5,-5.48482755730145,36.25));
#308931=CARTESIAN_POINT('',(9.5,5.48482755730145,28.75));
#308932=CARTESIAN_POINT('',(9.5,-5.48482755730145,28.75));
#308933=CARTESIAN_POINT('',(9.5,5.48482755730145,36.25));
#308934=CARTESIAN_POINT('Origin',(9.5,5.48482755730145,36.25));
#308935=CARTESIAN_POINT('',(-1.81887649324012E-16,10.9696551146029,28.75));
#308936=CARTESIAN_POINT('',(9.5,5.48482755730145,28.75));
#308937=CARTESIAN_POINT('',(-1.81887649324012E-16,10.9696551146029,36.25));
#308938=CARTESIAN_POINT('Origin',(-1.81887649324012E-16,10.9696551146029,
36.25));
#308939=CARTESIAN_POINT('',(-9.5,5.48482755730145,28.75));
#308940=CARTESIAN_POINT('',(-1.81887649324012E-16,10.9696551146029,28.75));
#308941=CARTESIAN_POINT('',(-9.5,5.48482755730145,36.25));
#308942=CARTESIAN_POINT('Origin',(-9.5,5.48482755730145,36.25));
#308943=CARTESIAN_POINT('',(-9.5,5.48482755730145,28.75));
#308944=CARTESIAN_POINT('Origin',(0.,0.,28.75));
#308945=CARTESIAN_POINT('Origin',(0.,5.28128932132296E-15,28.75));
#308946=CARTESIAN_POINT('Origin',(0.,0.,-6.25));
#308947=CARTESIAN_POINT('',(0.,0.,0.));
#308948=CARTESIAN_POINT('Origin',(0.,8.67361737988403E-16,4.3));
#308949=CARTESIAN_POINT('',(-4.95790425747066,1.64791259544213E-16,3.25790425747067));
#308950=CARTESIAN_POINT('',(-5.73382214207426,-3.69911165529381E-15,4.03382214207426));
#308951=CARTESIAN_POINT('',(-6.,1.32573658499991E-16,4.3));
#308952=CARTESIAN_POINT('',(-4.17899100816595,2.48759446686254,3.1633416575335));
#308953=CARTESIAN_POINT('Ctrl Pts',(-4.17899100816605,2.48759446686292,
3.1633416575334));
#308954=CARTESIAN_POINT('Ctrl Pts',(-4.35976599882962,2.2078253190039,3.1755770463795));
#308955=CARTESIAN_POINT('Ctrl Pts',(-4.51120120864995,1.9101569924174,3.18761785547117));
#308956=CARTESIAN_POINT('Ctrl Pts',(-4.75167253802496,1.28565862670522,
3.21105851922133));
#308957=CARTESIAN_POINT('Ctrl Pts',(-4.84071390792199,0.958207282422365,
3.2229942327288));
#308958=CARTESIAN_POINT('Ctrl Pts',(-4.9296140215725,0.416876072737902,
3.24277553752449));
#308959=CARTESIAN_POINT('Ctrl Pts',(-4.95035223594235,0.208575748336291,
3.25035223594236));
#308960=CARTESIAN_POINT('Ctrl Pts',(-4.95790425747066,-1.0998146837693E-14,
3.25790425747067));
#308961=CARTESIAN_POINT('',(-1.20731623616734,4.71110173778723,3.16334165753294));
#308962=CARTESIAN_POINT('Origin',(2.99770677028732E-14,-1.99840144432528E-14,
3.16334165753296));
#308963=CARTESIAN_POINT('Ctrl Pts',(-5.73382214207426,-1.47104550762833E-14,
4.03382214207426));
#308964=CARTESIAN_POINT('Ctrl Pts',(-5.67965864914995,0.463559823425577,
3.97965864914995));
#308965=CARTESIAN_POINT('Ctrl Pts',(-5.56866706255198,0.919207299152243,
3.92486143298303));
#308966=CARTESIAN_POINT('Ctrl Pts',(-5.34205662154187,1.51737050224436,
3.85075284488971));
#308967=CARTESIAN_POINT('Ctrl Pts',(-5.2725514384,1.67890370382941,3.83071749499014));
#308968=CARTESIAN_POINT('Ctrl Pts',(-5.04000190306274,2.15372430153968,
3.76951790508672));
#308969=CARTESIAN_POINT('Ctrl Pts',(-4.85211037594447,2.4560892862115,3.72690108827535));
#308970=CARTESIAN_POINT('Ctrl Pts',(-4.21965696989943,3.27662074140819,
3.59952510479816));
#308971=CARTESIAN_POINT('Ctrl Pts',(-3.7037171783334,3.73029790186619,3.51307468723862));
#308972=CARTESIAN_POINT('Ctrl Pts',(-2.90020595016428,4.19934957757759,
3.39749471643447));
#308973=CARTESIAN_POINT('Ctrl Pts',(-2.5831446231689,4.36452052269484,3.35326171353216));
#308974=CARTESIAN_POINT('Ctrl Pts',(-1.85663861005444,4.60294910828577,
3.2525436348559));
#308975=CARTESIAN_POINT('Ctrl Pts',(-1.53427994520919,4.6735834616892,3.20816601785766));
#308976=CARTESIAN_POINT('Ctrl Pts',(-1.20731623616735,4.71110173778724,
3.16334165753295));
#308977=CARTESIAN_POINT('Origin',(0.,8.67361737988403E-16,5.));
#308978=CARTESIAN_POINT('',(6.,2.75510821701405E-15,-3.46875));
#308979=CARTESIAN_POINT('',(6.,2.98062226889103E-15,-3.6875));
#308980=CARTESIAN_POINT('',(6.,1.32573658499991E-16,5.));
#308981=CARTESIAN_POINT('',(-3.52671151375444,-4.85410196624999,-4.3));
#308982=CARTESIAN_POINT('Ctrl Pts',(-3.52671151375468,-4.8541019662498,
-4.29999999999999));
#308983=CARTESIAN_POINT('Ctrl Pts',(-3.01702740994254,-5.22440914351759,
-4.27172359402267));
#308984=CARTESIAN_POINT('Ctrl Pts',(-2.45213658317982,-5.51217749530336,
-4.24217304225748));
#308985=CARTESIAN_POINT('Ctrl Pts',(-1.25347469899042,-5.90134277786329,
-4.18269831181752));
#308986=CARTESIAN_POINT('Ctrl Pts',(-0.627290301592286,-6.00028203988638,
-4.1531587114977));
#308987=CARTESIAN_POINT('Ctrl Pts',(0.780649576506183,-5.9996503626714,
-4.08995709601937));
#308988=CARTESIAN_POINT('Ctrl Pts',(1.55112467953324,-5.84800091941097,
-4.05316439625781));
#308989=CARTESIAN_POINT('Ctrl Pts',(2.99115560746716,-5.25909995323094,
-3.9799435147521));
#308990=CARTESIAN_POINT('Ctrl Pts',(3.64708340346823,-4.82741575923643,
-3.94564211591625));
#308991=CARTESIAN_POINT('Ctrl Pts',(4.76587129969454,-3.72958885758529,
-3.87269323203537));
#308992=CARTESIAN_POINT('Ctrl Pts',(5.21476518269572,-3.07076816043726,
-3.83508774624553));
#308993=CARTESIAN_POINT('Ctrl Pts',(5.8254457701165,-1.63178380133655,-3.76320804987384));
#308994=CARTESIAN_POINT('Ctrl Pts',(5.98710430498857,-0.86783042733205,
-3.72845522456362));
#308995=CARTESIAN_POINT('Ctrl Pts',(5.99975331957655,-0.0628355432998811,
-3.69046537630555));
#308996=CARTESIAN_POINT('Ctrl Pts',(6.,-0.0314121545073137,-3.68898242306487));
#308997=CARTESIAN_POINT('Ctrl Pts',(6.,6.93787513263274E-15,-3.6875));
#308998=CARTESIAN_POINT('',(-5.92794875776502,-0.927050983124574,-4.3));
#308999=CARTESIAN_POINT('Origin',(0.,8.67361737988403E-16,-4.3));
#309000=CARTESIAN_POINT('Ctrl Pts',(6.,2.0122792321331E-15,-3.46875));
#309001=CARTESIAN_POINT('Ctrl Pts',(6.,-0.292663539025992,-3.48256157030785));
#309002=CARTESIAN_POINT('Ctrl Pts',(5.97858754364113,-0.585590117231843,
-3.49638555413373));
#309003=CARTESIAN_POINT('Ctrl Pts',(5.82222002909116,-1.64460792499764,
-3.54636341935705));
#309004=CARTESIAN_POINT('Ctrl Pts',(5.5607466448591,-2.38349895084104,-3.58050080876941));
#309005=CARTESIAN_POINT('Ctrl Pts',(4.76927675868354,-3.72310608228378,
-3.65360125733108));
#309006=CARTESIAN_POINT('Ctrl Pts',(4.24579242054897,-4.31055256457267,
-3.69055077540168));
#309007=CARTESIAN_POINT('Ctrl Pts',(2.99271814667052,-5.26045286831389,
-3.76157686148056));
#309008=CARTESIAN_POINT('Ctrl Pts',(2.27204555389018,-5.60952042043114,
-3.79857954700951));
#309009=CARTESIAN_POINT('Ctrl Pts',(0.755636327633439,-6.00226359092732,
-3.87236787236862));
#309010=CARTESIAN_POINT('Ctrl Pts',(-0.0235323394529939,-6.04959639713139,
-3.90658291849198));
#309011=CARTESIAN_POINT('Ctrl Pts',(-1.56944643722608,-5.84420783515746,
-3.97896325289623));
#309012=CARTESIAN_POINT('Ctrl Pts',(-2.32079973347914,-5.58854451710374,
-4.01641457981235));
#309013=CARTESIAN_POINT('Ctrl Pts',(-3.67844415256058,-4.80419770598322,
-4.08878796902789));
#309014=CARTESIAN_POINT('Ctrl Pts',(-4.27248937251792,-4.28451816332565,
-4.12368375995929));
#309015=CARTESIAN_POINT('Ctrl Pts',(-5.05912931149185,-3.26512372236398,
-4.18442461750057));
#309016=CARTESIAN_POINT('Ctrl Pts',(-5.31626731416515,-2.82721615051172,
-4.2082765699416));
#309017=CARTESIAN_POINT('Ctrl Pts',(-5.71215595317702,-1.9028913933687,
-4.2545485907623));
#309018=CARTESIAN_POINT('Ctrl Pts',(-5.85073664177685,-1.42077729957134,
-4.27669974279977));
#309019=CARTESIAN_POINT('Ctrl Pts',(-5.92794875776501,-0.927050983124573,
-4.30000000000001));
#309020=CARTESIAN_POINT('Origin',(0.,8.67361737988403E-16,5.));
#309021=CARTESIAN_POINT('',(6.,3.32323015539645E-15,-1.71875));
#309022=CARTESIAN_POINT('',(6.,-5.58213622101655E-16,-1.9375));
#309023=CARTESIAN_POINT('',(6.,1.32573658499991E-16,5.));
#309024=CARTESIAN_POINT('Ctrl Pts',(6.,6.52256026967279E-15,-3.6875));
#309025=CARTESIAN_POINT('Ctrl Pts',(6.,0.754851426978661,-3.65187655476185));
#309026=CARTESIAN_POINT('Ctrl Pts',(5.85754231131096,1.50326411623468,-3.61758911902599));
#309027=CARTESIAN_POINT('Ctrl Pts',(5.29207719224363,2.93370952013802,-3.54728967566669));
#309028=CARTESIAN_POINT('Ctrl Pts',(4.86462320380596,3.59834926176515,-3.51005674514032));
#309029=CARTESIAN_POINT('Ctrl Pts',(3.78446274319373,4.71990668353304,-3.43727333018283));
#309030=CARTESIAN_POINT('Ctrl Pts',(3.14436250545196,5.16842862379681,-3.40325514303962));
#309031=CARTESIAN_POINT('Ctrl Pts',(1.71060281984634,5.80561894256311,-3.32961151325641));
#309032=CARTESIAN_POINT('Ctrl Pts',(0.927540309668796,5.98089784650727,
-3.29190925804666));
#309033=CARTESIAN_POINT('Ctrl Pts',(-0.642997127075086,6.01574222164111,
-3.22091085987786));
#309034=CARTESIAN_POINT('Ctrl Pts',(-1.41515883852677,5.88218433805444,
-3.18476544364091));
#309035=CARTESIAN_POINT('Ctrl Pts',(-2.86894581371622,5.32702879267005,
-3.11141927176926));
#309036=CARTESIAN_POINT('Ctrl Pts',(-3.53625863096382,4.90947819517605,
-3.07684941682089));
#309037=CARTESIAN_POINT('Ctrl Pts',(-4.6795110472583,3.83701775744516,-3.00419039101464));
#309038=CARTESIAN_POINT('Ctrl Pts',(-5.14230996632516,3.19016997761122,
-2.9666563133062));
#309039=CARTESIAN_POINT('Ctrl Pts',(-5.78559661601467,1.76775945417096,
-2.89450493598388));
#309040=CARTESIAN_POINT('Ctrl Pts',(-5.9650504210191,1.00810019736398,-2.8600749278492));
#309041=CARTESIAN_POINT('Ctrl Pts',(-6.02636626662587,-0.554006862010353,
-2.78635494362863));
#309042=CARTESIAN_POINT('Ctrl Pts',(-5.90116044522712,-1.34171831741748,
-2.74996681296589));
#309043=CARTESIAN_POINT('Ctrl Pts',(-5.3559200560131,-2.81498908441548,
-2.67859332848681));
#309044=CARTESIAN_POINT('Ctrl Pts',(-4.94440107418828,-3.48752970239708,
-2.64150076868213));
#309045=CARTESIAN_POINT('Ctrl Pts',(-3.89066652120622,-4.63291440095925,
-2.56854066851539));
#309046=CARTESIAN_POINT('Ctrl Pts',(-3.26006452534031,-5.09638730462185,
-2.53449878605424));
#309047=CARTESIAN_POINT('Ctrl Pts',(-1.84167979261482,-5.76512768826473,
-2.46108512339898));
#309048=CARTESIAN_POINT('Ctrl Pts',(-1.0646476216952,-5.95777476296554,
-2.42340024138862));
#309049=CARTESIAN_POINT('Ctrl Pts',(0.501567117423101,-6.02902034618537,
-2.35206500740862));
#309050=CARTESIAN_POINT('Ctrl Pts',(1.27536280312196,-5.91389860142432,
-2.316502392684));
#309051=CARTESIAN_POINT('Ctrl Pts',(2.74290332138521,-5.39333740010627,
-2.24304342297233));
#309052=CARTESIAN_POINT('Ctrl Pts',(3.42177892466692,-4.99029458024765,
-2.20811052867497));
#309053=CARTESIAN_POINT('Ctrl Pts',(4.58950176879661,-3.94387559037259,
-2.13576696772565));
#309054=CARTESIAN_POINT('Ctrl Pts',(5.066083143584,-3.30945112192263,-2.09832489426651));
#309055=CARTESIAN_POINT('Ctrl Pts',(5.74212308881292,-1.90426481076331,
-2.02592258302779));
#309056=CARTESIAN_POINT('Ctrl Pts',(5.93952523631834,-1.14901086376142,
-1.99172487673777));
#309057=CARTESIAN_POINT('Ctrl Pts',(5.99605415847058,-0.251399423361188,
-1.9493642070094));
#309058=CARTESIAN_POINT('Ctrl Pts',(6.,-0.125632992952679,-1.94342895487058));
#309059=CARTESIAN_POINT('Ctrl Pts',(6.,1.21430643318376E-15,-1.9375));
#309060=CARTESIAN_POINT('Ctrl Pts',(6.,8.2572837456496E-15,-1.71875));
#309061=CARTESIAN_POINT('Ctrl Pts',(6.,-0.380626147463122,-1.73671275960507));
#309062=CARTESIAN_POINT('Ctrl Pts',(5.96378105869915,-0.761301949215604,
-1.75467786252801));
#309063=CARTESIAN_POINT('Ctrl Pts',(5.74354061198417,-1.90264867938727,
-1.80854104843037));
#309064=CARTESIAN_POINT('Ctrl Pts',(5.44784922568642,-2.63234772832579,
-1.84313344932999));
#309065=CARTESIAN_POINT('Ctrl Pts',(4.59581412479552,-3.93460285458722,
-1.91648783842465));
#309066=CARTESIAN_POINT('Ctrl Pts',(4.04877122369217,-4.49554195946292,
-1.95258945402002));
#309067=CARTESIAN_POINT('Ctrl Pts',(2.75643213309168,-5.38826013945762,
-2.02361216748895));
#309068=CARTESIAN_POINT('Ctrl Pts',(2.01950923078473,-5.70550197669431,
-2.06131383676569));
#309069=CARTESIAN_POINT('Ctrl Pts',(0.484600928023682,-6.03033344932268,
-2.13494207511938));
#309070=CARTESIAN_POINT('Ctrl Pts',(-0.296964896493759,-6.04248112405295,
-2.1689591248813));
#309071=CARTESIAN_POINT('Ctrl Pts',(-1.82956974936608,-5.76759580806508,
-2.24175559630771));
#309072=CARTESIAN_POINT('Ctrl Pts',(-2.5654889922958,-5.48003748619595,
-2.27897933385702));
#309073=CARTESIAN_POINT('Ctrl Pts',(-3.8890650541548,-4.63622423181947,
-2.35069085588018));
#309074=CARTESIAN_POINT('Ctrl Pts',(-4.46303185697885,-4.08666189475346,
-2.38652333173586));
#309075=CARTESIAN_POINT('Ctrl Pts',(-5.35834192021326,-2.8083216078333,
-2.46016507094176));
#309076=CARTESIAN_POINT('Ctrl Pts',(-5.67542561455437,-2.09476336347253,
-2.49489254898579));
#309077=CARTESIAN_POINT('Ctrl Pts',(-6.0246894528286,-0.57123686740069,
-2.56679181387678));
#309078=CARTESIAN_POINT('Ctrl Pts',(-6.04750405750468,0.22552194160929,
-2.60439297986302));
#309079=CARTESIAN_POINT('Ctrl Pts',(-5.78526874443865,1.77087908084594,
-2.67732249083092));
#309080=CARTESIAN_POINT('Ctrl Pts',(-5.50714127525806,2.50533946687444,
-2.71163960583237));
#309081=CARTESIAN_POINT('Ctrl Pts',(-4.68608114771929,3.82697580146689,
-2.78487474353452));
#309082=CARTESIAN_POINT('Ctrl Pts',(-4.15102714321106,4.40156948651998,
-2.82162948145506));
#309083=CARTESIAN_POINT('Ctrl Pts',(-2.8765788559961,5.32535707165584,-2.89230229954621));
#309084=CARTESIAN_POINT('Ctrl Pts',(-2.14521668281624,5.65968734390764,
-2.93000359360147));
#309085=CARTESIAN_POINT('Ctrl Pts',(-0.616665035412588,6.01817695082359,
-3.00383737471598));
#309086=CARTESIAN_POINT('Ctrl Pts',(0.163766668494401,6.04747253546172,
-3.03790801272646));
#309087=CARTESIAN_POINT('Ctrl Pts',(1.70309619005384,5.80642697848102,-3.11051281019814));
#309088=CARTESIAN_POINT('Ctrl Pts',(2.44671138181905,5.53432659170943,-3.14785653591319));
#309089=CARTESIAN_POINT('Ctrl Pts',(3.7871031240861,4.71943158303236,-3.21990106976846));
#309090=CARTESIAN_POINT('Ctrl Pts',(4.37095580452145,4.18448897586484,-3.25523421552925));
#309091=CARTESIAN_POINT('Ctrl Pts',(5.29372927427807,2.9284545028034,-3.32878613780276));
#309092=CARTESIAN_POINT('Ctrl Pts',(5.62704057338196,2.22166316356583,-3.36390381011906));
#309093=CARTESIAN_POINT('Ctrl Pts',(5.93875916593771,0.989102212585849,
-3.42207163754923));
#309094=CARTESIAN_POINT('Ctrl Pts',(6.,0.494927234506341,-3.44539306828448));
#309095=CARTESIAN_POINT('Ctrl Pts',(6.,1.11022302462516E-15,-3.46875));
#309096=CARTESIAN_POINT('Origin',(0.,8.67361737988403E-16,5.));
#309097=CARTESIAN_POINT('',(6.,8.4276539834582E-15,0.0312499999999995));
#309098=CARTESIAN_POINT('',(6.,-1.04393619537516E-15,-0.187499999999998));
#309099=CARTESIAN_POINT('',(6.,1.32573658499991E-16,5.));
#309100=CARTESIAN_POINT('Ctrl Pts',(6.,-9.71445146547012E-16,-1.9375));
#309101=CARTESIAN_POINT('Ctrl Pts',(6.,0.665640471875957,-1.90608665685633));
#309102=CARTESIAN_POINT('Ctrl Pts',(5.88921848914381,1.32755052273931,-1.87517647489086));
#309103=CARTESIAN_POINT('Ctrl Pts',(5.41705865771732,2.69496750715489,-1.80987164452479));
#309104=CARTESIAN_POINT('Ctrl Pts',(5.02159721538787,3.37503138930331,-1.77293727150543));
#309105=CARTESIAN_POINT('Ctrl Pts',(3.99457896445447,4.54384315513085,-1.69982382128799));
#309106=CARTESIAN_POINT('Ctrl Pts',(3.37352355036687,5.02220291135671,-1.66567301015243));
#309107=CARTESIAN_POINT('Ctrl Pts',(1.97078370548772,5.72203206182956,-1.59250815734831));
#309108=CARTESIAN_POINT('Ctrl Pts',(1.20010096420365,5.93173216826455,-1.55485956601145));
#309109=CARTESIAN_POINT('Ctrl Pts',(-0.361353151303249,6.0389314328722,
-1.4832136780329));
#309110=CARTESIAN_POINT('Ctrl Pts',(-1.13668683587222,5.94199046393976,
-1.44813624315785));
#309111=CARTESIAN_POINT('Ctrl Pts',(-2.61760268257367,5.45561539145597,
-1.37457549783133));
#309112=CARTESIAN_POINT('Ctrl Pts',(-3.30780631183448,5.06694972231676,
-1.33919869933545));
#309113=CARTESIAN_POINT('Ctrl Pts',(-4.49913774577299,4.04631668711824,
-1.26718475525266));
#309114=CARTESIAN_POINT('Ctrl Pts',(-4.98888502519728,3.42431115051731,
-1.22985162143565));
#309115=CARTESIAN_POINT('Ctrl Pts',(-5.69666279625056,2.03638239701799,
-1.15722781766094));
#309116=CARTESIAN_POINT('Ctrl Pts',(-5.91154129727581,1.28549067240917,
-1.12316572167189));
#309117=CARTESIAN_POINT('Ctrl Pts',(-6.04616476158962,-0.278633634974818,
-1.04935053815589));
#309118=CARTESIAN_POINT('Ctrl Pts',(-5.95590352725045,-1.07753162344421,
-1.011648418605));
#309119=CARTESIAN_POINT('Ctrl Pts',(-5.4744757179434,-2.57579237792346,
-0.940941511216246));
#309120=CARTESIAN_POINT('Ctrl Pts',(-5.09492912060133,-3.26290322787857,
-0.904252451447548));
#309121=CARTESIAN_POINT('Ctrl Pts',(-4.09435342234445,-4.45442056860119,
-0.831005603940027));
#309122=CARTESIAN_POINT('Ctrl Pts',(-3.48272795096895,-4.94734424768627,
-0.796666107542287));
#309123=CARTESIAN_POINT('Ctrl Pts',(-2.09560774824645,-5.67726362426316,
-0.723763493542176));
#309124=CARTESIAN_POINT('Ctrl Pts',(-1.33145851154505,-5.90340064515452,
-0.686168439737121));
#309125=CARTESIAN_POINT('Ctrl Pts',(0.224904569146673,-6.04548147749041,
-0.614242362558919));
#309126=CARTESIAN_POINT('Ctrl Pts',(1.00166095459279,-5.96616377216184,
-0.579549121659716));
#309127=CARTESIAN_POINT('Ctrl Pts',(2.49535830087068,-5.51299323361295,
-0.505898938545184));
#309128=CARTESIAN_POINT('Ctrl Pts',(3.19646467145431,-5.13833237345376,
-0.470012587137202));
#309129=CARTESIAN_POINT('Ctrl Pts',(4.41018090931122,-4.14277565323689,
-0.398335112895427));
#309130=CARTESIAN_POINT('Ctrl Pts',(4.91228199444614,-3.53294658077878,
-0.361124188318027));
#309131=CARTESIAN_POINT('Ctrl Pts',(5.65028338940432,-2.16198759426555,
-0.288309906928332));
#309132=CARTESIAN_POINT('Ctrl Pts',(5.88189550365007,-1.41534172658309,
-0.25429373806313));
#309133=CARTESIAN_POINT('Ctrl Pts',(5.98842683025393,-0.430575243748781,
-0.207819990223741));
#309134=CARTESIAN_POINT('Ctrl Pts',(6.,-0.215160329695893,-0.197653987855623));
#309135=CARTESIAN_POINT('Ctrl Pts',(6.,-5.34294830600857E-15,-0.187499999999998));
#309136=CARTESIAN_POINT('Ctrl Pts',(6.,3.19189119579733E-15,0.031249999999999));
#309137=CARTESIAN_POINT('Ctrl Pts',(6.,-0.470725023537795,0.00903523494968755));
#309138=CARTESIAN_POINT('Ctrl Pts',(5.94460269534144,-0.940908633524372,
-0.0131539793560597));
#309139=CARTESIAN_POINT('Ctrl Pts',(5.6510038405261,-2.16379476967363,-0.0708652265586574));
#309140=CARTESIAN_POINT('Ctrl Pts',(5.31985538512461,-2.88357663845083,
-0.106275724424197));
#309141=CARTESIAN_POINT('Ctrl Pts',(4.4055256383186,-4.14615152032113,-0.17984313561366));
#309142=CARTESIAN_POINT('Ctrl Pts',(3.83442737751384,-4.67935459625399,
-0.214890425153952));
#309143=CARTESIAN_POINT('Ctrl Pts',(2.50699655821698,-5.50821748300203,
-0.28655693361699));
#309144=CARTESIAN_POINT('Ctrl Pts',(1.75991933057626,-5.79034779941002,
-0.324202315297019));
#309145=CARTESIAN_POINT('Ctrl Pts',(0.213357498858581,-6.04630617784676,
-0.397349198359447));
#309146=CARTESIAN_POINT('Ctrl Pts',(-0.570328131021847,-6.02312656494286,
-0.431510709464236));
#309147=CARTESIAN_POINT('Ctrl Pts',(-2.08765133392454,-5.67880280627236,
-0.5046339403095));
#309148=CARTESIAN_POINT('Ctrl Pts',(-2.80671098652772,-5.35999656574419,
-0.541556669620217));
#309149=CARTESIAN_POINT('Ctrl Pts',(-4.09440223185377,-4.45707223313806,
-0.61251961411017));
#309150=CARTESIAN_POINT('Ctrl Pts',(-4.64736815452183,-3.87708535521748,
-0.649638225160458));
#309151=CARTESIAN_POINT('Ctrl Pts',(-5.4847736324752,-2.55254213490508,
-0.723437752878511));
#309152=CARTESIAN_POINT('Ctrl Pts',(-5.76780330380029,-1.82501351119829,
-0.757622761511133));
#309153=CARTESIAN_POINT('Ctrl Pts',(-6.04426086165223,-0.290475166533927,
-0.830041704806752));
#309154=CARTESIAN_POINT('Ctrl Pts',(-6.03031629973367,0.502760525796865,
-0.867476605552441));
#309155=CARTESIAN_POINT('Ctrl Pts',(-5.69822517251945,2.03521656565479,
-0.939797279349468));
#309156=CARTESIAN_POINT('Ctrl Pts',(-5.38464996142156,2.75996713860472,
-0.974759009091658));
#309157=CARTESIAN_POINT('Ctrl Pts',(-4.50115627225226,4.04230360576368,
-1.04822554495606));
#309158=CARTESIAN_POINT('Ctrl Pts',(-3.94195716762769,4.5892824407932,-1.08375062569196));
#309159=CARTESIAN_POINT('Ctrl Pts',(-2.63174187997251,5.44998025903682,
-1.15510871084719));
#309160=CARTESIAN_POINT('Ctrl Pts',(-1.889514023902,5.7496100397065,-1.19279163926159));
#309161=CARTESIAN_POINT('Ctrl Pts',(-0.348527245563993,6.0398542003992,
-1.26618829883601));
#309162=CARTESIAN_POINT('Ctrl Pts',(0.434138257918517,6.03430450251552,
-1.30023510347325));
#309163=CARTESIAN_POINT('Ctrl Pts',(1.95932774100072,5.7245793778829,-1.37320683225349));
#309164=CARTESIAN_POINT('Ctrl Pts',(2.68696677606726,5.42126028600814,-1.41028877474877));
#309165=CARTESIAN_POINT('Ctrl Pts',(3.99277269973531,4.54774992880339,-1.48163580445412));
#309166=CARTESIAN_POINT('Ctrl Pts',(4.55632857822104,3.98299503126182,-1.51806926917442));
#309167=CARTESIAN_POINT('Ctrl Pts',(5.42285754322966,2.68154750848389,-1.59179487168831));
#309168=CARTESIAN_POINT('Ctrl Pts',(5.72298770964204,1.96099533051178,-1.62620541801734));
#309169=CARTESIAN_POINT('Ctrl Pts',(5.95935034168459,0.806412872961356,
-1.68069323307533));
#309170=CARTESIAN_POINT('Ctrl Pts',(6.,0.403234300545509,-1.69972030155839));
#309171=CARTESIAN_POINT('Ctrl Pts',(6.,1.03389519168218E-14,-1.71875));
#309172=CARTESIAN_POINT('Origin',(0.,8.67361737988403E-16,5.));
#309173=CARTESIAN_POINT('',(6.,2.1826494699417E-15,1.78125));
#309174=CARTESIAN_POINT('',(6.,1.60951317472757E-14,1.5625));
#309175=CARTESIAN_POINT('',(6.,1.32573658499991E-16,5.));
#309176=CARTESIAN_POINT('Ctrl Pts',(6.,-5.55111512312578E-15,-0.187499999999998));
#309177=CARTESIAN_POINT('Ctrl Pts',(6.,0.576081354367094,-0.160313189660176));
#309178=CARTESIAN_POINT('Ctrl Pts',(5.91702638582546,1.1503376579636,-0.133212508317213));
#309179=CARTESIAN_POINT('Ctrl Pts',(5.53219240607711,2.44889478307763,-0.0719301460114863));
#309180=CARTESIAN_POINT('Ctrl Pts',(5.16939551881057,3.14320557919123,-0.0358881017258123));
#309181=CARTESIAN_POINT('Ctrl Pts',(4.20118386713354,4.35294341729667,0.0371566471285775));
#309182=CARTESIAN_POINT('Ctrl Pts',(3.60575241514653,4.85763567656062,0.0715039495953657));
#309183=CARTESIAN_POINT('Ctrl Pts',(2.24408834398242,5.61993818487351,0.143736272976772));
#309184=CARTESIAN_POINT('Ctrl Pts',(1.48822218673184,5.86556326238038,0.181243759105709));
#309185=CARTESIAN_POINT('Ctrl Pts',(-0.068515577213796,6.05016071869312,
0.253806687248921));
#309186=CARTESIAN_POINT('Ctrl Pts',(-0.854081099803064,5.9899642220239,
0.288479978808746));
#309187=CARTESIAN_POINT('Ctrl Pts',(-2.3536877004239,5.57335017439412,0.361862270813308));
#309188=CARTESIAN_POINT('Ctrl Pts',(-3.05392899935969,5.22259080642952,
0.397816636184359));
#309189=CARTESIAN_POINT('Ctrl Pts',(-4.29634190905553,4.26286384933163,
0.468922163407154));
#309190=CARTESIAN_POINT('Ctrl Pts',(-4.8221635816438,3.65748698279963,0.506621093160949));
#309191=CARTESIAN_POINT('Ctrl Pts',(-5.59796976267574,2.29408392787543,
0.58019556420475));
#309192=CARTESIAN_POINT('Ctrl Pts',(-5.84708647207173,1.55295549233918,
0.614211902553629));
#309193=CARTESIAN_POINT('Ctrl Pts',(-6.05076398279004,0.00948217176010763,
0.687052511111859));
#309194=CARTESIAN_POINT('Ctrl Pts',(-6.00047413546166,-0.778593467100894,
0.72424389521885));
#309195=CARTESIAN_POINT('Ctrl Pts',(-5.59887394310715,-2.29632999880747,
0.795869916301666));
#309196=CARTESIAN_POINT('Ctrl Pts',(-5.24935217544605,-3.01079584896184,
0.831838609920422));
#309197=CARTESIAN_POINT('Ctrl Pts',(-4.30285973647881,-4.25249889353262,
0.905501307099982));
#309198=CARTESIAN_POINT('Ctrl Pts',(-3.71936449972661,-4.7712339531767,
0.940144686345269));
#309199=CARTESIAN_POINT('Ctrl Pts',(-2.37432149700639,-5.56642681405337,
1.0121106591994));
#309200=CARTESIAN_POINT('Ctrl Pts',(-1.6225717168347,-5.83007269088046,
1.04969619377305));
#309201=CARTESIAN_POINT('Ctrl Pts',(-0.0706144035415794,-6.04987811861958,
1.12255801108307));
#309202=CARTESIAN_POINT('Ctrl Pts',(0.714067011565161,-6.00800326027973,
1.15693267329168));
#309203=CARTESIAN_POINT('Ctrl Pts',(2.22264915056004,-5.62710306320001,
1.23019698636496));
#309204=CARTESIAN_POINT('Ctrl Pts',(2.93225948086817,-5.29207694793741,
1.26678866993634));
#309205=CARTESIAN_POINT('Ctrl Pts',(4.19898813659643,-4.35912259188468,
1.33754652637883));
#309206=CARTESIAN_POINT('Ctrl Pts',(4.73952956446563,-3.76433231500237,
1.37524957719054));
#309207=CARTESIAN_POINT('Ctrl Pts',(5.54571268861111,-2.41743703093539,
1.44903641764982));
#309208=CARTESIAN_POINT('Ctrl Pts',(5.81096626829843,-1.68274023662274,
1.48308701550236));
#309209=CARTESIAN_POINT('Ctrl Pts',(5.97649250358845,-0.61353127993814,
1.53354582813126));
#309210=CARTESIAN_POINT('Ctrl Pts',(6.,-0.306646382963594,1.54802854212027));
#309211=CARTESIAN_POINT('Ctrl Pts',(6.,2.77555756156289E-14,1.5625));
#309212=CARTESIAN_POINT('Ctrl Pts',(6.,1.49880108324396E-14,1.78125));
#309213=CARTESIAN_POINT('Ctrl Pts',(6.,-0.572678939529224,1.75422375866001));
#309214=CARTESIAN_POINT('Ctrl Pts',(5.91800369014654,-1.14358786020556,
1.72728104921443));
#309215=CARTESIAN_POINT('Ctrl Pts',(5.53635369796318,-2.43944113070009,
1.66612628899505));
#309216=CARTESIAN_POINT('Ctrl Pts',(5.17479590479424,-3.13428132315402,
1.63012862891726));
#309217=CARTESIAN_POINT('Ctrl Pts',(4.20441390584562,-4.35106713781484,
1.55675458711265));
#309218=CARTESIAN_POINT('Ctrl Pts',(3.60352824145776,-4.86039911440975,
1.52210592293855));
#309219=CARTESIAN_POINT('Ctrl Pts',(2.23436680393038,-5.62382857334181,
1.44952066142893));
#309220=CARTESIAN_POINT('Ctrl Pts',(1.47794603415836,-5.86817859973392,
1.41200687718543));
#309221=CARTESIAN_POINT('Ctrl Pts',(-0.0721756084407044,-6.04920383351369,
1.33979299456714));
#309222=CARTESIAN_POINT('Ctrl Pts',(-0.850441636930328,-5.98955870406894,
1.30542745698193));
#309223=CARTESIAN_POINT('Ctrl Pts',(-2.35818450799125,-5.57353001966035,
1.23168852223451));
#309224=CARTESIAN_POINT('Ctrl Pts',(-3.07136132076605,-5.21458358919537,
1.195144093216));
#309225=CARTESIAN_POINT('Ctrl Pts',(-4.30947960728758,-4.24709108315852,
1.12386120914637));
#309226=CARTESIAN_POINT('Ctrl Pts',(-4.82489175537719,-3.65099079453108,
1.08680520734935));
#309227=CARTESIAN_POINT('Ctrl Pts',(-5.59599279880615,-2.29923521512223,
1.01380594949795));
#309228=CARTESIAN_POINT('Ctrl Pts',(-5.84604828250109,-1.55735104566999,
0.979745535292359));
#309229=CARTESIAN_POINT('Ctrl Pts',(-6.05208909268611,-0.00297120746707236,
0.906390219177862));
#309230=CARTESIAN_POINT('Ctrl Pts',(-5.9995981480835,0.795412185708006,
0.868712384746716));
#309231=CARTESIAN_POINT('Ctrl Pts',(-5.59200466403976,2.30862617337791,
0.797299794537919));
#309232=CARTESIAN_POINT('Ctrl Pts',(-5.2474791233062,3.01069928691735,0.761863119915467));
#309233=CARTESIAN_POINT('Ctrl Pts',(-4.30577501001307,4.2512148277737,0.688378585303151));
#309234=CARTESIAN_POINT('Ctrl Pts',(-3.71513418603691,4.77601332690382,
0.653345745772946));
#309235=CARTESIAN_POINT('Ctrl Pts',(-2.36324112314454,5.57064612279665,
0.581080490070765));
#309236=CARTESIAN_POINT('Ctrl Pts',(-1.61444853991224,5.83185572665356,
0.543663212007828));
#309237=CARTESIAN_POINT('Ctrl Pts',(-0.0706927808031071,6.04924027915339,
0.471204808540938));
#309238=CARTESIAN_POINT('Ctrl Pts',(0.708908523410627,6.0079728699457,0.437048411347023));
#309239=CARTESIAN_POINT('Ctrl Pts',(2.21342193544873,5.63075564668377,0.364020424512322));
#309240=CARTESIAN_POINT('Ctrl Pts',(2.9236870728096,5.29683472622097,0.327380771732109));
#309241=CARTESIAN_POINT('Ctrl Pts',(4.19210437752919,4.36576624896074,0.256648075820155));
#309242=CARTESIAN_POINT('Ctrl Pts',(4.73366689496251,3.77172868347265,0.21894543912036));
#309243=CARTESIAN_POINT('Ctrl Pts',(5.54196569879411,2.42600175560982,0.145144518953668));
#309244=CARTESIAN_POINT('Ctrl Pts',(5.808342707209,1.69175542142419,0.111088435031726));
#309245=CARTESIAN_POINT('Ctrl Pts',(5.97601291190124,0.619751558434104,
0.0604977233453745));
#309246=CARTESIAN_POINT('Ctrl Pts',(6.,0.309758556663313,0.0458683296287967));
#309247=CARTESIAN_POINT('Ctrl Pts',(6.,2.63677968348475E-15,0.0312499999999991));
#309248=CARTESIAN_POINT('Origin',(0.,8.67361737988403E-16,5.));
#309249=CARTESIAN_POINT('',(6.,-2.57049285423475E-15,3.53125));
#309250=CARTESIAN_POINT('',(6.,2.60871389689021E-14,3.31250000000001));
#309251=CARTESIAN_POINT('',(6.,1.32573658499991E-16,5.));
#309252=CARTESIAN_POINT('',(-5.56513300460776,2.24260889167614,4.3));
#309253=CARTESIAN_POINT('Ctrl Pts',(-5.56513300460779,2.24260889167618,
4.29999999999994));
#309254=CARTESIAN_POINT('Ctrl Pts',(-5.29598978898201,2.91049966737262,
4.26703435210964));
#309255=CARTESIAN_POINT('Ctrl Pts',(-4.90881103715039,3.52449133733131,
4.23285234862231));
#309256=CARTESIAN_POINT('Ctrl Pts',(-3.89806696721271,4.62670295206297,
4.16273310160683));
#309257=CARTESIAN_POINT('Ctrl Pts',(-3.26813626689166,5.09122723636252,
4.12868632009684));
#309258=CARTESIAN_POINT('Ctrl Pts',(-1.85084558505042,5.76217410259774,
4.05528958373036));
#309259=CARTESIAN_POINT('Ctrl Pts',(-1.07425068762339,5.95603362377136,
4.01760664630479));
#309260=CARTESIAN_POINT('Ctrl Pts',(0.491642689492169,6.02982815809019,
3.94624866377506));
#309261=CARTESIAN_POINT('Ctrl Pts',(1.26554985762075,5.91599613957569,3.91072341508568));
#309262=CARTESIAN_POINT('Ctrl Pts',(2.73404541385783,5.39785774924788,3.83725691317482));
#309263=CARTESIAN_POINT('Ctrl Pts',(3.41372714253246,4.99583250130562,3.80229531421047));
#309264=CARTESIAN_POINT('Ctrl Pts',(4.58314192306331,3.95123953039067,3.72997453717357));
#309265=CARTESIAN_POINT('Ctrl Pts',(5.06067127023562,3.31769082048273,3.69253960393319));
#309266=CARTESIAN_POINT('Ctrl Pts',(5.7389811573739,1.91372004594514,3.62012073521678));
#309267=CARTESIAN_POINT('Ctrl Pts',(5.93763030254109,1.15877496180985,3.58593567047772));
#309268=CARTESIAN_POINT('Ctrl Pts',(5.99584573501727,0.257955583484155,
3.54342360963193));
#309269=CARTESIAN_POINT('Ctrl Pts',(6.,0.128908368236316,3.53733352853618));
#309270=CARTESIAN_POINT('Ctrl Pts',(6.,-1.2941037130787E-14,3.53125));
#309271=CARTESIAN_POINT('',(-6.,1.32573658499991E-16,4.3));
#309272=CARTESIAN_POINT('Origin',(0.,8.67361737988403E-16,4.3));
#309273=CARTESIAN_POINT('',(-5.51281765513596,-2.36829928456402,4.30000000000377));
#309274=CARTESIAN_POINT('Origin',(0.,8.67361737988403E-16,4.3));
#309275=CARTESIAN_POINT('Ctrl Pts',(6.,4.65599780952175E-14,3.31250000000001));
#309276=CARTESIAN_POINT('Ctrl Pts',(6.,0.383786548380919,3.33061190732474));
#309277=CARTESIAN_POINT('Ctrl Pts',(5.96317705814195,0.76760918361683,3.34872551768492));
#309278=CARTESIAN_POINT('Ctrl Pts',(5.74049833989295,1.91186775775114,3.40272612124355));
#309279=CARTESIAN_POINT('Ctrl Pts',(5.44357047524973,2.64122801660512,3.43734118463211));
#309280=CARTESIAN_POINT('Ctrl Pts',(4.58935776101163,3.94211204251619,3.51070363071812));
#309281=CARTESIAN_POINT('Ctrl Pts',(4.04147277688072,4.50208780601877,3.54676248963149));
#309282=CARTESIAN_POINT('Ctrl Pts',(2.7478864932634,5.39260451994447,3.61780907600754));
#309283=CARTESIAN_POINT('Ctrl Pts',(2.01058506327089,5.70863538339475,3.65551007466445));
#309284=CARTESIAN_POINT('Ctrl Pts',(0.475243583065782,6.03108562778345,
3.72912302902632));
#309285=CARTESIAN_POINT('Ctrl Pts',(-0.30640013799983,6.04201748954695,
3.76313936707741));
#309286=CARTESIAN_POINT('Ctrl Pts',(-1.83851098665274,5.76473566870732,
3.83594861519836));
#309287=CARTESIAN_POINT('Ctrl Pts',(-2.57387223944839,5.4760881030531,3.87316319334589));
#309288=CARTESIAN_POINT('Ctrl Pts',(-3.89624091234994,4.630229613505,3.94485035061565));
#309289=CARTESIAN_POINT('Ctrl Pts',(-4.46949934320597,4.07962684941699,
3.98072132995236));
#309290=CARTESIAN_POINT('Ctrl Pts',(-5.36284646836113,2.79970179088196,
4.05436912497271));
#309291=CARTESIAN_POINT('Ctrl Pts',(-5.67877217909002,2.08566338352181,
4.08907200122834));
#309292=CARTESIAN_POINT('Ctrl Pts',(-5.99112250266236,0.713090643414479,
4.15384735713948));
#309293=CARTESIAN_POINT('Ctrl Pts',(-6.03292388979285,0.0764271502393404,
4.18389319963645));
#309294=CARTESIAN_POINT('Ctrl Pts',(-5.91624513769634,-1.17978628549896,
4.24317725069079));
#309295=CARTESIAN_POINT('Ctrl Pts',(-5.76053056719885,-1.79168461261426,
4.27111370130226));
#309296=CARTESIAN_POINT('Ctrl Pts',(-5.51281765513233,-2.36829928456293,
4.30000000000162));
#309297=CARTESIAN_POINT('Origin',(2.99770677028732E-14,-1.99840144432528E-14,
-5.765625));
#309298=CARTESIAN_POINT('',(2.99770677028731E-14,-4.86334165753292,2.));
#309299=CARTESIAN_POINT('',(2.99770677028731E-14,-4.86334165753292,2.21875));
#309300=CARTESIAN_POINT('',(6.05497229851522E-14,-4.86334165753297,-5.765625));
#309301=CARTESIAN_POINT('Ctrl Pts',(-5.95587579405768E-16,-4.86334165753292,
2.21875));
#309302=CARTESIAN_POINT('Ctrl Pts',(1.58019549404244,-4.86334165753292,
2.30625));
#309303=CARTESIAN_POINT('Ctrl Pts',(2.85860050315749,-3.93452605039576,
2.39375));
#309304=CARTESIAN_POINT('Ctrl Pts',(4.13700551227253,-3.0057104432586,2.48125));
#309305=CARTESIAN_POINT('Ctrl Pts',(4.62531277436636,-1.5028552216293,2.56875));
#309306=CARTESIAN_POINT('Ctrl Pts',(5.11362003646019,7.95366714520796E-16,
2.65625));
#309307=CARTESIAN_POINT('Ctrl Pts',(4.62531277436636,1.5028552216293,2.74375));
#309308=CARTESIAN_POINT('Ctrl Pts',(4.13700551227253,3.0057104432586,2.83125));
#309309=CARTESIAN_POINT('Ctrl Pts',(2.85860050315749,3.93452605039576,2.91875));
#309310=CARTESIAN_POINT('Ctrl Pts',(1.58019549404244,4.86334165753292,3.00625));
#309311=CARTESIAN_POINT('Ctrl Pts',(0.,4.86334165753293,3.09375));
#309312=CARTESIAN_POINT('Ctrl Pts',(-0.613256677462664,4.86334165753293,
3.12770779793088));
#309313=CARTESIAN_POINT('Ctrl Pts',(-1.20731623616734,4.71110173778723,
3.16334165753294));
#309314=CARTESIAN_POINT('Ctrl Pts',(-5.95587579405768E-16,-4.86334165753292,
2.));
#309315=CARTESIAN_POINT('Ctrl Pts',(1.58019549404244,-4.86334165753292,
2.0875));
#309316=CARTESIAN_POINT('Ctrl Pts',(2.85860050315749,-3.93452605039576,
2.175));
#309317=CARTESIAN_POINT('Ctrl Pts',(4.13700551227253,-3.0057104432586,2.2625));
#309318=CARTESIAN_POINT('Ctrl Pts',(4.62531277436636,-1.5028552216293,2.35));
#309319=CARTESIAN_POINT('Ctrl Pts',(5.11362003646019,7.95366714520796E-16,
2.4375));
#309320=CARTESIAN_POINT('Ctrl Pts',(4.62531277436636,1.5028552216293,2.525));
#309321=CARTESIAN_POINT('Ctrl Pts',(4.13700551227253,3.0057104432586,2.6125));
#309322=CARTESIAN_POINT('Ctrl Pts',(2.85860050315749,3.93452605039576,2.7));
#309323=CARTESIAN_POINT('Ctrl Pts',(1.58019549404244,4.86334165753292,2.7875));
#309324=CARTESIAN_POINT('Ctrl Pts',(0.,4.86334165753293,2.875));
#309325=CARTESIAN_POINT('Ctrl Pts',(-1.58019549404244,4.86334165753292,
2.9625));
#309326=CARTESIAN_POINT('Ctrl Pts',(-2.85860050315749,3.93452605039576,
3.05));
#309327=CARTESIAN_POINT('Ctrl Pts',(-3.66754060707839,3.34679666228816,
3.10536763278335));
#309328=CARTESIAN_POINT('Ctrl Pts',(-4.17899100816594,2.48759446686254,
3.1633416575335));
#309329=CARTESIAN_POINT('Origin',(2.99770677028732E-14,-1.99840144432528E-14,
-5.765625));
#309330=CARTESIAN_POINT('',(2.99770677028731E-14,-4.86334165753292,0.25));
#309331=CARTESIAN_POINT('',(2.99770677028731E-14,-4.86334165753292,0.46875));
#309332=CARTESIAN_POINT('',(6.05497229851522E-14,-4.86334165753297,-5.765625));
#309333=CARTESIAN_POINT('Ctrl Pts',(-5.95587579405768E-16,-4.86334165753292,
0.46875));
#309334=CARTESIAN_POINT('Ctrl Pts',(1.58019549404244,-4.86334165753292,
0.556250000000001));
#309335=CARTESIAN_POINT('Ctrl Pts',(2.85860050315749,-3.93452605039576,
0.64375));
#309336=CARTESIAN_POINT('Ctrl Pts',(4.13700551227253,-3.0057104432586,0.731250000000001));
#309337=CARTESIAN_POINT('Ctrl Pts',(4.62531277436636,-1.5028552216293,0.81875));
#309338=CARTESIAN_POINT('Ctrl Pts',(5.11362003646019,7.95366714520796E-16,
0.906250000000001));
#309339=CARTESIAN_POINT('Ctrl Pts',(4.62531277436636,1.5028552216293,0.99375));
#309340=CARTESIAN_POINT('Ctrl Pts',(4.13700551227253,3.0057104432586,1.08125));
#309341=CARTESIAN_POINT('Ctrl Pts',(2.85860050315749,3.93452605039576,1.16875));
#309342=CARTESIAN_POINT('Ctrl Pts',(1.58019549404244,4.86334165753292,1.25625));
#309343=CARTESIAN_POINT('Ctrl Pts',(0.,4.86334165753293,1.34375));
#309344=CARTESIAN_POINT('Ctrl Pts',(-1.58019549404244,4.86334165753292,
1.43125));
#309345=CARTESIAN_POINT('Ctrl Pts',(-2.85860050315749,3.93452605039576,
1.51875));
#309346=CARTESIAN_POINT('Ctrl Pts',(-4.13700551227253,3.0057104432586,1.60625));
#309347=CARTESIAN_POINT('Ctrl Pts',(-4.62531277436636,1.5028552216293,1.69375));
#309348=CARTESIAN_POINT('Ctrl Pts',(-5.11362003646019,2.04784239646214E-15,
1.78125));
#309349=CARTESIAN_POINT('Ctrl Pts',(-4.62531277436636,-1.5028552216293,
1.86875));
#309350=CARTESIAN_POINT('Ctrl Pts',(-4.13700551227253,-3.00571044325859,
1.95625));
#309351=CARTESIAN_POINT('Ctrl Pts',(-2.85860050315749,-3.93452605039576,
2.04375));
#309352=CARTESIAN_POINT('Ctrl Pts',(-1.58019549404244,-4.86334165753292,
2.13125));
#309353=CARTESIAN_POINT('Ctrl Pts',(-5.95587579405768E-16,-4.86334165753292,
2.21875));
#309354=CARTESIAN_POINT('Ctrl Pts',(-5.95587579405768E-16,-4.86334165753292,
0.25));
#309355=CARTESIAN_POINT('Ctrl Pts',(1.58019549404244,-4.86334165753292,
0.337500000000001));
#309356=CARTESIAN_POINT('Ctrl Pts',(2.85860050315749,-3.93452605039576,
0.425));
#309357=CARTESIAN_POINT('Ctrl Pts',(4.13700551227253,-3.0057104432586,0.512500000000001));
#309358=CARTESIAN_POINT('Ctrl Pts',(4.62531277436636,-1.5028552216293,0.6));
#309359=CARTESIAN_POINT('Ctrl Pts',(5.11362003646019,7.95366714520796E-16,
0.687500000000001));
#309360=CARTESIAN_POINT('Ctrl Pts',(4.62531277436636,1.5028552216293,0.775));
#309361=CARTESIAN_POINT('Ctrl Pts',(4.13700551227253,3.0057104432586,0.8625));
#309362=CARTESIAN_POINT('Ctrl Pts',(2.85860050315749,3.93452605039576,0.95));
#309363=CARTESIAN_POINT('Ctrl Pts',(1.58019549404244,4.86334165753292,1.0375));
#309364=CARTESIAN_POINT('Ctrl Pts',(0.,4.86334165753293,1.125));
#309365=CARTESIAN_POINT('Ctrl Pts',(-1.58019549404244,4.86334165753292,
1.2125));
#309366=CARTESIAN_POINT('Ctrl Pts',(-2.85860050315749,3.93452605039576,
1.3));
#309367=CARTESIAN_POINT('Ctrl Pts',(-4.13700551227253,3.0057104432586,1.3875));
#309368=CARTESIAN_POINT('Ctrl Pts',(-4.62531277436636,1.5028552216293,1.475));
#309369=CARTESIAN_POINT('Ctrl Pts',(-5.11362003646019,2.04784239646214E-15,
1.5625));
#309370=CARTESIAN_POINT('Ctrl Pts',(-4.62531277436636,-1.5028552216293,
1.65));
#309371=CARTESIAN_POINT('Ctrl Pts',(-4.13700551227253,-3.00571044325859,
1.7375));
#309372=CARTESIAN_POINT('Ctrl Pts',(-2.85860050315749,-3.93452605039576,
1.825));
#309373=CARTESIAN_POINT('Ctrl Pts',(-1.58019549404244,-4.86334165753292,
1.9125));
#309374=CARTESIAN_POINT('Ctrl Pts',(-5.95587579405768E-16,-4.86334165753292,
2.));
#309375=CARTESIAN_POINT('Origin',(2.99770677028732E-14,-1.99840144432528E-14,
-5.765625));
#309376=CARTESIAN_POINT('',(2.99770677028731E-14,-4.86334165753292,-1.5));
#309377=CARTESIAN_POINT('',(2.99770677028731E-14,-4.86334165753292,-1.28125));
#309378=CARTESIAN_POINT('',(6.05497229851522E-14,-4.86334165753297,-5.765625));
#309379=CARTESIAN_POINT('Ctrl Pts',(-5.95587579405768E-16,-4.86334165753292,
-1.28125));
#309380=CARTESIAN_POINT('Ctrl Pts',(1.58019549404244,-4.86334165753292,
-1.19375));
#309381=CARTESIAN_POINT('Ctrl Pts',(2.85860050315749,-3.93452605039576,
-1.10625));
#309382=CARTESIAN_POINT('Ctrl Pts',(4.13700551227253,-3.0057104432586,-1.01875));
#309383=CARTESIAN_POINT('Ctrl Pts',(4.62531277436636,-1.5028552216293,-0.93125));
#309384=CARTESIAN_POINT('Ctrl Pts',(5.11362003646019,7.95366714520796E-16,
-0.843749999999999));
#309385=CARTESIAN_POINT('Ctrl Pts',(4.62531277436636,1.5028552216293,-0.75625));
#309386=CARTESIAN_POINT('Ctrl Pts',(4.13700551227253,3.0057104432586,-0.668749999999999));
#309387=CARTESIAN_POINT('Ctrl Pts',(2.85860050315749,3.93452605039576,-0.58125));
#309388=CARTESIAN_POINT('Ctrl Pts',(1.58019549404244,4.86334165753292,-0.49375));
#309389=CARTESIAN_POINT('Ctrl Pts',(0.,4.86334165753293,-0.40625));
#309390=CARTESIAN_POINT('Ctrl Pts',(-1.58019549404244,4.86334165753292,
-0.318749999999999));
#309391=CARTESIAN_POINT('Ctrl Pts',(-2.85860050315749,3.93452605039576,
-0.23125));
#309392=CARTESIAN_POINT('Ctrl Pts',(-4.13700551227253,3.0057104432586,-0.143749999999999));
#309393=CARTESIAN_POINT('Ctrl Pts',(-4.62531277436636,1.5028552216293,-0.056249999999999));
#309394=CARTESIAN_POINT('Ctrl Pts',(-5.11362003646019,2.04784239646214E-15,
0.0312500000000009));
#309395=CARTESIAN_POINT('Ctrl Pts',(-4.62531277436636,-1.5028552216293,
0.11875));
#309396=CARTESIAN_POINT('Ctrl Pts',(-4.13700551227253,-3.00571044325859,
0.20625));
#309397=CARTESIAN_POINT('Ctrl Pts',(-2.85860050315749,-3.93452605039576,
0.29375));
#309398=CARTESIAN_POINT('Ctrl Pts',(-1.58019549404244,-4.86334165753292,
0.381250000000001));
#309399=CARTESIAN_POINT('Ctrl Pts',(-5.95587579405768E-16,-4.86334165753292,
0.46875));
#309400=CARTESIAN_POINT('Ctrl Pts',(-5.95587579405768E-16,-4.86334165753292,
-1.5));
#309401=CARTESIAN_POINT('Ctrl Pts',(1.58019549404244,-4.86334165753292,
-1.4125));
#309402=CARTESIAN_POINT('Ctrl Pts',(2.85860050315749,-3.93452605039576,
-1.325));
#309403=CARTESIAN_POINT('Ctrl Pts',(4.13700551227253,-3.0057104432586,-1.2375));
#309404=CARTESIAN_POINT('Ctrl Pts',(4.62531277436636,-1.5028552216293,-1.15));
#309405=CARTESIAN_POINT('Ctrl Pts',(5.11362003646019,7.95366714520796E-16,
-1.0625));
#309406=CARTESIAN_POINT('Ctrl Pts',(4.62531277436636,1.5028552216293,-0.975));
#309407=CARTESIAN_POINT('Ctrl Pts',(4.13700551227253,3.0057104432586,-0.887499999999999));
#309408=CARTESIAN_POINT('Ctrl Pts',(2.85860050315749,3.93452605039576,-0.8));
#309409=CARTESIAN_POINT('Ctrl Pts',(1.58019549404244,4.86334165753292,-0.7125));
#309410=CARTESIAN_POINT('Ctrl Pts',(0.,4.86334165753293,-0.625));
#309411=CARTESIAN_POINT('Ctrl Pts',(-1.58019549404244,4.86334165753292,
-0.537499999999999));
#309412=CARTESIAN_POINT('Ctrl Pts',(-2.85860050315749,3.93452605039576,
-0.45));
#309413=CARTESIAN_POINT('Ctrl Pts',(-4.13700551227253,3.0057104432586,-0.362499999999999));
#309414=CARTESIAN_POINT('Ctrl Pts',(-4.62531277436636,1.5028552216293,-0.275));
#309415=CARTESIAN_POINT('Ctrl Pts',(-5.11362003646019,2.04784239646214E-15,
-0.187499999999999));
#309416=CARTESIAN_POINT('Ctrl Pts',(-4.62531277436636,-1.5028552216293,
-0.1));
#309417=CARTESIAN_POINT('Ctrl Pts',(-4.13700551227253,-3.00571044325859,
-0.0124999999999995));
#309418=CARTESIAN_POINT('Ctrl Pts',(-2.85860050315749,-3.93452605039576,
0.075));
#309419=CARTESIAN_POINT('Ctrl Pts',(-1.58019549404244,-4.86334165753292,
0.162500000000001));
#309420=CARTESIAN_POINT('Ctrl Pts',(-5.95587579405768E-16,-4.86334165753292,
0.25));
#309421=CARTESIAN_POINT('Origin',(2.99770677028732E-14,-1.99840144432528E-14,
-5.765625));
#309422=CARTESIAN_POINT('',(6.05497229851522E-14,-4.86334165753297,-3.16334165753295));
#309423=CARTESIAN_POINT('',(2.99770677028731E-14,-4.86334165753292,-3.03125));
#309424=CARTESIAN_POINT('',(6.05497229851522E-14,-4.86334165753297,-5.765625));
#309425=CARTESIAN_POINT('',(-2.21250112451954,-4.33092725081995,-3.16334165753294));
#309426=CARTESIAN_POINT('Origin',(2.99770677028732E-14,-1.99840144432528E-14,
-3.16334165753295));
#309427=CARTESIAN_POINT('Ctrl Pts',(-2.21250112451954,-4.33092725081995,
-3.16334165753294));
#309428=CARTESIAN_POINT('Ctrl Pts',(-1.17031043941251,-4.86334165753293,
-3.0960534776929));
#309429=CARTESIAN_POINT('Ctrl Pts',(-5.95587579405768E-16,-4.86334165753292,
-3.03125));
#309430=CARTESIAN_POINT('Ctrl Pts',(0.,6.09472152853892,-4.9453125));
#309431=CARTESIAN_POINT('Ctrl Pts',(-1.98029506767702,6.09472152853892,
-4.8578125));
#309432=CARTESIAN_POINT('Ctrl Pts',(-3.58238743130461,4.93073329257085,
-4.7703125));
#309433=CARTESIAN_POINT('Ctrl Pts',(-5.18447979493221,3.76674505660277,
-4.6828125));
#309434=CARTESIAN_POINT('Ctrl Pts',(-5.7964246247213,1.88337252830138,-4.5953125));
#309435=CARTESIAN_POINT('Ctrl Pts',(-6.40836945451038,2.1271229329878E-15,
-4.5078125));
#309436=CARTESIAN_POINT('Ctrl Pts',(-5.7964246247213,-1.88337252830138,
-4.4203125));
#309437=CARTESIAN_POINT('Ctrl Pts',(-5.18447979493221,-3.76674505660276,
-4.3328125));
#309438=CARTESIAN_POINT('Ctrl Pts',(-3.58238743130461,-4.93073329257084,
-4.2453125));
#309439=CARTESIAN_POINT('Ctrl Pts',(-1.98029506767702,-6.09472152853892,
-4.1578125));
#309440=CARTESIAN_POINT('Ctrl Pts',(-7.46388121161965E-16,-6.09472152853892,
-4.0703125));
#309441=CARTESIAN_POINT('Ctrl Pts',(1.98029506767702,-6.09472152853892,
-3.9828125));
#309442=CARTESIAN_POINT('Ctrl Pts',(3.58238743130461,-4.93073329257084,
-3.8953125));
#309443=CARTESIAN_POINT('Ctrl Pts',(5.18447979493221,-3.76674505660276,
-3.8078125));
#309444=CARTESIAN_POINT('Ctrl Pts',(5.7964246247213,-1.88337252830138,-3.7203125));
#309445=CARTESIAN_POINT('Ctrl Pts',(6.40836945451038,5.57525104943835E-16,
-3.6328125));
#309446=CARTESIAN_POINT('Ctrl Pts',(5.7964246247213,1.88337252830138,-3.5453125));
#309447=CARTESIAN_POINT('Ctrl Pts',(5.18447979493221,3.76674505660277,-3.4578125));
#309448=CARTESIAN_POINT('Ctrl Pts',(3.58238743130462,4.93073329257084,-3.3703125));
#309449=CARTESIAN_POINT('Ctrl Pts',(1.98029506767702,6.09472152853892,-3.2828125));
#309450=CARTESIAN_POINT('Ctrl Pts',(0.,6.09472152853892,-3.1953125));
#309451=CARTESIAN_POINT('Ctrl Pts',(-1.98029506767702,6.09472152853892,
-3.1078125));
#309452=CARTESIAN_POINT('Ctrl Pts',(-3.58238743130461,4.93073329257085,
-3.0203125));
#309453=CARTESIAN_POINT('Ctrl Pts',(-5.18447979493221,3.76674505660277,
-2.9328125));
#309454=CARTESIAN_POINT('Ctrl Pts',(-5.7964246247213,1.88337252830138,-2.8453125));
#309455=CARTESIAN_POINT('Ctrl Pts',(-6.40836945451038,2.1271229329878E-15,
-2.7578125));
#309456=CARTESIAN_POINT('Ctrl Pts',(-5.7964246247213,-1.88337252830138,
-2.6703125));
#309457=CARTESIAN_POINT('Ctrl Pts',(-5.18447979493221,-3.76674505660276,
-2.5828125));
#309458=CARTESIAN_POINT('Ctrl Pts',(-3.58238743130461,-4.93073329257084,
-2.4953125));
#309459=CARTESIAN_POINT('Ctrl Pts',(-1.98029506767702,-6.09472152853892,
-2.4078125));
#309460=CARTESIAN_POINT('Ctrl Pts',(-7.46388121161965E-16,-6.09472152853892,
-2.3203125));
#309461=CARTESIAN_POINT('Ctrl Pts',(1.98029506767702,-6.09472152853892,
-2.2328125));
#309462=CARTESIAN_POINT('Ctrl Pts',(3.58238743130461,-4.93073329257084,
-2.1453125));
#309463=CARTESIAN_POINT('Ctrl Pts',(5.18447979493221,-3.76674505660276,
-2.0578125));
#309464=CARTESIAN_POINT('Ctrl Pts',(5.7964246247213,-1.88337252830138,-1.9703125));
#309465=CARTESIAN_POINT('Ctrl Pts',(6.40836945451038,5.57525104943835E-16,
-1.8828125));
#309466=CARTESIAN_POINT('Ctrl Pts',(5.7964246247213,1.88337252830138,-1.7953125));
#309467=CARTESIAN_POINT('Ctrl Pts',(5.18447979493221,3.76674505660277,-1.7078125));
#309468=CARTESIAN_POINT('Ctrl Pts',(3.58238743130462,4.93073329257084,-1.6203125));
#309469=CARTESIAN_POINT('Ctrl Pts',(1.98029506767702,6.09472152853892,-1.5328125));
#309470=CARTESIAN_POINT('Ctrl Pts',(0.,6.09472152853892,-1.4453125));
#309471=CARTESIAN_POINT('Ctrl Pts',(-1.98029506767702,6.09472152853892,
-1.3578125));
#309472=CARTESIAN_POINT('Ctrl Pts',(-3.58238743130461,4.93073329257085,
-1.2703125));
#309473=CARTESIAN_POINT('Ctrl Pts',(-5.18447979493221,3.76674505660277,
-1.1828125));
#309474=CARTESIAN_POINT('Ctrl Pts',(-5.7964246247213,1.88337252830138,-1.0953125));
#309475=CARTESIAN_POINT('Ctrl Pts',(-6.40836945451038,2.1271229329878E-15,
-1.0078125));
#309476=CARTESIAN_POINT('Ctrl Pts',(-5.7964246247213,-1.88337252830138,
-0.9203125));
#309477=CARTESIAN_POINT('Ctrl Pts',(-5.18447979493221,-3.76674505660276,
-0.8328125));
#309478=CARTESIAN_POINT('Ctrl Pts',(-3.58238743130461,-4.93073329257084,
-0.7453125));
#309479=CARTESIAN_POINT('Ctrl Pts',(-1.98029506767702,-6.09472152853892,
-0.6578125));
#309480=CARTESIAN_POINT('Ctrl Pts',(-7.46388121161965E-16,-6.09472152853892,
-0.5703125));
#309481=CARTESIAN_POINT('Ctrl Pts',(1.98029506767702,-6.09472152853892,
-0.4828125));
#309482=CARTESIAN_POINT('Ctrl Pts',(3.58238743130461,-4.93073329257084,
-0.3953125));
#309483=CARTESIAN_POINT('Ctrl Pts',(5.18447979493221,-3.76674505660276,
-0.3078125));
#309484=CARTESIAN_POINT('Ctrl Pts',(5.7964246247213,-1.88337252830138,-0.2203125));
#309485=CARTESIAN_POINT('Ctrl Pts',(6.40836945451038,5.57525104943835E-16,
-0.1328125));
#309486=CARTESIAN_POINT('Ctrl Pts',(5.7964246247213,1.88337252830138,-0.0453125));
#309487=CARTESIAN_POINT('Ctrl Pts',(5.18447979493221,3.76674505660277,0.0421874999999997));
#309488=CARTESIAN_POINT('Ctrl Pts',(3.58238743130462,4.93073329257084,0.1296875));
#309489=CARTESIAN_POINT('Ctrl Pts',(1.98029506767702,6.09472152853892,0.217187499999999));
#309490=CARTESIAN_POINT('Ctrl Pts',(0.,6.09472152853892,0.3046875));
#309491=CARTESIAN_POINT('Ctrl Pts',(-1.98029506767702,6.09472152853892,
0.3921875));
#309492=CARTESIAN_POINT('Ctrl Pts',(-3.58238743130461,4.93073329257085,
0.4796875));
#309493=CARTESIAN_POINT('Ctrl Pts',(-5.18447979493221,3.76674505660277,
0.567187499999999));
#309494=CARTESIAN_POINT('Ctrl Pts',(-5.7964246247213,1.88337252830138,0.6546875));
#309495=CARTESIAN_POINT('Ctrl Pts',(-6.40836945451038,2.1271229329878E-15,
0.742187499999999));
#309496=CARTESIAN_POINT('Ctrl Pts',(-5.7964246247213,-1.88337252830138,
0.8296875));
#309497=CARTESIAN_POINT('Ctrl Pts',(-5.18447979493221,-3.76674505660276,
0.9171875));
#309498=CARTESIAN_POINT('Ctrl Pts',(-3.58238743130461,-4.93073329257084,
1.0046875));
#309499=CARTESIAN_POINT('Ctrl Pts',(-1.98029506767702,-6.09472152853892,
1.0921875));
#309500=CARTESIAN_POINT('Ctrl Pts',(-7.46388121161965E-16,-6.09472152853892,
1.1796875));
#309501=CARTESIAN_POINT('Ctrl Pts',(1.98029506767702,-6.09472152853892,
1.2671875));
#309502=CARTESIAN_POINT('Ctrl Pts',(3.58238743130461,-4.93073329257084,
1.3546875));
#309503=CARTESIAN_POINT('Ctrl Pts',(5.18447979493221,-3.76674505660276,
1.4421875));
#309504=CARTESIAN_POINT('Ctrl Pts',(5.7964246247213,-1.88337252830138,1.5296875));
#309505=CARTESIAN_POINT('Ctrl Pts',(6.40836945451038,5.57525104943835E-16,
1.6171875));
#309506=CARTESIAN_POINT('Ctrl Pts',(5.7964246247213,1.88337252830138,1.7046875));
#309507=CARTESIAN_POINT('Ctrl Pts',(5.18447979493221,3.76674505660277,1.7921875));
#309508=CARTESIAN_POINT('Ctrl Pts',(3.58238743130462,4.93073329257084,1.8796875));
#309509=CARTESIAN_POINT('Ctrl Pts',(1.98029506767702,6.09472152853892,1.9671875));
#309510=CARTESIAN_POINT('Ctrl Pts',(0.,6.09472152853892,2.0546875));
#309511=CARTESIAN_POINT('Ctrl Pts',(-1.98029506767702,6.09472152853892,
2.1421875));
#309512=CARTESIAN_POINT('Ctrl Pts',(-3.58238743130461,4.93073329257085,
2.2296875));
#309513=CARTESIAN_POINT('Ctrl Pts',(-5.18447979493221,3.76674505660277,
2.3171875));
#309514=CARTESIAN_POINT('Ctrl Pts',(-5.7964246247213,1.88337252830138,2.4046875));
#309515=CARTESIAN_POINT('Ctrl Pts',(-6.40836945451038,2.1271229329878E-15,
2.4921875));
#309516=CARTESIAN_POINT('Ctrl Pts',(-5.7964246247213,-1.88337252830138,
2.5796875));
#309517=CARTESIAN_POINT('Ctrl Pts',(-5.18447979493221,-3.76674505660276,
2.6671875));
#309518=CARTESIAN_POINT('Ctrl Pts',(-3.58238743130461,-4.93073329257084,
2.7546875));
#309519=CARTESIAN_POINT('Ctrl Pts',(-1.98029506767702,-6.09472152853892,
2.8421875));
#309520=CARTESIAN_POINT('Ctrl Pts',(-7.46388121161965E-16,-6.09472152853892,
2.9296875));
#309521=CARTESIAN_POINT('Ctrl Pts',(1.98029506767702,-6.09472152853892,
3.0171875));
#309522=CARTESIAN_POINT('Ctrl Pts',(3.58238743130461,-4.93073329257084,
3.1046875));
#309523=CARTESIAN_POINT('Ctrl Pts',(5.18447979493221,-3.76674505660276,
3.1921875));
#309524=CARTESIAN_POINT('Ctrl Pts',(5.7964246247213,-1.88337252830138,3.2796875));
#309525=CARTESIAN_POINT('Ctrl Pts',(6.40836945451038,5.57525104943835E-16,
3.3671875));
#309526=CARTESIAN_POINT('Ctrl Pts',(5.7964246247213,1.88337252830138,3.4546875));
#309527=CARTESIAN_POINT('Ctrl Pts',(5.18447979493221,3.76674505660277,3.5421875));
#309528=CARTESIAN_POINT('Ctrl Pts',(3.58238743130462,4.93073329257084,3.6296875));
#309529=CARTESIAN_POINT('Ctrl Pts',(1.98029506767702,6.09472152853892,3.7171875));
#309530=CARTESIAN_POINT('Ctrl Pts',(0.,6.09472152853892,3.8046875));
#309531=CARTESIAN_POINT('Ctrl Pts',(-1.98029506767702,6.09472152853892,
3.8921875));
#309532=CARTESIAN_POINT('Ctrl Pts',(-3.58238743130461,4.93073329257085,
3.9796875));
#309533=CARTESIAN_POINT('Ctrl Pts',(-5.18447979493221,3.76674505660277,
4.0671875));
#309534=CARTESIAN_POINT('Ctrl Pts',(-5.7964246247213,1.88337252830138,4.1546875));
#309535=CARTESIAN_POINT('Ctrl Pts',(-6.40836945451038,2.1271229329878E-15,
4.2421875));
#309536=CARTESIAN_POINT('Ctrl Pts',(-5.7964246247213,-1.88337252830138,
4.3296875));
#309537=CARTESIAN_POINT('Ctrl Pts',(-5.18447979493221,-3.76674505660276,
4.4171875));
#309538=CARTESIAN_POINT('Ctrl Pts',(-3.58238743130461,-4.93073329257084,
4.5046875));
#309539=CARTESIAN_POINT('Ctrl Pts',(-1.98029506767702,-6.09472152853892,
4.5921875));
#309540=CARTESIAN_POINT('Ctrl Pts',(-7.46388121161965E-16,-6.09472152853892,
4.6796875));
#309541=CARTESIAN_POINT('Ctrl Pts',(1.98029506767702,-6.09472152853892,
4.7671875));
#309542=CARTESIAN_POINT('Ctrl Pts',(3.58238743130461,-4.93073329257084,
4.8546875));
#309543=CARTESIAN_POINT('Ctrl Pts',(5.18447979493221,-3.76674505660276,
4.9421875));
#309544=CARTESIAN_POINT('Ctrl Pts',(5.7964246247213,-1.88337252830138,5.0296875));
#309545=CARTESIAN_POINT('Ctrl Pts',(6.40836945451038,5.57525104943835E-16,
5.1171875));
#309546=CARTESIAN_POINT('Ctrl Pts',(5.7964246247213,1.88337252830138,5.2046875));
#309547=CARTESIAN_POINT('Ctrl Pts',(5.18447979493221,3.76674505660277,5.2921875));
#309548=CARTESIAN_POINT('Ctrl Pts',(3.58238743130462,4.93073329257084,5.3796875));
#309549=CARTESIAN_POINT('Ctrl Pts',(1.98029506767702,6.09472152853892,5.4671875));
#309550=CARTESIAN_POINT('Ctrl Pts',(0.,6.09472152853892,5.5546875));
#309551=CARTESIAN_POINT('Ctrl Pts',(-1.98029506767702,6.09472152853892,
5.6421875));
#309552=CARTESIAN_POINT('Ctrl Pts',(-3.58238743130461,4.93073329257085,
5.7296875));
#309553=CARTESIAN_POINT('Ctrl Pts',(-5.18447979493221,3.76674505660277,
5.81718749999999));
#309554=CARTESIAN_POINT('Ctrl Pts',(-5.7964246247213,1.88337252830138,5.9046875));
#309555=CARTESIAN_POINT('Ctrl Pts',(-6.40836945451038,2.1271229329878E-15,
5.9921875));
#309556=CARTESIAN_POINT('Ctrl Pts',(-5.7964246247213,-1.88337252830138,
6.0796875));
#309557=CARTESIAN_POINT('Ctrl Pts',(-5.18447979493221,-3.76674505660276,
6.1671875));
#309558=CARTESIAN_POINT('Ctrl Pts',(-3.58238743130461,-4.93073329257084,
6.2546875));
#309559=CARTESIAN_POINT('Ctrl Pts',(-1.98029506767702,-6.09472152853892,
6.3421875));
#309560=CARTESIAN_POINT('Ctrl Pts',(-7.46388121161965E-16,-6.09472152853892,
6.4296875));
#309561=CARTESIAN_POINT('Ctrl Pts',(1.98029506767702,-6.09472152853892,
6.5171875));
#309562=CARTESIAN_POINT('Ctrl Pts',(3.58238743130461,-4.93073329257084,
6.6046875));
#309563=CARTESIAN_POINT('Ctrl Pts',(5.18447979493221,-3.76674505660276,
6.69218749999999));
#309564=CARTESIAN_POINT('Ctrl Pts',(5.7964246247213,-1.88337252830138,6.7796875));
#309565=CARTESIAN_POINT('Ctrl Pts',(5.88101053842786,-1.6230438542098,6.79178216456621));
#309566=CARTESIAN_POINT('Ctrl Pts',(5.94191924599894,-1.35618073443886,
6.80418041431716));
#309567=CARTESIAN_POINT('Ctrl Pts',(0.,4.8633208818601,-5.6562619948403));
#309568=CARTESIAN_POINT('Ctrl Pts',(-1.58018874361713,4.86332088186009,
-5.5687619948403));
#309569=CARTESIAN_POINT('Ctrl Pts',(-2.85858829152339,3.93450924252337,
-5.4812619948403));
#309570=CARTESIAN_POINT('Ctrl Pts',(-4.13698783942964,3.00569760318665,
-5.39376199484029));
#309571=CARTESIAN_POINT('Ctrl Pts',(-4.62529301552733,1.50284880159333,
-5.3062619948403));
#309572=CARTESIAN_POINT('Ctrl Pts',(-5.11359819162502,2.04784105885177E-15,
-5.2187619948403));
#309573=CARTESIAN_POINT('Ctrl Pts',(-4.62529301552733,-1.50284880159332,
-5.1312619948403));
#309574=CARTESIAN_POINT('Ctrl Pts',(-4.13698783942964,-3.00569760318664,
-5.0437619948403));
#309575=CARTESIAN_POINT('Ctrl Pts',(-2.85858829152339,-3.93450924252337,
-4.9562619948403));
#309576=CARTESIAN_POINT('Ctrl Pts',(-1.58018874361713,-4.86332088186009,
-4.8687619948403));
#309577=CARTESIAN_POINT('Ctrl Pts',(-5.95585035119645E-16,-4.86332088186009,
-4.7812619948403));
#309578=CARTESIAN_POINT('Ctrl Pts',(1.58018874361713,-4.86332088186009,
-4.6937619948403));
#309579=CARTESIAN_POINT('Ctrl Pts',(2.85858829152339,-3.93450924252337,
-4.6062619948403));
#309580=CARTESIAN_POINT('Ctrl Pts',(4.13698783942964,-3.00569760318665,
-4.5187619948403));
#309581=CARTESIAN_POINT('Ctrl Pts',(4.62529301552733,-1.50284880159333,
-4.4312619948403));
#309582=CARTESIAN_POINT('Ctrl Pts',(5.11359819162502,7.95370727351915E-16,
-4.3437619948403));
#309583=CARTESIAN_POINT('Ctrl Pts',(4.62529301552733,1.50284880159333,-4.2562619948403));
#309584=CARTESIAN_POINT('Ctrl Pts',(4.13698783942964,3.00569760318665,-4.1687619948403));
#309585=CARTESIAN_POINT('Ctrl Pts',(2.85858829152339,3.93450924252337,-4.0812619948403));
#309586=CARTESIAN_POINT('Ctrl Pts',(1.58018874361713,4.86332088186009,-3.9937619948403));
#309587=CARTESIAN_POINT('Ctrl Pts',(0.,4.8633208818601,-3.9062619948403));
#309588=CARTESIAN_POINT('Ctrl Pts',(-1.58018874361713,4.86332088186009,
-3.8187619948403));
#309589=CARTESIAN_POINT('Ctrl Pts',(-2.85858829152339,3.93450924252337,
-3.7312619948403));
#309590=CARTESIAN_POINT('Ctrl Pts',(-4.13698783942964,3.00569760318665,
-3.6437619948403));
#309591=CARTESIAN_POINT('Ctrl Pts',(-4.62529301552733,1.50284880159333,
-3.5562619948403));
#309592=CARTESIAN_POINT('Ctrl Pts',(-5.11359819162502,2.04784105885177E-15,
-3.4687619948403));
#309593=CARTESIAN_POINT('Ctrl Pts',(-4.62529301552733,-1.50284880159332,
-3.3812619948403));
#309594=CARTESIAN_POINT('Ctrl Pts',(-4.13698783942964,-3.00569760318664,
-3.2937619948403));
#309595=CARTESIAN_POINT('Ctrl Pts',(-2.85858829152339,-3.93450924252337,
-3.2062619948403));
#309596=CARTESIAN_POINT('Ctrl Pts',(-1.58018874361713,-4.86332088186009,
-3.1187619948403));
#309597=CARTESIAN_POINT('Ctrl Pts',(-5.95585035119645E-16,-4.86332088186009,
-3.0312619948403));
#309598=CARTESIAN_POINT('Ctrl Pts',(1.58018874361713,-4.86332088186009,
-2.9437619948403));
#309599=CARTESIAN_POINT('Ctrl Pts',(2.85858829152339,-3.93450924252337,
-2.8562619948403));
#309600=CARTESIAN_POINT('Ctrl Pts',(4.13698783942964,-3.00569760318665,
-2.7687619948403));
#309601=CARTESIAN_POINT('Ctrl Pts',(4.62529301552733,-1.50284880159333,
-2.6812619948403));
#309602=CARTESIAN_POINT('Ctrl Pts',(5.11359819162502,7.95370727351915E-16,
-2.5937619948403));
#309603=CARTESIAN_POINT('Ctrl Pts',(4.62529301552733,1.50284880159333,-2.5062619948403));
#309604=CARTESIAN_POINT('Ctrl Pts',(4.13698783942964,3.00569760318665,-2.4187619948403));
#309605=CARTESIAN_POINT('Ctrl Pts',(2.85858829152339,3.93450924252337,-2.3312619948403));
#309606=CARTESIAN_POINT('Ctrl Pts',(1.58018874361713,4.86332088186009,-2.2437619948403));
#309607=CARTESIAN_POINT('Ctrl Pts',(0.,4.8633208818601,-2.1562619948403));
#309608=CARTESIAN_POINT('Ctrl Pts',(-1.58018874361713,4.86332088186009,
-2.0687619948403));
#309609=CARTESIAN_POINT('Ctrl Pts',(-2.85858829152339,3.93450924252337,
-1.9812619948403));
#309610=CARTESIAN_POINT('Ctrl Pts',(-4.13698783942964,3.00569760318665,
-1.8937619948403));
#309611=CARTESIAN_POINT('Ctrl Pts',(-4.62529301552733,1.50284880159333,
-1.8062619948403));
#309612=CARTESIAN_POINT('Ctrl Pts',(-5.11359819162502,2.04784105885177E-15,
-1.7187619948403));
#309613=CARTESIAN_POINT('Ctrl Pts',(-4.62529301552733,-1.50284880159332,
-1.6312619948403));
#309614=CARTESIAN_POINT('Ctrl Pts',(-4.13698783942964,-3.00569760318664,
-1.5437619948403));
#309615=CARTESIAN_POINT('Ctrl Pts',(-2.85858829152339,-3.93450924252337,
-1.4562619948403));
#309616=CARTESIAN_POINT('Ctrl Pts',(-1.58018874361713,-4.86332088186009,
-1.3687619948403));
#309617=CARTESIAN_POINT('Ctrl Pts',(-5.95585035119645E-16,-4.86332088186009,
-1.2812619948403));
#309618=CARTESIAN_POINT('Ctrl Pts',(1.58018874361713,-4.86332088186009,
-1.1937619948403));
#309619=CARTESIAN_POINT('Ctrl Pts',(2.85858829152339,-3.93450924252337,
-1.1062619948403));
#309620=CARTESIAN_POINT('Ctrl Pts',(4.13698783942964,-3.00569760318665,
-1.0187619948403));
#309621=CARTESIAN_POINT('Ctrl Pts',(4.62529301552733,-1.50284880159333,
-0.931261994840301));
#309622=CARTESIAN_POINT('Ctrl Pts',(5.11359819162502,7.95370727351915E-16,
-0.8437619948403));
#309623=CARTESIAN_POINT('Ctrl Pts',(4.62529301552733,1.50284880159333,-0.756261994840301));
#309624=CARTESIAN_POINT('Ctrl Pts',(4.13698783942964,3.00569760318665,-0.6687619948403));
#309625=CARTESIAN_POINT('Ctrl Pts',(2.85858829152339,3.93450924252337,-0.581261994840301));
#309626=CARTESIAN_POINT('Ctrl Pts',(1.58018874361713,4.86332088186009,-0.493761994840301));
#309627=CARTESIAN_POINT('Ctrl Pts',(0.,4.8633208818601,-0.406261994840301));
#309628=CARTESIAN_POINT('Ctrl Pts',(-1.58018874361713,4.86332088186009,
-0.3187619948403));
#309629=CARTESIAN_POINT('Ctrl Pts',(-2.85858829152339,3.93450924252337,
-0.231261994840301));
#309630=CARTESIAN_POINT('Ctrl Pts',(-4.13698783942964,3.00569760318665,
-0.1437619948403));
#309631=CARTESIAN_POINT('Ctrl Pts',(-4.62529301552733,1.50284880159333,
-0.0562619948403003));
#309632=CARTESIAN_POINT('Ctrl Pts',(-5.11359819162502,2.04784105885177E-15,
0.0312380051596996));
#309633=CARTESIAN_POINT('Ctrl Pts',(-4.62529301552733,-1.50284880159332,
0.118738005159699));
#309634=CARTESIAN_POINT('Ctrl Pts',(-4.13698783942964,-3.00569760318664,
0.206238005159699));
#309635=CARTESIAN_POINT('Ctrl Pts',(-2.85858829152339,-3.93450924252337,
0.293738005159699));
#309636=CARTESIAN_POINT('Ctrl Pts',(-1.58018874361713,-4.86332088186009,
0.3812380051597));
#309637=CARTESIAN_POINT('Ctrl Pts',(-5.95585035119645E-16,-4.86332088186009,
0.468738005159699));
#309638=CARTESIAN_POINT('Ctrl Pts',(1.58018874361713,-4.86332088186009,
0.5562380051597));
#309639=CARTESIAN_POINT('Ctrl Pts',(2.85858829152339,-3.93450924252337,
0.643738005159699));
#309640=CARTESIAN_POINT('Ctrl Pts',(4.13698783942964,-3.00569760318665,
0.7312380051597));
#309641=CARTESIAN_POINT('Ctrl Pts',(4.62529301552733,-1.50284880159333,
0.818738005159699));
#309642=CARTESIAN_POINT('Ctrl Pts',(5.11359819162502,7.95370727351915E-16,
0.9062380051597));
#309643=CARTESIAN_POINT('Ctrl Pts',(4.62529301552733,1.50284880159333,0.993738005159699));
#309644=CARTESIAN_POINT('Ctrl Pts',(4.13698783942964,3.00569760318665,1.0812380051597));
#309645=CARTESIAN_POINT('Ctrl Pts',(2.85858829152339,3.93450924252337,1.1687380051597));
#309646=CARTESIAN_POINT('Ctrl Pts',(1.58018874361713,4.86332088186009,1.2562380051597));
#309647=CARTESIAN_POINT('Ctrl Pts',(0.,4.8633208818601,1.3437380051597));
#309648=CARTESIAN_POINT('Ctrl Pts',(-1.58018874361713,4.86332088186009,
1.4312380051597));
#309649=CARTESIAN_POINT('Ctrl Pts',(-2.85858829152339,3.93450924252337,
1.5187380051597));
#309650=CARTESIAN_POINT('Ctrl Pts',(-4.13698783942964,3.00569760318665,
1.6062380051597));
#309651=CARTESIAN_POINT('Ctrl Pts',(-4.62529301552733,1.50284880159333,
1.6937380051597));
#309652=CARTESIAN_POINT('Ctrl Pts',(-5.11359819162502,2.04784105885177E-15,
1.7812380051597));
#309653=CARTESIAN_POINT('Ctrl Pts',(-4.62529301552733,-1.50284880159332,
1.8687380051597));
#309654=CARTESIAN_POINT('Ctrl Pts',(-4.13698783942964,-3.00569760318664,
1.9562380051597));
#309655=CARTESIAN_POINT('Ctrl Pts',(-2.85858829152339,-3.93450924252337,
2.0437380051597));
#309656=CARTESIAN_POINT('Ctrl Pts',(-1.58018874361713,-4.86332088186009,
2.1312380051597));
#309657=CARTESIAN_POINT('Ctrl Pts',(-5.95585035119645E-16,-4.86332088186009,
2.2187380051597));
#309658=CARTESIAN_POINT('Ctrl Pts',(1.58018874361713,-4.86332088186009,
2.3062380051597));
#309659=CARTESIAN_POINT('Ctrl Pts',(2.85858829152339,-3.93450924252337,
2.3937380051597));
#309660=CARTESIAN_POINT('Ctrl Pts',(4.13698783942964,-3.00569760318665,
2.4812380051597));
#309661=CARTESIAN_POINT('Ctrl Pts',(4.62529301552733,-1.50284880159333,
2.5687380051597));
#309662=CARTESIAN_POINT('Ctrl Pts',(5.11359819162502,7.95370727351915E-16,
2.6562380051597));
#309663=CARTESIAN_POINT('Ctrl Pts',(4.62529301552733,1.50284880159333,2.7437380051597));
#309664=CARTESIAN_POINT('Ctrl Pts',(4.13698783942964,3.00569760318665,2.8312380051597));
#309665=CARTESIAN_POINT('Ctrl Pts',(2.85858829152339,3.93450924252337,2.9187380051597));
#309666=CARTESIAN_POINT('Ctrl Pts',(1.58018874361713,4.86332088186009,3.0062380051597));
#309667=CARTESIAN_POINT('Ctrl Pts',(0.,4.8633208818601,3.0937380051597));
#309668=CARTESIAN_POINT('Ctrl Pts',(-1.58018874361713,4.86332088186009,
3.1812380051597));
#309669=CARTESIAN_POINT('Ctrl Pts',(-2.85858829152339,3.93450924252337,
3.2687380051597));
#309670=CARTESIAN_POINT('Ctrl Pts',(-4.13698783942964,3.00569760318665,
3.3562380051597));
#309671=CARTESIAN_POINT('Ctrl Pts',(-4.62529301552733,1.50284880159333,
3.4437380051597));
#309672=CARTESIAN_POINT('Ctrl Pts',(-5.11359819162502,2.04784105885177E-15,
3.5312380051597));
#309673=CARTESIAN_POINT('Ctrl Pts',(-4.62529301552733,-1.50284880159332,
3.6187380051597));
#309674=CARTESIAN_POINT('Ctrl Pts',(-4.13698783942964,-3.00569760318664,
3.7062380051597));
#309675=CARTESIAN_POINT('Ctrl Pts',(-2.85858829152339,-3.93450924252337,
3.7937380051597));
#309676=CARTESIAN_POINT('Ctrl Pts',(-1.58018874361713,-4.86332088186009,
3.8812380051597));
#309677=CARTESIAN_POINT('Ctrl Pts',(-5.95585035119645E-16,-4.86332088186009,
3.9687380051597));
#309678=CARTESIAN_POINT('Ctrl Pts',(1.58018874361713,-4.86332088186009,
4.0562380051597));
#309679=CARTESIAN_POINT('Ctrl Pts',(2.85858829152339,-3.93450924252337,
4.1437380051597));
#309680=CARTESIAN_POINT('Ctrl Pts',(4.13698783942964,-3.00569760318665,
4.2312380051597));
#309681=CARTESIAN_POINT('Ctrl Pts',(4.62529301552733,-1.50284880159333,
4.3187380051597));
#309682=CARTESIAN_POINT('Ctrl Pts',(5.11359819162502,7.95370727351915E-16,
4.4062380051597));
#309683=CARTESIAN_POINT('Ctrl Pts',(4.62529301552733,1.50284880159333,4.4937380051597));
#309684=CARTESIAN_POINT('Ctrl Pts',(4.13698783942964,3.00569760318665,4.5812380051597));
#309685=CARTESIAN_POINT('Ctrl Pts',(2.85858829152339,3.93450924252337,4.6687380051597));
#309686=CARTESIAN_POINT('Ctrl Pts',(1.58018874361713,4.86332088186009,4.7562380051597));
#309687=CARTESIAN_POINT('Ctrl Pts',(0.,4.8633208818601,4.8437380051597));
#309688=CARTESIAN_POINT('Ctrl Pts',(-1.58018874361713,4.86332088186009,
4.9312380051597));
#309689=CARTESIAN_POINT('Ctrl Pts',(-2.85858829152339,3.93450924252337,
5.0187380051597));
#309690=CARTESIAN_POINT('Ctrl Pts',(-4.13698783942964,3.00569760318665,
5.1062380051597));
#309691=CARTESIAN_POINT('Ctrl Pts',(-4.62529301552733,1.50284880159333,
5.1937380051597));
#309692=CARTESIAN_POINT('Ctrl Pts',(-5.11359819162502,2.04784105885177E-15,
5.2812380051597));
#309693=CARTESIAN_POINT('Ctrl Pts',(-4.62529301552733,-1.50284880159332,
5.3687380051597));
#309694=CARTESIAN_POINT('Ctrl Pts',(-4.13698783942964,-3.00569760318664,
5.45623800515969));
#309695=CARTESIAN_POINT('Ctrl Pts',(-2.85858829152339,-3.93450924252337,
5.5437380051597));
#309696=CARTESIAN_POINT('Ctrl Pts',(-1.58018874361713,-4.86332088186009,
5.6312380051597));
#309697=CARTESIAN_POINT('Ctrl Pts',(-5.95585035119645E-16,-4.86332088186009,
5.7187380051597));
#309698=CARTESIAN_POINT('Ctrl Pts',(1.58018874361713,-4.86332088186009,
5.8062380051597));
#309699=CARTESIAN_POINT('Ctrl Pts',(2.85858829152339,-3.93450924252337,
5.8937380051597));
#309700=CARTESIAN_POINT('Ctrl Pts',(4.13698783942964,-3.00569760318665,
5.9812380051597));
#309701=CARTESIAN_POINT('Ctrl Pts',(4.62529301552733,-1.50284880159333,
6.0687380051597));
#309702=CARTESIAN_POINT('Ctrl Pts',(4.69278887050841,-1.2951179198905,6.0808326697259));
#309703=CARTESIAN_POINT('Ctrl Pts',(4.74139135185731,-1.08217283668972,
6.09323091947686));
#309704=CARTESIAN_POINT('Ctrl Pts',(6.,2.65065747129256E-14,1.5625));
#309705=CARTESIAN_POINT('Ctrl Pts',(6.,0.473732133569272,1.58485667856562));
#309706=CARTESIAN_POINT('Ctrl Pts',(5.94389257800599,0.946895016021675,
1.6071864926588));
#309707=CARTESIAN_POINT('Ctrl Pts',(5.64770904370383,2.17244600347447,1.66502350127759));
#309708=CARTESIAN_POINT('Ctrl Pts',(5.31536957028271,2.89188711817904,1.70046744841851));
#309709=CARTESIAN_POINT('Ctrl Pts',(4.39895257827164,4.15311566791862,1.77404135550628));
#309710=CARTESIAN_POINT('Ctrl Pts',(3.82704939643144,4.68538294493608,1.80905948364897));
#309711=CARTESIAN_POINT('Ctrl Pts',(2.49846473521043,5.51207511269938,1.88074612354776));
#309712=CARTESIAN_POINT('Ctrl Pts',(1.7510721703992,5.79301286248726,1.91838826687317));
#309713=CARTESIAN_POINT('Ctrl Pts',(0.204147040411568,6.04663706712432,
1.99151741577544));
#309714=CARTESIAN_POINT('Ctrl Pts',(-0.579605426814209,6.02225380331358,
2.02568982903828));
#309715=CARTESIAN_POINT('Ctrl Pts',(-2.09637414501486,5.67557241238266,
2.09882255514758));
#309716=CARTESIAN_POINT('Ctrl Pts',(-2.81483629742654,5.35571705240381,
2.13573376658461));
#309717=CARTESIAN_POINT('Ctrl Pts',(-4.10127598593334,4.45079123039165,
2.20666972598103));
#309718=CARTESIAN_POINT('Ctrl Pts',(-4.65351072191004,3.86976109467243,
2.24383825254408));
#309719=CARTESIAN_POINT('Ctrl Pts',(-5.48891111541853,2.54363857790455,
2.31764245793256));
#309720=CARTESIAN_POINT('Ctrl Pts',(-5.7707654703417,1.81563335639617,2.35181543594963));
#309721=CARTESIAN_POINT('Ctrl Pts',(-6.04470409317909,0.280751068370845,
2.42425061084664));
#309722=CARTESIAN_POINT('Ctrl Pts',(-6.02949439172197,-0.512333236812288,
2.46167836723043));
#309723=CARTESIAN_POINT('Ctrl Pts',(-5.69499213987656,-2.04431033388393,
2.53397643844432));
#309724=CARTESIAN_POINT('Ctrl Pts',(-5.38018169086334,-2.76871518145314,
2.56896695243465));
#309725=CARTESIAN_POINT('Ctrl Pts',(-4.49451807829644,-4.04966880786669,
2.64244088373343));
#309726=CARTESIAN_POINT('Ctrl Pts',(-3.93448113525675,-4.59568124109636,
2.67792948743115));
#309727=CARTESIAN_POINT('Ctrl Pts',(-2.62304423346144,-5.45415327610023,
2.7493099428143));
#309728=CARTESIAN_POINT('Ctrl Pts',(-1.88046359937015,-5.75255908400189,
2.78699085532114));
#309729=CARTESIAN_POINT('Ctrl Pts',(-0.339071917529684,-6.04040283393684,
2.86037068214262));
#309730=CARTESIAN_POINT('Ctrl Pts',(0.443667288736679,-6.03362176991941,
2.89442275038474));
#309731=CARTESIAN_POINT('Ctrl Pts',(1.96832289167546,-5.72147630793342,
2.96740581367033));
#309732=CARTESIAN_POINT('Ctrl Pts',(2.69537329403833,-5.41706837063913,
3.00447721562741));
#309733=CARTESIAN_POINT('Ctrl Pts',(3.99992726994981,-4.54149783876324,
3.07579809851961));
#309734=CARTESIAN_POINT('Ctrl Pts',(4.5627506802707,-3.97568211547479,3.11227661747247));
#309735=CARTESIAN_POINT('Ctrl Pts',(5.42726028909776,-2.67262381178519,
3.18600770383688));
#309736=CARTESIAN_POINT('Ctrl Pts',(5.72620297456507,-1.95158464272292,
3.22039953338864));
#309737=CARTESIAN_POINT('Ctrl Pts',(5.96001028500831,-0.799856624140742,
3.27475263988459));
#309738=CARTESIAN_POINT('Ctrl Pts',(6.,-0.39994790712138,3.29362539519932));
#309739=CARTESIAN_POINT('Ctrl Pts',(6.,4.85722573273506E-14,3.31250000000001));
#309740=CARTESIAN_POINT('Ctrl Pts',(-5.51281765513598,-2.36829928456402,
4.30000000000379));
#309741=CARTESIAN_POINT('Ctrl Pts',(-5.65503173457777,-1.9040941811954,
4.24743727896327));
#309742=CARTESIAN_POINT('Ctrl Pts',(-5.79869704924777,-1.24715028022825,
4.17742481762423));
#309743=CARTESIAN_POINT('Ctrl Pts',(-5.76255122889151,-0.295979987394846,
4.06824939279623));
#309744=CARTESIAN_POINT('Ctrl Pts',(-5.75106682344018,-0.147589105085812,
4.05106682344018));
#309745=CARTESIAN_POINT('Ctrl Pts',(-5.73382214207426,-1.18860743158296E-14,
4.03382214207426));
#309746=CARTESIAN_POINT('Ctrl Pts',(-5.95587579405768E-16,-4.86334165753292,
-3.03125));
#309747=CARTESIAN_POINT('Ctrl Pts',(1.58019549404244,-4.86334165753292,
-2.94375));
#309748=CARTESIAN_POINT('Ctrl Pts',(2.85860050315749,-3.93452605039576,
-2.85625));
#309749=CARTESIAN_POINT('Ctrl Pts',(4.13700551227253,-3.0057104432586,-2.76875));
#309750=CARTESIAN_POINT('Ctrl Pts',(4.62531277436636,-1.5028552216293,-2.68125));
#309751=CARTESIAN_POINT('Ctrl Pts',(5.11362003646019,7.95366714520796E-16,
-2.59375));
#309752=CARTESIAN_POINT('Ctrl Pts',(4.62531277436636,1.5028552216293,-2.50625));
#309753=CARTESIAN_POINT('Ctrl Pts',(4.13700551227253,3.0057104432586,-2.41875));
#309754=CARTESIAN_POINT('Ctrl Pts',(2.85860050315749,3.93452605039576,-2.33125));
#309755=CARTESIAN_POINT('Ctrl Pts',(1.58019549404244,4.86334165753292,-2.24375));
#309756=CARTESIAN_POINT('Ctrl Pts',(0.,4.86334165753293,-2.15625));
#309757=CARTESIAN_POINT('Ctrl Pts',(-1.58019549404244,4.86334165753292,
-2.06875));
#309758=CARTESIAN_POINT('Ctrl Pts',(-2.85860050315749,3.93452605039576,
-1.98125));
#309759=CARTESIAN_POINT('Ctrl Pts',(-4.13700551227253,3.0057104432586,-1.89375));
#309760=CARTESIAN_POINT('Ctrl Pts',(-4.62531277436636,1.5028552216293,-1.80625));
#309761=CARTESIAN_POINT('Ctrl Pts',(-5.11362003646019,2.04784239646214E-15,
-1.71875));
#309762=CARTESIAN_POINT('Ctrl Pts',(-4.62531277436636,-1.5028552216293,
-1.63125));
#309763=CARTESIAN_POINT('Ctrl Pts',(-4.13700551227253,-3.00571044325859,
-1.54375));
#309764=CARTESIAN_POINT('Ctrl Pts',(-2.85860050315749,-3.93452605039576,
-1.45625));
#309765=CARTESIAN_POINT('Ctrl Pts',(-1.58019549404244,-4.86334165753292,
-1.36875));
#309766=CARTESIAN_POINT('Ctrl Pts',(-5.95587579405768E-16,-4.86334165753292,
-1.28125));
#309767=CARTESIAN_POINT('',(5.61169055981797,-3.60964178854093E-16,-3.91169055981797));
#309768=CARTESIAN_POINT('Ctrl Pts',(-2.21250112451911,-4.33092725082016,
-3.16334165753291));
#309769=CARTESIAN_POINT('Ctrl Pts',(-2.60719450358133,-4.14710387972064,
-3.17920192465262));
#309770=CARTESIAN_POINT('Ctrl Pts',(-2.97433163955537,-3.91057564075788,
-3.19414831697094));
#309771=CARTESIAN_POINT('Ctrl Pts',(-3.6304946963471,-3.35510992093543,
-3.22490945247993));
#309772=CARTESIAN_POINT('Ctrl Pts',(-3.91956573332253,-3.03773926555733,
-3.24048010635175));
#309773=CARTESIAN_POINT('Ctrl Pts',(-4.5672278566538,-2.10952655564697,
-3.28138802246961));
#309774=CARTESIAN_POINT('Ctrl Pts',(-4.81509817539142,-1.49220678589881,
-3.30351920138978));
#309775=CARTESIAN_POINT('Ctrl Pts',(-5.08200700866935,-0.261756534382178,
-3.34775565193902));
#309776=CARTESIAN_POINT('Ctrl Pts',(-5.09681794441811,0.38892707590372,
-3.37082896809827));
#309777=CARTESIAN_POINT('Ctrl Pts',(-4.93227195395555,1.35860806500034,
-3.40476619169824));
#309778=CARTESIAN_POINT('Ctrl Pts',(-4.84196850476752,1.68543727529175,
-3.41591449154964));
#309779=CARTESIAN_POINT('Ctrl Pts',(-4.48337515897765,2.61986203920909,
-3.45003070344122));
#309780=CARTESIAN_POINT('Ctrl Pts',(-4.12755756215163,3.18876467727029,
-3.47333923889199));
#309781=CARTESIAN_POINT('Ctrl Pts',(-3.16576211569989,4.21826206367995,
-3.52138522726153));
#309782=CARTESIAN_POINT('Ctrl Pts',(-2.57933682320399,4.61137003710499,
-3.5437507450149));
#309783=CARTESIAN_POINT('Ctrl Pts',(-1.38321071187134,5.1468107907079,-3.5882824311065));
#309784=CARTESIAN_POINT('Ctrl Pts',(-0.734020794814275,5.3011330060117,
-3.61071457969699));
#309785=CARTESIAN_POINT('Ctrl Pts',(0.279946897817617,5.34769015241393,
-3.64334071581177));
#309786=CARTESIAN_POINT('Ctrl Pts',(0.636284073092541,5.32892781932006,
-3.65490827023087));
#309787=CARTESIAN_POINT('Ctrl Pts',(1.33403158204166,5.22189855460367,-3.67831196246797));
#309788=CARTESIAN_POINT('Ctrl Pts',(1.67297966356761,5.13560563080429,-3.68996111196863));
#309789=CARTESIAN_POINT('Ctrl Pts',(2.72455580662618,4.75605569057548,-3.72701605611379));
#309790=CARTESIAN_POINT('Ctrl Pts',(3.33392558335127,4.36173352953152,-3.74913968805936));
#309791=CARTESIAN_POINT('Ctrl Pts',(4.35401110494811,3.4259477650097,-3.79390141753689));
#309792=CARTESIAN_POINT('Ctrl Pts',(4.78185486937148,2.84385742230068,-3.81743010764088));
#309793=CARTESIAN_POINT('Ctrl Pts',(5.24058372029848,1.86746156353265,-3.8515209540203));
#309794=CARTESIAN_POINT('Ctrl Pts',(5.36179283297534,1.52406097865491,-3.86252927606252));
#309795=CARTESIAN_POINT('Ctrl Pts',(5.54463674231665,0.788760206188264,
-3.88637233212224));
#309796=CARTESIAN_POINT('Ctrl Pts',(5.59905017436476,0.395144997205665,
-3.89905017436476));
#309797=CARTESIAN_POINT('Ctrl Pts',(5.61169055981797,-9.0205620750794E-16,
-3.91169055981797));
#309798=CARTESIAN_POINT('Ctrl Pts',(5.61169055981797,-1.38777878078145E-16,
-3.91169055981797));
#309799=CARTESIAN_POINT('Ctrl Pts',(5.62208535815845,-0.324946780808796,
-3.92208535815844));
#309800=CARTESIAN_POINT('Ctrl Pts',(5.60423157167623,-0.650928060576569,
-3.93245506337904));
#309801=CARTESIAN_POINT('Ctrl Pts',(5.45274517051411,-1.70904678777463,
-3.96593365768693));
#309802=CARTESIAN_POINT('Ctrl Pts',(5.20163226652447,-2.41677199412078,
-3.98794350103121));
#309803=CARTESIAN_POINT('Ctrl Pts',(4.63717212063039,-3.37429620405354,
-4.02279179045299));
#309804=CARTESIAN_POINT('Ctrl Pts',(4.41686272435106,-3.67622261701962,
-4.03449108433516));
#309805=CARTESIAN_POINT('Ctrl Pts',(3.62352289881408,-4.56616302478096,
-4.07140204215783));
#309806=CARTESIAN_POINT('Ctrl Pts',(2.9915333438317,-5.01055071564082,-4.09348040363817));
#309807=CARTESIAN_POINT('Ctrl Pts',(1.66811522085473,-5.64761620972557,
-4.13855742806273));
#309808=CARTESIAN_POINT('Ctrl Pts',(0.916971204147396,-5.84075811028472,
-4.16223199641104));
#309809=CARTESIAN_POINT('Ctrl Pts',(-0.0143208385757574,-5.89177397945501,
-4.18949497944445));
#309810=CARTESIAN_POINT('Ctrl Pts',(-0.179394107925109,-5.89380659597007,
-4.19425881377196));
#309811=CARTESIAN_POINT('Ctrl Pts',(-0.904890135639625,-5.87291322183324,
-4.21561668306337));
#309812=CARTESIAN_POINT('Ctrl Pts',(-1.46138320786938,-5.77716446381248,
-4.23261174044124));
#309813=CARTESIAN_POINT('Ctrl Pts',(-2.2637783039818,-5.51837303963243,
-4.25802866316144));
#309814=CARTESIAN_POINT('Ctrl Pts',(-2.52498189660555,-5.41314737249321,
-4.26646170234364));
#309815=CARTESIAN_POINT('Ctrl Pts',(-3.03708821495135,-5.16328569590837,
-4.28332938416876));
#309816=CARTESIAN_POINT('Ctrl Pts',(-3.28525172634026,-5.01924798335745,
-4.29167943232946));
#309817=CARTESIAN_POINT('Ctrl Pts',(-3.52671151375647,-4.85410196624857,
-4.30000000000005));
#309818=CARTESIAN_POINT('Origin',(2.99770677028732E-14,-1.99840144432528E-14,
-5.765625));
#309819=CARTESIAN_POINT('',(1.48910022457091,-4.62975945369497,-3.16334165753294));
#309820=CARTESIAN_POINT('Ctrl Pts',(1.48910022457091,-4.62975945369497,
-3.16334165753294));
#309821=CARTESIAN_POINT('Ctrl Pts',(2.22943715735947,-4.39163997818016,
-3.11806287316211));
#309822=CARTESIAN_POINT('Ctrl Pts',(2.85860050315749,-3.93452605039576,
-3.075));
#309823=CARTESIAN_POINT('Ctrl Pts',(4.13700551227253,-3.0057104432586,-2.9875));
#309824=CARTESIAN_POINT('Ctrl Pts',(4.62531277436636,-1.5028552216293,-2.9));
#309825=CARTESIAN_POINT('Ctrl Pts',(5.11362003646019,7.95366714520796E-16,
-2.8125));
#309826=CARTESIAN_POINT('Ctrl Pts',(4.62531277436636,1.5028552216293,-2.725));
#309827=CARTESIAN_POINT('Ctrl Pts',(4.13700551227253,3.0057104432586,-2.6375));
#309828=CARTESIAN_POINT('Ctrl Pts',(2.85860050315749,3.93452605039576,-2.55));
#309829=CARTESIAN_POINT('Ctrl Pts',(1.58019549404244,4.86334165753292,-2.4625));
#309830=CARTESIAN_POINT('Ctrl Pts',(0.,4.86334165753293,-2.375));
#309831=CARTESIAN_POINT('Ctrl Pts',(-1.58019549404244,4.86334165753292,
-2.2875));
#309832=CARTESIAN_POINT('Ctrl Pts',(-2.85860050315749,3.93452605039576,
-2.2));
#309833=CARTESIAN_POINT('Ctrl Pts',(-4.13700551227253,3.0057104432586,-2.1125));
#309834=CARTESIAN_POINT('Ctrl Pts',(-4.62531277436636,1.5028552216293,-2.025));
#309835=CARTESIAN_POINT('Ctrl Pts',(-5.11362003646019,2.04784239646214E-15,
-1.9375));
#309836=CARTESIAN_POINT('Ctrl Pts',(-4.62531277436636,-1.5028552216293,
-1.85));
#309837=CARTESIAN_POINT('Ctrl Pts',(-4.13700551227253,-3.00571044325859,
-1.7625));
#309838=CARTESIAN_POINT('Ctrl Pts',(-2.85860050315749,-3.93452605039576,
-1.675));
#309839=CARTESIAN_POINT('Ctrl Pts',(-1.58019549404244,-4.86334165753292,
-1.5875));
#309840=CARTESIAN_POINT('Ctrl Pts',(-5.95587579405768E-16,-4.86334165753292,
-1.5));
#309841=CARTESIAN_POINT('Origin',(2.99770677028732E-14,-1.99840144432528E-14,
-3.16334165753295));
#309842=CARTESIAN_POINT('Ctrl Pts',(0.,4.86333489545091,-5.87499609591012));
#309843=CARTESIAN_POINT('Ctrl Pts',(-1.5801932969088,4.8633348954509,-5.78749609591012));
#309844=CARTESIAN_POINT('Ctrl Pts',(-2.8585965285054,3.93452057975648,-5.69999609591012));
#309845=CARTESIAN_POINT('Ctrl Pts',(-4.13699976010199,3.00570626406207,
-5.61249609591012));
#309846=CARTESIAN_POINT('Ctrl Pts',(-4.62530634324419,1.50285313203104,
-5.52499609591012));
#309847=CARTESIAN_POINT('Ctrl Pts',(-5.11361292638638,2.04784196109569E-15,
-5.43749609591012));
#309848=CARTESIAN_POINT('Ctrl Pts',(-4.62530634324419,-1.50285313203103,
-5.34999609591012));
#309849=CARTESIAN_POINT('Ctrl Pts',(-4.13699976010199,-3.00570626406207,
-5.26249609591011));
#309850=CARTESIAN_POINT('Ctrl Pts',(-2.8585965285054,-3.93452057975648,
-5.17499609591012));
#309851=CARTESIAN_POINT('Ctrl Pts',(-1.5801932969088,-4.8633348954509,-5.08749609591013));
#309852=CARTESIAN_POINT('Ctrl Pts',(-5.95586751289557E-16,-4.8633348954509,
-4.99999609591012));
#309853=CARTESIAN_POINT('Ctrl Pts',(1.5801932969088,-4.8633348954509,-4.91249609591012));
#309854=CARTESIAN_POINT('Ctrl Pts',(2.8585965285054,-3.93452057975648,-4.82499609591012));
#309855=CARTESIAN_POINT('Ctrl Pts',(4.13699976010199,-3.00570626406207,
-4.73749609591012));
#309856=CARTESIAN_POINT('Ctrl Pts',(4.62530634324419,-1.50285313203104,
-4.64999609591012));
#309857=CARTESIAN_POINT('Ctrl Pts',(5.11361292638638,7.95368020620165E-16,
-4.56249609591012));
#309858=CARTESIAN_POINT('Ctrl Pts',(4.62530634324419,1.50285313203104,-4.47499609591012));
#309859=CARTESIAN_POINT('Ctrl Pts',(4.13699976010199,3.00570626406207,-4.38749609591012));
#309860=CARTESIAN_POINT('Ctrl Pts',(2.8585965285054,3.93452057975648,-4.29999609591012));
#309861=CARTESIAN_POINT('Ctrl Pts',(1.5801932969088,4.8633348954509,-4.21249609591012));
#309862=CARTESIAN_POINT('Ctrl Pts',(0.,4.86333489545091,-4.12499609591012));
#309863=CARTESIAN_POINT('Ctrl Pts',(-1.5801932969088,4.8633348954509,-4.03749609591012));
#309864=CARTESIAN_POINT('Ctrl Pts',(-2.8585965285054,3.93452057975648,-3.94999609591012));
#309865=CARTESIAN_POINT('Ctrl Pts',(-4.13699976010199,3.00570626406207,
-3.86249609591012));
#309866=CARTESIAN_POINT('Ctrl Pts',(-4.62530634324419,1.50285313203104,
-3.77499609591012));
#309867=CARTESIAN_POINT('Ctrl Pts',(-5.11361292638638,2.04784196109569E-15,
-3.68749609591012));
#309868=CARTESIAN_POINT('Ctrl Pts',(-4.62530634324419,-1.50285313203103,
-3.59999609591012));
#309869=CARTESIAN_POINT('Ctrl Pts',(-4.13699976010199,-3.00570626406207,
-3.51249609591012));
#309870=CARTESIAN_POINT('Ctrl Pts',(-2.8585965285054,-3.93452057975648,
-3.42499609591012));
#309871=CARTESIAN_POINT('Ctrl Pts',(-1.5801932969088,-4.8633348954509,-3.33749609591012));
#309872=CARTESIAN_POINT('Ctrl Pts',(-5.95586751289557E-16,-4.8633348954509,
-3.24999609591012));
#309873=CARTESIAN_POINT('Ctrl Pts',(1.5801932969088,-4.8633348954509,-3.16249609591012));
#309874=CARTESIAN_POINT('Ctrl Pts',(2.8585965285054,-3.93452057975648,-3.07499609591012));
#309875=CARTESIAN_POINT('Ctrl Pts',(4.13699976010199,-3.00570626406207,
-2.98749609591012));
#309876=CARTESIAN_POINT('Ctrl Pts',(4.62530634324419,-1.50285313203104,
-2.89999609591012));
#309877=CARTESIAN_POINT('Ctrl Pts',(5.11361292638638,7.95368020620165E-16,
-2.81249609591012));
#309878=CARTESIAN_POINT('Ctrl Pts',(4.62530634324419,1.50285313203104,-2.72499609591012));
#309879=CARTESIAN_POINT('Ctrl Pts',(4.13699976010199,3.00570626406207,-2.63749609591012));
#309880=CARTESIAN_POINT('Ctrl Pts',(2.8585965285054,3.93452057975648,-2.54999609591012));
#309881=CARTESIAN_POINT('Ctrl Pts',(1.5801932969088,4.8633348954509,-2.46249609591012));
#309882=CARTESIAN_POINT('Ctrl Pts',(0.,4.86333489545091,-2.37499609591012));
#309883=CARTESIAN_POINT('Ctrl Pts',(-1.5801932969088,4.8633348954509,-2.28749609591012));
#309884=CARTESIAN_POINT('Ctrl Pts',(-2.8585965285054,3.93452057975648,-2.19999609591012));
#309885=CARTESIAN_POINT('Ctrl Pts',(-4.13699976010199,3.00570626406207,
-2.11249609591012));
#309886=CARTESIAN_POINT('Ctrl Pts',(-4.62530634324419,1.50285313203104,
-2.02499609591012));
#309887=CARTESIAN_POINT('Ctrl Pts',(-5.11361292638638,2.04784196109569E-15,
-1.93749609591012));
#309888=CARTESIAN_POINT('Ctrl Pts',(-4.62530634324419,-1.50285313203103,
-1.84999609591012));
#309889=CARTESIAN_POINT('Ctrl Pts',(-4.13699976010199,-3.00570626406207,
-1.76249609591012));
#309890=CARTESIAN_POINT('Ctrl Pts',(-2.8585965285054,-3.93452057975648,
-1.67499609591012));
#309891=CARTESIAN_POINT('Ctrl Pts',(-1.5801932969088,-4.8633348954509,-1.58749609591012));
#309892=CARTESIAN_POINT('Ctrl Pts',(-5.95586751289557E-16,-4.8633348954509,
-1.49999609591012));
#309893=CARTESIAN_POINT('Ctrl Pts',(1.5801932969088,-4.8633348954509,-1.41249609591012));
#309894=CARTESIAN_POINT('Ctrl Pts',(2.8585965285054,-3.93452057975648,-1.32499609591012));
#309895=CARTESIAN_POINT('Ctrl Pts',(4.13699976010199,-3.00570626406207,
-1.23749609591012));
#309896=CARTESIAN_POINT('Ctrl Pts',(4.62530634324419,-1.50285313203104,
-1.14999609591012));
#309897=CARTESIAN_POINT('Ctrl Pts',(5.11361292638638,7.95368020620165E-16,
-1.06249609591012));
#309898=CARTESIAN_POINT('Ctrl Pts',(4.62530634324419,1.50285313203104,-0.974996095910122));
#309899=CARTESIAN_POINT('Ctrl Pts',(4.13699976010199,3.00570626406207,-0.887496095910121));
#309900=CARTESIAN_POINT('Ctrl Pts',(2.8585965285054,3.93452057975648,-0.799996095910123));
#309901=CARTESIAN_POINT('Ctrl Pts',(1.5801932969088,4.8633348954509,-0.712496095910121));
#309902=CARTESIAN_POINT('Ctrl Pts',(0.,4.86333489545091,-0.624996095910122));
#309903=CARTESIAN_POINT('Ctrl Pts',(-1.5801932969088,4.8633348954509,-0.537496095910121));
#309904=CARTESIAN_POINT('Ctrl Pts',(-2.8585965285054,3.93452057975648,-0.449996095910122));
#309905=CARTESIAN_POINT('Ctrl Pts',(-4.13699976010199,3.00570626406207,
-0.362496095910121));
#309906=CARTESIAN_POINT('Ctrl Pts',(-4.62530634324419,1.50285313203104,
-0.274996095910122));
#309907=CARTESIAN_POINT('Ctrl Pts',(-5.11361292638638,2.04784196109569E-15,
-0.187496095910121));
#309908=CARTESIAN_POINT('Ctrl Pts',(-4.62530634324419,-1.50285313203103,
-0.0999960959101223));
#309909=CARTESIAN_POINT('Ctrl Pts',(-4.13699976010199,-3.00570626406207,
-0.0124960959101217));
#309910=CARTESIAN_POINT('Ctrl Pts',(-2.8585965285054,-3.93452057975648,
0.0750039040898777));
#309911=CARTESIAN_POINT('Ctrl Pts',(-1.5801932969088,-4.8633348954509,0.162503904089879));
#309912=CARTESIAN_POINT('Ctrl Pts',(-5.95586751289557E-16,-4.8633348954509,
0.250003904089878));
#309913=CARTESIAN_POINT('Ctrl Pts',(1.5801932969088,-4.8633348954509,0.337503904089879));
#309914=CARTESIAN_POINT('Ctrl Pts',(2.8585965285054,-3.93452057975648,0.425003904089878));
#309915=CARTESIAN_POINT('Ctrl Pts',(4.13699976010199,-3.00570626406207,
0.512503904089878));
#309916=CARTESIAN_POINT('Ctrl Pts',(4.62530634324419,-1.50285313203104,
0.600003904089878));
#309917=CARTESIAN_POINT('Ctrl Pts',(5.11361292638638,7.95368020620165E-16,
0.687503904089878));
#309918=CARTESIAN_POINT('Ctrl Pts',(4.62530634324419,1.50285313203104,0.775003904089878));
#309919=CARTESIAN_POINT('Ctrl Pts',(4.13699976010199,3.00570626406207,0.862503904089877));
#309920=CARTESIAN_POINT('Ctrl Pts',(2.8585965285054,3.93452057975648,0.950003904089878));
#309921=CARTESIAN_POINT('Ctrl Pts',(1.5801932969088,4.8633348954509,1.03750390408988));
#309922=CARTESIAN_POINT('Ctrl Pts',(0.,4.86333489545091,1.12500390408988));
#309923=CARTESIAN_POINT('Ctrl Pts',(-1.5801932969088,4.8633348954509,1.21250390408988));
#309924=CARTESIAN_POINT('Ctrl Pts',(-2.8585965285054,3.93452057975648,1.30000390408988));
#309925=CARTESIAN_POINT('Ctrl Pts',(-4.13699976010199,3.00570626406207,
1.38750390408988));
#309926=CARTESIAN_POINT('Ctrl Pts',(-4.62530634324419,1.50285313203104,
1.47500390408988));
#309927=CARTESIAN_POINT('Ctrl Pts',(-5.11361292638638,2.04784196109569E-15,
1.56250390408988));
#309928=CARTESIAN_POINT('Ctrl Pts',(-4.62530634324419,-1.50285313203103,
1.65000390408988));
#309929=CARTESIAN_POINT('Ctrl Pts',(-4.13699976010199,-3.00570626406207,
1.73750390408988));
#309930=CARTESIAN_POINT('Ctrl Pts',(-2.8585965285054,-3.93452057975648,
1.82500390408988));
#309931=CARTESIAN_POINT('Ctrl Pts',(-1.5801932969088,-4.8633348954509,1.91250390408988));
#309932=CARTESIAN_POINT('Ctrl Pts',(-5.95586751289557E-16,-4.8633348954509,
2.00000390408988));
#309933=CARTESIAN_POINT('Ctrl Pts',(1.5801932969088,-4.8633348954509,2.08750390408988));
#309934=CARTESIAN_POINT('Ctrl Pts',(2.8585965285054,-3.93452057975648,2.17500390408988));
#309935=CARTESIAN_POINT('Ctrl Pts',(4.13699976010199,-3.00570626406207,
2.26250390408988));
#309936=CARTESIAN_POINT('Ctrl Pts',(4.62530634324419,-1.50285313203104,
2.35000390408988));
#309937=CARTESIAN_POINT('Ctrl Pts',(5.11361292638638,7.95368020620165E-16,
2.43750390408988));
#309938=CARTESIAN_POINT('Ctrl Pts',(4.62530634324419,1.50285313203104,2.52500390408988));
#309939=CARTESIAN_POINT('Ctrl Pts',(4.13699976010199,3.00570626406207,2.61250390408988));
#309940=CARTESIAN_POINT('Ctrl Pts',(2.8585965285054,3.93452057975648,2.70000390408988));
#309941=CARTESIAN_POINT('Ctrl Pts',(1.5801932969088,4.8633348954509,2.78750390408988));
#309942=CARTESIAN_POINT('Ctrl Pts',(0.,4.86333489545091,2.87500390408988));
#309943=CARTESIAN_POINT('Ctrl Pts',(-1.5801932969088,4.8633348954509,2.96250390408988));
#309944=CARTESIAN_POINT('Ctrl Pts',(-2.8585965285054,3.93452057975648,3.05000390408988));
#309945=CARTESIAN_POINT('Ctrl Pts',(-4.13699976010199,3.00570626406207,
3.13750390408988));
#309946=CARTESIAN_POINT('Ctrl Pts',(-4.62530634324419,1.50285313203104,
3.22500390408988));
#309947=CARTESIAN_POINT('Ctrl Pts',(-5.11361292638638,2.04784196109569E-15,
3.31250390408987));
#309948=CARTESIAN_POINT('Ctrl Pts',(-4.62530634324419,-1.50285313203103,
3.40000390408988));
#309949=CARTESIAN_POINT('Ctrl Pts',(-4.13699976010199,-3.00570626406207,
3.48750390408988));
#309950=CARTESIAN_POINT('Ctrl Pts',(-2.8585965285054,-3.93452057975648,
3.57500390408988));
#309951=CARTESIAN_POINT('Ctrl Pts',(-1.5801932969088,-4.8633348954509,3.66250390408988));
#309952=CARTESIAN_POINT('Ctrl Pts',(-5.95586751289557E-16,-4.8633348954509,
3.75000390408988));
#309953=CARTESIAN_POINT('Ctrl Pts',(1.5801932969088,-4.8633348954509,3.83750390408988));
#309954=CARTESIAN_POINT('Ctrl Pts',(2.8585965285054,-3.93452057975648,3.92500390408988));
#309955=CARTESIAN_POINT('Ctrl Pts',(4.13699976010199,-3.00570626406207,
4.01250390408988));
#309956=CARTESIAN_POINT('Ctrl Pts',(4.62530634324419,-1.50285313203104,
4.10000390408988));
#309957=CARTESIAN_POINT('Ctrl Pts',(5.11361292638638,7.95368020620165E-16,
4.18750390408988));
#309958=CARTESIAN_POINT('Ctrl Pts',(4.62530634324419,1.50285313203104,4.27500390408988));
#309959=CARTESIAN_POINT('Ctrl Pts',(4.13699976010199,3.00570626406207,4.36250390408988));
#309960=CARTESIAN_POINT('Ctrl Pts',(2.8585965285054,3.93452057975648,4.45000390408988));
#309961=CARTESIAN_POINT('Ctrl Pts',(1.5801932969088,4.8633348954509,4.53750390408988));
#309962=CARTESIAN_POINT('Ctrl Pts',(0.,4.86333489545091,4.62500390408988));
#309963=CARTESIAN_POINT('Ctrl Pts',(-1.5801932969088,4.8633348954509,4.71250390408988));
#309964=CARTESIAN_POINT('Ctrl Pts',(-2.8585965285054,3.93452057975648,4.80000390408988));
#309965=CARTESIAN_POINT('Ctrl Pts',(-4.13699976010199,3.00570626406207,
4.88750390408987));
#309966=CARTESIAN_POINT('Ctrl Pts',(-4.62530634324419,1.50285313203104,
4.97500390408988));
#309967=CARTESIAN_POINT('Ctrl Pts',(-5.11361292638638,2.04784196109569E-15,
5.06250390408988));
#309968=CARTESIAN_POINT('Ctrl Pts',(-4.62530634324419,-1.50285313203103,
5.15000390408988));
#309969=CARTESIAN_POINT('Ctrl Pts',(-4.13699976010199,-3.00570626406207,
5.23750390408988));
#309970=CARTESIAN_POINT('Ctrl Pts',(-2.8585965285054,-3.93452057975648,
5.32500390408988));
#309971=CARTESIAN_POINT('Ctrl Pts',(-1.5801932969088,-4.8633348954509,5.41250390408988));
#309972=CARTESIAN_POINT('Ctrl Pts',(-5.95586751289557E-16,-4.8633348954509,
5.50000390408988));
#309973=CARTESIAN_POINT('Ctrl Pts',(1.5801932969088,-4.8633348954509,5.58750390408987));
#309974=CARTESIAN_POINT('Ctrl Pts',(2.8585965285054,-3.93452057975648,5.67500390408988));
#309975=CARTESIAN_POINT('Ctrl Pts',(4.13699976010199,-3.00570626406207,
5.76250390408987));
#309976=CARTESIAN_POINT('Ctrl Pts',(4.62530634324419,-1.50285313203104,
5.85000390408988));
#309977=CARTESIAN_POINT('Ctrl Pts',(4.69280400630547,-1.29511668562952,
5.86209885779675));
#309978=CARTESIAN_POINT('Ctrl Pts',(4.74140733325457,-1.08216579389214,
5.87449741001046));
#309979=CARTESIAN_POINT('Ctrl Pts',(0.,6.09472152853892,-6.5859375));
#309980=CARTESIAN_POINT('Ctrl Pts',(-1.98029506767702,6.09472152853892,
-6.4984375));
#309981=CARTESIAN_POINT('Ctrl Pts',(-3.58238743130461,4.93073329257085,
-6.4109375));
#309982=CARTESIAN_POINT('Ctrl Pts',(-5.18447979493221,3.76674505660277,
-6.3234375));
#309983=CARTESIAN_POINT('Ctrl Pts',(-5.7964246247213,1.88337252830138,-6.2359375));
#309984=CARTESIAN_POINT('Ctrl Pts',(-6.40836945451038,2.1271229329878E-15,
-6.14843749999999));
#309985=CARTESIAN_POINT('Ctrl Pts',(-5.7964246247213,-1.88337252830138,
-6.0609375));
#309986=CARTESIAN_POINT('Ctrl Pts',(-5.18447979493221,-3.76674505660276,
-5.9734375));
#309987=CARTESIAN_POINT('Ctrl Pts',(-3.58238743130461,-4.93073329257084,
-5.8859375));
#309988=CARTESIAN_POINT('Ctrl Pts',(-1.98029506767702,-6.09472152853892,
-5.7984375));
#309989=CARTESIAN_POINT('Ctrl Pts',(-7.46388121161965E-16,-6.09472152853892,
-5.7109375));
#309990=CARTESIAN_POINT('Ctrl Pts',(1.98029506767702,-6.09472152853892,
-5.6234375));
#309991=CARTESIAN_POINT('Ctrl Pts',(3.58238743130461,-4.93073329257084,
-5.5359375));
#309992=CARTESIAN_POINT('Ctrl Pts',(5.18447979493221,-3.76674505660276,
-5.44843749999999));
#309993=CARTESIAN_POINT('Ctrl Pts',(5.7964246247213,-1.88337252830138,-5.3609375));
#309994=CARTESIAN_POINT('Ctrl Pts',(6.40836945451038,5.57525104943835E-16,
-5.27343749999999));
#309995=CARTESIAN_POINT('Ctrl Pts',(5.7964246247213,1.88337252830138,-5.1859375));
#309996=CARTESIAN_POINT('Ctrl Pts',(5.18447979493221,3.76674505660277,-5.09843749999999));
#309997=CARTESIAN_POINT('Ctrl Pts',(3.58238743130462,4.93073329257084,-5.0109375));
#309998=CARTESIAN_POINT('Ctrl Pts',(1.98029506767702,6.09472152853892,-4.9234375));
#309999=CARTESIAN_POINT('Ctrl Pts',(0.,6.09472152853892,-4.8359375));
#310000=CARTESIAN_POINT('Ctrl Pts',(-1.98029506767702,6.09472152853892,
-4.7484375));
#310001=CARTESIAN_POINT('Ctrl Pts',(-3.58238743130461,4.93073329257085,
-4.6609375));
#310002=CARTESIAN_POINT('Ctrl Pts',(-5.18447979493221,3.76674505660277,
-4.5734375));
#310003=CARTESIAN_POINT('Ctrl Pts',(-5.7964246247213,1.88337252830138,-4.4859375));
#310004=CARTESIAN_POINT('Ctrl Pts',(-6.40836945451038,2.1271229329878E-15,
-4.39843749999999));
#310005=CARTESIAN_POINT('Ctrl Pts',(-5.7964246247213,-1.88337252830138,
-4.3109375));
#310006=CARTESIAN_POINT('Ctrl Pts',(-5.18447979493221,-3.76674505660276,
-4.2234375));
#310007=CARTESIAN_POINT('Ctrl Pts',(-3.58238743130461,-4.93073329257084,
-4.1359375));
#310008=CARTESIAN_POINT('Ctrl Pts',(-1.98029506767702,-6.09472152853892,
-4.0484375));
#310009=CARTESIAN_POINT('Ctrl Pts',(-7.46388121161965E-16,-6.09472152853892,
-3.96093749999999));
#310010=CARTESIAN_POINT('Ctrl Pts',(1.98029506767702,-6.09472152853892,
-3.87343749999999));
#310011=CARTESIAN_POINT('Ctrl Pts',(3.58238743130461,-4.93073329257084,
-3.7859375));
#310012=CARTESIAN_POINT('Ctrl Pts',(5.18447979493221,-3.76674505660276,
-3.6984375));
#310013=CARTESIAN_POINT('Ctrl Pts',(5.7964246247213,-1.88337252830138,-3.6109375));
#310014=CARTESIAN_POINT('Ctrl Pts',(6.40836945451038,5.57525104943835E-16,
-3.5234375));
#310015=CARTESIAN_POINT('Ctrl Pts',(5.7964246247213,1.88337252830138,-3.4359375));
#310016=CARTESIAN_POINT('Ctrl Pts',(5.18447979493221,3.76674505660277,-3.34843749999999));
#310017=CARTESIAN_POINT('Ctrl Pts',(3.58238743130462,4.93073329257084,-3.2609375));
#310018=CARTESIAN_POINT('Ctrl Pts',(1.98029506767702,6.09472152853892,-3.1734375));
#310019=CARTESIAN_POINT('Ctrl Pts',(0.,6.09472152853892,-3.0859375));
#310020=CARTESIAN_POINT('Ctrl Pts',(-1.98029506767702,6.09472152853892,
-2.9984375));
#310021=CARTESIAN_POINT('Ctrl Pts',(-3.58238743130461,4.93073329257085,
-2.9109375));
#310022=CARTESIAN_POINT('Ctrl Pts',(-5.18447979493221,3.76674505660277,
-2.8234375));
#310023=CARTESIAN_POINT('Ctrl Pts',(-5.7964246247213,1.88337252830138,-2.7359375));
#310024=CARTESIAN_POINT('Ctrl Pts',(-6.40836945451038,2.1271229329878E-15,
-2.6484375));
#310025=CARTESIAN_POINT('Ctrl Pts',(-5.7964246247213,-1.88337252830138,
-2.5609375));
#310026=CARTESIAN_POINT('Ctrl Pts',(-5.18447979493221,-3.76674505660276,
-2.4734375));
#310027=CARTESIAN_POINT('Ctrl Pts',(-3.58238743130461,-4.93073329257084,
-2.3859375));
#310028=CARTESIAN_POINT('Ctrl Pts',(-1.98029506767702,-6.09472152853892,
-2.2984375));
#310029=CARTESIAN_POINT('Ctrl Pts',(-7.46388121161965E-16,-6.09472152853892,
-2.2109375));
#310030=CARTESIAN_POINT('Ctrl Pts',(1.98029506767702,-6.09472152853892,
-2.12343749999999));
#310031=CARTESIAN_POINT('Ctrl Pts',(3.58238743130461,-4.93073329257084,
-2.0359375));
#310032=CARTESIAN_POINT('Ctrl Pts',(5.18447979493221,-3.76674505660276,
-1.9484375));
#310033=CARTESIAN_POINT('Ctrl Pts',(5.7964246247213,-1.88337252830138,-1.8609375));
#310034=CARTESIAN_POINT('Ctrl Pts',(6.40836945451038,5.57525104943835E-16,
-1.7734375));
#310035=CARTESIAN_POINT('Ctrl Pts',(5.7964246247213,1.88337252830138,-1.6859375));
#310036=CARTESIAN_POINT('Ctrl Pts',(5.18447979493221,3.76674505660277,-1.5984375));
#310037=CARTESIAN_POINT('Ctrl Pts',(3.58238743130462,4.93073329257084,-1.5109375));
#310038=CARTESIAN_POINT('Ctrl Pts',(1.98029506767702,6.09472152853892,-1.4234375));
#310039=CARTESIAN_POINT('Ctrl Pts',(0.,6.09472152853892,-1.3359375));
#310040=CARTESIAN_POINT('Ctrl Pts',(-1.98029506767702,6.09472152853892,
-1.2484375));
#310041=CARTESIAN_POINT('Ctrl Pts',(-3.58238743130461,4.93073329257085,
-1.1609375));
#310042=CARTESIAN_POINT('Ctrl Pts',(-5.18447979493221,3.76674505660277,
-1.0734375));
#310043=CARTESIAN_POINT('Ctrl Pts',(-5.7964246247213,1.88337252830138,-0.9859375));
#310044=CARTESIAN_POINT('Ctrl Pts',(-6.40836945451038,2.1271229329878E-15,
-0.898437499999998));
#310045=CARTESIAN_POINT('Ctrl Pts',(-5.7964246247213,-1.88337252830138,
-0.8109375));
#310046=CARTESIAN_POINT('Ctrl Pts',(-5.18447979493221,-3.76674505660276,
-0.723437499999998));
#310047=CARTESIAN_POINT('Ctrl Pts',(-3.58238743130461,-4.93073329257084,
-0.6359375));
#310048=CARTESIAN_POINT('Ctrl Pts',(-1.98029506767702,-6.09472152853892,
-0.548437499999997));
#310049=CARTESIAN_POINT('Ctrl Pts',(-7.46388121161965E-16,-6.09472152853892,
-0.4609375));
#310050=CARTESIAN_POINT('Ctrl Pts',(1.98029506767702,-6.09472152853892,
-0.373437499999998));
#310051=CARTESIAN_POINT('Ctrl Pts',(3.58238743130461,-4.93073329257084,
-0.2859375));
#310052=CARTESIAN_POINT('Ctrl Pts',(5.18447979493221,-3.76674505660276,
-0.198437499999998));
#310053=CARTESIAN_POINT('Ctrl Pts',(5.7964246247213,-1.88337252830138,-0.110937499999998));
#310054=CARTESIAN_POINT('Ctrl Pts',(6.40836945451038,5.57525104943835E-16,
-0.0234374999999983));
#310055=CARTESIAN_POINT('Ctrl Pts',(5.7964246247213,1.88337252830138,0.0640625000000016));
#310056=CARTESIAN_POINT('Ctrl Pts',(5.18447979493221,3.76674505660277,0.151562500000001));
#310057=CARTESIAN_POINT('Ctrl Pts',(3.58238743130462,4.93073329257084,0.239062500000003));
#310058=CARTESIAN_POINT('Ctrl Pts',(1.98029506767702,6.09472152853892,0.326562500000002));
#310059=CARTESIAN_POINT('Ctrl Pts',(0.,6.09472152853892,0.4140625));
#310060=CARTESIAN_POINT('Ctrl Pts',(-1.98029506767702,6.09472152853892,
0.501562500000002));
#310061=CARTESIAN_POINT('Ctrl Pts',(-3.58238743130461,4.93073329257085,
0.5890625));
#310062=CARTESIAN_POINT('Ctrl Pts',(-5.18447979493221,3.76674505660277,
0.676562500000002));
#310063=CARTESIAN_POINT('Ctrl Pts',(-5.7964246247213,1.88337252830138,0.7640625));
#310064=CARTESIAN_POINT('Ctrl Pts',(-6.40836945451038,2.1271229329878E-15,
0.851562500000001));
#310065=CARTESIAN_POINT('Ctrl Pts',(-5.7964246247213,-1.88337252830138,
0.9390625));
#310066=CARTESIAN_POINT('Ctrl Pts',(-5.18447979493221,-3.76674505660276,
1.0265625));
#310067=CARTESIAN_POINT('Ctrl Pts',(-3.58238743130461,-4.93073329257084,
1.1140625));
#310068=CARTESIAN_POINT('Ctrl Pts',(-1.98029506767702,-6.09472152853892,
1.2015625));
#310069=CARTESIAN_POINT('Ctrl Pts',(-7.46388121161965E-16,-6.09472152853892,
1.2890625));
#310070=CARTESIAN_POINT('Ctrl Pts',(1.98029506767702,-6.09472152853892,
1.3765625));
#310071=CARTESIAN_POINT('Ctrl Pts',(3.58238743130461,-4.93073329257084,
1.4640625));
#310072=CARTESIAN_POINT('Ctrl Pts',(5.18447979493221,-3.76674505660276,
1.5515625));
#310073=CARTESIAN_POINT('Ctrl Pts',(5.7964246247213,-1.88337252830138,1.6390625));
#310074=CARTESIAN_POINT('Ctrl Pts',(6.40836945451038,5.57525104943835E-16,
1.7265625));
#310075=CARTESIAN_POINT('Ctrl Pts',(5.7964246247213,1.88337252830138,1.8140625));
#310076=CARTESIAN_POINT('Ctrl Pts',(5.18447979493221,3.76674505660277,1.9015625));
#310077=CARTESIAN_POINT('Ctrl Pts',(3.58238743130462,4.93073329257084,1.9890625));
#310078=CARTESIAN_POINT('Ctrl Pts',(1.98029506767702,6.09472152853892,2.0765625));
#310079=CARTESIAN_POINT('Ctrl Pts',(0.,6.09472152853892,2.1640625));
#310080=CARTESIAN_POINT('Ctrl Pts',(-1.98029506767702,6.09472152853892,
2.2515625));
#310081=CARTESIAN_POINT('Ctrl Pts',(-3.58238743130461,4.93073329257085,
2.33906250000001));
#310082=CARTESIAN_POINT('Ctrl Pts',(-5.18447979493221,3.76674505660277,
2.4265625));
#310083=CARTESIAN_POINT('Ctrl Pts',(-5.7964246247213,1.88337252830138,2.5140625));
#310084=CARTESIAN_POINT('Ctrl Pts',(-6.40836945451038,2.1271229329878E-15,
2.6015625));
#310085=CARTESIAN_POINT('Ctrl Pts',(-5.7964246247213,-1.88337252830138,
2.6890625));
#310086=CARTESIAN_POINT('Ctrl Pts',(-5.18447979493221,-3.76674505660276,
2.7765625));
#310087=CARTESIAN_POINT('Ctrl Pts',(-3.58238743130461,-4.93073329257084,
2.8640625));
#310088=CARTESIAN_POINT('Ctrl Pts',(-1.98029506767702,-6.09472152853892,
2.9515625));
#310089=CARTESIAN_POINT('Ctrl Pts',(-7.46388121161965E-16,-6.09472152853892,
3.0390625));
#310090=CARTESIAN_POINT('Ctrl Pts',(1.98029506767702,-6.09472152853892,
3.1265625));
#310091=CARTESIAN_POINT('Ctrl Pts',(3.58238743130461,-4.93073329257084,
3.2140625));
#310092=CARTESIAN_POINT('Ctrl Pts',(5.18447979493221,-3.76674505660276,
3.3015625));
#310093=CARTESIAN_POINT('Ctrl Pts',(5.7964246247213,-1.88337252830138,3.3890625));
#310094=CARTESIAN_POINT('Ctrl Pts',(6.40836945451038,5.57525104943835E-16,
3.4765625));
#310095=CARTESIAN_POINT('Ctrl Pts',(5.7964246247213,1.88337252830138,3.5640625));
#310096=CARTESIAN_POINT('Ctrl Pts',(5.18447979493221,3.76674505660277,3.6515625));
#310097=CARTESIAN_POINT('Ctrl Pts',(3.58238743130462,4.93073329257084,3.7390625));
#310098=CARTESIAN_POINT('Ctrl Pts',(1.98029506767702,6.09472152853892,3.8265625));
#310099=CARTESIAN_POINT('Ctrl Pts',(0.,6.09472152853892,3.91406250000001));
#310100=CARTESIAN_POINT('Ctrl Pts',(-1.98029506767702,6.09472152853892,
4.0015625));
#310101=CARTESIAN_POINT('Ctrl Pts',(-3.58238743130461,4.93073329257085,
4.0890625));
#310102=CARTESIAN_POINT('Ctrl Pts',(-5.18447979493221,3.76674505660277,
4.1765625));
#310103=CARTESIAN_POINT('Ctrl Pts',(-5.7964246247213,1.88337252830138,4.2640625));
#310104=CARTESIAN_POINT('Ctrl Pts',(-6.40836945451038,2.1271229329878E-15,
4.3515625));
#310105=CARTESIAN_POINT('Ctrl Pts',(-5.7964246247213,-1.88337252830138,
4.4390625));
#310106=CARTESIAN_POINT('Ctrl Pts',(-5.18447979493221,-3.76674505660276,
4.5265625));
#310107=CARTESIAN_POINT('Ctrl Pts',(-3.58238743130461,-4.93073329257084,
4.6140625));
#310108=CARTESIAN_POINT('Ctrl Pts',(-1.98029506767702,-6.09472152853892,
4.7015625));
#310109=CARTESIAN_POINT('Ctrl Pts',(-7.46388121161965E-16,-6.09472152853892,
4.7890625));
#310110=CARTESIAN_POINT('Ctrl Pts',(1.98029506767702,-6.09472152853892,
4.8765625));
#310111=CARTESIAN_POINT('Ctrl Pts',(3.58238743130461,-4.93073329257084,
4.9640625));
#310112=CARTESIAN_POINT('Ctrl Pts',(5.18447979493221,-3.76674505660276,
5.0515625));
#310113=CARTESIAN_POINT('Ctrl Pts',(5.7964246247213,-1.88337252830138,5.1390625));
#310114=CARTESIAN_POINT('Ctrl Pts',(5.88101256057792,-1.62303763067182,
5.15115745370687));
#310115=CARTESIAN_POINT('Ctrl Pts',(5.94192215234639,-1.3561680006146,5.16355600592057));
#310116=CARTESIAN_POINT('Ctrl Pts',(-4.95790425747066,-1.04777297948999E-14,
3.25790425747067));
#310117=CARTESIAN_POINT('Ctrl Pts',(-4.97293934348226,-0.415247004317136,
3.27293934348227));
#310118=CARTESIAN_POINT('Ctrl Pts',(-4.93570645798768,-0.831585854766426,
3.28787516811917));
#310119=CARTESIAN_POINT('Ctrl Pts',(-4.81116404609656,-1.40037558121051,
3.30810675581896));
#310120=CARTESIAN_POINT('Ctrl Pts',(-4.76783934596157,-1.55936796833944,
3.3136842461998));
#310121=CARTESIAN_POINT('Ctrl Pts',(-4.51360017410534,-2.3411247830559,
3.34192695424601));
#310122=CARTESIAN_POINT('Ctrl Pts',(-4.1901531859331,-2.92122112343498,
3.36542530920946));
#310123=CARTESIAN_POINT('Ctrl Pts',(-3.2864586721934,-3.98792201363658,
3.41441993821744));
#310124=CARTESIAN_POINT('Ctrl Pts',(-2.72857552162265,-4.3959419628284,
3.43666822694452));
#310125=CARTESIAN_POINT('Ctrl Pts',(-1.87695867632202,-4.82850004309927,
3.4696467797169));
#310126=CARTESIAN_POINT('Ctrl Pts',(-1.56418953111277,-4.95087589862769,
3.48128567849256));
#310127=CARTESIAN_POINT('Ctrl Pts',(-0.523733741453605,-5.24549600297378,
3.51854708885451));
#310128=CARTESIAN_POINT('Ctrl Pts',(0.176903345415829,-5.27616946074267,
3.54074355018794));
#310129=CARTESIAN_POINT('Ctrl Pts',(1.47610604773998,-5.11882248397312,
3.5847936147163));
#310130=CARTESIAN_POINT('Ctrl Pts',(2.12250830516505,-4.91118018333939,
3.60777680635765));
#310131=CARTESIAN_POINT('Ctrl Pts',(3.0241129566501,-4.41733830816663,3.64154899360656));
#310132=CARTESIAN_POINT('Ctrl Pts',(3.31754320793393,-4.21542459697997,
3.65273593097732));
#310133=CARTESIAN_POINT('Ctrl Pts',(4.11730640597835,-3.54210984184061,
3.68693489746714));
#310134=CARTESIAN_POINT('Ctrl Pts',(4.55655622643784,-2.99790903685779,
3.7101723791838));
#310135=CARTESIAN_POINT('Ctrl Pts',(5.23423769051958,-1.71858963227232,
3.75726483203539));
#310136=CARTESIAN_POINT('Ctrl Pts',(5.42487105484502,-1.02156461381141,
3.77925028508346));
#310137=CARTESIAN_POINT('Ctrl Pts',(5.52448070077831,0.00449183181578057,
3.81280309470563));
#310138=CARTESIAN_POINT('Ctrl Pts',(5.52414060342832,0.36457952165459,3.82450282693855));
#310139=CARTESIAN_POINT('Ctrl Pts',(5.41076537903406,1.50994706424661,3.86148648007847));
#310140=CARTESIAN_POINT('Ctrl Pts',(5.16954783102153,2.21447136914349,3.88356695868298));
#310141=CARTESIAN_POINT('Ctrl Pts',(4.50111020165292,3.45957691336163,3.92856148806867));
#310142=CARTESIAN_POINT('Ctrl Pts',(4.02525674415986,4.03647908758549,3.95223762409383));
#310143=CARTESIAN_POINT('Ctrl Pts',(3.30978474626372,4.61990466858687,3.98022046020723));
#310144=CARTESIAN_POINT('Ctrl Pts',(3.16227443582965,4.72868251477364,3.98570890981966));
#310145=CARTESIAN_POINT('Ctrl Pts',(2.39909092990884,5.23751197929896,4.01377576741889));
#310146=CARTESIAN_POINT('Ctrl Pts',(1.7146646306617,5.5238562776682,4.03699780574988));
#310147=CARTESIAN_POINT('Ctrl Pts',(0.194599395436199,5.83902880107215,
4.08488183438802));
#310148=CARTESIAN_POINT('Ctrl Pts',(-0.578175813405361,5.8207566644236,
4.10694279906758));
#310149=CARTESIAN_POINT('Ctrl Pts',(-2.02680681744372,5.54378769497724,
4.15214335059165));
#310150=CARTESIAN_POINT('Ctrl Pts',(-2.74802952750779,5.25050360603337,
4.17583159622874));
#310151=CARTESIAN_POINT('Ctrl Pts',(-3.6315318414213,4.6671975741733,4.20661545875264));
#310152=CARTESIAN_POINT('Ctrl Pts',(-3.86096261856221,4.49047984541216,
4.21504771190775));
#310153=CARTESIAN_POINT('Ctrl Pts',(-4.39279983820927,4.01526358263747,
4.23628931942137));
#310154=CARTESIAN_POINT('Ctrl Pts',(-4.6778048743089,3.69990131114164,4.24908677333639));
#310155=CARTESIAN_POINT('Ctrl Pts',(-5.17919548705663,3.00960849983932,
4.27475272437034));
#310156=CARTESIAN_POINT('Ctrl Pts',(-5.39318105256691,2.63599175969816,
4.28754473902495));
#310157=CARTESIAN_POINT('Ctrl Pts',(-5.56513300460777,2.24260889167615,
4.29999999999997));
#310158=CARTESIAN_POINT('Ctrl Pts',(6.,-1.04083408558608E-14,3.53125));
#310159=CARTESIAN_POINT('Ctrl Pts',(6.,-0.662567985849171,3.49998165563862));
#310160=CARTESIAN_POINT('Ctrl Pts',(5.89023888002911,-1.32148209989238,
3.46918647000026));
#310161=CARTESIAN_POINT('Ctrl Pts',(5.42118520370331,-2.68662270594139,
3.40405471308885));
#310162=CARTESIAN_POINT('Ctrl Pts',(5.02683829399696,-3.36719274876381,
3.36713193121169));
#310163=CARTESIAN_POINT('Ctrl Pts',(4.00167806548415,-4.53760947497116,
3.29400874410852));
#310164=CARTESIAN_POINT('Ctrl Pts',(3.38128471508339,-5.01699639073162,
3.25984728204102));
#310165=CARTESIAN_POINT('Ctrl Pts',(1.97963641525498,-5.71895831696652,
3.18670031794793));
#310166=CARTESIAN_POINT('Ctrl Pts',(1.20940416388651,-5.92982580166838,
3.14905492163172));
#310167=CARTESIAN_POINT('Ctrl Pts',(-0.351704872679288,-6.03949474463185,
3.07738850564888));
#310168=CARTESIAN_POINT('Ctrl Pts',(-1.12714151140623,-5.94380189291677,
3.04234108152995));
#310169=CARTESIAN_POINT('Ctrl Pts',(-2.60896859694703,-5.45977628556974,
2.96877370020871));
#310170=CARTESIAN_POINT('Ctrl Pts',(-3.29994699398712,-5.07210022951635,
2.93336335474523));
#310171=CARTESIAN_POINT('Ctrl Pts',(-4.49288000432945,-4.05324074403939,
2.86137269782642));
#310172=CARTESIAN_POINT('Ctrl Pts',(-4.98351548479417,-3.43209332791639,
2.82404768881904));
#310173=CARTESIAN_POINT('Ctrl Pts',(-5.69345137673978,-2.04535878292572,
2.75140961508628));
#310174=CARTESIAN_POINT('Ctrl Pts',(-5.90952163651921,-1.29476718768151,
2.71735350508463));
#310175=CARTESIAN_POINT('Ctrl Pts',(-6.04658161225873,0.26905624612609,
2.64355252059243));
#310176=CARTESIAN_POINT('Ctrl Pts',(-5.95760903598733,1.06796514813261,
2.60584988600272));
#310177=CARTESIAN_POINT('Ctrl Pts',(-5.47869485417073,2.56676990467233,
2.53511730571077));
#310178=CARTESIAN_POINT('Ctrl Pts',(-5.10034667160623,3.25439864082902,
2.49847743196067));
#310179=CARTESIAN_POINT('Ctrl Pts',(-4.10177951121022,4.44760592024899,
2.4252217782941));
#310180=CARTESIAN_POINT('Ctrl Pts',(-3.49086707735637,4.9416249658674,2.39086482120847));
#310181=CARTESIAN_POINT('Ctrl Pts',(-2.10493394767083,5.67379433086644,
2.31798267413971));
#310182=CARTESIAN_POINT('Ctrl Pts',(-1.34128866378715,5.90115742150157,
2.28039235900721));
#310183=CARTESIAN_POINT('Ctrl Pts',(0.214674357637074,6.04584984343904,
2.20844615196138));
#310184=CARTESIAN_POINT('Ctrl Pts',(0.991534561947968,5.96785131509141,
2.17377823337649));
#310185=CARTESIAN_POINT('Ctrl Pts',(2.48618119626386,5.51716889269461,2.10012172850341));
#310186=CARTESIAN_POINT('Ctrl Pts',(3.18810038614419,5.14355910318655,2.06419416006495));
#310187=CARTESIAN_POINT('Ctrl Pts',(4.40347232140798,4.1498821543838,1.99254252722497));
#310188=CARTESIAN_POINT('Ctrl Pts',(4.90648185944318,3.54096946358727,1.95534139008017));
#310189=CARTESIAN_POINT('Ctrl Pts',(5.64672397480825,2.17128984430686,1.88251379882356));
#310190=CARTESIAN_POINT('Ctrl Pts',(5.87958059376345,1.42496250709134,1.84849776826742));
#310191=CARTESIAN_POINT('Ctrl Pts',(5.98807536338565,0.437063488405821,
1.80187618773491));
#310192=CARTESIAN_POINT('Ctrl Pts',(6.,0.218403025168987,1.7915570192741));
#310193=CARTESIAN_POINT('Ctrl Pts',(6.,1.45716771982052E-14,1.78125));
#310194=CARTESIAN_POINT('Ctrl Pts',(-5.92794875776504,-0.927050983124583,
-4.30000000000003));
#310195=CARTESIAN_POINT('Ctrl Pts',(-5.77238411891593,-1.50027234926652,
-4.23487103723538));
#310196=CARTESIAN_POINT('Ctrl Pts',(-5.49784136204396,-2.18887483338659,
-4.15810865263192));
#310197=CARTESIAN_POINT('Ctrl Pts',(-4.59274666464774,-3.41508210903204,
-3.9830747098422));
#310198=CARTESIAN_POINT('Ctrl Pts',(-4.09211140668953,-3.8857077507361,
-3.90229607039226));
#310199=CARTESIAN_POINT('Ctrl Pts',(-3.37691945330692,-4.34821209201474,
-3.80291028591777));
#310200=CARTESIAN_POINT('Ctrl Pts',(-3.22602442370764,-4.43666223235013,
-3.7828527767864));
#310201=CARTESIAN_POINT('Ctrl Pts',(-2.49281137727437,-4.81852268766255,
-3.68617149588514));
#310202=CARTESIAN_POINT('Ctrl Pts',(-1.86226786933467,-5.00930313816897,
-3.60488089526184));
#310203=CARTESIAN_POINT('Ctrl Pts',(-0.978780411324384,-5.10442789867345,
-3.49216045408453));
#310204=CARTESIAN_POINT('Ctrl Pts',(-0.74299602777313,-5.11379701624593,
-3.46219799972188));
#310205=CARTESIAN_POINT('Ctrl Pts',(-0.187938582543416,-5.09834966075881,
-3.39195548336746));
#310206=CARTESIAN_POINT('Ctrl Pts',(0.167559191316829,-5.05999760683309,
-3.34821426240374));
#310207=CARTESIAN_POINT('Ctrl Pts',(0.86973501763252,-4.8885779974458,-3.25416402103133));
#310208=CARTESIAN_POINT('Ctrl Pts',(1.18664663868521,-4.77514585561402,
-3.20913740493096));
#310209=CARTESIAN_POINT('Ctrl Pts',(1.48910022457092,-4.629759453695,-3.16334165753295));
#310210=CARTESIAN_POINT('Origin',(9.215,5.3202827305824,5.));
#310211=CARTESIAN_POINT('',(9.5,5.3202827305819,4.19845583392694));
#310212=CARTESIAN_POINT('',(9.3575,5.56709997066096,4.19845583392679));
#310213=CARTESIAN_POINT('Ctrl Pts',(9.5,5.3202827305819,4.19845583392693));
#310214=CARTESIAN_POINT('Ctrl Pts',(9.50000000000002,5.33130549100061,4.19534623936907));
#310215=CARTESIAN_POINT('Ctrl Pts',(9.49935753322888,5.34243846979206,4.19252178224802));
#310216=CARTESIAN_POINT('Ctrl Pts',(9.49353446737686,5.39198941174876,4.18140331781018));
#310217=CARTESIAN_POINT('Ctrl Pts',(9.48064078915421,5.43017938720461,4.17694939724907));
#310218=CARTESIAN_POINT('Ctrl Pts',(9.44299369100292,5.49538607396019,4.17694939724907));
#310219=CARTESIAN_POINT('Ctrl Pts',(9.41636704119957,5.52564731457715,4.18140331781018));
#310220=CARTESIAN_POINT('Ctrl Pts',(9.37636619960977,5.55546570851116,4.19252178224798));
#310221=CARTESIAN_POINT('Ctrl Pts',(9.36704599054229,5.56158859045169,4.19534623936898));
#310222=CARTESIAN_POINT('Ctrl Pts',(9.3575,5.56709997066096,4.19845583392679));
#310223=CARTESIAN_POINT('',(9.5,5.32028273058909,-4.19845583392491));
#310224=CARTESIAN_POINT('',(9.5,5.3202827305824,5.));
#310225=CARTESIAN_POINT('',(9.35750000000016,5.56709997066087,-4.19845583392674));
#310226=CARTESIAN_POINT('Ctrl Pts',(9.35750000000016,5.56709997066087,-4.19845583392674));
#310227=CARTESIAN_POINT('Ctrl Pts',(9.3670459905424,5.56158859045162,-4.19534623936895));
#310228=CARTESIAN_POINT('Ctrl Pts',(9.37636619960982,5.55546570851112,-4.19252178224797));
#310229=CARTESIAN_POINT('Ctrl Pts',(9.41636704119957,5.52564731457715,-4.18140331781018));
#310230=CARTESIAN_POINT('Ctrl Pts',(9.44299369100292,5.49538607396019,-4.17694939724907));
#310231=CARTESIAN_POINT('Ctrl Pts',(9.48064078915421,5.43017938720461,-4.17694939724907));
#310232=CARTESIAN_POINT('Ctrl Pts',(9.49353446737686,5.39198941174876,-4.18140331781018));
#310233=CARTESIAN_POINT('Ctrl Pts',(9.4993575332286,5.34243846979447,-4.19252178224748));
#310234=CARTESIAN_POINT('Ctrl Pts',(9.49999999999974,5.33130549100545,-4.19534623936784));
#310235=CARTESIAN_POINT('Ctrl Pts',(9.5,5.32028273058909,-4.1984558339249));
#310236=CARTESIAN_POINT('',(9.3575,5.56709997066097,5.));
#310237=CARTESIAN_POINT('Origin',(-2.11419423634674E-15,10.6405654611648,
5.));
#310238=CARTESIAN_POINT('',(0.142500000000837,10.8873827012429,4.19845583392707));
#310239=CARTESIAN_POINT('',(-0.142499999999995,10.8873827012434,4.19845583392679));
#310240=CARTESIAN_POINT('Ctrl Pts',(0.142500000000829,10.8873827012429,
4.19845583392706));
#310241=CARTESIAN_POINT('Ctrl Pts',(0.132954009458285,10.8928940814523,
4.19534623936915));
#310242=CARTESIAN_POINT('Ctrl Pts',(0.122991333619391,10.8979041783033,
4.19252178224805));
#310243=CARTESIAN_POINT('Ctrl Pts',(0.0771674261772861,10.9176367263259,
4.18140331781018));
#310244=CARTESIAN_POINT('Ctrl Pts',(0.0376470981512924,10.9255654611648,
4.17694939724907));
#310245=CARTESIAN_POINT('Ctrl Pts',(-0.0376470981512968,10.9255654611648,
4.17694939724907));
#310246=CARTESIAN_POINT('Ctrl Pts',(-0.0771674261772924,10.9176367263259,
4.18140331781018));
#310247=CARTESIAN_POINT('Ctrl Pts',(-0.122991333619098,10.8979041783034,
4.19252178224798));
#310248=CARTESIAN_POINT('Ctrl Pts',(-0.13295400945771,10.8928940814526,
4.19534623936898));
#310249=CARTESIAN_POINT('Ctrl Pts',(-0.142499999999999,10.8873827012434,
4.19845583392679));
#310250=CARTESIAN_POINT('',(0.142499999990597,10.8873827012488,-4.19845583392373));
#310251=CARTESIAN_POINT('',(0.142499999999998,10.8873827012434,5.));
#310252=CARTESIAN_POINT('',(-0.142499999999839,10.8873827012435,-4.19845583392674));
#310253=CARTESIAN_POINT('Ctrl Pts',(-0.142499999999839,10.8873827012435,
-4.19845583392674));
#310254=CARTESIAN_POINT('Ctrl Pts',(-0.132954009457597,10.8928940814527,
-4.19534623936895));
#310255=CARTESIAN_POINT('Ctrl Pts',(-0.122991333619039,10.8979041783034,
-4.19252178224797));
#310256=CARTESIAN_POINT('Ctrl Pts',(-0.0771674261772909,10.9176367263259,
-4.18140331781018));
#310257=CARTESIAN_POINT('Ctrl Pts',(-0.0376470981512967,10.9255654611648,
-4.17694939724907));
#310258=CARTESIAN_POINT('Ctrl Pts',(0.0376470981512925,10.9255654611648,
-4.17694939724907));
#310259=CARTESIAN_POINT('Ctrl Pts',(0.0771674261772871,10.9176367263259,
-4.18140331781018));
#310260=CARTESIAN_POINT('Ctrl Pts',(0.122991333615721,10.8979041783048,
-4.19252178224716));
#310261=CARTESIAN_POINT('Ctrl Pts',(0.132954009451165,10.8928940814559,
-4.19534623936713));
#310262=CARTESIAN_POINT('Ctrl Pts',(0.142499999990594,10.8873827012488,
-4.19845583392373));
#310263=CARTESIAN_POINT('',(-0.142500000000002,10.8873827012434,5.));
#310264=CARTESIAN_POINT('Origin',(-9.215,5.3202827305824,5.));
#310265=CARTESIAN_POINT('',(-9.35749999999916,5.56709997066145,4.19845583392707));
#310266=CARTESIAN_POINT('',(-9.5,5.32028273058247,4.19845583392678));
#310267=CARTESIAN_POINT('Ctrl Pts',(-9.35749999999916,5.56709997066145,
4.19845583392706));
#310268=CARTESIAN_POINT('Ctrl Pts',(-9.36704599054174,5.56158859045205,
4.19534623936915));
#310269=CARTESIAN_POINT('Ctrl Pts',(-9.37636619960951,5.55546570851135,
4.19252178224805));
#310270=CARTESIAN_POINT('Ctrl Pts',(-9.41636704119957,5.52564731457715,
4.18140331781018));
#310271=CARTESIAN_POINT('Ctrl Pts',(-9.44299369100292,5.49538607396019,
4.17694939724907));
#310272=CARTESIAN_POINT('Ctrl Pts',(-9.48064078915421,5.43017938720461,
4.17694939724907));
#310273=CARTESIAN_POINT('Ctrl Pts',(-9.49353446737686,5.39198941174876,
4.18140331781018));
#310274=CARTESIAN_POINT('Ctrl Pts',(-9.49935753322886,5.34243846979225,
4.19252178224798));
#310275=CARTESIAN_POINT('Ctrl Pts',(-9.5,5.33130549100099,4.19534623936897));
#310276=CARTESIAN_POINT('Ctrl Pts',(-9.5,5.32028273058247,4.19845583392677));
#310277=CARTESIAN_POINT('',(-9.3575000000094,5.56709997065554,-4.19845583392373));
#310278=CARTESIAN_POINT('',(-9.3575,5.56709997066097,5.));
#310279=CARTESIAN_POINT('',(-9.5,5.32028273058339,-4.19845583392652));
#310280=CARTESIAN_POINT('Ctrl Pts',(-9.5,5.32028273058339,-4.19845583392651));
#310281=CARTESIAN_POINT('Ctrl Pts',(-9.49999999999996,5.33130549100161,
-4.19534623936881));
#310282=CARTESIAN_POINT('Ctrl Pts',(-9.49935753322882,5.34243846979256,
-4.19252178224791));
#310283=CARTESIAN_POINT('Ctrl Pts',(-9.49353446737686,5.39198941174876,
-4.18140331781018));
#310284=CARTESIAN_POINT('Ctrl Pts',(-9.48064078915421,5.43017938720461,
-4.17694939724907));
#310285=CARTESIAN_POINT('Ctrl Pts',(-9.44299369100292,5.49538607396019,
-4.17694939724907));
#310286=CARTESIAN_POINT('Ctrl Pts',(-9.41636704119957,5.52564731457715,
-4.18140331781018));
#310287=CARTESIAN_POINT('Ctrl Pts',(-9.37636619961271,5.55546570850896,
-4.19252178224716));
#310288=CARTESIAN_POINT('Ctrl Pts',(-9.36704599054841,5.56158859044768,
-4.19534623936713));
#310289=CARTESIAN_POINT('Ctrl Pts',(-9.3575000000094,5.56709997065554,-4.19845583392373));
#310290=CARTESIAN_POINT('',(-9.5,5.3202827305824,5.));
#310291=CARTESIAN_POINT('Origin',(-9.215,-5.3202827305824,5.));
#310292=CARTESIAN_POINT('',(-9.5,-5.3202827305819,4.19845583392694));
#310293=CARTESIAN_POINT('',(-9.3575,-5.56709997066096,4.19845583392679));
#310294=CARTESIAN_POINT('Ctrl Pts',(-9.5,-5.3202827305819,4.19845583392693));
#310295=CARTESIAN_POINT('Ctrl Pts',(-9.50000000000002,-5.33130549100061,
4.19534623936907));
#310296=CARTESIAN_POINT('Ctrl Pts',(-9.49935753322888,-5.34243846979206,
4.19252178224802));
#310297=CARTESIAN_POINT('Ctrl Pts',(-9.49353446737686,-5.39198941174876,
4.18140331781018));
#310298=CARTESIAN_POINT('Ctrl Pts',(-9.48064078915421,-5.43017938720461,
4.17694939724907));
#310299=CARTESIAN_POINT('Ctrl Pts',(-9.44299369100292,-5.49538607396019,
4.17694939724907));
#310300=CARTESIAN_POINT('Ctrl Pts',(-9.41636704119957,-5.52564731457715,
4.18140331781018));
#310301=CARTESIAN_POINT('Ctrl Pts',(-9.37636619960977,-5.55546570851116,
4.19252178224798));
#310302=CARTESIAN_POINT('Ctrl Pts',(-9.36704599054229,-5.56158859045169,
4.19534623936898));
#310303=CARTESIAN_POINT('Ctrl Pts',(-9.3575,-5.56709997066096,4.19845583392679));
#310304=CARTESIAN_POINT('',(-9.5,-5.32028273058909,-4.19845583392491));
#310305=CARTESIAN_POINT('',(-9.5,-5.3202827305824,5.));
#310306=CARTESIAN_POINT('',(-9.35750000000016,-5.56709997066087,-4.19845583392674));
#310307=CARTESIAN_POINT('Ctrl Pts',(-9.35750000000016,-5.56709997066087,
-4.19845583392674));
#310308=CARTESIAN_POINT('Ctrl Pts',(-9.36704599054239,-5.56158859045162,
-4.19534623936895));
#310309=CARTESIAN_POINT('Ctrl Pts',(-9.37636619960982,-5.55546570851112,
-4.19252178224797));
#310310=CARTESIAN_POINT('Ctrl Pts',(-9.41636704119957,-5.52564731457715,
-4.18140331781018));
#310311=CARTESIAN_POINT('Ctrl Pts',(-9.44299369100292,-5.49538607396019,
-4.17694939724907));
#310312=CARTESIAN_POINT('Ctrl Pts',(-9.48064078915421,-5.43017938720461,
-4.17694939724907));
#310313=CARTESIAN_POINT('Ctrl Pts',(-9.49353446737686,-5.39198941174876,
-4.18140331781018));
#310314=CARTESIAN_POINT('Ctrl Pts',(-9.4993575332286,-5.34243846979447,
-4.19252178224748));
#310315=CARTESIAN_POINT('Ctrl Pts',(-9.49999999999974,-5.33130549100545,
-4.19534623936784));
#310316=CARTESIAN_POINT('Ctrl Pts',(-9.5,-5.32028273058909,-4.1984558339249));
#310317=CARTESIAN_POINT('',(-9.3575,-5.56709997066097,5.));
#310318=CARTESIAN_POINT('Origin',(-1.62630325872825E-15,-10.6405654611648,
5.));
#310319=CARTESIAN_POINT('',(-0.142500000000841,-10.8873827012429,4.19845583392707));
#310320=CARTESIAN_POINT('',(0.142499999999992,-10.8873827012434,4.19845583392679));
#310321=CARTESIAN_POINT('Ctrl Pts',(-0.142500000000832,-10.8873827012429,
4.19845583392706));
#310322=CARTESIAN_POINT('Ctrl Pts',(-0.132954009458289,-10.8928940814523,
4.19534623936915));
#310323=CARTESIAN_POINT('Ctrl Pts',(-0.122991333619395,-10.8979041783033,
4.19252178224806));
#310324=CARTESIAN_POINT('Ctrl Pts',(-0.0771674261772907,-10.9176367263259,
4.18140331781018));
#310325=CARTESIAN_POINT('Ctrl Pts',(-0.0376470981512962,-10.9255654611648,
4.17694939724907));
#310326=CARTESIAN_POINT('Ctrl Pts',(0.037647098151293,-10.9255654611648,
4.17694939724907));
#310327=CARTESIAN_POINT('Ctrl Pts',(0.0771674261772873,-10.9176367263259,
4.18140331781018));
#310328=CARTESIAN_POINT('Ctrl Pts',(0.122991333619093,-10.8979041783034,
4.19252178224798));
#310329=CARTESIAN_POINT('Ctrl Pts',(0.132954009457706,-10.8928940814526,
4.19534623936898));
#310330=CARTESIAN_POINT('Ctrl Pts',(0.142499999999995,-10.8873827012434,
4.19845583392679));
#310331=CARTESIAN_POINT('',(-0.1424999999906,-10.8873827012488,-4.19845583392373));
#310332=CARTESIAN_POINT('',(-0.142500000000002,-10.8873827012434,5.));
#310333=CARTESIAN_POINT('',(0.142499999999835,-10.8873827012435,-4.19845583392674));
#310334=CARTESIAN_POINT('Ctrl Pts',(0.142499999999835,-10.8873827012435,
-4.19845583392674));
#310335=CARTESIAN_POINT('Ctrl Pts',(0.132954009457593,-10.8928940814527,
-4.19534623936895));
#310336=CARTESIAN_POINT('Ctrl Pts',(0.122991333619035,-10.8979041783034,
-4.19252178224797));
#310337=CARTESIAN_POINT('Ctrl Pts',(0.0771674261772873,-10.9176367263259,
-4.18140331781018));
#310338=CARTESIAN_POINT('Ctrl Pts',(0.0376470981512929,-10.9255654611648,
-4.17694939724907));
#310339=CARTESIAN_POINT('Ctrl Pts',(-0.0376470981512963,-10.9255654611648,
-4.17694939724907));
#310340=CARTESIAN_POINT('Ctrl Pts',(-0.0771674261772907,-10.9176367263259,
-4.18140331781018));
#310341=CARTESIAN_POINT('Ctrl Pts',(-0.122991333615725,-10.8979041783048,
-4.19252178224716));
#310342=CARTESIAN_POINT('Ctrl Pts',(-0.132954009451169,-10.8928940814559,
-4.19534623936713));
#310343=CARTESIAN_POINT('Ctrl Pts',(-0.142499999990597,-10.8873827012488,
-4.19845583392373));
#310344=CARTESIAN_POINT('',(0.142499999999998,-10.8873827012434,5.));
#310345=CARTESIAN_POINT('Origin',(9.215,-5.3202827305824,5.));
#310346=CARTESIAN_POINT('',(9.35749999999916,-5.56709997066145,4.19845583392707));
#310347=CARTESIAN_POINT('',(9.5,-5.32028273058247,4.19845583392678));
#310348=CARTESIAN_POINT('Ctrl Pts',(9.35749999999916,-5.56709997066145,
4.19845583392706));
#310349=CARTESIAN_POINT('Ctrl Pts',(9.36704599054174,-5.56158859045205,
4.19534623936915));
#310350=CARTESIAN_POINT('Ctrl Pts',(9.3763661996095,-5.55546570851135,4.19252178224805));
#310351=CARTESIAN_POINT('Ctrl Pts',(9.41636704119957,-5.52564731457715,
4.18140331781018));
#310352=CARTESIAN_POINT('Ctrl Pts',(9.44299369100292,-5.49538607396019,
4.17694939724907));
#310353=CARTESIAN_POINT('Ctrl Pts',(9.48064078915421,-5.43017938720461,
4.17694939724907));
#310354=CARTESIAN_POINT('Ctrl Pts',(9.49353446737686,-5.39198941174876,
4.18140331781018));
#310355=CARTESIAN_POINT('Ctrl Pts',(9.49935753322886,-5.34243846979225,
4.19252178224798));
#310356=CARTESIAN_POINT('Ctrl Pts',(9.5,-5.33130549100099,4.19534623936897));
#310357=CARTESIAN_POINT('Ctrl Pts',(9.5,-5.32028273058247,4.19845583392677));
#310358=CARTESIAN_POINT('',(9.3575000000094,-5.56709997065554,-4.19845583392373));
#310359=CARTESIAN_POINT('',(9.3575,-5.56709997066097,5.));
#310360=CARTESIAN_POINT('',(9.5,-5.3202827305834,-4.19845583392651));
#310361=CARTESIAN_POINT('Ctrl Pts',(9.5,-5.3202827305834,-4.19845583392651));
#310362=CARTESIAN_POINT('Ctrl Pts',(9.49999999999996,-5.33130549100162,
-4.19534623936881));
#310363=CARTESIAN_POINT('Ctrl Pts',(9.49935753322882,-5.34243846979256,
-4.19252178224791));
#310364=CARTESIAN_POINT('Ctrl Pts',(9.49353446737686,-5.39198941174876,
-4.18140331781018));
#310365=CARTESIAN_POINT('Ctrl Pts',(9.48064078915421,-5.43017938720461,
-4.17694939724907));
#310366=CARTESIAN_POINT('Ctrl Pts',(9.44299369100292,-5.49538607396019,
-4.17694939724907));
#310367=CARTESIAN_POINT('Ctrl Pts',(9.41636704119957,-5.52564731457715,
-4.18140331781018));
#310368=CARTESIAN_POINT('Ctrl Pts',(9.37636619961271,-5.55546570850896,
-4.19252178224716));
#310369=CARTESIAN_POINT('Ctrl Pts',(9.36704599054841,-5.56158859044768,
-4.19534623936713));
#310370=CARTESIAN_POINT('Ctrl Pts',(9.3575000000094,-5.56709997065554,-4.19845583392373));
#310371=CARTESIAN_POINT('',(9.5,-5.3202827305824,5.));
#310372=CARTESIAN_POINT('Origin',(0.,0.,-5.));
#310373=CARTESIAN_POINT('',(9.5,0.,-5.));
#310374=CARTESIAN_POINT('Ctrl Pts',(9.5,-5.32028273061113,-4.19845583391869));
#310375=CARTESIAN_POINT('Ctrl Pts',(9.5,-2.47900257549584,-5.));
#310376=CARTESIAN_POINT('Ctrl Pts',(9.5,-8.86951651586679E-16,-5.));
#310377=CARTESIAN_POINT('',(4.75,-8.22724133595217,-5.));
#310378=CARTESIAN_POINT('Ctrl Pts',(4.75000000000002,-8.22724133595217,
-4.99999999999999));
#310379=CARTESIAN_POINT('Ctrl Pts',(6.89687920642992,-6.98774004820225,
-4.99999999999999));
#310380=CARTESIAN_POINT('Ctrl Pts',(9.3575000000334,-5.56709997064169,-4.1984558339159));
#310381=CARTESIAN_POINT('Origin',(0.,0.,-5.));
#310382=CARTESIAN_POINT('Origin',(0.,0.,-5.));
#310383=CARTESIAN_POINT('Ctrl Pts',(0.142499999975816,-10.8873827012573,
-4.1984558339189));
#310384=CARTESIAN_POINT('Ctrl Pts',(2.60312079357385,-9.46674262369993,
-5.));
#310385=CARTESIAN_POINT('Ctrl Pts',(4.75000000000002,-8.22724133595217,
-4.99999999999999));
#310386=CARTESIAN_POINT('',(-4.75,-8.22724133595217,-5.));
#310387=CARTESIAN_POINT('Ctrl Pts',(-4.74999999999998,-8.22724133595218,
-5.));
#310388=CARTESIAN_POINT('Ctrl Pts',(-2.60312079357007,-9.4667426237021,
-5.));
#310389=CARTESIAN_POINT('Ctrl Pts',(-0.142499999966577,-10.8873827012627,
-4.1984558339159));
#310390=CARTESIAN_POINT('Origin',(0.,0.,-5.));
#310391=CARTESIAN_POINT('Origin',(0.,0.,-5.));
#310392=CARTESIAN_POINT('Ctrl Pts',(-9.35750000002419,-5.567099970647,-4.19845583391891));
#310393=CARTESIAN_POINT('Ctrl Pts',(-6.89687920642616,-6.98774004820442,
-5.));
#310394=CARTESIAN_POINT('Ctrl Pts',(-4.74999999999998,-8.22724133595218,
-5.));
#310395=CARTESIAN_POINT('',(-9.5,0.,-5.));
#310396=CARTESIAN_POINT('Ctrl Pts',(-9.5,8.86951651586679E-16,-5.));
#310397=CARTESIAN_POINT('Ctrl Pts',(-9.5,-2.47900257549816,-5.));
#310398=CARTESIAN_POINT('Ctrl Pts',(-9.5,-5.32028273061684,-4.19845583391707));
#310399=CARTESIAN_POINT('Origin',(0.,0.,-5.));
#310400=CARTESIAN_POINT('Origin',(0.,0.,-5.));
#310401=CARTESIAN_POINT('Ctrl Pts',(-9.5,5.32028273061112,-4.19845583391869));
#310402=CARTESIAN_POINT('Ctrl Pts',(-9.5,2.47900257549584,-5.));
#310403=CARTESIAN_POINT('Ctrl Pts',(-9.5,8.86951651586679E-16,-5.));
#310404=CARTESIAN_POINT('',(-4.75,8.22724133595217,-5.));
#310405=CARTESIAN_POINT('Ctrl Pts',(-4.75,8.22724133595217,-5.));
#310406=CARTESIAN_POINT('Ctrl Pts',(-6.89687920642992,6.98774004820225,
-5.));
#310407=CARTESIAN_POINT('Ctrl Pts',(-9.35750000003342,5.56709997064168,
-4.1984558339159));
#310408=CARTESIAN_POINT('Origin',(0.,0.,-5.));
#310409=CARTESIAN_POINT('Origin',(0.,0.,-5.));
#310410=CARTESIAN_POINT('Ctrl Pts',(-0.142499999975832,10.8873827012573,
-4.19845583391891));
#310411=CARTESIAN_POINT('Ctrl Pts',(-2.60312079357384,9.46674262369993,
-5.));
#310412=CARTESIAN_POINT('Ctrl Pts',(-4.75,8.22724133595217,-5.));
#310413=CARTESIAN_POINT('',(4.75,8.22724133595217,-5.));
#310414=CARTESIAN_POINT('Ctrl Pts',(4.74999999999998,8.22724133595218,-5.));
#310415=CARTESIAN_POINT('Ctrl Pts',(2.60312079357007,9.46674262370209,-5.));
#310416=CARTESIAN_POINT('Ctrl Pts',(0.142499999966585,10.8873827012627,
-4.1984558339159));
#310417=CARTESIAN_POINT('Origin',(0.,0.,-5.));
#310418=CARTESIAN_POINT('Origin',(0.,0.,-5.));
#310419=CARTESIAN_POINT('Ctrl Pts',(9.35750000002419,5.567099970647,-4.19845583391891));
#310420=CARTESIAN_POINT('Ctrl Pts',(6.89687920642616,6.98774004820442,-5.));
#310421=CARTESIAN_POINT('Ctrl Pts',(4.74999999999998,8.22724133595218,-5.));
#310422=CARTESIAN_POINT('Ctrl Pts',(9.5,-8.86951651586679E-16,-5.));
#310423=CARTESIAN_POINT('Ctrl Pts',(9.5,2.47900257549816,-5.));
#310424=CARTESIAN_POINT('Ctrl Pts',(9.5,5.32028273061684,-4.19845583391707));
#310425=CARTESIAN_POINT('Origin',(0.,0.,-5.));
#310426=CARTESIAN_POINT('Origin',(0.,0.,5.));
#310427=CARTESIAN_POINT('',(4.75,8.22724133595217,5.));
#310428=CARTESIAN_POINT('Ctrl Pts',(4.75,8.22724133595218,4.99999999999999));
#310429=CARTESIAN_POINT('Ctrl Pts',(2.60312079357424,9.46674262369969,4.99999999999999));
#310430=CARTESIAN_POINT('Ctrl Pts',(0.142499999976817,10.8873827012568,
4.19845583391923));
#310431=CARTESIAN_POINT('',(-4.75,8.22724133595217,5.));
#310432=CARTESIAN_POINT('Ctrl Pts',(-0.14249999997599,10.8873827012572,
4.19845583391897));
#310433=CARTESIAN_POINT('Ctrl Pts',(-2.60312079357392,9.46674262369989,
5.));
#310434=CARTESIAN_POINT('Ctrl Pts',(-4.75000000000002,8.22724133595217,
5.));
#310435=CARTESIAN_POINT('Origin',(0.,0.,5.));
#310436=CARTESIAN_POINT('Origin',(0.,0.,5.));
#310437=CARTESIAN_POINT('Ctrl Pts',(-4.75000000000002,8.22724133595217,
5.));
#310438=CARTESIAN_POINT('Ctrl Pts',(-6.89687920642577,6.98774004820465,
4.99999999999999));
#310439=CARTESIAN_POINT('Ctrl Pts',(-9.35750000002319,5.56709997064759,
4.19845583391923));
#310440=CARTESIAN_POINT('',(-9.5,0.,5.));
#310441=CARTESIAN_POINT('Ctrl Pts',(-9.5,5.32028273061021,4.19845583391894));
#310442=CARTESIAN_POINT('Ctrl Pts',(-9.5,2.47900257549547,5.));
#310443=CARTESIAN_POINT('Ctrl Pts',(-9.5,-8.86951651586679E-16,5.));
#310444=CARTESIAN_POINT('Origin',(0.,0.,5.));
#310445=CARTESIAN_POINT('Origin',(0.,0.,5.));
#310446=CARTESIAN_POINT('Ctrl Pts',(-9.5,-8.86951651586679E-16,5.));
#310447=CARTESIAN_POINT('Ctrl Pts',(-9.5,-2.47900257549523,5.));
#310448=CARTESIAN_POINT('Ctrl Pts',(-9.5,-5.32028273060964,4.19845583391911));
#310449=CARTESIAN_POINT('',(-4.75,-8.22724133595217,5.));
#310450=CARTESIAN_POINT('Ctrl Pts',(-9.35750000002403,-5.5670999706471,
4.19845583391896));
#310451=CARTESIAN_POINT('Ctrl Pts',(-6.8968792064261,-6.98774004820445,
5.));
#310452=CARTESIAN_POINT('Ctrl Pts',(-4.75,-8.22724133595218,4.99999999999999));
#310453=CARTESIAN_POINT('Origin',(0.,0.,5.));
#310454=CARTESIAN_POINT('Origin',(0.,0.,5.));
#310455=CARTESIAN_POINT('Ctrl Pts',(-4.75,-8.22724133595218,4.99999999999999));
#310456=CARTESIAN_POINT('Ctrl Pts',(-2.60312079357424,-9.46674262369969,
4.99999999999999));
#310457=CARTESIAN_POINT('Ctrl Pts',(-0.142499999976817,-10.8873827012568,
4.19845583391923));
#310458=CARTESIAN_POINT('',(4.75,-8.22724133595217,5.));
#310459=CARTESIAN_POINT('Ctrl Pts',(0.142499999975978,-10.8873827012572,
4.19845583391896));
#310460=CARTESIAN_POINT('Ctrl Pts',(2.6031207935739,-9.46674262369989,4.99999999999999));
#310461=CARTESIAN_POINT('Ctrl Pts',(4.75,-8.22724133595218,4.99999999999999));
#310462=CARTESIAN_POINT('Origin',(0.,0.,5.));
#310463=CARTESIAN_POINT('Origin',(0.,0.,5.));
#310464=CARTESIAN_POINT('Ctrl Pts',(4.75,-8.22724133595218,4.99999999999999));
#310465=CARTESIAN_POINT('Ctrl Pts',(6.89687920642576,-6.98774004820466,
5.));
#310466=CARTESIAN_POINT('Ctrl Pts',(9.35750000002319,-5.56709997064759,
4.19845583391923));
#310467=CARTESIAN_POINT('',(9.5,0.,5.));
#310468=CARTESIAN_POINT('Ctrl Pts',(9.5,-5.32028273061021,4.19845583391894));
#310469=CARTESIAN_POINT('Ctrl Pts',(9.5,-2.47900257549547,5.));
#310470=CARTESIAN_POINT('Ctrl Pts',(9.5,8.86951651586679E-16,5.));
#310471=CARTESIAN_POINT('Origin',(0.,0.,5.));
#310472=CARTESIAN_POINT('Origin',(0.,0.,5.));
#310473=CARTESIAN_POINT('Ctrl Pts',(9.5,8.86951651586679E-16,5.));
#310474=CARTESIAN_POINT('Ctrl Pts',(9.5,2.47900257549523,5.));
#310475=CARTESIAN_POINT('Ctrl Pts',(9.5,5.32028273060964,4.19845583391911));
#310476=CARTESIAN_POINT('Ctrl Pts',(9.35750000002403,5.5670999706471,4.19845583391896));
#310477=CARTESIAN_POINT('Ctrl Pts',(6.8968792064261,6.98774004820445,5.));
#310478=CARTESIAN_POINT('Ctrl Pts',(4.75,8.22724133595218,4.99999999999999));
#310479=CARTESIAN_POINT('Origin',(0.,0.,5.));
#310480=CARTESIAN_POINT('Origin',(0.,8.67361737988403E-16,5.));
#310481=CARTESIAN_POINT('Origin',(9.5,-5.48482755730145,5.));
#310482=CARTESIAN_POINT('Origin',(-1.04722137768024E-15,-10.9696551146029,
5.));
#310483=CARTESIAN_POINT('Origin',(-9.5,-5.48482755730145,5.));
#310484=CARTESIAN_POINT('Origin',(-9.5,5.48482755730145,5.));
#310485=CARTESIAN_POINT('Origin',(-1.87852400592822E-15,10.9696551146029,
5.));
#310486=CARTESIAN_POINT('Origin',(9.5,5.48482755730145,5.));
#310487=CARTESIAN_POINT('Origin',(0.,0.,5.));
#310488=CARTESIAN_POINT('',(-6.7,4.68483825596759E-17,5.));
#310489=CARTESIAN_POINT('Origin',(0.,8.67361737988403E-16,5.));
#310490=CARTESIAN_POINT('Origin',(0.,0.,-5.));
#310491=CARTESIAN_POINT('',(6.7,4.68483825596763E-17,-5.));
#310492=CARTESIAN_POINT('Origin',(0.,8.67361737988403E-16,-5.));
#310493=CARTESIAN_POINT('Origin',(0.,8.67361737988403E-16,-5.));
#310494=CARTESIAN_POINT('',(6.7,4.68483825596764E-17,-5.));
#310495=CARTESIAN_POINT('Origin',(0.,8.67361737988403E-16,4.3));
#310496=CARTESIAN_POINT('',(-6.,1.32573658499991E-16,4.3));
#310497=CARTESIAN_POINT('',(-28.75,-14.7745526128092,733.072494025912));
#310498=CARTESIAN_POINT('',(-55.,-14.7745526128092,733.072494025912));
#310499=CARTESIAN_POINT('',(0.,0.,0.));
#310500=CARTESIAN_POINT('',(-700.,1.21302377921855E-14,5.55111512312578E-14));
#310501=CARTESIAN_POINT('',(-350.,64.9999999999994,786.679542586191));
#310502=CARTESIAN_POINT('',(-76.,65.,786.679542586191));
#310503=CARTESIAN_POINT('',(-350.,65.,786.679542586191));
#310504=CARTESIAN_POINT('',(-1.03739584397204E-14,-1.87969082175028E-12,
17.468310215999));
#310505=CARTESIAN_POINT('',(-29.9999999999999,-596.186000000001,-593.823583645623));
#310506=CARTESIAN_POINT('',(-689.000000000372,-350.999999999996,629.255540596918));
#310507=CARTESIAN_POINT('',(-52.7694692252869,-97.9199999800001,-74.9652496205201));
#310508=CARTESIAN_POINT('',(-346.089749425718,-237.316749888869,900.));
#310509=CARTESIAN_POINT('',(0.,-1.37043154602168E-13,-79.5535534289969));
#310510=CARTESIAN_POINT('',(0.,0.,0.));
#310511=CARTESIAN_POINT('',(0.,0.,0.));
#310512=CARTESIAN_POINT('',(-350.,64.9999999999994,646.679542586191));
#310513=CARTESIAN_POINT('',(-350.,64.9999999999994,506.679542586191));
#310514=CARTESIAN_POINT('',(-350.,64.9999999999994,366.679542586191));
#310515=CARTESIAN_POINT('',(-350.,64.9999999999994,226.679542586191));
#310516=CARTESIAN_POINT('',(-350.,64.9999999999994,86.6795425861905));
#310517=CARTESIAN_POINT('',(-350.,64.9999999999994,-53.3204574138095));
#310518=CARTESIAN_POINT('',(-350.,64.9999999999994,-193.32045741381));
#310519=CARTESIAN_POINT('',(-350.,64.9999999999994,-333.32045741381));
#310520=CARTESIAN_POINT('',(-350.,64.9999999999994,-473.32045741381));
#310521=CARTESIAN_POINT('',(-350.,64.9999999999994,-613.32045741381));
#310522=CARTESIAN_POINT('',(-350.,64.9999999999994,-753.32045741381));
#310523=CARTESIAN_POINT('',(-624.,64.9999999999989,786.67954258619));
#310524=CARTESIAN_POINT('',(-624.,64.9999999999989,646.67954258619));
#310525=CARTESIAN_POINT('',(-624.,64.9999999999989,506.67954258619));
#310526=CARTESIAN_POINT('',(-624.,64.9999999999989,366.67954258619));
#310527=CARTESIAN_POINT('',(-624.,64.9999999999989,226.67954258619));
#310528=CARTESIAN_POINT('',(-624.,64.9999999999989,86.6795425861896));
#310529=CARTESIAN_POINT('',(-624.,64.9999999999989,-53.3204574138104));
#310530=CARTESIAN_POINT('',(-624.,64.9999999999989,-193.32045741381));
#310531=CARTESIAN_POINT('',(-624.,64.9999999999989,-333.32045741381));
#310532=CARTESIAN_POINT('',(-624.,64.9999999999989,-473.320457413811));
#310533=CARTESIAN_POINT('',(-624.,64.9999999999989,-613.320457413811));
#310534=CARTESIAN_POINT('',(-624.,64.9999999999989,-753.32045741381));
#310535=CARTESIAN_POINT('',(-76.,65.,646.679542586191));
#310536=CARTESIAN_POINT('',(-76.,65.,506.679542586191));
#310537=CARTESIAN_POINT('',(-76.,65.,366.679542586191));
#310538=CARTESIAN_POINT('',(-76.,65.,226.679542586191));
#310539=CARTESIAN_POINT('',(-76.,65.,86.6795425861913));
#310540=CARTESIAN_POINT('',(-76.,65.,-53.3204574138088));
#310541=CARTESIAN_POINT('',(-76.,65.,-193.320457413809));
#310542=CARTESIAN_POINT('',(-76.,65.,-333.320457413809));
#310543=CARTESIAN_POINT('',(-76.,65.,-473.320457413809));
#310544=CARTESIAN_POINT('',(-76.,65.,-613.320457413809));
#310545=CARTESIAN_POINT('',(-76.,65.,-753.320457413809));
#310546=CARTESIAN_POINT('',(-350.,65.,646.679542586191));
#310547=CARTESIAN_POINT('',(-350.,65.,506.679542586191));
#310548=CARTESIAN_POINT('',(-350.,65.,366.679542586191));
#310549=CARTESIAN_POINT('',(-350.,65.,226.679542586191));
#310550=CARTESIAN_POINT('',(-350.,65.,86.6795425861913));
#310551=CARTESIAN_POINT('',(-350.,65.,-53.3204574138088));
#310552=CARTESIAN_POINT('',(-350.,65.,-193.320457413809));
#310553=CARTESIAN_POINT('',(-350.,65.,-333.320457413809));
#310554=CARTESIAN_POINT('',(-350.,65.,-473.320457413809));
#310555=CARTESIAN_POINT('',(-350.,65.,-613.320457413809));
#310556=CARTESIAN_POINT('',(-350.,65.,-753.320457413809));
#310557=CARTESIAN_POINT('',(0.,6.35342497653196E-15,-1335.17763309729));
#310558=CARTESIAN_POINT('',(-55.,-505.000000000001,-623.823583645623));
#310559=CARTESIAN_POINT('',(-29.9999999999999,-596.185999999999,629.518940596913));
#310560=CARTESIAN_POINT('',(-670.,-596.185999999998,629.518940596916));
#310561=CARTESIAN_POINT('',(-645.,-505.000000000001,-563.823583645623));
#310562=CARTESIAN_POINT('',(-670.,-596.186000000001,-593.823583645623));
#310563=CARTESIAN_POINT('',(-689.000000000377,-350.999999999996,-593.823583645622));
#310564=CARTESIAN_POINT('',(-700.,6.93889390390723E-15,147.530465806044));
#310565=CARTESIAN_POINT('',(-996.089749425718,-237.316749888869,900.));
#310566=CARTESIAN_POINT('',(-996.089749425718,-237.316749888869,-910.));
#310567=CARTESIAN_POINT('',(-346.089749425718,-237.316749888869,-910.));
#310568=CARTESIAN_POINT('',(1.12959785944277E-13,116.043771674681,-115.938012334369));
#310569=CARTESIAN_POINT('',(-3.46944695195361E-14,161.843598183728,-69.4080685677062));
#310570=CARTESIAN_POINT('',(-3.46944695195361E-14,271.027275945681,-1293.05012614444));
#310571=CARTESIAN_POINT('',(4.85722573273506E-14,307.361912710021,-1228.490165925));
#310572=CARTESIAN_POINT('',(-3.46944695195361E-14,268.754100198787,-1249.32529469151));
#310573=CARTESIAN_POINT('',(-700.,-1.88737914186277E-12,1241.56957097783));
#310574=CARTESIAN_POINT('',(-700.,-1.37043154602168E-13,1386.59144271689));
#310575=CARTESIAN_POINT('',(-700.,-253.051427817394,1336.80787044136));
#310576=CARTESIAN_POINT('',(-700.,-116.417554146358,1331.66099350985));
#310577=CARTESIAN_POINT('',(-700.,-273.137929323082,68.3702274196014));
#310578=CARTESIAN_POINT('',(-700.,-310.11029788046,101.287717359324));
#310579=CARTESIAN_POINT('',(-700.,-361.624814238056,74.3829714899288));
#310580=UNCERTAINTY_MEASURE_WITH_UNIT(LENGTH_MEASURE(0.01),#310624,
'DISTANCE_ACCURACY_VALUE',
'Maximum model space distance between geometric entities at asserted c
onnectivities');
#310581=UNCERTAINTY_MEASURE_WITH_UNIT(LENGTH_MEASURE(0.01),#310624,
'DISTANCE_ACCURACY_VALUE',
'Maximum model space distance between geometric entities at asserted c
onnectivities');
#310582=UNCERTAINTY_MEASURE_WITH_UNIT(LENGTH_MEASURE(0.01),#310624,
'DISTANCE_ACCURACY_VALUE',
'Maximum model space distance between geometric entities at asserted c
onnectivities');
#310583=UNCERTAINTY_MEASURE_WITH_UNIT(LENGTH_MEASURE(0.01),#310624,
'DISTANCE_ACCURACY_VALUE',
'Maximum model space distance between geometric entities at asserted c
onnectivities');
#310584=UNCERTAINTY_MEASURE_WITH_UNIT(LENGTH_MEASURE(0.01),#310624,
'DISTANCE_ACCURACY_VALUE',
'Maximum model space distance between geometric entities at asserted c
onnectivities');
#310585=UNCERTAINTY_MEASURE_WITH_UNIT(LENGTH_MEASURE(0.01),#310624,
'DISTANCE_ACCURACY_VALUE',
'Maximum model space distance between geometric entities at asserted c
onnectivities');
#310586=UNCERTAINTY_MEASURE_WITH_UNIT(LENGTH_MEASURE(0.01),#310624,
'DISTANCE_ACCURACY_VALUE',
'Maximum model space distance between geometric entities at asserted c
onnectivities');
#310587=UNCERTAINTY_MEASURE_WITH_UNIT(LENGTH_MEASURE(0.01),#310624,
'DISTANCE_ACCURACY_VALUE',
'Maximum model space distance between geometric entities at asserted c
onnectivities');
#310588=UNCERTAINTY_MEASURE_WITH_UNIT(LENGTH_MEASURE(0.01),#310624,
'DISTANCE_ACCURACY_VALUE',
'Maximum model space distance between geometric entities at asserted c
onnectivities');
#310589=UNCERTAINTY_MEASURE_WITH_UNIT(LENGTH_MEASURE(0.01),#310624,
'DISTANCE_ACCURACY_VALUE',
'Maximum model space distance between geometric entities at asserted c
onnectivities');
#310590=UNCERTAINTY_MEASURE_WITH_UNIT(LENGTH_MEASURE(0.01),#310624,
'DISTANCE_ACCURACY_VALUE',
'Maximum model space distance between geometric entities at asserted c
onnectivities');
#310591=UNCERTAINTY_MEASURE_WITH_UNIT(LENGTH_MEASURE(0.01),#310624,
'DISTANCE_ACCURACY_VALUE',
'Maximum model space distance between geometric entities at asserted c
onnectivities');
#310592=UNCERTAINTY_MEASURE_WITH_UNIT(LENGTH_MEASURE(0.01),#310624,
'DISTANCE_ACCURACY_VALUE',
'Maximum model space distance between geometric entities at asserted c
onnectivities');
#310593=UNCERTAINTY_MEASURE_WITH_UNIT(LENGTH_MEASURE(0.01),#310624,
'DISTANCE_ACCURACY_VALUE',
'Maximum model space distance between geometric entities at asserted c
onnectivities');
#310594=UNCERTAINTY_MEASURE_WITH_UNIT(LENGTH_MEASURE(0.01),#310624,
'DISTANCE_ACCURACY_VALUE',
'Maximum model space distance between geometric entities at asserted c
onnectivities');
#310595=UNCERTAINTY_MEASURE_WITH_UNIT(LENGTH_MEASURE(0.01),#310624,
'DISTANCE_ACCURACY_VALUE',
'Maximum model space distance between geometric entities at asserted c
onnectivities');
#310596=UNCERTAINTY_MEASURE_WITH_UNIT(LENGTH_MEASURE(0.01),#310624,
'DISTANCE_ACCURACY_VALUE',
'Maximum model space distance between geometric entities at asserted c
onnectivities');
#310597=UNCERTAINTY_MEASURE_WITH_UNIT(LENGTH_MEASURE(0.01),#310624,
'DISTANCE_ACCURACY_VALUE',
'Maximum model space distance between geometric entities at asserted c
onnectivities');
#310598=UNCERTAINTY_MEASURE_WITH_UNIT(LENGTH_MEASURE(0.01),#310624,
'DISTANCE_ACCURACY_VALUE',
'Maximum model space distance between geometric entities at asserted c
onnectivities');
#310599=UNCERTAINTY_MEASURE_WITH_UNIT(LENGTH_MEASURE(0.01),#310624,
'DISTANCE_ACCURACY_VALUE',
'Maximum model space distance between geometric entities at asserted c
onnectivities');
#310600=UNCERTAINTY_MEASURE_WITH_UNIT(LENGTH_MEASURE(0.01),#310624,
'DISTANCE_ACCURACY_VALUE',
'Maximum model space distance between geometric entities at asserted c
onnectivities');
#310601=UNCERTAINTY_MEASURE_WITH_UNIT(LENGTH_MEASURE(0.01),#310624,
'DISTANCE_ACCURACY_VALUE',
'Maximum model space distance between geometric entities at asserted c
onnectivities');
#310602=(
GEOMETRIC_REPRESENTATION_CONTEXT(3)
GLOBAL_UNCERTAINTY_ASSIGNED_CONTEXT((#310580))
GLOBAL_UNIT_ASSIGNED_CONTEXT((#310624,#310626,#310627))
REPRESENTATION_CONTEXT('','3D')
);
#310603=(
GEOMETRIC_REPRESENTATION_CONTEXT(3)
GLOBAL_UNCERTAINTY_ASSIGNED_CONTEXT((#310581))
GLOBAL_UNIT_ASSIGNED_CONTEXT((#310624,#310626,#310627))
REPRESENTATION_CONTEXT('','3D')
);
#310604=(
GEOMETRIC_REPRESENTATION_CONTEXT(3)
GLOBAL_UNCERTAINTY_ASSIGNED_CONTEXT((#310582))
GLOBAL_UNIT_ASSIGNED_CONTEXT((#310624,#310626,#310627))
REPRESENTATION_CONTEXT('','3D')
);
#310605=(
GEOMETRIC_REPRESENTATION_CONTEXT(3)
GLOBAL_UNCERTAINTY_ASSIGNED_CONTEXT((#310583))
GLOBAL_UNIT_ASSIGNED_CONTEXT((#310624,#310626,#310627))
REPRESENTATION_CONTEXT('','3D')
);
#310606=(
GEOMETRIC_REPRESENTATION_CONTEXT(3)
GLOBAL_UNCERTAINTY_ASSIGNED_CONTEXT((#310584))
GLOBAL_UNIT_ASSIGNED_CONTEXT((#310624,#310626,#310627))
REPRESENTATION_CONTEXT('','3D')
);
#310607=(
GEOMETRIC_REPRESENTATION_CONTEXT(3)
GLOBAL_UNCERTAINTY_ASSIGNED_CONTEXT((#310585))
GLOBAL_UNIT_ASSIGNED_CONTEXT((#310624,#310626,#310627))
REPRESENTATION_CONTEXT('','3D')
);
#310608=(
GEOMETRIC_REPRESENTATION_CONTEXT(3)
GLOBAL_UNCERTAINTY_ASSIGNED_CONTEXT((#310586))
GLOBAL_UNIT_ASSIGNED_CONTEXT((#310624,#310626,#310627))
REPRESENTATION_CONTEXT('','3D')
);
#310609=(
GEOMETRIC_REPRESENTATION_CONTEXT(3)
GLOBAL_UNCERTAINTY_ASSIGNED_CONTEXT((#310587))
GLOBAL_UNIT_ASSIGNED_CONTEXT((#310624,#310626,#310627))
REPRESENTATION_CONTEXT('','3D')
);
#310610=(
GEOMETRIC_REPRESENTATION_CONTEXT(3)
GLOBAL_UNCERTAINTY_ASSIGNED_CONTEXT((#310588))
GLOBAL_UNIT_ASSIGNED_CONTEXT((#310624,#310626,#310627))
REPRESENTATION_CONTEXT('','3D')
);
#310611=(
GEOMETRIC_REPRESENTATION_CONTEXT(3)
GLOBAL_UNCERTAINTY_ASSIGNED_CONTEXT((#310589))
GLOBAL_UNIT_ASSIGNED_CONTEXT((#310624,#310626,#310627))
REPRESENTATION_CONTEXT('','3D')
);
#310612=(
GEOMETRIC_REPRESENTATION_CONTEXT(3)
GLOBAL_UNCERTAINTY_ASSIGNED_CONTEXT((#310590))
GLOBAL_UNIT_ASSIGNED_CONTEXT((#310624,#310626,#310627))
REPRESENTATION_CONTEXT('','3D')
);
#310613=(
GEOMETRIC_REPRESENTATION_CONTEXT(3)
GLOBAL_UNCERTAINTY_ASSIGNED_CONTEXT((#310591))
GLOBAL_UNIT_ASSIGNED_CONTEXT((#310624,#310626,#310627))
REPRESENTATION_CONTEXT('','3D')
);
#310614=(
GEOMETRIC_REPRESENTATION_CONTEXT(3)
GLOBAL_UNCERTAINTY_ASSIGNED_CONTEXT((#310592))
GLOBAL_UNIT_ASSIGNED_CONTEXT((#310624,#310626,#310627))
REPRESENTATION_CONTEXT('','3D')
);
#310615=(
GEOMETRIC_REPRESENTATION_CONTEXT(3)
GLOBAL_UNCERTAINTY_ASSIGNED_CONTEXT((#310593))
GLOBAL_UNIT_ASSIGNED_CONTEXT((#310624,#310626,#310627))
REPRESENTATION_CONTEXT('','3D')
);
#310616=(
GEOMETRIC_REPRESENTATION_CONTEXT(3)
GLOBAL_UNCERTAINTY_ASSIGNED_CONTEXT((#310594))
GLOBAL_UNIT_ASSIGNED_CONTEXT((#310624,#310626,#310627))
REPRESENTATION_CONTEXT('','3D')
);
#310617=(
GEOMETRIC_REPRESENTATION_CONTEXT(3)
GLOBAL_UNCERTAINTY_ASSIGNED_CONTEXT((#310595))
GLOBAL_UNIT_ASSIGNED_CONTEXT((#310624,#310626,#310627))
REPRESENTATION_CONTEXT('','3D')
);
#310618=(
GEOMETRIC_REPRESENTATION_CONTEXT(3)
GLOBAL_UNCERTAINTY_ASSIGNED_CONTEXT((#310596))
GLOBAL_UNIT_ASSIGNED_CONTEXT((#310624,#310626,#310627))
REPRESENTATION_CONTEXT('','3D')
);
#310619=(
GEOMETRIC_REPRESENTATION_CONTEXT(3)
GLOBAL_UNCERTAINTY_ASSIGNED_CONTEXT((#310597))
GLOBAL_UNIT_ASSIGNED_CONTEXT((#310624,#310626,#310627))
REPRESENTATION_CONTEXT('','3D')
);
#310620=(
GEOMETRIC_REPRESENTATION_CONTEXT(3)
GLOBAL_UNCERTAINTY_ASSIGNED_CONTEXT((#310598))
GLOBAL_UNIT_ASSIGNED_CONTEXT((#310624,#310626,#310627))
REPRESENTATION_CONTEXT('','3D')
);
#310621=(
GEOMETRIC_REPRESENTATION_CONTEXT(3)
GLOBAL_UNCERTAINTY_ASSIGNED_CONTEXT((#310599))
GLOBAL_UNIT_ASSIGNED_CONTEXT((#310624,#310626,#310627))
REPRESENTATION_CONTEXT('','3D')
);
#310622=(
GEOMETRIC_REPRESENTATION_CONTEXT(3)
GLOBAL_UNCERTAINTY_ASSIGNED_CONTEXT((#310600))
GLOBAL_UNIT_ASSIGNED_CONTEXT((#310624,#310626,#310627))
REPRESENTATION_CONTEXT('','3D')
);
#310623=(
GEOMETRIC_REPRESENTATION_CONTEXT(3)
GLOBAL_UNCERTAINTY_ASSIGNED_CONTEXT((#310601))
GLOBAL_UNIT_ASSIGNED_CONTEXT((#310624,#310626,#310627))
REPRESENTATION_CONTEXT('','3D')
);
#310624=(
LENGTH_UNIT()
NAMED_UNIT(*)
SI_UNIT(.MILLI.,.METRE.)
);
#310625=(
LENGTH_UNIT()
NAMED_UNIT(*)
SI_UNIT($,.METRE.)
);
#310626=(
NAMED_UNIT(*)
PLANE_ANGLE_UNIT()
SI_UNIT($,.RADIAN.)
);
#310627=(
NAMED_UNIT(*)
SI_UNIT($,.STERADIAN.)
SOLID_ANGLE_UNIT()
);
#310628=SHAPE_DEFINITION_REPRESENTATION(#310649,#310893);
#310629=SHAPE_DEFINITION_REPRESENTATION(#310650,#310894);
#310630=SHAPE_DEFINITION_REPRESENTATION(#310651,#310895);
#310631=SHAPE_DEFINITION_REPRESENTATION(#310652,#310896);
#310632=SHAPE_DEFINITION_REPRESENTATION(#310653,#310897);
#310633=SHAPE_DEFINITION_REPRESENTATION(#310654,#310898);
#310634=SHAPE_DEFINITION_REPRESENTATION(#310655,#310899);
#310635=SHAPE_DEFINITION_REPRESENTATION(#310656,#310900);
#310636=SHAPE_DEFINITION_REPRESENTATION(#310657,#310901);
#310637=SHAPE_DEFINITION_REPRESENTATION(#310796,#310902);
#310638=SHAPE_DEFINITION_REPRESENTATION(#310797,#310903);
#310639=SHAPE_DEFINITION_REPRESENTATION(#310798,#310904);
#310640=SHAPE_DEFINITION_REPRESENTATION(#310799,#310905);
#310641=SHAPE_DEFINITION_REPRESENTATION(#310800,#310906);
#310642=SHAPE_DEFINITION_REPRESENTATION(#310801,#310907);
#310643=SHAPE_DEFINITION_REPRESENTATION(#310802,#310908);
#310644=SHAPE_DEFINITION_REPRESENTATION(#310803,#310909);
#310645=SHAPE_DEFINITION_REPRESENTATION(#310804,#310910);
#310646=SHAPE_DEFINITION_REPRESENTATION(#310807,#310911);
#310647=SHAPE_DEFINITION_REPRESENTATION(#310808,#310912);
#310648=SHAPE_DEFINITION_REPRESENTATION(#310809,#310913);
#310649=PRODUCT_DEFINITION_SHAPE('',$,#310915);
#310650=PRODUCT_DEFINITION_SHAPE('',$,#310916);
#310651=PRODUCT_DEFINITION_SHAPE('',$,#310917);
#310652=PRODUCT_DEFINITION_SHAPE('',$,#310918);
#310653=PRODUCT_DEFINITION_SHAPE('',$,#310919);
#310654=PRODUCT_DEFINITION_SHAPE('',$,#310920);
#310655=PRODUCT_DEFINITION_SHAPE('',$,#310921);
#310656=PRODUCT_DEFINITION_SHAPE('',$,#310922);
#310657=PRODUCT_DEFINITION_SHAPE('',$,#310923);
#310658=PRODUCT_DEFINITION_SHAPE($,$,#682);
#310659=PRODUCT_DEFINITION_SHAPE($,$,#683);
#310660=PRODUCT_DEFINITION_SHAPE($,$,#684);
#310661=PRODUCT_DEFINITION_SHAPE($,$,#685);
#310662=PRODUCT_DEFINITION_SHAPE($,$,#686);
#310663=PRODUCT_DEFINITION_SHAPE($,$,#687);
#310664=PRODUCT_DEFINITION_SHAPE($,$,#688);
#310665=PRODUCT_DEFINITION_SHAPE($,$,#689);
#310666=PRODUCT_DEFINITION_SHAPE($,$,#690);
#310667=PRODUCT_DEFINITION_SHAPE($,$,#691);
#310668=PRODUCT_DEFINITION_SHAPE($,$,#692);
#310669=PRODUCT_DEFINITION_SHAPE($,$,#693);
#310670=PRODUCT_DEFINITION_SHAPE($,$,#694);
#310671=PRODUCT_DEFINITION_SHAPE($,$,#695);
#310672=PRODUCT_DEFINITION_SHAPE($,$,#696);
#310673=PRODUCT_DEFINITION_SHAPE($,$,#697);
#310674=PRODUCT_DEFINITION_SHAPE($,$,#698);
#310675=PRODUCT_DEFINITION_SHAPE($,$,#699);
#310676=PRODUCT_DEFINITION_SHAPE($,$,#700);
#310677=PRODUCT_DEFINITION_SHAPE($,$,#701);
#310678=PRODUCT_DEFINITION_SHAPE($,$,#702);
#310679=PRODUCT_DEFINITION_SHAPE($,$,#703);
#310680=PRODUCT_DEFINITION_SHAPE($,$,#704);
#310681=PRODUCT_DEFINITION_SHAPE($,$,#705);
#310682=PRODUCT_DEFINITION_SHAPE($,$,#706);
#310683=PRODUCT_DEFINITION_SHAPE($,$,#707);
#310684=PRODUCT_DEFINITION_SHAPE($,$,#708);
#310685=PRODUCT_DEFINITION_SHAPE($,$,#709);
#310686=PRODUCT_DEFINITION_SHAPE($,$,#710);
#310687=PRODUCT_DEFINITION_SHAPE($,$,#711);
#310688=PRODUCT_DEFINITION_SHAPE($,$,#712);
#310689=PRODUCT_DEFINITION_SHAPE($,$,#713);
#310690=PRODUCT_DEFINITION_SHAPE($,$,#714);
#310691=PRODUCT_DEFINITION_SHAPE($,$,#715);
#310692=PRODUCT_DEFINITION_SHAPE($,$,#716);
#310693=PRODUCT_DEFINITION_SHAPE($,$,#717);
#310694=PRODUCT_DEFINITION_SHAPE($,$,#718);
#310695=PRODUCT_DEFINITION_SHAPE($,$,#719);
#310696=PRODUCT_DEFINITION_SHAPE($,$,#720);
#310697=PRODUCT_DEFINITION_SHAPE($,$,#721);
#310698=PRODUCT_DEFINITION_SHAPE($,$,#722);
#310699=PRODUCT_DEFINITION_SHAPE($,$,#723);
#310700=PRODUCT_DEFINITION_SHAPE($,$,#724);
#310701=PRODUCT_DEFINITION_SHAPE($,$,#725);
#310702=PRODUCT_DEFINITION_SHAPE($,$,#726);
#310703=PRODUCT_DEFINITION_SHAPE($,$,#727);
#310704=PRODUCT_DEFINITION_SHAPE($,$,#728);
#310705=PRODUCT_DEFINITION_SHAPE($,$,#729);
#310706=PRODUCT_DEFINITION_SHAPE($,$,#730);
#310707=PRODUCT_DEFINITION_SHAPE($,$,#731);
#310708=PRODUCT_DEFINITION_SHAPE($,$,#732);
#310709=PRODUCT_DEFINITION_SHAPE($,$,#733);
#310710=PRODUCT_DEFINITION_SHAPE($,$,#734);
#310711=PRODUCT_DEFINITION_SHAPE($,$,#735);
#310712=PRODUCT_DEFINITION_SHAPE($,$,#736);
#310713=PRODUCT_DEFINITION_SHAPE($,$,#737);
#310714=PRODUCT_DEFINITION_SHAPE($,$,#738);
#310715=PRODUCT_DEFINITION_SHAPE($,$,#739);
#310716=PRODUCT_DEFINITION_SHAPE($,$,#740);
#310717=PRODUCT_DEFINITION_SHAPE($,$,#741);
#310718=PRODUCT_DEFINITION_SHAPE($,$,#742);
#310719=PRODUCT_DEFINITION_SHAPE($,$,#743);
#310720=PRODUCT_DEFINITION_SHAPE($,$,#744);
#310721=PRODUCT_DEFINITION_SHAPE($,$,#745);
#310722=PRODUCT_DEFINITION_SHAPE($,$,#746);
#310723=PRODUCT_DEFINITION_SHAPE($,$,#747);
#310724=PRODUCT_DEFINITION_SHAPE($,$,#748);
#310725=PRODUCT_DEFINITION_SHAPE($,$,#749);
#310726=PRODUCT_DEFINITION_SHAPE($,$,#750);
#310727=PRODUCT_DEFINITION_SHAPE($,$,#751);
#310728=PRODUCT_DEFINITION_SHAPE($,$,#752);
#310729=PRODUCT_DEFINITION_SHAPE($,$,#753);
#310730=PRODUCT_DEFINITION_SHAPE($,$,#754);
#310731=PRODUCT_DEFINITION_SHAPE($,$,#755);
#310732=PRODUCT_DEFINITION_SHAPE($,$,#756);
#310733=PRODUCT_DEFINITION_SHAPE($,$,#757);
#310734=PRODUCT_DEFINITION_SHAPE($,$,#758);
#310735=PRODUCT_DEFINITION_SHAPE($,$,#759);
#310736=PRODUCT_DEFINITION_SHAPE($,$,#760);
#310737=PRODUCT_DEFINITION_SHAPE($,$,#761);
#310738=PRODUCT_DEFINITION_SHAPE($,$,#762);
#310739=PRODUCT_DEFINITION_SHAPE($,$,#763);
#310740=PRODUCT_DEFINITION_SHAPE($,$,#764);
#310741=PRODUCT_DEFINITION_SHAPE($,$,#765);
#310742=PRODUCT_DEFINITION_SHAPE($,$,#766);
#310743=PRODUCT_DEFINITION_SHAPE($,$,#767);
#310744=PRODUCT_DEFINITION_SHAPE($,$,#768);
#310745=PRODUCT_DEFINITION_SHAPE($,$,#769);
#310746=PRODUCT_DEFINITION_SHAPE($,$,#770);
#310747=PRODUCT_DEFINITION_SHAPE($,$,#771);
#310748=PRODUCT_DEFINITION_SHAPE($,$,#772);
#310749=PRODUCT_DEFINITION_SHAPE($,$,#773);
#310750=PRODUCT_DEFINITION_SHAPE($,$,#774);
#310751=PRODUCT_DEFINITION_SHAPE($,$,#775);
#310752=PRODUCT_DEFINITION_SHAPE($,$,#776);
#310753=PRODUCT_DEFINITION_SHAPE($,$,#777);
#310754=PRODUCT_DEFINITION_SHAPE($,$,#778);
#310755=PRODUCT_DEFINITION_SHAPE($,$,#779);
#310756=PRODUCT_DEFINITION_SHAPE($,$,#780);
#310757=PRODUCT_DEFINITION_SHAPE($,$,#781);
#310758=PRODUCT_DEFINITION_SHAPE($,$,#782);
#310759=PRODUCT_DEFINITION_SHAPE($,$,#783);
#310760=PRODUCT_DEFINITION_SHAPE($,$,#784);
#310761=PRODUCT_DEFINITION_SHAPE($,$,#785);
#310762=PRODUCT_DEFINITION_SHAPE($,$,#786);
#310763=PRODUCT_DEFINITION_SHAPE($,$,#787);
#310764=PRODUCT_DEFINITION_SHAPE($,$,#788);
#310765=PRODUCT_DEFINITION_SHAPE($,$,#789);
#310766=PRODUCT_DEFINITION_SHAPE($,$,#790);
#310767=PRODUCT_DEFINITION_SHAPE($,$,#791);
#310768=PRODUCT_DEFINITION_SHAPE($,$,#792);
#310769=PRODUCT_DEFINITION_SHAPE($,$,#793);
#310770=PRODUCT_DEFINITION_SHAPE($,$,#794);
#310771=PRODUCT_DEFINITION_SHAPE($,$,#795);
#310772=PRODUCT_DEFINITION_SHAPE($,$,#796);
#310773=PRODUCT_DEFINITION_SHAPE($,$,#797);
#310774=PRODUCT_DEFINITION_SHAPE($,$,#798);
#310775=PRODUCT_DEFINITION_SHAPE($,$,#799);
#310776=PRODUCT_DEFINITION_SHAPE($,$,#800);
#310777=PRODUCT_DEFINITION_SHAPE($,$,#801);
#310778=PRODUCT_DEFINITION_SHAPE($,$,#802);
#310779=PRODUCT_DEFINITION_SHAPE($,$,#803);
#310780=PRODUCT_DEFINITION_SHAPE($,$,#804);
#310781=PRODUCT_DEFINITION_SHAPE($,$,#805);
#310782=PRODUCT_DEFINITION_SHAPE($,$,#806);
#310783=PRODUCT_DEFINITION_SHAPE($,$,#807);
#310784=PRODUCT_DEFINITION_SHAPE($,$,#808);
#310785=PRODUCT_DEFINITION_SHAPE($,$,#809);
#310786=PRODUCT_DEFINITION_SHAPE($,$,#810);
#310787=PRODUCT_DEFINITION_SHAPE($,$,#811);
#310788=PRODUCT_DEFINITION_SHAPE($,$,#812);
#310789=PRODUCT_DEFINITION_SHAPE($,$,#813);
#310790=PRODUCT_DEFINITION_SHAPE($,$,#814);
#310791=PRODUCT_DEFINITION_SHAPE($,$,#815);
#310792=PRODUCT_DEFINITION_SHAPE($,$,#816);
#310793=PRODUCT_DEFINITION_SHAPE($,$,#817);
#310794=PRODUCT_DEFINITION_SHAPE($,$,#818);
#310795=PRODUCT_DEFINITION_SHAPE($,$,#819);
#310796=PRODUCT_DEFINITION_SHAPE('',$,#310924);
#310797=PRODUCT_DEFINITION_SHAPE('',$,#310925);
#310798=PRODUCT_DEFINITION_SHAPE('',$,#310926);
#310799=PRODUCT_DEFINITION_SHAPE('',$,#310927);
#310800=PRODUCT_DEFINITION_SHAPE('',$,#310928);
#310801=PRODUCT_DEFINITION_SHAPE('',$,#310929);
#310802=PRODUCT_DEFINITION_SHAPE('',$,#310930);
#310803=PRODUCT_DEFINITION_SHAPE('',$,#310931);
#310804=PRODUCT_DEFINITION_SHAPE('',$,#310932);
#310805=PRODUCT_DEFINITION_SHAPE($,$,#820);
#310806=PRODUCT_DEFINITION_SHAPE($,$,#821);
#310807=PRODUCT_DEFINITION_SHAPE('',$,#310933);
#310808=PRODUCT_DEFINITION_SHAPE('',$,#310934);
#310809=PRODUCT_DEFINITION_SHAPE('',$,#310935);
#310810=PRODUCT_DEFINITION_SHAPE($,$,#822);
#310811=PRODUCT_DEFINITION_SHAPE($,$,#823);
#310812=PRODUCT_DEFINITION_SHAPE($,$,#824);
#310813=PRODUCT_DEFINITION_SHAPE($,$,#825);
#310814=PRODUCT_DEFINITION_SHAPE($,$,#826);
#310815=PRODUCT_DEFINITION_SHAPE($,$,#827);
#310816=PRODUCT_DEFINITION_SHAPE($,$,#828);
#310817=PRODUCT_DEFINITION_SHAPE($,$,#829);
#310818=PRODUCT_DEFINITION_SHAPE($,$,#830);
#310819=PRODUCT_DEFINITION_SHAPE($,$,#831);
#310820=PRODUCT_DEFINITION_SHAPE($,$,#832);
#310821=PRODUCT_DEFINITION_SHAPE($,$,#833);
#310822=PRODUCT_DEFINITION_SHAPE($,$,#834);
#310823=PRODUCT_DEFINITION_SHAPE($,$,#835);
#310824=PRODUCT_DEFINITION_SHAPE($,$,#836);
#310825=PRODUCT_DEFINITION_SHAPE($,$,#837);
#310826=PRODUCT_DEFINITION_SHAPE($,$,#838);
#310827=PRODUCT_DEFINITION_SHAPE($,$,#839);
#310828=PRODUCT_DEFINITION_SHAPE($,$,#840);
#310829=PRODUCT_DEFINITION_SHAPE($,$,#841);
#310830=PRODUCT_DEFINITION_SHAPE($,$,#842);
#310831=PRODUCT_DEFINITION_SHAPE($,$,#843);
#310832=PRODUCT_DEFINITION_SHAPE($,$,#844);
#310833=PRODUCT_DEFINITION_SHAPE($,$,#845);
#310834=PRODUCT_DEFINITION_SHAPE($,$,#846);
#310835=PRODUCT_DEFINITION_SHAPE($,$,#847);
#310836=PRODUCT_DEFINITION_SHAPE($,$,#848);
#310837=PRODUCT_DEFINITION_SHAPE($,$,#849);
#310838=PRODUCT_DEFINITION_SHAPE($,$,#850);
#310839=PRODUCT_DEFINITION_SHAPE($,$,#851);
#310840=PRODUCT_DEFINITION_SHAPE($,$,#852);
#310841=PRODUCT_DEFINITION_SHAPE($,$,#853);
#310842=PRODUCT_DEFINITION_SHAPE($,$,#854);
#310843=PRODUCT_DEFINITION_SHAPE($,$,#855);
#310844=PRODUCT_DEFINITION_SHAPE($,$,#856);
#310845=PRODUCT_DEFINITION_SHAPE($,$,#857);
#310846=PRODUCT_DEFINITION_SHAPE($,$,#858);
#310847=PRODUCT_DEFINITION_SHAPE($,$,#859);
#310848=PRODUCT_DEFINITION_SHAPE($,$,#860);
#310849=PRODUCT_DEFINITION_SHAPE($,$,#861);
#310850=PRODUCT_DEFINITION_SHAPE($,$,#862);
#310851=PRODUCT_DEFINITION_SHAPE($,$,#863);
#310852=PRODUCT_DEFINITION_SHAPE($,$,#864);
#310853=PRODUCT_DEFINITION_SHAPE($,$,#865);
#310854=PRODUCT_DEFINITION_SHAPE($,$,#866);
#310855=PRODUCT_DEFINITION_SHAPE($,$,#867);
#310856=PRODUCT_DEFINITION_SHAPE($,$,#868);
#310857=PRODUCT_DEFINITION_SHAPE($,$,#869);
#310858=PRODUCT_DEFINITION_SHAPE($,$,#870);
#310859=PRODUCT_DEFINITION_SHAPE($,$,#871);
#310860=PRODUCT_DEFINITION_SHAPE($,$,#872);
#310861=PRODUCT_DEFINITION_SHAPE($,$,#873);
#310862=PRODUCT_DEFINITION_SHAPE($,$,#874);
#310863=PRODUCT_DEFINITION_SHAPE($,$,#875);
#310864=PRODUCT_DEFINITION_SHAPE($,$,#876);
#310865=PRODUCT_DEFINITION_SHAPE($,$,#877);
#310866=PRODUCT_DEFINITION_SHAPE($,$,#878);
#310867=PRODUCT_DEFINITION_SHAPE($,$,#879);
#310868=PRODUCT_DEFINITION_SHAPE($,$,#880);
#310869=PRODUCT_DEFINITION_SHAPE($,$,#881);
#310870=PRODUCT_DEFINITION_SHAPE($,$,#882);
#310871=PRODUCT_DEFINITION_SHAPE($,$,#883);
#310872=PRODUCT_DEFINITION_SHAPE($,$,#884);
#310873=PRODUCT_DEFINITION_SHAPE($,$,#885);
#310874=PRODUCT_DEFINITION_SHAPE($,$,#886);
#310875=PRODUCT_DEFINITION_SHAPE($,$,#887);
#310876=PRODUCT_DEFINITION_SHAPE($,$,#888);
#310877=PRODUCT_DEFINITION_SHAPE($,$,#889);
#310878=PRODUCT_DEFINITION_SHAPE($,$,#890);
#310879=PRODUCT_DEFINITION_SHAPE($,$,#891);
#310880=PRODUCT_DEFINITION_SHAPE($,$,#892);
#310881=PRODUCT_DEFINITION_SHAPE($,$,#893);
#310882=PRODUCT_DEFINITION_SHAPE($,$,#894);
#310883=PRODUCT_DEFINITION_SHAPE($,$,#895);
#310884=PRODUCT_DEFINITION_SHAPE($,$,#896);
#310885=PRODUCT_DEFINITION_SHAPE($,$,#897);
#310886=PRODUCT_DEFINITION_SHAPE($,$,#898);
#310887=PRODUCT_DEFINITION_SHAPE($,$,#899);
#310888=PRODUCT_DEFINITION_SHAPE($,$,#900);
#310889=PRODUCT_DEFINITION_SHAPE($,$,#901);
#310890=PRODUCT_DEFINITION_SHAPE($,$,#902);
#310891=PRODUCT_DEFINITION_SHAPE($,$,#903);
#310892=PRODUCT_DEFINITION_SHAPE($,$,#904);
#310893=SHAPE_REPRESENTATION('',(#93963,#104783,#104784,#104785,#104786,
#104787,#104788,#104789,#104790,#104791,#104792,#104793,#104794,#104795,
#104796,#104797,#104798,#104799,#104800,#104801,#104802,#104803,#104804,
#104805,#104806,#104807,#104808,#104809,#104810,#104811,#104812,#104813,
#104814,#104815,#104816,#104817,#104818,#104819,#104820,#104821,#104822,
#104823,#104824,#104825,#104826,#104827,#104828,#104829,#104830,#104831,
#104832,#104833,#104834,#104835,#104836,#104837,#104838,#104839,#104840,
#104841,#104842,#104843,#104844,#104845,#104846,#104847,#104848,#104849,
#104850,#104851,#104852,#104853,#104854,#104855,#104856,#104857,#104858,
#104859,#104860,#104861,#104862,#104863),#310602);
#310894=SHAPE_REPRESENTATION('',(#93964),#310603);
#310895=SHAPE_REPRESENTATION('',(#94023),#310604);
#310896=SHAPE_REPRESENTATION('',(#94082),#310605);
#310897=SHAPE_REPRESENTATION('',(#103332),#310606);
#310898=SHAPE_REPRESENTATION('',(#103339,#103974,#103975,#103976,#103977,
#103978,#103979,#103980,#103981,#103982,#103983,#103984,#103985,#103986,
#103987,#103988,#103989,#103990,#103991,#103992,#103993,#103994,#103995,
#103996,#103997,#103998,#103999,#104000,#104001,#104002,#104003,#104004,
#104005,#104006,#104007,#104008,#104009,#104010,#104011,#104012,#104013,
#104014,#104015,#104016,#104017,#104018,#104019,#104020,#104021,#104022,
#104023,#104024,#104025,#104026,#104027,#104028,#104029,#104030,#104031,
#104032,#104033,#104034,#104035,#104036,#104037,#104038,#104039,#104040,
#104041,#104042,#104043,#104044,#104045,#104046,#104047,#104048,#104049,
#104050,#104051,#104052,#104053,#104054,#104055,#104056,#104057,#104058,
#104059,#104060,#104061,#104062,#104063,#104064,#104065,#104066,#104067,
#104068,#104069,#104070,#104071,#104072,#104073,#104074,#104075,#104076,
#104077,#104078,#104079,#104080,#104081,#104082,#104083,#104084,#104085,
#104086,#104087,#104088,#104089,#104090,#104091,#104092,#104093,#104094,
#104095,#104096,#104097,#104098,#104099,#104100,#104101,#104102,#104103,
#104104,#104105,#104106,#104107,#104108,#104109,#104110,#104111),#310607);
#310899=SHAPE_REPRESENTATION('',(#103340),#310608);
#310900=SHAPE_REPRESENTATION('',(#103547),#310609);
#310901=SHAPE_REPRESENTATION('',(#103923),#310610);
#310902=SHAPE_REPRESENTATION('',(#104112),#310611);
#310903=SHAPE_REPRESENTATION('',(#104129),#310612);
#310904=SHAPE_REPRESENTATION('',(#104223),#310613);
#310905=SHAPE_REPRESENTATION('',(#104248),#310614);
#310906=SHAPE_REPRESENTATION('',(#104543),#310615);
#310907=SHAPE_REPRESENTATION('',(#104554),#310616);
#310908=SHAPE_REPRESENTATION('',(#104561,#104634,#104635),#310617);
#310909=SHAPE_REPRESENTATION('',(#104562),#310618);
#310910=SHAPE_REPRESENTATION('',(#104597),#310619);
#310911=SHAPE_REPRESENTATION('',(#104636,#104781,#104782),#310620);
#310912=SHAPE_REPRESENTATION('',(#104637),#310621);
#310913=SHAPE_REPRESENTATION('',(#104720),#310622);
#310914=PRODUCT_DEFINITION_CONTEXT('part definition',#310979,'design');
#310915=PRODUCT_DEFINITION('MAT-024','MAT-024',#310936,#310914);
#310916=PRODUCT_DEFINITION('Right Side Channel Support Rail',
'Right Side Channel Support Rail',#310937,#310914);
#310917=PRODUCT_DEFINITION('Left Side Channel Support Rail',
'Left Side Channel Support Rail',#310938,#310914);
#310918=PRODUCT_DEFINITION('Motor with Mount Bracket',
'Motor with Mount Bracket',#310939,#310914);
#310919=PRODUCT_DEFINITION('Chain Sprocket Cover',
'Chain Sprocket Cover',#310940,#310914);
#310920=PRODUCT_DEFINITION('Chain Tensioner Sprocket',
'Chain Tensioner Sprocket',#310941,#310914);
#310921=PRODUCT_DEFINITION('15-Tooth Sprocket','15-Tooth Sprocket',#310942,
#310914);
#310922=PRODUCT_DEFINITION('30-Tooth Sprocket','30-Tooth Sprocket',#310943,
#310914);
#310923=PRODUCT_DEFINITION('Chain Link','Chain Link',#310944,#310914);
#310924=PRODUCT_DEFINITION('Steel Tube Conveyor Roller',
'Steel Tube Conveyor Roller',#310945,#310914);
#310925=PRODUCT_DEFINITION('Precision Ball Bearing',
'Precision Ball Bearing',#310946,#310914);
#310926=PRODUCT_DEFINITION('Hexagonal Axle Shaft',
'Hexagonal Axle Shaft',#310947,#310914);
#310927=PRODUCT_DEFINITION('Base Anchor Foot','Base Anchor Foot',#310948,
#310914);
#310928=PRODUCT_DEFINITION('Side Rail Cross Brace',
'Side Rail Cross Brace',#310949,#310914);
#310929=PRODUCT_DEFINITION('End cap','End Cap',#310950,#310914);
#310930=PRODUCT_DEFINITION('Conveyor Support Leg Assembly',
'Conveyor Support Leg Assembly',#310951,#310914);
#310931=PRODUCT_DEFINITION('Leg Gusset Bracket','Leg Gusset Bracket',#310952,
#310914);
#310932=PRODUCT_DEFINITION('Conveyor Support Leg',
'Conveyor Support Leg',#310953,#310914);
#310933=PRODUCT_DEFINITION('Screw and Nut Assembly',
'Screw and Nut Assembly',#310954,#310914);
#310934=PRODUCT_DEFINITION('Class 8.8 Steel Hex Head Screw',
'Class 8.8 Steel Hex Head Screw',#310955,#310914);
#310935=PRODUCT_DEFINITION('Zinc-Plated Steel Hex Nut',
'Zinc-Plated Steel Hex Nut',#310956,#310914);
#310936=PRODUCT_DEFINITION_FORMATION('',$,#310981);
#310937=PRODUCT_DEFINITION_FORMATION('',$,#310982);
#310938=PRODUCT_DEFINITION_FORMATION('',$,#310983);
#310939=PRODUCT_DEFINITION_FORMATION('',$,#310984);
#310940=PRODUCT_DEFINITION_FORMATION('',$,#310985);
#310941=PRODUCT_DEFINITION_FORMATION('',$,#310986);
#310942=PRODUCT_DEFINITION_FORMATION('',$,#310987);
#310943=PRODUCT_DEFINITION_FORMATION('',$,#310988);
#310944=PRODUCT_DEFINITION_FORMATION('',$,#310989);
#310945=PRODUCT_DEFINITION_FORMATION('',$,#310990);
#310946=PRODUCT_DEFINITION_FORMATION('',$,#310991);
#310947=PRODUCT_DEFINITION_FORMATION('',$,#310992);
#310948=PRODUCT_DEFINITION_FORMATION('',$,#310993);
#310949=PRODUCT_DEFINITION_FORMATION('',$,#310994);
#310950=PRODUCT_DEFINITION_FORMATION('',$,#310995);
#310951=PRODUCT_DEFINITION_FORMATION('',$,#310996);
#310952=PRODUCT_DEFINITION_FORMATION('',$,#310997);
#310953=PRODUCT_DEFINITION_FORMATION('',$,#310998);
#310954=PRODUCT_DEFINITION_FORMATION('',$,#310999);
#310955=PRODUCT_DEFINITION_FORMATION('',$,#311000);
#310956=PRODUCT_DEFINITION_FORMATION('',$,#311001);
#310957=PRODUCT_RELATED_PRODUCT_CATEGORY('MAT-024','MAT-024',(#310981));
#310958=PRODUCT_RELATED_PRODUCT_CATEGORY(
'Right Side Channel Support Rail','Right Side Channel Support Rail',(#310982));
#310959=PRODUCT_RELATED_PRODUCT_CATEGORY(
'Left Side Channel Support Rail','Left Side Channel Support Rail',(#310983));
#310960=PRODUCT_RELATED_PRODUCT_CATEGORY('Motor with Mount Bracket',
'Motor with Mount Bracket',(#310984));
#310961=PRODUCT_RELATED_PRODUCT_CATEGORY('Chain Sprocket Cover',
'Chain Sprocket Cover',(#310985));
#310962=PRODUCT_RELATED_PRODUCT_CATEGORY('Chain Tensioner Sprocket',
'Chain Tensioner Sprocket',(#310986));
#310963=PRODUCT_RELATED_PRODUCT_CATEGORY('15-Tooth Sprocket',
'15-Tooth Sprocket',(#310987));
#310964=PRODUCT_RELATED_PRODUCT_CATEGORY('30-Tooth Sprocket',
'30-Tooth Sprocket',(#310988));
#310965=PRODUCT_RELATED_PRODUCT_CATEGORY('Chain Link','Chain Link',(#310989));
#310966=PRODUCT_RELATED_PRODUCT_CATEGORY('Steel Tube Conveyor Roller',
'Steel Tube Conveyor Roller',(#310990));
#310967=PRODUCT_RELATED_PRODUCT_CATEGORY('Precision Ball Bearing',
'Precision Ball Bearing',(#310991));
#310968=PRODUCT_RELATED_PRODUCT_CATEGORY('Hexagonal Axle Shaft',
'Hexagonal Axle Shaft',(#310992));
#310969=PRODUCT_RELATED_PRODUCT_CATEGORY('Base Anchor Foot',
'Base Anchor Foot',(#310993));
#310970=PRODUCT_RELATED_PRODUCT_CATEGORY('Side Rail Cross Brace',
'Side Rail Cross Brace',(#310994));
#310971=PRODUCT_RELATED_PRODUCT_CATEGORY('End Cap','End Cap',(#310995));
#310972=PRODUCT_RELATED_PRODUCT_CATEGORY(
'Conveyor Support Leg Assembly','Conveyor Support Leg Assembly',(#310996));
#310973=PRODUCT_RELATED_PRODUCT_CATEGORY('Leg Gusset Bracket',
'Leg Gusset Bracket',(#310997));
#310974=PRODUCT_RELATED_PRODUCT_CATEGORY('Conveyor Support Leg',
'Conveyor Support Leg',(#310998));
#310975=PRODUCT_RELATED_PRODUCT_CATEGORY('Screw and Nut Assembly',
'Screw and Nut Assembly',(#310999));
#310976=PRODUCT_RELATED_PRODUCT_CATEGORY(
'Class 8.8 Steel Hex Head Screw','Class 8.8 Steel Hex Head Screw',(#311000));
#310977=PRODUCT_RELATED_PRODUCT_CATEGORY('Zinc-Plated Steel Hex Nut',
'Zinc-Plated Steel Hex Nut',(#311001));
#310978=APPLICATION_PROTOCOL_DEFINITION('international standard',
'automotive_design',2009,#310979);
#310979=APPLICATION_CONTEXT(
'Core Data for Automotive Mechanical Design Process');
#310980=PRODUCT_CONTEXT('part definition',#310979,'mechanical');
#310981=PRODUCT('MAT-024','MAT-024','STEP AP214',(#310980));
#310982=PRODUCT('Right Side Channel Support Rail',
'Right Side Channel Support Rail',$,(#310980));
#310983=PRODUCT('Left Side Channel Support Rail',
'Left Side Channel Support Rail',$,(#310980));
#310984=PRODUCT('Motor with Mount Bracket','Motor with Mount Bracket',$,
(#310980));
#310985=PRODUCT('Chain Sprocket Cover','Chain Sprocket Cover',$,(#310980));
#310986=PRODUCT('Chain Tensioner Sprocket','Chain Tensioner Sprocket',$,
(#310980));
#310987=PRODUCT('15-Tooth Sprocket','15-Tooth Sprocket',$,(#310980));
#310988=PRODUCT('30-Tooth Sprocket','30-Tooth Sprocket',$,(#310980));
#310989=PRODUCT('Chain Link','Chain Link',$,(#310980));
#310990=PRODUCT('Steel Tube Conveyor Roller',
'Steel Tube Conveyor Roller',$,(#310980));
#310991=PRODUCT('Precision Ball Bearing','Precision Ball Bearing',$,(#310980));
#310992=PRODUCT('Hexagonal Axle Shaft','Hexagonal Axle Shaft',$,(#310980));
#310993=PRODUCT('Base Anchor Foot','Base Anchor Foot',$,(#310980));
#310994=PRODUCT('Side Rail Cross Brace','Side Rail Cross Brace',$,(#310980));
#310995=PRODUCT('End cap','End Cap','End cap',(#310980));
#310996=PRODUCT('Conveyor Support Leg Assembly',
'Conveyor Support Leg Assembly',$,(#310980));
#310997=PRODUCT('Leg Gusset Bracket','Leg Gusset Bracket',$,(#310980));
#310998=PRODUCT('Conveyor Support Leg','Conveyor Support Leg',$,(#310980));
#310999=PRODUCT('Screw and Nut Assembly','Screw and Nut Assembly',$,(#310980));
#311000=PRODUCT('Class 8.8 Steel Hex Head Screw',
'Class 8.8 Steel Hex Head Screw',$,(#310980));
#311001=PRODUCT('Zinc-Plated Steel Hex Nut','Zinc-Plated Steel Hex Nut',
$,(#310980));
#311002=PRESENTATION_STYLE_ASSIGNMENT((#311009));
#311003=PRESENTATION_STYLE_ASSIGNMENT((#311010));
#311004=PRESENTATION_STYLE_ASSIGNMENT((#311011));
#311005=PRESENTATION_STYLE_ASSIGNMENT((#311012));
#311006=PRESENTATION_STYLE_ASSIGNMENT((#311013));
#311007=PRESENTATION_STYLE_ASSIGNMENT((#311014));
#311008=PRESENTATION_STYLE_ASSIGNMENT((#311015));
#311009=SURFACE_STYLE_USAGE(.BOTH.,#311016);
#311010=SURFACE_STYLE_USAGE(.BOTH.,#311017);
#311011=SURFACE_STYLE_USAGE(.BOTH.,#311018);
#311012=SURFACE_STYLE_USAGE(.BOTH.,#311019);
#311013=SURFACE_STYLE_USAGE(.BOTH.,#311020);
#311014=SURFACE_STYLE_USAGE(.BOTH.,#311021);
#311015=SURFACE_STYLE_USAGE(.BOTH.,#311022);
#311016=SURFACE_SIDE_STYLE('',(#311023));
#311017=SURFACE_SIDE_STYLE('',(#311024));
#311018=SURFACE_SIDE_STYLE('',(#311025));
#311019=SURFACE_SIDE_STYLE('',(#311026));
#311020=SURFACE_SIDE_STYLE('',(#311027));
#311021=SURFACE_SIDE_STYLE('',(#311028));
#311022=SURFACE_SIDE_STYLE('',(#311029));
#311023=SURFACE_STYLE_FILL_AREA(#311030);
#311024=SURFACE_STYLE_FILL_AREA(#311031);
#311025=SURFACE_STYLE_FILL_AREA(#311032);
#311026=SURFACE_STYLE_FILL_AREA(#311033);
#311027=SURFACE_STYLE_FILL_AREA(#311034);
#311028=SURFACE_STYLE_FILL_AREA(#311035);
#311029=SURFACE_STYLE_FILL_AREA(#311036);
#311030=FILL_AREA_STYLE('Steel - Satin',(#311037));
#311031=FILL_AREA_STYLE('Opaque(97,158,199)',(#311038));
#311032=FILL_AREA_STYLE('Opaque(227,224,212)',(#311039));
#311033=FILL_AREA_STYLE('Opaque(20,51,87)',(#311040));
#311034=FILL_AREA_STYLE('Opaque(61,176,222)',(#311041));
#311035=FILL_AREA_STYLE('Opaque(122,133,145)',(#311042));
#311036=FILL_AREA_STYLE('Opaque(31,36,43)',(#311043));
#311037=FILL_AREA_STYLE_COLOUR('Steel - Satin',#311044);
#311038=FILL_AREA_STYLE_COLOUR('Opaque(97,158,199)',#311045);
#311039=FILL_AREA_STYLE_COLOUR('Opaque(227,224,212)',#311046);
#311040=FILL_AREA_STYLE_COLOUR('Opaque(20,51,87)',#311047);
#311041=FILL_AREA_STYLE_COLOUR('Opaque(61,176,222)',#311048);
#311042=FILL_AREA_STYLE_COLOUR('Opaque(122,133,145)',#311049);
#311043=FILL_AREA_STYLE_COLOUR('Opaque(31,36,43)',#311050);
#311044=COLOUR_RGB('Steel - Satin',0.627450980392157,0.627450980392157,
0.627450980392157);
#311045=COLOUR_RGB('Opaque(97,158,199)',0.380392156862745,0.619607843137255,
0.780392156862745);
#311046=COLOUR_RGB('Opaque(227,224,212)',0.890196078431372,0.87843137254902,
0.831372549019608);
#311047=COLOUR_RGB('Opaque(20,51,87)',0.0784313725490196,0.2,0.341176470588235);
#311048=COLOUR_RGB('Opaque(61,176,222)',0.23921568627451,0.690196078431373,
0.870588235294118);
#311049=COLOUR_RGB('Opaque(122,133,145)',0.47843137254902,0.52156862745098,
0.568627450980392);
#311050=COLOUR_RGB('Opaque(31,36,43)',0.12156862745098,0.141176470588235,
0.168627450980392);
ENDSEC;
END-ISO-10303-21;
